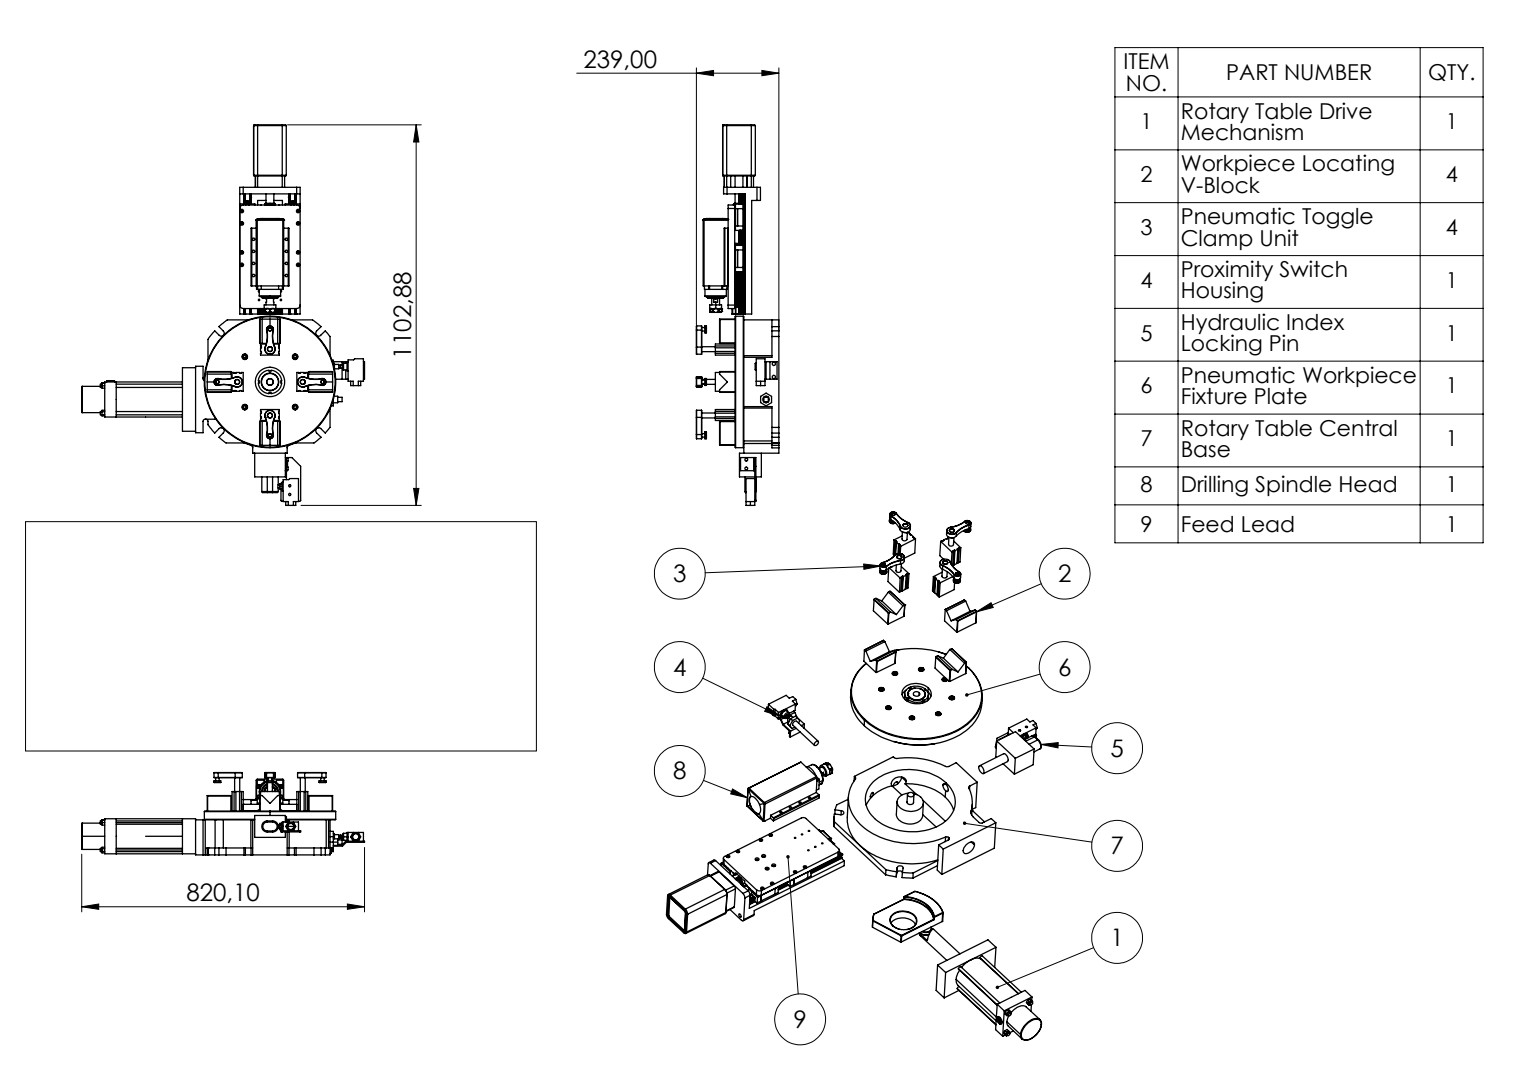
ISO-10303-21;
HEADER;
FILE_DESCRIPTION (('STEP AP214'),
    '1' );
FILE_NAME ('BR-Y-104',
    '2026-10-07T11:37:37',
    ( '' ),
    ( '' ),
    'SwSTEP 2.0',
    'SolidWorks 2020',
    '' );
FILE_SCHEMA (( 'AUTOMOTIVE_DESIGN' ));
ENDSEC;

DATA;
#1 = CARTESIAN_POINT ( 'NONE',  ( 98.82205551832399237, -39.36200594543229414, 279.3785665600675543 ) ) ;
#2 = VECTOR ( 'NONE', #11114, 1000.000000000000000 ) ;
#3 = CARTESIAN_POINT ( 'NONE',  ( -7.205548786489490269E-13, 127.0000000000000000, 111.1250000000000000 ) ) ;
#4 = CARTESIAN_POINT ( 'NONE',  ( 105.4244293397738659, -47.72525222749325735, 147.4584824187689662 ) ) ;
#5 = LINE ( 'NONE', #3140, #30301 ) ;
#6 = CARTESIAN_POINT ( 'NONE',  ( 55.11501535284990183, 101.5999999999999943, 183.9403141659174992 ) ) ;
#7 = DIRECTION ( 'NONE',  ( 0.000000000000000000, 1.000000000000000000, 0.000000000000000000 ) ) ;
#8 = EDGE_CURVE ( 'NONE', #34789, #75812, #45689, .T. ) ;
#9 = CARTESIAN_POINT ( 'NONE',  ( 9.168977498726896158, 73.76155057898466794, 130.2336791939843295 ) ) ;
#10 = CARTESIAN_POINT ( 'NONE',  ( 112.4341072229889136, -46.44469865882210513, 248.9661014663869878 ) ) ;
#11 = CARTESIAN_POINT ( 'NONE',  ( 92.31685958143638970, 83.38015080693119785, -74.38497350661467067 ) ) ;
#12 = AXIS2_PLACEMENT_3D ( 'NONE', #30544, #63723, #30982 ) ;
#13 = ORIENTED_EDGE ( 'NONE', *, *, #80261, .T. ) ;
#14 = CARTESIAN_POINT ( 'NONE',  ( -194.1576000000000022, 0.000000000000000000, -12.69999999999999929 ) ) ;
#15 = EDGE_LOOP ( 'NONE', ( #73624, #35100, #2042, #65680 ) ) ;
#16 = CARTESIAN_POINT ( 'NONE',  ( 97.53157056845665807, -31.04763954905634193, 126.9108633711489915 ) ) ;
#17 = CARTESIAN_POINT ( 'NONE',  ( 83.56670559755357885, -36.73837296219067383, 249.5838068554176630 ) ) ;
#18 = EDGE_CURVE ( 'NONE', #81211, #49424, #24383, .T. ) ;
#19 = VERTEX_POINT ( 'NONE', #31186 ) ;
#20 = ORIENTED_EDGE ( 'NONE', *, *, #86122, .T. ) ;
#21 = ORIENTED_EDGE ( 'NONE', *, *, #73612, .F. ) ;
#22 = DIRECTION ( 'NONE',  ( 0.000000000000000000, 0.000000000000000000, -1.000000000000000000 ) ) ;
#23 = LINE ( 'NONE', #20915, #47197 ) ;
#24 = CARTESIAN_POINT ( 'NONE',  ( 199.3900000000000148, 46.38749999999999574, -50.79999999999999716 ) ) ;
#25 = CARTESIAN_POINT ( 'NONE',  ( 179.7974245136208253, -36.32844715993472562, 237.4678068554150059 ) ) ;
#26 = CARTESIAN_POINT ( 'NONE',  ( 108.8610815749077574, -28.26302276435299987, 182.7404713219719667 ) ) ;
#27 = CARTESIAN_POINT ( 'NONE',  ( 118.1260584382194025, -36.12034675239389259, 269.8822919425776945 ) ) ;
#28 = DIRECTION ( 'NONE',  ( 0.7071067811865491270, -0.7071067811865459074, 7.071067811865492096E-16 ) ) ;
#29 = EDGE_LOOP ( 'NONE', ( #51270, #35552, #65434, #23515 ) ) ;
#30 = CARTESIAN_POINT ( 'NONE',  ( 0.8292115003195463796, 69.84999999999999432, 118.5559999999999832 ) ) ;
#31 = VECTOR ( 'NONE', #9113, 1000.000000000000000 ) ;
#32 = DIRECTION ( 'NONE',  ( 0.2588190451025215166, 0.000000000000000000, -0.9659258262890680902 ) ) ;
#33 = ORIENTED_EDGE ( 'NONE', *, *, #1736, .F. ) ;
#34 = ORIENTED_EDGE ( 'NONE', *, *, #61854, .T. ) ;
#35 = EDGE_CURVE ( 'NONE', #22057, #40854, #8280, .T. ) ;
#36 = DIRECTION ( 'NONE',  ( 0.000000000000000000, 0.000000000000000000, -1.000000000000000000 ) ) ;
#37 = DIRECTION ( 'NONE',  ( 0.000000000000000000, 0.000000000000000000, 1.000000000000000000 ) ) ;
#38 = LINE ( 'NONE', #47715, #64581 ) ;
#39 = CARTESIAN_POINT ( 'NONE',  ( 20.03715912545644073, -24.42818131006202265, 129.9678068554150627 ) ) ;
#40 = CARTESIAN_POINT ( 'NONE',  ( 90.06670390244703128, -104.2784471599414644, 0.2178068554180012661 ) ) ;
#41 = CIRCLE ( 'NONE', #63855, 11.49999999999999645 ) ;
#42 = CARTESIAN_POINT ( 'NONE',  ( 112.8494018163660968, -30.44343212223953543, 198.9067055423629711 ) ) ;
#43 = CARTESIAN_POINT ( 'NONE',  ( 116.1621043582934902, -29.05491297703968101, 74.38419670448293175 ) ) ;
#44 = CARTESIAN_POINT ( 'NONE',  ( 140.9629299006807059, -46.47944715994099596, -5.074374724088994704 ) ) ;
#45 = VERTEX_POINT ( 'NONE', #80264 ) ;
#46 = DIRECTION ( 'NONE',  ( 0.000000000000000000, 0.000000000000000000, -1.000000000000000000 ) ) ;
#47 = ORIENTED_EDGE ( 'NONE', *, *, #89162, .T. ) ;
#48 = LINE ( 'NONE', #40482, #73685 ) ;
#49 = ORIENTED_EDGE ( 'NONE', *, *, #34842, .F. ) ;
#50 = LINE ( 'NONE', #6413, #88589 ) ;
#51 = CARTESIAN_POINT ( 'NONE',  ( 151.0371591254573502, -24.42818131005592974, 249.9678068554149490 ) ) ;
#52 = DIRECTION ( 'NONE',  ( 0.000000000000000000, 0.000000000000000000, -1.000000000000000000 ) ) ;
#53 = AXIS2_PLACEMENT_3D ( 'NONE', #43663, #9164, #36861 ) ;
#54 = CARTESIAN_POINT ( 'NONE',  ( 50.56670390244699576, -22.48495420874030515, 342.9256252759119548 ) ) ;
#55 = ORIENTED_EDGE ( 'NONE', *, *, #81296, .T. ) ;
#56 = CARTESIAN_POINT ( 'NONE',  ( 117.9477513149503523, -41.48675964724572651, 58.49848241876792798 ) ) ;
#58 = DIRECTION ( 'NONE',  ( 0.000000000000000000, -1.000000000000000000, 0.000000000000000000 ) ) ;
#57 = FACE_OUTER_BOUND ( 'NONE', #13007, .T. ) ;
#59 = LINE ( 'NONE', #15039, #77144 ) ;
#60 = CARTESIAN_POINT ( 'NONE',  ( 131.4961476553978912, -17.75123073100106552, 2.855912073278314534 ) ) ;
#61 = EDGE_LOOP ( 'NONE', ( #69387, #53740 ) ) ;
#62 = EDGE_CURVE ( 'NONE', #88900, #78359, #73421, .T. ) ;
#63 = CIRCLE ( 'NONE', #39212, 3.250000000000002665 ) ;
#64 = ADVANCED_FACE ( 'NONE', ( #72976, #57557 ), #58012, .F. ) ;
#65 = DIRECTION ( 'NONE',  ( -0.7071067811865475727, -0.7071067811865475727, 0.000000000000000000 ) ) ;
#66 = ADVANCED_FACE ( 'NONE', ( #65279 ), #44369, .F. ) ;
#67 = DIRECTION ( 'NONE',  ( 0.000000000000000000, -1.000000000000000000, 0.000000000000000000 ) ) ;
#69 = CARTESIAN_POINT ( 'NONE',  ( 163.2449138992999735, -32.11662333284611748, -5.074374724088000832 ) ) ;
#68 = CIRCLE ( 'NONE', #26139, 0.1499999999999965528 ) ;
#70 = VERTEX_POINT ( 'NONE', #52061 ) ;
#71 = CARTESIAN_POINT ( 'NONE',  ( 98.28804800891427362, -28.73186473263583807, 76.73848241876795839 ) ) ;
#72 = ADVANCED_FACE ( 'NONE', ( #9419 ), #85748, .F. ) ;
#74 = CARTESIAN_POINT ( 'NONE',  ( 151.0371591254582881, -46.82818131005593187, 249.9678068554149490 ) ) ;
#73 = FACE_OUTER_BOUND ( 'NONE', #27829, .T. ) ;
#75 = CARTESIAN_POINT ( 'NONE',  ( -9.261585182541612227, 239.0000000000000000, 152.5407914452011369 ) ) ;
#76 = AXIS2_PLACEMENT_3D ( 'NONE', #21854, #16377, #36372 ) ;
#77 = CARTESIAN_POINT ( 'NONE',  ( 128.6924155486683503, -121.3595312563307260, 250.2191008560389776 ) ) ;
#78 = ORIENTED_EDGE ( 'NONE', *, *, #28035, .F. ) ;
#79 = CARTESIAN_POINT ( 'NONE',  ( 116.1942131220465768, -33.21547736372282600, 135.1184824187679396 ) ) ;
#80 = ADVANCED_FACE ( 'NONE', ( #30759 ), #10313, .F. ) ;
#81 = VECTOR ( 'NONE', #81815, 1000.000000000000000 ) ;
#83 = ORIENTED_EDGE ( 'NONE', *, *, #76173, .T. ) ;
#82 = PLANE ( 'NONE',  #68963 ) ;
#84 = CARTESIAN_POINT ( 'NONE',  ( 95.25611604350974915, -37.33230102880721546, 267.3670538473395482 ) ) ;
#85 = DIRECTION ( 'NONE',  ( 0.000000000000000000, 0.000000000000000000, -1.000000000000000000 ) ) ;
#86 = CARTESIAN_POINT ( 'NONE',  ( 143.0667039024470171, -90.27844715994091018, 230.7030882296565721 ) ) ;
#87 = EDGE_CURVE ( 'NONE', #55444, #20525, #67497, .T. ) ;
#88 = CARTESIAN_POINT ( 'NONE',  ( 57.91199999999999903, 20.32000000000000028, 178.6098374884404905 ) ) ;
#89 = CARTESIAN_POINT ( 'NONE',  ( 19.56648329127400032, 0.2215528400590013880, 342.9256252759119548 ) ) ;
#90 = DIRECTION ( 'NONE',  ( 0.000000000000000000, 0.000000000000000000, 1.000000000000000000 ) ) ;
#91 = CARTESIAN_POINT ( 'NONE',  ( -90.24991642302028083, 70.17656663518272353, 94.33976020835999066 ) ) ;
#92 = VECTOR ( 'NONE', #88319, 1000.000000000000000 ) ;
#93 = CARTESIAN_POINT ( 'NONE',  ( 102.2986265273211188, -45.30740241592388884, 187.1727681330549729 ) ) ;
#94 = ORIENTED_EDGE ( 'NONE', *, *, #21602, .F. ) ;
#95 = ORIENTED_EDGE ( 'NONE', *, *, #27973, .F. ) ;
#96 = CARTESIAN_POINT ( 'NONE',  ( 102.7360552222912418, -45.06754756083040547, 163.6149166392309837 ) ) ;
#97 = CARTESIAN_POINT ( 'NONE',  ( 41.56648329127398966, -27.82844715994070484, 78.92562527591199739 ) ) ;
#98 = CARTESIAN_POINT ( 'NONE',  ( 110.5196960824274868, -45.46740155661881033, 19.31967854399191253 ) ) ;
#99 = CARTESIAN_POINT ( 'NONE',  ( 23.49611623194277499, 85.45756874832173366, 299.1102940853953100 ) ) ;
#100 = VECTOR ( 'NONE', #56288, 1000.000000000000000 ) ;
#101 = CARTESIAN_POINT ( 'NONE',  ( 97.80969231062213964, -40.51824920587227297, 266.6357212253427633 ) ) ;
#102 = CARTESIAN_POINT ( 'NONE',  ( 107.3303934170485405, -25.27334761448656764, 321.8751915430112263 ) ) ;
#103 = CIRCLE ( 'NONE', #55178, 11.45913725231036118 ) ;
#104 = CARTESIAN_POINT ( 'NONE',  ( 107.0667039024470313, -104.2784471599420897, -20.48315503890502143 ) ) ;
#105 = CARTESIAN_POINT ( 'NONE',  ( -3.968750000000754508, 127.0000000000000000, 100.8961411191535973 ) ) ;
#106 = CARTESIAN_POINT ( 'NONE',  ( 117.3910620576583312, -35.19077923515891371, 218.9441967044829482 ) ) ;
#107 = CARTESIAN_POINT ( 'NONE',  ( 102.3035641816324102, -89.52844715994213232, -21.78219314458246103 ) ) ;
#108 = ORIENTED_EDGE ( 'NONE', *, *, #23655, .T. ) ;
#109 = ORIENTED_EDGE ( 'NONE', *, *, #12463, .F. ) ;
#110 = CARTESIAN_POINT ( 'NONE',  ( -84.20430400022949868, 76.20343663217360586, -99.77245543246449699 ) ) ;
#111 = CARTESIAN_POINT ( 'NONE',  ( -91.81710919847694186, 87.03046781249439334, -75.00112839233729289 ) ) ;
#112 = CARTESIAN_POINT ( 'NONE',  ( 98.04125204931517601, -41.04130019950920172, 122.6806003489451342 ) ) ;
#113 = DIRECTION ( 'NONE',  ( -1.000000000000000000, 0.000000000000000000, 0.000000000000000000 ) ) ;
#114 = VECTOR ( 'NONE', #52134, 1000.000000000000114 ) ;
#115 = ADVANCED_FACE ( 'NONE', ( #66606 ), #81165, .T. ) ;
#116 = DIRECTION ( 'NONE',  ( 0.000000000000000000, 0.000000000000000000, 1.000000000000000000 ) ) ;
#117 = ORIENTED_EDGE ( 'NONE', *, *, #52215, .T. ) ;
#118 = CARTESIAN_POINT ( 'NONE',  ( 109.6225776363756950, -25.10716277166327615, 25.90419670448196143 ) ) ;
#119 = EDGE_CURVE ( 'NONE', #83222, #86794, #67726, .T. ) ;
#120 = CARTESIAN_POINT ( 'NONE',  ( 116.8850244782298091, -41.80638879970206290, 243.4346728949589647 ) ) ;
#121 = VERTEX_POINT ( 'NONE', #20268 ) ;
#122 = DIRECTION ( 'NONE',  ( 0.000000000000000000, -1.000000000000000000, 0.000000000000000000 ) ) ;
#123 = CARTESIAN_POINT ( 'NONE',  ( 48.16670390244701139, -28.27351298637280408, 342.9256252759109884 ) ) ;
#124 = CARTESIAN_POINT ( 'NONE',  ( 116.9882021585877823, -35.34044312313820058, 168.9370952240663257 ) ) ;
#125 = CARTESIAN_POINT ( 'NONE',  ( 103.0685998583681311, -29.61280089403793525, 58.30237608387695047 ) ) ;
#126 = CARTESIAN_POINT ( 'NONE',  ( 103.0413726597163446, -26.41035368485499646, 166.3603871806729444 ) ) ;
#127 = CIRCLE ( 'NONE', #16099, 7.143750000000004263 ) ;
#128 = DIRECTION ( 'NONE',  ( 1.000000000000000000, 4.163336342344333240E-14, 0.000000000000000000 ) ) ;
#129 = ORIENTED_EDGE ( 'NONE', *, *, #9296, .T. ) ;
#130 = CARTESIAN_POINT ( 'NONE',  ( 27.27158787008327678, 127.0000000000000000, 85.23828826961327820 ) ) ;
#131 = ORIENTED_EDGE ( 'NONE', *, *, #64159, .T. ) ;
#133 = ORIENTED_EDGE ( 'NONE', *, *, #51168, .F. ) ;
#132 = VECTOR ( 'NONE', #74907, 1000.000000000000000 ) ;
#134 = EDGE_CURVE ( 'NONE', #34012, #57634, #4396, .T. ) ;
#135 = DIRECTION ( 'NONE',  ( 0.000000000000000000, -1.000000000000000000, 0.000000000000000000 ) ) ;
#136 = ORIENTED_EDGE ( 'NONE', *, *, #72395, .F. ) ;
#137 = VERTEX_POINT ( 'NONE', #67956 ) ;
#138 = DIRECTION ( 'NONE',  ( 0.000000000000000000, 0.000000000000000000, -1.000000000000000000 ) ) ;
#139 = CARTESIAN_POINT ( 'NONE',  ( 114.8228036748933079, -33.15234975719755539, 103.5924198280769843 ) ) ;
#140 = VECTOR ( 'NONE', #87504, 1000.000000000000000 ) ;
#141 = CARTESIAN_POINT ( 'NONE',  ( 96.49566810458604493, -31.31724962161759507, 245.9499109901969689 ) ) ;
#142 = CARTESIAN_POINT ( 'NONE',  ( 116.8369567342160451, -40.30247308064095790, 218.5470538473399529 ) ) ;
#143 = CARTESIAN_POINT ( 'NONE',  ( 114.8031991714176741, -43.68443766454699073, 34.24419670448197905 ) ) ;
#144 = CARTESIAN_POINT ( 'NONE',  ( 1.925672578516905147E-22, 69.84999999999999432, 130.5560000000000116 ) ) ;
#145 = CARTESIAN_POINT ( 'NONE',  ( 116.7940250750810804, -39.39174829627296504, 94.61447052041835093 ) ) ;
#146 = VECTOR ( 'NONE', #83071, 1000.000000000000000 ) ;
#147 = EDGE_CURVE ( 'NONE', #87632, #64364, #18910, .T. ) ;
#148 = ORIENTED_EDGE ( 'NONE', *, *, #76335, .T. ) ;
#149 = CARTESIAN_POINT ( 'NONE',  ( 70.08426215166053908, -140.6784470016797570, 245.7568090486316805 ) ) ;
#150 = CARTESIAN_POINT ( 'NONE',  ( 98.15811136316399654, -31.42099212808717468, 130.9108633711499863 ) ) ;
#151 = CARTESIAN_POINT ( 'NONE',  ( 106.8402339230401452, -48.62808610490878891, 77.56133956162491927 ) ) ;
#152 = CARTESIAN_POINT ( 'NONE',  ( 104.8318391505165010, -26.46503486849124087, 260.2470538473397710 ) ) ;
#153 = ORIENTED_EDGE ( 'NONE', *, *, #81834, .T. ) ;
#154 = CARTESIAN_POINT ( 'NONE',  ( 115.5175571194294122, -29.60495148624196204, 224.3718157521009573 ) ) ;
#155 = CARTESIAN_POINT ( 'NONE',  ( 47.62500000000000000, 94.53880000000000905, 225.4249999999999829 ) ) ;
#156 = CARTESIAN_POINT ( 'NONE',  ( 107.0664832912739399, -36.72944715994095333, 293.9356252759109793 ) ) ;
#157 = DIRECTION ( 'NONE',  ( 1.000000000000000000, 0.000000000000000000, 0.000000000000000000 ) ) ;
#159 = CARTESIAN_POINT ( 'NONE',  ( 167.2371591254543262, -47.82818131005522844, 249.9678068554149775 ) ) ;
#158 = DIRECTION ( 'NONE',  ( -1.000000000000000078E-15, 0.000000000000000000, 1.000000000000000000 ) ) ;
#160 = CARTESIAN_POINT ( 'NONE',  ( 41.56670390244777735, -36.32844715994104234, 300.4678068554150059 ) ) ;
#161 = CARTESIAN_POINT ( 'NONE',  ( 93.91125933621934507, -111.8737466215629013, -21.78219314458179667 ) ) ;
#162 = DIRECTION ( 'NONE',  ( 3.100000000000000258E-29, -3.100000000000000044E-14, -1.000000000000000000 ) ) ;
#163 = AXIS2_PLACEMENT_3D ( 'NONE', #54109, #40507, #5097 ) ;
#164 = CARTESIAN_POINT ( 'NONE',  ( 88.17226027475679473, -58.72944715994100306, 239.5838068554174924 ) ) ;
#165 = PLANE ( 'NONE',  #8255 ) ;
#166 = ADVANCED_FACE ( 'NONE', ( #82057 ), #80705, .F. ) ;
#167 = CARTESIAN_POINT ( 'NONE',  ( -103.1875000000000000, 127.0000000000000000, -1.080832317973422076E-12 ) ) ;
#169 = ORIENTED_EDGE ( 'NONE', *, *, #32648, .T. ) ;
#168 = DIRECTION ( 'NONE',  ( 0.000000000000000000, 1.000000000000000000, 0.000000000000000000 ) ) ;
#170 = CARTESIAN_POINT ( 'NONE',  ( 147.0667039024470739, -140.6784471599409017, 222.2178068554179902 ) ) ;
#171 = CARTESIAN_POINT ( 'NONE',  ( 96.89273651078235616, -34.20293982824353662, 276.1327681330536734 ) ) ;
#172 = CARTESIAN_POINT ( 'NONE',  ( 117.0331605330187728, -30.31849857022486816, 140.2813395616249750 ) ) ;
#173 = CARTESIAN_POINT ( 'NONE',  ( 106.2234015700748699, -47.79681864418333959, 263.5280062282922131 ) ) ;
#174 = CARTESIAN_POINT ( 'NONE',  ( 51.56670390244799762, -33.35206098992650681, -5.074374724088000832 ) ) ;
#175 = CIRCLE ( 'NONE', #23415, 3.000000000000002665 ) ;
#177 = LINE ( 'NONE', #49653, #51558 ) ;
#176 = DIRECTION ( 'NONE',  ( 1.000000000000000000, 0.000000000000000000, 1.821299053822143307E-16 ) ) ;
#178 = CARTESIAN_POINT ( 'NONE',  ( 164.9212702847350158, -29.73316016639540749, -5.074374724088000832 ) ) ;
#179 = CARTESIAN_POINT ( 'NONE',  ( 84.06648329127399677, -18.82844715994099971, 93.42562527591199739 ) ) ;
#180 = VECTOR ( 'NONE', #42235, 1000.000000000000000 ) ;
#181 = ORIENTED_EDGE ( 'NONE', *, *, #13082, .F. ) ;
#182 = DIRECTION ( 'NONE',  ( 1.000000000000000000, 0.000000000000000000, 0.000000000000000000 ) ) ;
#183 = EDGE_LOOP ( 'NONE', ( #41737, #81659, #77262, #76610 ) ) ;
#184 = CARTESIAN_POINT ( 'NONE',  ( 104.1791519563360993, -28.66003454886012136, 189.7724198280769770 ) ) ;
#185 = EDGE_CURVE ( 'NONE', #48213, #31965, #19881, .T. ) ;
#187 = ORIENTED_EDGE ( 'NONE', *, *, #67758, .F. ) ;
#186 = CARTESIAN_POINT ( 'NONE',  ( 112.0622504009905356, -45.49043716283868832, 187.9900270775093247 ) ) ;
#188 = CARTESIAN_POINT ( 'NONE',  ( -7.661254700127833495, 82.54999999999999716, 275.4630000000000223 ) ) ;
#189 = CARTESIAN_POINT ( 'NONE',  ( 103.8142050530422864, -26.84757730287823563, 161.3299109901969643 ) ) ;
#190 = DIRECTION ( 'NONE',  ( 0.000000000000000000, 1.000000000000000000, 0.000000000000000000 ) ) ;
#191 = EDGE_CURVE ( 'NONE', #23949, #76533, #47936, .T. ) ;
#192 = DIRECTION ( 'NONE',  ( 1.000000000000000000, 0.000000000000000000, 2.283216351027200160E-14 ) ) ;
#193 = DIRECTION ( 'NONE',  ( 0.7071067811865779928, -0.7071067811865171526, 7.071067811865786933E-16 ) ) ;
#194 = AXIS2_PLACEMENT_3D ( 'NONE', #47993, #62984, #27575 ) ;
#195 = LINE ( 'NONE', #54679, #27346 ) ;
#196 = CARTESIAN_POINT ( 'NONE',  ( 31.78666935232898894, -29.62846900982320264, -5.074374724088000832 ) ) ;
#197 = CARTESIAN_POINT ( 'NONE',  ( 97.28369645613162220, -37.51102008256657427, 101.3899109901979472 ) ) ;
#198 = EDGE_LOOP ( 'NONE', ( #58309, #71427, #79095, #45563, #21025 ) ) ;
#199 = ORIENTED_EDGE ( 'NONE', *, *, #77128, .T. ) ;
#201 = ORIENTED_EDGE ( 'NONE', *, *, #40061, .T. ) ;
#200 = VECTOR ( 'NONE', #2081, 1000.000000000000000 ) ;
#202 = CARTESIAN_POINT ( 'NONE',  ( 106.1501016865858844, -27.91533782510476058, 46.59015473446797984 ) ) ;
#203 = DIRECTION ( 'NONE',  ( 5.512527431108029424E-15, -1.000000000000000000, 0.000000000000000000 ) ) ;
#205 = FACE_OUTER_BOUND ( 'NONE', #10836, .T. ) ;
#204 = CARTESIAN_POINT ( 'NONE',  ( 104.6152064257953640, -27.26083179018629465, 196.2784824187679362 ) ) ;
#206 = DIRECTION ( 'NONE',  ( 0.000000000000000000, 0.000000000000000000, -1.000000000000000000 ) ) ;
#207 = DIRECTION ( 'NONE',  ( 1.000000000000000000, 0.000000000000000000, 0.000000000000000000 ) ) ;
#208 = VECTOR ( 'NONE', #84296, 1000.000000000000000 ) ;
#209 = CARTESIAN_POINT ( 'NONE',  ( 37.06648329127298780, 12.92155284005730387, 361.9756252759109998 ) ) ;
#210 = CARTESIAN_POINT ( 'NONE',  ( 41.56670390244777735, -36.32844715994104234, 300.4678068554150059 ) ) ;
#211 = CARTESIAN_POINT ( 'NONE',  ( 67.65599188636636541, -68.44419502099285069, 246.9104243438740696 ) ) ;
#212 = CARTESIAN_POINT ( 'NONE',  ( 107.3333893024683903, -26.32957087652219741, 120.0556252759109555 ) ) ;
#213 = EDGE_LOOP ( 'NONE', ( #60741, #6929, #76892, #6396, #4910, #86505 ) ) ;
#214 = ORIENTED_EDGE ( 'NONE', *, *, #36681, .T. ) ;
#215 = ORIENTED_EDGE ( 'NONE', *, *, #58002, .F. ) ;
#216 = DIRECTION ( 'NONE',  ( -0.000000000000000000, 1.000000000000000000, -0.000000000000000000 ) ) ;
#217 = CARTESIAN_POINT ( 'NONE',  ( 9.720633968232110273E-16, 127.0000000000000000, -111.1250000000000000 ) ) ;
#218 = FACE_OUTER_BOUND ( 'NONE', #6817, .T. ) ;
#219 = CARTESIAN_POINT ( 'NONE',  ( 98.44383420958352815, -35.98725590436672661, 184.0642808457819797 ) ) ;
#220 = CARTESIAN_POINT ( 'NONE',  ( 107.0667039024470313, -104.2784471599414502, 0.2178068554180012661 ) ) ;
#221 = CARTESIAN_POINT ( 'NONE',  ( 104.4907063090252848, -26.97860099647315835, 26.28081536904196014 ) ) ;
#222 = ORIENTED_EDGE ( 'NONE', *, *, #9367, .T. ) ;
#224 = ORIENTED_EDGE ( 'NONE', *, *, #76975, .F. ) ;
#223 = VERTEX_POINT ( 'NONE', #60677 ) ;
#225 = AXIS2_PLACEMENT_3D ( 'NONE', #81195, #12130, #54323 ) ;
#226 = CARTESIAN_POINT ( 'NONE',  ( 136.6090958654750978, -19.77717416134860073, 2.822018739140460308 ) ) ;
#227 = ORIENTED_EDGE ( 'NONE', *, *, #86908, .T. ) ;
#228 = VERTEX_POINT ( 'NONE', #75677 ) ;
#229 = DIRECTION ( 'NONE',  ( 0.7071067811989784069, -0.7071067811741166276, 2.899137802813994686E-29 ) ) ;
#230 = CARTESIAN_POINT ( 'NONE',  ( 115.9278856700424143, -36.79130581669468825, 260.2530118773256049 ) ) ;
#231 = VERTEX_POINT ( 'NONE', #46142 ) ;
#232 = VECTOR ( 'NONE', #61372, 1000.000000000000000 ) ;
#233 = DIRECTION ( 'NONE',  ( 0.000000000000000000, 0.000000000000000000, 1.000000000000000000 ) ) ;
#234 = CARTESIAN_POINT ( 'NONE',  ( -118.6305646578576045, 74.28520294732120988, 54.51736277023807986 ) ) ;
#235 = ORIENTED_EDGE ( 'NONE', *, *, #62757, .T. ) ;
#236 = ORIENTED_EDGE ( 'NONE', *, *, #27432, .F. ) ;
#237 = VECTOR ( 'NONE', #41224, 1000.000000000000114 ) ;
#238 = EDGE_CURVE ( 'NONE', #48773, #70137, #68413, .T. ) ;
#239 = FACE_OUTER_BOUND ( 'NONE', #13018, .T. ) ;
#240 = ORIENTED_EDGE ( 'NONE', *, *, #81916, .T. ) ;
#241 = VERTEX_POINT ( 'NONE', #73874 ) ;
#242 = EDGE_CURVE ( 'NONE', #42621, #19042, #11659, .T. ) ;
#243 = CARTESIAN_POINT ( 'NONE',  ( 102.1978417368446657, -43.31572210571547998, 254.8880903695915947 ) ) ;
#244 = EDGE_CURVE ( 'NONE', #1586, #65784, #48833, .T. ) ;
#245 = CARTESIAN_POINT ( 'NONE',  ( 117.7016330746719035, -39.82606306527180351, 138.5889586092439743 ) ) ;
#246 = CARTESIAN_POINT ( 'NONE',  ( 109.7644292386350457, -47.42453529627131559, 92.78514908543495210 ) ) ;
#247 = SURFACE_STYLE_FILL_AREA ( #77911 ) ;
#248 = DIRECTION ( 'NONE',  ( 0.000000000000000000, 1.000000000000000000, 0.000000000000000000 ) ) ;
#249 = CARTESIAN_POINT ( 'NONE',  ( 118.0406971908402340, -35.41012545131285094, 234.9337205140059552 ) ) ;
#250 = PLANE ( 'NONE',  #16765 ) ;
#251 = CARTESIAN_POINT ( 'NONE',  ( 97.07202379341690346, -35.37891260357572776, 127.2189961379345533 ) ) ;
#252 = ORIENTED_EDGE ( 'NONE', *, *, #45616, .F. ) ;
#253 = CARTESIAN_POINT ( 'NONE',  ( 129.9447564289581010, 80.89704698943971550, 12.61967231918858445 ) ) ;
#255 = EDGE_LOOP ( 'NONE', ( #36658, #16819, #37232, #21617 ) ) ;
#254 = EDGE_CURVE ( 'NONE', #38623, #81994, #26176, .T. ) ;
#256 = VECTOR ( 'NONE', #25789, 1000.000000000000000 ) ;
#257 = EDGE_CURVE ( 'NONE', #42008, #10149, #60224, .T. ) ;
#258 = EDGE_LOOP ( 'NONE', ( #12072, #35059, #37559, #82671 ) ) ;
#259 = CARTESIAN_POINT ( 'NONE',  ( 1.387778780781445676E-14, 224.4999999999999432, 97.27542076772557778 ) ) ;
#260 = EDGE_CURVE ( 'NONE', #76240, #83594, #40692, .T. ) ;
#261 = EDGE_CURVE ( 'NONE', #85910, #25889, #5287, .T. ) ;
#262 = CARTESIAN_POINT ( 'NONE',  ( 50.03799999999999670, 101.5999999999999943, 206.3750000000000000 ) ) ;
#263 = AXIS2_PLACEMENT_3D ( 'NONE', #9661, #10113, #65519 ) ;
#264 = CARTESIAN_POINT ( 'NONE',  ( 113.9865487620526920, -28.11017913222394071, 119.5261014663869474 ) ) ;
#265 = CARTESIAN_POINT ( 'NONE',  ( -6.586072245893089594, 71.69064597417980167, 130.3897833686264676 ) ) ;
#266 = ADVANCED_FACE ( 'NONE', ( #53845 ), #12696, .T. ) ;
#267 = DIRECTION ( 'NONE',  ( 0.000000000000000000, 0.000000000000000000, 1.000000000000000000 ) ) ;
#268 = CYLINDRICAL_SURFACE ( 'NONE', #55688, 7.143750000000004263 ) ;
#271 = CARTESIAN_POINT ( 'NONE',  ( 107.2427983594548948, -47.16656068249876910, 208.5899109901969837 ) ) ;
#270 = CARTESIAN_POINT ( 'NONE',  ( 97.84728005659533778, -40.60342492179871954, 56.64262628539218269 ) ) ;
#269 = LINE ( 'NONE', #28879, #27362 ) ;
#272 = LINE ( 'NONE', #64302, #50971 ) ;
#273 = CARTESIAN_POINT ( 'NONE',  ( 73.06648329127396835, -8.729447159941065237, 14.67562527591093513 ) ) ;
#274 = VERTEX_POINT ( 'NONE', #40238 ) ;
#275 = AXIS2_PLACEMENT_3D ( 'NONE', #19482, #13126, #74898 ) ;
#276 = CARTESIAN_POINT ( 'NONE',  ( 25.56670390244797275, -62.87844715994099687, 262.0928068554150059 ) ) ;
#277 = EDGE_CURVE ( 'NONE', #55396, #20871, #38896, .T. ) ;
#278 = DIRECTION ( 'NONE',  ( 0.000000000000000000, 0.000000000000000000, -1.000000000000000000 ) ) ;
#279 = CARTESIAN_POINT ( 'NONE',  ( 25.56670390244797275, -62.87844715994099687, 173.2178068554149775 ) ) ;
#280 = EDGE_CURVE ( 'NONE', #76657, #85611, #63382, .T. ) ;
#281 = CARTESIAN_POINT ( 'NONE',  ( 147.0268936274260057, -137.6319380618105015, 245.9633055630636704 ) ) ;
#283 = EDGE_LOOP ( 'NONE', ( #66370, #22379, #4924, #25013 ) ) ;
#282 = CARTESIAN_POINT ( 'NONE',  ( 97.18209604296552584, -40.28622700274314639, 266.6013395616253661 ) ) ;
#284 = FACE_OUTER_BOUND ( 'NONE', #2553, .T. ) ;
#285 = CARTESIAN_POINT ( 'NONE',  ( 102.0403423364015509, -46.60028036886249225, 172.2137205140059564 ) ) ;
#286 = CARTESIAN_POINT ( 'NONE',  ( 96.65901483881968659, -33.00673566691533978, 22.06514908543494258 ) ) ;
#287 = CARTESIAN_POINT ( 'NONE',  ( 102.8263616157396854, -46.30098559033366001, 173.2441967044829596 ) ) ;
#288 = DIRECTION ( 'NONE',  ( 0.000000000000000000, 1.000000000000000000, 1.541976423090495239E-15 ) ) ;
#289 = CARTESIAN_POINT ( 'NONE',  ( 194.0667039024482392, -40.32844715993407192, 129.9678068554150343 ) ) ;
#291 = DIRECTION ( 'NONE',  ( -0.9254794337955623007, -0.3787978585227819162, 0.000000000000000000 ) ) ;
#290 = DIRECTION ( 'NONE',  ( 1.000000000000000000, 6.897260540483778545E-11, 0.000000000000000000 ) ) ;
#292 = CARTESIAN_POINT ( 'NONE',  ( 102.0670550211478940, -27.97049802524514561, 190.4897919370553723 ) ) ;
#293 = LINE ( 'NONE', #27992, #72853 ) ;
#294 = ORIENTED_EDGE ( 'NONE', *, *, #45450, .F. ) ;
#295 = DIRECTION ( 'NONE',  ( 0.000000000000000000, -1.000000000000000000, 0.000000000000000000 ) ) ;
#296 = VERTEX_POINT ( 'NONE', #28870 ) ;
#297 = ORIENTED_EDGE ( 'NONE', *, *, #22548, .T. ) ;
#298 = EDGE_CURVE ( 'NONE', #22750, #69972, #67790, .T. ) ;
#299 = ORIENTED_EDGE ( 'NONE', *, *, #29707, .F. ) ;
#300 = CARTESIAN_POINT ( 'NONE',  ( 108.9812119692459049, -46.95502683147942236, 78.72419670448194040 ) ) ;
#301 = DIRECTION ( 'NONE',  ( 1.000000000000000000, 0.000000000000000000, -9.299908063537909262E-17 ) ) ;
#302 = EDGE_CURVE ( 'NONE', #30540, #70341, #82951, .T. ) ;
#303 = EDGE_CURVE ( 'NONE', #54782, #72244, #41574, .T. ) ;
#304 = CARTESIAN_POINT ( 'NONE',  ( 113.7066566934868348, -44.24661119772650864, 118.1542348793510797 ) ) ;
#305 = CARTESIAN_POINT ( 'NONE',  ( 114.3743266858445935, -29.18402207539437399, 170.4641967044829585 ) ) ;
#306 = EDGE_CURVE ( 'NONE', #30320, #66948, #55191, .T. ) ;
#307 = CIRCLE ( 'NONE', #48127, 2.500000000000002220 ) ;
#308 = CARTESIAN_POINT ( 'NONE',  ( 106.3786087989843736, -45.75936958534449417, 266.9505150661723860 ) ) ;
#309 = ORIENTED_EDGE ( 'NONE', *, *, #18028, .F. ) ;
#310 = EDGE_LOOP ( 'NONE', ( #10446, #4525, #31738, #66778 ) ) ;
#311 = VERTEX_POINT ( 'NONE', #89763 ) ;
#312 = CARTESIAN_POINT ( 'NONE',  ( 29.00000000000003553, 172.0000000000000000, 183.8826257785461280 ) ) ;
#313 = CARTESIAN_POINT ( 'NONE',  ( 0.000000000000000000, 184.0000000000000000, 101.0189074266571794 ) ) ;
#314 = DIRECTION ( 'NONE',  ( 1.000000000000000078E-15, -1.000000000000000000, 3.100000000000000044E-14 ) ) ;
#315 = CARTESIAN_POINT ( 'NONE',  ( 105.8005616001767919, -26.72389448867465589, 20.17631252315041124 ) ) ;
#316 = CARTESIAN_POINT ( 'NONE',  ( 89.95943163722039060, 94.84315624882769669, 94.61941200740749025 ) ) ;
#317 = LINE ( 'NONE', #34380, #47959 ) ;
#318 = FACE_OUTER_BOUND ( 'NONE', #73984, .T. ) ;
#319 = DIRECTION ( 'NONE',  ( 0.000000000000000000, 0.000000000000000000, -1.000000000000000000 ) ) ;
#320 = CARTESIAN_POINT ( 'NONE',  ( 116.7068942081672276, -31.36975501082240569, 29.24229194257799236 ) ) ;
#321 = LINE ( 'NONE', #15311, #8132 ) ;
#323 = EDGE_LOOP ( 'NONE', ( #9517, #37915, #44390, #42427, #11200 ) ) ;
#322 = AXIS2_PLACEMENT_3D ( 'NONE', #12515, #67464, #82472 ) ;
#324 = CARTESIAN_POINT ( 'NONE',  ( 199.3900000000000148, 59.08750000000000568, -50.79999999999999716 ) ) ;
#325 = DIRECTION ( 'NONE',  ( 0.000000000000000000, 0.000000000000000000, 1.000000000000000000 ) ) ;
#326 = CARTESIAN_POINT ( 'NONE',  ( 115.3104451506078192, -40.98773602117310588, 91.26523322673496352 ) ) ;
#327 = AXIS2_PLACEMENT_3D ( 'NONE', #13933, #74815, #67998 ) ;
#328 = VECTOR ( 'NONE', #6728, 1000.000000000000114 ) ;
#329 = CARTESIAN_POINT ( 'NONE',  ( 188.5667039024483529, -48.82844715993431350, 293.2178068554150059 ) ) ;
#330 = VECTOR ( 'NONE', #57470, 1000.000000000000000 ) ;
#331 = DIRECTION ( 'NONE',  ( -1.000000000000000000, -4.299999999999999979E-14, -1.000000000000000078E-15 ) ) ;
#332 = ORIENTED_EDGE ( 'NONE', *, *, #80901, .T. ) ;
#333 = ORIENTED_EDGE ( 'NONE', *, *, #85560, .F. ) ;
#334 = DIRECTION ( 'NONE',  ( -1.000000000000000078E-15, 1.000000000000000000, 0.000000000000000000 ) ) ;
#335 = ORIENTED_EDGE ( 'NONE', *, *, #11625, .F. ) ;
#336 = ORIENTED_EDGE ( 'NONE', *, *, #71330, .T. ) ;
#337 = DIRECTION ( 'NONE',  ( 0.000000000000000000, 1.000000000000000000, 0.000000000000000000 ) ) ;
#338 = CARTESIAN_POINT ( 'NONE',  ( 105.5787418010314695, -46.69191849206237066, 143.8901547344689789 ) ) ;
#339 = DIRECTION ( 'NONE',  ( 0.000000000000000000, 0.000000000000000000, -1.000000000000000000 ) ) ;
#340 = CARTESIAN_POINT ( 'NONE',  ( 108.5410322698540853, -26.38715707682645117, 100.9641967044829727 ) ) ;
#341 = CARTESIAN_POINT ( 'NONE',  ( -179.8898777604655095, 101.5999999999999943, 114.2999999999999972 ) ) ;
#342 = ORIENTED_EDGE ( 'NONE', *, *, #66737, .T. ) ;
#343 = CARTESIAN_POINT ( 'NONE',  ( -479.3614999999999782, 100.8062500000000057, 94.61194598552329182 ) ) ;
#344 =( BOUNDED_CURVE ( )  B_SPLINE_CURVE ( 3, ( #44, #89538, #6404, #82288 ),
 .UNSPECIFIED., .F., .F. ) 
 B_SPLINE_CURVE_WITH_KNOTS ( ( 4, 4 ),
 ( 1.570796326796012332, 3.141592653591100071 ),
 .UNSPECIFIED. ) 
 CURVE ( )  GEOMETRIC_REPRESENTATION_ITEM ( )  RATIONAL_B_SPLINE_CURVE ( ( 1.000000000000000000, 0.8047378541243199734, 0.8047378541243199734, 1.000000000000000000 ) ) 
 REPRESENTATION_ITEM ( '' )  );
#345 = ORIENTED_EDGE ( 'NONE', *, *, #9906, .F. ) ;
#347 = EDGE_CURVE ( 'NONE', #71530, #74616, #28405, .T. ) ;
#346 = EDGE_LOOP ( 'NONE', ( #42852, #56752, #84948, #3553, #65109, #46842, #22187 ) ) ;
#348 = EDGE_CURVE ( 'NONE', #63582, #58541, #14803, .T. ) ;
#349 = EDGE_CURVE ( 'NONE', #47011, #27495, #88110, .T. ) ;
#351 = LINE ( 'NONE', #55290, #78955 ) ;
#350 = AXIS2_PLACEMENT_3D ( 'NONE', #71260, #57605, #29916 ) ;
#352 = ORIENTED_EDGE ( 'NONE', *, *, #65760, .T. ) ;
#353 = CARTESIAN_POINT ( 'NONE',  ( 99.85651329992167291, -30.12038005267077878, 275.7356252759109907 ) ) ;
#354 = CARTESIAN_POINT ( 'NONE',  ( 102.3028228262999164, -26.72980997527264790, 136.4422919425779526 ) ) ;
#355 = DIRECTION ( 'NONE',  ( 1.000000000000000078E-15, 1.000000000000000083E-30, -1.000000000000000000 ) ) ;
#356 = DIRECTION ( 'NONE',  ( 0.000000000000000000, 0.000000000000000000, 1.000000000000000000 ) ) ;
#357 = CARTESIAN_POINT ( 'NONE',  ( 103.8413319783160489, -46.68031304110885316, 78.32705384733995402 ) ) ;
#358 = CARTESIAN_POINT ( 'NONE',  ( 113.1782937855189175, -44.75186858143347024, 263.0939586106779871 ) ) ;
#359 = ORIENTED_EDGE ( 'NONE', *, *, #83740, .T. ) ;
#360 = DIRECTION ( 'NONE',  ( 0.000000000000000000, 0.000000000000000000, -1.000000000000000000 ) ) ;
#361 = EDGE_CURVE ( 'NONE', #26848, #11707, #28630, .T. ) ;
#362 = ADVANCED_FACE ( 'NONE', ( #20710 ), #6627, .T. ) ;
#363 = CYLINDRICAL_SURFACE ( 'NONE', #49100, 2.517500000000005844 ) ;
#364 = ORIENTED_EDGE ( 'NONE', *, *, #10443, .F. ) ;
#365 = EDGE_CURVE ( 'NONE', #79893, #74303, #7526, .T. ) ;
#366 = DIRECTION ( 'NONE',  ( 0.000000000000000000, 1.000000000000000000, 0.000000000000000000 ) ) ;
#367 = CARTESIAN_POINT ( 'NONE',  ( 8.616376310055921195, 91.75252788878626120, 118.2428346993085313 ) ) ;
#368 = CARTESIAN_POINT ( 'NONE',  ( 106.5180884070038161, -25.68959433010697779, 45.12800622829193742 ) ) ;
#369 = DIRECTION ( 'NONE',  ( 0.000000000000000000, 0.000000000000000000, 1.000000000000000000 ) ) ;
#370 = ADVANCED_FACE ( 'NONE', ( #49293, #62029 ), #15244, .T. ) ;
#371 = FACE_OUTER_BOUND ( 'NONE', #73680, .T. ) ;
#372 = CARTESIAN_POINT ( 'NONE',  ( 115.7849560329669316, -41.79918665415381440, 93.40735705935379940 ) ) ;
#373 = CARTESIAN_POINT ( 'NONE',  ( 113.6564618781686704, -45.68400828401192371, 33.08133956162595268 ) ) ;
#375 = CARTESIAN_POINT ( 'NONE',  ( 116.9011659702703270, -33.23038410113878882, 110.0984824187679578 ) ) ;
#374 = CARTESIAN_POINT ( 'NONE',  ( 123.6837132603319560, -55.86395651782485317, 239.5838068554170377 ) ) ;
#376 = FACE_BOUND ( 'NONE', #32605, .T. ) ;
#377 = DIRECTION ( 'NONE',  ( -3.100000000000000258E-29, 3.100000000000000044E-14, 1.000000000000000000 ) ) ;
#378 = VERTEX_POINT ( 'NONE', #7971 ) ;
#379 = FACE_OUTER_BOUND ( 'NONE', #43441, .T. ) ;
#380 = LINE ( 'NONE', #54868, #23274 ) ;
#381 = CYLINDRICAL_SURFACE ( 'NONE', #47045, 27.49999999999999645 ) ;
#382 = EDGE_LOOP ( 'NONE', ( #48463, #62234, #46660, #29247, #79434, #62043 ) ) ;
#384 = EDGE_CURVE ( 'NONE', #62636, #60868, #42469, .T. ) ;
#383 = AXIS2_PLACEMENT_3D ( 'NONE', #79227, #30612, #36545 ) ;
#385 = CARTESIAN_POINT ( 'NONE',  ( 97.81305373959743577, -40.51655628150228949, 62.63606721061723448 ) ) ;
#387 = ORIENTED_EDGE ( 'NONE', *, *, #40134, .F. ) ;
#386 = CARTESIAN_POINT ( 'NONE',  ( 113.7136498174399577, -45.61921998050937077, 188.0994347997199725 ) ) ;
#388 = DIRECTION ( 'NONE',  ( 0.000000000000000000, 0.000000000000000000, 1.000000000000000000 ) ) ;
#389 = CARTESIAN_POINT ( 'NONE',  ( 116.3968524479345348, -41.42853965253563331, 199.4556252759109611 ) ) ;
#390 = DIRECTION ( 'NONE',  ( 0.000000000000000000, 0.000000000000000000, -1.000000000000000000 ) ) ;
#391 = CARTESIAN_POINT ( 'NONE',  ( -12.70000000000000107, 82.54999999999999716, 117.8738102209307641 ) ) ;
#392 = ADVANCED_FACE ( 'NONE', ( #48831 ), #55637, .F. ) ;
#393 = CARTESIAN_POINT ( 'NONE',  ( -487.2989999999999782, 14.28749999999982201, 90.48749999999999716 ) ) ;
#394 = VERTEX_POINT ( 'NONE', #62925 ) ;
#395 = CIRCLE ( 'NONE', #51150, 2.029999999999997140 ) ;
#396 = CONTEXT_DEPENDENT_SHAPE_REPRESENTATION ( #72491, #66277 ) ;
#397 = VERTEX_POINT ( 'NONE', #70200 ) ;
#398 = EDGE_LOOP ( 'NONE', ( #88242, #56816, #40923, #15353 ) ) ;
#399 = AXIS2_PLACEMENT_3D ( 'NONE', #39695, #12012, #46047 ) ;
#400 = B_SPLINE_CURVE_WITH_KNOTS ( 'NONE', 3,
 ( #74384, #34379, #5797, #83006, #53452, #62087, #20761, #48432, #41187, #82114, #19868, #6241, #39844, #69366, #89822, #68914, #6681, #20327 ),
 .UNSPECIFIED., .F., .F.,
 ( 4, 2, 2, 2, 2, 2, 2, 2, 4 ),
 ( 0.000000000000000000, 0.06249223058255102409, 0.1249844611651020482, 0.1874766917476530792, 0.2499689223302040963, 0.3124611529127551135, 0.3749533834953061584, 0.4374456140778571478, 0.4999378446604081927 ),
 .UNSPECIFIED. ) ;
#401 = ORIENTED_EDGE ( 'NONE', *, *, #80513, .F. ) ;
#402 = CARTESIAN_POINT ( 'NONE',  ( 0.000000000000000000, 8.255000000000000782, 0.000000000000000000 ) ) ;
#403 = CARTESIAN_POINT ( 'NONE',  ( 100.7501737310821994, -45.80018108968007340, 233.0803871806729717 ) ) ;
#404 = CARTESIAN_POINT ( 'NONE',  ( 107.0664832912739399, -36.72944715994095333, 293.6356252759106837 ) ) ;
#405 = LINE ( 'NONE', #34471, #15075 ) ;
#406 = EDGE_CURVE ( 'NONE', #68641, #20681, #82800, .T. ) ;
#409 = ADVANCED_FACE ( 'NONE', ( #6043 ), #47786, .F. ) ;
#408 = DIRECTION ( 'NONE',  ( 0.000000000000000000, 0.000000000000000000, 1.000000000000000000 ) ) ;
#407 = DIRECTION ( 'NONE',  ( -1.000000000000000078E-15, 1.000000000000000000, 0.000000000000000000 ) ) ;
#410 = LINE ( 'NONE', #49435, #25440 ) ;
#411 = CARTESIAN_POINT ( 'NONE',  ( 96.66715014961923202, -32.91509328854561289, 21.03467289495897319 ) ) ;
#412 = ORIENTED_EDGE ( 'NONE', *, *, #13605, .T. ) ;
#413 = ORIENTED_EDGE ( 'NONE', *, *, #1503, .F. ) ;
#414 = CARTESIAN_POINT ( 'NONE',  ( 89.10937460273881072, -56.62589376934804619, 14.92562527591089072 ) ) ;
#415 = DIRECTION ( 'NONE',  ( 1.000000000000000000, 0.000000000000000000, 0.000000000000000000 ) ) ;
#416 = CARTESIAN_POINT ( 'NONE',  ( 104.3638673426610950, -27.29495504168068365, 221.2984824187679465 ) ) ;
#417 =( REPRESENTATION_RELATIONSHIP ('NONE','NONE', #82876, #19449 ) REPRESENTATION_RELATIONSHIP_WITH_TRANSFORMATION ( #69892 )SHAPE_REPRESENTATION_RELATIONSHIP( ) );
#418 = LINE ( 'NONE', #69017, #71892 ) ;
#419 = VECTOR ( 'NONE', #36946, 1000.000000000000000 ) ;
#420 = CARTESIAN_POINT ( 'NONE',  ( 112.4472966703648780, -46.45872411559670212, 98.97848241876694431 ) ) ;
#421 = CARTESIAN_POINT ( 'NONE',  ( 97.81193015299326987, -40.51731617131004271, 31.63594527021773573 ) ) ;
#422 = CARTESIAN_POINT ( 'NONE',  ( 99.09526974470551863, -30.55101700259475095, 21.80228081981730526 ) ) ;
#423 = ORIENTED_EDGE ( 'NONE', *, *, #49489, .T. ) ;
#424 = EDGE_CURVE ( 'NONE', #58432, #84394, #41641, .T. ) ;
#425 = DIRECTION ( 'NONE',  ( 0.000000000000000000, 0.000000000000000000, -1.000000000000000000 ) ) ;
#426 = ORIENTED_EDGE ( 'NONE', *, *, #55411, .F. ) ;
#427 = EDGE_LOOP ( 'NONE', ( #4062, #28838, #78754, #43787 ) ) ;
#428 = CARTESIAN_POINT ( 'NONE',  ( -92.26493792250037984, 84.21376545118704371, 74.44936585838431142 ) ) ;
#429 = CARTESIAN_POINT ( 'NONE',  ( 114.5810018449060834, -31.08954144758037685, 260.7825356868496556 ) ) ;
#430 = VECTOR ( 'NONE', #89507, 1000.000000000000000 ) ;
#431 = ADVANCED_FACE ( 'NONE', ( #81897 ), #67340, .F. ) ;
#432 = CARTESIAN_POINT ( 'NONE',  ( 164.7830935719630361, -29.99615139349950965, 193.9678068554150059 ) ) ;
#433 = DIRECTION ( 'NONE',  ( 0.000000000000000000, 0.000000000000000000, -1.000000000000000000 ) ) ;
#434 = CARTESIAN_POINT ( 'NONE',  ( 105.8694971003958614, -26.37070548771162493, 321.6188579224977389 ) ) ;
#435 = CARTESIAN_POINT ( 'NONE',  ( 85.00925061400988625, 69.93366089391891194, -82.64146475440696804 ) ) ;
#436 = ORIENTED_EDGE ( 'NONE', *, *, #26526, .T. ) ;
#437 = DIRECTION ( 'NONE',  ( 3.999999999999999995E-14, -1.000000000000000000, 4.100000000000000342E-29 ) ) ;
#438 = CARTESIAN_POINT ( 'NONE',  ( 101.9929361239610586, -45.44564905068737914, 183.1569278323868275 ) ) ;
#439 = ORIENTED_EDGE ( 'NONE', *, *, #54997, .F. ) ;
#440 = CARTESIAN_POINT ( 'NONE',  ( 103.5987056385471448, -46.56110768157568458, 57.30705384733997221 ) ) ;
#441 = ORIENTED_EDGE ( 'NONE', *, *, #18893, .T. ) ;
#442 = CARTESIAN_POINT ( 'NONE',  ( 110.7250417795893611, -29.43255185136001728, 277.5252332267342581 ) ) ;
#443 = DIRECTION ( 'NONE',  ( 0.000000000000000000, 0.000000000000000000, -1.000000000000000000 ) ) ;
#444 = CARTESIAN_POINT ( 'NONE',  ( 113.3375292005774639, -44.23527279707086279, 193.1299109901969757 ) ) ;
#445 = CARTESIAN_POINT ( 'NONE',  ( 23.75871628398702384, 82.54999999999999716, 298.1325000000000500 ) ) ;
#446 = DIRECTION ( 'NONE',  ( 1.000000000000000000, 8.843517682682131024E-16, 1.000000000000000078E-15 ) ) ;
#447 = DIRECTION ( 'NONE',  ( 0.000000000000000000, 1.000000000000000000, 0.000000000000000000 ) ) ;
#448 = CARTESIAN_POINT ( 'NONE',  ( 57.56670390244832447, -48.82844715994039575, 257.2178068554150627 ) ) ;
#449 = EDGE_CURVE ( 'NONE', #89731, #57212, #70727, .T. ) ;
#450 = CARTESIAN_POINT ( 'NONE',  ( 100.8224507837568638, -45.17634439094529597, 253.0699109901969450 ) ) ;
#451 = CARTESIAN_POINT ( 'NONE',  ( 108.4288913835557935, -46.66050271621784873, 117.6868369591917798 ) ) ;
#452 = ORIENTED_EDGE ( 'NONE', *, *, #80459, .T. ) ;
#453 = LINE ( 'NONE', #77219, #11024 ) ;
#454 = ORIENTED_EDGE ( 'NONE', *, *, #16500, .T. ) ;
#455 = CARTESIAN_POINT ( 'NONE',  ( 117.6520138419322734, -33.39117794972031561, 125.0575300378149706 ) ) ;
#456 = CARTESIAN_POINT ( 'NONE',  ( 120.0602177517065314, 48.67389603571125178, -51.28856941560783866 ) ) ;
#457 = AXIS2_PLACEMENT_3D ( 'NONE', #40016, #13662, #12778 ) ;
#458 = ORIENTED_EDGE ( 'NONE', *, *, #7648, .F. ) ;
#460 = EDGE_CURVE ( 'NONE', #23716, #59746, #25705, .T. ) ;
#459 = ORIENTED_EDGE ( 'NONE', *, *, #13256, .F. ) ;
#462 = VERTEX_POINT ( 'NONE', #5128 ) ;
#461 = EDGE_CURVE ( 'NONE', #89089, #79893, #19649, .T. ) ;
#463 = LINE ( 'NONE', #21362, #81231 ) ;
#464 = ADVANCED_FACE ( 'NONE', ( #20109, #60985 ), #12393, .T. ) ;
#465 = DIRECTION ( 'NONE',  ( 1.000000000000000078E-15, -1.000000000000000083E-30, -1.000000000000000000 ) ) ;
#466 = DIRECTION ( 'NONE',  ( 9.351236661543306751E-17, -3.725950533538267725E-29, -1.000000000000000000 ) ) ;
#467 = CARTESIAN_POINT ( 'NONE',  ( 46.03715912545432332, -48.62818131006086020, 249.9678068554150343 ) ) ;
#468 = CARTESIAN_POINT ( 'NONE',  ( 165.2748236753145079, -30.08671355699731720, 313.9678068554149490 ) ) ;
#469 = CARTESIAN_POINT ( 'NONE',  ( 114.5787023362084085, -39.92261033116096058, 166.3252332267339852 ) ) ;
#470 = CARTESIAN_POINT ( 'NONE',  ( 99.31704471179752147, -28.81544643672065220, 266.7051490854347549 ) ) ;
#471 = CARTESIAN_POINT ( 'NONE',  ( 181.9694315774339941, -34.03355364505720360, -5.074374724088000832 ) ) ;
#472 = ORIENTED_EDGE ( 'NONE', *, *, #66905, .F. ) ;
#473 = CARTESIAN_POINT ( 'NONE',  ( 10.08011576702975809, 74.81331742494347736, 118.1269967869636019 ) ) ;
#474 = EDGE_CURVE ( 'NONE', #57694, #54558, #12854, .T. ) ;
#475 = DIRECTION ( 'NONE',  ( 0.000000000000000000, 1.000000000000000000, 0.000000000000000000 ) ) ;
#476 = ORIENTED_EDGE ( 'NONE', *, *, #40956, .T. ) ;
#477 = ORIENTED_EDGE ( 'NONE', *, *, #19060, .T. ) ;
#478 = ADVANCED_FACE ( 'NONE', ( #33732 ), #15616, .T. ) ;
#479 = LINE ( 'NONE', #75450, #54659 ) ;
#480 = VECTOR ( 'NONE', #16393, 1000.000000000000000 ) ;
#481 = LINE ( 'NONE', #28173, #48342 ) ;
#482 = FACE_OUTER_BOUND ( 'NONE', #29717, .T. ) ;
#483 = LINE ( 'NONE', #35438, #14390 ) ;
#484 = CARTESIAN_POINT ( 'NONE',  ( 125.0664851986225159, -56.72944715994101728, 14.67562527591098842 ) ) ;
#485 = EDGE_CURVE ( 'NONE', #9163, #84782, #46440, .T. ) ;
#486 = CARTESIAN_POINT ( 'NONE',  ( 113.4141308401190287, -30.97102092343966007, 208.8352769709339896 ) ) ;
#487 = CARTESIAN_POINT ( 'NONE',  ( 115.7653496281367325, -43.62456195820889349, 48.30514908543492680 ) ) ;
#488 = ORIENTED_EDGE ( 'NONE', *, *, #73147, .F. ) ;
#489 = CARTESIAN_POINT ( 'NONE',  ( 47.62500000000000000, 111.1250000000000000, 257.1750000000000114 ) ) ;
#490 = ORIENTED_EDGE ( 'NONE', *, *, #23966, .T. ) ;
#491 = AXIS2_PLACEMENT_3D ( 'NONE', #81875, #41838, #63202 ) ;
#492 = CARTESIAN_POINT ( 'NONE',  ( -75.10852726169378002, 77.68452076096561143, -91.72954497613109481 ) ) ;
#493 = ORIENTED_EDGE ( 'NONE', *, *, #28288, .T. ) ;
#494 = CARTESIAN_POINT ( 'NONE',  ( 100.9540432847708757, -28.70751825035962668, 261.5939957165031728 ) ) ;
#495 = ORIENTED_EDGE ( 'NONE', *, *, #3649, .T. ) ;
#496 = DIRECTION ( 'NONE',  ( 0.000000000000000000, 1.000000000000000000, 0.000000000000000000 ) ) ;
#497 = DIRECTION ( 'NONE',  ( 0.7071067811864661934, 0.7071067811866289521, 7.071067811864654918E-16 ) ) ;
#498 = CARTESIAN_POINT ( 'NONE',  ( 68.18676274767041434, -81.16192765749869409, 247.4310652601930087 ) ) ;
#499 = AXIS2_PLACEMENT_3D ( 'NONE', #66233, #38984, #31726 ) ;
#500 = DIRECTION ( 'NONE',  ( 0.000000000000000000, 0.000000000000000000, 1.000000000000000000 ) ) ;
#501 = ORIENTED_EDGE ( 'NONE', *, *, #4272, .F. ) ;
#502 = CARTESIAN_POINT ( 'NONE',  ( 117.0750736332619937, -31.98354782443029620, 64.19086337114899266 ) ) ;
#504 = CARTESIAN_POINT ( 'NONE',  ( 85.31568053864954493, 74.16976894168004719, -98.82395782888116287 ) ) ;
#503 = PLANE ( 'NONE',  #15905 ) ;
#505 = CARTESIAN_POINT ( 'NONE',  ( 123.0664832912757021, -36.72944715993921960, 13.92562527591098487 ) ) ;
#506 = CARTESIAN_POINT ( 'NONE',  ( 132.5731111080376081, -16.41810224486803449, 1.981704920701433448 ) ) ;
#507 = ORIENTED_EDGE ( 'NONE', *, *, #40768, .T. ) ;
#508 = DIRECTION ( 'NONE',  ( -1.000000000000000000, -1.734723475976808672E-15, 0.000000000000000000 ) ) ;
#509 = PLANE ( 'NONE',  #44376 ) ;
#510 = DIRECTION ( 'NONE',  ( 1.000000000000000000, 0.000000000000000000, 0.000000000000000000 ) ) ;
#511 = EDGE_LOOP ( 'NONE', ( #26969, #6552, #8684, #42903 ) ) ;
#512 = CARTESIAN_POINT ( 'NONE',  ( 114.0955628336689500, -44.50577255156974843, 129.1613395616249704 ) ) ;
#515 = EDGE_CURVE ( 'NONE', #85162, #7841, #6469, .T. ) ;
#514 = CARTESIAN_POINT ( 'NONE',  ( 0.000000000000000000, 117.4749999999999943, -103.1875000000000000 ) ) ;
#513 = LINE ( 'NONE', #48640, #59500 ) ;
#516 = DIRECTION ( 'NONE',  ( 0.000000000000000000, -1.000000000000000000, 0.000000000000000000 ) ) ;
#517 = VECTOR ( 'NONE', #25289, 1000.000000000000000 ) ;
#518 = CARTESIAN_POINT ( 'NONE',  ( 162.8595971212720031, -23.19206098994050436, -5.074374724088000832 ) ) ;
#519 = CARTESIAN_POINT ( 'NONE',  ( 97.33998274022617636, -37.75834089694784979, 122.4099109901959679 ) ) ;
#521 = ORIENTED_EDGE ( 'NONE', *, *, #75430, .F. ) ;
#520 = FACE_OUTER_BOUND ( 'NONE', #29437, .T. ) ;
#522 = CARTESIAN_POINT ( 'NONE',  ( 115.0380569359701326, -30.04493676975927485, 265.3813395616251682 ) ) ;
#523 = FACE_OUTER_BOUND ( 'NONE', #41384, .T. ) ;
#524 = FACE_OUTER_BOUND ( 'NONE', #14285, .T. ) ;
#525 = CARTESIAN_POINT ( 'NONE',  ( 114.6154092934512647, -77.76606036807542921, 250.2178068554179902 ) ) ;
#526 = LINE ( 'NONE', #77290, #28220 ) ;
#527 = CARTESIAN_POINT ( 'NONE',  ( 48.16670390244701139, -26.71338133339251542, -5.074374724088000832 ) ) ;
#528 = DIRECTION ( 'NONE',  ( 0.000000000000000000, 0.000000000000000000, 1.000000000000000000 ) ) ;
#529 = CARTESIAN_POINT ( 'NONE',  ( 108.1128363339379632, -46.45408497333518483, 202.6613395616259652 ) ) ;
#530 = ORIENTED_EDGE ( 'NONE', *, *, #45775, .T. ) ;
#531 = EDGE_LOOP ( 'NONE', ( #19739, #23308, #31403, #15444, #2300 ) ) ;
#532 = CARTESIAN_POINT ( 'NONE',  ( 113.1755435565086998, -43.14875213554007161, 154.6130118773249649 ) ) ;
#533 = EDGE_CURVE ( 'NONE', #28842, #89511, #38792, .T. ) ;
#534 = AXIS2_PLACEMENT_3D ( 'NONE', #54365, #54819, #13078 ) ;
#535 = CARTESIAN_POINT ( 'NONE',  ( 31.89136050872263439, -31.76306994223845948, 237.4678068554150059 ) ) ;
#536 = CARTESIAN_POINT ( 'NONE',  ( 98.24278011039416469, -41.58876472015902692, 23.15872616303999010 ) ) ;
#537 = AXIS2_PLACEMENT_3D ( 'NONE', #14393, #82553, #62968 ) ;
#538 = CARTESIAN_POINT ( 'NONE',  ( 69.26949937496598864, -71.54137415153812185, 361.9756252759101471 ) ) ;
#539 = DIRECTION ( 'NONE',  ( 1.000000000000000078E-15, 1.000000000000000083E-30, -1.000000000000000000 ) ) ;
#540 = DIRECTION ( 'NONE',  ( -1.000000000000000000, 0.000000000000000000, 0.000000000000000000 ) ) ;
#541 = AXIS2_PLACEMENT_3D ( 'NONE', #19415, #46652, #5344 ) ;
#542 = CARTESIAN_POINT ( 'NONE',  ( 193.0371591254572934, -23.42818131005411786, 237.4678068554150059 ) ) ;
#543 = CYLINDRICAL_SURFACE ( 'NONE', #74912, 9.999999999999998224 ) ;
#544 = CARTESIAN_POINT ( 'NONE',  ( 115.4997179687694882, -29.61999039777954579, 224.3718157521009573 ) ) ;
#545 = CARTESIAN_POINT ( 'NONE',  ( 0.4111459596590908983, 95.14999999999999147, 118.3559999999999945 ) ) ;
#546 = ORIENTED_EDGE ( 'NONE', *, *, #43939, .F. ) ;
#547 = ORIENTED_EDGE ( 'NONE', *, *, #56743, .F. ) ;
#548 = CARTESIAN_POINT ( 'NONE',  ( 98.30753417703368768, -41.72887546760895106, 86.73979194043660357 ) ) ;
#549 = CARTESIAN_POINT ( 'NONE',  ( 82.81647637678409524, -18.77596264856125430, 6.749779334551668342 ) ) ;
#550 = CARTESIAN_POINT ( 'NONE',  ( 113.1793785465512201, -44.75106650107741046, 124.0924085711809965 ) ) ;
#551 = CARTESIAN_POINT ( 'NONE',  ( 25.56670390244797275, -67.87844715994100397, 262.0928068554150059 ) ) ;
#552 = CARTESIAN_POINT ( 'NONE',  ( 11.93654059743609963, 78.49423263675578255, 117.7526061616926398 ) ) ;
#553 = ORIENTED_EDGE ( 'NONE', *, *, #37978, .T. ) ;
#554 = FACE_OUTER_BOUND ( 'NONE', #32275, .T. ) ;
#555 = CARTESIAN_POINT ( 'NONE',  ( 118.1077515449285613, -36.21032982800684152, 268.8518157521015723 ) ) ;
#557 = EDGE_LOOP ( 'NONE', ( #41449, #70059, #56330, #26549 ) ) ;
#556 = EDGE_CURVE ( 'NONE', #40009, #71950, #88711, .T. ) ;
#558 = EDGE_CURVE ( 'NONE', #50481, #68206, #62341, .T. ) ;
#559 = CARTESIAN_POINT ( 'NONE',  ( 107.0664832912739968, -36.72944715994100306, 287.6356252759109680 ) ) ;
#560 = FACE_BOUND ( 'NONE', #57673, .T. ) ;
#561 = ADVANCED_FACE ( 'NONE', ( #55484, #43213 ), #64129, .F. ) ;
#562 = PLANE ( 'NONE',  #46520 ) ;
#563 = CARTESIAN_POINT ( 'NONE',  ( 107.1962421797556289, -28.07588791089852265, 77.89475703625792846 ) ) ;
#564 = CARTESIAN_POINT ( 'NONE',  ( 113.5786777234211939, -44.94349119991360197, 164.1099109901969655 ) ) ;
#565 = LINE ( 'NONE', #61440, #85629 ) ;
#566 = EDGE_LOOP ( 'NONE', ( #67679, #88603, #1718, #53923 ) ) ;
#567 = EDGE_CURVE ( 'NONE', #27001, #32371, #2511, .T. ) ;
#568 = DIRECTION ( 'NONE',  ( 4.237773401492740281E-14, -1.000000000000000000, 0.000000000000000000 ) ) ;
#569 = EDGE_LOOP ( 'NONE', ( #65281, #35010, #45549, #63195, #36234, #78377 ) ) ;
#570 = ORIENTED_EDGE ( 'NONE', *, *, #83826, .F. ) ;
#571 = VECTOR ( 'NONE', #71127, 1000.000000000000000 ) ;
#572 = CARTESIAN_POINT ( 'NONE',  ( -187.8075999999999794, 20.32000000000000028, -12.69999999999999929 ) ) ;
#573 = ORIENTED_EDGE ( 'NONE', *, *, #24287, .F. ) ;
#574 = ORIENTED_EDGE ( 'NONE', *, *, #33050, .F. ) ;
#575 = CARTESIAN_POINT ( 'NONE',  ( -7.941868552260229762E-13, 127.0000000000000000, 107.7702177616926065 ) ) ;
#576 = AXIS2_PLACEMENT_3D ( 'NONE', #61805, #46, #41357 ) ;
#577 = CARTESIAN_POINT ( 'NONE',  ( 106.9471680199217332, -25.26948335760882713, 320.5674069059367639 ) ) ;
#578 = EDGE_CURVE ( 'NONE', #82390, #82238, #27804, .T. ) ;
#579 = CARTESIAN_POINT ( 'NONE',  ( 113.7032067727884197, -42.10625226631949403, 87.70670554236198768 ) ) ;
#580 = CARTESIAN_POINT ( 'NONE',  ( 106.8511556536399780, -47.80415145147887301, 227.5489586092439538 ) ) ;
#581 = CARTESIAN_POINT ( 'NONE',  ( 103.3114313307233658, -27.02747569519249993, 215.3699109901969848 ) ) ;
#582 = CARTESIAN_POINT ( 'NONE',  ( 112.1705331031350283, -27.62378402076942763, 30.66991099019694644 ) ) ;
#583 = CARTESIAN_POINT ( 'NONE',  ( 41.56648329127399677, 0.2215528400590013880, 76.80862527591200717 ) ) ;
#584 = CARTESIAN_POINT ( 'NONE',  ( 60.32499999999999574, 82.54999999999999716, 358.0130000000000337 ) ) ;
#585 = EDGE_LOOP ( 'NONE', ( #73914, #36571, #16667, #18856, #51645, #20721, #25049, #39551, #67761, #8021, #890, #9072, #69488, #83607, #32589, #87543 ) ) ;
#586 = DIRECTION ( 'NONE',  ( -0.8660254037844381525, 0.000000000000000000, -0.5000000000000007772 ) ) ;
#587 = CARTESIAN_POINT ( 'NONE',  ( 96.67439905703392355, -92.77844715994214653, -21.78219314458237932 ) ) ;
#588 = CARTESIAN_POINT ( 'NONE',  ( 70.69106258991376990, -139.4536831229399070, 247.3802696298695594 ) ) ;
#589 = CARTESIAN_POINT ( 'NONE',  ( 96.20363159075253634, -34.36081134307595164, 106.1556252759109640 ) ) ;
#590 = CARTESIAN_POINT ( 'NONE',  ( 101.6881215347969345, -27.70586588967184483, 85.50419670448295051 ) ) ;
#592 = VECTOR ( 'NONE', #33740, 1000.000000000000000 ) ;
#591 = CARTESIAN_POINT ( 'NONE',  ( 106.8354617269136497, -47.19621815579884583, 272.5584824187680510 ) ) ;
#593 = VERTEX_POINT ( 'NONE', #57292 ) ;
#594 = UNCERTAINTY_MEASURE_WITH_UNIT (LENGTH_MEASURE( 1.000000000000000082E-05 ), #15036, 'distance_accuracy_value', 'NONE');
#595 = CARTESIAN_POINT ( 'NONE',  ( 101.6505379212622699, -45.63756515480785225, 247.1413395616249602 ) ) ;
#596 = DIRECTION ( 'NONE',  ( 0.000000000000000000, 0.000000000000000000, 1.000000000000000000 ) ) ;
#597 = VECTOR ( 'NONE', #60325, 1000.000000000000000 ) ;
#599 = CARTESIAN_POINT ( 'NONE',  ( 11.42157353567683842, 76.98139724742750900, 130.0556313956597592 ) ) ;
#598 = VECTOR ( 'NONE', #63493, 1000.000000000000114 ) ;
#600 = CARTESIAN_POINT ( 'NONE',  ( 49.16670390244654243, -28.27351298637376686, 193.9678068554150911 ) ) ;
#602 = CARTESIAN_POINT ( 'NONE',  ( 68.69590989347372556, -139.3001951612658900, 245.8075977448462197 ) ) ;
#601 = DIRECTION ( 'NONE',  ( 0.000000000000000000, 0.000000000000000000, 1.000000000000000000 ) ) ;
#603 = DIRECTION ( 'NONE',  ( 1.000000000000000078E-15, -1.000000000000000083E-30, -1.000000000000000000 ) ) ;
#604 = DIRECTION ( 'NONE',  ( -0.6757246285173468259, -5.929722281754665310E-16, 0.7371541402007408816 ) ) ;
#605 = FACE_OUTER_BOUND ( 'NONE', #87469, .T. ) ;
#606 = VECTOR ( 'NONE', #21628, 1000.000000000000000 ) ;
#607 = CARTESIAN_POINT ( 'NONE',  ( -7.746062721843856025, 92.64813751154241572, 130.3278237768880672 ) ) ;
#608 = LINE ( 'NONE', #29227, #58991 ) ;
#609 = FACE_OUTER_BOUND ( 'NONE', #72490, .T. ) ;
#611 = VERTEX_POINT ( 'NONE', #50480 ) ;
#610 = CARTESIAN_POINT ( 'NONE',  ( 98.34985889676497095, -31.65658483615705521, 260.9064586116816145 ) ) ;
#612 = CARTESIAN_POINT ( 'NONE',  ( 103.2512128930084288, -131.5792096921222480, 250.2178068554180470 ) ) ;
#613 = CARTESIAN_POINT ( 'NONE',  ( 96.99510461011969653, -33.95209312647379818, 251.1127681330538337 ) ) ;
#614 = CARTESIAN_POINT ( 'NONE',  ( 99.10138041440774259, -45.50374834597938900, 152.9899109901969894 ) ) ;
#615 = CARTESIAN_POINT ( 'NONE',  ( 101.3723308891022157, -27.97080072976544685, 21.53562527591096298 ) ) ;
#616 = LINE ( 'NONE', #21531, #83843 ) ;
#619 = EDGE_CURVE ( 'NONE', #6607, #89473, #22352, .T. ) ;
#618 = CARTESIAN_POINT ( 'NONE',  ( 82.31780288914308130, -35.14744377621693161, 7.339349742403836530 ) ) ;
#617 = DIRECTION ( 'NONE',  ( 0.000000000000000000, 0.000000000000000000, -1.000000000000000000 ) ) ;
#620 = CARTESIAN_POINT ( 'NONE',  ( 116.3231543710223121, -32.93883412237410369, 190.1356252759109680 ) ) ;
#621 = CARTESIAN_POINT ( 'NONE',  ( 129.9528072873947053, 84.62817240485476589, 12.53569626682358695 ) ) ;
#622 = EDGE_CURVE ( 'NONE', #11051, #83707, #61099, .T. ) ;
#623 = VERTEX_POINT ( 'NONE', #20999 ) ;
#624 = DIRECTION ( 'NONE',  ( -3.100000000000000258E-29, 3.100000000000000044E-14, 1.000000000000000000 ) ) ;
#625 = EDGE_LOOP ( 'NONE', ( #85460, #52936 ) ) ;
#626 = CARTESIAN_POINT ( 'NONE',  ( 102.7266122873206768, -44.08618886718738139, 161.5752769709339702 ) ) ;
#628 = VERTEX_POINT ( 'NONE', #14642 ) ;
#627 = CARTESIAN_POINT ( 'NONE',  ( 193.5667039024483529, -48.82844715993410034, 300.4678068554149490 ) ) ;
#629 = CARTESIAN_POINT ( 'NONE',  ( -462.0260000000000105, 53.97500000000000142, -3.174999999999999822 ) ) ;
#630 = CARTESIAN_POINT ( 'NONE',  ( 116.9962961068553113, -33.62662860631130712, 170.0670538473399631 ) ) ;
#631 = CARTESIAN_POINT ( 'NONE',  ( 162.7131505118551047, -33.70561438051486647, 313.9678068554149490 ) ) ;
#632 = DIRECTION ( 'NONE',  ( 0.000000000000000000, -1.000000000000000000, 0.000000000000000000 ) ) ;
#633 = CARTESIAN_POINT ( 'NONE',  ( 111.4434818239271436, -27.72135023051140834, 85.71645798515046977 ) ) ;
#634 = CARTESIAN_POINT ( 'NONE',  ( -80.88709205069390862, 70.52090377575432001, 86.67734222162562219 ) ) ;
#635 = DIRECTION ( 'NONE',  ( 1.000000000000000000, 0.000000000000000000, 0.000000000000000000 ) ) ;
#636 = CARTESIAN_POINT ( 'NONE',  ( 112.1775644307544013, -28.39036538331624726, 94.63848241876893042 ) ) ;
#637 = ORIENTED_EDGE ( 'NONE', *, *, #20066, .T. ) ;
#638 = VERTEX_POINT ( 'NONE', #15986 ) ;
#639 = ORIENTED_EDGE ( 'NONE', *, *, #3250, .F. ) ;
#640 = VECTOR ( 'NONE', #25417, 1000.000000000000000 ) ;
#641 = CARTESIAN_POINT ( 'NONE',  ( 115.2933828064165311, -33.43605939358163681, 50.56158330589693861 ) ) ;
#642 = EDGE_CURVE ( 'NONE', #45558, #61357, #53228, .T. ) ;
#643 = CARTESIAN_POINT ( 'NONE',  ( 27.27158787008327678, 184.0000000000000000, 80.02307622376218887 ) ) ;
#645 = FACE_OUTER_BOUND ( 'NONE', #52755, .T. ) ;
#644 = CARTESIAN_POINT ( 'NONE',  ( 107.5349099188610893, -47.08895302312297559, 188.6003871806719587 ) ) ;
#646 = CIRCLE ( 'NONE', #12254, 3.000000000000002665 ) ;
#647 = DIRECTION ( 'NONE',  ( -1.000000000000000000, 0.000000000000000000, 0.000000000000000000 ) ) ;
#648 = DIRECTION ( 'NONE',  ( 3.999999999999999995E-14, -1.000000000000000000, 4.100000000000000342E-29 ) ) ;
#649 = DIRECTION ( 'NONE',  ( -2.900000000000000265E-14, 2.000000000000000155E-15, -1.000000000000000000 ) ) ;
#650 = CARTESIAN_POINT ( 'NONE',  ( 54.06670390244700997, -79.67844715994098692, 222.2178068554179902 ) ) ;
#651 = CARTESIAN_POINT ( 'NONE',  ( 67.18382773639109473, -67.99014260483819783, 246.1660416551738990 ) ) ;
#652 = CARTESIAN_POINT ( 'NONE',  ( 114.0075736764523100, -28.98025818340840942, 114.4956252759109816 ) ) ;
#653 = ORIENTED_EDGE ( 'NONE', *, *, #73659, .T. ) ;
#654 = ORIENTED_EDGE ( 'NONE', *, *, #48753, .F. ) ;
#655 = ORIENTED_EDGE ( 'NONE', *, *, #13603, .F. ) ;
#656 = LINE ( 'NONE', #28362, #8199 ) ;
#657 = CARTESIAN_POINT ( 'NONE',  ( -97.63858630140161665, 92.64237678566784950, -86.67213519546656642 ) ) ;
#658 = CARTESIAN_POINT ( 'NONE',  ( 102.0659489093014685, -27.97114065885338263, 130.4898948659551365 ) ) ;
#659 = DIRECTION ( 'NONE',  ( 1.000000000000000000, 3.930900487435134677E-14, 0.000000000000000000 ) ) ;
#660 = CARTESIAN_POINT ( 'NONE',  ( 112.1932604131138760, -43.70204218538222563, 180.8871379886389832 ) ) ;
#661 = AXIS2_PLACEMENT_3D ( 'NONE', #79117, #10504, #25470 ) ;
#662 = VECTOR ( 'NONE', #54108, 1000.000000000000000 ) ;
#663 = DIRECTION ( 'NONE',  ( -0.8660254037844382635, -0.5000000000000008882, 1.550000000000000022E-14 ) ) ;
#664 = VECTOR ( 'NONE', #62185, 1000.000000000000000 ) ;
#665 = AXIS2_PLACEMENT_3D ( 'NONE', #8895, #11561, #17475 ) ;
#666 = CARTESIAN_POINT ( 'NONE',  ( 83.06670390244796920, -61.87844715994100397, 204.3338068554149913 ) ) ;
#667 = VERTEX_POINT ( 'NONE', #62769 ) ;
#669 = ORIENTED_EDGE ( 'NONE', *, *, #45253, .F. ) ;
#668 = ORIENTED_EDGE ( 'NONE', *, *, #40170, .F. ) ;
#670 = VECTOR ( 'NONE', #88324, 1000.000000000000000 ) ;
#671 = CIRCLE ( 'NONE', #54333, 1.000000000000000888 ) ;
#672 = DIRECTION ( 'NONE',  ( 3.100000000000000258E-29, -3.100000000000000044E-14, -1.000000000000000000 ) ) ;
#673 = ORIENTED_EDGE ( 'NONE', *, *, #65969, .T. ) ;
#674 = EDGE_LOOP ( 'NONE', ( #44663, #41328, #16227, #43214 ) ) ;
#675 = LINE ( 'NONE', #22483, #55023 ) ;
#676 = EDGE_CURVE ( 'NONE', #8470, #22374, #75390, .T. ) ;
#677 = CARTESIAN_POINT ( 'NONE',  ( 104.8088860400571463, -27.60915219823615985, 236.6892023535159808 ) ) ;
#678 = CARTESIAN_POINT ( 'NONE',  ( 72.96458098368650269, 127.0000000000000000, 65.02708098368729850 ) ) ;
#679 = ORIENTED_EDGE ( 'NONE', *, *, #28156, .T. ) ;
#680 = CYLINDRICAL_SURFACE ( 'NONE', #60979, 2.750000000000002665 ) ;
#681 = CARTESIAN_POINT ( 'NONE',  ( -114.0590328520549832, 70.22562679785821160, 63.52550556333007137 ) ) ;
#682 = ORIENTED_EDGE ( 'NONE', *, *, #19511, .F. ) ;
#683 = ORIENTED_EDGE ( 'NONE', *, *, #39535, .T. ) ;
#684 = CARTESIAN_POINT ( 'NONE',  ( -127.5252020268932114, 20.32000000000000028, 177.0380000000000109 ) ) ;
#685 = EDGE_LOOP ( 'NONE', ( #78794, #39701 ) ) ;
#686 = VERTEX_POINT ( 'NONE', #72289 ) ;
#687 = VECTOR ( 'NONE', #72878, 1000.000000000000000 ) ;
#688 = ADVANCED_FACE ( 'NONE', ( #31376, #44999, #10057 ), #30499, .F. ) ;
#689 = CARTESIAN_POINT ( 'NONE',  ( 106.1481202089414637, -44.86820639808929201, 280.3052332267342877 ) ) ;
#690 = CARTESIAN_POINT ( 'NONE',  ( 102.3026241189005532, -26.72939285866361914, 140.4422919425769578 ) ) ;
#691 = CARTESIAN_POINT ( 'NONE',  ( 98.47671751366513604, -30.86049585540210671, 120.8499109901969604 ) ) ;
#692 = CARTESIAN_POINT ( 'NONE',  ( 97.81168895331838087, -40.51742574516882200, 287.6356252759109680 ) ) ;
#693 = ADVANCED_FACE ( 'NONE', ( #58200 ), #71402, .F. ) ;
#694 = DIRECTION ( 'NONE',  ( -0.8660254037844392627, 0.4999999999999990008, -1.549999999999999706E-14 ) ) ;
#695 = CARTESIAN_POINT ( 'NONE',  ( 109.9601702690906677, -48.22123515106449787, 238.7727681330539724 ) ) ;
#696 = FACE_OUTER_BOUND ( 'NONE', #29082, .T. ) ;
#697 = CARTESIAN_POINT ( 'NONE',  ( 142.8698897858160706, -0.9167816978817300289, 542.9756252759101471 ) ) ;
#698 = ORIENTED_EDGE ( 'NONE', *, *, #71843, .F. ) ;
#699 = DIRECTION ( 'NONE',  ( -1.000000000000000000, -4.299999999999999979E-14, -1.000000000000000078E-15 ) ) ;
#700 = ORIENTED_EDGE ( 'NONE', *, *, #62620, .T. ) ;
#701 = VERTEX_POINT ( 'NONE', #9167 ) ;
#702 = DIRECTION ( 'NONE',  ( 0.000000000000000000, -1.000000000000000000, 2.048885995248199879E-16 ) ) ;
#703 = AXIS2_PLACEMENT_3D ( 'NONE', #37504, #57493, #58381 ) ;
#704 = CARTESIAN_POINT ( 'NONE',  ( 115.7771187221315898, -31.78005509801509021, 135.2375939364552266 ) ) ;
#705 = ORIENTED_EDGE ( 'NONE', *, *, #10479, .F. ) ;
#706 = CARTESIAN_POINT ( 'NONE',  ( 98.45613130301506999, -42.66979608177781813, 126.8070538473389490 ) ) ;
#707 = CARTESIAN_POINT ( 'NONE',  ( 120.6562317954107328, -37.89495061977655155, 302.6356252759109680 ) ) ;
#708 = AXIS2_PLACEMENT_3D ( 'NONE', #61591, #89328, #88881 ) ;
#709 = FACE_OUTER_BOUND ( 'NONE', #24326, .T. ) ;
#710 = DIRECTION ( 'NONE',  ( 0.000000000000000000, -1.000000000000000000, 0.000000000000000000 ) ) ;
#713 = CARTESIAN_POINT ( 'NONE',  ( 100.8363305107023820, -45.83159080358277748, 238.1108633711489517 ) ) ;
#712 = CARTESIAN_POINT ( 'NONE',  ( 102.0553424010809351, -45.40300992569917327, 57.15924359062986326 ) ) ;
#711 = CARTESIAN_POINT ( 'NONE',  ( 103.1875000000000000, 127.0000000000000000, -7.937499999999639400 ) ) ;
#714 = PLANE ( 'NONE',  #87235 ) ;
#715 = DIRECTION ( 'NONE',  ( 1.000000000000000078E-15, -1.000000000000000083E-30, -1.000000000000000000 ) ) ;
#716 = ORIENTED_EDGE ( 'NONE', *, *, #77579, .T. ) ;
#717 = CARTESIAN_POINT ( 'NONE',  ( 103.1875000000000000, 117.4749999999999943, 7.937500000000360600 ) ) ;
#718 = FACE_OUTER_BOUND ( 'NONE', #75674, .T. ) ;
#719 = CARTESIAN_POINT ( 'NONE',  ( 107.5667039024470455, -113.7784471599413791, 2.217806855418308132 ) ) ;
#720 = CARTESIAN_POINT ( 'NONE',  ( 146.8610933598213251, -137.5366814833658395, 246.4167843500817412 ) ) ;
#722 = EDGE_LOOP ( 'NONE', ( #23623, #15028, #2356, #87724 ) ) ;
#721 = CARTESIAN_POINT ( 'NONE',  ( 172.5664832912740110, 0.2215528400590013880, 318.9256252759120116 ) ) ;
#723 = CARTESIAN_POINT ( 'NONE',  ( 0.000000000000000000, 101.5999999999999943, 0.000000000000000000 ) ) ;
#724 = CARTESIAN_POINT ( 'NONE',  ( 101.9611696646907433, -46.55956485693801028, 167.1832443235299763 ) ) ;
#725 = CARTESIAN_POINT ( 'NONE',  ( 115.7285985590555129, -43.59543139906921283, 44.30514908543492680 ) ) ;
#726 = CARTESIAN_POINT ( 'NONE',  ( 109.8676264040644526, -26.64249633179236909, 170.8613395616249591 ) ) ;
#727 = CARTESIAN_POINT ( 'NONE',  ( 97.33784125381592389, -34.07106473404611080, 32.11479195932787434 ) ) ;
#728 = DIRECTION ( 'NONE',  ( 1.000000000000000000, 0.000000000000000000, 9.462128050782575008E-16 ) ) ;
#730 = CARTESIAN_POINT ( 'NONE',  ( 0.000000000000000000, 0.000000000000000000, 0.000000000000000000 ) ) ;
#729 = CARTESIAN_POINT ( 'NONE',  ( -13.86911000615384104, 238.5000000000000000, 102.9892450244911828 ) ) ;
#731 = DIRECTION ( 'NONE',  ( -0.000000000000000000, -0.000000000000000000, 1.000000000000000000 ) ) ;
#732 = DIRECTION ( 'NONE',  ( 0.000000000000000000, 0.000000000000000000, 1.000000000000000000 ) ) ;
#733 = VERTEX_POINT ( 'NONE', #85930 ) ;
#734 = CARTESIAN_POINT ( 'NONE',  ( 107.0667039024470313, -104.2784471599418197, -11.78219314458200984 ) ) ;
#735 = CIRCLE ( 'NONE', #25428, 2.117000000000000881 ) ;
#736 = VECTOR ( 'NONE', #34922, 1000.000000000000000 ) ;
#737 = AXIS2_PLACEMENT_3D ( 'NONE', #66551, #4341, #52876 ) ;
#738 = AXIS2_PLACEMENT_3D ( 'NONE', #72305, #37331, #64151 ) ;
#739 = EDGE_CURVE ( 'NONE', #86672, #54266, #21377, .T. ) ;
#740 = ORIENTED_EDGE ( 'NONE', *, *, #36493, .T. ) ;
#741 = ORIENTED_EDGE ( 'NONE', *, *, #80273, .F. ) ;
#742 = VECTOR ( 'NONE', #7772, 1000.000000000000000 ) ;
#743 = CIRCLE ( 'NONE', #67453, 0.5000000000000004441 ) ;
#745 = ORIENTED_EDGE ( 'NONE', *, *, #84172, .F. ) ;
#744 = DIRECTION ( 'NONE',  ( 0.000000000000000000, -1.000000000000000000, 0.000000000000000000 ) ) ;
#746 = CARTESIAN_POINT ( 'NONE',  ( 112.7479404651553949, -27.97242311821442584, 65.61848241876793963 ) ) ;
#747 = DIRECTION ( 'NONE',  ( -0.9068632946707808618, 0.4214249218767877059, 0.000000000000000000 ) ) ;
#748 = CARTESIAN_POINT ( 'NONE',  ( 165.6738106836045006, -28.98061976758433289, 237.4678068554150059 ) ) ;
#749 = CARTESIAN_POINT ( 'NONE',  ( 113.7785824165150643, -44.76317014998476651, 189.1299109901969757 ) ) ;
#751 = CARTESIAN_POINT ( 'NONE',  ( 97.36980136507975203, -37.22440909395530184, 270.7895626852197779 ) ) ;
#750 = AXIS2_PLACEMENT_3D ( 'NONE', #24215, #59157, #1983 ) ;
#752 = VERTEX_POINT ( 'NONE', #65897 ) ;
#753 = VERTEX_POINT ( 'NONE', #23701 ) ;
#754 = ORIENTED_EDGE ( 'NONE', *, *, #13256, .T. ) ;
#755 = ADVANCED_FACE ( 'NONE', ( #10935 ), #56167, .T. ) ;
#756 = ORIENTED_EDGE ( 'NONE', *, *, #83309, .F. ) ;
#757 = DIRECTION ( 'NONE',  ( -2.999999999999999839E-15, 1.000000000000000000, -2.999999999999999900E-30 ) ) ;
#758 = DIRECTION ( 'NONE',  ( -4.237773401492740281E-14, 1.000000000000000000, 0.000000000000000000 ) ) ;
#759 = CARTESIAN_POINT ( 'NONE',  ( 97.31585577103271589, -39.30600539877234922, 162.5314611377484084 ) ) ;
#760 = CARTESIAN_POINT ( 'NONE',  ( 112.1393456390005952, -28.01282277954388888, 74.65645860948981749 ) ) ;
#761 = VECTOR ( 'NONE', #1970, 1000.000000000000000 ) ;
#762 = CARTESIAN_POINT ( 'NONE',  ( 85.30153658290296903, 90.93932679090998761, 98.83759631548571178 ) ) ;
#763 = CYLINDRICAL_SURFACE ( 'NONE', #81462, 13.16666666666669627 ) ;
#764 = EDGE_CURVE ( 'NONE', #26493, #14667, #50932, .T. ) ;
#765 = CYLINDRICAL_SURFACE ( 'NONE', #44229, 34.13125000000000142 ) ;
#766 = CARTESIAN_POINT ( 'NONE',  ( -11.74378193249606106, 87.38464304823123996, 130.0267385514075329 ) ) ;
#767 = CARTESIAN_POINT ( 'NONE',  ( 96.71096103112829212, -32.93116260832594122, 21.03467289495897319 ) ) ;
#768 = CARTESIAN_POINT ( 'NONE',  ( -41.60202597009397607, 76.06518036156089124, 54.55338361873603503 ) ) ;
#769 = EDGE_CURVE ( 'NONE', #62133, #32868, #1079, .T. ) ;
#770 = VERTEX_POINT ( 'NONE', #57750 ) ;
#771 = EDGE_CURVE ( 'NONE', #74494, #28457, #8136, .T. ) ;
#772 = DIRECTION ( 'NONE',  ( 0.000000000000000000, 1.000000000000000000, 0.000000000000000000 ) ) ;
#773 = CARTESIAN_POINT ( 'NONE',  ( 41.56648329127398966, -18.82844715994071194, 258.9256252759120116 ) ) ;
#774 = CARTESIAN_POINT ( 'NONE',  ( 100.6392880577574687, -41.80624237711439406, 89.67666179816296790 ) ) ;
#775 = ADVANCED_FACE ( 'NONE', ( #86365 ), #65018, .T. ) ;
#776 = B_SPLINE_CURVE_WITH_KNOTS ( 'NONE', 3,
 ( #76928, #55545, #48739, #1068, #42379, #61936, #14706, #7433, #21978, #76474, #29230, #13800, #610, #13359, #49645, #42826, #76023, #34679 ),
 .UNSPECIFIED., .F., .F.,
 ( 4, 2, 2, 2, 2, 2, 2, 2, 4 ),
 ( 0.000000000000000000, 0.06250000008602163426, 0.1250000001720432685, 0.1875000002580649028, 0.2500000003440865370, 0.3125000004301081713, 0.3750000005161298056, 0.4375000006021514398, 0.5000000006881730741 ),
 .UNSPECIFIED. ) ;
#777 = AXIS2_PLACEMENT_3D ( 'NONE', #25052, #40017, #47268 ) ;
#778 = VECTOR ( 'NONE', #6983, 1000.000000000000000 ) ;
#779 = EDGE_CURVE ( 'NONE', #44762, #23939, #63516, .T. ) ;
#780 = DIRECTION ( 'NONE',  ( -1.000000000000000000, 0.000000000000000000, 0.000000000000000000 ) ) ;
#781 = CARTESIAN_POINT ( 'NONE',  ( 116.3212776292271258, -32.94146857470711609, 44.13562527591097506 ) ) ;
#782 = ORIENTED_EDGE ( 'NONE', *, *, #58682, .T. ) ;
#783 = VERTEX_POINT ( 'NONE', #55463 ) ;
#784 = DIRECTION ( 'NONE',  ( 1.000000000000000000, -1.000000000000000078E-15, 0.000000000000000000 ) ) ;
#785 = ORIENTED_EDGE ( 'NONE', *, *, #8187, .F. ) ;
#786 = ORIENTED_EDGE ( 'NONE', *, *, #30299, .T. ) ;
#787 = ADVANCED_FACE ( 'NONE', ( #7793 ), #6449, .F. ) ;
#788 = CARTESIAN_POINT ( 'NONE',  ( 104.0080147226004925, -45.04654038386073012, 138.7272975916119435 ) ) ;
#789 = CARTESIAN_POINT ( 'NONE',  ( 1.145694247088684285E-22, 95.25000000000000000, 118.5560000000000116 ) ) ;
#790 = CARTESIAN_POINT ( 'NONE',  ( 117.8979321085648877, -39.04567734339117635, 104.6708633711489824 ) ) ;
#791 = DIRECTION ( 'NONE',  ( -0.7071067811865779928, 0.7071067811865171526, -7.071067811865785947E-16 ) ) ;
#792 = EDGE_LOOP ( 'NONE', ( #87956, #8143, #70608, #66324, #45131 ) ) ;
#793 = AXIS2_PLACEMENT_3D ( 'NONE', #52763, #58282, #86014 ) ;
#794 = VECTOR ( 'NONE', #12046, 1000.000000000000000 ) ;
#795 = TOROIDAL_SURFACE ( 'NONE', #87816, 11.75000000000000000, 2.125000000000000000 ) ;
#796 = ORIENTED_EDGE ( 'NONE', *, *, #68724, .F. ) ;
#797 = ORIENTED_EDGE ( 'NONE', *, *, #47110, .F. ) ;
#798 = CIRCLE ( 'NONE', #70252, 3.000000000000002665 ) ;
#799 = EDGE_CURVE ( 'NONE', #65439, #55059, #50406, .T. ) ;
#800 = FACE_OUTER_BOUND ( 'NONE', #89670, .T. ) ;
#801 = ORIENTED_EDGE ( 'NONE', *, *, #59322, .T. ) ;
#802 = CARTESIAN_POINT ( 'NONE',  ( 97.51798386322114709, -31.03399775848789233, 280.8984824187687082 ) ) ;
#803 = CARTESIAN_POINT ( 'NONE',  ( 106.9748050991984059, -47.17592283179411083, 183.5699109901969734 ) ) ;
#804 = EDGE_CURVE ( 'NONE', #2492, #78417, #79484, .T. ) ;
#805 = FACE_OUTER_BOUND ( 'NONE', #29803, .T. ) ;
#806 = CARTESIAN_POINT ( 'NONE',  ( 101.9928297044944543, -45.44558343088166907, 128.1563855231297850 ) ) ;
#807 = CARTESIAN_POINT ( 'NONE',  ( 113.8434436840914117, -28.76112614263219669, 135.5156252759109634 ) ) ;
#809 = EDGE_CURVE ( 'NONE', #84681, #23299, #69575, .T. ) ;
#808 = CYLINDRICAL_SURFACE ( 'NONE', #21880, 9.999999999999998224 ) ;
#810 = VERTEX_POINT ( 'NONE', #35943 ) ;
#811 = AXIS2_PLACEMENT_3D ( 'NONE', #82943, #28399, #22065 ) ;
#812 = CARTESIAN_POINT ( 'NONE',  ( 144.8664832912740223, -71.52944715994085811, 394.9756252759100903 ) ) ;
#813 = EDGE_CURVE ( 'NONE', #65108, #77202, #82778, .T. ) ;
#814 = DIRECTION ( 'NONE',  ( 0.000000000000000000, 0.000000000000000000, 1.000000000000000000 ) ) ;
#815 = AXIS2_PLACEMENT_3D ( 'NONE', #55356, #35825, #83549 ) ;
#816 = ORIENTED_EDGE ( 'NONE', *, *, #29499, .T. ) ;
#817 = DIRECTION ( 'NONE',  ( -3.100000000000000258E-29, 3.100000000000000044E-14, 1.000000000000000000 ) ) ;
#818 = CARTESIAN_POINT ( 'NONE',  ( 0.8322866307615671699, 95.14999999999997726, 118.5559999999999832 ) ) ;
#819 = CARTESIAN_POINT ( 'NONE',  ( 99.76197604230684135, -44.21744263965017296, 21.96133956162593748 ) ) ;
#820 = CARTESIAN_POINT ( 'NONE',  ( 23.04101804865160119, 56.72370184857491182, 30.34351131950213798 ) ) ;
#821 = CIRCLE ( 'NONE', #18255, 0.4999999999999976685 ) ;
#822 = PLANE ( 'NONE',  #31862 ) ;
#823 = CARTESIAN_POINT ( 'NONE',  ( 105.7154773393596372, -46.72385839336168090, 73.46895860995762462 ) ) ;
#824 = CARTESIAN_POINT ( 'NONE',  ( 104.7983354006062058, -46.84845355260645761, 27.38895860924495196 ) ) ;
#826 = CARTESIAN_POINT ( 'NONE',  ( 117.5859182825551983, -33.41202194707546624, 125.0575300378149706 ) ) ;
#825 = CARTESIAN_POINT ( 'NONE',  ( 97.53201903585136279, -39.74950769135491413, 111.5705769356003287 ) ) ;
#827 = FACE_OUTER_BOUND ( 'NONE', #18181, .T. ) ;
#828 = CARTESIAN_POINT ( 'NONE',  ( 172.5664832912740110, -9.303447159940999356, 201.0426252759120018 ) ) ;
#829 = VERTEX_POINT ( 'NONE', #27783 ) ;
#830 = CYLINDRICAL_SURFACE ( 'NONE', #17828, 3.500000000000003109 ) ;
#831 = FACE_BOUND ( 'NONE', #32263, .T. ) ;
#832 = PLANE ( 'NONE',  #52859 ) ;
#833 = VECTOR ( 'NONE', #85571, 1000.000000000000000 ) ;
#834 = VERTEX_POINT ( 'NONE', #56373 ) ;
#835 = DIRECTION ( 'NONE',  ( -1.000000000000000000, -1.734723475976808672E-15, 0.000000000000000000 ) ) ;
#837 = VERTEX_POINT ( 'NONE', #15063 ) ;
#836 = CARTESIAN_POINT ( 'NONE',  ( 108.3716159000525039, -47.75258262280652843, 162.6822919425769669 ) ) ;
#838 = CARTESIAN_POINT ( 'NONE',  ( 41.56670390244688207, -36.32844715994109208, 193.9678068554150911 ) ) ;
#839 = CARTESIAN_POINT ( 'NONE',  ( 114.6212291911790402, -29.51397259194560263, 230.4327681330539690 ) ) ;
#840 = CARTESIAN_POINT ( 'NONE',  ( 99.26130681012091372, -43.75918647830361863, 52.90991099019698396 ) ) ;
#841 = CARTESIAN_POINT ( 'NONE',  ( 100.8594679592200833, 82.54999999999999716, 82.89895571708400723 ) ) ;
#842 = DIRECTION ( 'NONE',  ( -1.000000000000000000, -4.299999999999999979E-14, 1.230419385187874527E-43 ) ) ;
#843 = VECTOR ( 'NONE', #71770, 1000.000000000000000 ) ;
#844 = FACE_OUTER_BOUND ( 'NONE', #84054, .T. ) ;
#845 = ORIENTED_EDGE ( 'NONE', *, *, #49423, .F. ) ;
#846 = AXIS2_PLACEMENT_3D ( 'NONE', #32859, #19245, #80142 ) ;
#847 = EDGE_LOOP ( 'NONE', ( #47913, #48812, #20485, #2433, #41329, #27512, #86444, #59413, #54279, #89920 ) ) ;
#848 = ORIENTED_EDGE ( 'NONE', *, *, #1891, .F. ) ;
#849 = VERTEX_POINT ( 'NONE', #62748 ) ;
#850 = CARTESIAN_POINT ( 'NONE',  ( 41.56648329127499153, -27.82844715994070484, 83.67562527591201160 ) ) ;
#851 = CARTESIAN_POINT ( 'NONE',  ( 115.7761331719916171, -31.00018137778016936, 250.2899109901966028 ) ) ;
#852 = CARTESIAN_POINT ( 'NONE',  ( 33.91903122894440514, -35.91149509761246605, 193.9678068554150911 ) ) ;
#853 = CARTESIAN_POINT ( 'NONE',  ( 136.1684221027214790, -16.94667169169761678, 2.376609173410517695 ) ) ;
#855 = DIRECTION ( 'NONE',  ( -1.000000000000000000, 0.000000000000000000, 0.000000000000000000 ) ) ;
#854 = CARTESIAN_POINT ( 'NONE',  ( 125.0664851986225159, -56.72944715994101728, 14.92562527591098842 ) ) ;
#856 = DIRECTION ( 'NONE',  ( -7.723290606088049820E-15, 0.000000000000000000, -1.000000000000000000 ) ) ;
#857 = CARTESIAN_POINT ( 'NONE',  ( 109.6484814735558189, -46.85267042889636002, 47.77562527591094721 ) ) ;
#858 = ORIENTED_EDGE ( 'NONE', *, *, #68817, .T. ) ;
#859 = AXIS2_PLACEMENT_3D ( 'NONE', #84695, #41975, #69709 ) ;
#860 = ORIENTED_EDGE ( 'NONE', *, *, #37022, .F. ) ;
#861 = VECTOR ( 'NONE', #43079, 1000.000000000000000 ) ;
#862 = EDGE_CURVE ( 'NONE', #52251, #6347, #68681, .T. ) ;
#863 = DIRECTION ( 'NONE',  ( 1.000000000000000000, 4.237773401492740281E-14, 0.000000000000000000 ) ) ;
#864 = AXIS2_PLACEMENT_3D ( 'NONE', #1232, #17420, #79664 ) ;
#865 = CARTESIAN_POINT ( 'NONE',  ( 97.81483072311490901, -40.51614641965803543, 17.63529977666319937 ) ) ;
#866 = EDGE_CURVE ( 'NONE', #4589, #18695, #41839, .T. ) ;
#867 = CARTESIAN_POINT ( 'NONE',  ( 101.6507727546967743, -27.01955209951630010, 251.4813395616246510 ) ) ;
#868 = CARTESIAN_POINT ( 'NONE',  ( 193.0371591254586860, -47.82818131005411999, 117.4678068554150627 ) ) ;
#869 = ADVANCED_FACE ( 'NONE', ( #70025 ), #14620, .F. ) ;
#870 = CARTESIAN_POINT ( 'NONE',  ( 116.7039036015865037, -32.90075090702275418, 95.13943479971997874 ) ) ;
#871 = DIRECTION ( 'NONE',  ( 0.7071067811865461294, 0.000000000000000000, 0.7071067811865489050 ) ) ;
#872 = CARTESIAN_POINT ( 'NONE',  ( 103.2786946225953244, -27.47457500332495783, 21.38560984476657367 ) ) ;
#873 = EDGE_CURVE ( 'NONE', #43897, #27298, #82327, .T. ) ;
#874 = ORIENTED_EDGE ( 'NONE', *, *, #10631, .F. ) ;
#875 = PLANE ( 'NONE',  #44348 ) ;
#876 = ADVANCED_FACE ( 'NONE', ( #524 ), #35485, .F. ) ;
#877 = VERTEX_POINT ( 'NONE', #75499 ) ;
#878 = ORIENTED_EDGE ( 'NONE', *, *, #89050, .T. ) ;
#879 = VECTOR ( 'NONE', #87402, 1000.000000000000000 ) ;
#881 = B_SPLINE_CURVE_WITH_KNOTS ( 'NONE', 3,
 ( #17422, #9269, #64236, #16531, #16978, #85591, #23803, #2008, #36967, #71065, #72394, #50588, #2459, #10596, #51039, #38300, #44661, #57403, #43321, #8836, #71948, #85144, #37418, #22911, #51470 ),
 .UNSPECIFIED., .F., .F.,
 ( 4, 2, 2, 2, 2, 2, 2, 2, 2, 1, 2, 2, 4 ),
 ( 0.000000000000000000, 0.002464394434560686874, 0.003696591651841050694, 0.004928788869121414513, 0.007393183303682179450, 0.008625380520962545872, 0.009857577738242914028, 0.01232197217280368330, 0.01355416939008405666, 0.01478636660736442829, 0.01601856382464479991, 0.01725076104192517154, 0.01971515547648590785 ),
 .UNSPECIFIED. ) ;
#880 = CARTESIAN_POINT ( 'NONE',  ( -79.76397050720386517, 93.94641470820118911, 87.71185091857950056 ) ) ;
#882 = CARTESIAN_POINT ( 'NONE',  ( 106.2775494337459037, -46.09182447052010190, 258.9292023535161889 ) ) ;
#883 = ADVANCED_FACE ( 'NONE', ( #13270 ), #75941, .F. ) ;
#884 = CARTESIAN_POINT ( 'NONE',  ( 116.7951252649886555, -39.38782981628543922, 193.6147919404536992 ) ) ;
#885 = SHAPE_REPRESENTATION ( 'Workpiece Locating V-Block', ( #50656 ), #34903 ) ;
#886 = CARTESIAN_POINT ( 'NONE',  ( -118.0434137139726118, 88.91291927174616205, 11.02232302911455264 ) ) ;
#887 = EDGE_CURVE ( 'NONE', #701, #2874, #49105, .T. ) ;
#888 = DIRECTION ( 'NONE',  ( 1.000000000000000000, -1.000000000000000078E-15, 0.000000000000000000 ) ) ;
#889 = CARTESIAN_POINT ( 'NONE',  ( 74.70173812346097009, 79.26437155269050550, -92.06079644778149884 ) ) ;
#890 = ORIENTED_EDGE ( 'NONE', *, *, #36462, .T. ) ;
#891 = DIRECTION ( 'NONE',  ( 0.1858654558203195195, -0.9825752044157765042, 0.000000000000000000 ) ) ;
#892 = DIRECTION ( 'NONE',  ( -3.491483361109385222E-15, 0.000000000000000000, 1.000000000000000000 ) ) ;
#893 = VERTEX_POINT ( 'NONE', #76385 ) ;
#894 = CARTESIAN_POINT ( 'NONE',  ( 110.3719962439868425, -47.27708535874812412, 52.80610146638697699 ) ) ;
#895 = ORIENTED_EDGE ( 'NONE', *, *, #68923, .F. ) ;
#896 = CARTESIAN_POINT ( 'NONE',  ( 101.0819131387675611, -42.86434890131523900, 21.38384839950496641 ) ) ;
#897 = ADVANCED_FACE ( 'NONE', ( #76834 ), #14164, .T. ) ;
#898 = CYLINDRICAL_SURFACE ( 'NONE', #14088, 4.749999999999976907 ) ;
#899 = CARTESIAN_POINT ( 'NONE',  ( 116.4500618263486444, -39.48841239489308919, 183.5984824187689526 ) ) ;
#900 = LINE ( 'NONE', #84028, #66537 ) ;
#901 = CARTESIAN_POINT ( 'NONE',  ( -3.968750000000770051, 127.0000000000000000, 105.4788588808462038 ) ) ;
#902 = DIRECTION ( 'NONE',  ( 1.000000000000000000, 4.163336342344333240E-14, 0.000000000000000000 ) ) ;
#903 = LINE ( 'NONE', #51260, #75514 ) ;
#904 = CARTESIAN_POINT ( 'NONE',  ( 109.2209341577003698, -48.43284210327079364, 273.7213395616253706 ) ) ;
#905 = CARTESIAN_POINT ( 'NONE',  ( 76.80574412431069220, 90.93089219781636245, -90.31319802837579402 ) ) ;
#906 = ORIENTED_EDGE ( 'NONE', *, *, #59103, .T. ) ;
#907 = CARTESIAN_POINT ( 'NONE',  ( 48.45959712129000252, -28.98061976758940617, -5.074374724088000832 ) ) ;
#908 = ORIENTED_EDGE ( 'NONE', *, *, #55610, .T. ) ;
#909 = CARTESIAN_POINT ( 'NONE',  ( 117.9015171282527916, -39.13767059441630636, 99.64038718067195077 ) ) ;
#910 = CARTESIAN_POINT ( 'NONE',  ( 121.8078998857219375, 45.20015392834827850, -46.98888152329894297 ) ) ;
#911 = ORIENTED_EDGE ( 'NONE', *, *, #31846, .F. ) ;
#912 = DIRECTION ( 'NONE',  ( 0.000000000000000000, 0.000000000000000000, -1.000000000000000000 ) ) ;
#913 = ORIENTED_EDGE ( 'NONE', *, *, #78891, .T. ) ;
#914 = VERTEX_POINT ( 'NONE', #980 ) ;
#915 = DIRECTION ( 'NONE',  ( -0.7071067811865475727, 0.7071067811865475727, 0.000000000000000000 ) ) ;
#916 = LINE ( 'NONE', #34531, #21635 ) ;
#917 = DIRECTION ( 'NONE',  ( -1.000000000000000000, 3.651563665954184899E-16, 0.000000000000000000 ) ) ;
#918 = CARTESIAN_POINT ( 'NONE',  ( 50.56670390244759972, -18.82844715994099971, -5.074374724088000832 ) ) ;
#919 = FACE_OUTER_BOUND ( 'NONE', #24563, .T. ) ;
#920 = CARTESIAN_POINT ( 'NONE',  ( 100.4792253034169960, -27.85352395805916359, 31.59657765686396758 ) ) ;
#922 = EDGE_CURVE ( 'NONE', #4290, #47689, #37387, .T. ) ;
#921 = FACE_BOUND ( 'NONE', #56521, .T. ) ;
#923 = ORIENTED_EDGE ( 'NONE', *, *, #29698, .F. ) ;
#924 = DIRECTION ( 'NONE',  ( 1.000000000000000000, 0.000000000000000000, -7.340987889507870014E-14 ) ) ;
#925 = EDGE_CURVE ( 'NONE', #41798, #56710, #4893, .T. ) ;
#926 = VECTOR ( 'NONE', #24690, 1000.000000000000000 ) ;
#927 = DIRECTION ( 'NONE',  ( 1.000000000000000000, 4.299999999999999979E-14, 1.000000000000000078E-15 ) ) ;
#928 = ORIENTED_EDGE ( 'NONE', *, *, #2414, .T. ) ;
#929 = EDGE_LOOP ( 'NONE', ( #3602, #48230, #57007, #56048 ) ) ;
#930 = CIRCLE ( 'NONE', #79267, 30.99999999999998579 ) ;
#931 = AXIS2_PLACEMENT_3D ( 'NONE', #34340, #61592, #6645 ) ;
#932 = CARTESIAN_POINT ( 'NONE',  ( 25.56670390244797275, -48.82844715994099971, 293.2178068554150627 ) ) ;
#933 = VECTOR ( 'NONE', #68373, 1000.000000000000000 ) ;
#934 = CARTESIAN_POINT ( 'NONE',  ( 19.56648329127400032, 0.2215528400590083269, 323.8756252759109202 ) ) ;
#935 = CARTESIAN_POINT ( 'NONE',  ( 97.12554568906318764, -37.99677948043573394, 16.42730063705512578 ) ) ;
#936 = VECTOR ( 'NONE', #85029, 1000.000000000000000 ) ;
#937 = DIRECTION ( 'NONE',  ( 0.000000000000000000, 0.000000000000000000, 1.000000000000000000 ) ) ;
#938 = DIRECTION ( 'NONE',  ( 0.000000000000000000, 1.365923996832131856E-16, -1.000000000000000000 ) ) ;
#939 = CARTESIAN_POINT ( 'NONE',  ( 98.04376085404715013, -35.95281974173802553, 185.6686103042669629 ) ) ;
#940 = CARTESIAN_POINT ( 'NONE',  ( 122.6197261538189593, 73.74150706513661646, 44.83011014023653473 ) ) ;
#941 = CARTESIAN_POINT ( 'NONE',  ( 102.5390659930443746, -27.28968240376552501, 95.43276813305395478 ) ) ;
#942 = ORIENTED_EDGE ( 'NONE', *, *, #84667, .T. ) ;
#943 = CARTESIAN_POINT ( 'NONE',  ( 132.1198940698264153, -20.67261125153088841, 7.590611884327144843 ) ) ;
#944 = VERTEX_POINT ( 'NONE', #22782 ) ;
#945 = CARTESIAN_POINT ( 'NONE',  ( -76.79083731950203173, 74.16215221268210200, -90.32738470895317562 ) ) ;
#946 = ORIENTED_EDGE ( 'NONE', *, *, #71953, .T. ) ;
#947 = CARTESIAN_POINT ( 'NONE',  ( 116.3212776292270973, -32.94146857470704504, 49.13562527591097506 ) ) ;
#948 = EDGE_LOOP ( 'NONE', ( #39295, #50309, #44340, #82075, #28155, #33375, #36970, #41977, #80232, #84882, #47381, #79009, #7396, #61225 ) ) ;
#949 = DIRECTION ( 'NONE',  ( 1.000000000000000000, 0.000000000000000000, 0.000000000000000000 ) ) ;
#950 = CARTESIAN_POINT ( 'NONE',  ( 34.92499999999999716, 82.54999999999999716, 290.4490000000000123 ) ) ;
#951 = CARTESIAN_POINT ( 'NONE',  ( 0.000000000000000000, 111.1250000000000000, 0.000000000000000000 ) ) ;
#952 = VECTOR ( 'NONE', #55966, 1000.000000000000000 ) ;
#953 = FACE_BOUND ( 'NONE', #7835, .T. ) ;
#954 = ORIENTED_EDGE ( 'NONE', *, *, #47098, .T. ) ;
#955 = CARTESIAN_POINT ( 'NONE',  ( 110.4638204314202881, -47.27238515144596676, 57.83657765686300678 ) ) ;
#957 = CARTESIAN_POINT ( 'NONE',  ( 87.44698480207823366, 71.76234181793741129, -96.94335780202294472 ) ) ;
#956 = CARTESIAN_POINT ( 'NONE',  ( 116.3201356630459884, -32.94258242523766711, 69.13562527591093954 ) ) ;
#958 = DIRECTION ( 'NONE',  ( -1.000000000000000078E-15, 1.000000000000000000, 0.000000000000000000 ) ) ;
#959 = CARTESIAN_POINT ( 'NONE',  ( 131.8592257737627449, -17.08568546291111190, 2.471387922376312218 ) ) ;
#960 = VERTEX_POINT ( 'NONE', #11251 ) ;
#961 = CARTESIAN_POINT ( 'NONE',  ( 77.31648329127399677, -36.72944715994107412, 14.92562527591094046 ) ) ;
#962 = CARTESIAN_POINT ( 'NONE',  ( 104.4899545134221910, -26.97880756921290413, 155.2814586042531459 ) ) ;
#963 = CARTESIAN_POINT ( 'NONE',  ( 107.0664832912739399, -49.89611382660763184, 308.7195067599733420 ) ) ;
#964 = CARTESIAN_POINT ( 'NONE',  ( 103.1973475860487639, -46.47157139977531415, 113.2756252759109827 ) ) ;
#966 = CARTESIAN_POINT ( 'NONE',  ( 48.86082318535700608, -35.55794170701751256, -5.074374724088000832 ) ) ;
#965 = CARTESIAN_POINT ( 'NONE',  ( 162.9033555647770015, -33.89581943344391135, -5.074374724088000832 ) ) ;
#967 = CARTESIAN_POINT ( 'NONE',  ( 99.06670390244704549, -104.2784471599421323, -21.78219314458201694 ) ) ;
#968 = CIRCLE ( 'NONE', #16988, 7.143750000000004263 ) ;
#969 = EDGE_CURVE ( 'NONE', #72419, #64336, #76549, .T. ) ;
#970 = VERTEX_POINT ( 'NONE', #3995 ) ;
#971 = EDGE_CURVE ( 'NONE', #54474, #73652, #20012, .T. ) ;
#972 = CARTESIAN_POINT ( 'NONE',  ( 97.46300000000010755, 82.54999999999999716, -12.69999999999898144 ) ) ;
#973 = EDGE_CURVE ( 'NONE', #19682, #50715, #60572, .T. ) ;
#974 = CARTESIAN_POINT ( 'NONE',  ( 98.36735121233628831, -42.37464764417345719, 142.7965776568629508 ) ) ;
#976 = VERTEX_POINT ( 'NONE', #80758 ) ;
#975 = CARTESIAN_POINT ( 'NONE',  ( 90.06670420047028358, -137.6784471599409585, 222.2178068554179902 ) ) ;
#977 = EDGE_CURVE ( 'NONE', #57623, #62556, #57271, .T. ) ;
#978 = CARTESIAN_POINT ( 'NONE',  ( 115.6373213143783545, -30.77082676042347487, 275.3099109901965562 ) ) ;
#979 = CARTESIAN_POINT ( 'NONE',  ( 194.0371591254572934, -24.42818131005417825, 300.4678068554149490 ) ) ;
#980 = CARTESIAN_POINT ( 'NONE',  ( 51.03742451361310373, -23.42844715994068849, 193.9678068554150911 ) ) ;
#981 = CARTESIAN_POINT ( 'NONE',  ( 103.2512128930081730, -76.97768462775967180, 250.2178068554180470 ) ) ;
#982 = CARTESIAN_POINT ( 'NONE',  ( 80.06648329127399677, -8.350947159940998787, 293.6356252759119911 ) ) ;
#983 = EDGE_CURVE ( 'NONE', #35866, #2341, #17632, .T. ) ;
#984 = CARTESIAN_POINT ( 'NONE',  ( 68.76253601752615907, -136.8623718444874555, 247.4903208786739981 ) ) ;
#985 = CARTESIAN_POINT ( 'NONE',  ( -93.49502539975199511, 69.93364840292896645, 91.12742965731035838 ) ) ;
#986 = VECTOR ( 'NONE', #84387, 1000.000000000000000 ) ;
#987 = CARTESIAN_POINT ( 'NONE',  ( 116.1939227058878714, -40.33550099034470549, 193.5270538473399426 ) ) ;
#988 = ORIENTED_EDGE ( 'NONE', *, *, #73179, .F. ) ;
#989 = ORIENTED_EDGE ( 'NONE', *, *, #13021, .F. ) ;
#990 = CARTESIAN_POINT ( 'NONE',  ( 107.8658914883948512, -27.90296577952642210, 151.4358690201829631 ) ) ;
#991 = EDGE_CURVE ( 'NONE', #50564, #38934, #59391, .T. ) ;
#992 = VECTOR ( 'NONE', #4749, 1000.000000000000000 ) ;
#993 = CARTESIAN_POINT ( 'NONE',  ( 51.42025729302798709, -31.94127993907680718, -5.074374724088000832 ) ) ;
#994 = AXIS2_PLACEMENT_3D ( 'NONE', #60875, #53588, #6362 ) ;
#995 = CARTESIAN_POINT ( 'NONE',  ( 117.6440909798951253, -33.30491947301820232, 280.0756252759109657 ) ) ;
#996 = CYLINDRICAL_SURFACE ( 'NONE', #75479, 7.143749999999999822 ) ;
#997 = ADVANCED_FACE ( 'NONE', ( #45744 ), #73028, .F. ) ;
#998 = CARTESIAN_POINT ( 'NONE',  ( 158.0667039024469886, -67.87844715994090450, 120.2178068554179902 ) ) ;
#999 = CARTESIAN_POINT ( 'NONE',  ( 107.3241674272228892, -25.27320757387406402, 321.5865679059475610 ) ) ;
#1000 = FACE_OUTER_BOUND ( 'NONE', #74644, .T. ) ;
#1001 = CARTESIAN_POINT ( 'NONE',  ( 131.0667039024480118, -67.87844715994100397, 207.5838068554149913 ) ) ;
#1002 = CARTESIAN_POINT ( 'NONE',  ( 112.4430884738663821, -45.67687932769439385, 238.0070538473389377 ) ) ;
#1003 = DIRECTION ( 'NONE',  ( 1.000000000000000078E-15, -1.000000000000000083E-30, -1.000000000000000000 ) ) ;
#1004 = VERTEX_POINT ( 'NONE', #15963 ) ;
#1005 = ORIENTED_EDGE ( 'NONE', *, *, #10407, .T. ) ;
#1006 = EDGE_CURVE ( 'NONE', #6675, #59868, #43643, .T. ) ;
#1007 = CARTESIAN_POINT ( 'NONE',  ( 99.04406184276894010, -42.84125761936532939, 86.84395860719635607 ) ) ;
#1008 = CARTESIAN_POINT ( 'NONE',  ( 82.81058719979510840, -18.91414947189774409, 6.758631288823465866 ) ) ;
#1009 = DIRECTION ( 'NONE',  ( -0.9254794337955620787, -0.3787978585227822492, 0.000000000000000000 ) ) ;
#1010 = FACE_OUTER_BOUND ( 'NONE', #74696, .T. ) ;
#1011 = VECTOR ( 'NONE', #20035, 1000.000000000000000 ) ;
#1012 = CARTESIAN_POINT ( 'NONE',  ( 114.3402351757609097, -43.26825200597433962, 34.24419670448197905 ) ) ;
#1013 = DIRECTION ( 'NONE',  ( -3.100000000000000258E-29, 3.100000000000000044E-14, 1.000000000000000000 ) ) ;
#1014 = CLOSED_SHELL ( 'NONE', ( #3243, #64982, #6193, #64038, #15469, #48042, #25476 ) ) ;
#1015 = ORIENTED_EDGE ( 'NONE', *, *, #78887, .F. ) ;
#1016 = CARTESIAN_POINT ( 'NONE',  ( 112.1383799374394670, -26.85658479980368440, 15.71086337114896381 ) ) ;
#1017 = DIRECTION ( 'NONE',  ( 0.000000000000000000, 1.000000000000000000, 0.000000000000000000 ) ) ;
#1018 = B_SPLINE_CURVE_WITH_KNOTS ( 'NONE', 3,
 ( #43540, #14059, #62654, #428, #76288, #35382, #57168, #8604, #77636, #56725, #28117, #43086, #41741, #71282, #64450, #70369, #55805, #83560, #36302, #48997, #42634, #21786, #63552, #64010, #70829, #1788, #14519, #22685, #36751, #29485, #35836, #880, #2231, #56264, #29040, #21326, #84471, #50355, #29941, #1338, #42197, #69928, #8145, #84011, #77195, #22234, #69478, #78094, #57625 ),
 .UNSPECIFIED., .F., .F.,
 ( 4, 2, 2, 2, 2, 2, 2, 2, 2, 2, 2, 2, 2, 2, 2, 1, 2, 2, 2, 2, 2, 2, 2, 2, 4 ),
 ( 0.01987186023414422645, 0.02111356671950567407, 0.02235527320486711822, 0.02483868617559002040, 0.02608039266095149578, 0.02732209914631297809, 0.02980551211703592190, 0.03228892508775886572, 0.03353063157312033415, 0.03477233805848178871, 0.03725575102920469783, 0.03849745751456615239, 0.03973916399992760695, 0.04222257697065050913, 0.04346428345601198451, 0.04470598994137346682, 0.04594769642673494914, 0.04718940291209643145, 0.04967281588281940996, 0.05091452236818086452, 0.05215622885354231908, 0.05463964182426526983, 0.05588134830962676602, 0.05712305479498826222, 0.05960646776571128236 ),
 .UNSPECIFIED. ) ;
#1019 = CARTESIAN_POINT ( 'NONE',  ( 112.4118754778678380, -46.40445981238691076, 252.9661014663871583 ) ) ;
#1020 = ORIENTED_EDGE ( 'NONE', *, *, #22420, .F. ) ;
#1021 = B_SPLINE_CURVE_WITH_KNOTS ( 'NONE', 3,
 ( #71671, #64846, #73436, #24410, #51194, #87082, #18468, #18022, #72989, #59353, #45705, #3069, #87525, #9885, #58898, #73886, #65723, #17148 ),
 .UNSPECIFIED., .F., .F.,
 ( 4, 2, 2, 2, 2, 2, 2, 2, 4 ),
 ( 0.000000000000000000, 0.06249843191113654828, 0.1249968638222730966, 0.1874952957334096448, 0.2499937276445461931, 0.3124921595556827691, 0.3749905914668192897, 0.4374890233779558102, 0.4999874552890923862 ),
 .UNSPECIFIED. ) ;
#1022 = CARTESIAN_POINT ( 'NONE',  ( 77.74802179993278628, -38.20859666167125113, 7.273989459505274091 ) ) ;
#1023 = DIRECTION ( 'NONE',  ( 0.000000000000000000, 0.000000000000000000, 1.000000000000000000 ) ) ;
#1024 = DIRECTION ( 'NONE',  ( -4.237773401492740281E-14, 1.000000000000000000, 0.000000000000000000 ) ) ;
#1025 = CARTESIAN_POINT ( 'NONE',  ( 98.46239236780679960, -37.66247686286469332, 79.21856656006798403 ) ) ;
#1026 = CARTESIAN_POINT ( 'NONE',  ( 102.0405519839503086, -46.59986864225058412, 168.2137205140059564 ) ) ;
#1027 = DIRECTION ( 'NONE',  ( 0.000000000000000000, 0.000000000000000000, -1.000000000000000000 ) ) ;
#1028 = ORIENTED_EDGE ( 'NONE', *, *, #76526, .F. ) ;
#1029 = EDGE_CURVE ( 'NONE', #69678, #54710, #73477, .T. ) ;
#1030 = FACE_OUTER_BOUND ( 'NONE', #20809, .T. ) ;
#1031 = ORIENTED_EDGE ( 'NONE', *, *, #56201, .F. ) ;
#1032 = ORIENTED_EDGE ( 'NONE', *, *, #44128, .F. ) ;
#1033 = CARTESIAN_POINT ( 'NONE',  ( 107.0667039024482818, -36.72944715994103149, 249.5838068554170093 ) ) ;
#1034 = ORIENTED_EDGE ( 'NONE', *, *, #40096, .F. ) ;
#1035 = ORIENTED_EDGE ( 'NONE', *, *, #1775, .F. ) ;
#1036 = DIRECTION ( 'NONE',  ( 0.2588190451025180749, 0.000000000000000000, -0.9659258262890690894 ) ) ;
#1037 = CARTESIAN_POINT ( 'NONE',  ( 112.1857315011839802, -29.85591823435125747, 103.9895626852199655 ) ) ;
#1038 = CARTESIAN_POINT ( 'NONE',  ( 118.1310582692406257, -36.20923403681121044, 268.8518157521014587 ) ) ;
#1039 = CARTESIAN_POINT ( 'NONE',  ( 194.5667039024482960, -47.82844715993405771, 300.4678068554149490 ) ) ;
#1040 = DIRECTION ( 'NONE',  ( 0.000000000000000000, 0.000000000000000000, -1.000000000000000000 ) ) ;
#1041 = ADVANCED_FACE ( 'NONE', ( #85016 ), #1147, .F. ) ;
#1042 = VECTOR ( 'NONE', #24862, 1000.000000000000000 ) ;
#1043 = ORIENTED_EDGE ( 'NONE', *, *, #73675, .T. ) ;
#1044 = DIRECTION ( 'NONE',  ( -1.000000000000000000, -2.756263715554006823E-15, 0.000000000000000000 ) ) ;
#1045 = VECTOR ( 'NONE', #50807, 1000.000000000000000 ) ;
#1046 = CYLINDRICAL_SURFACE ( 'NONE', #15910, 2.999999999999999112 ) ;
#1047 = DIRECTION ( 'NONE',  ( 0.000000000000000000, -1.000000000000000000, 0.000000000000000000 ) ) ;
#1048 = CARTESIAN_POINT ( 'NONE',  ( 117.2073019650709256, -38.89799087863980276, 108.6708633711499772 ) ) ;
#1049 = EDGE_CURVE ( 'NONE', #77857, #70798, #9839, .T. ) ;
#1050 = CARTESIAN_POINT ( 'NONE',  ( 98.26918992425659383, -28.71468409831775404, 80.73848241876795839 ) ) ;
#1052 = CARTESIAN_POINT ( 'NONE',  ( 99.30039714715974242, -28.79844535499942637, 270.7051490854347549 ) ) ;
#1051 = CIRCLE ( 'NONE', #41678, 218.1859999999999786 ) ;
#1053 = ORIENTED_EDGE ( 'NONE', *, *, #85400, .T. ) ;
#1054 = AXIS2_PLACEMENT_3D ( 'NONE', #30838, #23597, #85383 ) ;
#1055 = CARTESIAN_POINT ( 'NONE',  ( 98.83914287153486100, -29.34771585412822859, 235.7565776568629872 ) ) ;
#1056 = DIRECTION ( 'NONE',  ( 0.000000000000000000, -1.000000000000000000, 0.000000000000000000 ) ) ;
#1057 = CIRCLE ( 'NONE', #69269, 2.500000000000002220 ) ;
#1058 = PLANE ( 'NONE',  #80794 ) ;
#1060 = CARTESIAN_POINT ( 'NONE',  ( 68.70366513962476063, -139.2930699478345389, 245.9105554508155649 ) ) ;
#1059 = PLANE ( 'NONE',  #8576 ) ;
#1061 = DIRECTION ( 'NONE',  ( 0.000000000000000000, 0.000000000000000000, 1.000000000000000000 ) ) ;
#1062 = DIRECTION ( 'NONE',  ( 0.000000000000000000, 0.000000000000000000, -1.000000000000000000 ) ) ;
#1063 = CARTESIAN_POINT ( 'NONE',  ( 12.53573128184445551, 84.62794568765841063, -117.8914214560859932 ) ) ;
#1064 = CARTESIAN_POINT ( 'NONE',  ( -12.70000000000000107, 82.54999999999999716, 129.9368274816650910 ) ) ;
#1065 = CARTESIAN_POINT ( 'NONE',  ( -3.174999999999644995, 104.3431970271541616, -33.98325472291465132 ) ) ;
#1066 = DIRECTION ( 'NONE',  ( 0.000000000000000000, 0.000000000000000000, 1.000000000000000000 ) ) ;
#1067 = AXIS2_PLACEMENT_3D ( 'NONE', #89420, #55748, #68523 ) ;
#1069 = VERTEX_POINT ( 'NONE', #73932 ) ;
#1068 = CARTESIAN_POINT ( 'NONE',  ( 113.2454986924611831, -28.75867294014850017, 259.5522919431510331 ) ) ;
#1070 = CARTESIAN_POINT ( 'NONE',  ( 116.3212776292296127, -32.94146857471318413, 9.635625275910941312 ) ) ;
#1071 = CARTESIAN_POINT ( 'NONE',  ( 110.9007760261032871, -26.97308707819648887, 269.7784824187680783 ) ) ;
#1072 = CARTESIAN_POINT ( 'NONE',  ( 113.8434436840914117, -28.76112614263219669, 135.5156252759109634 ) ) ;
#1073 = CARTESIAN_POINT ( 'NONE',  ( 97.08395347075709481, -39.80944164022105980, 17.56419670448195092 ) ) ;
#1074 = AXIS2_PLACEMENT_3D ( 'NONE', #83789, #85142, #1565 ) ;
#1075 = DIRECTION ( 'NONE',  ( 0.000000000000000000, 0.000000000000000000, -1.000000000000000000 ) ) ;
#1077 = CARTESIAN_POINT ( 'NONE',  ( 82.81181082189971221, -36.54506369576082392, 6.756870619999560290 ) ) ;
#1076 = DIRECTION ( 'NONE',  ( 0.000000000000000000, 0.000000000000000000, 1.000000000000000000 ) ) ;
#1078 = CARTESIAN_POINT ( 'NONE',  ( 80.06648329127399677, -8.729447159940999512, 308.6356252759119911 ) ) ;
#1079 = CIRCLE ( 'NONE', #5432, 7.143750000000001599 ) ;
#1080 = ORIENTED_EDGE ( 'NONE', *, *, #12504, .T. ) ;
#1081 = EDGE_CURVE ( 'NONE', #311, #15646, #50008, .T. ) ;
#1082 = DIRECTION ( 'NONE',  ( 0.000000000000000000, 1.000000000000000000, 0.000000000000000000 ) ) ;
#1083 = ORIENTED_EDGE ( 'NONE', *, *, #51612, .F. ) ;
#1084 = EDGE_CURVE ( 'NONE', #81584, #10240, #66415, .T. ) ;
#1085 = CARTESIAN_POINT ( 'NONE',  ( 115.8434954054525292, -34.49858887834006538, 168.4590864947439854 ) ) ;
#1087 = ORIENTED_EDGE ( 'NONE', *, *, #37246, .T. ) ;
#1086 = DIRECTION ( 'NONE',  ( -4.299999999999999979E-14, 1.000000000000000000, -4.400000000000000367E-29 ) ) ;
#1088 = CARTESIAN_POINT ( 'NONE',  ( 69.25757238336807120, -1.944390235229864539, 361.9756252759101471 ) ) ;
#1089 = EDGE_CURVE ( 'NONE', #82238, #52360, #8707, .T. ) ;
#1090 = CARTESIAN_POINT ( 'NONE',  ( 107.6517678568360452, -47.10594642807011923, 148.6213395616249784 ) ) ;
#1091 = LINE ( 'NONE', #34257, #64234 ) ;
#1092 = CARTESIAN_POINT ( 'NONE',  ( 100.9550073947607416, -28.70676405461405878, 150.5943758343188676 ) ) ;
#1093 = DIRECTION ( 'NONE',  ( 1.000000000000000000, 1.132880637372608296E-15, 0.000000000000000000 ) ) ;
#1094 = CARTESIAN_POINT ( 'NONE',  ( -85.00925061400930360, 69.93366089391888352, 82.64146475440757911 ) ) ;
#1095 = EDGE_CURVE ( 'NONE', #23005, #54148, #34462, .T. ) ;
#1096 = CARTESIAN_POINT ( 'NONE',  ( -254.0000000000000000, 93.66249999999999432, 15.87500000000039968 ) ) ;
#1097 = CARTESIAN_POINT ( 'NONE',  ( 97.87212830949604836, -31.93334231290197067, 90.93181575210196854 ) ) ;
#1098 = AXIS2_PLACEMENT_3D ( 'NONE', #46225, #82143, #67591 ) ;
#1099 = EDGE_LOOP ( 'NONE', ( #50497, #23649, #64387, #74455 ) ) ;
#1100 = EDGE_LOOP ( 'NONE', ( #17602, #31733, #14707, #68615 ) ) ;
#1102 = EDGE_LOOP ( 'NONE', ( #66047, #88508, #70924, #49259 ) ) ;
#1101 = VECTOR ( 'NONE', #3865, 1000.000000000000000 ) ;
#1103 = CARTESIAN_POINT ( 'NONE',  ( 104.4962338114797262, -45.76661171243296877, 63.79967854399193072 ) ) ;
#1104 = CARTESIAN_POINT ( 'NONE',  ( -76.20505178924449297, 127.0000000000000000, 76.20505178924310030 ) ) ;
#1106 = CARTESIAN_POINT ( 'NONE',  ( 117.0718954832505148, -35.46248234554022360, 38.92729194342982879 ) ) ;
#1105 = CARTESIAN_POINT ( 'NONE',  ( 97.38117110781249153, -35.36630255995241612, 177.2156252759109805 ) ) ;
#1107 = CARTESIAN_POINT ( 'NONE',  ( 98.35008263532775175, -31.65619168214967871, 55.90512834145738452 ) ) ;
#1108 = CARTESIAN_POINT ( 'NONE',  ( 107.0667039024470313, -104.2784471599413934, 2.217806855418003043 ) ) ;
#1109 = ADVANCED_FACE ( 'NONE', ( #1881 ), #58941, .F. ) ;
#1110 = CYLINDRICAL_SURFACE ( 'NONE', #1074, 3.174999999999997158 ) ;
#1111 = DIRECTION ( 'NONE',  ( 0.000000000000000000, 0.000000000000000000, 1.000000000000000000 ) ) ;
#1112 = DIRECTION ( 'NONE',  ( 4.299999999999999979E-14, -1.000000000000000000, 0.000000000000000000 ) ) ;
#1113 = CARTESIAN_POINT ( 'NONE',  ( 96.05093434719793777, -37.29646042206077539, 121.3794347997209684 ) ) ;
#1114 = ORIENTED_EDGE ( 'NONE', *, *, #42132, .T. ) ;
#1115 = EDGE_LOOP ( 'NONE', ( #85274, #9415 ) ) ;
#1116 = ORIENTED_EDGE ( 'NONE', *, *, #64438, .T. ) ;
#1117 = FILL_AREA_STYLE ('',( #49240 ) ) ;
#1118 = CARTESIAN_POINT ( 'NONE',  ( -96.94208673522986430, 93.33885111288434189, -87.44839512528828607 ) ) ;
#1119 = AXIS2_PLACEMENT_3D ( 'NONE', #62798, #47484, #18902 ) ;
#1120 = FACE_OUTER_BOUND ( 'NONE', #51217, .T. ) ;
#1121 = LINE ( 'NONE', #34282, #64196 ) ;
#1122 = CARTESIAN_POINT ( 'NONE',  ( 102.0328030160422230, -28.93470572416599751, 218.3509475124479593 ) ) ;
#1123 = VECTOR ( 'NONE', #70345, 1000.000000000000000 ) ;
#1124 = APPLICATION_CONTEXT ( 'automotive_design' ) ;
#1125 = VECTOR ( 'NONE', #24217, 1000.000000000000000 ) ;
#1126 = CARTESIAN_POINT ( 'NONE',  ( 116.3283240494693160, -32.94276334974209419, 64.13562527591099638 ) ) ;
#1127 = CARTESIAN_POINT ( 'NONE',  ( 128.2586590417343473, -60.54728653293321372, 394.9756252759100903 ) ) ;
#1128 = ORIENTED_EDGE ( 'NONE', *, *, #82632, .T. ) ;
#1130 = ORIENTED_EDGE ( 'NONE', *, *, #23416, .T. ) ;
#1129 = VERTEX_POINT ( 'NONE', #47992 ) ;
#1131 = AXIS2_PLACEMENT_3D ( 'NONE', #86583, #87473, #80666 ) ;
#1132 = CARTESIAN_POINT ( 'NONE',  ( 172.5664832912740110, 0.2215528400590013880, 261.0426252759119734 ) ) ;
#1133 = ORIENTED_EDGE ( 'NONE', *, *, #3086, .T. ) ;
#1134 = VERTEX_POINT ( 'NONE', #61189 ) ;
#1135 = CARTESIAN_POINT ( 'NONE',  ( 80.06648281188262217, -21.47944715903999224, 8.225259175037979986 ) ) ;
#1136 = CARTESIAN_POINT ( 'NONE',  ( 105.1749981762835802, -28.04127050161159218, 256.6787261630399826 ) ) ;
#1137 = CIRCLE ( 'NONE', #51867, 218.1859999999999786 ) ;
#1138 = CARTESIAN_POINT ( 'NONE',  ( 105.7154763623905325, -46.72385826930020158, 272.4689585321721097 ) ) ;
#1139 = ORIENTED_EDGE ( 'NONE', *, *, #52392, .F. ) ;
#1140 = VECTOR ( 'NONE', #9711, 1000.000000000000000 ) ;
#1141 = AXIS2_PLACEMENT_3D ( 'NONE', #65937, #38679, #53176 ) ;
#1142 = EDGE_CURVE ( 'NONE', #55592, #16504, #81665, .T. ) ;
#1143 = FACE_OUTER_BOUND ( 'NONE', #20323, .T. ) ;
#1144 = CARTESIAN_POINT ( 'NONE',  ( -125.2622172144571522, 69.13895712999180887, 36.80031982249843026 ) ) ;
#1145 = VERTEX_POINT ( 'NONE', #33486 ) ;
#1146 = ORIENTED_EDGE ( 'NONE', *, *, #46506, .T. ) ;
#1147 = CONICAL_SURFACE ( 'NONE', #80912, 1.571100913904360796, 1.047197551196591414 ) ;
#1148 = DIRECTION ( 'NONE',  ( 1.000000000000000078E-15, 1.000000000000000083E-30, -1.000000000000000000 ) ) ;
#1149 = EDGE_LOOP ( 'NONE', ( #68518, #70003, #30605, #37059 ) ) ;
#1150 = ORIENTED_EDGE ( 'NONE', *, *, #9525, .F. ) ;
#1151 = EDGE_CURVE ( 'NONE', #29300, #69198, #38864, .T. ) ;
#1152 = CARTESIAN_POINT ( 'NONE',  ( 98.99928044157054785, -35.48447157832033128, 264.0223760838769635 ) ) ;
#1153 = CARTESIAN_POINT ( 'NONE',  ( 101.9737040637596124, -45.89197751792076474, 187.1727681330539781 ) ) ;
#1154 = CARTESIAN_POINT ( 'NONE',  ( 102.3122812202564376, -27.43633205498510108, 120.4527681330539792 ) ) ;
#1155 = LINE ( 'NONE', #58661, #6547 ) ;
#1156 = CARTESIAN_POINT ( 'NONE',  ( 193.0371591254586008, -47.82818131005421236, 193.9678068554150343 ) ) ;
#1157 = CARTESIAN_POINT ( 'NONE',  ( 117.4126858048608000, -35.18755665659306686, 214.9441967044829767 ) ) ;
#1158 = LINE ( 'NONE', #36120, #6583 ) ;
#1159 = PLANE ( 'NONE',  #88725 ) ;
#1160 = ORIENTED_EDGE ( 'NONE', *, *, #77085, .F. ) ;
#1161 = DIRECTION ( 'NONE',  ( 0.000000000000000000, 0.000000000000000000, -1.000000000000000000 ) ) ;
#1162 = VERTEX_POINT ( 'NONE', #12156 ) ;
#1163 = EDGE_LOOP ( 'NONE', ( #74376, #83384, #75990, #89814 ) ) ;
#1164 = CARTESIAN_POINT ( 'NONE',  ( -254.0000000000000000, 3.174999999999999822, -41.27499999999999858 ) ) ;
#1165 = AXIS2_PLACEMENT_3D ( 'NONE', #18310, #30611, #59188 ) ;
#1166 = CIRCLE ( 'NONE', #18523, 2.117000000000000881 ) ;
#1167 = DIRECTION ( 'NONE',  ( 1.000000000000000000, 4.443626637970137948E-14, 0.000000000000000000 ) ) ;
#1168 = EDGE_CURVE ( 'NONE', #65321, #37445, #68012, .T. ) ;
#1169 = ORIENTED_EDGE ( 'NONE', *, *, #25991, .T. ) ;
#1170 = CARTESIAN_POINT ( 'NONE',  ( 117.2382404677042729, -39.01746902538002360, 148.6499109901969859 ) ) ;
#1171 = DIRECTION ( 'NONE',  ( 0.000000000000000000, 0.000000000000000000, -1.000000000000000000 ) ) ;
#1172 = CARTESIAN_POINT ( 'NONE',  ( 107.0667039024470313, -104.2784471599420471, -19.18411693322902423 ) ) ;
#1173 = DIRECTION ( 'NONE',  ( 0.000000000000000000, 0.000000000000000000, -1.000000000000000000 ) ) ;
#1176 = CARTESIAN_POINT ( 'NONE',  ( 115.7579298488886224, -31.01215564512775558, 250.2899109901966028 ) ) ;
#1175 = FACE_OUTER_BOUND ( 'NONE', #74451, .T. ) ;
#1174 = CARTESIAN_POINT ( 'NONE',  ( 142.8824340801165249, -74.11588153691421610, 540.9756252759101471 ) ) ;
#1177 = DIRECTION ( 'NONE',  ( -3.100000000000000258E-29, 3.100000000000000044E-14, 1.000000000000000000 ) ) ;
#1178 = DIRECTION ( 'NONE',  ( -0.000000000000000000, 1.000000000000000000, 0.000000000000000000 ) ) ;
#1179 = CARTESIAN_POINT ( 'NONE',  ( 151.0667039024469886, -79.67844715994088745, 190.2178068554179902 ) ) ;
#1180 = DIRECTION ( 'NONE',  ( 0.000000000000000000, 0.000000000000000000, -1.000000000000000000 ) ) ;
#1181 = DIRECTION ( 'NONE',  ( 0.000000000000000000, -1.000000000000000000, 0.000000000000000000 ) ) ;
#1182 = PRODUCT_DEFINITION ( 'UNKNOWN', '', #76925, #64183 ) ;
#1183 = DIRECTION ( 'NONE',  ( -0.9254794337955620787, -0.3787978585227822492, 0.000000000000000000 ) ) ;
#1185 = ORIENTED_EDGE ( 'NONE', *, *, #8505, .T. ) ;
#1184 = CARTESIAN_POINT ( 'NONE',  ( 110.9088526855213388, -26.95253601363527807, 269.7784824187680783 ) ) ;
#1186 = PLANE ( 'NONE',  #3121 ) ;
#1187 = CARTESIAN_POINT ( 'NONE',  ( 97.65468660891812647, -41.26425114427870255, 171.6841967044819626 ) ) ;
#1188 = CARTESIAN_POINT ( 'NONE',  ( 115.6731346838618464, -43.66482979471727077, 39.27467289495895386 ) ) ;
#1189 = CARTESIAN_POINT ( 'NONE',  ( 112.2265052985635236, -45.83807782717671131, 208.9870538473389558 ) ) ;
#1190 = VECTOR ( 'NONE', #44932, 1000.000000000000000 ) ;
#1191 = CARTESIAN_POINT ( 'NONE',  ( 105.7995183767597211, -26.72403497849174059, 31.17729195139352427 ) ) ;
#1192 = FACE_OUTER_BOUND ( 'NONE', #57543, .T. ) ;
#1194 = CARTESIAN_POINT ( 'NONE',  ( 51.06670390244799762, -33.35206098992630075, -5.074374724088000832 ) ) ;
#1193 = CYLINDRICAL_SURFACE ( 'NONE', #21742, 2.030000000001311644 ) ;
#1195 = DIRECTION ( 'NONE',  ( -3.999999999999999995E-14, 1.000000000000000000, -4.100000000000000342E-29 ) ) ;
#1196 = CARTESIAN_POINT ( 'NONE',  ( 0.000000000000000000, 0.000000000000000000, 0.000000000000000000 ) ) ;
#1197 = VERTEX_POINT ( 'NONE', #55253 ) ;
#1198 = DIRECTION ( 'NONE',  ( 0.000000000000000000, 1.000000000000000000, 0.000000000000000000 ) ) ;
#1199 = AXIS2_PLACEMENT_3D ( 'NONE', #57374, #64210, #15161 ) ;
#1200 = CIRCLE ( 'NONE', #15728, 6.571100913904396990 ) ;
#1201 = EDGE_LOOP ( 'NONE', ( #30232, #45202 ) ) ;
#1202 = VERTEX_POINT ( 'NONE', #26225 ) ;
#1203 = EDGE_CURVE ( 'NONE', #37163, #33963, #54349, .T. ) ;
#1204 = VECTOR ( 'NONE', #3252, 1000.000000000000114 ) ;
#1206 = ORIENTED_EDGE ( 'NONE', *, *, #46372, .T. ) ;
#1205 = CYLINDRICAL_SURFACE ( 'NONE', #12500, 10.00000000000000711 ) ;
#1207 = CARTESIAN_POINT ( 'NONE',  ( 101.0787430638809496, -27.46603582566407908, 66.54514908543495721 ) ) ;
#1208 = CARTESIAN_POINT ( 'NONE',  ( 63.03715912545643363, -24.42818131006017168, 129.9678068554150911 ) ) ;
#1209 = EDGE_CURVE ( 'NONE', #36892, #42299, #54799, .T. ) ;
#1210 = VECTOR ( 'NONE', #71058, 1000.000000000000000 ) ;
#1211 = DIRECTION ( 'NONE',  ( 1.000000000000000000, 0.000000000000000000, 0.000000000000000000 ) ) ;
#1212 = CARTESIAN_POINT ( 'NONE',  ( 117.8238795360118445, -33.99523349031771602, 165.0365776568629315 ) ) ;
#1213 = EDGE_CURVE ( 'NONE', #59215, #59751, #18967, .T. ) ;
#1214 = AXIS2_PLACEMENT_3D ( 'NONE', #4908, #60752, #6253 ) ;
#1215 = VECTOR ( 'NONE', #17266, 1000.000000000000000 ) ;
#1216 = CARTESIAN_POINT ( 'NONE',  ( 116.1088647163993386, -36.23144265813309772, 273.3048007804578674 ) ) ;
#1217 = ORIENTED_EDGE ( 'NONE', *, *, #20900, .F. ) ;
#1218 = ORIENTED_EDGE ( 'NONE', *, *, #74092, .F. ) ;
#1219 = ORIENTED_EDGE ( 'NONE', *, *, #23918, .F. ) ;
#1220 = ORIENTED_EDGE ( 'NONE', *, *, #26232, .F. ) ;
#1221 = CARTESIAN_POINT ( 'NONE',  ( 116.3212776292267989, -32.94146857470629186, 109.1356252759109680 ) ) ;
#1222 = CARTESIAN_POINT ( 'NONE',  ( 0.000000000000000000, 101.5999999999999943, 0.000000000000000000 ) ) ;
#1223 = PLANE ( 'NONE',  #63688 ) ;
#1224 = CARTESIAN_POINT ( 'NONE',  ( 109.7248659172085468, -27.00080517855199602, 74.86479194292134309 ) ) ;
#1225 = CARTESIAN_POINT ( 'NONE',  ( 97.63858630140103401, 92.64237678566784950, 86.67213519546724854 ) ) ;
#1226 = CARTESIAN_POINT ( 'NONE',  ( 74.06670390244701707, -90.27844715994098124, 45.21780685541799727 ) ) ;
#1227 = EDGE_CURVE ( 'NONE', #46193, #83432, #400, .T. ) ;
#1228 = CARTESIAN_POINT ( 'NONE',  ( 51.42025729304100423, -33.70561438051981185, 313.9678068554150059 ) ) ;
#1229 = CARTESIAN_POINT ( 'NONE',  ( 168.0371591254546217, -48.62818131005519007, 129.9678068554150059 ) ) ;
#1230 = EDGE_CURVE ( 'NONE', #47280, #23292, #33932, .T. ) ;
#1231 = CARTESIAN_POINT ( 'NONE',  ( 114.0759046727996093, -46.25395340493279406, 33.08133956162495792 ) ) ;
#1232 = CARTESIAN_POINT ( 'NONE',  ( 41.56648329127499153, -32.07844715994070839, 18.92562527591200094 ) ) ;
#1233 = VERTEX_POINT ( 'NONE', #53904 ) ;
#1234 = CARTESIAN_POINT ( 'NONE',  ( 109.7248663305506824, -27.00080529972676402, 269.8647919088584786 ) ) ;
#1235 = CIRCLE ( 'NONE', #78146, 5.599999999999994316 ) ;
#1236 = CARTESIAN_POINT ( 'NONE',  ( -53.64297985755450782, 53.97500000000000142, 70.79999999999999716 ) ) ;
#1237 = CARTESIAN_POINT ( 'NONE',  ( 99.02147155855831784, -38.11057432192225747, 89.27951894101998676 ) ) ;
#1238 = VECTOR ( 'NONE', #55571, 1000.000000000000000 ) ;
#1239 = DIRECTION ( 'NONE',  ( 0.000000000000000000, 0.000000000000000000, -1.000000000000000000 ) ) ;
#1240 = FACE_OUTER_BOUND ( 'NONE', #74366, .T. ) ;
#1241 = VERTEX_POINT ( 'NONE', #61630 ) ;
#1242 = ORIENTED_EDGE ( 'NONE', *, *, #88066, .T. ) ;
#1243 = CARTESIAN_POINT ( 'NONE',  ( 116.3195061320206207, -32.94150711290046729, 139.1356252759109680 ) ) ;
#1244 = ORIENTED_EDGE ( 'NONE', *, *, #63545, .T. ) ;
#1245 = EDGE_LOOP ( 'NONE', ( #56958, #54258, #46238, #1220 ) ) ;
#1246 = CARTESIAN_POINT ( 'NONE',  ( 113.3535730310440215, -29.74740315656111989, 155.9368214011359726 ) ) ;
#1247 = CIRCLE ( 'NONE', #51976, 6.647542495715439870 ) ;
#1248 = CARTESIAN_POINT ( 'NONE',  ( 0.000000000000000000, 65.60000000000000853, 0.000000000000000000 ) ) ;
#1249 = CARTESIAN_POINT ( 'NONE',  ( 117.6173583669683040, -42.17933576662011319, 89.44705384733997278 ) ) ;
#1250 = LINE ( 'NONE', #55720, #50250 ) ;
#1251 = ORIENTED_EDGE ( 'NONE', *, *, #68598, .T. ) ;
#1252 = VECTOR ( 'NONE', #76868, 1000.000000000000000 ) ;
#1253 = EDGE_LOOP ( 'NONE', ( #76808, #30804, #21641, #56351 ) ) ;
#1254 = ORIENTED_EDGE ( 'NONE', *, *, #34297, .F. ) ;
#1255 = ADVANCED_FACE ( 'NONE', ( #13946 ), #5345, .T. ) ;
#1256 = AXIS2_PLACEMENT_3D ( 'NONE', #56524, #84270, #2479 ) ;
#1257 = CYLINDRICAL_SURFACE ( 'NONE', #57135, 3.968749999999992895 ) ;
#1258 = ORIENTED_EDGE ( 'NONE', *, *, #10802, .T. ) ;
#1259 = CARTESIAN_POINT ( 'NONE',  ( 111.0379167980823496, -47.01981040405703993, 17.85753003781598380 ) ) ;
#1260 = CARTESIAN_POINT ( 'NONE',  ( 109.3632651814324817, -25.89385771158341853, 180.9222919425779708 ) ) ;
#1261 = DIRECTION ( 'NONE',  ( -0.000000000000000000, -0.000000000000000000, -1.000000000000000000 ) ) ;
#1262 = LINE ( 'NONE', #28968, #50442 ) ;
#1263 = CARTESIAN_POINT ( 'NONE',  ( 117.5808906079046352, -33.32045621506634347, 130.0880062282919880 ) ) ;
#1264 = DIRECTION ( 'NONE',  ( -0.04216478779797398074, 0.9991106698809455455, 0.000000000000000000 ) ) ;
#1265 = ORIENTED_EDGE ( 'NONE', *, *, #51238, .T. ) ;
#1266 = CIRCLE ( 'NONE', #37574, 4.762500000000002842 ) ;
#1267 = DIRECTION ( 'NONE',  ( -1.000000000000000078E-15, 1.000000000000000083E-30, 1.000000000000000000 ) ) ;
#1268 = ORIENTED_EDGE ( 'NONE', *, *, #83334, .T. ) ;
#1269 = AXIS2_PLACEMENT_3D ( 'NONE', #52081, #59360, #60251 ) ;
#1270 = CARTESIAN_POINT ( 'NONE',  ( 100.8874142568969887, -44.70019346635132962, 133.0531993215868454 ) ) ;
#1271 = ORIENTED_EDGE ( 'NONE', *, *, #74088, .F. ) ;
#1272 = ORIENTED_EDGE ( 'NONE', *, *, #67656, .T. ) ;
#1273 = FACE_OUTER_BOUND ( 'NONE', #73997, .T. ) ;
#1274 = CARTESIAN_POINT ( 'NONE',  ( 173.9900000000000091, 20.32000000000000028, 71.37400000000000944 ) ) ;
#1275 = CARTESIAN_POINT ( 'NONE',  ( 95.25894796463062164, -35.71821259427313322, 36.25848241876794731 ) ) ;
#1276 = FACE_OUTER_BOUND ( 'NONE', #42259, .T. ) ;
#1277 = CARTESIAN_POINT ( 'NONE',  ( 192.5667039024473013, -23.42844715993434335, 249.9678068554149775 ) ) ;
#1278 = CARTESIAN_POINT ( 'NONE',  ( 109.6430121376341731, -46.48008673325654883, 73.78145860982388626 ) ) ;
#1279 = CARTESIAN_POINT ( 'NONE',  ( 110.1676348244934616, -46.62498374987622896, 52.80610146638697699 ) ) ;
#1281 = CARTESIAN_POINT ( 'NONE',  ( 102.0922439024871551, -27.59239485085799970, 141.4727681330539895 ) ) ;
#1280 = CARTESIAN_POINT ( 'NONE',  ( 37.03715912545347777, -48.62818131006128652, 129.9678068554150911 ) ) ;
#1282 = FACE_OUTER_BOUND ( 'NONE', #76067, .T. ) ;
#1283 = DIRECTION ( 'NONE',  ( -0.08544974978095701279, -0.9963424814100680926, 0.000000000000000000 ) ) ;
#1284 = EDGE_LOOP ( 'NONE', ( #79248, #45274, #6602, #1217 ) ) ;
#1285 = VECTOR ( 'NONE', #59340, 1000.000000000000000 ) ;
#1286 = DIRECTION ( 'NONE',  ( 0.8660254037844345998, 0.5000000000000069944, -1.550000000000018954E-14 ) ) ;
#1287 = PLANE ( 'NONE',  #62261 ) ;
#1288 = LINE ( 'NONE', #22190, #77551 ) ;
#1289 = ORIENTED_EDGE ( 'NONE', *, *, #60837, .T. ) ;
#1290 = ADVANCED_FACE ( 'NONE', ( #75283 ), #32583, .F. ) ;
#1291 = CYLINDRICAL_SURFACE ( 'NONE', #89725, 25.39999999999999858 ) ;
#1293 = ORIENTED_EDGE ( 'NONE', *, *, #65322, .F. ) ;
#1292 = CARTESIAN_POINT ( 'NONE',  ( 101.9629764938643035, -45.91127772325894085, 187.1727681330539781 ) ) ;
#1294 = LINE ( 'NONE', #23102, #82825 ) ;
#1295 = CARTESIAN_POINT ( 'NONE',  ( 96.65238424151439744, -35.53540495314400260, 202.2356252759109623 ) ) ;
#1296 = CARTESIAN_POINT ( 'NONE',  ( 101.7337754387761635, -26.99498644972499051, 96.46324432352997746 ) ) ;
#1297 = CARTESIAN_POINT ( 'NONE',  ( 119.5435152932140284, -31.57448135767196362, 293.6356252759107974 ) ) ;
#1298 = CARTESIAN_POINT ( 'NONE',  ( 107.0664832912739968, -36.72944715994100306, 287.6356252759109680 ) ) ;
#1299 = AXIS2_PLACEMENT_3D ( 'NONE', #44643, #72376, #1552 ) ;
#1300 = CARTESIAN_POINT ( 'NONE',  ( 141.3509999999999991, 0.000000000000000000, -141.3509999999999991 ) ) ;
#1301 = VERTEX_POINT ( 'NONE', #33039 ) ;
#1302 = EDGE_CURVE ( 'NONE', #71592, #61394, #60732, .T. ) ;
#1303 = EDGE_LOOP ( 'NONE', ( #77384, #63806 ) ) ;
#1304 = VERTEX_POINT ( 'NONE', #47095 ) ;
#1305 = VERTEX_POINT ( 'NONE', #40299 ) ;
#1306 = DIRECTION ( 'NONE',  ( 1.907762142705490052E-15, 7.167082501179359715E-16, -1.000000000000000000 ) ) ;
#1307 = CARTESIAN_POINT ( 'NONE',  ( 118.6539291974399219, -39.21253252500506647, 254.6584824187681022 ) ) ;
#1308 = LINE ( 'NONE', #36273, #19986 ) ;
#1309 = DIRECTION ( 'NONE',  ( 0.7759704746411385523, -0.6307692307692301936, 0.000000000000000000 ) ) ;
#1310 = ADVANCED_FACE ( 'NONE', ( #70258 ), #78437, .F. ) ;
#1311 = CIRCLE ( 'NONE', #81076, 3.700000000000001954 ) ;
#1313 = CARTESIAN_POINT ( 'NONE',  ( 86.06670390244796920, -58.35344715994099829, 10.91780685541479734 ) ) ;
#1312 = DIRECTION ( 'NONE',  ( 0.000000000000000000, 0.000000000000000000, -1.000000000000000000 ) ) ;
#1314 = DIRECTION ( 'NONE',  ( 0.000000000000000000, -0.7071067811865474617, -0.7071067811865474617 ) ) ;
#1315 = CARTESIAN_POINT ( 'NONE',  ( 115.9104104090373539, -31.16785412357883800, 34.27276813305396530 ) ) ;
#1316 = ORIENTED_EDGE ( 'NONE', *, *, #15848, .F. ) ;
#1317 = CIRCLE ( 'NONE', #82579, 0.5000000000000004441 ) ;
#1319 = ORIENTED_EDGE ( 'NONE', *, *, #57624, .F. ) ;
#1318 = VECTOR ( 'NONE', #65684, 1000.000000000000000 ) ;
#1320 = CARTESIAN_POINT ( 'NONE',  ( 97.07210785868812764, -35.37808982346257380, 17.22062569094285678 ) ) ;
#1321 = CARTESIAN_POINT ( 'NONE',  ( 104.7413546109693527, -27.22895552020974108, 281.2670538473389570 ) ) ;
#1322 = CARTESIAN_POINT ( 'NONE',  ( 181.5667039024459939, -18.82844715994031048, -5.074374724088000832 ) ) ;
#1323 = EDGE_CURVE ( 'NONE', #68582, #48583, #42528, .T. ) ;
#1324 = CIRCLE ( 'NONE', #86910, 2.999999999999919176 ) ;
#1325 = CARTESIAN_POINT ( 'NONE',  ( 102.6065612795740805, -27.36740250608086100, 136.4422919425769578 ) ) ;
#1327 = EDGE_CURVE ( 'NONE', #9843, #1981, #60064, .T. ) ;
#1326 = DIRECTION ( 'NONE',  ( -0.7071067811865487940, 0.000000000000000000, 0.7071067811865463515 ) ) ;
#1328 = EDGE_CURVE ( 'NONE', #38211, #27387, #71169, .T. ) ;
#1329 = AXIS2_PLACEMENT_3D ( 'NONE', #73383, #39311, #72509 ) ;
#1330 = CARTESIAN_POINT ( 'NONE',  ( 108.5946222506355952, -26.81343367791396659, 20.95493592026397778 ) ) ;
#1331 = ORIENTED_EDGE ( 'NONE', *, *, #52309, .T. ) ;
#1332 = FACE_BOUND ( 'NONE', #25903, .T. ) ;
#1333 = CARTESIAN_POINT ( 'NONE',  ( 134.0664832912740110, -8.729447159940999512, 2.408125275911999097 ) ) ;
#1334 = EDGE_CURVE ( 'NONE', #8126, #49439, #57738, .T. ) ;
#1335 = AXIS2_PLACEMENT_3D ( 'NONE', #83746, #42825, #63746 ) ;
#1336 = ORIENTED_EDGE ( 'NONE', *, *, #44690, .T. ) ;
#1337 = VERTEX_POINT ( 'NONE', #84803 ) ;
#1338 = CARTESIAN_POINT ( 'NONE',  ( -76.20774946062844890, 89.94786999841842601, 90.81826664112044512 ) ) ;
#1339 = CARTESIAN_POINT ( 'NONE',  ( 105.8471956337337190, -45.50678253122700312, 253.8987261630398677 ) ) ;
#1340 = DIRECTION ( 'NONE',  ( 0.000000000000000000, 0.000000000000000000, -1.000000000000000000 ) ) ;
#1341 = CARTESIAN_POINT ( 'NONE',  ( -117.8827734314469069, 84.21498941703525531, 12.61757617297219802 ) ) ;
#1342 = LINE ( 'NONE', #15426, #49019 ) ;
#1343 = CIRCLE ( 'NONE', #68054, 13.44999999999999396 ) ;
#1344 = CARTESIAN_POINT ( 'NONE',  ( 81.46681417397508085, 70.27900073646854651, -86.13269706310863683 ) ) ;
#1345 = VERTEX_POINT ( 'NONE', #4344 ) ;
#1346 = LINE ( 'NONE', #70381, #55192 ) ;
#1347 = FACE_OUTER_BOUND ( 'NONE', #6550, .T. ) ;
#1348 = ORIENTED_EDGE ( 'NONE', *, *, #46560, .F. ) ;
#1349 = CARTESIAN_POINT ( 'NONE',  ( 112.5143773164265184, -27.84083190490108706, 94.63848241876793566 ) ) ;
#1350 = ORIENTED_EDGE ( 'NONE', *, *, #34749, .F. ) ;
#1351 = CARTESIAN_POINT ( 'NONE',  ( 105.0857350373783561, -45.56626257478142605, 26.81146744712498275 ) ) ;
#1352 = CARTESIAN_POINT ( 'NONE',  ( 116.8165727570488741, -34.15080317556459732, 129.0313754411595824 ) ) ;
#1353 = CARTESIAN_POINT ( 'NONE',  ( 116.7860849611261500, -31.33117650353035799, 179.2299109901969700 ) ) ;
#1354 = CARTESIAN_POINT ( 'NONE',  ( 131.3179999999999836, 53.97500000000000142, 50.79999999999999716 ) ) ;
#1355 = CARTESIAN_POINT ( 'NONE',  ( 87.06648329127403940, -46.72944715994105280, -4.824374724089049771 ) ) ;
#1356 = FACE_BOUND ( 'NONE', #25770, .T. ) ;
#1357 = LINE ( 'NONE', #85388, #71182 ) ;
#1358 = VECTOR ( 'NONE', #26134, 1000.000000000000000 ) ;
#1359 = CARTESIAN_POINT ( 'NONE',  ( 116.1774319148507573, -31.53050193741562524, 285.2384824187680579 ) ) ;
#1360 = CARTESIAN_POINT ( 'NONE',  ( 110.4730404891439832, -46.15996163262695973, 117.8541770027330529 ) ) ;
#1361 = ORIENTED_EDGE ( 'NONE', *, *, #7930, .F. ) ;
#1362 = CARTESIAN_POINT ( 'NONE',  ( 136.7660003837311535, -37.25405382162939105, 6.823682607504132136 ) ) ;
#1363 = VERTEX_POINT ( 'NONE', #59288 ) ;
#1364 = CARTESIAN_POINT ( 'NONE',  ( 101.4776230940428832, -27.87746311998561666, 106.5241967044819944 ) ) ;
#1365 = CARTESIAN_POINT ( 'NONE',  ( 122.3663862029045504, 44.85577228901693303, -45.51497792402615516 ) ) ;
#1366 = VERTEX_POINT ( 'NONE', #25221 ) ;
#1367 = EDGE_LOOP ( 'NONE', ( #36346, #35082, #79316, #26677 ) ) ;
#1368 = EDGE_CURVE ( 'NONE', #40826, #8807, #66105, .T. ) ;
#1369 = ORIENTED_EDGE ( 'NONE', *, *, #61406, .F. ) ;
#1370 = CARTESIAN_POINT ( 'NONE',  ( 99.04406175382935373, -42.84125750402932908, 121.8439585956957103 ) ) ;
#1371 = LINE ( 'NONE', #6828, #59327 ) ;
#1372 = CARTESIAN_POINT ( 'NONE',  ( -186.2398777604655038, 20.32000000000000028, -6.349999999999999645 ) ) ;
#1373 = CARTESIAN_POINT ( 'NONE',  ( 179.1667039024476082, -26.71338133338671028, 193.9678068554150059 ) ) ;
#1374 = DIRECTION ( 'NONE',  ( 0.000000000000000000, 1.000000000000000000, 0.000000000000000000 ) ) ;
#1375 = CARTESIAN_POINT ( 'NONE',  ( 116.3364580279229301, -41.54664843801584340, 284.4441967044824082 ) ) ;
#1376 = DIRECTION ( 'NONE',  ( -1.000000000000000000, -2.756263715554006823E-15, 0.000000000000000000 ) ) ;
#1377 = ORIENTED_EDGE ( 'NONE', *, *, #75271, .F. ) ;
#1378 = FACE_OUTER_BOUND ( 'NONE', #72636, .T. ) ;
#1379 = CIRCLE ( 'NONE', #11547, 4.750000000000004441 ) ;
#1380 = DIRECTION ( 'NONE',  ( -0.7071067811865187069, -0.7071067811865764385, -7.071067811865181482E-16 ) ) ;
#1381 = EDGE_LOOP ( 'NONE', ( #14389, #45601, #45690, #35665 ) ) ;
#1382 = VERTEX_POINT ( 'NONE', #52449 ) ;
#1383 = CIRCLE ( 'NONE', #83926, 4.874999999999990230 ) ;
#1384 = VECTOR ( 'NONE', #24697, 1000.000000000000000 ) ;
#1385 = CARTESIAN_POINT ( 'NONE',  ( 161.4809174648183330, -48.32844715993547879, 300.4678068554149490 ) ) ;
#1386 = EDGE_CURVE ( 'NONE', #86177, #20936, #44319, .T. ) ;
#1387 = CARTESIAN_POINT ( 'NONE',  ( 106.5131950068454216, -24.24167068730766417, 320.8164078654934315 ) ) ;
#1388 = ADVANCED_FACE ( 'NONE', ( #30270 ), #32030, .F. ) ;
#1389 = DIRECTION ( 'NONE',  ( -2.170915417798913418E-16, 0.000000000000000000, -1.000000000000000000 ) ) ;
#1390 = DIRECTION ( 'NONE',  ( -0.02150753337723538411, -0.0009076677972193728959, -0.9997682742251812194 ) ) ;
#1391 = CARTESIAN_POINT ( 'NONE',  ( 100.6939357996894557, -31.04202505589751837, 190.1695626852199439 ) ) ;
#1392 = LINE ( 'NONE', #63611, #18562 ) ;
#1393 = CARTESIAN_POINT ( 'NONE',  ( 124.9987061611030299, 69.92834781287285750, 37.68974897191494478 ) ) ;
#1394 = CARTESIAN_POINT ( 'NONE',  ( 114.5992475275822784, -44.05128143045557465, 98.21276813305395592 ) ) ;
#1395 = VERTEX_POINT ( 'NONE', #51577 ) ;
#1396 = CARTESIAN_POINT ( 'NONE',  ( 71.24189083761808661, -0.9290567490904538817, 542.9756252759101471 ) ) ;
#1397 = ORIENTED_EDGE ( 'NONE', *, *, #20074, .T. ) ;
#1399 = EDGE_CURVE ( 'NONE', #84277, #89309, #85337, .T. ) ;
#1398 = AXIS2_PLACEMENT_3D ( 'NONE', #85405, #71315, #36783 ) ;
#1400 = AXIS2_PLACEMENT_3D ( 'NONE', #57244, #72240, #85883 ) ;
#1401 = CARTESIAN_POINT ( 'NONE',  ( 103.2832162603179285, -27.47272535187759956, 276.3852211716737202 ) ) ;
#1402 = ORIENTED_EDGE ( 'NONE', *, *, #53008, .T. ) ;
#1403 = EDGE_CURVE ( 'NONE', #64560, #10945, #72925, .T. ) ;
#1404 = EDGE_CURVE ( 'NONE', #77239, #78071, #17527, .T. ) ;
#1405 = CARTESIAN_POINT ( 'NONE',  ( 152.4532656103850172, -72.54314042502360849, 542.9756252759101471 ) ) ;
#1406 = ORIENTED_EDGE ( 'NONE', *, *, #28026, .F. ) ;
#1407 = CARTESIAN_POINT ( 'NONE',  ( 188.5667039024484950, -48.82844715993430640, 139.7178068554150059 ) ) ;
#1408 = CIRCLE ( 'NONE', #11581, 7.937500000000000000 ) ;
#1409 = CARTESIAN_POINT ( 'NONE',  ( 67.06670390244705970, -127.7048595798752899, 245.5588919304049682 ) ) ;
#1410 = EDGE_CURVE ( 'NONE', #78226, #87811, #22759, .T. ) ;
#1411 = CARTESIAN_POINT ( 'NONE',  ( 172.5664832912740110, -36.32844715994070839, 194.1756252759119832 ) ) ;
#1412 = ORIENTED_EDGE ( 'NONE', *, *, #75155, .T. ) ;
#1413 = CARTESIAN_POINT ( 'NONE',  ( 98.07775226919108036, -31.40506188283435307, 85.90133956162493689 ) ) ;
#1414 = EDGE_CURVE ( 'NONE', #50785, #8401, #18401, .T. ) ;
#1416 = CARTESIAN_POINT ( 'NONE',  ( 93.49502539975264881, 69.93364840292898066, -91.12742965730970468 ) ) ;
#1415 = CARTESIAN_POINT ( 'NONE',  ( 99.09538940105012728, -30.55084863300459475, 165.8023339492073944 ) ) ;
#1417 = CARTESIAN_POINT ( 'NONE',  ( 0.000000000000000000, 61.59999999999999432, 130.5560000000000116 ) ) ;
#1418 = CARTESIAN_POINT ( 'NONE',  ( 107.0664832912730020, -36.72944715994189835, 342.9256252759109884 ) ) ;
#1419 = ORIENTED_EDGE ( 'NONE', *, *, #29735, .F. ) ;
#1420 = ADVANCED_FACE ( 'NONE', ( #38399 ), #3890, .F. ) ;
#1421 = CARTESIAN_POINT ( 'NONE',  ( 131.3164832912739826, -36.72944715994100306, 14.92562527591099553 ) ) ;
#1422 = DIRECTION ( 'NONE',  ( 0.000000000000000000, 1.000000000000000000, 0.000000000000000000 ) ) ;
#1423 = EDGE_CURVE ( 'NONE', #44341, #74855, #9375, .T. ) ;
#1424 = CARTESIAN_POINT ( 'NONE',  ( 144.0667052733537901, -83.77844715994089597, 55.21780685541800437 ) ) ;
#1425 = CARTESIAN_POINT ( 'NONE',  ( 113.0894857754661587, -28.19359922731340262, 125.5870538473399591 ) ) ;
#1427 = CARTESIAN_POINT ( 'NONE',  ( 141.0667039024479834, -50.82844715994100682, 198.9178068554149945 ) ) ;
#1426 = DIRECTION ( 'NONE',  ( 0.000000000000000000, 0.000000000000000000, 1.000000000000000000 ) ) ;
#1428 = LINE ( 'NONE', #77732, #37903 ) ;
#1429 = VECTOR ( 'NONE', #18753, 1000.000000000000000 ) ;
#1430 = VERTEX_POINT ( 'NONE', #64784 ) ;
#1431 = CYLINDRICAL_SURFACE ( 'NONE', #27367, 3.000000000000002665 ) ;
#1432 = CARTESIAN_POINT ( 'NONE',  ( 116.5394839232219510, -34.29517225379352396, 120.0270538473389479 ) ) ;
#1434 = ORIENTED_EDGE ( 'NONE', *, *, #81091, .F. ) ;
#1433 = CARTESIAN_POINT ( 'NONE',  ( 270.8910000000000196, 40.03750000000000142, -2.032000000000000028 ) ) ;
#1435 = VECTOR ( 'NONE', #88705, 1000.000000000000227 ) ;
#1436 = EDGE_CURVE ( 'NONE', #65478, #55247, #52010, .T. ) ;
#1437 = CARTESIAN_POINT ( 'NONE',  ( 117.5198883501232103, -40.51604253736888950, 19.54991099019698453 ) ) ;
#1438 = FACE_OUTER_BOUND ( 'NONE', #32979, .T. ) ;
#1439 = DIRECTION ( 'NONE',  ( 0.000000000000000000, 0.000000000000000000, 1.000000000000000000 ) ) ;
#1441 = EDGE_CURVE ( 'NONE', #36268, #46468, #45639, .T. ) ;
#1440 = CARTESIAN_POINT ( 'NONE',  ( 151.0371591254572934, -24.42818131005592974, 300.4678068554149490 ) ) ;
#1442 = CARTESIAN_POINT ( 'NONE',  ( 151.0371591254575208, -24.42818131005592264, 180.4678068554149775 ) ) ;
#1443 = EDGE_CURVE ( 'NONE', #65895, #81510, #3004, .T. ) ;
#1444 = DIRECTION ( 'NONE',  ( -0.7071067811865634489, 0.7071067811865315855, -7.071067811865641980E-16 ) ) ;
#1445 = CARTESIAN_POINT ( 'NONE',  ( 183.5150000000000148, 36.86249999999999716, -53.61543552338530105 ) ) ;
#1446 = ADVANCED_FACE ( 'NONE', ( #51138, #11142 ), #86131, .T. ) ;
#1447 = CARTESIAN_POINT ( 'NONE',  ( 104.1325824198641499, -27.39908484284267587, 250.3184824187684683 ) ) ;
#1448 = ORIENTED_EDGE ( 'NONE', *, *, #36885, .F. ) ;
#1449 = ORIENTED_EDGE ( 'NONE', *, *, #60949, .F. ) ;
#1450 = CARTESIAN_POINT ( 'NONE',  ( 113.3955173535308063, -30.52198670013464010, 145.8758690201829609 ) ) ;
#1451 = AXIS2_PLACEMENT_3D ( 'NONE', #77132, #55746, #63036 ) ;
#1452 = CARTESIAN_POINT ( 'NONE',  ( 3.175000000000355094, 111.1250000000000000, -33.98325472291460159 ) ) ;
#1453 = CARTESIAN_POINT ( 'NONE',  ( 105.0114852080080254, -45.89751720821543302, 23.82063092494396273 ) ) ;
#1454 = CARTESIAN_POINT ( 'NONE',  ( -446.0240000000000009, 14.28749999999982201, 85.72499999999999432 ) ) ;
#1455 = CARTESIAN_POINT ( 'NONE',  ( 134.0664832912739826, -18.72944715994100306, -5.074374724089001809 ) ) ;
#1456 = VECTOR ( 'NONE', #84613, 1000.000000000000000 ) ;
#1457 = DIRECTION ( 'NONE',  ( 0.000000000000000000, 0.000000000000000000, 1.000000000000000000 ) ) ;
#1458 = DIRECTION ( 'NONE',  ( 1.000000000000000078E-15, 0.000000000000000000, -1.000000000000000000 ) ) ;
#1459 = FACE_OUTER_BOUND ( 'NONE', #4609, .T. ) ;
#1461 = CARTESIAN_POINT ( 'NONE',  ( 116.0363244534468805, -41.99923036749497385, 238.4041967044829562 ) ) ;
#1460 = AXIS2_PLACEMENT_3D ( 'NONE', #71793, #50434, #71357 ) ;
#1462 = CARTESIAN_POINT ( 'NONE',  ( -1.790903581468949841E-22, 95.14999999999999147, 118.3560000000000088 ) ) ;
#1463 = VERTEX_POINT ( 'NONE', #58402 ) ;
#1464 = ORIENTED_EDGE ( 'NONE', *, *, #37003, .T. ) ;
#1465 = DIRECTION ( 'NONE',  ( 0.000000000000000000, 0.000000000000000000, -1.000000000000000000 ) ) ;
#1466 = CARTESIAN_POINT ( 'NONE',  ( -83.54193218351851158, 95.25015226514365452, -84.12159398442685188 ) ) ;
#1467 = VECTOR ( 'NONE', #23210, 1000.000000000000000 ) ;
#1468 = CARTESIAN_POINT ( 'NONE',  ( 97.82696674394188108, -40.55455350847689289, 122.6383624784102722 ) ) ;
#1469 = DIRECTION ( 'NONE',  ( 0.000000000000000000, 0.000000000000000000, 1.000000000000000000 ) ) ;
#1470 = CARTESIAN_POINT ( 'NONE',  ( 106.6352542858682284, -26.36832623700844280, 36.09753003781596448 ) ) ;
#1471 = LINE ( 'NONE', #42765, #9304 ) ;
#1472 = VERTEX_POINT ( 'NONE', #66554 ) ;
#1473 = CARTESIAN_POINT ( 'NONE',  ( 110.2975601020867202, -46.68703778808450267, 8.827053847339950465 ) ) ;
#1474 = CARTESIAN_POINT ( 'NONE',  ( 61.56670390244634916, -23.42844715994023375, 180.4678068554151196 ) ) ;
#1475 = CARTESIAN_POINT ( 'NONE',  ( 97.61519122654028990, -41.12945951998310790, 256.6727681330537507 ) ) ;
#1476 = ORIENTED_EDGE ( 'NONE', *, *, #57990, .F. ) ;
#1477 = VECTOR ( 'NONE', #62930, 1000.000000000000000 ) ;
#1478 = CARTESIAN_POINT ( 'NONE',  ( 77.40528906089568295, -37.42303004212706696, 6.877070700249887203 ) ) ;
#1479 = CARTESIAN_POINT ( 'NONE',  ( 73.06670390244801183, -50.82844715994100682, 10.91780685541510110 ) ) ;
#1480 = FACE_OUTER_BOUND ( 'NONE', #2476, .T. ) ;
#1481 = CARTESIAN_POINT ( 'NONE',  ( 108.0475348069766284, -44.83298120013808585, 115.4909475124489830 ) ) ;
#1482 = CARTESIAN_POINT ( 'NONE',  ( 110.7038792373522824, -48.03394190404919328, 203.8241967044819489 ) ) ;
#1483 = CARTESIAN_POINT ( 'NONE',  ( 31.56670390244800828, -32.29483332968611364, -5.074374724088000832 ) ) ;
#1484 = VERTEX_POINT ( 'NONE', #23906 ) ;
#1485 = CARTESIAN_POINT ( 'NONE',  ( 130.3998166246070127, 12.92155284005802685, 349.2756252759110680 ) ) ;
#1486 = VECTOR ( 'NONE', #6356, 1000.000000000000000 ) ;
#1487 = ORIENTED_EDGE ( 'NONE', *, *, #80879, .F. ) ;
#1488 = ORIENTED_EDGE ( 'NONE', *, *, #52165, .T. ) ;
#1489 = CARTESIAN_POINT ( 'NONE',  ( 141.8664832912729992, -1.929447159941394263, 361.9756252759109998 ) ) ;
#1490 = EDGE_LOOP ( 'NONE', ( #21592, #40625, #23212, #44186 ) ) ;
#1491 = ORIENTED_EDGE ( 'NONE', *, *, #3137, .F. ) ;
#1492 = DIRECTION ( 'NONE',  ( 1.000000000000000000, 6.145690160522439356E-16, 0.000000000000000000 ) ) ;
#1493 = EDGE_CURVE ( 'NONE', #9584, #8177, #75540, .T. ) ;
#1494 = EDGE_CURVE ( 'NONE', #29444, #6827, #10263, .T. ) ;
#1495 = DIRECTION ( 'NONE',  ( -0.000000000000000000, 1.000000000000000000, -0.000000000000000000 ) ) ;
#1496 = CARTESIAN_POINT ( 'NONE',  ( 100.3410792892688761, -42.04179533522079026, 91.28099125664796532 ) ) ;
#1497 = CARTESIAN_POINT ( 'NONE',  ( 108.0161133123553725, -24.89170165127225332, 265.0127681330534415 ) ) ;
#1498 = EDGE_CURVE ( 'NONE', #17889, #3581, #82453, .T. ) ;
#1499 = CARTESIAN_POINT ( 'NONE',  ( -12.70000000000000107, 82.54999999999999716, 129.9368274816650910 ) ) ;
#1500 = CARTESIAN_POINT ( 'NONE',  ( 99.48898161933324502, -91.15344715994181968, -11.78219314458242550 ) ) ;
#1501 = ORIENTED_EDGE ( 'NONE', *, *, #74747, .T. ) ;
#1502 = AXIS2_PLACEMENT_3D ( 'NONE', #54107, #67766, #39599 ) ;
#1503 = EDGE_CURVE ( 'NONE', #25396, #23110, #20428, .T. ) ;
#1504 = ORIENTED_EDGE ( 'NONE', *, *, #70487, .F. ) ;
#1505 = DIRECTION ( 'NONE',  ( 0.000000000000000000, 1.000000000000000000, 0.000000000000000000 ) ) ;
#1506 = DIRECTION ( 'NONE',  ( -3.100000000000000258E-29, 3.100000000000000044E-14, 1.000000000000000000 ) ) ;
#1507 = CARTESIAN_POINT ( 'NONE',  ( 70.74156425739846554, -139.3372952672478675, 247.4251605867160890 ) ) ;
#1508 = VECTOR ( 'NONE', #40924, 1000.000000000000000 ) ;
#1509 = ADVANCED_FACE ( 'NONE', ( #61970, #32925 ), #67902, .T. ) ;
#1510 = CARTESIAN_POINT ( 'NONE',  ( 97.33998274022607688, -37.75834089694785689, 126.4099109901969626 ) ) ;
#1511 = CARTESIAN_POINT ( 'NONE',  ( 102.2821109723304431, -27.37735778705684098, 120.4527681330539792 ) ) ;
#1512 = CARTESIAN_POINT ( 'NONE',  ( 116.3563860081925725, -41.55700552044970664, 288.4441967044822945 ) ) ;
#1513 = ORIENTED_EDGE ( 'NONE', *, *, #16568, .T. ) ;
#1514 = CARTESIAN_POINT ( 'NONE',  ( 113.2201423986613520, -45.14488000985961946, 228.0784824187679760 ) ) ;
#1515 = CARTESIAN_POINT ( 'NONE',  ( 83.06670390244804025, -42.97311385574013798, 207.5838068554169809 ) ) ;
#1516 = DIRECTION ( 'NONE',  ( 0.000000000000000000, 0.000000000000000000, 1.000000000000000000 ) ) ;
#1517 = DIRECTION ( 'NONE',  ( 1.000000000000000078E-15, -1.000000000000000083E-30, -1.000000000000000000 ) ) ;
#1519 = CARTESIAN_POINT ( 'NONE',  ( 69.72411017813010403, 120.6499999999999915, -69.72411017812979139 ) ) ;
#1518 = LINE ( 'NONE', #42816, #49126 ) ;
#1520 = PLANE ( 'NONE',  #1780 ) ;
#1521 = CARTESIAN_POINT ( 'NONE',  ( 141.8545562996768012, -1.932463243632623229, 394.9756252759100903 ) ) ;
#1522 = CARTESIAN_POINT ( 'NONE',  ( 131.3881603334745307, -37.35482103167609580, 6.853567712192067951 ) ) ;
#1523 = CIRCLE ( 'NONE', #72707, 11.45913725231036118 ) ;
#1524 = DIRECTION ( 'NONE',  ( 0.000000000000000000, 0.000000000000000000, -1.000000000000000000 ) ) ;
#1525 = DIRECTION ( 'NONE',  ( -1.047445008332813989E-14, 0.000000000000000000, 1.000000000000000000 ) ) ;
#1526 = CARTESIAN_POINT ( 'NONE',  ( 107.0664832912739968, -36.72944715994100306, 287.6356252759109680 ) ) ;
#1527 = EDGE_CURVE ( 'NONE', #55604, #83594, #25669, .T. ) ;
#1529 = VERTEX_POINT ( 'NONE', #54239 ) ;
#1528 = LINE ( 'NONE', #63747, #61685 ) ;
#1530 = DIRECTION ( 'NONE',  ( -1.000000000000000000, 0.000000000000000000, 2.900000000000000265E-14 ) ) ;
#1531 = CARTESIAN_POINT ( 'NONE',  ( 100.8351866834200337, -45.15911532695984931, 257.0699109901966608 ) ) ;
#1532 = CARTESIAN_POINT ( 'NONE',  ( 102.6835365363430981, -27.27046913952221985, 176.4213395616249898 ) ) ;
#1533 = CARTESIAN_POINT ( 'NONE',  ( 100.4654578171049337, -27.83497312075872188, 31.59657765686396758 ) ) ;
#1534 =( GEOMETRIC_REPRESENTATION_CONTEXT ( 3 ) GLOBAL_UNCERTAINTY_ASSIGNED_CONTEXT ( ( #21509 ) ) GLOBAL_UNIT_ASSIGNED_CONTEXT ( ( #51859, #16479, #85981 ) ) REPRESENTATION_CONTEXT ( 'NONE', 'WORKASPACE' ) );
#1536 = CARTESIAN_POINT ( 'NONE',  ( 81.36335724984412821, -34.30134337669328914, 7.962481652686962619 ) ) ;
#1535 = DIRECTION ( 'NONE',  ( 0.000000000000000000, 1.000000000000000000, 0.000000000000000000 ) ) ;
#1537 = CARTESIAN_POINT ( 'NONE',  ( 97.92333446084529669, -40.78093374296712881, 137.6583996970876456 ) ) ;
#1538 = EDGE_CURVE ( 'NONE', #50564, #46362, #46531, .T. ) ;
#1539 = VERTEX_POINT ( 'NONE', #34271 ) ;
#1540 = FACE_OUTER_BOUND ( 'NONE', #74364, .T. ) ;
#1541 = ORIENTED_EDGE ( 'NONE', *, *, #69904, .T. ) ;
#1542 = VECTOR ( 'NONE', #76999, 1000.000000000000000 ) ;
#1543 = CARTESIAN_POINT ( 'NONE',  ( 115.6043783821399558, -39.74888713174190968, 177.9905150661719802 ) ) ;
#1545 = VERTEX_POINT ( 'NONE', #40641 ) ;
#1544 = CARTESIAN_POINT ( 'NONE',  ( -479.3614999999999782, 97.78694598552380057, 3.968750000000479616 ) ) ;
#1546 = AXIS2_PLACEMENT_3D ( 'NONE', #84659, #29240, #27879 ) ;
#1547 = DIRECTION ( 'NONE',  ( 0.000000000000000000, -1.000000000000000000, 0.000000000000000000 ) ) ;
#1548 = CARTESIAN_POINT ( 'NONE',  ( 102.0615167388205293, -46.55869598106821883, 168.2137205140059564 ) ) ;
#1549 = DIRECTION ( 'NONE',  ( 1.000000000000000078E-15, 0.000000000000000000, 1.000000000000000000 ) ) ;
#1550 = FACE_BOUND ( 'NONE', #55978, .T. ) ;
#1551 = CARTESIAN_POINT ( 'NONE',  ( 110.8974114899633463, -27.49234298998610271, 85.76376216369907013 ) ) ;
#1552 = DIRECTION ( 'NONE',  ( 1.000000000000000000, 0.000000000000000000, 0.000000000000000000 ) ) ;
#1553 = CARTESIAN_POINT ( 'NONE',  ( 97.82527667066705135, -40.55047884729894747, 96.63846944729883148 ) ) ;
#1554 = EDGE_CURVE ( 'NONE', #74158, #31761, #61083, .T. ) ;
#1555 = CARTESIAN_POINT ( 'NONE',  ( 96.76615086495793605, -37.93025403122317130, 86.43086337114897333 ) ) ;
#1556 = ORIENTED_EDGE ( 'NONE', *, *, #26606, .T. ) ;
#1557 = AXIS2_PLACEMENT_3D ( 'NONE', #77427, #56968, #20674 ) ;
#1558 = EDGE_LOOP ( 'NONE', ( #88400, #79193, #56424, #64076 ) ) ;
#1559 = CARTESIAN_POINT ( 'NONE',  ( 97.94737569220006890, -41.00876738043628222, 58.10729759161198160 ) ) ;
#1560 = DIRECTION ( 'NONE',  ( -1.000000000000000078E-15, -1.000000000000000083E-30, 1.000000000000000000 ) ) ;
#1562 = CARTESIAN_POINT ( 'NONE',  ( 100.8874679703711195, -44.70022144079540993, 37.05229195109952656 ) ) ;
#1561 = CARTESIAN_POINT ( 'NONE',  ( 98.96845470676157674, -30.25173782105014197, 191.7775300378149836 ) ) ;
#1563 = LINE ( 'NONE', #29264, #27555 ) ;
#1564 = CARTESIAN_POINT ( 'NONE',  ( 46.32460016641643108, -48.34074026909789268, 129.9678068554150911 ) ) ;
#1565 = DIRECTION ( 'NONE',  ( 0.000000000000000000, 0.000000000000000000, 1.000000000000000000 ) ) ;
#1566 = CARTESIAN_POINT ( 'NONE',  ( -100.8961411191535973, 127.0000000000000000, 3.968749999998880451 ) ) ;
#1567 = CARTESIAN_POINT ( 'NONE',  ( 67.64413875234457407, -68.43291640910719309, 246.8985623378813159 ) ) ;
#1568 = CARTESIAN_POINT ( 'NONE',  ( 108.3168256696638281, -47.05733704442519638, 117.6727681330539639 ) ) ;
#1569 = ORIENTED_EDGE ( 'NONE', *, *, #59201, .F. ) ;
#1570 = ORIENTED_EDGE ( 'NONE', *, *, #83036, .T. ) ;
#1571 = VERTEX_POINT ( 'NONE', #18861 ) ;
#1572 = CIRCLE ( 'NONE', #49391, 13.44999999999999396 ) ;
#1573 = ADVANCED_FACE ( 'NONE', ( #75171, #55136 ), #5237, .T. ) ;
#1574 =( LENGTH_UNIT ( ) NAMED_UNIT ( * ) SI_UNIT ( .MILLI., .METRE. ) );
#1575 = CARTESIAN_POINT ( 'NONE',  ( 51.24204729617298426, -31.76306994223730840, 237.4678068554150059 ) ) ;
#1576 = LINE ( 'NONE', #36087, #46456 ) ;
#1577 = CARTESIAN_POINT ( 'NONE',  ( -473.2019999999999982, 53.97500000000000142, -3.174999999999999822 ) ) ;
#1578 = CARTESIAN_POINT ( 'NONE',  ( 102.6495774910181780, -44.17201850306531696, 204.9804713219729706 ) ) ;
#1579 = VECTOR ( 'NONE', #24525, 1000.000000000000000 ) ;
#1580 = ADVANCED_FACE ( 'NONE', ( #61521 ), #47438, .T. ) ;
#1581 = PLANE ( 'NONE',  #53701 ) ;
#1582 = B_SPLINE_CURVE_WITH_KNOTS ( 'NONE', 3,
 ( #68511, #27613, #81707, #33969, #19908, #40789, #13541, #28053, #41225, #34870, #68955, #6278, #61672, #54394, #20805, #13988, #47590, #34421 ),
 .UNSPECIFIED., .F., .F.,
 ( 4, 2, 2, 2, 2, 2, 2, 2, 4 ),
 ( 0.5000000002310567293, 0.5625000002021746104, 0.6250000001732924915, 0.6875000001444104836, 0.7500000001155283647, 0.8125000000866462457, 0.8750000000577642378, 0.9375000000288821189, 1.000000000000000000 ),
 .UNSPECIFIED. ) ;
#1583 = CARTESIAN_POINT ( 'NONE',  ( 97.74620163809125017, -42.67179083687646823, 141.7661014663869707 ) ) ;
#1584 = CARTESIAN_POINT ( 'NONE',  ( 165.6738106836043585, -28.98061976758451053, 237.4678068554150059 ) ) ;
#1585 = ORIENTED_EDGE ( 'NONE', *, *, #13032, .F. ) ;
#1587 = ORIENTED_EDGE ( 'NONE', *, *, #52130, .F. ) ;
#1586 = VERTEX_POINT ( 'NONE', #81563 ) ;
#1588 = AXIS2_PLACEMENT_3D ( 'NONE', #9865, #37126, #79814 ) ;
#1589 = CARTESIAN_POINT ( 'NONE',  ( 28.57499999999999929, 87.13271776169258942, 310.8325000000000387 ) ) ;
#1590 = ORIENTED_EDGE ( 'NONE', *, *, #84891, .F. ) ;
#1591 = ORIENTED_EDGE ( 'NONE', *, *, #56835, .F. ) ;
#1592 = LINE ( 'NONE', #8403, #57970 ) ;
#1593 = LINE ( 'NONE', #33068, #83246 ) ;
#1594 = CARTESIAN_POINT ( 'NONE',  ( 98.31940232332729579, -40.15947632561638869, 243.0434880678019738 ) ) ;
#1595 = DIRECTION ( 'NONE',  ( -0.000000000000000000, -0.000000000000000000, -1.000000000000000000 ) ) ;
#1596 = ORIENTED_EDGE ( 'NONE', *, *, #78100, .F. ) ;
#1597 = CARTESIAN_POINT ( 'NONE',  ( 100.0187664783711483, -40.62989960760008046, 9.635625275910943088 ) ) ;
#1598 = DIRECTION ( 'NONE',  ( -4.299999999999999979E-14, 1.000000000000000000, -4.400000000000000367E-29 ) ) ;
#1599 = VERTEX_POINT ( 'NONE', #19312 ) ;
#1600 = ORIENTED_EDGE ( 'NONE', *, *, #21100, .T. ) ;
#1601 = DIRECTION ( 'NONE',  ( 1.000000000000000000, 0.000000000000000000, -0.000000000000000000 ) ) ;
#1602 = ORIENTED_EDGE ( 'NONE', *, *, #5397, .T. ) ;
#1603 = EDGE_LOOP ( 'NONE', ( #84238, #42439, #85968, #88448, #51749, #46852, #88301, #60459, #68291, #59099, #73730, #61079, #86150, #31030, #81684, #69215, #63173, #39550, #87001, #53196, #28094, #73403, #88949, #30386 ) ) ;
#1604 = EDGE_CURVE ( 'NONE', #27384, #82662, #81115, .T. ) ;
#1605 = EDGE_CURVE ( 'NONE', #72685, #51113, #82002, .T. ) ;
#1606 = VECTOR ( 'NONE', #41005, 1000.000000000000114 ) ;
#1607 = CARTESIAN_POINT ( 'NONE',  ( 115.7114656938015429, -36.32299383444259888, 266.6699951314962505 ) ) ;
#1608 = CARTESIAN_POINT ( 'NONE',  ( 117.5094658089964241, -40.42262428419060427, 178.5680062282919778 ) ) ;
#1609 = AXIS2_PLACEMENT_3D ( 'NONE', #15949, #58595, #43631 ) ;
#1610 = ADVANCED_FACE ( 'NONE', ( #39738 ), #81397, .T. ) ;
#1611 = CARTESIAN_POINT ( 'NONE',  ( 97.59110611908489830, -31.08311649095515250, 130.9108633711489915 ) ) ;
#1612 =( NAMED_UNIT ( * ) SI_UNIT ( $, .STERADIAN. ) SOLID_ANGLE_UNIT ( ) );
#1613 = CARTESIAN_POINT ( 'NONE',  ( 20.56670390244748603, -48.82844715994200158, 129.9678068554150627 ) ) ;
#1614 = CARTESIAN_POINT ( 'NONE',  ( 115.8552077933167794, -44.67884570232850194, 229.2413395616249545 ) ) ;
#1615 = DIRECTION ( 'NONE',  ( 1.000000000000000000, 4.299999999999999979E-14, 1.000000000000000078E-15 ) ) ;
#1616 = AXIS2_PLACEMENT_3D ( 'NONE', #45612, #38825, #79744 ) ;
#1617 = CARTESIAN_POINT ( 'NONE',  ( 1.224646799147354440E-15, 210.0000000000000000, 144.6557476874258441 ) ) ;
#1618 = VERTEX_POINT ( 'NONE', #88813 ) ;
#1619 = CARTESIAN_POINT ( 'NONE',  ( 164.5667039024479834, -50.82844715994100682, 10.91780685541479734 ) ) ;
#1620 = ORIENTED_EDGE ( 'NONE', *, *, #59322, .F. ) ;
#1621 = EDGE_CURVE ( 'NONE', #77970, #1241, #49387, .T. ) ;
#1622 = ORIENTED_EDGE ( 'NONE', *, *, #61664, .T. ) ;
#1623 = AXIS2_PLACEMENT_3D ( 'NONE', #46896, #47349, #54597 ) ;
#1624 = EDGE_CURVE ( 'NONE', #49936, #14756, #19759, .T. ) ;
#1625 = TOROIDAL_SURFACE ( 'NONE', #36441, 154.1697486074984909, 6.349999999999999645 ) ;
#1626 = CARTESIAN_POINT ( 'NONE',  ( 113.7136498174399577, -45.61921998050937077, 188.0994347997199725 ) ) ;
#1627 = VERTEX_POINT ( 'NONE', #6140 ) ;
#1628 = CARTESIAN_POINT ( 'NONE',  ( 102.3603858057123972, -46.03211757857948783, 127.2041967044829960 ) ) ;
#1629 = CARTESIAN_POINT ( 'NONE',  ( 97.81399847929220925, -40.51646572127298640, 256.6355814287313137 ) ) ;
#1630 = CARTESIAN_POINT ( 'NONE',  ( 135.9194882200285690, -34.69035895458431185, 7.660272404649855815 ) ) ;
#1631 = DIRECTION ( 'NONE',  ( 0.000000000000000000, 0.000000000000000000, -1.000000000000000000 ) ) ;
#1634 = CARTESIAN_POINT ( 'NONE',  ( 113.7851844261089695, -26.99768152489570738, 235.5956252759109759 ) ) ;
#1633 = CARTESIAN_POINT ( 'NONE',  ( -454.6936515812919879, 53.97500000000000142, -3.174999999999999822 ) ) ;
#1632 = CARTESIAN_POINT ( 'NONE',  ( 143.9834832912729894, -71.52944715994142655, 352.4506252759077825 ) ) ;
#1635 = CYLINDRICAL_SURFACE ( 'NONE', #36468, 12.70000000000000107 ) ;
#1637 = EDGE_CURVE ( 'NONE', #12195, #79540, #27020, .T. ) ;
#1636 = DIRECTION ( 'NONE',  ( -4.299999999999999979E-14, 1.000000000000000000, 0.000000000000000000 ) ) ;
#1638 = DIRECTION ( 'NONE',  ( -0.7071067811865475727, 0.7071067811865475727, 0.000000000000000000 ) ) ;
#1639 = CARTESIAN_POINT ( 'NONE',  ( 134.0664832912740110, -8.729447159940999512, 4.925625275911999168 ) ) ;
#1640 = CARTESIAN_POINT ( 'NONE',  ( 117.0608945241952483, -38.08045311458047877, 259.7189586097406391 ) ) ;
#1641 = CARTESIAN_POINT ( 'NONE',  ( 107.0664832912740394, -56.47944715994103149, -4.824374724089029343 ) ) ;
#1642 = AXIS2_PLACEMENT_3D ( 'NONE', #6574, #49231, #61972 ) ;
#1644 = ORIENTED_EDGE ( 'NONE', *, *, #23752, .F. ) ;
#1643 = CARTESIAN_POINT ( 'NONE',  ( 117.5355484441921163, -36.80252840376058288, 263.8213395616250523 ) ) ;
#1645 = PLANE ( 'NONE',  #8923 ) ;
#1646 = CARTESIAN_POINT ( 'NONE',  ( 99.08440026364779385, -45.52245356036965518, 156.9899109901969609 ) ) ;
#1647 = CARTESIAN_POINT ( 'NONE',  ( 97.35162482889903401, -32.85093483786611301, 37.02419670448292521 ) ) ;
#1648 = CARTESIAN_POINT ( 'NONE',  ( 117.3342495501102007, -34.51337161069084658, 179.9956252759109532 ) ) ;
#1649 = LINE ( 'NONE', #29349, #83719 ) ;
#1650 = CARTESIAN_POINT ( 'NONE',  ( 152.0368932755770857, -23.42844715993588522, 249.9678068554149490 ) ) ;
#1652 = DIRECTION ( 'NONE',  ( 0.000000000000000000, 0.000000000000000000, 1.000000000000000000 ) ) ;
#1651 = FACE_OUTER_BOUND ( 'NONE', #25600, .T. ) ;
#1653 = DIRECTION ( 'NONE',  ( 0.000000000000000000, 0.000000000000000000, 1.000000000000000000 ) ) ;
#1654 = LINE ( 'NONE', #56123, #5955 ) ;
#1655 = EDGE_LOOP ( 'NONE', ( #58719, #47475, #58604, #81433 ) ) ;
#1656 = AXIS2_PLACEMENT_3D ( 'NONE', #65732, #23978, #4421 ) ;
#1657 = DIRECTION ( 'NONE',  ( -0.7071067811865510144, 0.000000000000000000, 0.7071067811865441310 ) ) ;
#1658 = EDGE_LOOP ( 'NONE', ( #89720, #70654, #32040, #47006 ) ) ;
#1659 = ORIENTED_EDGE ( 'NONE', *, *, #58078, .F. ) ;
#1660 = CONICAL_SURFACE ( 'NONE', #16179, 9.571100913904340146, 0.7853981633974539411 ) ;
#1662 = ORIENTED_EDGE ( 'NONE', *, *, #34458, .T. ) ;
#1661 = CARTESIAN_POINT ( 'NONE',  ( 41.56648329127499153, -27.82844715994070484, 203.6756252759119832 ) ) ;
#1663 = CARTESIAN_POINT ( 'NONE',  ( 98.60777729073579678, -43.80857954853289016, 67.86895860924497015 ) ) ;
#1664 = DIRECTION ( 'NONE',  ( 0.000000000000000000, -1.000000000000000000, 0.000000000000000000 ) ) ;
#1665 = AXIS2_PLACEMENT_3D ( 'NONE', #30439, #29996, #84972 ) ;
#1666 = CARTESIAN_POINT ( 'NONE',  ( 71.24189083761808661, -0.9290567490904538817, 542.9756252759101471 ) ) ;
#1667 = CARTESIAN_POINT ( 'NONE',  ( 96.00793635059680753, -35.77758691827158799, 182.2461014663869889 ) ) ;
#1668 = EDGE_CURVE ( 'NONE', #27718, #55509, #54582, .T. ) ;
#1669 = CARTESIAN_POINT ( 'NONE',  ( 100.8732324256648951, -44.32512360075851632, 12.03276813305398463 ) ) ;
#1670 = VERTEX_POINT ( 'NONE', #2002 ) ;
#1671 = ORIENTED_EDGE ( 'NONE', *, *, #58217, .F. ) ;
#1672 = VERTEX_POINT ( 'NONE', #14747 ) ;
#1673 = DIRECTION ( 'NONE',  ( -1.000000000000000000, -1.541976423090496028E-15, 0.000000000000000000 ) ) ;
#1674 = FACE_OUTER_BOUND ( 'NONE', #5073, .T. ) ;
#1675 = DIRECTION ( 'NONE',  ( 4.299999999999999979E-14, -1.000000000000000000, 4.400000000000000367E-29 ) ) ;
#1676 = CARTESIAN_POINT ( 'NONE',  ( 98.60478223830740774, 127.0000000000000000, 3.859079674607175002E-13 ) ) ;
#1677 = CARTESIAN_POINT ( 'NONE',  ( 82.89895571708159139, 82.96445444011520465, 100.8594679592221155 ) ) ;
#1678 = DIRECTION ( 'NONE',  ( 0.5000000000000015543, 0.8660254037844377084, -2.688821387764056676E-14 ) ) ;
#1679 = PLANE ( 'NONE',  #16706 ) ;
#1680 = CARTESIAN_POINT ( 'NONE',  ( 130.3998166246059895, 12.92155284005730387, 358.9756252759109998 ) ) ;
#1681 = CARTESIAN_POINT ( 'NONE',  ( 117.4903696573864522, -37.28369426754697002, 18.78419670448294809 ) ) ;
#1682 = ORIENTED_EDGE ( 'NONE', *, *, #11573, .T. ) ;
#1683 = LINE ( 'NONE', #15759, #75101 ) ;
#1684 = VECTOR ( 'NONE', #64083, 1000.000000000000000 ) ;
#1685 = CARTESIAN_POINT ( 'NONE',  ( 76.20505178924339873, 120.6499999999999915, 76.20505178924419454 ) ) ;
#1686 = CARTESIAN_POINT ( 'NONE',  ( 98.42009728606723229, -37.10485906011713553, 114.1671379886389559 ) ) ;
#1687 = CIRCLE ( 'NONE', #19050, 10.04999999999999361 ) ;
#1688 = ADVANCED_FACE ( 'NONE', ( #70144 ), #28818, .F. ) ;
#1689 = CARTESIAN_POINT ( 'NONE',  ( 90.44969454456403923, -17.59493780205715652, 229.5838068554169809 ) ) ;
#1690 = CARTESIAN_POINT ( 'NONE',  ( 118.5256205435843526, -36.72944715994100306, 394.9756252759102040 ) ) ;
#1691 = ORIENTED_EDGE ( 'NONE', *, *, #2750, .F. ) ;
#1692 = ORIENTED_EDGE ( 'NONE', *, *, #42690, .T. ) ;
#1693 = CARTESIAN_POINT ( 'NONE',  ( 99.50491052054114505, -43.30599679329080942, 136.8954324092491959 ) ) ;
#1694 = ORIENTED_EDGE ( 'NONE', *, *, #55189, .F. ) ;
#1695 = ORIENTED_EDGE ( 'NONE', *, *, #73004, .F. ) ;
#1696 = CIRCLE ( 'NONE', #74241, 1.499999999999987788 ) ;
#1697 = CARTESIAN_POINT ( 'NONE',  ( 103.3528332358002331, -45.35993549251112711, 133.6968214011349403 ) ) ;
#1698 = CARTESIAN_POINT ( 'NONE',  ( 107.9678037105606450, -121.2545485715094316, -21.78219314458149114 ) ) ;
#1699 = CARTESIAN_POINT ( 'NONE',  ( 117.3602503114455402, -32.64000144215158628, 95.13943479972097350 ) ) ;
#1700 = AXIS2_PLACEMENT_3D ( 'NONE', #61047, #54207, #6539 ) ;
#1701 = CARTESIAN_POINT ( 'NONE',  ( 112.4304735641928374, -45.18349285385466629, 18.02636112242024424 ) ) ;
#1702 = ORIENTED_EDGE ( 'NONE', *, *, #76963, .T. ) ;
#1703 = ORIENTED_EDGE ( 'NONE', *, *, #9525, .T. ) ;
#1704 = VERTEX_POINT ( 'NONE', #84243 ) ;
#1705 = EDGE_CURVE ( 'NONE', #27930, #72137, #18994, .T. ) ;
#1706 = AXIS2_PLACEMENT_3D ( 'NONE', #3506, #72112, #31203 ) ;
#1707 = CARTESIAN_POINT ( 'NONE',  ( 98.28768183251310120, -28.73153112808589427, 80.73848241876795839 ) ) ;
#1708 = ORIENTED_EDGE ( 'NONE', *, *, #73968, .F. ) ;
#1709 = ADVANCED_FACE ( 'NONE', ( #34722 ), #56947, .F. ) ;
#1710 = CARTESIAN_POINT ( 'NONE',  ( 111.5675350091857325, -45.45035926415926752, 272.9556252759110180 ) ) ;
#1711 = CARTESIAN_POINT ( 'NONE',  ( 107.6557286256638264, -47.79009794008123890, 193.6308633711489620 ) ) ;
#1712 = DIRECTION ( 'NONE',  ( 0.000000000000000000, 0.000000000000000000, -1.000000000000000000 ) ) ;
#1713 = CARTESIAN_POINT ( 'NONE',  ( -37.97768777873315571, 53.97499999999997300, 70.36347694520327423 ) ) ;
#1714 = EDGE_CURVE ( 'NONE', #61133, #37103, #77865, .T. ) ;
#1715 = CARTESIAN_POINT ( 'NONE',  ( 98.20239980326637408, -43.33262854484335946, 107.8480062282919647 ) ) ;
#1716 = AXIS2_PLACEMENT_3D ( 'NONE', #66058, #16155, #51094 ) ;
#1717 = CARTESIAN_POINT ( 'NONE',  ( 107.0664832912739968, -36.72944715994100306, 287.6356252759109680 ) ) ;
#1718 = ORIENTED_EDGE ( 'NONE', *, *, #34498, .F. ) ;
#1719 = DIRECTION ( 'NONE',  ( -0.7071067811865765496, 0.7071067811865185959, -7.071067811865773128E-16 ) ) ;
#1720 = EDGE_CURVE ( 'NONE', #34717, #38575, #50130, .T. ) ;
#1721 = EDGE_LOOP ( 'NONE', ( #9907, #28709, #20435, #18619 ) ) ;
#1722 = CARTESIAN_POINT ( 'NONE',  ( 66.95718368952854860, -124.7784471599409954, 55.21780685541800437 ) ) ;
#1723 = ORIENTED_EDGE ( 'NONE', *, *, #20357, .T. ) ;
#1724 = ORIENTED_EDGE ( 'NONE', *, *, #1621, .T. ) ;
#1725 = DIRECTION ( 'NONE',  ( -3.491483361109380094E-15, 0.000000000000000000, 1.000000000000000000 ) ) ;
#1726 = CARTESIAN_POINT ( 'NONE',  ( 79.06648329127300201, -36.72944715994189835, 361.9756252759109998 ) ) ;
#1727 = CARTESIAN_POINT ( 'NONE',  ( 115.8917813183058740, -31.17956921574393903, 34.27276813305396530 ) ) ;
#1728 = CARTESIAN_POINT ( 'NONE',  ( 5.483693934069210130, 69.93014865207605624, 37.70952975325106848 ) ) ;
#1729 = CARTESIAN_POINT ( 'NONE',  ( -546.0365000000000464, 53.97500000000000142, 14.22400000000000020 ) ) ;
#1730 = DIRECTION ( 'NONE',  ( 0.000000000000000000, -1.000000000000000000, 0.000000000000000000 ) ) ;
#1731 = CARTESIAN_POINT ( 'NONE',  ( 112.3909220325769667, -27.83061929752856400, 54.65943479972096242 ) ) ;
#1733 = CARTESIAN_POINT ( 'NONE',  ( 99.43809884604152671, -27.69271567064635065, 146.6356252759109395 ) ) ;
#1732 = DIRECTION ( 'NONE',  ( -0.000000000000000000, 1.000000000000000000, -0.000000000000000000 ) ) ;
#1734 = FACE_BOUND ( 'NONE', #62684, .T. ) ;
#1736 = EDGE_CURVE ( 'NONE', #19136, #23399, #48323, .T. ) ;
#1735 = DIRECTION ( 'NONE',  ( 0.000000000000000000, 0.000000000000000000, -1.000000000000000000 ) ) ;
#1737 = ORIENTED_EDGE ( 'NONE', *, *, #19258, .F. ) ;
#1738 = DIRECTION ( 'NONE',  ( 1.000000000000000078E-15, -1.000000000000000000, 0.000000000000000000 ) ) ;
#1739 = AXIS2_PLACEMENT_3D ( 'NONE', #45180, #80628, #79299 ) ;
#1740 = DIRECTION ( 'NONE',  ( 0.000000000000000000, 0.000000000000000000, 1.000000000000000000 ) ) ;
#1741 = CARTESIAN_POINT ( 'NONE',  ( 110.0667047667142953, -67.87844715994094713, 115.9678068554179902 ) ) ;
#1742 = VERTEX_POINT ( 'NONE', #13838 ) ;
#1743 = CYLINDRICAL_SURFACE ( 'NONE', #8533, 2.500000000000002220 ) ;
#1745 = VERTEX_POINT ( 'NONE', #41521 ) ;
#1744 = CARTESIAN_POINT ( 'NONE',  ( 113.6419851944692425, -45.67235822675655754, 183.0689586092439640 ) ) ;
#1746 = DIRECTION ( 'NONE',  ( 1.000000000000000000, 0.000000000000000000, 9.462128050782575008E-16 ) ) ;
#1747 = CARTESIAN_POINT ( 'NONE',  ( 116.5464386332369600, -41.20266105201044127, 224.4756252759109714 ) ) ;
#1748 = CARTESIAN_POINT ( 'NONE',  ( 96.04171114508396556, -38.01470880000633201, 82.43086337114895912 ) ) ;
#1749 = CARTESIAN_POINT ( 'NONE',  ( 115.0921083526524313, -30.62179339271783007, 250.3457344079624818 ) ) ;
#1750 = AXIS2_PLACEMENT_3D ( 'NONE', #28533, #56229, #83979 ) ;
#1751 = CARTESIAN_POINT ( 'NONE',  ( -7.205548786489490269E-13, 101.5999999999999943, 103.1875000000000000 ) ) ;
#1752 = FACE_OUTER_BOUND ( 'NONE', #52042, .T. ) ;
#1753 = ORIENTED_EDGE ( 'NONE', *, *, #85215, .T. ) ;
#1754 = AXIS2_PLACEMENT_3D ( 'NONE', #6182, #33870, #20258 ) ;
#1755 = ORIENTED_EDGE ( 'NONE', *, *, #60357, .T. ) ;
#1756 = ORIENTED_EDGE ( 'NONE', *, *, #68896, .F. ) ;
#1757 = VERTEX_POINT ( 'NONE', #62426 ) ;
#1758 = LINE ( 'NONE', #63982, #48154 ) ;
#1759 = CARTESIAN_POINT ( 'NONE',  ( 100.6563598938200812, -44.95093154396422364, 228.0499109901969348 ) ) ;
#1760 = CARTESIAN_POINT ( 'NONE',  ( 142.8821648370248170, -72.54478064608022692, 542.9756252759101471 ) ) ;
#1761 = DIRECTION ( 'NONE',  ( 1.000000000000000000, 0.000000000000000000, 0.000000000000000000 ) ) ;
#1762 = AXIS2_PLACEMENT_3D ( 'NONE', #40307, #88483, #18978 ) ;
#1764 = CARTESIAN_POINT ( 'NONE',  ( 90.65754775987920766, 74.81620433377381119, 76.39898589339244950 ) ) ;
#1763 = CARTESIAN_POINT ( 'NONE',  ( 192.5667039024474434, -23.42844715993433624, 180.4678068554150343 ) ) ;
#1765 = PLANE ( 'NONE',  #84930 ) ;
#1766 = ADVANCED_FACE ( 'NONE', ( #83332 ), #76511, .F. ) ;
#1767 = CARTESIAN_POINT ( 'NONE',  ( 102.7461184130007581, -25.66741906146929253, 20.37276813305294354 ) ) ;
#1768 = VERTEX_POINT ( 'NONE', #64231 ) ;
#1769 = CIRCLE ( 'NONE', #75679, 2.999999999999988898 ) ;
#1770 = VERTEX_POINT ( 'NONE', #49230 ) ;
#1771 = ORIENTED_EDGE ( 'NONE', *, *, #45505, .T. ) ;
#1772 = AXIS2_PLACEMENT_3D ( 'NONE', #8531, #21718, #42565 ) ;
#1773 = DIRECTION ( 'NONE',  ( 1.000000000000000000, 8.673617379883546378E-16, 9.757819552368989676E-16 ) ) ;
#1774 = CARTESIAN_POINT ( 'NONE',  ( 105.7995771162975416, -24.27178701759104840, 322.4846826458744431 ) ) ;
#1775 = EDGE_CURVE ( 'NONE', #14287, #13459, #35615, .T. ) ;
#1776 = CARTESIAN_POINT ( 'NONE',  ( 117.4208826025846690, -36.15918394849474282, 269.8822919425771829 ) ) ;
#1777 = VECTOR ( 'NONE', #19377, 1000.000000000000000 ) ;
#1778 = PLANE ( 'NONE',  #32775 ) ;
#1779 = CARTESIAN_POINT ( 'NONE',  ( 116.9564367646782728, -33.61053620760072391, 125.0575300378159795 ) ) ;
#1780 = AXIS2_PLACEMENT_3D ( 'NONE', #14699, #63285, #70099 ) ;
#1781 = DIRECTION ( 'NONE',  ( -1.000000000000000000, 0.000000000000000000, 0.000000000000000000 ) ) ;
#1782 = ORIENTED_EDGE ( 'NONE', *, *, #57519, .F. ) ;
#1783 = CARTESIAN_POINT ( 'NONE',  ( 74.19170390244700286, -80.65344715994098124, 45.21780685541799727 ) ) ;
#1784 = CARTESIAN_POINT ( 'NONE',  ( 97.60787293175452817, -39.98237518918260491, 57.59005031470000091 ) ) ;
#1786 = ORIENTED_EDGE ( 'NONE', *, *, #238, .F. ) ;
#1785 = B_SPLINE_CURVE_WITH_KNOTS ( 'NONE', 3,
 ( #11511, #25577, #26926, #53253, #18768, #82360, #20122, #74184, #53704, #60994, #81470, #40095, #47796, #26478, #40993, #68714, #87369, #81910, #25130, #62779, #77774, #14654, #7382, #50036, #56406 ),
 .UNSPECIFIED., .F., .F.,
 ( 4, 2, 2, 2, 2, 2, 2, 2, 2, 1, 2, 2, 4 ),
 ( 0.000000000000000000, 0.002464400387950989747, 0.003696600581926483536, 0.004928800775901976891, 0.007393201163853002633, 0.008625401357828533719, 0.009857601551804066539, 0.01232200193975515994, 0.01355420213373072051, 0.01478640232770627762, 0.01601860252168183646, 0.01725080271565739357, 0.01971520310360850431 ),
 .UNSPECIFIED. ) ;
#1787 = ORIENTED_EDGE ( 'NONE', *, *, #17427, .F. ) ;
#1788 = CARTESIAN_POINT ( 'NONE',  ( -83.24211534968669923, 95.24969287062863543, 84.42134122279109931 ) ) ;
#1789 = CARTESIAN_POINT ( 'NONE',  ( 115.9514134386872826, -36.57345012324869060, 285.2730118773255867 ) ) ;
#1790 = ADVANCED_FACE ( 'NONE', ( #15185 ), #15640, .F. ) ;
#1791 = DIRECTION ( 'NONE',  ( 0.000000000000000000, -1.000000000000000000, 0.000000000000000000 ) ) ;
#1792 = DIRECTION ( 'NONE',  ( 1.000000000000000078E-15, 1.000000000000000083E-30, -1.000000000000000000 ) ) ;
#1793 = CARTESIAN_POINT ( 'NONE',  ( 116.3186249068845939, -32.94868901192853627, 254.1356252759109395 ) ) ;
#1794 = VERTEX_POINT ( 'NONE', #76962 ) ;
#1795 = CARTESIAN_POINT ( 'NONE',  ( 29.56648329127400388, 15.62155284005900491, 328.6381252759109088 ) ) ;
#1796 = CARTESIAN_POINT ( 'NONE',  ( 152.0371591254582881, -47.82818131005588214, 300.4678068554149490 ) ) ;
#1797 = CIRCLE ( 'NONE', #52519, 2.517500000000005844 ) ;
#1798 = ORIENTED_EDGE ( 'NONE', *, *, #78237, .T. ) ;
#1799 = CARTESIAN_POINT ( 'NONE',  ( 97.22546204445637841, -31.69621874537715556, 95.96229194257799122 ) ) ;
#1800 = ORIENTED_EDGE ( 'NONE', *, *, #20414, .T. ) ;
#1801 = CARTESIAN_POINT ( 'NONE',  ( 110.6296508234850222, -44.49217663217273611, 27.34099125664796048 ) ) ;
#1802 = EDGE_CURVE ( 'NONE', #74993, #84792, #81200, .T. ) ;
#1803 = CARTESIAN_POINT ( 'NONE',  ( 99.04451456929375297, -42.84186625629031653, 126.8437268382981387 ) ) ;
#1804 = CARTESIAN_POINT ( 'NONE',  ( 97.98063455390165188, -41.72806076336413383, 176.7146728949589658 ) ) ;
#1805 = LINE ( 'NONE', #30840, #53471 ) ;
#1806 = DIRECTION ( 'NONE',  ( 1.000000000000000000, 0.000000000000000000, 0.000000000000000000 ) ) ;
#1807 = CARTESIAN_POINT ( 'NONE',  ( 116.3212776292296127, -32.94146857471318413, 287.6356252759109680 ) ) ;
#1808 = AXIS2_PLACEMENT_3D ( 'NONE', #24429, #39384, #67089 ) ;
#1809 = CARTESIAN_POINT ( 'NONE',  ( 68.91673588226457525, -69.56165432392101877, 247.5002287295815790 ) ) ;
#1810 = CARTESIAN_POINT ( 'NONE',  ( 116.3557873595856336, -41.55669258580370951, 284.4441967044824082 ) ) ;
#1811 = CARTESIAN_POINT ( 'NONE',  ( 106.4460240858017528, -46.73159911271572753, 117.5290179274728075 ) ) ;
#1812 = ORIENTED_EDGE ( 'NONE', *, *, #43102, .T. ) ;
#1813 = CARTESIAN_POINT ( 'NONE',  ( 72.96458098368701428, 101.5999999999999943, -78.00648098368678518 ) ) ;
#1814 = VERTEX_POINT ( 'NONE', #8372 ) ;
#1815 = CARTESIAN_POINT ( 'NONE',  ( 117.7233698349432132, -39.83239211553974712, 134.5889586092439743 ) ) ;
#1816 = PLANE ( 'NONE',  #74416 ) ;
#1817 = ORIENTED_EDGE ( 'NONE', *, *, #32049, .F. ) ;
#1818 = ORIENTED_EDGE ( 'NONE', *, *, #12913, .F. ) ;
#1819 = EDGE_LOOP ( 'NONE', ( #40428, #80947 ) ) ;
#1820 = B_SPLINE_CURVE_WITH_KNOTS ( 'NONE', 3,
 ( #34572, #20518, #75917, #13685, #69105 ),
 .UNSPECIFIED., .F., .F.,
 ( 4, 1, 4 ),
 ( 0.000000000000000000, 0.4316414630428307975, 1.000000000000000000 ),
 .UNSPECIFIED. ) ;
#1821 = CARTESIAN_POINT ( 'NONE',  ( 21.03715912545824551, -47.82818131006186491, 300.4678068554150059 ) ) ;
#1822 = DIRECTION ( 'NONE',  ( -0.000000000000000000, 1.000000000000000000, -0.000000000000000000 ) ) ;
#1823 = CARTESIAN_POINT ( 'NONE',  ( 0.000000000000000000, 223.9999999999999716, 154.6557476874258441 ) ) ;
#1824 = FACE_OUTER_BOUND ( 'NONE', #7569, .T. ) ;
#1825 = DIRECTION ( 'NONE',  ( 0.000000000000000000, 0.000000000000000000, 1.000000000000000000 ) ) ;
#1826 = EDGE_CURVE ( 'NONE', #68103, #39224, #1563, .T. ) ;
#1827 = CARTESIAN_POINT ( 'NONE',  ( 106.6068465219953794, -25.68577410589699994, 36.09753003781596448 ) ) ;
#1828 = AXIS2_PLACEMENT_3D ( 'NONE', #54145, #81016, #19216 ) ;
#1829 = DIRECTION ( 'NONE',  ( 0.000000000000000000, 0.8660254037844383745, -0.5000000000000003331 ) ) ;
#1830 = VERTEX_POINT ( 'NONE', #17415 ) ;
#1831 = CARTESIAN_POINT ( 'NONE',  ( 11.02121562796429899, 76.18511308578193564, 118.0435185069309227 ) ) ;
#1832 = CARTESIAN_POINT ( 'NONE',  ( 32.25690895537100289, -33.54226604285010893, -5.074374724088000832 ) ) ;
#1833 = EDGE_LOOP ( 'NONE', ( #81821, #34815, #69385, #52376 ) ) ;
#1834 = ORIENTED_EDGE ( 'NONE', *, *, #34415, .T. ) ;
#1835 = AXIS2_PLACEMENT_3D ( 'NONE', #87398, #74220, #60113 ) ;
#1836 = CARTESIAN_POINT ( 'NONE',  ( 80.06648329127399677, -21.47944715994105991, 1.625625275910943746 ) ) ;
#1837 = DIRECTION ( 'NONE',  ( -0.7071067811874389708, 0.7071067811856560636, 0.000000000000000000 ) ) ;
#1838 = CARTESIAN_POINT ( 'NONE',  ( 162.5667039024470171, -32.29483332968611364, -5.074374724088000832 ) ) ;
#1839 = DIRECTION ( 'NONE',  ( 0.000000000000000000, 0.000000000000000000, 1.000000000000000000 ) ) ;
#1840 = DIRECTION ( 'NONE',  ( -1.000000000000000000, -2.756263715554006823E-15, 0.000000000000000000 ) ) ;
#1841 = CARTESIAN_POINT ( 'NONE',  ( 103.9834678596679538, -28.76382429851063449, 214.7924198280769872 ) ) ;
#1843 = DIRECTION ( 'NONE',  ( -4.237773401492740281E-14, 1.000000000000000000, 0.000000000000000000 ) ) ;
#1842 = AXIS2_PLACEMENT_3D ( 'NONE', #41040, #67400, #66965 ) ;
#1844 = CARTESIAN_POINT ( 'NONE',  ( 123.4547429832808945, 72.86362559908033631, 42.47335031276299588 ) ) ;
#1845 = CARTESIAN_POINT ( 'NONE',  ( 104.2019728789896078, -25.17854340234507760, 90.26991099019693365 ) ) ;
#1846 = ORIENTED_EDGE ( 'NONE', *, *, #60116, .T. ) ;
#1848 = ADVANCED_FACE ( 'NONE', ( #30598 ), #44655, .F. ) ;
#1847 = CYLINDRICAL_SURFACE ( 'NONE', #68361, 0.4999999999999976685 ) ;
#1849 = EDGE_LOOP ( 'NONE', ( #88194, #34939, #52622, #61995 ) ) ;
#1850 = CARTESIAN_POINT ( 'NONE',  ( 72.96458098368701428, 117.4749999999999943, -65.02708098368670164 ) ) ;
#1851 = EDGE_CURVE ( 'NONE', #85229, #66416, #26062, .T. ) ;
#1852 = LINE ( 'NONE', #29548, #70283 ) ;
#1853 = ORIENTED_EDGE ( 'NONE', *, *, #7488, .F. ) ;
#1854 = DIRECTION ( 'NONE',  ( 0.5477458065102255302, 0.7071067811865671127, 0.4471851198893302959 ) ) ;
#1855 = ORIENTED_EDGE ( 'NONE', *, *, #32760, .T. ) ;
#1856 = CARTESIAN_POINT ( 'NONE',  ( -103.1875000000000000, 127.0000000000000000, -1.080832317973422076E-12 ) ) ;
#1857 = CARTESIAN_POINT ( 'NONE',  ( 67.36714851195648635, -67.87168324244640871, 246.8533852577239998 ) ) ;
#1858 = DIRECTION ( 'NONE',  ( 1.000000000000000078E-15, 0.000000000000000000, -1.000000000000000000 ) ) ;
#1859 = EDGE_LOOP ( 'NONE', ( #80684, #22830, #9417, #17174 ) ) ;
#1860 = CARTESIAN_POINT ( 'NONE',  ( 106.8407094991504209, -48.60307516909384873, 77.56133956162491927 ) ) ;
#1861 = CARTESIAN_POINT ( 'NONE',  ( 97.75839927879950153, -40.38492254185889863, 166.6242597985468308 ) ) ;
#1862 = LINE ( 'NONE', #43169, #22040 ) ;
#1863 = CARTESIAN_POINT ( 'NONE',  ( -11.65426927613973085, 77.70835675146533106, 117.7811321253428787 ) ) ;
#1864 = VERTEX_POINT ( 'NONE', #16088 ) ;
#1865 = AXIS2_PLACEMENT_3D ( 'NONE', #58280, #51884, #79640 ) ;
#1866 = CARTESIAN_POINT ( 'NONE',  ( 172.5664832912740110, -36.32844715994070839, 23.67562527591200094 ) ) ;
#1867 = CARTESIAN_POINT ( 'NONE',  ( -454.6936515812919879, 53.97500000000000142, 3.174999999999999822 ) ) ;
#1868 = CARTESIAN_POINT ( 'NONE',  ( 219.9639999999999986, 40.03750000000000142, -58.73749999999999716 ) ) ;
#1869 = CARTESIAN_POINT ( 'NONE',  ( 106.0743987232105212, -48.56321320874933889, 108.5099109901969712 ) ) ;
#1871 = DIRECTION ( 'NONE',  ( -0.7071067811865192621, -0.7071067811865758834, -7.071067811865186413E-16 ) ) ;
#1870 = DIRECTION ( 'NONE',  ( 1.000000000000000078E-15, -1.000000000000000083E-30, -1.000000000000000000 ) ) ;
#1872 = FACE_BOUND ( 'NONE', #82136, .T. ) ;
#1873 = VECTOR ( 'NONE', #29964, 1000.000000000000000 ) ;
#1874 = ORIENTED_EDGE ( 'NONE', *, *, #12701, .T. ) ;
#1875 = DIRECTION ( 'NONE',  ( 0.000000000000000000, 1.000000000000000000, 0.000000000000000000 ) ) ;
#1876 = CARTESIAN_POINT ( 'NONE',  ( 98.02110346605356028, -41.80092515478911963, 177.7451490854339795 ) ) ;
#1878 = ORIENTED_EDGE ( 'NONE', *, *, #63667, .T. ) ;
#1877 = FACE_OUTER_BOUND ( 'NONE', #3764, .T. ) ;
#1879 = CARTESIAN_POINT ( 'NONE',  ( 110.8002664325828164, -46.40403567634503901, 13.85753003781498016 ) ) ;
#1880 = CARTESIAN_POINT ( 'NONE',  ( 94.06648329127393993, -36.72944715994095333, 294.6356252759106837 ) ) ;
#1881 = FACE_OUTER_BOUND ( 'NONE', #1933, .T. ) ;
#1882 = CARTESIAN_POINT ( 'NONE',  ( 163.5667039024460223, -18.82844715994111340, -5.074374724088000832 ) ) ;
#1883 = LINE ( 'NONE', #28686, #81939 ) ;
#1884 = DIRECTION ( 'NONE',  ( -0.000000000000000000, 1.000000000000000000, 0.000000000000000000 ) ) ;
#1885 = CARTESIAN_POINT ( 'NONE',  ( 118.0655259830059265, -38.35211242607485360, 223.7099109901979546 ) ) ;
#1886 = VERTEX_POINT ( 'NONE', #45098 ) ;
#1887 = ORIENTED_EDGE ( 'NONE', *, *, #8187, .T. ) ;
#1888 = CARTESIAN_POINT ( 'NONE',  ( 115.7036244402283529, -40.42759782077664710, 209.9482499725639855 ) ) ;
#1889 = CONICAL_SURFACE ( 'NONE', #88912, 1.258750000000002922, 1.029744258676650093 ) ;
#1890 = DIRECTION ( 'NONE',  ( -2.108538789381372925E-16, 0.5150380749100580413, 0.8571673007021100021 ) ) ;
#1891 = EDGE_CURVE ( 'NONE', #43116, #66809, #65233, .T. ) ;
#1892 = CARTESIAN_POINT ( 'NONE',  ( 116.2961902049681697, -40.76469377450285947, 54.93015473446794061 ) ) ;
#1893 = CARTESIAN_POINT ( 'NONE',  ( 23.08731596616043191, 87.15077889410697765, 301.6545639882101000 ) ) ;
#1894 = VECTOR ( 'NONE', #46363, 1000.000000000000000 ) ;
#1895 = AXIS2_PLACEMENT_3D ( 'NONE', #16774, #79005, #44455 ) ;
#1896 = CARTESIAN_POINT ( 'NONE',  ( 29.56670390244857316, -48.82844715994099971, 300.4678068554149490 ) ) ;
#1897 = ADVANCED_FACE ( 'NONE', ( #72386, #45530 ), #51033, .F. ) ;
#1898 = CARTESIAN_POINT ( 'NONE',  ( 160.7738106836351051, -48.62134037874900372, 129.9678068554149775 ) ) ;
#1899 = CARTESIAN_POINT ( 'NONE',  ( 194.5667039024479834, -67.87844715994100397, 300.9178068554150514 ) ) ;
#1900 = CARTESIAN_POINT ( 'NONE',  ( 135.2444258376725941, 20.32000000000000028, 147.4575741623265799 ) ) ;
#1901 = CARTESIAN_POINT ( 'NONE',  ( 96.83034234600413015, -40.83861266248845823, 251.6422919425777138 ) ) ;
#1902 = CARTESIAN_POINT ( 'NONE',  ( 11.95695845665503043, 86.60868480869159214, 117.7509010089503363 ) ) ;
#1903 = ORIENTED_EDGE ( 'NONE', *, *, #34266, .T. ) ;
#1904 = PRODUCT ( 'Hydraulic Index Locking Pin', 'Hydraulic Index Locking Pin', '', ( #18150 ) ) ;
#1905 = ORIENTED_EDGE ( 'NONE', *, *, #30326, .F. ) ;
#1906 = EDGE_CURVE ( 'NONE', #78790, #42810, #62296, .T. ) ;
#1907 = EDGE_CURVE ( 'NONE', #41462, #11071, #64672, .T. ) ;
#1908 = CARTESIAN_POINT ( 'NONE',  ( 107.3241674272228892, -25.27320757387406402, 321.5865679059475610 ) ) ;
#1909 = LINE ( 'NONE', #56399, #17152 ) ;
#1910 = CARTESIAN_POINT ( 'NONE',  ( 115.0382812869126923, -42.90717343850143806, 124.3008843337145493 ) ) ;
#1911 = LINE ( 'NONE', #44558, #57846 ) ;
#1912 = EDGE_CURVE ( 'NONE', #54183, #19039, #23242, .T. ) ;
#1913 = CARTESIAN_POINT ( 'NONE',  ( 106.0550521757682816, -27.00111521709629514, 46.15848241876796720 ) ) ;
#1914 = CARTESIAN_POINT ( 'NONE',  ( 11.65927451492354550, 77.72029911766621524, 117.7806352395324723 ) ) ;
#1915 = ORIENTED_EDGE ( 'NONE', *, *, #61465, .T. ) ;
#1916 = CARTESIAN_POINT ( 'NONE',  ( 115.6092852924205943, -42.78035731602705027, 49.33562527591095659 ) ) ;
#1917 = CARTESIAN_POINT ( 'NONE',  ( 27.27158787008327678, 184.0000000000000000, 80.02307622376218887 ) ) ;
#1918 = TOROIDAL_SURFACE ( 'NONE', #52641, 11.75000000000000000, 2.550000000000000266 ) ;
#1919 = EDGE_CURVE ( 'NONE', #28582, #4939, #58727, .T. ) ;
#1920 = CARTESIAN_POINT ( 'NONE',  ( 109.9602307476630330, -48.22147533147688847, 242.7727681330539724 ) ) ;
#1921 = ORIENTED_EDGE ( 'NONE', *, *, #75931, .T. ) ;
#1922 = CIRCLE ( 'NONE', #42546, 4.749999999999976907 ) ;
#1923 = FACE_OUTER_BOUND ( 'NONE', #29612, .T. ) ;
#1924 = CARTESIAN_POINT ( 'NONE',  ( 116.7956705048818833, -39.38589551711255865, 19.61517315323455080 ) ) ;
#1925 = CARTESIAN_POINT ( 'NONE',  ( 50.03799999999999670, 20.32000000000000028, 178.6098374884404905 ) ) ;
#1926 = ADVANCED_FACE ( 'NONE', ( #30152 ), #2454, .F. ) ;
#1927 = CARTESIAN_POINT ( 'NONE',  ( 99.91476266851738330, -32.73750773393640401, 108.7395189410199663 ) ) ;
#1928 = CARTESIAN_POINT ( 'NONE',  ( 113.1681127151884141, -26.54159316308081173, 200.6470538473399756 ) ) ;
#1929 = LINE ( 'NONE', #56417, #15979 ) ;
#1930 = EDGE_LOOP ( 'NONE', ( #65051, #37161, #36735, #53971 ) ) ;
#1931 = CYLINDRICAL_SURFACE ( 'NONE', #10276, 17.33514202138210081 ) ;
#1932 = VERTEX_POINT ( 'NONE', #22906 ) ;
#1933 = EDGE_LOOP ( 'NONE', ( #38657, #38106, #30690, #37524 ) ) ;
#1934 = VECTOR ( 'NONE', #63013, 1000.000000000000000 ) ;
#1935 = CARTESIAN_POINT ( 'NONE',  ( 83.06670390244808289, -58.72944715994108122, 207.5838068554169809 ) ) ;
#1936 = ORIENTED_EDGE ( 'NONE', *, *, #27418, .F. ) ;
#1937 = VERTEX_POINT ( 'NONE', #23798 ) ;
#1938 = DIRECTION ( 'NONE',  ( -6.524622321627019585E-16, -4.013151879589939944E-16, -1.000000000000000000 ) ) ;
#1939 = CARTESIAN_POINT ( 'NONE',  ( 97.12553659991493760, -37.99670770671464481, 42.42725359356597181 ) ) ;
#1940 = CARTESIAN_POINT ( 'NONE',  ( 103.4870123794286059, -45.04810440550495798, 136.6876579233149300 ) ) ;
#1941 = CARTESIAN_POINT ( 'NONE',  ( 105.6290166497307581, -47.07739640705644035, 257.4670538473392298 ) ) ;
#1942 = EDGE_CURVE ( 'NONE', #34565, #32370, #37863, .T. ) ;
#1943 = EDGE_CURVE ( 'NONE', #50013, #35318, #85140, .T. ) ;
#1944 = CARTESIAN_POINT ( 'NONE',  ( 126.8164832912740110, -46.47944715994101017, 14.92562527591099020 ) ) ;
#1945 = ORIENTED_EDGE ( 'NONE', *, *, #81206, .T. ) ;
#1946 = EDGE_CURVE ( 'NONE', #1794, #35668, #24234, .T. ) ;
#1947 = EDGE_LOOP ( 'NONE', ( #11641, #38894 ) ) ;
#1948 = CARTESIAN_POINT ( 'NONE',  ( -487.2989999999999782, 93.66249999999999432, 82.23860802895320887 ) ) ;
#1949 = EDGE_CURVE ( 'NONE', #63134, #36007, #78323, .T. ) ;
#1950 = DIRECTION ( 'NONE',  ( 0.000000000000000000, 0.000000000000000000, -1.000000000000000000 ) ) ;
#1951 = CARTESIAN_POINT ( 'NONE',  ( 70.50919912965197511, -139.8621867207610308, 247.1491889055018305 ) ) ;
#1952 = VECTOR ( 'NONE', #71675, 1000.000000000000000 ) ;
#1953 = CARTESIAN_POINT ( 'NONE',  ( 114.5992475275822784, -44.05128143045557465, 98.21276813305395592 ) ) ;
#1954 = FACE_BOUND ( 'NONE', #72816, .T. ) ;
#1955 = ORIENTED_EDGE ( 'NONE', *, *, #57171, .T. ) ;
#1956 = CARTESIAN_POINT ( 'NONE',  ( 96.53679867426635042, -40.09171982297686299, 281.5603871806728762 ) ) ;
#1957 = CYLINDRICAL_SURFACE ( 'NONE', #84880, 6.349999999999994316 ) ;
#1958 =( NAMED_UNIT ( * ) PLANE_ANGLE_UNIT ( ) SI_UNIT ( $, .RADIAN. ) );
#1959 = AXIS2_PLACEMENT_3D ( 'NONE', #75785, #19470, #26721 ) ;
#1960 = CARTESIAN_POINT ( 'NONE',  ( 11.75171833347117811, 77.73468025497935230, 130.0260221836642813 ) ) ;
#1961 = LINE ( 'NONE', #35113, #15568 ) ;
#1963 = CARTESIAN_POINT ( 'NONE',  ( 167.6524903400755875, -49.32844715993520879, 180.4678068554150059 ) ) ;
#1962 = CARTESIAN_POINT ( 'NONE',  ( 57.56670390244744340, -48.82844715994040286, 170.7178068554150911 ) ) ;
#1964 = CARTESIAN_POINT ( 'NONE',  ( 188.5667039024484097, -48.82844715993431350, 257.2178068554150059 ) ) ;
#1965 = CARTESIAN_POINT ( 'NONE',  ( -462.0260000000000105, 53.97500000000000142, -3.174999999999999822 ) ) ;
#1966 = DIRECTION ( 'NONE',  ( 0.000000000000000000, 0.000000000000000000, 1.000000000000000000 ) ) ;
#1967 = CARTESIAN_POINT ( 'NONE',  ( -10.78734560828563360, 89.26522093196130925, 130.1097824653510315 ) ) ;
#1968 = CARTESIAN_POINT ( 'NONE',  ( 97.81168843500762478, -40.51741166756562507, 12.63579318495451176 ) ) ;
#1969 = CARTESIAN_POINT ( 'NONE',  ( 21.03689327557613709, -23.42844715994197813, 193.9678068554150627 ) ) ;
#1971 = VERTEX_POINT ( 'NONE', #79659 ) ;
#1970 = DIRECTION ( 'NONE',  ( -0.9254794337955621897, -0.3787978585227821382, 0.000000000000000000 ) ) ;
#1972 = CARTESIAN_POINT ( 'NONE',  ( 36.23715912545429063, -47.82818131006125384, 249.9678068554150343 ) ) ;
#1973 = CARTESIAN_POINT ( 'NONE',  ( 116.3368571269942464, -41.54685706111320087, 288.4441967044822945 ) ) ;
#1974 = CARTESIAN_POINT ( 'NONE',  ( 95.91002759172351944, -32.73343517516348555, 172.0527681330539735 ) ) ;
#1975 = CARTESIAN_POINT ( 'NONE',  ( 102.3596500697202174, -47.65578173298946751, 283.2527681330539053 ) ) ;
#1977 = DIRECTION ( 'NONE',  ( 0.000000000000000000, 0.000000000000000000, -1.000000000000000000 ) ) ;
#1976 = DIRECTION ( 'NONE',  ( 1.000000000000000000, 0.000000000000000000, 0.000000000000000000 ) ) ;
#1978 = LINE ( 'NONE', #50556, #23345 ) ;
#1979 = EDGE_LOOP ( 'NONE', ( #57902, #80804, #1590, #27732, #34775 ) ) ;
#1980 = CARTESIAN_POINT ( 'NONE',  ( 71.25614885437424562, -84.12815644128085069, 540.9756252759101471 ) ) ;
#1981 = VERTEX_POINT ( 'NONE', #16527 ) ;
#1982 = CARTESIAN_POINT ( 'NONE',  ( 98.65123886609836745, -31.74476095556103061, 81.90133956162493689 ) ) ;
#1984 = EDGE_LOOP ( 'NONE', ( #10043, #68745, #95, #71951, #82324, #55575 ) ) ;
#1983 = DIRECTION ( 'NONE',  ( 4.299999999999999979E-14, -1.000000000000000000, 4.400000000000000367E-29 ) ) ;
#1985 = AXIS2_PLACEMENT_3D ( 'NONE', #70024, #47761, #75044 ) ;
#1986 = LINE ( 'NONE', #16070, #88215 ) ;
#1987 = CARTESIAN_POINT ( 'NONE',  ( 96.87985868497426623, -34.61725761836213167, 212.1641967044819808 ) ) ;
#1988 = FACE_OUTER_BOUND ( 'NONE', #21891, .T. ) ;
#1989 = CARTESIAN_POINT ( 'NONE',  ( 110.8549113655039378, -45.98405751658768992, 147.8856630510708214 ) ) ;
#1990 = DIRECTION ( 'NONE',  ( -1.000000000000000000, -1.000000000000000078E-15, 5.773159642023980606E-15 ) ) ;
#1991 = FACE_OUTER_BOUND ( 'NONE', #56263, .T. ) ;
#1992 = CARTESIAN_POINT ( 'NONE',  ( 146.5099599153435008, -138.2352025272441836, 245.9283337036430055 ) ) ;
#1993 = CARTESIAN_POINT ( 'NONE',  ( 116.0282290876930773, -41.23944930189807678, 98.45557829630303104 ) ) ;
#1994 = CARTESIAN_POINT ( 'NONE',  ( 118.1720832024965802, -36.20253795304678590, 118.8641967044829784 ) ) ;
#1995 = VERTEX_POINT ( 'NONE', #9708 ) ;
#1996 = ORIENTED_EDGE ( 'NONE', *, *, #71175, .F. ) ;
#1997 = AXIS2_PLACEMENT_3D ( 'NONE', #48456, #76195, #47125 ) ;
#1998 = CARTESIAN_POINT ( 'NONE',  ( 98.44769980935930676, -38.78975051229773641, 52.94444044875496047 ) ) ;
#1999 = CARTESIAN_POINT ( 'NONE',  ( 119.2637946045970097, -42.39761235918182081, 3.024967495036162912 ) ) ;
#2001 = DIRECTION ( 'NONE',  ( -1.000000000000000000, 0.000000000000000000, 0.000000000000000000 ) ) ;
#2000 = CARTESIAN_POINT ( 'NONE',  ( 99.40370404213548738, -29.74227323812501211, 226.7261014663869503 ) ) ;
#2002 = CARTESIAN_POINT ( 'NONE',  ( 4.665904304751420031E-15, 92.07499999999998863, -38.10000000000000142 ) ) ;
#2003 = DIRECTION ( 'NONE',  ( 1.000000000000000078E-15, -1.000000000000000000, 0.000000000000000000 ) ) ;
#2004 = EDGE_CURVE ( 'NONE', #55608, #6226, #43488, .T. ) ;
#2005 = DIRECTION ( 'NONE',  ( 0.000000000000000000, 0.000000000000000000, -1.000000000000000000 ) ) ;
#2006 = ADVANCED_FACE ( 'NONE', ( #31472, #59176 ), #86906, .F. ) ;
#2007 = DIRECTION ( 'NONE',  ( 1.000000000000000000, 0.000000000000000000, 0.000000000000000000 ) ) ;
#2008 = CARTESIAN_POINT ( 'NONE',  ( 11.32175623853374091, 76.95891767344909340, 118.0145928970902816 ) ) ;
#2009 = CARTESIAN_POINT ( 'NONE',  ( 117.0023065291009061, -39.93004192841232936, 158.5784824187679476 ) ) ;
#2010 = ORIENTED_EDGE ( 'NONE', *, *, #76441, .F. ) ;
#2011 = ORIENTED_EDGE ( 'NONE', *, *, #41800, .F. ) ;
#2012 = VERTEX_POINT ( 'NONE', #80102 ) ;
#2013 = EDGE_CURVE ( 'NONE', #61542, #42555, #33274, .T. ) ;
#2014 = EDGE_CURVE ( 'NONE', #42554, #76542, #40577, .T. ) ;
#2015 = CARTESIAN_POINT ( 'NONE',  ( 1.668880554893940493, 69.93234144696143062, 130.5479136978233896 ) ) ;
#2016 = CARTESIAN_POINT ( 'NONE',  ( 145.3595637443018234, -69.45303146431501773, 247.4784022495120155 ) ) ;
#2017 = CARTESIAN_POINT ( 'NONE',  ( 97.70664598133903667, -40.25154286292865891, 131.6128750669620047 ) ) ;
#2018 = CARTESIAN_POINT ( 'NONE',  ( 98.15069168346546746, -41.26105110007194554, 102.7006730368125886 ) ) ;
#2019 = CARTESIAN_POINT ( 'NONE',  ( 115.6671688226974197, -35.76553148137116267, 231.7214237029249659 ) ) ;
#2020 = EDGE_CURVE ( 'NONE', #49604, #54780, #78350, .T. ) ;
#2021 = VECTOR ( 'NONE', #60130, 1000.000000000000000 ) ;
#2022 = CARTESIAN_POINT ( 'NONE',  ( 76.24325998657069192, -5.906223855237660914, -4.824374724089060429 ) ) ;
#2023 = CIRCLE ( 'NONE', #41097, 38.10000000000000142 ) ;
#2024 = EDGE_CURVE ( 'NONE', #71038, #26842, #11493, .T. ) ;
#2025 = CARTESIAN_POINT ( 'NONE',  ( 102.9133425085070712, -27.12904003091135152, 155.4013395616249795 ) ) ;
#2026 = DIRECTION ( 'NONE',  ( 0.000000000000000000, 1.000000000000000000, 0.000000000000000000 ) ) ;
#2027 = EDGE_LOOP ( 'NONE', ( #79805, #9909, #35090, #9036, #6972, #60590 ) ) ;
#2029 = ORIENTED_EDGE ( 'NONE', *, *, #65942, .T. ) ;
#2028 = ORIENTED_EDGE ( 'NONE', *, *, #46820, .T. ) ;
#2030 = DIRECTION ( 'NONE',  ( 1.000000000000000000, 1.000000000000000078E-15, 0.000000000000000000 ) ) ;
#2031 = ORIENTED_EDGE ( 'NONE', *, *, #43091, .T. ) ;
#2032 = ORIENTED_EDGE ( 'NONE', *, *, #52612, .F. ) ;
#2033 = CARTESIAN_POINT ( 'NONE',  ( -103.1875000000000000, 117.4749999999999943, -1.080832317973422076E-12 ) ) ;
#2034 = CARTESIAN_POINT ( 'NONE',  ( 131.5359215223094793, -35.65293368213150416, 7.043713522540487659 ) ) ;
#2035 = EDGE_CURVE ( 'NONE', #3324, #86462, #81453, .T. ) ;
#2036 = CARTESIAN_POINT ( 'NONE',  ( 110.1825742734413609, -44.80353631977761353, 15.67570941721097100 ) ) ;
#2037 = CARTESIAN_POINT ( 'NONE',  ( 88.90000000000000568, 66.67499999999999716, 346.0750000000000455 ) ) ;
#2038 = ORIENTED_EDGE ( 'NONE', *, *, #67864, .T. ) ;
#2039 = CARTESIAN_POINT ( 'NONE',  ( 116.4162535572406227, -39.30367360901732354, 9.635625275910939536 ) ) ;
#2040 = EDGE_CURVE ( 'NONE', #19992, #80451, #49255, .T. ) ;
#2041 = CARTESIAN_POINT ( 'NONE',  ( -126.8825202696031198, 58.88652527941982129, 30.75229511181026609 ) ) ;
#2042 = ORIENTED_EDGE ( 'NONE', *, *, #74462, .F. ) ;
#2043 = EDGE_LOOP ( 'NONE', ( #68408, #37115, #73877, #16147 ) ) ;
#2044 = CIRCLE ( 'NONE', #42603, 2.517500000000005844 ) ;
#2045 = CARTESIAN_POINT ( 'NONE',  ( 109.6431318019857741, -46.48005661577610681, 112.7814924369443048 ) ) ;
#2046 = CIRCLE ( 'NONE', #73144, 0.2999999999999943823 ) ;
#2047 = ORIENTED_EDGE ( 'NONE', *, *, #41980, .T. ) ;
#2048 = ORIENTED_EDGE ( 'NONE', *, *, #59193, .F. ) ;
#2049 = VECTOR ( 'NONE', #49400, 999.9999999999998863 ) ;
#2050 = CARTESIAN_POINT ( 'NONE',  ( 99.35983957736841887, -39.50259174935074213, 264.4195189410201579 ) ) ;
#2052 = CARTESIAN_POINT ( 'NONE',  ( 118.9428397581607442, -36.92852597549882177, 153.8127681330539644 ) ) ;
#2051 = AXIS2_PLACEMENT_3D ( 'NONE', #14860, #42527, #7586 ) ;
#2053 = CARTESIAN_POINT ( 'NONE',  ( 108.2752786314947429, -47.69320359391970499, 157.6518157521019532 ) ) ;
#2054 = LINE ( 'NONE', #1156, #52467 ) ;
#2055 = CARTESIAN_POINT ( 'NONE',  ( 98.03678599612689482, -44.40402742967116723, 222.8870538473399563 ) ) ;
#2056 = CYLINDRICAL_SURFACE ( 'NONE', #89128, 12.69999999999999929 ) ;
#2057 = CARTESIAN_POINT ( 'NONE',  ( 68.09411347895392908, -99.27098689615887395, 247.4783998280180128 ) ) ;
#2058 = ORIENTED_EDGE ( 'NONE', *, *, #78733, .F. ) ;
#2059 = CARTESIAN_POINT ( 'NONE',  ( -130.4793906290846621, 70.66229531820916065, -4.488385961153167791 ) ) ;
#2060 = ORIENTED_EDGE ( 'NONE', *, *, #17855, .F. ) ;
#2061 = EDGE_CURVE ( 'NONE', #51053, #60205, #12385, .T. ) ;
#2062 = VERTEX_POINT ( 'NONE', #26903 ) ;
#2063 = ADVANCED_FACE ( 'NONE', ( #20103 ), #73913, .F. ) ;
#2064 = CARTESIAN_POINT ( 'NONE',  ( 97.01576029581003979, -41.44069443601846814, 211.6632443235299945 ) ) ;
#2065 = ORIENTED_EDGE ( 'NONE', *, *, #74567, .F. ) ;
#2066 = CARTESIAN_POINT ( 'NONE',  ( 97.95630822081318456, -30.46975087157407458, 165.8594347997199634 ) ) ;
#2067 = DIRECTION ( 'NONE',  ( 1.000000000000000000, 0.000000000000000000, 0.000000000000000000 ) ) ;
#2068 = DIRECTION ( 'NONE',  ( 0.000000000000000000, 0.000000000000000000, 1.000000000000000000 ) ) ;
#2069 = FACE_OUTER_BOUND ( 'NONE', #72844, .T. ) ;
#2072 = CARTESIAN_POINT ( 'NONE',  ( 99.55514648348079731, -29.48070623161996551, 246.7156252759109520 ) ) ;
#2071 = CARTESIAN_POINT ( 'NONE',  ( 99.48017111314335637, -43.25549976577509881, 56.89151756084950762 ) ) ;
#2070 = DIRECTION ( 'NONE',  ( -1.000000000000000000, 1.000000000000000078E-15, 0.000000000000000000 ) ) ;
#2073 = DIRECTION ( 'NONE',  ( 0.000000000000000000, 0.000000000000000000, -1.000000000000000000 ) ) ;
#2074 = DIRECTION ( 'NONE',  ( 0.000000000000000000, -1.000000000000000000, 0.000000000000000000 ) ) ;
#2075 = DIRECTION ( 'NONE',  ( 0.000000000000000000, 0.000000000000000000, -1.000000000000000000 ) ) ;
#2076 = DIRECTION ( 'NONE',  ( 1.000000000000000000, 0.000000000000000000, 0.000000000000000000 ) ) ;
#2077 = FACE_OUTER_BOUND ( 'NONE', #12884, .T. ) ;
#2078 = LINE ( 'NONE', #21180, #28830 ) ;
#2080 = ORIENTED_EDGE ( 'NONE', *, *, #9388, .F. ) ;
#2079 = CARTESIAN_POINT ( 'NONE',  ( 102.8854998099173628, -43.62190156306392197, 195.5838068554170945 ) ) ;
#2081 = DIRECTION ( 'NONE',  ( -1.092739197465703932E-16, 1.000000000000000000, 0.000000000000000000 ) ) ;
#2082 = CARTESIAN_POINT ( 'NONE',  ( 98.26213988389305598, -31.03978702703054537, 145.8699109901969848 ) ) ;
#2083 = CARTESIAN_POINT ( 'NONE',  ( 117.9887704088505274, -38.42580343310776669, 64.69181575210097890 ) ) ;
#2084 = CARTESIAN_POINT ( 'NONE',  ( 96.63066398506619237, -35.53291458860860530, 202.2356252759109623 ) ) ;
#2085 = CARTESIAN_POINT ( 'NONE',  ( 33.92127028473601769, -29.73316016639540749, 342.9256252759119548 ) ) ;
#2086 = CARTESIAN_POINT ( 'NONE',  ( 36.65249034007530327, -49.32844715994124130, 300.4678068554150059 ) ) ;
#2088 = CARTESIAN_POINT ( 'NONE',  ( 163.2569089553700223, -33.54226604285010893, -5.074374724088000832 ) ) ;
#2087 = DIRECTION ( 'NONE',  ( 0.000000000000000000, 0.000000000000000000, 1.000000000000000000 ) ) ;
#2089 = CARTESIAN_POINT ( 'NONE',  ( 107.0664832912739399, -36.72944715994096754, 300.2406250056037038 ) ) ;
#2090 = PLANE ( 'NONE',  #6152 ) ;
#2091 = VERTEX_POINT ( 'NONE', #5122 ) ;
#2093 = EDGE_CURVE ( 'NONE', #43862, #24524, #11942, .T. ) ;
#2092 = AXIS2_PLACEMENT_3D ( 'NONE', #19499, #34808, #8462 ) ;
#2094 = DIRECTION ( 'NONE',  ( 0.000000000000000000, 0.000000000000000000, -1.000000000000000000 ) ) ;
#2095 = CIRCLE ( 'NONE', #4929, 4.762500000000000178 ) ;
#2096 = ORIENTED_EDGE ( 'NONE', *, *, #26575, .F. ) ;
#2097 = ORIENTED_EDGE ( 'NONE', *, *, #65777, .F. ) ;
#2099 = VERTEX_POINT ( 'NONE', #68251 ) ;
#2098 = DIRECTION ( 'NONE',  ( 0.000000000000000000, 1.000000000000000000, 0.000000000000000000 ) ) ;
#2100 = CARTESIAN_POINT ( 'NONE',  ( 114.0075736764522389, -28.98025818340847692, 110.4956252759109816 ) ) ;
#2101 = CARTESIAN_POINT ( 'NONE',  ( 36.65249034007526063, -48.32844715994123419, 300.4678068554150059 ) ) ;
#2102 = LINE ( 'NONE', #28917, #67367 ) ;
#2103 = DIRECTION ( 'NONE',  ( -4.237773401492740281E-14, 1.000000000000000000, 0.000000000000000000 ) ) ;
#2104 = CARTESIAN_POINT ( 'NONE',  ( 104.4155842956043614, -46.14412563975625403, 22.35848241876892217 ) ) ;
#2105 = ORIENTED_EDGE ( 'NONE', *, *, #24082, .F. ) ;
#2106 = EDGE_CURVE ( 'NONE', #64360, #47447, #53685, .T. ) ;
#2107 = VERTEX_POINT ( 'NONE', #61415 ) ;
#2108 = ORIENTED_EDGE ( 'NONE', *, *, #25100, .T. ) ;
#2109 = CIRCLE ( 'NONE', #67309, 8.928100000000000591 ) ;
#2110 = AXIS2_PLACEMENT_3D ( 'NONE', #73687, #36936, #64637 ) ;
#2111 = DIRECTION ( 'NONE',  ( -1.000000000000000000, 0.000000000000000000, -2.108231265501709878E-16 ) ) ;
#2112 = AXIS2_PLACEMENT_3D ( 'NONE', #54801, #19863, #47549 ) ;
#2113 = CARTESIAN_POINT ( 'NONE',  ( 33.78129701732233059, -35.65087443489924368, 117.4678068554150485 ) ) ;
#2114 = CARTESIAN_POINT ( 'NONE',  ( 97.07207206033048408, -35.37844118961633910, 117.2189586084917465 ) ) ;
#2115 = AXIS2_PLACEMENT_3D ( 'NONE', #72445, #25624, #25172 ) ;
#2116 = FACE_OUTER_BOUND ( 'NONE', #56016, .T. ) ;
#2117 = CARTESIAN_POINT ( 'NONE',  ( 161.4809174648185603, -49.32844715993547169, 180.4678068554150059 ) ) ;
#2118 = EDGE_CURVE ( 'NONE', #43566, #38211, #79774, .T. ) ;
#2119 = LINE ( 'NONE', #17528, #69835 ) ;
#2120 = ADVANCED_FACE ( 'NONE', ( #74606 ), #13043, .F. ) ;
#2122 = LINE ( 'NONE', #71173, #32626 ) ;
#2121 = AXIS2_PLACEMENT_3D ( 'NONE', #62039, #89773, #41583 ) ;
#2124 = EDGE_CURVE ( 'NONE', #47880, #64107, #46324, .T. ) ;
#2123 = AXIS2_PLACEMENT_3D ( 'NONE', #56026, #28332, #8820 ) ;
#2125 = CARTESIAN_POINT ( 'NONE',  ( 107.0664832912739968, -36.72944715994100306, 277.6356252759110248 ) ) ;
#2126 = CARTESIAN_POINT ( 'NONE',  ( 96.70769389551958284, -42.43415482991314036, 26.72705384733997747 ) ) ;
#2127 = ORIENTED_EDGE ( 'NONE', *, *, #59610, .F. ) ;
#2128 = EDGE_CURVE ( 'NONE', #83421, #73910, #72499, .T. ) ;
#2129 = DIRECTION ( 'NONE',  ( 0.000000000000000000, 0.000000000000000000, 1.000000000000000000 ) ) ;
#2130 = CARTESIAN_POINT ( 'NONE',  ( 0.000000000000000000, 65.60000000000000853, 0.000000000000000000 ) ) ;
#2131 = CARTESIAN_POINT ( 'NONE',  ( 108.5685384152640864, -45.25263643686804471, 120.5214237029249915 ) ) ;
#2132 = EDGE_CURVE ( 'NONE', #7741, #13694, #46432, .T. ) ;
#2133 = CARTESIAN_POINT ( 'NONE',  ( 97.53201689872335578, -39.74949948161557955, 96.57057676354683906 ) ) ;
#2134 = ADVANCED_FACE ( 'NONE', ( #19203 ), #19642, .F. ) ;
#2135 = CARTESIAN_POINT ( 'NONE',  ( 25.56670390244832447, -48.82844715994168183, 257.2178068554150059 ) ) ;
#2136 = ORIENTED_EDGE ( 'NONE', *, *, #46594, .F. ) ;
#2137 = VERTEX_POINT ( 'NONE', #87793 ) ;
#2138 = LINE ( 'NONE', #28949, #75783 ) ;
#2139 = ORIENTED_EDGE ( 'NONE', *, *, #23065, .T. ) ;
#2140 = VERTEX_POINT ( 'NONE', #25558 ) ;
#2141 = EDGE_CURVE ( 'NONE', #16953, #80801, #53232, .T. ) ;
#2142 = CARTESIAN_POINT ( 'NONE',  ( 115.8989637469753831, -39.93316602039875107, 169.9692023535169483 ) ) ;
#2143 = DIRECTION ( 'NONE',  ( 0.000000000000000000, 1.000000000000000000, 0.000000000000000000 ) ) ;
#2144 = CARTESIAN_POINT ( 'NONE',  ( 102.5487710710870033, -27.30991770518087591, 91.43276813305395478 ) ) ;
#2145 = STYLED_ITEM ( 'NONE', ( #66142 ), #80104 ) ;
#2146 = CARTESIAN_POINT ( 'NONE',  ( 111.2589507039926673, -45.80977664277359196, 17.92067989835221553 ) ) ;
#2147 = ORIENTED_EDGE ( 'NONE', *, *, #60736, .T. ) ;
#2148 = VECTOR ( 'NONE', #84868, 1000.000000000000000 ) ;
#2149 = ORIENTED_EDGE ( 'NONE', *, *, #11022, .T. ) ;
#2150 = ORIENTED_EDGE ( 'NONE', *, *, #60777, .T. ) ;
#2151 = CARTESIAN_POINT ( 'NONE',  ( 100.0385306026334717, -40.93546354753772221, 159.5738046553059917 ) ) ;
#2152 = CARTESIAN_POINT ( 'NONE',  ( 117.4695374193713775, -37.69008693337416815, 78.75276813305399060 ) ) ;
#2153 = ORIENTED_EDGE ( 'NONE', *, *, #73110, .T. ) ;
#2154 = CARTESIAN_POINT ( 'NONE',  ( 104.4960957391109417, -46.84663716100912012, 47.37848241876796607 ) ) ;
#2155 = CARTESIAN_POINT ( 'NONE',  ( 102.8351866564443924, -46.28106417705388509, 173.2441967044829596 ) ) ;
#2156 = DIRECTION ( 'NONE',  ( -0.000000000000000000, 1.000000000000000000, 0.000000000000000000 ) ) ;
#2157 = DIRECTION ( 'NONE',  ( -7.136255983449500255E-16, 0.000000000000000000, -1.000000000000000000 ) ) ;
#2158 = CARTESIAN_POINT ( 'NONE',  ( 114.0221110621602492, -28.96402831996850225, 110.4956252759109816 ) ) ;
#2159 = CARTESIAN_POINT ( 'NONE',  ( 48.45959712127231711, -26.00627455219176554, 313.9678068554150059 ) ) ;
#2160 = ORIENTED_EDGE ( 'NONE', *, *, #19869, .F. ) ;
#2161 = FACE_BOUND ( 'NONE', #29161, .T. ) ;
#2162 = VERTEX_POINT ( 'NONE', #60515 ) ;
#2163 = CARTESIAN_POINT ( 'NONE',  ( 107.0664832912739399, -36.72944715994096754, 300.2406250056037038 ) ) ;
#2164 = CARTESIAN_POINT ( 'NONE',  ( 151.0667039024469886, -67.87844715994090450, 190.2178068554179902 ) ) ;
#2165 = EDGE_CURVE ( 'NONE', #24211, #76657, #46873, .T. ) ;
#2166 = ORIENTED_EDGE ( 'NONE', *, *, #69271, .T. ) ;
#2167 = CONICAL_SURFACE ( 'NONE', #38393, 1.258750000000002922, 1.029744258676650093 ) ;
#2168 = LINE ( 'NONE', #56199, #62006 ) ;
#2169 = AXIS2_PLACEMENT_3D ( 'NONE', #19405, #25766, #87556 ) ;
#2170 = VECTOR ( 'NONE', #76166, 1000.000000000000000 ) ;
#2171 = CARTESIAN_POINT ( 'NONE',  ( 123.6837132603320413, -56.64645651782490177, 239.5838068554164693 ) ) ;
#2172 = CARTESIAN_POINT ( 'NONE',  ( 99.06573214631099233, -44.35618096740151373, 36.92038718067297509 ) ) ;
#2173 = CARTESIAN_POINT ( 'NONE',  ( 75.31670390244798341, -50.82844715994100682, 88.43480685541499042 ) ) ;
#2174 = AXIS2_PLACEMENT_3D ( 'NONE', #70061, #41881, #83254 ) ;
#2175 = CYLINDRICAL_SURFACE ( 'NONE', #5758, 0.5000000000000004441 ) ;
#2176 = FACE_OUTER_BOUND ( 'NONE', #18334, .T. ) ;
#2177 = CARTESIAN_POINT ( 'NONE',  ( 101.5079035968563943, -28.64143341885324290, 50.55562527591095545 ) ) ;
#2179 = CARTESIAN_POINT ( 'NONE',  ( 109.1969564574039282, -26.54663071456431211, 135.9127681330539872 ) ) ;
#2178 = CARTESIAN_POINT ( 'NONE',  ( 0.000000000000000000, 2.269999999999994245, 0.000000000000000000 ) ) ;
#2180 = CYLINDRICAL_SURFACE ( 'NONE', #26274, 0.5000000000000104361 ) ;
#2181 = CARTESIAN_POINT ( 'NONE',  ( -446.0240000000000009, 104.7749999999999915, 50.79999999999999716 ) ) ;
#2182 = ORIENTED_EDGE ( 'NONE', *, *, #45449, .F. ) ;
#2183 = LINE ( 'NONE', #38465, #64338 ) ;
#2184 = VECTOR ( 'NONE', #82406, 1000.000000000000114 ) ;
#2185 = CIRCLE ( 'NONE', #13772, 3.999999999999992895 ) ;
#2186 = CARTESIAN_POINT ( 'NONE',  ( 173.9900000000000091, 21.46300000000000097, 41.63456447661474868 ) ) ;
#2187 = EDGE_LOOP ( 'NONE', ( #30572, #48799, #30481, #67896 ) ) ;
#2188 = LINE ( 'NONE', #29442, #60705 ) ;
#2189 = EDGE_CURVE ( 'NONE', #28049, #56291, #13728, .T. ) ;
#2191 = ORIENTED_EDGE ( 'NONE', *, *, #58584, .F. ) ;
#2190 = CARTESIAN_POINT ( 'NONE',  ( 96.69933951777882442, -35.27033920508573317, 181.2156252759109805 ) ) ;
#2192 = LINE ( 'NONE', #83973, #66848 ) ;
#2193 = CARTESIAN_POINT ( 'NONE',  ( 118.6781471654015689, -39.21772221756580734, 254.6584824187681022 ) ) ;
#2194 = CARTESIAN_POINT ( 'NONE',  ( 101.6557087385557736, -27.03816153323032268, 101.4937205140059575 ) ) ;
#2195 = CARTESIAN_POINT ( 'NONE',  ( 102.0693260774676077, -27.96916680133194788, 251.4954626382068170 ) ) ;
#2196 = DIRECTION ( 'NONE',  ( 4.299999999999999979E-14, -1.000000000000000000, 4.400000000000000367E-29 ) ) ;
#2197 = AXIS2_PLACEMENT_3D ( 'NONE', #49101, #70021, #56815 ) ;
#2198 = DIRECTION ( 'NONE',  ( 0.000000000000000000, 0.000000000000000000, 1.000000000000000000 ) ) ;
#2199 = EDGE_LOOP ( 'NONE', ( #46345, #19487, #45707, #60891 ) ) ;
#2200 = EDGE_CURVE ( 'NONE', #24293, #72149, #60865, .T. ) ;
#2201 = CIRCLE ( 'NONE', #32644, 2.029999999999997140 ) ;
#2202 = EDGE_LOOP ( 'NONE', ( #9887, #66284, #10875, #64176 ) ) ;
#2203 = ORIENTED_EDGE ( 'NONE', *, *, #46360, .F. ) ;
#2204 = ORIENTED_EDGE ( 'NONE', *, *, #24360, .F. ) ;
#2205 = LINE ( 'NONE', #8118, #27880 ) ;
#2206 = CARTESIAN_POINT ( 'NONE',  ( 106.5673366543293383, -47.17799660047543853, 243.5384824187679556 ) ) ;
#2207 = FACE_OUTER_BOUND ( 'NONE', #61381, .T. ) ;
#2208 = CARTESIAN_POINT ( 'NONE',  ( 131.5918432679227692, -35.51852171454133611, 2.740177351677670625 ) ) ;
#2210 = DIRECTION ( 'NONE',  ( 0.000000000000000000, 0.000000000000000000, 1.000000000000000000 ) ) ;
#2209 = CARTESIAN_POINT ( 'NONE',  ( 110.2536356736639078, -101.8611209747513868, -19.78219314458209865 ) ) ;
#2211 = DIRECTION ( 'NONE',  ( 0.9834602067019598826, 0.1811243270069988198, 0.000000000000000000 ) ) ;
#2212 = CARTESIAN_POINT ( 'NONE',  ( 99.04884357002234196, -44.37228004027687689, 36.92038718067297509 ) ) ;
#2213 = VERTEX_POINT ( 'NONE', #41413 ) ;
#2214 = VERTEX_POINT ( 'NONE', #82791 ) ;
#2215 = VECTOR ( 'NONE', #80038, 1000.000000000000000 ) ;
#2216 = ORIENTED_EDGE ( 'NONE', *, *, #77802, .T. ) ;
#2217 = CARTESIAN_POINT ( 'NONE',  ( 107.0664832912739968, -36.72944715994100306, 293.2242906452868851 ) ) ;
#2218 = VECTOR ( 'NONE', #39800, 1000.000000000000000 ) ;
#2219 = DIRECTION ( 'NONE',  ( 0.8758084860610321210, 0.03696114963002913867, 0.4812414873652411940 ) ) ;
#2220 = CARTESIAN_POINT ( 'NONE',  ( 113.3415799102510277, -29.55617248177381740, 285.5032443235294863 ) ) ;
#2221 = EDGE_CURVE ( 'NONE', #55274, #46818, #44913, .T. ) ;
#2222 = DIRECTION ( 'NONE',  ( 0.000000000000000000, 0.000000000000000000, 1.000000000000000000 ) ) ;
#2223 = CARTESIAN_POINT ( 'NONE',  ( 103.4152017835536270, -27.65577212482034497, 126.3813395616249835 ) ) ;
#2224 = EDGE_CURVE ( 'NONE', #51923, #24886, #89215, .T. ) ;
#2225 = CARTESIAN_POINT ( 'NONE',  ( 105.7148859710100339, -46.72376874668114510, 27.46891152066978847 ) ) ;
#2226 = ORIENTED_EDGE ( 'NONE', *, *, #83708, .F. ) ;
#2227 = LINE ( 'NONE', #35832, #3709 ) ;
#2228 = EDGE_CURVE ( 'NONE', #8503, #22291, #18794, .T. ) ;
#2229 = CARTESIAN_POINT ( 'NONE',  ( 101.1158614047228070, -28.69863163947533735, 195.5838086201111992 ) ) ;
#2230 = ORIENTED_EDGE ( 'NONE', *, *, #88066, .F. ) ;
#2231 = CARTESIAN_POINT ( 'NONE',  ( -79.21949419058834962, 93.55466788070657458, 88.20392011030202184 ) ) ;
#2232 = CARTESIAN_POINT ( 'NONE',  ( 104.9598549460505126, -28.12176414095025834, 281.6987261630399644 ) ) ;
#2233 = VECTOR ( 'NONE', #17843, 1000.000000000000114 ) ;
#2234 = ADVANCED_FACE ( 'NONE', ( #77753 ), #41852, .T. ) ;
#2235 = AXIS2_PLACEMENT_3D ( 'NONE', #81438, #46860, #26447 ) ;
#2236 = DIRECTION ( 'NONE',  ( 0.000000000000000000, 0.000000000000000000, 1.000000000000000000 ) ) ;
#2237 = AXIS2_PLACEMENT_3D ( 'NONE', #1823, #57207, #23182 ) ;
#2238 = DIRECTION ( 'NONE',  ( 0.000000000000000000, -1.000000000000000000, 0.000000000000000000 ) ) ;
#2239 = EDGE_CURVE ( 'NONE', #23384, #56843, #21449, .T. ) ;
#2240 = CYLINDRICAL_SURFACE ( 'NONE', #2429, 2.517500000000005844 ) ;
#2241 = VECTOR ( 'NONE', #42500, 1000.000000000000000 ) ;
#2242 = EDGE_LOOP ( 'NONE', ( #82053, #59237, #69794, #15889 ) ) ;
#2243 = CARTESIAN_POINT ( 'NONE',  ( 29.77381068363512995, -48.62134037875389936, 180.4678068554150911 ) ) ;
#2244 = DIRECTION ( 'NONE',  ( -1.000000000000000078E-15, -1.000000000000000083E-30, 1.000000000000000000 ) ) ;
#2245 = VERTEX_POINT ( 'NONE', #15076 ) ;
#2246 = CARTESIAN_POINT ( 'NONE',  ( 98.64717563880898865, -43.89145428829765194, 76.89943479971999807 ) ) ;
#2247 = EDGE_LOOP ( 'NONE', ( #64116, #5451, #68628, #29875 ) ) ;
#2248 = CARTESIAN_POINT ( 'NONE',  ( 116.6246688045503248, -35.02307164793359107, 48.38956268521998538 ) ) ;
#2249 = VECTOR ( 'NONE', #61719, 1000.000000000000000 ) ;
#2250 = CARTESIAN_POINT ( 'NONE',  ( 117.1137397764925794, -36.70408575741609525, 89.82803621957074824 ) ) ;
#2251 = CARTESIAN_POINT ( 'NONE',  ( 99.76930146980365066, -30.21680002102808515, 190.7470538473399415 ) ) ;
#2252 = CARTESIAN_POINT ( 'NONE',  ( 83.56670390244801183, -35.47069715994107497, 218.8274735512160589 ) ) ;
#2253 = DIRECTION ( 'NONE',  ( 0.000000000000000000, 0.000000000000000000, 1.000000000000000000 ) ) ;
#2254 = DIRECTION ( 'NONE',  ( -1.000000000000000000, -1.000000000000000078E-15, 0.000000000000000000 ) ) ;
#2255 = VECTOR ( 'NONE', #7789, 1000.000000000000000 ) ;
#2256 = CARTESIAN_POINT ( 'NONE',  ( 116.5760347145385367, -42.45360038892302157, 274.3832443235299365 ) ) ;
#2257 = VERTEX_POINT ( 'NONE', #538 ) ;
#2258 = CYLINDRICAL_SURFACE ( 'NONE', #76327, 0.5000000000000172085 ) ;
#2259 = ORIENTED_EDGE ( 'NONE', *, *, #67555, .F. ) ;
#2260 = CARTESIAN_POINT ( 'NONE',  ( 108.6553284749260229, -25.75107874774626993, 145.9737205140069420 ) ) ;
#2261 = LINE ( 'NONE', #50383, #1873 ) ;
#2262 = ORIENTED_EDGE ( 'NONE', *, *, #58636, .F. ) ;
#2263 = CIRCLE ( 'NONE', #22569, 7.999999999999992895 ) ;
#2264 = ORIENTED_EDGE ( 'NONE', *, *, #48437, .T. ) ;
#2265 = ORIENTED_EDGE ( 'NONE', *, *, #2519, .F. ) ;
#2266 = CARTESIAN_POINT ( 'NONE',  ( 107.0664832912739399, -36.72944715994095333, 302.4856252759109907 ) ) ;
#2267 = DIRECTION ( 'NONE',  ( 3.100000000000000258E-29, -3.100000000000000044E-14, -1.000000000000000000 ) ) ;
#2268 = CARTESIAN_POINT ( 'NONE',  ( 117.2610056464983899, -34.82931580038571440, 203.9851490854349549 ) ) ;
#2269 = CARTESIAN_POINT ( 'NONE',  ( -462.0260000000000105, 53.97500000000000142, -2.412999999999919876 ) ) ;
#2270 = CARTESIAN_POINT ( 'NONE',  ( 143.6785940946288633, -138.5762527540428835, 247.5817532094160072 ) ) ;
#2271 = DIRECTION ( 'NONE',  ( 0.000000000000000000, 1.000000000000000000, 0.000000000000000000 ) ) ;
#2272 = CARTESIAN_POINT ( 'NONE',  ( 117.5122013968931327, -37.28485508719111863, 14.78419670448294454 ) ) ;
#2273 = DIRECTION ( 'NONE',  ( -1.000000000000000078E-15, 1.000000000000000000, 0.000000000000000000 ) ) ;
#2274 = ORIENTED_EDGE ( 'NONE', *, *, #31325, .T. ) ;
#2275 = CARTESIAN_POINT ( 'NONE',  ( 97.39132285814163481, -39.27863230505913350, 172.5314464909690173 ) ) ;
#2276 = CARTESIAN_POINT ( 'NONE',  ( -48.67264380398864176, 64.60000000000000853, 66.68100227564391957 ) ) ;
#2277 = EDGE_CURVE ( 'NONE', #8532, #10148, #83228, .T. ) ;
#2278 = EDGE_LOOP ( 'NONE', ( #26146, #60774, #48811, #5437, #49983, #10714, #79016, #72653, #66355, #63648, #52989, #54495, #41268, #18003 ) ) ;
#2279 = ORIENTED_EDGE ( 'NONE', *, *, #48571, .T. ) ;
#2280 = CIRCLE ( 'NONE', #86442, 2.117000000000007987 ) ;
#2281 = CARTESIAN_POINT ( 'NONE',  ( -12.69999999999999929, 82.54999999999999716, 129.9368274816650057 ) ) ;
#2282 = CARTESIAN_POINT ( 'NONE',  ( 177.1649999999999920, 5.112500000000000711, -58.73749999999999716 ) ) ;
#2284 = CONICAL_SURFACE ( 'NONE', #26902, 13.31607168056649115, 0.1047197551196538678 ) ;
#2283 = CARTESIAN_POINT ( 'NONE',  ( 110.6887065042383256, -47.98678726807249006, 207.8241967044819489 ) ) ;
#2285 = CARTESIAN_POINT ( 'NONE',  ( 47.62500000000000000, 66.67499999999999716, 292.1000000000000227 ) ) ;
#2286 = EDGE_CURVE ( 'NONE', #58230, #18059, #63217, .T. ) ;
#2287 = CYLINDRICAL_SURFACE ( 'NONE', #65139, 2.117000000000000881 ) ;
#2288 = FACE_OUTER_BOUND ( 'NONE', #45660, .T. ) ;
#2289 = CARTESIAN_POINT ( 'NONE',  ( 98.10212974493634874, -35.44374275293071008, 225.6476579233149948 ) ) ;
#2291 = CARTESIAN_POINT ( 'NONE',  ( 118.7081646409640427, -34.65111545711814500, 44.96705384733895272 ) ) ;
#2290 = FACE_OUTER_BOUND ( 'NONE', #53030, .T. ) ;
#2292 = CARTESIAN_POINT ( 'NONE',  ( 126.3208227659863638, 64.39779484612361671, 32.98409395337385064 ) ) ;
#2293 = CARTESIAN_POINT ( 'NONE',  ( 117.4914506980151572, -37.69211045134998272, 78.75276813305399060 ) ) ;
#2294 = ORIENTED_EDGE ( 'NONE', *, *, #64461, .F. ) ;
#2295 = LINE ( 'NONE', #56326, #17593 ) ;
#2296 = VERTEX_POINT ( 'NONE', #76402 ) ;
#2297 = DIRECTION ( 'NONE',  ( 0.000000000000000000, 0.000000000000000000, -1.000000000000000000 ) ) ;
#2298 = B_SPLINE_CURVE_WITH_KNOTS ( 'NONE', 3,
 ( #3064, #28982, #86185, #14912 ),
 .UNSPECIFIED., .F., .F.,
 ( 4, 4 ),
 ( -0.3974825557268150122, -0.3842043193313849914 ),
 .UNSPECIFIED. ) ;
#2299 = CARTESIAN_POINT ( 'NONE',  ( 100.9524021217529111, -28.70875815854373769, 276.5941401920176190 ) ) ;
#2300 = ORIENTED_EDGE ( 'NONE', *, *, #74106, .T. ) ;
#2301 = CARTESIAN_POINT ( 'NONE',  ( 71.06648329127399677, -8.729447159940999512, 323.8756252759120002 ) ) ;
#2302 = ORIENTED_EDGE ( 'NONE', *, *, #57521, .T. ) ;
#2303 = DIRECTION ( 'NONE',  ( -0.4999999999999989453, -0.8660254037844392627, 2.684678751731760294E-14 ) ) ;
#2304 = CARTESIAN_POINT ( 'NONE',  ( 163.1639762274590169, -34.03355364505800651, 193.9678068554150059 ) ) ;
#2306 = VECTOR ( 'NONE', #60851, 1000.000000000000000 ) ;
#2305 = CARTESIAN_POINT ( 'NONE',  ( 0.000000000000000000, 127.0000000000000000, 0.000000000000000000 ) ) ;
#2307 = ORIENTED_EDGE ( 'NONE', *, *, #46424, .T. ) ;
#2308 = EDGE_CURVE ( 'NONE', #9456, #67515, #7262, .T. ) ;
#2309 = CARTESIAN_POINT ( 'NONE',  ( 114.5834136592134200, -44.03589093681723909, 98.21276813305395592 ) ) ;
#2310 = AXIS2_PLACEMENT_3D ( 'NONE', #35040, #41840, #85017 ) ;
#2311 = VECTOR ( 'NONE', #86354, 1000.000000000000000 ) ;
#2312 = DIRECTION ( 'NONE',  ( 0.000000000000000000, 0.000000000000000000, 1.000000000000000000 ) ) ;
#2313 = CIRCLE ( 'NONE', #50193, 8.636000000000004562 ) ;
#2314 = CARTESIAN_POINT ( 'NONE',  ( 134.0664832912740110, -46.72944715994100306, 4.925625275910997303 ) ) ;
#2315 = CARTESIAN_POINT ( 'NONE',  ( 0.000000000000000000, 117.4749999999999943, -98.14560000000000173 ) ) ;
#2316 = CARTESIAN_POINT ( 'NONE',  ( 127.1498166246069985, 12.92155284005802685, 349.2756252759110680 ) ) ;
#2317 = VERTEX_POINT ( 'NONE', #76849 ) ;
#2318 = CARTESIAN_POINT ( 'NONE',  ( 115.9999835663602425, -32.15690669870756579, 120.2027918068147869 ) ) ;
#2319 = DIRECTION ( 'NONE',  ( 0.000000000000000000, -1.000000000000000000, 0.000000000000000000 ) ) ;
#2320 = DIRECTION ( 'NONE',  ( 0.000000000000000000, 1.000000000000000000, 0.000000000000000000 ) ) ;
#2322 = CYLINDRICAL_SURFACE ( 'NONE', #12343, 9.999999999999998224 ) ;
#2321 = DIRECTION ( 'NONE',  ( 0.000000000000000000, 0.000000000000000000, -1.000000000000000000 ) ) ;
#2323 = FACE_OUTER_BOUND ( 'NONE', #74053, .T. ) ;
#2324 = AXIS2_PLACEMENT_3D ( 'NONE', #19974, #41733, #69919 ) ;
#2325 = EDGE_LOOP ( 'NONE', ( #59045, #35444 ) ) ;
#2326 = AXIS2_PLACEMENT_3D ( 'NONE', #9134, #51327, #50895 ) ;
#2327 = CARTESIAN_POINT ( 'NONE',  ( 47.62500000000000000, 69.84999999999999432, 288.9250000000000114 ) ) ;
#2328 = CARTESIAN_POINT ( 'NONE',  ( 112.4269750522866076, -44.91043508143932428, 174.0384824187679556 ) ) ;
#2329 = EDGE_CURVE ( 'NONE', #89894, #9402, #88512, .T. ) ;
#2331 = ORIENTED_EDGE ( 'NONE', *, *, #77422, .F. ) ;
#2330 = LINE ( 'NONE', #23675, #16717 ) ;
#2332 = CARTESIAN_POINT ( 'NONE',  ( 111.1466539572837320, -45.61852150024213870, 23.91848241876692782 ) ) ;
#2333 = LINE ( 'NONE', #57726, #3410 ) ;
#2334 = CARTESIAN_POINT ( 'NONE',  ( 110.8544976311862627, -45.98422686449477936, 52.88562747957674048 ) ) ;
#2335 = ADVANCED_FACE ( 'NONE', ( #70491 ), #27351, .F. ) ;
#2336 = CARTESIAN_POINT ( 'NONE',  ( 168.0371591254543944, -48.62818131005519717, 249.9678068554149775 ) ) ;
#2337 = CARTESIAN_POINT ( 'NONE',  ( 147.0667039024469886, -67.87844715994090450, 222.2178068554179902 ) ) ;
#2338 = ADVANCED_FACE ( 'NONE', ( #56834 ), #996, .T. ) ;
#2339 = CARTESIAN_POINT ( 'NONE',  ( 98.06605190618643064, -40.64173669134676459, 231.6527681330539679 ) ) ;
#2340 = ORIENTED_EDGE ( 'NONE', *, *, #72951, .F. ) ;
#2341 = VERTEX_POINT ( 'NONE', #1454 ) ;
#2342 = CARTESIAN_POINT ( 'NONE',  ( 102.9614994733801439, -44.58294233512814486, 208.6244404487539725 ) ) ;
#2343 = CARTESIAN_POINT ( 'NONE',  ( 117.0713428532484244, -35.45787740602197857, 54.92720707917401768 ) ) ;
#2344 = CARTESIAN_POINT ( 'NONE',  ( 114.4295241859595933, -42.56572631025478870, 44.73682140113599814 ) ) ;
#2345 = CARTESIAN_POINT ( 'NONE',  ( 23.18046939137932583, 86.82760181162625202, 305.0120167406822702 ) ) ;
#2346 = CARTESIAN_POINT ( 'NONE',  ( -473.2019999999999982, 53.97500000000000142, -1.387778780781445991E-14 ) ) ;
#2347 = EDGE_CURVE ( 'NONE', #70579, #56973, #88091, .T. ) ;
#2348 = CARTESIAN_POINT ( 'NONE',  ( 115.0988951105837117, -100.2184096729307328, 2.217806855417864043 ) ) ;
#2349 = ORIENTED_EDGE ( 'NONE', *, *, #6584, .T. ) ;
#2350 = PLANE ( 'NONE',  #26051 ) ;
#2351 = DIRECTION ( 'NONE',  ( 0.000000000000000000, 1.000000000000000000, 0.000000000000000000 ) ) ;
#2352 = EDGE_CURVE ( 'NONE', #18286, #38056, #51216, .T. ) ;
#2353 = CARTESIAN_POINT ( 'NONE',  ( 97.63514171170966449, -41.12017164899860688, 256.6727681330537507 ) ) ;
#2354 = DIRECTION ( 'NONE',  ( 0.000000000000000000, 1.000000000000000000, 0.000000000000000000 ) ) ;
#2355 = ORIENTED_EDGE ( 'NONE', *, *, #75957, .T. ) ;
#2356 = ORIENTED_EDGE ( 'NONE', *, *, #15049, .T. ) ;
#2357 = DIRECTION ( 'NONE',  ( 1.000000000000000000, 3.999999999999999995E-14, 1.000000000000000078E-15 ) ) ;
#2358 = DIRECTION ( 'NONE',  ( 0.9999999853157766072, 0.0001713722456143218888, 0.000000000000000000 ) ) ;
#2359 = DIRECTION ( 'NONE',  ( 1.000000000000000000, 0.000000000000000000, 0.000000000000000000 ) ) ;
#2360 = CARTESIAN_POINT ( 'NONE',  ( 99.99294959284291906, -33.44233276930008714, 9.425625275910963552 ) ) ;
#2361 = VECTOR ( 'NONE', #14084, 1000.000000000000000 ) ;
#2362 = CARTESIAN_POINT ( 'NONE',  ( 103.0217603822331398, -26.37318333953113836, 16.37276813305293999 ) ) ;
#2364 = DIRECTION ( 'NONE',  ( 0.000000000000000000, 1.000000000000000000, 0.000000000000000000 ) ) ;
#2363 = VECTOR ( 'NONE', #69256, 1000.000000000000000 ) ;
#2365 = ORIENTED_EDGE ( 'NONE', *, *, #71733, .T. ) ;
#2366 = CIRCLE ( 'NONE', #31386, 0.5000000000000004441 ) ;
#2367 = CARTESIAN_POINT ( 'NONE',  ( 118.7813114821712901, -34.63805691389952557, 44.96705384733895272 ) ) ;
#2368 = VECTOR ( 'NONE', #76069, 1000.000000000000000 ) ;
#2369 = DIRECTION ( 'NONE',  ( -0.7071067811864676367, -0.7071067811866273978, -7.071067811864669709E-16 ) ) ;
#2370 = AXIS2_PLACEMENT_3D ( 'NONE', #51800, #58622, #16865 ) ;
#2371 = CARTESIAN_POINT ( 'NONE',  ( 105.0216316738932107, -25.86677467614671500, 280.2365776568631759 ) ) ;
#2372 = ORIENTED_EDGE ( 'NONE', *, *, #78459, .F. ) ;
#2373 = CARTESIAN_POINT ( 'NONE',  ( 82.57637212004242144, -17.60518726036903203, 2.783021291305785905 ) ) ;
#2374 = CARTESIAN_POINT ( 'NONE',  ( 97.81863755922226744, -40.53440256270629760, 17.63675073572146346 ) ) ;
#2375 = CARTESIAN_POINT ( 'NONE',  ( 160.7738106836350482, -48.62134037874900372, 180.4678068554150059 ) ) ;
#2376 = CARTESIAN_POINT ( 'NONE',  ( 99.60924227704973077, -33.40991670024246218, 98.81094751244894780 ) ) ;
#2377 = CARTESIAN_POINT ( 'NONE',  ( 99.06932979199925171, -29.95266829982950441, 211.7670538473399517 ) ) ;
#2378 = FACE_OUTER_BOUND ( 'NONE', #26754, .T. ) ;
#2379 = ORIENTED_EDGE ( 'NONE', *, *, #6516, .F. ) ;
#2380 = VECTOR ( 'NONE', #46487, 1000.000000000000000 ) ;
#2381 = DIRECTION ( 'NONE',  ( 0.7071067811861589947, -0.7071067811869361508, 0.000000000000000000 ) ) ;
#2382 = ORIENTED_EDGE ( 'NONE', *, *, #13447, .T. ) ;
#2383 = EDGE_LOOP ( 'NONE', ( #3491, #12437, #2480, #38867, #9258 ) ) ;
#2384 = CARTESIAN_POINT ( 'NONE',  ( 95.60734603896358408, -36.72944715994100306, 300.2406250056037038 ) ) ;
#2385 = VERTEX_POINT ( 'NONE', #5011 ) ;
#2386 = ORIENTED_EDGE ( 'NONE', *, *, #75745, .F. ) ;
#2387 = CARTESIAN_POINT ( 'NONE',  ( 76.20505178924389611, 120.6499999999999915, -76.20505178924359768 ) ) ;
#2388 = AXIS2_PLACEMENT_3D ( 'NONE', #47422, #61503, #12935 ) ;
#2389 = ADVANCED_FACE ( 'NONE', ( #87244 ), #10927, .F. ) ;
#2390 = B_SPLINE_CURVE_WITH_KNOTS ( 'NONE', 3,
 ( #7423, #48730, #29221, #63284, #69654, #35115, #62824, #602, #15597, #21515, #1060, #56908, #49185, #76919, #50085, #77819, #28770, #38692, #65952, #44608, #2409, #23754, #23321, #16931, #36922, #64624, #51861, #72344, #10111, #66397, #17814, #71461, #50987, #43722, #17371, #51422, #9224, #38255, #78728, #16485, #79171, #4187, #37820, #65074, #58684 ),
 .UNSPECIFIED., .F., .F.,
 ( 4, 2, 2, 2, 1, 1, 2, 2, 2, 1, 1, 2, 2, 2, 2, 1, 1, 1, 2, 2, 2, 2, 1, 1, 2, 2, 4 ),
 ( 0.000000000000000000, 0.03125000000003638062, 0.04687500000005471318, 0.06250000000007303880, 0.09375000000011092516, 0.1093750000001298545, 0.1171875000001566386, 0.1250000000001834088, 0.1875000000003400336, 0.2187500000004195255, 0.2343750000004746481, 0.2421875000004988232, 0.2500000000005230261, 0.3750000000008891776, 0.4375000000010721979, 0.4687500000011416423, 0.4843750000011794454, 0.4921875000012016499, 0.4960937500012127521, 0.5000000000012239099, 0.6250000000010771384, 0.6875000000010104140, 0.7187500000009768852, 0.7343750000009601209, 0.7421875000009404699, 0.7500000000009208190, 1.000000000000000000 ),
 .UNSPECIFIED. ) ;
#2391 = CARTESIAN_POINT ( 'NONE',  ( 112.1370707133610551, -28.01151978404558207, 24.65666564914236858 ) ) ;
#2392 = CARTESIAN_POINT ( 'NONE',  ( 100.0120368033278311, -41.59636475471172901, 126.2295626852199746 ) ) ;
#2393 = CARTESIAN_POINT ( 'NONE',  ( 111.7490138926534797, -27.39026733005105640, 279.7070538473396937 ) ) ;
#2394 = DIRECTION ( 'NONE',  ( 0.000000000000000000, 0.000000000000000000, 1.000000000000000000 ) ) ;
#2395 = ORIENTED_EDGE ( 'NONE', *, *, #26112, .F. ) ;
#2396 = VERTEX_POINT ( 'NONE', #53574 ) ;
#2397 = FACE_OUTER_BOUND ( 'NONE', #40658, .T. ) ;
#2398 = DIRECTION ( 'NONE',  ( 0.000000000000000000, 1.000000000000000000, 0.000000000000000000 ) ) ;
#2399 = DIRECTION ( 'NONE',  ( 0.8660254037844382635, 0.5000000000000008882, -1.550000000000000022E-14 ) ) ;
#2400 = AXIS2_PLACEMENT_3D ( 'NONE', #64029, #1806, #29505 ) ;
#2401 = DIRECTION ( 'NONE',  ( 0.000000000000000000, -1.000000000000000000, 0.000000000000000000 ) ) ;
#2402 = ORIENTED_EDGE ( 'NONE', *, *, #19038, .F. ) ;
#2403 = EDGE_CURVE ( 'NONE', #22043, #36708, #81778, .T. ) ;
#2404 = PRODUCT_DEFINITION_CONTEXT ( 'detailed design', #26055, 'design' ) ;
#2405 = CARTESIAN_POINT ( 'NONE',  ( 108.0141129856239957, -24.91663700320364327, 265.0127681330535552 ) ) ;
#2406 = CARTESIAN_POINT ( 'NONE',  ( 96.67145939589113368, -37.96898657530446997, 37.42133956162496844 ) ) ;
#2407 = CARTESIAN_POINT ( 'NONE',  ( 270.8910000000000196, 40.03750000000000142, -67.11950000000000216 ) ) ;
#2409 = CARTESIAN_POINT ( 'NONE',  ( 68.75201276470878042, -139.2464705024164857, 246.2314480513125261 ) ) ;
#2408 = CARTESIAN_POINT ( 'NONE',  ( 123.6837132603318992, -16.81243780205710436, 239.5838068554165545 ) ) ;
#2410 = FACE_OUTER_BOUND ( 'NONE', #58762, .T. ) ;
#2411 = CYLINDRICAL_SURFACE ( 'NONE', #66983, 2.500000000000002220 ) ;
#2412 = CARTESIAN_POINT ( 'NONE',  ( -469.3583484187089994, 53.97500000000000142, -3.174999999999999822 ) ) ;
#2413 = LINE ( 'NONE', #16050, #15526 ) ;
#2414 = EDGE_CURVE ( 'NONE', #34580, #72320, #63, .T. ) ;
#2415 = DIRECTION ( 'NONE',  ( 1.000000000000000000, 0.000000000000000000, 0.000000000000000000 ) ) ;
#2416 = FACE_OUTER_BOUND ( 'NONE', #34062, .T. ) ;
#2417 = ADVANCED_FACE ( 'NONE', ( #39969 ), #32256, .T. ) ;
#2418 = DIRECTION ( 'NONE',  ( 0.7071067811865187069, 0.7071067811865764385, 7.071067811865181482E-16 ) ) ;
#2419 = CARTESIAN_POINT ( 'NONE',  ( 97.19579330311479737, -33.30690068839255957, 286.0613395616251751 ) ) ;
#2420 = CARTESIAN_POINT ( 'NONE',  ( 103.5424053135282634, -26.88047730603072694, 186.3499109901969746 ) ) ;
#2421 = CARTESIAN_POINT ( 'NONE',  ( 104.6438654950096350, -47.53759819287119370, 23.38895860924494841 ) ) ;
#2422 = VECTOR ( 'NONE', #86944, 1000.000000000000000 ) ;
#2424 = CARTESIAN_POINT ( 'NONE',  ( 0.000000000000000000, 127.0000000000000000, 0.000000000000000000 ) ) ;
#2423 = CARTESIAN_POINT ( 'NONE',  ( 61.56670390244634916, -23.42844715994043270, 180.4678068554151196 ) ) ;
#2425 = CARTESIAN_POINT ( 'NONE',  ( 41.56648329127399677, -18.82844715994099971, 16.80862527591200006 ) ) ;
#2426 = CIRCLE ( 'NONE', #50253, 3.299999999999997158 ) ;
#2427 = AXIS2_PLACEMENT_3D ( 'NONE', #81072, #79730, #72455 ) ;
#2428 = AXIS2_PLACEMENT_3D ( 'NONE', #75182, #5245, #32934 ) ;
#2429 = AXIS2_PLACEMENT_3D ( 'NONE', #71288, #17648, #29491 ) ;
#2430 = EDGE_CURVE ( 'NONE', #52659, #76993, #18186, .T. ) ;
#2431 = VERTEX_POINT ( 'NONE', #19529 ) ;
#2432 = LINE ( 'NONE', #50105, #73729 ) ;
#2433 = ORIENTED_EDGE ( 'NONE', *, *, #81943, .F. ) ;
#2434 = CARTESIAN_POINT ( 'NONE',  ( 116.8058161338297509, -37.62879752186919546, 74.75276813305298163 ) ) ;
#2436 = ORIENTED_EDGE ( 'NONE', *, *, #62322, .T. ) ;
#2435 = CARTESIAN_POINT ( 'NONE',  ( 31.90335556477753087, -33.89581943344372661, 117.4678068554150485 ) ) ;
#2437 = FACE_OUTER_BOUND ( 'NONE', #38144, .T. ) ;
#2438 = CARTESIAN_POINT ( 'NONE',  ( 97.42226921825846375, -40.63044708855864684, 202.6327681330539860 ) ) ;
#2439 = DIRECTION ( 'NONE',  ( 1.000000000000000000, 0.000000000000000000, 0.000000000000000000 ) ) ;
#2440 = CARTESIAN_POINT ( 'NONE',  ( 152.0371591254585155, -47.82818131005588214, 193.9678068554149775 ) ) ;
#2441 = DIRECTION ( 'NONE',  ( 1.000000000000000000, 4.299999999999999979E-14, 1.000000000000000078E-15 ) ) ;
#2442 = EDGE_CURVE ( 'NONE', #6249, #50785, #59903, .T. ) ;
#2443 = CARTESIAN_POINT ( 'NONE',  ( 107.0664832912739399, -36.72944715994095333, 302.6356252759109680 ) ) ;
#2444 = CARTESIAN_POINT ( 'NONE',  ( -7.199374239792870816E-13, 101.5999999999999943, 98.14560000000000173 ) ) ;
#2445 = CARTESIAN_POINT ( 'NONE',  ( 101.9926790296990617, -45.44549198893967201, 97.15644839471165994 ) ) ;
#2446 = CARTESIAN_POINT ( 'NONE',  ( 114.2951562036313646, -44.16484043540982185, 118.2022919425779719 ) ) ;
#2447 = ORIENTED_EDGE ( 'NONE', *, *, #64197, .F. ) ;
#2448 = ORIENTED_EDGE ( 'NONE', *, *, #1323, .T. ) ;
#2449 = CARTESIAN_POINT ( 'NONE',  ( 98.70151408295986073, -32.45115127476004346, 92.39396425827794701 ) ) ;
#2450 = CLOSED_SHELL ( 'NONE', ( #67978, #44873, #65919, #73944, #9506, #75828, #29716, #45419, #66834, #4528 ) ) ;
#2451 = DIRECTION ( 'NONE',  ( -1.000000000000000000, -4.299999999999999979E-14, -1.000000000000000078E-15 ) ) ;
#2453 = DIRECTION ( 'NONE',  ( 0.000000000000000000, 1.000000000000000000, 0.000000000000000000 ) ) ;
#2452 = CARTESIAN_POINT ( 'NONE',  ( 104.0204373342842814, -47.42213563049708824, 213.3556252759109668 ) ) ;
#2454 = CYLINDRICAL_SURFACE ( 'NONE', #20307, 2.500000000000002220 ) ;
#2455 = DIRECTION ( 'NONE',  ( 0.000000000000000000, -1.000000000000000000, 0.000000000000000000 ) ) ;
#2456 = CARTESIAN_POINT ( 'NONE',  ( -72.96458098368600531, 127.0000000000000000, -67.92268098368781182 ) ) ;
#2457 = EDGE_CURVE ( 'NONE', #48113, #52443, #27414, .T. ) ;
#2458 = DIRECTION ( 'NONE',  ( 0.000000000000000000, 1.000000000000000000, 0.000000000000000000 ) ) ;
#2459 = CARTESIAN_POINT ( 'NONE',  ( 9.196777273860476498, 73.92746944614621896, 118.1991088758754813 ) ) ;
#2460 = EDGE_CURVE ( 'NONE', #38655, #6628, #78419, .T. ) ;
#2461 = CARTESIAN_POINT ( 'NONE',  ( 97.76587557681018836, -42.65924729906321744, 141.7661014663869707 ) ) ;
#2462 = VERTEX_POINT ( 'NONE', #84014 ) ;
#2463 = ORIENTED_EDGE ( 'NONE', *, *, #46767, .F. ) ;
#2464 = ORIENTED_EDGE ( 'NONE', *, *, #38378, .T. ) ;
#2465 = ADVANCED_FACE ( 'NONE', ( #40860 ), #14970, .F. ) ;
#2466 = CARTESIAN_POINT ( 'NONE',  ( 145.2750608293226833, -69.56425712815943996, 247.5000682988239760 ) ) ;
#2467 = CARTESIAN_POINT ( 'NONE',  ( 146.2016781114348305, -68.71199849507584645, 247.1480963241265272 ) ) ;
#2468 = EDGE_CURVE ( 'NONE', #11178, #18383, #21790, .T. ) ;
#2469 = CARTESIAN_POINT ( 'NONE',  ( 172.5664832912728457, -27.82844715994070484, 141.9256252759119832 ) ) ;
#2470 = CARTESIAN_POINT ( 'NONE',  ( 98.38024141146789248, -41.69495811671281160, 102.7397364358299683 ) ) ;
#2471 = CARTESIAN_POINT ( 'NONE',  ( 115.6591437269271694, -35.69643618062379176, 236.7518998934009460 ) ) ;
#2472 = TOROIDAL_SURFACE ( 'NONE', #43088, 13.50000000000000000, 0.5000000000000000000 ) ;
#2473 = DIRECTION ( 'NONE',  ( -0.000000000000000000, 1.000000000000000000, 0.000000000000000000 ) ) ;
#2474 = CARTESIAN_POINT ( 'NONE',  ( 104.5625478726873894, -48.31265885861421339, 182.4070538473399665 ) ) ;
#2475 = FACE_OUTER_BOUND ( 'NONE', #4820, .T. ) ;
#2476 = EDGE_LOOP ( 'NONE', ( #82219, #32746, #88557, #78259, #36525, #35506, #87850, #66493, #83455, #35952, #23042, #13862, #17754, #32156, #54995, #34490 ) ) ;
#2478 = ORIENTED_EDGE ( 'NONE', *, *, #80459, .F. ) ;
#2477 = EDGE_LOOP ( 'NONE', ( #89283, #43761, #21479, #6064, #55922 ) ) ;
#2479 = DIRECTION ( 'NONE',  ( 0.000000000000000000, 0.000000000000000000, -1.000000000000000000 ) ) ;
#2480 = ORIENTED_EDGE ( 'NONE', *, *, #65974, .F. ) ;
#2481 = ORIENTED_EDGE ( 'NONE', *, *, #35705, .F. ) ;
#2482 = CARTESIAN_POINT ( 'NONE',  ( 204.2160000000000082, 52.73749999999999716, -40.48124999999945572 ) ) ;
#2483 = CARTESIAN_POINT ( 'NONE',  ( 133.6902059199614143, -33.99866847873242648, 8.209451181318698332 ) ) ;
#2484 = CARTESIAN_POINT ( 'NONE',  ( 106.3528233092926740, -46.09786297945525035, 263.9596785439923678 ) ) ;
#2485 = CARTESIAN_POINT ( 'NONE',  ( 116.3114837287122754, -32.94280867712679850, 274.1356252759109680 ) ) ;
#2486 = ORIENTED_EDGE ( 'NONE', *, *, #31297, .F. ) ;
#2487 = AXIS2_PLACEMENT_3D ( 'NONE', #78848, #86101, #15719 ) ;
#2488 = AXIS2_PLACEMENT_3D ( 'NONE', #42561, #63024, #42126 ) ;
#2489 = CARTESIAN_POINT ( 'NONE',  ( 114.0969355440510355, -42.17668752783679054, 9.635625275910941312 ) ) ;
#2490 = FACE_BOUND ( 'NONE', #213, .T. ) ;
#2491 = VERTEX_POINT ( 'NONE', #20881 ) ;
#2492 = VERTEX_POINT ( 'NONE', #35841 ) ;
#2493 = VECTOR ( 'NONE', #56354, 1000.000000000000000 ) ;
#2494 = VECTOR ( 'NONE', #83577, 1000.000000000000000 ) ;
#2495 = DIRECTION ( 'NONE',  ( 0.000000000000000000, 0.000000000000000000, -1.000000000000000000 ) ) ;
#2496 = AXIS2_PLACEMENT_3D ( 'NONE', #9728, #36987, #56519 ) ;
#2497 = ORIENTED_EDGE ( 'NONE', *, *, #86925, .T. ) ;
#2498 = ORIENTED_EDGE ( 'NONE', *, *, #31190, .T. ) ;
#2499 = EDGE_CURVE ( 'NONE', #28622, #16389, #84475, .T. ) ;
#2500 = CARTESIAN_POINT ( 'NONE',  ( 114.7745679063646378, -33.04956858091291139, 18.60384839950496172 ) ) ;
#2501 = CARTESIAN_POINT ( 'NONE',  ( 117.0895389762686136, -39.67643183956238317, 183.5984824187679578 ) ) ;
#2502 = CARTESIAN_POINT ( 'NONE',  ( 97.76587557681018836, -42.65924729906321744, 141.7661014663869707 ) ) ;
#2503 = CARTESIAN_POINT ( 'NONE',  ( 182.5667039024459939, -19.82844715994031759, 342.9256252759109884 ) ) ;
#2504 = CARTESIAN_POINT ( 'NONE',  ( 115.9598434605651107, -30.16574962093465828, 255.3203871806729524 ) ) ;
#2505 = DIRECTION ( 'NONE',  ( 1.000000000000000000, 0.000000000000000000, 0.000000000000000000 ) ) ;
#2506 = CARTESIAN_POINT ( 'NONE',  ( 71.09939861440099662, 20.32000000000000028, 177.8662485265279827 ) ) ;
#2507 = CARTESIAN_POINT ( 'NONE',  ( -130.2871811975775813, 72.98383416765817344, 8.394281761909056172 ) ) ;
#2508 = ORIENTED_EDGE ( 'NONE', *, *, #15756, .F. ) ;
#2509 = VERTEX_POINT ( 'NONE', #14062 ) ;
#2510 = AXIS2_PLACEMENT_3D ( 'NONE', #86283, #13549, #13115 ) ;
#2511 = CIRCLE ( 'NONE', #89528, 0.5000000000000004441 ) ;
#2512 = CARTESIAN_POINT ( 'NONE',  ( 109.4554010020096513, -25.88943074854985227, 179.8918157521019339 ) ) ;
#2513 = ORIENTED_EDGE ( 'NONE', *, *, #76054, .F. ) ;
#2514 = EDGE_CURVE ( 'NONE', #12810, #44525, #54917, .T. ) ;
#2515 = CARTESIAN_POINT ( 'NONE',  ( 111.4173512164996254, -47.75262429423162303, 172.8756252759109771 ) ) ;
#2516 = CARTESIAN_POINT ( 'NONE',  ( -24.79284581386642827, 184.0000000000000000, 0.000000000000000000 ) ) ;
#2517 = CARTESIAN_POINT ( 'NONE',  ( 136.5173892390752712, -35.48112160756611644, 7.135585143040955813 ) ) ;
#2518 = CARTESIAN_POINT ( 'NONE',  ( 51.06648329127330044, -0.7548456658612000547, 331.7756252759120343 ) ) ;
#2519 = EDGE_CURVE ( 'NONE', #38575, #4939, #34813, .T. ) ;
#2522 = CARTESIAN_POINT ( 'NONE',  ( 96.79764630557892247, -40.75620882907055176, 242.6118157521009664 ) ) ;
#2521 = CARTESIAN_POINT ( 'NONE',  ( 90.44969454456413871, -53.34645651782494724, 239.5838068554169809 ) ) ;
#2520 = CARTESIAN_POINT ( 'NONE',  ( 98.00595362218291484, -39.44849273793310829, 277.6356252759110248 ) ) ;
#2523 = LINE ( 'NONE', #57915, #19075 ) ;
#2524 = DIRECTION ( 'NONE',  ( 0.000000000000000000, 0.000000000000000000, 1.000000000000000000 ) ) ;
#2525 = DIRECTION ( 'NONE',  ( 0.000000000000000000, 1.000000000000000000, 0.000000000000000000 ) ) ;
#2526 = EDGE_CURVE ( 'NONE', #8195, #79540, #13099, .T. ) ;
#2527 = CARTESIAN_POINT ( 'NONE',  ( 107.0664832912739399, -36.72944715994096754, 299.5704287327187103 ) ) ;
#2528 = CARTESIAN_POINT ( 'NONE',  ( 176.7738106835694225, -48.62134037881071436, 249.9678068554149775 ) ) ;
#2529 = EDGE_CURVE ( 'NONE', #54739, #53364, #18864, .T. ) ;
#2530 = CARTESIAN_POINT ( 'NONE',  ( 73.06670390244801183, -58.72944715994112386, 198.9178068554149945 ) ) ;
#2532 = ORIENTED_EDGE ( 'NONE', *, *, #31514, .F. ) ;
#2531 = CARTESIAN_POINT ( 'NONE',  ( 114.8835829893441911, -32.52868086562086347, 195.5838068554168103 ) ) ;
#2533 = EDGE_CURVE ( 'NONE', #69150, #57574, #33384, .T. ) ;
#2534 = DIRECTION ( 'NONE',  ( -3.100000000000000258E-29, 3.100000000000000044E-14, 1.000000000000000000 ) ) ;
#2535 = CARTESIAN_POINT ( 'NONE',  ( 107.5668325082694139, -47.79493819276859057, 192.6003871806729535 ) ) ;
#2536 = CARTESIAN_POINT ( 'NONE',  ( 98.64735160015825954, -43.89130460420365409, 72.89943479972099283 ) ) ;
#2537 = CARTESIAN_POINT ( 'NONE',  ( 98.34346157482828232, -29.86603762143552032, 196.8080062282919869 ) ) ;
#2538 = DIRECTION ( 'NONE',  ( 0.000000000000000000, 0.000000000000000000, 1.000000000000000000 ) ) ;
#2539 = PLANE ( 'NONE',  #66307 ) ;
#2541 = LINE ( 'NONE', #8919, #2241 ) ;
#2540 = LINE ( 'NONE', #62954, #23247 ) ;
#2542 = CARTESIAN_POINT ( 'NONE',  ( 115.0889047250496304, -30.61763668164335428, 69.34395860908813347 ) ) ;
#2543 = DIRECTION ( 'NONE',  ( -0.000000000000000000, -0.000000000000000000, 1.000000000000000000 ) ) ;
#2544 = VERTEX_POINT ( 'NONE', #49909 ) ;
#2545 = VECTOR ( 'NONE', #22991, 1000.000000000000000 ) ;
#2546 = ADVANCED_FACE ( 'NONE', ( #57172 ), #77642, .F. ) ;
#2547 = DIRECTION ( 'NONE',  ( 0.000000000000000000, 0.000000000000000000, 1.000000000000000000 ) ) ;
#2548 = EDGE_CURVE ( 'NONE', #85262, #26105, #68216, .T. ) ;
#2549 = VERTEX_POINT ( 'NONE', #51694 ) ;
#2550 = ORIENTED_EDGE ( 'NONE', *, *, #83461, .F. ) ;
#2551 = CARTESIAN_POINT ( 'NONE',  ( 114.8228036748933079, -33.15234975719755539, 103.5924198280769843 ) ) ;
#2553 = EDGE_LOOP ( 'NONE', ( #85925, #24242, #36675, #80564 ) ) ;
#2552 = CARTESIAN_POINT ( 'NONE',  ( -12.70000000000000107, 82.54999999999999716, -129.9368274816650910 ) ) ;
#2554 = CARTESIAN_POINT ( 'NONE',  ( 115.2499566122392736, -44.12502604085369029, 79.25372051400697160 ) ) ;
#2555 = CARTESIAN_POINT ( 'NONE',  ( 123.6837132603319560, -53.34645651782485487, 229.5838068554170093 ) ) ;
#2556 = EDGE_CURVE ( 'NONE', #76619, #84501, #79441, .T. ) ;
#2557 = DIRECTION ( 'NONE',  ( 1.000000000000000000, 3.999999999999999995E-14, 1.000000000000000078E-15 ) ) ;
#2558 = DIRECTION ( 'NONE',  ( 0.000000000000000000, 0.000000000000000000, 1.000000000000000000 ) ) ;
#2559 = VECTOR ( 'NONE', #87502, 1000.000000000000000 ) ;
#2560 = CARTESIAN_POINT ( 'NONE',  ( 106.6352542858682284, -26.36832623700835398, 40.09753003781596448 ) ) ;
#2561 = ORIENTED_EDGE ( 'NONE', *, *, #35543, .T. ) ;
#2562 = ORIENTED_EDGE ( 'NONE', *, *, #7027, .T. ) ;
#2563 = ORIENTED_EDGE ( 'NONE', *, *, #89281, .T. ) ;
#2564 = AXIS2_PLACEMENT_3D ( 'NONE', #83197, #46395, #47297 ) ;
#2565 = AXIS2_PLACEMENT_3D ( 'NONE', #44897, #9954, #78999 ) ;
#2566 = LINE ( 'NONE', #87458, #12345 ) ;
#2567 = CARTESIAN_POINT ( 'NONE',  ( 57.14999999999999858, 60.86974387893089755, 323.0879999999999654 ) ) ;
#2568 = DIRECTION ( 'NONE',  ( 0.000000000000000000, 0.000000000000000000, 1.000000000000000000 ) ) ;
#2569 = DIRECTION ( 'NONE',  ( -1.000000000000000000, 0.000000000000000000, 0.000000000000000000 ) ) ;
#2570 = DIRECTION ( 'NONE',  ( 0.7071067811868672059, 0.7071067811862279395, 6.612322855857878503E-17 ) ) ;
#2571 = CARTESIAN_POINT ( 'NONE',  ( 97.78477890316482046, -40.45109945164446685, 52.62952827575012549 ) ) ;
#2572 = CARTESIAN_POINT ( 'NONE',  ( 67.06681736700808472, -67.87844715931913697, 245.5130139978070076 ) ) ;
#2573 = CARTESIAN_POINT ( 'NONE',  ( -6.676094946653681639, 93.36325093810603448, 130.3857439148796686 ) ) ;
#2574 = CARTESIAN_POINT ( 'NONE',  ( 114.3378803067696765, -44.16957155219879638, 73.19276813305397411 ) ) ;
#2575 = ORIENTED_EDGE ( 'NONE', *, *, #75040, .T. ) ;
#2576 = ADVANCED_FACE ( 'NONE', ( #43542 ), #65345, .F. ) ;
#2577 = VECTOR ( 'NONE', #78490, 1000.000000000000000 ) ;
#2578 = CARTESIAN_POINT ( 'NONE',  ( 102.0670556523651129, -27.97049767320797642, 270.4897918799564422 ) ) ;
#2579 = VECTOR ( 'NONE', #6464, 1000.000000000000000 ) ;
#2580 = EDGE_CURVE ( 'NONE', #65668, #43936, #65776, .T. ) ;
#2581 = VECTOR ( 'NONE', #41232, 1000.000000000000000 ) ;
#2582 = LINE ( 'NONE', #30278, #40896 ) ;
#2583 = CARTESIAN_POINT ( 'NONE',  ( 114.7692409103599687, -39.43078961860824450, 131.3766617981629565 ) ) ;
#2584 = AXIS2_PLACEMENT_3D ( 'NONE', #60286, #27574, #40741 ) ;
#2585 = CARTESIAN_POINT ( 'NONE',  ( 97.80804003460494300, -40.50849928945232392, 96.63485748601286218 ) ) ;
#2586 = DIRECTION ( 'NONE',  ( 0.7071067811739204512, -0.7071067811991745833, 0.000000000000000000 ) ) ;
#2587 = ORIENTED_EDGE ( 'NONE', *, *, #83860, .T. ) ;
#2588 = ORIENTED_EDGE ( 'NONE', *, *, #74749, .T. ) ;
#2589 = CARTESIAN_POINT ( 'NONE',  ( -72.96458098368600531, 117.4749999999999943, -72.96458098368781009 ) ) ;
#2590 = ORIENTED_EDGE ( 'NONE', *, *, #8065, .T. ) ;
#2591 = VERTEX_POINT ( 'NONE', #16310 ) ;
#2592 = CARTESIAN_POINT ( 'NONE',  ( 99.50276801249795255, -32.11225214635365433, 167.3215833058969793 ) ) ;
#2593 = LINE ( 'NONE', #1698, #76570 ) ;
#2594 = CARTESIAN_POINT ( 'NONE',  ( 97.81677459100555438, -31.87350772351088679, 131.9413395616259947 ) ) ;
#2595 = CARTESIAN_POINT ( 'NONE',  ( 97.31584367109211087, -39.30597582529259171, 121.5314585950798403 ) ) ;
#2596 = VECTOR ( 'NONE', #70871, 1000.000000000000114 ) ;
#2597 = CARTESIAN_POINT ( 'NONE',  ( 117.0897445426788295, -37.64026809670689744, 18.75396567128554892 ) ) ;
#2598 = ORIENTED_EDGE ( 'NONE', *, *, #57285, .F. ) ;
#2599 = ORIENTED_EDGE ( 'NONE', *, *, #69975, .F. ) ;
#2600 = EDGE_LOOP ( 'NONE', ( #46917, #45524, #28204, #67495 ) ) ;
#2601 = CARTESIAN_POINT ( 'NONE',  ( 102.5899018517108772, -44.13627803831183627, 199.9499951314959674 ) ) ;
#2602 = CARTESIAN_POINT ( 'NONE',  ( 104.7546666864753320, -46.91776733316893200, 72.39848241876795498 ) ) ;
#2603 = VERTEX_POINT ( 'NONE', #29488 ) ;
#2604 = CARTESIAN_POINT ( 'NONE',  ( 115.5933672690474765, -28.53551910654237389, 39.43562527591099354 ) ) ;
#2605 = CARTESIAN_POINT ( 'NONE',  ( 104.4482647075962518, -26.61598136914473400, 196.2784824187679362 ) ) ;
#2606 = DIRECTION ( 'NONE',  ( 0.000000000000000000, -9.999999999999953445E-16, 1.000000000000000000 ) ) ;
#2607 = CARTESIAN_POINT ( 'NONE',  ( 97.81168569434709070, -40.51740311210409828, 127.6359003399277441 ) ) ;
#2608 = CARTESIAN_POINT ( 'NONE',  ( 108.2766895582742848, -26.33922418024667422, 125.9841967044819597 ) ) ;
#2609 = FACE_BOUND ( 'NONE', #21078, .T. ) ;
#2610 = ORIENTED_EDGE ( 'NONE', *, *, #83767, .T. ) ;
#2611 = DIRECTION ( 'NONE',  ( 1.000000000000000000, 0.000000000000000000, 0.000000000000000000 ) ) ;
#2612 = AXIS2_PLACEMENT_3D ( 'NONE', #50412, #86290, #24070 ) ;
#2613 = ORIENTED_EDGE ( 'NONE', *, *, #68493, .T. ) ;
#2614 = DIRECTION ( 'NONE',  ( 0.000000000000000000, 0.000000000000000000, 1.000000000000000000 ) ) ;
#2615 = CARTESIAN_POINT ( 'NONE',  ( -7.205548786489490269E-13, 127.0000000000000000, 103.1875000000000000 ) ) ;
#2616 = VERTEX_POINT ( 'NONE', #86241 ) ;
#2617 = CIRCLE ( 'NONE', #35929, 25.39999999999999858 ) ;
#2618 = CARTESIAN_POINT ( 'NONE',  ( 116.3259679314843282, -32.93868236591013243, 264.1356252759109680 ) ) ;
#2619 = AXIS2_PLACEMENT_3D ( 'NONE', #65973, #78755, #30135 ) ;
#2620 = CARTESIAN_POINT ( 'NONE',  ( 107.0664832912739968, 19.62155284005901024, 330.1506252759110680 ) ) ;
#2621 = CARTESIAN_POINT ( 'NONE',  ( 96.92686062739846875, -39.15330414739766240, 56.51276813305394597 ) ) ;
#2622 = DIRECTION ( 'NONE',  ( 0.7071067811866516006, -0.7071067811864434338, 0.000000000000000000 ) ) ;
#2623 = ADVANCED_FACE ( 'NONE', ( #24020 ), #36754, .T. ) ;
#2624 = DIRECTION ( 'NONE',  ( -4.237773401492740281E-14, 1.000000000000000000, 0.000000000000000000 ) ) ;
#2625 = FACE_OUTER_BOUND ( 'NONE', #55968, .T. ) ;
#2626 = ADVANCED_FACE ( 'NONE', ( #43089 ), #43987, .F. ) ;
#2627 = CARTESIAN_POINT ( 'NONE',  ( 113.0644005321300511, -46.09090919705352718, 68.02991099019695298 ) ) ;
#2629 = CARTESIAN_POINT ( 'NONE',  ( 98.00553567079155926, -41.84099229931889852, 132.7356252759109623 ) ) ;
#2628 = CARTESIAN_POINT ( 'NONE',  ( 181.8884939055946575, -32.11662333283960180, 237.4678068554150059 ) ) ;
#2630 = LINE ( 'NONE', #24848, #17598 ) ;
#2631 = CARTESIAN_POINT ( 'NONE',  ( 74.15067561874209900, 120.6499999999999915, 68.53801554307469246 ) ) ;
#2632 = ORIENTED_EDGE ( 'NONE', *, *, #298, .T. ) ;
#2633 = DIRECTION ( 'NONE',  ( 0.000000000000000000, 0.000000000000000000, -1.000000000000000000 ) ) ;
#2635 = EDGE_CURVE ( 'NONE', #72873, #48257, #4414, .T. ) ;
#2634 = AXIS2_PLACEMENT_3D ( 'NONE', #66343, #30502, #71407 ) ;
#2636 = DIRECTION ( 'NONE',  ( 0.000000000000000000, 0.000000000000000000, -1.000000000000000000 ) ) ;
#2637 = CARTESIAN_POINT ( 'NONE',  ( 25.56670390244797275, -62.87844715994099687, 137.2178068554150059 ) ) ;
#2638 = VECTOR ( 'NONE', #4954, 1000.000000000000000 ) ;
#2639 = EDGE_CURVE ( 'NONE', #28741, #49561, #9054, .T. ) ;
#2640 = DIRECTION ( 'NONE',  ( -1.000000000000000078E-15, 1.000000000000000083E-30, 1.000000000000000000 ) ) ;
#2642 = ORIENTED_EDGE ( 'NONE', *, *, #1443, .F. ) ;
#2641 = CARTESIAN_POINT ( 'NONE',  ( 99.05215007911658631, -29.93811023049936892, 215.7670538473399517 ) ) ;
#2643 = CARTESIAN_POINT ( 'NONE',  ( 33.78309357196258844, -29.99615139349924675, 342.9256252759109884 ) ) ;
#2644 = CARTESIAN_POINT ( 'NONE',  ( 96.75123844313058896, -34.86533355485506291, 237.1841967044819626 ) ) ;
#2645 = CARTESIAN_POINT ( 'NONE',  ( 96.74875621672018156, -38.50074266403909462, 87.46133956162493917 ) ) ;
#2646 = CIRCLE ( 'NONE', #25835, 4.875000000000017764 ) ;
#2647 = CARTESIAN_POINT ( 'NONE',  ( 194.0667039024479834, -40.32844715993407902, 300.4678068554149490 ) ) ;
#2648 = VECTOR ( 'NONE', #89767, 1000.000000000000000 ) ;
#2649 = CARTESIAN_POINT ( 'NONE',  ( 99.09497285450953541, -30.55141387270104048, 191.8022096076827552 ) ) ;
#2650 = CARTESIAN_POINT ( 'NONE',  ( 115.7831076721481764, -41.80230950652948252, 78.40645860958801450 ) ) ;
#2651 = ORIENTED_EDGE ( 'NONE', *, *, #41288, .F. ) ;
#2652 = EDGE_CURVE ( 'NONE', #77917, #64042, #85371, .T. ) ;
#2653 = ORIENTED_EDGE ( 'NONE', *, *, #88370, .F. ) ;
#2654 = ADVANCED_FACE ( 'NONE', ( #29943 ), #51246, .T. ) ;
#2655 = VERTEX_POINT ( 'NONE', #78554 ) ;
#2656 = AXIS2_PLACEMENT_3D ( 'NONE', #36792, #63601, #44476 ) ;
#2657 = EDGE_LOOP ( 'NONE', ( #68451, #82652, #40751, #53725 ) ) ;
#2658 = CARTESIAN_POINT ( 'NONE',  ( 27.27158787008325902, 184.0000000000000000, -5.920431057502157584E-15 ) ) ;
#2659 = CARTESIAN_POINT ( 'NONE',  ( 105.3240584539683482, -26.47319898023377149, 11.20991099019697046 ) ) ;
#2660 = CARTESIAN_POINT ( 'NONE',  ( 7.661254700127822836, 98.64746158385918307, 275.4630000000000223 ) ) ;
#2661 = CARTESIAN_POINT ( 'NONE',  ( 131.3164832912740110, -36.72944715994100306, 3.101481641215535046 ) ) ;
#2662 = EDGE_CURVE ( 'NONE', #35967, #46977, #71833, .T. ) ;
#2664 = CARTESIAN_POINT ( 'NONE',  ( 75.68572508987453773, 76.20320268897035021, 91.25368348339081592 ) ) ;
#2663 = DIRECTION ( 'NONE',  ( 1.000000000000000000, 4.299999999999999979E-14, 1.000000000000000078E-15 ) ) ;
#2665 = CARTESIAN_POINT ( 'NONE',  ( 179.8585841295800094, -30.08671355700241179, -5.074374724088000832 ) ) ;
#2666 = CARTESIAN_POINT ( 'NONE',  ( 115.0373743241724327, -39.87857374794037923, 192.9495626852199450 ) ) ;
#2667 = ORIENTED_EDGE ( 'NONE', *, *, #22230, .F. ) ;
#2668 = AXIS2_PLACEMENT_3D ( 'NONE', #71158, #37954, #77965 ) ;
#2669 = ORIENTED_EDGE ( 'NONE', *, *, #58690, .F. ) ;
#2670 = VERTEX_POINT ( 'NONE', #86691 ) ;
#2671 = CARTESIAN_POINT ( 'NONE',  ( 110.8549203045407978, -45.98405385848638360, 182.8856638173630529 ) ) ;
#2672 = CARTESIAN_POINT ( 'NONE',  ( 112.1541913332956284, -45.76570811864959154, 253.9965776568629110 ) ) ;
#2673 = CARTESIAN_POINT ( 'NONE',  ( 97.81168895331838087, -40.51742574516882200, 287.6356252759109680 ) ) ;
#2674 = CARTESIAN_POINT ( 'NONE',  ( 0.000000000000000000, 184.0000000000000000, 101.0189074266571794 ) ) ;
#2675 = ORIENTED_EDGE ( 'NONE', *, *, #74928, .F. ) ;
#2676 = AXIS2_PLACEMENT_3D ( 'NONE', #78933, #16698, #44380 ) ;
#2677 = CARTESIAN_POINT ( 'NONE',  ( 107.0667039024470313, -104.2784471599418197, -11.78219314458200984 ) ) ;
#2678 = ORIENTED_EDGE ( 'NONE', *, *, #5270, .T. ) ;
#2679 = ADVANCED_FACE ( 'NONE', ( #53006 ), #52128, .F. ) ;
#2680 = DIRECTION ( 'NONE',  ( 0.000000000000000000, 0.000000000000000000, -1.000000000000000000 ) ) ;
#2681 = CARTESIAN_POINT ( 'NONE',  ( 111.5476492967639359, -29.48535330821865941, 286.0672975916113501 ) ) ;
#2682 = CIRCLE ( 'NONE', #50511, 2.500000000000002220 ) ;
#2683 = AXIS2_PLACEMENT_3D ( 'NONE', #52529, #5317, #32552 ) ;
#2684 = DIRECTION ( 'NONE',  ( 0.000000000000000000, 0.000000000000000000, -1.000000000000000000 ) ) ;
#2685 = CARTESIAN_POINT ( 'NONE',  ( 25.56670390244797275, -58.35344715994099829, 173.2178068554149775 ) ) ;
#2686 = DIRECTION ( 'NONE',  ( 0.000000000000000000, 0.000000000000000000, 1.000000000000000000 ) ) ;
#2687 = ORIENTED_EDGE ( 'NONE', *, *, #76279, .T. ) ;
#2688 = CARTESIAN_POINT ( 'NONE',  ( 0.000000000000000000, 44.45000000000000284, 0.000000000000000000 ) ) ;
#2689 = VECTOR ( 'NONE', #77875, 1000.000000000000000 ) ;
#2690 = FACE_OUTER_BOUND ( 'NONE', #33003, .T. ) ;
#2691 = ORIENTED_EDGE ( 'NONE', *, *, #72281, .T. ) ;
#2692 = CARTESIAN_POINT ( 'NONE',  ( 109.6839073351967642, -47.46854297047285343, 87.75467289495897205 ) ) ;
#2693 = EDGE_LOOP ( 'NONE', ( #48499, #38481 ) ) ;
#2694 = CARTESIAN_POINT ( 'NONE',  ( 114.9815630121539272, -32.32897180620768296, 28.66480078045796631 ) ) ;
#2695 = CIRCLE ( 'NONE', #66468, 2.500000000000002220 ) ;
#2696 = LINE ( 'NONE', #16767, #70704 ) ;
#2697 = CARTESIAN_POINT ( 'NONE',  ( 112.4011824308993397, -28.99526907646757934, 86.03967854399191140 ) ) ;
#2698 = EDGE_CURVE ( 'NONE', #82109, #43994, #17645, .T. ) ;
#2699 = CARTESIAN_POINT ( 'NONE',  ( 116.8176351461798816, -34.15490266430645505, 15.03129702300762638 ) ) ;
#2700 = CARTESIAN_POINT ( 'NONE',  ( 91.27445496092437338, -35.37506862591278889, 302.6356252759109680 ) ) ;
#2701 = CIRCLE ( 'NONE', #7039, 0.5000000000000004441 ) ;
#2702 = CARTESIAN_POINT ( 'NONE',  ( 68.90393785523644965, -69.55022374562288690, 247.4982723397321251 ) ) ;
#2703 = CARTESIAN_POINT ( 'NONE',  ( 117.5626006132557535, -36.54510529939036445, 284.8413395616253752 ) ) ;
#2704 = DIRECTION ( 'NONE',  ( 0.000000000000000000, -0.000000000000000000, 1.000000000000000000 ) ) ;
#2705 = VERTEX_POINT ( 'NONE', #19426 ) ;
#2706 = EDGE_CURVE ( 'NONE', #5970, #80043, #52218, .T. ) ;
#2707 = DIRECTION ( 'NONE',  ( -0.000000000000000000, -0.000000000000000000, -1.000000000000000000 ) ) ;
#2708 = EDGE_LOOP ( 'NONE', ( #58431, #17831, #43894, #14719 ) ) ;
#2709 = CARTESIAN_POINT ( 'NONE',  ( 105.7148016331714757, -24.90641244965552659, 156.1670538473399574 ) ) ;
#2710 = CARTESIAN_POINT ( 'NONE',  ( 79.69020591994394920, -21.46022584114962939, 1.641799370505243827 ) ) ;
#2711 = EDGE_LOOP ( 'NONE', ( #29510, #40676, #50421, #40816 ) ) ;
#2712 = ORIENTED_EDGE ( 'NONE', *, *, #40555, .F. ) ;
#2713 = EDGE_LOOP ( 'NONE', ( #7717, #89123 ) ) ;
#2714 = AXIS2_PLACEMENT_3D ( 'NONE', #31294, #58989, #11763 ) ;
#2715 = DIRECTION ( 'NONE',  ( -0.7071067811865192621, -0.7071067811865758834, -7.071067811865186413E-16 ) ) ;
#2716 = CARTESIAN_POINT ( 'NONE',  ( 89.60916260784479448, 224.4999999999999432, 134.1927865330827103 ) ) ;
#2717 = CARTESIAN_POINT ( 'NONE',  ( 96.12852455334814294, -38.72269610271991525, 201.4699109901969791 ) ) ;
#2718 = CARTESIAN_POINT ( 'NONE',  ( 144.8664832912739939, -71.52944715994085811, 361.9756252759100335 ) ) ;
#2719 = DIRECTION ( 'NONE',  ( 0.000000000000000000, 1.000000000000000000, 0.000000000000000000 ) ) ;
#2720 = DIRECTION ( 'NONE',  ( 1.000000000000000000, 4.299999999999999979E-14, 1.000000000000000078E-15 ) ) ;
#2721 = CARTESIAN_POINT ( 'NONE',  ( 117.5407444095047111, -36.54548251031545192, 284.8413395616252615 ) ) ;
#2722 = DIRECTION ( 'NONE',  ( 1.000000000000000000, 4.163336342344333240E-14, 0.000000000000000000 ) ) ;
#2723 = VERTEX_POINT ( 'NONE', #18524 ) ;
#2724 = CARTESIAN_POINT ( 'NONE',  ( 97.79627733347969354, -40.47956530005762232, 172.6323719911590899 ) ) ;
#2725 = LINE ( 'NONE', #42681, #24433 ) ;
#2727 = VERTEX_POINT ( 'NONE', #73946 ) ;
#2726 = VECTOR ( 'NONE', #73705, 1000.000000000000000 ) ;
#2728 = DIRECTION ( 'NONE',  ( 0.000000000000000000, 0.000000000000000000, 1.000000000000000000 ) ) ;
#2729 = LINE ( 'NONE', #78601, #83208 ) ;
#2730 = CARTESIAN_POINT ( 'NONE',  ( 112.4780167374716058, -46.34085331822173970, 257.9965776568635647 ) ) ;
#2731 = CARTESIAN_POINT ( 'NONE',  ( 1.387778780781445676E-14, 223.9999999999999716, 97.27542076772557778 ) ) ;
#2732 = EDGE_CURVE ( 'NONE', #70235, #30868, #67125, .T. ) ;
#2733 = PLANE ( 'NONE',  #44835 ) ;
#2734 = CARTESIAN_POINT ( 'NONE',  ( 184.5664832912729878, -81.37844715994266664, 361.9756252759109998 ) ) ;
#2735 = ADVANCED_FACE ( 'NONE', ( #88485 ), #26242, .F. ) ;
#2736 = CARTESIAN_POINT ( 'NONE',  ( 98.89771913768545630, -40.63891803577419637, 216.1162293518859485 ) ) ;
#2738 = CARTESIAN_POINT ( 'NONE',  ( 117.4328057974122714, -37.95573561897357706, 49.73276813305393773 ) ) ;
#2737 = CARTESIAN_POINT ( 'NONE',  ( 56.06670390244699576, -67.87844715994098976, 190.2178068554179902 ) ) ;
#2739 = CARTESIAN_POINT ( 'NONE',  ( 126.5345833325615104, 62.85051826981599987, 32.15513509386430258 ) ) ;
#2740 = CARTESIAN_POINT ( 'NONE',  ( 109.0807882705640139, -47.64528240413121551, 127.7337205140059382 ) ) ;
#2741 = ORIENTED_EDGE ( 'NONE', *, *, #83393, .F. ) ;
#2742 = DIRECTION ( 'NONE',  ( 0.000000000000000000, 0.000000000000000000, -1.000000000000000000 ) ) ;
#2743 = ORIENTED_EDGE ( 'NONE', *, *, #61260, .F. ) ;
#2744 = EDGE_CURVE ( 'NONE', #18726, #80899, #47888, .T. ) ;
#2745 = DIRECTION ( 'NONE',  ( 1.000000000000000078E-15, -1.000000000000000000, 0.000000000000000000 ) ) ;
#2746 = CARTESIAN_POINT ( 'NONE',  ( 110.2240687061785707, -27.20640067271266460, 275.8215515107314104 ) ) ;
#2747 = EDGE_LOOP ( 'NONE', ( #68008, #47012, #36592, #22120 ) ) ;
#2748 = VECTOR ( 'NONE', #79612, 1000.000000000000000 ) ;
#2749 = CARTESIAN_POINT ( 'NONE',  ( 107.0667039024469886, -67.87844715994094713, 93.21780685541800437 ) ) ;
#2750 = EDGE_CURVE ( 'NONE', #52484, #27146, #59495, .T. ) ;
#2751 = ORIENTED_EDGE ( 'NONE', *, *, #56201, .T. ) ;
#2752 = PLANE ( 'NONE',  #5918 ) ;
#2753 = DIRECTION ( 'NONE',  ( 4.299999999999999979E-14, -1.000000000000000000, 4.400000000000000367E-29 ) ) ;
#2755 = LINE ( 'NONE', #78623, #59670 ) ;
#2754 = AXIS2_PLACEMENT_3D ( 'NONE', #84563, #50902, #49098 ) ;
#2756 = VERTEX_POINT ( 'NONE', #38518 ) ;
#2757 = AXIS2_PLACEMENT_3D ( 'NONE', #23707, #65023, #56851 ) ;
#2758 = EDGE_CURVE ( 'NONE', #66915, #46344, #79890, .T. ) ;
#2759 = CARTESIAN_POINT ( 'NONE',  ( 95.46334413863738177, -34.19939227723602926, 106.1556252759109640 ) ) ;
#2760 = CARTESIAN_POINT ( 'NONE',  ( 97.80795155074446257, -40.50828509696400914, 166.6348390368860635 ) ) ;
#2761 = CARTESIAN_POINT ( 'NONE',  ( 38.10000000000000142, 95.25000000000000000, 283.4005000000000223 ) ) ;
#2762 = CARTESIAN_POINT ( 'NONE',  ( 104.4081006369549982, -46.45808913368724546, 142.3647919406123208 ) ) ;
#2763 = ORIENTED_EDGE ( 'NONE', *, *, #21714, .T. ) ;
#2764 = EDGE_CURVE ( 'NONE', #51166, #61833, #7332, .T. ) ;
#2765 = AXIS2_PLACEMENT_3D ( 'NONE', #7711, #28138, #27706 ) ;
#2766 = CARTESIAN_POINT ( 'NONE',  ( 99.76704648670056486, 88.91113633199481114, -84.21071524772746386 ) ) ;
#2767 = CARTESIAN_POINT ( 'NONE',  ( 47.62500000000000000, 73.02500000000000568, 219.0749999999999886 ) ) ;
#2768 = VECTOR ( 'NONE', #53000, 1000.000000000000000 ) ;
#2769 = DIRECTION ( 'NONE',  ( -1.000000000000000000, 0.000000000000000000, 0.000000000000000000 ) ) ;
#2770 = CIRCLE ( 'NONE', #60767, 2.517500000000005844 ) ;
#2772 = CARTESIAN_POINT ( 'NONE',  ( 67.06670390244707392, -137.6766936484476958, 245.4930518797220032 ) ) ;
#2771 = DIRECTION ( 'NONE',  ( 1.000000000000000000, 4.163336342344333240E-14, 0.000000000000000000 ) ) ;
#2773 = DIRECTION ( 'NONE',  ( 0.000000000000000000, 0.000000000000000000, 1.000000000000000000 ) ) ;
#2774 = ORIENTED_EDGE ( 'NONE', *, *, #57742, .T. ) ;
#2775 = CARTESIAN_POINT ( 'NONE',  ( 116.3130905035090876, -32.93898513502411163, 35.13562527591096796 ) ) ;
#2776 = CARTESIAN_POINT ( 'NONE',  ( 111.1483613326457629, -47.07112276671751516, 168.8756252759109486 ) ) ;
#2777 = VECTOR ( 'NONE', #34885, 999.9999999999998863 ) ;
#2779 = ORIENTED_EDGE ( 'NONE', *, *, #75020, .T. ) ;
#2778 = FACE_OUTER_BOUND ( 'NONE', #78792, .T. ) ;
#2780 = CARTESIAN_POINT ( 'NONE',  ( 97.33063402535807995, -33.15845140301009053, 17.03467289495797132 ) ) ;
#2781 = DIRECTION ( 'NONE',  ( 0.000000000000000000, 1.000000000000000000, 0.000000000000000000 ) ) ;
#2782 = CARTESIAN_POINT ( 'NONE',  ( 101.9935131536830255, -45.44600547682843938, 52.15652309846547752 ) ) ;
#2783 = PLANE ( 'NONE',  #22479 ) ;
#2784 = EDGE_LOOP ( 'NONE', ( #26357, #21741, #19433, #87508 ) ) ;
#2785 = CARTESIAN_POINT ( 'NONE',  ( 196.2150000000000034, 43.68799999999999528, 44.45000000000000284 ) ) ;
#2786 = CARTESIAN_POINT ( 'NONE',  ( 116.7732407090126827, -35.28285290846962141, 218.9441967044829482 ) ) ;
#2787 = VERTEX_POINT ( 'NONE', #50598 ) ;
#2788 = EDGE_LOOP ( 'NONE', ( #36538, #22888, #1028, #17291 ) ) ;
#2789 = EDGE_CURVE ( 'NONE', #9116, #25721, #63798, .T. ) ;
#2790 = AXIS2_PLACEMENT_3D ( 'NONE', #76630, #62543, #83010 ) ;
#2791 = CARTESIAN_POINT ( 'NONE',  ( 117.1060311394199402, -37.55296641157723769, 185.1930118773259437 ) ) ;
#2792 = DIRECTION ( 'NONE',  ( 1.000000000000000000, 0.000000000000000000, 0.000000000000000000 ) ) ;
#2793 = CARTESIAN_POINT ( 'NONE',  ( 107.5258121372104227, -46.79223613538503912, 39.04444044875393871 ) ) ;
#2794 = CARTESIAN_POINT ( 'NONE',  ( -96.94152442043684914, 93.33921197991993779, 87.44900557253197348 ) ) ;
#2795 = CARTESIAN_POINT ( 'NONE',  ( 31.78666935232998725, -36.02818131005891189, 342.9256252759119548 ) ) ;
#2796 = FACE_OUTER_BOUND ( 'NONE', #75278, .T. ) ;
#2797 = VERTEX_POINT ( 'NONE', #77876 ) ;
#2798 = DIRECTION ( 'NONE',  ( 0.000000000000000000, 1.000000000000000000, 0.000000000000000000 ) ) ;
#2799 = LINE ( 'NONE', #44102, #58933 ) ;
#2800 = CARTESIAN_POINT ( 'NONE',  ( 101.3060704567421197, -26.40153104436172526, 255.4813395616251626 ) ) ;
#2801 = CARTESIAN_POINT ( 'NONE',  ( 12.57992033961893341, 83.37360573934186903, 117.6855557170023019 ) ) ;
#2802 = ORIENTED_EDGE ( 'NONE', *, *, #18081, .T. ) ;
#2803 = AXIS2_PLACEMENT_3D ( 'NONE', #76364, #49979, #28655 ) ;
#2804 = CARTESIAN_POINT ( 'NONE',  ( 33.96670390244744198, -28.27351298637434240, 313.9678068554150059 ) ) ;
#2805 = LINE ( 'NONE', #73162, #20065 ) ;
#2806 = CARTESIAN_POINT ( 'NONE',  ( 188.5667039024483529, -48.82844715993431350, 290.7178068554150059 ) ) ;
#2807 = CARTESIAN_POINT ( 'NONE',  ( 6.938893903907229955E-15, 50.79999999999999716, 216.0269999999999868 ) ) ;
#2808 = CARTESIAN_POINT ( 'NONE',  ( 109.4546162266722575, -25.87086512622489920, 25.90419670448196143 ) ) ;
#2810 = FACE_OUTER_BOUND ( 'NONE', #61011, .T. ) ;
#2809 = AXIS2_PLACEMENT_3D ( 'NONE', #64440, #50346, #78085 ) ;
#2811 = AXIS2_PLACEMENT_3D ( 'NONE', #73164, #46336, #10941 ) ;
#2812 = ORIENTED_EDGE ( 'NONE', *, *, #86456, .T. ) ;
#2813 = EDGE_CURVE ( 'NONE', #19234, #64957, #57658, .T. ) ;
#2814 = CARTESIAN_POINT ( 'NONE',  ( 110.4707641138770668, -47.29393344369797347, 53.83657765686300678 ) ) ;
#2815 = CARTESIAN_POINT ( 'NONE',  ( 118.3411383306134468, -33.07924694129162901, 284.0756252759109657 ) ) ;
#2816 = VERTEX_POINT ( 'NONE', #13071 ) ;
#2817 = VECTOR ( 'NONE', #5606, 1000.000000000000000 ) ;
#2818 = DIRECTION ( 'NONE',  ( -1.000000000000000078E-15, 1.000000000000000083E-30, 1.000000000000000000 ) ) ;
#2819 = CARTESIAN_POINT ( 'NONE',  ( 97.82709414970555883, -40.55490225695719175, 17.63852738896761707 ) ) ;
#2820 = STYLED_ITEM ( 'NONE', ( #7866 ), #65184 ) ;
#2821 = DIRECTION ( 'NONE',  ( 0.000000000000000000, -1.000000000000000000, 0.000000000000000000 ) ) ;
#2822 = CARTESIAN_POINT ( 'NONE',  ( 107.4866789999374390, -28.54983079893278486, 92.85380465530596439 ) ) ;
#2823 = CARTESIAN_POINT ( 'NONE',  ( 108.1840971438632550, -47.11637154254925974, 198.6613395616249989 ) ) ;
#2824 = CARTESIAN_POINT ( 'NONE',  ( 51.06670390244899238, -32.29483332968430886, -5.074374724088000832 ) ) ;
#2825 = DIRECTION ( 'NONE',  ( 0.000000000000000000, 0.000000000000000000, 1.000000000000000000 ) ) ;
#2826 = EDGE_LOOP ( 'NONE', ( #73856, #10535, #25706, #5708 ) ) ;
#2827 = VECTOR ( 'NONE', #16599, 1000.000000000000000 ) ;
#2828 = CYLINDRICAL_SURFACE ( 'NONE', #17543, 2.116999999999993776 ) ;
#2829 = ORIENTED_EDGE ( 'NONE', *, *, #27986, .T. ) ;
#2830 = ORIENTED_EDGE ( 'NONE', *, *, #67015, .T. ) ;
#2831 = LINE ( 'NONE', #35997, #27075 ) ;
#2832 = ORIENTED_EDGE ( 'NONE', *, *, #43523, .T. ) ;
#2833 = VERTEX_POINT ( 'NONE', #28364 ) ;
#2834 = CYLINDRICAL_SURFACE ( 'NONE', #80225, 3.499999999999996003 ) ;
#2835 = CARTESIAN_POINT ( 'NONE',  ( 102.0670447425352165, -27.97050339635270788, 41.48976872766033352 ) ) ;
#2836 = EDGE_CURVE ( 'NONE', #20875, #48555, #1576, .T. ) ;
#2837 = VECTOR ( 'NONE', #22180, 1000.000000000000000 ) ;
#2838 = CARTESIAN_POINT ( 'NONE',  ( 99.43039265704440766, -41.59799905411310306, 141.1886103042669731 ) ) ;
#2839 = CARTESIAN_POINT ( 'NONE',  ( 118.1265197682042327, -36.12032134488166690, 273.8822919425775808 ) ) ;
#2840 = ADVANCED_FACE ( 'NONE', ( #82131 ), #47563, .T. ) ;
#2841 = CARTESIAN_POINT ( 'NONE',  ( -2.883802008152356322, 70.17481864577712258, 130.5247784292598112 ) ) ;
#2842 = ADVANCED_FACE ( 'NONE', ( #63343, #1120 ), #40759, .F. ) ;
#2843 = EDGE_LOOP ( 'NONE', ( #38287, #47019, #30923, #33243 ) ) ;
#2844 = CARTESIAN_POINT ( 'NONE',  ( 104.5600616111754562, -27.04296758930388833, 136.2779522869518303 ) ) ;
#2845 = EDGE_CURVE ( 'NONE', #12768, #20192, #22930, .T. ) ;
#2846 = ORIENTED_EDGE ( 'NONE', *, *, #21323, .F. ) ;
#2847 = DIRECTION ( 'NONE',  ( 1.000000000000000000, 4.510281037539788691E-14, 0.000000000000000000 ) ) ;
#2848 = CARTESIAN_POINT ( 'NONE',  ( 226.4410000000000025, 40.03750000000000142, 10.66800000000000104 ) ) ;
#2849 = DIRECTION ( 'NONE',  ( 0.000000000000000000, 1.000000000000000000, 0.000000000000000000 ) ) ;
#2850 = CARTESIAN_POINT ( 'NONE',  ( -135.2444258376732193, 101.5999999999999943, -147.4575741623275746 ) ) ;
#2851 = VERTEX_POINT ( 'NONE', #52353 ) ;
#2852 = CARTESIAN_POINT ( 'NONE',  ( 96.80868943730629894, -40.84730494075294871, 251.6422919425777138 ) ) ;
#2853 = CARTESIAN_POINT ( 'NONE',  ( 117.5312049024071257, -37.01681686833584450, 39.80419670448193159 ) ) ;
#2854 = CARTESIAN_POINT ( 'NONE',  ( 113.1782937674814491, -44.75186859554625585, 119.0939586088680500 ) ) ;
#2856 = DIRECTION ( 'NONE',  ( 0.7071067811866377228, -0.7071067811864573116, 0.000000000000000000 ) ) ;
#2855 = DIRECTION ( 'NONE',  ( -1.000000000000000078E-15, 0.000000000000000000, 1.000000000000000000 ) ) ;
#2857 = DIRECTION ( 'NONE',  ( 1.000000000000000000, -3.885780586187990841E-13, 0.000000000000000000 ) ) ;
#2858 = CARTESIAN_POINT ( 'NONE',  ( 67.06670390244700286, -67.87844715994098976, 222.2178068554179902 ) ) ;
#2859 = CARTESIAN_POINT ( 'NONE',  ( 131.7480217999342926, -38.20859666167535096, 7.273989459506820410 ) ) ;
#2860 = EDGE_CURVE ( 'NONE', #50592, #42067, #14600, .T. ) ;
#2861 = EDGE_CURVE ( 'NONE', #38542, #32624, #25126, .T. ) ;
#2862 = DIRECTION ( 'NONE',  ( -0.1858654557293184517, 0.9825752044329902901, 0.000000000000000000 ) ) ;
#2863 = CARTESIAN_POINT ( 'NONE',  ( 115.7834167274817503, -41.80178756718994748, 163.4063445344124261 ) ) ;
#2864 = DIRECTION ( 'NONE',  ( 0.000000000000000000, 1.000000000000000000, 0.000000000000000000 ) ) ;
#2865 = AXIS2_PLACEMENT_3D ( 'NONE', #73796, #80184, #86552 ) ;
#2866 = CARTESIAN_POINT ( 'NONE',  ( 49.35031423293201414, -29.99615139349890569, 313.9678068554150059 ) ) ;
#2867 = CARTESIAN_POINT ( 'NONE',  ( 116.5566381636777322, -42.44192488244189576, 278.3832443235297660 ) ) ;
#2868 = CARTESIAN_POINT ( 'NONE',  ( 103.8073934974285066, -26.82688076304711444, 161.3299109901969643 ) ) ;
#2869 = CARTESIAN_POINT ( 'NONE',  ( 96.31605362642591217, -41.77429727756310740, 57.67562527591096710 ) ) ;
#2871 = DIRECTION ( 'NONE',  ( 0.7071067811865758834, -0.7071067811865192621, 7.071067811865766226E-16 ) ) ;
#2870 = PLANE ( 'NONE',  #50830 ) ;
#2872 = CARTESIAN_POINT ( 'NONE',  ( 82.80042800423679239, -36.38432671277497832, 3.076561810303515276 ) ) ;
#2873 = AXIS2_PLACEMENT_3D ( 'NONE', #63355, #56978, #84719 ) ;
#2874 = VERTEX_POINT ( 'NONE', #58738 ) ;
#2875 = CARTESIAN_POINT ( 'NONE',  ( 107.0667039024470313, -104.2784471599420897, -20.48315503890502143 ) ) ;
#2876 = VERTEX_POINT ( 'NONE', #66452 ) ;
#2877 = CARTESIAN_POINT ( 'NONE',  ( 103.6990349130722677, -26.13358598113153164, 51.32133956162493149 ) ) ;
#2878 = AXIS2_PLACEMENT_3D ( 'NONE', #86496, #67361, #11063 ) ;
#2880 = VERTEX_POINT ( 'NONE', #73267 ) ;
#2879 = DIRECTION ( 'NONE',  ( 1.000000000000000078E-15, -1.000000000000000083E-30, -1.000000000000000000 ) ) ;
#2881 = CARTESIAN_POINT ( 'NONE',  ( 99.04401119945882215, -42.84118153451598943, 47.84395147023094097 ) ) ;
#2882 = CARTESIAN_POINT ( 'NONE',  ( 110.4916936757735186, -26.90617889774112825, 205.8099109901969541 ) ) ;
#2883 = CARTESIAN_POINT ( 'NONE',  ( 32.06670390244764945, -33.35206098992742341, 313.9678068554150059 ) ) ;
#2884 = LINE ( 'NONE', #51017, #12434 ) ;
#2885 = CARTESIAN_POINT ( 'NONE',  ( 77.06670390244701707, -90.27844715994098124, 230.7030882296565721 ) ) ;
#2886 = CARTESIAN_POINT ( 'NONE',  ( 97.06107109957150669, -37.99641198294513345, 47.42729194408147464 ) ) ;
#2887 = CARTESIAN_POINT ( 'NONE',  ( 194.5667039024479834, -48.82844715994099971, 310.9178068554150514 ) ) ;
#2888 = CARTESIAN_POINT ( 'NONE',  ( 99.08956738544915765, -42.79550390363951351, 96.84396446119878021 ) ) ;
#2889 = AXIS2_PLACEMENT_3D ( 'NONE', #48360, #76095, #49273 ) ;
#2890 = CARTESIAN_POINT ( 'NONE',  ( 111.8077268321493563, -46.78591733285071541, 137.9270538473399768 ) ) ;
#2891 = EDGE_LOOP ( 'NONE', ( #4565, #87707, #60253, #39963 ) ) ;
#2892 = ORIENTED_EDGE ( 'NONE', *, *, #72960, .T. ) ;
#2893 = ADVANCED_FACE ( 'NONE', ( #24685 ), #11049, .F. ) ;
#2894 = CARTESIAN_POINT ( 'NONE',  ( 115.7982244386701609, -33.26055366603426933, 95.57110711542094350 ) ) ;
#2895 = DIRECTION ( 'NONE',  ( 0.000000000000000000, 1.000000000000000000, 0.000000000000000000 ) ) ;
#2897 = CARTESIAN_POINT ( 'NONE',  ( 52.38749999999999574, 94.53880000000000905, 250.8250000000000171 ) ) ;
#2896 = CARTESIAN_POINT ( 'NONE',  ( 111.8874393434637682, -45.23954810143637673, 208.9870538473389558 ) ) ;
#2898 = DIRECTION ( 'NONE',  ( 9.351236661543306751E-17, -3.725950533538267725E-29, -1.000000000000000000 ) ) ;
#2900 = EDGE_CURVE ( 'NONE', #30367, #30159, #57865, .T. ) ;
#2899 = DIRECTION ( 'NONE',  ( 0.000000000000000000, 1.000000000000000000, 0.000000000000000000 ) ) ;
#2901 = AXIS2_PLACEMENT_3D ( 'NONE', #33441, #54750, #19371 ) ;
#2902 = CARTESIAN_POINT ( 'NONE',  ( 118.1268077877470830, 74.81620433377382540, -10.08232578576091854 ) ) ;
#2903 = CARTESIAN_POINT ( 'NONE',  ( -12.70000000000000107, 82.54999999999999716, 117.8738102209307641 ) ) ;
#2904 = LINE ( 'NONE', #44660, #11603 ) ;
#2905 = DIRECTION ( 'NONE',  ( 0.000000000000000000, -0.7071067811865280328, -0.7071067811865670016 ) ) ;
#2906 = CARTESIAN_POINT ( 'NONE',  ( 116.6407469026009238, -40.79910830432095281, 168.5070538473399608 ) ) ;
#2907 = ORIENTED_EDGE ( 'NONE', *, *, #43181, .F. ) ;
#2908 = VERTEX_POINT ( 'NONE', #31048 ) ;
#2909 = CARTESIAN_POINT ( 'NONE',  ( 90.57859886853759690, -68.78570139166994579, 247.5000682988239760 ) ) ;
#2910 = CARTESIAN_POINT ( 'NONE',  ( 146.9135422721272448, -68.02287184880887594, 246.2552768418564710 ) ) ;
#2911 = DIRECTION ( 'NONE',  ( 0.000000000000000000, 1.000000000000000000, 0.000000000000000000 ) ) ;
#2912 = CARTESIAN_POINT ( 'NONE',  ( 97.81186694083565669, -40.51786060332464956, 102.6356630628624060 ) ) ;
#2913 = CARTESIAN_POINT ( 'NONE',  ( 116.2459175369934172, -38.08366948007849118, 221.5280903695909842 ) ) ;
#2914 = AXIS2_PLACEMENT_3D ( 'NONE', #18645, #74054, #60409 ) ;
#2915 = EDGE_CURVE ( 'NONE', #28761, #77463, #23377, .T. ) ;
#2916 = CARTESIAN_POINT ( 'NONE',  ( 3.174999999999879918, 17.78000000000000114, -33.98325472291465132 ) ) ;
#2917 = CARTESIAN_POINT ( 'NONE',  ( 98.37959078170875671, -29.89446464491232192, 200.8080062282919869 ) ) ;
#2918 = CARTESIAN_POINT ( 'NONE',  ( -30.89999999999999858, 53.97500000000000142, 50.79999999999999716 ) ) ;
#2919 = VERTEX_POINT ( 'NONE', #2469 ) ;
#2921 = ORIENTED_EDGE ( 'NONE', *, *, #10620, .F. ) ;
#2920 = VERTEX_POINT ( 'NONE', #45110 ) ;
#2922 = AXIS2_PLACEMENT_3D ( 'NONE', #15425, #58514, #9487 ) ;
#2923 = CARTESIAN_POINT ( 'NONE',  ( 0.000000000000000000, 67.86880000000000734, 259.9944000000000415 ) ) ;
#2924 = DIRECTION ( 'NONE',  ( -0.9963424814100678706, 0.08544974978095865037, 0.000000000000000000 ) ) ;
#2925 = CARTESIAN_POINT ( 'NONE',  ( 172.5664832912740110, -36.32844715994070839, 18.92562527591200094 ) ) ;
#2926 = CARTESIAN_POINT ( 'NONE',  ( 114.1852310984691883, -41.65497984893937655, 11.17475703625792072 ) ) ;
#2927 = VECTOR ( 'NONE', #1076, 1000.000000000000000 ) ;
#2928 = CARTESIAN_POINT ( 'NONE',  ( 115.7831074623854590, -41.80230988274058035, 273.4064585755251642 ) ) ;
#2929 = ORIENTED_EDGE ( 'NONE', *, *, #70817, .T. ) ;
#2930 = CARTESIAN_POINT ( 'NONE',  ( 116.3422999134539566, -39.38573384602094052, 9.635625275910941312 ) ) ;
#2931 = CYLINDRICAL_SURFACE ( 'NONE', #70630, 2.500000000000002220 ) ;
#2932 = VERTEX_POINT ( 'NONE', #45541 ) ;
#2934 = ORIENTED_EDGE ( 'NONE', *, *, #46666, .F. ) ;
#2933 = CIRCLE ( 'NONE', #73985, 0.5000000000000004441 ) ;
#2935 = CYLINDRICAL_SURFACE ( 'NONE', #19748, 9.999999999999998224 ) ;
#2936 = ORIENTED_EDGE ( 'NONE', *, *, #82900, .T. ) ;
#2937 = ORIENTED_EDGE ( 'NONE', *, *, #22747, .T. ) ;
#2938 = CARTESIAN_POINT ( 'NONE',  ( 110.3949268851355328, -45.15168757608171290, 22.31051506617198754 ) ) ;
#2939 = VECTOR ( 'NONE', #80924, 1000.000000000000000 ) ;
#2940 = CARTESIAN_POINT ( 'NONE',  ( 103.0412047595748959, -26.40992324271003966, 170.3603871806729444 ) ) ;
#2941 = CARTESIAN_POINT ( 'NONE',  ( 103.1828028919049558, -27.07824557232541807, 130.3813395616259925 ) ) ;
#2942 = DIRECTION ( 'NONE',  ( -1.000000000000000078E-15, 1.000000000000000083E-30, 1.000000000000000000 ) ) ;
#2943 = CARTESIAN_POINT ( 'NONE',  ( 99.14341341762981585, -43.50528616620496791, 31.88991099019594699 ) ) ;
#2944 = CARTESIAN_POINT ( 'NONE',  ( 115.3234718241651535, -45.22984455807579707, 264.1899109901965517 ) ) ;
#2945 = DIRECTION ( 'NONE',  ( 0.000000000000000000, -1.000000000000000000, 0.000000000000000000 ) ) ;
#2946 = EDGE_CURVE ( 'NONE', #42715, #65869, #30164, .T. ) ;
#2947 = DIRECTION ( 'NONE',  ( 3.360405532702990443E-14, -1.000000000000000000, 0.000000000000000000 ) ) ;
#2948 = CARTESIAN_POINT ( 'NONE',  ( -130.3273007233323142, 72.45841406287408404, 7.755409066832052112 ) ) ;
#2949 = VERTEX_POINT ( 'NONE', #79226 ) ;
#2950 = VERTEX_POINT ( 'NONE', #78782 ) ;
#2951 = VECTOR ( 'NONE', #72879, 1000.000000000000000 ) ;
#2952 = CARTESIAN_POINT ( 'NONE',  ( 96.69933951777882442, -35.27033920508573317, 181.2156252759109805 ) ) ;
#2953 = VERTEX_POINT ( 'NONE', #86482 ) ;
#2954 = CARTESIAN_POINT ( 'NONE',  ( 98.00691293156391737, -30.39673331971502179, 160.8289586092449497 ) ) ;
#2955 = CARTESIAN_POINT ( 'NONE',  ( 97.80969231062213964, -40.51824920587227297, 266.6357212253427633 ) ) ;
#2956 = CARTESIAN_POINT ( 'NONE',  ( 1.387778780781445676E-14, 239.0000000000000000, 97.27542076772557778 ) ) ;
#2957 = LINE ( 'NONE', #11095, #63039 ) ;
#2960 = CARTESIAN_POINT ( 'NONE',  ( 110.9847977634195928, -46.36662828626490551, 278.8841967044824059 ) ) ;
#2959 = FACE_OUTER_BOUND ( 'NONE', #48584, .T. ) ;
#2958 = CARTESIAN_POINT ( 'NONE',  ( -487.2989999999999782, 21.43125000000035030, 6.988054014476359654 ) ) ;
#2961 = CARTESIAN_POINT ( 'NONE',  ( 33.78309357196401663, -29.99615139349950965, 313.9678068554150059 ) ) ;
#2962 = FACE_OUTER_BOUND ( 'NONE', #41421, .T. ) ;
#2963 = AXIS2_PLACEMENT_3D ( 'NONE', #80579, #60548, #88735 ) ;
#2964 = CARTESIAN_POINT ( 'NONE',  ( 109.7212149768267437, -26.99983785526716318, 270.8646645069375722 ) ) ;
#2965 = ADVANCED_FACE ( 'NONE', ( #4242 ), #69374, .F. ) ;
#2966 = CARTESIAN_POINT ( 'NONE',  ( 32.25690895537100289, -33.54226604285010893, 342.9256252759119548 ) ) ;
#2967 = ADVANCED_FACE ( 'NONE', ( #44669 ), #44213, .F. ) ;
#2968 = CARTESIAN_POINT ( 'NONE',  ( 98.30753420875569759, -41.72887552247058096, 257.7397919454337512 ) ) ;
#2970 = ORIENTED_EDGE ( 'NONE', *, *, #89696, .F. ) ;
#2969 = CARTESIAN_POINT ( 'NONE',  ( 104.1015251979861773, -44.20529628163873781, 195.5838068554170661 ) ) ;
#2971 = CARTESIAN_POINT ( 'NONE',  ( 83.56670559755343675, -40.03837296219064967, 239.5838068554176914 ) ) ;
#2972 = CARTESIAN_POINT ( 'NONE',  ( 117.3133064751534249, -34.51789172102134984, 183.9956252759109532 ) ) ;
#2973 = CARTESIAN_POINT ( 'NONE',  ( 112.7598396812348369, -27.95408244994987967, 65.61848241876793963 ) ) ;
#2974 = CARTESIAN_POINT ( 'NONE',  ( 117.9939971868874125, -34.78344139941312108, 194.9546728949589749 ) ) ;
#2975 = PLANE ( 'NONE',  #30037 ) ;
#2976 = DIRECTION ( 'NONE',  ( 1.000000000000000000, 4.163336342344333240E-14, 0.000000000000000000 ) ) ;
#2977 = CONICAL_SURFACE ( 'NONE', #5894, 1.571100913904333041, 1.047197551196591858 ) ;
#2979 = CARTESIAN_POINT ( 'NONE',  ( 116.9975143198770269, -38.00265672266952066, 39.72466762246843786 ) ) ;
#2978 = CARTESIAN_POINT ( 'NONE',  ( 80.06648329127402519, -46.42944715994105565, 4.925625275910944012 ) ) ;
#2980 = DIRECTION ( 'NONE',  ( 1.000000000000000000, 1.261617073437676668E-15, 9.462128050782575008E-16 ) ) ;
#2981 = FACE_OUTER_BOUND ( 'NONE', #28946, .T. ) ;
#2982 = VERTEX_POINT ( 'NONE', #59630 ) ;
#2983 = CARTESIAN_POINT ( 'NONE',  ( 97.12553845659432739, -37.99676787625246988, 66.42808859729984761 ) ) ;
#2984 = ORIENTED_EDGE ( 'NONE', *, *, #3400, .F. ) ;
#2985 = VERTEX_POINT ( 'NONE', #38308 ) ;
#2986 = CARTESIAN_POINT ( 'NONE',  ( 103.1631342820178929, -29.09950819311272951, 119.8752769709339816 ) ) ;
#2987 = VECTOR ( 'NONE', #10602, 1000.000000000000000 ) ;
#2989 = ORIENTED_EDGE ( 'NONE', *, *, #21081, .F. ) ;
#2988 = CARTESIAN_POINT ( 'NONE',  ( -11.89044713366393680, 87.03112570152840988, -130.0135071244502853 ) ) ;
#2990 = CARTESIAN_POINT ( 'NONE',  ( 96.66103594285313250, -37.56076609107801545, 97.38991099019594344 ) ) ;
#2991 = DIRECTION ( 'NONE',  ( 1.000000000000000078E-15, -1.000000000000000083E-30, -1.000000000000000000 ) ) ;
#2993 = CARTESIAN_POINT ( 'NONE',  ( 77.40046754268362861, -18.03188136815523279, 6.871351212842800926 ) ) ;
#2992 = AXIS2_PLACEMENT_3D ( 'NONE', #72250, #50897, #44516 ) ;
#2994 = DIRECTION ( 'NONE',  ( 1.000000000000000000, 0.000000000000000000, 0.000000000000000000 ) ) ;
#2995 = CARTESIAN_POINT ( 'NONE',  ( 105.4283229756613309, -27.08692670426131954, 15.20991099019697401 ) ) ;
#2996 = ORIENTED_EDGE ( 'NONE', *, *, #11015, .T. ) ;
#2997 = ORIENTED_EDGE ( 'NONE', *, *, #62383, .T. ) ;
#2999 = EDGE_LOOP ( 'NONE', ( #63002, #56856, #5047, #17409, #54291, #77223, #34139, #34652, #30607, #29751, #12971, #71726, #7525, #26455, #29483, #22789 ) ) ;
#2998 = VECTOR ( 'NONE', #39579, 1000.000000000000000 ) ;
#3000 = CARTESIAN_POINT ( 'NONE',  ( 125.0235919798090833, -56.62589376934764118, -5.074374724088935196 ) ) ;
#3001 = DIRECTION ( 'NONE',  ( 1.000000000000000000, 8.673617379883546378E-16, 9.757819552368989676E-16 ) ) ;
#3002 = CARTESIAN_POINT ( 'NONE',  ( 0.000000000000000000, 101.5999999999999943, -103.1875000000000000 ) ) ;
#3003 = CARTESIAN_POINT ( 'NONE',  ( 129.9417039024469886, -68.87844715994091871, 138.7178068554180186 ) ) ;
#3004 = LINE ( 'NONE', #85694, #39287 ) ;
#3006 = EDGE_CURVE ( 'NONE', #2797, #70996, #83842, .T. ) ;
#3005 = CARTESIAN_POINT ( 'NONE',  ( 97.79626992864577062, -40.47954699870867756, 52.63196278063107769 ) ) ;
#3007 = AXIS2_PLACEMENT_3D ( 'NONE', #78593, #71762, #83602 ) ;
#3008 = CARTESIAN_POINT ( 'NONE',  ( 72.06648329127396835, -9.729447159941065237, 14.92562527591093691 ) ) ;
#3009 = CARTESIAN_POINT ( 'NONE',  ( 74.38497350661437224, 83.38015080693121206, 92.31685958143667392 ) ) ;
#3010 = CARTESIAN_POINT ( 'NONE',  ( 99.14404768239418786, -44.40400490628097430, 41.95086337114900488 ) ) ;
#3011 = EDGE_LOOP ( 'NONE', ( #54618, #26924, #77400, #78953 ) ) ;
#3012 = CARTESIAN_POINT ( 'NONE',  ( 7.752238106858494682, 92.64409645872694909, 130.3274943305225122 ) ) ;
#3013 = CARTESIAN_POINT ( 'NONE',  ( 126.6062568295380260, 45.75147977268651545, 31.87055648571903532 ) ) ;
#3014 = DIRECTION ( 'NONE',  ( 0.000000000000000000, 0.000000000000000000, 1.000000000000000000 ) ) ;
#3015 = CARTESIAN_POINT ( 'NONE',  ( 114.5297761857384415, -31.21626383854846765, 107.1509475124489654 ) ) ;
#3016 = ADVANCED_FACE ( 'NONE', ( #3796, #52787 ), #80554, .F. ) ;
#3017 = EDGE_CURVE ( 'NONE', #32697, #73034, #89030, .T. ) ;
#3018 = CARTESIAN_POINT ( 'NONE',  ( 97.78499608817705280, -40.45164102492867642, 96.62997540673826791 ) ) ;
#3019 = VECTOR ( 'NONE', #47360, 1000.000000000000000 ) ;
#3020 = CARTESIAN_POINT ( 'NONE',  ( -446.0240000000000009, 93.66249999999999432, 90.48749999999999716 ) ) ;
#3021 = ORIENTED_EDGE ( 'NONE', *, *, #29193, .T. ) ;
#3022 = ORIENTED_EDGE ( 'NONE', *, *, #18736, .F. ) ;
#3023 = EDGE_CURVE ( 'NONE', #28371, #5243, #34541, .T. ) ;
#3024 = DIRECTION ( 'NONE',  ( -2.170915417798913418E-16, 0.000000000000000000, -1.000000000000000000 ) ) ;
#3025 = VECTOR ( 'NONE', #19725, 1000.000000000000000 ) ;
#3026 = ORIENTED_EDGE ( 'NONE', *, *, #12789, .T. ) ;
#3027 = EDGE_LOOP ( 'NONE', ( #48707, #4492, #67828, #78131, #34277, #73610 ) ) ;
#3028 = EDGE_CURVE ( 'NONE', #64725, #32634, #70806, .T. ) ;
#3029 = CARTESIAN_POINT ( 'NONE',  ( 99.82831888057269509, -43.73513634207608902, 188.3701547344689686 ) ) ;
#3030 = EDGE_CURVE ( 'NONE', #45213, #82293, #20566, .T. ) ;
#3031 = CARTESIAN_POINT ( 'NONE',  ( -487.2989999999999782, 22.53639197104660141, 90.48749999999999716 ) ) ;
#3032 = AXIS2_PLACEMENT_3D ( 'NONE', #32379, #68272, #87814 ) ;
#3033 = CARTESIAN_POINT ( 'NONE',  ( 96.00479252368074867, -37.29883552165912874, 117.3794347997199594 ) ) ;
#3034 = LINE ( 'NONE', #23930, #39994 ) ;
#3035 = EDGE_CURVE ( 'NONE', #54987, #56697, #11507, .T. ) ;
#3036 = CARTESIAN_POINT ( 'NONE',  ( 104.4076680213851489, -46.45796240592144244, 17.36483092543189244 ) ) ;
#3037 = ORIENTED_EDGE ( 'NONE', *, *, #67402, .T. ) ;
#3038 = EDGE_CURVE ( 'NONE', #23716, #49134, #19215, .T. ) ;
#3039 = AXIS2_PLACEMENT_3D ( 'NONE', #66814, #19562, #39106 ) ;
#3040 = ORIENTED_EDGE ( 'NONE', *, *, #50901, .T. ) ;
#3041 = ORIENTED_EDGE ( 'NONE', *, *, #54810, .F. ) ;
#3042 = EDGE_CURVE ( 'NONE', #1363, #27566, #46445, .T. ) ;
#3043 = CARTESIAN_POINT ( 'NONE',  ( 109.9085748933103162, -45.56225229135190347, 205.6423760838769681 ) ) ;
#3044 = CARTESIAN_POINT ( 'NONE',  ( 100.9280588457464489, -46.89575235069233372, 52.14419670448194921 ) ) ;
#3045 = ORIENTED_EDGE ( 'NONE', *, *, #2639, .T. ) ;
#3046 = CARTESIAN_POINT ( 'NONE',  ( 97.79189512308828114, -32.01662636557816199, 50.95276813305294183 ) ) ;
#3047 = CARTESIAN_POINT ( 'NONE',  ( 98.30744901804703773, -41.72866419761319179, 251.7400428627262272 ) ) ;
#3048 = CARTESIAN_POINT ( 'NONE',  ( 107.0664832912739968, 19.62155284005901024, 333.4006252759110112 ) ) ;
#3049 = DIRECTION ( 'NONE',  ( 1.000000000000000000, 4.012088370409549976E-14, 0.000000000000000000 ) ) ;
#3050 = CARTESIAN_POINT ( 'NONE',  ( 116.8065287754011337, -43.47971597432173496, 159.3441967044829539 ) ) ;
#3051 = EDGE_CURVE ( 'NONE', #58818, #51146, #39200, .T. ) ;
#3052 = PLANE ( 'NONE',  #49461 ) ;
#3053 = VERTEX_POINT ( 'NONE', #87807 ) ;
#3054 = CARTESIAN_POINT ( 'NONE',  ( 184.3595971212631071, -48.62134037874749026, 129.9678068554150059 ) ) ;
#3055 = CIRCLE ( 'NONE', #46533, 5.599999999999994316 ) ;
#3056 = VERTEX_POINT ( 'NONE', #66910 ) ;
#3057 = DIRECTION ( 'NONE',  ( 4.299999999999999979E-14, -1.000000000000000000, 4.400000000000000367E-29 ) ) ;
#3058 = DIRECTION ( 'NONE',  ( 0.000000000000000000, -0.000000000000000000, 1.000000000000000000 ) ) ;
#3059 = ORIENTED_EDGE ( 'NONE', *, *, #48221, .T. ) ;
#3060 = VECTOR ( 'NONE', #65842, 999.9999999999998863 ) ;
#3061 = DIRECTION ( 'NONE',  ( 0.3182345505295408605, 0.3182345505294081889, -0.8930025429407280058 ) ) ;
#3062 = CARTESIAN_POINT ( 'NONE',  ( 98.72235591169328472, -42.97945265871884857, 66.83848241876793850 ) ) ;
#3063 = CARTESIAN_POINT ( 'NONE',  ( -479.3614999999999782, 53.97500000000000142, 50.79999999999999716 ) ) ;
#3064 = CARTESIAN_POINT ( 'NONE',  ( 107.9678037105606023, -87.30234574837474781, -19.18411693322955003 ) ) ;
#3065 = DIRECTION ( 'NONE',  ( 0.000000000000000000, 0.000000000000000000, -1.000000000000000000 ) ) ;
#3066 = CARTESIAN_POINT ( 'NONE',  ( 98.34688518126456813, -32.29864090244028318, 50.95276813305393659 ) ) ;
#3068 = CARTESIAN_POINT ( 'NONE',  ( 114.1099639442525699, -29.07320488188167218, 195.4841967044819739 ) ) ;
#3067 = DIRECTION ( 'NONE',  ( -1.000000000000000000, 0.000000000000000000, -2.108231265501709878E-16 ) ) ;
#3069 = CARTESIAN_POINT ( 'NONE',  ( 99.09461421399829817, -30.55189217855991757, 60.80243564339674833 ) ) ;
#3070 = LINE ( 'NONE', #30333, #46669 ) ;
#3071 = ORIENTED_EDGE ( 'NONE', *, *, #17294, .F. ) ;
#3072 = CIRCLE ( 'NONE', #33470, 42.54500000000000171 ) ;
#3073 = CARTESIAN_POINT ( 'NONE',  ( 134.0664832912739826, -36.72944715994100306, 14.92562527591099908 ) ) ;
#3074 = EDGE_CURVE ( 'NONE', #25046, #85174, #31586, .T. ) ;
#3075 = CARTESIAN_POINT ( 'NONE',  ( 143.0667039024470171, -118.2784471599408960, 230.7030882296565721 ) ) ;
#3076 = EDGE_CURVE ( 'NONE', #39961, #13820, #74179, .T. ) ;
#3077 = CARTESIAN_POINT ( 'NONE',  ( 82.96822048844396136, -129.2743616038035555, 249.3173333679100097 ) ) ;
#3078 = VECTOR ( 'NONE', #53283, 1000.000000000000000 ) ;
#3079 = ADVANCED_FACE ( 'NONE', ( #55042, #19655 ), #26033, .F. ) ;
#3080 = DIRECTION ( 'NONE',  ( 0.000000000000000000, 1.000000000000000000, 0.000000000000000000 ) ) ;
#3082 = ORIENTED_EDGE ( 'NONE', *, *, #36963, .F. ) ;
#3081 = CARTESIAN_POINT ( 'NONE',  ( 117.9786848761844453, -34.69554937534774552, 203.9851490854349549 ) ) ;
#3083 = CARTESIAN_POINT ( 'NONE',  ( 105.7993243576699740, -26.72405701148164425, 145.1773073154230929 ) ) ;
#3084 = CARTESIAN_POINT ( 'NONE',  ( 118.1046235831494755, -32.34975429571041161, 245.1270538473389706 ) ) ;
#3085 = CARTESIAN_POINT ( 'NONE',  ( 108.0381942455320967, -25.67262681319542494, 105.9946728949589811 ) ) ;
#3086 = EDGE_CURVE ( 'NONE', #59810, #59306, #11959, .T. ) ;
#3087 = CARTESIAN_POINT ( 'NONE',  ( 97.33812840985710579, -34.06989766951477350, 252.1185538372223789 ) ) ;
#3088 = FACE_OUTER_BOUND ( 'NONE', #30243, .T. ) ;
#3089 = FACE_OUTER_BOUND ( 'NONE', #23564, .T. ) ;
#3090 = CARTESIAN_POINT ( 'NONE',  ( 113.1776118851075523, -44.75237816312386485, 264.0940798895346688 ) ) ;
#3091 = VERTEX_POINT ( 'NONE', #53698 ) ;
#3092 = ORIENTED_EDGE ( 'NONE', *, *, #87930, .T. ) ;
#3093 = VERTEX_POINT ( 'NONE', #81465 ) ;
#3094 = CIRCLE ( 'NONE', #14702, 2.117000000000000881 ) ;
#3095 = ORIENTED_EDGE ( 'NONE', *, *, #80064, .T. ) ;
#3096 = CARTESIAN_POINT ( 'NONE',  ( 116.3212776292269837, -32.94146857470673240, 74.13562527591093954 ) ) ;
#3097 = CARTESIAN_POINT ( 'NONE',  ( 106.2269110120561635, -47.75074920971118075, 263.5280062282920994 ) ) ;
#3098 = CARTESIAN_POINT ( 'NONE',  ( -69.72411017813060141, 120.6499999999999915, 69.72411017812929401 ) ) ;
#3099 = CARTESIAN_POINT ( 'NONE',  ( 47.62500000000000000, 69.84999999999999432, 292.1000000000000227 ) ) ;
#3101 = CARTESIAN_POINT ( 'NONE',  ( 89.13771950014249512, 72.45860812971086773, 78.16952835488777396 ) ) ;
#3100 = CARTESIAN_POINT ( 'NONE',  ( -492.0614999999999668, 14.28750000000026077, 15.87499999999969802 ) ) ;
#3102 = CARTESIAN_POINT ( 'NONE',  ( 173.9900000000000091, 20.32000000000000028, 71.37400000000000944 ) ) ;
#3103 = AXIS2_PLACEMENT_3D ( 'NONE', #79956, #38152, #4076 ) ;
#3104 = CARTESIAN_POINT ( 'NONE',  ( 115.3915529780678781, -40.29397869100746021, 212.9390864947429804 ) ) ;
#3105 = ORIENTED_EDGE ( 'NONE', *, *, #42203, .F. ) ;
#3106 = ORIENTED_EDGE ( 'NONE', *, *, #1441, .F. ) ;
#3107 = VERTEX_POINT ( 'NONE', #74619 ) ;
#3108 = AXIS2_PLACEMENT_3D ( 'NONE', #72090, #44361, #64381 ) ;
#3109 = FACE_BOUND ( 'NONE', #78919, .T. ) ;
#3110 = CARTESIAN_POINT ( 'NONE',  ( 98.38056673804321406, -41.69552625526764444, 181.7398107738224553 ) ) ;
#3111 = CARTESIAN_POINT ( 'NONE',  ( 105.2300248619054344, -26.52326248388681051, 271.2061014663865990 ) ) ;
#3112 = DIRECTION ( 'NONE',  ( 1.000000000000000078E-15, -1.000000000000000083E-30, -1.000000000000000000 ) ) ;
#3113 = DIRECTION ( 'NONE',  ( -1.000000000000000078E-15, 1.000000000000000000, 0.000000000000000000 ) ) ;
#3114 = CARTESIAN_POINT ( 'NONE',  ( 141.0667039024479834, -50.82844715994100682, 310.9178068554150514 ) ) ;
#3116 = ORIENTED_EDGE ( 'NONE', *, *, #65169, .T. ) ;
#3115 = VECTOR ( 'NONE', #25222, 1000.000000000000000 ) ;
#3117 = CARTESIAN_POINT ( 'NONE',  ( 97.33759702722761631, -34.07205617727079527, 57.11479585955967764 ) ) ;
#3118 = ORIENTED_EDGE ( 'NONE', *, *, #26315, .F. ) ;
#3119 = LINE ( 'NONE', #37644, #65548 ) ;
#3120 = CARTESIAN_POINT ( 'NONE',  ( 110.1825742734413609, -44.80353631977761353, 15.67570941721097100 ) ) ;
#3121 = AXIS2_PLACEMENT_3D ( 'NONE', #15266, #48855, #55656 ) ;
#3122 = DIRECTION ( 'NONE',  ( 1.000000000000000078E-15, 0.000000000000000000, -1.000000000000000000 ) ) ;
#3123 = EDGE_CURVE ( 'NONE', #59883, #27284, #6049, .T. ) ;
#3124 = EDGE_CURVE ( 'NONE', #26617, #74993, #5594, .T. ) ;
#3125 = DIRECTION ( 'NONE',  ( 4.299999999999999979E-14, -1.000000000000000000, 4.400000000000000367E-29 ) ) ;
#3126 = CIRCLE ( 'NONE', #14750, 1.500000000000001332 ) ;
#3127 = CARTESIAN_POINT ( 'NONE',  ( 31.90335556477812773, -33.89581943344378345, 342.9256252759109884 ) ) ;
#3128 = ORIENTED_EDGE ( 'NONE', *, *, #41850, .T. ) ;
#3129 = FACE_OUTER_BOUND ( 'NONE', #76203, .T. ) ;
#3130 = EDGE_CURVE ( 'NONE', #73516, #22726, #80355, .T. ) ;
#3131 = CARTESIAN_POINT ( 'NONE',  ( 107.0664832912750057, -36.72944715993903486, 3.024967495036150922 ) ) ;
#3132 = ORIENTED_EDGE ( 'NONE', *, *, #63384, .F. ) ;
#3133 = CARTESIAN_POINT ( 'NONE',  ( 97.28826076399516865, -33.11373220042904109, 66.04419670448297097 ) ) ;
#3134 = ORIENTED_EDGE ( 'NONE', *, *, #36753, .F. ) ;
#3136 = CIRCLE ( 'NONE', #7483, 4.500000000000003553 ) ;
#3135 = CARTESIAN_POINT ( 'NONE',  ( 112.8214380862813755, -44.54936551000075440, 32.50384839950498872 ) ) ;
#3137 = EDGE_CURVE ( 'NONE', #87926, #55506, #28713, .T. ) ;
#3138 = PLANE ( 'NONE',  #51795 ) ;
#3139 = CARTESIAN_POINT ( 'NONE',  ( 97.72568451978753501, -37.74236564027221874, 77.83205949637394383 ) ) ;
#3140 = CARTESIAN_POINT ( 'NONE',  ( 67.06670390244707392, -137.6784471599409869, 228.4678068554179902 ) ) ;
#3141 = ADVANCED_FACE ( 'NONE', ( #63232 ), #49129, .F. ) ;
#3142 = CARTESIAN_POINT ( 'NONE',  ( 92.91125933621934507, -113.6057974291316981, -19.26696060647573105 ) ) ;
#3143 = CYLINDRICAL_SURFACE ( 'NONE', #12103, 24.50000000000000711 ) ;
#3144 = CARTESIAN_POINT ( 'NONE',  ( 116.4070807376042609, -31.97209126034463011, 40.20133956162496958 ) ) ;
#3146 = EDGE_CURVE ( 'NONE', #19524, #58138, #56850, .T. ) ;
#3145 = DIRECTION ( 'NONE',  ( 0.000000000000000000, -0.8660254037844383745, -0.5000000000000003331 ) ) ;
#3147 = ORIENTED_EDGE ( 'NONE', *, *, #23047, .F. ) ;
#3148 = DIRECTION ( 'NONE',  ( 0.000000000000000000, 0.000000000000000000, 1.000000000000000000 ) ) ;
#3149 = ORIENTED_EDGE ( 'NONE', *, *, #11965, .F. ) ;
#3150 = CARTESIAN_POINT ( 'NONE',  ( 111.8139374584311554, -25.81739915606283375, 130.7499109901969518 ) ) ;
#3151 = CARTESIAN_POINT ( 'NONE',  ( 79.00802158143517318, -21.26771232012923463, 1.799893082726899740 ) ) ;
#3152 = ORIENTED_EDGE ( 'NONE', *, *, #799, .T. ) ;
#3153 = ORIENTED_EDGE ( 'NONE', *, *, #55507, .T. ) ;
#3154 = ADVANCED_FACE ( 'NONE', ( #14648 ), #84594, .T. ) ;
#3155 = AXIS2_PLACEMENT_3D ( 'NONE', #31336, #37271, #57706 ) ;
#3156 = DIRECTION ( 'NONE',  ( 0.000000000000000000, -1.000000000000000000, 0.000000000000000000 ) ) ;
#3157 = DIRECTION ( 'NONE',  ( 0.000000000000000000, 0.4999999999999995004, 0.8660254037844390407 ) ) ;
#3158 = CARTESIAN_POINT ( 'NONE',  ( 109.1965444620390571, -27.18343884754219886, 224.9013395616259459 ) ) ;
#3159 = CARTESIAN_POINT ( 'NONE',  ( 172.5664832912740110, -9.303447159940999356, 138.9256252759119832 ) ) ;
#3160 = CARTESIAN_POINT ( 'NONE',  ( 130.3998166246070127, 12.92155284005802685, 349.2756252759110680 ) ) ;
#3161 = CARTESIAN_POINT ( 'NONE',  ( 97.81170999498195329, -40.51745678363457159, 187.6351607544849287 ) ) ;
#3162 = CARTESIAN_POINT ( 'NONE',  ( 97.28846512631339749, -33.11380776793520653, 62.04419670448196911 ) ) ;
#3163 = EDGE_CURVE ( 'NONE', #17742, #41217, #13740, .T. ) ;
#3164 = CARTESIAN_POINT ( 'NONE',  ( 98.04129921502178036, -41.04139788470866534, 42.68115173508382298 ) ) ;
#3165 = ORIENTED_EDGE ( 'NONE', *, *, #82118, .T. ) ;
#3166 = CARTESIAN_POINT ( 'NONE',  ( 105.0192423035563678, -26.92869720746245576, 171.2403743890392320 ) ) ;
#3167 = DIRECTION ( 'NONE',  ( -0.9770521142508956647, -0.000000000000000000, 0.2130003897598659046 ) ) ;
#3168 = CIRCLE ( 'NONE', #78661, 12.69999999999999929 ) ;
#3170 = ORIENTED_EDGE ( 'NONE', *, *, #16091, .F. ) ;
#3169 = EDGE_CURVE ( 'NONE', #75163, #32749, #49582, .T. ) ;
#3171 = AXIS2_PLACEMENT_3D ( 'NONE', #33661, #51948, #31080 ) ;
#3172 = DIRECTION ( 'NONE',  ( 0.7071067811865784369, -0.7071067811865165975, 7.071067811865791864E-16 ) ) ;
#3173 = DIRECTION ( 'NONE',  ( 0.000000000000000000, 0.000000000000000000, 1.000000000000000000 ) ) ;
#3174 = CARTESIAN_POINT ( 'NONE',  ( 104.3301552612371381, -26.04411461992200927, 245.2880062282919482 ) ) ;
#3175 = FACE_OUTER_BOUND ( 'NONE', #62080, .T. ) ;
#3176 = LINE ( 'NONE', #30874, #50678 ) ;
#3177 = DIRECTION ( 'NONE',  ( -0.04216478779797398074, 0.9991106698809455455, 0.000000000000000000 ) ) ;
#3178 = CARTESIAN_POINT ( 'NONE',  ( 100.3258375188005402, -30.68160747159130963, 235.1790864947439559 ) ) ;
#3180 = CARTESIAN_POINT ( 'NONE',  ( 103.9639062230919251, -47.31423993612432355, 58.33753003781600199 ) ) ;
#3179 = DIRECTION ( 'NONE',  ( -1.000000000000000000, -4.299999999999999979E-14, -1.000000000000000078E-15 ) ) ;
#3181 = CARTESIAN_POINT ( 'NONE',  ( 111.1294417335836044, 64.57244353077730636, 68.52200795564769464 ) ) ;
#3182 = CARTESIAN_POINT ( 'NONE',  ( 102.6790914627476070, -46.92570513279398625, 137.2651490854349561 ) ) ;
#3183 = ORIENTED_EDGE ( 'NONE', *, *, #68690, .F. ) ;
#3184 = CARTESIAN_POINT ( 'NONE',  ( 179.7974245136200011, -36.32844715994040996, 342.9256252759119548 ) ) ;
#3185 = ORIENTED_EDGE ( 'NONE', *, *, #57679, .F. ) ;
#3186 = CARTESIAN_POINT ( 'NONE',  ( 82.54999999999999716, 95.25000000000000000, 280.2255000000000109 ) ) ;
#3187 = FACE_OUTER_BOUND ( 'NONE', #7952, .T. ) ;
#3188 = CARTESIAN_POINT ( 'NONE',  ( 115.8332703014196312, -31.75044964869108810, 275.2380515835822052 ) ) ;
#3189 = EDGE_LOOP ( 'NONE', ( #71067, #73722, #49504, #27268 ) ) ;
#3190 = AXIS2_PLACEMENT_3D ( 'NONE', #44429, #24903, #23581 ) ;
#3191 = EDGE_CURVE ( 'NONE', #23399, #67629, #41787, .T. ) ;
#3192 = DIRECTION ( 'NONE',  ( 0.000000000000000000, 1.000000000000000000, 0.000000000000000000 ) ) ;
#3193 = ORIENTED_EDGE ( 'NONE', *, *, #4873, .T. ) ;
#3194 = CARTESIAN_POINT ( 'NONE',  ( 110.2536356736639220, -106.6957733451320394, 2.217806855418086087 ) ) ;
#3195 = EDGE_CURVE ( 'NONE', #66655, #15446, #15088, .T. ) ;
#3196 = DIRECTION ( 'NONE',  ( 0.000000000000000000, 0.000000000000000000, 1.000000000000000000 ) ) ;
#3197 = CIRCLE ( 'NONE', #10449, 3.500000000000003109 ) ;
#3198 = CARTESIAN_POINT ( 'NONE',  ( 141.0667039024479834, -48.82844715994099971, 250.9178068554160461 ) ) ;
#3199 = ORIENTED_EDGE ( 'NONE', *, *, #89002, .T. ) ;
#3200 = VECTOR ( 'NONE', #39348, 1000.000000000000114 ) ;
#3201 = CARTESIAN_POINT ( 'NONE',  ( 101.6994268497411724, -27.72483345503921370, 85.50419670448295051 ) ) ;
#3202 = DIRECTION ( 'NONE',  ( 0.000000000000000000, 0.000000000000000000, 1.000000000000000000 ) ) ;
#3203 = CARTESIAN_POINT ( 'NONE',  ( 97.78490694950903617, -40.45141876997547570, 166.6299563115132116 ) ) ;
#3204 = CARTESIAN_POINT ( 'NONE',  ( -55.48342271751670296, 20.32000000000000028, 171.1197181046785261 ) ) ;
#3205 = CARTESIAN_POINT ( 'NONE',  ( 105.7154773070653704, -46.72385838926080481, 142.4689586073946543 ) ) ;
#3206 = ORIENTED_EDGE ( 'NONE', *, *, #39653, .T. ) ;
#3207 = VECTOR ( 'NONE', #82179, 1000.000000000000000 ) ;
#3208 = CARTESIAN_POINT ( 'NONE',  ( 100.8465607796070742, 83.38002811471481834, -82.91466710319141953 ) ) ;
#3209 = LINE ( 'NONE', #30019, #61414 ) ;
#3210 = VECTOR ( 'NONE', #26083, 1000.000000000000000 ) ;
#3211 = CARTESIAN_POINT ( 'NONE',  ( 71.06648329127399677, -8.729447159940999512, -5.074374724088000832 ) ) ;
#3212 = VECTOR ( 'NONE', #50264, 1000.000000000000000 ) ;
#3214 = PLANE ( 'NONE',  #31191 ) ;
#3213 = CARTESIAN_POINT ( 'NONE',  ( 117.1057691840046147, -37.46862480412959684, 249.7680016665607354 ) ) ;
#3215 = DIRECTION ( 'NONE',  ( 0.000000000000000000, 1.000000000000000000, 0.000000000000000000 ) ) ;
#3216 = EDGE_CURVE ( 'NONE', #74303, #21031, #48681, .T. ) ;
#3217 = EDGE_LOOP ( 'NONE', ( #66937, #30175 ) ) ;
#3218 = LINE ( 'NONE', #45850, #54897 ) ;
#3219 = CARTESIAN_POINT ( 'NONE',  ( 112.1511370651176662, -26.84216853020821958, 165.6984824187679521 ) ) ;
#3221 = EDGE_LOOP ( 'NONE', ( #56278, #7392, #79586 ) ) ;
#3220 = CARTESIAN_POINT ( 'NONE',  ( 144.4409906766500455, -0.9165124547899898833, 540.9756252759101471 ) ) ;
#3222 = CARTESIAN_POINT ( 'NONE',  ( 116.2977993645975232, -41.52656014244012539, 284.4441967044824082 ) ) ;
#3223 = CARTESIAN_POINT ( 'NONE',  ( 79.56670390244796920, -50.82844715994100682, 104.9178068554150087 ) ) ;
#3224 = CARTESIAN_POINT ( 'NONE',  ( 98.54782847511336286, -41.97726656945443580, 51.76585797866146521 ) ) ;
#3225 = FACE_BOUND ( 'NONE', #50152, .T. ) ;
#3226 = ORIENTED_EDGE ( 'NONE', *, *, #41674, .F. ) ;
#3227 = CARTESIAN_POINT ( 'NONE',  ( 102.0677619940791914, -27.97008352907843687, 30.48995469929853286 ) ) ;
#3228 = ORIENTED_EDGE ( 'NONE', *, *, #59103, .F. ) ;
#3229 = VECTOR ( 'NONE', #9904, 1000.000000000000000 ) ;
#3230 = ORIENTED_EDGE ( 'NONE', *, *, #31735, .F. ) ;
#3231 = EDGE_CURVE ( 'NONE', #61365, #36567, #8275, .T. ) ;
#3232 = CARTESIAN_POINT ( 'NONE',  ( 109.9841060568515729, -28.36190534590500434, 206.2415833058969667 ) ) ;
#3233 = VECTOR ( 'NONE', #6596, 1000.000000000000000 ) ;
#3234 = DIRECTION ( 'NONE',  ( -1.000000000000000000, 1.011922027653136551E-15, 0.000000000000000000 ) ) ;
#3235 = CARTESIAN_POINT ( 'NONE',  ( 99.19755098026091389, -30.44051964901187191, 42.22158330589692810 ) ) ;
#3236 = CARTESIAN_POINT ( 'NONE',  ( -95.16331303980125256, 94.60320878023493663, 89.38347482486680917 ) ) ;
#3237 = EDGE_CURVE ( 'NONE', #33634, #13721, #35974, .T. ) ;
#3238 = ADVANCED_FACE ( 'NONE', ( #41867 ), #15543, .F. ) ;
#3239 = CARTESIAN_POINT ( 'NONE',  ( 108.4174892568073005, -26.73503592836434706, 79.96895860887276797 ) ) ;
#3240 = CYLINDRICAL_SURFACE ( 'NONE', #58938, 9.999999999999998224 ) ;
#3241 = ORIENTED_EDGE ( 'NONE', *, *, #60322, .F. ) ;
#3242 = LINE ( 'NONE', #37310, #40634 ) ;
#3243 = ADVANCED_FACE ( 'NONE', ( #79113 ), #10501, .F. ) ;
#3244 = CARTESIAN_POINT ( 'NONE',  ( -31.27367473141074683, 148.4450814996825443, 74.45358409497265484 ) ) ;
#3245 = VERTEX_POINT ( 'NONE', #2806 ) ;
#3246 = CARTESIAN_POINT ( 'NONE',  ( 117.4695305279094981, -36.80206755349689729, 263.8213395616251660 ) ) ;
#3247 = CARTESIAN_POINT ( 'NONE',  ( 10.08805235722132565, 90.30997682696688855, 118.1269383658995338 ) ) ;
#3248 = VERTEX_POINT ( 'NONE', #3687 ) ;
#3249 = VECTOR ( 'NONE', #48898, 1000.000000000000000 ) ;
#3250 = EDGE_CURVE ( 'NONE', #25538, #23113, #65902, .T. ) ;
#3251 = CARTESIAN_POINT ( 'NONE',  ( 116.8171228667533796, -34.15291832118845150, 84.03145860919784127 ) ) ;
#3252 = DIRECTION ( 'NONE',  ( 0.9130365726098600421, 0.000000000000000000, 0.4078776986755215939 ) ) ;
#3253 = CARTESIAN_POINT ( 'NONE',  ( -465.6921742093550165, 47.62500000000000000, 3.174999999999999822 ) ) ;
#3254 = CARTESIAN_POINT ( 'NONE',  ( 0.000000000000000000, 124.5870000000000033, 0.000000000000000000 ) ) ;
#3255 = CARTESIAN_POINT ( 'NONE',  ( 96.60079736239889314, -36.47965167166085365, 192.3070538473399438 ) ) ;
#3256 = DIRECTION ( 'NONE',  ( 0.000000000000000000, 1.000000000000000000, 0.000000000000000000 ) ) ;
#3257 = EDGE_CURVE ( 'NONE', #21223, #28033, #72293, .T. ) ;
#3258 = EDGE_LOOP ( 'NONE', ( #10676, #48610 ) ) ;
#3259 = CIRCLE ( 'NONE', #74314, 3.000000000000002665 ) ;
#3260 = CARTESIAN_POINT ( 'NONE',  ( 112.9878179797879909, -28.09632633057573159, 40.59848241876795782 ) ) ;
#3261 = DIRECTION ( 'NONE',  ( 2.900000000000000265E-14, -2.000000000000000155E-15, 1.000000000000000000 ) ) ;
#3262 = CARTESIAN_POINT ( 'NONE',  ( 111.7391504816189212, -27.40993963462091543, 279.7070538473396937 ) ) ;
#3263 = ORIENTED_EDGE ( 'NONE', *, *, #64249, .T. ) ;
#3264 = ADVANCED_FACE ( 'NONE', ( #51813 ), #9609, .T. ) ;
#3265 = CIRCLE ( 'NONE', #72887, 9.425000000000000711 ) ;
#3266 = DIRECTION ( 'NONE',  ( 1.000000000000000078E-15, -1.000000000000000000, 3.100000000000000044E-14 ) ) ;
#3267 = CARTESIAN_POINT ( 'NONE',  ( 105.7160904893042783, -46.72395770272043336, 18.46948113466270769 ) ) ;
#3268 = DIRECTION ( 'NONE',  ( 0.000000000000000000, 0.000000000000000000, 1.000000000000000000 ) ) ;
#3269 = CARTESIAN_POINT ( 'NONE',  ( 114.8246268090051245, -34.19154740317726038, 86.89666179816296676 ) ) ;
#3270 = CARTESIAN_POINT ( 'NONE',  ( 98.24294948823698803, -42.32252413779357170, 182.7756252759109543 ) ) ;
#3271 = LINE ( 'NONE', #67262, #65315 ) ;
#3272 = ORIENTED_EDGE ( 'NONE', *, *, #5036, .F. ) ;
#3273 = PLANE ( 'NONE',  #49425 ) ;
#3274 = EDGE_LOOP ( 'NONE', ( #29356, #25141, #17679, #23241 ) ) ;
#3275 = ORIENTED_EDGE ( 'NONE', *, *, #16027, .F. ) ;
#3276 = CARTESIAN_POINT ( 'NONE',  ( 0.000000000000000000, 114.2999999999999972, 0.000000000000000000 ) ) ;
#3277 =( BOUNDED_CURVE ( )  B_SPLINE_CURVE ( 3, ( #1908, #7374, #21913, #28711 ),
 .UNSPECIFIED., .F., .T. ) 
 B_SPLINE_CURVE_WITH_KNOTS ( ( 4, 4 ),
 ( 1.506129919829842123, 1.572423208257343274 ),
 .UNSPECIFIED. ) 
 CURVE ( )  GEOMETRIC_REPRESENTATION_ITEM ( )  RATIONAL_B_SPLINE_CURVE ( ( 1.000000000000000000, 0.9996338001896092340, 0.9996338001896092340, 1.000000000000000000 ) ) 
 REPRESENTATION_ITEM ( '' )  );
#3278 = ORIENTED_EDGE ( 'NONE', *, *, #8194, .F. ) ;
#3279 = ORIENTED_EDGE ( 'NONE', *, *, #89079, .T. ) ;
#3280 = CARTESIAN_POINT ( 'NONE',  ( 112.0675020739599006, -45.48750542127923779, 168.9906668250784776 ) ) ;
#3281 = CARTESIAN_POINT ( 'NONE',  ( 99.09569553996823288, -30.55044851293582653, 41.80222573704838851 ) ) ;
#3282 = CARTESIAN_POINT ( 'NONE',  ( 98.01892258562502036, -37.12227740767932715, 115.7714674471239675 ) ) ;
#3283 = B_SPLINE_CURVE_WITH_KNOTS ( 'NONE', 3,
 ( #20790, #13973, #42112, #69838, #69391 ),
 .UNSPECIFIED., .F., .F.,
 ( 4, 1, 4 ),
 ( 0.000000000000000000, 0.5713596581863561452, 1.000000000000000000 ),
 .UNSPECIFIED. ) ;
#3284 = CARTESIAN_POINT ( 'NONE',  ( 105.4140021367065003, -47.06753073853725056, 37.44991099019695469 ) ) ;
#3285 = VECTOR ( 'NONE', #50335, 1000.000000000000000 ) ;
#3286 = CARTESIAN_POINT ( 'NONE',  ( -11.39831192919941927, 76.93384533283848725, 130.0576265831481635 ) ) ;
#3287 = ORIENTED_EDGE ( 'NONE', *, *, #64697, .T. ) ;
#3288 = CARTESIAN_POINT ( 'NONE',  ( 103.2790154487345688, -27.47444377515469682, 136.3855822504286266 ) ) ;
#3289 = ORIENTED_EDGE ( 'NONE', *, *, #36504, .T. ) ;
#3290 = CARTESIAN_POINT ( 'NONE',  ( 80.06648329127401098, -41.22944715994105280, 4.925625275910944012 ) ) ;
#3291 = CARTESIAN_POINT ( 'NONE',  ( 117.0605793477646444, -38.08267519577708526, 33.71899569443299782 ) ) ;
#3292 = ADVANCED_FACE ( 'NONE', ( #87259 ), #30504, .F. ) ;
#3293 = DIRECTION ( 'NONE',  ( -1.000000000000000000, -3.999999999999999995E-14, -1.000000000000000078E-15 ) ) ;
#3294 = VECTOR ( 'NONE', #20015, 1000.000000000000000 ) ;
#3295 = DIRECTION ( 'NONE',  ( -0.000000000000000000, 1.000000000000000000, -0.000000000000000000 ) ) ;
#3296 = ORIENTED_EDGE ( 'NONE', *, *, #51682, .F. ) ;
#3297 = CARTESIAN_POINT ( 'NONE',  ( 115.6554515427140473, -30.75822225795367970, 279.3099109901966131 ) ) ;
#3298 = CARTESIAN_POINT ( 'NONE',  ( 104.2291421067619694, -46.80627582718438617, 18.35848241876792031 ) ) ;
#3299 = SURFACE_STYLE_USAGE ( .BOTH. , #17812 ) ;
#3300 = CARTESIAN_POINT ( 'NONE',  ( 90.44969454456415292, -53.34645651782494724, 229.5838068554169809 ) ) ;
#3302 = DIRECTION ( 'NONE',  ( 0.000000000000000000, 0.000000000000000000, -1.000000000000000000 ) ) ;
#3301 = CARTESIAN_POINT ( 'NONE',  ( 76.24325998657069192, -5.906223855237660914, -5.074374724089060429 ) ) ;
#3303 = FACE_OUTER_BOUND ( 'NONE', #82744, .T. ) ;
#3304 = CARTESIAN_POINT ( 'NONE',  ( 83.06670390244796920, -67.87844715994100397, 201.9838068554149970 ) ) ;
#3305 = CARTESIAN_POINT ( 'NONE',  ( 51.06670390244799762, -33.35206098992630075, 342.9256252759119548 ) ) ;
#3306 = FACE_OUTER_BOUND ( 'NONE', #82321, .T. ) ;
#3307 = CARTESIAN_POINT ( 'NONE',  ( 99.04410099017079006, -42.84131659189329611, 161.8437698291777735 ) ) ;
#3308 = AXIS2_PLACEMENT_3D ( 'NONE', #22031, #8389, #659 ) ;
#3309 = DIRECTION ( 'NONE',  ( 1.000000000000000078E-15, -1.000000000000000083E-30, -1.000000000000000000 ) ) ;
#3310 = CARTESIAN_POINT ( 'NONE',  ( 111.7836659179374408, -46.75466717335095268, 287.9146728949587555 ) ) ;
#3311 = CARTESIAN_POINT ( 'NONE',  ( 109.3584748782654401, -25.91645705315499981, 180.9222919425779708 ) ) ;
#3312 = CARTESIAN_POINT ( 'NONE',  ( 106.6058858729755201, -25.66269263286424263, 36.09753003781596448 ) ) ;
#3314 = PLANE ( 'NONE',  #39955 ) ;
#3313 = FACE_OUTER_BOUND ( 'NONE', #54090, .T. ) ;
#3315 = CARTESIAN_POINT ( 'NONE',  ( 81.97596355239819843, -34.74831825238398864, 2.232988539021949492 ) ) ;
#3317 = EDGE_CURVE ( 'NONE', #45463, #28588, #11335, .T. ) ;
#3316 = AXIS2_PLACEMENT_3D ( 'NONE', #89644, #6080, #54627 ) ;
#3318 = ORIENTED_EDGE ( 'NONE', *, *, #88036, .T. ) ;
#3319 = FACE_OUTER_BOUND ( 'NONE', #48560, .T. ) ;
#3320 = ORIENTED_EDGE ( 'NONE', *, *, #23264, .T. ) ;
#3321 = AXIS2_PLACEMENT_3D ( 'NONE', #11100, #2524, #79282 ) ;
#3322 = CARTESIAN_POINT ( 'NONE',  ( 114.7602587138392209, -43.68247563549507362, 79.25372051400597684 ) ) ;
#3324 = VERTEX_POINT ( 'NONE', #9172 ) ;
#3323 = CARTESIAN_POINT ( 'NONE',  ( 6.966821914208871647, 93.16860575031896019, 130.3699860581843382 ) ) ;
#3325 = CARTESIAN_POINT ( 'NONE',  ( 1.598849875094818280E-14, 101.5999999999999943, -130.5560000000000116 ) ) ;
#3326 = CARTESIAN_POINT ( 'NONE',  ( 101.4371718687638406, -46.21494532752021200, 203.1622919425779514 ) ) ;
#3327 = CARTESIAN_POINT ( 'NONE',  ( 107.7702177616926065, 120.6499999999999915, 4.179089330879380409E-13 ) ) ;
#3328 = CARTESIAN_POINT ( 'NONE',  ( 105.7153080974451882, -46.72383283222870887, 147.4690131811856872 ) ) ;
#3329 = DIRECTION ( 'NONE',  ( 0.000000000000000000, -1.000000000000000000, 0.000000000000000000 ) ) ;
#3330 = DIRECTION ( 'NONE',  ( -6.831565154159360295E-14, 1.000000000000000000, 0.000000000000000000 ) ) ;
#3331 = PRODUCT_DEFINITION ( 'UNKNOWN', '', #4369, #22642 ) ;
#3332 = FACE_OUTER_BOUND ( 'NONE', #52166, .T. ) ;
#3333 = CARTESIAN_POINT ( 'NONE',  ( 111.3489484856832235, -45.76813167571804541, 97.92856849314694045 ) ) ;
#3334 = CARTESIAN_POINT ( 'NONE',  ( 108.9483104351207317, -46.92736419409159510, 127.7337205140069472 ) ) ;
#3335 = ORIENTED_EDGE ( 'NONE', *, *, #973, .T. ) ;
#3336 = VERTEX_POINT ( 'NONE', #37770 ) ;
#3337 = CARTESIAN_POINT ( 'NONE',  ( 107.2073525216087120, -27.33494443775582639, 76.50824997256394511 ) ) ;
#3338 = CARTESIAN_POINT ( 'NONE',  ( 31.56670390244800828, -32.29483332968611364, -5.074374724088000832 ) ) ;
#3340 = DIRECTION ( 'NONE',  ( 0.000000000000000000, 0.000000000000000000, -1.000000000000000000 ) ) ;
#3339 = CARTESIAN_POINT ( 'NONE',  ( 101.2091419812965256, -45.28691980162477648, 238.1108633711489517 ) ) ;
#3341 = CARTESIAN_POINT ( 'NONE',  ( 25.56670390244797275, -62.87844715994099687, 293.2178068554150627 ) ) ;
#3342 = CARTESIAN_POINT ( 'NONE',  ( 179.4595971212889935, -28.98061976758940617, -5.074374724088000832 ) ) ;
#3343 = B_SPLINE_CURVE_WITH_KNOTS ( 'NONE', 3,
 ( #16058, #84658, #1077, #27878, #76937, #8804, #50100, #15158, #35131, #56469, #71476, #50554, #64206, #14266, #84217, #55553, #42834, #28789, #618, #21987, #9238, #49203, #21073, #43286, #70571, #7443, #41939, #14715, #48749, #57368, #63300, #8345, #1536, #62842, #28315, #77836, #85109 ),
 .UNSPECIFIED., .F., .F.,
 ( 4, 2, 2, 1, 2, 2, 2, 1, 1, 2, 2, 2, 2, 1, 2, 2, 2, 1, 1, 1, 2, 4 ),
 ( 0.6666501603264138875, 0.6874845253060100081, 0.6926931165509091493, 0.6979017077958082904, 0.7083188902856059066, 0.7499876202447992579, 0.7525919158672497167, 0.7551962114897000644, 0.7604048027346009819, 0.7708219852244027059, 0.7916563502040085964, 0.8124907151836144870, 0.8176993064285161816, 0.8229078976734178763, 0.8333250801632203775, 0.8749938101224256082, 0.8775981057448752898, 0.8802024013673249714, 0.8854109926122243346, 0.8958281751020222838, 0.9166625400816181823, 1.000000000000000000 ),
 .UNSPECIFIED. ) ;
#3344 = ADVANCED_FACE ( 'NONE', ( #86813 ), #10940, .F. ) ;
#3345 = CARTESIAN_POINT ( 'NONE',  ( 117.8738102209308920, 82.54999999999999716, -12.69999999999876827 ) ) ;
#3346 = DIRECTION ( 'NONE',  ( -1.387778780781444413E-14, -1.000000000000000000, 0.000000000000000000 ) ) ;
#3347 = AXIS2_PLACEMENT_3D ( 'NONE', #55568, #56024, #63315 ) ;
#3348 = FACE_OUTER_BOUND ( 'NONE', #21113, .T. ) ;
#3349 = ADVANCED_FACE ( 'NONE', ( #72732, #43672 ), #85936, .F. ) ;
#3350 = DIRECTION ( 'NONE',  ( -0.000000000000000000, 1.000000000000000000, 0.000000000000000000 ) ) ;
#3351 = CARTESIAN_POINT ( 'NONE',  ( 102.0922439024870982, -27.59239485085791088, 145.4727681330539610 ) ) ;
#3352 = EDGE_CURVE ( 'NONE', #66793, #76220, #23706, .T. ) ;
#3353 = VERTEX_POINT ( 'NONE', #3253 ) ;
#3354 = ORIENTED_EDGE ( 'NONE', *, *, #70618, .F. ) ;
#3355 = ADVANCED_FACE ( 'NONE', ( #71408 ), #38206, .T. ) ;
#3356 = CARTESIAN_POINT ( 'NONE',  ( 86.71899144006731319, -85.80981821983746727, 250.2201230397200220 ) ) ;
#3357 = CARTESIAN_POINT ( 'NONE',  ( 97.33784134183721903, -34.07106442030320892, 152.1147919335942333 ) ) ;
#3358 = DIRECTION ( 'NONE',  ( -1.000000000000000000, 0.000000000000000000, 0.000000000000000000 ) ) ;
#3359 = CARTESIAN_POINT ( 'NONE',  ( 97.86644802266228282, -40.64892155565895848, 102.6469608634411372 ) ) ;
#3360 = VECTOR ( 'NONE', #83469, 1000.000000000000000 ) ;
#3361 = CARTESIAN_POINT ( 'NONE',  ( 108.3334346252740517, -46.73486118540429857, 268.6772908713167567 ) ) ;
#3362 = CARTESIAN_POINT ( 'NONE',  ( 102.9670468844020235, -26.46427747797763175, 175.3908633711489813 ) ) ;
#3363 = CYLINDRICAL_SURFACE ( 'NONE', #34239, 9.999999999999998224 ) ;
#3364 = ORIENTED_EDGE ( 'NONE', *, *, #17294, .T. ) ;
#3366 = VERTEX_POINT ( 'NONE', #59074 ) ;
#3365 = ORIENTED_EDGE ( 'NONE', *, *, #29121, .T. ) ;
#3367 = ADVANCED_FACE ( 'NONE', ( #24580 ), #52247, .F. ) ;
#3368 = CARTESIAN_POINT ( 'NONE',  ( 97.90457037977253663, -40.73788048421130981, 62.65513217813478519 ) ) ;
#3369 = DIRECTION ( 'NONE',  ( 0.000000000000000000, 1.000000000000000000, 0.000000000000000000 ) ) ;
#3370 = DIRECTION ( 'NONE',  ( 3.100000000000000258E-29, -3.100000000000000044E-14, -1.000000000000000000 ) ) ;
#3371 = CARTESIAN_POINT ( 'NONE',  ( 114.0851551000824600, -43.95502333027237540, 264.6215833058971043 ) ) ;
#3372 = LINE ( 'NONE', #66469, #46346 ) ;
#3373 = ORIENTED_EDGE ( 'NONE', *, *, #13817, .T. ) ;
#3374 = CARTESIAN_POINT ( 'NONE',  ( 110.3061846121042464, -44.54875278746831668, 9.635625275910943088 ) ) ;
#3375 = CARTESIAN_POINT ( 'NONE',  ( 163.0664832912739826, -0.7548456658610993575, 333.4006252759120343 ) ) ;
#3376 = ORIENTED_EDGE ( 'NONE', *, *, #64892, .F. ) ;
#3377 = VERTEX_POINT ( 'NONE', #50938 ) ;
#3378 = VECTOR ( 'NONE', #53973, 1000.000000000000000 ) ;
#3379 = CARTESIAN_POINT ( 'NONE',  ( 116.5693234920293406, -33.54757666135687089, 114.0835099680320468 ) ) ;
#3380 = ORIENTED_EDGE ( 'NONE', *, *, #47014, .T. ) ;
#3381 = VERTEX_POINT ( 'NONE', #80009 ) ;
#3382 = FACE_OUTER_BOUND ( 'NONE', #82012, .T. ) ;
#3383 = VECTOR ( 'NONE', #82830, 1000.000000000000000 ) ;
#3384 = CARTESIAN_POINT ( 'NONE',  ( 105.7183000297088284, -45.16381338481517815, 36.87241982807598362 ) ) ;
#3385 = CARTESIAN_POINT ( 'NONE',  ( 96.16820482414080118, -32.01123326506838396, 211.0013395616249738 ) ) ;
#3386 = CARTESIAN_POINT ( 'NONE',  ( 95.33621695423326514, -38.27597901479985865, 151.4299109901969871 ) ) ;
#3387 = DIRECTION ( 'NONE',  ( 0.000000000000000000, 1.000000000000000000, 0.000000000000000000 ) ) ;
#3388 = CARTESIAN_POINT ( 'NONE',  ( 105.1090458072749527, -25.85091697680629608, 271.2061014663872243 ) ) ;
#3389 = CARTESIAN_POINT ( 'NONE',  ( 141.8664832912729992, -71.52944715994142655, 352.4506252759077825 ) ) ;
#3390 = CARTESIAN_POINT ( 'NONE',  ( -129.9778716492873230, 79.25971567868511158, -12.27341459163442039 ) ) ;
#3391 = ORIENTED_EDGE ( 'NONE', *, *, #2013, .T. ) ;
#3392 = VERTEX_POINT ( 'NONE', #17764 ) ;
#3393 = EDGE_CURVE ( 'NONE', #60724, #64884, #18658, .T. ) ;
#3394 = CARTESIAN_POINT ( 'NONE',  ( 115.0114139542580318, -28.97761122332106964, 194.4537205140059370 ) ) ;
#3395 = VERTEX_POINT ( 'NONE', #59523 ) ;
#3396 = CARTESIAN_POINT ( 'NONE',  ( 95.90979441981569664, -32.73335165780250122, 176.0527681330539735 ) ) ;
#3397 = CARTESIAN_POINT ( 'NONE',  ( 116.3259679314843282, -32.93868236591013243, 264.1356252759109680 ) ) ;
#3398 = AXIS2_PLACEMENT_3D ( 'NONE', #24982, #52649, #18157 ) ;
#3399 = CARTESIAN_POINT ( 'NONE',  ( 123.1292039024470029, -68.87844715994093292, 222.2178068554179902 ) ) ;
#3400 = EDGE_CURVE ( 'NONE', #19567, #38055, #1235, .T. ) ;
#3401 = LINE ( 'NONE', #46493, #50803 ) ;
#3402 = CARTESIAN_POINT ( 'NONE',  ( 32.09598329127712901, -23.42844715994121785, 237.4678068554150059 ) ) ;
#3405 = CARTESIAN_POINT ( 'NONE',  ( 100.1919508713739759, -45.35525880799009713, 268.0289586092443415 ) ) ;
#3404 = CARTESIAN_POINT ( 'NONE',  ( 70.63919639214310564, 65.60000000000000853, 95.21359708083839735 ) ) ;
#3403 = LINE ( 'NONE', #58358, #84123 ) ;
#3406 = CARTESIAN_POINT ( 'NONE',  ( 71.25529199314600248, -79.12815651470191369, 394.9756252759101471 ) ) ;
#3407 = DIRECTION ( 'NONE',  ( 0.000000000000000000, 0.000000000000000000, -1.000000000000000000 ) ) ;
#3408 = ADVANCED_BREP_SHAPE_REPRESENTATION ( '', ( #20639, #50656 ), #4304 ) ;
#3409 = CARTESIAN_POINT ( 'NONE',  ( 97.07198150990221563, -35.37932431885204210, 272.2185945074161282 ) ) ;
#3410 = VECTOR ( 'NONE', #78654, 1000.000000000000000 ) ;
#3411 = CARTESIAN_POINT ( 'NONE',  ( 67.49635100332064042, -137.4243301806155841, 246.7471779864713994 ) ) ;
#3412 = DIRECTION ( 'NONE',  ( -3.100000000000000258E-29, 3.100000000000000044E-14, 1.000000000000000000 ) ) ;
#3413 = CARTESIAN_POINT ( 'NONE',  ( 97.81169182074827972, -40.51741433969252881, 77.63574375254798099 ) ) ;
#3415 = ORIENTED_EDGE ( 'NONE', *, *, #59729, .T. ) ;
#3414 = CARTESIAN_POINT ( 'NONE',  ( 114.5003034259403876, -40.32092683139836709, 195.5838068554168103 ) ) ;
#3416 = CARTESIAN_POINT ( 'NONE',  ( 136.4532669483820086, -20.09809895853697626, 7.205238605735853952 ) ) ;
#3417 = CARTESIAN_POINT ( 'NONE',  ( 113.1683672335202431, -26.54116819535108363, 204.6470538473399756 ) ) ;
#3418 = CARTESIAN_POINT ( 'NONE',  ( 110.4565933333529699, -47.24995733706104062, 53.83657765686300678 ) ) ;
#3419 = CARTESIAN_POINT ( 'NONE',  ( 110.2692182064865420, -26.72542277727598403, 230.8299109901969643 ) ) ;
#3420 = CARTESIAN_POINT ( 'NONE',  ( 71.06648329127399677, -18.82844715994099971, -5.074374724088000832 ) ) ;
#3421 = FACE_OUTER_BOUND ( 'NONE', #44834, .T. ) ;
#3423 = CARTESIAN_POINT ( 'NONE',  ( 99.03269296098446262, -42.71672268585848542, 37.83590083622135580 ) ) ;
#3422 = CARTESIAN_POINT ( 'NONE',  ( 37.06648329127400388, 12.92155284005802685, 335.5992267699910485 ) ) ;
#3424 = DIRECTION ( 'NONE',  ( 0.000000000000000000, -1.000000000000000000, 0.000000000000000000 ) ) ;
#3425 = DIRECTION ( 'NONE',  ( 1.000000000000000000, 0.000000000000000000, 0.000000000000000000 ) ) ;
#3426 = VECTOR ( 'NONE', #74195, 1000.000000000000000 ) ;
#3427 = CARTESIAN_POINT ( 'NONE',  ( 97.53191058446375905, -39.74916629817411717, 66.57112017202103971 ) ) ;
#3428 = EDGE_CURVE ( 'NONE', #10086, #80351, #7057, .T. ) ;
#3429 = ORIENTED_EDGE ( 'NONE', *, *, #25778, .T. ) ;
#3430 = ORIENTED_EDGE ( 'NONE', *, *, #49161, .F. ) ;
#3431 = CARTESIAN_POINT ( 'NONE',  ( 115.5032561769494066, -38.06248691838574416, 113.1238483995059596 ) ) ;
#3433 = ORIENTED_EDGE ( 'NONE', *, *, #35404, .F. ) ;
#3432 = FACE_OUTER_BOUND ( 'NONE', #89510, .T. ) ;
#3434 = CARTESIAN_POINT ( 'NONE',  ( 103.3702027031294648, -47.12181610991854086, 98.31657765686297523 ) ) ;
#3435 = DIRECTION ( 'NONE',  ( 0.000000000000000000, 0.000000000000000000, 1.000000000000000000 ) ) ;
#3436 = CARTESIAN_POINT ( 'NONE',  ( 78.64593636902102958, -16.36767598605628393, 7.908804215164068729 ) ) ;
#3437 = CARTESIAN_POINT ( 'NONE',  ( -44.45000000000000284, 50.79999999999999716, 206.3750000000000000 ) ) ;
#3438 = CARTESIAN_POINT ( 'NONE',  ( 105.5226833586260682, -46.38761039419750176, 37.44991099019695469 ) ) ;
#3439 = ORIENTED_EDGE ( 'NONE', *, *, #23571, .T. ) ;
#3440 = ORIENTED_EDGE ( 'NONE', *, *, #73892, .F. ) ;
#3441 = VERTEX_POINT ( 'NONE', #73616 ) ;
#3442 = AXIS2_PLACEMENT_3D ( 'NONE', #11677, #66625, #40255 ) ;
#3443 = CARTESIAN_POINT ( 'NONE',  ( 147.0667039024470739, -137.6784471599409017, 228.4678068554179902 ) ) ;
#3444 = DIRECTION ( 'NONE',  ( 1.000000000000000078E-15, 1.000000000000000083E-30, -1.000000000000000000 ) ) ;
#3446 = AXIS2_PLACEMENT_3D ( 'NONE', #51287, #18570, #3173 ) ;
#3445 = CARTESIAN_POINT ( 'NONE',  ( 196.2150000000000034, 37.33800000000000097, 50.79999999999999716 ) ) ;
#3447 = CARTESIAN_POINT ( 'NONE',  ( -446.0240000000000009, 53.97500000000000142, -1.387778780781445991E-14 ) ) ;
#3448 = CARTESIAN_POINT ( 'NONE',  ( 130.5667039024479834, -36.72944715994100306, 239.5838068554162987 ) ) ;
#3449 = CARTESIAN_POINT ( 'NONE',  ( 109.7256116747375785, -27.00100285621926233, 50.86608334895753813 ) ) ;
#3450 = EDGE_CURVE ( 'NONE', #51171, #80177, #61760, .T. ) ;
#3451 = CARTESIAN_POINT ( 'NONE',  ( 223.2659999999999911, 52.73749999999999716, -32.00399999999999778 ) ) ;
#3452 = CARTESIAN_POINT ( 'NONE',  ( -7.303152832728717847, 92.94038696238578723, 130.3515497892399821 ) ) ;
#3453 = CARTESIAN_POINT ( 'NONE',  ( 112.7298150101557894, -27.26422151970076158, 54.65943479971996055 ) ) ;
#3454 = ORIENTED_EDGE ( 'NONE', *, *, #53244, .F. ) ;
#3455 = EDGE_CURVE ( 'NONE', #79347, #59817, #19546, .T. ) ;
#3456 = ORIENTED_EDGE ( 'NONE', *, *, #348, .T. ) ;
#3457 = CARTESIAN_POINT ( 'NONE',  ( 1.653891986036727157, 95.16955141394545592, 130.5480982590283929 ) ) ;
#3458 = CARTESIAN_POINT ( 'NONE',  ( -158.9822249764580135, 20.32000000000000028, 107.9500000000000028 ) ) ;
#3459 = FACE_BOUND ( 'NONE', #49722, .T. ) ;
#3460 = CARTESIAN_POINT ( 'NONE',  ( 98.14730025337767927, -34.17130281729839680, 138.9223760838769692 ) ) ;
#3461 = VECTOR ( 'NONE', #53125, 1000.000000000000000 ) ;
#3462 = AXIS2_PLACEMENT_3D ( 'NONE', #13486, #56133, #747 ) ;
#3463 = CARTESIAN_POINT ( 'NONE',  ( 34.27258461953899626, -35.55794170701810941, -5.074374724088000832 ) ) ;
#3464 = EDGE_LOOP ( 'NONE', ( #42569, #33408, #27715, #60217, #68798, #53637, #1185, #81075, #30294, #70743, #67951, #15665, #4398, #59481, #21360, #55428, #73289, #84793, #23699, #19501, #86373, #70073 ) ) ;
#3465 = EDGE_LOOP ( 'NONE', ( #22122, #15213, #52644, #21783 ) ) ;
#3466 = EDGE_CURVE ( 'NONE', #51387, #71603, #40435, .T. ) ;
#3467 = CARTESIAN_POINT ( 'NONE',  ( 151.0371591254575776, -24.42818131005592974, 117.4678068554150485 ) ) ;
#3468 = CIRCLE ( 'NONE', #15079, 16.00000000000000000 ) ;
#3469 = ORIENTED_EDGE ( 'NONE', *, *, #88264, .F. ) ;
#3470 = ORIENTED_EDGE ( 'NONE', *, *, #14907, .F. ) ;
#3471 = EDGE_CURVE ( 'NONE', #54390, #10350, #12838, .T. ) ;
#3472 = CARTESIAN_POINT ( 'NONE',  ( 57.14999999999999858, 69.84999999999999432, 323.0879999999999654 ) ) ;
#3473 = CARTESIAN_POINT ( 'NONE',  ( 102.8032110495234264, -45.10208326393837552, 168.6453928297069353 ) ) ;
#3474 = FACE_OUTER_BOUND ( 'NONE', #11009, .T. ) ;
#3475 = CARTESIAN_POINT ( 'NONE',  ( 68.53801554307449351, 120.6499999999999915, -74.15067561874229796 ) ) ;
#3476 = DIRECTION ( 'NONE',  ( -1.000000000000000078E-15, 1.000000000000000000, 0.000000000000000000 ) ) ;
#3477 = VERTEX_POINT ( 'NONE', #5028 ) ;
#3478 = ORIENTED_EDGE ( 'NONE', *, *, #38035, .F. ) ;
#3479 = ORIENTED_EDGE ( 'NONE', *, *, #7458, .T. ) ;
#3480 = CARTESIAN_POINT ( 'NONE',  ( 104.4487311862825578, -28.48030787377049577, 203.1271379886389639 ) ) ;
#3481 = CARTESIAN_POINT ( 'NONE',  ( 98.62940354253828446, -43.90657238178356181, 76.89943479971999807 ) ) ;
#3482 = CARTESIAN_POINT ( 'NONE',  ( 96.70769389551958284, -42.43415482991314036, 26.72705384733997747 ) ) ;
#3483 = CARTESIAN_POINT ( 'NONE',  ( 64.68306507141296890, -72.55818180160879649, 361.9756252759101471 ) ) ;
#3484 = CARTESIAN_POINT ( 'NONE',  ( 182.5667039024478413, -32.29483332967956244, 193.9678068554150059 ) ) ;
#3485 = CARTESIAN_POINT ( 'NONE',  ( 98.16828830165673025, -31.29763223543249850, 166.8899109901969950 ) ) ;
#3486 = LINE ( 'NONE', #30751, #59578 ) ;
#3487 = EDGE_LOOP ( 'NONE', ( #22652, #78379, #77739, #75778 ) ) ;
#3488 = CARTESIAN_POINT ( 'NONE',  ( 116.3212776292270973, -32.94146857470704504, 49.13562527591097506 ) ) ;
#3489 = ORIENTED_EDGE ( 'NONE', *, *, #1775, .T. ) ;
#3490 = FACE_OUTER_BOUND ( 'NONE', #41059, .T. ) ;
#3491 = ORIENTED_EDGE ( 'NONE', *, *, #4004, .F. ) ;
#3492 = ORIENTED_EDGE ( 'NONE', *, *, #83767, .F. ) ;
#3493 = AXIS2_PLACEMENT_3D ( 'NONE', #36604, #29780, #57471 ) ;
#3494 = DIRECTION ( 'NONE',  ( -0.000000000000000000, 0.000000000000000000, -1.000000000000000000 ) ) ;
#3495 = CARTESIAN_POINT ( 'NONE',  ( 70.63919639214310564, 100.5999999999999659, 56.85413200336923012 ) ) ;
#3496 = CARTESIAN_POINT ( 'NONE',  ( 101.1408812403245747, -27.39851324166288649, 65.51467289495799662 ) ) ;
#3497 = CARTESIAN_POINT ( 'NONE',  ( 86.06670390244796920, -48.82844715994099971, 310.9178068554150514 ) ) ;
#3498 = VECTOR ( 'NONE', #48714, 1000.000000000000114 ) ;
#3499 = EDGE_CURVE ( 'NONE', #67881, #66948, #40876, .T. ) ;
#3500 = DIRECTION ( 'NONE',  ( 4.299999999999999979E-14, -1.000000000000000000, 4.400000000000000367E-29 ) ) ;
#3501 = CARTESIAN_POINT ( 'NONE',  ( 24.79284581386629327, 127.0000000000000000, -3.384395586952189366E-14 ) ) ;
#3502 = CARTESIAN_POINT ( 'NONE',  ( 107.8187922529720026, -26.97765417004747945, 70.01562527591099183 ) ) ;
#3504 = CARTESIAN_POINT ( 'NONE',  ( 116.7748712849171255, -40.56502120445009751, 189.5270538473389479 ) ) ;
#3503 = FACE_OUTER_BOUND ( 'NONE', #64211, .T. ) ;
#3505 = DIRECTION ( 'NONE',  ( 0.000000000000000000, -1.000000000000000000, 0.000000000000000000 ) ) ;
#3506 = CARTESIAN_POINT ( 'NONE',  ( 27.27158787008325902, 184.0000000000000000, -5.920431057502157584E-15 ) ) ;
#3507 = ORIENTED_EDGE ( 'NONE', *, *, #4307, .T. ) ;
#3508 = FACE_OUTER_BOUND ( 'NONE', #6204, .T. ) ;
#3509 = DIRECTION ( 'NONE',  ( 0.000000000000000000, 0.000000000000000000, -1.000000000000000000 ) ) ;
#3510 = CARTESIAN_POINT ( 'NONE',  ( 97.60821144546386563, -39.98336359112931859, 136.5904942992093538 ) ) ;
#3511 = CARTESIAN_POINT ( 'NONE',  ( 177.0371591254545365, -48.62818131005479927, 193.9678068554150059 ) ) ;
#3513 = ORIENTED_EDGE ( 'NONE', *, *, #36390, .F. ) ;
#3512 = CARTESIAN_POINT ( 'NONE',  ( 116.8989603263487567, -40.32514756444775372, 218.5470538473399529 ) ) ;
#3514 = CARTESIAN_POINT ( 'NONE',  ( 97.80413494325495094, -40.49892049533512051, 146.6340343114085840 ) ) ;
#3515 = CARTESIAN_POINT ( 'NONE',  ( 111.6179861195847849, -46.13269558042843244, 243.9356252759109509 ) ) ;
#3516 = CARTESIAN_POINT ( 'NONE',  ( 104.9540660161283370, -25.01839229886434524, 121.2184824187679766 ) ) ;
#3517 = LINE ( 'NONE', #31217, #34566 ) ;
#3518 = CARTESIAN_POINT ( 'NONE',  ( 82.49755700851245876, -38.01506174167302987, 7.157201688890673985 ) ) ;
#3519 = CARTESIAN_POINT ( 'NONE',  ( 128.5492039024480277, -51.22944715994093912, 231.5838068554170093 ) ) ;
#3520 = DIRECTION ( 'NONE',  ( 1.000000000000000078E-15, -1.000000000000000083E-30, -1.000000000000000000 ) ) ;
#3521 = EDGE_LOOP ( 'NONE', ( #36204, #39976, #27229, #43307, #43469 ) ) ;
#3522 = VECTOR ( 'NONE', #75529, 999.9999999999998863 ) ;
#3523 = EDGE_CURVE ( 'NONE', #55364, #65449, #59232, .T. ) ;
#3524 = VECTOR ( 'NONE', #83759, 1000.000000000000000 ) ;
#3525 = AXIS2_PLACEMENT_3D ( 'NONE', #13100, #56185, #40783 ) ;
#3526 = AXIS2_PLACEMENT_3D ( 'NONE', #32532, #10753, #86632 ) ;
#3527 = VERTEX_POINT ( 'NONE', #39985 ) ;
#3528 = ORIENTED_EDGE ( 'NONE', *, *, #29932, .T. ) ;
#3529 = VECTOR ( 'NONE', #59244, 1000.000000000000114 ) ;
#3530 = CIRCLE ( 'NONE', #26738, 2.117000000000007987 ) ;
#3531 = ORIENTED_EDGE ( 'NONE', *, *, #47110, .T. ) ;
#3532 = DIRECTION ( 'NONE',  ( 0.000000000000000000, 1.000000000000000000, 0.000000000000000000 ) ) ;
#3533 = CARTESIAN_POINT ( 'NONE',  ( 97.21679027376985971, -33.31418093018012172, 282.0613395616252888 ) ) ;
#3534 = DIRECTION ( 'NONE',  ( 0.000000000000000000, 1.000000000000000000, 0.000000000000000000 ) ) ;
#3535 = CARTESIAN_POINT ( 'NONE',  ( 131.9692527705847169, -34.94806367531011659, 2.376725340804888731 ) ) ;
#3536 = ADVANCED_FACE ( 'NONE', ( #68604 ), #67700, .T. ) ;
#3537 = ADVANCED_FACE ( 'NONE', ( #26804 ), #33627, .T. ) ;
#3539 = DIRECTION ( 'NONE',  ( -1.000000000000000000, -1.541976423090496028E-15, 0.000000000000000000 ) ) ;
#3538 = DIRECTION ( 'NONE',  ( 1.000000000000000000, 4.163336342344333240E-14, 0.000000000000000000 ) ) ;
#3540 = CARTESIAN_POINT ( 'NONE',  ( 115.9692459539148643, -35.07008363779494431, 203.4076579233149573 ) ) ;
#3541 = ORIENTED_EDGE ( 'NONE', *, *, #83553, .T. ) ;
#3542 = ORIENTED_EDGE ( 'NONE', *, *, #71061, .T. ) ;
#3543 = ORIENTED_EDGE ( 'NONE', *, *, #20270, .F. ) ;
#3544 = LINE ( 'NONE', #10796, #16633 ) ;
#3546 = ADVANCED_FACE ( 'NONE', ( #87699 ), #13193, .T. ) ;
#3545 = CARTESIAN_POINT ( 'NONE',  ( 105.7152538737207834, -46.72382489312290943, 182.4690088981411407 ) ) ;
#3547 = DIRECTION ( 'NONE',  ( 1.000000000000000000, 0.000000000000000000, 0.000000000000000000 ) ) ;
#3548 = CARTESIAN_POINT ( 'NONE',  ( 116.4309197881342612, -37.49355097060504249, 35.20539282970796791 ) ) ;
#3549 = CARTESIAN_POINT ( 'NONE',  ( 118.2605848834651425, 92.12496802699139664, 8.385272115322319308 ) ) ;
#3550 = CARTESIAN_POINT ( 'NONE',  ( 193.0371591254585155, -47.82818131005411999, 180.4678068554150343 ) ) ;
#3551 = EDGE_CURVE ( 'NONE', #88193, #23818, #74962, .T. ) ;
#3552 = DIRECTION ( 'NONE',  ( 0.000000000000000000, 0.000000000000000000, -1.000000000000000000 ) ) ;
#3553 = ORIENTED_EDGE ( 'NONE', *, *, #14732, .F. ) ;
#3554 = CARTESIAN_POINT ( 'NONE',  ( 173.9900000000000091, 37.33800000000000097, 32.46912895322940074 ) ) ;
#3555 = ORIENTED_EDGE ( 'NONE', *, *, #9128, .T. ) ;
#3556 = CARTESIAN_POINT ( 'NONE',  ( 172.5667039024480687, -36.32844715993499563, 129.9678068554150059 ) ) ;
#3557 = CARTESIAN_POINT ( 'NONE',  ( 105.2414988608755522, -45.18937368885499950, 30.23761417911497063 ) ) ;
#3558 = CIRCLE ( 'NONE', #22446, 4.762500000000000178 ) ;
#3559 = CARTESIAN_POINT ( 'NONE',  ( 89.06648138392553449, -56.72944715994104570, -5.074374724089047106 ) ) ;
#3560 = AXIS2_PLACEMENT_3D ( 'NONE', #18472, #58464, #67077 ) ;
#3561 = CARTESIAN_POINT ( 'NONE',  ( 172.5664832912740110, -32.07844715994070839, 194.1756252759119832 ) ) ;
#3562 = FACE_OUTER_BOUND ( 'NONE', #19344, .T. ) ;
#3563 = ORIENTED_EDGE ( 'NONE', *, *, #4315, .F. ) ;
#3564 = CARTESIAN_POINT ( 'NONE',  ( 71.24189083761808661, -0.9290567490904538817, 540.9756252759101471 ) ) ;
#3565 = EDGE_CURVE ( 'NONE', #43245, #5020, #52687, .T. ) ;
#3566 = DIRECTION ( 'NONE',  ( 1.000000000000000000, 0.000000000000000000, 0.000000000000000000 ) ) ;
#3567 = ORIENTED_EDGE ( 'NONE', *, *, #18617, .T. ) ;
#3568 = CARTESIAN_POINT ( 'NONE',  ( 117.3389957193927131, -32.64844533837379004, 99.13943479972098771 ) ) ;
#3569 = ORIENTED_EDGE ( 'NONE', *, *, #67007, .T. ) ;
#3570 = EDGE_CURVE ( 'NONE', #32266, #69245, #75200, .T. ) ;
#3571 = CARTESIAN_POINT ( 'NONE',  ( 114.7034172354883168, -32.83980166744527196, 43.62384839950495063 ) ) ;
#3572 = EDGE_CURVE ( 'NONE', #54506, #83131, #72295, .T. ) ;
#3573 = CARTESIAN_POINT ( 'NONE',  ( 102.0492436467375654, -45.42708556363530192, 88.15966356583727759 ) ) ;
#3574 = CARTESIAN_POINT ( 'NONE',  ( 105.1055546886446308, -45.37138199117224957, 68.83015473446796761 ) ) ;
#3575 = LINE ( 'NONE', #17660, #7097 ) ;
#3576 = DIRECTION ( 'NONE',  ( 0.000000000000000000, -1.000000000000000000, 0.000000000000000000 ) ) ;
#3577 = EDGE_CURVE ( 'NONE', #66754, #16125, #18204, .T. ) ;
#3578 = CARTESIAN_POINT ( 'NONE',  ( 112.7812478461076040, -67.87844715994094713, 245.8358747327640117 ) ) ;
#3579 = CARTESIAN_POINT ( 'NONE',  ( 109.6483737747080198, -46.85224817473300618, 43.77562527591094721 ) ) ;
#3580 = CARTESIAN_POINT ( 'NONE',  ( 22.49541547940750164, -78.44951497180814215, 342.9256252759109884 ) ) ;
#3581 = VERTEX_POINT ( 'NONE', #53591 ) ;
#3582 = CARTESIAN_POINT ( 'NONE',  ( -3.174999999999644995, 124.5870000000000033, -33.98325472291465132 ) ) ;
#3583 = AXIS2_PLACEMENT_3D ( 'NONE', #26369, #33633, #89501 ) ;
#3584 = ORIENTED_EDGE ( 'NONE', *, *, #49359, .F. ) ;
#3585 = CARTESIAN_POINT ( 'NONE',  ( 48.79742451362098166, -36.32844715994040996, -5.074374724088000832 ) ) ;
#3586 = VECTOR ( 'NONE', #16838, 1000.000000000000000 ) ;
#3587 = AXIS2_PLACEMENT_3D ( 'NONE', #87118, #79875, #44874 ) ;
#3588 = AXIS2_PLACEMENT_3D ( 'NONE', #82069, #47499, #84753 ) ;
#3589 = EDGE_LOOP ( 'NONE', ( #36625, #20781, #42240, #17760 ) ) ;
#3590 = VERTEX_POINT ( 'NONE', #46335 ) ;
#3591 = CIRCLE ( 'NONE', #55758, 1.000000000000000888 ) ;
#3592 = DIRECTION ( 'NONE',  ( 0.000000000000000000, -1.000000000000000000, 0.000000000000000000 ) ) ;
#3593 = AXIS2_PLACEMENT_3D ( 'NONE', #24118, #38620, #37292 ) ;
#3594 = CARTESIAN_POINT ( 'NONE',  ( 115.3120223323506792, -44.18753462406608179, 233.2413395616259493 ) ) ;
#3595 = CARTESIAN_POINT ( 'NONE',  ( 101.0140741488528846, -28.73402828939939369, 125.5909382567238453 ) ) ;
#3596 = LINE ( 'NONE', #65219, #86816 ) ;
#3597 = CARTESIAN_POINT ( 'NONE',  ( 100.9432064590905469, -28.29215089373294489, 71.57562527591099411 ) ) ;
#3598 = CARTESIAN_POINT ( 'NONE',  ( 98.15075042664197724, -41.26116664859105043, 42.70068335180353358 ) ) ;
#3599 = ORIENTED_EDGE ( 'NONE', *, *, #13625, .F. ) ;
#3600 = CARTESIAN_POINT ( 'NONE',  ( 97.78478760265450376, -40.45112112471975507, 172.6299302010647239 ) ) ;
#3601 = CARTESIAN_POINT ( 'NONE',  ( 63.56670390244745050, -47.82844715994014706, 129.9678068554150911 ) ) ;
#3602 = ORIENTED_EDGE ( 'NONE', *, *, #89579, .F. ) ;
#3603 = FACE_OUTER_BOUND ( 'NONE', #9763, .T. ) ;
#3604 = LINE ( 'NONE', #11766, #22319 ) ;
#3605 = CARTESIAN_POINT ( 'NONE',  ( 107.5091008941355994, -47.12332782054438951, 237.6099109901969655 ) ) ;
#3606 = CARTESIAN_POINT ( 'NONE',  ( 164.9212702847350158, -29.73316016639540749, -5.074374724088000832 ) ) ;
#3607 = AXIS2_PLACEMENT_3D ( 'NONE', #78386, #70661, #1171 ) ;
#3608 = LINE ( 'NONE', #58999, #12955 ) ;
#3609 = CARTESIAN_POINT ( 'NONE',  ( 97.81413906161476746, -40.51632882248723888, 267.6361360915977343 ) ) ;
#3610 = CARTESIAN_POINT ( 'NONE',  ( 114.8173571680961231, -40.38677627709480333, 227.8981341137909453 ) ) ;
#3612 = CARTESIAN_POINT ( 'NONE',  ( 104.0490797691970073, -47.33883444496879633, 63.36800622829197494 ) ) ;
#3611 = DIRECTION ( 'NONE',  ( 0.7071067811866377228, -0.7071067811864573116, 0.000000000000000000 ) ) ;
#3613 = CARTESIAN_POINT ( 'NONE',  ( 117.1417030460440003, 73.45442465866868531, 57.64679522113551968 ) ) ;
#3614 = CARTESIAN_POINT ( 'NONE',  ( 114.0157635323931515, -28.07379075743241259, 119.5261014663869474 ) ) ;
#3615 = ORIENTED_EDGE ( 'NONE', *, *, #62505, .F. ) ;
#3616 = CARTESIAN_POINT ( 'NONE',  ( 133.3151861768397168, -21.40257939794838293, 8.160477455083581688 ) ) ;
#3617 = ORIENTED_EDGE ( 'NONE', *, *, #17476, .F. ) ;
#3618 = DIRECTION ( 'NONE',  ( -6.524622321627019585E-16, -3.741823817616790462E-31, -1.000000000000000000 ) ) ;
#3619 = DIRECTION ( 'NONE',  ( -0.9254794337955623007, -0.3787978585227819162, 0.000000000000000000 ) ) ;
#3620 = DIRECTION ( 'NONE',  ( 0.000000000000000000, 0.000000000000000000, -1.000000000000000000 ) ) ;
#3621 = ORIENTED_EDGE ( 'NONE', *, *, #78173, .F. ) ;
#3622 = CARTESIAN_POINT ( 'NONE',  ( 97.79834681188958712, -40.48468739506365210, 51.63281160315436580 ) ) ;
#3624 = ORIENTED_EDGE ( 'NONE', *, *, #67742, .T. ) ;
#3623 = CARTESIAN_POINT ( 'NONE',  ( 104.0952645214482430, -46.76829794407347407, 107.3470538473389411 ) ) ;
#3625 = LINE ( 'NONE', #25407, #53791 ) ;
#3626 = LINE ( 'NONE', #36818, #72255 ) ;
#3627 = AXIS2_PLACEMENT_3D ( 'NONE', #24939, #15904, #71322 ) ;
#3628 = DIRECTION ( 'NONE',  ( 1.000000000000000078E-15, -1.000000000000000000, 0.000000000000000000 ) ) ;
#3629 = VERTEX_POINT ( 'NONE', #81360 ) ;
#3630 = CARTESIAN_POINT ( 'NONE',  ( 116.9427733469681385, -33.21558069166144378, 114.0984824187679720 ) ) ;
#3631 = EDGE_CURVE ( 'NONE', #50606, #71390, #83912, .T. ) ;
#3632 = CIRCLE ( 'NONE', #54360, 2.517500000000000071 ) ;
#3633 = DIRECTION ( 'NONE',  ( 1.000000000000000000, 0.000000000000000000, 0.000000000000000000 ) ) ;
#3634 = FACE_BOUND ( 'NONE', #68129, .T. ) ;
#3635 = CARTESIAN_POINT ( 'NONE',  ( 32.09598329127609873, -23.42844715994129956, 193.9678068554150911 ) ) ;
#3636 = EDGE_CURVE ( 'NONE', #45956, #11616, #5573, .T. ) ;
#3637 = CARTESIAN_POINT ( 'NONE',  ( 116.3212776292272537, -32.94146857470742162, 144.1356252759109680 ) ) ;
#3638 = ORIENTED_EDGE ( 'NONE', *, *, #88566, .F. ) ;
#3639 = EDGE_CURVE ( 'NONE', #77842, #64816, #77212, .T. ) ;
#3640 = EDGE_LOOP ( 'NONE', ( #24121, #11356, #56768, #63460 ) ) ;
#3641 = DIRECTION ( 'NONE',  ( -1.000000000000000078E-15, 1.000000000000000000, 0.000000000000000000 ) ) ;
#3642 = DIRECTION ( 'NONE',  ( 1.000000000000000078E-15, 1.000000000000000083E-30, -1.000000000000000000 ) ) ;
#3643 = CARTESIAN_POINT ( 'NONE',  ( 177.1649999999999920, 5.112500000000000711, -7.937500000000000000 ) ) ;
#3644 = EDGE_CURVE ( 'NONE', #41573, #70760, #28139, .T. ) ;
#3645 = ADVANCED_FACE ( 'NONE', ( #55830 ), #67932, .T. ) ;
#3647 = CARTESIAN_POINT ( 'NONE',  ( 93.79772160076439036, -35.59147263058779487, 299.5704287327187103 ) ) ;
#3646 = FACE_OUTER_BOUND ( 'NONE', #46762, .T. ) ;
#3648 = DIRECTION ( 'NONE',  ( 9.912705577010326536E-16, 1.000000000000000000, 0.000000000000000000 ) ) ;
#3649 = EDGE_CURVE ( 'NONE', #24119, #5757, #31685, .T. ) ;
#3650 = EDGE_CURVE ( 'NONE', #623, #79790, #41762, .T. ) ;
#3651 = CIRCLE ( 'NONE', #41367, 10.26166025953212468 ) ;
#3652 = EDGE_LOOP ( 'NONE', ( #65461, #50322, #39157, #72622 ) ) ;
#3653 = AXIS2_PLACEMENT_3D ( 'NONE', #38063, #36731, #64432 ) ;
#3654 = VECTOR ( 'NONE', #59725, 1000.000000000000000 ) ;
#3655 = AXIS2_PLACEMENT_3D ( 'NONE', #13751, #6936, #28260 ) ;
#3657 = EDGE_CURVE ( 'NONE', #35758, #26375, #76305, .T. ) ;
#3656 = FACE_OUTER_BOUND ( 'NONE', #37612, .T. ) ;
#3658 = CARTESIAN_POINT ( 'NONE',  ( 99.36405074150921735, -30.70139697576588134, 151.7984824187679465 ) ) ;
#3660 = ORIENTED_EDGE ( 'NONE', *, *, #21086, .F. ) ;
#3659 = DIRECTION ( 'NONE',  ( 0.9999999853157766072, 0.0001713722456134502174, 0.000000000000000000 ) ) ;
#3661 = CARTESIAN_POINT ( 'NONE',  ( 98.38136461969652657, -29.78821554292439444, 41.78991099019696520 ) ) ;
#3662 = DIRECTION ( 'NONE',  ( 1.000000000000000078E-15, -1.000000000000000083E-30, -1.000000000000000000 ) ) ;
#3663 = CARTESIAN_POINT ( 'NONE',  ( 172.5664832912729878, -27.82844715994070484, 318.9256252759120116 ) ) ;
#3664 = EDGE_CURVE ( 'NONE', #76633, #10599, #23030, .T. ) ;
#3665 = VECTOR ( 'NONE', #23121, 1000.000000000000000 ) ;
#3666 = VERTEX_POINT ( 'NONE', #43106 ) ;
#3667 = CARTESIAN_POINT ( 'NONE',  ( 223.2659999999999911, 52.73749999999999716, -44.45000000000000284 ) ) ;
#3668 = ORIENTED_EDGE ( 'NONE', *, *, #67409, .F. ) ;
#3669 = ORIENTED_EDGE ( 'NONE', *, *, #1328, .T. ) ;
#3670 = VECTOR ( 'NONE', #89572, 1000.000000000000000 ) ;
#3671 = CARTESIAN_POINT ( 'NONE',  ( 112.1289716242999361, -44.03925847519028025, 199.4901547344690016 ) ) ;
#3672 = CYLINDRICAL_SURFACE ( 'NONE', #73405, 2.030000000001869864 ) ;
#3673 = CARTESIAN_POINT ( 'NONE',  ( -100.0213216842699779, 88.17609398443094904, 83.90854149456468747 ) ) ;
#3674 = AXIS2_PLACEMENT_3D ( 'NONE', #56916, #83748, #70562 ) ;
#3675 = CARTESIAN_POINT ( 'NONE',  ( 183.5150000000000148, 21.46300000000000097, 59.96543552338529537 ) ) ;
#3676 = CARTESIAN_POINT ( 'NONE',  ( 0.000000000000000000, 8.255000000000000782, 0.000000000000000000 ) ) ;
#3677 = EDGE_LOOP ( 'NONE', ( #25344, #41434 ) ) ;
#3678 = CARTESIAN_POINT ( 'NONE',  ( -74.15067561874160162, 120.6499999999999915, -68.53801554307528932 ) ) ;
#3679 = CARTESIAN_POINT ( 'NONE',  ( 116.3130905035090876, -32.93898513502411163, 35.13562527591096796 ) ) ;
#3680 = EDGE_LOOP ( 'NONE', ( #75447, #6355, #76872, #82445 ) ) ;
#3681 = CARTESIAN_POINT ( 'NONE',  ( 106.2286657330468103, -47.72771449247521502, 267.5280062282920994 ) ) ;
#3682 = CARTESIAN_POINT ( 'NONE',  ( 11.39249797916225759, 88.17791239546554038, 118.0075204203976114 ) ) ;
#3683 = EDGE_LOOP ( 'NONE', ( #37779, #86747, #48970, #84441 ) ) ;
#3684 = EDGE_CURVE ( 'NONE', #59373, #41311, #73765, .T. ) ;
#3685 = FILL_AREA_STYLE ('',( #37767 ) ) ;
#3686 = DIRECTION ( 'NONE',  ( -1.000000000000000000, 0.000000000000000000, 0.000000000000000000 ) ) ;
#3687 = CARTESIAN_POINT ( 'NONE',  ( 182.4202572930269923, -31.94127993907680718, -5.074374724088000832 ) ) ;
#3689 = EDGE_CURVE ( 'NONE', #31817, #11027, #21806, .T. ) ;
#3688 = CARTESIAN_POINT ( 'NONE',  ( 77.39114642429960611, 127.0000000000000000, -71.77848634863110533 ) ) ;
#3691 = CARTESIAN_POINT ( 'NONE',  ( 102.2170635254687454, -46.00716819922848799, 208.1927681330539599 ) ) ;
#3690 = STYLED_ITEM ( 'NONE', ( #30873 ), #80543 ) ;
#3692 = LINE ( 'NONE', #31384, #19527 ) ;
#3693 = ORIENTED_EDGE ( 'NONE', *, *, #61802, .F. ) ;
#3694 = CARTESIAN_POINT ( 'NONE',  ( 97.03360904796217312, -33.74039811955494628, 27.09562527591097236 ) ) ;
#3695 = CARTESIAN_POINT ( 'NONE',  ( 72.06648329127399677, -9.729447159941065237, -4.824374724089063982 ) ) ;
#3696 = VECTOR ( 'NONE', #13797, 1000.000000000000000 ) ;
#3697 = CARTESIAN_POINT ( 'NONE',  ( 116.5821416419259435, -42.35362450032752690, 283.4137205140060587 ) ) ;
#3698 = ORIENTED_EDGE ( 'NONE', *, *, #86343, .T. ) ;
#3699 = CARTESIAN_POINT ( 'NONE',  ( 81.12494507884962047, -16.19118199975293848, 1.799893109327372009 ) ) ;
#3700 = CARTESIAN_POINT ( 'NONE',  ( 98.04140782067196369, -41.04162603110138718, 17.68090933045322899 ) ) ;
#3701 = LINE ( 'NONE', #74532, #55266 ) ;
#3702 = CARTESIAN_POINT ( 'NONE',  ( 114.7692409103599687, -39.43078961860824450, 131.3766617981629565 ) ) ;
#3703 = CARTESIAN_POINT ( 'NONE',  ( 116.6256809191353909, -40.94358996305180654, 249.4956252759109532 ) ) ;
#3704 = DIRECTION ( 'NONE',  ( -0.000000000000000000, 1.000000000000000000, -0.000000000000000000 ) ) ;
#3705 = ORIENTED_EDGE ( 'NONE', *, *, #4708, .F. ) ;
#3706 = CARTESIAN_POINT ( 'NONE',  ( 135.5598545223519693, -39.04079274305309610, 1.981704437697082488 ) ) ;
#3707 = EDGE_LOOP ( 'NONE', ( #12509, #31854, #37787, #38344 ) ) ;
#3708 = EDGE_LOOP ( 'NONE', ( #86674, #58448, #5739, #63634 ) ) ;
#3709 = VECTOR ( 'NONE', #70823, 1000.000000000000114 ) ;
#3710 = VECTOR ( 'NONE', #80088, 1000.000000000000000 ) ;
#3711 = DIRECTION ( 'NONE',  ( 1.000000000000000000, 0.000000000000000000, 0.000000000000000000 ) ) ;
#3712 = AXIS2_PLACEMENT_3D ( 'NONE', #39625, #80999, #88702 ) ;
#3713 = ORIENTED_EDGE ( 'NONE', *, *, #21319, .F. ) ;
#3714 = ORIENTED_EDGE ( 'NONE', *, *, #48510, .F. ) ;
#3715 = DIRECTION ( 'NONE',  ( 0.000000000000000000, 1.000000000000000000, 0.000000000000000000 ) ) ;
#3716 = VECTOR ( 'NONE', #8640, 1000.000000000000000 ) ;
#3717 = CARTESIAN_POINT ( 'NONE',  ( 100.9535868929799989, -28.70787548350885388, 25.59406758372123392 ) ) ;
#3718 = CARTESIAN_POINT ( 'NONE',  ( 99.50386058399449496, -32.75919911893461034, 135.3638483995049739 ) ) ;
#3720 = CARTESIAN_POINT ( 'NONE',  ( 99.10996421577944204, -43.53389204880360097, 31.88991099019594699 ) ) ;
#3719 = VECTOR ( 'NONE', #61055, 1000.000000000000000 ) ;
#3721 = VERTEX_POINT ( 'NONE', #69497 ) ;
#3722 = DIRECTION ( 'NONE',  ( 0.000000000000000000, 0.000000000000000000, -1.000000000000000000 ) ) ;
#3723 = ORIENTED_EDGE ( 'NONE', *, *, #17531, .F. ) ;
#3724 = AXIS2_PLACEMENT_3D ( 'NONE', #82886, #32914, #40629 ) ;
#3725 = FACE_OUTER_BOUND ( 'NONE', #16206, .T. ) ;
#3726 = ORIENTED_EDGE ( 'NONE', *, *, #57993, .F. ) ;
#3727 = DIRECTION ( 'NONE',  ( 0.000000000000000000, 0.000000000000000000, 1.000000000000000000 ) ) ;
#3728 = DIRECTION ( 'NONE',  ( -0.04216478779797398074, 0.9991106698809455455, 0.000000000000000000 ) ) ;
#3729 = DIRECTION ( 'NONE',  ( 1.000000000000000078E-15, -1.000000000000000083E-30, -1.000000000000000000 ) ) ;
#3730 = AXIS2_PLACEMENT_3D ( 'NONE', #30373, #9044, #2222 ) ;
#3731 = EDGE_CURVE ( 'NONE', #26105, #85262, #8497, .T. ) ;
#3732 = DIRECTION ( 'NONE',  ( 0.000000000000000000, 0.000000000000000000, -1.000000000000000000 ) ) ;
#3733 = VERTEX_POINT ( 'NONE', #69944 ) ;
#3734 = CARTESIAN_POINT ( 'NONE',  ( 100.1774089044720881, -45.37350532423673144, 272.0289586092443415 ) ) ;
#3735 = CARTESIAN_POINT ( 'NONE',  ( 111.1459338097010914, -47.05202348217205355, 18.88800622829195319 ) ) ;
#3736 =( LENGTH_UNIT ( ) NAMED_UNIT ( * ) SI_UNIT ( .MILLI., .METRE. ) );
#3737 = VECTOR ( 'NONE', #84099, 1000.000000000000000 ) ;
#3738 = EDGE_CURVE ( 'NONE', #68582, #12535, #85414, .T. ) ;
#3740 = DIRECTION ( 'NONE',  ( 2.900000000000000265E-14, -2.000000000000000155E-15, 1.000000000000000000 ) ) ;
#3739 = CARTESIAN_POINT ( 'NONE',  ( 47.62500000000000000, 111.1250000000000000, 257.1750000000000114 ) ) ;
#3741 = CARTESIAN_POINT ( 'NONE',  ( 107.0664832912730020, -36.72944715994189835, 361.9756252759109998 ) ) ;
#3742 = EDGE_CURVE ( 'NONE', #75550, #1586, #63574, .T. ) ;
#3743 = CARTESIAN_POINT ( 'NONE',  ( -50.03799999999999670, 101.5999999999999943, 206.3750000000000000 ) ) ;
#3744 = CARTESIAN_POINT ( 'NONE',  ( 83.06670390244796920, -64.87844715994098976, 231.5838068554150198 ) ) ;
#3745 = EDGE_CURVE ( 'NONE', #37737, #2431, #35401, .T. ) ;
#3746 = PLANE ( 'NONE',  #6882 ) ;
#3747 = PLANE ( 'NONE',  #31791 ) ;
#3748 = DIRECTION ( 'NONE',  ( 0.000000000000000000, 0.000000000000000000, -1.000000000000000000 ) ) ;
#3749 = EDGE_CURVE ( 'NONE', #86967, #73636, #69045, .T. ) ;
#3750 = CARTESIAN_POINT ( 'NONE',  ( 111.1461885285858671, -47.05266801877174032, 22.88800622829195675 ) ) ;
#3751 = CARTESIAN_POINT ( 'NONE',  ( 110.1374552785425323, -26.11139123911904036, 210.8403871806729626 ) ) ;
#3752 = CARTESIAN_POINT ( 'NONE',  ( 96.89995799317335923, -32.33320227283598314, 57.01372051400599616 ) ) ;
#3754 = FACE_OUTER_BOUND ( 'NONE', #40941, .T. ) ;
#3753 = CARTESIAN_POINT ( 'NONE',  ( 137.0667039024479834, -50.82844715994100682, 10.91780685541479734 ) ) ;
#3755 = DIRECTION ( 'NONE',  ( 1.000000000000000078E-15, -1.000000000000000083E-30, -1.000000000000000000 ) ) ;
#3756 = EDGE_CURVE ( 'NONE', #84589, #44354, #49476, .T. ) ;
#3757 = VECTOR ( 'NONE', #82035, 1000.000000000000000 ) ;
#3758 = ORIENTED_EDGE ( 'NONE', *, *, #77992, .T. ) ;
#3759 = CARTESIAN_POINT ( 'NONE',  ( 97.06107108242123616, -37.99641184083684919, 187.4272919328122953 ) ) ;
#3760 = ORIENTED_EDGE ( 'NONE', *, *, #23279, .T. ) ;
#3761 = ADVANCED_FACE ( 'NONE', ( #54931 ), #8166, .T. ) ;
#3762 = CARTESIAN_POINT ( 'NONE',  ( 97.55373691267115532, -39.00345059616618215, 52.51276813305294411 ) ) ;
#3764 = EDGE_LOOP ( 'NONE', ( #73099, #42268, #13323, #10176 ) ) ;
#3763 = CARTESIAN_POINT ( 'NONE',  ( 4.048368076483533251, 94.58941606601858609, 130.4932642680670654 ) ) ;
#3765 = DIRECTION ( 'NONE',  ( -1.000000000000000000, 0.000000000000000000, 0.000000000000000000 ) ) ;
#3766 = CARTESIAN_POINT ( 'NONE',  ( 103.8265608274144398, -48.10271009292816302, 213.3556252759109668 ) ) ;
#3767 = CARTESIAN_POINT ( 'NONE',  ( 163.0667039024478697, -33.35206098992140511, 193.9678068554149775 ) ) ;
#3768 = LINE ( 'NONE', #2440, #5172 ) ;
#3769 = DIRECTION ( 'NONE',  ( 1.000000000000000000, 4.163336342344333240E-14, 0.000000000000000000 ) ) ;
#3770 = CARTESIAN_POINT ( 'NONE',  ( 95.60734603896362671, -36.72944715994100306, 312.6356252759112522 ) ) ;
#3771 = ADVANCED_FACE ( 'NONE', ( #84492 ), #77658, .T. ) ;
#3772 = CARTESIAN_POINT ( 'NONE',  ( 131.6146038194004007, -37.97617057399416751, 2.716753174567031692 ) ) ;
#3773 = DIRECTION ( 'NONE',  ( 0.000000000000000000, -0.5000000000000007772, 0.8660254037844381525 ) ) ;
#3774 = CARTESIAN_POINT ( 'NONE',  ( 96.37928053093608582, -33.66421044892479131, 141.1041967044829732 ) ) ;
#3775 = ORIENTED_EDGE ( 'NONE', *, *, #28084, .F. ) ;
#3776 = ORIENTED_EDGE ( 'NONE', *, *, #52717, .T. ) ;
#3777 = VECTOR ( 'NONE', #65567, 1000.000000000000000 ) ;
#3778 = CARTESIAN_POINT ( 'NONE',  ( 102.5524010923236915, -28.48932656383806972, 96.89491663923000431 ) ) ;
#3779 = AXIS2_PLACEMENT_3D ( 'NONE', #86414, #78718, #10103 ) ;
#3780 = LINE ( 'NONE', #66438, #13834 ) ;
#3781 = AXIS2_PLACEMENT_3D ( 'NONE', #47669, #88590, #75403 ) ;
#3783 = CARTESIAN_POINT ( 'NONE',  ( 41.56648329127399677, -9.303447159940999356, 78.92562527591199739 ) ) ;
#3782 = CARTESIAN_POINT ( 'NONE',  ( 116.5994914424365021, -40.81117973626238893, 209.5165776568629497 ) ) ;
#3784 = VECTOR ( 'NONE', #77088, 1000.000000000000000 ) ;
#3785 = DIRECTION ( 'NONE',  ( 0.000000000000000000, 1.000000000000000000, 0.000000000000000000 ) ) ;
#3786 = CARTESIAN_POINT ( 'NONE',  ( 98.58946256649487339, -99.96145986183429955, -19.78219314458215550 ) ) ;
#3787 = CARTESIAN_POINT ( 'NONE',  ( 117.9189190431816172, 79.26437155269050550, -12.27470785613960835 ) ) ;
#3788 = CARTESIAN_POINT ( 'NONE',  ( -12.29201543513789652, 79.25066774386124280, 117.9171666014395043 ) ) ;
#3789 = CARTESIAN_POINT ( 'NONE',  ( 1.387778780781445676E-14, 239.0000000000000000, 90.27542076772557778 ) ) ;
#3790 = DIRECTION ( 'NONE',  ( 0.000000000000000000, 1.000000000000000000, 0.000000000000000000 ) ) ;
#3791 = CARTESIAN_POINT ( 'NONE',  ( 103.4759237351580623, -46.49349013887667326, 142.2956252759109645 ) ) ;
#3792 = ORIENTED_EDGE ( 'NONE', *, *, #60951, .F. ) ;
#3793 = ORIENTED_EDGE ( 'NONE', *, *, #73379, .T. ) ;
#3794 = CARTESIAN_POINT ( 'NONE',  ( 130.8259623650636172, -69.00418878328892447, 247.5000682988239760 ) ) ;
#3795 = DIRECTION ( 'NONE',  ( 0.000000000000000000, 0.000000000000000000, 1.000000000000000000 ) ) ;
#3796 = FACE_BOUND ( 'NONE', #78200, .T. ) ;
#3798 = EDGE_CURVE ( 'NONE', #74769, #67371, #6811, .T. ) ;
#3797 = LINE ( 'NONE', #31484, #16345 ) ;
#3799 = CIRCLE ( 'NONE', #87897, 5.000000000000004441 ) ;
#3800 = DIRECTION ( 'NONE',  ( 3.100000000000000258E-29, -3.100000000000000044E-14, -1.000000000000000000 ) ) ;
#3801 =( BOUNDED_CURVE ( )  B_SPLINE_CURVE ( 3, ( #64744, #24307, #51973, #79731 ),
 .UNSPECIFIED., .F., .T. ) 
 B_SPLINE_CURVE_WITH_KNOTS ( ( 4, 4 ),
 ( 1.570796326793645337, 3.141592653589136308 ),
 .UNSPECIFIED. ) 
 CURVE ( )  GEOMETRIC_REPRESENTATION_ITEM ( )  RATIONAL_B_SPLINE_CURVE ( ( 1.000000000000000000, 0.8047378541242249383, 0.8047378541242249383, 1.000000000000000000 ) ) 
 REPRESENTATION_ITEM ( '' )  );
#3802 = CIRCLE ( 'NONE', #21247, 1.000000000000000888 ) ;
#3803 = CARTESIAN_POINT ( 'NONE',  ( 102.6834449319766378, -27.27027144519976787, 180.4213395616249898 ) ) ;
#3804 = FACE_OUTER_BOUND ( 'NONE', #54938, .T. ) ;
#3805 = ORIENTED_EDGE ( 'NONE', *, *, #17430, .T. ) ;
#3807 = ORIENTED_EDGE ( 'NONE', *, *, #50702, .T. ) ;
#3806 = ORIENTED_EDGE ( 'NONE', *, *, #71834, .F. ) ;
#3808 = CARTESIAN_POINT ( 'NONE',  ( 111.1351804138767108, -45.89630524753858509, 63.90945011243512397 ) ) ;
#3809 = DIRECTION ( 'NONE',  ( 0.000000000000000000, 0.000000000000000000, -1.000000000000000000 ) ) ;
#3810 = CARTESIAN_POINT ( 'NONE',  ( 131.3165190107491185, -36.55810522840583587, 6.749822759741316069 ) ) ;
#3811 = CARTESIAN_POINT ( 'NONE',  ( 105.3283384058428851, -27.49606390364131414, 276.6682499725636717 ) ) ;
#3812 = CARTESIAN_POINT ( 'NONE',  ( -446.0240000000000009, 53.97500000000000142, 101.5999999999999943 ) ) ;
#3813 = EDGE_LOOP ( 'NONE', ( #88115, #39666, #14670, #13222 ) ) ;
#3814 = EDGE_CURVE ( 'NONE', #87871, #80786, #55383, .T. ) ;
#3815 = CARTESIAN_POINT ( 'NONE',  ( -74.15067561874160162, 120.6499999999999915, -68.53801554307528932 ) ) ;
#3816 = DIRECTION ( 'NONE',  ( -0.02150753337723812844, -0.0009076677972192511400, -0.9997682742251809973 ) ) ;
#3817 = ORIENTED_EDGE ( 'NONE', *, *, #71946, .T. ) ;
#3818 = ORIENTED_EDGE ( 'NONE', *, *, #35470, .T. ) ;
#3819 = ADVANCED_FACE ( 'NONE', ( #17221, #78119 ), #17661, .F. ) ;
#3820 = DIRECTION ( 'NONE',  ( 0.000000000000000000, -1.000000000000000000, 0.000000000000000000 ) ) ;
#3821 = ORIENTED_EDGE ( 'NONE', *, *, #37455, .T. ) ;
#3822 = ORIENTED_EDGE ( 'NONE', *, *, #13507, .F. ) ;
#3823 = CARTESIAN_POINT ( 'NONE',  ( 104.4882991616644290, -26.97926274729164575, 156.2813675130791751 ) ) ;
#3824 = CARTESIAN_POINT ( 'NONE',  ( 114.2970346969270565, -32.18244176163005221, 33.69527697093299423 ) ) ;
#3825 = CARTESIAN_POINT ( 'NONE',  ( 98.36125384756333290, -29.88003685912757490, 200.8080062282919869 ) ) ;
#3826 = CARTESIAN_POINT ( 'NONE',  ( 115.0229693000241156, -29.09019634776596419, 189.4232443235299570 ) ) ;
#3827 = CARTESIAN_POINT ( 'NONE',  ( 63.06670390244707392, -40.32844715994016838, 180.4678068554151196 ) ) ;
#3828 = CARTESIAN_POINT ( 'NONE',  ( 96.77613930368880801, -40.76464245898888095, 242.6118157521009664 ) ) ;
#3829 = CARTESIAN_POINT ( 'NONE',  ( 107.0667039024470313, -104.2784471599408676, 19.21780685541799016 ) ) ;
#3830 = DIRECTION ( 'NONE',  ( 0.000000000000000000, 1.000000000000000000, 0.000000000000000000 ) ) ;
#3831 = VERTEX_POINT ( 'NONE', #85830 ) ;
#3832 = ORIENTED_EDGE ( 'NONE', *, *, #72216, .F. ) ;
#3833 = VECTOR ( 'NONE', #60083, 1000.000000000000000 ) ;
#3834 = AXIS2_PLACEMENT_3D ( 'NONE', #63675, #55033, #13732 ) ;
#3835 = CARTESIAN_POINT ( 'NONE',  ( 107.0664832912739399, -36.72944715994096754, 296.0306255462182321 ) ) ;
#3836 = CARTESIAN_POINT ( 'NONE',  ( 99.72210660708088881, -29.26842865273154004, 225.6956252759109702 ) ) ;
#3837 = VERTEX_POINT ( 'NONE', #24482 ) ;
#3838 = VECTOR ( 'NONE', #48336, 1000.000000000000000 ) ;
#3839 = CARTESIAN_POINT ( 'NONE',  ( 117.7793243111075157, -34.00655811778471360, 169.0365776568629599 ) ) ;
#3840 = PLANE ( 'NONE',  #10867 ) ;
#3841 = CARTESIAN_POINT ( 'NONE',  ( -8.813809904571851206, 69.38616896394334788, 37.07268381226281662 ) ) ;
#3842 = AXIS2_PLACEMENT_3D ( 'NONE', #36859, #57745, #72282 ) ;
#3843 = CARTESIAN_POINT ( 'NONE',  ( 107.0667039024470313, -104.2784471599414502, 0.2178068554180012661 ) ) ;
#3844 = CARTESIAN_POINT ( 'NONE',  ( 143.2522959336310748, -139.0102598546870922, 247.5112310255240118 ) ) ;
#3845 = EDGE_CURVE ( 'NONE', #87253, #75711, #50372, .T. ) ;
#3848 = CARTESIAN_POINT ( 'NONE',  ( 95.25611604350974915, -37.33230102880721546, 267.3670538473395482 ) ) ;
#3847 = DIRECTION ( 'NONE',  ( -0.000000000000000000, -0.000000000000000000, 1.000000000000000000 ) ) ;
#3846 = DIRECTION ( 'NONE',  ( 0.000000000000000000, 0.000000000000000000, -1.000000000000000000 ) ) ;
#3849 = LINE ( 'NONE', #9776, #78567 ) ;
#3850 = EDGE_CURVE ( 'NONE', #44698, #89450, #63272, .T. ) ;
#3851 = CARTESIAN_POINT ( 'NONE',  ( 0.000000000000000000, 17.78000000000000114, 0.000000000000000000 ) ) ;
#3852 = CARTESIAN_POINT ( 'NONE',  ( 99.09464024186620179, -30.55185734355772098, 271.8020006611150734 ) ) ;
#3853 = ADVANCED_FACE ( 'NONE', ( #45336 ), #44451, .T. ) ;
#3854 = CARTESIAN_POINT ( 'NONE',  ( 67.10629922391730418, -137.6313948336576232, 245.9678581484365907 ) ) ;
#3855 = DIRECTION ( 'NONE',  ( 1.000000000000000000, 4.510281037539819615E-14, 0.000000000000000000 ) ) ;
#3856 = CARTESIAN_POINT ( 'NONE',  ( 97.07207206141239908, -35.37844118198271559, 77.21895860788390564 ) ) ;
#3858 = ORIENTED_EDGE ( 'NONE', *, *, #2106, .T. ) ;
#3857 = CARTESIAN_POINT ( 'NONE',  ( 98.71706140474314850, -34.42688893107280990, 195.5838068554172366 ) ) ;
#3859 = EDGE_CURVE ( 'NONE', #24397, #60648, #74883, .T. ) ;
#3860 = CYLINDRICAL_SURFACE ( 'NONE', #81467, 3.300000000000000711 ) ;
#3861 = CARTESIAN_POINT ( 'NONE',  ( 95.88624405714097065, -32.72491640434669335, 176.0527681330539735 ) ) ;
#3862 = CARTESIAN_POINT ( 'NONE',  ( 107.9456208643995012, -25.71123053419755422, 111.0251490854349754 ) ) ;
#3863 = CARTESIAN_POINT ( 'NONE',  ( 98.80492496406409941, -29.31701487593723598, 231.7565776568629587 ) ) ;
#3864 = CARTESIAN_POINT ( 'NONE',  ( 163.2449138993005988, -32.11662333284040471, 313.9678068554149490 ) ) ;
#3865 = DIRECTION ( 'NONE',  ( 1.907762142705490052E-15, 7.167082501179359715E-16, -1.000000000000000000 ) ) ;
#3866 = CIRCLE ( 'NONE', #73486, 2.116999999999993776 ) ;
#3868 = CARTESIAN_POINT ( 'NONE',  ( 116.9761379366299536, -35.34627962053155414, 39.93653275092082566 ) ) ;
#3867 = CARTESIAN_POINT ( 'NONE',  ( 173.9899999999999807, 52.73749999999999716, -52.28750000000000142 ) ) ;
#3869 = DIRECTION ( 'NONE',  ( 0.000000000000000000, 0.000000000000000000, 1.000000000000000000 ) ) ;
#3870 = DIRECTION ( 'NONE',  ( 1.000000000000000078E-15, -1.000000000000000083E-30, -1.000000000000000000 ) ) ;
#3871 = CARTESIAN_POINT ( 'NONE',  ( 107.0664832912739968, -36.72944715994100306, 287.6356252759109680 ) ) ;
#3872 = VERTEX_POINT ( 'NONE', #85386 ) ;
#3873 = EDGE_LOOP ( 'NONE', ( #7907, #32328, #73171, #70582 ) ) ;
#3874 = EDGE_CURVE ( 'NONE', #75709, #88176, #47359, .T. ) ;
#3875 = CARTESIAN_POINT ( 'NONE',  ( 99.91372553312717741, -41.39787175238471661, 101.2095626852199644 ) ) ;
#3877 = ORIENTED_EDGE ( 'NONE', *, *, #33688, .F. ) ;
#3876 = CARTESIAN_POINT ( 'NONE',  ( -3.174999999999664979, 111.1250000000000000, -31.75000000000000000 ) ) ;
#3878 = CARTESIAN_POINT ( 'NONE',  ( 117.0854383170105564, -39.53109055650221393, 94.60991099019693706 ) ) ;
#3879 = DIRECTION ( 'NONE',  ( 3.100000000000000258E-29, -3.100000000000000044E-14, -1.000000000000000000 ) ) ;
#3880 = CARTESIAN_POINT ( 'NONE',  ( 78.15700282949597977, -16.74831852143626776, 7.618261863063606754 ) ) ;
#3881 = DIRECTION ( 'NONE',  ( 1.639958061481212836E-42, -4.100000000000000342E-29, -1.000000000000000000 ) ) ;
#3882 = CARTESIAN_POINT ( 'NONE',  ( 97.35451824726682446, -37.88753622196094994, 41.42133956162496844 ) ) ;
#3883 = ORIENTED_EDGE ( 'NONE', *, *, #74025, .T. ) ;
#3884 = EDGE_LOOP ( 'NONE', ( #55485, #43005, #50208, #1541 ) ) ;
#3885 = ORIENTED_EDGE ( 'NONE', *, *, #60743, .T. ) ;
#3886 = DIRECTION ( 'NONE',  ( 0.000000000000000000, -1.000000000000000000, 0.000000000000000000 ) ) ;
#3888 = CARTESIAN_POINT ( 'NONE',  ( 73.06648329127402519, -46.72944715994106701, -4.824374724089063982 ) ) ;
#3887 = CARTESIAN_POINT ( 'NONE',  ( 96.70615320395842218, -37.17927570127480408, 112.3489586092439652 ) ) ;
#3889 = CARTESIAN_POINT ( 'NONE',  ( 97.33784131355466229, -34.07106452111344908, 117.1147919418627197 ) ) ;
#3890 = CYLINDRICAL_SURFACE ( 'NONE', #71207, 3.299999999999997158 ) ;
#3891 = CARTESIAN_POINT ( 'NONE',  ( 97.81452210549078075, -40.51628237377364883, 52.63520911028864901 ) ) ;
#3892 = FACE_OUTER_BOUND ( 'NONE', #68733, .T. ) ;
#3893 = CARTESIAN_POINT ( 'NONE',  ( -10.40475206047886836, 89.83749360592842947, 130.1408237963791805 ) ) ;
#3894 = CARTESIAN_POINT ( 'NONE',  ( 0.000000000000000000, 117.4749999999999943, -110.3312500000000114 ) ) ;
#3895 = CARTESIAN_POINT ( 'NONE',  ( 97.30890135812528285, -33.12136451854834007, 66.04419670448297097 ) ) ;
#3896 = VERTEX_POINT ( 'NONE', #30396 ) ;
#3897 = VERTEX_POINT ( 'NONE', #78572 ) ;
#3898 = CARTESIAN_POINT ( 'NONE',  ( 3.291704278000434414, 94.82304653311919651, 130.5151038487541939 ) ) ;
#3899 = DIRECTION ( 'NONE',  ( 1.639958061481212836E-42, -4.100000000000000342E-29, -1.000000000000000000 ) ) ;
#3900 = CONICAL_SURFACE ( 'NONE', #54630, 1.624999999999987566, 1.029744258676650093 ) ;
#3902 = EDGE_CURVE ( 'NONE', #43122, #1162, #15882, .T. ) ;
#3901 = CARTESIAN_POINT ( 'NONE',  ( 82.02983075842482208, -92.77767617834393832, 250.2178068554179902 ) ) ;
#3903 = CARTESIAN_POINT ( 'NONE',  ( 101.0810522191901981, -29.63898995574150419, 148.4538046553059587 ) ) ;
#3904 = VECTOR ( 'NONE', #25181, 1000.000000000000000 ) ;
#3905 = CIRCLE ( 'NONE', #50324, 173.3227045127110273 ) ;
#3906 = AXIS2_PLACEMENT_3D ( 'NONE', #3463, #72069, #79341 ) ;
#3907 = EDGE_CURVE ( 'NONE', #66196, #3366, #89475, .T. ) ;
#3908 = CARTESIAN_POINT ( 'NONE',  ( 33.96670390244699433, -28.27351298637401200, -5.074374724088000832 ) ) ;
#3909 = ORIENTED_EDGE ( 'NONE', *, *, #10072, .T. ) ;
#3910 = ORIENTED_EDGE ( 'NONE', *, *, #54882, .T. ) ;
#3911 = DIRECTION ( 'NONE',  ( 0.000000000000000000, 0.000000000000000000, 1.000000000000000000 ) ) ;
#3912 = ORIENTED_EDGE ( 'NONE', *, *, #71345, .F. ) ;
#3913 = EDGE_LOOP ( 'NONE', ( #31915, #88377, #7942 ) ) ;
#3914 = CARTESIAN_POINT ( 'NONE',  ( 141.0667039024479834, -58.72944715994110254, 250.9178068554160461 ) ) ;
#3915 = CARTESIAN_POINT ( 'NONE',  ( 112.6322303140947838, -44.29905650357037672, 179.5006309249449430 ) ) ;
#3916 = FACE_BOUND ( 'NONE', #1115, .T. ) ;
#3917 = AXIS2_PLACEMENT_3D ( 'NONE', #27024, #56950, #14751 ) ;
#3918 = AXIS2_PLACEMENT_3D ( 'NONE', #54513, #5968, #40012 ) ;
#3919 = FACE_BOUND ( 'NONE', #68705, .T. ) ;
#3920 = PLANE ( 'NONE',  #88005 ) ;
#3921 = VERTEX_POINT ( 'NONE', #72181 ) ;
#3922 = AXIS2_PLACEMENT_3D ( 'NONE', #47491, #67058, #74771 ) ;
#3923 = ADVANCED_FACE ( 'NONE', ( #86704 ), #10832, .F. ) ;
#3924 = ORIENTED_EDGE ( 'NONE', *, *, #7846, .T. ) ;
#3925 = ORIENTED_EDGE ( 'NONE', *, *, #49577, .T. ) ;
#3926 = CARTESIAN_POINT ( 'NONE',  ( 98.43814749271325582, -36.05658283995993685, 189.0947570362579597 ) ) ;
#3927 = CARTESIAN_POINT ( 'NONE',  ( 101.4890226443523744, -27.89551843606815495, 110.5241967044819944 ) ) ;
#3928 = CARTESIAN_POINT ( 'NONE',  ( 114.8031991714177451, -43.68443766454706889, 38.24419670448192221 ) ) ;
#3929 = CARTESIAN_POINT ( 'NONE',  ( 117.0602230546818703, -38.08518235923209971, 253.7190022475310229 ) ) ;
#3930 = CARTESIAN_POINT ( 'NONE',  ( 110.2536356736639078, -101.8611209747513868, -19.78219314458209865 ) ) ;
#3931 = CARTESIAN_POINT ( 'NONE',  ( 163.0664832912739826, 19.62155284005901024, 327.8006252759110453 ) ) ;
#3932 = CARTESIAN_POINT ( 'NONE',  ( 102.9671325615611437, -26.46449201736525225, 171.3908633711489813 ) ) ;
#3933 = CARTESIAN_POINT ( 'NONE',  ( 107.0664832912739968, -36.72944715994100306, 287.6356252759109680 ) ) ;
#3934 = ORIENTED_EDGE ( 'NONE', *, *, #14312, .F. ) ;
#3935 = CARTESIAN_POINT ( 'NONE',  ( 1.796236281188243881E-22, 69.84999999999999432, 118.5560000000000116 ) ) ;
#3936 = VERTEX_POINT ( 'NONE', #2700 ) ;
#3937 = ORIENTED_EDGE ( 'NONE', *, *, #41802, .T. ) ;
#3938 = CARTESIAN_POINT ( 'NONE',  ( 97.81461822720238786, -40.51595288653417981, 132.6359866545674890 ) ) ;
#3939 = ORIENTED_EDGE ( 'NONE', *, *, #36113, .T. ) ;
#3940 = ORIENTED_EDGE ( 'NONE', *, *, #6641, .T. ) ;
#3941 = AXIS2_PLACEMENT_3D ( 'NONE', #44606, #87647, #23751 ) ;
#3942 = CARTESIAN_POINT ( 'NONE',  ( -446.0240000000000009, 3.174999999999999822, -1.387778780781445991E-14 ) ) ;
#3943 = ORIENTED_EDGE ( 'NONE', *, *, #75724, .F. ) ;
#3944 = CARTESIAN_POINT ( 'NONE',  ( 116.3212776292296127, -32.94146857471318413, 287.6356252759109680 ) ) ;
#3945 = CARTESIAN_POINT ( 'NONE',  ( 113.4596546395850680, -46.70781606211470205, 68.02991099019695298 ) ) ;
#3946 = CARTESIAN_POINT ( 'NONE',  ( 51.23005224011622261, -33.89581943344351345, 193.9678068554150911 ) ) ;
#3947 = CARTESIAN_POINT ( 'NONE',  ( 46.83715912545429916, -47.82818131006083462, 237.4678068554150059 ) ) ;
#3948 = LINE ( 'NONE', #31649, #78956 ) ;
#3949 = CARTESIAN_POINT ( 'NONE',  ( 109.9668656698224822, -46.07028316908886723, 97.81562527591097478 ) ) ;
#3951 = CARTESIAN_POINT ( 'NONE',  ( 117.4355769707882473, -40.49052663852277334, 169.5375300378159693 ) ) ;
#3950 = CARTESIAN_POINT ( 'NONE',  ( 72.17003668186727339, -45.68655394112764156, 14.92562527591097776 ) ) ;
#3952 = CARTESIAN_POINT ( 'NONE',  ( 97.06670390244703128, -109.9573555057411340, 17.71780685541815714 ) ) ;
#3953 = EDGE_CURVE ( 'NONE', #84928, #42564, #84934, .T. ) ;
#3954 = LINE ( 'NONE', #37593, #32226 ) ;
#3955 = ORIENTED_EDGE ( 'NONE', *, *, #34121, .F. ) ;
#3956 = FACE_OUTER_BOUND ( 'NONE', #75464, .T. ) ;
#3957 = EDGE_CURVE ( 'NONE', #17048, #13307, #32851, .T. ) ;
#3958 = CARTESIAN_POINT ( 'NONE',  ( 31.71315051185421297, -33.70561438052095582, 193.9678068554150911 ) ) ;
#3959 = EDGE_CURVE ( 'NONE', #53860, #137, #64472, .T. ) ;
#3960 = CARTESIAN_POINT ( 'NONE',  ( 103.8797721312301547, -106.6957733451327215, -19.78219314458193168 ) ) ;
#3961 = FACE_OUTER_BOUND ( 'NONE', #27959, .T. ) ;
#3963 = ORIENTED_EDGE ( 'NONE', *, *, #73004, .T. ) ;
#3962 = CARTESIAN_POINT ( 'NONE',  ( 96.14524839136181811, -32.00129468986670389, 211.0013395616249738 ) ) ;
#3964 = EDGE_CURVE ( 'NONE', #57201, #18286, #79002, .T. ) ;
#3965 = CARTESIAN_POINT ( 'NONE',  ( 107.0667039024470313, -104.2784471599413934, 2.217806855418003043 ) ) ;
#3966 = CARTESIAN_POINT ( 'NONE',  ( 116.2377588530493995, -41.80555791324388082, 259.4241967044827106 ) ) ;
#3967 = CARTESIAN_POINT ( 'NONE',  ( 117.2518684062627727, -39.29770432102194633, 119.6299109901969615 ) ) ;
#3968 = VECTOR ( 'NONE', #26272, 1000.000000000000000 ) ;
#3969 = CARTESIAN_POINT ( 'NONE',  ( 193.0371591254572365, -23.42818131005412496, 300.4678068554149490 ) ) ;
#3970 = CARTESIAN_POINT ( 'NONE',  ( 82.10313645209993183, -38.57950990140825098, 7.523361336351456430 ) ) ;
#3971 = CARTESIAN_POINT ( 'NONE',  ( 172.5664832912740110, -9.303447159940999356, 18.92562527591200094 ) ) ;
#3972 = CARTESIAN_POINT ( 'NONE',  ( 164.7812970173289955, -35.65087443492610930, 193.9678068554150059 ) ) ;
#3973 = VERTEX_POINT ( 'NONE', #44001 ) ;
#3974 = CIRCLE ( 'NONE', #15588, 7.199999999999998401 ) ;
#3975 = VECTOR ( 'NONE', #27151, 1000.000000000000000 ) ;
#3976 = VECTOR ( 'NONE', #24362, 1000.000000000000000 ) ;
#3977 = EDGE_LOOP ( 'NONE', ( #36622, #51457, #49224, #77566 ) ) ;
#3978 = ORIENTED_EDGE ( 'NONE', *, *, #866, .F. ) ;
#3979 = EDGE_CURVE ( 'NONE', #70069, #39961, #44453, .T. ) ;
#3980 = ORIENTED_EDGE ( 'NONE', *, *, #65488, .F. ) ;
#3981 = DIRECTION ( 'NONE',  ( 0.000000000000000000, 0.000000000000000000, -1.000000000000000000 ) ) ;
#3982 = CARTESIAN_POINT ( 'NONE',  ( 104.5881800117806932, -26.60309611811081254, 281.2670538473395823 ) ) ;
#3983 = FACE_OUTER_BOUND ( 'NONE', #80737, .T. ) ;
#3984 = EDGE_CURVE ( 'NONE', #79449, #88193, #70403, .T. ) ;
#3985 = LINE ( 'NONE', #85345, #68695 ) ;
#3987 = DIRECTION ( 'NONE',  ( 0.000000000000000000, 0.000000000000000000, -1.000000000000000000 ) ) ;
#3986 = CARTESIAN_POINT ( 'NONE',  ( 122.2189888861420286, -111.9861225405540353, -19.18411693322877198 ) ) ;
#3988 = CARTESIAN_POINT ( 'NONE',  ( 104.9258105463076873, -28.46061097091046577, 199.7009912566479386 ) ) ;
#3989 = EDGE_LOOP ( 'NONE', ( #47707, #62457 ) ) ;
#3990 = VERTEX_POINT ( 'NONE', #30841 ) ;
#3991 = ORIENTED_EDGE ( 'NONE', *, *, #40474, .F. ) ;
#3992 = VECTOR ( 'NONE', #27514, 1000.000000000000000 ) ;
#3993 = DIRECTION ( 'NONE',  ( 1.000000000000000000, 0.000000000000000000, 0.000000000000000000 ) ) ;
#3994 = CARTESIAN_POINT ( 'NONE',  ( 104.4079088469246130, -46.45803334375896299, 182.3648505240071245 ) ) ;
#3995 = CARTESIAN_POINT ( 'NONE',  ( -487.2989999999999782, 18.41194598552324990, 83.34375000000000000 ) ) ;
#3996 = CARTESIAN_POINT ( 'NONE',  ( 113.0371668699568204, -44.84250099658410704, 29.51301187732496700 ) ) ;
#3997 = CARTESIAN_POINT ( 'NONE',  ( 118.5451175586561874, 95.14807216649714405, 1.659552426424649729 ) ) ;
#3998 = CYLINDRICAL_SURFACE ( 'NONE', #11467, 0.9999999999991942001 ) ;
#3999 = DIRECTION ( 'NONE',  ( 0.000000000000000000, 0.000000000000000000, -1.000000000000000000 ) ) ;
#4000 = VERTEX_POINT ( 'NONE', #58530 ) ;
#4001 = DIRECTION ( 'NONE',  ( 0.000000000000000000, 0.000000000000000000, 1.000000000000000000 ) ) ;
#4002 = ORIENTED_EDGE ( 'NONE', *, *, #27222, .T. ) ;
#4004 = EDGE_CURVE ( 'NONE', #21043, #43807, #26692, .T. ) ;
#4003 = CARTESIAN_POINT ( 'NONE',  ( 83.56670559755343675, -40.03837296219067099, 249.5838068554176630 ) ) ;
#4005 = CARTESIAN_POINT ( 'NONE',  ( 99.12746238500623974, -38.62725459667914407, 54.33094751244893672 ) ) ;
#4006 = AXIS2_PLACEMENT_3D ( 'NONE', #62057, #27544, #85664 ) ;
#4007 = CARTESIAN_POINT ( 'NONE',  ( 135.5068622967207830, -16.38644903112292894, 7.895285856717910278 ) ) ;
#4008 = ADVANCED_FACE ( 'NONE', ( #24920 ), #47573, .T. ) ;
#4009 = CYLINDRICAL_SURFACE ( 'NONE', #78061, 2.750000000000002665 ) ;
#4010 = CARTESIAN_POINT ( 'NONE',  ( -8.690350657389011246, 91.82034414994009808, 118.2374269007433440 ) ) ;
#4011 = ORIENTED_EDGE ( 'NONE', *, *, #16740, .F. ) ;
#4012 = LINE ( 'NONE', #59851, #114 ) ;
#4013 = CARTESIAN_POINT ( 'NONE',  ( 119.5843592605237120, 53.27973259447988141, -52.38750000000000995 ) ) ;
#4014 = VERTEX_POINT ( 'NONE', #38537 ) ;
#4015 = CARTESIAN_POINT ( 'NONE',  ( 97.54218415029114908, -32.48978251111615378, 100.9927681330539713 ) ) ;
#4016 = ORIENTED_EDGE ( 'NONE', *, *, #35881, .T. ) ;
#4017 = CARTESIAN_POINT ( 'NONE',  ( 100.6982016950751699, -42.46504578929962292, 56.33241982807696502 ) ) ;
#4018 = CARTESIAN_POINT ( 'NONE',  ( 142.8687636814962616, 5.654319119531167281, 361.9756252759100335 ) ) ;
#4019 = CARTESIAN_POINT ( 'NONE',  ( 99.62013013265574557, -29.94545647671011679, 77.17015473446797102 ) ) ;
#4020 = CARTESIAN_POINT ( 'NONE',  ( 123.6837132603319418, -53.34645651782485487, 239.5838068554170377 ) ) ;
#4021 = DIRECTION ( 'NONE',  ( 0.9130365726098600421, -0.000000000000000000, 0.4078776986755216494 ) ) ;
#4022 = VECTOR ( 'NONE', #18685, 1000.000000000000000 ) ;
#4023 = FACE_OUTER_BOUND ( 'NONE', #50223, .T. ) ;
#4024 = CARTESIAN_POINT ( 'NONE',  ( 110.5624684038761814, -46.61161715960605534, 33.84705384733993583 ) ) ;
#4025 = CYLINDRICAL_SURFACE ( 'NONE', #58292, 0.4999999999999933387 ) ;
#4026 = ORIENTED_EDGE ( 'NONE', *, *, #41664, .F. ) ;
#4027 = CARTESIAN_POINT ( 'NONE',  ( -48.67264380398864176, 54.97499999999996589, 66.68100227564391957 ) ) ;
#4028 = CIRCLE ( 'NONE', #56198, 2.117000000000007987 ) ;
#4029 = ORIENTED_EDGE ( 'NONE', *, *, #80806, .F. ) ;
#4031 = EDGE_CURVE ( 'NONE', #78275, #57034, #51709, .T. ) ;
#4030 = AXIS2_PLACEMENT_3D ( 'NONE', #44635, #64216, #64650 ) ;
#4032 = CARTESIAN_POINT ( 'NONE',  ( -118.1268077877469977, 74.81620433377381119, 10.08232578576174099 ) ) ;
#4033 = ORIENTED_EDGE ( 'NONE', *, *, #33159, .T. ) ;
#4034 = ORIENTED_EDGE ( 'NONE', *, *, #12569, .F. ) ;
#4035 = CARTESIAN_POINT ( 'NONE',  ( -3.175000000000120171, 17.78000000000000114, -33.98325472291465132 ) ) ;
#4036 = AXIS2_PLACEMENT_3D ( 'NONE', #47451, #20670, #82910 ) ;
#4037 = ORIENTED_EDGE ( 'NONE', *, *, #51338, .F. ) ;
#4038 = CARTESIAN_POINT ( 'NONE',  ( 116.5994914424366016, -40.81117973626242446, 213.5165776568640013 ) ) ;
#4039 = CARTESIAN_POINT ( 'NONE',  ( 98.47266077831692144, -31.55723625645210362, 125.8945218809075470 ) ) ;
#4040 = FACE_OUTER_BOUND ( 'NONE', #569, .T. ) ;
#4041 = CARTESIAN_POINT ( 'NONE',  ( 112.8177273059790764, -27.29031728650405597, 45.62895860924398761 ) ) ;
#4042 = CARTESIAN_POINT ( 'NONE',  ( 143.0664832912740110, -8.729447159940999512, -5.074374724088000832 ) ) ;
#4043 = ORIENTED_EDGE ( 'NONE', *, *, #87102, .T. ) ;
#4044 = FACE_OUTER_BOUND ( 'NONE', #20744, .T. ) ;
#4045 = EDGE_CURVE ( 'NONE', #78144, #37970, #73960, .T. ) ;
#4046 = VECTOR ( 'NONE', #67580, 1000.000000000000000 ) ;
#4047 = AXIS2_PLACEMENT_3D ( 'NONE', #28872, #44145, #71886 ) ;
#4048 = CYLINDRICAL_SURFACE ( 'NONE', #52014, 31.75000000000000000 ) ;
#4049 = ORIENTED_EDGE ( 'NONE', *, *, #30302, .T. ) ;
#4050 = LINE ( 'NONE', #10863, #30063 ) ;
#4051 = CARTESIAN_POINT ( 'NONE',  ( 125.5177273812784762, -131.0330679306342461, 55.21780685541800437 ) ) ;
#4052 = CARTESIAN_POINT ( 'NONE',  ( 98.91597900623158068, -29.29754952351876796, 230.7261014663869503 ) ) ;
#4053 = LINE ( 'NONE', #12215, #21138 ) ;
#4054 = EDGE_CURVE ( 'NONE', #8960, #63665, #52584, .T. ) ;
#4055 = DIRECTION ( 'NONE',  ( 9.351236661543306751E-17, -3.725950533538267725E-29, -1.000000000000000000 ) ) ;
#4056 = CARTESIAN_POINT ( 'NONE',  ( 77.85525873416882803, -38.37463194330737082, 2.472581811079971104 ) ) ;
#4057 = CARTESIAN_POINT ( 'NONE',  ( 114.2024335102360908, -32.03537151136463734, 253.7124198280768042 ) ) ;
#4059 = CARTESIAN_POINT ( 'NONE',  ( 104.7644060343265551, -46.87484541886965417, 68.39848241876794077 ) ) ;
#4058 = DIRECTION ( 'NONE',  ( 1.000000000000000078E-15, -1.000000000000000083E-30, -1.000000000000000000 ) ) ;
#4060 = CARTESIAN_POINT ( 'NONE',  ( 112.1769819967410768, 67.02335788169725106, 66.79262069672253688 ) ) ;
#4061 = CARTESIAN_POINT ( 'NONE',  ( 97.89382931228060158, -31.60946541130721954, 110.9213395616259703 ) ) ;
#4062 = ORIENTED_EDGE ( 'NONE', *, *, #65190, .F. ) ;
#4063 = FACE_OUTER_BOUND ( 'NONE', #32493, .T. ) ;
#4064 = ORIENTED_EDGE ( 'NONE', *, *, #48198, .F. ) ;
#4065 = DIRECTION ( 'NONE',  ( 1.000000000000000000, -0.000000000000000000, 2.108231265501709878E-16 ) ) ;
#4066 = DIRECTION ( 'NONE',  ( 0.8660254037844379305, 0.000000000000000000, -0.5000000000000011102 ) ) ;
#4067 = CARTESIAN_POINT ( 'NONE',  ( 19.56648329127303043, -18.82844715994100326, 342.9256252759109884 ) ) ;
#4069 = ORIENTED_EDGE ( 'NONE', *, *, #17170, .T. ) ;
#4068 = EDGE_CURVE ( 'NONE', #54103, #41996, #66232, .T. ) ;
#4070 = CARTESIAN_POINT ( 'NONE',  ( 97.12558208529860337, -37.99706834861481042, 51.42732375708717996 ) ) ;
#4072 = EDGE_LOOP ( 'NONE', ( #12695, #78909 ) ) ;
#4071 = CARTESIAN_POINT ( 'NONE',  ( 97.50197496249766971, -32.47188371672483242, 100.9927681330539713 ) ) ;
#4073 = DIRECTION ( 'NONE',  ( 1.000000000000000078E-15, -1.000000000000000083E-30, -1.000000000000000000 ) ) ;
#4074 = CARTESIAN_POINT ( 'NONE',  ( 147.9050922409201121, -0.9159188039171800577, 542.9756252759101471 ) ) ;
#4075 = VECTOR ( 'NONE', #69517, 1000.000000000000114 ) ;
#4076 = DIRECTION ( 'NONE',  ( -1.000000000000000000, -2.756263715554006823E-15, 0.000000000000000000 ) ) ;
#4077 = ORIENTED_EDGE ( 'NONE', *, *, #86797, .F. ) ;
#4078 = CARTESIAN_POINT ( 'NONE',  ( 108.2792694979413568, -26.31707411447196421, 129.9841967044819739 ) ) ;
#4079 = APPLICATION_PROTOCOL_DEFINITION ( 'draft international standard', 'automotive_design', 1998, #86420 ) ;
#4080 = CARTESIAN_POINT ( 'NONE',  ( 168.5667039024480687, -48.82844715993517326, 300.4678068554149490 ) ) ;
#4081 = CARTESIAN_POINT ( 'NONE',  ( 91.91229715706504066, -111.9484203394872850, -19.21044887263775891 ) ) ;
#4082 = ORIENTED_EDGE ( 'NONE', *, *, #12572, .F. ) ;
#4083 = EDGE_CURVE ( 'NONE', #64107, #47880, #968, .T. ) ;
#4084 = ORIENTED_EDGE ( 'NONE', *, *, #37132, .F. ) ;
#4085 = DIRECTION ( 'NONE',  ( 0.000000000000000000, 0.000000000000000000, 1.000000000000000000 ) ) ;
#4086 = EDGE_CURVE ( 'NONE', #81729, #45431, #45779, .T. ) ;
#4087 = LINE ( 'NONE', #31788, #80241 ) ;
#4088 = EDGE_CURVE ( 'NONE', #60868, #9815, #53023, .T. ) ;
#4089 = PLANE ( 'NONE',  #64691 ) ;
#4090 = EDGE_CURVE ( 'NONE', #62556, #26370, #60766, .T. ) ;
#4092 = CARTESIAN_POINT ( 'NONE',  ( 67.06673837846007302, -137.6758525980020806, 245.5072637273240161 ) ) ;
#4091 = CARTESIAN_POINT ( 'NONE',  ( 0.000000000000000000, 127.0000000000000000, 42.54500000000000171 ) ) ;
#4093 = CARTESIAN_POINT ( 'NONE',  ( 41.56648329127399677, -18.82844715994099971, 256.8086252759120498 ) ) ;
#4094 = CIRCLE ( 'NONE', #86776, 7.999999999999992895 ) ;
#4095 = ORIENTED_EDGE ( 'NONE', *, *, #9873, .F. ) ;
#4096 = VECTOR ( 'NONE', #56793, 1000.000000000000000 ) ;
#4097 = DIRECTION ( 'NONE',  ( 0.9130365726098600421, 0.000000000000000000, 0.4078776986755215939 ) ) ;
#4098 = CARTESIAN_POINT ( 'NONE',  ( 97.71246005893831921, -41.20616857227587815, 212.6937205140059461 ) ) ;
#4100 = VERTEX_POINT ( 'NONE', #67139 ) ;
#4099 = CARTESIAN_POINT ( 'NONE',  ( 105.8259002483207922, -25.33766151058717142, 321.6188579224977389 ) ) ;
#4101 = VECTOR ( 'NONE', #45439, 1000.000000000000000 ) ;
#4102 = CARTESIAN_POINT ( 'NONE',  ( 97.89279369561094768, -33.33727167892453735, 62.04419670448196911 ) ) ;
#4103 = CARTESIAN_POINT ( 'NONE',  ( 108.3332121129147225, -46.73488633077575827, 52.67731614845624932 ) ) ;
#4104 = CARTESIAN_POINT ( 'NONE',  ( 97.81168895331838087, -40.51742574516882200, 11.63562527591094309 ) ) ;
#4105 = VECTOR ( 'NONE', #79320, 1000.000000000000000 ) ;
#4106 = CARTESIAN_POINT ( 'NONE',  ( 173.8164832912740110, 12.92155284005802685, 349.2756252759111248 ) ) ;
#4107 = ORIENTED_EDGE ( 'NONE', *, *, #65605, .T. ) ;
#4108 = DIRECTION ( 'NONE',  ( 1.000000000000000000, 1.000000000000013883E-15, 4.440892098500630106E-16 ) ) ;
#4109 = VECTOR ( 'NONE', #17206, 1000.000000000000000 ) ;
#4110 = AXIS2_PLACEMENT_3D ( 'NONE', #71347, #36370, #58144 ) ;
#4111 = VERTEX_POINT ( 'NONE', #81691 ) ;
#4112 = EDGE_LOOP ( 'NONE', ( #48740, #73787, #79436, #49787 ) ) ;
#4113 = CARTESIAN_POINT ( 'NONE',  ( 100.2828564484647274, -30.98100942051235052, 212.1987261630399360 ) ) ;
#4114 = CARTESIAN_POINT ( 'NONE',  ( 105.7167024970128608, -46.72405552150465269, 53.46869760484980816 ) ) ;
#4115 = CARTESIAN_POINT ( 'NONE',  ( -85.52787878288653189, 91.23859726994542996, 98.64044413063014360 ) ) ;
#4116 = ADVANCED_FACE ( 'NONE', ( #87154 ), #18998, .F. ) ;
#4117 = CARTESIAN_POINT ( 'NONE',  ( 173.9900000000000091, 52.73749999999999716, -62.78087104677060637 ) ) ;
#4118 = AXIS2_PLACEMENT_3D ( 'NONE', #12771, #68181, #83166 ) ;
#4119 = DIRECTION ( 'NONE',  ( 0.000000000000000000, 0.000000000000000000, -1.000000000000000000 ) ) ;
#4120 = ORIENTED_EDGE ( 'NONE', *, *, #22845, .F. ) ;
#4121 = DIRECTION ( 'NONE',  ( 1.000000000000000000, 2.999999999999999839E-15, 1.000000000000000078E-15 ) ) ;
#4122 = DIRECTION ( 'NONE',  ( 0.4999999999999994449, 0.8660254037844390407, -2.684678751731759347E-14 ) ) ;
#4123 = ORIENTED_EDGE ( 'NONE', *, *, #34464, .T. ) ;
#4124 = CARTESIAN_POINT ( 'NONE',  ( 96.68905559037375497, -32.92312794843576995, 21.03467289495897319 ) ) ;
#4125 = DIRECTION ( 'NONE',  ( -0.7071067811865495711, 0.000000000000000000, 0.7071067811865455743 ) ) ;
#4126 = EDGE_LOOP ( 'NONE', ( #54924, #32505 ) ) ;
#4127 = CARTESIAN_POINT ( 'NONE',  ( 99.04406185070456559, -42.84125762965616957, 81.84395860822249347 ) ) ;
#4128 = DIRECTION ( 'NONE',  ( 0.7071067811865758834, -0.7071067811865192621, 7.071067811865765240E-16 ) ) ;
#4129 = CARTESIAN_POINT ( 'NONE',  ( 83.73314995793998605, 12.92155284005730387, 355.9756252759109998 ) ) ;
#4130 = CARTESIAN_POINT ( 'NONE',  ( 122.2221484686745185, -96.57698625956679450, -11.78219314458225853 ) ) ;
#4131 = VECTOR ( 'NONE', #28596, 1000.000000000000114 ) ;
#4132 = VECTOR ( 'NONE', #47429, 1000.000000000000000 ) ;
#4133 = CARTESIAN_POINT ( 'NONE',  ( 98.50201126197670476, -30.70924794336980668, 201.8384824187679385 ) ) ;
#4134 = CARTESIAN_POINT ( 'NONE',  ( 4.052643387441906775, 70.61235367433147303, 118.2872599129365057 ) ) ;
#4135 = VERTEX_POINT ( 'NONE', #88501 ) ;
#4136 = CARTESIAN_POINT ( 'NONE',  ( 115.2006710226633004, -43.31943727361606733, 84.28419670448195689 ) ) ;
#4137 = ADVANCED_FACE ( 'NONE', ( #38983 ), #88939, .F. ) ;
#4138 = DIRECTION ( 'NONE',  ( 1.000000000000000078E-15, -1.000000000000000083E-30, -1.000000000000000000 ) ) ;
#4139 = ORIENTED_EDGE ( 'NONE', *, *, #52958, .T. ) ;
#4141 = EDGE_CURVE ( 'NONE', #52360, #19111, #12186, .T. ) ;
#4140 = ORIENTED_EDGE ( 'NONE', *, *, #28041, .T. ) ;
#4142 = VERTEX_POINT ( 'NONE', #53933 ) ;
#4143 = ADVANCED_FACE ( 'NONE', ( #5369 ), #33516, .F. ) ;
#4144 = CARTESIAN_POINT ( 'NONE',  ( 78.49243656059439900, -38.98954602991467056, 7.829737348688145637 ) ) ;
#4145 = CARTESIAN_POINT ( 'NONE',  ( 141.0664832912740110, -8.729447159940995959, -4.824374724088991151 ) ) ;
#4146 = CARTESIAN_POINT ( 'NONE',  ( 112.0636451658066193, -45.48965997882522316, 152.9902778487048636 ) ) ;
#4147 = CARTESIAN_POINT ( 'NONE',  ( 110.7682021097048306, -28.22102727396991284, 132.5680903695919710 ) ) ;
#4148 = CARTESIAN_POINT ( 'NONE',  ( 110.2625522973084600, -26.74624433126517076, 230.8299109901969643 ) ) ;
#4149 = EDGE_CURVE ( 'NONE', #45090, #23101, #11262, .T. ) ;
#4150 = DIRECTION ( 'NONE',  ( 0.000000000000000000, 0.000000000000000000, 1.000000000000000000 ) ) ;
#4151 = EDGE_LOOP ( 'NONE', ( #9354, #88619 ) ) ;
#4152 = VECTOR ( 'NONE', #34784, 1000.000000000000000 ) ;
#4153 = EDGE_CURVE ( 'NONE', #35419, #51043, #47124, .T. ) ;
#4154 = CARTESIAN_POINT ( 'NONE',  ( 135.2499137886250935, -39.21189172703900994, 1.845048092479758095 ) ) ;
#4155 = ORIENTED_EDGE ( 'NONE', *, *, #70123, .T. ) ;
#4156 = VERTEX_POINT ( 'NONE', #40321 ) ;
#4157 = ADVANCED_FACE ( 'NONE', ( #68042, #19892 ), #42550, .T. ) ;
#4158 = AXIS2_PLACEMENT_3D ( 'NONE', #33701, #54554, #69120 ) ;
#4159 = ADVANCED_FACE ( 'NONE', ( #70277 ), #56177, .F. ) ;
#4160 = CARTESIAN_POINT ( 'NONE',  ( 223.2659999999999911, 52.73749999999999716, -32.00399999999999778 ) ) ;
#4161 = EDGE_LOOP ( 'NONE', ( #16368, #78238, #47634, #25917 ) ) ;
#4162 = ORIENTED_EDGE ( 'NONE', *, *, #87447, .F. ) ;
#4163 = DIRECTION ( 'NONE',  ( 0.7071067811865784369, -0.7071067811865165975, 7.071067811865480264E-16 ) ) ;
#4164 = DIRECTION ( 'NONE',  ( 0.7071067811865431318, -0.7071067811865517916, 7.071067811865425043E-16 ) ) ;
#4165 = EDGE_CURVE ( 'NONE', #1484, #54987, #83927, .T. ) ;
#4166 = LINE ( 'NONE', #59110, #4022 ) ;
#4167 = CARTESIAN_POINT ( 'NONE',  ( 105.6324958909751075, -46.33196107771311745, 146.8809912566479738 ) ) ;
#4168 = CARTESIAN_POINT ( 'NONE',  ( 97.06250871634010480, -39.81605817309107920, 21.56419670448195092 ) ) ;
#4169 = ORIENTED_EDGE ( 'NONE', *, *, #2189, .T. ) ;
#4170 = AXIS2_PLACEMENT_3D ( 'NONE', #13419, #41103, #42887 ) ;
#4171 = EDGE_CURVE ( 'NONE', #43699, #82504, #79437, .T. ) ;
#4172 = CARTESIAN_POINT ( 'NONE',  ( -88.20503424218274802, 71.54629894495528220, -79.21825297796436871 ) ) ;
#4174 = ORIENTED_EDGE ( 'NONE', *, *, #74964, .F. ) ;
#4173 = EDGE_CURVE ( 'NONE', #40480, #68811, #82455, .T. ) ;
#4175 = VECTOR ( 'NONE', #18293, 1000.000000000000000 ) ;
#4176 = LINE ( 'NONE', #52725, #54794 ) ;
#4177 = VERTEX_POINT ( 'NONE', #89392 ) ;
#4178 = CARTESIAN_POINT ( 'NONE',  ( 97.74156636318205926, -40.34206866484610288, 167.6208556024714653 ) ) ;
#4179 = CIRCLE ( 'NONE', #31725, 3.499999999999996003 ) ;
#4180 = FACE_OUTER_BOUND ( 'NONE', #6599, .T. ) ;
#4181 = CARTESIAN_POINT ( 'NONE',  ( 97.81556180715350024, -40.52687500387260400, 131.6364377373729440 ) ) ;
#4182 = LINE ( 'NONE', #45048, #56706 ) ;
#4183 = ORIENTED_EDGE ( 'NONE', *, *, #13488, .T. ) ;
#4184 = CARTESIAN_POINT ( 'NONE',  ( 101.5973605122076862, -47.27098594307553725, 17.19562527591095247 ) ) ;
#4185 = CARTESIAN_POINT ( 'NONE',  ( 115.9822161205003397, -42.21601869724081268, 14.38705384733995984 ) ) ;
#4187 = CARTESIAN_POINT ( 'NONE',  ( 69.39098523492604897, -138.6132424365590623, 247.3878207843068537 ) ) ;
#4186 = FACE_OUTER_BOUND ( 'NONE', #25960, .T. ) ;
#4188 = CARTESIAN_POINT ( 'NONE',  ( 112.1393585966182656, -28.01283025110964786, 145.6568144398399340 ) ) ;
#4189 = DIRECTION ( 'NONE',  ( -1.000000000000000000, -4.299999999999999979E-14, -1.000000000000000078E-15 ) ) ;
#4190 = LINE ( 'NONE', #60937, #70232 ) ;
#4191 = VECTOR ( 'NONE', #3167, 1000.000000000000114 ) ;
#4192 = EDGE_CURVE ( 'NONE', #61394, #71543, #77107, .T. ) ;
#4193 = CARTESIAN_POINT ( 'NONE',  ( 113.2454986892643802, -28.75867293750068043, 10.55229194345644039 ) ) ;
#4194 = EDGE_CURVE ( 'NONE', #8698, #37391, #44436, .T. ) ;
#4195 = EDGE_CURVE ( 'NONE', #27163, #62031, #66364, .T. ) ;
#4196 = DIRECTION ( 'NONE',  ( -1.000000000000000000, 0.000000000000000000, -1.840813417405305102E-14 ) ) ;
#4197 = CARTESIAN_POINT ( 'NONE',  ( 96.88405369895032493, -39.16353706000892032, 56.51276813305394597 ) ) ;
#4198 = CARTESIAN_POINT ( 'NONE',  ( 101.2007021600770855, -45.34774740814643934, 193.1013395616249682 ) ) ;
#4199 = CARTESIAN_POINT ( 'NONE',  ( 99.96594057013267332, -44.39231554709003547, 42.98133956162492098 ) ) ;
#4200 = ADVANCED_FACE ( 'NONE', ( #89847 ), #13527, .T. ) ;
#4202 = CARTESIAN_POINT ( 'NONE',  ( 151.0371591254573787, -24.95799193692592866, 249.9678068554149490 ) ) ;
#4201 = CARTESIAN_POINT ( 'NONE',  ( 177.1649999999999920, 14.63749999999999929, -52.38749999999999574 ) ) ;
#4203 = DIRECTION ( 'NONE',  ( 0.000000000000000000, 1.000000000000000000, 0.000000000000000000 ) ) ;
#4204 = AXIS2_PLACEMENT_3D ( 'NONE', #83664, #90, #27340 ) ;
#4205 = ORIENTED_EDGE ( 'NONE', *, *, #88673, .F. ) ;
#4206 = CARTESIAN_POINT ( 'NONE',  ( 172.5664832912740110, -32.07844715994070839, 258.9256252759120116 ) ) ;
#4207 = ORIENTED_EDGE ( 'NONE', *, *, #20358, .F. ) ;
#4208 = CARTESIAN_POINT ( 'NONE',  ( 107.8912859324307192, -26.39220933555703752, 111.0251490854339806 ) ) ;
#4210 = VERTEX_POINT ( 'NONE', #34406 ) ;
#4209 = CARTESIAN_POINT ( 'NONE',  ( 7.283224538747764321, 92.95786475339244248, 130.3529002834609969 ) ) ;
#4211 = CARTESIAN_POINT ( 'NONE',  ( 52.06670390244699576, -68.87844715994100397, 180.4678068554179902 ) ) ;
#4212 = CARTESIAN_POINT ( 'NONE',  ( 110.8089421659425540, -26.35361831834165969, 245.7889586092439629 ) ) ;
#4213 = CARTESIAN_POINT ( 'NONE',  ( 163.0664832912739826, 12.92155284005902516, 336.6506252759110112 ) ) ;
#4214 = PLANE ( 'NONE',  #89922 ) ;
#4215 = DIRECTION ( 'NONE',  ( 1.000000000000000078E-15, 0.000000000000000000, 1.000000000000000000 ) ) ;
#4216 = CARTESIAN_POINT ( 'NONE',  ( 116.1804594027163517, -40.96476762480074996, 9.425625275910979539 ) ) ;
#4217 = VECTOR ( 'NONE', #69205, 1000.000000000000000 ) ;
#4218 = DIRECTION ( 'NONE',  ( -1.000000000000000000, -8.163404592832032979E-16, 0.000000000000000000 ) ) ;
#4219 = CARTESIAN_POINT ( 'NONE',  ( -84.91200770515607132, 74.81660785136577374, 99.17101862044627580 ) ) ;
#4220 = CARTESIAN_POINT ( 'NONE',  ( 103.2204921605863888, -27.09891563476508836, 175.3908633711489813 ) ) ;
#4221 = ORIENTED_EDGE ( 'NONE', *, *, #34620, .F. ) ;
#4222 = ORIENTED_EDGE ( 'NONE', *, *, #83968, .T. ) ;
#4223 = AXIS2_PLACEMENT_3D ( 'NONE', #40840, #62186, #20423 ) ;
#4224 = CARTESIAN_POINT ( 'NONE',  ( 103.2343105203340201, -28.73928255177903068, 91.86444044875396742 ) ) ;
#4225 = DIRECTION ( 'NONE',  ( -0.7071067811865784369, 0.7071067811865165975, -7.071067811865480264E-16 ) ) ;
#4227 = CARTESIAN_POINT ( 'NONE',  ( 107.5667039024470455, -113.7784471599420613, -19.78219314458171141 ) ) ;
#4226 = CARTESIAN_POINT ( 'NONE',  ( 110.8764511561472119, -27.72125199330416478, 240.7584824187679544 ) ) ;
#4228 = DIRECTION ( 'NONE',  ( 1.000000000000000078E-15, 0.000000000000000000, -1.000000000000000000 ) ) ;
#4229 = LINE ( 'NONE', #83118, #49579 ) ;
#4230 = CARTESIAN_POINT ( 'NONE',  ( 118.1704280561596931, 74.16215221268205937, 9.571784452934572585 ) ) ;
#4231 = AXIS2_PLACEMENT_3D ( 'NONE', #29075, #15456, #57206 ) ;
#4232 = CARTESIAN_POINT ( 'NONE',  ( -4.091298994373309128, 70.49827730944788584, 118.4878841633551474 ) ) ;
#4233 = DIRECTION ( 'NONE',  ( 1.639958061481212836E-42, -4.100000000000000342E-29, -1.000000000000000000 ) ) ;
#4234 = CARTESIAN_POINT ( 'NONE',  ( 31.56670390244800828, -33.35206098992711077, 237.4678068554150059 ) ) ;
#4236 = CARTESIAN_POINT ( 'NONE',  ( 110.6887065042383256, -47.98678726807249006, 207.8241967044819489 ) ) ;
#4235 = AXIS2_PLACEMENT_3D ( 'NONE', #11559, #63500, #66051 ) ;
#4237 = EDGE_LOOP ( 'NONE', ( #60350, #14798 ) ) ;
#4238 = ORIENTED_EDGE ( 'NONE', *, *, #48664, .F. ) ;
#4239 = DIRECTION ( 'NONE',  ( 0.7071067811865604513, 0.000000000000000000, -0.7071067811865344721 ) ) ;
#4240 = CARTESIAN_POINT ( 'NONE',  ( 108.4174892996514075, -26.73503593485758145, 150.9689586054618360 ) ) ;
#4241 = VECTOR ( 'NONE', #29666, 1000.000000000000000 ) ;
#4242 = FACE_OUTER_BOUND ( 'NONE', #42519, .T. ) ;
#4243 = DIRECTION ( 'NONE',  ( 1.000000000000000000, -0.000000000000000000, 2.108231265501710124E-16 ) ) ;
#4244 = ORIENTED_EDGE ( 'NONE', *, *, #4944, .F. ) ;
#4245 = CARTESIAN_POINT ( 'NONE',  ( 99.04404884010753563, -42.84124075760115602, 267.8439569258346751 ) ) ;
#4246 = EDGE_CURVE ( 'NONE', #43807, #18476, #3283, .T. ) ;
#4247 = CARTESIAN_POINT ( 'NONE',  ( 109.3585227812971539, -25.91623105973918939, 184.9222919425779708 ) ) ;
#4248 = EDGE_CURVE ( 'NONE', #29169, #86897, #7611, .T. ) ;
#4249 = LINE ( 'NONE', #18318, #38584 ) ;
#4250 = ORIENTED_EDGE ( 'NONE', *, *, #78426, .T. ) ;
#4252 = ORIENTED_EDGE ( 'NONE', *, *, #64976, .T. ) ;
#4251 = ORIENTED_EDGE ( 'NONE', *, *, #30489, .F. ) ;
#4253 = AXIS2_PLACEMENT_3D ( 'NONE', #41794, #20931, #49057 ) ;
#4254 = EDGE_CURVE ( 'NONE', #84281, #82155, #2593, .T. ) ;
#4255 = CARTESIAN_POINT ( 'NONE',  ( -11.00664350276215941, 76.20047485311516766, 118.0441341279204721 ) ) ;
#4256 = CARTESIAN_POINT ( 'NONE',  ( 188.5667039024479834, -67.87844715994100397, 173.2178068554149775 ) ) ;
#4257 = CARTESIAN_POINT ( 'NONE',  ( 97.81555538561684671, -40.52686194202485837, 166.6364365798628171 ) ) ;
#4258 = CARTESIAN_POINT ( 'NONE',  ( 115.2261106523039444, -36.95351711827176899, 41.62237608387797394 ) ) ;
#4259 = EDGE_CURVE ( 'NONE', #83807, #51539, #49605, .T. ) ;
#4260 = DIRECTION ( 'NONE',  ( 0.7071067811571474238, 0.7071067812159476107, 0.000000000000000000 ) ) ;
#4261 = EDGE_LOOP ( 'NONE', ( #57389, #30712 ) ) ;
#4262 = LINE ( 'NONE', #61007, #47994 ) ;
#4263 = CIRCLE ( 'NONE', #15885, 2.500000000000002220 ) ;
#4264 = DIRECTION ( 'NONE',  ( -0.04216478779797398074, 0.9991106698809455455, 1.084202172485504434E-19 ) ) ;
#4265 = EDGE_LOOP ( 'NONE', ( #76368, #16996, #77568, #21622 ) ) ;
#4266 = EDGE_LOOP ( 'NONE', ( #24443, #28092, #88300, #78688 ) ) ;
#4267 = ADVANCED_FACE ( 'NONE', ( #64810 ), #23048, .F. ) ;
#4268 = LINE ( 'NONE', #59656, #67666 ) ;
#4269 = EDGE_LOOP ( 'NONE', ( #55960, #32869, #57323, #66768 ) ) ;
#4270 = EDGE_LOOP ( 'NONE', ( #6902, #9144, #40909, #60507, #65679 ) ) ;
#4271 = DIRECTION ( 'NONE',  ( -1.000000000000000078E-15, 1.000000000000000000, 0.000000000000000000 ) ) ;
#4272 = EDGE_CURVE ( 'NONE', #60191, #24962, #85893, .T. ) ;
#4273 = CARTESIAN_POINT ( 'NONE',  ( 102.0495883242188171, -29.81664044981240025, 74.99813411379096806 ) ) ;
#4274 = CARTESIAN_POINT ( 'NONE',  ( 108.1841437630847338, -47.11680481413669952, 202.6613395616249704 ) ) ;
#4275 = AXIS2_PLACEMENT_3D ( 'NONE', #27906, #57398, #8832 ) ;
#4276 = CARTESIAN_POINT ( 'NONE',  ( 113.6717327907684165, -45.56316108038149082, 188.0994347997199725 ) ) ;
#4278 = CARTESIAN_POINT ( 'NONE',  ( 118.1029919389229406, -36.12161712796727642, 269.8822919425776945 ) ) ;
#4277 = LINE ( 'NONE', #33320, #46100 ) ;
#4279 = CARTESIAN_POINT ( 'NONE',  ( -3.968750000000770051, 120.6499999999999915, 105.4788588808462038 ) ) ;
#4280 = DIRECTION ( 'NONE',  ( 0.000000000000000000, 0.000000000000000000, 1.000000000000000000 ) ) ;
#4281 = EDGE_LOOP ( 'NONE', ( #13317, #49329 ) ) ;
#4282 = EDGE_CURVE ( 'NONE', #36892, #34120, #15326, .T. ) ;
#4283 = VECTOR ( 'NONE', #60707, 999.9999999999998863 ) ;
#4284 = VERTEX_POINT ( 'NONE', #78901 ) ;
#4285 = ADVANCED_FACE ( 'NONE', ( #3474 ), #15774, .T. ) ;
#4286 = AXIS2_PLACEMENT_3D ( 'NONE', #3445, #51574, #78876 ) ;
#4287 = AXIS2_PLACEMENT_3D ( 'NONE', #39761, #68388, #20237 ) ;
#4288 = CARTESIAN_POINT ( 'NONE',  ( 183.5150000000000148, 52.73749999999999716, -26.11912895322935313 ) ) ;
#4289 = CARTESIAN_POINT ( 'NONE',  ( 99.05215007911658631, -29.93811023049936892, 215.7670538473399517 ) ) ;
#4290 = VERTEX_POINT ( 'NONE', #85277 ) ;
#4291 = CARTESIAN_POINT ( 'NONE',  ( 103.6385507868184277, -26.22095696399066966, 210.3394347997209763 ) ) ;
#4292 = DIRECTION ( 'NONE',  ( 1.000000000000000078E-15, 0.000000000000000000, -1.000000000000000000 ) ) ;
#4293 = CARTESIAN_POINT ( 'NONE',  ( -6.832456821293724225, 69.76561602091111070, 37.50674678103825244 ) ) ;
#4294 = DIRECTION ( 'NONE',  ( 0.000000000000000000, 0.000000000000000000, 1.000000000000000000 ) ) ;
#4295 = CARTESIAN_POINT ( 'NONE',  ( 143.3672529448882642, -139.2813379893231343, 247.4476445910851510 ) ) ;
#4298 = CARTESIAN_POINT ( 'NONE',  ( 96.58568816239609589, -40.17018292043292860, 282.5908633711490552 ) ) ;
#4297 = LINE ( 'NONE', #24735, #58623 ) ;
#4296 = CARTESIAN_POINT ( 'NONE',  ( 97.86360378202594745, -40.49644234972143408, 277.6356252759112522 ) ) ;
#4299 = DIRECTION ( 'NONE',  ( 0.000000000000000000, 1.000000000000000000, 0.000000000000000000 ) ) ;
#4300 = LINE ( 'NONE', #30664, #24978 ) ;
#4301 = FACE_OUTER_BOUND ( 'NONE', #13829, .T. ) ;
#4302 = VECTOR ( 'NONE', #21212, 1000.000000000000000 ) ;
#4303 = LINE ( 'NONE', #38361, #41347 ) ;
#4304 =( GEOMETRIC_REPRESENTATION_CONTEXT ( 3 ) GLOBAL_UNCERTAINTY_ASSIGNED_CONTEXT ( ( #33563 ) ) GLOBAL_UNIT_ASSIGNED_CONTEXT ( ( #70451, #75914, #70908 ) ) REPRESENTATION_CONTEXT ( 'NONE', 'WORKASPACE' ) );
#4305 = CARTESIAN_POINT ( 'NONE',  ( -72.96458098368751166, 127.0000000000000000, 65.82083098368619289 ) ) ;
#4306 = CARTESIAN_POINT ( 'NONE',  ( 97.81168883536605563, -40.51740680051663190, 96.63562987897269352 ) ) ;
#4307 = EDGE_CURVE ( 'NONE', #70385, #9455, #35083, .T. ) ;
#4309 = VERTEX_POINT ( 'NONE', #31165 ) ;
#4308 = DIRECTION ( 'NONE',  ( 1.000000000000000078E-15, 0.000000000000000000, -1.000000000000000000 ) ) ;
#4310 = CARTESIAN_POINT ( 'NONE',  ( 194.5667039024479834, -67.87844715994100397, 20.91780685541479912 ) ) ;
#4311 = CARTESIAN_POINT ( 'NONE',  ( 106.9748012750099946, -47.17635858745483546, 187.5699109901969734 ) ) ;
#4312 = CARTESIAN_POINT ( 'NONE',  ( 113.9169062821921727, -28.05502007051373070, 120.5565776568639507 ) ) ;
#4313 = CARTESIAN_POINT ( 'NONE',  ( 104.1737878132142043, -26.63141132829087354, 221.2984824187679465 ) ) ;
#4314 = CARTESIAN_POINT ( 'NONE',  ( 27.27158787008328389, 184.0000000000000000, 106.1020876358972629 ) ) ;
#4315 = EDGE_CURVE ( 'NONE', #32905, #16980, #30289, .T. ) ;
#4316 = CARTESIAN_POINT ( 'NONE',  ( 37.06648329127298780, 12.92155284005730387, 355.9756252759109998 ) ) ;
#4318 = DIRECTION ( 'NONE',  ( -1.514143847546114723E-15, -0.8660254037844387076, 0.4999999999999998890 ) ) ;
#4317 = DIRECTION ( 'NONE',  ( -1.000000000000000000, -1.000000000000000078E-15, 0.000000000000000000 ) ) ;
#4319 = CARTESIAN_POINT ( 'NONE',  ( 107.0664832912739968, -36.72944715994100306, 287.6356252759109680 ) ) ;
#4320 = CARTESIAN_POINT ( 'NONE',  ( 150.5667039024473297, -25.42844715993594562, 300.4678068554149490 ) ) ;
#4321 = CARTESIAN_POINT ( 'NONE',  ( 131.4004675426834865, -19.42701295172721387, 2.979899338979302037 ) ) ;
#4322 = AXIS2_PLACEMENT_3D ( 'NONE', #59666, #74660, #20151 ) ;
#4323 = ORIENTED_EDGE ( 'NONE', *, *, #74462, .T. ) ;
#4324 = ORIENTED_EDGE ( 'NONE', *, *, #66591, .T. ) ;
#4325 = AXIS2_PLACEMENT_3D ( 'NONE', #31197, #60237, #38904 ) ;
#4326 = CARTESIAN_POINT ( 'NONE',  ( 97.58007606596183336, -34.66094392094686327, 105.5781341137909664 ) ) ;
#4328 = ORIENTED_EDGE ( 'NONE', *, *, #59587, .F. ) ;
#4327 = CARTESIAN_POINT ( 'NONE',  ( 107.5667039024470455, -113.7784471599413791, 2.217806855418308132 ) ) ;
#4329 = CARTESIAN_POINT ( 'NONE',  ( 105.3199149336540046, -48.42511963160323774, 143.4584824187689662 ) ) ;
#4330 = DIRECTION ( 'NONE',  ( -2.108231265501709878E-16, 0.000000000000000000, 1.000000000000000000 ) ) ;
#4331 = DIRECTION ( 'NONE',  ( 9.351236661543306751E-17, -3.725950533538267725E-29, -1.000000000000000000 ) ) ;
#4332 = EDGE_CURVE ( 'NONE', #26394, #5757, #44344, .T. ) ;
#4333 = CARTESIAN_POINT ( 'NONE',  ( 104.0667030381801936, -67.87844715994094713, 173.2178086137559774 ) ) ;
#4334 = CARTESIAN_POINT ( 'NONE',  ( 116.3212776292293569, -32.94146857471253753, 110.1356252759109822 ) ) ;
#4335 = CARTESIAN_POINT ( 'NONE',  ( 112.4622727538958884, -27.87370092883236694, 49.62895860924398761 ) ) ;
#4336 = ORIENTED_EDGE ( 'NONE', *, *, #74635, .T. ) ;
#4337 = VECTOR ( 'NONE', #55934, 1000.000000000000000 ) ;
#4338 = ORIENTED_EDGE ( 'NONE', *, *, #33616, .F. ) ;
#4339 = EDGE_LOOP ( 'NONE', ( #37405, #61513 ) ) ;
#4340 = ADVANCED_FACE ( 'NONE', ( #64368 ), #37554, .F. ) ;
#4341 = DIRECTION ( 'NONE',  ( -1.000000000000000000, 0.000000000000000000, 0.000000000000000000 ) ) ;
#4343 = DIRECTION ( 'NONE',  ( 0.000000000000000000, 1.000000000000000000, 0.000000000000000000 ) ) ;
#4342 = CARTESIAN_POINT ( 'NONE',  ( 98.40655050692429029, -32.18313002855528993, 131.9413395616250000 ) ) ;
#4344 = CARTESIAN_POINT ( 'NONE',  ( 182.4202572930400095, -33.70561438051981185, -5.074374724088000832 ) ) ;
#4345 = CARTESIAN_POINT ( 'NONE',  ( 33.78309357195740859, -29.99615139352333060, 193.9678068554150911 ) ) ;
#4346 = DIRECTION ( 'NONE',  ( 2.900000000000000265E-14, -2.000000000000000155E-15, 1.000000000000000000 ) ) ;
#4347 = AXIS2_PLACEMENT_3D ( 'NONE', #81002, #52775, #26462 ) ;
#4348 = CARTESIAN_POINT ( 'NONE',  ( 173.9900000000000091, 0.000000000000000000, -131.6533725204182019 ) ) ;
#4349 = DIRECTION ( 'NONE',  ( -1.000000000000000000, -1.000000000000000078E-15, -1.000000000000000078E-15 ) ) ;
#4350 = CARTESIAN_POINT ( 'NONE',  ( 96.73636544059188225, -37.96124694896867169, 41.42133956162496844 ) ) ;
#4351 = VERTEX_POINT ( 'NONE', #78005 ) ;
#4352 = ORIENTED_EDGE ( 'NONE', *, *, #69221, .T. ) ;
#4353 = CIRCLE ( 'NONE', #30423, 4.750000000000004441 ) ;
#4354 = CARTESIAN_POINT ( 'NONE',  ( 139.9417039024470171, -80.65344715994091018, 45.21780685541799727 ) ) ;
#4355 = CARTESIAN_POINT ( 'NONE',  ( -7.661254700127829942, 66.45253841614081125, 275.4630000000000223 ) ) ;
#4356 = PLANE ( 'NONE',  #322 ) ;
#4357 = CARTESIAN_POINT ( 'NONE',  ( 115.0306645585770298, -38.52089976383655312, 146.4680903695919767 ) ) ;
#4358 = VECTOR ( 'NONE', #85533, 1000.000000000000000 ) ;
#4359 = ADVANCED_FACE ( 'NONE', ( #23495 ), #57986, .F. ) ;
#4360 = ADVANCED_FACE ( 'NONE', ( #16659 ), #51160, .F. ) ;
#4361 = CARTESIAN_POINT ( 'NONE',  ( 87.17003668186721654, -54.68655584847608964, -5.074374724089126154 ) ) ;
#4362 = ORIENTED_EDGE ( 'NONE', *, *, #88052, .F. ) ;
#4363 = ORIENTED_EDGE ( 'NONE', *, *, #78833, .F. ) ;
#4364 = CIRCLE ( 'NONE', #88475, 0.3000000000000062617 ) ;
#4365 = CARTESIAN_POINT ( 'NONE',  ( 107.0667039024470313, -104.2784471599409528, 222.2178068554179902 ) ) ;
#4366 = ADVANCED_FACE ( 'NONE', ( #65254 ), #23928, .F. ) ;
#4367 = ORIENTED_EDGE ( 'NONE', *, *, #33334, .F. ) ;
#4368 = ORIENTED_EDGE ( 'NONE', *, *, #69515, .F. ) ;
#4369 = PRODUCT_DEFINITION_FORMATION_WITH_SPECIFIED_SOURCE ( 'ANY', '', #38722, .NOT_KNOWN. ) ;
#4370 = DIRECTION ( 'NONE',  ( -0.000000000000000000, 1.000000000000000000, -0.000000000000000000 ) ) ;
#4371 = CARTESIAN_POINT ( 'NONE',  ( 104.2245914675057321, -27.77399204033938318, 201.7406309249449521 ) ) ;
#4372 = EDGE_CURVE ( 'NONE', #14487, #29010, #58426, .T. ) ;
#4373 = CARTESIAN_POINT ( 'NONE',  ( 122.2221484686747317, -101.0284471599423171, -21.78219314458213063 ) ) ;
#4374 = AXIS2_PLACEMENT_3D ( 'NONE', #33557, #87196, #52627 ) ;
#4375 = LINE ( 'NONE', #19787, #8114 ) ;
#4376 = CARTESIAN_POINT ( 'NONE',  ( -109.3711719371063822, 56.43282072966933072, 71.29388279269264217 ) ) ;
#4377 = ORIENTED_EDGE ( 'NONE', *, *, #50333, .T. ) ;
#4378 = ORIENTED_EDGE ( 'NONE', *, *, #71601, .T. ) ;
#4379 = EDGE_CURVE ( 'NONE', #13459, #54369, #44796, .T. ) ;
#4380 = VERTEX_POINT ( 'NONE', #86599 ) ;
#4381 = VERTEX_POINT ( 'NONE', #8512 ) ;
#4382 = EDGE_CURVE ( 'NONE', #77354, #40177, #81552, .T. ) ;
#4383 = CARTESIAN_POINT ( 'NONE',  ( 104.3071780974205183, -29.01783752938878180, 188.1680903695909706 ) ) ;
#4384 = CARTESIAN_POINT ( 'NONE',  ( 110.1645224859485808, -46.70684747839494833, 97.81562527591097478 ) ) ;
#4385 = CARTESIAN_POINT ( 'NONE',  ( 108.9812119692459049, -46.95502683147942236, 82.72419670448194040 ) ) ;
#4386 = CARTESIAN_POINT ( 'NONE',  ( 104.4065072340926577, -46.45762169397040964, 252.3649774052962300 ) ) ;
#4387 = DIRECTION ( 'NONE',  ( 0.000000000000000000, 1.000000000000000000, 0.000000000000000000 ) ) ;
#4388 = LINE ( 'NONE', #3484, #79459 ) ;
#4389 = CARTESIAN_POINT ( 'NONE',  ( 117.8006386470660658, -34.09280371250640940, 160.0061014663869798 ) ) ;
#4390 = DIRECTION ( 'NONE',  ( 0.000000000000000000, 0.000000000000000000, 1.000000000000000000 ) ) ;
#4391 = VERTEX_POINT ( 'NONE', #67035 ) ;
#4392 = DIRECTION ( 'NONE',  ( 0.000000000000000000, 1.000000000000000000, 0.000000000000000000 ) ) ;
#4393 = VERTEX_POINT ( 'NONE', #80679 ) ;
#4394 = EDGE_LOOP ( 'NONE', ( #9420, #41528, #9038, #63812, #54045 ) ) ;
#4395 = DIRECTION ( 'NONE',  ( 1.000000000000000078E-15, 0.000000000000000000, -1.000000000000000000 ) ) ;
#4396 = LINE ( 'NONE', #89310, #30010 ) ;
#4398 = ORIENTED_EDGE ( 'NONE', *, *, #64525, .T. ) ;
#4397 = AXIS2_PLACEMENT_3D ( 'NONE', #18884, #77203, #891 ) ;
#4399 = DIRECTION ( 'NONE',  ( 0.000000000000000000, 1.000000000000000000, 0.000000000000000000 ) ) ;
#4400 = ORIENTED_EDGE ( 'NONE', *, *, #36676, .F. ) ;
#4401 = CARTESIAN_POINT ( 'NONE',  ( 111.8884855208196569, -27.93222315804501932, 130.6774218487876453 ) ) ;
#4402 = CARTESIAN_POINT ( 'NONE',  ( 107.6031522308233974, -26.28253885536559764, 95.03562527591097364 ) ) ;
#4403 = CARTESIAN_POINT ( 'NONE',  ( 103.7793689006360580, -43.80298085837112154, 0.4256252759109674932 ) ) ;
#4404 = B_SPLINE_CURVE_WITH_KNOTS ( 'NONE', 3,
 ( #4877, #17175, #31227, #44858, #38057, #32568, #59818, #58922, #45295, #25759, #73015, #73457, #10784, #59375, #38487, #66187, #52541, #3096 ),
 .UNSPECIFIED., .F., .F.,
 ( 4, 2, 2, 2, 2, 2, 2, 2, 4 ),
 ( 0.4999999996252184609, 0.5624999996720660977, 0.6249999997189138456, 0.6874999997657615936, 0.7499999998126092304, 0.8124999998594568673, 0.8749999999063046152, 0.9374999999531523631, 1.000000000000000000 ),
 .UNSPECIFIED. ) ;
#4405 = CARTESIAN_POINT ( 'NONE',  ( 132.3254539024480323, -42.97311385573998876, 207.5838068554170377 ) ) ;
#4406 = CYLINDRICAL_SURFACE ( 'NONE', #68755, 7.199999999999998401 ) ;
#4407 = CARTESIAN_POINT ( 'NONE',  ( 97.87212830949604836, -31.93334231290197067, 90.93181575210196854 ) ) ;
#4409 = CARTESIAN_POINT ( 'NONE',  ( 113.6005200848514107, -45.61596423689125146, 179.0689586092439640 ) ) ;
#4408 = CARTESIAN_POINT ( 'NONE',  ( 89.06648138392553449, -56.72944715994104570, -4.824374724089047106 ) ) ;
#4410 = LINE ( 'NONE', #86190, #87171 ) ;
#4411 = CARTESIAN_POINT ( 'NONE',  ( 51.27381068362094396, -23.19206098993945275, 342.9256252759109884 ) ) ;
#4412 = ORIENTED_EDGE ( 'NONE', *, *, #30964, .F. ) ;
#4413 = CARTESIAN_POINT ( 'NONE',  ( 51.06670390244799762, -33.35206098992630075, -5.074374724088000832 ) ) ;
#4414 = CIRCLE ( 'NONE', #65297, 29.00000000000000000 ) ;
#4415 = B_SPLINE_CURVE_WITH_KNOTS ( 'NONE', 3,
 ( #19740, #33815, #75610, #73809, #88798, #52865, #47424, #61065, #4772, #18847, #46968, #75151, #54673, #25203, #53781, #74263, #39284, #32456 ),
 .UNSPECIFIED., .F., .F.,
 ( 4, 2, 2, 2, 2, 2, 2, 2, 4 ),
 ( 0.000000000000000000, 0.06249238482208734763, 0.1249847696441746953, 0.1874771544662620359, 0.2499695392883493905, 0.3124619241104367173, 0.3749543089325240719, 0.4374466937546114265, 0.4999390785766987810 ),
 .UNSPECIFIED. ) ;
#4416 = DIRECTION ( 'NONE',  ( -1.000000000000000000, 6.036837696399408848E-13, 0.000000000000000000 ) ) ;
#4417 = AXIS2_PLACEMENT_3D ( 'NONE', #29238, #57367, #1976 ) ;
#4418 = CARTESIAN_POINT ( 'NONE',  ( -74.15067561874160162, 127.0000000000000000, -68.53801554307528932 ) ) ;
#4420 = EDGE_LOOP ( 'NONE', ( #18490, #13736, #2274, #22151 ) ) ;
#4419 = CARTESIAN_POINT ( 'NONE',  ( 103.2876017065440664, -26.96590681778891252, 215.3699109901969848 ) ) ;
#4421 = DIRECTION ( 'NONE',  ( 9.912705577010326536E-16, 1.000000000000000000, 0.000000000000000000 ) ) ;
#4422 = CARTESIAN_POINT ( 'NONE',  ( 96.54178838847580835, -40.18459672615917100, 282.5908633711491120 ) ) ;
#4423 = CARTESIAN_POINT ( 'NONE',  ( 114.8035609388329021, -44.68778416175712920, 114.2022919425779719 ) ) ;
#4424 = CARTESIAN_POINT ( 'NONE',  ( 172.5667039024480687, -42.82844715993500273, 300.4678068554149490 ) ) ;
#4425 = EDGE_CURVE ( 'NONE', #29546, #38331, #73848, .T. ) ;
#4426 = CARTESIAN_POINT ( 'NONE',  ( 11.00078833628932173, 88.90974477516434149, -130.0918550420129236 ) ) ;
#4427 = FACE_OUTER_BOUND ( 'NONE', #35154, .T. ) ;
#4428 = CARTESIAN_POINT ( 'NONE',  ( 57.14999999999999858, 95.25000000000000000, 304.0379999999999541 ) ) ;
#4429 = ORIENTED_EDGE ( 'NONE', *, *, #69265, .T. ) ;
#4430 = AXIS2_PLACEMENT_3D ( 'NONE', #64080, #9119, #949 ) ;
#4431 = ORIENTED_EDGE ( 'NONE', *, *, #31694, .F. ) ;
#4432 = ORIENTED_EDGE ( 'NONE', *, *, #58954, .T. ) ;
#4433 = ORIENTED_EDGE ( 'NONE', *, *, #63334, .F. ) ;
#4434 = LINE ( 'NONE', #80740, #50896 ) ;
#4435 = CARTESIAN_POINT ( 'NONE',  ( 105.0216744116726630, -25.86700170375123520, 276.2365776568634033 ) ) ;
#4436 = LINE ( 'NONE', #76035, #20054 ) ;
#4437 = CARTESIAN_POINT ( 'NONE',  ( 144.0769060499356726, -139.5326789363695070, 247.4193337233699879 ) ) ;
#4439 = CARTESIAN_POINT ( 'NONE',  ( 70.06670390834486284, -140.6784471658387758, 245.4415720115519832 ) ) ;
#4438 = DIRECTION ( 'NONE',  ( -4.299999999999999979E-14, 1.000000000000000000, -4.400000000000000367E-29 ) ) ;
#4440 = CARTESIAN_POINT ( 'NONE',  ( 104.2579841207466984, -28.11985932224000351, 209.7619436376009787 ) ) ;
#4441 = ORIENTED_EDGE ( 'NONE', *, *, #23065, .F. ) ;
#4442 = ORIENTED_EDGE ( 'NONE', *, *, #82573, .T. ) ;
#4443 = ORIENTED_EDGE ( 'NONE', *, *, #9309, .T. ) ;
#4444 = EDGE_CURVE ( 'NONE', #2908, #18234, #5259, .T. ) ;
#4445 = DIRECTION ( 'NONE',  ( 0.000000000000000000, 0.000000000000000000, -1.000000000000000000 ) ) ;
#4446 = B_SPLINE_CURVE_WITH_KNOTS ( 'NONE', 3,
 ( #23982, #71246, #85775, #29902, #29450, #51656, #2649, #58473, #64416, #23107, #36717, #57130, #42599, #8562, #30347, #15383, #70335, #71685 ),
 .UNSPECIFIED., .F., .F.,
 ( 4, 2, 2, 2, 2, 2, 2, 2, 4 ),
 ( 0.5000275190869877262, 0.5625240792011142466, 0.6250206393152407669, 0.6875171994293673983, 0.7500137595434939186, 0.8125103196576204390, 0.8750068797717469593, 0.9375034398858734797, 1.000000000000000000 ),
 .UNSPECIFIED. ) ;
#4447 = DIRECTION ( 'NONE',  ( -0.000000000000000000, -0.000000000000000000, -1.000000000000000000 ) ) ;
#4448 = DIRECTION ( 'NONE',  ( 0.000000000000000000, 0.000000000000000000, 1.000000000000000000 ) ) ;
#4449 = CARTESIAN_POINT ( 'NONE',  ( 114.6135591410776016, -41.37377328621888495, 14.81872616303997425 ) ) ;
#4450 = VECTOR ( 'NONE', #68836, 1000.000000000000000 ) ;
#4451 = CARTESIAN_POINT ( 'NONE',  ( 118.0074504647926688, 88.17653575778740560, 11.39323553397083444 ) ) ;
#4452 = CIRCLE ( 'NONE', #18971, 2.750000000000002665 ) ;
#4453 = DIRECTION ( 'NONE',  ( 0.000000000000000000, 0.000000000000000000, 1.000000000000000000 ) ) ;
#4454 = CARTESIAN_POINT ( 'NONE',  ( 109.7813264909552515, -47.51098736074730766, 242.7727681330539724 ) ) ;
#4455 = CARTESIAN_POINT ( 'NONE',  ( 107.0667039024470313, -104.2784471599408676, 19.21780685541799016 ) ) ;
#4456 = VERTEX_POINT ( 'NONE', #74308 ) ;
#4457 = DIRECTION ( 'NONE',  ( -0.7071067811865692221, -0.7071067811865259234, -7.071067811865685367E-16 ) ) ;
#4458 = AXIS2_PLACEMENT_3D ( 'NONE', #38524, #25342, #5361 ) ;
#4459 = PLANE ( 'NONE',  #6046 ) ;
#4460 = CARTESIAN_POINT ( 'NONE',  ( 100.9805754248354788, -42.21072563198327998, 54.72809036959092310 ) ) ;
#4461 = CARTESIAN_POINT ( 'NONE',  ( 136.5173892390865831, -17.48112160758304867, 7.135585143028393418 ) ) ;
#4462 = CARTESIAN_POINT ( 'NONE',  ( 182.2420472961719895, -31.76306994223730840, -5.074374724088000832 ) ) ;
#4463 = EDGE_CURVE ( 'NONE', #1539, #26346, #26878, .T. ) ;
#4464 = CARTESIAN_POINT ( 'NONE',  ( -5.634993000313458289, 93.96183429002098819, 118.4245090560989837 ) ) ;
#4465 = ORIENTED_EDGE ( 'NONE', *, *, #80244, .T. ) ;
#4466 = DIRECTION ( 'NONE',  ( -0.000000000000000000, -1.000000000000000000, 0.000000000000000000 ) ) ;
#4467 = DIRECTION ( 'NONE',  ( -1.000000000000000000, -4.299999999999999979E-14, -1.000000000000000078E-15 ) ) ;
#4468 = EDGE_CURVE ( 'NONE', #87925, #48525, #81139, .T. ) ;
#4469 = ORIENTED_EDGE ( 'NONE', *, *, #25900, .F. ) ;
#4470 = CARTESIAN_POINT ( 'NONE',  ( 101.7558625676976618, -27.03530485730228250, 100.4632443235299633 ) ) ;
#4471 = ORIENTED_EDGE ( 'NONE', *, *, #81841, .T. ) ;
#4472 = ADVANCED_FACE ( 'NONE', ( #18432 ), #25697, .T. ) ;
#4473 = CARTESIAN_POINT ( 'NONE',  ( 115.2492312947614437, -32.84933048162275071, 63.61337220902895950 ) ) ;
#4474 = VECTOR ( 'NONE', #75714, 1000.000000000000000 ) ;
#4475 = CARTESIAN_POINT ( 'NONE',  ( 116.8171228655006075, -34.15291831812996293, 70.03145860946138157 ) ) ;
#4476 = CARTESIAN_POINT ( 'NONE',  ( 116.3507336416864746, -38.17139756410392692, 65.12348806780198629 ) ) ;
#4477 = EDGE_CURVE ( 'NONE', #29470, #28274, #76239, .T. ) ;
#4478 = DIRECTION ( 'NONE',  ( 1.000000000000000000, 1.000000000000000078E-15, 0.000000000000000000 ) ) ;
#4479 = CARTESIAN_POINT ( 'NONE',  ( 125.5177273812784762, -137.6784471599409301, 222.2178068554179902 ) ) ;
#4480 = CARTESIAN_POINT ( 'NONE',  ( 118.0985323217624057, -37.71894194680212564, 29.74324432352998215 ) ) ;
#4481 = VECTOR ( 'NONE', #89437, 1000.000000000000000 ) ;
#4482 = CARTESIAN_POINT ( 'NONE',  ( 130.5667039024481255, -40.02944715994100022, 239.5838068554162987 ) ) ;
#4483 = ORIENTED_EDGE ( 'NONE', *, *, #77723, .F. ) ;
#4484 = DIRECTION ( 'NONE',  ( -4.093947403305260305E-16, 1.000000000000000000, -6.162975822039159109E-32 ) ) ;
#4485 = ORIENTED_EDGE ( 'NONE', *, *, #24366, .F. ) ;
#4486 = CARTESIAN_POINT ( 'NONE',  ( 77.71552635665730691, -20.16021090639628710, 2.608895778936489940 ) ) ;
#4487 = ORIENTED_EDGE ( 'NONE', *, *, #59743, .F. ) ;
#4488 = ORIENTED_EDGE ( 'NONE', *, *, #36368, .F. ) ;
#4489 = EDGE_CURVE ( 'NONE', #56634, #71751, #79798, .T. ) ;
#4490 = VECTOR ( 'NONE', #50742, 1000.000000000000000 ) ;
#4491 = CARTESIAN_POINT ( 'NONE',  ( 173.9900000000000091, 101.5999999999999943, 71.37400000000000944 ) ) ;
#4492 = ORIENTED_EDGE ( 'NONE', *, *, #62549, .T. ) ;
#4493 = CARTESIAN_POINT ( 'NONE',  ( 110.0587659310071729, -27.38278898179161658, 234.8299109901969643 ) ) ;
#4494 = CARTESIAN_POINT ( 'NONE',  ( 97.80136889829883273, -40.49211973435467371, 126.6329963442747442 ) ) ;
#4495 = CARTESIAN_POINT ( 'NONE',  ( 98.30753412580686756, -41.72887537901419108, 187.7397919323684334 ) ) ;
#4496 = CARTESIAN_POINT ( 'NONE',  ( 116.2315886754559386, -31.76121500512346074, 65.22133956162595325 ) ) ;
#4497 = AXIS2_PLACEMENT_3D ( 'NONE', #52951, #65293, #23965 ) ;
#4498 = DIRECTION ( 'NONE',  ( -3.100000000000000258E-29, 3.100000000000000044E-14, 1.000000000000000000 ) ) ;
#4499 = VERTEX_POINT ( 'NONE', #17553 ) ;
#4500 = CARTESIAN_POINT ( 'NONE',  ( 109.7248998095299868, -27.00080582534542017, 114.8665783998315533 ) ) ;
#4501 = DIRECTION ( 'NONE',  ( 0.000000000000000000, -1.000000000000000000, 0.000000000000000000 ) ) ;
#4502 = EDGE_LOOP ( 'NONE', ( #18058, #89019, #52076, #26220 ) ) ;
#4503 = DIRECTION ( 'NONE',  ( -2.900000000000000265E-14, 2.000000000000000155E-15, -1.000000000000000000 ) ) ;
#4504 = CARTESIAN_POINT ( 'NONE',  ( 98.30746919718092158, -41.72870820425139726, 112.7403801342047416 ) ) ;
#4505 = CARTESIAN_POINT ( 'NONE',  ( 118.0279888096068390, -35.50094427011355691, 233.9032443235299752 ) ) ;
#4506 = DIRECTION ( 'NONE',  ( 0.000000000000000000, -1.000000000000000000, 0.000000000000000000 ) ) ;
#4507 = LINE ( 'NONE', #32196, #82601 ) ;
#4508 = CARTESIAN_POINT ( 'NONE',  ( 79.11888855178027313, -39.31186128672827351, 1.764000668897422130 ) ) ;
#4509 = AXIS2_PLACEMENT_3D ( 'NONE', #33754, #28266, #13318 ) ;
#4510 = CARTESIAN_POINT ( 'NONE',  ( 111.5095219758393483, -44.62071306430618023, 257.4190864947434534 ) ) ;
#4512 = CARTESIAN_POINT ( 'NONE',  ( 99.51750086509218818, -43.88776608678588786, 77.92991099019597812 ) ) ;
#4511 = CARTESIAN_POINT ( 'NONE',  ( 182.3467384525657167, -29.62846900981657683, 193.9678068554150059 ) ) ;
#4513 = CARTESIAN_POINT ( 'NONE',  ( 122.0810025972884034, 74.11507855671040090, 46.27428068823228813 ) ) ;
#4514 = CARTESIAN_POINT ( 'NONE',  ( 117.7240352459720043, -39.83258586197658246, 138.5889586092439743 ) ) ;
#4515 = ORIENTED_EDGE ( 'NONE', *, *, #27620, .F. ) ;
#4516 = CARTESIAN_POINT ( 'NONE',  ( 132.3477924061144222, -20.87777042261643601, 7.743969477060447026 ) ) ;
#4517 = VERTEX_POINT ( 'NONE', #32501 ) ;
#4518 = DIRECTION ( 'NONE',  ( -0.000000000000000000, -1.000000000000000000, -0.000000000000000000 ) ) ;
#4519 = CIRCLE ( 'NONE', #53815, 4.750000000000004441 ) ;
#4520 = CARTESIAN_POINT ( 'NONE',  ( 122.2189888861420286, -111.9861225405540353, -19.18411693322877198 ) ) ;
#4521 = DIRECTION ( 'NONE',  ( 0.000000000000000000, 0.000000000000000000, -1.000000000000000000 ) ) ;
#4522 = ORIENTED_EDGE ( 'NONE', *, *, #26681, .T. ) ;
#4523 = LINE ( 'NONE', #45386, #1215 ) ;
#4525 = ORIENTED_EDGE ( 'NONE', *, *, #43523, .F. ) ;
#4524 = CARTESIAN_POINT ( 'NONE',  ( 108.9929891821633134, -47.66111943275755181, 122.7032443235299723 ) ) ;
#4526 = DIRECTION ( 'NONE',  ( 0.000000000000000000, 1.000000000000000000, 0.000000000000000000 ) ) ;
#4527 = CARTESIAN_POINT ( 'NONE',  ( -129.9368274816650626, 82.96445444011519044, -12.70000000000045404 ) ) ;
#4528 = ADVANCED_FACE ( 'NONE', ( #3916, #60197 ), #73397, .T. ) ;
#4529 = DIRECTION ( 'NONE',  ( 0.000000000000000000, 0.000000000000000000, -1.000000000000000000 ) ) ;
#4530 = VERTEX_POINT ( 'NONE', #72952 ) ;
#4531 = AXIS2_PLACEMENT_3D ( 'NONE', #49039, #35424, #76772 ) ;
#4532 = CARTESIAN_POINT ( 'NONE',  ( 109.0765542020472907, -47.62233732142709641, 127.7337205140059382 ) ) ;
#4533 = SHAPE_DEFINITION_REPRESENTATION ( #67029, #19449 ) ;
#4534 = EDGE_CURVE ( 'NONE', #66251, #28958, #10722, .T. ) ;
#4535 = CARTESIAN_POINT ( 'NONE',  ( 31.89136050872173911, -31.76306994223854119, 117.4678068554150485 ) ) ;
#4536 = DIRECTION ( 'NONE',  ( 0.000000000000000000, 0.000000000000000000, 1.000000000000000000 ) ) ;
#4537 = ORIENTED_EDGE ( 'NONE', *, *, #34187, .F. ) ;
#4538 = ORIENTED_EDGE ( 'NONE', *, *, #17583, .T. ) ;
#4539 = CARTESIAN_POINT ( 'NONE',  ( 41.56648329127399677, 0.2215528400590013880, 21.04262527591200183 ) ) ;
#4540 = B_SPLINE_SURFACE_WITH_KNOTS ( 'NONE', 3, 3, ( 
 ( #64494, #2270, #29525, #9526 ),
 ( #84952, #37228, #16342, #70415 ),
 ( #57208, #9975, #77229, #16787 ),
 ( #37680, #64933, #43578, #29972 ),
 ( #42675, #58546, #30858, #58114 ) ),
 .UNSPECIFIED., .F., .F., .F.,
 ( 4, 1, 4 ),
 ( 4, 4 ),
 ( 0.000000000000000000, 0.5714285714285709528, 1.000000000000000000 ),
 ( 4.195560071017320097E-05, 0.2154603786882610117 ),
 .UNSPECIFIED. ) ;
#4541 = CARTESIAN_POINT ( 'NONE',  ( 63.03715912545825262, -46.82818131006018092, 249.9678068554150343 ) ) ;
#4542 = CARTESIAN_POINT ( 'NONE',  ( 112.0659115677942310, -45.48839629263709128, 157.9897919375864603 ) ) ;
#4543 = CARTESIAN_POINT ( 'NONE',  ( -7.205548786489490269E-13, 117.4749999999999943, 103.1875000000000000 ) ) ;
#4544 = AXIS2_PLACEMENT_3D ( 'NONE', #29708, #2003, #57399 ) ;
#4546 = CARTESIAN_POINT ( 'NONE',  ( -9.275582543403935176, 73.86526018886296185, -118.1929554227103267 ) ) ;
#4545 = CARTESIAN_POINT ( 'NONE',  ( 104.4897549782674417, -26.97886241702974885, 105.2814749527903615 ) ) ;
#4547 = FACE_OUTER_BOUND ( 'NONE', #43550, .T. ) ;
#4548 = AXIS2_PLACEMENT_3D ( 'NONE', #56114, #28896, #21642 ) ;
#4549 = ORIENTED_EDGE ( 'NONE', *, *, #3250, .T. ) ;
#4550 = EDGE_CURVE ( 'NONE', #79544, #60263, #66127, .T. ) ;
#4551 = DIRECTION ( 'NONE',  ( -1.000000000000000000, 9.376883653928684652E-16, 1.500301384628589584E-15 ) ) ;
#4552 = CARTESIAN_POINT ( 'NONE',  ( 111.8874393434637682, -45.23954810143637673, 208.9870538473389558 ) ) ;
#4553 = VECTOR ( 'NONE', #7313, 1000.000000000000000 ) ;
#4555 = ORIENTED_EDGE ( 'NONE', *, *, #88789, .F. ) ;
#4554 = DIRECTION ( 'NONE',  ( -1.000000000000000000, 0.000000000000000000, 0.000000000000000000 ) ) ;
#4556 = CARTESIAN_POINT ( 'NONE',  ( 115.6651410650258214, -32.06827565682262815, 65.22133956162495849 ) ) ;
#4557 = CARTESIAN_POINT ( 'NONE',  ( 117.0519585894030001, -35.94438672013124858, 53.88895366790352881 ) ) ;
#4558 = DIRECTION ( 'NONE',  ( -3.100000000000000258E-29, 3.100000000000000044E-14, 1.000000000000000000 ) ) ;
#4559 = AXIS2_PLACEMENT_3D ( 'NONE', #7540, #41585, #77475 ) ;
#4560 = DIRECTION ( 'NONE',  ( 1.000000000000000000, -1.709087168450053042E-15, 0.000000000000000000 ) ) ;
#4561 = ADVANCED_FACE ( 'NONE', ( #31612 ), #52477, .T. ) ;
#4562 = ORIENTED_EDGE ( 'NONE', *, *, #34291, .F. ) ;
#4563 = PLANE ( 'NONE',  #15329 ) ;
#4564 = ORIENTED_EDGE ( 'NONE', *, *, #88178, .F. ) ;
#4565 = ORIENTED_EDGE ( 'NONE', *, *, #73775, .F. ) ;
#4566 = CARTESIAN_POINT ( 'NONE',  ( 98.23953817868523686, -35.94630056370082372, 227.6872975916109567 ) ) ;
#4567 =( REPRESENTATION_RELATIONSHIP ('NONE','NONE', #82876, #885 ) REPRESENTATION_RELATIONSHIP_WITH_TRANSFORMATION ( #28089 )SHAPE_REPRESENTATION_RELATIONSHIP( ) );
#4568 = DIRECTION ( 'NONE',  ( 0.000000000000000000, 0.000000000000000000, 1.000000000000000000 ) ) ;
#4569 = CARTESIAN_POINT ( 'NONE',  ( -82.89895571708294142, 83.38918798244689867, 100.8594679592209502 ) ) ;
#4570 = CARTESIAN_POINT ( 'NONE',  ( 115.7831076496464249, -41.80230954688622091, 154.4064586059346595 ) ) ;
#4571 = DIRECTION ( 'NONE',  ( 0.000000000000000000, 0.000000000000000000, -1.000000000000000000 ) ) ;
#4573 = VERTEX_POINT ( 'NONE', #38874 ) ;
#4572 = VECTOR ( 'NONE', #22994, 1000.000000000000000 ) ;
#4574 = FACE_OUTER_BOUND ( 'NONE', #30067, .T. ) ;
#4575 = FACE_OUTER_BOUND ( 'NONE', #80124, .T. ) ;
#4576 = ORIENTED_EDGE ( 'NONE', *, *, #69295, .F. ) ;
#4577 = CARTESIAN_POINT ( 'NONE',  ( 96.34404753607181249, -39.41381804822120216, 16.53372051400597798 ) ) ;
#4578 = ORIENTED_EDGE ( 'NONE', *, *, #49606, .F. ) ;
#4580 = EDGE_LOOP ( 'NONE', ( #33206, #53501, #39020, #4323, #51486, #11776 ) ) ;
#4579 = EDGE_CURVE ( 'NONE', #82504, #43699, #67548, .T. ) ;
#4581 = CARTESIAN_POINT ( 'NONE',  ( 106.8863607564096725, -44.89016293055450291, 270.3766617981627860 ) ) ;
#4582 = CARTESIAN_POINT ( 'NONE',  ( 31.56670390244800828, -33.35206098992711077, 342.9256252759119548 ) ) ;
#4583 = CARTESIAN_POINT ( 'NONE',  ( 23.22033092422023159, 78.41772510193747792, 300.5067426286719297 ) ) ;
#4584 = CARTESIAN_POINT ( 'NONE',  ( 20.03715912545739997, -46.82818131006202123, 129.9678068554150627 ) ) ;
#4585 = DIRECTION ( 'NONE',  ( -0.7071067811578587436, 0.7071067812152364018, 0.000000000000000000 ) ) ;
#4586 = CONICAL_SURFACE ( 'NONE', #43737, 188.9759999999999991, 0.7853981633974758125 ) ;
#4587 = CARTESIAN_POINT ( 'NONE',  ( 117.2394727393827765, -34.25896837304814113, 205.0156252759109634 ) ) ;
#4588 = CARTESIAN_POINT ( 'NONE',  ( 24.79284581386643893, 184.0000000000000000, 106.1020876358972629 ) ) ;
#4589 = VERTEX_POINT ( 'NONE', #36947 ) ;
#4590 = VECTOR ( 'NONE', #84397, 1000.000000000000000 ) ;
#4591 = CARTESIAN_POINT ( 'NONE',  ( 106.8402480490632342, -48.62734320582506342, 73.56133956162497611 ) ) ;
#4592 = CARTESIAN_POINT ( 'NONE',  ( 32.25690895537100289, -33.54226604285010893, -5.074374724088000832 ) ) ;
#4593 = ORIENTED_EDGE ( 'NONE', *, *, #1423, .F. ) ;
#4594 = ORIENTED_EDGE ( 'NONE', *, *, #37798, .F. ) ;
#4595 = EDGE_LOOP ( 'NONE', ( #78765, #27282, #59296, #21833 ) ) ;
#4596 = ADVANCED_FACE ( 'NONE', ( #31457 ), #57834, .T. ) ;
#4597 = CARTESIAN_POINT ( 'NONE',  ( -68.53801554307339927, 120.6499999999999915, -74.15067561874339219 ) ) ;
#4599 = EDGE_CURVE ( 'NONE', #70197, #22586, #3768, .T. ) ;
#4598 = DIRECTION ( 'NONE',  ( 0.000000000000000000, 1.000000000000000000, 0.000000000000000000 ) ) ;
#4600 = CYLINDRICAL_SURFACE ( 'NONE', #42180, 2.116999999999980009 ) ;
#4601 = CARTESIAN_POINT ( 'NONE',  ( 103.3362113047044772, -29.43782462767379116, 118.2709475124489842 ) ) ;
#4602 = CARTESIAN_POINT ( 'NONE',  ( 97.14909927861904748, -40.01315743934404878, 237.5813395616249579 ) ) ;
#4603 = VECTOR ( 'NONE', #73253, 1000.000000000000000 ) ;
#4604 = CARTESIAN_POINT ( 'NONE',  ( -487.2989999999999782, 100.8062500000000057, 86.36305401447658880 ) ) ;
#4605 = ORIENTED_EDGE ( 'NONE', *, *, #46308, .F. ) ;
#4606 = FACE_OUTER_BOUND ( 'NONE', #12495, .T. ) ;
#4607 = ORIENTED_EDGE ( 'NONE', *, *, #23186, .F. ) ;
#4609 = EDGE_LOOP ( 'NONE', ( #82337, #46693, #74543, #83845 ) ) ;
#4608 = AXIS2_PLACEMENT_3D ( 'NONE', #71908, #72353, #9666 ) ;
#4610 = CARTESIAN_POINT ( 'NONE',  ( 107.0664832912739541, -36.72944715994095333, 305.7008218191032256 ) ) ;
#4611 = VERTEX_POINT ( 'NONE', #71043 ) ;
#4612 = VERTEX_POINT ( 'NONE', #86890 ) ;
#4613 = CARTESIAN_POINT ( 'NONE',  ( 20.03715912545733602, -46.82818131006202123, 193.9678068554150627 ) ) ;
#4614 = DIRECTION ( 'NONE',  ( 0.7071067811865473507, 0.000000000000000000, -0.7071067811865476838 ) ) ;
#4615 = CARTESIAN_POINT ( 'NONE',  ( 97.06112373929039450, -37.99668619498721256, 26.42731374779140197 ) ) ;
#4616 = CARTESIAN_POINT ( 'NONE',  ( 99.64399296875224366, -31.54106566633107533, 160.2514674471249521 ) ) ;
#4617 = AXIS2_PLACEMENT_3D ( 'NONE', #51747, #55317, #83073 ) ;
#4618 = CARTESIAN_POINT ( 'NONE',  ( 105.1555015486555078, -47.05240725173535310, 12.42991099019596923 ) ) ;
#4619 = DIRECTION ( 'NONE',  ( 0.000000000000000000, 0.000000000000000000, -1.000000000000000000 ) ) ;
#4620 = ORIENTED_EDGE ( 'NONE', *, *, #46310, .T. ) ;
#4621 = CARTESIAN_POINT ( 'NONE',  ( -92.32962665258507684, 82.54999999999999716, -74.36911441044765070 ) ) ;
#4622 = AXIS2_PLACEMENT_3D ( 'NONE', #87415, #16593, #72009 ) ;
#4623 = EDGE_LOOP ( 'NONE', ( #58418, #31773 ) ) ;
#4624 = CARTESIAN_POINT ( 'NONE',  ( 131.0667039024480118, -58.35344715994099829, 231.5838068554150198 ) ) ;
#4625 = ORIENTED_EDGE ( 'NONE', *, *, #59195, .F. ) ;
#4626 = CARTESIAN_POINT ( 'NONE',  ( 99.16350003447738004, -30.55523068857526070, 166.7982118921487142 ) ) ;
#4627 = CARTESIAN_POINT ( 'NONE',  ( 83.34564128298197261, -139.5081389887196792, 247.5112265945679724 ) ) ;
#4628 = CARTESIAN_POINT ( 'NONE',  ( 99.08970013401406618, -42.79568349143557526, 131.8439815248826221 ) ) ;
#4629 = DIRECTION ( 'NONE',  ( -0.000000000000000000, -0.000000000000000000, -1.000000000000000000 ) ) ;
#4630 = ORIENTED_EDGE ( 'NONE', *, *, #42086, .T. ) ;
#4631 = CARTESIAN_POINT ( 'NONE',  ( 96.66715014961923202, -32.91509328854561289, 21.03467289495897319 ) ) ;
#4632 = CARTESIAN_POINT ( 'NONE',  ( 109.6537587170975030, -46.87336088289573865, 43.77562527591094721 ) ) ;
#4635 = EDGE_CURVE ( 'NONE', #11339, #44492, #58712, .T. ) ;
#4634 = FACE_OUTER_BOUND ( 'NONE', #56633, .T. ) ;
#4633 = CARTESIAN_POINT ( 'NONE',  ( -487.2989999999999782, 97.78694598552370110, 18.25625000000050235 ) ) ;
#4636 = CARTESIAN_POINT ( 'NONE',  ( 104.4899661847896368, -26.97880442220879260, 146.2818772940478596 ) ) ;
#4637 = CARTESIAN_POINT ( 'NONE',  ( 106.6019379103756535, -25.27972995136449441, 322.9014499992877631 ) ) ;
#4638 = CARTESIAN_POINT ( 'NONE',  ( -3.968750000000754508, 120.6499999999999915, 100.8961411191535973 ) ) ;
#4639 = CARTESIAN_POINT ( 'NONE',  ( 85.24325998657072034, -58.55267046464445002, 14.67562527591094756 ) ) ;
#4640 = CARTESIAN_POINT ( 'NONE',  ( 72.96458098368701428, 117.4749999999999943, -72.96458098368670164 ) ) ;
#4641 = ORIENTED_EDGE ( 'NONE', *, *, #33159, .F. ) ;
#4642 = CARTESIAN_POINT ( 'NONE',  ( 99.95068698205643898, -44.40877713917536340, 46.98133956162592284 ) ) ;
#4643 = CARTESIAN_POINT ( 'NONE',  ( 103.7231914492017637, -26.19396519929847145, 201.3089586092439731 ) ) ;
#4644 = CARTESIAN_POINT ( 'NONE',  ( 112.7717388973142647, -27.93574178168534061, 65.61848241876793963 ) ) ;
#4645 = CIRCLE ( 'NONE', #55385, 4.762500000000000178 ) ;
#4647 = CARTESIAN_POINT ( 'NONE',  ( 149.4409906032288973, -0.9156555935619370423, 394.9756252759100903 ) ) ;
#4646 = FACE_OUTER_BOUND ( 'NONE', #63564, .T. ) ;
#4648 = FACE_OUTER_BOUND ( 'NONE', #61663, .T. ) ;
#4649 = VECTOR ( 'NONE', #45141, 1000.000000000000000 ) ;
#4650 = EDGE_CURVE ( 'NONE', #68005, #70474, #37848, .T. ) ;
#4651 = ORIENTED_EDGE ( 'NONE', *, *, #30926, .F. ) ;
#4652 = DIRECTION ( 'NONE',  ( 0.000000000000000000, 0.000000000000000000, -1.000000000000000000 ) ) ;
#4653 = ORIENTED_EDGE ( 'NONE', *, *, #60973, .F. ) ;
#4654 = CARTESIAN_POINT ( 'NONE',  ( 97.42673588038243793, -38.38435052442952866, 87.46133956162493917 ) ) ;
#4655 = EDGE_CURVE ( 'NONE', #9197, #63483, #24655, .T. ) ;
#4657 = EDGE_LOOP ( 'NONE', ( #47184, #42725, #74552, #10877 ) ) ;
#4656 = CARTESIAN_POINT ( 'NONE',  ( 7.043515244065597258, 93.11782407023925145, 130.3658622353028136 ) ) ;
#4658 = CARTESIAN_POINT ( 'NONE',  ( 107.5091008941355994, -47.12332782054429714, 233.6099109901969655 ) ) ;
#4659 = DIRECTION ( 'NONE',  ( -4.237773401492740281E-14, 1.000000000000000000, 0.000000000000000000 ) ) ;
#4660 = CARTESIAN_POINT ( 'NONE',  ( 80.06648329127399677, -8.729447159940999512, 4.925625275911999168 ) ) ;
#4661 = DIRECTION ( 'NONE',  ( -1.000000000000000078E-15, 1.000000000000000000, 0.000000000000000000 ) ) ;
#4662 = CARTESIAN_POINT ( 'NONE',  ( 115.0889047255370770, -30.61763668237492908, 80.34395860901999242 ) ) ;
#4663 = EDGE_CURVE ( 'NONE', #18701, #8408, #30583, .T. ) ;
#4664 = AXIS2_PLACEMENT_3D ( 'NONE', #75186, #6153, #39312 ) ;
#4665 = EDGE_CURVE ( 'NONE', #20875, #15623, #55915, .T. ) ;
#4666 = DIRECTION ( 'NONE',  ( 0.000000000000000000, -1.000000000000000000, 0.000000000000000000 ) ) ;
#4667 = CARTESIAN_POINT ( 'NONE',  ( 37.56670390244833158, -48.82844715994119866, 249.9678068554150343 ) ) ;
#4668 = CARTESIAN_POINT ( 'NONE',  ( 116.7860849611261500, -31.33117650353035799, 179.2299109901969700 ) ) ;
#4669 = EDGE_LOOP ( 'NONE', ( #51025, #88414, #58517, #70659 ) ) ;
#4670 = ORIENTED_EDGE ( 'NONE', *, *, #13499, .F. ) ;
#4671 = VECTOR ( 'NONE', #61175, 1000.000000000000000 ) ;
#4672 = EDGE_CURVE ( 'NONE', #85158, #68630, #2884, .T. ) ;
#4673 = CARTESIAN_POINT ( 'NONE',  ( 116.0040243724562146, -33.83170925634997417, 130.5196785439929670 ) ) ;
#4674 = VECTOR ( 'NONE', #66600, 1000.000000000000000 ) ;
#4675 = DIRECTION ( 'NONE',  ( -0.8660254037844382635, -0.5000000000000008882, 1.550000000000000022E-14 ) ) ;
#4677 = DIRECTION ( 'NONE',  ( -5.551115123125777653E-14, -1.000000000000000000, 0.000000000000000000 ) ) ;
#4676 = CARTESIAN_POINT ( 'NONE',  ( 115.3604274781776411, -30.50455558986046256, 260.3508633711485345 ) ) ;
#4678 = CARTESIAN_POINT ( 'NONE',  ( 179.4595971212889935, -28.98061976758940617, -5.074374724088000832 ) ) ;
#4679 = ADVANCED_FACE ( 'NONE', ( #51885 ), #37398, .T. ) ;
#4680 = CARTESIAN_POINT ( 'NONE',  ( 51.06648329127400388, -18.82844715994099971, 333.4006252759120343 ) ) ;
#4681 = VECTOR ( 'NONE', #26631, 1000.000000000000000 ) ;
#4682 = CARTESIAN_POINT ( 'NONE',  ( 118.2371168503541838, 73.28361289573329884, 8.694557611693589649 ) ) ;
#4683 = DIRECTION ( 'NONE',  ( -0.9254794337955620787, -0.3787978585227822492, 0.000000000000000000 ) ) ;
#4684 = DIRECTION ( 'NONE',  ( 0.000000000000000000, 0.000000000000000000, -1.000000000000000000 ) ) ;
#4685 = DIRECTION ( 'NONE',  ( 0.000000000000000000, 0.000000000000000000, 1.000000000000000000 ) ) ;
#4686 = CARTESIAN_POINT ( 'NONE',  ( 117.1710321396411416, -41.15233254730030410, 208.4861014663869696 ) ) ;
#4687 = ORIENTED_EDGE ( 'NONE', *, *, #4920, .F. ) ;
#4688 = VECTOR ( 'NONE', #77267, 1000.000000000000000 ) ;
#4690 = ORIENTED_EDGE ( 'NONE', *, *, #46902, .T. ) ;
#4689 = EDGE_CURVE ( 'NONE', #65816, #49816, #85505, .T. ) ;
#4691 = CARTESIAN_POINT ( 'NONE',  ( -97.63922045723913357, 72.45841406287408404, -86.67141577317428869 ) ) ;
#4692 = LINE ( 'NONE', #60525, #5547 ) ;
#4693 = CARTESIAN_POINT ( 'NONE',  ( 108.4182250531618763, -26.73512938305734110, 184.9693472879707201 ) ) ;
#4694 = DIRECTION ( 'NONE',  ( 0.000000000000000000, 1.000000000000000000, 0.000000000000000000 ) ) ;
#4695 = CARTESIAN_POINT ( 'NONE',  ( 115.8229818292872295, -31.72577650744706901, 94.24017908913180008 ) ) ;
#4696 = ORIENTED_EDGE ( 'NONE', *, *, #70237, .F. ) ;
#4697 = PLANE ( 'NONE',  #3032 ) ;
#4698 = CARTESIAN_POINT ( 'NONE',  ( 97.05801352979682406, -41.42088835504144839, 211.6632443235299945 ) ) ;
#4699 = LINE ( 'NONE', #80121, #3833 ) ;
#4700 = ORIENTED_EDGE ( 'NONE', *, *, #62567, .T. ) ;
#4701 = VERTEX_POINT ( 'NONE', #59600 ) ;
#4702 = ADVANCED_FACE ( 'NONE', ( #39613 ), #33259, .F. ) ;
#4703 = VECTOR ( 'NONE', #56703, 1000.000000000000000 ) ;
#4704 = CARTESIAN_POINT ( 'NONE',  ( 108.8069666745183639, -46.61095096727596143, 63.71573676758425364 ) ) ;
#4706 = ADVANCED_FACE ( 'NONE', ( #33709 ), #32345, .T. ) ;
#4705 = CARTESIAN_POINT ( 'NONE',  ( -15.88716625750469902, 91.07499999999996021, -53.54073290201169044 ) ) ;
#4707 = CARTESIAN_POINT ( 'NONE',  ( 98.04152846853264691, -41.04187693203201093, 166.6812038652217041 ) ) ;
#4708 = EDGE_CURVE ( 'NONE', #70, #58818, #82663, .T. ) ;
#4709 = CARTESIAN_POINT ( 'NONE',  ( 105.7780793485435851, -44.78982812472496988, 35.26809036959094357 ) ) ;
#4710 = CARTESIAN_POINT ( 'NONE',  ( 117.2433672581536968, -42.84935593481555571, 124.3956252759109731 ) ) ;
#4711 = CARTESIAN_POINT ( 'NONE',  ( 147.4575741623270062, 101.5999999999999943, -135.2444258376734183 ) ) ;
#4712 = ORIENTED_EDGE ( 'NONE', *, *, #13239, .F. ) ;
#4713 = EDGE_CURVE ( 'NONE', #40161, #80487, #36214, .T. ) ;
#4714 = CARTESIAN_POINT ( 'NONE',  ( 49.21213752016101495, -29.73316016639650172, 313.9678068554150059 ) ) ;
#4715 = CARTESIAN_POINT ( 'NONE',  ( 97.95250717983365973, -32.49412669507731266, 25.56312527591095929 ) ) ;
#4716 = ORIENTED_EDGE ( 'NONE', *, *, #41987, .F. ) ;
#4717 = ORIENTED_EDGE ( 'NONE', *, *, #71378, .T. ) ;
#4718 = VECTOR ( 'NONE', #60646, 1000.000000000000000 ) ;
#4719 = CARTESIAN_POINT ( 'NONE',  ( -57.91199999999999903, 20.32000000000000028, 178.6098374884404905 ) ) ;
#4720 = EDGE_LOOP ( 'NONE', ( #2642, #2588, #42246, #5622 ) ) ;
#4721 = ORIENTED_EDGE ( 'NONE', *, *, #7417, .T. ) ;
#4722 = CYLINDRICAL_SURFACE ( 'NONE', #51592, 7.937500000000000000 ) ;
#4723 = CARTESIAN_POINT ( 'NONE',  ( 104.1257281832662613, -27.47619977921510781, 54.74384839950496939 ) ) ;
#4724 = CARTESIAN_POINT ( 'NONE',  ( 110.1440020323170330, -26.08875547494869451, 214.8403871806729342 ) ) ;
#4725 = CARTESIAN_POINT ( 'NONE',  ( 112.7681627534586681, -45.43114336468926950, 178.0384824187679556 ) ) ;
#4727 = CARTESIAN_POINT ( 'NONE',  ( 100.5643946202652756, -27.81952766013699119, 26.56610146638793779 ) ) ;
#4726 = CARTESIAN_POINT ( 'NONE',  ( 97.81938603920509934, -40.53623202280513738, 21.63691838182942107 ) ) ;
#4728 = DIRECTION ( 'NONE',  ( 0.000000000000000000, -1.000000000000000000, 0.000000000000000000 ) ) ;
#4729 = PLANE ( 'NONE',  #67107 ) ;
#4730 = VERTEX_POINT ( 'NONE', #60499 ) ;
#4731 = VECTOR ( 'NONE', #76980, 1000.000000000000000 ) ;
#4732 = ORIENTED_EDGE ( 'NONE', *, *, #77938, .T. ) ;
#4733 = AXIS2_PLACEMENT_3D ( 'NONE', #50180, #43366, #16579 ) ;
#4734 = DIRECTION ( 'NONE',  ( -0.000000000000000000, -0.000000000000000000, -1.000000000000000000 ) ) ;
#4735 = CARTESIAN_POINT ( 'NONE',  ( 110.1504846022309607, -26.06634163003500859, 214.8403871806729342 ) ) ;
#4736 = ORIENTED_EDGE ( 'NONE', *, *, #73574, .F. ) ;
#4737 = CARTESIAN_POINT ( 'NONE',  ( 113.7507820938996872, -44.72989589602062210, 193.1299109901969757 ) ) ;
#4738 = DIRECTION ( 'NONE',  ( 0.000000000000000000, 0.000000000000000000, -1.000000000000000000 ) ) ;
#4739 = DIRECTION ( 'NONE',  ( 1.000000000000000078E-15, 1.000000000000000083E-30, -1.000000000000000000 ) ) ;
#4740 = CARTESIAN_POINT ( 'NONE',  ( 181.8764988495240118, -33.54226604284930602, -5.074374724088000832 ) ) ;
#4741 = CARTESIAN_POINT ( 'NONE',  ( 70.06202783732101125, -36.73691869758536654, 361.9756252759101471 ) ) ;
#4743 = DIRECTION ( 'NONE',  ( 0.000000000000000000, 0.000000000000000000, 1.000000000000000000 ) ) ;
#4742 = CARTESIAN_POINT ( 'NONE',  ( 113.7157087630704240, -42.06174584507512293, 277.6356252759110816 ) ) ;
#4744 = CARTESIAN_POINT ( 'NONE',  ( 29.56648329127298069, 25.62155284005700295, 361.9756252759109998 ) ) ;
#4745 = CARTESIAN_POINT ( 'NONE',  ( 149.4532656544376721, -72.54365454176046057, 361.9756252759100335 ) ) ;
#4746 = VECTOR ( 'NONE', #74236, 1000.000000000000000 ) ;
#4747 = CARTESIAN_POINT ( 'NONE',  ( 0.000000000000000000, 223.9999999999999716, 164.1557476874258441 ) ) ;
#4748 = CARTESIAN_POINT ( 'NONE',  ( 3.968750000000050182, 127.0000000000000000, -100.8961411191535973 ) ) ;
#4749 = DIRECTION ( 'NONE',  ( -2.981567257902526681E-15, 0.8571673007021100021, 0.5150380749100580413 ) ) ;
#4750 = CARTESIAN_POINT ( 'NONE',  ( 105.7995184961486217, -26.72403496493496888, 76.17729194189745101 ) ) ;
#4752 = VERTEX_POINT ( 'NONE', #53670 ) ;
#4751 = CARTESIAN_POINT ( 'NONE',  ( -12.27452259663393264, 85.83635631587365822, -117.9189384461415813 ) ) ;
#4753 = CARTESIAN_POINT ( 'NONE',  ( 41.56670390244689628, -36.32844715994109208, 180.4678068554150911 ) ) ;
#4754 = CARTESIAN_POINT ( 'NONE',  ( 101.3926005705062749, -45.54394758209068073, 222.1213395616249784 ) ) ;
#4755 = CARTESIAN_POINT ( 'NONE',  ( 96.03574380810476896, -41.06042880536169548, 92.62419670448296927 ) ) ;
#4756 = CARTESIAN_POINT ( 'NONE',  ( 116.9258602667948566, -41.82750404599077854, 239.4346728949589647 ) ) ;
#4757 = CARTESIAN_POINT ( 'NONE',  ( 107.0664832912750057, -36.72944715993903486, 4.925625275910970657 ) ) ;
#4758 = CARTESIAN_POINT ( 'NONE',  ( 116.3212776292296127, -32.94146857471318413, 287.6356252759109680 ) ) ;
#4760 = CARTESIAN_POINT ( 'NONE',  ( 103.6593828106357904, -46.19869665420930005, 38.30169458292214557 ) ) ;
#4759 = DIRECTION ( 'NONE',  ( 0.000000000000000000, 0.000000000000000000, -1.000000000000000000 ) ) ;
#4761 = CARTESIAN_POINT ( 'NONE',  ( 179.7974245136200011, -36.32844715994040996, 193.9678068554150059 ) ) ;
#4762 = CARTESIAN_POINT ( 'NONE',  ( 69.63919639214307722, 92.07499999999998863, 53.63573739454427880 ) ) ;
#4763 = ADVANCED_FACE ( 'NONE', ( #12370, #81437 ), #4214, .F. ) ;
#4764 = ORIENTED_EDGE ( 'NONE', *, *, #39152, .T. ) ;
#4765 = EDGE_CURVE ( 'NONE', #7062, #74740, #81876, .T. ) ;
#4766 = ORIENTED_EDGE ( 'NONE', *, *, #28796, .T. ) ;
#4767 = CARTESIAN_POINT ( 'NONE',  ( 115.6810990589499397, -33.93640840262257541, 133.5105150661719620 ) ) ;
#4768 = ADVANCED_FACE ( 'NONE', ( #45517 ), #25099, .T. ) ;
#4770 = ORIENTED_EDGE ( 'NONE', *, *, #12341, .F. ) ;
#4769 = CARTESIAN_POINT ( 'NONE',  ( 21.73093249848547259, 47.21781368078172392, 31.29576654108570111 ) ) ;
#4771 = VECTOR ( 'NONE', #45623, 1000.000000000000000 ) ;
#4772 = CARTESIAN_POINT ( 'NONE',  ( 104.4898545173444973, -26.97883498049986883, 90.27984912381337779 ) ) ;
#4773 = CARTESIAN_POINT ( 'NONE',  ( 98.00553567079155926, -41.84099229931889852, 132.7356252759109623 ) ) ;
#4774 = DIRECTION ( 'NONE',  ( 1.000000000000000078E-15, 0.000000000000000000, 1.000000000000000000 ) ) ;
#4775 = CARTESIAN_POINT ( 'NONE',  ( 77.96454488115479364, -16.94667115355656151, 7.474641677899402481 ) ) ;
#4776 = EDGE_CURVE ( 'NONE', #88384, #78380, #88690, .T. ) ;
#4777 = EDGE_CURVE ( 'NONE', #3721, #89894, #60048, .T. ) ;
#4778 = CYLINDRICAL_SURFACE ( 'NONE', #24444, 9.524999999999998579 ) ;
#4779 = DIRECTION ( 'NONE',  ( 1.000000000000000078E-15, 1.000000000000000083E-30, -1.000000000000000000 ) ) ;
#4780 = CARTESIAN_POINT ( 'NONE',  ( 116.8058161338298504, -37.62879752186918836, 78.75276813305399060 ) ) ;
#4781 = VERTEX_POINT ( 'NONE', #26446 ) ;
#4782 = ORIENTED_EDGE ( 'NONE', *, *, #27446, .T. ) ;
#4783 = VERTEX_POINT ( 'NONE', #80526 ) ;
#4784 = EDGE_CURVE ( 'NONE', #86805, #69972, #74151, .T. ) ;
#4785 = VECTOR ( 'NONE', #4138, 1000.000000000000000 ) ;
#4786 = PLANE ( 'NONE',  #18166 ) ;
#4788 = LINE ( 'NONE', #5235, #17155 ) ;
#4787 = CARTESIAN_POINT ( 'NONE',  ( 102.3610132369663432, -45.97051510703448685, 168.2137205140059564 ) ) ;
#4789 = DIRECTION ( 'NONE',  ( -1.000000000000000000, -1.734723475976808672E-15, 0.000000000000000000 ) ) ;
#4790 = EDGE_CURVE ( 'NONE', #2982, #52784, #78320, .T. ) ;
#4791 = DIRECTION ( 'NONE',  ( 0.000000000000000000, 0.000000000000000000, 1.000000000000000000 ) ) ;
#4792 = CARTESIAN_POINT ( 'NONE',  ( -68.53801554307499089, 120.6499999999999915, 74.15067561874188584 ) ) ;
#4793 = CARTESIAN_POINT ( 'NONE',  ( 41.56648329127499153, -36.32844715994070839, 83.67562527591201160 ) ) ;
#4794 = DIRECTION ( 'NONE',  ( -1.000000000000000078E-15, 0.000000000000000000, 1.000000000000000000 ) ) ;
#4795 = CARTESIAN_POINT ( 'NONE',  ( 116.1047473792920357, -29.10330858331343151, 74.38419670448293175 ) ) ;
#4796 = ORIENTED_EDGE ( 'NONE', *, *, #22027, .T. ) ;
#4798 = EDGE_LOOP ( 'NONE', ( #83931, #169 ) ) ;
#4797 = EDGE_CURVE ( 'NONE', #54712, #28958, #8678, .T. ) ;
#4799 = CARTESIAN_POINT ( 'NONE',  ( 162.7866693523299944, -36.02818131005322044, 193.9678068554149775 ) ) ;
#4800 = CARTESIAN_POINT ( 'NONE',  ( 126.6659102797931808, 46.32248961978775981, 31.63262298343003920 ) ) ;
#4801 = LINE ( 'NONE', #19772, #49644 ) ;
#4802 = CARTESIAN_POINT ( 'NONE',  ( 98.92690986002996567, -36.11615286530263091, 144.0852332267349709 ) ) ;
#4803 = EDGE_CURVE ( 'NONE', #31453, #63618, #67841, .T. ) ;
#4804 = CIRCLE ( 'NONE', #70087, 5.599999999999994316 ) ;
#4805 = AXIS2_PLACEMENT_3D ( 'NONE', #33070, #54377, #19444 ) ;
#4806 = CARTESIAN_POINT ( 'NONE',  ( 136.8164806451551669, -18.72944715939129523, 6.749772901088581634 ) ) ;
#4807 = VERTEX_POINT ( 'NONE', #11544 ) ;
#4808 = ORIENTED_EDGE ( 'NONE', *, *, #31445, .F. ) ;
#4809 = FACE_OUTER_BOUND ( 'NONE', #78924, .T. ) ;
#4810 = ORIENTED_EDGE ( 'NONE', *, *, #76659, .T. ) ;
#4811 = ORIENTED_EDGE ( 'NONE', *, *, #56951, .T. ) ;
#4812 = LINE ( 'NONE', #75198, #66583 ) ;
#4813 = EDGE_CURVE ( 'NONE', #4000, #21358, #40122, .T. ) ;
#4814 = CARTESIAN_POINT ( 'NONE',  ( 98.38943151359886485, -34.93026649658274607, 212.5958690201829597 ) ) ;
#4815 = DIRECTION ( 'NONE',  ( -1.000000000000000000, 0.000000000000000000, 0.000000000000000000 ) ) ;
#4816 = ADVANCED_FACE ( 'NONE', ( #18798 ), #87397, .T. ) ;
#4817 = PLANE ( 'NONE',  #38563 ) ;
#4818 = CARTESIAN_POINT ( 'NONE',  ( -109.4150722537221867, 56.95621006804009312, 71.22652974919590463 ) ) ;
#4819 = ORIENTED_EDGE ( 'NONE', *, *, #87208, .F. ) ;
#4820 = EDGE_LOOP ( 'NONE', ( #70863, #83092, #88200, #13402 ) ) ;
#4821 = CIRCLE ( 'NONE', #38214, 4.762500000000002842 ) ;
#4822 = ORIENTED_EDGE ( 'NONE', *, *, #21901, .F. ) ;
#4823 = EDGE_LOOP ( 'NONE', ( #86998, #19685, #65029, #53257 ) ) ;
#4824 = CARTESIAN_POINT ( 'NONE',  ( 115.6671688226974197, -35.76553148137116267, 231.7214237029249659 ) ) ;
#4826 = CARTESIAN_POINT ( 'NONE',  ( 114.5834136592134200, -44.03589093681723909, 98.21276813305395592 ) ) ;
#4825 = VECTOR ( 'NONE', #4659, 1000.000000000000000 ) ;
#4827 = CARTESIAN_POINT ( 'NONE',  ( 98.60777729073571152, -43.80857954853296121, 71.86895860924397539 ) ) ;
#4828 = CARTESIAN_POINT ( 'NONE',  ( 109.6404665629360267, -46.48072720445416195, 252.7816004336761466 ) ) ;
#4829 = CARTESIAN_POINT ( 'NONE',  ( 77.11675609725448055, -140.6784471599409869, 245.5822774315739991 ) ) ;
#4830 = DIRECTION ( 'NONE',  ( 1.000000000000000078E-15, -1.000000000000000083E-30, -1.000000000000000000 ) ) ;
#4831 = CARTESIAN_POINT ( 'NONE',  ( 103.0497676667862947, -26.43187579209836002, 166.3603871806729444 ) ) ;
#4832 = DIRECTION ( 'NONE',  ( 0.000000000000000000, 1.000000000000000000, 0.000000000000000000 ) ) ;
#4833 = ORIENTED_EDGE ( 'NONE', *, *, #81603, .T. ) ;
#4834 = FACE_OUTER_BOUND ( 'NONE', #32177, .T. ) ;
#4835 = ORIENTED_EDGE ( 'NONE', *, *, #9659, .F. ) ;
#4836 = ORIENTED_EDGE ( 'NONE', *, *, #10479, .T. ) ;
#4837 = CYLINDRICAL_SURFACE ( 'NONE', #41834, 2.517500000000005844 ) ;
#4838 = DIRECTION ( 'NONE',  ( 1.000000000000000000, 0.000000000000000000, 0.000000000000000000 ) ) ;
#4839 = ORIENTED_EDGE ( 'NONE', *, *, #54784, .T. ) ;
#4840 = VECTOR ( 'NONE', #4779, 1000.000000000000000 ) ;
#4841 = ADVANCED_FACE ( 'NONE', ( #33322 ), #74219, .T. ) ;
#4842 = CARTESIAN_POINT ( 'NONE',  ( 107.0664832912739968, -8.979447159941031487, -5.074374724089029343 ) ) ;
#4843 = VERTEX_POINT ( 'NONE', #68299 ) ;
#4844 = CARTESIAN_POINT ( 'NONE',  ( 115.7831076647344588, -41.80230951982593979, 178.4064586084813016 ) ) ;
#4845 = CARTESIAN_POINT ( 'NONE',  ( 96.07744114619573850, -37.92110155076959899, 81.40038718067299328 ) ) ;
#4846 = PLANE ( 'NONE',  #69282 ) ;
#4847 = DIRECTION ( 'NONE',  ( 0.000000000000000000, 0.000000000000000000, 1.000000000000000000 ) ) ;
#4848 = CARTESIAN_POINT ( 'NONE',  ( 123.5667039024469886, -71.37844715994093292, 222.2178068554179902 ) ) ;
#4850 = CARTESIAN_POINT ( 'NONE',  ( 97.40233316251689644, -42.04621543282986096, 172.7146728949589942 ) ) ;
#4849 = FACE_OUTER_BOUND ( 'NONE', #37716, .T. ) ;
#4851 = FACE_OUTER_BOUND ( 'NONE', #27361, .T. ) ;
#4852 = LINE ( 'NONE', #68427, #33726 ) ;
#4853 = EDGE_LOOP ( 'NONE', ( #37804, #41543, #10759, #75209 ) ) ;
#4854 = CARTESIAN_POINT ( 'NONE',  ( 107.0664832912739541, -36.72944715994095333, 307.1356252759109680 ) ) ;
#4855 = CARTESIAN_POINT ( 'NONE',  ( 92.91125933621934507, -113.6057974291314565, -11.78219314458173272 ) ) ;
#4856 = DIRECTION ( 'NONE',  ( 0.9834602067019604377, 0.1811243270069963496, 0.000000000000000000 ) ) ;
#4857 = CARTESIAN_POINT ( 'NONE',  ( 32.56670390244712365, -18.82844715994099616, -5.074374724088000832 ) ) ;
#4859 = ORIENTED_EDGE ( 'NONE', *, *, #12120, .T. ) ;
#4858 = CARTESIAN_POINT ( 'NONE',  ( 118.1283360304583994, -32.34034571477864262, 249.1270538473389706 ) ) ;
#4860 = CARTESIAN_POINT ( 'NONE',  ( 24.79284581386643893, 184.0000000000000000, 106.1020876358972629 ) ) ;
#4861 = CARTESIAN_POINT ( 'NONE',  ( 97.48672026426986292, -32.61689163886055809, 12.00419670448293985 ) ) ;
#4862 = CARTESIAN_POINT ( 'NONE',  ( 116.9629591039797845, -33.20839883953882321, 110.0984824187679578 ) ) ;
#4863 = CARTESIAN_POINT ( 'NONE',  ( 70.63919639214310564, 91.07499999999996021, 53.63573739454427880 ) ) ;
#4864 = CARTESIAN_POINT ( 'NONE',  ( 12.67977336836082891, 83.37982733273462088, -129.9388093972407603 ) ) ;
#4865 = EDGE_CURVE ( 'NONE', #76536, #26931, #52822, .T. ) ;
#4866 = FACE_OUTER_BOUND ( 'NONE', #12549, .T. ) ;
#4867 = DIRECTION ( 'NONE',  ( -2.981567257902526681E-15, 0.8571673007021100021, 0.5150380749100580413 ) ) ;
#4868 = ORIENTED_EDGE ( 'NONE', *, *, #862, .F. ) ;
#4869 = VECTOR ( 'NONE', #26634, 1000.000000000000000 ) ;
#4870 = AXIS2_PLACEMENT_3D ( 'NONE', #47714, #75453, #20492 ) ;
#4871 = ADVANCED_FACE ( 'NONE', ( #61022 ), #88750, .T. ) ;
#4872 = ORIENTED_EDGE ( 'NONE', *, *, #37268, .T. ) ;
#4873 = EDGE_CURVE ( 'NONE', #80721, #83896, #54180, .T. ) ;
#4874 = ORIENTED_EDGE ( 'NONE', *, *, #88312, .T. ) ;
#4875 = ADVANCED_FACE ( 'NONE', ( #88308 ), #54626, .F. ) ;
#4876 = VERTEX_POINT ( 'NONE', #60112 ) ;
#4877 = CARTESIAN_POINT ( 'NONE',  ( 97.81169150544869240, -40.51741169384158781, 71.63577594787710723 ) ) ;
#4878 = CARTESIAN_POINT ( 'NONE',  ( 104.4960957391109559, -46.84663716100901354, 43.37848241876896083 ) ) ;
#4879 = CARTESIAN_POINT ( 'NONE',  ( 72.26648329127297643, -1.929447159941394263, 342.9256252759109884 ) ) ;
#4880 = CARTESIAN_POINT ( 'NONE',  ( 87.66583711884676688, -139.6647249350598656, 247.4938686140749837 ) ) ;
#4882 = CARTESIAN_POINT ( 'NONE',  ( 69.59601834107196794, -140.2077779303689908, 245.9389812651000113 ) ) ;
#4881 = DIRECTION ( 'NONE',  ( 0.000000000000000000, 0.000000000000000000, 1.000000000000000000 ) ) ;
#4883 = CARTESIAN_POINT ( 'NONE',  ( 101.8145705177301892, -43.46543587290290134, 231.4724198280769940 ) ) ;
#4884 = ORIENTED_EDGE ( 'NONE', *, *, #77980, .T. ) ;
#4885 = ORIENTED_EDGE ( 'NONE', *, *, #8686, .F. ) ;
#4886 = ORIENTED_EDGE ( 'NONE', *, *, #76905, .T. ) ;
#4887 = EDGE_CURVE ( 'NONE', #61102, #77844, #81944, .T. ) ;
#4888 = CIRCLE ( 'NONE', #534, 24.63800000000000168 ) ;
#4889 = DIRECTION ( 'NONE',  ( 0.0001211784769810529054, -0.7071067708032295895, 0.7071067811865515695 ) ) ;
#4890 = CIRCLE ( 'NONE', #6317, 1.000000000000000888 ) ;
#4891 = CARTESIAN_POINT ( 'NONE',  ( 116.8170317996813736, -34.15256532312115212, 104.0313894407264996 ) ) ;
#4892 = CARTESIAN_POINT ( 'NONE',  ( 1.387778780781445676E-14, 239.0000000000000000, 97.27542076772557778 ) ) ;
#4893 = LINE ( 'NONE', #79877, #11248 ) ;
#4894 = CARTESIAN_POINT ( 'NONE',  ( 98.24278011039416469, -41.58876472015902692, 23.15872616303999010 ) ) ;
#4895 = EDGE_CURVE ( 'NONE', #87481, #34970, #11079, .T. ) ;
#4896 = DIRECTION ( 'NONE',  ( -7.980413499659419871E-32, 1.000000000000000000, 3.785359618865284342E-16 ) ) ;
#4897 = VECTOR ( 'NONE', #26224, 1000.000000000000114 ) ;
#4898 = PLANE ( 'NONE',  #8627 ) ;
#4899 = CARTESIAN_POINT ( 'NONE',  ( 100.6696166679599003, -29.33055989933767904, 260.6441967044828516 ) ) ;
#4900 = PLANE ( 'NONE',  #42862 ) ;
#4902 = ORIENTED_EDGE ( 'NONE', *, *, #60403, .F. ) ;
#4901 = EDGE_CURVE ( 'NONE', #82261, #75851, #23145, .T. ) ;
#4903 = PLANE ( 'NONE',  #5472 ) ;
#4904 = CARTESIAN_POINT ( 'NONE',  ( 80.06648329127399677, -8.350947159940998787, 308.6356252759119911 ) ) ;
#4905 = CARTESIAN_POINT ( 'NONE',  ( 114.3647906391003630, -33.01227106732497418, 42.01951894101996032 ) ) ;
#4906 = VECTOR ( 'NONE', #50613, 1000.000000000000114 ) ;
#4907 = DIRECTION ( 'NONE',  ( -0.000000000000000000, 1.000000000000000000, 0.000000000000000000 ) ) ;
#4908 = CARTESIAN_POINT ( 'NONE',  ( 0.000000000000000000, 44.45000000000000284, 0.000000000000000000 ) ) ;
#4909 = DIRECTION ( 'NONE',  ( -0.8571673007021084478, -0.5150380749100604838, -8.571673007021083688E-16 ) ) ;
#4910 = ORIENTED_EDGE ( 'NONE', *, *, #61291, .T. ) ;
#4911 = DIRECTION ( 'NONE',  ( 1.000000000000000078E-15, 0.000000000000000000, 1.000000000000000000 ) ) ;
#4912 = CARTESIAN_POINT ( 'NONE',  ( 125.2832873508473455, 54.59514987206014069, -36.72832927292047600 ) ) ;
#4913 = EDGE_LOOP ( 'NONE', ( #17845, #82775, #14973, #80685 ) ) ;
#4914 = CARTESIAN_POINT ( 'NONE',  ( 98.45854724665603896, -30.84808103350501085, 120.8499109901969604 ) ) ;
#4915 = ORIENTED_EDGE ( 'NONE', *, *, #50358, .T. ) ;
#4916 = CARTESIAN_POINT ( 'NONE',  ( 100.8685319560204050, -42.60665150962044123, 81.35241982807694683 ) ) ;
#4917 = DIRECTION ( 'NONE',  ( 0.000000000000000000, 0.000000000000000000, -1.000000000000000000 ) ) ;
#4918 = CARTESIAN_POINT ( 'NONE',  ( 112.8895349442155265, -29.35594087158844445, 120.9882499725639633 ) ) ;
#4919 = CARTESIAN_POINT ( 'NONE',  ( 131.0667039024480118, -67.87844715994100397, 231.5838068554150198 ) ) ;
#4920 = EDGE_CURVE ( 'NONE', #40277, #9193, #18341, .T. ) ;
#4921 = FACE_OUTER_BOUND ( 'NONE', #41166, .T. ) ;
#4922 = CARTESIAN_POINT ( 'NONE',  ( 99.74686247383996829, -44.23293585951837059, 17.96133956162493206 ) ) ;
#4923 = CARTESIAN_POINT ( 'NONE',  ( 97.07208394142573127, -35.37832485732319299, 182.2194452067948873 ) ) ;
#4924 = ORIENTED_EDGE ( 'NONE', *, *, #30752, .F. ) ;
#4925 = VECTOR ( 'NONE', #31546, 999.9999999999998863 ) ;
#4926 = DIRECTION ( 'NONE',  ( 0.000000000000000000, 1.000000000000000000, 0.000000000000000000 ) ) ;
#4927 = ORIENTED_EDGE ( 'NONE', *, *, #39896, .T. ) ;
#4928 = CARTESIAN_POINT ( 'NONE',  ( -117.9189190431815462, 79.26437155269051971, 12.27470785614043436 ) ) ;
#4929 = AXIS2_PLACEMENT_3D ( 'NONE', #46373, #67741, #39575 ) ;
#4930 = ORIENTED_EDGE ( 'NONE', *, *, #6167, .T. ) ;
#4931 = VERTEX_POINT ( 'NONE', #73761 ) ;
#4932 = CARTESIAN_POINT ( 'NONE',  ( -492.0614999999999668, 14.28749999999982201, 90.48749999999999716 ) ) ;
#4933 = ORIENTED_EDGE ( 'NONE', *, *, #78641, .T. ) ;
#4934 = CARTESIAN_POINT ( 'NONE',  ( 101.2091419812964830, -45.28691980162484754, 242.1108633711499465 ) ) ;
#4935 = CARTESIAN_POINT ( 'NONE',  ( 97.61330010463601070, -39.99285327795418254, 126.5905029351318802 ) ) ;
#4936 = FACE_OUTER_BOUND ( 'NONE', #10175, .T. ) ;
#4937 = CARTESIAN_POINT ( 'NONE',  ( 110.3719271596222882, -47.27686491584164941, 48.80610146638797175 ) ) ;
#4938 = DIRECTION ( 'NONE',  ( -1.000000000000000000, 0.000000000000000000, 3.491483361109380094E-15 ) ) ;
#4939 = VERTEX_POINT ( 'NONE', #39239 ) ;
#4940 = CARTESIAN_POINT ( 'NONE',  ( 182.2300522401169758, -33.89581943343728199, 313.9678068554149490 ) ) ;
#4941 = EDGE_CURVE ( 'NONE', #64462, #86177, #25609, .T. ) ;
#4942 = LINE ( 'NONE', #88072, #23024 ) ;
#4943 = VERTEX_POINT ( 'NONE', #5171 ) ;
#4944 = EDGE_CURVE ( 'NONE', #1484, #88413, #60565, .T. ) ;
#4945 = VECTOR ( 'NONE', #85269, 1000.000000000000000 ) ;
#4946 = CARTESIAN_POINT ( 'NONE',  ( 193.0374249753377001, -23.42844715993431848, 129.9678068554150343 ) ) ;
#4947 = CARTESIAN_POINT ( 'NONE',  ( 34.67381068362062280, -26.00627455219358453, 342.9256252759109884 ) ) ;
#4948 = CARTESIAN_POINT ( 'NONE',  ( 117.4695305279094981, -36.80206755349689729, 263.8213395616251660 ) ) ;
#4949 = DIRECTION ( 'NONE',  ( -0.8660254037844390407, 0.000000000000000000, -0.4999999999999995004 ) ) ;
#4950 = VECTOR ( 'NONE', #1730, 1000.000000000000000 ) ;
#4951 = CARTESIAN_POINT ( 'NONE',  ( 85.31670390244703128, -104.2784471599409670, 19.21780685541800437 ) ) ;
#4952 = LINE ( 'NONE', #32647, #1190 ) ;
#4953 = CARTESIAN_POINT ( 'NONE',  ( 113.0872481101271205, -29.11229423309321618, 273.9667055423626039 ) ) ;
#4955 = CARTESIAN_POINT ( 'NONE',  ( 113.4926247784320452, -28.54816540729044405, 75.54705384733995288 ) ) ;
#4954 = DIRECTION ( 'NONE',  ( 0.000000000000000000, 0.000000000000000000, 1.000000000000000000 ) ) ;
#4956 = CARTESIAN_POINT ( 'NONE',  ( 120.5244058523157662, 74.60816462893807000, 50.18922276370457780 ) ) ;
#4957 = CARTESIAN_POINT ( 'NONE',  ( 95.96722792477895325, -36.58315769931292749, 156.3280062282919687 ) ) ;
#4958 = ORIENTED_EDGE ( 'NONE', *, *, #85234, .F. ) ;
#4959 = CARTESIAN_POINT ( 'NONE',  ( 57.14999999999999858, 60.86974387893089755, 326.2630000000000337 ) ) ;
#4960 = VERTEX_POINT ( 'NONE', #81500 ) ;
#4961 = DIRECTION ( 'NONE',  ( 0.000000000000000000, 0.000000000000000000, -1.000000000000000000 ) ) ;
#4962 = AXIS2_PLACEMENT_3D ( 'NONE', #65180, #44719, #65621 ) ;
#4963 = DIRECTION ( 'NONE',  ( 1.000000000000000078E-15, 1.000000000000000083E-30, -1.000000000000000000 ) ) ;
#4964 = DIRECTION ( 'NONE',  ( 0.000000000000000000, 1.000000000000000000, 0.000000000000000000 ) ) ;
#4965 = EDGE_LOOP ( 'NONE', ( #19056, #80784, #40633, #54726, #43123 ) ) ;
#4966 = DIRECTION ( 'NONE',  ( 1.000000000000000000, 0.000000000000000000, 9.351236661543306751E-17 ) ) ;
#4968 = ORIENTED_EDGE ( 'NONE', *, *, #80762, .F. ) ;
#4967 = CARTESIAN_POINT ( 'NONE',  ( 114.2838679902333610, -44.31336211532283897, 158.1813395616249807 ) ) ;
#4969 = CARTESIAN_POINT ( 'NONE',  ( 19.56670390244643443, -25.42844715994203852, 180.4678068554150911 ) ) ;
#4970 = CARTESIAN_POINT ( 'NONE',  ( -130.4924867222203773, 94.58014758961631685, 4.091264198876692681 ) ) ;
#4971 = CARTESIAN_POINT ( 'NONE',  ( 108.5351697880554696, -105.7036166034834963, -19.78219314458196010 ) ) ;
#4972 = LINE ( 'NONE', #60365, #32186 ) ;
#4973 = VERTEX_POINT ( 'NONE', #22287 ) ;
#4974 = CARTESIAN_POINT ( 'NONE',  ( 97.96720171806632038, -41.86261760143219846, 136.7356252759109623 ) ) ;
#4975 = APPLICATION_PROTOCOL_DEFINITION ( 'draft international standard', 'automotive_design', 1998, #12135 ) ;
#4976 = CARTESIAN_POINT ( 'NONE',  ( 106.5667039024470313, -99.52844715994206126, -19.78219314458215550 ) ) ;
#4977 = DIRECTION ( 'NONE',  ( 0.000000000000000000, -1.000000000000000000, 0.000000000000000000 ) ) ;
#4978 = ORIENTED_EDGE ( 'NONE', *, *, #38037, .F. ) ;
#4979 = EDGE_CURVE ( 'NONE', #61259, #7662, #85767, .T. ) ;
#4980 = EDGE_CURVE ( 'NONE', #64268, #63182, #88670, .T. ) ;
#4981 = ORIENTED_EDGE ( 'NONE', *, *, #19440, .T. ) ;
#4982 = LINE ( 'NONE', #30118, #27812 ) ;
#4983 = CARTESIAN_POINT ( 'NONE',  ( 94.61941200740719182, 94.84315624882772511, -89.95943163722073166 ) ) ;
#4984 = PLANE ( 'NONE',  #41057 ) ;
#4985 = CARTESIAN_POINT ( 'NONE',  ( 3.174999999999889688, 124.5870000000000033, 31.75000000000000000 ) ) ;
#4986 = EDGE_CURVE ( 'NONE', #68369, #33468, #71336, .T. ) ;
#4988 = DIRECTION ( 'NONE',  ( 0.000000000000000000, 0.000000000000000000, -1.000000000000000000 ) ) ;
#4987 = LINE ( 'NONE', #47189, #82819 ) ;
#4989 = CARTESIAN_POINT ( 'NONE',  ( 113.2454463666727946, -28.75862960087268405, 179.5522973137137228 ) ) ;
#4990 = VECTOR ( 'NONE', #29562, 1000.000000000000114 ) ;
#4991 = VERTEX_POINT ( 'NONE', #23204 ) ;
#4992 = EDGE_CURVE ( 'NONE', #36895, #11918, #7408, .T. ) ;
#4993 = AXIS2_PLACEMENT_3D ( 'NONE', #26299, #53975, #21740 ) ;
#4994 = LINE ( 'NONE', #61727, #28812 ) ;
#4995 = CARTESIAN_POINT ( 'NONE',  ( 103.8504807240353500, -26.87063827031099450, 206.3394347997199816 ) ) ;
#4996 = EDGE_CURVE ( 'NONE', #49134, #63259, #6000, .T. ) ;
#4998 = ORIENTED_EDGE ( 'NONE', *, *, #79153, .T. ) ;
#4997 = CARTESIAN_POINT ( 'NONE',  ( -71.09939861440099662, 101.5999999999999943, 177.8662485265279827 ) ) ;
#4999 = CARTESIAN_POINT ( 'NONE',  ( 97.00151786184787284, -41.45262973156711439, 57.67562527591096710 ) ) ;
#5000 = CYLINDRICAL_SURFACE ( 'NONE', #35672, 9.999999999999998224 ) ;
#5001 = LINE ( 'NONE', #12264, #5018 ) ;
#5002 = CARTESIAN_POINT ( 'NONE',  ( 97.75828313668286285, -40.38462675027328430, 22.62423254407919160 ) ) ;
#5003 = ORIENTED_EDGE ( 'NONE', *, *, #65300, .T. ) ;
#5004 = DIRECTION ( 'NONE',  ( 0.8660254037844387076, -0.4999999999999998335, 1.550000000000002231E-14 ) ) ;
#5005 = ORIENTED_EDGE ( 'NONE', *, *, #88470, .T. ) ;
#5006 = VERTEX_POINT ( 'NONE', #35900 ) ;
#5007 = CARTESIAN_POINT ( 'NONE',  ( 106.9593448401346620, -46.12439510495315886, 229.0111071154209696 ) ) ;
#5008 = VECTOR ( 'NONE', #32730, 1000.000000000000114 ) ;
#5009 = CARTESIAN_POINT ( 'NONE',  ( 173.9900000000000091, 20.32000000000000028, 71.37400000000000944 ) ) ;
#5010 = AXIS2_PLACEMENT_3D ( 'NONE', #56810, #14607, #41387 ) ;
#5011 = CARTESIAN_POINT ( 'NONE',  ( 184.5664832912729878, 25.62155284005700295, 361.9756252759109998 ) ) ;
#5012 = CIRCLE ( 'NONE', #16636, 4.874999999999990230 ) ;
#5013 = CARTESIAN_POINT ( 'NONE',  ( 116.7951252642580329, -39.38782981925626103, 154.6147919402135642 ) ) ;
#5014 = CARTESIAN_POINT ( 'NONE',  ( 82.81648329127399677, -36.72944715994106701, 3.101481641215461327 ) ) ;
#5015 = AXIS2_PLACEMENT_3D ( 'NONE', #1963, #35567, #83738 ) ;
#5016 = ORIENTED_EDGE ( 'NONE', *, *, #50973, .T. ) ;
#5017 = FACE_OUTER_BOUND ( 'NONE', #21001, .T. ) ;
#5018 = VECTOR ( 'NONE', #39958, 1000.000000000000000 ) ;
#5019 = CARTESIAN_POINT ( 'NONE',  ( 116.3212776292269268, -32.94146857470660450, 84.13562527591095375 ) ) ;
#5020 = VERTEX_POINT ( 'NONE', #64068 ) ;
#5021 = CARTESIAN_POINT ( 'NONE',  ( 99.76197604230684135, -44.21744263965017296, 21.96133956162593748 ) ) ;
#5022 = ORIENTED_EDGE ( 'NONE', *, *, #6422, .F. ) ;
#5023 = VERTEX_POINT ( 'NONE', #49513 ) ;
#5024 = CARTESIAN_POINT ( 'NONE',  ( 114.7541070161690158, -40.70454043057743121, 241.2528522743529606 ) ) ;
#5025 = PLANE ( 'NONE',  #6821 ) ;
#5026 = CARTESIAN_POINT ( 'NONE',  ( 113.8091913586854531, -43.81457933525494042, 158.1813395616259754 ) ) ;
#5027 = DIRECTION ( 'NONE',  ( 0.000000000000000000, 0.000000000000000000, 1.000000000000000000 ) ) ;
#5028 = CARTESIAN_POINT ( 'NONE',  ( 177.8371591254545194, -47.82818131005477369, 180.4678068554150343 ) ) ;
#5029 = CARTESIAN_POINT ( 'NONE',  ( -492.0614999999999668, 93.66249999999999432, 90.48749999999999716 ) ) ;
#5030 = EDGE_CURVE ( 'NONE', #48763, #65538, #23636, .T. ) ;
#5031 = CARTESIAN_POINT ( 'NONE',  ( 110.0644950372451945, -26.04256623378434554, 215.8708633711489711 ) ) ;
#5032 = LINE ( 'NONE', #11851, #84848 ) ;
#5033 = ORIENTED_EDGE ( 'NONE', *, *, #23143, .T. ) ;
#5034 = CARTESIAN_POINT ( 'NONE',  ( 118.0477628396966310, -38.34468641101997122, 69.72229194257801055 ) ) ;
#5035 = CARTESIAN_POINT ( 'NONE',  ( 116.3183303039212291, -32.94226276200836878, 104.1356252759109680 ) ) ;
#5036 = EDGE_CURVE ( 'NONE', #85840, #76619, #8207, .T. ) ;
#5037 = ORIENTED_EDGE ( 'NONE', *, *, #82023, .F. ) ;
#5038 = CIRCLE ( 'NONE', #54348, 24.50000000000000711 ) ;
#5039 = ORIENTED_EDGE ( 'NONE', *, *, #17313, .F. ) ;
#5040 = ORIENTED_EDGE ( 'NONE', *, *, #14758, .T. ) ;
#5041 = CARTESIAN_POINT ( 'NONE',  ( 105.7976818973178581, -26.72428486692769312, 160.1772091339258282 ) ) ;
#5042 = CARTESIAN_POINT ( 'NONE',  ( -123.4696824136392053, 20.32000000000000028, -179.8898777604655095 ) ) ;
#5043 = CARTESIAN_POINT ( 'NONE',  ( 117.0667039024470313, -104.2784471599412086, 7.717806855417980394 ) ) ;
#5044 = CARTESIAN_POINT ( 'NONE',  ( 99.63185314732805864, -32.29918761127225224, 128.7290427505439823 ) ) ;
#5045 = CARTESIAN_POINT ( 'NONE',  ( 96.75123844313058896, -34.86533355485506291, 237.1841967044819626 ) ) ;
#5046 = CARTESIAN_POINT ( 'NONE',  ( 103.1875000000000000, 117.4749999999999943, 3.602774393244745134E-13 ) ) ;
#5047 = ORIENTED_EDGE ( 'NONE', *, *, #43636, .F. ) ;
#5048 = CARTESIAN_POINT ( 'NONE',  ( 129.9368274816652331, 83.38918798244689867, -12.69999999999863505 ) ) ;
#5049 = LINE ( 'NONE', #45024, #11322 ) ;
#5050 = VERTEX_POINT ( 'NONE', #22742 ) ;
#5051 = ORIENTED_EDGE ( 'NONE', *, *, #38184, .T. ) ;
#5052 = AXIS2_PLACEMENT_3D ( 'NONE', #3871, #64324, #86109 ) ;
#5053 = EDGE_CURVE ( 'NONE', #31466, #21936, #69233, .T. ) ;
#5054 = LINE ( 'NONE', #60449, #40154 ) ;
#5055 = ORIENTED_EDGE ( 'NONE', *, *, #764, .T. ) ;
#5056 = ORIENTED_EDGE ( 'NONE', *, *, #20635, .T. ) ;
#5057 = CARTESIAN_POINT ( 'NONE',  ( 152.5667039024472160, -23.42844715993585325, 129.9678068554149775 ) ) ;
#5058 = VECTOR ( 'NONE', #74347, 1000.000000000000000 ) ;
#5059 = CARTESIAN_POINT ( 'NONE',  ( 107.0667039024470313, -104.2784471599418197, -11.78219314458200984 ) ) ;
#5060 = DIRECTION ( 'NONE',  ( 0.1811243268507098381, -0.9834602067307437467, 0.000000000000000000 ) ) ;
#5061 = CARTESIAN_POINT ( 'NONE',  ( 99.60253261678104764, -31.60088882024776780, 165.2819436375999658 ) ) ;
#5062 = CARTESIAN_POINT ( 'NONE',  ( 101.3600985487617692, -27.95198515609010315, 25.53562527591096654 ) ) ;
#5063 = CARTESIAN_POINT ( 'NONE',  ( 109.7229095233572878, -27.00028666605756555, 125.8649514782447199 ) ) ;
#5064 = VERTEX_POINT ( 'NONE', #5411 ) ;
#5065 = DIRECTION ( 'NONE',  ( -1.000000000000000000, 9.376883653928684652E-16, 1.500301384628589584E-15 ) ) ;
#5066 = ORIENTED_EDGE ( 'NONE', *, *, #16121, .T. ) ;
#5067 = CARTESIAN_POINT ( 'NONE',  ( 162.0667039024469886, -68.87844715994089029, 55.21780685541800437 ) ) ;
#5068 = ORIENTED_EDGE ( 'NONE', *, *, #67811, .F. ) ;
#5069 = CARTESIAN_POINT ( 'NONE',  ( 31.89136050872121331, -31.76306994223872238, 193.9678068554150911 ) ) ;
#5070 = CARTESIAN_POINT ( 'NONE',  ( 108.8673596973266058, 37.33800000000000097, 58.73749999999999716 ) ) ;
#5071 = CARTESIAN_POINT ( 'NONE',  ( 117.0922404263411778, -37.60051096986498465, 133.7571228985926552 ) ) ;
#5072 = FACE_OUTER_BOUND ( 'NONE', #24791, .T. ) ;
#5073 = EDGE_LOOP ( 'NONE', ( #25165, #17668, #3430, #31072 ) ) ;
#5074 = CARTESIAN_POINT ( 'NONE',  ( 107.1956731390977779, -26.28293224109629733, 35.06705384733893283 ) ) ;
#5075 = AXIS2_PLACEMENT_3D ( 'NONE', #89456, #62633, #408 ) ;
#5076 = CARTESIAN_POINT ( 'NONE',  ( 111.9491823805485922, -27.46919719833538309, 55.68991099019693536 ) ) ;
#5077 = AXIS2_PLACEMENT_3D ( 'NONE', #83899, #21670, #28458 ) ;
#5078 =( LENGTH_UNIT ( ) NAMED_UNIT ( * ) SI_UNIT ( .MILLI., .METRE. ) );
#5079 = VECTOR ( 'NONE', #48586, 1000.000000000000000 ) ;
#5081 = DIRECTION ( 'NONE',  ( -1.000000000000000000, 0.000000000000000000, 0.000000000000000000 ) ) ;
#5080 = LINE ( 'NONE', #12348, #15836 ) ;
#5082 = LINE ( 'NONE', #26426, #8983 ) ;
#5083 = DIRECTION ( 'NONE',  ( 0.000000000000000000, 0.000000000000000000, -1.000000000000000000 ) ) ;
#5084 = PLANE ( 'NONE',  #36834 ) ;
#5085 = ADVANCED_FACE ( 'NONE', ( #82176 ), #7200, .F. ) ;
#5086 = AXIS2_PLACEMENT_3D ( 'NONE', #62727, #62275, #55888 ) ;
#5087 = CARTESIAN_POINT ( 'NONE',  ( 51.23005224011598102, -33.89581943344511217, 342.9256252759109884 ) ) ;
#5088 = EDGE_CURVE ( 'NONE', #4730, #54028, #14006, .T. ) ;
#5089 = FACE_OUTER_BOUND ( 'NONE', #13996, .T. ) ;
#5090 = ORIENTED_EDGE ( 'NONE', *, *, #17976, .F. ) ;
#5091 = CARTESIAN_POINT ( 'NONE',  ( 97.31040724827032307, -32.83447933365327742, 41.02419670448193045 ) ) ;
#5092 = CARTESIAN_POINT ( 'NONE',  ( 117.9325828832643026, -34.70414220975756336, 199.9851490854349549 ) ) ;
#5093 = CARTESIAN_POINT ( 'NONE',  ( 114.5831001172654595, -44.03558617456690172, 94.21276813305395592 ) ) ;
#5094 = EDGE_CURVE ( 'NONE', #74091, #88572, #10334, .T. ) ;
#5096 = CARTESIAN_POINT ( 'NONE',  ( 25.56670390244745050, -48.82844715994178841, 170.7178068554150627 ) ) ;
#5095 = CARTESIAN_POINT ( 'NONE',  ( 194.0371591254572934, -24.89890238294407965, 300.4678068554149490 ) ) ;
#5097 = DIRECTION ( 'NONE',  ( 0.000000000000000000, 0.000000000000000000, -1.000000000000000000 ) ) ;
#5098 = AXIS2_PLACEMENT_3D ( 'NONE', #70473, #83656, #35937 ) ;
#5099 = AXIS2_PLACEMENT_3D ( 'NONE', #721, #20727, #22528 ) ;
#5100 = CARTESIAN_POINT ( 'NONE',  ( 72.96458098368701428, 127.0000000000000000, -72.96458098368670164 ) ) ;
#5101 = ORIENTED_EDGE ( 'NONE', *, *, #61889, .F. ) ;
#5102 = CARTESIAN_POINT ( 'NONE',  ( 117.1895451461016648, -38.97942580829903392, 99.64038718067195077 ) ) ;
#5103 = EDGE_CURVE ( 'NONE', #58908, #41468, #74447, .T. ) ;
#5105 = ORIENTED_EDGE ( 'NONE', *, *, #8074, .T. ) ;
#5104 = CARTESIAN_POINT ( 'NONE',  ( 11.71028986373773861, 87.46520591134841993, 130.0297596498208463 ) ) ;
#5106 = CARTESIAN_POINT ( 'NONE',  ( 118.0177608886752836, -35.41288285714062312, 234.9337205140059552 ) ) ;
#5107 = DIRECTION ( 'NONE',  ( 0.000000000000000000, -1.000000000000000000, 0.000000000000000000 ) ) ;
#5108 = DIRECTION ( 'NONE',  ( 0.000000000000000000, 0.000000000000000000, -1.000000000000000000 ) ) ;
#5109 = ADVANCED_FACE ( 'NONE', ( #89426 ), #33550, .F. ) ;
#5110 = DIRECTION ( 'NONE',  ( 1.000000000000000000, 0.000000000000000000, 0.000000000000000000 ) ) ;
#5111 = CARTESIAN_POINT ( 'NONE',  ( 105.7995185016981026, -26.72403496430482406, 81.17729194145603344 ) ) ;
#5112 = CARTESIAN_POINT ( 'NONE',  ( 131.8552587341645221, -38.37463194330769767, 2.472581811083949255 ) ) ;
#5113 = DIRECTION ( 'NONE',  ( 0.000000000000000000, -1.000000000000000000, 0.000000000000000000 ) ) ;
#5114 = CARTESIAN_POINT ( 'NONE',  ( 98.25516505653058630, -40.97492784622586015, 171.6841967044829573 ) ) ;
#5115 = ORIENTED_EDGE ( 'NONE', *, *, #87035, .T. ) ;
#5116 = ORIENTED_EDGE ( 'NONE', *, *, #14443, .T. ) ;
#5117 = CARTESIAN_POINT ( 'NONE',  ( 115.5384384484689804, -31.27996107247446744, 140.7130118773259539 ) ) ;
#5118 = LINE ( 'NONE', #5579, #18233 ) ;
#5120 = CARTESIAN_POINT ( 'NONE',  ( 106.1586424053106299, -121.2541776101292186, -11.78219314458148226 ) ) ;
#5119 = CARTESIAN_POINT ( 'NONE',  ( 97.63766479707265944, -34.12929003103651127, 247.1127681330529811 ) ) ;
#5121 = AXIS2_PLACEMENT_3D ( 'NONE', #8792, #57356, #48736 ) ;
#5122 = CARTESIAN_POINT ( 'NONE',  ( 149.4512091874902922, -60.54365471797113685, 361.9756252759100335 ) ) ;
#5123 = CARTESIAN_POINT ( 'NONE',  ( 3.968749999999229949, 120.6499999999999915, 100.8961411191535973 ) ) ;
#5124 = PLANE ( 'NONE',  #24094 ) ;
#5125 = CARTESIAN_POINT ( 'NONE',  ( 168.0371591254546217, -48.62818131005518296, 117.4678068554150485 ) ) ;
#5126 = CYLINDRICAL_SURFACE ( 'NONE', #69075, 9.425000000000000711 ) ;
#5127 = CARTESIAN_POINT ( 'NONE',  ( 107.5647246096319236, -47.74832088493825211, 192.6003871806729535 ) ) ;
#5128 = CARTESIAN_POINT ( 'NONE',  ( 49.21213752016101495, -29.73316016639650172, 237.4678068554150059 ) ) ;
#5129 = ORIENTED_EDGE ( 'NONE', *, *, #57413, .F. ) ;
#5130 = VERTEX_POINT ( 'NONE', #27187 ) ;
#5131 = CARTESIAN_POINT ( 'NONE',  ( -88.24354053934787601, 71.14122173980733521, -96.22129751242513862 ) ) ;
#5132 = CARTESIAN_POINT ( 'NONE',  ( 53.56670390244828184, -48.82844715994055917, 300.4678068554150059 ) ) ;
#5133 = CARTESIAN_POINT ( 'NONE',  ( -27.27158787008326968, 184.0000000000000000, 85.23828826961327820 ) ) ;
#5134 = CARTESIAN_POINT ( 'NONE',  ( 31.56670390244800828, -33.35206098992711077, -5.074374724088000832 ) ) ;
#5136 = FACE_OUTER_BOUND ( 'NONE', #78983, .T. ) ;
#5135 = VECTOR ( 'NONE', #38406, 1000.000000000000000 ) ;
#5137 = VERTEX_POINT ( 'NONE', #54862 ) ;
#5138 = CIRCLE ( 'NONE', #42858, 13.00000000000000355 ) ;
#5139 = CARTESIAN_POINT ( 'NONE',  ( 99.04388118832164878, -42.84098620836660132, 61.84393314859575241 ) ) ;
#5140 = CIRCLE ( 'NONE', #5211, 2.999999999999933387 ) ;
#5141 = VECTOR ( 'NONE', #32143, 1000.000000000000000 ) ;
#5142 = EDGE_CURVE ( 'NONE', #28975, #81967, #53804, .T. ) ;
#5143 = CARTESIAN_POINT ( 'NONE',  ( 96.85831052012196096, -34.61278962133658155, 216.1641967044819808 ) ) ;
#5144 = DIRECTION ( 'NONE',  ( 0.000000000000000000, 0.000000000000000000, -1.000000000000000000 ) ) ;
#5145 = ORIENTED_EDGE ( 'NONE', *, *, #29847, .T. ) ;
#5146 = CIRCLE ( 'NONE', #74789, 4.749999999999976907 ) ;
#5147 = CARTESIAN_POINT ( 'NONE',  ( 50.79999999999999716, 69.84999999999999432, 257.1750000000000114 ) ) ;
#5148 = CARTESIAN_POINT ( 'NONE',  ( -254.0000000000000000, 93.66249999999999432, 95.25000000000000000 ) ) ;
#5149 = CARTESIAN_POINT ( 'NONE',  ( 72.17003668186724497, -9.772340378754513779, 14.92562527591103461 ) ) ;
#5150 = CARTESIAN_POINT ( 'NONE',  ( 105.1735626975883662, -45.17443245699572429, 25.20713798863899413 ) ) ;
#5152 = AXIS2_PLACEMENT_3D ( 'NONE', #84294, #43363, #15236 ) ;
#5151 = CARTESIAN_POINT ( 'NONE',  ( 102.3506485400807975, -46.05136549539959390, 123.2041967044829818 ) ) ;
#5153 = DIRECTION ( 'NONE',  ( 0.7071067811864661934, 0.7071067811866289521, 7.071067811864654918E-16 ) ) ;
#5154 = EDGE_LOOP ( 'NONE', ( #63827, #17226, #55272, #36192 ) ) ;
#5155 = CIRCLE ( 'NONE', #815, 3.299999999999999822 ) ;
#5156 = DIRECTION ( 'NONE',  ( 0.9068632946707807507, -0.4214249218767880945, 9.080193194566099635E-16 ) ) ;
#5157 = CARTESIAN_POINT ( 'NONE',  ( 82.81648124396200217, -18.63640413217068925, 6.749771997051031036 ) ) ;
#5158 = ORIENTED_EDGE ( 'NONE', *, *, #87521, .T. ) ;
#5159 = ORIENTED_EDGE ( 'NONE', *, *, #12701, .F. ) ;
#5160 = ADVANCED_FACE ( 'NONE', ( #81283 ), #26290, .F. ) ;
#5161 = CARTESIAN_POINT ( 'NONE',  ( 56.06670390244700997, -79.67844715994098692, 85.21780685541799016 ) ) ;
#5162 = ORIENTED_EDGE ( 'NONE', *, *, #61363, .T. ) ;
#5163 = ORIENTED_EDGE ( 'NONE', *, *, #6131, .T. ) ;
#5164 = DIRECTION ( 'NONE',  ( 0.000000000000000000, 1.000000000000000000, 0.000000000000000000 ) ) ;
#5165 = AXIS2_PLACEMENT_3D ( 'NONE', #51868, #50994, #16492 ) ;
#5166 = CARTESIAN_POINT ( 'NONE',  ( 102.0478764085966361, -45.04113848309104640, 51.56670554236298187 ) ) ;
#5167 = CARTESIAN_POINT ( 'NONE',  ( 114.1397626436471171, -29.04081378529519597, 199.4841967044819739 ) ) ;
#5168 = CARTESIAN_POINT ( 'NONE',  ( 98.10941331148539746, -42.08998169807674117, 161.7556252759109725 ) ) ;
#5170 = CARTESIAN_POINT ( 'NONE',  ( 115.9265467165007379, -42.18176083994490000, 14.38705384733995984 ) ) ;
#5169 = CARTESIAN_POINT ( 'NONE',  ( 97.87036982965192067, -40.65816500629669150, 21.64744875867875251 ) ) ;
#5171 = CARTESIAN_POINT ( 'NONE',  ( -127.0239848601435995, 53.97500000000000142, 30.16249999999999787 ) ) ;
#5172 = VECTOR ( 'NONE', #43299, 1000.000000000000000 ) ;
#5173 = CARTESIAN_POINT ( 'NONE',  ( 188.5667039024479834, -62.87844715994099687, 137.2178068554150059 ) ) ;
#5175 = ORIENTED_EDGE ( 'NONE', *, *, #61362, .T. ) ;
#5174 = EDGE_CURVE ( 'NONE', #45687, #15550, #19931, .T. ) ;
#5176 = ADVANCED_FACE ( 'NONE', ( #41690 ), #53967, .F. ) ;
#5177 = ORIENTED_EDGE ( 'NONE', *, *, #32590, .T. ) ;
#5178 = CIRCLE ( 'NONE', #55924, 1.000000000000000888 ) ;
#5179 = CYLINDRICAL_SURFACE ( 'NONE', #41512, 13.00000000000000355 ) ;
#5180 = CARTESIAN_POINT ( 'NONE',  ( 113.1256532486054880, -46.02994946121840769, 223.0480062282919675 ) ) ;
#5181 = ORIENTED_EDGE ( 'NONE', *, *, #52435, .F. ) ;
#5182 = CARTESIAN_POINT ( 'NONE',  ( 117.1973380236488111, -34.26920065746595867, 209.0156252759109634 ) ) ;
#5183 = CARTESIAN_POINT ( 'NONE',  ( 100.9546727506802455, -28.70702577259136135, 35.59395861520961546 ) ) ;
#5184 = AXIS2_PLACEMENT_3D ( 'NONE', #72080, #69958, #78903 ) ;
#5185 = CARTESIAN_POINT ( 'NONE',  ( -21.51128027773100015, 61.17290208904554305, 31.44902489669063073 ) ) ;
#5186 = EDGE_CURVE ( 'NONE', #48446, #25704, #67627, .T. ) ;
#5187 = LINE ( 'NONE', #41035, #37729 ) ;
#5188 = CARTESIAN_POINT ( 'NONE',  ( 140.0667039024470171, -90.27844715994091018, 51.21780685541800437 ) ) ;
#5190 = CARTESIAN_POINT ( 'NONE',  ( 188.5667039024479834, -62.87844715994099687, 257.2178068554150059 ) ) ;
#5189 = CARTESIAN_POINT ( 'NONE',  ( 115.1018088917358426, -38.78897616956993488, 277.6356252759109680 ) ) ;
#5191 = CARTESIAN_POINT ( 'NONE',  ( 101.9933622192556015, -45.44592330270667446, 173.1564353148846465 ) ) ;
#5192 = DIRECTION ( 'NONE',  ( 0.7071067811989762975, -0.7071067811741188480, 2.899137802814003655E-29 ) ) ;
#5193 = CARTESIAN_POINT ( 'NONE',  ( 19.56670390244643443, -25.42844715994203852, 180.4678068554150911 ) ) ;
#5194 = LINE ( 'NONE', #27416, #34155 ) ;
#5195 = DIRECTION ( 'NONE',  ( 1.000000000000000000, 4.163336342344333240E-14, 0.000000000000000000 ) ) ;
#5196 = EDGE_CURVE ( 'NONE', #72082, #39122, #33106, .T. ) ;
#5197 = DIRECTION ( 'NONE',  ( -1.000000000000000000, 0.000000000000000000, 1.094868876412250136E-15 ) ) ;
#5199 = ORIENTED_EDGE ( 'NONE', *, *, #31953, .T. ) ;
#5198 = DIRECTION ( 'NONE',  ( -0.000000000000000000, -0.000000000000000000, -1.000000000000000000 ) ) ;
#5200 = PLANE ( 'NONE',  #7466 ) ;
#5201 = CARTESIAN_POINT ( 'NONE',  ( 118.8150946519381250, -38.46269469016341702, 223.7099109901969598 ) ) ;
#5202 = CARTESIAN_POINT ( 'NONE',  ( 114.7260775003150712, -43.80144150384058577, 119.2327681330539804 ) ) ;
#5203 = CARTESIAN_POINT ( 'NONE',  ( 118.1491249375158645, -36.11907637682050165, 269.8822919425776945 ) ) ;
#5204 = DIRECTION ( 'NONE',  ( 1.000000000000000000, 4.163336342344333240E-14, 0.000000000000000000 ) ) ;
#5205 = DIRECTION ( 'NONE',  ( 0.000000000000000000, 0.000000000000000000, -1.000000000000000000 ) ) ;
#5206 = FACE_OUTER_BOUND ( 'NONE', #62465, .T. ) ;
#5207 = DIRECTION ( 'NONE',  ( 0.000000000000000000, 0.000000000000000000, -1.000000000000000000 ) ) ;
#5208 = PLANE ( 'NONE',  #34085 ) ;
#5209 = CIRCLE ( 'NONE', #44293, 9.425000000000000711 ) ;
#5210 = AXIS2_PLACEMENT_3D ( 'NONE', #35376, #34934, #21779 ) ;
#5211 = AXIS2_PLACEMENT_3D ( 'NONE', #74162, #11938, #49566 ) ;
#5212 = CIRCLE ( 'NONE', #19732, 0.5000000000000004441 ) ;
#5213 = ORIENTED_EDGE ( 'NONE', *, *, #41344, .F. ) ;
#5214 = VERTEX_POINT ( 'NONE', #19029 ) ;
#5215 = CARTESIAN_POINT ( 'NONE',  ( 104.1185212827848545, -44.74603268130591971, 141.7181341137909669 ) ) ;
#5216 = EDGE_CURVE ( 'NONE', #38814, #71713, #42213, .T. ) ;
#5218 = ORIENTED_EDGE ( 'NONE', *, *, #19222, .T. ) ;
#5217 = PLANE ( 'NONE',  #2388 ) ;
#5219 = DIRECTION ( 'NONE',  ( 0.000000000000000000, 1.000000000000000000, 0.000000000000000000 ) ) ;
#5220 = CARTESIAN_POINT ( 'NONE',  ( 113.0643619202157453, -28.22920495858477352, 125.5870538473399591 ) ) ;
#5221 = DIRECTION ( 'NONE',  ( 0.000000000000000000, 0.000000000000000000, 1.000000000000000000 ) ) ;
#5222 = EDGE_CURVE ( 'NONE', #10055, #87762, #62150, .T. ) ;
#5223 = EDGE_CURVE ( 'NONE', #89871, #64817, #41244, .T. ) ;
#5224 = CARTESIAN_POINT ( 'NONE',  ( 92.81551872686563343, -113.5468731908973723, -19.18411693322874356 ) ) ;
#5225 = CARTESIAN_POINT ( 'NONE',  ( -75.67519899969657615, 76.18740257834568297, 91.26337341211453236 ) ) ;
#5226 = CARTESIAN_POINT ( 'NONE',  ( 97.81169789812091153, -40.51742632959496859, 107.6355761348045519 ) ) ;
#5227 = EDGE_CURVE ( 'NONE', #72723, #16229, #68530, .T. ) ;
#5229 = CARTESIAN_POINT ( 'NONE',  ( 116.4719273984281784, -32.36179259691358823, 59.16038718067295576 ) ) ;
#5228 = VECTOR ( 'NONE', #47995, 1000.000000000000114 ) ;
#5230 = VERTEX_POINT ( 'NONE', #13559 ) ;
#5231 = ORIENTED_EDGE ( 'NONE', *, *, #85702, .F. ) ;
#5232 = VERTEX_POINT ( 'NONE', #48058 ) ;
#5233 = LINE ( 'NONE', #32922, #8062 ) ;
#5235 = CARTESIAN_POINT ( 'NONE',  ( -28.99999999999997513, 172.0000000000000000, 183.8826257785461280 ) ) ;
#5234 = CARTESIAN_POINT ( 'NONE',  ( 113.2097911582632292, -29.11871762112829032, 160.5356252759109736 ) ) ;
#5236 = VECTOR ( 'NONE', #48189, 1000.000000000000000 ) ;
#5237 = PLANE ( 'NONE',  #87148 ) ;
#5238 = DIRECTION ( 'NONE',  ( 0.7118375500324360949, -0.7021341844428906631, 0.01717234406061140736 ) ) ;
#5239 = DIRECTION ( 'NONE',  ( 0.000000000000000000, -1.000000000000000000, 0.000000000000000000 ) ) ;
#5240 = DIRECTION ( 'NONE',  ( 0.0001484127182026448726, -0.8660253910675250744, -0.5000000000000052180 ) ) ;
#5241 = DIRECTION ( 'NONE',  ( -4.237773401492740281E-14, 1.000000000000000000, 0.000000000000000000 ) ) ;
#5242 = CARTESIAN_POINT ( 'NONE',  ( 97.64212626138829876, -32.24102647341085515, 75.97276813305397525 ) ) ;
#5243 = VERTEX_POINT ( 'NONE', #75793 ) ;
#5244 = ORIENTED_EDGE ( 'NONE', *, *, #6536, .F. ) ;
#5245 = DIRECTION ( 'NONE',  ( 0.000000000000000000, -1.000000000000000000, 0.000000000000000000 ) ) ;
#5246 = DIRECTION ( 'NONE',  ( 1.000000000000000000, 0.000000000000000000, 0.000000000000000000 ) ) ;
#5247 = CARTESIAN_POINT ( 'NONE',  ( 107.0664832912739257, -50.22944715994095333, 312.1356252759112522 ) ) ;
#5248 = CARTESIAN_POINT ( 'NONE',  ( 102.2276451341571999, -43.90295244235954897, 149.9099951314959753 ) ) ;
#5249 = B_SPLINE_CURVE_WITH_KNOTS ( 'NONE', 3,
 ( #421, #69921, #7686, #31875, #66846, #30098, #30983, #23310, #25064, #85973, #57797, #80050, #11442, #79605, #3291, #58670, #17805, #51408 ),
 .UNSPECIFIED., .F., .F.,
 ( 4, 2, 2, 2, 2, 2, 2, 2, 4 ),
 ( 0.5000352890896443414, 0.5625308779534388126, 0.6250264668172332838, 0.6875220556810277550, 0.7500176445448221152, 0.8125132334086166974, 0.8750088222724110576, 0.9375044111362055288, 1.000000000000000000 ),
 .UNSPECIFIED. ) ;
#5250 = EDGE_CURVE ( 'NONE', #52977, #6408, #68975, .T. ) ;
#5251 = DIRECTION ( 'NONE',  ( 0.000000000000000000, 0.000000000000000000, -1.000000000000000000 ) ) ;
#5252 = ORIENTED_EDGE ( 'NONE', *, *, #17423, .T. ) ;
#5253 = ORIENTED_EDGE ( 'NONE', *, *, #11813, .T. ) ;
#5254 = CARTESIAN_POINT ( 'NONE',  ( 107.0664832912739399, -36.72944715994095333, 311.6356252759109680 ) ) ;
#5255 = ORIENTED_EDGE ( 'NONE', *, *, #11778, .F. ) ;
#5256 = ORIENTED_EDGE ( 'NONE', *, *, #32648, .F. ) ;
#5257 = CARTESIAN_POINT ( 'NONE',  ( 77.42411991178802566, -19.49143581486272225, 6.902478035881912000 ) ) ;
#5258 = CARTESIAN_POINT ( 'NONE',  ( 111.4343887032284783, -44.43980907907789657, 209.4187261630399632 ) ) ;
#5259 = LINE ( 'NONE', #59315, #77191 ) ;
#5260 = LINE ( 'NONE', #5719, #32735 ) ;
#5261 = DIRECTION ( 'NONE',  ( -0.000000000000000000, -1.000000000000000000, -0.000000000000000000 ) ) ;
#5262 = AXIS2_PLACEMENT_3D ( 'NONE', #49235, #6578, #70148 ) ;
#5263 = EDGE_LOOP ( 'NONE', ( #87268, #44025, #39183, #38550 ) ) ;
#5264 = ORIENTED_EDGE ( 'NONE', *, *, #25267, .F. ) ;
#5266 = ADVANCED_FACE ( 'NONE', ( #1282 ), #77583, .F. ) ;
#5265 = AXIS2_PLACEMENT_3D ( 'NONE', #68587, #61743, #89479 ) ;
#5267 = AXIS2_PLACEMENT_3D ( 'NONE', #84018, #63105, #69933 ) ;
#5268 = ORIENTED_EDGE ( 'NONE', *, *, #31343, .F. ) ;
#5269 = ORIENTED_EDGE ( 'NONE', *, *, #50579, .F. ) ;
#5270 = EDGE_CURVE ( 'NONE', #88352, #83829, #83961, .T. ) ;
#5271 = CARTESIAN_POINT ( 'NONE',  ( 99.55502339443899018, -39.99451353983162960, 229.4709475124479638 ) ) ;
#5272 = EDGE_CURVE ( 'NONE', #87926, #37760, #43933, .T. ) ;
#5273 = CARTESIAN_POINT ( 'NONE',  ( 115.1840797895677611, -43.30599572718466561, 88.28419670448195689 ) ) ;
#5274 = CARTESIAN_POINT ( 'NONE',  ( 109.6783822832554449, -47.44587409406599932, 87.75467289495897205 ) ) ;
#5275 = CARTESIAN_POINT ( 'NONE',  ( 111.1802904571995896, -44.25639671664211505, 249.5838068554169524 ) ) ;
#5276 = B_SPLINE_SURFACE_WITH_KNOTS ( 'NONE', 3, 3, ( 
 ( #34173, #27817, #21466, #63692, #1473, #69611, #62335, #56858, #55493, #49135, #82810, #35515, #70056, #21923, #42325, #89613, #76419, #1016, #20571, #41874, #28721, #6930, #83249, #48687, #84148, #27370, #49589, #15094, #8283, #48240, #84599, #35979, #22362, #41430, #69159, #34631, #118, #80017, #3694, #9616, #51374, #37776, #43680, #71415, #30951, #10507, #31387, #17332, #23712, #9177, #44564, #79119, #10070, #15998, #16885, #72740, #59082, #72300, #78690, #65473, #86820, #58213, #44113, #65030, #3260, #58640, #17771, #78239, #57763, #64585, #85500, #36877, #2367, #38212, #16437, #86374, #65908, #24587, #22818, #24147, #1916, #51819, #79570, #30068, #23281, #85942, #45010, #52252, #64142, #2814, #50945, #71853, #37326, #29613, #30509, #45445, #85048, #8741, #36442, #57302, #50492, #74970, #18662, #10946, #59972, #38651, #45892, #74521, #61326, #66352, #68162, #39095, #73169, #66804, #53599, #33636, #89049, #54041, #46341, #5034, #39992, #32733, #60425, #26810, #5944, #59528, #4591, #31836, #5492, #11854, #87266, #26372, #32276, #54491, #82255, #20014, #39547, #88173, #25930, #87705, #74069, #25472, #53142, #19108, #25030, #81365, #4136, #60887, #11401, #67250, #80914, #46790, #81800, #88616, #52693, #12300, #19552, #67708, #33188, #80452, #47242, #18211, #12756, #40442, #73625, #83149, #76313, #28607, #69955, #82705, #49484, #21354, #7722, #6373, #68612, #909, #54939, #40885, #77221, #70401, #13640, #89505, #49027, #27716, #27265, #42663, #7282, #63129, #1364, #84502, #20463, #55393, #35411, #21815, #63585, #76763, #34523, #34063, #62682, #48579, #61767, #56294, #48135, #75869, #41324, #42225, #84038, #14087, #69052, #20906, #14993, #8175, #55839, #35867, #29067, #75426, #56755, #41771, #14548, #47691, #34968, #6820, #62230, #455, #28149, #69506, #13200, #16, #83589, #49932, #43569, #16778, #58104, #30405, #3150, #85837, #22710, #15447, #65368, #58538, #23171, #1815, #29514, #23609, #84944, #85395, #8633, #36328, #64037, #57196, #77667, #71307, #9076, #70861, #50381, #78129, #51715, #51267, #44459, #36776, #43117, #15890, #64478, #2260, #37219, #30849, #29963, #37671, #57651, #22261, #79010, #50842, #78580, #16332, #44009, #86263, #71745, #72190, #9515, #9966, #64923, #2709, #24045, #69803, #49783, #22559, #7126, #7575, #42962, #70696, #48875, #41615, #8476, #34821, #76615, #62075, #77068, #49335, #1212, #42072, #57045, #55677, #14396, #89811, #83429, #21204, #76158, #62530, #305, #28002, #13489, #28452, #63425, #77511, #41174, #63889, #28918, #83891, #15293, #34365, #14848, #35261, #84790, #36173, #62970, #56136, #42516, #48421, #13937, #35713, #1667, #29368, #22114, #21663, #69353, #70245, #8019, #56603, #20749, #84348, #50233, #68904, #6670, #749, #27563, #55243, #82995, #39090, #66801, #3255, #25026, #60421, #59968, #10503, #45442, #31383, #38208, #53136, #87701, #25927, #73165, #25469, #31831, #59078, #53594, #32273, #67246, #4133, #52689, #10943, #17766, #38646, #80910, #4587, #17327, #24582, #52249, #45007, #86817, #3691, #80013, #72297, #87262, #18659, #46337, #10065, #32729, #74066, #80449, #11850, #30948, #73621, #66348, #81362, #5031, #59525, #18207, #11398, #72735, #65905, #39543, #88168, #19103, #37772, #45887, #65469, #58637, #86371, #24142, #79567, #51816, #20901, #7276, #61763, #26807, #20459, #34963, #41766, #54935, #13196, #12751, #13635, #55834, #26368, #5941, #40439, #33632, #74966, #68156, #76308, #54488, #6815, #48574, #62675, #60882, #75863, #39989, #34518, #48129, #81796, #61323, #34059, #62225, #69501, #12297, #40881, #89045, #54037, #19549, #67703, #82251, #20010, #33184, #47687, #47239, #83584, #10, #14081, #75422, #74517, #68608, #5488, #6368, #41320, #450, #88613, #28142, #89500, #46786, #27261, #82699, #69048, #27710, #55387, #83142, #43110, #7715, #22705, #69949, #36771, #29508, #64474, #77661, #57645, #30400, #14987, #15442, #50836, #78575, #56750, #49479, #16326, #42656, #84496, #35405, #84939, #57190, #9071, #49926, #64918, #63580, #22255, #63123, #904, #2256, #50377, #29959, #70856, #85390, #58097, #70396, #8628, #44003, #71739, #36322, #77216, #9510, #8169, #64032, #28601, #78124, #15886, #23165, #1810, #2703, #1359, #43564, #56289 ),
 ( #84033, #21809, #37214, #35861, #71303, #29061, #21348, #49022, #76758, #14542, #42220, #18543, #72184, #51710, #44454, #18093, #24484, #9961, #38985, #79461, #80793, #4922, #46228, #52146, #45339, #73059, #10398, #58970, #72633, #52586, #80344, #16773, #38540, #73963, #73509, #24040, #86707, #44904, #17224, #66694, #11280, #39439, #79908, #4480, #10834, #38103, #67141, #45782, #11740, #17663, #66234, #4024, #31276, #31727, #32168, #59863, #30843, #87595, #59425, #25353, #37665, #65362, #53025, #3144, #79004, #32612, #85832, #65793, #58532, #87156, #3579, #86257, #23603, #24923, #51261, #13975, #7170, #5371, #68045, #20351, #34408, #76196, #89395, #47126, #81250, #75310, #61220, #53485, #41211, #33519, #74863, #27155, #54828, #19000, #13089, #48457, #48024, #88505, #88941, #19443, #26257, #68938, #75760, #41654, #26694, #13529, #19895, #12637, #69392, #6708, #55280, #82146, #40774, #54376, #5831, #47576, #62116, #82594, #33069, #89850, #33955, #27600, #46684, #74414, #83039, #67594, #12188, #20792, #60313, #53935, #39873, #61654, #40324, #60769, #88049, #68499, #25812, #81693, #6265, #69840, #42551, #84825, #8967, #50725, #63923, #21700, #55718, #49821, #35751, #28040, #15775, #14437, #21242, #83465, #29404, #43452, #1249, #35295, #70279, #36665, #2144, #43000, #64369, #78006, #62565, #71192, #28956, #1699, #8513, #84385, #48912, #49374, #22154, #15327, #8056, #78463, #57083, #63464, #340, #77108, #29851, #22592, #50266, #85278, #57539, #790, #76651, #23049, #16222, #77546, #42114, #7612, #43900, #63008, #56638, #28489, #56178, #71634, #70739, #36210, #34860, #83928, #14886, #65255, #57988, #32848, #37992, #23496, #53713, #3033, #5612, #19674, #33304, #65688, #60090, #87826, #23929, #78902, #85721, #30290, #5151, #19231, #4710, #9851, #44798, #74637, #67820, #18778, #40104, #81480, #37108, #46907, #32388, #39660, #74198, #25590, #2594, #51602, #53263, #81033, #72526, #26486, #60543, #46461, #64813, #79352, #12414, #88291, #26046, #61002, #88731, #30732, #51161, #54159, #81921, #11976, #16660, #72079, #47356, #37555, #67360, #44345, #58427, #9399, #86154, #17113, #10287, #7832, #61439, #41001, #33750, #7389, #13754, #89169, #28263, #68721, #70064, #84159, #35527, #41439, #34642, #62346, #89623, #48249, #61891, #41885, #69621, #6062, #27826, #63251, #62787, #13315, #75981, #34185, #6487, #55958, #564, #28729, #69169, #83702, #126, #27379, #56416, #35080, #1026, #6940, #55504, #83257, #20582, #21018, #21473, #49147, #20132, #76883, #48696, #14664, #26939, #54607, #42334, #82367, #68281, #21933, #75085, #55057, #47805, #76426, #82818, #75542, #12876, #14205, #40561, #3270, #86383, #84612, #57312, #9628, #23722, #65484, #78698, #36450, #70521, #64596, #50504, #42778, #30520, #64155, #77784, #15562, #79131, #85059, #37334, #51382, #30961, #63702, #16447, #8292, #65039, #23290, #22370, #8750, #36887, #2823, #44576, #15103, #43688, #1928, #29182, #50047, #35988, #29624, #22826, #1482, #43235, #56870, #49602, #58222, #16897, #78250, #77328, #16007, #70977, #71425, #50953, #37785, #9190, #72308, #2377, #30077, #57771, #85512, #10081, #58648, #85951, #44124, #71863, #10518, #25483, #72749, #39558, #32286, #67261, #80464, #60439, #33198, #17780, #18223, #53609, #81375, #59541, #52261, #19120, #45458, #87275, #38223, #87714, #59984, #11866, #52704, #67718, #66361, #25041, #65916, #4148, #31848, #86829, #73178, #10956, #38661, #24159, #39108, #74083, #88183, #51829, #74534, #5045, #4602, #25939, #45021, #53154, #45903, #5504, #46801, #73634, #66817, #80923, #59093, #24598, #46352, #12310, #40003, #32743, #18671, #80026, #60899, #79580, #17341, #31396, #3703, #11410, #49042, #13653, #68622, #62240, #76776, #83601, #6834, #54950, #54504, #55406, #7735, #68175, #47701, #82267, #75441, #75881, #76323, #21368, #54055, #82717, #13212, #5957, #33646, #81814, #6386, #34075, #74982, #20025, #61337, #35426, #14102, #470, #61780, #26382, #40895, #19565, #89064, #27, #14564, #47253, #42238, #89519, #88628, #27275, #69064, #69966, #12766, #69519, #20478, #48146, #40455, #27727, #26823, #41783, #34537, #7295, #41335, #34980, #83161, #20919, #48590, #28164, #55851, #62693, #1375, #2721, #56766, #36340, #21827 ),
 ( #78141, #23185, #37230, #63142, #23620, #78592, #43580, #9529, #84051, #64496, #29527, #44471, #58116, #64049, #15900, #2272, #8186, #35879, #85410, #64935, #85848, #71761, #71319, #63596, #9087, #36788, #29974, #70417, #57665, #30419, #51278, #50853, #43129, #16344, #79025, #16791, #44022, #57210, #29079, #72202, #9977, #42677, #22271, #84514, #49946, #77678, #15460, #920, #70872, #28620, #56306, #49497, #77231, #15003, #8643, #1827, #84954, #22720, #50396, #37682, #31290, #18112, #88065, #53499, #18559, #73076, #59439, #24056, #39000, #86277, #53042, #45797, #80809, #4041, #73977, #46698, #58983, #31743, #67155, #4937, #10855, #65809, #32632, #86724, #38554, #51725, #11297, #73523, #25374, #66249, #81265, #79923, #87170, #79478, #17677, #45356, #10414, #24497, #52159, #24936, #65382, #52600, #87610, #11757, #3162, #25830, #46242, #66710, #39454, #58548, #4496, #80361, #19013, #60330, #32181, #59877, #74429, #72648, #38117, #30860, #17238, #44917, #3597, #27168, #74877, #48040, #82608, #13542, #19460, #20367, #76213, #62581, #54843, #82160, #75775, #357, #7183, #41226, #68512, #68061, #68956, #21256, #81709, #61234, #5846, #88956, #40343, #33534, #41670, #19909, #62131, #13989, #28054, #26273, #6725, #5388, #89864, #34422, #47144, #26710, #89410, #27614, #34871, #67609, #6280, #54395, #12652, #47591, #33087, #75326, #13106, #88519, #40790, #33970, #48926, #55296, #69408, #61674, #39892, #83054, #60785, #20806, #48470, #55734, #53949, #83482, #12203, #35764, #8073, #63476, #76669, #1715, #36682, #50741, #14451, #37125, #2158, #57095, #23069, #7625, #78022, #43015, #58005, #71651, #77560, #29417, #15790, #21715, #49386, #8982, #78476, #9413, #85293, #84838, #77121, #22608, #50280, #43465, #83944, #71206, #16239, #64826, #64383, #56652, #29867, #2608, #30309, #57551, #70753, #42562, #43915, #85738, #56191, #1263, #70295, #28969, #14898, #84399, #23512, #22166, #42127, #69854, #35311, #807, #63025, #28500, #49833, #15345, #8527, #36225, #63935, #38889, #46135, #16678, #45248, #10304, #30749, #86170, #44363, #31180, #58879, #37571, #44812, #58441, #87951, #66597, #52927, #86616, #78917, #38010, #72092, #23944, #52492, #39345, #9864, #73866, #17127, #51176, #72540, #31630, #11651, #67051, #32076, #24389, #72968, #65271, #80255, #3050, #4389, #59333, #59772, #17567, #87503, #60215, #65704, #10735, #80698, #18447, #52052, #79368, #4831, #3485, #79813, #51622, #24827, #87061, #25261, #38439, #32514, #66145, #3932, #18000, #45681, #73414, #11186, #34316, #82051, #26170, #61129, #89755, #82942, #33872, #55182, #68849, #53389, #62021, #19805, #54737, #89303, #75218, #18903, #40230, #12999, #6184, #88857, #41566, #47929, #54287, #81157, #67948, #27506, #13439, #75670, #76104, #41125, #81608, #46588, #48370, #69301, #40686, #32974, #88409, #6620, #53838, #47485, #67491, #5279, #82500, #68406, #61567, #7072, #13883, #12094, #19358, #74325, #20703, #27067, #39778, #34770, #47030, #62473, #25716, #60670, #20260, #74765, #12544, #5737, #26611, #33427, #56998, #84741, #21152, #42910, #78374, #77913, #28398, #63375, #49284, #56086, #71106, #15690, #43812, #1157, #43362, #49734, #77014, #71552, #50176, #85187, #22064, #70649, #28862, #35662, #56551, #8881, #22500, #35207, #2055, #63835, #36580, #48824, #76561, #64283, #7518, #83378, #29760, #22958, #83834, #42021, #1614, #70191, #69749, #50632, #77457, #57445, #9314, #37015, #62917, #7963, #16136, #249, #27952, #29315, #14795, #14342, #15235, #84293, #695, #55630, #21609, #42462, #8423, #36119, #78816, #3828, #57897, #24720, #38341, #9758, #23844, #51949, #52384, #59665, #30203, #58774, #51512, #44254, #37461, #85634, #44704, #72432, #51076, #58342, #71988, #11543, #80147, #66490, #10200, #2504, #79259, #23409, #65160, #66039, #52821, #16576, #87396, #30646, #64720, #86071, #45142, #25156, #80594, #45578, #37906, #86514, #2944, #31521, #17021, #17897, #72867, #73304, #31081, #11078, #73760, #65607, #24283, #4278, #31971, #3388, #79707, #18340, #17462, #10637, #59226, #86955, #38784, #46026, #67840, #82836, #81499, #40121, #87845, #19251, #46924, #11992, #88307, #60564, #26065, #39238, #54179, #89194, #13331, #66945, #89642, #54625, #19693, #75563, #60111 ),
 ( #75104, #47373, #40580, #46481, #12892, #41018, #27395, #81942, #74659, #68298, #55074, #34207, #6078, #5631, #5170, #33767, #48263, #18797, #53733, #32864, #12432, #67381, #33321, #68740, #61021, #26958, #6510, #61909, #20597, #88749, #81051, #61460, #26507, #74218, #75997, #82386, #20150, #4727, #32406, #39678, #47823, #25608, #53282, #30879, #44040, #582, #34658, #29995, #15919, #6958, #85865, #83272, #143, #62361, #9546, #23635, #71335, #14226, #50416, #79042, #72221, #23203, #44489, #58133, #41458, #51295, #9107, #71775, #78608, #64511, #27841, #29541, #2291, #85428, #78159, #58563, #37251, #43596, #69186, #57226, #16807, #2738, #64954, #65400, #30438, #69636, #55520, #37701, #86293, #57685, #21039, #76443, #9992, #41902, #36803, #48713, #7405, #3180, #50870, #16363, #24073, #51743, #35096, #62803, #84971, #13774, #22741, #3612, #32651, #73094, #74446, #88535, #12221, #18129, #39017, #66727, #4059, #52619, #66268, #46258, #73994, #10432, #32200, #67626, #67173, #17695, #80380, #38570, #45375, #60347, #4955, #33105, #45813, #88085, #4512, #31758, #60802, #39470, #39909, #11316, #59897, #73542, #24952, #87629, #25848, #11773, #24512, #81282, #53059, #53514, #38135, #65827, #19028, #86741, #72665, #80829, #31307, #46715, #25393, #5410, #18578, #26289, #79493, #10872, #17255, #44935, #59003, #52176, #59454, #79939, #87188, #27186, #12672, #27633, #89882, #41689, #82626, #7643, #6297, #54861, #40363, #33988, #61690, #26729, #13123, #75344, #40807, #53966, #68974, #14005, #28070, #81726, #14466, #69424, #34440, #375, #74894, #55314, #20387, #35332, #48944, #48057, #6741, #83070, #88973, #54412, #76231, #55753, #76686, #62599, #62149, #82175, #20824, #48489, #7199, #61251, #34889, #83500, #42143, #21271, #89425, #69871, #63044, #826, #19478, #75792, #19930, #47161, #68077, #33549, #68529, #47611, #13558, #41243, #5864, #58023, #36244, #78497, #2629, #44381, #42582, #57571, #21731, #16257, #2179, #63496, #77582, #15810, #43932, #23531, #83960, #22629, #15367, #8092, #1281, #49403, #8546, #63954, #14916, #22184, #35782, #65292, #71670, #30331, #1733, #56209, #43032, #77139, #28986, #29888, #16699, #70317, #51193, #84416, #28516, #49853, #8999, #78934, #72110, #9433, #29434, #50302, #56672, #70774, #85315, #23088, #57114, #71227, #9884, #37144, #84860, #78042, #43483, #36700, #64845, #85759, #37591, #64401, #50762, #52513, #79833, #74341, #52950, #87972, #24847, #45704, #3951, #38461, #31652, #73885, #25285, #38030, #4850, #66618, #80718, #51641, #23964, #46156, #10326, #86189, #32536, #25734, #58897, #44831, #4409, #72988, #72559, #53409, #80278, #18467, #46608, #39795, #65722, #10756, #11672, #67071, #18922, #32095, #17589, #79385, #18021, #59352, #17147, #39365, #3504, #31201, #86635, #87524, #60241, #87081, #24409, #66165, #81176, #12112, #11208, #3068, #30769, #58459, #52073, #73435, #59792, #45271, #38908, #60689, #82072, #54754, #47946, #40702, #83397, #89774, #6201, #32991, #19822, #13902, #55204, #27525, #27968, #82961, #33445, #88427, #271, #21172, #27085, #74784, #40251, #20718, #5754, #89322, #19375, #47050, #34334, #82519, #20281, #48841, #55646, #53856, #61148, #26188, #48388, #33888, #81625, #76122, #88873, #62492, #76581, #14362, #61585, #75687, #13456, #47503, #68425, #75240, #41584, #69318, #7092, #67512, #34786, #26629, #12564, #5302, #67968, #41142, #54305, #13015, #68866, #6638, #62040, #83852, #21629, #8898, #63851, #1634, #85649, #64738, #28420, #7982, #713, #64301, #70666, #56104, #85209, #35682, #37032, #51093, #2522, #8441, #29334, #57014, #56570, #15256, #28881, #36599, #2072, #62934, #84756, #30223, #29777, #70212, #42929, #1176, #63395, #22975, #57468, #23427, #36138, #50650, #22519, #84313, #78831, #78392, #57914, #50199, #77932, #15706, #77474, #43381, #16154, #43829, #77035, #71568, #71123, #9329, #49302, #14813, #42040, #42480, #35228, #69767, #7539, #22084, #49749, #3848, #3405, #30662, #31988, #17479, #80167, #80611, #46045, #86087, #31096, #52401, #38804, #25175, #31542, #10217, #9775, #72884, #86535, #37479, #73325, #58360, #65181, #2960, #86975, #11098, #51967, #51530, #58790, #66509, #4298, #38357, #59682, #17914, #44271, #87414, #79723, #59245 ),
 ( #23858, #79280, #17040, #24736, #24301, #44720, #45593, #72449, #52837, #18360, #16592, #45161, #10651, #66057, #72008, #37922, #65622, #64582, #2362, #28718, #50489, #85938, #85495, #35976, #70964, #56854, #63687, #78686, #23277, #51371, #8738, #50941, #57299, #84596, #79116, #57759, #2808, #29610, #78233, #36438, #43222, #64138, #16434, #30065, #42764, #9611, #71411, #44110, #56402, #84145, #71850, #15091, #1012, #37322, #30506, #1470, #49585, #9174, #77768, #77316, #58208, #85043, #65027, #16880, #44560, #70504, #15547, #23709, #7821, #35512, #36874, #22359, #21919, #22814, #1913, #8278, #63234, #29167, #50033, #15995, #43676, #51443, #71919, #30131, #2877, #65970, #3762, #9683, #64646, #31451, #57828, #37392, #85118, #10132, #72365, #24214, #65094, #80078, #78752, #30576, #22886, #16505, #44184, #9245, #85564, #23342, #51009, #36509, #79194, #86447, #10570, #64213, #86884, #51880, #16951, #72803, #57376, #37841, #58275, #17833, #59156, #86006, #44631, #38274, #79634, #58706, #24647, #17393, #2434, #50562, #52314, #45510, #23778, #43747, #36941, #45075, #65539, #3322, #78303, #16066, #31014, #73232, #1982, #29681, #71484, #87330, #66872, #59592, #33254, #39607, #25092, #54114, #4654, #6013, #20082, #33704, #67313, #60493, #88239, #25536, #74145, #87774, #67773, #5562, #31901, #53664, #89124, #88684, #39169, #11920, #60041, #32340, #81870, #26441, #54556, #5102, #19621, #25995, #53211, #82322, #60955, #61395, #32798, #81431, #19183, #46410, #46854, #47308, #75039, #45958, #12826, #74585, #40511, #52756, #80520, #68231, #18274, #4208, #26883, #47757, #80980, #73695, #12365, #18728, #11472, #11011, #40054, #38716, #66419, #22321, #20533, #83211, #35478, #49548, #1432, #14614, #62293, #6443, #519, #76380, #68676, #56366, #55004, #61835, #34137, #69569, #62743, #7343, #35936, #20972, #77281, #42730, #83655, #15057, #28678, #13264, #84108, #35032, #42286, #49099, #28216, #89571, #79, #55907, #21426, #48649, #29134, #7788, #14159, #40953, #27777, #41833, #21879, #63198, #48201, #70472, #76828, #974, #27330, #82772, #8241, #75935, #13707, #63651, #56814, #41393, #69122, #70019, #55458, #6887, #84564, #75493, #34589, #3658, #86781, #85010, #57721, #10032, #24112, #65867, #79082, #36839, #70928, #64991, #50904, #43185, #30912, #29574, #36401, #8701, #44079, #37284, #71812, #10472, #85462, #51779, #17293, #58171, #79531, #3219, #77737, #58602, #9582, #16845, #23674, #2776, #64105, #64549, #30472, #85901, #23239, #31352, #72258, #78650, #15511, #2328, #86334, #37739, #65437, #38174, #44973, #15956, #1876, #72706, #59043, #51335, #57263, #22777, #50000, #78197, #44523, #50451, #43637, #71375, #9142, #30028, #16401, #47199, #10909, #80415, #73130, #46753, #53102, #38615, #67670, #18169, #19515, #33593, #74935, #80868, #74034, #11814, #39059, #87668, #11358, #81325, #19068, #45411, #67210, #12714, #12256, #52657, #25433, #73584, #45852, #5449, #39951, #68118, #18623, #33145, #39511, #66766, #5899, #74485, #40405, #46301, #4995, #32695, #59936, #88128, #59492, #4552, #60390, #60840, #61288, #79980, #25887, #32238, #4098, #87225, #17734, #53558, #88575, #66310, #26331, #31798, #24551, #54004, #81763, #52214, #24994, #75826, #26770, #61729, #416, #77179, #82216, #84001, #54902, #89012, #82666, #69466, #49444, #14956, #69916, #34481, #20864, #75386, #28108, #47653, #14508, #7240, #35824, #42182, #14050, #62187, #20424, #55355, #28564, #56250, #89925, #27221, #21775, #48094, #27676, #13160, #62642, #34930, #76726, #83107, #42624, #41283, #48533, #40842, #69016, #6782, #89465, #13600, #76274, #41732, #54453, #55793, #48987, #63085, #19972, #70360, #7682, #83548, #35373, #68572, #21313, #867, #8134, #6335, #34026, #16296, #2672, #8591, #36287, #85799, #65333, #86229, #72154, #78541, #63999, #9475, #43975, #64891, #70815, #71709, #37635, #24008, #37184, #43529, #30372, #51683, #58503, #58066, #29931, #29475, #23572, #72604, #43076, #22674, #57155, #50347, #1776, #84904, #3111, #71271, #51233, #30810, #79430, #77625, #78977, #56714, #16741, #44420, #17190, #44876, #9930, #9042, #85358, #49894, #10369, #22219, #63541, #1321, #29028, #84458, #15410, #36742, #78086, #57616, #15849, #64442, #2220, #23129 ),
 ( #50802, #59392, #87122, #38072, #52994, #88017, #12158, #65761, #88473, #53453, #18512, #74385, #58942, #39407, #4449, #19417, #33040, #38954, #80760, #67113, #73029, #10800, #60287, #39845, #60734, #46654, #46197, #38505, #73933, #11713, #4894, #45312, #32584, #67564, #26226, #25779, #18064, #81221, #53905, #81666, #18968, #32137, #3996, #5346, #47097, #17633, #24892, #31696, #52558, #66206, #80318, #74833, #45746, #3548, #31243, #86680, #52114, #24451, #79878, #73478, #11252, #66663, #59835, #25327, #87567, #8828, #68013, #7910, #62866, #83327, #48776, #5799, #83783, #21555, #202, #7468, #21099, #50578, #29260, #15635, #49226, #40300, #641, #33487, #76507, #15180, #1998, #61190, #36527, #69699, #12611, #35155, #76958, #27902, #77404, #49680, #1559, #42412, #57392, #56035, #14743, #55579, #70140, #35608, #14290, #28340, #63325, #1103, #41963, #28813, #63782, #77860, #56496, #64227, #56943, #84239, #50123, #22009, #42857, #70595, #85135, #29700, #8368, #36067, #84685, #22447, #43309, #71054, #22902, #11029, #86900, #3337, #51028, #24229, #58722, #79654, #85581, #86464, #52332, #38733, #31031, #58291, #51895, #66437, #73248, #17411, #44650, #44198, #45093, #87347, #57845, #37407, #71934, #65110, #16523, #9702, #17848, #86022, #38289, #80097, #4224, #2449, #72818, #71500, #65987, #10584, #23357, #2894, #65555, #3778, #31916, #43764, #72382, #30592, #78767, #23794, #9261, #51460, #79208, #64664, #16966, #10150, #25108, #31467, #45525, #37858, #16084, #59172, #36955, #24667, #59611, #78318, #30148, #47773, #18743, #52771, #46428, #33269, #13279, #68691, #33720, #88255, #74602, #39184, #54127, #11488, #68247, #60972, #89589, #6029, #67789, #26012, #74160, #19198, #82338, #20099, #53681, #80997, #75508, #11936, #75056, #87788, #54571, #26457, #12843, #66887, #73711, #61410, #60057, #45976, #40969, #6459, #39624, #4673, #81884, #32813, #32354, #34151, #12380, #89139, #61850, #80535, #25551, #60509, #40526, #26897, #18288, #19637, #67328, #53227, #5577, #81448, #5117, #46867, #40071, #88700, #47324, #21445, #14629, #49114, #77750, #62758, #1450, #84577, #35493, #56829, #70486, #55022, #35954, #76844, #56385, #990, #42302, #20548, #41848, #70035, #7802, #532, #43200, #49564, #55925, #82787, #69587, #63668, #15071, #77296, #15524, #42746, #83223, #48215, #50015, #70944, #63213, #34607, #96, #8254, #55472, #28697, #69137, #6903, #84124, #21893, #29148, #8717, #36419, #13724, #20988, #75950, #22335, #83671, #41409, #64119, #48666, #27347, #62310, #27793, #76396, #14175, #7358, #35048, #28231, #78664, #58614, #86353, #22791, #44538, #79994, #79546, #30042, #65007, #50919, #57737, #72718, #17309, #45423, #2791, #44987, #51351, #16415, #73142, #51792, #86795, #23687, #72276, #30487, #37300, #58186, #10484, #71391, #44090, #85476, #71826, #23252, #9594, #31366, #85916, #38185, #65879, #17748, #15971, #30925, #85023, #3671, #65450, #36850, #79097, #16858, #59055, #24564, #57280, #10046, #37752, #9153, #64563, #50467, #3232, #24123, #78211, #52230, #2342, #38627, #10924, #1888, #29587, #43653, #53115, #4113, #39072, #67683, #54467, #59506, #61304, #32253, #66326, #59948, #46764, #26781, #82232, #47218, #11827, #88141, #52669, #5462, #25007, #81774, #74496, #13172, #19526, #81342, #39523, #87679, #32708, #5917, #33608, #67225, #4566, #89023, #25448, #5007, #80427, #39966, #12271, #54016, #60402, #19985, #18638, #25904, #18184, #46318, #74046, #66779, #80883, #53572, #19081, #31811, #33160, #26348, #40418, #87242, #47668, #74947, #60856, #12727, #45865, #88588, #68132, #75401, #73597, #11378, #83561, #69929, #75840, #13612, #63095, #42635, #63553, #49455, #55806, #41297, #76738, #21327, #42198, #48106, #48998, #14968, #1339, #14520, #20877, #7695, #29041, #35837, #35383, #7255, #6792, #882, #49906, #41742, #84012, #429, #27689, #22235, #28576, #56726, #62655, #56265, #69479, #76289, #34942, #21787, #77196, #69028, #70370, #8146, #84472, #89477, #61742, #77637, #34492, #34036, #40857, #68585, #62204, #82678, #6349, #48545, #20437, #27236, #28118, #54915, #55098, #55367, #83119, #14060, #65343, #79439, #31253, #44430, #2232, #36303, #30380, #16309, #8605, #86239, #84915, #1789, #64011, #9483, #2681 ),
 ( #43985, #58951, #57626, #71718, #29486, #85367, #23141, #78095, #64451, #36752, #29942, #15422, #58075, #3120, #17202, #43087, #65773, #30822, #85811, #51692, #57169, #16749, #37196, #86688, #10378, #64899, #23582, #72165, #50356, #15863, #37645, #44885, #38081, #24016, #51244, #43541, #78985, #9940, #58513, #22686, #72615, #3557, #24460, #52127, #50816, #70830, #71283, #9053, #78552, #46208, #45757, #46663, #88926, #59402, #38965, #73488, #66674, #18072, #11264, #19425, #87578, #39855, #10811, #4905, #80772, #73038, #60746, #87136, #66217, #38514, #73945, #67124, #11723, #40308, #25335, #53915, #47108, #88026, #74843, #33048, #17643, #88484, #39417, #18980, #53462, #32594, #4005, #4460, #60295, #25790, #53002, #5813, #12171, #18522, #45321, #32149, #26240, #67574, #5355, #68022, #81675, #59846, #31705, #12622, #33500, #81233, #24904, #52569, #61201, #74394, #26680, #80327, #79889, #21227, #76181, #13957, #8039, #77094, #40756, #20338, #13069, #76637, #83017, #68478, #7599, #48004, #49358, #63451, #14873, #20774, #41640, #69376, #68924, #27587, #41199, #48900, #14418, #75293, #7151, #42539, #42099, #82578, #55265, #13513, #75741, #35283, #69826, #35735, #48442, #62993, #34846, #6690, #1237, #774, #70268, #62552, #326, #28023, #89834, #55703, #28473, #56166, #89375, #83915, #83450, #21684, #6252, #33942, #54357, #61638, #47562, #82126, #19880, #34391, #27140, #54814, #62101, #8499, #23917, #78448, #44329, #72512, #65674, #63911, #36652, #78888, #3015, #44783, #57968, #15762, #22580, #36196, #28940, #72062, #30718, #64353, #56625, #43434, #84369, #1686, #30279, #17099, #22141, #51589, #84813, #49807, #50252, #9385, #79334, #10274, #9837, #2131, #50708, #15315, #85706, #77536, #37543, #37094, #42981, #65241, #43887, #29836, #77990, #85267, #58413, #86141, #57524, #57069, #37976, #71180, #23032, #70726, #2583, #64795, #16648, #16210, #29388, #8954, #71620, #23481, #51149, #73385, #66117, #52466, #24797, #80223, #3460, #18417, #53362, #67466, #31155, #53810, #18875, #73836, #39751, #24358, #4802, #59742, #74737, #88382, #4357, #46106, #32487, #38414, #3903, #25683, #5248, #26143, #12064, #11623, #31600, #39313, #67020, #60186, #10707, #87918, #32938, #81576, #81128, #11155, #46559, #19323, #46999, #74292, #87476, #59300, #60641, #12516, #72935, #17969, #87032, #45653, #38863, #66567, #40196, #32047, #58851, #86586, #52025, #17542, #79784, #45219, #25232, #52895, #80668, #27036, #55150, #55597, #62884, #33397, #61987, #54705, #47455, #12966, #61098, #47897, #75641, #54251, #48339, #14309, #88827, #69264, #34283, #49244, #660, #68818, #20672, #7041, #40655, #68376, #219, #69719, #28367, #76525, #82912, #6154, #13853, #76072, #34737, #75187, #41534, #41985, #56055, #62444, #13411, #27920, #83802, #21577, #83348, #89727, #33843, #21121, #76981, #61534, #82473, #89271, #20227, #41095, #6589, #7491, #27476, #48794, #35173, #14764, #82020, #67918, #26579, #5705, #19773, #77425, #1578, #29722, #30166, #37429, #7929, #36546, #29280, #22032, #15198, #35631, #22469, #50145, #28834, #36089, #49702, #80444, #57867, #44215, #77878, #70157, #56965, #63345, #42880, #43783, #30613, #1122, #65131, #8390, #42434, #63801, #22920, #2913, #58315, #23379, #15653, #64245, #56515, #71519, #84258, #85600, #50600, #70613, #51048, #57417, #43333, #84706, #8848, #71959, #9724, #71074, #2019, #86042, #85152, #78341, #16104, #9278, #36978, #78785, #64689, #25020, #2471, #16540, #52684, #60415, #88159, #80900, #67241, #39537, #5024, #18200, #33176, #68147, #82244, #45879, #68599, #33622, #39085, #19542, #74511, #89491, #13188, #19095, #60872, #47231, #53130, #18651, #40431, #19999, #40871, #26799, #88604, #46331, #54029, #26361, #74958, #25463, #81788, #47680, #6361, #12741, #25919, #5932, #34052, #61755, #61316, #12291, #74060, #89038, #27251, #87696, #32722, #11841, #53585, #81356, #46778, #75414, #39981, #54481, #54927, #73611, #32267, #11391, #66794, #4581, #59962, #67696, #5478, #69940, #70386, #77653, #48120, #76750, #41756, #62217, #27701, #75854, #62666, #442, #69041, #76301, #1, #29500, #8161, #84487, #28134, #20450, #69492, #13626, #55379, #84025, #70845, #41312, #15434, #48564, #82690, #14072, #63114, #43101 ),
 ( #22248, #49918, #55825, #20892, #8618, #7268, #83575, #6805, #56279, #28590, #35851, #21340, #36314, #34954, #49013, #34508, #14534, #42212, #83134, #7707, #35397, #896, #21800, #49470, #42648, #56741, #77208, #64024, #63568, #14979, #29054, #1351, #1801, #86700, #24476, #2694, #85381, #52139, #50828, #30392, #15877, #30836, #3135, #44896, #85825, #10827, #9501, #58089, #43554, #37209, #64910, #29953, #16320, #78566, #43997, #57183, #72177, #17216, #31268, #84929, #17655, #72625, #37657, #3571, #78113, #58525, #23595, #38531, #79899, #51255, #9952, #86251, #2248, #57637, #79453, #58963, #45332, #65787, #65354, #23156, #24032, #51703, #10390, #64466, #38095, #73051, #66228, #4017, #78998, #22697, #50368, #71295, #9064, #16764, #71732, #36763, #44446, #45774, #87589, #32162, #25347, #4473, #59857, #19437, #18535, #67588, #53929, #68036, #80338, #74408, #24916, #5366, #18993, #11275, #53018, #60307, #33061, #47121, #87147, #67136, #80787, #73502, #38979, #59417, #46221, #73957, #18086, #11734, #66687, #61213, #60761, #81687, #39432, #52580, #4916, #32606, #88042, #46677, #40318, #25805, #74856, #53477, #31719, #12631, #81244, #12183, #39867, #88497, #26251, #5824, #33512, #24324, #71594, #38382, #31122, #59707, #66084, #37947, #58385, #37511, #59270, #10677, #45187, #73353, #72909, #78861, #43860, #45619, #66536, #72477, #30249, #85675, #3875, #51118, #44748, #64765, #2551, #79750, #10242, #65646, #4326, #11123, #9355, #16618, #37062, #31566, #51559, #57942, #86999, #44299, #17940, #32012, #38831, #79306, #3431, #58822, #65210, #86113, #9801, #17507, #24761, #23453, #86559, #23002, #52431, #72032, #23887, #2986, #30688, #80191, #50679, #78418, #17064, #16180, #51991, #74260, #68786, #47421, #82434, #19293, #40162, #88349, #32908, #26108, #68339, #19736, #32453, #89237, #61062, #75147, #46068, #18384, #40623, #4767, #80636, #27002, #20193, #53325, #39281, #88795, #67426, #66986, #47868, #46965, #12933, #41061, #34252, #60150, #5215, #6120, #61502, #13376, #26547, #12032, #73805, #12482, #53778, #11591, #33811, #87888, #25651, #81093, #81543, #74699, #67883, #75607, #60607, #54669, #6553, #5672, #87442, #25199, #52862, #18844, #33363, #54220, #81982, #46525, #39716, #76491, #49210, #42397, #35139, #77845, #84223, #626, #27439, #41502, #56930, #21539, #77387, #15621, #8812, #7002, #69680, #21993, #36049, #43293, #1085, #48761, #82880, #76943, #62849, #55117, #42841, #69234, #48305, #20641, #56018, #14723, #83768, #22432, #7451, #63765, #29245, #70122, #1543, #15163, #89687, #70580, #7894, #28797, #35593, #63310, #76038, #14273, #56478, #49662, #28325, #71035, #8353, #84666, #13818, #41947, #50107, #61953, #34698, #62406, #184, #27887, #55562, #83313, #21082, #44867, #2666, #64883, #72148, #66653, #80310, #86223, #38064, #24442, #30365, #58060, #17624, #87114, #18057, #3988, #10361, #85790, #31234, #65752, #86671, #23563, #3540, #59382, #45735, #58930, #65327, #52104, #73466, #11244, #79870, #51673, #51226, #45304, #4440, #78971, #44410, #16732, #9922, #37627, #3104, #24883, #30801, #73021, #52549, #38946, #9465, #10791, #78532, #38495, #66195, #58494, #24000, #72596, #31687, #32128, #50794, #79422, #17182, #85352, #23122, #16288, #43968, #71703, #37174, #53443, #67103, #6673, #75276, #61621, #5336, #87557, #88462, #40733, #82106, #4883, #89356, #33478, #19856, #18504, #80747, #13051, #32575, #52985, #27118, #82557, #25768, #11704, #61181, #39835, #39397, #54795, #19406, #68459, #13491, #59826, #60277, #67553, #47544, #33923, #75720, #88908, #46644, #46189, #74822, #60723, #73923, #6233, #88006, #81210, #18960, #53896, #47087, #81657, #20319, #33031, #47985, #41177, #68004, #68906, #25320, #74375, #12147, #12600, #26661, #54340, #40292, #26218, #5787, #21664, #14850, #7577, #50235, #56605, #62971, #89813, #48877, #70699, #22116, #84349, #84791, #49784, #308, #55246, #57046, #77967, #83894, #62079, #42517, #751, #62531, #56140, #76162, #13939, #1216, #49337, #77069, #15742, #22561, #20751, #28003, #82998, #77512, #28453, #48423, #15296, #55678, #29370, #43415, #71160, #70247, #8020, #35714, #76618, #35263, #21206, #28919, #42963, #41620, #63428, #34369, #8479, #83431, #36175, #14397, #42073 ),
 ( #63890, #27565, #1669, #69357, #7128, #34823, #69804, #86123, #2995, #59280, #44309, #72916, #66096, #17072, #38389, #52001, #36634, #17518, #30696, #37955, #72486, #58393, #2104, #23461, #23894, #79314, #72039, #24774, #31132, #37522, #64334, #51129, #45199, #86567, #58831, #87006, #24333, #64775, #29816, #31575, #52442, #51568, #57505, #44761, #65221, #37071, #10254, #50686, #78428, #65654, #3438, #79760, #80204, #17948, #85245, #2560, #23013, #10684, #3882, #16191, #45627, #30262, #8936, #43868, #71602, #9363, #57949, #85684, #78869, #9812, #16626, #40175, #67893, #4335, #26120, #61512, #61075, #11601, #46537, #32464, #39293, #54229, #88806, #27012, #74272, #26558, #32917, #60163, #54681, #33372, #68350, #5229, #53788, #12041, #18853, #39728, #81991, #5684, #18393, #75161, #46974, #19749, #32022, #59720, #47431, #80647, #66547, #12945, #6133, #66996, #25212, #74711, #53336, #52871, #33822, #60617, #40632, #82444, #20207, #46081, #81108, #89246, #73363, #11134, #12493, #87898, #87453, #38839, #4780, #73816, #25660, #67437, #88361, #81555, #19303, #76502, #76049, #69693, #89699, #27451, #14737, #7463, #35151, #1555, #70591, #34262, #13827, #6563, #70135, #14284, #61962, #1097, #41513, #42851, #56940, #8363, #41959, #62861, #636, #62417, #21094, #34714, #42408, #7905, #68795, #28335, #36062, #35603, #69243, #48772, #7012, #197, #28808, #63321, #29256, #56031, #56492, #83778, #27898, #84680, #84234, #63778, #21551, #49222, #76953, #83323, #22004, #49675, #77399, #82890, #15175, #47877, #75617, #55128, #20651, #13386, #48315, #41074, #55573, #45089, #78315, #64224, #86019, #2446, #1994, #17408, #71930, #37854, #65983, #59167, #57388, #30144, #72378, #86460, #38286, #51456, #9257, #43305, #37404, #23354, #15631, #3334, #29695, #8824, #71051, #16519, #9698, #44195, #72814, #57840, #24226, #79649, #30588, #51890, #65551, #50119, #31028, #65107, #79205, #23791, #2890, #36523, #36952, #58287, #16963, #85578, #3774, #44645, #51024, #77856, #64660, #58718, #10147, #10581, #31464, #22443, #85132, #22897, #50574, #16080, #78764, #43760, #71497, #60054, #12837, #19195, #25547, #52328, #11485, #33265, #74598, #46864, #47320, #12376, #52767, #17844, #19633, #40522, #46425, #24663, #67325, #53224, #25105, #18739, #38730, #66432, #53678, #74157, #11932, #68244, #75053, #73244, #80531, #45522, #40067, #80993, #11025, #67785, #18285, #81881, #6026, #33716, #39620, #5114, #32808, #39181, #87784, #73707, #81444, #5572, #4220, #60506, #86896, #60969, #45973, #88250, #66883, #4668, #88696, #26454, #80093, #26008, #54124, #31913, #32351, #59607, #87344, #56381, #83220, #14172, #62306, #6900, #93, #42298, #83667, #6456, #63209, #35044, #21442, #20095, #82335, #14626, #68687, #54568, #987, #84120, #27342, #13275, #62754, #41405, #40966, #21890, #20985, #76840, #15068, #8251, #34147, #69133, #49110, #35490, #77293, #529, #48212, #47768, #76393, #27788, #75505, #70032, #61846, #89586, #55018, #55469, #48661, #41844, #49560, #34603, #28693, #42742, #69583, #70482, #7798, #89136, #61407, #26893, #82783, #20544, #7355, #28228, #55921, #75947, #13720, #22787, #2786, #30484, #56825, #78659, #25330, #23684, #64115, #9150, #85020, #1885, #16855, #51348, #80764, #36847, #79093, #85472, #50464, #18516, #85912, #32142, #57733, #16412, #64559, #71387, #2339, #44535, #58182, #70940, #38957, #9591, #72273, #84574, #22332, #11257, #43197, #29145, #66668, #59840, #29584, #77746, #37297, #15968, #15521, #87571, #23249, #4454, #46202, #73938, #8713, #43649, #52997, #35951, #63663, #65004, #78207, #50012, #50916, #30039, #36416, #1447, #57277, #44087, #71822, #5805, #88920, #33492, #62094, #47102, #75733, #68918, #19872, #41194, #54808, #39410, #20332, #61195, #40747, #75286, #26675, #4899, #26233, #54352, #82120, #74837, #27579, #33936, #40303, #67118, #53908, #47998, #89368, #61633, #89827, #27132, #67567, #32587, #34383, #55259, #47555, #60290, #13063, #68016, #39849, #68471, #53456, #81227, #6247, #82570, #13506, #83011, #20767, #88020, #5349, #25782, #6685, #48436, #18973, #11717, #33043, #46657, #74389, #12164, #60738, #88477, #81670, #19420, #12614, #71176, #84363, #42532, #42092, #42976, #85261, #55696, #35278, #69820 ),
 ( #63443, #63905, #8948, #41634, #70263, #62988, #83444, #21221, #69370, #56158, #83908, #62544, #7591, #48892, #23027, #1681, #77983, #21678, #13950, #767, #7144, #76631, #77529, #64349, #34840, #36647, #28466, #76176, #49352, #56619, #2126, #29831, #57064, #77087, #8034, #320, #15310, #28018, #29384, #22134, #14413, #84808, #1231, #14866, #35728, #28933, #15755, #43428, #49801, #70716, #57517, #8493, #36191, #22574, #50247, #86579, #38407, #79327, #4350, #3010, #51581, #9381, #30711, #58406, #23474, #9829, #72055, #37536, #50701, #65667, #10700, #24790, #78442, #11148, #66111, #31149, #10268, #57963, #30275, #65235, #32039, #45646, #17089, #3453, #79776, #85699, #51144, #72929, #52458, #73377, #59294, #58844, #78883, #24349, #52018, #17534, #16644, #86136, #44323, #23912, #44776, #72503, #80217, #37969, #3895, #17963, #66560, #64789, #45212, #43881, #31591, #87024, #38853, #59734, #87468, #16205, #71616, #37089, #2574, #74285, #4795, #60180, #80661, #5242, #32931, #11615, #18867, #32479, #61978, #40646, #27028, #60633, #52888, #12057, #18407, #87912, #26571, #13401, #46097, #20220, #81122, #25226, #46551, #5697, #75632, #41088, #6146, #88374, #46991, #39307, #54244, #73829, #68366, #33387, #67012, #33835, #40188, #26136, #39744, #81568, #54696, #82462, #53802, #53352, #47891, #67457, #19317, #25674, #88818, #61090, #12959, #74729, #68810, #12508, #67909, #82010, #19765, #47444, #75177, #61526, #89262, #6579, #34276, #14755, #49693, #63792, #89716, #50135, #15190, #70149, #49236, #7030, #69257, #76516, #71066, #84697, #652, #42424, #28824, #34729, #62434, #22022, #1568, #22459, #8379, #7921, #212, #35621, #63336, #1113, #27913, #56506, #29270, #77871, #84248, #69710, #77415, #15645, #43322, #42870, #56047, #55589, #70605, #8837, #83339, #36079, #56955, #36537, #21112, #27467, #55142, #82904, #20664, #7480, #48330, #76065, #13844, #41526, #83792, #48786, #14301, #41976, #35165, #62876, #28355, #21566, #76970, #2461, #3791, #71949, #24240, #38301, #80110, #78331, #3351, #57405, #51908, #37870, #9270, #23369, #51471, #79667, #59182, #29713, #58305, #51040, #43775, #36968, #85145, #44208, #9716, #50589, #57857, #71510, #11044, #17424, #65999, #37419, #2009, #78777, #22912, #64679, #65568, #52345, #16095, #86915, #30157, #64237, #85592, #44662, #24679, #17861, #45104, #65122, #86035, #16532, #31043, #2906, #72830, #72396, #30604, #10597, #79221, #23804, #16979, #10161, #31478, #45536, #58733, #86477, #73260, #32368, #11951, #87361, #12392, #74612, #26468, #67339, #82349, #81009, #39636, #25121, #18755, #46439, #11501, #87800, #60068, #25566, #38745, #53691, #88710, #12853, #66447, #89148, #54138, #19209, #88266, #45989, #18303, #53240, #20108, #33731, #5127, #81458, #67800, #73721, #39195, #60984, #40539, #61421, #47338, #46881, #81896, #26026, #74172, #47785, #19648, #26910, #60520, #40084, #32827, #5587, #33282, #75066, #68261, #66902, #6042, #54586, #75520, #52782, #59623, #4236, #4686, #31930, #80548, #35965, #69148, #55035, #76858, #83237, #82799, #8268, #62768, #28706, #56841, #50023, #48228, #20998, #63225, #77308, #29157, #42313, #106, #34161, #28243, #14185, #6468, #84136, #20559, #89600, #61865, #7370, #544, #35057, #63676, #48674, #15082, #70496, #21454, #42756, #56393, #40982, #21906, #55936, #70045, #14641, #83681, #27358, #27803, #49122, #7813, #76407, #84587, #35503, #41859, #68702, #55483, #49574, #1002, #1461, #22351, #13292, #6915, #75963, #13733, #41418, #34617, #62324, #69599, #16427, #15985, #9603, #29601, #57291, #44549, #37313, #65017, #31375, #10495, #64128, #43665, #36429, #10056, #44103, #1901, #30940, #71401, #72727, #86806, #38200, #71839, #2800, #30498, #2353, #50931, #64572, #72288, #37764, #8727, #58199, #65896, #65462, #9166, #78675, #36863, #30054, #58628, #3246, #59068, #85929, #22804, #50479, #86364, #79557, #3681, #24134, #23700, #78223, #51364, #79109, #16870, #85033, #51805, #17320, #24573, #44998, #57749, #77759, #15537, #43212, #70954, #85486, #23267, #19092, #61314, #31821, #11388, #18197, #39082, #80441, #45876, #81786, #59959, #12288, #26358, #68145, #66338, #81353, #45435, #39977, #25916, #87254, #66791, #39533, #67693, #47229, #17758, #46328 ),
 ( #74956, #11838, #5475, #5930, #89036, #25017, #87693, #33173, #54027, #33619, #46775, #4577, #73158, #67238, #53127, #10934, #60869, #59517, #38636, #4124, #74057, #5021, #32718, #12739, #25459, #19539, #40429, #60412, #52242, #88600, #80004, #52681, #88156, #74507, #53582, #73608, #32264, #80897, #18648, #7266, #2943, #42646, #49011, #55377, #82242, #41310, #63112, #14530, #76748, #77206, #42210, #82688, #47678, #49467, #70384, #76299, #54478, #34952, #83132, #54925, #48561, #68596, #6359, #83572, #14070, #69039, #27699, #13623, #21338, #69938, #75412, #69489, #14977, #7705, #20448, #20890, #75852, #48118, #35395, #894, #8159, #41754, #28587, #62664, #6803, #35849, #56277, #21798, #440, #28132, #55823, #62215, #84023, #63565, #26797, #61753, #19997, #13186, #40869, #34050, #89488, #27249, #34505, #84484, #3133, #24030, #57181, #71730, #78563, #57635, #85379, #86249, #50826, #16762, #44894, #38093, #36312, #9062, #51253, #65352, #17214, #30390, #78110, #22246, #16318, #2246, #49916, #72175, #70843, #77651, #15432, #23154, #43995, #9498, #51701, #36761, #30834, #58522, #37207, #79450, #44443, #29052, #9950, #64908, #58087, #2692, #85823, #43099, #15875, #23592, #78996, #64463, #72623, #37654, #29951, #56739, #43551, #10388, #1349, #8615, #64022, #1799, #84927, #29497, #22695, #50366, #71293, #3568, #46219, #4470, #4015, #87587, #17653, #45330, #32604, #25345, #53016, #19434, #88494, #52137, #31717, #24473, #88039, #32160, #79897, #18991, #59414, #60759, #74854, #26249, #59855, #80785, #18532, #53927, #25803, #87145, #86698, #81685, #47119, #73955, #31266, #11732, #39429, #24914, #67134, #73049, #10825, #60305, #4914, #53474, #12629, #65785, #38528, #52578, #66226, #81242, #46675, #80336, #74405, #18084, #58961, #45772, #73499, #12181, #39865, #67586, #11273, #38977, #66685, #5364, #33059, #61211, #83030, #29729, #29284, #68489, #13522, #89386, #6259, #22473, #56970, #85156, #41205, #84709, #89843, #27149, #22925, #1583, #36549, #62110, #20785, #68932, #75752, #6701, #50149, #63804, #75303, #43335, #13969, #77882, #88935, #26688, #15657, #47569, #33509, #71077, #64250, #33949, #48450, #27594, #34400, #55273, #2025, #76190, #8851, #50602, #78344, #13080, #48014, #57420, #40316, #68034, #69386, #54821, #54368, #41649, #7163, #82139, #5822, #19888, #40766, #61647, #34854, #82587, #20345, #66458, #51484, #80120, #73276, #24250, #45545, #59194, #43785, #24689, #10172, #45115, #79678, #65579, #9283, #30616, #3362, #86487, #79232, #31944, #38313, #44674, #71523, #58317, #52357, #3803, #66011, #86929, #85602, #2474, #36986, #37880, #31052, #58745, #4247, #16993, #17871, #11054, #51921, #38756, #59635, #64692, #87371, #17434, #72841, #10605, #31489, #30171, #86045, #25132, #52792, #72408, #16106, #57870, #23382, #51050, #23815, #78788, #16545, #44222, #71964, #9727, #37433, #65134, #2917, #34176, #40097, #18317, #60995, #19221, #18769, #12406, #32380, #60082, #47350, #67813, #5600, #61883, #13306, #66918, #46452, #39207, #12868, #46898, #4698, #33743, #74186, #75532, #89614, #40994, #74627, #33295, #88723, #5143, #53705, #67352, #75079, #40551, #11512, #26479, #68715, #68274, #11966, #81471, #39649, #32841, #61433, #6055, #27371, #54151, #89161, #81913, #60533, #80562, #26930, #6481, #19664, #54598, #82361, #26038, #20124, #47798, #45999, #25579, #73733, #87817, #53254, #81023, #88281, #8285, #62338, #48241, #56861, #77778, #21012, #35518, #42326, #21467, #49137, #50040, #14655, #70512, #8743, #1920, #120, #62780, #15097, #29174, #70971, #84151, #41876, #75975, #70058, #55951, #13748, #76875, #21926, #28723, #7826, #41433, #69612, #63244, #1019, #28256, #36444, #77321, #83696, #20572, #7383, #1475, #42772, #35982, #15553, #63694, #48690, #69161, #43228, #64145, #56408, #82811, #49591, #84602, #83250, #22364, #6932, #34632, #55050, #27818, #55494, #76420, #14197, #35072, #555, #50494, #37778, #37328, #16000, #58642, #30071, #72742, #31390, #10509, #65033, #30511, #58215, #50947, #71856, #23283, #10073, #72302, #22820, #85944, #38215, #3262, #2371, #9620, #85502, #57765, #86377, #30954, #3697, #2815, #24151, #23715, #78692, #59085, #65475, #45013, #51376, #79123, #16890, #44116, #44566, #51822 ),
 ( #79572, #17334, #65910, #29615, #57306, #85053, #78241, #16440, #43682, #71417, #9181, #36880, #64588, #7677, #41725, #35817, #21769, #14044, #1767, #411, #7235, #69458, #14950, #8125, #42619, #71264, #56244, #84895, #78079, #29023, #50340, #63992, #48524, #29467, #69908, #42177, #35368, #20856, #63533, #70807, #22665, #76265, #9035, #36281, #1315, #70352, #28102, #55785, #63078, #2212, #15840, #49437, #56708, #49889, #83537, #21307, #43069, #43521, #36734, #57149, #84450, #48981, #22214, #77618, #15401, #76719, #8581, #64434, #29920, #57609, #857, #34925, #62635, #14502, #28555, #77173, #83995, #15339, #3044, #29861, #77554, #50734, #36674, #43459, #58435, #65265, #31175, #78470, #30742, #37119, #64377, #58874, #37565, #72534, #9407, #30303, #16233, #23061, #43909, #86164, #9859, #22602, #79363, #51170, #23938, #36219, #8521, #51614, #84832, #70746, #17121, #10298, #71200, #57998, #64820, #71643, #2602, #38004, #85731, #44807, #86609, #24384, #50274, #85287, #65697, #3481, #43008, #16670, #2152, #63929, #23506, #78911, #1707, #29411, #57089, #78015, #15783, #44357, #72086, #8976, #57545, #87498, #26165, #19353, #60210, #81602, #5273, #79808, #60664, #46130, #81152, #25710, #11645, #45243, #66590, #39339, #32509, #25256, #67943, #74320, #80693, #53384, #67046, #72963, #4384, #4826, #87945, #52922, #5731, #12089, #18443, #17562, #32071, #88403, #39773, #67486, #12538, #32969, #17995, #10730, #74760, #33422, #18898, #38434, #46581, #73860, #80250, #53833, #3927, #31623, #47025, #40225, #61123, #88852, #52047, #66140, #45676, #59328, #87056, #24822, #52487, #73409, #11181, #38885, #59767, #49279, #55177, #76100, #13879, #41121, #89751, #13435, #83375, #21148, #47480, #54282, #42017, #68845, #26605, #27501, #75665, #82496, #7514, #14338, #70187, #82938, #69745, #41561, #6615, #7959, #76556, #21604, #48366, #69297, #20698, #62017, #7068, #35203, #48820, #61562, #28394, #245, #62913, #75213, #12994, #690, #33867, #19799, #56082, #77009, #20255, #34765, #62468, #27948, #55625, #14791, #83831, #42458, #35657, #63371, #89299, #34312, #82046, #40679, #68400, #6179, #27063, #54733, #47924, #2052, #84288, #71985, #70644, #77453, #22060, #85184, #78370, #22955, #51508, #36575, #65157, #58339, #9312, #30641, #44251, #28858, #9755, #50628, #30200, #16132, #8420, #29757, #77909, #56995, #15686, #29312, #84738, #86068, #8877, #51073, #2940, #17018, #15231, #57894, #49730, #78813, #64717, #36115, #50172, #43810, #16572, #23840, #56545, #71549, #43358, #63830, #1608, #42907, #71104, #64279, #22497, #57442, #37012, #37902, #37458, #2501, #85630, #23405, #79256, #44701, #72429, #10197, #1153, #58771, #60559, #31517, #65603, #59223, #46023, #26061, #81494, #46477, #11075, #87393, #51946, #66941, #24280, #81048, #73757, #12429, #18793, #80590, #38780, #86952, #31968, #5167, #32861, #66486, #3825, #88304, #24717, #4274, #79704, #39235, #11538, #53279, #59661, #19248, #17894, #25153, #17459, #45574, #73301, #38337, #52380, #80144, #52817, #3385, #18337, #25604, #39675, #31078, #53730, #74214, #4724, #32403, #72864, #45138, #60107, #46921, #74655, #87842, #11989, #67377, #10633, #66036, #86510, #41899, #62801, #48711, #55070, #12889, #75995, #20595, #41455, #47370, #48261, #14223, #580, #82834, #20147, #13771, #28280, #35094, #69184, #6506, #6075, #49165, #55973, #68737, #89638, #27392, #54622, #13327, #26954, #6954, #34656, #61018, #67836, #55518, #82382, #40118, #41015, #89190, #33764, #21036, #27839, #83715, #34204, #83270, #62358, #47819, #21490, #141, #76896, #61905, #76440, #69633, #75560, #7403, #5628, #33317, #75100, #88745, #26503, #54176, #81937, #19690, #40576, #68295, #61456, #16462, #37350, #70537, #85074, #1941, #70992, #8764, #9643, #64171, #30091, #58238, #51399, #49616, #22386, #64609, #78711, #30537, #43704, #1497, #35546, #29638, #15578, #7848, #85529, #84175, #1038, #63264, #36465, #57330, #22840, #65056, #50065, #44141, #71879, #50521, #2839, #57786, #42348, #23303, #78264, #71440, #16022, #9207, #28746, #29202, #36900, #2393, #77799, #85965, #50969, #43249, #70078, #56882, #23736, #14680, #56432, #21947, #77342, #8306, #15119, #42796, #36003, #63717, #84626, #59555, #17794, #17356 ),
 ( #72765, #74103, #39571, #4618, #87292, #38675, #86403, #58664, #65932, #60457, #11883, #80042, #31864, #18240, #24176, #51842, #11428, #80940, #67278, #87731, #4168, #79596, #25055, #52719, #80482, #45036, #45918, #53171, #5062, #73648, #59112, #39130, #32762, #88199, #66832, #45474, #10534, #10973, #38237, #73194, #3720, #31410, #86845, #24613, #52277, #18687, #66377, #32302, #46369, #25958, #3284, #60000, #72325, #25503, #79152, #16912, #44589, #10096, #37800, #65501, #30976, #47720, #12784, #33217, #88645, #19143, #33665, #61354, #40021, #47274, #60918, #487, #69087, #89083, #54968, #26840, #89537, #81392, #26403, #82735, #41797, #46815, #48606, #19582, #53625, #75000, #34096, #14121, #69534, #34552, #54523, #75460, #67736, #20499, #12328, #6851, #61800, #74548, #62257, #68638, #82287, #40476, #20043, #83176, #20934, #13229, #81829, #76343, #68193, #40916, #5524, #27294, #48166, #41353, #6403, #7311, #5975, #75899, #54075, #13667, #43, #27742, #55426, #34996, #62709, #28178, #43150, #78161, #2293, #55868, #36359, #84531, #84072, #49963, #7752, #29098, #15020, #21844, #42694, #56324, #49514, #57687, #35901, #15921, #29997, #44042, #42254, #57228, #21386, #43598, #1845, #63159, #77250, #15481, #71337, #23205, #83619, #22288, #70435, #35443, #941, #49060, #8208, #63613, #14579, #1394, #28638, #64956, #9109, #56782, #29543, #77697, #64069, #76792, #70891, #84973, #16365, #69983, #50872, #8661, #22743, #50418, #36805, #78610, #71777, #64513, #85430, #9548, #37253, #4061, #51297, #18131, #10874, #39472, #45815, #17697, #38137, #86295, #59005, #32202, #59899, #65830, #30881, #87631, #24075, #3614, #79044, #66270, #38572, #80382, #31309, #46260, #44937, #86743, #16809, #72667, #10434, #65402, #51745, #79495, #17257, #2740, #45377, #52621, #66729, #30440, #53061, #73544, #73096, #52178, #9994, #72223, #24514, #73996, #25395, #79941, #31760, #59456, #37703, #3182, #24954, #4514, #80831, #11318, #87190, #58565, #39019, #18580, #11775, #58135, #85867, #23637, #44491, #82177, #47163, #40809, #55316, #62151, #40365, #83072, #89427, #5866, #32653, #81728, #13560, #54863, #27188, #27635, #82628, #33107, #88087, #89884, #20826, #26731, #4957, #47613, #33551, #5412, #88975, #19030, #46717, #33990, #54414, #19932, #48491, #76233, #53516, #60804, #25850, #20389, #61253, #81284, #48059, #88537, #14007, #67175, #60349, #75346, #13125, #68531, #19480, #68079, #53968, #61692, #75794, #74448, #12223, #41245, #74896, #39911, #6299, #26291, #12674, #68976, #6743, #67628, #34442, #86078, #2512, #29768, #24292, #2952, #37914, #64729, #85641, #43821, #78383, #71560, #23850, #65172, #77924, #44712, #16584, #30654, #1626, #63843, #51521, #50188, #36130, #72439, #65613, #8890, #23418, #30214, #9321, #37023, #3394, #57906, #58351, #86524, #79714, #15698, #50642, #79269, #17032, #58780, #71998, #57456, #29326, #51085, #78822, #57006, #10208, #22508, #84748, #43372, #44262, #9767, #37469, #31087, #16146, #51958, #41691, #69426, #7201, #71115, #36591, #64291, #2064, #85200, #22967, #66955, #10642, #31979, #4735, #87853, #4289, #88756, #67387, #12441, #39247, #60119, #18349, #52828, #46036, #88315, #39684, #52390, #19261, #81059, #5180, #66046, #38347, #60574, #24727, #3836, #46933, #40129, #73314, #25617, #32412, #73768, #11555, #67851, #53293, #32873, #61027, #54186, #80157, #25164, #26074, #81509, #33330, #46488, #59673, #31533, #18806, #74227, #59236, #53739, #86966, #17904, #45584, #12002, #74665, #5638, #26515, #80601, #17468, #45151, #72875, #11088, #38794, #66500, #87403, #76005, #21050, #55529, #41467, #75114, #6519, #69197, #62370, #55082, #7859, #14239, #20605, #47380, #34215, #28293, #69647, #41915, #42360, #7415, #47834, #12899, #14690, #35559, #6971, #19698, #152, #48271, #20159, #13781, #33774, #61468, #48722, #34665, #27852, #63275, #70089, #68303, #75572, #40588, #35107, #83280, #6087, #62815, #13342, #76911, #1052, #28760, #76456, #591, #55985, #61919, #82845, #68748, #83729, #21507, #89202, #26968, #49177, #89652, #81950, #54634, #41029, #27402, #82397, #44150, #10106, #57341, #9652, #16035, #43714, #63730, #36018, #43262, #37813, #51411, #85083, #9216, #85536, #1512, #29214, #78721, #58248, #79164 ) ),
 .UNSPECIFIED., .F., .F., .F.,
 ( 4, 3, 1, 1, 1, 3, 4 ),
 ( 4, 1, 1, 1, 1, 1, 1, 1, 1, 1, 1, 1, 1, 1, 1, 1, 1, 1, 1, 1, 1, 1, 1, 1, 1, 1, 1, 1, 1, 1, 1, 1, 1, 1, 1, 1, 1, 1, 1, 1, 1, 1, 1, 1, 1, 1, 1, 1, 1, 1, 1, 1, 1, 1, 1, 1, 1, 1, 1, 1, 1, 1, 1, 1, 1, 1, 1, 1, 1, 1, 1, 1, 1, 1, 1, 1, 1, 1, 1, 1, 1, 1, 1, 1, 1, 1, 1, 1, 1, 1, 1, 1, 1, 1, 1, 1, 1, 1, 1, 1, 1, 1, 1, 1, 1, 1, 1, 1, 1, 1, 1, 1, 1, 1, 1, 1, 1, 1, 1, 1, 1, 1, 1, 1, 1, 1, 1, 1, 1, 1, 1, 1, 1, 1, 1, 1, 1, 1, 1, 1, 1, 1, 1, 1, 1, 1, 1, 1, 1, 1, 1, 1, 1, 1, 1, 1, 1, 1, 1, 1, 1, 1, 1, 1, 1, 1, 1, 1, 1, 1, 1, 1, 1, 1, 1, 1, 1, 1, 1, 1, 1, 1, 1, 1, 1, 1, 1, 1, 1, 1, 1, 1, 1, 1, 1, 1, 1, 1, 1, 1, 1, 1, 1, 1, 1, 1, 1, 1, 1, 1, 1, 1, 1, 1, 1, 1, 1, 1, 1, 1, 1, 1, 1, 1, 1, 1, 1, 1, 1, 1, 1, 1, 1, 1, 1, 1, 1, 1, 1, 1, 1, 1, 1, 1, 1, 1, 1, 1, 1, 1, 1, 1, 1, 1, 1, 1, 1, 1, 1, 1, 1, 1, 1, 1, 1, 1, 1, 1, 1, 1, 1, 1, 1, 1, 1, 1, 1, 1, 1, 1, 1, 1, 1, 1, 1, 1, 1, 1, 1, 1, 1, 1, 1, 1, 1, 1, 1, 1, 1, 1, 1, 1, 1, 1, 1, 1, 1, 1, 1, 1, 1, 1, 1, 1, 1, 1, 1, 1, 1, 1, 1, 1, 1, 1, 1, 1, 1, 1, 1, 1, 1, 1, 1, 1, 1, 1, 1, 1, 1, 1, 1, 1, 1, 1, 1, 1, 1, 1, 1, 1, 1, 1, 1, 1, 1, 1, 1, 1, 1, 1, 1, 1, 1, 1, 1, 1, 1, 1, 1, 1, 1, 1, 1, 1, 1, 1, 1, 1, 1, 1, 1, 1, 1, 1, 1, 1, 1, 1, 1, 1, 1, 1, 1, 1, 1, 1, 1, 1, 1, 1, 1, 1, 1, 1, 1, 1, 1, 1, 1, 1, 1, 1, 1, 1, 1, 1, 1, 1, 1, 1, 1, 1, 1, 1, 1, 1, 1, 1, 1, 1, 1, 1, 1, 1, 1, 1, 1, 1, 1, 1, 1, 1, 1, 1, 1, 1, 1, 1, 1, 1, 1, 1, 1, 1, 1, 1, 1, 1, 1, 1, 1, 1, 1, 1, 1, 1, 1, 1, 1, 1, 1, 1, 1, 1, 1, 1, 1, 1, 1, 1, 1, 1, 1, 1, 1, 1, 1, 1, 1, 1, 1, 1, 1, 1, 1, 1, 1, 1, 1, 1, 1, 1, 1, 1, 1, 1, 1, 1, 1, 1, 1, 1, 1, 1, 1, 1, 1, 1, 1, 1, 1, 1, 1, 1, 1, 4 ),
 ( -1.602212253331664948, -1.570796326795749875, -0.6731984257695950991, -0.2243994752565149908, 0.6731984257696440599, 1.570796326795800057, 1.602526412597075067 ),
 ( 0.000000000000000000, 0.4990644329702639825, 0.9981288659405289643, 1.497193298910790116, 1.996257731881059927, 2.994386597821590001, 3.992515463762110084, 4.491579896732379673, 4.990644329702639936, 5.489708762672909970, 5.988773195643170233, 6.986902061583700529, 7.985030927524229938, 8.484095360494489313, 8.983159793464759346, 9.482224226435020498, 9.981288659405290531, 10.97941752534580040, 11.97754639128630139, 12.47661082425659984, 12.97567525722690007, 13.47473969019709905, 13.97380412316740106, 14.97193298910790027, 15.97006185504850073, 16.46912628801869971, 16.96819072098899994, 17.46725515395930017, 17.96631958692950093, 18.96444845286999836, 19.96257731881059883, 20.46164175178079958, 20.96070618475109981, 21.45977061772140004, 21.95883505069160080, 22.95696391663220126, 23.95509278257270225, 24.45415721554289945, 24.95322164851319968, 25.45228608148349991, 25.95135051445370067, 26.94947938039430113, 27.94760824633480212, 28.44667267930509880, 28.94573711227529955, 29.44480154524559978, 29.94386597821590001, 30.94199484415640100, 31.94012371009690199, 32.43918814306720577, 32.93825257603739942, 33.43731700900769965, 33.93638144197799988, 34.93451030791850087, 35.93263917385900186, 36.43170360682930209, 36.93076803979960232, 37.42983247276980308, 37.92889690574009620, 38.92702577168060429, 39.92515463762109817, 40.42421907059139841, 40.92328350356169864, 41.42234793653189939, 41.92141236950219962, 42.91954123544270061, 43.91767010138330107, 44.41673453435349472, 44.91579896732380206, 45.41486340029400282, 45.91392783326430305, 46.91205669920479693, 47.91018556514539739, 48.40924999811559815, 48.90831443108589838, 49.40737886405619861, 49.90644329702639936, 50.90457216296699983, 51.90270102890750081, 52.40176546187770157, 52.90082989484799469, 53.39989432781830203, 53.89895876078850279, 54.89708762672909614, 55.89521649266960424, 56.39428092563989736, 56.89334535861009812, 57.39240979158039835, 57.89147422455069858, 58.88960309049119957, 59.88773195643170055, 60.38679638940200078, 60.88586082237220154, 61.38492525534249467, 61.88398968831280200, 62.88211855425329588, 63.88024742019380398, 64.37931185316409710, 64.87837628613441154, 65.37744071910459809, 65.87650515207489832, 66.87463401801539931, 67.87276288395590029, 68.37182731692620052, 68.87089174989650076, 69.36995618286670151, 69.86902061583700174, 70.86714948177750273, 71.86527834771810319, 72.36434278068828974, 72.86340721365860418, 73.36247164662880493, 73.86153607959910516, 74.85966494553959194, 75.85779381148019240, 76.35685824445040737, 76.85592267742069339, 77.35498711039100783, 77.85405154336119438, 78.85218040930179484, 79.85030927524229583, 80.34937370821249658, 80.84843814118279681, 81.34750257415311125, 81.84656700712329780, 82.84469587306389826, 83.84282473900439925, 84.34188917197469948, 84.84095360494490023, 85.34001803791520047, 85.83908247088550070, 86.83721133682600168, 87.83534020276650267, 88.33440463573680290, 88.83346906870698945, 89.33253350167728968, 89.83159793464760412, 90.82972680058810511, 91.82785566652860609, 92.32692009949890632, 92.82598453246910708, 93.32504896543939310, 93.82411339840969333, 94.82224226435020853, 95.82037113029070952, 96.31943556326099554, 96.81849999623130998, 97.31756442920149652, 97.81662886217179675, 98.81475772811229774, 99.81288659405289820, 100.3119510270229995, 100.8110154599930013, 101.3100798929639978, 101.8091443259339997, 102.8072731918740033, 103.8054020578150016, 104.3044664907849892, 104.8035309237550052, 105.3025953567259876, 105.8016597896960036, 106.7997886556370020, 107.7979175215769914, 108.2969819545470074, 108.7960463875180039, 109.2951108204880057, 109.7941752534579933, 110.7923041193989917, 111.7904329853389953, 112.2894974183089971, 112.7885618512799937, 113.2876262842500097, 113.7866907172199973, 114.7848195831609956, 115.7829484491009993, 116.2820128820720100, 116.7810773150420118, 117.2801417480119994, 117.7792061809820012, 118.7773350469229996, 119.7754639128630032, 120.2745283458339998, 120.7735927788040016, 121.2726572117740034, 121.7717216447440052, 122.7698505106850035, 123.7679793766259877, 124.2670438095959895, 124.7661082425660055, 125.2651726755359931, 125.7642371085070039, 126.7623659744470075, 127.7604948403880059, 128.2595592733580077, 128.7586237063279953, 129.2576881392979828, 129.7567525722689936, 130.7548814382089972, 131.7530103041499956, 132.2520747371200116, 132.7511391700899992, 133.2502036030609815, 133.7492680360309976, 134.7473969019710012, 135.7455257679119995, 136.2445902008820156, 136.7436546338520031, 137.2427190668229855, 137.7417834997930015, 138.7399123657329767, 139.7380412316740035, 140.2371056646440195, 140.7361700976149734, 141.2352345305849894, 141.7342989635550055, 142.7324278294960038, 143.7305566954360074, 144.2296211284059950, 144.7286855613770058, 145.2277499943469934, 145.7268144273169810, 146.7249432932580078, 147.7230721591979830, 148.2221365921679990, 148.7212010251390097, 149.2202654581089973, 149.7193298910789849, 150.7174587570200117, 151.7155876229599869, 152.2146520559309977, 152.7137164889010137, 153.2127809218710013, 153.7118453548409889, 154.7099742207820157, 155.7081030867219908, 156.2071675196930016, 156.7062319526630176, 157.2052963856329768, 157.7043608186039876, 158.7024896845440196, 159.7006185504849896, 160.1996829834550056, 160.6987474164249932, 161.1978118493950092, 161.6968762823659915, 162.6950051483059951, 163.6931340142469935, 164.1921984472169811, 164.6912628801869971, 165.1903273131570131, 165.6893917461279955, 166.6875206120679991, 167.6856494780089974, 168.1847139109789850, 168.6837783439490011, 169.1828427769200118, 169.6819072098899994, 170.6800360758300030, 171.6781649417710014, 172.1772293747409890, 172.6762938077110050, 173.1753582406820158, 173.6744226736520034, 174.6725515395920070, 175.6706804055330053, 176.6688092714740037, 177.1678737044439913, 177.6669381374140073, 178.6650670033550057, 179.6631958692950093, 180.1622603022650253, 180.6613247352360077, 181.1603891682059952, 181.6594536011760113, 182.6575824671170096, 183.6557113330570132, 184.1547757660279956, 184.6538401989979832, 185.1529046319679992, 185.6519690649380152, 186.6500979308789852, 187.6482267968190172, 188.1472912297899995, 188.6463556627599871, 189.1454200957300031, 189.6444845286999907, 190.6426133946409891, 191.6407422605809927, 192.1398066935519751, 192.6388711265219911, 193.1379355594920071, 193.6369999924630179, 194.6351288584029930, 195.6332577243439914, 196.1323221573140074, 196.6313865902839950, 197.1304510232539826, 197.6295154562249934, 198.6276443221649970, 199.6257731881059954, 200.1248376210760114, 200.6239020540459990, 201.1229664870159866, 201.6220309199869973, 202.6201597859270009, 203.6182886518679993, 204.1173530848380153, 204.6164175178080029, 205.1154819507789853, 205.6145463837490013, 206.6126752496890049, 207.6108041156300033, 208.1098685485999908, 208.6089329815700069, 209.1079974145409892, 209.6070618475110052, 210.6051907134520036, 211.6033195793920072, 212.1023840123619948, 212.6014484453330056, 213.1005128783029932, 213.5995773112729808, 214.5977061772140075, 215.5958350431539827, 216.0948994761239987, 216.5939639090950095, 217.0930283420649971, 217.5920927750350131, 218.5902216409760115, 219.5883505069159867, 220.0874149398869974, 220.5864793728569850, 221.0855438058270011, 221.5846082387970171, 222.5827371047380154, 223.5808659706779906, 224.0799304036490014, 224.5789948366189890, 225.0780592695890050, 225.5771237025589926, 226.5752525685000194, 227.5733814344410177, 228.0724458674109769, 228.5715103003809929, 229.0705747333509805, 229.5696391663219913, 230.5677680322619949, 231.5658968982030217, 232.0649613311730093, 232.5640257641429969, 233.0630901971129845, 233.5621546300839952, 234.5602834960239989, 235.5584123619649972, 236.0574767949350132, 236.5565412279050008, 237.0556056608760116, 237.5546700938459992, 238.5527989597860028, 239.5509278257270012, 240.0499922586970172, 240.5490566916670048, 241.0481211246380155, 241.5471855576080031, 242.5453144235479783, 243.5434432894890051, 244.0425077224589927, 244.5415721554290087, 245.0406365884000195, 245.5397010213700071, 246.5378298873109770, 247.5359587532509806, 248.0350231862209966, 248.5340876191920074, 249.0331520521619950, 249.5322164851320110, 250.5303453510730094, 251.5284742170129846, 252.0275386499830006, 252.5266030829539829, 253.0256675159239990, 253.5247319488940150, 254.5228608148350133, 255.5209896807749885, 256.0200541137460277, 256.5191185467160153, 257.0181829796860029, 257.5172474126559905, 258.5153762785969889, 259.5135051445370209, 260.0125695775079748, 260.5116340104780193, 261.0106984434480069, 261.5097628764180513, 262.5078917423589928, 263.5060206082999912, 264.0050850412700356, 264.5041494742399664, 265.0032139072100108, 265.5022783401809647, 266.5004072061209968, 267.4985360720619951, 267.9976005050319827, 268.4966649380020272, 268.9957293709719579, 269.4947938039430255, 270.4929226698830007, 271.4910515358239991, 271.9901159687939867, 272.4891804017639743, 272.9882448347349850, 273.4873092677049726, 274.4854381336450047, 275.4835669995860030, 275.9826314325560475, 276.4816958655259782, 276.9807602984969890, 277.4798247314670334, 278.4779535974070086, 279.4760824633480070, 279.9751468963179946, 280.4742113292880390, 280.9732757622589929, 281.4723401952289805, 282.4704690611699789, 283.4685979271100109, 283.9676623600799985, 284.4667267930510093, 284.9657912260209969, 285.4648556589909845, 286.4629845249319828, 287.4611133908720149, 287.9601778238429688, 288.4592422568130132, 288.9583066897830008, 289.4573711227530453, 290.4554999886939868, 291.4536288546339620, 291.9526932876050296, 292.4517577205749603, 292.9508221535450048, 293.4498865865149924, 294.4480154524559907, 295.4461443183960228, 295.9452087513669767, 296.4442731843370211, 296.9433376173070087, 297.4424020502780195, 298.4405309162180515, 299.4386597821589930, 299.9377242151289806, 300.4367886480989682, 300.9358530810690127, 301.4349175140399666, 302.4330463799799986, 303.4311752459209970, 303.9302396788909846, 304.4293041118610290, 304.9283685448309598, 305.4274329778020274, 306.4255618437420026, 307.4236907096830009, 307.9227551426529885, 308.4218195756230330, 308.9208840085939869, 309.4199484415639745, 310.4180773075040065, 311.4162061734450049, 311.9152706064150493, 312.4143350393849801, 312.9133994723560477, 313.4124639053259784, 314.4105927712660105, 315.4087216372070088, 315.9077860701769964, 316.4068505031480072, 316.9059149361179948, 317.4049793690880392, 318.4031082350289807, 319.4012371009689559, 319.9003015339390004, 320.3993659669100111, 320.8984303998799987, 321.3974948328499863, 322.3956236987909847, 323.3937525647310167, 323.8928169977019706, 324.3918814306720151, 324.8909458636420027, 325.3900102966119903, 326.3881391625530455, 327.3862680284929638, 327.8853324614640314, 328.3843968944339622, 328.8834613274040066, 329.3825257603739942, 330.3806546263149926, 331.3787834922550246, 331.8778479252259785, 332.3769123581960230, 332.8759767911659537, 333.3750412241370213, 334.3731700900769965, 335.3712989560180517, 335.8703633889879825, 336.3694278219579701, 336.8684922549280145, 337.3675566878989684, 338.3656855538390005, 339.3638144197799988, 339.8628788527500433, 340.3619432857199740, 340.8610077186899616, 341.3600721516610292, 342.3582010176010044, 343.3563298835420028, 343.8553943165119904, 344.3544587494820348, 344.8535231824529887, 345.3525876154230332, 346.3507164813629515, 347.3488453473040067, 347.8479097802739943, 348.3469742132439819, 348.8460386462150495, 349.3451030791849803 ),
 .UNSPECIFIED. ) ;
#5277 = FACE_OUTER_BOUND ( 'NONE', #63993, .T. ) ;
#5278 = CARTESIAN_POINT ( 'NONE',  ( 108.0837332833436903, -25.31555065790283976, 321.9052427074753382 ) ) ;
#5279 = CARTESIAN_POINT ( 'NONE',  ( 109.6058369744873886, -26.58188510553521056, 195.8813395616249977 ) ) ;
#5280 = LINE ( 'NONE', #25262, #55233 ) ;
#5281 = EDGE_LOOP ( 'NONE', ( #69172, #68289, #3335, #46454, #66843 ) ) ;
#5282 = CARTESIAN_POINT ( 'NONE',  ( 130.0566129357926570, 76.91670260214422683, -11.41267162807792168 ) ) ;
#5284 = ORIENTED_EDGE ( 'NONE', *, *, #3572, .F. ) ;
#5283 = ADVANCED_FACE ( 'NONE', ( #1734, #21732, #77140, #376, #85316, #23089, #14917, #49854, #28517, #827 ), #14467, .F. ) ;
#5285 = EDGE_CURVE ( 'NONE', #87042, #9292, #46553, .T. ) ;
#5286 = ORIENTED_EDGE ( 'NONE', *, *, #48110, .T. ) ;
#5287 = LINE ( 'NONE', #32981, #77861 ) ;
#5288 = AXIS2_PLACEMENT_3D ( 'NONE', #1935, #65050, #8299 ) ;
#5289 = ORIENTED_EDGE ( 'NONE', *, *, #45576, .T. ) ;
#5290 = ADVANCED_FACE ( 'NONE', ( #70318 ), #2180, .T. ) ;
#5291 = B_SPLINE_CURVE_WITH_KNOTS ( 'NONE', 3,
 ( #34983, #70420, #13656, #35884 ),
 .UNSPECIFIED., .F., .F.,
 ( 4, 4 ),
 ( -0.3974825557268110154, -0.3842043193313819938 ),
 .UNSPECIFIED. ) ;
#5292 = DIRECTION ( 'NONE',  ( 0.000000000000000000, -0.8660254037844432595, 0.4999999999999921174 ) ) ;
#5293 = CARTESIAN_POINT ( 'NONE',  ( 109.7217209985873723, -26.99997186863735621, 90.86504839370768138 ) ) ;
#5294 = CARTESIAN_POINT ( 'NONE',  ( 104.1077555235347631, -46.72609462085661391, 107.3470538473389411 ) ) ;
#5295 = CARTESIAN_POINT ( 'NONE',  ( -10.54933103719152143, 75.47881567405516989, 130.1290928247797751 ) ) ;
#5296 = AXIS2_PLACEMENT_3D ( 'NONE', #5890, #744, #63420 ) ;
#5297 = EDGE_CURVE ( 'NONE', #11982, #19831, #35333, .T. ) ;
#5298 = CARTESIAN_POINT ( 'NONE',  ( 107.0664832912730020, -36.72944715994189835, 342.9256252759109884 ) ) ;
#5299 = CARTESIAN_POINT ( 'NONE',  ( 51.24204729617298426, -31.76306994223730840, -5.074374724088000832 ) ) ;
#5302 = CARTESIAN_POINT ( 'NONE',  ( 115.8368392028493190, -44.66223131803943858, 229.2413395616249545 ) ) ;
#5301 = CARTESIAN_POINT ( 'NONE',  ( -492.0614999999999668, 14.28749999999982201, 90.48749999999999716 ) ) ;
#5300 = DIRECTION ( 'NONE',  ( 0.000000000000000000, -1.000000000000000000, 0.000000000000000000 ) ) ;
#5303 = CARTESIAN_POINT ( 'NONE',  ( -160.2664750769294812, 101.5999999999999943, -148.0533267522755807 ) ) ;
#5304 = CYLINDRICAL_SURFACE ( 'NONE', #27886, 4.500000000000003553 ) ;
#5305 = ORIENTED_EDGE ( 'NONE', *, *, #67681, .F. ) ;
#5306 = FACE_OUTER_BOUND ( 'NONE', #17306, .T. ) ;
#5307 = EDGE_CURVE ( 'NONE', #37024, #29858, #42184, .T. ) ;
#5308 = CARTESIAN_POINT ( 'NONE',  ( 128.5492039024480562, -43.72944715994093912, 207.5838068554170377 ) ) ;
#5309 = CARTESIAN_POINT ( 'NONE',  ( 97.31323396095949363, -38.96131870160394328, 136.5057903769251482 ) ) ;
#5310 = EDGE_CURVE ( 'NONE', #27284, #47135, #33535, .T. ) ;
#5311 = DIRECTION ( 'NONE',  ( 0.000000000000000000, 0.000000000000000000, 1.000000000000000000 ) ) ;
#5313 = ORIENTED_EDGE ( 'NONE', *, *, #53539, .F. ) ;
#5312 = CARTESIAN_POINT ( 'NONE',  ( 103.0736367338192139, -47.94042275923426644, 252.3041967044822798 ) ) ;
#5314 = LINE ( 'NONE', #75699, #87222 ) ;
#5315 = CARTESIAN_POINT ( 'NONE',  ( 113.7700232194324883, -29.06831460768450626, 285.5032443235299979 ) ) ;
#5316 = CARTESIAN_POINT ( 'NONE',  ( 95.97749374758174667, -37.21091289986100037, 112.3489586092449599 ) ) ;
#5317 = DIRECTION ( 'NONE',  ( 0.7071067811865969777, -0.7071067811864980568, 0.000000000000000000 ) ) ;
#5318 = DIRECTION ( 'NONE',  ( 0.000000000000000000, 1.000000000000000000, 0.000000000000000000 ) ) ;
#5319 = AXIS2_PLACEMENT_3D ( 'NONE', #71737, #9507, #9957 ) ;
#5321 = CARTESIAN_POINT ( 'NONE',  ( 3.968749999999215294, 120.6499999999999915, 105.4788588808464027 ) ) ;
#5320 = CARTESIAN_POINT ( 'NONE',  ( 177.0371591254543944, -48.62818131005480637, 237.4678068554150059 ) ) ;
#5322 = CARTESIAN_POINT ( 'NONE',  ( -50.35902679310718355, 148.4450814996825443, 27.95514712793348977 ) ) ;
#5323 = CARTESIAN_POINT ( 'NONE',  ( 73.17003668186727339, -8.979447159941065237, 14.92562527591093691 ) ) ;
#5324 = EDGE_LOOP ( 'NONE', ( #52472, #14426 ) ) ;
#5325 = EDGE_LOOP ( 'NONE', ( #77996, #11515, #17710, #80426, #77333 ) ) ;
#5326 = ORIENTED_EDGE ( 'NONE', *, *, #15556, .F. ) ;
#5327 = VERTEX_POINT ( 'NONE', #64402 ) ;
#5328 = DIRECTION ( 'NONE',  ( 0.000000000000000000, 1.000000000000000000, 0.000000000000000000 ) ) ;
#5329 = CARTESIAN_POINT ( 'NONE',  ( 100.6111884388667335, -28.52632756463412633, 11.60705384733995515 ) ) ;
#5330 = CARTESIAN_POINT ( 'NONE',  ( 134.0664832912740110, 0.2215528400590013880, 293.6356252759119911 ) ) ;
#5331 = ADVANCED_FACE ( 'NONE', ( #9000 ), #15811, .F. ) ;
#5332 = DIRECTION ( 'NONE',  ( -1.000000000000000000, 0.000000000000000000, 0.000000000000000000 ) ) ;
#5335 = EDGE_CURVE ( 'NONE', #4752, #31084, #1021, .T. ) ;
#5334 = CARTESIAN_POINT ( 'NONE',  ( 41.56648329127398966, -27.57844715994070484, 261.9256252759120116 ) ) ;
#5333 = LINE ( 'NONE', #80744, #20661 ) ;
#5336 = CARTESIAN_POINT ( 'NONE',  ( 113.9432952986174854, -30.83689873488770061, 228.8248007804579629 ) ) ;
#5337 = ORIENTED_EDGE ( 'NONE', *, *, #39900, .F. ) ;
#5338 = ORIENTED_EDGE ( 'NONE', *, *, #9361, .T. ) ;
#5339 = ORIENTED_EDGE ( 'NONE', *, *, #25665, .F. ) ;
#5340 = AXIS2_PLACEMENT_3D ( 'NONE', #51972, #10657, #87868 ) ;
#5341 = CARTESIAN_POINT ( 'NONE',  ( 74.15067561874269586, 120.6499999999999915, -68.53801554307419508 ) ) ;
#5342 = VECTOR ( 'NONE', #33504, 1000.000000000000114 ) ;
#5343 = LINE ( 'NONE', #47550, #70965 ) ;
#5344 = DIRECTION ( 'NONE',  ( -0.7071067811865475727, 0.000000000000000000, -0.7071067811865475727 ) ) ;
#5345 = PLANE ( 'NONE',  #15680 ) ;
#5346 = CARTESIAN_POINT ( 'NONE',  ( 116.4244759746951985, -37.56879123375174601, 30.17491663923099665 ) ) ;
#5347 = CARTESIAN_POINT ( 'NONE',  ( 118.5559670995753407, 95.24969287062864964, -0.8338386114217244405 ) ) ;
#5348 = CARTESIAN_POINT ( 'NONE',  ( 107.0667039024467186, -36.72944715994091069, 195.5838068554169809 ) ) ;
#5349 = CARTESIAN_POINT ( 'NONE',  ( 115.9511604156667772, -42.07746527209881293, 278.3832443235305618 ) ) ;
#5350 = DIRECTION ( 'NONE',  ( 0.000000000000000000, 1.000000000000000000, 0.000000000000000000 ) ) ;
#5351 = EDGE_LOOP ( 'NONE', ( #75429, #65487 ) ) ;
#5352 = LINE ( 'NONE', #62548, #62068 ) ;
#5353 = AXIS2_PLACEMENT_3D ( 'NONE', #20928, #55418, #33209 ) ;
#5354 = DIRECTION ( 'NONE',  ( -0.000000000000000000, 1.000000000000000000, -0.000000000000000000 ) ) ;
#5355 = CARTESIAN_POINT ( 'NONE',  ( 109.9854453146643039, -44.35239847312019634, 60.68523322673397047 ) ) ;
#5356 = VECTOR ( 'NONE', #78484, 1000.000000000000000 ) ;
#5357 = DIRECTION ( 'NONE',  ( -0.7071067811865512365, 0.000000000000000000, 0.7071067811865436870 ) ) ;
#5358 = CARTESIAN_POINT ( 'NONE',  ( 107.0664832912739399, -36.72944715994095333, 311.6343304127839815 ) ) ;
#5359 = CARTESIAN_POINT ( 'NONE',  ( -10.09401914261505517, 90.30230937457700691, 118.1264283250772564 ) ) ;
#5360 = EDGE_LOOP ( 'NONE', ( #8884, #6285 ) ) ;
#5361 = DIRECTION ( 'NONE',  ( -1.000000000000000000, 0.000000000000000000, 0.000000000000000000 ) ) ;
#5362 = CARTESIAN_POINT ( 'NONE',  ( -47.02966122971771767, 65.60000000000000853, -44.00307561052233751 ) ) ;
#5363 = VERTEX_POINT ( 'NONE', #11673 ) ;
#5364 = CARTESIAN_POINT ( 'NONE',  ( 102.6160711382646156, -46.84739750188308705, 132.2346728949579528 ) ) ;
#5365 = ORIENTED_EDGE ( 'NONE', *, *, #34693, .F. ) ;
#5366 = CARTESIAN_POINT ( 'NONE',  ( 111.7311378220509255, -29.53965576977622831, 69.04099125664797043 ) ) ;
#5367 = FACE_OUTER_BOUND ( 'NONE', #29897, .T. ) ;
#5368 = CARTESIAN_POINT ( 'NONE',  ( 102.4863184357179051, -28.52587382674474981, 101.9253928297069791 ) ) ;
#5369 = FACE_OUTER_BOUND ( 'NONE', #18449, .T. ) ;
#5370 = CARTESIAN_POINT ( 'NONE',  ( 177.8371591254545478, -47.82818131005477369, 117.4678068554150485 ) ) ;
#5371 = CARTESIAN_POINT ( 'NONE',  ( 96.17045672112728028, -38.71987694442820782, 47.48229194257797303 ) ) ;
#5372 = AXIS2_PLACEMENT_3D ( 'NONE', #9450, #16273, #43500 ) ;
#5373 = LINE ( 'NONE', #19001, #23693 ) ;
#5374 = CARTESIAN_POINT ( 'NONE',  ( 163.0664832912739826, -0.7548456658610993575, 333.4006252759120343 ) ) ;
#5375 = VERTEX_POINT ( 'NONE', #86636 ) ;
#5376 = CARTESIAN_POINT ( 'NONE',  ( -118.1931971052175783, 73.86197090048098346, 9.272510012971169502 ) ) ;
#5377 = ORIENTED_EDGE ( 'NONE', *, *, #9296, .F. ) ;
#5379 = EDGE_CURVE ( 'NONE', #12604, #2603, #52514, .T. ) ;
#5378 = EDGE_LOOP ( 'NONE', ( #88618, #74920, #19766, #63380, #521, #25496 ) ) ;
#5380 = ADVANCED_FACE ( 'NONE', ( #11209 ), #38031, .F. ) ;
#5381 = EDGE_CURVE ( 'NONE', #67371, #54555, #46157, .T. ) ;
#5382 = DIRECTION ( 'NONE',  ( 1.000000000000000078E-15, -1.000000000000000000, 0.000000000000000000 ) ) ;
#5383 = ORIENTED_EDGE ( 'NONE', *, *, #7749, .T. ) ;
#5384 = CARTESIAN_POINT ( 'NONE',  ( 116.8464009251322153, -35.91275531464980020, 253.8927681330545454 ) ) ;
#5385 = CARTESIAN_POINT ( 'NONE',  ( 117.6028659061361736, -33.31333136338176359, 130.0880062282919880 ) ) ;
#5386 = CARTESIAN_POINT ( 'NONE',  ( 102.8734617018388633, -27.62276334107901121, 125.4186639751545869 ) ) ;
#5387 = CARTESIAN_POINT ( 'NONE',  ( 116.8181881254705274, -34.15704652260703966, 130.0311224560221035 ) ) ;
#5388 = CARTESIAN_POINT ( 'NONE',  ( 109.7700798034136511, -47.44693503648352362, 88.78514908543493789 ) ) ;
#5389 = CARTESIAN_POINT ( 'NONE',  ( 107.0664832912750057, -36.72944715993903486, 4.925625275910970657 ) ) ;
#5390 = EDGE_LOOP ( 'NONE', ( #42426, #41819, #67161, #56127 ) ) ;
#5391 = DIRECTION ( 'NONE',  ( -1.000000000000000000, 0.000000000000000000, 0.000000000000000000 ) ) ;
#5392 = EDGE_CURVE ( 'NONE', #68630, #79853, #74132, .T. ) ;
#5393 = VECTOR ( 'NONE', #68884, 1000.000000000000000 ) ;
#5394 = VECTOR ( 'NONE', #75774, 999.9999999999998863 ) ;
#5395 = DIRECTION ( 'NONE',  ( 0.000000000000000000, 1.000000000000000000, 0.000000000000000000 ) ) ;
#5396 = EDGE_LOOP ( 'NONE', ( #15482, #17028, #56494, #54162 ) ) ;
#5397 = EDGE_CURVE ( 'NONE', #52525, #17066, #2630, .T. ) ;
#5398 = CIRCLE ( 'NONE', #59056, 3.500000000000003109 ) ;
#5399 = CYLINDRICAL_SURFACE ( 'NONE', #47471, 2.517499999999998739 ) ;
#5400 = VECTOR ( 'NONE', #8620, 1000.000000000000000 ) ;
#5401 = PLANE ( 'NONE',  #1959 ) ;
#5402 = CARTESIAN_POINT ( 'NONE',  ( 97.57986484199619781, -43.79006170206860560, 261.8356252759109566 ) ) ;
#5403 = CARTESIAN_POINT ( 'NONE',  ( 90.06670420047028358, -131.9777253117771636, 222.2178068554179902 ) ) ;
#5404 = VECTOR ( 'NONE', #79234, 1000.000000000000000 ) ;
#5405 = DIRECTION ( 'NONE',  ( -0.000000000000000000, -0.000000000000000000, 1.000000000000000000 ) ) ;
#5406 = LINE ( 'NONE', #32197, #63549 ) ;
#5407 = ADVANCED_FACE ( 'NONE', ( #30332 ), #17590, .F. ) ;
#5408 = CARTESIAN_POINT ( 'NONE',  ( 98.80150335516665905, -38.88496061976939444, 275.9524198280767564 ) ) ;
#5410 = CARTESIAN_POINT ( 'NONE',  ( 107.6020193903983966, -26.30459096080998904, 91.03562527591097364 ) ) ;
#5409 = CARTESIAN_POINT ( 'NONE',  ( 116.3121618740066623, -32.93870344941997530, 39.13562527591096796 ) ) ;
#5411 = CARTESIAN_POINT ( 'NONE',  ( 20.56670390244748603, -48.82844715994200158, 129.9678068554150627 ) ) ;
#5412 = CARTESIAN_POINT ( 'NONE',  ( 114.2838679902333610, -44.31336211532283897, 158.1813395616249807 ) ) ;
#5413 = ORIENTED_EDGE ( 'NONE', *, *, #57133, .T. ) ;
#5414 = LINE ( 'NONE', #89428, #45186 ) ;
#5415 = VERTEX_POINT ( 'NONE', #85760 ) ;
#5416 = CARTESIAN_POINT ( 'NONE',  ( 107.0667039024470313, -104.2784471599409102, 17.71780685541799016 ) ) ;
#5417 = DIRECTION ( 'NONE',  ( 0.000000000000000000, 0.000000000000000000, -1.000000000000000000 ) ) ;
#5418 = CARTESIAN_POINT ( 'NONE',  ( 135.1249450788490378, -34.19118199975285677, 1.799893109327216578 ) ) ;
#5419 = ORIENTED_EDGE ( 'NONE', *, *, #61560, .T. ) ;
#5420 = EDGE_CURVE ( 'NONE', #8128, #25485, #13252, .T. ) ;
#5421 = AXIS2_PLACEMENT_3D ( 'NONE', #13118, #37584, #16252 ) ;
#5422 = CARTESIAN_POINT ( 'NONE',  ( 97.06098165937136457, -37.99585007323931762, 62.42765791910697715 ) ) ;
#5424 = ORIENTED_EDGE ( 'NONE', *, *, #4996, .T. ) ;
#5423 = CARTESIAN_POINT ( 'NONE',  ( 102.6790914627476070, -46.92570513279398625, 137.2651490854349561 ) ) ;
#5425 = CARTESIAN_POINT ( 'NONE',  ( 144.1872411114284773, -138.0587426716868151, 247.6570821702239869 ) ) ;
#5426 = AXIS2_PLACEMENT_3D ( 'NONE', #64233, #7475, #43317 ) ;
#5427 = CARTESIAN_POINT ( 'NONE',  ( -130.2872239869710143, 92.11674985319542941, 8.393624206580916791 ) ) ;
#5428 = AXIS2_PLACEMENT_3D ( 'NONE', #54403, #53957, #68965 ) ;
#5429 = CARTESIAN_POINT ( 'NONE',  ( 108.3334480883274722, -46.73485935487656917, 118.6772919420508430 ) ) ;
#5430 = CARTESIAN_POINT ( 'NONE',  ( 99.04406186696009229, -42.84125765073620329, 76.84395861032450625 ) ) ;
#5431 = ORIENTED_EDGE ( 'NONE', *, *, #86780, .F. ) ;
#5432 = AXIS2_PLACEMENT_3D ( 'NONE', #64573, #2354, #4125 ) ;
#5433 = SHAPE_DEFINITION_REPRESENTATION ( #46585, #64293 ) ;
#5434 = DIRECTION ( 'NONE',  ( 0.000000000000000000, 0.000000000000000000, -1.000000000000000000 ) ) ;
#5435 = PLANE ( 'NONE',  #64452 ) ;
#5436 = ORIENTED_EDGE ( 'NONE', *, *, #4444, .T. ) ;
#5437 = ORIENTED_EDGE ( 'NONE', *, *, #25200, .T. ) ;
#5438 = CARTESIAN_POINT ( 'NONE',  ( 172.5664832912729878, -27.82844715994070484, 18.92562527591200094 ) ) ;
#5439 = CARTESIAN_POINT ( 'NONE',  ( 84.19383299529407338, 88.91243380484084469, -99.78216974382846161 ) ) ;
#5440 = DIRECTION ( 'NONE',  ( 0.000000000000000000, 1.000000000000000000, 0.000000000000000000 ) ) ;
#5441 = CARTESIAN_POINT ( 'NONE',  ( 172.5664832912729878, -27.82844715994070484, 258.9256252759120116 ) ) ;
#5444 = EDGE_CURVE ( 'NONE', #38655, #86561, #29205, .T. ) ;
#5443 = CARTESIAN_POINT ( 'NONE',  ( -11.02404012120765842, 76.19011824550719325, -118.0432514857309911 ) ) ;
#5442 = DIRECTION ( 'NONE',  ( 3.999999999999999995E-14, -1.000000000000000000, 4.100000000000000342E-29 ) ) ;
#5445 = LINE ( 'NONE', #68114, #10349 ) ;
#5446 = AXIS2_PLACEMENT_3D ( 'NONE', #1248, #35749, #56176 ) ;
#5447 = VERTEX_POINT ( 'NONE', #66619 ) ;
#5448 = LINE ( 'NONE', #12255, #10007 ) ;
#5449 = CARTESIAN_POINT ( 'NONE',  ( 112.7790632652331482, -27.19118669266625687, 200.6470538473389809 ) ) ;
#5451 = ORIENTED_EDGE ( 'NONE', *, *, #41175, .T. ) ;
#5450 = LINE ( 'NONE', #4997, #48643 ) ;
#5452 = CARTESIAN_POINT ( 'NONE',  ( 106.0550521757682816, -27.00111521709629514, 46.15848241876796720 ) ) ;
#5453 = LINE ( 'NONE', #87671, #40011 ) ;
#5454 = FACE_OUTER_BOUND ( 'NONE', #53926, .T. ) ;
#5455 = DIRECTION ( 'NONE',  ( 0.000000000000000000, 0.000000000000000000, 1.000000000000000000 ) ) ;
#5456 = VERTEX_POINT ( 'NONE', #58460 ) ;
#5457 = EDGE_CURVE ( 'NONE', #5214, #37298, #4410, .T. ) ;
#5458 = DIRECTION ( 'NONE',  ( -1.175184669632759901E-16, 1.000000000000000000, 2.000000000000003705E-15 ) ) ;
#5459 = VECTOR ( 'NONE', #11881, 1000.000000000000000 ) ;
#5460 = ORIENTED_EDGE ( 'NONE', *, *, #62886, .F. ) ;
#5461 = VERTEX_POINT ( 'NONE', #3952 ) ;
#5462 = CARTESIAN_POINT ( 'NONE',  ( 114.2499829074921820, -30.67355260991839216, 220.8034880678019647 ) ) ;
#5463 = EDGE_CURVE ( 'NONE', #5997, #54334, #32096, .T. ) ;
#5464 = VECTOR ( 'NONE', #21761, 1000.000000000000000 ) ;
#5465 = CARTESIAN_POINT ( 'NONE',  ( 98.54763758010979302, -41.97696078833845235, 52.76539822096258803 ) ) ;
#5466 = VECTOR ( 'NONE', #63769, 1000.000000000000000 ) ;
#5467 = CARTESIAN_POINT ( 'NONE',  ( -118.3860192952351014, 93.55239623846829033, -6.356965277239823742 ) ) ;
#5468 = CYLINDRICAL_SURFACE ( 'NONE', #34455, 1.999999999999995781 ) ;
#5469 = DIRECTION ( 'NONE',  ( 0.000000000000000000, 0.000000000000000000, -1.000000000000000000 ) ) ;
#5470 = ORIENTED_EDGE ( 'NONE', *, *, #67338, .T. ) ;
#5471 = CARTESIAN_POINT ( 'NONE',  ( -41.60202597009397607, 65.59999999999998010, 50.85338361873603219 ) ) ;
#5472 = AXIS2_PLACEMENT_3D ( 'NONE', #33497, #40305, #55262 ) ;
#5473 = CYLINDRICAL_SURFACE ( 'NONE', #89048, 34.13125000000000142 ) ;
#5474 = VERTEX_POINT ( 'NONE', #59793 ) ;
#5475 = CARTESIAN_POINT ( 'NONE',  ( 100.4652087429556815, -44.82591848225601439, 12.03276813305398463 ) ) ;
#5476 = EDGE_LOOP ( 'NONE', ( #76093, #83527 ) ) ;
#5477 = ORIENTED_EDGE ( 'NONE', *, *, #60787, .T. ) ;
#5478 = CARTESIAN_POINT ( 'NONE',  ( 115.7079196686036653, -36.25352450022288764, 271.7004713219723726 ) ) ;
#5479 = AXIS2_PLACEMENT_3D ( 'NONE', #36802, #16362, #57225 ) ;
#5480 = FACE_BOUND ( 'NONE', #70811, .T. ) ;
#5481 = CARTESIAN_POINT ( 'NONE',  ( 104.0088209277215583, -27.43890701233894092, 165.3299109901969643 ) ) ;
#5482 = DIRECTION ( 'NONE',  ( 0.7071067811865344721, 0.000000000000000000, 0.7071067811865604513 ) ) ;
#5483 = DIRECTION ( 'NONE',  ( 1.000000000000000000, 4.163336342344333240E-14, 0.000000000000000000 ) ) ;
#5484 = VECTOR ( 'NONE', #51037, 1000.000000000000000 ) ;
#5485 = CYLINDRICAL_SURFACE ( 'NONE', #37631, 0.5000000000000104361 ) ;
#5486 = AXIS2_PLACEMENT_3D ( 'NONE', #42470, #70203, #30980 ) ;
#5487 = CARTESIAN_POINT ( 'NONE',  ( 10.40652293068787237, 75.26502159733162500, 130.1406823708988156 ) ) ;
#5488 = CARTESIAN_POINT ( 'NONE',  ( 101.2698767154569168, -26.33663883357058921, 251.4813395616249920 ) ) ;
#5489 = CARTESIAN_POINT ( 'NONE',  ( 51.06648329127400388, 25.62155284005901379, 339.0006252759110339 ) ) ;
#5490 = VECTOR ( 'NONE', #88016, 1000.000000000000000 ) ;
#5491 = EDGE_LOOP ( 'NONE', ( #48251, #44791, #53737, #18869 ) ) ;
#5492 = CARTESIAN_POINT ( 'NONE',  ( 117.4907998085504062, -37.69205034685562339, 74.75276813305397638 ) ) ;
#5493 = DIRECTION ( 'NONE',  ( 0.000000000000000000, 0.000000000000000000, 1.000000000000000000 ) ) ;
#5494 = ORIENTED_EDGE ( 'NONE', *, *, #78133, .T. ) ;
#5496 = ADVANCED_FACE ( 'NONE', ( #72111 ), #37592, .T. ) ;
#5495 = ORIENTED_EDGE ( 'NONE', *, *, #33810, .T. ) ;
#5498 = ORIENTED_EDGE ( 'NONE', *, *, #89800, .T. ) ;
#5497 = EDGE_CURVE ( 'NONE', #28392, #34697, #51642, .T. ) ;
#5499 = EDGE_CURVE ( 'NONE', #33876, #11706, #66860, .T. ) ;
#5500 = LINE ( 'NONE', #53605, #14427 ) ;
#5501 = CYLINDRICAL_SURFACE ( 'NONE', #79080, 4.750000000000004441 ) ;
#5502 = CARTESIAN_POINT ( 'NONE',  ( 25.56670390244808289, -42.82844715994167473, 257.2178068554150059 ) ) ;
#5503 = CARTESIAN_POINT ( 'NONE',  ( 99.80647774793122551, -41.44074323372286273, 144.6147570362579415 ) ) ;
#5504 = CARTESIAN_POINT ( 'NONE',  ( 115.2688234373398046, -30.20251741173218818, 240.3613395616249875 ) ) ;
#5505 = LINE ( 'NONE', #54057, #81 ) ;
#5506 = ORIENTED_EDGE ( 'NONE', *, *, #84263, .F. ) ;
#5507 = CARTESIAN_POINT ( 'NONE',  ( 130.2064250969986006, 90.93081950567962224, -9.551273559373818500 ) ) ;
#5508 = EDGE_CURVE ( 'NONE', #783, #78421, #13313, .T. ) ;
#5509 = VECTOR ( 'NONE', #48236, 1000.000000000000000 ) ;
#5510 = CARTESIAN_POINT ( 'NONE',  ( 136.6493805748345665, -37.67376371870763307, 2.871651383882680708 ) ) ;
#5511 = VERTEX_POINT ( 'NONE', #67072 ) ;
#5513 = ORIENTED_EDGE ( 'NONE', *, *, #88264, .T. ) ;
#5512 = VECTOR ( 'NONE', #27725, 1000.000000000000000 ) ;
#5514 = ADVANCED_FACE ( 'NONE', ( #53410 ), #18923, .F. ) ;
#5515 = FACE_OUTER_BOUND ( 'NONE', #85195, .T. ) ;
#5516 = EDGE_LOOP ( 'NONE', ( #41606, #76428, #2590 ) ) ;
#5517 = ORIENTED_EDGE ( 'NONE', *, *, #7445, .T. ) ;
#5518 = CARTESIAN_POINT ( 'NONE',  ( 107.0664832912739541, -36.72944715994095333, 307.1356252759109680 ) ) ;
#5519 = CARTESIAN_POINT ( 'NONE',  ( -12.61757850223405519, 80.88535426119446470, -129.9449579601741505 ) ) ;
#5520 = LINE ( 'NONE', #78815, #30719 ) ;
#5521 = DIRECTION ( 'NONE',  ( 0.000000000000000000, 0.000000000000000000, -1.000000000000000000 ) ) ;
#5522 = EDGE_CURVE ( 'NONE', #59384, #8859, #64095, .T. ) ;
#5523 = CARTESIAN_POINT ( 'NONE',  ( 109.0154912191213583, -27.88557705556195998, 179.3143245899819647 ) ) ;
#5524 = CARTESIAN_POINT ( 'NONE',  ( 116.2704737988580206, -31.74013610724590961, 69.22133956162495849 ) ) ;
#5525 = ORIENTED_EDGE ( 'NONE', *, *, #2836, .F. ) ;
#5526 = CARTESIAN_POINT ( 'NONE',  ( 164.9190312289439930, -35.91149509761220315, -5.074374724088000832 ) ) ;
#5527 = EDGE_LOOP ( 'NONE', ( #19094, #2058, #66080, #20754 ) ) ;
#5528 = CARTESIAN_POINT ( 'NONE',  ( -92.27764637677461224, 80.88465057165898031, -74.43377912862176515 ) ) ;
#5529 = VERTEX_POINT ( 'NONE', #68867 ) ;
#5530 = LINE ( 'NONE', #80047, #43196 ) ;
#5531 = ORIENTED_EDGE ( 'NONE', *, *, #51235, .F. ) ;
#5532 = CARTESIAN_POINT ( 'NONE',  ( 99.64972233663489476, -29.98183745677715351, 166.7387298538411073 ) ) ;
#5533 = AXIS2_PLACEMENT_3D ( 'NONE', #85862, #29992, #8204 ) ;
#5534 = DIRECTION ( 'NONE',  ( 1.000000000000000000, 0.000000000000000000, 2.108231265501709878E-16 ) ) ;
#5535 = CARTESIAN_POINT ( 'NONE',  ( 116.7444820060442083, -34.14078160163364828, 134.0345115328372856 ) ) ;
#5537 = FACE_OUTER_BOUND ( 'NONE', #47265, .T. ) ;
#5536 = CIRCLE ( 'NONE', #37430, 4.875000000000017764 ) ;
#5538 = VERTEX_POINT ( 'NONE', #55205 ) ;
#5539 = AXIS2_PLACEMENT_3D ( 'NONE', #16821, #3196, #79506 ) ;
#5540 = CARTESIAN_POINT ( 'NONE',  ( 100.5368863760760973, -27.78183265877541430, 30.56610146638794134 ) ) ;
#5541 = CARTESIAN_POINT ( 'NONE',  ( 104.7499416563296961, -46.93859083614567140, 68.39848241876794077 ) ) ;
#5542 = SURFACE_SIDE_STYLE ('',( #82302 ) ) ;
#5544 = DIRECTION ( 'NONE',  ( 0.7071067811865473507, 0.7071067811865476838, 0.000000000000000000 ) ) ;
#5543 = LINE ( 'NONE', #54539, #85490 ) ;
#5545 = CARTESIAN_POINT ( 'NONE',  ( 116.3212776292293569, -32.94146857471253753, 110.1356252759109822 ) ) ;
#5546 = FACE_BOUND ( 'NONE', #55591, .T. ) ;
#5547 = VECTOR ( 'NONE', #47790, 1000.000000000000000 ) ;
#5548 = CARTESIAN_POINT ( 'NONE',  ( 70.56670390244700286, -68.87844715994098976, 222.2178068554179902 ) ) ;
#5549 = CIRCLE ( 'NONE', #37518, 10.00000000000000711 ) ;
#5550 = CARTESIAN_POINT ( 'NONE',  ( 95.35945913470564506, -35.72541260001472097, 298.1356252759109680 ) ) ;
#5551 = ORIENTED_EDGE ( 'NONE', *, *, #29206, .T. ) ;
#5552 = CARTESIAN_POINT ( 'NONE',  ( 114.1203865811702087, -46.31439608500644312, 33.08133956162495792 ) ) ;
#5553 = CARTESIAN_POINT ( 'NONE',  ( 118.0249073071387471, -38.34132458482030614, 69.72229194257801055 ) ) ;
#5554 = VECTOR ( 'NONE', #88031, 1000.000000000000000 ) ;
#5555 = AXIS2_PLACEMENT_3D ( 'NONE', #2749, #43157, #77256 ) ;
#5558 = EDGE_CURVE ( 'NONE', #41931, #57180, #39366, .T. ) ;
#5557 = CARTESIAN_POINT ( 'NONE',  ( 141.0664832912740110, -8.729447159940995959, -4.824374724088991151 ) ) ;
#5556 = CARTESIAN_POINT ( 'NONE',  ( 99.50511838765265793, -43.30624115933716922, 171.8947509423747135 ) ) ;
#5559 = CARTESIAN_POINT ( 'NONE',  ( 144.9829487194917590, -139.7622023428961029, 245.5930228935639832 ) ) ;
#5560 = CARTESIAN_POINT ( 'NONE',  ( 127.3855720247629222, -85.76459861161312404, 250.2191008560389776 ) ) ;
#5561 = ORIENTED_EDGE ( 'NONE', *, *, #72944, .T. ) ;
#5562 = CARTESIAN_POINT ( 'NONE',  ( 103.5129713284350146, -46.47169217660395191, 93.28610146638693834 ) ) ;
#5564 = ORIENTED_EDGE ( 'NONE', *, *, #80802, .F. ) ;
#5563 = DIRECTION ( 'NONE',  ( -0.9130365726098601531, 0.000000000000000000, -0.4078776986755215384 ) ) ;
#5565 = CARTESIAN_POINT ( 'NONE',  ( 96.70388795518327640, -35.81005419191409089, 227.2556252759109725 ) ) ;
#5566 = CARTESIAN_POINT ( 'NONE',  ( 105.7144241109852345, -46.72372135719457020, 253.4708212861533241 ) ) ;
#5567 = CARTESIAN_POINT ( 'NONE',  ( 115.0663604721750488, -42.78498363884347810, 148.3107124467303777 ) ) ;
#5568 = CARTESIAN_POINT ( 'NONE',  ( -28.99999999999997513, 172.0000000000000000, 183.8826257785461280 ) ) ;
#5569 = CARTESIAN_POINT ( 'NONE',  ( 97.81169817874256012, -40.51742791483425776, 82.63555527327814332 ) ) ;
#5570 = LINE ( 'NONE', #33263, #12897 ) ;
#5571 = DIRECTION ( 'NONE',  ( -2.973811673103097665E-16, 0.000000000000000000, -1.000000000000000000 ) ) ;
#5572 = CARTESIAN_POINT ( 'NONE',  ( 109.6835627966675162, -27.30531164764922991, 174.8613395616259822 ) ) ;
#5573 = CIRCLE ( 'NONE', #27343, 20.63750000000000284 ) ;
#5574 = ORIENTED_EDGE ( 'NONE', *, *, #86507, .F. ) ;
#5575 = VERTEX_POINT ( 'NONE', #32992 ) ;
#5576 = VECTOR ( 'NONE', #2103, 1000.000000000000000 ) ;
#5577 = CARTESIAN_POINT ( 'NONE',  ( 112.3917779585437131, -43.81249117439911345, 139.5215833058969679 ) ) ;
#5578 = ADVANCED_FACE ( 'NONE', ( #4851 ), #48389, .F. ) ;
#5579 = CARTESIAN_POINT ( 'NONE',  ( 188.5667039024479834, -58.35344715994099829, 259.9678068554150059 ) ) ;
#5581 = CARTESIAN_POINT ( 'NONE',  ( 71.24076473329807868, 5.642044068322332961, 361.9756252759101471 ) ) ;
#5580 = CARTESIAN_POINT ( 'NONE',  ( 106.8506556707825013, -46.50783423188139665, 268.5584824187674258 ) ) ;
#5582 = CARTESIAN_POINT ( 'NONE',  ( 41.56648329127398966, -27.57844715994070484, 201.9256252759119832 ) ) ;
#5583 = DIRECTION ( 'NONE',  ( -0.4999999999999990563, 0.000000000000000000, -0.8660254037844392627 ) ) ;
#5584 = LINE ( 'NONE', #61862, #61796 ) ;
#5585 = LINE ( 'NONE', #17859, #13035 ) ;
#5586 = CARTESIAN_POINT ( 'NONE',  ( 106.1656040943334460, -121.2545485715091047, -11.78219314458148226 ) ) ;
#5587 = CARTESIAN_POINT ( 'NONE',  ( 108.1794352217186344, -47.07304438381573419, 202.6613395616249704 ) ) ;
#5588 = DIRECTION ( 'NONE',  ( 0.7071067811874244269, -0.7071067811856707186, 7.071067811874251411E-16 ) ) ;
#5589 = ORIENTED_EDGE ( 'NONE', *, *, #22322, .T. ) ;
#5590 = ORIENTED_EDGE ( 'NONE', *, *, #16353, .T. ) ;
#5591 = AXIS2_PLACEMENT_3D ( 'NONE', #65291, #17146, #23963 ) ;
#5592 = LINE ( 'NONE', #12858, #82256 ) ;
#5593 = DIRECTION ( 'NONE',  ( 0.000000000000000000, 1.000000000000000000, 0.000000000000000000 ) ) ;
#5594 = LINE ( 'NONE', #40546, #75139 ) ;
#5595 = DIRECTION ( 'NONE',  ( 0.000000000000000000, 0.000000000000000000, -1.000000000000000000 ) ) ;
#5597 = CARTESIAN_POINT ( 'NONE',  ( 34.96670390244699433, -26.71338133339301635, -5.074374724088000832 ) ) ;
#5596 = VECTOR ( 'NONE', #39950, 1000.000000000000000 ) ;
#5598 = ORIENTED_EDGE ( 'NONE', *, *, #3017, .T. ) ;
#5599 = CARTESIAN_POINT ( 'NONE',  ( 107.0664832912739968, -36.72944715994100306, 287.6356252759109680 ) ) ;
#5600 = CARTESIAN_POINT ( 'NONE',  ( 101.4252639664679094, -46.23501037223531540, 207.1622919425779514 ) ) ;
#5601 = DIRECTION ( 'NONE',  ( 9.351236661543306751E-17, -3.725950533538267725E-29, -1.000000000000000000 ) ) ;
#5603 = VERTEX_POINT ( 'NONE', #60690 ) ;
#5602 = ADVANCED_FACE ( 'NONE', ( #13016 ), #74342, .T. ) ;
#5604 = CIRCLE ( 'NONE', #2765, 31.75000000000000000 ) ;
#5605 = EDGE_CURVE ( 'NONE', #75812, #26236, #75241, .T. ) ;
#5606 = DIRECTION ( 'NONE',  ( -1.000000000000000000, -4.299999999999999979E-14, -1.000000000000000078E-15 ) ) ;
#5607 = LINE ( 'NONE', #47353, #10128 ) ;
#5608 = EDGE_CURVE ( 'NONE', #36627, #83684, #62582, .T. ) ;
#5609 = CARTESIAN_POINT ( 'NONE',  ( 100.8872380539724247, -44.70003101589365713, 163.0522683080627075 ) ) ;
#5610 = CARTESIAN_POINT ( 'NONE',  ( 111.0712550167563677, -29.58490437025668740, 32.48809036959193719 ) ) ;
#5612 = CARTESIAN_POINT ( 'NONE',  ( 99.66919142226757344, -46.01935155626545537, 118.0413395616259606 ) ) ;
#5611 = AXIS2_PLACEMENT_3D ( 'NONE', #4511, #32199, #59896 ) ;
#5613 = FACE_OUTER_BOUND ( 'NONE', #66534, .T. ) ;
#5614 = ORIENTED_EDGE ( 'NONE', *, *, #64657, .F. ) ;
#5615 = EDGE_CURVE ( 'NONE', #23299, #61548, #26189, .T. ) ;
#5616 = AXIS2_PLACEMENT_3D ( 'NONE', #25293, #52962, #18474 ) ;
#5617 = PLANE ( 'NONE',  #42165 ) ;
#5618 = CARTESIAN_POINT ( 'NONE',  ( 82.31780288913714116, -17.14744377620639781, 7.339349742409305044 ) ) ;
#5619 = ORIENTED_EDGE ( 'NONE', *, *, #51143, .F. ) ;
#5620 = ORIENTED_EDGE ( 'NONE', *, *, #89388, .T. ) ;
#5621 = DIRECTION ( 'NONE',  ( -0.7071067811865274777, 0.7071067811865675568, -7.071067811864971448E-16 ) ) ;
#5622 = ORIENTED_EDGE ( 'NONE', *, *, #18355, .F. ) ;
#5623 = ORIENTED_EDGE ( 'NONE', *, *, #79508, .F. ) ;
#5624 = DIRECTION ( 'NONE',  ( -4.237773401492740281E-14, 1.000000000000000000, 0.000000000000000000 ) ) ;
#5625 = EDGE_CURVE ( 'NONE', #59703, #76619, #81626, .T. ) ;
#5626 = CIRCLE ( 'NONE', #73755, 16.00000000000000000 ) ;
#5627 = CARTESIAN_POINT ( 'NONE',  ( 109.3970511370136904, -44.97690468586920787, 72.21813411379096692 ) ) ;
#5628 = CARTESIAN_POINT ( 'NONE',  ( 110.8247753047693749, -26.30972152642112150, 249.7889586092445882 ) ) ;
#5629 = CARTESIAN_POINT ( 'NONE',  ( 96.76471471792625323, -35.27954033865438532, 181.2156252759109805 ) ) ;
#5631 = CARTESIAN_POINT ( 'NONE',  ( 111.0379167980822928, -47.01981040405694756, 13.85753003781498016 ) ) ;
#5630 = PLANE ( 'NONE',  #78054 ) ;
#5632 = CARTESIAN_POINT ( 'NONE',  ( 106.0039306387646860, -11.55185827894094786, 322.0356252759110021 ) ) ;
#5633 = FACE_OUTER_BOUND ( 'NONE', #85283, .T. ) ;
#5634 = ORIENTED_EDGE ( 'NONE', *, *, #80248, .T. ) ;
#5635 = B_SPLINE_CURVE_WITH_KNOTS ( 'NONE', 3,
 ( #56799, #54983, #35915, #82753, #20516, #15037, #15496, #70453, #8225, #69103, #63629, #1415, #68655, #84546, #44060, #85884, #72241, #78181, #15939, #65421, #44955, #9124, #1861, #3203, #72690, #8680, #2760, #64531, #36824 ),
 .UNSPECIFIED., .F., .F.,
 ( 4, 2, 2, 2, 2, 2, 2, 2, 2, 2, 1, 1, 1, 1, 1, 2, 4 ),
 ( 0.000000000000000000, 0.06250185081845154034, 0.1250037016369030807, 0.1875055524553546071, 0.2500074032738061613, 0.3125092540922577156, 0.3750111049107092143, 0.4375129557291607685, 0.4687638811383865733, 0.4843893438429994203, 0.4922020751953060658, 0.4961084408714594440, 0.4980616237095359944, 0.4990382151285742696, 0.4995265108380935182, 0.4997706586928529204, 0.5000148065476123227 ),
 .UNSPECIFIED. ) ;
#5636 = AXIS2_PLACEMENT_3D ( 'NONE', #37638, #3113, #10803 ) ;
#5637 = LINE ( 'NONE', #31978, #54533 ) ;
#5638 = CARTESIAN_POINT ( 'NONE',  ( 97.12779447186500192, -40.02021159927672755, 241.5813395616249863 ) ) ;
#5639 = ORIENTED_EDGE ( 'NONE', *, *, #63169, .F. ) ;
#5640 = CARTESIAN_POINT ( 'NONE',  ( 98.43480628652092435, -29.82486610537253569, 195.7775300378159784 ) ) ;
#5641 = PLANE ( 'NONE',  #28235 ) ;
#5642 = DIRECTION ( 'NONE',  ( 1.000000000000000000, 0.000000000000000000, 0.000000000000000000 ) ) ;
#5643 = CARTESIAN_POINT ( 'NONE',  ( 180.3521107875639871, -35.65087443492551245, -5.074374724088000832 ) ) ;
#5644 = PLANE ( 'NONE',  #39818 ) ;
#5646 = CARTESIAN_POINT ( 'NONE',  ( 25.56670390244797275, -67.87844715994100397, 293.2178068554150627 ) ) ;
#5645 = CARTESIAN_POINT ( 'NONE',  ( 114.2883772398465538, -33.13574786571706454, 277.6356252759109680 ) ) ;
#5647 = CARTESIAN_POINT ( 'NONE',  ( 107.0667039024470313, -104.2784471599409528, 45.21780685541799727 ) ) ;
#5648 = DIRECTION ( 'NONE',  ( -1.000000000000000000, 0.000000000000000000, 4.277118011829300531E-15 ) ) ;
#5649 = CARTESIAN_POINT ( 'NONE',  ( 92.91125933621934507, -113.6057974291316981, -19.26696060647573105 ) ) ;
#5650 = CARTESIAN_POINT ( 'NONE',  ( -12.59999999999999964, 82.54999999999999716, -190.5010000000000048 ) ) ;
#5651 = DIRECTION ( 'NONE',  ( 0.000000000000000000, -1.000000000000000000, 0.000000000000000000 ) ) ;
#5652 = DIRECTION ( 'NONE',  ( 1.000000000000000000, 0.000000000000000000, 0.000000000000000000 ) ) ;
#5654 = ORIENTED_EDGE ( 'NONE', *, *, #24887, .F. ) ;
#5653 = CARTESIAN_POINT ( 'NONE',  ( -1.654053778667912145, 95.16954379564980115, -118.5472977239360830 ) ) ;
#5655 = VECTOR ( 'NONE', #66396, 1000.000000000000000 ) ;
#5656 = CYLINDRICAL_SURFACE ( 'NONE', #56794, 6.571100913904396990 ) ;
#5657 = CARTESIAN_POINT ( 'NONE',  ( 97.03688691280343903, -41.43079139552996537, 211.6632443235299945 ) ) ;
#5658 = CARTESIAN_POINT ( 'NONE',  ( 114.5674230198705317, -44.02034806205370643, 94.21276813305395592 ) ) ;
#5659 = CARTESIAN_POINT ( 'NONE',  ( 111.0094172226674374, -46.42718045843506047, 278.8841967044824059 ) ) ;
#5660 = DIRECTION ( 'NONE',  ( 0.000000000000000000, 0.000000000000000000, -1.000000000000000000 ) ) ;
#5661 = CARTESIAN_POINT ( 'NONE',  ( 68.53801554307449351, 120.6499999999999915, -74.15067561874229796 ) ) ;
#5664 = EDGE_CURVE ( 'NONE', #22107, #30158, #47504, .T. ) ;
#5663 = CARTESIAN_POINT ( 'NONE',  ( 50.96943157743499597, -34.03355364505720360, -5.074374724088000832 ) ) ;
#5662 = LINE ( 'NONE', #74689, #18801 ) ;
#5665 = CARTESIAN_POINT ( 'NONE',  ( 31.89136050872298966, -31.76306994223740432, -5.074374724088000832 ) ) ;
#5666 = CARTESIAN_POINT ( 'NONE',  ( 132.6459363690182158, -21.09121833381622935, 1.942446336659213513 ) ) ;
#5667 = AXIS2_PLACEMENT_3D ( 'NONE', #7135, #22567, #50241 ) ;
#5668 = AXIS2_PLACEMENT_3D ( 'NONE', #25024, #11395, #24581 ) ;
#5669 = EDGE_CURVE ( 'NONE', #78421, #12031, #11821, .T. ) ;
#5670 = ORIENTED_EDGE ( 'NONE', *, *, #9489, .F. ) ;
#5671 = ORIENTED_EDGE ( 'NONE', *, *, #63009, .T. ) ;
#5672 = CARTESIAN_POINT ( 'NONE',  ( 116.7762654731291860, -36.89220852042034693, 153.2352769709339668 ) ) ;
#5673 = AXIS2_PLACEMENT_3D ( 'NONE', #27722, #7289, #22 ) ;
#5675 = ORIENTED_EDGE ( 'NONE', *, *, #4665, .F. ) ;
#5674 = LINE ( 'NONE', #88796, #89401 ) ;
#5676 = CARTESIAN_POINT ( 'NONE',  ( -254.0000000000000000, 14.28750000000026077, 6.349999999999710099 ) ) ;
#5677 = CARTESIAN_POINT ( 'NONE',  ( 113.8292797163801851, -28.77778007523028947, 135.5156252759109634 ) ) ;
#5678 = DIRECTION ( 'NONE',  ( 1.000000000000000000, 1.000000000000000078E-15, 0.000000000000000000 ) ) ;
#5679 = VECTOR ( 'NONE', #66892, 1000.000000000000000 ) ;
#5680 = DIRECTION ( 'NONE',  ( -6.524622321627019585E-16, -4.013151879589939944E-16, -1.000000000000000000 ) ) ;
#5681 = LINE ( 'NONE', #66543, #62102 ) ;
#5682 = DIRECTION ( 'NONE',  ( 0.000000000000000000, 0.000000000000000000, 1.000000000000000000 ) ) ;
#5683 = VECTOR ( 'NONE', #87533, 1000.000000000000114 ) ;
#5684 = CARTESIAN_POINT ( 'NONE',  ( 104.1495640007033217, -46.68084741754461220, 62.33753003781600199 ) ) ;
#5685 = EDGE_LOOP ( 'NONE', ( #59721, #87560, #42855, #18953 ) ) ;
#5686 = ORIENTED_EDGE ( 'NONE', *, *, #55498, .F. ) ;
#5687 = ORIENTED_EDGE ( 'NONE', *, *, #20576, .T. ) ;
#5688 = ADVANCED_FACE ( 'NONE', ( #82520 ), #60242, .T. ) ;
#5689 = DIRECTION ( 'NONE',  ( -1.000000000000000000, -3.999999999999999995E-14, -1.000000000000000078E-15 ) ) ;
#5691 = LINE ( 'NONE', #75170, #23008 ) ;
#5690 = CARTESIAN_POINT ( 'NONE',  ( 96.69720940280909360, -36.59277893904148726, 152.3280062282909739 ) ) ;
#5692 = DIRECTION ( 'NONE',  ( -3.100000000000000258E-29, 3.100000000000000044E-14, 1.000000000000000000 ) ) ;
#5693 = DIRECTION ( 'NONE',  ( -0.09234423430305457869, -0.06932666101729537123, 0.9933108055705301975 ) ) ;
#5694 = DIRECTION ( 'NONE',  ( 0.000000000000000000, 0.000000000000000000, -1.000000000000000000 ) ) ;
#5695 = CARTESIAN_POINT ( 'NONE',  ( 88.20392011030118340, 93.55466788070657458, 79.21949419058924491 ) ) ;
#5696 = CARTESIAN_POINT ( 'NONE',  ( 101.9935007850360620, -45.44599742214800386, 178.1564475108619945 ) ) ;
#5697 = CARTESIAN_POINT ( 'NONE',  ( 96.11054930851071276, -38.00668368623060189, 86.43086337114897333 ) ) ;
#5698 = ORIENTED_EDGE ( 'NONE', *, *, #39851, .T. ) ;
#5699 = ORIENTED_EDGE ( 'NONE', *, *, #26616, .T. ) ;
#5700 = ORIENTED_EDGE ( 'NONE', *, *, #78720, .T. ) ;
#5701 = EDGE_CURVE ( 'NONE', #44803, #41711, #82073, .T. ) ;
#5702 = DIRECTION ( 'NONE',  ( 0.000000000000000000, 0.000000000000000000, 1.000000000000000000 ) ) ;
#5703 = CARTESIAN_POINT ( 'NONE',  ( -89.38347482486648232, 94.60320878023493663, -95.16331303980157941 ) ) ;
#5704 = CARTESIAN_POINT ( 'NONE',  ( 122.2221484686747459, -107.5284471599419192, -21.78219314458190681 ) ) ;
#5705 = CARTESIAN_POINT ( 'NONE',  ( 100.3885320853208896, -32.03533449533603772, 203.6566617981629577 ) ) ;
#5706 = CIRCLE ( 'NONE', #78272, 36.57600000000000051 ) ;
#5707 = DIRECTION ( 'NONE',  ( -3.100000000000000258E-29, 3.100000000000000044E-14, 1.000000000000000000 ) ) ;
#5708 = ORIENTED_EDGE ( 'NONE', *, *, #64246, .F. ) ;
#5710 = EDGE_LOOP ( 'NONE', ( #59053, #79670, #15981, #57002, #87201, #51776 ) ) ;
#5709 = ORIENTED_EDGE ( 'NONE', *, *, #23596, .F. ) ;
#5711 = CARTESIAN_POINT ( 'NONE',  ( 70.14948329127297200, -71.52944715994141234, 342.9256252759110453 ) ) ;
#5712 = CARTESIAN_POINT ( 'NONE',  ( 135.1908702341724506, -21.23918067504807894, 1.822998012174642968 ) ) ;
#5713 = ORIENTED_EDGE ( 'NONE', *, *, #8156, .F. ) ;
#5714 = VERTEX_POINT ( 'NONE', #27526 ) ;
#5715 = CARTESIAN_POINT ( 'NONE',  ( 141.3509999999999991, 0.000000000000000000, 141.3509999999999991 ) ) ;
#5716 = EDGE_CURVE ( 'NONE', #19751, #49481, #75635, .T. ) ;
#5717 = CARTESIAN_POINT ( 'NONE',  ( 116.3029726692365813, -35.00788115540211010, 200.4168214011349676 ) ) ;
#5718 = AXIS2_PLACEMENT_3D ( 'NONE', #62512, #13036, #27546 ) ;
#5719 = CARTESIAN_POINT ( 'NONE',  ( 69.63919639214310564, 101.5999999999999943, 0.000000000000000000 ) ) ;
#5720 = CARTESIAN_POINT ( 'NONE',  ( -109.4815320936060061, 57.56471201436704632, 71.12429803595952649 ) ) ;
#5721 = AXIS2_PLACEMENT_3D ( 'NONE', #64400, #57570, #63953 ) ;
#5722 = ORIENTED_EDGE ( 'NONE', *, *, #71101, .F. ) ;
#5724 = ORIENTED_EDGE ( 'NONE', *, *, #558, .F. ) ;
#5723 = AXIS2_PLACEMENT_3D ( 'NONE', #20898, #38872, #77213 ) ;
#5725 = DIRECTION ( 'NONE',  ( -0.9963424814100680926, 0.08544974978095698503, 0.000000000000000000 ) ) ;
#5726 = ORIENTED_EDGE ( 'NONE', *, *, #88491, .F. ) ;
#5727 = EDGE_LOOP ( 'NONE', ( #35153, #3045, #53805 ) ) ;
#5728 = ADVANCED_FACE ( 'NONE', ( #63396 ), #83398, .T. ) ;
#5729 = CARTESIAN_POINT ( 'NONE',  ( 113.4754094548699186, -31.62960856676687982, 242.1795189410199782 ) ) ;
#5730 = VECTOR ( 'NONE', #10618, 1000.000000000000000 ) ;
#5731 = CARTESIAN_POINT ( 'NONE',  ( 111.0910783018720025, -25.55641485417826431, 99.80133956162498521 ) ) ;
#5732 = CARTESIAN_POINT ( 'NONE',  ( 98.66494773507966443, -43.87633619481174918, 76.89943479971999807 ) ) ;
#5733 = CARTESIAN_POINT ( 'NONE',  ( 115.7727261665505836, -40.42085123866506535, 249.5838068554168103 ) ) ;
#5734 = EDGE_CURVE ( 'NONE', #89264, #76080, #272, .T. ) ;
#5735 = CARTESIAN_POINT ( 'NONE',  ( 133.1862368104802670, -16.12360705087672130, 8.106403045237987826 ) ) ;
#5736 = CARTESIAN_POINT ( 'NONE',  ( 105.8320912101120399, -25.33698730529098953, 321.9074507037550461 ) ) ;
#5737 = CARTESIAN_POINT ( 'NONE',  ( 103.6386224297199163, -26.22117658871400181, 206.3394347997209763 ) ) ;
#5738 = DIRECTION ( 'NONE',  ( 0.000000000000000000, 0.8660254037844387076, 0.4999999999999998890 ) ) ;
#5739 = ORIENTED_EDGE ( 'NONE', *, *, #86797, .T. ) ;
#5740 = CARTESIAN_POINT ( 'NONE',  ( -27.27158787008326968, 184.0000000000000000, 101.0189074266571794 ) ) ;
#5741 = ORIENTED_EDGE ( 'NONE', *, *, #46269, .F. ) ;
#5742 = VERTEX_POINT ( 'NONE', #36600 ) ;
#5743 = AXIS2_PLACEMENT_3D ( 'NONE', #21977, #36492, #62833 ) ;
#5744 = CARTESIAN_POINT ( 'NONE',  ( 45.76696975232771081, -48.62818131006091704, 180.4678068554150911 ) ) ;
#5745 = ORIENTED_EDGE ( 'NONE', *, *, #42698, .F. ) ;
#5746 = CARTESIAN_POINT ( 'NONE',  ( 97.75827573275111604, -40.38460791318124166, 137.6242309511203246 ) ) ;
#5747 = CARTESIAN_POINT ( 'NONE',  ( 98.34920873643025629, -31.65775108644640312, 91.90656420394297754 ) ) ;
#5748 = CARTESIAN_POINT ( 'NONE',  ( 111.0826007845189736, -25.57995003598136208, 99.80133956162498521 ) ) ;
#5749 = CARTESIAN_POINT ( 'NONE',  ( -10.52353995119061381, 75.44045292000316749, 130.1311838323437371 ) ) ;
#5750 = DIRECTION ( 'NONE',  ( 0.000000000000000000, -1.000000000000000000, 0.000000000000000000 ) ) ;
#5751 = CARTESIAN_POINT ( 'NONE',  ( 149.4409906032288973, -0.9156555935619370423, 394.9756252759100903 ) ) ;
#5754 = CARTESIAN_POINT ( 'NONE',  ( 99.10268845779070546, -29.98093639561600909, 211.7670538473399517 ) ) ;
#5753 = DIRECTION ( 'NONE',  ( 1.000000000000000000, 0.000000000000000000, 0.000000000000000000 ) ) ;
#5752 = CARTESIAN_POINT ( 'NONE',  ( 19.56670390244734747, -25.42844715994192129, 300.4678068554150059 ) ) ;
#5755 = DIRECTION ( 'NONE',  ( 0.000000000000000000, 0.000000000000000000, 1.000000000000000000 ) ) ;
#5756 = DIRECTION ( 'NONE',  ( 1.000000000000000000, 0.000000000000000000, 0.000000000000000000 ) ) ;
#5757 = VERTEX_POINT ( 'NONE', #49303 ) ;
#5758 = AXIS2_PLACEMENT_3D ( 'NONE', #71666, #49849, #36240 ) ;
#5759 = DIRECTION ( 'NONE',  ( 1.000000000000000000, 4.163336342344333240E-14, 0.000000000000000000 ) ) ;
#5760 = CARTESIAN_POINT ( 'NONE',  ( 0.000000000000000000, 50.79999999999999716, 265.5569999999999595 ) ) ;
#5761 = CARTESIAN_POINT ( 'NONE',  ( 131.0667039024480118, -64.87844715994098976, 207.5838068554149913 ) ) ;
#5762 = DIRECTION ( 'NONE',  ( -0.7071067811865506814, 0.7071067811865443531, -7.071067811865500971E-16 ) ) ;
#5764 = VERTEX_POINT ( 'NONE', #13903 ) ;
#5763 = CARTESIAN_POINT ( 'NONE',  ( 116.9671346634708442, -41.74840980516093936, 248.4651490854349731 ) ) ;
#5765 = CARTESIAN_POINT ( 'NONE',  ( 111.1917831817336975, -27.58851263026131306, 194.7389780491331521 ) ) ;
#5766 = CARTESIAN_POINT ( 'NONE',  ( 96.89316087236547048, -34.20304521249558150, 272.1327681330539576 ) ) ;
#5767 = CARTESIAN_POINT ( 'NONE',  ( 95.96792091384095613, -36.58316683298836125, 152.3280062282919971 ) ) ;
#5768 = CARTESIAN_POINT ( 'NONE',  ( 97.81169952324414396, -40.51743120087827776, 141.6355106266202313 ) ) ;
#5769 = CARTESIAN_POINT ( 'NONE',  ( 97.39129596614627360, -39.27853438940273634, 102.5314386769556876 ) ) ;
#5770 = VECTOR ( 'NONE', #32365, 1000.000000000000000 ) ;
#5772 = DIRECTION ( 'NONE',  ( 1.000000000000000000, 0.000000000000000000, 0.000000000000000000 ) ) ;
#5771 = LINE ( 'NONE', #33011, #4283 ) ;
#5773 = DIRECTION ( 'NONE',  ( -0.4078776986755215384, 0.000000000000000000, 0.9130365726098602641 ) ) ;
#5774 = CARTESIAN_POINT ( 'NONE',  ( 71.06648329127399677, -8.729447159940999512, 342.9256252759119548 ) ) ;
#5775 = ORIENTED_EDGE ( 'NONE', *, *, #46372, .F. ) ;
#5776 = ADVANCED_FACE ( 'NONE', ( #77036 ), #76582, .F. ) ;
#5777 = ORIENTED_EDGE ( 'NONE', *, *, #45261, .T. ) ;
#5778 = ORIENTED_EDGE ( 'NONE', *, *, #35823, .F. ) ;
#5779 = AXIS2_PLACEMENT_3D ( 'NONE', #31921, #16971, #10590 ) ;
#5780 = ORIENTED_EDGE ( 'NONE', *, *, #24270, .T. ) ;
#5781 = FACE_OUTER_BOUND ( 'NONE', #14219, .T. ) ;
#5782 = CARTESIAN_POINT ( 'NONE',  ( 104.2468583329775811, -46.74335657891433726, 18.35848241876792031 ) ) ;
#5783 = CARTESIAN_POINT ( 'NONE',  ( 113.5015236877822389, -120.9585416479406348, -9.274842254010115639 ) ) ;
#5785 = CARTESIAN_POINT ( 'NONE',  ( 145.4449125191942187, -139.3071378063975203, 245.7427791856104875 ) ) ;
#5784 = AXIS2_PLACEMENT_3D ( 'NONE', #2978, #23876, #44736 ) ;
#5786 = CARTESIAN_POINT ( 'NONE',  ( 36.65249034007450746, -49.32844715994130524, 129.9678068554150911 ) ) ;
#5787 = CARTESIAN_POINT ( 'NONE',  ( 105.2433400634091925, -28.35518594498741507, 259.6695626852197734 ) ) ;
#5788 = ORIENTED_EDGE ( 'NONE', *, *, #15223, .T. ) ;
#5789 = ORIENTED_EDGE ( 'NONE', *, *, #65411, .T. ) ;
#5790 = CIRCLE ( 'NONE', #75224, 2.029999999999997140 ) ;
#5792 = ORIENTED_EDGE ( 'NONE', *, *, #53890, .F. ) ;
#5791 = CIRCLE ( 'NONE', #85559, 2.124999999999994227 ) ;
#5793 = EDGE_CURVE ( 'NONE', #16304, #57152, #43382, .T. ) ;
#5794 = DIRECTION ( 'NONE',  ( -1.000000000000000000, -1.000000000000000078E-15, 0.000000000000000000 ) ) ;
#5795 = CARTESIAN_POINT ( 'NONE',  ( 98.15101130392974937, -41.26167982539337942, 101.7011238567067011 ) ) ;
#5796 = DIRECTION ( 'NONE',  ( -1.000000000000000078E-15, 0.000000000000000000, 1.000000000000000000 ) ) ;
#5797 = CARTESIAN_POINT ( 'NONE',  ( 115.0859250807818910, -30.61377459442804039, 274.3439221958257690 ) ) ;
#5798 = EDGE_CURVE ( 'NONE', #960, #25814, #3136, .T. ) ;
#5799 = CARTESIAN_POINT ( 'NONE',  ( 114.4295241859595933, -42.56572631025478870, 44.73682140113599814 ) ) ;
#5800 = DIRECTION ( 'NONE',  ( 0.000000000000000000, -1.000000000000000000, 0.000000000000000000 ) ) ;
#5802 = EDGE_CURVE ( 'NONE', #75262, #34651, #57469, .T. ) ;
#5801 = AXIS2_PLACEMENT_3D ( 'NONE', #51830, #31849, #23724 ) ;
#5803 = CARTESIAN_POINT ( 'NONE',  ( 83.56670390244799762, -36.72944715994108122, 229.5838068554169524 ) ) ;
#5804 = PRODUCT_DEFINITION_FORMATION_WITH_SPECIFIED_SOURCE ( 'ANY', '', #11164, .NOT_KNOWN. ) ;
#5805 = CARTESIAN_POINT ( 'NONE',  ( 103.3362402991319442, -47.20309360805218546, 252.3041967044827913 ) ) ;
#5806 = LINE ( 'NONE', #27580, #71941 ) ;
#5807 = EDGE_CURVE ( 'NONE', #83951, #5456, #42041, .T. ) ;
#5808 = ORIENTED_EDGE ( 'NONE', *, *, #45188, .F. ) ;
#5809 = EDGE_CURVE ( 'NONE', #33347, #54218, #77122, .T. ) ;
#5810 = DIRECTION ( 'NONE',  ( 0.000000000000000000, -1.000000000000000000, 0.000000000000000000 ) ) ;
#5811 = CIRCLE ( 'NONE', #76866, 5.599999999999994316 ) ;
#5812 = CARTESIAN_POINT ( 'NONE',  ( 25.56670390244797275, -62.87844715994099687, 142.0928068554150059 ) ) ;
#5813 = CARTESIAN_POINT ( 'NONE',  ( 114.9159532999967723, -33.08434830970520579, 56.97856656006794651 ) ) ;
#5814 = ADVANCED_FACE ( 'NONE', ( #14814 ), #1635, .F. ) ;
#5815 = DIRECTION ( 'NONE',  ( 0.000000000000000000, 1.000000000000000000, 0.000000000000000000 ) ) ;
#5816 = EDGE_CURVE ( 'NONE', #33347, #61554, #35229, .T. ) ;
#5817 = CARTESIAN_POINT ( 'NONE',  ( 57.56670390244718760, -42.82844715994040996, 170.7178068554150911 ) ) ;
#5818 = LINE ( 'NONE', #39860, #5342 ) ;
#5819 = EDGE_LOOP ( 'NONE', ( #59355, #48354 ) ) ;
#5820 = CARTESIAN_POINT ( 'NONE',  ( 57.14999999999999858, 69.84999999999999432, 280.2255000000000109 ) ) ;
#5821 = ORIENTED_EDGE ( 'NONE', *, *, #41372, .T. ) ;
#5822 = CARTESIAN_POINT ( 'NONE',  ( 117.8008629928215782, -34.09274860618955216, 164.0061014663869798 ) ) ;
#5823 = ORIENTED_EDGE ( 'NONE', *, *, #87919, .T. ) ;
#5824 = CARTESIAN_POINT ( 'NONE',  ( 112.2084326156563066, -29.27471527533065299, 89.03051506617198640 ) ) ;
#5825 = ADVANCED_FACE ( 'NONE', ( #83853, #63852 ), #714, .T. ) ;
#5826 = LINE ( 'NONE', #4018, #46016 ) ;
#5827 = CARTESIAN_POINT ( 'NONE',  ( 117.1284314671335665, -36.25205438732766083, 115.2958690201829626 ) ) ;
#5828 = DIRECTION ( 'NONE',  ( 0.7071067811985215501, -0.7071067811745735954, 0.000000000000000000 ) ) ;
#5829 = DIRECTION ( 'NONE',  ( 1.000000000000000078E-15, -1.000000000000000083E-30, -1.000000000000000000 ) ) ;
#5830 = AXIS2_PLACEMENT_3D ( 'NONE', #67234, #32715, #52678 ) ;
#5831 = CARTESIAN_POINT ( 'NONE',  ( 95.32466046839788021, -34.95410283156319053, 67.20705384733894050 ) ) ;
#5832 = DIRECTION ( 'NONE',  ( 0.7071067708032310328, 0.0001211784769794162209, 0.7071067811865502373 ) ) ;
#5833 = DIRECTION ( 'NONE',  ( -0.9999999853157766072, -0.0001713722456120069274, 0.000000000000000000 ) ) ;
#5834 = VERTEX_POINT ( 'NONE', #50200 ) ;
#5835 = CARTESIAN_POINT ( 'NONE',  ( 77.55659459556798652, -19.85370728022772013, 2.783021134847694089 ) ) ;
#5836 = ORIENTED_EDGE ( 'NONE', *, *, #31797, .T. ) ;
#5837 = ORIENTED_EDGE ( 'NONE', *, *, #86155, .T. ) ;
#5838 = EDGE_CURVE ( 'NONE', #52709, #40784, #55647, .T. ) ;
#5839 = LINE ( 'NONE', #88950, #86209 ) ;
#5840 = ORIENTED_EDGE ( 'NONE', *, *, #23811, .T. ) ;
#5841 = CARTESIAN_POINT ( 'NONE',  ( 97.44287158780957725, -40.59272077381807975, 251.6422919425783675 ) ) ;
#5842 = CARTESIAN_POINT ( 'NONE',  ( 117.3314307007336481, -34.78826007317788083, 154.9756252759109714 ) ) ;
#5843 = ADVANCED_FACE ( 'NONE', ( #70213 ), #69768, .T. ) ;
#5844 = CARTESIAN_POINT ( 'NONE',  ( 0.8399620612054651270, 69.85000000000003695, -118.5560000000000400 ) ) ;
#5845 = DIRECTION ( 'NONE',  ( 0.000000000000000000, -1.000000000000000000, 0.000000000000000000 ) ) ;
#5846 = CARTESIAN_POINT ( 'NONE',  ( 100.2987399830848432, -46.45735886148204941, 83.09276813305294240 ) ) ;
#5848 = ADVANCED_FACE ( 'NONE', ( #7093 ), #15257, .T. ) ;
#5847 = FACE_OUTER_BOUND ( 'NONE', #7286, .T. ) ;
#5849 = ORIENTED_EDGE ( 'NONE', *, *, #60743, .F. ) ;
#5850 = DIRECTION ( 'NONE',  ( 4.299999999999999979E-14, -1.000000000000000000, 0.000000000000000000 ) ) ;
#5851 = VECTOR ( 'NONE', #66411, 1000.000000000000000 ) ;
#5852 = EDGE_CURVE ( 'NONE', #43862, #27454, #10391, .T. ) ;
#5853 = CARTESIAN_POINT ( 'NONE',  ( 80.48314995793998605, 12.92155284005802862, 355.9756252759109998 ) ) ;
#5854 = ORIENTED_EDGE ( 'NONE', *, *, #63910, .T. ) ;
#5855 = CIRCLE ( 'NONE', #29008, 38.10000000000000142 ) ;
#5856 = FACE_OUTER_BOUND ( 'NONE', #52161, .T. ) ;
#5857 = CARTESIAN_POINT ( 'NONE',  ( 149.4409906032289257, -0.9156555935619231645, 543.8623766218582887 ) ) ;
#5858 = CARTESIAN_POINT ( 'NONE',  ( 116.5166575185069462, -42.41785904284980546, 278.3832443235298797 ) ) ;
#5859 = LINE ( 'NONE', #61246, #43133 ) ;
#5860 = CARTESIAN_POINT ( 'NONE',  ( 25.56670390244748248, -48.82844715994178841, 137.2178068554150627 ) ) ;
#5861 = DIRECTION ( 'NONE',  ( 0.000000000000000000, 0.000000000000000000, -1.000000000000000000 ) ) ;
#5862 = CARTESIAN_POINT ( 'NONE',  ( 101.7353989658528661, -28.52926574610319932, 25.53562527591096654 ) ) ;
#5864 = CARTESIAN_POINT ( 'NONE',  ( 111.7842945758856246, -25.88553347519915349, 130.7499109901969518 ) ) ;
#5863 = CARTESIAN_POINT ( 'NONE',  ( 107.0667039024470313, -104.2784471599418197, -11.78219314458200984 ) ) ;
#5865 = CARTESIAN_POINT ( 'NONE',  ( 138.0667039024479550, -14.72944715994091069, 199.5838068554170093 ) ) ;
#5866 = CARTESIAN_POINT ( 'NONE',  ( 117.1686558484209826, -33.85615284218268073, 149.0470538473389581 ) ) ;
#5867 = EDGE_LOOP ( 'NONE', ( #37005, #35358 ) ) ;
#5868 = DIRECTION ( 'NONE',  ( 0.08219486863338737459, 0.05370816768103092026, 0.9951680442491540601 ) ) ;
#5869 = ORIENTED_EDGE ( 'NONE', *, *, #17666, .T. ) ;
#5870 = CIRCLE ( 'NONE', #29073, 50.79999999999999716 ) ;
#5871 = DIRECTION ( 'NONE',  ( -1.000000000000000000, 0.000000000000000000, -9.713237310806269221E-16 ) ) ;
#5872 = DIRECTION ( 'NONE',  ( 3.999999999999999995E-14, -1.000000000000000000, 4.100000000000000342E-29 ) ) ;
#5873 = CARTESIAN_POINT ( 'NONE',  ( 177.4809174648215730, -48.32844715993478246, 129.9678068554150059 ) ) ;
#5874 = ORIENTED_EDGE ( 'NONE', *, *, #70925, .T. ) ;
#5875 = CARTESIAN_POINT ( 'NONE',  ( 109.7274606350641903, -27.00149574038083955, 60.86486693327666586 ) ) ;
#5877 = ORIENTED_EDGE ( 'NONE', *, *, #45802, .T. ) ;
#5876 = CARTESIAN_POINT ( 'NONE',  ( 103.4531379826000261, -46.55545292317445671, 142.2956252759109645 ) ) ;
#5878 = CARTESIAN_POINT ( 'NONE',  ( 63.06670390244700997, -79.67844715994098692, 120.2178068554179902 ) ) ;
#5879 = CARTESIAN_POINT ( 'NONE',  ( -130.0566101429361368, 88.18319050751495070, 11.41270026320447428 ) ) ;
#5880 = DIRECTION ( 'NONE',  ( -0.7071067812123270624, -0.7071067811607679721, 0.000000000000000000 ) ) ;
#5881 = CARTESIAN_POINT ( 'NONE',  ( 173.9900000000000091, 5.112500000000000711, -7.937500000000000000 ) ) ;
#5882 = ORIENTED_EDGE ( 'NONE', *, *, #80979, .T. ) ;
#5883 = EDGE_LOOP ( 'NONE', ( #43237, #15243 ) ) ;
#5885 = VERTEX_POINT ( 'NONE', #15707 ) ;
#5884 = AXIS2_PLACEMENT_3D ( 'NONE', #62901, #41110, #42896 ) ;
#5886 = CIRCLE ( 'NONE', #77010, 7.499999999999996447 ) ;
#5887 = EDGE_LOOP ( 'NONE', ( #80313, #60469, #21818, #23580 ) ) ;
#5888 = DIRECTION ( 'NONE',  ( 0.000000000000000000, 0.000000000000000000, -1.000000000000000000 ) ) ;
#5889 = CARTESIAN_POINT ( 'NONE',  ( 107.8867142951287974, -26.70539886071778923, 250.0113088905621623 ) ) ;
#5890 = CARTESIAN_POINT ( 'NONE',  ( 41.56648329127399677, 0.2215528400590013880, 258.9256252759120116 ) ) ;
#5892 = LINE ( 'NONE', #45844, #22545 ) ;
#5891 = CARTESIAN_POINT ( 'NONE',  ( 115.8252488141339427, -31.72970135207203057, 104.2398208576954630 ) ) ;
#5893 = CARTESIAN_POINT ( 'NONE',  ( 52.06670390244700286, -77.67844715994100113, 180.4678068554179902 ) ) ;
#5894 = AXIS2_PLACEMENT_3D ( 'NONE', #3564, #31263, #10821 ) ;
#5895 = ORIENTED_EDGE ( 'NONE', *, *, #65706, .T. ) ;
#5896 = FACE_OUTER_BOUND ( 'NONE', #83381, .T. ) ;
#5897 = LINE ( 'NONE', #88573, #28871 ) ;
#5898 = EDGE_CURVE ( 'NONE', #2880, #34477, #35022, .T. ) ;
#5899 = CARTESIAN_POINT ( 'NONE',  ( 116.5663773505004315, -40.88766770462209621, 204.4861014663869696 ) ) ;
#5901 = ORIENTED_EDGE ( 'NONE', *, *, #50920, .F. ) ;
#5900 = DIRECTION ( 'NONE',  ( 1.000000000000000078E-15, 1.000000000000000083E-30, -1.000000000000000000 ) ) ;
#5902 = ADVANCED_FACE ( 'NONE', ( #85650 ), #23428, .T. ) ;
#5903 = CARTESIAN_POINT ( 'NONE',  ( 108.4470127171751983, -27.04659769318761775, 100.9641967044819779 ) ) ;
#5904 = CARTESIAN_POINT ( 'NONE',  ( 151.0371591254572934, -24.42818131005592974, 313.9678068554149490 ) ) ;
#5905 = DIRECTION ( 'NONE',  ( 0.000000000000000000, 0.000000000000000000, 1.000000000000000000 ) ) ;
#5906 = AXIS2_PLACEMENT_3D ( 'NONE', #42863, #7472, #206 ) ;
#5907 = CARTESIAN_POINT ( 'NONE',  ( 162.7866693523298522, -36.02818131005322755, 237.4678068554150059 ) ) ;
#5908 = VECTOR ( 'NONE', #36831, 1000.000000000000000 ) ;
#5909 = EDGE_CURVE ( 'NONE', #2603, #55318, #48041, .T. ) ;
#5910 = ORIENTED_EDGE ( 'NONE', *, *, #85334, .T. ) ;
#5911 = CARTESIAN_POINT ( 'NONE',  ( -487.2989999999999782, 21.43125000000029701, 15.23694598552314972 ) ) ;
#5912 = ADVANCED_FACE ( 'NONE', ( #25176 ), #23859, .T. ) ;
#5913 = B_SPLINE_CURVE_WITH_KNOTS ( 'NONE', 3,
 ( #36275, #69485, #54920, #7700, #889, #77201, #34947, #77645, #48553, #62659, #69034, #55816, #89483, #34499, #83126, #20885, #76294, #14065, #14972, #63559, #1344, #41749, #83566, #76743, #29046, #435, #56734, #84478, #27243, #21333, #22241, #15427, #43093, #6354, #82682, #48112, #75847, #41303, #49005, #14525, #78103, #72170, #37202, #52132, #65779, #71725, #23585, #9944 ),
 .UNSPECIFIED., .F., .F.,
 ( 4, 2, 2, 2, 2, 2, 2, 2, 2, 1, 2, 2, 2, 2, 2, 2, 2, 2, 2, 2, 2, 1, 2, 2, 4 ),
 ( 0.05960646776571126848, 0.06208927922045071740, 0.06333068494782044533, 0.06457209067519016632, 0.06705490212992966381, 0.06829630785729939868, 0.06953771358466911967, 0.07202052503940853390, 0.07326193076677825489, 0.07450333649414797588, 0.07574474222151769687, 0.07698614794888740398, 0.07946895940362684596, 0.08195177085836627406, 0.08319317658573600893, 0.08443458231310574380, 0.08691739376784522741, 0.08815879949521496228, 0.08940020522258468327, 0.09188301667732418077, 0.09312442240469391563, 0.09436582813206365050, 0.09560723385943339925, 0.09684863958680312024, 0.09933145104154256222 ),
 .UNSPECIFIED. ) ;
#5914 = ORIENTED_EDGE ( 'NONE', *, *, #62547, .F. ) ;
#5915 = ORIENTED_EDGE ( 'NONE', *, *, #38752, .T. ) ;
#5916 = B_SPLINE_CURVE_WITH_KNOTS ( 'NONE', 3,
 ( #41503, #7003, #29246, #14274, #84224, #34701, #62407, #84668, #21994, #186, #55563, #83314, #22433, #41949, #50109, #77846, #16952, #37393 ),
 .UNSPECIFIED., .F., .F.,
 ( 4, 2, 2, 2, 2, 2, 2, 2, 4 ),
 ( 0.5000699581767007462, 0.5625612134046131807, 0.6250524686325256152, 0.6875437238604379386, 0.7500349790883503731, 0.8125262343162628076, 0.8750174895441751310, 0.9375087447720875655, 1.000000000000000000 ),
 .UNSPECIFIED. ) ;
#5917 = CARTESIAN_POINT ( 'NONE',  ( 114.2010777387499587, -30.61601215110631458, 225.8339642582779447 ) ) ;
#5918 = AXIS2_PLACEMENT_3D ( 'NONE', #23646, #43608, #8217 ) ;
#5919 = EDGE_CURVE ( 'NONE', #1069, #69462, #2523, .T. ) ;
#5920 = DIRECTION ( 'NONE',  ( 0.000000000000000000, 1.000000000000000000, 0.000000000000000000 ) ) ;
#5921 = DIRECTION ( 'NONE',  ( 0.000000000000000000, -1.000000000000000000, 0.000000000000000000 ) ) ;
#5922 = EDGE_CURVE ( 'NONE', #14739, #67885, #32103, .T. ) ;
#5923 = CARTESIAN_POINT ( 'NONE',  ( 109.6430120555397707, -46.48008675582220661, 153.7814586030977466 ) ) ;
#5924 = CIRCLE ( 'NONE', #47977, 15.69999999999999574 ) ;
#5925 = CARTESIAN_POINT ( 'NONE',  ( 83.73314995794051185, 12.92155284005802685, 335.5992267699911054 ) ) ;
#5926 = VERTEX_POINT ( 'NONE', #3406 ) ;
#5927 = CARTESIAN_POINT ( 'NONE',  ( 179.4595971212723100, -26.00627455218570461, 313.9678068554149490 ) ) ;
#5928 = CARTESIAN_POINT ( 'NONE',  ( 172.5664832912740110, 0.2215528400590013880, 318.9256252759120116 ) ) ;
#5929 = ORIENTED_EDGE ( 'NONE', *, *, #30363, .T. ) ;
#5930 = CARTESIAN_POINT ( 'NONE',  ( 105.1635383257858507, -47.00901688944614421, 12.42991099019596923 ) ) ;
#5931 = VERTEX_POINT ( 'NONE', #65623 ) ;
#5932 = CARTESIAN_POINT ( 'NONE',  ( 101.7278717236064836, -30.55458258274888905, 258.4623760838770750 ) ) ;
#5933 = ADVANCED_FACE ( 'NONE', ( #31543 ), #33601, .F. ) ;
#5934 = CARTESIAN_POINT ( 'NONE',  ( 47.62500000000000000, 111.1250000000000000, 257.1750000000000114 ) ) ;
#5935 = CARTESIAN_POINT ( 'NONE',  ( 97.29384000864233428, -37.12803473146956890, 161.3584824187679487 ) ) ;
#5936 = LINE ( 'NONE', #80446, #21491 ) ;
#5937 = CARTESIAN_POINT ( 'NONE',  ( 107.0664832912739968, -36.72944715994100306, 287.6356252759109680 ) ) ;
#5938 = CARTESIAN_POINT ( 'NONE',  ( 165.2748236753140247, -30.08671355700301575, -5.074374724088000832 ) ) ;
#5939 = CARTESIAN_POINT ( 'NONE',  ( 25.56670390244797275, -48.82844715994099971, 293.2178068554150627 ) ) ;
#5940 = EDGE_CURVE ( 'NONE', #11071, #61542, #58361, .T. ) ;
#5941 = CARTESIAN_POINT ( 'NONE',  ( 98.80492496406409941, -29.31701487593723598, 231.7565776568629587 ) ) ;
#5942 = CARTESIAN_POINT ( 'NONE',  ( 223.2659999999999911, 36.86249999999999716, -2.032000000000000028 ) ) ;
#5943 = ORIENTED_EDGE ( 'NONE', *, *, #9393, .T. ) ;
#5944 = CARTESIAN_POINT ( 'NONE',  ( 96.61310803562074057, -37.29506674262550803, 72.36991099019596163 ) ) ;
#5945 = CARTESIAN_POINT ( 'NONE',  ( 87.06648329127401098, -46.72944715994105280, 14.67562527591094934 ) ) ;
#5946 = ORIENTED_EDGE ( 'NONE', *, *, #11065, .F. ) ;
#5947 = VERTEX_POINT ( 'NONE', #65182 ) ;
#5948 = ORIENTED_EDGE ( 'NONE', *, *, #50388, .T. ) ;
#5949 = CIRCLE ( 'NONE', #33488, 13.00000000000000355 ) ;
#5950 = CIRCLE ( 'NONE', #8878, 4.762500000000000178 ) ;
#5951 = CARTESIAN_POINT ( 'NONE',  ( 98.34940958104101583, -31.65739082969338369, 160.9063178345361962 ) ) ;
#5952 = DIRECTION ( 'NONE',  ( -1.000000000000000000, 0.000000000000000000, 1.071939472051879986E-15 ) ) ;
#5953 = PLANE ( 'NONE',  #79958 ) ;
#5954 = FACE_BOUND ( 'NONE', #68854, .T. ) ;
#5955 = VECTOR ( 'NONE', #8460, 1000.000000000000000 ) ;
#5956 = CARTESIAN_POINT ( 'NONE',  ( 114.6928066196564515, -42.01481596195104373, 161.1623760838769783 ) ) ;
#5957 = CARTESIAN_POINT ( 'NONE',  ( 99.38090234834324121, -28.75341736348360655, 261.6746728949589169 ) ) ;
#5959 = EDGE_CURVE ( 'NONE', #84182, #45804, #3849, .T. ) ;
#5958 = CARTESIAN_POINT ( 'NONE',  ( 112.0640897386794563, -45.48941479919412245, 58.98962357542096413 ) ) ;
#5960 = VERTEX_POINT ( 'NONE', #45594 ) ;
#5961 = CARTESIAN_POINT ( 'NONE',  ( 130.0566101429361936, 88.18319050751496491, -11.41270026320357189 ) ) ;
#5962 = ADVANCED_FACE ( 'NONE', ( #72450 ), #59246, .F. ) ;
#5963 = CARTESIAN_POINT ( 'NONE',  ( 41.56648329127398966, -27.82844715994070484, 18.92562527591200094 ) ) ;
#5964 = CIRCLE ( 'NONE', #17554, 2.500000000000002220 ) ;
#5965 = VERTEX_POINT ( 'NONE', #64739 ) ;
#5966 = ORIENTED_EDGE ( 'NONE', *, *, #15096, .F. ) ;
#5967 = AXIS2_PLACEMENT_3D ( 'NONE', #54604, #28727, #82365 ) ;
#5968 = DIRECTION ( 'NONE',  ( 0.000000000000000000, 0.000000000000000000, 1.000000000000000000 ) ) ;
#5969 = VERTEX_POINT ( 'NONE', #2961 ) ;
#5970 = VERTEX_POINT ( 'NONE', #30663 ) ;
#5971 = DIRECTION ( 'NONE',  ( -1.000000000000000000, 0.000000000000000000, 0.000000000000000000 ) ) ;
#5972 = CARTESIAN_POINT ( 'NONE',  ( 128.5492039024480846, -58.72944715994093201, 207.5838068554170377 ) ) ;
#5973 = DIRECTION ( 'NONE',  ( -1.000000000000000000, 1.011922027653136551E-15, 0.000000000000000000 ) ) ;
#5974 = CARTESIAN_POINT ( 'NONE',  ( 112.9548150380649503, -42.91681406074877003, 157.6038483995049830 ) ) ;
#5975 = CARTESIAN_POINT ( 'NONE',  ( 104.7497970125497204, -46.93922829031851762, 72.39848241876795498 ) ) ;
#5976 = CARTESIAN_POINT ( 'NONE',  ( 25.56670390244828539, -48.82844715994168183, 295.7178068554150059 ) ) ;
#5977 = EDGE_LOOP ( 'NONE', ( #88634, #62408 ) ) ;
#5978 = CARTESIAN_POINT ( 'NONE',  ( -77.69145367648802392, 73.00424585431358082, -89.55259891852590215 ) ) ;
#5979 = ORIENTED_EDGE ( 'NONE', *, *, #87623, .T. ) ;
#5980 = AXIS2_PLACEMENT_3D ( 'NONE', #38848, #5238, #5693 ) ;
#5981 = CARTESIAN_POINT ( 'NONE',  ( -34.93928583487483763, 65.60000000000000853, 35.93880153443800651 ) ) ;
#5982 = ORIENTED_EDGE ( 'NONE', *, *, #85735, .T. ) ;
#5983 = DIRECTION ( 'NONE',  ( 1.000000000000000000, 8.673617379883546378E-16, 9.757819552368989676E-16 ) ) ;
#5984 = DIRECTION ( 'NONE',  ( -0.7071067811865345831, 0.000000000000000000, -0.7071067811865604513 ) ) ;
#5985 = FACE_OUTER_BOUND ( 'NONE', #54548, .T. ) ;
#5986 = AXIS2_PLACEMENT_3D ( 'NONE', #7656, #14927, #35344 ) ;
#5987 = ADVANCED_FACE ( 'NONE', ( #44721 ), #10218, .T. ) ;
#5988 = CYLINDRICAL_SURFACE ( 'NONE', #36500, 0.9999999999999731326 ) ;
#5989 = ORIENTED_EDGE ( 'NONE', *, *, #47000, .T. ) ;
#5990 = CARTESIAN_POINT ( 'NONE',  ( 99.27722696178533113, -43.74484797918319856, 56.90991099019593236 ) ) ;
#5991 = CARTESIAN_POINT ( 'NONE',  ( 106.8402480490632342, -48.62734320582506342, 73.56133956162497611 ) ) ;
#5992 = PRESENTATION_STYLE_ASSIGNMENT (( #68209 ) ) ;
#5994 = FACE_OUTER_BOUND ( 'NONE', #22245, .T. ) ;
#5993 = DIRECTION ( 'NONE',  ( 0.000000000000000000, 1.000000000000000000, 0.000000000000000000 ) ) ;
#5995 = CARTESIAN_POINT ( 'NONE',  ( 107.0664832912739399, -36.72944715994096754, 296.5517437918485939 ) ) ;
#5996 = CARTESIAN_POINT ( 'NONE',  ( -0.8322931907936803597, 69.95000000000001705, 118.3559999999999519 ) ) ;
#5997 = VERTEX_POINT ( 'NONE', #73326 ) ;
#5998 = CIRCLE ( 'NONE', #22017, 4.875000000000017764 ) ;
#5999 = DIRECTION ( 'NONE',  ( 9.351236661543306751E-17, -3.725950533538267725E-29, -1.000000000000000000 ) ) ;
#6000 = CIRCLE ( 'NONE', #69800, 7.499999999999996447 ) ;
#6001 = CARTESIAN_POINT ( 'NONE',  ( 107.0664832912750057, -36.72944715993903486, 9.125625275910969947 ) ) ;
#6002 = DIRECTION ( 'NONE',  ( 0.000000000000000000, 1.000000000000000000, 0.000000000000000000 ) ) ;
#6003 = VERTEX_POINT ( 'NONE', #79724 ) ;
#6004 = CARTESIAN_POINT ( 'NONE',  ( 97.20510023974232183, -31.68580462152881339, 91.96229194257693962 ) ) ;
#6006 = CARTESIAN_POINT ( 'NONE',  ( 0.000000000000000000, 92.07499999999998863, 39.10000000000005116 ) ) ;
#6005 = DIRECTION ( 'NONE',  ( 0.000000000000000000, 0.000000000000000000, 1.000000000000000000 ) ) ;
#6007 = CYLINDRICAL_SURFACE ( 'NONE', #84289, 2.749999999999974687 ) ;
#6008 = EDGE_CURVE ( 'NONE', #86967, #60336, #52402, .T. ) ;
#6009 = EDGE_CURVE ( 'NONE', #78871, #26653, #17480, .T. ) ;
#6010 = DIRECTION ( 'NONE',  ( 0.000000000000000000, 1.000000000000000000, 0.000000000000000000 ) ) ;
#6011 = ORIENTED_EDGE ( 'NONE', *, *, #6855, .T. ) ;
#6012 = EDGE_CURVE ( 'NONE', #17169, #71916, #56867, .T. ) ;
#6013 = CARTESIAN_POINT ( 'NONE',  ( 99.36524671511907059, -42.81259845621065807, 87.85848241876792031 ) ) ;
#6015 = EDGE_LOOP ( 'NONE', ( #61285, #39036, #56974, #71418 ) ) ;
#6014 = CARTESIAN_POINT ( 'NONE',  ( 12.06576689403630454, 86.60966479152391173, 129.9976963971240025 ) ) ;
#6016 = VECTOR ( 'NONE', #12823, 1000.000000000000000 ) ;
#6017 = EDGE_CURVE ( 'NONE', #11918, #36895, #80112, .T. ) ;
#6018 = CARTESIAN_POINT ( 'NONE',  ( 117.4525030917817645, -36.13006561810995976, 224.8727681330539667 ) ) ;
#6019 = DIRECTION ( 'NONE',  ( 0.000000000000000000, 0.000000000000000000, 1.000000000000000000 ) ) ;
#6020 = CARTESIAN_POINT ( 'NONE',  ( 116.5687119429383642, -33.54617018878323620, 149.0836319459096728 ) ) ;
#6021 = FACE_OUTER_BOUND ( 'NONE', #49369, .T. ) ;
#6022 = CARTESIAN_POINT ( 'NONE',  ( 109.7248659309123013, -27.00080518256924478, 80.86479194179250385 ) ) ;
#6023 = CARTESIAN_POINT ( 'NONE',  ( 144.0667052733537901, -83.77844715994089597, 55.21780685541800437 ) ) ;
#6024 = ADVANCED_FACE ( 'NONE', ( #10652 ), #38358, .F. ) ;
#6025 = CARTESIAN_POINT ( 'NONE',  ( -98.26026929335812099, 73.28356282573676594, 85.96437953530717380 ) ) ;
#6026 = CARTESIAN_POINT ( 'NONE',  ( 103.2980200187117390, -27.06831524915186904, 170.3603871806729444 ) ) ;
#6027 = ORIENTED_EDGE ( 'NONE', *, *, #49419, .T. ) ;
#6028 = ORIENTED_EDGE ( 'NONE', *, *, #41359, .T. ) ;
#6029 = CARTESIAN_POINT ( 'NONE',  ( 97.68334685095105385, -37.21243378447991290, 117.8111071154209526 ) ) ;
#6030 = EDGE_CURVE ( 'NONE', #26732, #33670, #35078, .T. ) ;
#6031 = CIRCLE ( 'NONE', #58270, 5.599999999999994316 ) ;
#6032 = DIRECTION ( 'NONE',  ( 1.000000000000000000, 0.000000000000000000, 0.000000000000000000 ) ) ;
#6034 = DIRECTION ( 'NONE',  ( 4.299999999999999979E-14, -1.000000000000000000, 4.400000000000000367E-29 ) ) ;
#6033 = CARTESIAN_POINT ( 'NONE',  ( 100.0046238269857639, -29.91446987444276928, 246.7156252759109520 ) ) ;
#6035 = DIRECTION ( 'NONE',  ( -1.000000000000000078E-15, 0.000000000000000000, 1.000000000000000000 ) ) ;
#6036 = EDGE_CURVE ( 'NONE', #57999, #76564, #46678, .T. ) ;
#6037 = DIRECTION ( 'NONE',  ( 0.000000000000000000, 1.000000000000000000, 0.000000000000000000 ) ) ;
#6038 = FACE_OUTER_BOUND ( 'NONE', #60661, .T. ) ;
#6039 = DIRECTION ( 'NONE',  ( 0.000000000000000000, -1.000000000000000000, 0.000000000000000000 ) ) ;
#6040 = DIRECTION ( 'NONE',  ( 0.7071067811865446862, -0.7071067811865504593, 0.000000000000000000 ) ) ;
#6041 = B_SPLINE_SURFACE_WITH_KNOTS ( 'NONE', 3, 3, ( 
 ( #46816, #74104, #23846, #64722 ),
 ( #25959, #79261, #74549, #65162 ),
 ( #17023, #44706, #64285, #11429 ),
 ( #2057, #39131, #32303, #87732 ),
 ( #25504, #46370, #57447, #85189 ),
 ( #22961, #78376, #51078, #16138 ),
 ( #71554, #37017, #61356, #67738 ) ),
 .UNSPECIFIED., .F., .F., .F.,
 ( 4, 1, 1, 1, 4 ),
 ( 4, 4 ),
 ( -0.0004298309602272039798, 0.2857142857142860315, 0.5714285714285709528, 0.8571428571428569843, 1.000429830960229971 ),
 ( 0.08686432420013849576, 1.000429830960229971 ),
 .UNSPECIFIED. ) ;
#6042 = CARTESIAN_POINT ( 'NONE',  ( 103.7301789885933658, -26.21598454391059363, 205.3089586092439731 ) ) ;
#6043 = FACE_OUTER_BOUND ( 'NONE', #3274, .T. ) ;
#6044 = EDGE_LOOP ( 'NONE', ( #76094, #26745 ) ) ;
#6045 = ORIENTED_EDGE ( 'NONE', *, *, #75444, .T. ) ;
#6046 = AXIS2_PLACEMENT_3D ( 'NONE', #3556, #53001, #61637 ) ;
#6047 = DIRECTION ( 'NONE',  ( 0.000000000000000000, 0.000000000000000000, -1.000000000000000000 ) ) ;
#6048 = CARTESIAN_POINT ( 'NONE',  ( 79.31510987520707090, -16.05633243510678554, 1.690787911858472770 ) ) ;
#6049 = LINE ( 'NONE', #12398, #89676 ) ;
#6050 = CARTESIAN_POINT ( 'NONE',  ( 36.65249034007535300, -49.32844715994124130, 249.9678068554150343 ) ) ;
#6051 = AXIS2_PLACEMENT_3D ( 'NONE', #88438, #81637, #18938 ) ;
#6052 = CARTESIAN_POINT ( 'NONE',  ( 25.56670390244797275, -58.35344715994099829, 134.4678068554150059 ) ) ;
#6053 = ORIENTED_EDGE ( 'NONE', *, *, #84154, .F. ) ;
#6054 = CARTESIAN_POINT ( 'NONE',  ( 100.8869726253045513, -44.69981113982900922, 62.05224101154388450 ) ) ;
#6055 = CARTESIAN_POINT ( 'NONE',  ( 118.7903470546216482, -38.45904373001069843, 223.7099109901969598 ) ) ;
#6056 = VERTEX_POINT ( 'NONE', #4744 ) ;
#6057 = CIRCLE ( 'NONE', #51036, 175.7032523792620111 ) ;
#6058 = CARTESIAN_POINT ( 'NONE',  ( -7.674860457568732031, 92.55144245102577827, 118.3077557055132161 ) ) ;
#6059 = LINE ( 'NONE', #33747, #39093 ) ;
#6060 = DIRECTION ( 'NONE',  ( -4.237773401492740281E-14, 1.000000000000000000, 0.000000000000000000 ) ) ;
#6061 = CARTESIAN_POINT ( 'NONE',  ( 109.0595394021483742, -27.66723669546327358, 27.72237608387795404 ) ) ;
#6062 = CARTESIAN_POINT ( 'NONE',  ( 116.8268856436350518, -43.49382415615948361, 159.3441967044829539 ) ) ;
#6063 = DIRECTION ( 'NONE',  ( 1.000000000000000000, 0.000000000000000000, 0.000000000000000000 ) ) ;
#6064 = ORIENTED_EDGE ( 'NONE', *, *, #6716, .T. ) ;
#6065 = EDGE_CURVE ( 'NONE', #73752, #73831, #6095, .T. ) ;
#6066 = DIRECTION ( 'NONE',  ( -2.108538789381372925E-16, 0.5150380749100580413, 0.8571673007021100021 ) ) ;
#6067 = CARTESIAN_POINT ( 'NONE',  ( 115.6377686515996999, -42.05128457402461351, 68.38507870720354731 ) ) ;
#6068 = ORIENTED_EDGE ( 'NONE', *, *, #82003, .F. ) ;
#6069 = EDGE_LOOP ( 'NONE', ( #19306, #40053, #46832, #51115 ) ) ;
#6070 = CARTESIAN_POINT ( 'NONE',  ( 3.292096649336123892, 94.82294024675948663, 118.5109520256350208 ) ) ;
#6071 = ORIENTED_EDGE ( 'NONE', *, *, #10614, .T. ) ;
#6072 = ORIENTED_EDGE ( 'NONE', *, *, #38605, .T. ) ;
#6073 = DIRECTION ( 'NONE',  ( 0.8660254037844390407, 0.000000000000000000, -0.4999999999999995004 ) ) ;
#6074 = CARTESIAN_POINT ( 'NONE',  ( 109.1774539423994952, -45.00591588954721800, 47.19813411379097801 ) ) ;
#6075 = CARTESIAN_POINT ( 'NONE',  ( 97.45268567403179816, -40.90835349962023315, 231.6527681330539679 ) ) ;
#6076 = CARTESIAN_POINT ( 'NONE',  ( 97.93839266929572318, -41.72010113774609152, 221.7241967044819546 ) ) ;
#6078 = CARTESIAN_POINT ( 'NONE',  ( 101.6204011159890541, -47.22657592904984369, 13.19562527591094891 ) ) ;
#6077 = LINE ( 'NONE', #33766, #20000 ) ;
#6079 = DIRECTION ( 'NONE',  ( 0.000000000000000000, 1.000000000000000000, 0.000000000000000000 ) ) ;
#6080 = DIRECTION ( 'NONE',  ( 0.000000000000000000, 1.000000000000000000, 0.000000000000000000 ) ) ;
#6081 = ORIENTED_EDGE ( 'NONE', *, *, #80766, .T. ) ;
#6082 = VECTOR ( 'NONE', #11793, 1000.000000000000000 ) ;
#6083 = AXIS2_PLACEMENT_3D ( 'NONE', #79258, #54520, #62255 ) ;
#6084 = CARTESIAN_POINT ( 'NONE',  ( 97.28369645613162220, -37.51102008256657427, 101.3899109901979472 ) ) ;
#6085 = EDGE_CURVE ( 'NONE', #30833, #66460, #68313, .T. ) ;
#6086 = CARTESIAN_POINT ( 'NONE',  ( 113.3690198962888758, -27.59211078819982887, 89.60800622829195561 ) ) ;
#6087 = CARTESIAN_POINT ( 'NONE',  ( 118.1543649935527185, -36.20813824561556515, 268.8518157521014587 ) ) ;
#6088 = ORIENTED_EDGE ( 'NONE', *, *, #85066, .T. ) ;
#6089 = CARTESIAN_POINT ( 'NONE',  ( 96.85831052012196096, -34.61278962133658155, 216.1641967044819808 ) ) ;
#6090 = CARTESIAN_POINT ( 'NONE',  ( 107.0664832912739968, -36.72944715994100306, 287.6356252759109680 ) ) ;
#6091 = CARTESIAN_POINT ( 'NONE',  ( 99.50458969558927436, -43.30562421865187872, 22.89600243872639140 ) ) ;
#6092 = LINE ( 'NONE', #12449, #22404 ) ;
#6094 = DIRECTION ( 'NONE',  ( -0.000000000000000000, 1.000000000000000000, 0.000000000000000000 ) ) ;
#6093 = CARTESIAN_POINT ( 'NONE',  ( 114.7357040289479642, -40.07855725538382075, 277.6356252759111953 ) ) ;
#6095 = LINE ( 'NONE', #18361, #87295 ) ;
#6096 = DIRECTION ( 'NONE',  ( 1.000000000000000078E-15, -1.000000000000000083E-30, -1.000000000000000000 ) ) ;
#6097 = CARTESIAN_POINT ( 'NONE',  ( 106.5667039024470313, -108.2470741265389620, -19.78219314458190681 ) ) ;
#6098 = DIRECTION ( 'NONE',  ( 0.000000000000000000, 1.000000000000000000, 0.000000000000000000 ) ) ;
#6099 = FACE_OUTER_BOUND ( 'NONE', #72737, .T. ) ;
#6100 = CARTESIAN_POINT ( 'NONE',  ( -27.27158787008326968, 184.0000000000000000, 90.32146847885337593 ) ) ;
#6101 = VECTOR ( 'NONE', #34390, 1000.000000000000000 ) ;
#6103 = ORIENTED_EDGE ( 'NONE', *, *, #36413, .F. ) ;
#6102 = CARTESIAN_POINT ( 'NONE',  ( 101.1435383712028511, -28.73162758398862238, 195.5838068554171514 ) ) ;
#6104 = CYLINDRICAL_SURFACE ( 'NONE', #64082, 0.4999999999999982236 ) ;
#6105 = CARTESIAN_POINT ( 'NONE',  ( 100.7367085078155640, -45.81951824476916357, 237.0803871806729717 ) ) ;
#6106 = CARTESIAN_POINT ( 'NONE',  ( 103.1746689306972939, -27.05803214298817849, 126.3813395616259783 ) ) ;
#6107 = CARTESIAN_POINT ( 'NONE',  ( 101.2698767154569168, -26.33663883357058921, 251.4813395616249920 ) ) ;
#6108 = CARTESIAN_POINT ( 'NONE',  ( 88.90000000000000568, 66.67499999999999716, 244.4749999999999943 ) ) ;
#6109 = FACE_OUTER_BOUND ( 'NONE', #40985, .T. ) ;
#6111 = DIRECTION ( 'NONE',  ( 1.000000000000000000, -5.337610695313248426E-16, 0.000000000000000000 ) ) ;
#6110 = DIRECTION ( 'NONE',  ( -1.000000000000000000, 0.000000000000000000, 0.000000000000000000 ) ) ;
#6112 = DIRECTION ( 'NONE',  ( -1.000000000000000000, 0.000000000000000000, 0.000000000000000000 ) ) ;
#6113 = AXIS2_PLACEMENT_3D ( 'NONE', #34013, #61714, #14494 ) ;
#6114 = CARTESIAN_POINT ( 'NONE',  ( -465.6921742093539933, 60.32499999999999574, -3.174999999999999822 ) ) ;
#6115 = VECTOR ( 'NONE', #1267, 1000.000000000000000 ) ;
#6116 = ORIENTED_EDGE ( 'NONE', *, *, #76740, .T. ) ;
#6117 = ORIENTED_EDGE ( 'NONE', *, *, #29807, .T. ) ;
#6118 = EDGE_CURVE ( 'NONE', #686, #19911, #65828, .T. ) ;
#6119 = CIRCLE ( 'NONE', #26402, 25.39999999999999858 ) ;
#6120 = CARTESIAN_POINT ( 'NONE',  ( 108.3145574644059224, -45.20850512633867169, 142.1152769709339907 ) ) ;
#6122 = ORIENTED_EDGE ( 'NONE', *, *, #8150, .T. ) ;
#6121 = LINE ( 'NONE', #73807, #22688 ) ;
#6123 = LINE ( 'NONE', #53328, #25685 ) ;
#6124 = EDGE_CURVE ( 'NONE', #1539, #13040, #66964, .T. ) ;
#6125 = CARTESIAN_POINT ( 'NONE',  ( 96.72090476913471946, -37.82382852467499390, 122.4099109901969626 ) ) ;
#6126 = CARTESIAN_POINT ( 'NONE',  ( 105.7137884042412139, -46.72360237654041271, 148.4694629689294061 ) ) ;
#6127 = ADVANCED_FACE ( 'NONE', ( #34225 ), #74235, .T. ) ;
#6128 = AXIS2_PLACEMENT_3D ( 'NONE', #20061, #25977, #47294 ) ;
#6129 = DIRECTION ( 'NONE',  ( -0.000000000000000000, 1.000000000000000000, 0.000000000000000000 ) ) ;
#6130 = LINE ( 'NONE', #74709, #43288 ) ;
#6131 = EDGE_CURVE ( 'NONE', #43708, #22746, #39694, .T. ) ;
#6132 = DIRECTION ( 'NONE',  ( 1.000000000000000078E-15, -1.000000000000000000, 0.000000000000000000 ) ) ;
#6133 = CARTESIAN_POINT ( 'NONE',  ( 113.0644005321300511, -46.09090919705352718, 68.02991099019695298 ) ) ;
#6134 = ORIENTED_EDGE ( 'NONE', *, *, #75777, .T. ) ;
#6135 = VERTEX_POINT ( 'NONE', #80612 ) ;
#6136 = ORIENTED_EDGE ( 'NONE', *, *, #29617, .T. ) ;
#6137 = CARTESIAN_POINT ( 'NONE',  ( 107.5667039024470313, -100.3098201933451605, -19.78219314458212708 ) ) ;
#6139 = DIRECTION ( 'NONE',  ( 0.000000000000000000, 1.000000000000000000, 0.000000000000000000 ) ) ;
#6138 = CARTESIAN_POINT ( 'NONE',  ( 114.0663967180212950, -29.08153105160607410, 150.4746728949579619 ) ) ;
#6140 = CARTESIAN_POINT ( 'NONE',  ( 144.1741131095133994, -138.0461895383712942, 247.6591799766680140 ) ) ;
#6141 = CARTESIAN_POINT ( 'NONE',  ( 182.4202572930258839, -31.94127993907126140, 237.4678068554150059 ) ) ;
#6142 = ADVANCED_FACE ( 'NONE', ( #60128 ), #60583, .T. ) ;
#6143 = CARTESIAN_POINT ( 'NONE',  ( 86.06670390244796920, -50.82844715994100682, 250.9178068554150514 ) ) ;
#6144 = CARTESIAN_POINT ( 'NONE',  ( 92.32962665258456525, 82.54999999999999716, 74.36911441044829019 ) ) ;
#6145 = CYLINDRICAL_SURFACE ( 'NONE', #12475, 2.517499999999998739 ) ;
#6146 = CARTESIAN_POINT ( 'NONE',  ( 115.1498815335951491, -43.27828968249936992, 88.28419670448195689 ) ) ;
#6147 = VERTEX_POINT ( 'NONE', #67399 ) ;
#6148 = VERTEX_POINT ( 'NONE', #81517 ) ;
#6149 = ORIENTED_EDGE ( 'NONE', *, *, #14150, .T. ) ;
#6150 = CARTESIAN_POINT ( 'NONE',  ( 51.06648329127400388, 19.62155284005901024, 333.4006252759110112 ) ) ;
#6151 = CARTESIAN_POINT ( 'NONE',  ( -92.02731164704657374, 95.25015599858943460, -92.60677566276801542 ) ) ;
#6152 = AXIS2_PLACEMENT_3D ( 'NONE', #57490, #49768, #42502 ) ;
#6153 = DIRECTION ( 'NONE',  ( 0.000000000000000000, -1.000000000000000000, 0.000000000000000000 ) ) ;
#6154 = CARTESIAN_POINT ( 'NONE',  ( 116.3142130228717264, -37.48801553205211690, 186.5795189410199555 ) ) ;
#6155 = CIRCLE ( 'NONE', #56895, 2.517500000000005844 ) ;
#6156 = CARTESIAN_POINT ( 'NONE',  ( 97.07209691576048272, -35.37819998029382162, 27.21882120925108239 ) ) ;
#6157 = EDGE_LOOP ( 'NONE', ( #84451, #51196, #64072, #13535 ) ) ;
#6159 = VERTEX_POINT ( 'NONE', #19270 ) ;
#6158 = ORIENTED_EDGE ( 'NONE', *, *, #70057, .F. ) ;
#6160 = DIRECTION ( 'NONE',  ( -1.000000000000000078E-15, 1.000000000000000083E-30, 1.000000000000000000 ) ) ;
#6161 = CARTESIAN_POINT ( 'NONE',  ( 134.0664832912739826, -21.47944715994100306, 1.625625275910997480 ) ) ;
#6162 = VERTEX_POINT ( 'NONE', #21059 ) ;
#6163 = ORIENTED_EDGE ( 'NONE', *, *, #33409, .T. ) ;
#6164 = CARTESIAN_POINT ( 'NONE',  ( 77.43469508765193154, -19.52719034724596270, 6.916533740477924574 ) ) ;
#6165 = AXIS2_PLACEMENT_3D ( 'NONE', #29279, #27475, #76071 ) ;
#6166 = CARTESIAN_POINT ( 'NONE',  ( 106.8838381269920745, -46.12323054477403161, 223.9806309249449612 ) ) ;
#6167 = EDGE_CURVE ( 'NONE', #20535, #26172, #16240, .T. ) ;
#6168 = CARTESIAN_POINT ( 'NONE',  ( 158.0667039024469886, -67.87844715994090450, 85.21780685541799016 ) ) ;
#6169 = CARTESIAN_POINT ( 'NONE',  ( -112.4269219824620478, 67.52370228190351042, 66.37105824381433195 ) ) ;
#6170 = ORIENTED_EDGE ( 'NONE', *, *, #39839, .T. ) ;
#6171 = VERTEX_POINT ( 'NONE', #34673 ) ;
#6172 = AXIS2_PLACEMENT_3D ( 'NONE', #87194, #24958, #10438 ) ;
#6173 = CARTESIAN_POINT ( 'NONE',  ( 107.0667039024479834, -36.72944715994100306, 239.5838068554170093 ) ) ;
#6174 = ORIENTED_EDGE ( 'NONE', *, *, #42937, .F. ) ;
#6175 = ORIENTED_EDGE ( 'NONE', *, *, #43855, .F. ) ;
#6176 = EDGE_CURVE ( 'NONE', #1337, #53380, #82971, .T. ) ;
#6177 = AXIS2_PLACEMENT_3D ( 'NONE', #63854, #43383, #64303 ) ;
#6178 = CARTESIAN_POINT ( 'NONE',  ( 102.8259602516037177, -43.70423678882019658, 244.9595189410199794 ) ) ;
#6179 = CARTESIAN_POINT ( 'NONE',  ( 95.28658997325378266, -38.28252189325972665, 151.4299109901969871 ) ) ;
#6180 = CARTESIAN_POINT ( 'NONE',  ( 110.4495079430909641, -47.22796928374267367, 57.83657765686300678 ) ) ;
#6181 = CARTESIAN_POINT ( 'NONE',  ( 112.3819288266831933, -43.64340785303151904, 249.5838068554168956 ) ) ;
#6182 = CARTESIAN_POINT ( 'NONE',  ( 188.5667039024479834, -65.37844715994100397, 173.2178068554149775 ) ) ;
#6183 = CARTESIAN_POINT ( 'NONE',  ( 108.0878824955162969, -25.31592121169968479, 322.1035414506763459 ) ) ;
#6184 = CARTESIAN_POINT ( 'NONE',  ( 106.9749963086187279, -47.15413504876184447, 183.5699109901969734 ) ) ;
#6185 = DIRECTION ( 'NONE',  ( -1.000000000000000078E-15, 1.000000000000000083E-30, 1.000000000000000000 ) ) ;
#6186 = ORIENTED_EDGE ( 'NONE', *, *, #1081, .F. ) ;
#6187 = CARTESIAN_POINT ( 'NONE',  ( -129.9368274816651194, 81.71102547120852932, 12.69999999999954809 ) ) ;
#6188 = ORIENTED_EDGE ( 'NONE', *, *, #16385, .F. ) ;
#6189 = ORIENTED_EDGE ( 'NONE', *, *, #87977, .F. ) ;
#6190 = DIRECTION ( 'NONE',  ( 0.000000000000000000, 0.000000000000000000, 1.000000000000000000 ) ) ;
#6191 = ORIENTED_EDGE ( 'NONE', *, *, #64163, .T. ) ;
#6192 = DIRECTION ( 'NONE',  ( -3.100000000000000258E-29, 3.100000000000000044E-14, 1.000000000000000000 ) ) ;
#6193 = ADVANCED_FACE ( 'NONE', ( #82854 ), #14248, .T. ) ;
#6194 =( BOUNDED_CURVE ( )  B_SPLINE_CURVE ( 3, ( #77075, #51572, #3000, #72921 ),
 .UNSPECIFIED., .F., .F. ) 
 B_SPLINE_CURVE_WITH_KNOTS ( ( 4, 4 ),
 ( 3.141592653593537232, 4.712388980388810822 ),
 .UNSPECIFIED. ) 
 CURVE ( )  GEOMETRIC_REPRESENTATION_ITEM ( )  RATIONAL_B_SPLINE_CURVE ( ( 1.000000000000000000, 0.8047378541242761196, 0.8047378541242761196, 1.000000000000000000 ) ) 
 REPRESENTATION_ITEM ( '' )  );
#6195 = CARTESIAN_POINT ( 'NONE',  ( 102.5580992528948912, -27.32936716964785262, 95.43276813305395478 ) ) ;
#6196 = CARTESIAN_POINT ( 'NONE',  ( -7.057195792612153795, 71.99130726259811297, 130.3651223555374941 ) ) ;
#6197 = CARTESIAN_POINT ( 'NONE',  ( -50.03799999999999670, 0.000000000000000000, 206.3750000000000000 ) ) ;
#6198 = PLANE ( 'NONE',  #52814 ) ;
#6201 = CARTESIAN_POINT ( 'NONE',  ( 101.4371718687638406, -46.21494532752021200, 203.1622919425779514 ) ) ;
#6200 = LINE ( 'NONE', #12563, #31077 ) ;
#6199 = DIRECTION ( 'NONE',  ( 0.000000000000000000, 0.000000000000000000, -1.000000000000000000 ) ) ;
#6202 = DIRECTION ( 'NONE',  ( 1.000000000000000078E-15, -1.000000000000000083E-30, -1.000000000000000000 ) ) ;
#6203 = FACE_OUTER_BOUND ( 'NONE', #78703, .T. ) ;
#6204 = EDGE_LOOP ( 'NONE', ( #70066, #3026, #55067, #82122 ) ) ;
#6205 = FACE_OUTER_BOUND ( 'NONE', #16900, .T. ) ;
#6206 = VECTOR ( 'NONE', #17621, 1000.000000000000000 ) ;
#6207 = CARTESIAN_POINT ( 'NONE',  ( -3.968750000000770051, 120.6499999999999915, 105.4788588808462038 ) ) ;
#6208 = DIRECTION ( 'NONE',  ( 1.000000000000000078E-15, -1.000000000000000083E-30, -1.000000000000000000 ) ) ;
#6209 = CARTESIAN_POINT ( 'NONE',  ( -89.60916260784479448, 238.5000000000000000, 134.1927865330827103 ) ) ;
#6211 = ORIENTED_EDGE ( 'NONE', *, *, #47633, .F. ) ;
#6210 = CARTESIAN_POINT ( 'NONE',  ( 100.2192867603235840, -28.80968922735345927, 260.6441967044821695 ) ) ;
#6212 = CARTESIAN_POINT ( 'NONE',  ( -3.174999999999664979, 111.1250000000000000, -31.75000000000000000 ) ) ;
#6213 = CARTESIAN_POINT ( 'NONE',  ( 117.4513846513745960, -35.59318846168486772, 274.9127681330539872 ) ) ;
#6214 = CARTESIAN_POINT ( 'NONE',  ( 114.5432832596865325, -29.39626808186021378, 145.4441967044819819 ) ) ;
#6215 = DIRECTION ( 'NONE',  ( -1.000000000000000000, 0.000000000000000000, 0.000000000000000000 ) ) ;
#6216 = CARTESIAN_POINT ( 'NONE',  ( 97.80494262393504812, -40.50090711907665764, 102.6342054156130246 ) ) ;
#6218 = PLANE ( 'NONE',  #57329 ) ;
#6217 = DIRECTION ( 'NONE',  ( 0.000000000000000000, 0.000000000000000000, 1.000000000000000000 ) ) ;
#6219 = CARTESIAN_POINT ( 'NONE',  ( 134.0664832912740110, -46.72944715994100306, 4.925625275910997303 ) ) ;
#6220 = CARTESIAN_POINT ( 'NONE',  ( -487.2989999999999782, 86.51875000000001137, 94.61194598552339130 ) ) ;
#6221 = ORIENTED_EDGE ( 'NONE', *, *, #60158, .T. ) ;
#6222 = CIRCLE ( 'NONE', #81646, 2.500000000000002220 ) ;
#6223 = ORIENTED_EDGE ( 'NONE', *, *, #82792, .T. ) ;
#6224 = ORIENTED_EDGE ( 'NONE', *, *, #69511, .T. ) ;
#6225 = EDGE_CURVE ( 'NONE', #59810, #42074, #66992, .T. ) ;
#6226 = VERTEX_POINT ( 'NONE', #42370 ) ;
#6227 = CARTESIAN_POINT ( 'NONE',  ( 107.5667039024470455, -113.7784471599420613, -19.78219314458171141 ) ) ;
#6228 = CARTESIAN_POINT ( 'NONE',  ( 116.4547782460826255, -32.24742764444982157, 15.18133956162492915 ) ) ;
#6229 = CARTESIAN_POINT ( 'NONE',  ( 164.9667039024475059, -28.27351298636832766, 237.4678068554150059 ) ) ;
#6230 = ADVANCED_FACE ( 'NONE', ( #55093 ), #76016, .T. ) ;
#6231 = DIRECTION ( 'NONE',  ( -0.000000000000000000, -0.000000000000000000, -1.000000000000000000 ) ) ;
#6232 = CARTESIAN_POINT ( 'NONE',  ( 182.4202572930400095, -33.70561438051981185, -5.074374724088000832 ) ) ;
#6233 = CARTESIAN_POINT ( 'NONE',  ( 116.0913394378304702, -33.14858145062638073, 248.5495626852199678 ) ) ;
#6234 = ORIENTED_EDGE ( 'NONE', *, *, #59230, .T. ) ;
#6235 = ORIENTED_EDGE ( 'NONE', *, *, #28451, .T. ) ;
#6236 = EDGE_LOOP ( 'NONE', ( #15494, #3095, #25016, #35416 ) ) ;
#6237 = VECTOR ( 'NONE', #52625, 999.9999999999998863 ) ;
#6238 = CARTESIAN_POINT ( 'NONE',  ( 34.67381068360400320, -28.98061976758901892, -5.074374724088000832 ) ) ;
#6239 = CARTESIAN_POINT ( 'NONE',  ( 105.7155907543573790, -46.72387588654685686, 102.4688864389793110 ) ) ;
#6240 = DIRECTION ( 'NONE',  ( 6.524622321627019585E-16, 3.741823817616790462E-31, 1.000000000000000000 ) ) ;
#6241 = CARTESIAN_POINT ( 'NONE',  ( 99.09464024186353015, -30.55185734356122396, 275.8020006352290352 ) ) ;
#6242 = AXIS2_PLACEMENT_3D ( 'NONE', #76921, #14249, #8788 ) ;
#6243 = DIRECTION ( 'NONE',  ( 0.000000000000000000, 1.000000000000000000, 0.000000000000000000 ) ) ;
#6244 = EDGE_CURVE ( 'NONE', #81257, #74753, #51042, .T. ) ;
#6245 = DIRECTION ( 'NONE',  ( 0.000000000000000000, 1.000000000000000000, 0.000000000000000000 ) ) ;
#6246 = ADVANCED_FACE ( 'NONE', ( #69655 ), #43271, .F. ) ;
#6247 = CARTESIAN_POINT ( 'NONE',  ( 105.2300248619626757, -26.52326248392216357, 275.2061014663877927 ) ) ;
#6248 = DIRECTION ( 'NONE',  ( 4.299999999999999979E-14, -1.000000000000000000, 4.400000000000000367E-29 ) ) ;
#6249 = VERTEX_POINT ( 'NONE', #8328 ) ;
#6250 = LINE ( 'NONE', #68921, #12940 ) ;
#6251 = DIRECTION ( 'NONE',  ( 1.000000000000000078E-15, 1.000000000000000083E-30, -1.000000000000000000 ) ) ;
#6252 = CARTESIAN_POINT ( 'NONE',  ( 114.9276189159122907, -38.92769025571944042, 96.42809036959192781 ) ) ;
#6253 = DIRECTION ( 'NONE',  ( 0.000000000000000000, 0.000000000000000000, 1.000000000000000000 ) ) ;
#6254 = CARTESIAN_POINT ( 'NONE',  ( 97.81169160209351787, -40.51741184665055329, 67.63577596198375375 ) ) ;
#6255 = ORIENTED_EDGE ( 'NONE', *, *, #19055, .F. ) ;
#6256 = CARTESIAN_POINT ( 'NONE',  ( 78.35735255115685050, -34.57277629267482411, 7.749696248610925764 ) ) ;
#6257 = VECTOR ( 'NONE', #72913, 1000.000000000000000 ) ;
#6258 = ORIENTED_EDGE ( 'NONE', *, *, #53593, .T. ) ;
#6259 = CARTESIAN_POINT ( 'NONE',  ( 97.98636869442889008, -41.85180495037556625, 136.7356252759109623 ) ) ;
#6260 = EDGE_LOOP ( 'NONE', ( #79761, #49258, #35291, #60478 ) ) ;
#6261 = CARTESIAN_POINT ( 'NONE',  ( 41.56648329127499153, -32.07844715994070839, 263.6756252759120116 ) ) ;
#6262 = CARTESIAN_POINT ( 'NONE',  ( 98.20536012454746810, -36.63577306554869750, 107.7501547344689783 ) ) ;
#6263 = CARTESIAN_POINT ( 'NONE',  ( 63.03715912545826683, -46.82818131006018092, 236.4678068554150343 ) ) ;
#6264 = CARTESIAN_POINT ( 'NONE',  ( 74.67063729340679856, -69.52133568612056536, 247.5307829608580050 ) ) ;
#6265 = CARTESIAN_POINT ( 'NONE',  ( 118.8673094125028200, -35.40175986820349152, 79.91562527591095488 ) ) ;
#6266 = AXIS2_PLACEMENT_3D ( 'NONE', #40173, #80645, #5682 ) ;
#6267 = CARTESIAN_POINT ( 'NONE',  ( 172.5667039024480687, -36.32844715993499563, 129.9678068554150059 ) ) ;
#6268 = ORIENTED_EDGE ( 'NONE', *, *, #25378, .T. ) ;
#6269 = LINE ( 'NONE', #343, #54088 ) ;
#6270 = ORIENTED_EDGE ( 'NONE', *, *, #26131, .F. ) ;
#6271 = ORIENTED_EDGE ( 'NONE', *, *, #25926, .T. ) ;
#6272 = ADVANCED_FACE ( 'NONE', ( #62379, #41476 ), #1520, .T. ) ;
#6273 = DIRECTION ( 'NONE',  ( 0.000000000000000000, 0.000000000000000000, 1.000000000000000000 ) ) ;
#6274 = ORIENTED_EDGE ( 'NONE', *, *, #68447, .F. ) ;
#6275 = CARTESIAN_POINT ( 'NONE',  ( 97.83217745605946902, -40.05230289513916375, 266.6013395616258776 ) ) ;
#6276 = CARTESIAN_POINT ( 'NONE',  ( 95.28708132950120557, -38.28245711228485959, 147.4299109901969871 ) ) ;
#6277 = CARTESIAN_POINT ( 'NONE',  ( -123.4696824136392053, 20.32000000000000028, -179.8898777604655095 ) ) ;
#6278 = CARTESIAN_POINT ( 'NONE',  ( 108.4174892569846946, -26.73503592839110610, 140.9689586088591966 ) ) ;
#6279 = B_SPLINE_CURVE_WITH_KNOTS ( 'NONE', 3,
 ( #22716, #36336, #35422, #84047, #70413, #14097, #41777, #63592, #43125, #64045, #49942, #56302, #69513, #34975, #14999, #41330, #42673, #84950 ),
 .UNSPECIFIED., .F., .F.,
 ( 4, 2, 2, 2, 2, 2, 2, 2, 4 ),
 ( 0.5000003672892693318, 0.5625003213781106792, 0.6250002754669520266, 0.6875002295557932630, 0.7500001836446346104, 0.8125001377334759578, 0.8750000918223173052, 0.9375000459111586526, 1.000000000000000000 ),
 .UNSPECIFIED. ) ;
#6280 = CARTESIAN_POINT ( 'NONE',  ( 110.1579320793587442, -46.68562272277494429, 93.81562527591097478 ) ) ;
#6281 = CARTESIAN_POINT ( 'NONE',  ( 108.4209149160002710, -26.73547159001482498, 95.96804306659618078 ) ) ;
#6282 = ORIENTED_EDGE ( 'NONE', *, *, #88739, .F. ) ;
#6283 = DIRECTION ( 'NONE',  ( 0.000000000000000000, 0.000000000000000000, 1.000000000000000000 ) ) ;
#6284 = CARTESIAN_POINT ( 'NONE',  ( 112.0662701423777463, -45.48819631686011888, 158.9896538191669606 ) ) ;
#6285 = ORIENTED_EDGE ( 'NONE', *, *, #3191, .F. ) ;
#6286 = CIRCLE ( 'NONE', #41096, 7.143749999999999822 ) ;
#6287 = DIRECTION ( 'NONE',  ( 0.000000000000000000, -1.000000000000000000, 0.000000000000000000 ) ) ;
#6288 = EDGE_CURVE ( 'NONE', #72100, #74329, #50086, .T. ) ;
#6289 = CYLINDRICAL_SURFACE ( 'NONE', #80350, 4.749999999999976907 ) ;
#6290 = CARTESIAN_POINT ( 'NONE',  ( 100.2615012876617726, -45.41023301258256595, 277.0594347997204636 ) ) ;
#6291 = DIRECTION ( 'NONE',  ( -0.7071067811864634178, 0.7071067811866316166, -7.071067811864330499E-16 ) ) ;
#6292 = AXIS2_PLACEMENT_3D ( 'NONE', #14676, #55969, #6952 ) ;
#6293 = CARTESIAN_POINT ( 'NONE',  ( 107.5667039024470313, -100.3098201933444926, 2.217806855417892020 ) ) ;
#6294 = CARTESIAN_POINT ( 'NONE',  ( 56.06670390244700997, -79.67844715994098692, 120.2178068554179902 ) ) ;
#6295 = CARTESIAN_POINT ( 'NONE',  ( 103.0217603569634690, -26.37318327779222216, 20.37276813305394185 ) ) ;
#6297 = CARTESIAN_POINT ( 'NONE',  ( 108.5348814579965904, -26.43029805172858460, 100.9641967044829727 ) ) ;
#6296 = CARTESIAN_POINT ( 'NONE',  ( 97.79849751320908524, -40.48507364506422590, 101.6332966594512754 ) ) ;
#6298 = CARTESIAN_POINT ( 'NONE',  ( 48.79742451362098166, -36.32844715994040996, -5.074374724088000832 ) ) ;
#6299 = CARTESIAN_POINT ( 'NONE',  ( 102.9497400982657069, -26.42094052169726837, 175.3908633711489813 ) ) ;
#6300 = DIRECTION ( 'NONE',  ( 0.7017307308178937220, -0.7121747104280534701, -0.01952340268762070216 ) ) ;
#6301 = VERTEX_POINT ( 'NONE', #8786 ) ;
#6302 = LINE ( 'NONE', #80835, #13495 ) ;
#6303 = CARTESIAN_POINT ( 'NONE',  ( 83.06670390244796920, -67.87844715994100397, 231.5838068554150198 ) ) ;
#6304 = DIRECTION ( 'NONE',  ( 1.000000000000000078E-15, -1.000000000000000000, 0.000000000000000000 ) ) ;
#6305 = ORIENTED_EDGE ( 'NONE', *, *, #50819, .T. ) ;
#6306 = ADVANCED_FACE ( 'NONE', ( #35116 ), #69207, .T. ) ;
#6307 = EDGE_CURVE ( 'NONE', #63968, #39230, #35592, .T. ) ;
#6308 = CARTESIAN_POINT ( 'NONE',  ( 98.35048176673211628, -31.65547862740807616, 61.90667382029496935 ) ) ;
#6310 = ORIENTED_EDGE ( 'NONE', *, *, #55368, .T. ) ;
#6309 = CARTESIAN_POINT ( 'NONE',  ( 109.5188487141873850, -46.90749067903785630, 132.7641967044819751 ) ) ;
#6311 = CYLINDRICAL_SURFACE ( 'NONE', #45112, 4.750000000000004441 ) ;
#6312 = CARTESIAN_POINT ( 'NONE',  ( -130.1664033068596495, 90.28418055714726620, 10.08203418473845936 ) ) ;
#6313 = CARTESIAN_POINT ( 'NONE',  ( 90.44969454456405344, -20.11243780205715481, 229.5838068554169809 ) ) ;
#6314 = CARTESIAN_POINT ( 'NONE',  ( -458.3598257906459708, 47.62500000000000000, -3.174999999999999822 ) ) ;
#6315 = ORIENTED_EDGE ( 'NONE', *, *, #17305, .T. ) ;
#6316 = ITEM_DEFINED_TRANSFORMATION ( 'NONE', 'NONE', #46349,  #50656 ) ;
#6317 = AXIS2_PLACEMENT_3D ( 'NONE', #6229, #12594, #18957 ) ;
#6318 = EDGE_CURVE ( 'NONE', #86212, #51499, #17372, .T. ) ;
#6319 = ORIENTED_EDGE ( 'NONE', *, *, #2845, .F. ) ;
#6320 = ORIENTED_EDGE ( 'NONE', *, *, #66389, .F. ) ;
#6321 = EDGE_LOOP ( 'NONE', ( #5256, #65707, #58201, #18689 ) ) ;
#6322 = FACE_OUTER_BOUND ( 'NONE', #62638, .T. ) ;
#6323 = DIRECTION ( 'NONE',  ( 0.000000000000000000, 0.000000000000000000, -1.000000000000000000 ) ) ;
#6324 = FACE_OUTER_BOUND ( 'NONE', #47432, .T. ) ;
#6325 = ADVANCED_FACE ( 'NONE', ( #2410 ), #72785, .F. ) ;
#6326 = DIRECTION ( 'NONE',  ( -0.000000000000000000, 1.000000000000000000, -0.000000000000000000 ) ) ;
#6328 = CARTESIAN_POINT ( 'NONE',  ( 116.3212776292296127, -32.94146857471318413, 287.6356252759109680 ) ) ;
#6327 = CARTESIAN_POINT ( 'NONE',  ( 102.0669035284297479, -27.97058685607146700, 105.4898057718093156 ) ) ;
#6329 = DIRECTION ( 'NONE',  ( 1.000000000000000000, 1.000000000000000078E-15, 0.000000000000000000 ) ) ;
#6330 = ORIENTED_EDGE ( 'NONE', *, *, #3953, .T. ) ;
#6331 = CIRCLE ( 'NONE', #59991, 4.762500000000001066 ) ;
#6332 = ORIENTED_EDGE ( 'NONE', *, *, #9029, .T. ) ;
#6333 = DIRECTION ( 'NONE',  ( 0.000000000000000000, 0.000000000000000000, 1.000000000000000000 ) ) ;
#6334 = LINE ( 'NONE', #83106, #44742 ) ;
#6335 = CARTESIAN_POINT ( 'NONE',  ( 98.19951187208815213, -40.85743130997446571, 252.6727681330533812 ) ) ;
#6336 = DIRECTION ( 'NONE',  ( 0.5000000000000003331, 0.000000000000000000, 0.8660254037844383745 ) ) ;
#6337 = EDGE_CURVE ( 'NONE', #70385, #70167, #10112, .T. ) ;
#6338 = CARTESIAN_POINT ( 'NONE',  ( 118.1148702536303290, -35.48641528967803538, 79.91562527591095488 ) ) ;
#6340 = EDGE_CURVE ( 'NONE', #88945, #59559, #10994, .T. ) ;
#6339 = CYLINDRICAL_SURFACE ( 'NONE', #73404, 12.69999999999999929 ) ;
#6341 = ADVANCED_FACE ( 'NONE', ( #3303 ), #45491, .T. ) ;
#6342 = CARTESIAN_POINT ( 'NONE',  ( 111.0271110396046765, -27.49575338583956352, 20.75426942819767362 ) ) ;
#6343 = VERTEX_POINT ( 'NONE', #86428 ) ;
#6344 = LINE ( 'NONE', #34032, #80630 ) ;
#6345 = EDGE_CURVE ( 'NONE', #38746, #26493, #23513, .T. ) ;
#6346 = ORIENTED_EDGE ( 'NONE', *, *, #29504, .T. ) ;
#6347 = VERTEX_POINT ( 'NONE', #73214 ) ;
#6348 = CARTESIAN_POINT ( 'NONE',  ( 34.27482367531500529, -30.08671355700301575, -5.074374724088000832 ) ) ;
#6349 = CARTESIAN_POINT ( 'NONE',  ( 108.8902037297786762, -46.63625027785658972, 274.1530118773256390 ) ) ;
#6350 = AXIS2_PLACEMENT_3D ( 'NONE', #37482, #65185, #65626 ) ;
#6351 = DIRECTION ( 'NONE',  ( -0.9254794337955623007, -0.3787978585227819162, 0.000000000000000000 ) ) ;
#6352 = CARTESIAN_POINT ( 'NONE',  ( 100.9544641706648065, -28.70718897609401665, 140.5939795459164543 ) ) ;
#6353 = CARTESIAN_POINT ( 'NONE',  ( 97.07207206064353500, -35.37844118740781596, 81.21895860831540404 ) ) ;
#6354 = CARTESIAN_POINT ( 'NONE',  ( 89.12695577293594340, 72.47328848629024378, -78.17938156622481927 ) ) ;
#6355 = ORIENTED_EDGE ( 'NONE', *, *, #42854, .F. ) ;
#6356 = DIRECTION ( 'NONE',  ( -0.9999999853157766072, -0.0001713722456143214551, 0.000000000000000000 ) ) ;
#6357 = DIRECTION ( 'NONE',  ( 0.000000000000000000, -1.000000000000000000, 0.000000000000000000 ) ) ;
#6358 = ORIENTED_EDGE ( 'NONE', *, *, #42537, .F. ) ;
#6359 = CARTESIAN_POINT ( 'NONE',  ( 117.4878618838608872, -37.01562663403593234, 43.80419670448293346 ) ) ;
#6360 = VERTEX_POINT ( 'NONE', #29660 ) ;
#6361 = CARTESIAN_POINT ( 'NONE',  ( 114.0298635175061008, -31.59016113260716097, 257.1385665600676589 ) ) ;
#6362 = DIRECTION ( 'NONE',  ( 1.000000000000000000, 0.000000000000000000, 0.000000000000000000 ) ) ;
#6363 = CARTESIAN_POINT ( 'NONE',  ( 98.64540312569886282, -41.76920806142285159, 161.7556252759109725 ) ) ;
#6364 = CARTESIAN_POINT ( 'NONE',  ( 23.11218988842089672, 78.03196636687118826, 304.4337129636800796 ) ) ;
#6365 = CARTESIAN_POINT ( 'NONE',  ( 131.0667039024480118, -61.87844715994100397, 207.5838068554149913 ) ) ;
#6366 = DIRECTION ( 'NONE',  ( -0.7071067811571960515, 0.7071067812158990940, 0.000000000000000000 ) ) ;
#6367 = FACE_OUTER_BOUND ( 'NONE', #77444, .T. ) ;
#6368 = CARTESIAN_POINT ( 'NONE',  ( 96.22287284433019749, -34.36014117848482385, 252.1432443235303538 ) ) ;
#6369 = CARTESIAN_POINT ( 'NONE',  ( 92.26493792250094828, 84.21376545118702950, -74.44936585838367193 ) ) ;
#6370 = VERTEX_POINT ( 'NONE', #71462 ) ;
#6371 = VECTOR ( 'NONE', #84925, 1000.000000000000000 ) ;
#6372 = EDGE_LOOP ( 'NONE', ( #67957, #41774, #73157, #58921, #62892 ) ) ;
#6373 = CARTESIAN_POINT ( 'NONE',  ( 103.3469782872468130, -47.18711328981185460, 98.31657765686297523 ) ) ;
#6374 = CARTESIAN_POINT ( 'NONE',  ( 122.5505378705195909, 44.80423684447521993, -45.01691195935249112 ) ) ;
#6375 = VECTOR ( 'NONE', #19609, 1000.000000000000000 ) ;
#6376 = AXIS2_PLACEMENT_3D ( 'NONE', #40699, #82958, #27082 ) ;
#6377 = ORIENTED_EDGE ( 'NONE', *, *, #69578, .F. ) ;
#6378 = ORIENTED_EDGE ( 'NONE', *, *, #85745, .F. ) ;
#6379 = EDGE_LOOP ( 'NONE', ( #29242, #79517, #85233, #49817, #49646, #1703 ) ) ;
#6380 = CIRCLE ( 'NONE', #2051, 4.874999999999990230 ) ;
#6381 = CARTESIAN_POINT ( 'NONE',  ( 116.3214453605167478, -32.94026287388232532, 159.1356252759109680 ) ) ;
#6382 = DIRECTION ( 'NONE',  ( -1.000000000000000000, 0.000000000000000000, 0.000000000000000000 ) ) ;
#6383 = DIRECTION ( 'NONE',  ( 1.000000000000000078E-15, -1.000000000000000083E-30, -1.000000000000000000 ) ) ;
#6384 = DIRECTION ( 'NONE',  ( -4.237773401492740281E-14, 1.000000000000000000, 0.000000000000000000 ) ) ;
#6385 = CARTESIAN_POINT ( 'NONE',  ( 102.9190449779222405, -43.75998617602524376, 159.9709475124489586 ) ) ;
#6386 = CARTESIAN_POINT ( 'NONE',  ( 100.1243021666677606, -44.53607127582347402, 262.9984824187678782 ) ) ;
#6387 = CARTESIAN_POINT ( 'NONE',  ( 104.4069165777156059, -46.45774650464046829, 58.36469172372787284 ) ) ;
#6388 = ORIENTED_EDGE ( 'NONE', *, *, #79508, .T. ) ;
#6389 = CARTESIAN_POINT ( 'NONE',  ( 129.9761744276714523, 85.85000629251470627, 12.29186252049211880 ) ) ;
#6390 = CARTESIAN_POINT ( 'NONE',  ( 138.8167039024479834, -67.87844715994100397, 60.91780685541480267 ) ) ;
#6391 = ORIENTED_EDGE ( 'NONE', *, *, #54427, .F. ) ;
#6392 = ORIENTED_EDGE ( 'NONE', *, *, #65080, .F. ) ;
#6393 = LINE ( 'NONE', #81820, #60443 ) ;
#6394 = EDGE_CURVE ( 'NONE', #32539, #79573, #52493, .T. ) ;
#6395 = ORIENTED_EDGE ( 'NONE', *, *, #72472, .F. ) ;
#6396 = ORIENTED_EDGE ( 'NONE', *, *, #81332, .T. ) ;
#6397 = LINE ( 'NONE', #48160, #38253 ) ;
#6398 = CARTESIAN_POINT ( 'NONE',  ( 182.0667039024476139, -32.29483332967959086, 313.9678068554149490 ) ) ;
#6399 = EDGE_CURVE ( 'NONE', #20410, #16018, #14820, .T. ) ;
#6400 = LINE ( 'NONE', #34093, #11517 ) ;
#6401 = LINE ( 'NONE', #42252, #8454 ) ;
#6402 = CARTESIAN_POINT ( 'NONE',  ( 115.3626348109362425, -40.36077478062563983, 207.9086103042679667 ) ) ;
#6403 = CARTESIAN_POINT ( 'NONE',  ( 95.29943635023701631, -34.95028898632038050, 71.20705384733993526 ) ) ;
#6404 = CARTESIAN_POINT ( 'NONE',  ( 141.0664832912740394, -46.72944715994108122, -4.970821333495771377 ) ) ;
#6405 = ORIENTED_EDGE ( 'NONE', *, *, #13290, .T. ) ;
#6406 = ADVANCED_FACE ( 'NONE', ( #57353, #85094 ), #22863, .T. ) ;
#6407 = CARTESIAN_POINT ( 'NONE',  ( -72.96458098368600531, 117.4749999999999943, -72.96458098368781009 ) ) ;
#6408 = VERTEX_POINT ( 'NONE', #36923 ) ;
#6409 = ADVANCED_FACE ( 'NONE', ( #64626 ), #57807, .F. ) ;
#6410 = EDGE_CURVE ( 'NONE', #78558, #73485, #7548, .T. ) ;
#6411 = FACE_OUTER_BOUND ( 'NONE', #27480, .T. ) ;
#6412 = VERTEX_POINT ( 'NONE', #44163 ) ;
#6413 = CARTESIAN_POINT ( 'NONE',  ( 143.9834832912729894, -1.929447159941392931, 352.4506252759079530 ) ) ;
#6414 = CARTESIAN_POINT ( 'NONE',  ( 117.0467990990870675, -131.0263588434231110, 250.2203867545810283 ) ) ;
#6415 = CARTESIAN_POINT ( 'NONE',  ( 112.4849986523878442, -45.14882631497925303, 133.0314946533368925 ) ) ;
#6416 = ADVANCED_FACE ( 'NONE', ( #71902 ), #9660, .T. ) ;
#6417 = AXIS2_PLACEMENT_3D ( 'NONE', #81310, #67196, #73567 ) ;
#6418 = FACE_BOUND ( 'NONE', #41890, .T. ) ;
#6419 = ORIENTED_EDGE ( 'NONE', *, *, #7776, .F. ) ;
#6420 = CARTESIAN_POINT ( 'NONE',  ( 115.6914824993820901, -43.67961476919119690, 43.27467289495795200 ) ) ;
#6421 = VECTOR ( 'NONE', #10000, 1000.000000000000000 ) ;
#6422 = EDGE_CURVE ( 'NONE', #25932, #4530, #65075, .T. ) ;
#6424 = PLANE ( 'NONE',  #52955 ) ;
#6423 = CARTESIAN_POINT ( 'NONE',  ( 1.166476076187854022E-15, 114.2999999999999972, 9.525000000000000355 ) ) ;
#6425 = CARTESIAN_POINT ( 'NONE',  ( 158.0667039024469886, -67.87844715994090450, 120.2178068554179902 ) ) ;
#6426 = CARTESIAN_POINT ( 'NONE',  ( 131.6688901780889296, -17.37024878623243751, 2.654395752964755051 ) ) ;
#6427 = ORIENTED_EDGE ( 'NONE', *, *, #18510, .F. ) ;
#6428 = CARTESIAN_POINT ( 'NONE',  ( 0.000000000000000000, 20.32000000000000028, 0.000000000000000000 ) ) ;
#6429 = EDGE_CURVE ( 'NONE', #58142, #24085, #13382, .T. ) ;
#6430 = PLANE ( 'NONE',  #48709 ) ;
#6431 = CARTESIAN_POINT ( 'NONE',  ( 6.802569982901797644E-16, 69.84999999999999432, 118.5560000000000116 ) ) ;
#6432 = ORIENTED_EDGE ( 'NONE', *, *, #60162, .F. ) ;
#6433 = CARTESIAN_POINT ( 'NONE',  ( 108.9892323659770170, -46.99785963944585632, 78.72419670448194040 ) ) ;
#6435 = DIRECTION ( 'NONE',  ( 1.000000000000000000, 0.000000000000000000, 3.491483361109385222E-15 ) ) ;
#6434 = LINE ( 'NONE', #47751, #46462 ) ;
#6436 = CARTESIAN_POINT ( 'NONE',  ( 193.0371591254583734, -47.82818131005411999, 313.9678068554149490 ) ) ;
#6437 = VECTOR ( 'NONE', #780, 1000.000000000000000 ) ;
#6438 = VECTOR ( 'NONE', #47304, 1000.000000000000000 ) ;
#6439 = PRESENTATION_LAYER_ASSIGNMENT (  '', '', ( #23901 ) ) ;
#6440 = AXIS2_PLACEMENT_3D ( 'NONE', #77470, #710, #7979 ) ;
#6441 = CARTESIAN_POINT ( 'NONE',  ( 135.1911801492854011, -84.41530667025313051, 249.3055338466990065 ) ) ;
#6442 = EDGE_LOOP ( 'NONE', ( #81703, #80864, #13278, #43018, #80926, #20940 ) ) ;
#6443 = CARTESIAN_POINT ( 'NONE',  ( 98.20106483660288177, -31.34956418181673854, 121.8803871806729546 ) ) ;
#6445 = ORIENTED_EDGE ( 'NONE', *, *, #85042, .F. ) ;
#6444 = CARTESIAN_POINT ( 'NONE',  ( 97.80792351950141494, -40.51905676813210988, 116.6359120812046939 ) ) ;
#6446 = AXIS2_PLACEMENT_3D ( 'NONE', #51966, #17478, #52400 ) ;
#6447 = CARTESIAN_POINT ( 'NONE',  ( 116.1995025514323316, -41.78438384397597360, 259.4241967044825969 ) ) ;
#6448 = CARTESIAN_POINT ( 'NONE',  ( 97.86619352455458909, -40.64832413407319933, 252.6469055415188620 ) ) ;
#6449 = CYLINDRICAL_SURFACE ( 'NONE', #33035, 38.10000000000000142 ) ;
#6450 = FACE_BOUND ( 'NONE', #21334, .T. ) ;
#6451 = CARTESIAN_POINT ( 'NONE',  ( 87.31648329127401098, -46.47944715994105280, 14.92562527591095112 ) ) ;
#6452 = ADVANCED_FACE ( 'NONE', ( #26864 ), #18258, .F. ) ;
#6453 = LINE ( 'NONE', #61843, #54934 ) ;
#6454 = CARTESIAN_POINT ( 'NONE',  ( -99.63271100832207594, 75.84295037288958952, 84.36969927706194028 ) ) ;
#6455 = EDGE_CURVE ( 'NONE', #3936, #783, #48170, .T. ) ;
#6456 = CARTESIAN_POINT ( 'NONE',  ( 118.1473594538626486, -37.63838399483783093, 188.7613395616259595 ) ) ;
#6457 = EDGE_LOOP ( 'NONE', ( #63258, #10362, #21308, #58387, #67657, #6886 ) ) ;
#6458 = ORIENTED_EDGE ( 'NONE', *, *, #37422, .F. ) ;
#6459 = CARTESIAN_POINT ( 'NONE',  ( 113.0289363901617889, -43.32575541760495241, 129.5930118773259778 ) ) ;
#6460 = LINE ( 'NONE', #46868, #60231 ) ;
#6462 = LINE ( 'NONE', #13283, #5679 ) ;
#6461 = CARTESIAN_POINT ( 'NONE',  ( 115.3146942856800337, -32.23016485065021897, 20.64348806780197521 ) ) ;
#6463 = DIRECTION ( 'NONE',  ( 0.000000000000000000, 0.000000000000000000, -1.000000000000000000 ) ) ;
#6464 = DIRECTION ( 'NONE',  ( -0.000000000000000000, -0.000000000000000000, 1.000000000000000000 ) ) ;
#6465 = CARTESIAN_POINT ( 'NONE',  ( 135.2444258376730204, 0.000000000000000000, -147.4575741623271767 ) ) ;
#6466 = DIRECTION ( 'NONE',  ( -3.100000000000000258E-29, 3.100000000000000044E-14, 1.000000000000000000 ) ) ;
#6467 = DIRECTION ( 'NONE',  ( 0.000000000000000000, 0.000000000000000000, -1.000000000000000000 ) ) ;
#6468 = CARTESIAN_POINT ( 'NONE',  ( 96.16101635903902434, -35.07578045570937775, 221.1946728949589840 ) ) ;
#6469 = LINE ( 'NONE', #61422, #27205 ) ;
#6470 = ORIENTED_EDGE ( 'NONE', *, *, #70535, .T. ) ;
#6471 = ORIENTED_EDGE ( 'NONE', *, *, #60434, .F. ) ;
#6472 = CARTESIAN_POINT ( 'NONE',  ( -86.93292302958607820, 72.22361908171431821, -97.40459591070893453 ) ) ;
#6473 = CARTESIAN_POINT ( 'NONE',  ( 82.31791107858144585, -20.31136518418547965, 7.339178645752261865 ) ) ;
#6474 = CARTESIAN_POINT ( 'NONE',  ( 116.3216177720312317, -32.94249360885015676, 184.1356252759109680 ) ) ;
#6475 = CARTESIAN_POINT ( 'NONE',  ( 172.5664832912740110, -18.82844715994099971, 81.04262527591200183 ) ) ;
#6476 = AXIS2_PLACEMENT_3D ( 'NONE', #8190, #42680, #69522 ) ;
#6477 = CARTESIAN_POINT ( 'NONE',  ( 194.5667039024480403, -40.82844715993405771, 249.9678068554149775 ) ) ;
#6478 = ORIENTED_EDGE ( 'NONE', *, *, #12450, .T. ) ;
#6479 = DIRECTION ( 'NONE',  ( 0.000000000000000000, 1.000000000000000000, 0.000000000000000000 ) ) ;
#6480 = CIRCLE ( 'NONE', #74626, 12.44599999999999795 ) ;
#6481 = CARTESIAN_POINT ( 'NONE',  ( 113.2201423986613520, -45.14488000985961946, 228.0784824187679760 ) ) ;
#6482 = VERTEX_POINT ( 'NONE', #5545 ) ;
#6483 = CARTESIAN_POINT ( 'NONE',  ( -1.652225533659690049, 95.06819236710590815, 118.5472263177064889 ) ) ;
#6484 = DIRECTION ( 'NONE',  ( 1.000000000000000000, 3.999999999999999995E-14, 1.000000000000000078E-15 ) ) ;
#6485 = CARTESIAN_POINT ( 'NONE',  ( -105.4788588808464027, 120.6499999999999915, 3.968749999998844924 ) ) ;
#6486 = CARTESIAN_POINT ( 'NONE',  ( 112.1086029179114547, -30.31019831854434443, 77.36523322673394887 ) ) ;
#6487 = CARTESIAN_POINT ( 'NONE',  ( 101.9613826146451885, -46.55915482862852173, 163.1832443235299763 ) ) ;
#6488 = CARTESIAN_POINT ( 'NONE',  ( 105.8444747722200674, -25.33565403619829226, 322.4846826458744431 ) ) ;
#6489 = ORIENTED_EDGE ( 'NONE', *, *, #13107, .F. ) ;
#6490 = DIRECTION ( 'NONE',  ( -0.8660254037844387076, 0.4999999999999998890, 0.000000000000000000 ) ) ;
#6491 = EDGE_CURVE ( 'NONE', #47477, #14995, #80961, .T. ) ;
#6492 = CARTESIAN_POINT ( 'NONE',  ( 99.42197401388541778, -43.20727476509772202, 66.88677594099895884 ) ) ;
#6493 = VERTEX_POINT ( 'NONE', #45937 ) ;
#6494 = ORIENTED_EDGE ( 'NONE', *, *, #9824, .T. ) ;
#6495 = AXIS2_PLACEMENT_3D ( 'NONE', #68455, #47983, #67550 ) ;
#6496 = CIRCLE ( 'NONE', #2169, 13.49999999999999822 ) ;
#6497 = CARTESIAN_POINT ( 'NONE',  ( 11.02155491792549924, 88.91427639974089914, 118.0434862571550099 ) ) ;
#6498 = AXIS2_PLACEMENT_3D ( 'NONE', #7238, #40403, #54900 ) ;
#6499 = ORIENTED_EDGE ( 'NONE', *, *, #69170, .F. ) ;
#6500 = EDGE_LOOP ( 'NONE', ( #74205, #67199, #86606, #69951, #18273, #76747 ) ) ;
#6501 = LINE ( 'NONE', #34200, #17892 ) ;
#6502 = CIRCLE ( 'NONE', #10905, 4.749999999999976907 ) ;
#6503 = EDGE_CURVE ( 'NONE', #23851, #2670, #11453, .T. ) ;
#6504 = EDGE_CURVE ( 'NONE', #40777, #74550, #22090, .T. ) ;
#6505 = CARTESIAN_POINT ( 'NONE',  ( 102.6785256587874926, -29.36752282311925200, 84.92670554236298130 ) ) ;
#6506 = CARTESIAN_POINT ( 'NONE',  ( 96.66004714996478242, -35.80616453621266970, 231.2556252759109725 ) ) ;
#6507 = ADVANCED_FACE ( 'NONE', ( #75476 ), #88220, .T. ) ;
#6508 = CARTESIAN_POINT ( 'NONE',  ( 113.7366723824214887, -44.71300795807898965, 193.1299109901969757 ) ) ;
#6510 = CARTESIAN_POINT ( 'NONE',  ( 111.3142535964730371, -27.23286288913599051, 20.74133956162494030 ) ) ;
#6509 = DIRECTION ( 'NONE',  ( -1.000000000000000000, 0.000000000000000000, 0.000000000000000000 ) ) ;
#6511 = CARTESIAN_POINT ( 'NONE',  ( -458.3598257906459708, 47.62500000000000000, 3.174999999999999822 ) ) ;
#6512 = DIRECTION ( 'NONE',  ( 0.000000000000000000, 0.000000000000000000, -1.000000000000000000 ) ) ;
#6513 = EDGE_CURVE ( 'NONE', #89449, #64543, #37532, .T. ) ;
#6514 = EDGE_LOOP ( 'NONE', ( #45341, #3807, #52181, #75038 ) ) ;
#6515 = ORIENTED_EDGE ( 'NONE', *, *, #54234, .T. ) ;
#6516 = EDGE_CURVE ( 'NONE', #55655, #87716, #5082, .T. ) ;
#6517 = CARTESIAN_POINT ( 'NONE',  ( 118.1148702536304427, -35.48641528967804248, 83.91562527591095488 ) ) ;
#6518 = CARTESIAN_POINT ( 'NONE',  ( 102.9537058647788967, -46.35710148923402585, 92.25562527591097250 ) ) ;
#6519 = CARTESIAN_POINT ( 'NONE',  ( 110.8326918741827711, -26.28777313046090569, 249.7889586092445882 ) ) ;
#6520 = ORIENTED_EDGE ( 'NONE', *, *, #66494, .F. ) ;
#6521 = CARTESIAN_POINT ( 'NONE',  ( 107.5100371804366688, -47.14531440222233272, 237.6099109901969655 ) ) ;
#6522 = CARTESIAN_POINT ( 'NONE',  ( 99.09570902266669634, -30.55043182097106680, 35.80229194939514059 ) ) ;
#6523 =( NAMED_UNIT ( * ) PLANE_ANGLE_UNIT ( ) SI_UNIT ( $, .RADIAN. ) );
#6524 = DIRECTION ( 'NONE',  ( 1.000000000000000078E-15, -1.000000000000000083E-30, -1.000000000000000000 ) ) ;
#6525 = CARTESIAN_POINT ( 'NONE',  ( 117.0407245441959816, -35.29532848343978202, 29.94117331857431807 ) ) ;
#6526 = CIRCLE ( 'NONE', #45655, 3.174999999999997158 ) ;
#6528 = DIRECTION ( 'NONE',  ( 0.000000000000000000, 0.000000000000000000, 1.000000000000000000 ) ) ;
#6527 = CARTESIAN_POINT ( 'NONE',  ( 112.6803783697433516, -30.99839248778516776, 277.6356252759110248 ) ) ;
#6529 = CARTESIAN_POINT ( 'NONE',  ( 117.0719014705369716, -35.46251353140062434, 174.9272894658773509 ) ) ;
#6531 = EDGE_CURVE ( 'NONE', #26221, #51337, #54095, .T. ) ;
#6530 = LINE ( 'NONE', #61036, #10569 ) ;
#6532 = CARTESIAN_POINT ( 'NONE',  ( 8.387180980836969724, 92.12328101316224149, -118.2604483546762282 ) ) ;
#6533 = CARTESIAN_POINT ( 'NONE',  ( 151.5667039024483245, -48.82844715993591223, 300.4678068554149490 ) ) ;
#6534 = CARTESIAN_POINT ( 'NONE',  ( 116.3121618740066623, -32.93870344941997530, 39.13562527591096796 ) ) ;
#6535 = CARTESIAN_POINT ( 'NONE',  ( 51.03742451361635091, -23.42844715994068849, 117.4678068554150485 ) ) ;
#6536 = EDGE_CURVE ( 'NONE', #3590, #7607, #59773, .T. ) ;
#6538 = ORIENTED_EDGE ( 'NONE', *, *, #28055, .F. ) ;
#6537 = CARTESIAN_POINT ( 'NONE',  ( -72.96458098368751166, 127.0000000000000000, 72.96458098368620426 ) ) ;
#6539 = DIRECTION ( 'NONE',  ( 1.000000000000000000, -4.163336342344333240E-14, 0.000000000000000000 ) ) ;
#6540 = CARTESIAN_POINT ( 'NONE',  ( 117.2187229798756363, -34.26400738748503727, 209.0156252759109634 ) ) ;
#6541 = CARTESIAN_POINT ( 'NONE',  ( 95.77906782739819391, -40.33899944578667629, 127.5727681330539554 ) ) ;
#6542 = CARTESIAN_POINT ( 'NONE',  ( 105.0131270392176646, -25.82159629633810738, 276.2365776568634033 ) ) ;
#6543 = CARTESIAN_POINT ( 'NONE',  ( 97.81171236172070849, -40.51746256574213589, 261.6350867226296941 ) ) ;
#6545 = CARTESIAN_POINT ( 'NONE',  ( 83.06670390244796920, -58.72944715994093912, 207.5838068554149913 ) ) ;
#6544 = CARTESIAN_POINT ( 'NONE',  ( 116.3212776292296127, -32.94146857471318413, 287.6356252759109680 ) ) ;
#6546 = LINE ( 'NONE', #81085, #16069 ) ;
#6547 = VECTOR ( 'NONE', #22499, 1000.000000000000000 ) ;
#6548 = CARTESIAN_POINT ( 'NONE',  ( 72.25757238336808541, -1.944390235229867425, 361.9756252759101471 ) ) ;
#6549 = AXIS2_PLACEMENT_3D ( 'NONE', #16158, #31547, #65187 ) ;
#6550 = EDGE_LOOP ( 'NONE', ( #12801, #8970, #77761, #49075 ) ) ;
#6551 = DIRECTION ( 'NONE',  ( 1.000000000000000000, 0.000000000000000000, 0.000000000000000000 ) ) ;
#6552 = ORIENTED_EDGE ( 'NONE', *, *, #75938, .F. ) ;
#6553 = CARTESIAN_POINT ( 'NONE',  ( 112.9437820074331569, -43.62348782359368471, 152.5733722090289746 ) ) ;
#6555 = VERTEX_POINT ( 'NONE', #61379 ) ;
#6554 = CARTESIAN_POINT ( 'NONE',  ( 22.25283182517284075, 48.39572325881615456, 30.92657878646921432 ) ) ;
#6556 = DIRECTION ( 'NONE',  ( -0.7071067811865495711, 0.000000000000000000, 0.7071067811865455743 ) ) ;
#6557 = CARTESIAN_POINT ( 'NONE',  ( 99.11802762103509679, -45.48540990049882282, 152.9899109901969894 ) ) ;
#6558 = CARTESIAN_POINT ( 'NONE',  ( 104.4066719782816790, -46.45767031374273870, 148.3653026159171588 ) ) ;
#6559 = CARTESIAN_POINT ( 'NONE',  ( -47.05489187827554076, 92.24160055789619150, 74.44168661866966374 ) ) ;
#6560 = CARTESIAN_POINT ( 'NONE',  ( -91.50401754987770175, 76.93600387762164416, 75.38287938185037262 ) ) ;
#6561 = LINE ( 'NONE', #76048, #86108 ) ;
#6562 = EDGE_CURVE ( 'NONE', #27190, #49111, #31884, .T. ) ;
#6563 = CARTESIAN_POINT ( 'NONE',  ( 116.7176835877704946, -38.50936494796418685, 88.68133956162593279 ) ) ;
#6564 = VERTEX_POINT ( 'NONE', #39590 ) ;
#6565 = ORIENTED_EDGE ( 'NONE', *, *, #41456, .F. ) ;
#6566 = VERTEX_POINT ( 'NONE', #25521 ) ;
#6567 = CIRCLE ( 'NONE', #76198, 2.517499999999998739 ) ;
#6568 = AXIS2_PLACEMENT_3D ( 'NONE', #5568, #33260, #74592 ) ;
#6569 = CARTESIAN_POINT ( 'NONE',  ( 31.75000000000000000, 24.56180297284579694, -3.174999999999999822 ) ) ;
#6571 = CARTESIAN_POINT ( 'NONE',  ( 28.57499999999999929, 77.96728223830730542, 294.9574999999999818 ) ) ;
#6570 = CARTESIAN_POINT ( 'NONE',  ( 97.31342953368671544, -35.99458159538090030, 142.2670538473389570 ) ) ;
#6572 = VECTOR ( 'NONE', #68618, 1000.000000000000000 ) ;
#6573 = DIRECTION ( 'NONE',  ( 0.000000000000000000, 1.000000000000000000, 0.000000000000000000 ) ) ;
#6574 = CARTESIAN_POINT ( 'NONE',  ( 183.5150000000000148, 14.63749999999999929, -14.28749999999999964 ) ) ;
#6576 = FACE_OUTER_BOUND ( 'NONE', #74868, .T. ) ;
#6575 = AXIS2_PLACEMENT_3D ( 'NONE', #39383, #17608, #59808 ) ;
#6577 = CARTESIAN_POINT ( 'NONE',  ( 194.5664832912739826, 0.2215528400590013880, -5.074374724088000832 ) ) ;
#6578 = DIRECTION ( 'NONE',  ( -4.237773401492740281E-14, 1.000000000000000000, 0.000000000000000000 ) ) ;
#6579 = CARTESIAN_POINT ( 'NONE',  ( 98.16825066461156268, -43.24752039522714142, 106.8175300378159704 ) ) ;
#6580 = ORIENTED_EDGE ( 'NONE', *, *, #1414, .T. ) ;
#6581 = EDGE_LOOP ( 'NONE', ( #41739, #16307, #89460, #44337 ) ) ;
#6582 = ORIENTED_EDGE ( 'NONE', *, *, #67116, .F. ) ;
#6583 = VECTOR ( 'NONE', #50177, 1000.000000000000114 ) ;
#6584 = EDGE_CURVE ( 'NONE', #7678, #6003, #53191, .T. ) ;
#6585 = FACE_OUTER_BOUND ( 'NONE', #46124, .T. ) ;
#6586 = DIRECTION ( 'NONE',  ( 0.000000000000000000, 0.000000000000000000, 1.000000000000000000 ) ) ;
#6587 = DIRECTION ( 'NONE',  ( 4.299999999999999979E-14, -1.000000000000000000, 4.400000000000000367E-29 ) ) ;
#6589 = CARTESIAN_POINT ( 'NONE',  ( 100.2649065926023297, -31.37786052998579223, 198.6261856076869776 ) ) ;
#6588 = CIRCLE ( 'NONE', #58759, 3.499999999999996003 ) ;
#6590 = EDGE_CURVE ( 'NONE', #87925, #55605, #83194, .T. ) ;
#6591 = CIRCLE ( 'NONE', #5099, 2.116999999999980009 ) ;
#6592 = CARTESIAN_POINT ( 'NONE',  ( 104.0667030381801936, -70.87844715994094713, 173.2178086137559774 ) ) ;
#6593 = EDGE_LOOP ( 'NONE', ( #52539, #85685, #2712 ) ) ;
#6595 = ORIENTED_EDGE ( 'NONE', *, *, #78349, .F. ) ;
#6594 = EDGE_LOOP ( 'NONE', ( #20081, #79463, #81931, #87329, #17183 ) ) ;
#6596 = DIRECTION ( 'NONE',  ( 1.000000000000000078E-15, -1.000000000000000083E-30, -1.000000000000000000 ) ) ;
#6597 = DIRECTION ( 'NONE',  ( 0.000000000000000000, 1.000000000000000000, 0.000000000000000000 ) ) ;
#6598 = ORIENTED_EDGE ( 'NONE', *, *, #1368, .T. ) ;
#6599 = EDGE_LOOP ( 'NONE', ( #29196, #73199 ) ) ;
#6600 = CARTESIAN_POINT ( 'NONE',  ( -48.02966122971776741, 91.07499999999996021, 74.26049396966043048 ) ) ;
#6601 = CARTESIAN_POINT ( 'NONE',  ( 115.4123442176498173, -41.04489973583525142, 239.8663452106589773 ) ) ;
#6602 = ORIENTED_EDGE ( 'NONE', *, *, #38525, .F. ) ;
#6603 = PLANE ( 'NONE',  #69679 ) ;
#6604 = VECTOR ( 'NONE', #10866, 1000.000000000000000 ) ;
#6605 = CARTESIAN_POINT ( 'NONE',  ( -121.9014056762777329, 74.22174993621874250, 46.74836492626587159 ) ) ;
#6606 = ORIENTED_EDGE ( 'NONE', *, *, #42189, .F. ) ;
#6607 = VERTEX_POINT ( 'NONE', #505 ) ;
#6608 = PLANE ( 'NONE',  #72525 ) ;
#6609 = AXIS2_PLACEMENT_3D ( 'NONE', #50543, #35571, #56456 ) ;
#6610 = ORIENTED_EDGE ( 'NONE', *, *, #82344, .T. ) ;
#6611 = ORIENTED_EDGE ( 'NONE', *, *, #47315, .T. ) ;
#6612 = ADVANCED_FACE ( 'NONE', ( #41375 ), #71423, .F. ) ;
#6613 = EDGE_CURVE ( 'NONE', #83706, #79712, #41817, .T. ) ;
#6614 = CARTESIAN_POINT ( 'NONE',  ( 109.5637425988213636, -28.92903792723274847, 232.6480903695909603 ) ) ;
#6615 = CARTESIAN_POINT ( 'NONE',  ( 95.75500511041516916, -40.34669435480882527, 131.5727681330539554 ) ) ;
#6616 = EDGE_CURVE ( 'NONE', #54796, #20434, #35014, .T. ) ;
#6617 = CARTESIAN_POINT ( 'NONE',  ( 116.5135284680788175, -32.37261310794432490, 104.1699109901969535 ) ) ;
#6618 = CARTESIAN_POINT ( 'NONE',  ( 101.9411125306454124, -42.93772781322726217, 249.5838068554172366 ) ) ;
#6619 = CARTESIAN_POINT ( 'NONE',  ( 133.3217830637516101, -16.08035908359601152, 8.141856907853265213 ) ) ;
#6620 = CARTESIAN_POINT ( 'NONE',  ( 107.6544996609965352, -47.76702919738148267, 193.6308633711489620 ) ) ;
#6621 = CARTESIAN_POINT ( 'NONE',  ( 46.48091746482130304, -49.32844715994084339, 300.4678068554150059 ) ) ;
#6622 = ORIENTED_EDGE ( 'NONE', *, *, #13910, .T. ) ;
#6623 = CARTESIAN_POINT ( 'NONE',  ( 130.3463096697861943, 72.22361908171431821, 7.404590904609912982 ) ) ;
#6624 = ORIENTED_EDGE ( 'NONE', *, *, #76370, .F. ) ;
#6625 = EDGE_CURVE ( 'NONE', #3921, #12790, #63631, .T. ) ;
#6626 = ORIENTED_EDGE ( 'NONE', *, *, #45969, .T. ) ;
#6627 = CYLINDRICAL_SURFACE ( 'NONE', #11176, 9.999999999999998224 ) ;
#6628 = VERTEX_POINT ( 'NONE', #20952 ) ;
#6629 = CARTESIAN_POINT ( 'NONE',  ( 69.56670390244704549, -118.2784471599409812, 45.21780685541799727 ) ) ;
#6630 = AXIS2_PLACEMENT_3D ( 'NONE', #82779, #20540, #67779 ) ;
#6631 = CARTESIAN_POINT ( 'NONE',  ( 95.67500926166044906, -33.46221576448694890, 141.1041967044829732 ) ) ;
#6632 = CARTESIAN_POINT ( 'NONE',  ( -12.69999999999999751, 81.76470274209911793, 129.9368274816649773 ) ) ;
#6633 = VECTOR ( 'NONE', #15534, 1000.000000000000000 ) ;
#6634 = DIRECTION ( 'NONE',  ( 0.4999999999999998890, 0.000000000000000000, -0.8660254037844387076 ) ) ;
#6635 = LINE ( 'NONE', #61582, #51356 ) ;
#6638 = CARTESIAN_POINT ( 'NONE',  ( 95.31970492887387536, -38.09378048407035777, 232.4184824187679794 ) ) ;
#6637 = DIRECTION ( 'NONE',  ( 8.659560562355552854E-17, -0.7071067811864968355, 0.7071067811865981989 ) ) ;
#6636 = CARTESIAN_POINT ( 'NONE',  ( 51.24204729617191845, -31.76306994223763880, 193.9678068554150911 ) ) ;
#6639 = CARTESIAN_POINT ( 'NONE',  ( 107.0664832912739541, -20.87944715994095546, 302.7856252759109452 ) ) ;
#6641 = EDGE_CURVE ( 'NONE', #88962, #75252, #59, .T. ) ;
#6640 = CARTESIAN_POINT ( 'NONE',  ( 107.0664832912739399, -36.72944715994096754, 296.0306255462182321 ) ) ;
#6642 = ORIENTED_EDGE ( 'NONE', *, *, #79967, .T. ) ;
#6643 = DIRECTION ( 'NONE',  ( 1.000000000000000000, 0.000000000000000000, 0.000000000000000000 ) ) ;
#6644 = CARTESIAN_POINT ( 'NONE',  ( 13.86911000615387302, 238.5000000000000000, 102.9892450244911686 ) ) ;
#6645 = DIRECTION ( 'NONE',  ( 0.000000000000000000, 0.000000000000000000, 1.000000000000000000 ) ) ;
#6646 = VECTOR ( 'NONE', #89694, 1000.000000000000000 ) ;
#6647 = CARTESIAN_POINT ( 'NONE',  ( 194.0371591254582881, -46.82818131005407736, 237.4678068554150059 ) ) ;
#6649 = ORIENTED_EDGE ( 'NONE', *, *, #66403, .T. ) ;
#6648 = CARTESIAN_POINT ( 'NONE',  ( 112.6874404347162084, -45.56185944854193792, 263.0270538473394026 ) ) ;
#6650 = CARTESIAN_POINT ( 'NONE',  ( 105.9948944823395891, -26.75816435948428307, 195.1613249903887493 ) ) ;
#6651 = CARTESIAN_POINT ( 'NONE',  ( 96.58491273044850800, -36.88769195468244533, 136.3384824187679385 ) ) ;
#6652 = CARTESIAN_POINT ( 'NONE',  ( 115.4446095375818970, -42.99269977972175383, 24.31562527591096767 ) ) ;
#6653 = CARTESIAN_POINT ( 'NONE',  ( 113.5922599384962552, -44.96062289245586641, 164.1099109901969655 ) ) ;
#6654 = DIRECTION ( 'NONE',  ( 0.7071067811865504593, 0.000000000000000000, 0.7071067811865445751 ) ) ;
#6655 = CARTESIAN_POINT ( 'NONE',  ( 36.65249034007446483, -48.32844715994130524, 129.9678068554150911 ) ) ;
#6656 = AXIS2_PLACEMENT_3D ( 'NONE', #73585, #5900, #45412 ) ;
#6658 = CARTESIAN_POINT ( 'NONE',  ( 25.56670390244797275, -62.87844715994099687, 252.3428068554150059 ) ) ;
#6657 = DIRECTION ( 'NONE',  ( 3.491483361109380094E-15, 0.000000000000000000, 1.000000000000000000 ) ) ;
#6659 = DIRECTION ( 'NONE',  ( 0.7071067811866279529, -0.7071067811864671926, 7.071067811866286874E-16 ) ) ;
#6660 = CARTESIAN_POINT ( 'NONE',  ( 107.0667039024469886, -70.87844715994094713, 93.21780685541800437 ) ) ;
#6661 = EDGE_LOOP ( 'NONE', ( #50660, #37749, #10474, #55160 ) ) ;
#6662 = VECTOR ( 'NONE', #57712, 1000.000000000000000 ) ;
#6663 = EDGE_LOOP ( 'NONE', ( #44477, #73581 ) ) ;
#6664 = ORIENTED_EDGE ( 'NONE', *, *, #58592, .F. ) ;
#6665 = ORIENTED_EDGE ( 'NONE', *, *, #9732, .F. ) ;
#6666 = CARTESIAN_POINT ( 'NONE',  ( 49.35031423293201414, -29.99615139349890569, -5.074374724088000832 ) ) ;
#6667 = CARTESIAN_POINT ( 'NONE',  ( 106.8416606513710008, -48.55305329746386178, 73.56133956162497611 ) ) ;
#6668 = CARTESIAN_POINT ( 'NONE',  ( 156.5667039024480971, -42.82844715993568485, 293.2178068554149490 ) ) ;
#6669 = DIRECTION ( 'NONE',  ( 0.000000000000000000, -1.000000000000000000, 0.000000000000000000 ) ) ;
#6670 = CARTESIAN_POINT ( 'NONE',  ( 107.5678551521628492, -47.81755451042874228, 188.6003871806729535 ) ) ;
#6671 = DIRECTION ( 'NONE',  ( 0.000000000000000000, 0.000000000000000000, -1.000000000000000000 ) ) ;
#6672 = EDGE_CURVE ( 'NONE', #70541, #52915, #56349, .T. ) ;
#6673 = CARTESIAN_POINT ( 'NONE',  ( 112.1081655520365388, -43.62419673505787898, 227.5009912566479784 ) ) ;
#6674 = EDGE_LOOP ( 'NONE', ( #84794, #57553, #83720, #34810 ) ) ;
#6675 = VERTEX_POINT ( 'NONE', #55889 ) ;
#6676 = VERTEX_POINT ( 'NONE', #6425 ) ;
#6677 = CARTESIAN_POINT ( 'NONE',  ( 24.79284581386643183, 127.0000000000000000, 101.0189074266571794 ) ) ;
#6678 = CARTESIAN_POINT ( 'NONE',  ( 116.3435622888236196, -40.58882322890893590, 183.5124998200998334 ) ) ;
#6679 = EDGE_CURVE ( 'NONE', #53803, #54103, #34118, .T. ) ;
#6680 = CARTESIAN_POINT ( 'NONE',  ( 98.34985890712087553, -31.65658481866827501, 75.90645861007901374 ) ) ;
#6681 = CARTESIAN_POINT ( 'NONE',  ( 97.31592806723180900, -39.30618353892431571, 276.5310398549307251 ) ) ;
#6682 = CARTESIAN_POINT ( 'NONE',  ( 177.8371591254545478, -47.82818131005477369, 129.9678068554150059 ) ) ;
#6683 = LINE ( 'NONE', #89825, #34261 ) ;
#6684 = CARTESIAN_POINT ( 'NONE',  ( 97.07201651732883363, -35.37898364459096001, 176.2190017941805422 ) ) ;
#6685 = CARTESIAN_POINT ( 'NONE',  ( 115.1244435679684699, -31.12738977229718884, 279.3099109901971815 ) ) ;
#6686 = CARTESIAN_POINT ( 'NONE',  ( -68.53801554307339927, 120.6499999999999915, -74.15067561874339219 ) ) ;
#6687 = ORIENTED_EDGE ( 'NONE', *, *, #41444, .F. ) ;
#6688 = LINE ( 'NONE', #62098, #79473 ) ;
#6689 = CYLINDRICAL_SURFACE ( 'NONE', #20563, 3.174999999999983391 ) ;
#6690 = CARTESIAN_POINT ( 'NONE',  ( 99.39318122740648676, -32.72677799018995870, 88.74999513149600716 ) ) ;
#6691 = AXIS2_PLACEMENT_3D ( 'NONE', #23368, #3350, #52343 ) ;
#6692 = EDGE_CURVE ( 'NONE', #86269, #87632, #55442, .T. ) ;
#6693 = VECTOR ( 'NONE', #23245, 1000.000000000000000 ) ;
#6694 = AXIS2_PLACEMENT_3D ( 'NONE', #30490, #23689, #51353 ) ;
#6695 = AXIS2_PLACEMENT_3D ( 'NONE', #26465, #54583, #39192 ) ;
#6696 = DIRECTION ( 'NONE',  ( -0.9254794337955620787, -0.3787978585227822492, 0.000000000000000000 ) ) ;
#6697 = DIRECTION ( 'NONE',  ( -1.000000000000000078E-15, 1.000000000000000000, 0.000000000000000000 ) ) ;
#6698 = EDGE_LOOP ( 'NONE', ( #20480, #67587, #30407, #21376, #27468 ) ) ;
#6699 = DIRECTION ( 'NONE',  ( 0.000000000000000000, 0.000000000000000000, -1.000000000000000000 ) ) ;
#6700 = ORIENTED_EDGE ( 'NONE', *, *, #46702, .T. ) ;
#6701 = CARTESIAN_POINT ( 'NONE',  ( 108.7432494476977922, -25.80391683235395917, 144.9432443235299672 ) ) ;
#6702 = ORIENTED_EDGE ( 'NONE', *, *, #27816, .T. ) ;
#6703 = CARTESIAN_POINT ( 'NONE',  ( 5.041900000000000048, 117.4749999999999943, -103.1875000000000000 ) ) ;
#6704 = CARTESIAN_POINT ( 'NONE',  ( 99.03419491772403660, -31.85514013008181777, 122.3120594963729673 ) ) ;
#6705 = CARTESIAN_POINT ( 'NONE',  ( -47.08814856060967458, 100.9334351204065001, 108.4402773162242823 ) ) ;
#6706 = CARTESIAN_POINT ( 'NONE',  ( 67.05444493988859733, -69.17499946017586865, 247.4285673639549827 ) ) ;
#6707 = AXIS2_PLACEMENT_3D ( 'NONE', #88018, #40743, #48434 ) ;
#6708 = CARTESIAN_POINT ( 'NONE',  ( 118.0115981831179113, -38.42934884787886318, 64.69181575210097890 ) ) ;
#6709 = CARTESIAN_POINT ( 'NONE',  ( 116.3212776292296127, -32.94146857471318413, 287.6356252759109680 ) ) ;
#6710 = ORIENTED_EDGE ( 'NONE', *, *, #81812, .F. ) ;
#6711 = CARTESIAN_POINT ( 'NONE',  ( -117.9083433361413285, 79.66725693986899159, -12.37555662352200336 ) ) ;
#6712 =( BOUNDED_CURVE ( )  B_SPLINE_CURVE ( 3, ( #29501, #58964, #85827, #57184 ),
 .UNSPECIFIED., .F., .T. ) 
 B_SPLINE_CURVE_WITH_KNOTS ( ( 4, 4 ),
 ( 5.813027347256379151, 6.753343267102791536 ),
 .UNSPECIFIED. ) 
 CURVE ( )  GEOMETRIC_REPRESENTATION_ITEM ( )  RATIONAL_B_SPLINE_CURVE ( ( 1.000000000000000000, 0.9276644927932374829, 0.9276644927932374829, 1.000000000000000000 ) ) 
 REPRESENTATION_ITEM ( '' )  );
#6713 = VERTEX_POINT ( 'NONE', #84091 ) ;
#6714 = AXIS2_PLACEMENT_3D ( 'NONE', #45189, #10678, #34253 ) ;
#6715 = ORIENTED_EDGE ( 'NONE', *, *, #74936, .F. ) ;
#6716 = EDGE_CURVE ( 'NONE', #50271, #41960, #65521, .T. ) ;
#6717 = LINE ( 'NONE', #20361, #64420 ) ;
#6718 = VERTEX_POINT ( 'NONE', #14597 ) ;
#6719 = EDGE_CURVE ( 'NONE', #88931, #55655, #49080, .T. ) ;
#6720 = CARTESIAN_POINT ( 'NONE',  ( 115.1619974903381518, -42.21817061296157192, 273.3527681330542691 ) ) ;
#6721 = CARTESIAN_POINT ( 'NONE',  ( 103.4608836344597194, -46.53438966646587005, 138.2956252759109645 ) ) ;
#6722 = CARTESIAN_POINT ( 'NONE',  ( 107.0664832912739541, -23.22944715994095333, 311.6356252759109680 ) ) ;
#6723 = CARTESIAN_POINT ( 'NONE',  ( 112.0638110394401679, -45.48956745532829871, 128.9896019377486027 ) ) ;
#6724 = ADVANCED_FACE ( 'NONE', ( #7773 ), #54985, .F. ) ;
#6725 = CARTESIAN_POINT ( 'NONE',  ( 102.9710815734590454, -46.31642646611675218, 88.25562527591095829 ) ) ;
#6726 = CYLINDRICAL_SURFACE ( 'NONE', #60956, 218.1859999999999786 ) ;
#6727 = ORIENTED_EDGE ( 'NONE', *, *, #19121, .T. ) ;
#6728 = DIRECTION ( 'NONE',  ( 0.000000000000000000, -0.7071067811865315855, -0.7071067811865634489 ) ) ;
#6729 = ADVANCED_FACE ( 'NONE', ( #21409 ), #89554, .T. ) ;
#6730 = DIRECTION ( 'NONE',  ( 0.000000000000000000, 0.000000000000000000, 1.000000000000000000 ) ) ;
#6731 = AXIS2_PLACEMENT_3D ( 'NONE', #56747, #49922, #41316 ) ;
#6732 = EDGE_LOOP ( 'NONE', ( #4607, #6799, #66363, #66183 ) ) ;
#6733 = DIRECTION ( 'NONE',  ( -1.000000000000000078E-15, 0.000000000000000000, 1.000000000000000000 ) ) ;
#6734 = CARTESIAN_POINT ( 'NONE',  ( 133.5842039024481096, -58.72944715994091780, 207.5838068554170377 ) ) ;
#6735 = CARTESIAN_POINT ( 'NONE',  ( 108.0121126588926046, -24.94157235513505100, 265.0127681330535552 ) ) ;
#6736 = LINE ( 'NONE', #81720, #17027 ) ;
#6737 = DIRECTION ( 'NONE',  ( 2.505701470911820065E-15, 0.000000000000000000, 1.000000000000000000 ) ) ;
#6738 = DIRECTION ( 'NONE',  ( 0.000000000000000000, 1.000000000000000000, 0.000000000000000000 ) ) ;
#6739 = CARTESIAN_POINT ( 'NONE',  ( 109.4546162266718454, -25.87086512622375878, 29.90419670448296685 ) ) ;
#6741 = CARTESIAN_POINT ( 'NONE',  ( 108.3168256696638281, -47.05733704442508980, 113.6727681330539639 ) ) ;
#6740 = CARTESIAN_POINT ( 'NONE',  ( 97.19020072829189871, -38.39417980001610431, 101.4598920277657186 ) ) ;
#6742 = CARTESIAN_POINT ( 'NONE',  ( -44.45000000000000284, 114.2999999999999972, 275.4630000000000223 ) ) ;
#6743 = CARTESIAN_POINT ( 'NONE',  ( 107.9218747862861250, -47.19940893231376577, 177.6413395616249886 ) ) ;
#6745 = EDGE_CURVE ( 'NONE', #48789, #57151, #42713, .T. ) ;
#6744 = CARTESIAN_POINT ( 'NONE',  ( 183.5150000000000148, 68.61249999999999716, -35.28456447661459805 ) ) ;
#6746 = ORIENTED_EDGE ( 'NONE', *, *, #89384, .T. ) ;
#6747 = LINE ( 'NONE', #34894, #46849 ) ;
#6748 = FACE_BOUND ( 'NONE', #68398, .T. ) ;
#6749 = EDGE_CURVE ( 'NONE', #12034, #72171, #35917, .T. ) ;
#6750 = CARTESIAN_POINT ( 'NONE',  ( 107.0667039024470313, -104.2784471599420755, -19.78219314458201694 ) ) ;
#6751 = ORIENTED_EDGE ( 'NONE', *, *, #40651, .T. ) ;
#6752 = CYLINDRICAL_SURFACE ( 'NONE', #25901, 5.041900000000000048 ) ;
#6754 = ORIENTED_EDGE ( 'NONE', *, *, #15746, .F. ) ;
#6753 = CARTESIAN_POINT ( 'NONE',  ( 117.2811830599562057, -39.02712847638015603, 148.6499109901969859 ) ) ;
#6755 = CARTESIAN_POINT ( 'NONE',  ( 72.96458098368701428, 117.4749999999999943, -72.96458098368670164 ) ) ;
#6756 = CARTESIAN_POINT ( 'NONE',  ( 97.03730526165486481, -41.43059529571826261, 207.6632443235299661 ) ) ;
#6757 = VECTOR ( 'NONE', #78361, 1000.000000000000000 ) ;
#6758 = CARTESIAN_POINT ( 'NONE',  ( 85.96437953530612219, 73.28356282573676594, 98.26026929335903048 ) ) ;
#6759 = CARTESIAN_POINT ( 'NONE',  ( -105.4788588808464027, 127.0000000000000000, 3.968749999998844924 ) ) ;
#6760 = CARTESIAN_POINT ( 'NONE',  ( 116.3114837287122754, -32.94280867712679850, 274.1356252759109680 ) ) ;
#6761 = ORIENTED_EDGE ( 'NONE', *, *, #44679, .T. ) ;
#6762 = AXIS2_PLACEMENT_3D ( 'NONE', #75247, #82970, #40708 ) ;
#6763 = VECTOR ( 'NONE', #27033, 1000.000000000000000 ) ;
#6764 = CONTEXT_DEPENDENT_SHAPE_REPRESENTATION ( #417, #59750 ) ;
#6765 = VERTEX_POINT ( 'NONE', #22307 ) ;
#6766 = ORIENTED_EDGE ( 'NONE', *, *, #54500, .T. ) ;
#6767 = VERTEX_POINT ( 'NONE', #49981 ) ;
#6768 = DIRECTION ( 'NONE',  ( 1.000000000000000078E-15, -1.000000000000000000, 0.000000000000000000 ) ) ;
#6769 = CARTESIAN_POINT ( 'NONE',  ( 97.91927484100293100, -41.73055353899491138, 217.7241967044829494 ) ) ;
#6770 = CARTESIAN_POINT ( 'NONE',  ( 29.77381068363482441, -48.62134037875501491, 249.9678068554150059 ) ) ;
#6771 = CARTESIAN_POINT ( 'NONE',  ( 136.5970450997423313, -17.65293374834612194, 2.807537076566525513 ) ) ;
#6773 = CARTESIAN_POINT ( 'NONE',  ( 0.000000000000000000, 127.0000000000000000, -103.1875000000000000 ) ) ;
#6772 = LINE ( 'NONE', #55346, #59560 ) ;
#6774 = DIRECTION ( 'NONE',  ( -8.673617379884035472E-16, -1.000000000000000000, 0.000000000000000000 ) ) ;
#6775 = AXIS2_PLACEMENT_3D ( 'NONE', #50056, #56423, #43697 ) ;
#6776 = EDGE_CURVE ( 'NONE', #38828, #71132, #1820, .T. ) ;
#6777 = EDGE_LOOP ( 'NONE', ( #35142, #56537, #570, #38893 ) ) ;
#6778 = EDGE_LOOP ( 'NONE', ( #30179, #38020, #19796, #18154 ) ) ;
#6779 = CARTESIAN_POINT ( 'NONE',  ( 194.0371591254584587, -46.82818131005407736, 180.4678068554150343 ) ) ;
#6780 = CARTESIAN_POINT ( 'NONE',  ( 177.4809174648213741, -48.32844715993478957, 249.9678068554149775 ) ) ;
#6781 = EDGE_CURVE ( 'NONE', #69697, #57874, #27780, .T. ) ;
#6782 = CARTESIAN_POINT ( 'NONE',  ( 101.9853755998761500, -45.08682593082387058, 243.1413395616249886 ) ) ;
#6783 = CARTESIAN_POINT ( 'NONE',  ( 172.5664832912729878, -27.57844715994070484, 78.92562527591199739 ) ) ;
#6784 = CARTESIAN_POINT ( 'NONE',  ( 116.9446180447426826, -41.83184233209001235, 89.44705384733897802 ) ) ;
#6785 = DIRECTION ( 'NONE',  ( 0.000000000000000000, 1.000000000000000000, 0.000000000000000000 ) ) ;
#6786 = CARTESIAN_POINT ( 'NONE',  ( 102.0661958919803425, -27.97100149082080378, 21.48984596613240683 ) ) ;
#6787 = ORIENTED_EDGE ( 'NONE', *, *, #71437, .T. ) ;
#6788 = DIRECTION ( 'NONE',  ( 0.000000000000000000, 1.000000000000000000, 0.000000000000000000 ) ) ;
#6789 = EDGE_LOOP ( 'NONE', ( #2741, #76107 ) ) ;
#6790 = ORIENTED_EDGE ( 'NONE', *, *, #14089, .F. ) ;
#6791 = CARTESIAN_POINT ( 'NONE',  ( 48.16670390244701139, -28.27351298637280408, -5.074374724088000832 ) ) ;
#6792 = CARTESIAN_POINT ( 'NONE',  ( 98.98570259493575918, -42.74373749968300729, 258.2672975916112819 ) ) ;
#6793 = VECTOR ( 'NONE', #21750, 1000.000000000000000 ) ;
#6794 = DIRECTION ( 'NONE',  ( -0.000000000000000000, -0.000000000000000000, -1.000000000000000000 ) ) ;
#6795 = EDGE_CURVE ( 'NONE', #65795, #61431, #32119, .T. ) ;
#6796 = CARTESIAN_POINT ( 'NONE',  ( 108.4170684944699019, -26.73498250654907693, 139.9689921095843772 ) ) ;
#6797 = DIRECTION ( 'NONE',  ( 0.000000000000000000, 0.000000000000000000, -1.000000000000000000 ) ) ;
#6798 = DIRECTION ( 'NONE',  ( -0.7071067811865784369, 0.7071067811865165975, -7.071067811865791864E-16 ) ) ;
#6799 = ORIENTED_EDGE ( 'NONE', *, *, #35830, .F. ) ;
#6800 = DIRECTION ( 'NONE',  ( 0.000000000000000000, 0.000000000000000000, -1.000000000000000000 ) ) ;
#6801 = CARTESIAN_POINT ( 'NONE',  ( 98.30747440715256857, -41.72872907108401108, 182.7402955621933813 ) ) ;
#6802 = ORIENTED_EDGE ( 'NONE', *, *, #6613, .T. ) ;
#6803 = CARTESIAN_POINT ( 'NONE',  ( 103.4771249150381749, -25.43533399052049049, 55.32133956162594046 ) ) ;
#6804 = ORIENTED_EDGE ( 'NONE', *, *, #34638, .T. ) ;
#6805 = CARTESIAN_POINT ( 'NONE',  ( 111.2703484347609333, -28.70728902343469002, 14.10289601855296837 ) ) ;
#6806 = EDGE_CURVE ( 'NONE', #59337, #59214, #36383, .T. ) ;
#6807 = CARTESIAN_POINT ( 'NONE',  ( 112.0672218174811974, -45.48765836883565328, 127.9900062656194564 ) ) ;
#6808 = CARTESIAN_POINT ( 'NONE',  ( 98.40655050692420502, -32.18313002855524729, 135.9413395616259947 ) ) ;
#6809 = CARTESIAN_POINT ( 'NONE',  ( 107.0667039024470313, -104.2784471599421323, -21.78219314458201694 ) ) ;
#6810 = AXIS2_PLACEMENT_3D ( 'NONE', #48859, #14378, #28434 ) ;
#6811 = LINE ( 'NONE', #6, #53048 ) ;
#6812 = FACE_OUTER_BOUND ( 'NONE', #46378, .T. ) ;
#6813 = VECTOR ( 'NONE', #58508, 1000.000000000000000 ) ;
#6814 = CARTESIAN_POINT ( 'NONE',  ( 1.594823438788931513, 69.92315182778645521, 130.5484606227018958 ) ) ;
#6815 = CARTESIAN_POINT ( 'NONE',  ( 113.8273992703627044, -26.93653503804465288, 235.5956252759109759 ) ) ;
#6816 = CARTESIAN_POINT ( 'NONE',  ( 91.11128979799246963, 89.26692529358288652, -75.85717701425140547 ) ) ;
#6817 = EDGE_LOOP ( 'NONE', ( #76793, #58348, #12878, #82892 ) ) ;
#6818 = CIRCLE ( 'NONE', #18418, 2.030000000001872529 ) ;
#6819 = VERTEX_POINT ( 'NONE', #38157 ) ;
#6820 = CARTESIAN_POINT ( 'NONE',  ( 109.0806625061526205, -47.64460086702110431, 123.7337205140059666 ) ) ;
#6821 = AXIS2_PLACEMENT_3D ( 'NONE', #87697, #18653, #45881 ) ;
#6822 = LINE ( 'NONE', #61768, #430 ) ;
#6823 = AXIS2_PLACEMENT_3D ( 'NONE', #77995, #8502, #58417 ) ;
#6824 = EDGE_CURVE ( 'NONE', #83969, #22713, #52381, .T. ) ;
#6825 = ORIENTED_EDGE ( 'NONE', *, *, #20550, .F. ) ;
#6826 = VERTEX_POINT ( 'NONE', #64973 ) ;
#6827 = VERTEX_POINT ( 'NONE', #2315 ) ;
#6828 = CARTESIAN_POINT ( 'NONE',  ( 32.09598329127609873, -23.42844715994129956, 193.9678068554150911 ) ) ;
#6829 = CARTESIAN_POINT ( 'NONE',  ( 25.56670390244722313, -42.82844715994178131, 137.2178068554150627 ) ) ;
#6830 = FACE_OUTER_BOUND ( 'NONE', #78515, .T. ) ;
#6831 = CARTESIAN_POINT ( 'NONE',  ( 3.968750000000000000, 120.6499999999999915, -105.4788588808464027 ) ) ;
#6832 = ADVANCED_FACE ( 'NONE', ( #50436 ), #37725, .T. ) ;
#6833 = CARTESIAN_POINT ( 'NONE',  ( 100.4889591185686015, -31.84898980388015843, 178.6366617981629474 ) ) ;
#6834 = CARTESIAN_POINT ( 'NONE',  ( 105.6290766085263044, -47.07696477925017575, 253.4670538473393719 ) ) ;
#6835 = CARTESIAN_POINT ( 'NONE',  ( 97.81170508561586985, -40.51744524251693491, 57.63550115181184452 ) ) ;
#6836 = ORIENTED_EDGE ( 'NONE', *, *, #53919, .F. ) ;
#6837 = CARTESIAN_POINT ( 'NONE',  ( 6.349546116388139261, 71.54336850463093356, 118.3864143103247812 ) ) ;
#6838 = VECTOR ( 'NONE', #82006, 1000.000000000000000 ) ;
#6839 = VECTOR ( 'NONE', #25383, 1000.000000000000000 ) ;
#6840 = CARTESIAN_POINT ( 'NONE',  ( 7.661254700127833495, 82.54999999999999716, 317.6630000000000109 ) ) ;
#6841 = ORIENTED_EDGE ( 'NONE', *, *, #55333, .F. ) ;
#6842 = ORIENTED_EDGE ( 'NONE', *, *, #73835, .F. ) ;
#6843 = AXIS2_PLACEMENT_3D ( 'NONE', #81615, #19364, #12550 ) ;
#6844 = CARTESIAN_POINT ( 'NONE',  ( 46.48091746482045750, -49.32844715994088602, 180.4678068554150911 ) ) ;
#6845 = VERTEX_POINT ( 'NONE', #3204 ) ;
#6846 = CARTESIAN_POINT ( 'NONE',  ( 78.56670390244701707, -90.27844715994098124, 51.21780685541800437 ) ) ;
#6847 = CARTESIAN_POINT ( 'NONE',  ( 97.53184222742581255, -39.74894927286113955, 16.57053032456689934 ) ) ;
#6848 = CARTESIAN_POINT ( 'NONE',  ( 33.91903122894598965, -35.91149509761181235, -5.074374724088000832 ) ) ;
#6849 = CARTESIAN_POINT ( 'NONE',  ( 62.56670390244828184, -48.82844715994019680, 300.4678068554150627 ) ) ;
#6850 = CARTESIAN_POINT ( 'NONE',  ( 98.03781028509631312, -36.02536330594374192, 190.6990864947429998 ) ) ;
#6851 = CARTESIAN_POINT ( 'NONE',  ( 96.87811797401508329, -32.32375813437732859, 61.01372051400599616 ) ) ;
#6853 = ADVANCED_FACE ( 'NONE', ( #65849 ), #58583, .F. ) ;
#6852 = CARTESIAN_POINT ( 'NONE',  ( 50.56670390244699576, -18.82844715994031048, -5.074374724088000832 ) ) ;
#6854 = VERTEX_POINT ( 'NONE', #64533 ) ;
#6855 = EDGE_CURVE ( 'NONE', #14017, #70942, #24872, .T. ) ;
#6856 = DIRECTION ( 'NONE',  ( 0.7071067811873696929, 0.7071067811857253416, 7.071067811873690333E-16 ) ) ;
#6857 = ORIENTED_EDGE ( 'NONE', *, *, #28591, .T. ) ;
#6858 = LINE ( 'NONE', #62264, #22943 ) ;
#6859 = ORIENTED_EDGE ( 'NONE', *, *, #84996, .F. ) ;
#6860 = B_SPLINE_CURVE_WITH_KNOTS ( 'NONE', 3,
 ( #5014, #26790, #32713, #74502, #60407, #46770, #12280, #66786, #32259, #87247, #39972, #54022, #59954, #25454, #87687, #31816, #47224, #54473, #74951, #59512, #82237, #19991, #75406, #13180, #40863, #25012, #52676, #80435, #61748, #70378 ),
 .UNSPECIFIED., .F., .F.,
 ( 4, 2, 2, 2, 1, 2, 2, 2, 2, 2, 2, 2, 1, 2, 2, 4 ),
 ( 0.5000000000000000000, 0.5625000000000165423, 0.5937500000000232037, 0.6093750000000266454, 0.6171875000000283107, 0.6210937500000291989, 0.6250000000000299760, 0.6875000000000308642, 0.7187500000000315303, 0.7500000000000321965, 0.8125000000000320854, 0.8437500000000304201, 0.8593750000000295319, 0.8671875000000290878, 0.8750000000000286438, 1.000000000000000000 ),
 .UNSPECIFIED. ) ;
#6861 = DIRECTION ( 'NONE',  ( 0.000000000000000000, 0.000000000000000000, 1.000000000000000000 ) ) ;
#6862 = CARTESIAN_POINT ( 'NONE',  ( 168.0371591254543944, -48.62818131005519717, 249.9678068554149775 ) ) ;
#6863 = CARTESIAN_POINT ( 'NONE',  ( 68.78290018810869810, -67.86861087870656206, 247.4717563792629846 ) ) ;
#6864 = VECTOR ( 'NONE', #86102, 1000.000000000000000 ) ;
#6865 = DIRECTION ( 'NONE',  ( -0.2588190451025206285, 0.000000000000000000, 0.9659258262890683122 ) ) ;
#6866 = ORIENTED_EDGE ( 'NONE', *, *, #29322, .F. ) ;
#6867 = CARTESIAN_POINT ( 'NONE',  ( 103.9507802182147600, -47.35902078718802954, 62.33753003781600199 ) ) ;
#6869 = CARTESIAN_POINT ( 'NONE',  ( 82.89895571708365196, 82.54999999999999716, -100.8594679592203818 ) ) ;
#6868 = CARTESIAN_POINT ( 'NONE',  ( 0.000000000000000000, 353.0471713899363522, 0.000000000000000000 ) ) ;
#6870 = CARTESIAN_POINT ( 'NONE',  ( 107.0664832912739399, -36.72944715994096754, 296.0306255462182321 ) ) ;
#6871 = LINE ( 'NONE', #76814, #22376 ) ;
#6872 = ORIENTED_EDGE ( 'NONE', *, *, #15858, .T. ) ;
#6873 = CARTESIAN_POINT ( 'NONE',  ( 100.2031981095150854, -29.33968530819532461, 121.6706578896535405 ) ) ;
#6874 = DIRECTION ( 'NONE',  ( 0.000000000000000000, 0.000000000000000000, 1.000000000000000000 ) ) ;
#6875 = CARTESIAN_POINT ( 'NONE',  ( 52.65249034007751305, -49.32844715994061602, 129.9678068554150911 ) ) ;
#6876 = ORIENTED_EDGE ( 'NONE', *, *, #56333, .T. ) ;
#6877 = CARTESIAN_POINT ( 'NONE',  ( 98.57234554589554421, -43.83823254894062416, 67.86895860924497015 ) ) ;
#6878 = AXIS2_PLACEMENT_3D ( 'NONE', #9641, #71438, #63714 ) ;
#6880 = DIRECTION ( 'NONE',  ( 1.000000000000000000, 8.843517682682131024E-16, 1.000000000000000078E-15 ) ) ;
#6879 = LINE ( 'NONE', #20527, #43625 ) ;
#6881 = DIRECTION ( 'NONE',  ( 1.000000000000000000, 0.000000000000000000, 0.000000000000000000 ) ) ;
#6882 = AXIS2_PLACEMENT_3D ( 'NONE', #23760, #51428, #38698 ) ;
#6883 = CIRCLE ( 'NONE', #80887, 4.500000000000003553 ) ;
#6884 = VECTOR ( 'NONE', #81579, 1000.000000000000000 ) ;
#6885 = CARTESIAN_POINT ( 'NONE',  ( 132.1532570847676595, -116.6569832596315166, 250.2191008560389776 ) ) ;
#6886 = ORIENTED_EDGE ( 'NONE', *, *, #62105, .F. ) ;
#6887 = CARTESIAN_POINT ( 'NONE',  ( 118.1851208724671238, -36.91582462397654751, 149.8127681330539644 ) ) ;
#6889 = ORIENTED_EDGE ( 'NONE', *, *, #17770, .F. ) ;
#6888 = DIRECTION ( 'NONE',  ( -0.4999999999999990008, 0.000000000000000000, 0.8660254037844392627 ) ) ;
#6890 = CARTESIAN_POINT ( 'NONE',  ( 97.24442698086048154, -40.26379795196656630, 262.6013395616254797 ) ) ;
#6891 = CARTESIAN_POINT ( 'NONE',  ( 98.04096435976430257, -41.04069707603596129, 252.6812049413570946 ) ) ;
#6892 = CARTESIAN_POINT ( 'NONE',  ( 0.000000000000000000, 65.60000000000000853, 0.000000000000000000 ) ) ;
#6893 = FACE_OUTER_BOUND ( 'NONE', #5867, .T. ) ;
#6894 = LINE ( 'NONE', #22330, #26794 ) ;
#6895 = AXIS2_PLACEMENT_3D ( 'NONE', #44826, #66613, #12107 ) ;
#6896 = CARTESIAN_POINT ( 'NONE',  ( 67.78013389119247734, -136.6656689513177696, 247.3338295459389826 ) ) ;
#6897 = DIRECTION ( 'NONE',  ( 0.000000000000000000, 0.000000000000000000, -1.000000000000000000 ) ) ;
#6898 = VECTOR ( 'NONE', #7808, 1000.000000000000000 ) ;
#6900 = CARTESIAN_POINT ( 'NONE',  ( 98.80555182512723889, -41.96590078842033478, 186.7756252759109543 ) ) ;
#6899 = AXIS2_PLACEMENT_3D ( 'NONE', #17138, #45262, #25273 ) ;
#6901 = VERTEX_POINT ( 'NONE', #78182 ) ;
#6902 = ORIENTED_EDGE ( 'NONE', *, *, #6590, .T. ) ;
#6903 = CARTESIAN_POINT ( 'NONE',  ( 111.6733053606431412, -27.77132819582071122, 166.1301547344679932 ) ) ;
#6904 = LINE ( 'NONE', #29149, #19730 ) ;
#6905 = ADVANCED_FACE ( 'NONE', ( #44061 ), #23654, .T. ) ;
#6907 = CARTESIAN_POINT ( 'NONE',  ( 79.68958420874191972, -33.97944715994105991, 1.625625275910942635 ) ) ;
#6906 = CARTESIAN_POINT ( 'NONE',  ( 98.92341559625380398, -33.23365848574461268, 12.43586902018295426 ) ) ;
#6908 = CARTESIAN_POINT ( 'NONE',  ( -103.1875000000000000, 127.0000000000000000, -1.080832317973422076E-12 ) ) ;
#6909 = EDGE_CURVE ( 'NONE', #14493, #24486, #1862, .T. ) ;
#6910 = LINE ( 'NONE', #33727, #2579 ) ;
#6911 = ADVANCED_FACE ( 'NONE', ( #30458 ), #58156, .T. ) ;
#6912 = CARTESIAN_POINT ( 'NONE',  ( 60.32499999999999574, 82.54999999999999716, 335.3740053999999304 ) ) ;
#6913 = CARTESIAN_POINT ( 'NONE',  ( 107.0667039024479834, -36.72944715994100306, 239.5838068554170093 ) ) ;
#6914 = CARTESIAN_POINT ( 'NONE',  ( 88.06670390244796920, -14.72944715994105991, 199.5838068554169809 ) ) ;
#6915 = CARTESIAN_POINT ( 'NONE',  ( 104.4161250475293343, -26.02246701806295448, 240.2575300378159682 ) ) ;
#6916 = CARTESIAN_POINT ( 'NONE',  ( 97.78518716477550754, -40.45211749721122629, 171.6302806827789311 ) ) ;
#6917 = ORIENTED_EDGE ( 'NONE', *, *, #58349, .T. ) ;
#6918 = ORIENTED_EDGE ( 'NONE', *, *, #65156, .T. ) ;
#6919 = EDGE_CURVE ( 'NONE', #47694, #68380, #71313, .T. ) ;
#6920 = EDGE_CURVE ( 'NONE', #77431, #38484, #16830, .T. ) ;
#6921 = CARTESIAN_POINT ( 'NONE',  ( -83.41622542100893156, 78.46444036551650925, -100.4321520267697707 ) ) ;
#6922 = CARTESIAN_POINT ( 'NONE',  ( -84.42134122279082931, 95.24969287062862122, -83.24211534968698345 ) ) ;
#6923 = CARTESIAN_POINT ( 'NONE',  ( 109.6438830164042031, -46.47987668453704657, 123.7798306129299846 ) ) ;
#6924 = CARTESIAN_POINT ( 'NONE',  ( 0.000000000000000000, 238.7999999999999829, 154.6557476874258441 ) ) ;
#6925 = CIRCLE ( 'NONE', #38826, 4.749999999999976907 ) ;
#6926 = EDGE_CURVE ( 'NONE', #17700, #2162, #72691, .T. ) ;
#6927 = FACE_OUTER_BOUND ( 'NONE', #37041, .T. ) ;
#6928 = ADVANCED_FACE ( 'NONE', ( #3634, #60261 ), #87993, .T. ) ;
#6929 = ORIENTED_EDGE ( 'NONE', *, *, #44609, .T. ) ;
#6930 = CARTESIAN_POINT ( 'NONE',  ( 99.73159624296292236, -44.24858557630691536, 17.96133956162493206 ) ) ;
#6931 = EDGE_CURVE ( 'NONE', #65097, #79518, #43615, .T. ) ;
#6932 = CARTESIAN_POINT ( 'NONE',  ( 115.9069864544413662, -30.09434420101750973, 264.3508633711492735 ) ) ;
#6933 = ORIENTED_EDGE ( 'NONE', *, *, #83123, .T. ) ;
#6934 = CARTESIAN_POINT ( 'NONE',  ( -11.93654268304338650, 86.60576128432494158, 117.9536290563174674 ) ) ;
#6935 = ADVANCED_FACE ( 'NONE', ( #50890 ), #78630, .F. ) ;
#6936 = DIRECTION ( 'NONE',  ( 0.000000000000000000, 0.000000000000000000, -1.000000000000000000 ) ) ;
#6937 = CARTESIAN_POINT ( 'NONE',  ( 116.9214244060436840, -38.68692813258547147, 168.6706793604847974 ) ) ;
#6938 = ADVANCED_FACE ( 'NONE', ( #18945 ), #67991, .F. ) ;
#6939 = CARTESIAN_POINT ( 'NONE',  ( 114.1581430127411352, -30.74577825543392606, 72.20237608387697037 ) ) ;
#6940 = CARTESIAN_POINT ( 'NONE',  ( 111.4263534857568771, -47.77543206737910708, 168.8756252759109486 ) ) ;
#6941 = CYLINDRICAL_SURFACE ( 'NONE', #84131, 4.762500000000002842 ) ;
#6942 = ORIENTED_EDGE ( 'NONE', *, *, #70237, .T. ) ;
#6943 = VECTOR ( 'NONE', #50867, 1000.000000000000000 ) ;
#6944 = CARTESIAN_POINT ( 'NONE',  ( 107.0667039024470313, -104.2784471599409528, 222.2178068554179902 ) ) ;
#6945 = VERTEX_POINT ( 'NONE', #26647 ) ;
#6946 = ORIENTED_EDGE ( 'NONE', *, *, #32941, .T. ) ;
#6947 = VECTOR ( 'NONE', #16726, 1000.000000000000000 ) ;
#6948 = CIRCLE ( 'NONE', #48936, 3.299999999999999822 ) ;
#6949 = CARTESIAN_POINT ( 'NONE',  ( 4.868064396069526900, 94.30179516618007085, 118.4578665249601102 ) ) ;
#6950 = EDGE_LOOP ( 'NONE', ( #51440, #38418, #68909, #17358 ) ) ;
#6951 = ORIENTED_EDGE ( 'NONE', *, *, #37541, .F. ) ;
#6952 = DIRECTION ( 'NONE',  ( 1.000000000000000000, 0.000000000000000000, 0.000000000000000000 ) ) ;
#6953 = CARTESIAN_POINT ( 'NONE',  ( 106.7337219657603100, -28.19449539544314476, 84.52956268522000016 ) ) ;
#6954 = CARTESIAN_POINT ( 'NONE',  ( 95.27000809083011745, -38.09955253919518015, 236.4184824187679510 ) ) ;
#6955 = ADVANCED_FACE ( 'NONE', ( #75260, #89344 ), #88895, .F. ) ;
#6956 = AXIS2_PLACEMENT_3D ( 'NONE', #76634, #2129, #42979 ) ;
#6957 = CARTESIAN_POINT ( 'NONE',  ( 113.1426608820138426, -26.58408993604425419, 204.6470538473399756 ) ) ;
#6959 = ADVANCED_FACE ( 'NONE', ( #41604 ), #17614, .F. ) ;
#6958 = CARTESIAN_POINT ( 'NONE',  ( 99.08262072259969955, -44.34008189452608661, 32.92038718067297509 ) ) ;
#6960 = DIRECTION ( 'NONE',  ( 1.000000000000000000, 0.000000000000000000, 0.000000000000000000 ) ) ;
#6961 = CARTESIAN_POINT ( 'NONE',  ( 108.3313211724201182, -46.73510064337951064, 93.67712277074488725 ) ) ;
#6962 = EDGE_CURVE ( 'NONE', #24929, #20886, #89795, .T. ) ;
#6963 = VECTOR ( 'NONE', #89812, 999.9999999999998863 ) ;
#6964 = ORIENTED_EDGE ( 'NONE', *, *, #67334, .T. ) ;
#6965 = AXIS2_PLACEMENT_3D ( 'NONE', #25339, #11726, #73948 ) ;
#6966 = ADVANCED_FACE ( 'NONE', ( #54774 ), #34805, .F. ) ;
#6967 = CIRCLE ( 'NONE', #17097, 1.000000000000000888 ) ;
#6968 = VECTOR ( 'NONE', #15751, 1000.000000000000000 ) ;
#6969 = CARTESIAN_POINT ( 'NONE',  ( 96.71010325458811963, -37.26253042779857338, 121.3794347997209684 ) ) ;
#6970 = CARTESIAN_POINT ( 'NONE',  ( 117.4914506980151572, -37.69211045134998272, 78.75276813305399060 ) ) ;
#6971 = CARTESIAN_POINT ( 'NONE',  ( 115.9975756407361018, -30.13790158448777845, 259.3203871806730945 ) ) ;
#6972 = ORIENTED_EDGE ( 'NONE', *, *, #47399, .F. ) ;
#6973 = CARTESIAN_POINT ( 'NONE',  ( 115.4600223225059494, -29.53725764737424342, 229.4022919425779605 ) ) ;
#6974 = CARTESIAN_POINT ( 'NONE',  ( 25.56670390244744340, -48.82844715994178841, 175.7178068554150627 ) ) ;
#6975 = DIRECTION ( 'NONE',  ( 1.000000000000000000, 3.999999999999999995E-14, 1.000000000000000078E-15 ) ) ;
#6976 = CARTESIAN_POINT ( 'NONE',  ( 72.96458098368650269, 127.0000000000000000, 67.92268098368730023 ) ) ;
#6978 = LINE ( 'NONE', #43270, #45641 ) ;
#6977 = FACE_OUTER_BOUND ( 'NONE', #33388, .T. ) ;
#6979 = DIRECTION ( 'NONE',  ( -1.000000000000000000, 1.816601132648505598E-15, 0.000000000000000000 ) ) ;
#6980 = DIRECTION ( 'NONE',  ( 0.000000000000000000, -1.000000000000000000, 0.000000000000000000 ) ) ;
#6981 = CARTESIAN_POINT ( 'NONE',  ( 0.8301440424157503495, 95.22976080284070122, -118.5538265829301565 ) ) ;
#6982 = AXIS2_PLACEMENT_3D ( 'NONE', #74538, #19127, #39561 ) ;
#6983 = DIRECTION ( 'NONE',  ( -1.000000000000000000, -4.299999999999999979E-14, -1.000000000000000078E-15 ) ) ;
#6984 = DIRECTION ( 'NONE',  ( 1.000000000000000000, 0.000000000000000000, 0.000000000000000000 ) ) ;
#6985 = LINE ( 'NONE', #28306, #18761 ) ;
#6987 = ORIENTED_EDGE ( 'NONE', *, *, #54071, .T. ) ;
#6986 = CARTESIAN_POINT ( 'NONE',  ( 107.0667039024470313, -104.2784471599420755, -19.78219314458201694 ) ) ;
#6988 = CARTESIAN_POINT ( 'NONE',  ( 107.0667039024467186, -36.72944715994091069, 195.5838068554169809 ) ) ;
#6989 = CARTESIAN_POINT ( 'NONE',  ( 99.36516439250377175, -29.66998179773359823, 275.7356252759109907 ) ) ;
#6990 = CARTESIAN_POINT ( 'NONE',  ( 108.0069324954157537, -26.34569400419502827, 151.0041967044829505 ) ) ;
#6991 = CARTESIAN_POINT ( 'NONE',  ( 100.8224507837568638, -45.17634439094529597, 253.0699109901969450 ) ) ;
#6992 = CARTESIAN_POINT ( 'NONE',  ( -45.51636842011945561, 65.60000000000000853, -45.51636842012056405 ) ) ;
#6993 = VECTOR ( 'NONE', #76413, 1000.000000000000000 ) ;
#6995 = CARTESIAN_POINT ( 'NONE',  ( 0.000000000000000000, 117.4749999999999943, -103.1875000000000000 ) ) ;
#6994 = DIRECTION ( 'NONE',  ( -1.000000000000000000, -0.000000000000000000, -0.000000000000000000 ) ) ;
#6996 = CARTESIAN_POINT ( 'NONE',  ( 108.3333560997344733, -46.73487186194755338, 138.6772847610721726 ) ) ;
#6997 = VECTOR ( 'NONE', #73521, 1000.000000000000000 ) ;
#6998 = PLANE ( 'NONE',  #73185 ) ;
#6999 = ORIENTED_EDGE ( 'NONE', *, *, #78443, .T. ) ;
#7000 = DIRECTION ( 'NONE',  ( -1.000000000000000000, -1.734723475976808672E-15, 0.000000000000000000 ) ) ;
#7001 = VERTEX_POINT ( 'NONE', #19840 ) ;
#7002 = CARTESIAN_POINT ( 'NONE',  ( 97.64684354035226477, -39.08338314719364348, 165.9438483995059528 ) ) ;
#7004 = ORIENTED_EDGE ( 'NONE', *, *, #65276, .T. ) ;
#7003 = CARTESIAN_POINT ( 'NONE',  ( 98.30741342104360569, -41.72858007013866910, 186.7402835883439138 ) ) ;
#7005 = FACE_OUTER_BOUND ( 'NONE', #28073, .T. ) ;
#7006 = CARTESIAN_POINT ( 'NONE',  ( 113.5515132932710713, -44.90922781482908732, 164.1099109901969655 ) ) ;
#7007 = FACE_OUTER_BOUND ( 'NONE', #63430, .T. ) ;
#7008 = LINE ( 'NONE', #33029, #79141 ) ;
#7009 = LINE ( 'NONE', #12941, #6646 ) ;
#7010 = CARTESIAN_POINT ( 'NONE',  ( 148.0533267522749838, 20.32000000000000028, -160.2664750769289697 ) ) ;
#7011 = DIRECTION ( 'NONE',  ( 0.000000000000000000, 0.000000000000000000, -1.000000000000000000 ) ) ;
#7012 = CARTESIAN_POINT ( 'NONE',  ( 98.13101841594837538, -32.75189731695855500, 100.9927681330539713 ) ) ;
#7013 = ORIENTED_EDGE ( 'NONE', *, *, #30020, .F. ) ;
#7014 = EDGE_LOOP ( 'NONE', ( #70795, #75809 ) ) ;
#7015 = EDGE_LOOP ( 'NONE', ( #31162, #32205 ) ) ;
#7016 = AXIS2_PLACEMENT_3D ( 'NONE', #14271, #41945, #88001 ) ;
#7017 = AXIS2_PLACEMENT_3D ( 'NONE', #2647, #44845, #16715 ) ;
#7018 = CARTESIAN_POINT ( 'NONE',  ( 41.56648329127499153, -36.32844715994070839, 254.1756252759120400 ) ) ;
#7020 = CARTESIAN_POINT ( 'NONE',  ( 101.9936210298387635, -45.44607158966083205, 37.15645861734014233 ) ) ;
#7019 = CARTESIAN_POINT ( 'NONE',  ( 102.9544237342424395, -27.85507949283302764, 176.4213395616249898 ) ) ;
#7021 = DIRECTION ( 'NONE',  ( 1.000000000000000078E-15, -1.000000000000000083E-30, -1.000000000000000000 ) ) ;
#7022 = EDGE_CURVE ( 'NONE', #64215, #2723, #84200, .T. ) ;
#7023 = CARTESIAN_POINT ( 'NONE',  ( 90.69304023831777783, -109.5826158781451340, -10.56397404668060780 ) ) ;
#7024 = EDGE_CURVE ( 'NONE', #75662, #21236, #20302, .T. ) ;
#7025 = DIRECTION ( 'NONE',  ( -1.000000000000000078E-15, 0.000000000000000000, 1.000000000000000000 ) ) ;
#7027 = EDGE_CURVE ( 'NONE', #10583, #42662, #50991, .T. ) ;
#7026 = AXIS2_PLACEMENT_3D ( 'NONE', #40544, #5593, #33288 ) ;
#7028 = DIRECTION ( 'NONE',  ( 0.000000000000000000, 0.000000000000000000, -1.000000000000000000 ) ) ;
#7029 = DIRECTION ( 'NONE',  ( 0.7071067811865434649, 0.7071067811865516806, 7.071067811865440820E-16 ) ) ;
#7030 = CARTESIAN_POINT ( 'NONE',  ( 98.22092589535427010, -43.31882777834842813, 111.8480062282919647 ) ) ;
#7031 = ORIENTED_EDGE ( 'NONE', *, *, #39109, .T. ) ;
#7032 = ORIENTED_EDGE ( 'NONE', *, *, #15977, .F. ) ;
#7033 = ORIENTED_EDGE ( 'NONE', *, *, #68027, .T. ) ;
#7034 = AXIS2_PLACEMENT_3D ( 'NONE', #26127, #53795, #67003 ) ;
#7035 = EDGE_CURVE ( 'NONE', #67326, #24182, #79999, .T. ) ;
#7036 = ADVANCED_FACE ( 'NONE', ( #19393 ), #13475, .T. ) ;
#7037 = CARTESIAN_POINT ( 'NONE',  ( 0.000000000000000000, 210.0000000000000000, 154.6557476874258441 ) ) ;
#7038 = CARTESIAN_POINT ( 'NONE',  ( 41.56648329127398966, -27.82844715994070484, 135.9256252759119832 ) ) ;
#7039 = AXIS2_PLACEMENT_3D ( 'NONE', #89892, #40817, #28079 ) ;
#7040 = LINE ( 'NONE', #48792, #36648 ) ;
#7041 = CARTESIAN_POINT ( 'NONE',  ( 113.2509217664418202, -31.40192927973085801, 182.2109475124489677 ) ) ;
#7042 = EDGE_CURVE ( 'NONE', #60711, #79108, #87248, .T. ) ;
#7043 = CARTESIAN_POINT ( 'NONE',  ( 167.2371591254542693, -47.82818131005522844, 313.9678068554149490 ) ) ;
#7044 = EDGE_CURVE ( 'NONE', #67515, #86125, #11833, .T. ) ;
#7045 = CARTESIAN_POINT ( 'NONE',  ( 134.0664832912739826, -9.029447159941003775, 8.225625275910998013 ) ) ;
#7046 = ORIENTED_EDGE ( 'NONE', *, *, #55799, .T. ) ;
#7048 = ORIENTED_EDGE ( 'NONE', *, *, #86607, .F. ) ;
#7047 = ORIENTED_EDGE ( 'NONE', *, *, #70922, .F. ) ;
#7049 = VECTOR ( 'NONE', #29422, 1000.000000000000000 ) ;
#7050 = LINE ( 'NONE', #68830, #34635 ) ;
#7051 = ORIENTED_EDGE ( 'NONE', *, *, #33199, .F. ) ;
#7052 = ORIENTED_EDGE ( 'NONE', *, *, #50031, .T. ) ;
#7053 = CARTESIAN_POINT ( 'NONE',  ( 78.26014418490247238, -20.80290789369970739, 7.687431601936206782 ) ) ;
#7054 = EDGE_CURVE ( 'NONE', #65246, #67223, #27862, .T. ) ;
#7055 = CARTESIAN_POINT ( 'NONE',  ( 101.7595872045747285, -44.48272901101389465, 238.5425356868499591 ) ) ;
#7056 = ORIENTED_EDGE ( 'NONE', *, *, #27552, .T. ) ;
#7057 = CIRCLE ( 'NONE', #57820, 1.000000000000000888 ) ;
#7058 = DIRECTION ( 'NONE',  ( 0.000000000000000000, 0.000000000000000000, 1.000000000000000000 ) ) ;
#7060 = EDGE_CURVE ( 'NONE', #82586, #50189, #36158, .T. ) ;
#7059 = AXIS2_PLACEMENT_3D ( 'NONE', #19419, #34382, #33042 ) ;
#7061 = CARTESIAN_POINT ( 'NONE',  ( -114.5280640324896808, 70.85472008698103252, 62.67561285116475744 ) ) ;
#7062 = VERTEX_POINT ( 'NONE', #28905 ) ;
#7063 = ORIENTED_EDGE ( 'NONE', *, *, #81554, .T. ) ;
#7064 = DIRECTION ( 'NONE',  ( -0.08544974978095701279, -0.9963424814100680926, -0.000000000000000000 ) ) ;
#7065 = ORIENTED_EDGE ( 'NONE', *, *, #72271, .F. ) ;
#7066 = VERTEX_POINT ( 'NONE', #70683 ) ;
#7067 = CARTESIAN_POINT ( 'NONE',  ( 114.3096959184101280, -40.49343719410034481, 286.2623760838771432 ) ) ;
#7068 = CARTESIAN_POINT ( 'NONE',  ( 97.81638875629413121, -31.87330516686267501, 135.9413395616259947 ) ) ;
#7069 = CARTESIAN_POINT ( 'NONE',  ( 103.2134869792595708, -46.43093390711695889, 117.2756252759109543 ) ) ;
#7070 = CARTESIAN_POINT ( 'NONE',  ( 99.34172024792457023, -34.41985901539234760, 249.5838068554171798 ) ) ;
#7071 = DIRECTION ( 'NONE',  ( 0.7071067811874389708, -0.7071067811856560636, 0.000000000000000000 ) ) ;
#7072 = CARTESIAN_POINT ( 'NONE',  ( 101.3491664457538945, -46.18916536780651683, 198.1318157521009482 ) ) ;
#7073 = CARTESIAN_POINT ( 'NONE',  ( 163.0667039024470171, -32.29483332968611364, -5.074374724088000832 ) ) ;
#7074 = CARTESIAN_POINT ( 'NONE',  ( 194.0371591254585155, -46.82818131005408446, 117.4678068554150627 ) ) ;
#7075 = ORIENTED_EDGE ( 'NONE', *, *, #76850, .F. ) ;
#7076 = CARTESIAN_POINT ( 'NONE',  ( 130.4023353925299489, 71.53177522571071734, 6.370020420676822503 ) ) ;
#7077 = ORIENTED_EDGE ( 'NONE', *, *, #61560, .F. ) ;
#7078 = EDGE_CURVE ( 'NONE', #59914, #49287, #8459, .T. ) ;
#7079 = VECTOR ( 'NONE', #84196, 1000.000000000000000 ) ;
#7080 = VERTEX_POINT ( 'NONE', #35700 ) ;
#7081 = DIRECTION ( 'NONE',  ( 4.299999999999999979E-14, -1.000000000000000000, 4.400000000000000367E-29 ) ) ;
#7082 = EDGE_CURVE ( 'NONE', #69308, #85489, #23472, .T. ) ;
#7083 = AXIS2_PLACEMENT_3D ( 'NONE', #59042, #64990, #45410 ) ;
#7084 = DIRECTION ( 'NONE',  ( 1.000000000000000000, 0.000000000000000000, 0.000000000000000000 ) ) ;
#7085 = VECTOR ( 'NONE', #22358, 1000.000000000000000 ) ;
#7086 = CARTESIAN_POINT ( 'NONE',  ( 107.9456392385311005, -25.71100025151098478, 115.0251490854349612 ) ) ;
#7087 = CARTESIAN_POINT ( 'NONE',  ( -9.371942588247355488, 73.96144982415154345, 130.2197749970455050 ) ) ;
#7088 = CARTESIAN_POINT ( 'NONE',  ( 3.968749999999229949, 120.6499999999999915, 100.8961411191535973 ) ) ;
#7089 = FACE_OUTER_BOUND ( 'NONE', #25418, .T. ) ;
#7092 = CARTESIAN_POINT ( 'NONE',  ( 98.91597900623165174, -29.29754952351882480, 226.7261014663869503 ) ) ;
#7091 = CARTESIAN_POINT ( 'NONE',  ( 103.1008684890620799, -45.92814942240114107, 57.25235007397393616 ) ) ;
#7090 = PLANE ( 'NONE',  #72513 ) ;
#7093 = FACE_OUTER_BOUND ( 'NONE', #29007, .T. ) ;
#7094 = CARTESIAN_POINT ( 'NONE',  ( 0.000000000000000000, 12.27000000000000313, 0.000000000000000000 ) ) ;
#7095 = VERTEX_POINT ( 'NONE', #14384 ) ;
#7096 = DIRECTION ( 'NONE',  ( 0.000000000000000000, 0.000000000000000000, -1.000000000000000000 ) ) ;
#7097 = VECTOR ( 'NONE', #45335, 1000.000000000000000 ) ;
#7098 = DIRECTION ( 'NONE',  ( 0.000000000000000000, -1.000000000000000000, 0.000000000000000000 ) ) ;
#7099 = FACE_BOUND ( 'NONE', #7499, .T. ) ;
#7100 = AXIS2_PLACEMENT_3D ( 'NONE', #16306, #22231, #27350 ) ;
#7101 = CARTESIAN_POINT ( 'NONE',  ( -48.02966122971777452, 66.60000000000003695, 108.3913132043271617 ) ) ;
#7102 = EDGE_CURVE ( 'NONE', #76987, #81147, #71142, .T. ) ;
#7104 = VERTEX_POINT ( 'NONE', #56122 ) ;
#7103 = CARTESIAN_POINT ( 'NONE',  ( 105.8886092880350560, -47.16805723083484736, 282.4870538473393253 ) ) ;
#7105 = CYLINDRICAL_SURFACE ( 'NONE', #65491, 5.041900000000001825 ) ;
#7106 = CARTESIAN_POINT ( 'NONE',  ( 96.59657429157336139, -36.21044007025302136, 171.2870538473399620 ) ) ;
#7107 = CARTESIAN_POINT ( 'NONE',  ( 95.25919473906076007, -35.71823372881362957, 32.25848241876794020 ) ) ;
#7108 = CARTESIAN_POINT ( 'NONE',  ( 96.60651355459405920, -37.15606806638657389, 157.3584824187679487 ) ) ;
#7109 = CARTESIAN_POINT ( 'NONE',  ( 34.67381068362099228, -26.00627455219321860, -5.074374724088000832 ) ) ;
#7110 = VECTOR ( 'NONE', #49412, 1000.000000000000000 ) ;
#7111 = CARTESIAN_POINT ( 'NONE',  ( 97.78479533213763375, -40.45114042110355967, 102.6299318713464714 ) ) ;
#7113 = DIRECTION ( 'NONE',  ( 0.000000000000000000, 0.000000000000000000, 1.000000000000000000 ) ) ;
#7112 = DIRECTION ( 'NONE',  ( 0.000000000000000000, 0.000000000000000000, 1.000000000000000000 ) ) ;
#7114 = DIRECTION ( 'NONE',  ( -0.000000000000000000, 1.000000000000000000, 0.000000000000000000 ) ) ;
#7115 = CARTESIAN_POINT ( 'NONE',  ( 63.56670390244739366, -47.82844715994014706, 180.4678068554151196 ) ) ;
#7116 = EDGE_LOOP ( 'NONE', ( #68504, #70383 ) ) ;
#7117 = EDGE_CURVE ( 'NONE', #43071, #5926, #74215, .T. ) ;
#7118 = LINE ( 'NONE', #35703, #73125 ) ;
#7119 = VERTEX_POINT ( 'NONE', #57489 ) ;
#7120 = ORIENTED_EDGE ( 'NONE', *, *, #49047, .F. ) ;
#7121 = VECTOR ( 'NONE', #81722, 1000.000000000000000 ) ;
#7122 = ORIENTED_EDGE ( 'NONE', *, *, #85011, .T. ) ;
#7123 = CARTESIAN_POINT ( 'NONE',  ( 107.3204973292724134, -25.70223992296343241, 71.04610146638795243 ) ) ;
#7124 = CARTESIAN_POINT ( 'NONE',  ( 50.87649884952499946, -33.54226604284930602, 342.9256252759119548 ) ) ;
#7125 = CYLINDRICAL_SURFACE ( 'NONE', #13762, 11.57110091390450179 ) ;
#7126 = CARTESIAN_POINT ( 'NONE',  ( 108.3715344132687051, -47.75189438633907457, 158.6822919425779617 ) ) ;
#7127 = DIRECTION ( 'NONE',  ( 0.000000000000000000, -1.000000000000000000, 0.000000000000000000 ) ) ;
#7128 = CARTESIAN_POINT ( 'NONE',  ( 110.0852322082900372, -46.03269033891531592, 12.82705384733995402 ) ) ;
#7129 = ORIENTED_EDGE ( 'NONE', *, *, #9959, .F. ) ;
#7131 = EDGE_CURVE ( 'NONE', #15176, #54672, #85227, .T. ) ;
#7130 = AXIS2_PLACEMENT_3D ( 'NONE', #2125, #319, #62987 ) ;
#7132 = VERTEX_POINT ( 'NONE', #50670 ) ;
#7133 = EDGE_LOOP ( 'NONE', ( #59269, #52202, #83808, #54745 ) ) ;
#7134 = LINE ( 'NONE', #49792, #75369 ) ;
#7135 = CARTESIAN_POINT ( 'NONE',  ( 25.56670390244744695, -48.82844715994178841, 173.2178068554150627 ) ) ;
#7136 = DIRECTION ( 'NONE',  ( 0.9242245927363033076, 0.3818493186865918876, 0.000000000000000000 ) ) ;
#7137 = CARTESIAN_POINT ( 'NONE',  ( 94.33669211993637305, 94.92443974548203300, 90.25311968877711877 ) ) ;
#7138 = ADVANCED_FACE ( 'NONE', ( #42060 ), #78411, .T. ) ;
#7139 = DIRECTION ( 'NONE',  ( -2.999999999999999839E-15, 1.000000000000000000, -2.999999999999999900E-30 ) ) ;
#7140 = EDGE_CURVE ( 'NONE', #68199, #3973, #46633, .T. ) ;
#7141 = DIRECTION ( 'NONE',  ( 0.000000000000000000, 1.000000000000000000, 0.000000000000000000 ) ) ;
#7142 = EDGE_CURVE ( 'NONE', #29714, #47593, #30709, .T. ) ;
#7143 = CARTESIAN_POINT ( 'NONE',  ( -12.04016146640379148, 86.59615096602188089, 129.9997639365609245 ) ) ;
#7144 = CARTESIAN_POINT ( 'NONE',  ( 97.12559377168363994, -39.79659400623925336, 21.56419670448195092 ) ) ;
#7145 = DIRECTION ( 'NONE',  ( 1.000000000000000000, 2.999999999999999839E-15, 1.000000000000000078E-15 ) ) ;
#7146 = ORIENTED_EDGE ( 'NONE', *, *, #86511, .T. ) ;
#7147 = CIRCLE ( 'NONE', #57903, 0.5000000000000079936 ) ;
#7148 = ADVANCED_FACE ( 'NONE', ( #49322 ), #69786, .T. ) ;
#7149 = DIRECTION ( 'NONE',  ( 1.000000000000000078E-15, -1.000000000000000083E-30, -1.000000000000000000 ) ) ;
#7150 = DIRECTION ( 'NONE',  ( 0.000000000000000000, 0.000000000000000000, -1.000000000000000000 ) ) ;
#7151 = CARTESIAN_POINT ( 'NONE',  ( 116.2870986197744969, -35.69205421237206366, 81.73380465530594563 ) ) ;
#7152 = CIRCLE ( 'NONE', #76784, 7.143750000000001599 ) ;
#7153 = AXIS2_PLACEMENT_3D ( 'NONE', #80907, #18656, #17765 ) ;
#7154 = EDGE_CURVE ( 'NONE', #38840, #14111, #13328, .T. ) ;
#7155 = CARTESIAN_POINT ( 'NONE',  ( -22.62762465138237644, 172.0000000000000000, 183.8826257785461280 ) ) ;
#7156 = EDGE_CURVE ( 'NONE', #38464, #33505, #29290, .T. ) ;
#7157 = CARTESIAN_POINT ( 'NONE',  ( 90.44969454456439450, -20.11243780205712639, 249.5838068554174924 ) ) ;
#7158 = VERTEX_POINT ( 'NONE', #24754 ) ;
#7159 = EDGE_LOOP ( 'NONE', ( #22491, #36896 ) ) ;
#7160 = VECTOR ( 'NONE', #57308, 999.9999999999998863 ) ;
#7161 = CARTESIAN_POINT ( 'NONE',  ( 79.32178306377458910, -34.08035908359609323, 8.141856907858651127 ) ) ;
#7162 = VERTEX_POINT ( 'NONE', #17500 ) ;
#7163 = CARTESIAN_POINT ( 'NONE',  ( 108.3661291232776023, -47.70624136733754028, 162.6822919425769669 ) ) ;
#7164 = ORIENTED_EDGE ( 'NONE', *, *, #70515, .T. ) ;
#7165 =( GEOMETRIC_REPRESENTATION_CONTEXT ( 3 ) GLOBAL_UNCERTAINTY_ASSIGNED_CONTEXT ( ( #28762 ) ) GLOBAL_UNIT_ASSIGNED_CONTEXT ( ( #3736, #71897, #44158 ) ) REPRESENTATION_CONTEXT ( 'NONE', 'WORKASPACE' ) );
#7166 = DIRECTION ( 'NONE',  ( 0.000000000000000000, -1.000000000000000000, 0.000000000000000000 ) ) ;
#7167 = CARTESIAN_POINT ( 'NONE',  ( 113.1640969444738971, -43.88191609279036243, 149.5825356868499512 ) ) ;
#7168 = DIRECTION ( 'NONE',  ( -1.054009200593500181E-15, -1.000000000000000000, 0.000000000000000000 ) ) ;
#7169 = AXIS2_PLACEMENT_3D ( 'NONE', #46950, #81965, #75588 ) ;
#7170 = CARTESIAN_POINT ( 'NONE',  ( 97.75304581901603740, -31.99688534799786765, 46.95276813305393659 ) ) ;
#7171 = LINE ( 'NONE', #63466, #86584 ) ;
#7172 = VERTEX_POINT ( 'NONE', #59700 ) ;
#7173 = CARTESIAN_POINT ( 'NONE',  ( -118.3034456680046702, 72.47328848629024378, -7.741103959107750399 ) ) ;
#7174 = VERTEX_POINT ( 'NONE', #18378 ) ;
#7175 = ORIENTED_EDGE ( 'NONE', *, *, #42821, .T. ) ;
#7176 = VECTOR ( 'NONE', #78493, 1000.000000000000000 ) ;
#7177 = DIRECTION ( 'NONE',  ( -1.000000000000000000, 0.000000000000000000, 0.000000000000000000 ) ) ;
#7178 = ORIENTED_EDGE ( 'NONE', *, *, #49138, .T. ) ;
#7179 = CARTESIAN_POINT ( 'NONE',  ( 98.44183741489689510, -42.05700530801252768, 11.76800622829193799 ) ) ;
#7180 = CARTESIAN_POINT ( 'NONE',  ( 114.5277216628477248, -29.41153075798395733, 145.4441967044819819 ) ) ;
#7181 = CARTESIAN_POINT ( 'NONE',  ( 97.81670390244700286, -67.87844715994096134, 222.2178068554179902 ) ) ;
#7182 = CARTESIAN_POINT ( 'NONE',  ( 116.7941748454729378, -39.39121522621098137, 129.6145142487127373 ) ) ;
#7183 = CARTESIAN_POINT ( 'NONE',  ( 108.9852221676114539, -46.97644323546262513, 78.72419670448194040 ) ) ;
#7184 = CARTESIAN_POINT ( 'NONE',  ( 109.6430121533087174, -46.48008672894804505, 262.7814586111080644 ) ) ;
#7185 = ORIENTED_EDGE ( 'NONE', *, *, #8377, .T. ) ;
#7186 = DIRECTION ( 'NONE',  ( 0.000000000000000000, 1.000000000000000000, 0.000000000000000000 ) ) ;
#7187 = DIRECTION ( 'NONE',  ( 0.000000000000000000, 0.000000000000000000, 1.000000000000000000 ) ) ;
#7188 = EDGE_CURVE ( 'NONE', #85115, #59657, #80062, .T. ) ;
#7190 = ORIENTED_EDGE ( 'NONE', *, *, #23703, .F. ) ;
#7189 = AXIS2_PLACEMENT_3D ( 'NONE', #25118, #11042, #19646 ) ;
#7191 = CARTESIAN_POINT ( 'NONE',  ( 0.000000000000000000, 50.79999999999999716, 265.5569999999999595 ) ) ;
#7192 = PLANE ( 'NONE',  #14544 ) ;
#7193 = CARTESIAN_POINT ( 'NONE',  ( 116.7701435943788653, -31.43623786049258584, 24.21181575210196257 ) ) ;
#7194 = CARTESIAN_POINT ( 'NONE',  ( 72.96458098368650269, 127.0000000000000000, 72.96458098368729850 ) ) ;
#7195 = CARTESIAN_POINT ( 'NONE',  ( 69.47395303589517823, 92.29081221604221241, 54.20185447853388894 ) ) ;
#7196 = CARTESIAN_POINT ( 'NONE',  ( 194.0667039024482108, -40.32844715993407192, 180.4678068554150343 ) ) ;
#7197 = CARTESIAN_POINT ( 'NONE',  ( 104.4155842956043614, -46.14412563975625403, 22.35848241876892217 ) ) ;
#7199 = CARTESIAN_POINT ( 'NONE',  ( 117.1424269838422987, -34.14023410701943817, 120.0270538473389479 ) ) ;
#7198 = CARTESIAN_POINT ( 'NONE',  ( 97.01979814536845481, -36.11691246787002285, 101.2783118708028098 ) ) ;
#7200 = CYLINDRICAL_SURFACE ( 'NONE', #47982, 2.500000000000002220 ) ;
#7201 = CARTESIAN_POINT ( 'NONE',  ( 114.8468557742592822, -29.67128889090990640, 209.4127681330539872 ) ) ;
#7202 = CARTESIAN_POINT ( 'NONE',  ( 129.7322073617410751, -147.4828892792592399, 72.80491793818269741 ) ) ;
#7203 = ORIENTED_EDGE ( 'NONE', *, *, #5664, .F. ) ;
#7204 = CARTESIAN_POINT ( 'NONE',  ( 172.5664832912740110, 0.2215528400590013880, 256.8086252759120498 ) ) ;
#7205 = AXIS2_PLACEMENT_3D ( 'NONE', #34611, #55477, #20554 ) ;
#7206 = LINE ( 'NONE', #76237, #21831 ) ;
#7207 = CARTESIAN_POINT ( 'NONE',  ( 162.8913605087219878, -31.76306994223740432, -5.074374724088000832 ) ) ;
#7208 = ORIENTED_EDGE ( 'NONE', *, *, #50630, .T. ) ;
#7209 = CIRCLE ( 'NONE', #49195, 0.5000000000000004441 ) ;
#7210 = DIRECTION ( 'NONE',  ( -1.000000000000000000, 0.000000000000000000, 0.000000000000000000 ) ) ;
#7212 = EDGE_LOOP ( 'NONE', ( #25505, #37112, #454, #32977 ) ) ;
#7211 = CARTESIAN_POINT ( 'NONE',  ( 106.9746081534954669, -47.19836424831742505, 187.5699109901969734 ) ) ;
#7213 = LINE ( 'NONE', #75358, #49456 ) ;
#7214 = CARTESIAN_POINT ( 'NONE',  ( 106.8511646352646380, -47.80368950967726249, 223.5489586092439538 ) ) ;
#7215 = CARTESIAN_POINT ( 'NONE',  ( 98.06260288352331145, 72.98383416765820186, 86.19129576945198323 ) ) ;
#7216 = LINE ( 'NONE', #34905, #72101 ) ;
#7218 = DIRECTION ( 'NONE',  ( 1.000000000000000000, 0.000000000000000000, 0.000000000000000000 ) ) ;
#7217 = CIRCLE ( 'NONE', #37689, 2.517500000000005844 ) ;
#7219 = ORIENTED_EDGE ( 'NONE', *, *, #66210, .T. ) ;
#7220 = AXIS2_PLACEMENT_3D ( 'NONE', #69280, #36558, #77890 ) ;
#7221 = EDGE_CURVE ( 'NONE', #43788, #6945, #30241, .T. ) ;
#7222 = ORIENTED_EDGE ( 'NONE', *, *, #56888, .T. ) ;
#7223 = ORIENTED_EDGE ( 'NONE', *, *, #30920, .T. ) ;
#7224 = VECTOR ( 'NONE', #79020, 1000.000000000000000 ) ;
#7225 = EDGE_LOOP ( 'NONE', ( #4998, #65786, #65384, #60754 ) ) ;
#7226 = DIRECTION ( 'NONE',  ( 0.000000000000000000, 1.000000000000000000, 0.000000000000000000 ) ) ;
#7227 = CARTESIAN_POINT ( 'NONE',  ( 118.0509465330791983, -35.49837129967784222, 229.9032443235299468 ) ) ;
#7228 = CARTESIAN_POINT ( 'NONE',  ( 72.96458098368650269, 117.4749999999999943, 72.96458098368729850 ) ) ;
#7229 = CARTESIAN_POINT ( 'NONE',  ( 107.0667039024470597, -133.7784471599409528, 25.71780685541800437 ) ) ;
#7230 = MECHANICAL_DESIGN_GEOMETRIC_PRESENTATION_REPRESENTATION (  '', ( #50720 ), #63772 ) ;
#7231 = CIRCLE ( 'NONE', #36209, 3.000000000000002665 ) ;
#7233 = DIRECTION ( 'NONE',  ( -0.7071067811865453523, -0.7071067811865496822, 0.000000000000000000 ) ) ;
#7232 = CARTESIAN_POINT ( 'NONE',  ( 162.0667039024469886, -68.87844715994089029, 222.2178068554179902 ) ) ;
#7234 = FACE_OUTER_BOUND ( 'NONE', #183, .T. ) ;
#7235 = CARTESIAN_POINT ( 'NONE',  ( 97.08353706812128792, -39.80957011747380392, 21.56419670448195092 ) ) ;
#7236 = ORIENTED_EDGE ( 'NONE', *, *, #33494, .T. ) ;
#7237 = ORIENTED_EDGE ( 'NONE', *, *, #47452, .T. ) ;
#7238 = CARTESIAN_POINT ( 'NONE',  ( 25.56670390244722313, -42.82844715994178131, 137.2178068554150627 ) ) ;
#7239 = CARTESIAN_POINT ( 'NONE',  ( 104.4910769649052895, -26.97849904278172417, 16.28477933405083178 ) ) ;
#7240 = CARTESIAN_POINT ( 'NONE',  ( 114.1395267584829014, -29.97404255306821241, 230.4327681330529742 ) ) ;
#7241 = EDGE_CURVE ( 'NONE', #65898, #53353, #87435, .T. ) ;
#7242 = AXIS2_PLACEMENT_3D ( 'NONE', #69203, #47839, #68756 ) ;
#7243 = DIRECTION ( 'NONE',  ( 0.000000000000000000, 0.000000000000000000, 1.000000000000000000 ) ) ;
#7244 = CARTESIAN_POINT ( 'NONE',  ( 97.28369645613172167, -37.51102008256656717, 97.38991099019594344 ) ) ;
#7245 = ADVANCED_FACE ( 'NONE', ( #79743, #72904 ), #52857, .F. ) ;
#7246 = CARTESIAN_POINT ( 'NONE',  ( -254.0000000000000000, 104.7749999999999915, 142.8750000000000000 ) ) ;
#7247 = EDGE_CURVE ( 'NONE', #28751, #45771, #17057, .T. ) ;
#7248 = CARTESIAN_POINT ( 'NONE',  ( -76.76533072354217779, 55.69843073979289727, 30.87393032424260753 ) ) ;
#7249 = ORIENTED_EDGE ( 'NONE', *, *, #89219, .F. ) ;
#7250 = DIRECTION ( 'NONE',  ( 1.000000000000000000, 0.000000000000000000, 0.000000000000000000 ) ) ;
#7251 = EDGE_CURVE ( 'NONE', #79223, #55335, #11116, .T. ) ;
#7252 = ORIENTED_EDGE ( 'NONE', *, *, #22626, .T. ) ;
#7253 = VERTEX_POINT ( 'NONE', #17934 ) ;
#7254 = LINE ( 'NONE', #76737, #64077 ) ;
#7255 = CARTESIAN_POINT ( 'NONE',  ( 97.87165577458247867, -34.79769342939158605, 257.6053928297065454 ) ) ;
#7256 = FACE_OUTER_BOUND ( 'NONE', #74119, .T. ) ;
#7257 = CARTESIAN_POINT ( 'NONE',  ( -117.9438598201574990, 86.63388195152280957, 12.03269986015488868 ) ) ;
#7258 = DIRECTION ( 'NONE',  ( -3.100000000000000258E-29, 3.100000000000000044E-14, 1.000000000000000000 ) ) ;
#7259 = ADVANCED_FACE ( 'NONE', ( #59264 ), #58811, .T. ) ;
#7260 = DIRECTION ( 'NONE',  ( -0.7071067811865462405, 0.000000000000000000, 0.7071067811865486830 ) ) ;
#7261 = EDGE_LOOP ( 'NONE', ( #38067, #49841, #8229, #77872 ) ) ;
#7262 = CIRCLE ( 'NONE', #29048, 11.57110091390434192 ) ;
#7263 = CARTESIAN_POINT ( 'NONE',  ( -123.4696824136392053, 101.5999999999999943, -179.8898777604655095 ) ) ;
#7264 = DIRECTION ( 'NONE',  ( 0.000000000000000000, 0.000000000000000000, -1.000000000000000000 ) ) ;
#7265 = EDGE_LOOP ( 'NONE', ( #54230, #18485, #1020 ) ) ;
#7266 = CARTESIAN_POINT ( 'NONE',  ( 96.83338659586634378, -38.89961736000394410, 31.49276813305495892 ) ) ;
#7267 = ORIENTED_EDGE ( 'NONE', *, *, #75622, .T. ) ;
#7268 = CARTESIAN_POINT ( 'NONE',  ( 114.5155466417691912, -41.88356374938643256, 12.77908649474396263 ) ) ;
#7269 = AXIS2_PLACEMENT_3D ( 'NONE', #35245, #42949, #69784 ) ;
#7270 = CARTESIAN_POINT ( 'NONE',  ( 168.5667039024482960, -48.82844715993516616, 180.4678068554150059 ) ) ;
#7271 = CARTESIAN_POINT ( 'NONE',  ( 98.33750497493203113, -41.21483588869663350, 196.7041967044829676 ) ) ;
#7272 = DIRECTION ( 'NONE',  ( -0.9999999999998281375, 0.000000000000000000, 5.861124988064729938E-07 ) ) ;
#7273 = DIRECTION ( 'NONE',  ( 0.000000000000000000, 0.000000000000000000, -1.000000000000000000 ) ) ;
#7274 = CARTESIAN_POINT ( 'NONE',  ( 41.56648329127398966, -27.82844715994070484, 78.92562527591199739 ) ) ;
#7275 = CARTESIAN_POINT ( 'NONE',  ( 172.5664832912729878, -27.82844715994070484, 15.92562527591200094 ) ) ;
#7276 = CARTESIAN_POINT ( 'NONE',  ( 115.4949314580552624, -29.50734498268579387, 225.4022919425769658 ) ) ;
#7277 = CARTESIAN_POINT ( 'NONE',  ( 77.01901799881285626, 91.23868085022587593, -90.13147184857885463 ) ) ;
#7278 = VECTOR ( 'NONE', #36907, 1000.000000000000000 ) ;
#7279 = ORIENTED_EDGE ( 'NONE', *, *, #556, .F. ) ;
#7280 = CARTESIAN_POINT ( 'NONE',  ( 136.5939002653012437, -37.81452881270037381, 7.047625865518532429 ) ) ;
#7281 = ORIENTED_EDGE ( 'NONE', *, *, #49359, .T. ) ;
#7282 = CARTESIAN_POINT ( 'NONE',  ( 116.6381559899473217, -29.65878987416117241, 105.3327681330539463 ) ) ;
#7283 = CARTESIAN_POINT ( 'NONE',  ( 119.5843592605237262, 52.19558960403061576, -52.38750000000002416 ) ) ;
#7284 = ORIENTED_EDGE ( 'NONE', *, *, #58792, .T. ) ;
#7285 = ORIENTED_EDGE ( 'NONE', *, *, #44170, .T. ) ;
#7286 = EDGE_LOOP ( 'NONE', ( #82988, #76591, #25242, #57925 ) ) ;
#7287 = AXIS2_PLACEMENT_3D ( 'NONE', #50048, #64597, #36451 ) ;
#7288 = CARTESIAN_POINT ( 'NONE',  ( 179.1667039024475230, -28.27351298636771659, 237.4678068554150059 ) ) ;
#7289 = DIRECTION ( 'NONE',  ( -4.237773401492740281E-14, 1.000000000000000000, 0.000000000000000000 ) ) ;
#7290 = FACE_OUTER_BOUND ( 'NONE', #87103, .T. ) ;
#7291 = AXIS2_PLACEMENT_3D ( 'NONE', #19497, #19051, #68101 ) ;
#7292 = DIRECTION ( 'NONE',  ( 0.000000000000000000, 1.000000000000000000, 0.000000000000000000 ) ) ;
#7293 = CARTESIAN_POINT ( 'NONE',  ( 3.174999999999879918, 124.5870000000000033, 33.98325472291465132 ) ) ;
#7294 = CARTESIAN_POINT ( 'NONE',  ( 113.2509217664418202, -31.40192927973085801, 182.2109475124489677 ) ) ;
#7295 = CARTESIAN_POINT ( 'NONE',  ( 116.6018303087422225, -42.36526137987677743, 279.4137205140061724 ) ) ;
#7296 = CARTESIAN_POINT ( 'NONE',  ( 97.86663541234594277, -40.64936128125661696, 57.64699884062476798 ) ) ;
#7297 = ORIENTED_EDGE ( 'NONE', *, *, #46817, .F. ) ;
#7298 = FACE_OUTER_BOUND ( 'NONE', #46385, .T. ) ;
#7299 = AXIS2_PLACEMENT_3D ( 'NONE', #68980, #21738, #13564 ) ;
#7300 = FACE_OUTER_BOUND ( 'NONE', #45974, .T. ) ;
#7301 = EDGE_CURVE ( 'NONE', #6408, #46574, #73798, .T. ) ;
#7302 = ORIENTED_EDGE ( 'NONE', *, *, #12341, .T. ) ;
#7303 = ORIENTED_EDGE ( 'NONE', *, *, #48623, .T. ) ;
#7304 = CARTESIAN_POINT ( 'NONE',  ( 172.5664832912728457, -18.82844715994071194, 21.92562527591192989 ) ) ;
#7305 = CYLINDRICAL_SURFACE ( 'NONE', #25410, 3.000000000000002665 ) ;
#7306 = ADVANCED_FACE ( 'NONE', ( #66074 ), #51548, .F. ) ;
#7307 = DIRECTION ( 'NONE',  ( 0.000000000000000000, 1.000000000000000000, 0.000000000000000000 ) ) ;
#7308 = DIRECTION ( 'NONE',  ( 0.000000000000000000, -1.000000000000000000, 0.000000000000000000 ) ) ;
#7309 = CIRCLE ( 'NONE', #36288, 2.030000000002079918 ) ;
#7310 = CARTESIAN_POINT ( 'NONE',  ( 99.85230398470191915, -41.30238370604462261, 186.1981341137909567 ) ) ;
#7311 = CARTESIAN_POINT ( 'NONE',  ( 98.55409819730274990, -43.85350384415066571, 71.86895860924397539 ) ) ;
#7312 = ORIENTED_EDGE ( 'NONE', *, *, #10778, .T. ) ;
#7313 = DIRECTION ( 'NONE',  ( -1.087812297297669405E-15, 1.000000000000000000, -3.100000000000000044E-14 ) ) ;
#7314 = ORIENTED_EDGE ( 'NONE', *, *, #77485, .F. ) ;
#7315 = CARTESIAN_POINT ( 'NONE',  ( -74.36911441044667015, 81.72118090664557144, -92.32962665258587265 ) ) ;
#7316 = ORIENTED_EDGE ( 'NONE', *, *, #84660, .F. ) ;
#7317 = DIRECTION ( 'NONE',  ( 1.821299053822143307E-16, 0.000000000000000000, -1.000000000000000000 ) ) ;
#7318 = ORIENTED_EDGE ( 'NONE', *, *, #75547, .T. ) ;
#7319 = LINE ( 'NONE', #69992, #34879 ) ;
#7320 = DIRECTION ( 'NONE',  ( -1.046082768126375896E-16, 0.000000000000000000, -1.000000000000000000 ) ) ;
#7321 = CARTESIAN_POINT ( 'NONE',  ( 113.1800950244601296, -44.75052191892536513, 274.0936886138787258 ) ) ;
#7322 = CIRCLE ( 'NONE', #50814, 15.69999999999999041 ) ;
#7323 = DIRECTION ( 'NONE',  ( -1.000000000000000000, 1.011922027653136551E-15, 0.000000000000000000 ) ) ;
#7324 = ORIENTED_EDGE ( 'NONE', *, *, #52668, .F. ) ;
#7325 = EDGE_CURVE ( 'NONE', #79308, #13477, #52422, .T. ) ;
#7326 = CARTESIAN_POINT ( 'NONE',  ( 96.31560519187928548, -41.77450771427546528, 61.67562527591097421 ) ) ;
#7328 = CARTESIAN_POINT ( 'NONE',  ( 118.5667039024470313, -104.2784471599411376, 17.71780685541799016 ) ) ;
#7327 = LINE ( 'NONE', #83192, #12981 ) ;
#7329 = DIRECTION ( 'NONE',  ( 2.900000000000000265E-14, -2.000000000000000155E-15, 1.000000000000000000 ) ) ;
#7330 = CARTESIAN_POINT ( 'NONE',  ( 134.0664832912739826, -15.97944715994100306, 1.625625275910997480 ) ) ;
#7331 = ORIENTED_EDGE ( 'NONE', *, *, #72210, .F. ) ;
#7332 = CIRCLE ( 'NONE', #85676, 2.749999999999974687 ) ;
#7333 = DIRECTION ( 'NONE',  ( -0.8543009526837940237, -0.03605348183280988883, 0.5185267868599396923 ) ) ;
#7334 = LINE ( 'NONE', #69112, #28369 ) ;
#7336 = DIRECTION ( 'NONE',  ( 1.000000000000000000, 4.163336342344333240E-14, 0.000000000000000000 ) ) ;
#7335 = VECTOR ( 'NONE', #54998, 1000.000000000000000 ) ;
#7337 = EDGE_LOOP ( 'NONE', ( #10568, #6933 ) ) ;
#7338 = CARTESIAN_POINT ( 'NONE',  ( 117.2433672581536968, -42.84935593481555571, 124.3956252759109731 ) ) ;
#7340 = CARTESIAN_POINT ( 'NONE',  ( 127.0664832912738262, -46.72944715994102438, 14.82207188531765318 ) ) ;
#7339 = CARTESIAN_POINT ( 'NONE',  ( 91.12500358871285755, -35.36225116344564157, 247.7440089327910755 ) ) ;
#7341 = DIRECTION ( 'NONE',  ( -1.000000000000000000, 8.775353200852647323E-16, 0.000000000000000000 ) ) ;
#7342 = CARTESIAN_POINT ( 'NONE',  ( 51.56670390244799762, -33.35206098992650681, -5.074374724088000832 ) ) ;
#7343 = CARTESIAN_POINT ( 'NONE',  ( 98.15811136316406760, -31.42099212808723863, 126.9108633711489915 ) ) ;
#7344 = AXIS2_PLACEMENT_3D ( 'NONE', #26384, #47254, #33200 ) ;
#7346 = ORIENTED_EDGE ( 'NONE', *, *, #52721, .T. ) ;
#7345 = CARTESIAN_POINT ( 'NONE',  ( 31.56670390244671509, -32.29483332968584364, 193.9678068554150911 ) ) ;
#7347 = CARTESIAN_POINT ( 'NONE',  ( 108.0121126588926046, -24.94157235513516468, 261.0127681330534415 ) ) ;
#7348 = FACE_OUTER_BOUND ( 'NONE', #61786, .T. ) ;
#7349 = DIRECTION ( 'NONE',  ( -0.7071067811866279529, 0.7071067811864671926, -7.071067811866286874E-16 ) ) ;
#7350 = CARTESIAN_POINT ( 'NONE',  ( 107.0664832912750057, -36.72944715993903486, 9.425625275910970657 ) ) ;
#7351 = EDGE_CURVE ( 'NONE', #36821, #75352, #80186, .T. ) ;
#7352 = LINE ( 'NONE', #62302, #21037 ) ;
#7353 = CARTESIAN_POINT ( 'NONE',  ( 67.17963690485876782, -137.3494469986182764, 246.8019061136969867 ) ) ;
#7354 = CARTESIAN_POINT ( 'NONE',  ( -88.25674559704555122, 71.15434825076368952, 96.20681132576139305 ) ) ;
#7355 = CARTESIAN_POINT ( 'NONE',  ( 99.57924082623969753, -30.38476633542323313, 215.7670538473399517 ) ) ;
#7356 = EDGE_LOOP ( 'NONE', ( #11026, #89700, #66603, #77445, #33510, #74262 ) ) ;
#7357 = ORIENTED_EDGE ( 'NONE', *, *, #76967, .F. ) ;
#7358 = CARTESIAN_POINT ( 'NONE',  ( 109.0885512386393259, -27.55405797182273631, 176.3234880678019465 ) ) ;
#7359 = CARTESIAN_POINT ( 'NONE',  ( -446.0240000000000009, 3.174999999999999822, -1.387778780781445991E-14 ) ) ;
#7360 = CARTESIAN_POINT ( 'NONE',  ( 113.3415799102510277, -29.55617248177381740, 285.5032443235294863 ) ) ;
#7361 = CARTESIAN_POINT ( 'NONE',  ( 63.06670390244799052, -40.32844715994017548, 249.9678068554150343 ) ) ;
#7362 = AXIS2_PLACEMENT_3D ( 'NONE', #20241, #35647, #69286 ) ;
#7363 = CARTESIAN_POINT ( 'NONE',  ( 109.6423509097492683, -46.48025314540840469, 267.7815664546420180 ) ) ;
#7364 = EDGE_CURVE ( 'NONE', #40724, #8960, #59535, .T. ) ;
#7365 = CARTESIAN_POINT ( 'NONE',  ( 68.53801554307449351, 127.0000000000000000, -74.15067561874229796 ) ) ;
#7366 = CIRCLE ( 'NONE', #68257, 11.45913725231036118 ) ;
#7367 = CARTESIAN_POINT ( 'NONE',  ( 1.166476076187854022E-15, 95.25000000000000000, -9.525000000000000355 ) ) ;
#7368 = DIRECTION ( 'NONE',  ( 0.000000000000000000, 0.000000000000000000, -1.000000000000000000 ) ) ;
#7369 = EDGE_CURVE ( 'NONE', #52825, #27442, #31113, .T. ) ;
#7370 = CARTESIAN_POINT ( 'NONE',  ( 118.7655994573051714, -38.45539276985795851, 223.7099109901969598 ) ) ;
#7371 = DIRECTION ( 'NONE',  ( 0.000000000000000000, 1.000000000000000000, 0.000000000000000000 ) ) ;
#7372 = ORIENTED_EDGE ( 'NONE', *, *, #4672, .F. ) ;
#7373 = ORIENTED_EDGE ( 'NONE', *, *, #87930, .F. ) ;
#7374 = CARTESIAN_POINT ( 'NONE',  ( 107.0709637938113445, -25.26751228799909299, 321.4478161181093583 ) ) ;
#7375 = CARTESIAN_POINT ( 'NONE',  ( 82.76600038373111090, -19.25405382162969303, 6.823682607504162334 ) ) ;
#7376 = DIRECTION ( 'NONE',  ( 1.000000000000000000, 4.510281037539788691E-14, 0.000000000000000000 ) ) ;
#7377 = CYLINDRICAL_SURFACE ( 'NONE', #36068, 2.749999999999974687 ) ;
#7378 = CIRCLE ( 'NONE', #56637, 4.762500000000002842 ) ;
#7379 = B_SPLINE_CURVE_WITH_KNOTS ( 'NONE', 3,
 ( #52273, #67731, #5519, #60913, #88641, #26397, #54070, #19578, #48602, #34091, #69081, #40471, #89078, #40911, #28174, #68188, #56318, #49508, #20039, #28633, #48161, #61795, #26836, #14116, #84065 ),
 .UNSPECIFIED., .F., .F.,
 ( 4, 2, 2, 2, 2, 2, 2, 2, 2, 1, 2, 2, 4 ),
 ( 0.05959919981814688211, 0.06208050401323544909, 0.06332115611077974993, 0.06456180820832406464, 0.06704311240341262468, 0.06828376450095689776, 0.06952441659850118472, 0.07200572079358977251, 0.07324637289113407335, 0.07448702498867838806, 0.07572767708622268890, 0.07696832918376700361, 0.07944963337885561916 ),
 .UNSPECIFIED. ) ;
#7380 = CARTESIAN_POINT ( 'NONE',  ( 97.81168895331838087, -40.51742574516882200, 287.6356252759109680 ) ) ;
#7381 = ORIENTED_EDGE ( 'NONE', *, *, #9709, .T. ) ;
#7382 = CARTESIAN_POINT ( 'NONE',  ( -1.640892575522350905, 95.07020838220610415, 118.3474229726581939 ) ) ;
#7383 = CARTESIAN_POINT ( 'NONE',  ( 96.26778515314977369, -34.36995442310919202, 256.1432443235300980 ) ) ;
#7384 = ORIENTED_EDGE ( 'NONE', *, *, #59975, .F. ) ;
#7385 = CARTESIAN_POINT ( 'NONE',  ( 77.72936414032395191, -38.17925173417307150, 7.255518600572461452 ) ) ;
#7386 = FACE_BOUND ( 'NONE', #7494, .T. ) ;
#7387 = LINE ( 'NONE', #27376, #23358 ) ;
#7388 = CARTESIAN_POINT ( 'NONE',  ( 107.2657893863845260, -28.07721033202879113, 72.86428084578200526 ) ) ;
#7389 = CARTESIAN_POINT ( 'NONE',  ( 108.0088980509730305, -26.32399177548269620, 151.0041967044829505 ) ) ;
#7390 = AXIS2_PLACEMENT_3D ( 'NONE', #33918, #70259, #36186 ) ;
#7391 = DIRECTION ( 'NONE',  ( 1.000000000000000078E-15, -1.000000000000000000, 0.000000000000000000 ) ) ;
#7392 = ORIENTED_EDGE ( 'NONE', *, *, #82329, .F. ) ;
#7393 = CARTESIAN_POINT ( 'NONE',  ( 142.8841478025725849, -84.11588139007200482, 542.9756252759101471 ) ) ;
#7394 = ORIENTED_EDGE ( 'NONE', *, *, #21957, .T. ) ;
#7396 = ORIENTED_EDGE ( 'NONE', *, *, #48538, .T. ) ;
#7395 = AXIS2_PLACEMENT_3D ( 'NONE', #64411, #42155, #77151 ) ;
#7397 = LINE ( 'NONE', #41447, #47346 ) ;
#7398 = ORIENTED_EDGE ( 'NONE', *, *, #74567, .T. ) ;
#7399 = ORIENTED_EDGE ( 'NONE', *, *, #80773, .T. ) ;
#7400 = DIRECTION ( 'NONE',  ( -0.000000000000000000, -0.000000000000000000, 1.000000000000000000 ) ) ;
#7401 = ADVANCED_FACE ( 'NONE', ( #45611 ), #66529, .T. ) ;
#7402 = CARTESIAN_POINT ( 'NONE',  ( 109.2109342822782168, -45.52796977871753370, 87.17718173283900285 ) ) ;
#7403 = CARTESIAN_POINT ( 'NONE',  ( 118.1050840190196567, -32.34957160481850025, 249.1270538473389706 ) ) ;
#7404 = CARTESIAN_POINT ( 'NONE',  ( 109.6005296801413351, -26.60309369064632534, 199.8813395616249977 ) ) ;
#7405 = CARTESIAN_POINT ( 'NONE',  ( 96.36089708107968477, -41.75325360632972149, 57.67562527591096710 ) ) ;
#7406 = CARTESIAN_POINT ( 'NONE',  ( 95.60734603896359829, -36.72944715994100306, 305.0306255462182321 ) ) ;
#7407 = CARTESIAN_POINT ( 'NONE',  ( -148.0533267522752112, 101.5999999999999943, 160.2664750769289697 ) ) ;
#7408 = CIRCLE ( 'NONE', #21952, 2.517500000000005844 ) ;
#7409 = ORIENTED_EDGE ( 'NONE', *, *, #86155, .F. ) ;
#7410 = CARTESIAN_POINT ( 'NONE',  ( 116.3212776292278363, -32.94146857470881429, 179.1356252759109395 ) ) ;
#7411 = DIRECTION ( 'NONE',  ( 0.000000000000000000, 1.000000000000000000, 0.000000000000000000 ) ) ;
#7412 = DIRECTION ( 'NONE',  ( -0.1811243269278930978, 0.9834602067165288952, 0.000000000000000000 ) ) ;
#7413 = CARTESIAN_POINT ( 'NONE',  ( 107.8912859324307334, -26.39220933555693094, 115.0251490854349612 ) ) ;
#7414 = CARTESIAN_POINT ( 'NONE',  ( 98.68712911129445331, -43.00583860492766064, 66.83848241876793850 ) ) ;
#7415 = CARTESIAN_POINT ( 'NONE',  ( 97.57529025620152652, -41.14803526195210992, 256.6727681330537507 ) ) ;
#7416 = ORIENTED_EDGE ( 'NONE', *, *, #44096, .F. ) ;
#7417 = EDGE_CURVE ( 'NONE', #29419, #49604, #85668, .T. ) ;
#7418 = CARTESIAN_POINT ( 'NONE',  ( 104.3243669996922307, -26.02151151870134171, 245.2880062282919482 ) ) ;
#7419 = CARTESIAN_POINT ( 'NONE',  ( -72.96458098368600531, 127.0000000000000000, -65.82083098368781293 ) ) ;
#7420 = CARTESIAN_POINT ( 'NONE',  ( 10.58784659601187350, 75.53659449424580430, 130.1259651751956312 ) ) ;
#7421 = DIRECTION ( 'NONE',  ( -1.000000000000000078E-15, 1.000000000000000000, -3.100000000000000044E-14 ) ) ;
#7423 = CARTESIAN_POINT ( 'NONE',  ( 68.69171528984767860, -139.3034585473416769, 245.6607614303540004 ) ) ;
#7422 = LINE ( 'NONE', #14697, #10002 ) ;
#7424 = CARTESIAN_POINT ( 'NONE',  ( 170.2205283966864897, 20.32000000000000028, 79.24800000000000466 ) ) ;
#7425 = CARTESIAN_POINT ( 'NONE',  ( 20.75871628398702384, 82.54999999999999716, 320.6630000000000109 ) ) ;
#7426 = CARTESIAN_POINT ( 'NONE',  ( 6.715083999775234069, 93.33742752469728998, -118.3661748111209420 ) ) ;
#7427 = EDGE_CURVE ( 'NONE', #75208, #22872, #16610, .T. ) ;
#7428 = AXIS2_PLACEMENT_3D ( 'NONE', #14154, #7341, #516 ) ;
#7429 = CARTESIAN_POINT ( 'NONE',  ( -10.09777173618929602, 90.29655250510948861, 130.1657284840295006 ) ) ;
#7430 = LINE ( 'NONE', #15602, #66256 ) ;
#7431 = EDGE_CURVE ( 'NONE', #3837, #27267, #34243, .T. ) ;
#7432 = LINE ( 'NONE', #22870, #17287 ) ;
#7434 = ORIENTED_EDGE ( 'NONE', *, *, #61383, .T. ) ;
#7433 = CARTESIAN_POINT ( 'NONE',  ( 105.7995184695716802, -26.72403496795282152, 260.1772919440113583 ) ) ;
#7435 = ADVANCED_FACE ( 'NONE', ( #48298 ), #41055, .T. ) ;
#7436 = FACE_OUTER_BOUND ( 'NONE', #36178, .T. ) ;
#7437 = CARTESIAN_POINT ( 'NONE',  ( 111.1360948925329808, -27.10735667079447353, 244.7584824187679544 ) ) ;
#7438 = CARTESIAN_POINT ( 'NONE',  ( 109.0722782120600840, -47.59916505968618594, 123.7337205140059666 ) ) ;
#7439 = CARTESIAN_POINT ( 'NONE',  ( 105.1596118751612323, -47.03031267540156080, 8.429910990196965770 ) ) ;
#7440 = DIRECTION ( 'NONE',  ( 0.7071067811865503483, 0.7071067811865445751, 0.000000000000000000 ) ) ;
#7441 = AXIS2_PLACEMENT_3D ( 'NONE', #48341, #13855, #10169 ) ;
#7443 = CARTESIAN_POINT ( 'NONE',  ( 81.91948822001464237, -34.69035895457181340, 7.660272404659449919 ) ) ;
#7442 = DIRECTION ( 'NONE',  ( -0.4999999999999998890, 0.000000000000000000, 0.8660254037844387076 ) ) ;
#7444 = CARTESIAN_POINT ( 'NONE',  ( 116.7951173353165188, -39.38786206668564915, 139.6147893462380409 ) ) ;
#7445 = EDGE_CURVE ( 'NONE', #32962, #84043, #7366, .T. ) ;
#7446 = CARTESIAN_POINT ( 'NONE',  ( -3.175000000000109956, 17.78000000000000114, -31.75000000000000000 ) ) ;
#7447 = ADVANCED_FACE ( 'NONE', ( #81536, #61947 ), #76032, .T. ) ;
#7448 = VERTEX_POINT ( 'NONE', #41494 ) ;
#7449 = DIRECTION ( 'NONE',  ( -3.100000000000000258E-29, 3.100000000000000044E-14, 1.000000000000000000 ) ) ;
#7450 = EDGE_LOOP ( 'NONE', ( #3584, #60194, #67290, #34318, #22309, #33034 ) ) ;
#7451 = CARTESIAN_POINT ( 'NONE',  ( 99.13191293290623207, -41.09468066504173578, 176.1371817328389966 ) ) ;
#7453 = ORIENTED_EDGE ( 'NONE', *, *, #30720, .T. ) ;
#7452 = FACE_OUTER_BOUND ( 'NONE', #33256, .T. ) ;
#7454 = CARTESIAN_POINT ( 'NONE',  ( 51.24204729617298426, -31.76306994223730840, 342.9256252759119548 ) ) ;
#7455 = CARTESIAN_POINT ( 'NONE',  ( 118.8928063919343145, -36.92768728534039013, 149.8127681330539644 ) ) ;
#7456 = DIRECTION ( 'NONE',  ( 0.7071067811566161820, 0.7071067812164789634, 0.000000000000000000 ) ) ;
#7457 = CARTESIAN_POINT ( 'NONE',  ( 172.5664832912740110, 0.2215528400590013880, 76.80862527591200717 ) ) ;
#7458 = EDGE_CURVE ( 'NONE', #37406, #65511, #13810, .T. ) ;
#7459 = CARTESIAN_POINT ( 'NONE',  ( 112.9729688188983658, -28.63767724599300735, 85.57429560595268470 ) ) ;
#7460 = AXIS2_PLACEMENT_3D ( 'NONE', #80213, #88814, #19761 ) ;
#7461 = CARTESIAN_POINT ( 'NONE',  ( 196.2150000000000034, 43.68799999999999528, 57.14999999999999858 ) ) ;
#7462 = FACE_OUTER_BOUND ( 'NONE', #34948, .T. ) ;
#7463 = CARTESIAN_POINT ( 'NONE',  ( 102.0418483691416469, -28.29933337693050532, 85.50419670448295051 ) ) ;
#7464 = VERTEX_POINT ( 'NONE', #54216 ) ;
#7465 = ORIENTED_EDGE ( 'NONE', *, *, #78125, .F. ) ;
#7467 = ORIENTED_EDGE ( 'NONE', *, *, #48631, .T. ) ;
#7466 = AXIS2_PLACEMENT_3D ( 'NONE', #4753, #60137, #67410 ) ;
#7468 = CARTESIAN_POINT ( 'NONE',  ( 102.0302726170450711, -29.40150668315268234, 46.98729759161196284 ) ) ;
#7469 = CARTESIAN_POINT ( 'NONE',  ( 134.5667039024471023, -105.9704134719595601, 250.2178068554179902 ) ) ;
#7471 = PLANE ( 'NONE',  #9953 ) ;
#7470 = CARTESIAN_POINT ( 'NONE',  ( 96.72778144249465981, -35.92320320382071230, 187.2765776568629406 ) ) ;
#7472 = DIRECTION ( 'NONE',  ( 0.000000000000000000, 1.000000000000000000, 0.000000000000000000 ) ) ;
#7473 = CARTESIAN_POINT ( 'NONE',  ( 131.0667039024480118, -61.87844715994100397, 225.9838068554150254 ) ) ;
#7474 = AXIS2_PLACEMENT_3D ( 'NONE', #77017, #14797, #62475 ) ;
#7475 = DIRECTION ( 'NONE',  ( 5.440892098500631367E-15, -1.000000000000000000, 3.100000000000000044E-14 ) ) ;
#7476 = EDGE_CURVE ( 'NONE', #74301, #28950, #103, .T. ) ;
#7477 = FACE_OUTER_BOUND ( 'NONE', #14553, .T. ) ;
#7478 = DIRECTION ( 'NONE',  ( 0.000000000000000000, 0.000000000000000000, -1.000000000000000000 ) ) ;
#7479 = EDGE_CURVE ( 'NONE', #75690, #32614, #68333, .T. ) ;
#7480 = CARTESIAN_POINT ( 'NONE',  ( 117.5589153096732105, -33.32758106675089493, 134.0880062282919880 ) ) ;
#7481 = ORIENTED_EDGE ( 'NONE', *, *, #39232, .F. ) ;
#7482 = ORIENTED_EDGE ( 'NONE', *, *, #50855, .F. ) ;
#7483 = AXIS2_PLACEMENT_3D ( 'NONE', #8442, #14363, #62935 ) ;
#7484 = ORIENTED_EDGE ( 'NONE', *, *, #10397, .T. ) ;
#7485 = EDGE_CURVE ( 'NONE', #81994, #84665, #6546, .T. ) ;
#7486 = DIRECTION ( 'NONE',  ( 0.000000000000000000, 0.000000000000000000, 1.000000000000000000 ) ) ;
#7487 = CARTESIAN_POINT ( 'NONE',  ( -100.8961411191535973, 120.6499999999999915, 3.968749999998880451 ) ) ;
#7488 = EDGE_CURVE ( 'NONE', #58627, #69807, #33804, .T. ) ;
#7489 = CARTESIAN_POINT ( 'NONE',  ( 152.0368932755773130, -23.42844715993587812, 129.9678068554149775 ) ) ;
#7490 = DIRECTION ( 'NONE',  ( 0.000000000000000000, -1.000000000000000000, 0.000000000000000000 ) ) ;
#7491 = CARTESIAN_POINT ( 'NONE',  ( 97.93802767643609286, -38.39294625876189571, 199.2880903695909751 ) ) ;
#7492 = LINE ( 'NONE', #27923, #62481 ) ;
#7493 = LINE ( 'NONE', #35178, #50384 ) ;
#7494 = EDGE_LOOP ( 'NONE', ( #6606, #75462 ) ) ;
#7496 = ORIENTED_EDGE ( 'NONE', *, *, #29183, .T. ) ;
#7495 = EDGE_LOOP ( 'NONE', ( #4885, #24710 ) ) ;
#7497 = AXIS2_PLACEMENT_3D ( 'NONE', #39813, #67535, #20737 ) ;
#7498 = CARTESIAN_POINT ( 'NONE',  ( 20.56670390244833158, -48.82844715994187368, 249.9678068554150059 ) ) ;
#7499 = EDGE_LOOP ( 'NONE', ( #88999, #5162 ) ) ;
#7500 = ORIENTED_EDGE ( 'NONE', *, *, #38690, .T. ) ;
#7501 = DIRECTION ( 'NONE',  ( 0.000000000000000000, 1.000000000000000000, 0.000000000000000000 ) ) ;
#7502 = CARTESIAN_POINT ( 'NONE',  ( 110.9273191204289191, -44.70580129652318391, 244.3672975916109635 ) ) ;
#7503 = CARTESIAN_POINT ( 'NONE',  ( 118.5256205435843526, -36.72944715994100306, 293.2242906452868851 ) ) ;
#7504 = ORIENTED_EDGE ( 'NONE', *, *, #24315, .T. ) ;
#7505 = VECTOR ( 'NONE', #9121, 1000.000000000000000 ) ;
#7506 = DIRECTION ( 'NONE',  ( -1.000000000000000078E-15, 1.000000000000000083E-30, 1.000000000000000000 ) ) ;
#7507 = CARTESIAN_POINT ( 'NONE',  ( -115.9581729443846143, 72.46394936478256454, 59.99146676500703990 ) ) ;
#7508 = ORIENTED_EDGE ( 'NONE', *, *, #20968, .T. ) ;
#7509 = VERTEX_POINT ( 'NONE', #4761 ) ;
#7510 = DIRECTION ( 'NONE',  ( 0.9963424814100663163, -0.08544974978097671925, 0.000000000000000000 ) ) ;
#7511 = ORIENTED_EDGE ( 'NONE', *, *, #32436, .F. ) ;
#7512 = ORIENTED_EDGE ( 'NONE', *, *, #19440, .F. ) ;
#7513 = CARTESIAN_POINT ( 'NONE',  ( 99.62303294566419254, -42.26939103296757594, 259.6538046553056915 ) ) ;
#7514 = CARTESIAN_POINT ( 'NONE',  ( 117.2437917682886592, -42.84961121563711828, 128.3956252759109873 ) ) ;
#7515 = CARTESIAN_POINT ( 'NONE',  ( 113.9719413768824694, -28.12837331961970122, 119.5261014663869474 ) ) ;
#7516 = CARTESIAN_POINT ( 'NONE',  ( 8.748570571408901218E-16, 117.4749999999999943, -96.04375000000000284 ) ) ;
#7517 = SURFACE_STYLE_FILL_AREA ( #21608 ) ;
#7518 = CARTESIAN_POINT ( 'NONE',  ( 107.2492351517315683, -24.88034519751278850, 226.0641967044829812 ) ) ;
#7519 = FACE_OUTER_BOUND ( 'NONE', #57138, .T. ) ;
#7520 = CARTESIAN_POINT ( 'NONE',  ( -98.60478223830740774, 127.0000000000000000, -1.074461880482445986E-12 ) ) ;
#7521 = ORIENTED_EDGE ( 'NONE', *, *, #25382, .F. ) ;
#7522 = CARTESIAN_POINT ( 'NONE',  ( 41.56648329127398966, -27.57844715994070484, 18.92562527591200094 ) ) ;
#7523 = ORIENTED_EDGE ( 'NONE', *, *, #85177, .F. ) ;
#7524 = VECTOR ( 'NONE', #52776, 1000.000000000000000 ) ;
#7525 = ORIENTED_EDGE ( 'NONE', *, *, #77993, .F. ) ;
#7526 = LINE ( 'NONE', #34778, #3992 ) ;
#7527 = CIRCLE ( 'NONE', #58290, 0.5000000000000004441 ) ;
#7528 = CARTESIAN_POINT ( 'NONE',  ( 103.2855693325404047, -27.47176340111613513, 136.3850188330253275 ) ) ;
#7529 = AXIS2_PLACEMENT_3D ( 'NONE', #73060, #10835, #87158 ) ;
#7530 = ORIENTED_EDGE ( 'NONE', *, *, #64647, .T. ) ;
#7531 = ADVANCED_FACE ( 'NONE', ( #54662 ), #75142, .T. ) ;
#7532 = CARTESIAN_POINT ( 'NONE',  ( 114.0810491752689160, -44.48971597834975000, 133.1613395616249989 ) ) ;
#7533 = DIRECTION ( 'NONE',  ( 0.000000000000000000, 0.000000000000000000, 1.000000000000000000 ) ) ;
#7534 = CARTESIAN_POINT ( 'NONE',  ( 68.86456684384336313, 353.0471713899363522, 56.22171674193015178 ) ) ;
#7535 = DIRECTION ( 'NONE',  ( 1.000000000000000000, 4.163336342344333240E-14, 0.000000000000000000 ) ) ;
#7536 = EDGE_CURVE ( 'NONE', #58062, #14741, #61498, .T. ) ;
#7539 = CARTESIAN_POINT ( 'NONE',  ( 110.8846227072671979, -27.01418920731900641, 265.7784824187680783 ) ) ;
#7538 = CARTESIAN_POINT ( 'NONE',  ( 114.7059021729713919, -43.25973416145915706, 58.26301525237845169 ) ) ;
#7537 = DIRECTION ( 'NONE',  ( 0.000000000000000000, 0.000000000000000000, -1.000000000000000000 ) ) ;
#7540 = CARTESIAN_POINT ( 'NONE',  ( 0.000000000000000000, 92.07499999999998863, 0.000000000000000000 ) ) ;
#7541 = CARTESIAN_POINT ( 'NONE',  ( -77.39114642430010349, 120.6499999999999915, 71.77848634863050847 ) ) ;
#7542 = ORIENTED_EDGE ( 'NONE', *, *, #47527, .T. ) ;
#7543 = CIRCLE ( 'NONE', #68429, 7.937500000000000000 ) ;
#7544 = DIRECTION ( 'NONE',  ( -1.000000000000000000, 0.000000000000000000, 2.820351377559424413E-14 ) ) ;
#7545 = ADVANCED_FACE ( 'NONE', ( #26102 ), #61056, .T. ) ;
#7546 = DIRECTION ( 'NONE',  ( 0.000000000000000000, 0.000000000000000000, -1.000000000000000000 ) ) ;
#7547 = CARTESIAN_POINT ( 'NONE',  ( -7.199374239792870816E-13, 117.4749999999999943, 98.14560000000000173 ) ) ;
#7548 = CIRCLE ( 'NONE', #19148, 9.810460662156732070 ) ;
#7549 = EDGE_CURVE ( 'NONE', #89358, #54421, #88786, .T. ) ;
#7550 = CARTESIAN_POINT ( 'NONE',  ( 146.5536166493005226, -137.3844657570545564, 246.8455049394716809 ) ) ;
#7552 = VERTEX_POINT ( 'NONE', #55111 ) ;
#7551 = CARTESIAN_POINT ( 'NONE',  ( 96.87130625142565066, -34.19761792387945576, 276.1327681330536734 ) ) ;
#7553 = ADVANCED_FACE ( 'NONE', ( #88342 ), #75601, .T. ) ;
#7554 = LINE ( 'NONE', #83866, #58229 ) ;
#7555 = CARTESIAN_POINT ( 'NONE',  ( 102.3026241189005532, -26.72939285866361914, 140.4422919425769578 ) ) ;
#7556 = CARTESIAN_POINT ( 'NONE',  ( 109.6429888323185224, -46.83113546657025950, 43.77562527591094721 ) ) ;
#7557 = CARTESIAN_POINT ( 'NONE',  ( 108.2828737166157964, -47.76209090725709672, 153.6518157521009584 ) ) ;
#7558 = PLANE ( 'NONE',  #9741 ) ;
#7559 = CARTESIAN_POINT ( 'NONE',  ( 97.81169951533574647, -40.51743117454552134, 102.6356342116286413 ) ) ;
#7561 = DIRECTION ( 'NONE',  ( 0.7071067811861589947, -0.7071067811869361508, 0.000000000000000000 ) ) ;
#7560 = DIRECTION ( 'NONE',  ( 0.000000000000000000, 1.000000000000000000, 0.000000000000000000 ) ) ;
#7562 = DIRECTION ( 'NONE',  ( 0.000000000000000000, 1.000000000000000000, 0.000000000000000000 ) ) ;
#7563 = DIRECTION ( 'NONE',  ( 0.000000000000000000, 1.000000000000000000, 0.000000000000000000 ) ) ;
#7564 = ORIENTED_EDGE ( 'NONE', *, *, #39208, .F. ) ;
#7565 = ADVANCED_FACE ( 'NONE', ( #26543 ), #46502, .F. ) ;
#7566 = CARTESIAN_POINT ( 'NONE',  ( 72.06648329127401098, -45.72944715994106701, 14.67562527591093513 ) ) ;
#7567 = ADVANCED_FACE ( 'NONE', ( #60145 ), #87880, .F. ) ;
#7568 = ORIENTED_EDGE ( 'NONE', *, *, #59083, .F. ) ;
#7569 = EDGE_LOOP ( 'NONE', ( #81110, #73297 ) ) ;
#7570 = ORIENTED_EDGE ( 'NONE', *, *, #13107, .T. ) ;
#7571 = CARTESIAN_POINT ( 'NONE',  ( 110.3472192523918238, -25.36789009815987228, 60.85276813305395649 ) ) ;
#7572 = LINE ( 'NONE', #83888, #41115 ) ;
#7573 = EDGE_CURVE ( 'NONE', #12738, #4589, #76938, .T. ) ;
#7574 = LINE ( 'NONE', #70695, #67441 ) ;
#7575 = CARTESIAN_POINT ( 'NONE',  ( 116.8472425118689841, -43.50793233799721094, 159.3441967044829539 ) ) ;
#7576 = AXIS2_PLACEMENT_3D ( 'NONE', #86311, #24088, #66746 ) ;
#7577 = CARTESIAN_POINT ( 'NONE',  ( 99.27767200979357654, -42.52643314540505060, 261.2581341137909590 ) ) ;
#7578 = ORIENTED_EDGE ( 'NONE', *, *, #75886, .F. ) ;
#7579 = VERTEX_POINT ( 'NONE', #178 ) ;
#7580 = ORIENTED_EDGE ( 'NONE', *, *, #8070, .T. ) ;
#7581 = AXIS2_PLACEMENT_3D ( 'NONE', #23924, #52902, #52032 ) ;
#7582 = ORIENTED_EDGE ( 'NONE', *, *, #69182, .T. ) ;
#7583 = CARTESIAN_POINT ( 'NONE',  ( 204.2160000000000082, 52.73749999999999716, -40.48124999999945572 ) ) ;
#7584 = CARTESIAN_POINT ( 'NONE',  ( 162.5667039024476139, -32.29483332967974718, 313.9678068554149490 ) ) ;
#7585 = CARTESIAN_POINT ( 'NONE',  ( 116.3183303039212291, -32.94226276200836878, 104.1356252759109680 ) ) ;
#7586 = DIRECTION ( 'NONE',  ( 0.000000000000000000, 0.000000000000000000, -1.000000000000000000 ) ) ;
#7587 = CARTESIAN_POINT ( 'NONE',  ( 100.8594679592200691, 83.38918798244691288, 82.89895571708403565 ) ) ;
#7588 = DIRECTION ( 'NONE',  ( 0.000000000000000000, 0.000000000000000000, -1.000000000000000000 ) ) ;
#7589 = CARTESIAN_POINT ( 'NONE',  ( 156.5667039024483529, -42.82844715993568485, 134.7178068554149775 ) ) ;
#7590 = CARTESIAN_POINT ( 'NONE',  ( 50.56670390244699576, -18.82844715994031048, -5.074374724088000832 ) ) ;
#7591 = CARTESIAN_POINT ( 'NONE',  ( 101.6204011159889831, -47.22657592904994317, 17.19562527591095247 ) ) ;
#7592 = CARTESIAN_POINT ( 'NONE',  ( 34.67381068360400320, -28.98061976758901892, -5.074374724088000832 ) ) ;
#7594 = ORIENTED_EDGE ( 'NONE', *, *, #51478, .T. ) ;
#7593 = CIRCLE ( 'NONE', #62694, 17.00000000000000000 ) ;
#7595 = ADVANCED_FACE ( 'NONE', ( #63301 ), #16059, .F. ) ;
#7596 = DIRECTION ( 'NONE',  ( 0.000000000000000000, -1.000000000000000000, 0.000000000000000000 ) ) ;
#7597 = EDGE_CURVE ( 'NONE', #35491, #78335, #53754, .T. ) ;
#7598 = DIRECTION ( 'NONE',  ( 0.000000000000000000, -1.000000000000000000, 0.000000000000000000 ) ) ;
#7599 = CARTESIAN_POINT ( 'NONE',  ( 98.91570299145236334, -37.17047609451836365, 74.18809036959095238 ) ) ;
#7600 = CIRCLE ( 'NONE', #68480, 50.79999999999999716 ) ;
#7601 = DIRECTION ( 'NONE',  ( 0.000000000000000000, 1.000000000000000000, 0.000000000000000000 ) ) ;
#7602 = VECTOR ( 'NONE', #28422, 1000.000000000000000 ) ;
#7603 = PLANE ( 'NONE',  #16947 ) ;
#7604 = EDGE_LOOP ( 'NONE', ( #54535, #24412, #47241, #75658 ) ) ;
#7605 = ORIENTED_EDGE ( 'NONE', *, *, #59367, .F. ) ;
#7606 = CARTESIAN_POINT ( 'NONE',  ( 77.71552635664649245, -35.29868341350233862, 7.242354772874388225 ) ) ;
#7607 = VERTEX_POINT ( 'NONE', #21988 ) ;
#7608 = ORIENTED_EDGE ( 'NONE', *, *, #45954, .F. ) ;
#7609 = LINE ( 'NONE', #6261, #43118 ) ;
#7610 = CARTESIAN_POINT ( 'NONE',  ( 97.38361328163530573, -33.95226689236985607, 137.5358690201829575 ) ) ;
#7611 = LINE ( 'NONE', #28039, #60528 ) ;
#7612 = CARTESIAN_POINT ( 'NONE',  ( 98.18387371117843543, -43.34642931133835475, 107.8480062282919647 ) ) ;
#7613 = CARTESIAN_POINT ( 'NONE',  ( 142.8841478025725849, -84.11588139007200482, 540.9756252759101471 ) ) ;
#7614 = ORIENTED_EDGE ( 'NONE', *, *, #58904, .T. ) ;
#7615 = CARTESIAN_POINT ( 'NONE',  ( 92.55667057654251551, -29.98664840991042269, 9.125625275910955736 ) ) ;
#7616 = VERTEX_POINT ( 'NONE', #15615 ) ;
#7617 = ORIENTED_EDGE ( 'NONE', *, *, #1493, .F. ) ;
#7619 = FACE_BOUND ( 'NONE', #67240, .T. ) ;
#7618 = VECTOR ( 'NONE', #29464, 1000.000000000000000 ) ;
#7620 = VERTEX_POINT ( 'NONE', #62843 ) ;
#7621 = CARTESIAN_POINT ( 'NONE',  ( 100.6111884388666766, -28.52632756463403751, 15.60705384733995871 ) ) ;
#7622 = CARTESIAN_POINT ( 'NONE',  ( 107.5668116379858787, -47.79447663526521239, 188.6003871806729535 ) ) ;
#7623 = CARTESIAN_POINT ( 'NONE',  ( 11.00664350276215941, 76.20047485311516766, -118.0441341279204721 ) ) ;
#7624 = DIRECTION ( 'NONE',  ( 0.7071067811865460184, 0.000000000000000000, -0.7071067811865489050 ) ) ;
#7625 = CARTESIAN_POINT ( 'NONE',  ( 96.02365317015762969, -37.20890873343472549, 112.3489586092449599 ) ) ;
#7626 = DIRECTION ( 'NONE',  ( 0.000000000000000000, 0.000000000000000000, 1.000000000000000000 ) ) ;
#7627 = EDGE_LOOP ( 'NONE', ( #78906, #19146, #10783, #85873 ) ) ;
#7628 = LINE ( 'NONE', #36228, #6115 ) ;
#7629 = LINE ( 'NONE', #57556, #37533 ) ;
#7631 = ORIENTED_EDGE ( 'NONE', *, *, #40285, .T. ) ;
#7630 = EDGE_CURVE ( 'NONE', #10930, #17773, #11553, .T. ) ;
#7632 = AXIS2_PLACEMENT_3D ( 'NONE', #19110, #14090, #7723 ) ;
#7633 = PLANE ( 'NONE',  #56164 ) ;
#7634 = CARTESIAN_POINT ( 'NONE',  ( 4.049525628232704122, 94.48868704156625142, 118.4874810299777437 ) ) ;
#7635 = CARTESIAN_POINT ( 'NONE',  ( 99.14341341762981585, -43.50528616620496791, 31.88991099019594699 ) ) ;
#7636 = CYLINDRICAL_SURFACE ( 'NONE', #44553, 3.500000000000003109 ) ;
#7637 = ADVANCED_FACE ( 'NONE', ( #22881 ), #42389, .F. ) ;
#7638 = DIRECTION ( 'NONE',  ( 0.000000000000000000, 0.000000000000000000, -1.000000000000000000 ) ) ;
#7639 = CARTESIAN_POINT ( 'NONE',  ( 156.5667039024483245, -42.82844715993568485, 173.2178068554149775 ) ) ;
#7640 = ADVANCED_FACE ( 'NONE', ( #57369 ), #49204, .F. ) ;
#7641 = CARTESIAN_POINT ( 'NONE',  ( 98.46141696562543189, -39.55439615822902510, 286.0133722090292849 ) ) ;
#7643 = CARTESIAN_POINT ( 'NONE',  ( 113.3016265961369697, -28.35762455946455773, 100.5670538473389684 ) ) ;
#7642 = CARTESIAN_POINT ( 'NONE',  ( 99.09540760583590213, -30.55081426086826113, 110.8023302363145461 ) ) ;
#7644 = DIRECTION ( 'NONE',  ( 0.000000000000000000, 0.000000000000000000, 1.000000000000000000 ) ) ;
#7645 = CARTESIAN_POINT ( 'NONE',  ( 108.4336792877692517, -20.78796745737986740, 293.6356252759109680 ) ) ;
#7646 = VERTEX_POINT ( 'NONE', #64207 ) ;
#7647 = CARTESIAN_POINT ( 'NONE',  ( -41.60202597009397607, 54.97499999999995879, 33.51824159735392783 ) ) ;
#7648 = EDGE_CURVE ( 'NONE', #83946, #1545, #1978, .T. ) ;
#7649 = FACE_BOUND ( 'NONE', #22946, .T. ) ;
#7650 = DIRECTION ( 'NONE',  ( -3.100000000000000258E-29, 3.100000000000000044E-14, 1.000000000000000000 ) ) ;
#7651 = EDGE_LOOP ( 'NONE', ( #4839, #67483, #36780, #19790 ) ) ;
#7652 = EDGE_CURVE ( 'NONE', #22487, #20369, #62399, .T. ) ;
#7653 = CARTESIAN_POINT ( 'NONE',  ( 270.8910000000000196, 65.43750000000000000, -2.032000000000000028 ) ) ;
#7655 = VERTEX_POINT ( 'NONE', #620 ) ;
#7654 = CARTESIAN_POINT ( 'NONE',  ( 117.8245512228195224, -33.99506276729055543, 169.0365776568629599 ) ) ;
#7656 = CARTESIAN_POINT ( 'NONE',  ( 162.7866693523289996, -36.02818131005891189, -5.074374724088000832 ) ) ;
#7657 = CARTESIAN_POINT ( 'NONE',  ( 117.2182995153958132, -34.26411022451439692, 205.0156252759109634 ) ) ;
#7658 = CARTESIAN_POINT ( 'NONE',  ( 96.14773132834588409, -38.72402830165600562, 47.48229194257797303 ) ) ;
#7659 = DIRECTION ( 'NONE',  ( 4.012088370409549976E-14, -1.000000000000000000, 0.000000000000000000 ) ) ;
#7660 = DIRECTION ( 'NONE',  ( 1.000000000000000078E-15, 0.000000000000000000, -1.000000000000000000 ) ) ;
#7661 = CARTESIAN_POINT ( 'NONE',  ( 109.6430121383572072, -46.48008673305788108, 77.78145860988261973 ) ) ;
#7662 = VERTEX_POINT ( 'NONE', #79187 ) ;
#7663 = EDGE_CURVE ( 'NONE', #48540, #38670, #5886, .T. ) ;
#7664 = ITEM_DEFINED_TRANSFORMATION ( 'NONE', 'NONE', #74002,  #50656 ) ;
#7665 = ORIENTED_EDGE ( 'NONE', *, *, #37483, .T. ) ;
#7666 = ADVANCED_FACE ( 'NONE', ( #37386 ), #79627, .F. ) ;
#7667 = ORIENTED_EDGE ( 'NONE', *, *, #29206, .F. ) ;
#7668 = VERTEX_POINT ( 'NONE', #59586 ) ;
#7669 = FACE_OUTER_BOUND ( 'NONE', #27591, .T. ) ;
#7670 = CARTESIAN_POINT ( 'NONE',  ( 99.53941477645811631, -29.46552450412116997, 246.7156252759109520 ) ) ;
#7671 = CARTESIAN_POINT ( 'NONE',  ( 143.0667039024470171, -83.77844715994091018, 55.21780685541800437 ) ) ;
#7672 = CARTESIAN_POINT ( 'NONE',  ( 50.88849390559378350, -32.11662333284569115, 117.4678068554150485 ) ) ;
#7673 = EDGE_CURVE ( 'NONE', #37315, #18895, #19107, .T. ) ;
#7675 = CARTESIAN_POINT ( 'NONE',  ( -12.70000000000000107, 82.54999999999999716, 129.9368274816650910 ) ) ;
#7674 = DIRECTION ( 'NONE',  ( -0.7071067811567173234, 0.7071067812163779331, 0.000000000000000000 ) ) ;
#7676 = CARTESIAN_POINT ( 'NONE',  ( 31.46648329127298993, 12.92155284005730387, 361.9756252759109998 ) ) ;
#7677 = CARTESIAN_POINT ( 'NONE',  ( 111.0547186471684995, -47.06334559972322751, 17.85753003781598380 ) ) ;
#7678 = VERTEX_POINT ( 'NONE', #2425 ) ;
#7679 = ORIENTED_EDGE ( 'NONE', *, *, #25926, .F. ) ;
#7680 = LINE ( 'NONE', #8588, #52810 ) ;
#7681 = PLANE ( 'NONE',  #27434 ) ;
#7682 = CARTESIAN_POINT ( 'NONE',  ( 112.0813997088635432, -45.80630777137064058, 248.9661014663869878 ) ) ;
#7683 = DIRECTION ( 'NONE',  ( 1.000000000000000078E-15, -1.000000000000000083E-30, -1.000000000000000000 ) ) ;
#7684 = VECTOR ( 'NONE', #4774, 1000.000000000000000 ) ;
#7685 = CARTESIAN_POINT ( 'NONE',  ( 104.3903674582245742, -25.93822912171390982, 86.26991099019598153 ) ) ;
#7686 = CARTESIAN_POINT ( 'NONE',  ( 99.04393567086002292, -42.84106820361873247, 31.84416257778224946 ) ) ;
#7687 = CARTESIAN_POINT ( 'NONE',  ( 103.2776430504499388, -27.47500554358347813, 21.38570024634822886 ) ) ;
#7688 = VERTEX_POINT ( 'NONE', #45070 ) ;
#7689 = DIRECTION ( 'NONE',  ( 0.000000000000000000, 0.6088800793514597132, 0.7932622825831063818 ) ) ;
#7690 = B_SPLINE_CURVE_WITH_KNOTS ( 'NONE', 3,
 ( #45426, #15974, #2343, #73143, #10926, #43654, #19082, #11828, #54468, #60858, #67227, #4114, #53116, #74948, #26349, #33609, #61306, #5465, #89025, #59508, #26783, #46766, #88143, #45867, #18185, #25450, #19987 ),
 .UNSPECIFIED., .F., .F.,
 ( 4, 2, 2, 2, 2, 2, 2, 2, 2, 2, 1, 1, 1, 2, 4 ),
 ( 0.000000000000000000, 0.06251142263352413297, 0.1250228452670482659, 0.1875342679005723989, 0.2500456905340965319, 0.3125571131676206371, 0.3750685358011447978, 0.4375799584346689031, 0.4688356697514310945, 0.4844635254098123567, 0.4922774532390031266, 0.4961844171535987891, 0.4981378991108966203, 0.4991146400895454804, 0.5000913810681943961 ),
 .UNSPECIFIED. ) ;
#7691 = ORIENTED_EDGE ( 'NONE', *, *, #66765, .F. ) ;
#7692 = ORIENTED_EDGE ( 'NONE', *, *, #7597, .F. ) ;
#7693 = EDGE_CURVE ( 'NONE', #67525, #4530, #4452, .T. ) ;
#7694 = PLANE ( 'NONE',  #29253 ) ;
#7695 = CARTESIAN_POINT ( 'NONE',  ( 114.6260888371869555, -31.15012018194425281, 255.7520594963732492 ) ) ;
#7696 = VECTOR ( 'NONE', #31389, 1000.000000000000000 ) ;
#7697 = CARTESIAN_POINT ( 'NONE',  ( 115.0372574805542740, -42.90846260123733913, 193.3022919391792698 ) ) ;
#7698 = CARTESIAN_POINT ( 'NONE',  ( 25.56670390244797275, -65.37844715994100397, 173.2178068554149775 ) ) ;
#7699 = CARTESIAN_POINT ( 'NONE',  ( 107.0667039024470313, -104.2784471599418197, -11.78219314458200984 ) ) ;
#7700 = CARTESIAN_POINT ( 'NONE',  ( 74.62312585591649849, 79.66685870724424490, -92.12448541806578817 ) ) ;
#7701 = ORIENTED_EDGE ( 'NONE', *, *, #61457, .F. ) ;
#7702 = DIRECTION ( 'NONE',  ( 0.000000000000000000, 0.000000000000000000, -1.000000000000000000 ) ) ;
#7703 = CARTESIAN_POINT ( 'NONE',  ( 109.6412978090997967, -46.48051820152372215, 183.7818762376771247 ) ) ;
#7704 = ORIENTED_EDGE ( 'NONE', *, *, #53723, .T. ) ;
#7705 = CARTESIAN_POINT ( 'NONE',  ( 112.8178475080015772, -27.29012000701139939, 49.62895860924498947 ) ) ;
#7706 = ORIENTED_EDGE ( 'NONE', *, *, #13742, .T. ) ;
#7707 = CARTESIAN_POINT ( 'NONE',  ( 98.56427472769081533, -33.61093641167653345, 20.45718173283900398 ) ) ;
#7708 = CARTESIAN_POINT ( 'NONE',  ( 172.5664832912729878, -27.82844715994070484, 198.9256252759119832 ) ) ;
#7709 = CARTESIAN_POINT ( 'NONE',  ( 108.5755967597531821, -27.06580334247533770, 189.9527681330539792 ) ) ;
#7710 = ADVANCED_FACE ( 'NONE', ( #44179 ), #9674, .F. ) ;
#7711 = CARTESIAN_POINT ( 'NONE',  ( -158.9822249764575020, 101.5999999999999943, 139.6999999999999886 ) ) ;
#7712 = DIRECTION ( 'NONE',  ( 1.000000000000000000, 4.163336342344333240E-14, 0.000000000000000000 ) ) ;
#7713 = CARTESIAN_POINT ( 'NONE',  ( 142.8679068202682458, 10.65431904611001634, 396.9756252759102040 ) ) ;
#7714 = LINE ( 'NONE', #30397, #14577 ) ;
#7715 = CARTESIAN_POINT ( 'NONE',  ( 116.2568870038579547, -41.81614494787783798, 259.4241967044827106 ) ) ;
#7716 = CARTESIAN_POINT ( 'NONE',  ( 99.36242816078741669, -43.15851294862928711, 116.8811511109068562 ) ) ;
#7717 = ORIENTED_EDGE ( 'NONE', *, *, #78008, .F. ) ;
#7719 = ADVANCED_FACE ( 'NONE', ( #52308 ), #16945, .T. ) ;
#7718 = AXIS2_PLACEMENT_3D ( 'NONE', #40812, #47167, #20393 ) ;
#7720 = CARTESIAN_POINT ( 'NONE',  ( 154.4532655810166091, -72.54279768053238797, 396.9756252759102040 ) ) ;
#7721 = VERTEX_POINT ( 'NONE', #72359 ) ;
#7722 = CARTESIAN_POINT ( 'NONE',  ( 98.29982688861167617, -42.45122269429050021, 97.78705384733993355 ) ) ;
#7723 = DIRECTION ( 'NONE',  ( 0.000000000000000000, 0.000000000000000000, -1.000000000000000000 ) ) ;
#7724 = CIRCLE ( 'NONE', #26582, 2.030000000001311644 ) ;
#7725 = ORIENTED_EDGE ( 'NONE', *, *, #42991, .F. ) ;
#7726 = LINE ( 'NONE', #79353, #73386 ) ;
#7727 = ORIENTED_EDGE ( 'NONE', *, *, #64673, .T. ) ;
#7728 = EDGE_LOOP ( 'NONE', ( #45921, #35994 ) ) ;
#7729 = AXIS2_PLACEMENT_3D ( 'NONE', #59864, #53026, #67142 ) ;
#7730 = CARTESIAN_POINT ( 'NONE',  ( -31.75000000000000000, 111.1250000000000000, 3.174999999999779998 ) ) ;
#7731 = LINE ( 'NONE', #8182, #68030 ) ;
#7732 = CARTESIAN_POINT ( 'NONE',  ( -41.60202597009397607, 54.97499999999995879, 50.85338361873603219 ) ) ;
#7733 = CARTESIAN_POINT ( 'NONE',  ( 33.98325472291465132, 24.56180297284579694, -3.174999999999999822 ) ) ;
#7734 = DIRECTION ( 'NONE',  ( 0.000000000000000000, 0.000000000000000000, 1.000000000000000000 ) ) ;
#7735 = CARTESIAN_POINT ( 'NONE',  ( 109.9953477121747767, -26.70153551007575388, 255.8499109901966051 ) ) ;
#7736 = CARTESIAN_POINT ( 'NONE',  ( 121.2862988949694483, -113.5675617909524817, -19.21044887263773049 ) ) ;
#7737 = ORIENTED_EDGE ( 'NONE', *, *, #34405, .F. ) ;
#7738 = CARTESIAN_POINT ( 'NONE',  ( 11.89015833661310850, 78.06809816022375514, 117.9583611672943277 ) ) ;
#7739 = DIRECTION ( 'NONE',  ( 1.000000000000000000, 0.000000000000000000, 0.000000000000000000 ) ) ;
#7740 = ORIENTED_EDGE ( 'NONE', *, *, #23144, .T. ) ;
#7741 = VERTEX_POINT ( 'NONE', #10126 ) ;
#7742 = CARTESIAN_POINT ( 'NONE',  ( 82.61444500289061921, -19.76411817600001442, 2.828498113172249528 ) ) ;
#7743 = AXIS2_PLACEMENT_3D ( 'NONE', #40152, #45176, #46957 ) ;
#7744 = FACE_OUTER_BOUND ( 'NONE', #86214, .T. ) ;
#7745 = CARTESIAN_POINT ( 'NONE',  ( 97.80400251452438454, -40.49860548021092654, 16.63400711711531699 ) ) ;
#7746 = ADVANCED_FACE ( 'NONE', ( #31444 ), #45502, .T. ) ;
#7747 = DIRECTION ( 'NONE',  ( 0.000000000000000000, 0.000000000000000000, 1.000000000000000000 ) ) ;
#7748 = CARTESIAN_POINT ( 'NONE',  ( 34.67381068360400320, -28.98061976758901892, -5.074374724088000832 ) ) ;
#7749 = EDGE_CURVE ( 'NONE', #44764, #75304, #38707, .T. ) ;
#7750 = CARTESIAN_POINT ( 'NONE',  ( 102.3821975904229333, -44.47993990548584975, 201.5543245899819738 ) ) ;
#7751 = CARTESIAN_POINT ( 'NONE',  ( 126.0950369046984747, 65.73012104574902992, 33.83669062937374861 ) ) ;
#7752 = CARTESIAN_POINT ( 'NONE',  ( 99.46959489307312197, -43.93319290153426238, 81.92991099019597812 ) ) ;
#7753 = ORIENTED_EDGE ( 'NONE', *, *, #14720, .T. ) ;
#7754 = CARTESIAN_POINT ( 'NONE',  ( 37.56670390244722313, -48.82844715994106366, 180.4678068554150911 ) ) ;
#7755 = VERTEX_POINT ( 'NONE', #12360 ) ;
#7756 = AXIS2_PLACEMENT_3D ( 'NONE', #36514, #22891, #50567 ) ;
#7757 = ADVANCED_FACE ( 'NONE', ( #60487 ), #6007, .F. ) ;
#7758 = CARTESIAN_POINT ( 'NONE',  ( 34.27482367531500529, -30.08671355700301575, -5.074374724088000832 ) ) ;
#7759 = ORIENTED_EDGE ( 'NONE', *, *, #54168, .F. ) ;
#7760 = CYLINDRICAL_SURFACE ( 'NONE', #66410, 34.13125000000000142 ) ;
#7761 = EDGE_CURVE ( 'NONE', #1197, #4589, #89117, .T. ) ;
#7762 = ORIENTED_EDGE ( 'NONE', *, *, #58424, .F. ) ;
#7763 = CARTESIAN_POINT ( 'NONE',  ( 107.0667039024470313, -104.2784471599421323, -21.78219314458201694 ) ) ;
#7764 = DIRECTION ( 'NONE',  ( 1.000000000000000078E-15, -1.000000000000000000, 0.000000000000000000 ) ) ;
#7765 = DIRECTION ( 'NONE',  ( 0.000000000000000000, 0.000000000000000000, 1.000000000000000000 ) ) ;
#7766 = AXIS2_PLACEMENT_3D ( 'NONE', #81248, #18092, #80792 ) ;
#7767 = LINE ( 'NONE', #63624, #1684 ) ;
#7768 = ORIENTED_EDGE ( 'NONE', *, *, #73671, .T. ) ;
#7769 = CARTESIAN_POINT ( 'NONE',  ( 103.5913855974186362, -46.58186107657011377, 57.30705384733997221 ) ) ;
#7770 = FILL_AREA_STYLE ('',( #49530 ) ) ;
#7772 = DIRECTION ( 'NONE',  ( 1.986798540846734824E-16, 0.000000000000000000, -1.000000000000000000 ) ) ;
#7771 = CARTESIAN_POINT ( 'NONE',  ( 107.0667039024479834, -48.82844715994099971, 160.9178068554150229 ) ) ;
#7773 = FACE_OUTER_BOUND ( 'NONE', #68488, .T. ) ;
#7774 = CARTESIAN_POINT ( 'NONE',  ( 133.3151098752327925, -16.05633243510672159, 1.690787911849395364 ) ) ;
#7775 = EDGE_LOOP ( 'NONE', ( #22072, #31962, #50120, #49364 ) ) ;
#7776 = EDGE_CURVE ( 'NONE', #47465, #51228, #45057, .T. ) ;
#7777 = DIRECTION ( 'NONE',  ( 1.000000000000000078E-15, -1.000000000000000083E-30, -1.000000000000000000 ) ) ;
#7778 = CARTESIAN_POINT ( 'NONE',  ( 116.3162492855249894, -32.94856389518969308, 154.1356252759109680 ) ) ;
#7779 = CARTESIAN_POINT ( 'NONE',  ( -127.5252020268932114, 101.5999999999999943, 177.0380000000000109 ) ) ;
#7780 = CARTESIAN_POINT ( 'NONE',  ( 96.00057345886969529, -37.20991081664785582, 112.3489586092449599 ) ) ;
#7782 = CARTESIAN_POINT ( 'NONE',  ( 172.5664832912729878, -18.82844715994071194, 138.9256252759119832 ) ) ;
#7781 = DIRECTION ( 'NONE',  ( -0.7071067811865462405, 0.000000000000000000, 0.7071067811865486830 ) ) ;
#7783 = LINE ( 'NONE', #35471, #74148 ) ;
#7784 = VECTOR ( 'NONE', #72011, 1000.000000000000000 ) ;
#7785 = EDGE_LOOP ( 'NONE', ( #7679, #59910, #42118, #48186 ) ) ;
#7786 = TOROIDAL_SURFACE ( 'NONE', #13553, 11.75000000000000000, 2.125000000000000000 ) ;
#7787 = CARTESIAN_POINT ( 'NONE',  ( 0.000000000000000000, 211.0000000000000000, 154.6557476874258441 ) ) ;
#7788 = CARTESIAN_POINT ( 'NONE',  ( 98.32242264099485851, -42.30440888850449710, 137.7661014663869992 ) ) ;
#7790 = ORIENTED_EDGE ( 'NONE', *, *, #88880, .F. ) ;
#7789 = DIRECTION ( 'NONE',  ( 0.000000000000000000, 0.000000000000000000, -1.000000000000000000 ) ) ;
#7791 = CARTESIAN_POINT ( 'NONE',  ( 96.55902551080276908, -40.08462249002850086, 277.5603871806729899 ) ) ;
#7792 = FACE_OUTER_BOUND ( 'NONE', #47351, .T. ) ;
#7793 = FACE_OUTER_BOUND ( 'NONE', #57939, .T. ) ;
#7794 = CARTESIAN_POINT ( 'NONE',  ( 89.44289600121240369, -83.08196156581377068, 250.2178068554179902 ) ) ;
#7795 = CARTESIAN_POINT ( 'NONE',  ( 180.1667039024476082, -26.71338133338667120, 193.9678068554150059 ) ) ;
#7796 = CARTESIAN_POINT ( 'NONE',  ( 31.78666935232975987, -36.02818131005922453, 313.9678068554150059 ) ) ;
#7797 = CYLINDRICAL_SURFACE ( 'NONE', #61656, 9.999999999999998224 ) ;
#7798 = CARTESIAN_POINT ( 'NONE',  ( 107.2322476904469966, -46.54200526979099095, 212.5899109901969837 ) ) ;
#7799 = ORIENTED_EDGE ( 'NONE', *, *, #61457, .T. ) ;
#7800 = VERTEX_POINT ( 'NONE', #67768 ) ;
#7801 = ADVANCED_FACE ( 'NONE', ( #4648 ), #33249, .T. ) ;
#7802 = CARTESIAN_POINT ( 'NONE',  ( 108.0961452412413166, -46.06846630830715128, 154.0834880678019374 ) ) ;
#7803 = CARTESIAN_POINT ( 'NONE',  ( -479.3614999999999782, 14.28750000000023945, 19.36139197104649767 ) ) ;
#7804 = CARTESIAN_POINT ( 'NONE',  ( 115.0635112019030686, -32.91162553226137533, 15.61301187732594364 ) ) ;
#7805 = AXIS2_PLACEMENT_3D ( 'NONE', #55343, #29018, #76713 ) ;
#7806 = CARTESIAN_POINT ( 'NONE',  ( 59.67079009362632291, -0.9310397146383332379, 542.9756252759101471 ) ) ;
#7807 = ADVANCED_FACE ( 'NONE', ( #20079 ), #47753, .F. ) ;
#7808 = DIRECTION ( 'NONE',  ( 0.000000000000000000, -1.000000000000000000, 0.000000000000000000 ) ) ;
#7809 = FACE_OUTER_BOUND ( 'NONE', #85300, .T. ) ;
#7810 = CIRCLE ( 'NONE', #541, 10.00000000000000888 ) ;
#7811 = CARTESIAN_POINT ( 'NONE',  ( 0.000000000000000000, 2.269999999999994245, -9.425000000000000711 ) ) ;
#7812 = CARTESIAN_POINT ( 'NONE',  ( 31.56670390244700641, -19.82844715994111340, 342.9256252759119548 ) ) ;
#7813 = CARTESIAN_POINT ( 'NONE',  ( 118.0279888096068390, -35.50094427011355691, 233.9032443235299752 ) ) ;
#7814 = CARTESIAN_POINT ( 'NONE',  ( 123.0664832912757163, -36.72944715993921960, -5.074374724089014244 ) ) ;
#7815 = ORIENTED_EDGE ( 'NONE', *, *, #81938, .T. ) ;
#7816 = ORIENTED_EDGE ( 'NONE', *, *, #69676, .T. ) ;
#7817 = LINE ( 'NONE', #14646, #41625 ) ;
#7818 = CARTESIAN_POINT ( 'NONE',  ( -75.69222284415457125, 88.91144712388911842, -91.24829632406229507 ) ) ;
#7819 = CARTESIAN_POINT ( 'NONE',  ( 97.83871787020589750, -40.58289724771079676, 122.6407992083991587 ) ) ;
#7820 = CARTESIAN_POINT ( 'NONE',  ( 151.0371591254575208, -24.42818131005592264, 193.9678068554149775 ) ) ;
#7821 = CARTESIAN_POINT ( 'NONE',  ( 100.4186822966650539, -43.90371905523895890, 42.98133956162492098 ) ) ;
#7822 = FACE_OUTER_BOUND ( 'NONE', #3521, .T. ) ;
#7823 = VERTEX_POINT ( 'NONE', #46848 ) ;
#7824 = EDGE_CURVE ( 'NONE', #56124, #22947, #87768, .T. ) ;
#7825 = CARTESIAN_POINT ( 'NONE',  ( 72.96458098368701428, 127.0000000000000000, -72.96458098368670164 ) ) ;
#7826 = CARTESIAN_POINT ( 'NONE',  ( 99.53925745938779812, -29.46537268684611632, 250.7156252759109520 ) ) ;
#7827 = ORIENTED_EDGE ( 'NONE', *, *, #14724, .F. ) ;
#7828 = CARTESIAN_POINT ( 'NONE',  ( 77.37801896924342770, -37.30949827216422676, 6.839365140900691031 ) ) ;
#7829 = DIRECTION ( 'NONE',  ( -0.04216478779797398074, 0.9991106698809455455, 0.000000000000000000 ) ) ;
#7830 = FACE_OUTER_BOUND ( 'NONE', #40384, .T. ) ;
#7831 = CARTESIAN_POINT ( 'NONE',  ( 104.6321197217979488, -45.03455396584281800, 60.15570941721099274 ) ) ;
#7832 = CARTESIAN_POINT ( 'NONE',  ( 107.6542194910912684, -47.14941140656445384, 148.6213395616249784 ) ) ;
#7833 = ORIENTED_CLOSED_SHELL ( 'NONE', *, #2450, .F. );
#7834 = CARTESIAN_POINT ( 'NONE',  ( 107.0667039024470313, -104.2784471599409528, 23.21780685541800082 ) ) ;
#7835 = EDGE_LOOP ( 'NONE', ( #49339, #29904 ) ) ;
#7836 = DIRECTION ( 'NONE',  ( -2.973811673103097665E-16, -0.000000000000000000, -1.000000000000000000 ) ) ;
#7837 = ORIENTED_EDGE ( 'NONE', *, *, #15525, .T. ) ;
#7838 = ORIENTED_EDGE ( 'NONE', *, *, #34373, .F. ) ;
#7839 = AXIS2_PLACEMENT_3D ( 'NONE', #67861, #26528, #35570 ) ;
#7840 = DIRECTION ( 'NONE',  ( 0.000000000000000000, 0.000000000000000000, -1.000000000000000000 ) ) ;
#7841 = VERTEX_POINT ( 'NONE', #80974 ) ;
#7842 = ORIENTED_EDGE ( 'NONE', *, *, #59061, .F. ) ;
#7843 = DIRECTION ( 'NONE',  ( 0.000000000000000000, 0.000000000000000000, 1.000000000000000000 ) ) ;
#7844 = AXIS2_PLACEMENT_3D ( 'NONE', #81164, #41904, #28748 ) ;
#7845 = LINE ( 'NONE', #53388, #88137 ) ;
#7846 = EDGE_CURVE ( 'NONE', #20236, #60890, #4519, .T. ) ;
#7847 = CARTESIAN_POINT ( 'NONE',  ( 99.00375160886646597, -32.60573182744733600, 95.38480078045697041 ) ) ;
#7848 = CARTESIAN_POINT ( 'NONE',  ( 100.1240125862563275, -44.53639691489608765, 266.9984824187678782 ) ) ;
#7849 = CARTESIAN_POINT ( 'NONE',  ( 117.9098725419245000, -34.70837513311212064, 203.9851490854349549 ) ) ;
#7850 = FACE_OUTER_BOUND ( 'NONE', #83657, .T. ) ;
#7851 = CARTESIAN_POINT ( 'NONE',  ( 113.1758862902701850, -44.75366746424991504, 94.09372177059972842 ) ) ;
#7852 = EDGE_CURVE ( 'NONE', #2949, #67327, #5950, .T. ) ;
#7853 = ORIENTED_EDGE ( 'NONE', *, *, #40241, .T. ) ;
#7854 = DIRECTION ( 'NONE',  ( 0.000000000000000000, 0.000000000000000000, -1.000000000000000000 ) ) ;
#7855 = CARTESIAN_POINT ( 'NONE',  ( 61.06670403655746782, -83.77844715994098124, 55.21780685541800437 ) ) ;
#7856 = CARTESIAN_POINT ( 'NONE',  ( 70.35947989645553946, -140.1803810602137617, 246.8545327174207387 ) ) ;
#7857 = CARTESIAN_POINT ( 'NONE',  ( 98.20106483660278229, -31.34956418181668880, 125.8803871806729546 ) ) ;
#7858 = CARTESIAN_POINT ( 'NONE',  ( 110.8102856614596021, -46.50649220725635757, 62.86705384733992474 ) ) ;
#7860 = AXIS2_PLACEMENT_3D ( 'NONE', #83022, #42987, #83453 ) ;
#7859 = CARTESIAN_POINT ( 'NONE',  ( 96.76538361991065074, -40.86468949728195099, 251.6422919425776001 ) ) ;
#7861 = VERTEX_POINT ( 'NONE', #26438 ) ;
#7862 = CARTESIAN_POINT ( 'NONE',  ( 116.0552987087602048, -42.01037774571695849, 238.4041967044829562 ) ) ;
#7863 = AXIS2_PLACEMENT_3D ( 'NONE', #22880, #56008, #35582 ) ;
#7864 = LINE ( 'NONE', #78277, #34134 ) ;
#7865 = AXIS2_PLACEMENT_3D ( 'NONE', #14892, #89858, #33964 ) ;
#7866 = PRESENTATION_STYLE_ASSIGNMENT (( #76915 ) ) ;
#7868 = DIRECTION ( 'NONE',  ( 0.000000000000000000, 0.000000000000000000, -1.000000000000000000 ) ) ;
#7867 = VECTOR ( 'NONE', #23528, 1000.000000000000000 ) ;
#7869 = LINE ( 'NONE', #69652, #12638 ) ;
#7871 = DIRECTION ( 'NONE',  ( 1.000000000000000000, 0.000000000000000000, 0.000000000000000000 ) ) ;
#7870 = DIRECTION ( 'NONE',  ( 0.000000000000000000, 0.000000000000000000, 1.000000000000000000 ) ) ;
#7872 = DIRECTION ( 'NONE',  ( 0.000000000000000000, 0.000000000000000000, -1.000000000000000000 ) ) ;
#7873 = CARTESIAN_POINT ( 'NONE',  ( 0.000000000000000000, 0.000000000000000000, 0.000000000000000000 ) ) ;
#7874 = CARTESIAN_POINT ( 'NONE',  ( 51.03742451361310373, -23.42844715994068849, 193.9678068554150911 ) ) ;
#7875 = ADVANCED_FACE ( 'NONE', ( #67308 ), #18269, .F. ) ;
#7876 = VECTOR ( 'NONE', #21171, 1000.000000000000000 ) ;
#7877 = DIRECTION ( 'NONE',  ( -1.000000000000000000, 0.000000000000000000, 0.000000000000000000 ) ) ;
#7878 = EDGE_CURVE ( 'NONE', #47474, #22206, #68226, .T. ) ;
#7879 = CARTESIAN_POINT ( 'NONE',  ( 109.7248659022256732, -27.00080517415949188, 10.86479194411551852 ) ) ;
#7880 = CARTESIAN_POINT ( 'NONE',  ( 92.91125933621933086, -94.95109689075242443, -19.26696060647628528 ) ) ;
#7882 = ORIENTED_EDGE ( 'NONE', *, *, #78459, .T. ) ;
#7881 = CARTESIAN_POINT ( 'NONE',  ( -3.968749999999935163, 120.6499999999999915, -100.8961411191535973 ) ) ;
#7883 = DIRECTION ( 'NONE',  ( 1.000000000000000000, 3.999999999999999995E-14, 1.000000000000000078E-15 ) ) ;
#7884 = CARTESIAN_POINT ( 'NONE',  ( 110.8247753047693749, -26.30972152642112150, 249.7889586092445882 ) ) ;
#7885 = CARTESIAN_POINT ( 'NONE',  ( 98.45631125714150755, -42.66967193002393088, 122.8070538473389490 ) ) ;
#7886 = CARTESIAN_POINT ( 'NONE',  ( 96.32186211137589282, -39.41937243639647903, 12.53372051400597442 ) ) ;
#7887 = DIRECTION ( 'NONE',  ( 1.327617956749546798E-15, -0.7071067811865555663, -0.7071067811865394681 ) ) ;
#7889 = CARTESIAN_POINT ( 'NONE',  ( 107.5667039024470313, -108.2470741265389620, -19.78219314458190681 ) ) ;
#7888 = DIRECTION ( 'NONE',  ( 1.000000000000000000, 4.299999999999999979E-14, 1.000000000000000078E-15 ) ) ;
#7890 = DIRECTION ( 'NONE',  ( 0.000000000000000000, 0.4999999999999995004, -0.8660254037844390407 ) ) ;
#7891 = EDGE_LOOP ( 'NONE', ( #32107, #84662, #32304, #2160 ) ) ;
#7892 = CARTESIAN_POINT ( 'NONE',  ( -3.968750000000770051, 120.6499999999999915, 105.4788588808462038 ) ) ;
#7893 = ORIENTED_EDGE ( 'NONE', *, *, #57603, .F. ) ;
#7894 = CARTESIAN_POINT ( 'NONE',  ( 100.1837753934783990, -31.62254652264567767, 180.2409912566479591 ) ) ;
#7896 = ORIENTED_EDGE ( 'NONE', *, *, #89251, .F. ) ;
#7895 = CARTESIAN_POINT ( 'NONE',  ( 91.91125933621933086, -101.0284471599423739, -21.78219314458213063 ) ) ;
#7897 = LINE ( 'NONE', #35596, #31580 ) ;
#7898 = CARTESIAN_POINT ( 'NONE',  ( 102.9221092647374149, -27.14930527916913050, 151.4013395616249511 ) ) ;
#7899 = CARTESIAN_POINT ( 'NONE',  ( 116.3159136950847170, -32.94903743517052419, 150.1356252759109680 ) ) ;
#7900 = CARTESIAN_POINT ( 'NONE',  ( 41.56670390244718050, -42.82844715994109208, 180.4678068554150911 ) ) ;
#7901 = CARTESIAN_POINT ( 'NONE',  ( 105.4788588808464027, 120.6499999999999915, 3.968750000000405009 ) ) ;
#7902 = CARTESIAN_POINT ( 'NONE',  ( -92.12462914090755817, 79.66725693986894896, 74.62294912200682973 ) ) ;
#7903 = CARTESIAN_POINT ( 'NONE',  ( 107.0667039024479834, -36.72944715994100306, 239.5838068554170093 ) ) ;
#7904 = AXIS2_PLACEMENT_3D ( 'NONE', #83592, #10723, #65256 ) ;
#7905 = CARTESIAN_POINT ( 'NONE',  ( 103.5129713284349720, -46.47169217660404428, 97.28610146638794731 ) ) ;
#7906 = ORIENTED_EDGE ( 'NONE', *, *, #78989, .F. ) ;
#7907 = ORIENTED_EDGE ( 'NONE', *, *, #35199, .F. ) ;
#7908 = VERTEX_POINT ( 'NONE', #11466 ) ;
#7909 = CIRCLE ( 'NONE', #81907, 3.500000000000003109 ) ;
#7910 = CARTESIAN_POINT ( 'NONE',  ( 97.81060075337646254, -38.34349919808700236, 42.88348806780201272 ) ) ;
#7911 = FACE_OUTER_BOUND ( 'NONE', #33733, .T. ) ;
#7913 = CARTESIAN_POINT ( 'NONE',  ( -44.45000000000000284, 50.79999999999999716, 206.3750000000000000 ) ) ;
#7912 = CARTESIAN_POINT ( 'NONE',  ( 98.02110346605356028, -41.80092515478911963, 177.7451490854339795 ) ) ;
#7914 = CIRCLE ( 'NONE', #42710, 4.000000000000002665 ) ;
#7915 = CARTESIAN_POINT ( 'NONE',  ( 163.0667039024468465, -32.29483332967940612, 193.9678068554149775 ) ) ;
#7917 = EDGE_CURVE ( 'NONE', #3897, #50079, #75033, .T. ) ;
#7916 = CYLINDRICAL_SURFACE ( 'NONE', #48017, 2.500000000000002220 ) ;
#7918 = DIRECTION ( 'NONE',  ( -1.000000000000000000, -1.541976423090496028E-15, 0.000000000000000000 ) ) ;
#7919 = CARTESIAN_POINT ( 'NONE',  ( 107.0664832912739541, -23.72944715994095688, 311.6343304127839815 ) ) ;
#7920 = CARTESIAN_POINT ( 'NONE',  ( 67.58630777427835312, -68.37784050924791757, 246.8383462433463933 ) ) ;
#7921 = CARTESIAN_POINT ( 'NONE',  ( 113.9719413768824694, -28.12837331961970122, 119.5261014663869474 ) ) ;
#7922 = ORIENTED_EDGE ( 'NONE', *, *, #1403, .F. ) ;
#7923 = VERTEX_POINT ( 'NONE', #6436 ) ;
#7924 = ORIENTED_EDGE ( 'NONE', *, *, #29692, .T. ) ;
#7925 = PRESENTATION_STYLE_ASSIGNMENT (( #70153 ) ) ;
#7926 = DIRECTION ( 'NONE',  ( 0.000000000000000000, 0.000000000000000000, -1.000000000000000000 ) ) ;
#7927 = CARTESIAN_POINT ( 'NONE',  ( 97.75843501427306137, -40.38501350233762821, 131.6242676007061903 ) ) ;
#7928 = CARTESIAN_POINT ( 'NONE',  ( 62.03742497533751532, -23.42844715994041849, 249.9678068554150343 ) ) ;
#7929 = CARTESIAN_POINT ( 'NONE',  ( 113.1326720373799617, -31.22635327163875374, 207.2309475124489495 ) ) ;
#7930 = EDGE_CURVE ( 'NONE', #67598, #66630, #40745, .T. ) ;
#7931 = AXIS2_PLACEMENT_3D ( 'NONE', #12359, #54551, #60947 ) ;
#7932 = DIRECTION ( 'NONE',  ( 0.7071067811865466846, -0.7071067811865483499, 7.071067811865460542E-16 ) ) ;
#7933 = VECTOR ( 'NONE', #18061, 1000.000000000000000 ) ;
#7934 = CIRCLE ( 'NONE', #58680, 4.500000000000003553 ) ;
#7935 = LINE ( 'NONE', #71078, #28610 ) ;
#7936 = EDGE_LOOP ( 'NONE', ( #35636, #71289 ) ) ;
#7938 = ORIENTED_EDGE ( 'NONE', *, *, #69390, .T. ) ;
#7937 = VERTEX_POINT ( 'NONE', #25533 ) ;
#7939 = CIRCLE ( 'NONE', #80504, 13.99999999999999822 ) ;
#7940 = CIRCLE ( 'NONE', #61613, 5.562600000000000655 ) ;
#7941 = DIRECTION ( 'NONE',  ( 0.2588190451025189631, 0.000000000000000000, 0.9659258262890688673 ) ) ;
#7942 = ORIENTED_EDGE ( 'NONE', *, *, #45195, .F. ) ;
#7943 = EDGE_LOOP ( 'NONE', ( #54308, #70249, #16013, #33847 ) ) ;
#7944 = CARTESIAN_POINT ( 'NONE',  ( 78.24498361945106240, -20.78962918510159952, 7.677444906559778737 ) ) ;
#7945 = CARTESIAN_POINT ( 'NONE',  ( 112.7895289397446561, -28.43984804668171051, 236.0272975916119549 ) ) ;
#7946 = EDGE_CURVE ( 'NONE', #88413, #88172, #88235, .T. ) ;
#7947 = CARTESIAN_POINT ( 'NONE',  ( 100.8874669139039355, -44.70022063263273537, 272.0522918462373241 ) ) ;
#7948 = ORIENTED_EDGE ( 'NONE', *, *, #75934, .T. ) ;
#7949 = CARTESIAN_POINT ( 'NONE',  ( 134.0664832912740110, -36.72944715994100306, -5.074374724089001809 ) ) ;
#7950 = CARTESIAN_POINT ( 'NONE',  ( -112.9545031557597099, 68.49197848692702451, 65.46872494430569134 ) ) ;
#7951 = ORIENTED_EDGE ( 'NONE', *, *, #3074, .T. ) ;
#7952 = EDGE_LOOP ( 'NONE', ( #65165, #34982, #21396 ) ) ;
#7953 = CARTESIAN_POINT ( 'NONE',  ( 45.66030316258350297, 82.54999999999999716, 346.9005000000000223 ) ) ;
#7954 = ORIENTED_EDGE ( 'NONE', *, *, #72453, .T. ) ;
#7955 = ORIENTED_EDGE ( 'NONE', *, *, #36671, .F. ) ;
#7956 = EDGE_CURVE ( 'NONE', #38989, #12332, #74142, .T. ) ;
#7957 = AXIS2_PLACEMENT_3D ( 'NONE', #75575, #53742, #61030 ) ;
#7958 = CARTESIAN_POINT ( 'NONE',  ( 113.8227294809096435, -41.31015272151215356, 271.1709475124484925 ) ) ;
#7959 = CARTESIAN_POINT ( 'NONE',  ( 102.6066768796756037, -46.86875521856975269, 132.2346728949579528 ) ) ;
#7960 = CARTESIAN_POINT ( 'NONE',  ( 117.3497117099304745, -32.73958051198272301, 94.10895860924395606 ) ) ;
#7961 = DIRECTION ( 'NONE',  ( -1.000000000000000000, -3.999999999999999995E-14, -1.000000000000000078E-15 ) ) ;
#7962 = SURFACE_SIDE_STYLE ('',( #7517 ) ) ;
#7963 = CARTESIAN_POINT ( 'NONE',  ( 112.4543492094282726, -45.69561878580546477, 234.0070538473389377 ) ) ;
#7964 = PLANE ( 'NONE',  #39959 ) ;
#7965 = EDGE_CURVE ( 'NONE', #80800, #50606, #32794, .T. ) ;
#7966 = PLANE ( 'NONE',  #65500 ) ;
#7967 = ORIENTED_EDGE ( 'NONE', *, *, #71001, .T. ) ;
#7968 = CARTESIAN_POINT ( 'NONE',  ( 46.48091746482041486, -48.32844715994088602, 180.4678068554150911 ) ) ;
#7969 = ORIENTED_EDGE ( 'NONE', *, *, #74224, .T. ) ;
#7970 = ORIENTED_EDGE ( 'NONE', *, *, #78837, .T. ) ;
#7971 = CARTESIAN_POINT ( 'NONE',  ( 19.89663890320305839, 44.45000000000000284, 32.49205688096009936 ) ) ;
#7972 = CIRCLE ( 'NONE', #84826, 3.000000000000002665 ) ;
#7973 = CARTESIAN_POINT ( 'NONE',  ( 50.56670390244699576, -18.82844715994031048, 342.9256252759119548 ) ) ;
#7974 = ORIENTED_EDGE ( 'NONE', *, *, #45300, .F. ) ;
#7975 = CARTESIAN_POINT ( 'NONE',  ( 109.0723201335305816, -47.59939223872296310, 127.7337205140059382 ) ) ;
#7976 = LINE ( 'NONE', #50645, #86287 ) ;
#7977 = VECTOR ( 'NONE', #8445, 1000.000000000000000 ) ;
#7978 = FACE_OUTER_BOUND ( 'NONE', #85148, .T. ) ;
#7979 = DIRECTION ( 'NONE',  ( 0.000000000000000000, 0.000000000000000000, 1.000000000000000000 ) ) ;
#7982 = CARTESIAN_POINT ( 'NONE',  ( 97.19046783542286505, -39.99946004141659017, 237.5813395616249579 ) ) ;
#7981 = CARTESIAN_POINT ( 'NONE',  ( 107.8260946937819398, -46.73210543769128833, 57.63636942760201265 ) ) ;
#7980 = CYLINDRICAL_SURFACE ( 'NONE', #47642, 3.000000000000002665 ) ;
#7983 = CARTESIAN_POINT ( 'NONE',  ( 106.6093434278972865, -26.33948225654953035, 321.1698005525342978 ) ) ;
#7984 = DIRECTION ( 'NONE',  ( 0.7071067811578790607, 0.7071067812152160847, 0.000000000000000000 ) ) ;
#7985 = CARTESIAN_POINT ( 'NONE',  ( 107.0664832912739541, -20.72944715994095333, 302.7856252759109452 ) ) ;
#7986 = EDGE_CURVE ( 'NONE', #82149, #45331, #69119, .T. ) ;
#7987 = FACE_OUTER_BOUND ( 'NONE', #48562, .T. ) ;
#7988 = EDGE_CURVE ( 'NONE', #30366, #80402, #56811, .T. ) ;
#7989 = DIRECTION ( 'NONE',  ( 0.000000000000000000, -1.000000000000000000, 0.000000000000000000 ) ) ;
#7990 = ADVANCED_FACE ( 'NONE', ( #14608 ), #56696, .F. ) ;
#7991 = DIRECTION ( 'NONE',  ( -0.7071067811865453523, -0.7071067811865496822, -7.071067811865460542E-16 ) ) ;
#7993 = ORIENTED_EDGE ( 'NONE', *, *, #82925, .F. ) ;
#7992 = CARTESIAN_POINT ( 'NONE',  ( 97.17500156396280886, -33.29969143728342829, 286.0613395616251751 ) ) ;
#7994 = PLANE ( 'NONE',  #50960 ) ;
#7995 = CARTESIAN_POINT ( 'NONE',  ( 117.2597117638302393, -39.02229875088008981, 148.6499109901969859 ) ) ;
#7996 = CARTESIAN_POINT ( 'NONE',  ( 112.7416762643710229, -27.24439759747685486, 50.65943479972101215 ) ) ;
#7997 = CARTESIAN_POINT ( 'NONE',  ( 96.00793635059680753, -35.77758691827158799, 182.2461014663869889 ) ) ;
#7998 = EDGE_CURVE ( 'NONE', #1864, #11319, #83651, .T. ) ;
#7999 = CARTESIAN_POINT ( 'NONE',  ( 98.34985881564388421, -31.65658497315240183, 31.90645862423135881 ) ) ;
#8000 = DIRECTION ( 'NONE',  ( 1.000000000000000000, 4.163336342344333240E-14, 0.000000000000000000 ) ) ;
#8002 = DIRECTION ( 'NONE',  ( 1.387778780781444492E-15, 0.000000000000000000, -1.000000000000000000 ) ) ;
#8001 = DIRECTION ( 'NONE',  ( -1.000000000000000000, 0.000000000000000000, 0.000000000000000000 ) ) ;
#8003 = DIRECTION ( 'NONE',  ( -0.9999999853157766072, -0.0001713722456150811827, 0.000000000000000000 ) ) ;
#8004 = LINE ( 'NONE', #22995, #29369 ) ;
#8005 = ORIENTED_EDGE ( 'NONE', *, *, #2744, .T. ) ;
#8006 = CARTESIAN_POINT ( 'NONE',  ( 128.0667039024480118, -58.72944715994110254, 10.91780685541499807 ) ) ;
#8007 = AXIS2_PLACEMENT_3D ( 'NONE', #52766, #74597, #81442 ) ;
#8008 = VECTOR ( 'NONE', #50898, 1000.000000000000000 ) ;
#8009 = AXIS2_PLACEMENT_3D ( 'NONE', #64340, #2111, #29821 ) ;
#8010 = CONICAL_SURFACE ( 'NONE', #28276, 24.50000000000000711, 0.7419472680059182590 ) ;
#8011 = VERTEX_POINT ( 'NONE', #64102 ) ;
#8012 = ORIENTED_EDGE ( 'NONE', *, *, #6719, .T. ) ;
#8014 = ORIENTED_EDGE ( 'NONE', *, *, #64355, .T. ) ;
#8013 = DIRECTION ( 'NONE',  ( -1.000000000000000000, 1.011922027653136551E-15, 0.000000000000000000 ) ) ;
#8015 = CARTESIAN_POINT ( 'NONE',  ( 117.0705705820183482, -32.08379757587637471, 55.16038718067301261 ) ) ;
#8016 = CARTESIAN_POINT ( 'NONE',  ( 70.06964507117767482, -140.6784471599286519, 245.5331643397809671 ) ) ;
#8017 = VECTOR ( 'NONE', #84742, 1000.000000000000000 ) ;
#8018 = DIRECTION ( 'NONE',  ( 1.000000000000000000, 0.000000000000000000, -1.821231995776179916E-16 ) ) ;
#8019 = CARTESIAN_POINT ( 'NONE',  ( 115.0729613760110084, -29.04219751930509119, 185.4232443235299570 ) ) ;
#8020 = CARTESIAN_POINT ( 'NONE',  ( 110.2835424219824034, -44.64187515646635518, 282.3067055423625789 ) ) ;
#8021 = ORIENTED_EDGE ( 'NONE', *, *, #81289, .F. ) ;
#8022 = EDGE_LOOP ( 'NONE', ( #54716, #83488, #2307, #18096 ) ) ;
#8023 = ORIENTED_EDGE ( 'NONE', *, *, #39509, .F. ) ;
#8024 = ORIENTED_EDGE ( 'NONE', *, *, #43855, .T. ) ;
#8025 = CARTESIAN_POINT ( 'NONE',  ( 101.9936209452192344, -45.44607154117929326, 107.1564586096423000 ) ) ;
#8026 = DIRECTION ( 'NONE',  ( 1.000000000000000000, 4.299999999999999979E-14, 1.000000000000000078E-15 ) ) ;
#8027 = LINE ( 'NONE', #76624, #17270 ) ;
#8028 = CARTESIAN_POINT ( 'NONE',  ( 107.0664832912739399, -36.72944715994095333, 290.1356252759106837 ) ) ;
#8029 = VECTOR ( 'NONE', #67867, 1000.000000000000000 ) ;
#8030 = CARTESIAN_POINT ( 'NONE',  ( 88.53717826876548713, 94.12569442554141119, 95.94886839522675359 ) ) ;
#8031 = DIRECTION ( 'NONE',  ( 0.000000000000000000, -1.000000000000000000, 0.000000000000000000 ) ) ;
#8032 = FACE_OUTER_BOUND ( 'NONE', #67940, .T. ) ;
#8033 = CARTESIAN_POINT ( 'NONE',  ( -11.02761275263880592, 88.85312730307458651, 130.0895250074965475 ) ) ;
#8034 = CARTESIAN_POINT ( 'NONE',  ( 117.3629797429381654, -38.21633193987523214, 28.71276813305395592 ) ) ;
#8035 = CARTESIAN_POINT ( 'NONE',  ( 97.81252181392954981, -40.51708140501057187, 272.6353344860016819 ) ) ;
#8036 = VERTEX_POINT ( 'NONE', #69565 ) ;
#8037 = CARTESIAN_POINT ( 'NONE',  ( 103.1875000000000000, 127.0000000000000000, 7.937500000000360600 ) ) ;
#8038 = CARTESIAN_POINT ( 'NONE',  ( 29.00000000000001421, 127.0000000000000000, 113.8826257785461280 ) ) ;
#8039 = CARTESIAN_POINT ( 'NONE',  ( 105.2602129278706400, -44.68979347096200883, 70.21666179816293152 ) ) ;
#8040 = CIRCLE ( 'NONE', #47177, 13.63963572536219715 ) ;
#8041 = EDGE_CURVE ( 'NONE', #82100, #70996, #35030, .T. ) ;
#8042 = VECTOR ( 'NONE', #10892, 1000.000000000000114 ) ;
#8043 = ADVANCED_FACE ( 'NONE', ( #27774 ), #43180, .F. ) ;
#8044 = CARTESIAN_POINT ( 'NONE',  ( 107.0667039024470313, -119.4690460831836276, -21.78219314458154798 ) ) ;
#8045 = DIRECTION ( 'NONE',  ( 0.000000000000000000, -1.000000000000000000, 0.000000000000000000 ) ) ;
#8046 = ORIENTED_EDGE ( 'NONE', *, *, #70831, .T. ) ;
#8047 = VERTEX_POINT ( 'NONE', #34585 ) ;
#8048 = ADVANCED_FACE ( 'NONE', ( #42283 ), #84559, .T. ) ;
#8049 = CARTESIAN_POINT ( 'NONE',  ( 115.0439452383992318, -109.4614598618342853, -19.78219314458184996 ) ) ;
#8050 = ORIENTED_EDGE ( 'NONE', *, *, #47623, .T. ) ;
#8051 = ORIENTED_EDGE ( 'NONE', *, *, #88668, .T. ) ;
#8052 = ADVANCED_FACE ( 'NONE', ( #1872, #55900 ), #48642, .T. ) ;
#8053 = CARTESIAN_POINT ( 'NONE',  ( 109.1422557193553047, -45.34451810791325954, 129.1958690201829825 ) ) ;
#8054 = EDGE_CURVE ( 'NONE', #69100, #19524, #62740, .T. ) ;
#8055 = CARTESIAN_POINT ( 'NONE',  ( -12.70000000000000462, 82.96441223327236969, 117.8738102209307641 ) ) ;
#8056 = CARTESIAN_POINT ( 'NONE',  ( 112.8137514937528891, -47.12132662887700008, 98.97848241876793907 ) ) ;
#8057 = EDGE_CURVE ( 'NONE', #66754, #75737, #56363, .T. ) ;
#8058 = DIRECTION ( 'NONE',  ( 0.000000000000000000, 0.000000000000000000, 1.000000000000000000 ) ) ;
#8059 = VECTOR ( 'NONE', #55363, 1000.000000000000000 ) ;
#8060 = ORIENTED_EDGE ( 'NONE', *, *, #4332, .F. ) ;
#8061 = VECTOR ( 'NONE', #37399, 1000.000000000000000 ) ;
#8062 = VECTOR ( 'NONE', #60624, 999.9999999999998863 ) ;
#8063 = EDGE_LOOP ( 'NONE', ( #15193, #69490, #36757, #22324 ) ) ;
#8064 = EDGE_LOOP ( 'NONE', ( #83886, #3320, #1150, #32681, #73638, #52637, #41775, #28996 ) ) ;
#8065 = EDGE_CURVE ( 'NONE', #24929, #40317, #75584, .T. ) ;
#8066 = CYLINDRICAL_SURFACE ( 'NONE', #84733, 2.116999999999993776 ) ;
#8067 = ORIENTED_EDGE ( 'NONE', *, *, #57062, .T. ) ;
#8068 = CARTESIAN_POINT ( 'NONE',  ( 111.2075918398242038, -27.22220237496667394, 284.7375300378162706 ) ) ;
#8069 = CARTESIAN_POINT ( 'NONE',  ( 97.40507707138063154, -42.14631300639911160, 177.7451490854349743 ) ) ;
#8070 = EDGE_CURVE ( 'NONE', #17172, #39484, #42723, .T. ) ;
#8071 = CARTESIAN_POINT ( 'NONE',  ( 12.70000000000000284, 81.72078997525719046, -117.8738102209307641 ) ) ;
#8072 = DIRECTION ( 'NONE',  ( -4.237773401492740281E-14, 1.000000000000000000, 0.000000000000000000 ) ) ;
#8073 = CARTESIAN_POINT ( 'NONE',  ( 101.5008874824296896, -27.91431070382771651, 106.5241967044819944 ) ) ;
#8074 = EDGE_CURVE ( 'NONE', #77506, #66460, #1428, .T. ) ;
#8075 = DIRECTION ( 'NONE',  ( -1.000000000000000000, 0.000000000000000000, -2.108231265501709878E-16 ) ) ;
#8076 = VERTEX_POINT ( 'NONE', #20530 ) ;
#8077 = AXIS2_PLACEMENT_3D ( 'NONE', #86892, #38283, #51019 ) ;
#8078 = LINE ( 'NONE', #27617, #67041 ) ;
#8079 = ORIENTED_EDGE ( 'NONE', *, *, #32049, .T. ) ;
#8080 = CARTESIAN_POINT ( 'NONE',  ( 194.5664832912739826, -18.82844715994099971, -5.074374724088000832 ) ) ;
#8081 = VECTOR ( 'NONE', #29575, 1000.000000000000000 ) ;
#8082 = EDGE_LOOP ( 'NONE', ( #47579, #58887, #32435, #23390 ) ) ;
#8083 = CARTESIAN_POINT ( 'NONE',  ( 107.0667039024470313, -104.2784471599420755, -19.78219314458201694 ) ) ;
#8084 = DIRECTION ( 'NONE',  ( -0.7071067811875165754, -0.7071067811855784591, -7.071067811875158601E-16 ) ) ;
#8085 = CARTESIAN_POINT ( 'NONE',  ( 111.0463177226254174, -47.04157800189014438, 17.85753003781598380 ) ) ;
#8086 = DIRECTION ( 'NONE',  ( 0.000000000000000000, 0.000000000000000000, -1.000000000000000000 ) ) ;
#8087 = AXIS2_PLACEMENT_3D ( 'NONE', #88225, #12353, #40044 ) ;
#8088 = DIRECTION ( 'NONE',  ( 0.000000000000000000, 0.000000000000000000, 1.000000000000000000 ) ) ;
#8089 = DIRECTION ( 'NONE',  ( 0.000000000000000000, 0.000000000000000000, -1.000000000000000000 ) ) ;
#8090 = CARTESIAN_POINT ( 'NONE',  ( 116.4719273984281784, -32.36179259691358823, 59.16038718067295576 ) ) ;
#8092 = CARTESIAN_POINT ( 'NONE',  ( 108.7397100058831256, -25.82697924850577920, 140.9432443235299672 ) ) ;
#8091 = FACE_OUTER_BOUND ( 'NONE', #31997, .T. ) ;
#8093 = CARTESIAN_POINT ( 'NONE',  ( -72.96458098368751166, 127.0000000000000000, 80.90208098368620426 ) ) ;
#8094 = DIRECTION ( 'NONE',  ( 0.000000000000000000, 1.000000000000000000, 0.000000000000000000 ) ) ;
#8095 = ORIENTED_EDGE ( 'NONE', *, *, #63519, .T. ) ;
#8096 = DIRECTION ( 'NONE',  ( 1.000000000000000000, 1.000000000000000078E-15, 0.000000000000000000 ) ) ;
#8097 = EDGE_CURVE ( 'NONE', #78413, #69399, #75927, .T. ) ;
#8098 = FACE_OUTER_BOUND ( 'NONE', #53166, .T. ) ;
#8099 = CARTESIAN_POINT ( 'NONE',  ( 0.000000000000000000, 82.54999999999999716, 206.3750000000000000 ) ) ;
#8100 = EDGE_CURVE ( 'NONE', #67885, #54402, #7783, .T. ) ;
#8101 = ORIENTED_EDGE ( 'NONE', *, *, #74307, .F. ) ;
#8102 = EDGE_CURVE ( 'NONE', #34909, #55155, #68317, .T. ) ;
#8103 = DIRECTION ( 'NONE',  ( 0.7071067811865525687, -0.7071067811865425767, 7.071067811865221912E-16 ) ) ;
#8105 = VERTEX_POINT ( 'NONE', #21421 ) ;
#8104 = CARTESIAN_POINT ( 'NONE',  ( 103.5274535807004384, -26.83869072616077744, 190.3499109901969746 ) ) ;
#8106 = PLANE ( 'NONE',  #27690 ) ;
#8107 = CARTESIAN_POINT ( 'NONE',  ( 97.38187162881654046, -40.64678755884852279, 202.6327681330539860 ) ) ;
#8108 = CARTESIAN_POINT ( 'NONE',  ( 113.5330014162060195, -28.49676089798827405, 75.54705384733995288 ) ) ;
#8109 = EDGE_CURVE ( 'NONE', #88572, #54506, #28209, .T. ) ;
#8110 = CARTESIAN_POINT ( 'NONE',  ( 94.33976020835903853, 70.17656663518266669, 90.24991642302124717 ) ) ;
#8111 = CARTESIAN_POINT ( 'NONE',  ( 196.2150000000000034, 37.33800000000000097, 50.79999999999999716 ) ) ;
#8112 = CARTESIAN_POINT ( 'NONE',  ( 46.48091746482126041, -48.32844715994084339, 300.4678068554150059 ) ) ;
#8113 = ORIENTED_EDGE ( 'NONE', *, *, #80354, .F. ) ;
#8114 = VECTOR ( 'NONE', #47016, 1000.000000000000000 ) ;
#8115 = ORIENTED_EDGE ( 'NONE', *, *, #6394, .T. ) ;
#8116 = ORIENTED_EDGE ( 'NONE', *, *, #43016, .F. ) ;
#8117 = ORIENTED_EDGE ( 'NONE', *, *, #62939, .T. ) ;
#8118 = CARTESIAN_POINT ( 'NONE',  ( 106.5667039024470313, -108.2470741265382799, 2.217806855418114065 ) ) ;
#8119 = CARTESIAN_POINT ( 'NONE',  ( 116.6057436952887372, -40.93480069938575383, 249.4956252759109532 ) ) ;
#8120 = CARTESIAN_POINT ( 'NONE',  ( 114.6444261855607891, -91.15344715994180547, -11.78219314458242550 ) ) ;
#8121 = FACE_OUTER_BOUND ( 'NONE', #86008, .T. ) ;
#8123 = DIRECTION ( 'NONE',  ( -0.9834602067153815907, -0.1811243269341220596, 0.000000000000000000 ) ) ;
#8122 = PLANE ( 'NONE',  #78712 ) ;
#8124 = PLANE ( 'NONE',  #73287 ) ;
#8125 = CARTESIAN_POINT ( 'NONE',  ( 111.1376129892989013, -47.03096861136451423, 22.88800622829195675 ) ) ;
#8126 = VERTEX_POINT ( 'NONE', #10469 ) ;
#8127 = VECTOR ( 'NONE', #52781, 1000.000000000000000 ) ;
#8128 = VERTEX_POINT ( 'NONE', #30468 ) ;
#8129 = AXIS2_PLACEMENT_3D ( 'NONE', #24557, #79537, #58177 ) ;
#8130 = AXIS2_PLACEMENT_3D ( 'NONE', #84126, #21447, #42304 ) ;
#8131 =( LENGTH_UNIT ( ) NAMED_UNIT ( * ) SI_UNIT ( .MILLI., .METRE. ) );
#8132 = VECTOR ( 'NONE', #24237, 1000.000000000000000 ) ;
#8133 = CARTESIAN_POINT ( 'NONE',  ( 109.7263425203086484, -27.00119676199070895, 15.86761370455112896 ) ) ;
#8134 = CARTESIAN_POINT ( 'NONE',  ( 96.93540839703301515, -34.51582869190843894, 252.1432443235293590 ) ) ;
#8135 = DIRECTION ( 'NONE',  ( -0.9825752044165969590, -0.1858654558159821002, 0.000000000000000000 ) ) ;
#8136 = B_SPLINE_CURVE_WITH_KNOTS ( 'NONE', 3,
 ( #79110, #17759, #52243, #37765, #16871, #16428, #72728, #44550, #44104, #38637, #51806, #9604, #10496, #52682, #3247, #80005, #71840, #3682, #37314, #58629, #45436, #80442, #73159, #31822, #18198 ),
 .UNSPECIFIED., .F., .F.,
 ( 4, 2, 2, 2, 2, 2, 2, 2, 2, 1, 2, 2, 4 ),
 ( 0.05960644416065473405, 0.06208808443815339029, 0.06332890457690272534, 0.06456972471565204652, 0.06705136499315070275, 0.06829218513190002393, 0.06953300527064934511, 0.07201464554814800134, 0.07325546568689735027, 0.07449628582564669921, 0.07573710596439604814, 0.07697792610314539707, 0.07945956638064405331 ),
 .UNSPECIFIED. ) ;
#8137 = CARTESIAN_POINT ( 'NONE',  ( 102.5967720069230893, -27.99243076246528261, 116.4527681330529703 ) ) ;
#8138 = DIRECTION ( 'NONE',  ( -1.000000000000000000, 0.000000000000000000, 9.299908063537909262E-17 ) ) ;
#8139 = CARTESIAN_POINT ( 'NONE',  ( -75.89055769641095139, 54.33720168335926815, 30.80247753283806844 ) ) ;
#8140 = ORIENTED_EDGE ( 'NONE', *, *, #47737, .F. ) ;
#8141 = CARTESIAN_POINT ( 'NONE',  ( 116.3214902495786873, -32.94210931476069248, 180.1356252759109680 ) ) ;
#8142 = VERTEX_POINT ( 'NONE', #31347 ) ;
#8143 = ORIENTED_EDGE ( 'NONE', *, *, #13308, .T. ) ;
#8144 = AXIS2_PLACEMENT_3D ( 'NONE', #28016, #40301, #33489 ) ;
#8145 = CARTESIAN_POINT ( 'NONE',  ( -75.00112839233693762, 87.03046781249436492, 91.81710919847719765 ) ) ;
#8146 = CARTESIAN_POINT ( 'NONE',  ( 101.2106992548341822, -44.07698544542078167, 268.4606309249448941 ) ) ;
#8147 = DIRECTION ( 'NONE',  ( -1.000000000000000000, 0.000000000000000000, 0.000000000000000000 ) ) ;
#8148 = CARTESIAN_POINT ( 'NONE',  ( 97.07206128885297858, -35.37854637286780957, 141.2189669822484461 ) ) ;
#8149 = CIRCLE ( 'NONE', #85071, 9.500000000000008882 ) ;
#8150 = EDGE_CURVE ( 'NONE', #86064, #29444, #34973, .T. ) ;
#8151 = EDGE_CURVE ( 'NONE', #46099, #2137, #71805, .T. ) ;
#8152 = CARTESIAN_POINT ( 'NONE',  ( 150.5667039024475571, -25.42844715993593852, 180.4678068554149775 ) ) ;
#8153 = CARTESIAN_POINT ( 'NONE',  ( 61.56670390244639890, -23.42844715994043270, 129.9678068554150911 ) ) ;
#8154 = ORIENTED_EDGE ( 'NONE', *, *, #53746, .T. ) ;
#8155 = DIRECTION ( 'NONE',  ( 0.000000000000000000, -0.5150380749100549327, -0.8571673007021118895 ) ) ;
#8156 = EDGE_CURVE ( 'NONE', #85809, #32010, #72702, .T. ) ;
#8157 = CARTESIAN_POINT ( 'NONE',  ( 83.06670390244801183, -42.21678055153920184, 231.5838068554169524 ) ) ;
#8158 = EDGE_LOOP ( 'NONE', ( #20110, #78432, #2029, #49660 ) ) ;
#8159 = CARTESIAN_POINT ( 'NONE',  ( 115.5739025235967716, -42.75529552070533867, 53.33562527591095659 ) ) ;
#8160 = ORIENTED_EDGE ( 'NONE', *, *, #46691, .F. ) ;
#8161 = CARTESIAN_POINT ( 'NONE',  ( 106.1481202089414637, -44.86820639808929201, 280.3052332267342877 ) ) ;
#8162 = EDGE_CURVE ( 'NONE', #61548, #88283, #17290, .T. ) ;
#8163 = CARTESIAN_POINT ( 'NONE',  ( 115.0383104642609311, -42.90711831593061731, 128.3024873213930448 ) ) ;
#8164 = CARTESIAN_POINT ( 'NONE',  ( 116.4020974974656042, -33.81230083437810663, 174.0670538473399347 ) ) ;
#8165 = DIRECTION ( 'NONE',  ( -0.7071067811869841124, 0.7071067811861110330, 0.000000000000000000 ) ) ;
#8166 = CYLINDRICAL_SURFACE ( 'NONE', #6731, 11.45913725231036118 ) ;
#8167 = CARTESIAN_POINT ( 'NONE',  ( -7.205548786489490269E-13, 127.0000000000000000, 103.1875000000000000 ) ) ;
#8168 = CARTESIAN_POINT ( 'NONE',  ( 68.91169813362903085, -69.55710376154327435, 247.4994584470433381 ) ) ;
#8169 = CARTESIAN_POINT ( 'NONE',  ( 104.5778203770529586, -26.56076746289640411, 281.2670538473396959 ) ) ;
#8170 = CARTESIAN_POINT ( 'NONE',  ( 79.21949419058893227, 93.55466788070661721, -88.20392011030149604 ) ) ;
#8171 = ADVANCED_FACE ( 'NONE', ( #2323 ), #38169, .F. ) ;
#8172 = ORIENTED_EDGE ( 'NONE', *, *, #31445, .T. ) ;
#8173 = CARTESIAN_POINT ( 'NONE',  ( 136.5307003794576133, -37.95069274174123564, 7.120636252910355957 ) ) ;
#8174 = ORIENTED_EDGE ( 'NONE', *, *, #74635, .F. ) ;
#8175 = CARTESIAN_POINT ( 'NONE',  ( 108.9928688995437653, -47.66043690685247469, 118.7032443235299723 ) ) ;
#8176 = CARTESIAN_POINT ( 'NONE',  ( 119.9517054789250210, 49.13249813668914356, -51.54132924209260835 ) ) ;
#8177 = VERTEX_POINT ( 'NONE', #79977 ) ;
#8178 = ORIENTED_EDGE ( 'NONE', *, *, #58478, .T. ) ;
#8179 = ORIENTED_EDGE ( 'NONE', *, *, #72960, .F. ) ;
#8180 = ADVANCED_FACE ( 'NONE', ( #66306 ), #37735, .F. ) ;
#8181 = DIRECTION ( 'NONE',  ( -0.9254794337955620787, -0.3787978585227822492, 0.000000000000000000 ) ) ;
#8182 = CARTESIAN_POINT ( 'NONE',  ( 52.06670390244699576, -67.87844715994100397, 55.21780685541800437 ) ) ;
#8183 = DIRECTION ( 'NONE',  ( 1.000000000000000000, 5.440892098500631367E-15, -1.376676550535195643E-28 ) ) ;
#8184 = FACE_OUTER_BOUND ( 'NONE', #30031, .T. ) ;
#8185 = CARTESIAN_POINT ( 'NONE',  ( 80.06648329127399677, -18.72944715994105991, -5.074374724089057764 ) ) ;
#8186 = CARTESIAN_POINT ( 'NONE',  ( 116.4744410436840383, -32.23804052137624865, 15.18133956162492915 ) ) ;
#8187 = EDGE_CURVE ( 'NONE', #53265, #24560, #86328, .T. ) ;
#8188 = CARTESIAN_POINT ( 'NONE',  ( 51.56670390244899238, -32.29483332968450782, -5.074374724088000832 ) ) ;
#8189 = ORIENTED_EDGE ( 'NONE', *, *, #75557, .F. ) ;
#8190 = CARTESIAN_POINT ( 'NONE',  ( 183.5150000000000148, 14.63749999999999929, -52.38749999999999574 ) ) ;
#8191 = VECTOR ( 'NONE', #30847, 1000.000000000000000 ) ;
#8192 = PLANE ( 'NONE',  #14251 ) ;
#8193 = VERTEX_POINT ( 'NONE', #24107 ) ;
#8195 = VERTEX_POINT ( 'NONE', #85896 ) ;
#8194 = EDGE_CURVE ( 'NONE', #77917, #85594, #65859, .T. ) ;
#8196 = VECTOR ( 'NONE', #66336, 1000.000000000000114 ) ;
#8197 = AXIS2_PLACEMENT_3D ( 'NONE', #83628, #62720, #15030 ) ;
#8198 = CARTESIAN_POINT ( 'NONE',  ( 82.60909586547545302, -19.77717416134804651, 2.822018739140870203 ) ) ;
#8199 = VECTOR ( 'NONE', #4239, 1000.000000000000114 ) ;
#8200 = LINE ( 'NONE', #84964, #9221 ) ;
#8201 = CARTESIAN_POINT ( 'NONE',  ( 188.5667039024479834, -62.87844715994099687, 173.2178068554149775 ) ) ;
#8202 = CIRCLE ( 'NONE', #24150, 13.16666666666669627 ) ;
#8203 = LINE ( 'NONE', #76340, #18711 ) ;
#8204 = DIRECTION ( 'NONE',  ( 0.000000000000000000, 0.000000000000000000, -1.000000000000000000 ) ) ;
#8205 = CARTESIAN_POINT ( 'NONE',  ( 111.2765704384832759, -44.16122339008717290, 212.4095626852199530 ) ) ;
#8206 = DIRECTION ( 'NONE',  ( -4.237773401492740281E-14, 1.000000000000000000, 0.000000000000000000 ) ) ;
#8207 = LINE ( 'NONE', #56781, #27702 ) ;
#8208 = CARTESIAN_POINT ( 'NONE',  ( 95.98894329157613470, -41.07880401750329469, 96.62419670448197451 ) ) ;
#8209 = ORIENTED_EDGE ( 'NONE', *, *, #23422, .T. ) ;
#8210 = LINE ( 'NONE', #64071, #11815 ) ;
#8211 = ORIENTED_EDGE ( 'NONE', *, *, #72869, .F. ) ;
#8212 = DIRECTION ( 'NONE',  ( 0.000000000000000000, -1.000000000000000000, 0.000000000000000000 ) ) ;
#8213 = VERTEX_POINT ( 'NONE', #23668 ) ;
#8214 = B_SPLINE_CURVE_WITH_KNOTS ( 'NONE', 3,
 ( #4334, #19302, #12040, #46973, #25659, #81106, #17947, #18852, #19747, #47430, #74710, #61510, #59719, #46535, #74271, #52441, #39727, #5226 ),
 .UNSPECIFIED., .F., .F.,
 ( 4, 2, 2, 2, 2, 2, 2, 2, 4 ),
 ( 0.000000000000000000, 0.06249999998159491699, 0.1249999999631898340, 0.1874999999447847510, 0.2499999999263796679, 0.3124999999079746127, 0.3749999998895695019, 0.4374999998711643912, 0.4999999998527593359 ),
 .UNSPECIFIED. ) ;
#8215 = CARTESIAN_POINT ( 'NONE',  ( 19.56670390244796920, -48.82844715994099971, 10.91780685541479734 ) ) ;
#8216 = ORIENTED_EDGE ( 'NONE', *, *, #16078, .T. ) ;
#8217 = DIRECTION ( 'NONE',  ( 1.000000000000000000, 0.000000000000000000, 9.351236661543306751E-17 ) ) ;
#8218 = EDGE_CURVE ( 'NONE', #6713, #29287, #3094, .T. ) ;
#8219 = CARTESIAN_POINT ( 'NONE',  ( 67.06670390244707392, -137.6779871412748832, 245.9128651760420041 ) ) ;
#8220 = AXIS2_PLACEMENT_3D ( 'NONE', #28271, #88740, #14673 ) ;
#8221 = CARTESIAN_POINT ( 'NONE',  ( 131.0667039024480118, -58.72944715994097464, 228.3338068554150198 ) ) ;
#8222 = ORIENTED_EDGE ( 'NONE', *, *, #27745, .F. ) ;
#8223 = CARTESIAN_POINT ( 'NONE',  ( 115.1840797895677611, -43.30599572718466561, 88.28419670448195689 ) ) ;
#8224 = PRESENTATION_STYLE_ASSIGNMENT (( #77716 ) ) ;
#8226 = LINE ( 'NONE', #15038, #42795 ) ;
#8225 = CARTESIAN_POINT ( 'NONE',  ( 104.4893447449655923, -26.97897155733640417, 165.2815092204904772 ) ) ;
#8227 = CARTESIAN_POINT ( 'NONE',  ( 191.6375511031394865, 22.69262065192448574, 328.6381252759109088 ) ) ;
#8228 = CARTESIAN_POINT ( 'NONE',  ( 115.0372574993704404, -42.90846257614333581, 143.3022919416527827 ) ) ;
#8229 = ORIENTED_EDGE ( 'NONE', *, *, #9209, .T. ) ;
#8230 = CARTESIAN_POINT ( 'NONE',  ( -47.82553099389205187, 100.8041302358256814, 75.75399279458846991 ) ) ;
#8231 = DIRECTION ( 'NONE',  ( 0.000000000000000000, 0.000000000000000000, -1.000000000000000000 ) ) ;
#8232 = DIRECTION ( 'NONE',  ( 1.000000000000000000, 0.000000000000000000, 0.000000000000000000 ) ) ;
#8233 = EDGE_CURVE ( 'NONE', #1069, #34489, #65457, .T. ) ;
#8234 = CARTESIAN_POINT ( 'NONE',  ( 95.46382812221506242, -34.19949780945433560, 102.1556252759109640 ) ) ;
#8236 = CARTESIAN_POINT ( 'NONE',  ( 127.0664832912740110, -46.72944715994101017, 14.67562527591099197 ) ) ;
#8235 = FACE_OUTER_BOUND ( 'NONE', #52359, .T. ) ;
#8237 = CARTESIAN_POINT ( 'NONE',  ( 72.96458098368650269, 127.0000000000000000, 72.96458098368729850 ) ) ;
#8238 = ADVANCED_FACE ( 'NONE', ( #59039 ), #85459, .F. ) ;
#8239 = EDGE_LOOP ( 'NONE', ( #55078, #23976, #21834, #58747 ) ) ;
#8240 = DIRECTION ( 'NONE',  ( 0.000000000000000000, 0.000000000000000000, 1.000000000000000000 ) ) ;
#8241 = CARTESIAN_POINT ( 'NONE',  ( 116.6093774848465472, -38.87601340171671893, 144.6499109901959628 ) ) ;
#8243 = ORIENTED_EDGE ( 'NONE', *, *, #53674, .F. ) ;
#8242 = DIRECTION ( 'NONE',  ( 9.030537910253610117E-13, -1.000000000000000000, 9.040537910253610592E-28 ) ) ;
#8244 = CARTESIAN_POINT ( 'NONE',  ( 109.4546162266722575, -25.87086512622489920, 25.90419670448196143 ) ) ;
#8245 = CARTESIAN_POINT ( 'NONE',  ( 194.0667039024473581, -24.92844715993408045, 249.9678068554149775 ) ) ;
#8246 = DIRECTION ( 'NONE',  ( -0.000000000000000000, 1.000000000000000000, -0.000000000000000000 ) ) ;
#8247 = CARTESIAN_POINT ( 'NONE',  ( 177.8371591254543205, -47.82818131005477369, 300.4678068554149490 ) ) ;
#8248 = FACE_OUTER_BOUND ( 'NONE', #41714, .T. ) ;
#8249 = CARTESIAN_POINT ( 'NONE',  ( 165.3359832912740046, -36.32844715994100682, -5.074374724088000832 ) ) ;
#8250 = DIRECTION ( 'NONE',  ( 0.000000000000000000, 0.000000000000000000, -1.000000000000000000 ) ) ;
#8251 = CARTESIAN_POINT ( 'NONE',  ( 113.6884830475839152, -29.53135334845044468, 199.4841967044829687 ) ) ;
#8252 = ORIENTED_EDGE ( 'NONE', *, *, #36016, .T. ) ;
#8253 = VERTEX_POINT ( 'NONE', #4093 ) ;
#8254 = CARTESIAN_POINT ( 'NONE',  ( 108.5815432132388878, -45.46059095889125246, 164.1444404487539828 ) ) ;
#8255 = AXIS2_PLACEMENT_3D ( 'NONE', #1065, #70560, #1525 ) ;
#8256 = PLANE ( 'NONE',  #64668 ) ;
#8257 = CIRCLE ( 'NONE', #19862, 1.000000000000000888 ) ;
#8258 = CARTESIAN_POINT ( 'NONE',  ( 112.0124476237220676, -28.73397683645143275, 285.6356252759109680 ) ) ;
#8259 = AXIS2_PLACEMENT_3D ( 'NONE', #22584, #44335, #29394 ) ;
#8260 = CARTESIAN_POINT ( 'NONE',  ( 72.25757238336811383, -1.944390235229867425, 394.9756252759101471 ) ) ;
#8261 = EDGE_CURVE ( 'NONE', #31858, #78258, #52210, .T. ) ;
#8262 = EDGE_CURVE ( 'NONE', #73152, #70182, #26297, .T. ) ;
#8263 = DIRECTION ( 'NONE',  ( 0.000000000000000000, 1.000000000000000000, 0.000000000000000000 ) ) ;
#8264 = DIRECTION ( 'NONE',  ( 1.000000000000000000, 4.299999999999999979E-14, 1.000000000000000078E-15 ) ) ;
#8265 = CARTESIAN_POINT ( 'NONE',  ( 113.2454986968446207, -28.75867294377915684, 105.5522919427003359 ) ) ;
#8266 = EDGE_CURVE ( 'NONE', #52316, #46913, #38608, .T. ) ;
#8267 = FACE_OUTER_BOUND ( 'NONE', #9614, .T. ) ;
#8268 = CARTESIAN_POINT ( 'NONE',  ( 112.1942863616536386, -45.78120396183496155, 212.9870538473389558 ) ) ;
#8269 = CARTESIAN_POINT ( 'NONE',  ( 97.53211619416173050, -39.74981511173461257, 171.5707515385688566 ) ) ;
#8270 = ORIENTED_EDGE ( 'NONE', *, *, #31933, .F. ) ;
#8271 = ORIENTED_EDGE ( 'NONE', *, *, #37995, .T. ) ;
#8272 = EDGE_CURVE ( 'NONE', #36906, #67921, #9138, .T. ) ;
#8273 = CARTESIAN_POINT ( 'NONE',  ( 117.0718954857576932, -35.46248235859899722, 88.92729194239142032 ) ) ;
#8274 = CARTESIAN_POINT ( 'NONE',  ( -80.89343850130802593, 94.60304557064716846, -86.67392531623340801 ) ) ;
#8275 = LINE ( 'NONE', #43219, #12770 ) ;
#8276 = CARTESIAN_POINT ( 'NONE',  ( 172.5664832912740110, -36.32844715994070839, 318.9256252759120116 ) ) ;
#8277 = AXIS2_PLACEMENT_3D ( 'NONE', #9537, #35892, #76786 ) ;
#8278 = CARTESIAN_POINT ( 'NONE',  ( 101.5079035968564654, -28.64143341885332816, 46.55562527591094835 ) ) ;
#8279 = CARTESIAN_POINT ( 'NONE',  ( 120.2221484686747317, -96.68314769832136335, -21.78219314458224076 ) ) ;
#8281 = EDGE_CURVE ( 'NONE', #12059, #34909, #88687, .T. ) ;
#8280 = CIRCLE ( 'NONE', #50269, 2.117000000000000881 ) ;
#8282 = ORIENTED_EDGE ( 'NONE', *, *, #18037, .T. ) ;
#8283 = CARTESIAN_POINT ( 'NONE',  ( 101.3604548305157920, -27.95253318249931596, 21.53562527591096298 ) ) ;
#8284 = CARTESIAN_POINT ( 'NONE',  ( 82.54999999999999716, 95.25000000000000000, 280.2255000000000109 ) ) ;
#8285 = CARTESIAN_POINT ( 'NONE',  ( 105.1109252617814604, -26.48919212138316581, 235.2270538473399313 ) ) ;
#8286 = EDGE_LOOP ( 'NONE', ( #52225, #51606 ) ) ;
#8287 = EDGE_CURVE ( 'NONE', #85160, #11890, #35352, .T. ) ;
#8288 = LINE ( 'NONE', #76878, #33220 ) ;
#8289 = LINE ( 'NONE', #22367, #55813 ) ;
#8290 = CARTESIAN_POINT ( 'NONE',  ( 80.06648329127402519, -46.72944715994105991, 4.925625275910944012 ) ) ;
#8291 = CARTESIAN_POINT ( 'NONE',  ( 115.1946057043837328, -37.48001498139237953, 76.57094751244896713 ) ) ;
#8292 = CARTESIAN_POINT ( 'NONE',  ( 114.1394676070193839, -29.04113448922185370, 195.4841967044819739 ) ) ;
#8293 = DIRECTION ( 'NONE',  ( 4.299999999999999979E-14, -1.000000000000000000, 4.400000000000000367E-29 ) ) ;
#8294 = VERTEX_POINT ( 'NONE', #73578 ) ;
#8295 = DIRECTION ( 'NONE',  ( 0.000000000000000000, 0.000000000000000000, -1.000000000000000000 ) ) ;
#8296 = ORIENTED_EDGE ( 'NONE', *, *, #24380, .F. ) ;
#8298 = EDGE_LOOP ( 'NONE', ( #11752, #11986, #4469, #54961 ) ) ;
#8297 = AXIS2_PLACEMENT_3D ( 'NONE', #6313, #7660, #61268 ) ;
#8299 = DIRECTION ( 'NONE',  ( -1.000000000000000000, -2.756263715554006823E-15, 0.000000000000000000 ) ) ;
#8300 = ORIENTED_EDGE ( 'NONE', *, *, #41642, .F. ) ;
#8301 = EDGE_LOOP ( 'NONE', ( #33096, #28179 ) ) ;
#8302 = FACE_BOUND ( 'NONE', #23000, .T. ) ;
#8303 = FACE_OUTER_BOUND ( 'NONE', #76421, .T. ) ;
#8305 = B_SPLINE_CURVE_WITH_KNOTS ( 'NONE', 3,
 ( #73524, #79479, #66711, #24937, #52601, #11298, #38119, #59878, #65810, #45798, #86278, #59440, #18560, #25375, #17239, #24057, #46243, #39001, #24498, #3598, #3164, #53044, #80810, #17678, #45357, #31291, #31744, #86725, #79924, #9530 ),
 .UNSPECIFIED., .F., .F.,
 ( 4, 2, 2, 2, 2, 2, 2, 2, 2, 2, 1, 1, 1, 1, 1, 1, 2, 4 ),
 ( 0.000000000000000000, 0.06250181204942577284, 0.1250036240988515457, 0.1875054361482773324, 0.2500072481977030914, 0.3125090602471288226, 0.3750108722965546648, 0.4375126843459803960, 0.4687635903706935392, 0.4843890433830502218, 0.4922017698892287019, 0.4961081331423181084, 0.4980613147688628395, 0.4990379055821350662, 0.4995262009887708743, 0.4997703486920889726, 0.4998924225437479940, 0.5000144963954069599 ),
 .UNSPECIFIED. ) ;
#8304 = CARTESIAN_POINT ( 'NONE',  ( 101.5215670198552544, -44.69967496328137457, 86.51527697093396796 ) ) ;
#8306 = CARTESIAN_POINT ( 'NONE',  ( 97.19579330311479737, -33.30690068839255957, 286.0613395616251751 ) ) ;
#8307 = CARTESIAN_POINT ( 'NONE',  ( 107.5667039024470455, -113.7784471599420613, -19.78219314458171141 ) ) ;
#8308 = LINE ( 'NONE', #1500, #29453 ) ;
#8309 = VERTEX_POINT ( 'NONE', #32688 ) ;
#8310 = ORIENTED_EDGE ( 'NONE', *, *, #33389, .F. ) ;
#8311 = DIRECTION ( 'NONE',  ( 0.000000000000000000, 0.000000000000000000, 1.000000000000000000 ) ) ;
#8312 = AXIS2_PLACEMENT_3D ( 'NONE', #79989, #17741, #5455 ) ;
#8313 = DIRECTION ( 'NONE',  ( 0.000000000000000000, 0.000000000000000000, -1.000000000000000000 ) ) ;
#8314 = ADVANCED_FACE ( 'NONE', ( #88122 ), #87664, .T. ) ;
#8315 = CARTESIAN_POINT ( 'NONE',  ( 70.55471543514235577, -139.7618167078771023, 247.2193956393660983 ) ) ;
#8316 = CARTESIAN_POINT ( 'NONE',  ( 118.1720832024965802, -36.20253795304678590, 118.8641967044829784 ) ) ;
#8317 = CARTESIAN_POINT ( 'NONE',  ( 102.5390659930443746, -27.28968240376552501, 95.43276813305395478 ) ) ;
#8319 = CYLINDRICAL_SURFACE ( 'NONE', #87204, 3.499999999999996003 ) ;
#8318 = CIRCLE ( 'NONE', #79406, 11.45913725231036118 ) ;
#8320 = ORIENTED_EDGE ( 'NONE', *, *, #1802, .F. ) ;
#8321 = VECTOR ( 'NONE', #21803, 1000.000000000000000 ) ;
#8322 = CARTESIAN_POINT ( 'NONE',  ( 116.5268644012694637, -41.19342475044518181, 228.4756252759109714 ) ) ;
#8323 = CARTESIAN_POINT ( 'NONE',  ( -22.62762465138237644, 172.0000000000000000, 183.8826257785461280 ) ) ;
#8324 = AXIS2_PLACEMENT_3D ( 'NONE', #43786, #85603, #63805 ) ;
#8325 = FACE_OUTER_BOUND ( 'NONE', #20911, .T. ) ;
#8327 = LINE ( 'NONE', #55537, #13770 ) ;
#8326 = CARTESIAN_POINT ( 'NONE',  ( 168.3595971214444376, -48.62134037892997895, 129.9678068554150059 ) ) ;
#8328 = CARTESIAN_POINT ( 'NONE',  ( -117.8738102209307215, 82.54999999999999716, -12.70000000000041318 ) ) ;
#8329 = DIRECTION ( 'NONE',  ( -0.000000000000000000, -1.000000000000000000, -0.000000000000000000 ) ) ;
#8330 = CARTESIAN_POINT ( 'NONE',  ( 132.2129280580803652, -38.76093376058476991, 7.655955902698878823 ) ) ;
#8331 = CARTESIAN_POINT ( 'NONE',  ( -11.39408073823492806, 88.17482193101731980, 130.0579986637597187 ) ) ;
#8332 = DIRECTION ( 'NONE',  ( 1.000000000000000000, 4.237773401492740281E-14, 0.000000000000000000 ) ) ;
#8333 = CYLINDRICAL_SURFACE ( 'NONE', #40485, 9.999999999999998224 ) ;
#8334 = CONICAL_SURFACE ( 'NONE', #6895, 11.57110091390449469, 0.7853981633974471688 ) ;
#8336 = ORIENTED_EDGE ( 'NONE', *, *, #10117, .F. ) ;
#8335 = DIRECTION ( 'NONE',  ( -4.237773401492740281E-14, 1.000000000000000000, 0.000000000000000000 ) ) ;
#8337 = CARTESIAN_POINT ( 'NONE',  ( 57.91199999999999903, 0.000000000000000000, 191.3008000794699797 ) ) ;
#8338 = CARTESIAN_POINT ( 'NONE',  ( 96.75420216176078725, -40.77324476150559462, 246.6118157521009664 ) ) ;
#8339 = CARTESIAN_POINT ( 'NONE',  ( 98.00710227423795118, -30.39686567179408172, 156.8289586092439549 ) ) ;
#8340 = CARTESIAN_POINT ( 'NONE',  ( 97.05449064767977063, -33.74661928051879300, 27.09562527591097236 ) ) ;
#8341 = VECTOR ( 'NONE', #82456, 1000.000000000000000 ) ;
#8342 = FACE_OUTER_BOUND ( 'NONE', #54952, .T. ) ;
#8343 = CIRCLE ( 'NONE', #89585, 2.116999999999980009 ) ;
#8345 = CARTESIAN_POINT ( 'NONE',  ( 81.50686229670706950, -34.38644903112238893, 7.895285856724627571 ) ) ;
#8344 = CARTESIAN_POINT ( 'NONE',  ( 100.8961411191535973, 120.6499999999999915, -3.968749999999580336 ) ) ;
#8346 = CARTESIAN_POINT ( 'NONE',  ( 109.6429292107771687, -46.48010952738405166, 138.7814519316777648 ) ) ;
#8347 = B_SPLINE_CURVE_WITH_KNOTS ( 'NONE', 3,
 ( #80272, #18015, #80712, #45698, #18461, #73880, #32528, #60234, #81620, #88868, #13010, #41137, #20713, #61579, #62486, #55198, #13896, #40697, #265, #68419, #27519, #67963, #67504, #76116, #89316, #41579, #6196, #27080, #82513, #54749, #21166, #75234, #69313, #7087, #47941, #75682, #33883, #62035, #20275, #13450, #48382, #5749, #82956, #5295, #83390, #76576, #47044, #55641, #68860, #88421, #89769, #12557, #47497, #19817, #27963, #32986, #34781, #60684, #26183, #26624, #48836, #6632, #53851 ),
 .UNSPECIFIED., .F., .F.,
 ( 4, 2, 2, 2, 1, 1, 1, 2, 2, 2, 2, 1, 1, 1, 1, 1, 2, 2, 2, 2, 2, 2, 2, 2, 1, 1, 1, 1, 2, 2, 2, 2, 1, 1, 1, 2, 2, 2, 4 ),
 ( 0.000000000000000000, 0.1249999999995831390, 0.1874999999993746669, 0.2187499999992704169, 0.2343749999992183475, 0.2421874999991923960, 0.2460937499991793231, 0.2480468749991724398, 0.2499999999991655286, 0.3124999999989367949, 0.3437499999988225530, 0.3593749999987653765, 0.3671874999987362886, 0.3710937499987211896, 0.3730468749987142507, 0.3740234374987106980, 0.3745117187487095323, 0.3749999999987083665, 0.4374999999987584376, 0.4687499999987840282, 0.4999999999988096189, 0.5624999999988609112, 0.5937499999988865573, 0.6093749999988995469, 0.6171874999989048760, 0.6210937499989086508, 0.6230468749989095389, 0.6240234374989099830, 0.6245117187489113153, 0.6249999999989126476, 0.6874999999990776267, 0.7187499999991611155, 0.7343749999992028599, 0.7421874999992246202, 0.7460937499992355004, 0.7480468749992409405, 0.7499999999992463806, 0.8749999999996231903, 1.000000000000000000 ),
 .UNSPECIFIED. ) ;
#8348 = AXIS2_PLACEMENT_3D ( 'NONE', #21159, #22073, #56093 ) ;
#8349 = EDGE_CURVE ( 'NONE', #47225, #2985, #5445, .T. ) ;
#8350 = ORIENTED_EDGE ( 'NONE', *, *, #49991, .T. ) ;
#8351 = DIRECTION ( 'NONE',  ( -4.237773401492740281E-14, 1.000000000000000000, 0.000000000000000000 ) ) ;
#8352 = ORIENTED_EDGE ( 'NONE', *, *, #44355, .F. ) ;
#8353 = CARTESIAN_POINT ( 'NONE',  ( 98.04376085404715013, -35.95281974173802553, 185.6686103042669629 ) ) ;
#8355 = EDGE_LOOP ( 'NONE', ( #12936, #72521, #82908, #33431 ) ) ;
#8354 = LINE ( 'NONE', #42398, #13778 ) ;
#8356 = CARTESIAN_POINT ( 'NONE',  ( 123.4696824136382105, 101.5999999999999943, -179.8898777604649979 ) ) ;
#8357 = CARTESIAN_POINT ( 'NONE',  ( 96.76471471792635271, -35.27954033865441374, 177.2156252759109805 ) ) ;
#8358 = CARTESIAN_POINT ( 'NONE',  ( 80.06648329127402519, -41.22944715994105280, -0.5743747240890559880 ) ) ;
#8359 = DIRECTION ( 'NONE',  ( -1.000000000000000000, 0.000000000000000000, -0.000000000000000000 ) ) ;
#8360 = CARTESIAN_POINT ( 'NONE',  ( 98.35372588324824505, -31.64965747931991302, 86.90591219145825619 ) ) ;
#8361 = DIRECTION ( 'NONE',  ( 1.000000000000000078E-15, -1.000000000000000083E-30, -1.000000000000000000 ) ) ;
#8362 = CYLINDRICAL_SURFACE ( 'NONE', #9199, 2.030000000001310312 ) ;
#8363 = CARTESIAN_POINT ( 'NONE',  ( 109.6029845306728419, -46.78454271877410520, 92.78514908543594686 ) ) ;
#8364 = ORIENTED_EDGE ( 'NONE', *, *, #80879, .T. ) ;
#8365 = ORIENTED_EDGE ( 'NONE', *, *, #83144, .T. ) ;
#8367 = ORIENTED_EDGE ( 'NONE', *, *, #34749, .T. ) ;
#8366 = VECTOR ( 'NONE', #75704, 1000.000000000000000 ) ;
#8368 = CARTESIAN_POINT ( 'NONE',  ( 101.8615262650677522, -29.55750872133152640, 72.00729759161094989 ) ) ;
#8369 = CARTESIAN_POINT ( 'NONE',  ( 107.0667039024470313, -104.2784471599408676, 19.21780685541799016 ) ) ;
#8371 = CARTESIAN_POINT ( 'NONE',  ( 70.06871658682176474, -140.6784471599409869, 245.5179332689559999 ) ) ;
#8370 = CARTESIAN_POINT ( 'NONE',  ( 103.1049807579881588, -45.67203811392940338, 173.2441967044819648 ) ) ;
#8372 = CARTESIAN_POINT ( 'NONE',  ( 60.32499999999999574, 82.54999999999999716, 330.0094617072599590 ) ) ;
#8373 = DIRECTION ( 'NONE',  ( 0.000000000000000000, -1.000000000000000000, 0.000000000000000000 ) ) ;
#8374 = ADVANCED_FACE ( 'NONE', ( #46298, #31794, #12251 ), #39944, .F. ) ;
#8375 = CARTESIAN_POINT ( 'NONE',  ( 61.00843881761244347, 65.60000000000000853, -33.74458626278666884 ) ) ;
#8376 = CARTESIAN_POINT ( 'NONE',  ( 165.3359832912740046, -36.32844715994100682, -5.074374724088000832 ) ) ;
#8377 = EDGE_CURVE ( 'NONE', #79697, #6854, #40398, .T. ) ;
#8378 = CARTESIAN_POINT ( 'NONE',  ( 67.45090841991523689, -68.24843840015816454, 246.6732856276495909 ) ) ;
#8379 = CARTESIAN_POINT ( 'NONE',  ( 118.8789388927533111, -36.16900092901214947, 118.8641967044819836 ) ) ;
#8380 = ORIENTED_EDGE ( 'NONE', *, *, #25773, .F. ) ;
#8381 = ADVANCED_FACE ( 'NONE', ( #39055, #59487 ), #66761, .T. ) ;
#8382 = ORIENTED_EDGE ( 'NONE', *, *, #8566, .T. ) ;
#8383 = ORIENTED_EDGE ( 'NONE', *, *, #4307, .F. ) ;
#8384 = EDGE_CURVE ( 'NONE', #54125, #74866, #74480, .T. ) ;
#8385 = CARTESIAN_POINT ( 'NONE',  ( 12.61757850223405519, 80.88535426119446470, 129.9449579601741505 ) ) ;
#8386 = CARTESIAN_POINT ( 'NONE',  ( -100.8594679592206802, 82.54999999999999716, -82.89895571708333932 ) ) ;
#8387 = VECTOR ( 'NONE', #78916, 1000.000000000000000 ) ;
#8388 = CARTESIAN_POINT ( 'NONE',  ( 97.07198155714206678, -35.37918349729778100, 131.2190186775771679 ) ) ;
#8389 = DIRECTION ( 'NONE',  ( 1.000000000000000078E-15, -1.000000000000000083E-30, -1.000000000000000000 ) ) ;
#8390 = CARTESIAN_POINT ( 'NONE',  ( 99.90434330870786539, -40.64524553156628173, 219.5423760838769738 ) ) ;
#8391 = AXIS2_PLACEMENT_3D ( 'NONE', #72589, #17177, #10353 ) ;
#8392 = VECTOR ( 'NONE', #46829, 1000.000000000000000 ) ;
#8393 = LINE ( 'NONE', #62887, #46515 ) ;
#8394 = DIRECTION ( 'NONE',  ( 1.000000000000000000, 0.000000000000000000, 0.000000000000000000 ) ) ;
#8395 = VERTEX_POINT ( 'NONE', #81758 ) ;
#8397 = ORIENTED_EDGE ( 'NONE', *, *, #32033, .T. ) ;
#8396 = ORIENTED_EDGE ( 'NONE', *, *, #38268, .F. ) ;
#8398 = ADVANCED_FACE ( 'NONE', ( #4547 ), #32235, .F. ) ;
#8399 = CIRCLE ( 'NONE', #59135, 21.75000000000000711 ) ;
#8400 = CARTESIAN_POINT ( 'NONE',  ( 135.5667039024470171, -90.27844715994091018, 51.21780685541800437 ) ) ;
#8401 = VERTEX_POINT ( 'NONE', #11810 ) ;
#8402 = ORIENTED_EDGE ( 'NONE', *, *, #63979, .F. ) ;
#8403 = CARTESIAN_POINT ( 'NONE',  ( 4.163101094985349692E-14, 120.6499999999999915, -98.60478223830740774 ) ) ;
#8404 = CARTESIAN_POINT ( 'NONE',  ( 143.2710647978358054, -69.54852422598250428, 247.5103554657479776 ) ) ;
#8405 = CARTESIAN_POINT ( 'NONE',  ( 115.7948931938460362, -35.19871557519451954, 240.3958690201829427 ) ) ;
#8406 = VECTOR ( 'NONE', #26506, 1000.000000000000000 ) ;
#8407 = FACE_OUTER_BOUND ( 'NONE', #12138, .T. ) ;
#8408 = VERTEX_POINT ( 'NONE', #39507 ) ;
#8409 = VECTOR ( 'NONE', #72721, 1000.000000000000114 ) ;
#8410 = AXIS2_PLACEMENT_3D ( 'NONE', #59783, #31189, #85751 ) ;
#8411 = CARTESIAN_POINT ( 'NONE',  ( 104.1241784947088149, -44.29815144288988193, 9.635625275910944865 ) ) ;
#8412 = CARTESIAN_POINT ( 'NONE',  ( 162.8913605087219878, -31.76306994223740432, -5.074374724088000832 ) ) ;
#8413 = VERTEX_POINT ( 'NONE', #55784 ) ;
#8414 = ORIENTED_EDGE ( 'NONE', *, *, #29367, .T. ) ;
#8415 = AXIS2_PLACEMENT_3D ( 'NONE', #78203, #15516, #39406 ) ;
#8416 = DIRECTION ( 'NONE',  ( 8.503806984168930281E-16, 0.000000000000000000, -1.000000000000000000 ) ) ;
#8417 = ORIENTED_EDGE ( 'NONE', *, *, #68253, .T. ) ;
#8418 = VERTEX_POINT ( 'NONE', #7676 ) ;
#8419 = CARTESIAN_POINT ( 'NONE',  ( 102.3843679657495329, -43.41581164733459985, 279.9080903695913776 ) ) ;
#8420 = CARTESIAN_POINT ( 'NONE',  ( 108.9491902927665734, -26.41713524962505133, 164.9327681330529742 ) ) ;
#8421 = CARTESIAN_POINT ( 'NONE',  ( 114.6914383512288254, -44.69963429152232237, 113.1718157521009687 ) ) ;
#8422 = SURFACE_STYLE_USAGE ( .BOTH. , #49732 ) ;
#8423 = CARTESIAN_POINT ( 'NONE',  ( 111.1274376763295635, -27.12782558180003889, 240.7584824187679544 ) ) ;
#8424 = DIRECTION ( 'NONE',  ( 4.299999999999999979E-14, -1.000000000000000000, 0.000000000000000000 ) ) ;
#8425 = LINE ( 'NONE', #50178, #34946 ) ;
#8426 = EDGE_LOOP ( 'NONE', ( #76762, #16841, #34066, #28559 ) ) ;
#8427 = CARTESIAN_POINT ( 'NONE',  ( -130.5477899301573927, 69.93364840292896645, -1.674143004589110140 ) ) ;
#8428 = VERTEX_POINT ( 'NONE', #21767 ) ;
#8429 = ORIENTED_EDGE ( 'NONE', *, *, #4489, .F. ) ;
#8430 = VECTOR ( 'NONE', #24139, 1000.000000000000000 ) ;
#8431 = ADVANCED_FACE ( 'NONE', ( #83994 ), #48523, .T. ) ;
#8432 = VECTOR ( 'NONE', #26540, 1000.000000000000000 ) ;
#8433 = ORIENTED_EDGE ( 'NONE', *, *, #991, .F. ) ;
#8434 = CARTESIAN_POINT ( 'NONE',  ( 96.02342237304465300, -37.20891875426686823, 116.3489586092439652 ) ) ;
#8435 = CARTESIAN_POINT ( 'NONE',  ( 107.0664832912739968, 19.62155284005901024, 336.6506252759110112 ) ) ;
#8436 = EDGE_CURVE ( 'NONE', #57610, #43708, #410, .T. ) ;
#8437 = DIRECTION ( 'NONE',  ( 0.000000000000000000, -1.000000000000000000, 0.000000000000000000 ) ) ;
#8438 = DIRECTION ( 'NONE',  ( -1.000000000000000000, -8.540177112501204385E-16, 0.000000000000000000 ) ) ;
#8441 = CARTESIAN_POINT ( 'NONE',  ( 101.6619702986603073, -45.61876124157276280, 243.1413395616249886 ) ) ;
#8440 = CARTESIAN_POINT ( 'NONE',  ( 112.5709320333848069, -45.13014110428505177, 58.03751997880807068 ) ) ;
#8439 = DIRECTION ( 'NONE',  ( -1.000000000000000000, -1.206764157201257538E-15, 0.000000000000000000 ) ) ;
#8442 = CARTESIAN_POINT ( 'NONE',  ( 74.06670390244701707, -90.27844715994098124, 51.21780685541800437 ) ) ;
#8443 = DIRECTION ( 'NONE',  ( 0.7071067811865483499, 0.7071067811865466846, 7.071067811865491110E-16 ) ) ;
#8444 = CARTESIAN_POINT ( 'NONE',  ( 134.0664832912739826, -9.029447159941003775, 4.925625275910997303 ) ) ;
#8445 = DIRECTION ( 'NONE',  ( 0.000000000000000000, -1.000000000000000000, 0.000000000000000000 ) ) ;
#8446 = CARTESIAN_POINT ( 'NONE',  ( 97.06107110138425753, -37.99641199796607793, 257.4272919453096051 ) ) ;
#8447 = CARTESIAN_POINT ( 'NONE',  ( 146.5179483142460128, -137.3672551618605269, 246.8848049447683763 ) ) ;
#8449 = VERTEX_POINT ( 'NONE', #77172 ) ;
#8448 = CARTESIAN_POINT ( 'NONE',  ( 96.51917584821923413, -40.19201726479878545, 286.5908633711491120 ) ) ;
#8450 = CARTESIAN_POINT ( 'NONE',  ( -3.175000000000109956, 24.56180297284579694, -31.75000000000000000 ) ) ;
#8451 = CARTESIAN_POINT ( 'NONE',  ( 105.3125257651413307, -48.47460025707392361, 147.4584824187679715 ) ) ;
#8452 = CARTESIAN_POINT ( 'NONE',  ( 106.5180998683148488, -25.68982506017174927, 41.12800622829193742 ) ) ;
#8453 = CARTESIAN_POINT ( 'NONE',  ( 117.4569897637122011, -35.45259360763351708, 189.9241967044829664 ) ) ;
#8454 = VECTOR ( 'NONE', #938, 1000.000000000000000 ) ;
#8455 = CARTESIAN_POINT ( 'NONE',  ( 248.6659999999999968, 52.73749999999999716, 10.66800000000000104 ) ) ;
#8456 = CARTESIAN_POINT ( 'NONE',  ( 51.34673845256583036, -36.02818131005845004, 237.4678068554150059 ) ) ;
#8458 = LINE ( 'NONE', #22993, #74725 ) ;
#8457 = CYLINDRICAL_SURFACE ( 'NONE', #37623, 4.875000000000017764 ) ;
#8459 = LINE ( 'NONE', #21191, #35036 ) ;
#8460 = DIRECTION ( 'NONE',  ( -1.000000000000000078E-15, 1.000000000000000083E-30, 1.000000000000000000 ) ) ;
#8461 = ORIENTED_EDGE ( 'NONE', *, *, #57159, .T. ) ;
#8462 = DIRECTION ( 'NONE',  ( -1.000000000000000000, 3.651563665954189830E-16, 0.000000000000000000 ) ) ;
#8463 = CIRCLE ( 'NONE', #7016, 3.299999999999997158 ) ;
#8465 = EDGE_CURVE ( 'NONE', #8076, #83603, #69457, .T. ) ;
#8464 = AXIS2_PLACEMENT_3D ( 'NONE', #28531, #82642, #49418 ) ;
#8466 = ORIENTED_EDGE ( 'NONE', *, *, #72556, .T. ) ;
#8467 = ORIENTED_EDGE ( 'NONE', *, *, #38910, .F. ) ;
#8468 = AXIS2_PLACEMENT_3D ( 'NONE', #19654, #12859, #81464 ) ;
#8470 = VERTEX_POINT ( 'NONE', #21305 ) ;
#8469 = FACE_OUTER_BOUND ( 'NONE', #4265, .T. ) ;
#8471 = CARTESIAN_POINT ( 'NONE',  ( 115.5559444348970857, -42.74257571503945741, 49.33562527591095659 ) ) ;
#8472 = CYLINDRICAL_SURFACE ( 'NONE', #537, 38.10000000000000142 ) ;
#8473 = CIRCLE ( 'NONE', #28750, 82.41591158490091118 ) ;
#8474 = DIRECTION ( 'NONE',  ( -1.000000000000000000, 0.000000000000000000, 5.463695987328529395E-16 ) ) ;
#8475 = EDGE_CURVE ( 'NONE', #36180, #15997, #60250, .T. ) ;
#8476 = CARTESIAN_POINT ( 'NONE',  ( 97.91841856125127208, -30.44371649139010927, 161.8594347997199918 ) ) ;
#8477 = CIRCLE ( 'NONE', #38859, 190.5000000000000000 ) ;
#8478 = VECTOR ( 'NONE', #73106, 1000.000000000000000 ) ;
#8479 = CARTESIAN_POINT ( 'NONE',  ( 114.6457050300329996, -40.66804080626008044, 287.8667055423626380 ) ) ;
#8480 = EDGE_LOOP ( 'NONE', ( #48865, #25062, #72959, #34194 ) ) ;
#8481 = ORIENTED_EDGE ( 'NONE', *, *, #73481, .F. ) ;
#8482 = ORIENTED_EDGE ( 'NONE', *, *, #35140, .T. ) ;
#8483 = ORIENTED_EDGE ( 'NONE', *, *, #71364, .F. ) ;
#8484 = DIRECTION ( 'NONE',  ( 1.000000000000000078E-15, -1.000000000000000000, 0.000000000000000000 ) ) ;
#8485 = CARTESIAN_POINT ( 'NONE',  ( 138.8167039024479834, -67.87844715994100397, 37.63480685541480852 ) ) ;
#8486 = LINE ( 'NONE', #35270, #33207 ) ;
#8487 = CARTESIAN_POINT ( 'NONE',  ( 80.06648329127402519, -46.72944715994105991, 8.225625275910942946 ) ) ;
#8488 = CARTESIAN_POINT ( 'NONE',  ( 87.44900557253099294, 93.33921197991990937, 96.94152442043777285 ) ) ;
#8489 = CARTESIAN_POINT ( 'NONE',  ( 34.92499999999999716, 82.54999999999999716, 302.8950000000000387 ) ) ;
#8490 = VECTOR ( 'NONE', #28169, 1000.000000000000000 ) ;
#8491 = DIRECTION ( 'NONE',  ( 0.000000000000000000, -1.000000000000000000, 0.000000000000000000 ) ) ;
#8492 = CARTESIAN_POINT ( 'NONE',  ( -546.0365000000000464, 53.97500000000000142, 50.79999999999999716 ) ) ;
#8493 = CARTESIAN_POINT ( 'NONE',  ( 110.5478855402368197, -46.57039549162855963, 37.84705384733994293 ) ) ;
#8494 = ADVANCED_FACE ( 'NONE', ( #7234 ), #28101, .T. ) ;
#8495 = ORIENTED_EDGE ( 'NONE', *, *, #2004, .F. ) ;
#8496 = CARTESIAN_POINT ( 'NONE',  ( 142.8821648370248170, -72.54478064608022692, 542.9756252759101471 ) ) ;
#8497 = CIRCLE ( 'NONE', #20096, 2.999999999999933387 ) ;
#8498 = CARTESIAN_POINT ( 'NONE',  ( -15.60269531711297830, 92.07499999999998863, -52.58204823848948450 ) ) ;
#8499 = CARTESIAN_POINT ( 'NONE',  ( 111.9587407205840890, -30.16069495786998544, 102.3852332267339591 ) ) ;
#8500 = CIRCLE ( 'NONE', #2668, 3.500000000000003109 ) ;
#8501 = FACE_OUTER_BOUND ( 'NONE', #63614, .T. ) ;
#8502 = DIRECTION ( 'NONE',  ( -1.000000000000000000, 0.000000000000000000, 0.000000000000000000 ) ) ;
#8503 = VERTEX_POINT ( 'NONE', #70351 ) ;
#8504 = EDGE_LOOP ( 'NONE', ( #15770, #26334, #71639, #3615 ) ) ;
#8505 = EDGE_CURVE ( 'NONE', #3053, #49629, #34019, .T. ) ;
#8506 = DIRECTION ( 'NONE',  ( 1.000000000000000000, 8.953411488912556626E-16, 0.000000000000000000 ) ) ;
#8507 = ORIENTED_EDGE ( 'NONE', *, *, #32673, .F. ) ;
#8508 = VERTEX_POINT ( 'NONE', #34474 ) ;
#8509 = EDGE_CURVE ( 'NONE', #593, #42450, #35367, .T. ) ;
#8510 = CARTESIAN_POINT ( 'NONE',  ( 113.1089835609813719, -43.92423027677314451, 144.5520594963729764 ) ) ;
#8511 = VECTOR ( 'NONE', #47048, 1000.000000000000000 ) ;
#8512 = CARTESIAN_POINT ( 'NONE',  ( 76.06670390244703128, -104.2784471599409812, 25.71780685541800437 ) ) ;
#8513 = CARTESIAN_POINT ( 'NONE',  ( 111.0909104302412373, -25.55688089738240976, 95.80133956162495679 ) ) ;
#8514 = CARTESIAN_POINT ( 'NONE',  ( 37.35959712133814747, -48.62134037883198090, 180.4678068554150911 ) ) ;
#8515 = VECTOR ( 'NONE', #15056, 999.9999999999998863 ) ;
#8516 = ORIENTED_EDGE ( 'NONE', *, *, #26265, .T. ) ;
#8517 = AXIS2_PLACEMENT_3D ( 'NONE', #30505, #24140, #1469 ) ;
#8518 = ORIENTED_EDGE ( 'NONE', *, *, #89490, .F. ) ;
#8519 = VERTEX_POINT ( 'NONE', #75820 ) ;
#8520 = CIRCLE ( 'NONE', #65057, 15.50000000000000000 ) ;
#8521 = CARTESIAN_POINT ( 'NONE',  ( 98.70474251149389033, -42.99264563182325816, 66.83848241876793850 ) ) ;
#8522 = VERTEX_POINT ( 'NONE', #63077 ) ;
#8523 = CARTESIAN_POINT ( 'NONE',  ( 99.81116105471912192, -29.32005551970541291, 270.7051490854354938 ) ) ;
#8524 = CARTESIAN_POINT ( 'NONE',  ( 97.74302678327005367, -41.52030872683848628, 192.7041967044819728 ) ) ;
#8525 = LINE ( 'NONE', #77119, #69827 ) ;
#8526 = CARTESIAN_POINT ( 'NONE',  ( 98.30746454995575334, -41.72870539506785548, 127.7397773158203620 ) ) ;
#8527 = CARTESIAN_POINT ( 'NONE',  ( 103.4684036848089050, -46.51393990267121836, 138.2956252759109645 ) ) ;
#8528 = CARTESIAN_POINT ( 'NONE',  ( 149.4409906032288973, -0.9156555935619370423, 394.9756252759100903 ) ) ;
#8529 = ORIENTED_EDGE ( 'NONE', *, *, #31487, .T. ) ;
#8530 = VECTOR ( 'NONE', #84911, 1000.000000000000000 ) ;
#8531 = CARTESIAN_POINT ( 'NONE',  ( -75.61066417432020614, 101.5999999999999943, 177.0380000000000109 ) ) ;
#8532 = VERTEX_POINT ( 'NONE', #89457 ) ;
#8533 = AXIS2_PLACEMENT_3D ( 'NONE', #28997, #15376, #56682 ) ;
#8534 = CARTESIAN_POINT ( 'NONE',  ( 98.04140018452436323, -41.04160969738705944, 132.6816209718298012 ) ) ;
#8535 = ORIENTED_EDGE ( 'NONE', *, *, #14089, .T. ) ;
#8536 = ORIENTED_EDGE ( 'NONE', *, *, #7142, .T. ) ;
#8537 = CARTESIAN_POINT ( 'NONE',  ( -487.2989999999999782, 6.038608028953049711, 90.48749999999999716 ) ) ;
#8538 = CARTESIAN_POINT ( 'NONE',  ( 51.42025729303981052, -33.70561438052008896, 193.9678068554150911 ) ) ;
#8539 = CARTESIAN_POINT ( 'NONE',  ( 101.6088808140983417, -47.24878093606274376, 17.19562527591095247 ) ) ;
#8540 = DIRECTION ( 'NONE',  ( 0.000000000000000000, 0.000000000000000000, 1.000000000000000000 ) ) ;
#8541 = ADVANCED_FACE ( 'NONE', ( #48980 ), #8124, .F. ) ;
#8542 = DIRECTION ( 'NONE',  ( 1.000000000000000000, 4.163336342344333240E-14, 0.000000000000000000 ) ) ;
#8543 = CARTESIAN_POINT ( 'NONE',  ( 117.0608945237863736, -38.08045311857467397, 74.71895860942261436 ) ) ;
#8544 = CARTESIAN_POINT ( 'NONE',  ( 114.5308976578478735, -43.10096916487051288, 63.26419670448296984 ) ) ;
#8546 = CARTESIAN_POINT ( 'NONE',  ( 96.69266148864274157, -35.94780844399463149, 142.2670538473399517 ) ) ;
#8545 = LINE ( 'NONE', #84859, #23194 ) ;
#8547 = CARTESIAN_POINT ( 'NONE',  ( 116.3212776292294421, -32.94146857471278622, 70.13562527591093954 ) ) ;
#8548 = CYLINDRICAL_SURFACE ( 'NONE', #58299, 2.116999999999980009 ) ;
#8549 = EDGE_LOOP ( 'NONE', ( #2632, #34325 ) ) ;
#8550 = VECTOR ( 'NONE', #6730, 1000.000000000000000 ) ;
#8551 = CARTESIAN_POINT ( 'NONE',  ( 20.03715912545739997, -46.82818131006202123, 129.9678068554150627 ) ) ;
#8552 = DIRECTION ( 'NONE',  ( -4.299999999999999979E-14, 1.000000000000000000, 0.000000000000000000 ) ) ;
#8553 = DIRECTION ( 'NONE',  ( 0.000000000000000000, 0.000000000000000000, -1.000000000000000000 ) ) ;
#8554 = ORIENTED_EDGE ( 'NONE', *, *, #43746, .F. ) ;
#8555 = CARTESIAN_POINT ( 'NONE',  ( 36.23715912545339535, -47.82818131006131779, 180.4678068554150911 ) ) ;
#8557 = ORIENTED_EDGE ( 'NONE', *, *, #33517, .T. ) ;
#8556 = CARTESIAN_POINT ( 'NONE',  ( 109.4554010020096513, -25.88943074854985227, 179.8918157521019339 ) ) ;
#8558 = CARTESIAN_POINT ( 'NONE',  ( 75.26949937496601706, -71.54137415153812185, 394.9756252759101471 ) ) ;
#8559 = CARTESIAN_POINT ( 'NONE',  ( 116.8778831976698882, -40.31743973661899361, 214.5470538473389581 ) ) ;
#8560 = CARTESIAN_POINT ( 'NONE',  ( 115.3013748915712711, -44.17149383341634206, 79.25372051400697160 ) ) ;
#8561 = CARTESIAN_POINT ( 'NONE',  ( 97.63922045723853671, 72.45841406287408404, 86.67141577317495660 ) ) ;
#8562 = CARTESIAN_POINT ( 'NONE',  ( 112.1368176753006338, -28.01137494322663102, 190.6564328795896586 ) ) ;
#8563 = AXIS2_PLACEMENT_3D ( 'NONE', #60502, #74596, #32349 ) ;
#8564 = CARTESIAN_POINT ( 'NONE',  ( 179.7974245136200011, -36.32844715994040996, -5.074374724088000832 ) ) ;
#8565 = VERTEX_POINT ( 'NONE', #56243 ) ;
#8566 = EDGE_CURVE ( 'NONE', #16628, #88630, #35815, .T. ) ;
#8567 = ORIENTED_EDGE ( 'NONE', *, *, #86852, .F. ) ;
#8568 = ORIENTED_EDGE ( 'NONE', *, *, #45907, .F. ) ;
#8569 = EDGE_CURVE ( 'NONE', #74616, #52978, #27215, .T. ) ;
#8570 = ORIENTED_EDGE ( 'NONE', *, *, #77192, .F. ) ;
#8571 = CARTESIAN_POINT ( 'NONE',  ( 172.5667039024478129, -36.32844715993500273, 300.4678068554149490 ) ) ;
#8572 = CARTESIAN_POINT ( 'NONE',  ( 110.2558863881303779, -26.76706588525435748, 230.8299109901969643 ) ) ;
#8573 = DIRECTION ( 'NONE',  ( 0.000000000000000000, 1.000000000000000000, 0.000000000000000000 ) ) ;
#8574 = CARTESIAN_POINT ( 'NONE',  ( 136.8164832912739826, -18.72944715994099951, 3.101481641215532825 ) ) ;
#8575 = EDGE_CURVE ( 'NONE', #42339, #84277, #84449, .T. ) ;
#8576 = AXIS2_PLACEMENT_3D ( 'NONE', #76918, #14246, #158 ) ;
#8577 = ADVANCED_FACE ( 'NONE', ( #22213 ), #49888, .T. ) ;
#8579 = CARTESIAN_POINT ( 'NONE',  ( 165.9667039024459996, -28.27351298637401200, -5.074374724088000832 ) ) ;
#8578 = LINE ( 'NONE', #1763, #7618 ) ;
#8580 = CARTESIAN_POINT ( 'NONE',  ( 107.0664832912739968, -8.350947159940998787, 333.4006252759120343 ) ) ;
#8581 = CARTESIAN_POINT ( 'NONE',  ( 97.78948648769619467, -29.31518076255846239, 45.78991099019697231 ) ) ;
#8582 = VERTEX_POINT ( 'NONE', #54895 ) ;
#8583 = ADVANCED_FACE ( 'NONE', ( #82660 ), #86408, .T. ) ;
#8584 = ORIENTED_EDGE ( 'NONE', *, *, #84149, .F. ) ;
#8585 = CIRCLE ( 'NONE', #82644, 5.041900000000001825 ) ;
#8587 = ORIENTED_EDGE ( 'NONE', *, *, #9605, .T. ) ;
#8586 = AXIS2_PLACEMENT_3D ( 'NONE', #45884, #66800, #11848 ) ;
#8588 = CARTESIAN_POINT ( 'NONE',  ( 194.0667039024482108, -40.32844715993407192, 180.4678068554150343 ) ) ;
#8590 = EDGE_CURVE ( 'NONE', #16335, #48763, #48088, .T. ) ;
#8589 = CARTESIAN_POINT ( 'NONE',  ( 97.79625303259112457, -40.47954707014128672, 17.63206288286017553 ) ) ;
#8591 = CARTESIAN_POINT ( 'NONE',  ( 117.9377692877171313, -39.05906590213764673, 254.6584824187675338 ) ) ;
#8592 = DIRECTION ( 'NONE',  ( 0.000000000000000000, 0.000000000000000000, -1.000000000000000000 ) ) ;
#8593 = VECTOR ( 'NONE', #32739, 1000.000000000000000 ) ;
#8594 = CARTESIAN_POINT ( 'NONE',  ( 97.33998274022617636, -37.75834089694784979, 122.4099109901959679 ) ) ;
#8595 = COLOUR_RGB ( '', 0.31764706, 0.68627451, 0.89019608) ;
#8596 = EDGE_CURVE ( 'NONE', #9390, #47902, #36732, .T. ) ;
#8597 = LINE ( 'NONE', #2674, #24265 ) ;
#8598 = ORIENTED_EDGE ( 'NONE', *, *, #30832, .F. ) ;
#8599 = DIRECTION ( 'NONE',  ( 0.000000000000000000, 1.000000000000000000, 0.000000000000000000 ) ) ;
#8600 = CARTESIAN_POINT ( 'NONE',  ( 78.94209639488894936, -34.21971364483395206, 1.822997995688476314 ) ) ;
#8601 = AXIS2_PLACEMENT_3D ( 'NONE', #60134, #48288, #61044 ) ;
#8602 = ORIENTED_EDGE ( 'NONE', *, *, #69802, .F. ) ;
#8603 = ORIENTED_EDGE ( 'NONE', *, *, #40169, .F. ) ;
#8604 = CARTESIAN_POINT ( 'NONE',  ( -91.61507027739536113, 87.79588542099537563, 75.24778849303649508 ) ) ;
#8605 = CARTESIAN_POINT ( 'NONE',  ( 103.0821812797523194, -45.97846664716049503, 283.6844404487542874 ) ) ;
#8606 = CARTESIAN_POINT ( 'NONE',  ( 196.2150000000000034, 37.33800000000000097, 50.79999999999999716 ) ) ;
#8607 = CARTESIAN_POINT ( 'NONE',  ( 97.33784131715731291, -34.07106450827230049, 86.11479194080892796 ) ) ;
#8608 = CIRCLE ( 'NONE', #57875, 7.937500000000000000 ) ;
#8609 = CARTESIAN_POINT ( 'NONE',  ( 107.0664832912739968, -36.72944715994100306, 287.6356252759109680 ) ) ;
#8610 = ORIENTED_EDGE ( 'NONE', *, *, #3051, .T. ) ;
#8611 = DIRECTION ( 'NONE',  ( -1.000000000000000078E-15, 1.000000000000000000, 0.000000000000000000 ) ) ;
#8612 = ADVANCED_FACE ( 'NONE', ( #23999 ), #51225, .T. ) ;
#8613 = CARTESIAN_POINT ( 'NONE',  ( -487.2989999999999782, 100.8062500000000057, 94.61194598552329182 ) ) ;
#8614 = ORIENTED_EDGE ( 'NONE', *, *, #49441, .T. ) ;
#8615 = CARTESIAN_POINT ( 'NONE',  ( 107.6031522308233974, -26.28253885536559764, 95.03562527591097364 ) ) ;
#8616 = EDGE_LOOP ( 'NONE', ( #54076, #71189, #24363, #22148 ) ) ;
#8617 = ADVANCED_FACE ( 'NONE', ( #64433 ), #10359, .T. ) ;
#8618 = CARTESIAN_POINT ( 'NONE',  ( 109.7027494226597071, -44.85393009491053817, 12.24956268521998304 ) ) ;
#8619 = ADVANCED_FACE ( 'NONE', ( #57148 ), #9464, .F. ) ;
#8620 = DIRECTION ( 'NONE',  ( 0.000000000000000000, 1.000000000000000000, 0.000000000000000000 ) ) ;
#8621 = CARTESIAN_POINT ( 'NONE',  ( 103.7602102885707183, -27.48919103108766748, 190.3499109901969746 ) ) ;
#8622 = CARTESIAN_POINT ( 'NONE',  ( 49.16670390244654953, -26.71338133339277121, 117.4678068554150485 ) ) ;
#8623 = DIRECTION ( 'NONE',  ( 1.000000000000000000, 4.299999999999999979E-14, 1.000000000000000078E-15 ) ) ;
#8625 = EDGE_CURVE ( 'NONE', #26264, #21297, #85350, .T. ) ;
#8624 = DIRECTION ( 'NONE',  ( -1.000000000000000000, 0.000000000000000000, 0.000000000000000000 ) ) ;
#8626 = CARTESIAN_POINT ( 'NONE',  ( 154.4532655810166091, -72.54279768053238797, 396.9756252759102040 ) ) ;
#8627 = AXIS2_PLACEMENT_3D ( 'NONE', #47101, #32586, #26674 ) ;
#8628 = CARTESIAN_POINT ( 'NONE',  ( 101.0616705854173460, -45.30470917520826646, 278.0899109901965858 ) ) ;
#8629 = CARTESIAN_POINT ( 'NONE',  ( 85.28591416242399248, 95.08639429146514033, -82.35292268805471849 ) ) ;
#8630 = ORIENTED_EDGE ( 'NONE', *, *, #36475, .F. ) ;
#8631 = CARTESIAN_POINT ( 'NONE',  ( 136.8037680012515409, -37.00431460297851061, 6.768845952122538812 ) ) ;
#8632 = ORIENTED_EDGE ( 'NONE', *, *, #25255, .T. ) ;
#8633 = CARTESIAN_POINT ( 'NONE',  ( 95.62763156918455820, -33.44862719079586810, 137.1041967044819501 ) ) ;
#8634 = FACE_OUTER_BOUND ( 'NONE', #89382, .T. ) ;
#8635 = ORIENTED_EDGE ( 'NONE', *, *, #50292, .F. ) ;
#8636 = ORIENTED_EDGE ( 'NONE', *, *, #61694, .T. ) ;
#8637 = ORIENTED_EDGE ( 'NONE', *, *, #37486, .F. ) ;
#8638 = DIRECTION ( 'NONE',  ( 0.000000000000000000, 0.000000000000000000, -1.000000000000000000 ) ) ;
#8639 = CARTESIAN_POINT ( 'NONE',  ( 116.3153332067577850, -32.94059133099460723, 170.1356252759109680 ) ) ;
#8640 = DIRECTION ( 'NONE',  ( 1.000000000000000078E-15, 0.000000000000000000, 1.000000000000000000 ) ) ;
#8641 = PLANE ( 'NONE',  #77096 ) ;
#8642 = CARTESIAN_POINT ( 'NONE',  ( 41.56670390244695312, -36.32844715994109208, 129.9678068554150911 ) ) ;
#8643 = CARTESIAN_POINT ( 'NONE',  ( 115.6112259330891305, -28.51835778375803798, 35.43562527591098643 ) ) ;
#8644 = CARTESIAN_POINT ( 'NONE',  ( 25.56670390244797275, -67.87844715994100397, 178.0928068554149775 ) ) ;
#8645 = VERTEX_POINT ( 'NONE', #57607 ) ;
#8646 = CARTESIAN_POINT ( 'NONE',  ( 127.0664832912740394, -54.72944906728950798, -4.824374724089008915 ) ) ;
#8647 = VECTOR ( 'NONE', #20300, 1000.000000000000000 ) ;
#8648 = LINE ( 'NONE', #49501, #50474 ) ;
#8649 = ORIENTED_EDGE ( 'NONE', *, *, #29402, .F. ) ;
#8650 = ORIENTED_EDGE ( 'NONE', *, *, #22790, .T. ) ;
#8651 = VECTOR ( 'NONE', #58400, 1000.000000000000000 ) ;
#8652 = AXIS2_PLACEMENT_3D ( 'NONE', #25137, #32385, #39655 ) ;
#8653 = CARTESIAN_POINT ( 'NONE',  ( 81.19087023417348803, -21.23918067504819263, 1.822998012174939397 ) ) ;
#8654 = DIRECTION ( 'NONE',  ( -1.000000000000000000, -6.493183223601999383E-14, -1.000000000000000078E-15 ) ) ;
#8655 = DIRECTION ( 'NONE',  ( 0.000000000000000000, 0.000000000000000000, -1.000000000000000000 ) ) ;
#8656 = FACE_BOUND ( 'NONE', #65713, .T. ) ;
#8657 = PLANE ( 'NONE',  #76596 ) ;
#8658 = CARTESIAN_POINT ( 'NONE',  ( 104.4064053327731472, -46.06725273453308489, 216.7781341137909692 ) ) ;
#8659 = CARTESIAN_POINT ( 'NONE',  ( 172.5664832912729878, -27.82844715994070484, 18.92562527591200094 ) ) ;
#8660 = CARTESIAN_POINT ( 'NONE',  ( 124.1141232347067529, 71.87613260885804323, 40.50830340569535792 ) ) ;
#8661 = CARTESIAN_POINT ( 'NONE',  ( 101.6553708923145649, -27.03755641387271069, 105.4937205140069665 ) ) ;
#8662 = ORIENTED_EDGE ( 'NONE', *, *, #2286, .T. ) ;
#8663 = DIRECTION ( 'NONE',  ( -0.7071067811892205457, 0.7071067811838745998, -7.071067811892213774E-16 ) ) ;
#8664 = ORIENTED_EDGE ( 'NONE', *, *, #38112, .F. ) ;
#8665 = AXIS2_PLACEMENT_3D ( 'NONE', #71975, #85616, #85167 ) ;
#8666 = DIRECTION ( 'NONE',  ( 0.000000000000000000, 0.000000000000000000, -1.000000000000000000 ) ) ;
#8667 = COLOUR_RGB ( '', 0.66274510, 0.83137255, 0.94901961) ;
#8668 = CARTESIAN_POINT ( 'NONE',  ( 41.56648329127398966, -27.82844715994070484, 138.9256252759119832 ) ) ;
#8669 = ORIENTED_EDGE ( 'NONE', *, *, #42492, .F. ) ;
#8670 = CARTESIAN_POINT ( 'NONE',  ( -2.852988951225258196E-12, 11.69999999999217977, 8.005813272589510943E-12 ) ) ;
#8671 = ORIENTED_EDGE ( 'NONE', *, *, #59216, .T. ) ;
#8672 = DIRECTION ( 'NONE',  ( -1.000000000000000000, 0.000000000000000000, -1.000000000000000078E-15 ) ) ;
#8673 = VECTOR ( 'NONE', #62687, 1000.000000000000000 ) ;
#8674 = CARTESIAN_POINT ( 'NONE',  ( 115.0388443161213416, -42.90644873051409292, 274.3020457939018115 ) ) ;
#8675 = DIRECTION ( 'NONE',  ( 0.000000000000000000, 1.000000000000000000, 0.000000000000000000 ) ) ;
#8676 = ORIENTED_EDGE ( 'NONE', *, *, #55628, .T. ) ;
#8677 = CARTESIAN_POINT ( 'NONE',  ( 109.9170780819575839, -46.81718586395340509, 72.79562527591099297 ) ) ;
#8678 = CIRCLE ( 'NONE', #4322, 5.041900000000000048 ) ;
#8679 = SURFACE_SIDE_STYLE ('',( #22304 ) ) ;
#8680 = CARTESIAN_POINT ( 'NONE',  ( 97.80409201228124516, -40.49881500342829810, 166.6340252493254752 ) ) ;
#8681 = CARTESIAN_POINT ( 'NONE',  ( 150.8167039024480118, -58.72944715994110254, 10.91780685541479734 ) ) ;
#8682 = ADVANCED_FACE ( 'NONE', ( #30364 ), #44409, .F. ) ;
#8683 = CARTESIAN_POINT ( 'NONE',  ( -12.51828503297007167, 80.89413879163728893, 117.6922344853366127 ) ) ;
#8684 = ORIENTED_EDGE ( 'NONE', *, *, #280, .F. ) ;
#8685 = AXIS2_PLACEMENT_3D ( 'NONE', #9429, #37140, #8088 ) ;
#8686 = EDGE_CURVE ( 'NONE', #9382, #30460, #47147, .T. ) ;
#8687 = DIRECTION ( 'NONE',  ( 0.000000000000000000, 1.000000000000000000, 0.000000000000000000 ) ) ;
#8688 = DIRECTION ( 'NONE',  ( 0.000000000000000000, 0.000000000000000000, -1.000000000000000000 ) ) ;
#8689 = CARTESIAN_POINT ( 'NONE',  ( 162.5667039024471308, -32.29483332967974718, 313.9678068554149490 ) ) ;
#8690 = EDGE_CURVE ( 'NONE', #71713, #16666, #65326, .T. ) ;
#8692 = EDGE_CURVE ( 'NONE', #23885, #31453, #63990, .T. ) ;
#8691 = CARTESIAN_POINT ( 'NONE',  ( 98.44073678691454177, -30.83591204966533894, 116.8499109901969604 ) ) ;
#8693 = B_SPLINE_CURVE_WITH_KNOTS ( 'NONE', 3,
 ( #67204, #5891, #88120, #66759, #25878, #53093, #33584, #18614, #4545, #6327, #74929, #53551, #46296, #53998, #32686, #47643, #81319, #60833 ),
 .UNSPECIFIED., .F., .F.,
 ( 4, 2, 2, 2, 2, 2, 2, 2, 4 ),
 ( 0.000000000000000000, 0.06249962285685504298, 0.1249992457137100860, 0.1874988685705651359, 0.2499984914274201719, 0.3124981142842752080, 0.3749977371411302718, 0.4374973599979852801, 0.4999969828548403439 ),
 .UNSPECIFIED. ) ;
#8695 = DIRECTION ( 'NONE',  ( 1.000000000000000078E-15, -1.000000000000000000, 0.000000000000000000 ) ) ;
#8694 = CYLINDRICAL_SURFACE ( 'NONE', #8768, 10.00000000000000711 ) ;
#8696 = CARTESIAN_POINT ( 'NONE',  ( -487.2989999999999782, 22.53639197104660141, 90.48749999999999716 ) ) ;
#8697 = EDGE_CURVE ( 'NONE', #59609, #24211, #79420, .T. ) ;
#8698 = VERTEX_POINT ( 'NONE', #84894 ) ;
#8700 = ADVANCED_FACE ( 'NONE', ( #85788 ), #43967, .F. ) ;
#8699 = DIRECTION ( 'NONE',  ( -4.299999999999999979E-14, 1.000000000000000000, -4.400000000000000367E-29 ) ) ;
#8701 = CARTESIAN_POINT ( 'NONE',  ( 113.2097911582632292, -29.11871762112829032, 160.5356252759109736 ) ) ;
#8703 = ORIENTED_EDGE ( 'NONE', *, *, #57058, .F. ) ;
#8702 = FACE_OUTER_BOUND ( 'NONE', #44461, .T. ) ;
#8704 = AXIS2_PLACEMENT_3D ( 'NONE', #17853, #43769, #31036 ) ;
#8705 = CARTESIAN_POINT ( 'NONE',  ( 115.3461623907573710, -31.52268719801068642, 30.27276813305296344 ) ) ;
#8706 = LINE ( 'NONE', #10038, #19352 ) ;
#8707 = LINE ( 'NONE', #52993, #51876 ) ;
#8708 = CARTESIAN_POINT ( 'NONE',  ( 97.69261636184602082, -78.35517403977323170, 250.2178068554180470 ) ) ;
#8709 = CARTESIAN_POINT ( 'NONE',  ( 1.598849875094819542E-14, 44.45000000000000284, -130.5560000000000116 ) ) ;
#8710 = EDGE_CURVE ( 'NONE', #13820, #24965, #17181, .T. ) ;
#8711 = TOROIDAL_SURFACE ( 'NONE', #31890, 11.75000000000000000, 2.125000000000000000 ) ;
#8712 = FACE_OUTER_BOUND ( 'NONE', #60714, .T. ) ;
#8713 = CARTESIAN_POINT ( 'NONE',  ( 114.7458293810857128, -30.61868467657531312, 244.3613395616259822 ) ) ;
#8714 = ORIENTED_EDGE ( 'NONE', *, *, #72286, .F. ) ;
#8715 = ORIENTED_EDGE ( 'NONE', *, *, #48760, .T. ) ;
#8716 = ADVANCED_FACE ( 'NONE', ( #36280 ), #1765, .F. ) ;
#8717 = CARTESIAN_POINT ( 'NONE',  ( 99.08321105494920289, -40.57595765811257138, 168.1158690201829700 ) ) ;
#8718 = VECTOR ( 'NONE', #36237, 1000.000000000000000 ) ;
#8719 = DIRECTION ( 'NONE',  ( 1.000000000000000000, 0.000000000000000000, 0.000000000000000000 ) ) ;
#8720 = CARTESIAN_POINT ( 'NONE',  ( 98.47292639957201743, -32.93111785796080682, 52.41491663922997901 ) ) ;
#8721 = CARTESIAN_POINT ( 'NONE',  ( 23.22106422052441133, 86.67941937331816860, 305.2876845235662699 ) ) ;
#8722 = CARTESIAN_POINT ( 'NONE',  ( -458.3598257906459708, 47.62500000000000000, 3.174999999999999822 ) ) ;
#8723 = CIRCLE ( 'NONE', #59460, 13.63963572536219715 ) ;
#8724 = DIRECTION ( 'NONE',  ( 1.067522139062650671E-15, 1.000000000000000000, 0.000000000000000000 ) ) ;
#8725 = FACE_OUTER_BOUND ( 'NONE', #39998, .T. ) ;
#8726 = CARTESIAN_POINT ( 'NONE',  ( 270.8910000000000196, 40.03750000000000142, -7.937500000000000000 ) ) ;
#8727 = CARTESIAN_POINT ( 'NONE',  ( 115.9412561796928429, -30.17946786548967353, 259.3203871806730945 ) ) ;
#8728 = CARTESIAN_POINT ( 'NONE',  ( 11.48301363694224442, 87.75296475977089017, 117.7977433391754118 ) ) ;
#8729 = ORIENTED_EDGE ( 'NONE', *, *, #77481, .F. ) ;
#8730 = ORIENTED_EDGE ( 'NONE', *, *, #38917, .T. ) ;
#8731 = EDGE_CURVE ( 'NONE', #11327, #70447, #71262, .T. ) ;
#8732 = DIRECTION ( 'NONE',  ( -2.900000000000000265E-14, 2.000000000000000155E-15, -1.000000000000000000 ) ) ;
#8733 = CARTESIAN_POINT ( 'NONE',  ( -88.44471653959766400, 93.33860577356858812, -78.95047879920376488 ) ) ;
#8734 = CIRCLE ( 'NONE', #50790, 4.750000000000004441 ) ;
#8735 = DIRECTION ( 'NONE',  ( 0.000000000000000000, -1.000000000000000000, 0.000000000000000000 ) ) ;
#8737 = ADVANCED_FACE ( 'NONE', ( #70192 ), #7964, .F. ) ;
#8736 = CARTESIAN_POINT ( 'NONE',  ( 103.1875000000000000, 117.4749999999999943, 3.602774393244745134E-13 ) ) ;
#8738 = CARTESIAN_POINT ( 'NONE',  ( 97.32756240345236165, -42.09278592124177010, 22.72705384733897205 ) ) ;
#8739 = DIRECTION ( 'NONE',  ( 0.000000000000000000, 0.000000000000000000, 1.000000000000000000 ) ) ;
#8740 = VERTEX_POINT ( 'NONE', #48371 ) ;
#8741 = CARTESIAN_POINT ( 'NONE',  ( 103.9444121564427235, -47.38074615057520589, 58.33753003781600199 ) ) ;
#8742 = FACE_OUTER_BOUND ( 'NONE', #64337, .T. ) ;
#8743 = CARTESIAN_POINT ( 'NONE',  ( 100.8231516252168234, -45.85084492350206631, 242.1108633711489517 ) ) ;
#8744 = VERTEX_POINT ( 'NONE', #62022 ) ;
#8745 = VECTOR ( 'NONE', #82403, 1000.000000000000000 ) ;
#8746 = DIRECTION ( 'NONE',  ( -7.559289460184342508E-16, 0.7559289460184340781, -0.6546536707080007345 ) ) ;
#8747 = CARTESIAN_POINT ( 'NONE',  ( 115.0382687573691527, -42.90718446363899830, 19.30286595434970209 ) ) ;
#8748 = DIRECTION ( 'NONE',  ( 0.000000000000000000, 0.000000000000000000, -1.000000000000000000 ) ) ;
#8749 = CARTESIAN_POINT ( 'NONE',  ( 112.4846873277006267, -29.98081840548436006, 117.3442808457819666 ) ) ;
#8750 = CARTESIAN_POINT ( 'NONE',  ( 95.38360599640527937, -38.85844429501600672, 197.4699109901969791 ) ) ;
#8751 = DIRECTION ( 'NONE',  ( 0.000000000000000000, 0.000000000000000000, -1.000000000000000000 ) ) ;
#8752 = VERTEX_POINT ( 'NONE', #27953 ) ;
#8753 = CYLINDRICAL_SURFACE ( 'NONE', #52313, 3.250000000000002665 ) ;
#8754 = VECTOR ( 'NONE', #25014, 1000.000000000000000 ) ;
#8755 = ORIENTED_EDGE ( 'NONE', *, *, #71273, .T. ) ;
#8756 = ORIENTED_EDGE ( 'NONE', *, *, #62994, .F. ) ;
#8757 = EDGE_CURVE ( 'NONE', #36458, #75252, #56552, .T. ) ;
#8758 = FACE_BOUND ( 'NONE', #60618, .T. ) ;
#8759 = EDGE_LOOP ( 'NONE', ( #15462, #58081, #53631, #61782 ) ) ;
#8760 = ORIENTED_EDGE ( 'NONE', *, *, #24177, .F. ) ;
#8761 = PLANE ( 'NONE',  #54111 ) ;
#8762 = CARTESIAN_POINT ( 'NONE',  ( 109.7225942113134067, -27.00020313397157423, 24.86497719015990882 ) ) ;
#8763 = CARTESIAN_POINT ( 'NONE',  ( 112.7360809596688966, -29.66769577629168353, 118.9486103042669782 ) ) ;
#8764 = CARTESIAN_POINT ( 'NONE',  ( 118.6786315247609167, -39.21782601141705271, 258.6584824187679033 ) ) ;
#8765 = AXIS2_PLACEMENT_3D ( 'NONE', #53918, #5815, #11725 ) ;
#8766 = CARTESIAN_POINT ( 'NONE',  ( -7.399926448127667200, 72.22026871922481916, 130.3465752436562468 ) ) ;
#8767 = VERTEX_POINT ( 'NONE', #28863 ) ;
#8768 = AXIS2_PLACEMENT_3D ( 'NONE', #22314, #62287, #42281 ) ;
#8769 = ORIENTED_EDGE ( 'NONE', *, *, #39109, .F. ) ;
#8770 = CARTESIAN_POINT ( 'NONE',  ( 150.5667039024483529, -47.82844715993594775, 249.9678068554149490 ) ) ;
#8771 = DIRECTION ( 'NONE',  ( -0.7071067812152160847, 0.7071067811578790607, 0.000000000000000000 ) ) ;
#8772 = CARTESIAN_POINT ( 'NONE',  ( 70.65700412096775551, -139.5313073890320368, 247.3443455604209760 ) ) ;
#8773 = EDGE_CURVE ( 'NONE', #4701, #24255, #13884, .T. ) ;
#8774 = AXIS2_PLACEMENT_3D ( 'NONE', #17804, #38243, #3727 ) ;
#8775 = CARTESIAN_POINT ( 'NONE',  ( 109.7815504499144339, -47.49240650911489325, 92.78514908543495210 ) ) ;
#8776 = CARTESIAN_POINT ( 'NONE',  ( -103.1875000000000000, 127.0000000000000000, -1.080832317973422076E-12 ) ) ;
#8777 = EDGE_LOOP ( 'NONE', ( #27747, #33110, #33191, #81616 ) ) ;
#8778 = UNCERTAINTY_MEASURE_WITH_UNIT (LENGTH_MEASURE( 1.000000000000000082E-05 ), #5078, 'distance_accuracy_value', 'NONE');
#8779 = CARTESIAN_POINT ( 'NONE',  ( 96.88875151864165503, -30.65867585538550344, 280.8984824187682534 ) ) ;
#8780 = LINE ( 'NONE', #8323, #31223 ) ;
#8781 = CARTESIAN_POINT ( 'NONE',  ( -487.2989999999999782, 101.9113919710471947, 11.11250000000054072 ) ) ;
#8782 = CARTESIAN_POINT ( 'NONE',  ( 172.5667039024478129, -36.32844715993500273, 300.4678068554149490 ) ) ;
#8783 = ADVANCED_FACE ( 'NONE', ( #7519 ), #48825, .T. ) ;
#8785 = FACE_OUTER_BOUND ( 'NONE', #9630, .T. ) ;
#8784 = LINE ( 'NONE', #70554, #17265 ) ;
#8786 = CARTESIAN_POINT ( 'NONE',  ( 97.81170242524891023, -40.51743837274789684, 121.6354095930283137 ) ) ;
#8787 = EDGE_CURVE ( 'NONE', #64021, #49178, #15291, .T. ) ;
#8788 = DIRECTION ( 'NONE',  ( 0.7759704746411385523, -0.6307692307692301936, 0.000000000000000000 ) ) ;
#8789 = CARTESIAN_POINT ( 'NONE',  ( 131.9720459102087489, -38.52018918697933714, 7.480061334670521589 ) ) ;
#8790 = AXIS2_PLACEMENT_3D ( 'NONE', #41784, #89066, #13654 ) ;
#8791 = EDGE_CURVE ( 'NONE', #49629, #51345, #55894, .T. ) ;
#8792 = CARTESIAN_POINT ( 'NONE',  ( 0.000000000000000000, 20.32000000000000028, 0.000000000000000000 ) ) ;
#8793 = CARTESIAN_POINT ( 'NONE',  ( 46.48091746482047171, -48.32844715994088602, 129.9678068554150911 ) ) ;
#8794 = DIRECTION ( 'NONE',  ( -1.000000000000000000, 1.122464679914735423E-15, 0.000000000000000000 ) ) ;
#8796 = EDGE_LOOP ( 'NONE', ( #37537, #4238 ) ) ;
#8795 = FACE_OUTER_BOUND ( 'NONE', #50182, .T. ) ;
#8797 = ADVANCED_FACE ( 'NONE', ( #70650 ), #83379, .F. ) ;
#8798 = CARTESIAN_POINT ( 'NONE',  ( 97.69261636184624820, -130.2017202801087876, 250.2178068554180470 ) ) ;
#8799 = CARTESIAN_POINT ( 'NONE',  ( 96.64195684025510502, -42.47035700268206426, 26.72705384733997747 ) ) ;
#8800 = CARTESIAN_POINT ( 'NONE',  ( 101.7695353289030322, -45.70857994070590991, 158.1527681330539963 ) ) ;
#8801 = CARTESIAN_POINT ( 'NONE',  ( 111.4245298313290107, -46.22390286880558818, 23.91848241876792969 ) ) ;
#8802 = STYLED_ITEM ( 'NONE', ( #50984 ), #28324 ) ;
#8804 = CARTESIAN_POINT ( 'NONE',  ( 82.79255470691698804, -36.36732994130517227, 6.785344856283535897 ) ) ;
#8803 = CYLINDRICAL_SURFACE ( 'NONE', #21801, 7.199999999999998401 ) ;
#8805 = CARTESIAN_POINT ( 'NONE',  ( 116.3212776292297406, -32.94146857471347545, 140.1356252759109680 ) ) ;
#8806 = ADVANCED_FACE ( 'NONE', ( #62918 ), #250, .F. ) ;
#8807 = VERTEX_POINT ( 'NONE', #29316 ) ;
#8808 = DIRECTION ( 'NONE',  ( -1.000000000000000000, -8.540177112501204385E-16, 0.000000000000000000 ) ) ;
#8809 = VERTEX_POINT ( 'NONE', #42022 ) ;
#8810 = EDGE_CURVE ( 'NONE', #32576, #20813, #1158, .T. ) ;
#8811 = AXIS2_PLACEMENT_3D ( 'NONE', #84031, #9508, #85831 ) ;
#8812 = CARTESIAN_POINT ( 'NONE',  ( 99.60253261678104764, -31.60088882024776780, 165.2819436375999658 ) ) ;
#8813 = ORIENTED_EDGE ( 'NONE', *, *, #25368, .T. ) ;
#8814 = VECTOR ( 'NONE', #9792, 1000.000000000000000 ) ;
#8815 = CARTESIAN_POINT ( 'NONE',  ( 72.96458098368701428, 127.0000000000000000, -72.96458098368670164 ) ) ;
#8816 = CARTESIAN_POINT ( 'NONE',  ( 98.27975524859429868, -42.29919363830185119, 182.7756252759109543 ) ) ;
#8817 = DIRECTION ( 'NONE',  ( 0.000000000000000000, -1.000000000000000000, 0.000000000000000000 ) ) ;
#8818 = DIRECTION ( 'NONE',  ( 1.000000000000000078E-15, 1.000000000000000083E-30, -1.000000000000000000 ) ) ;
#8819 = CARTESIAN_POINT ( 'NONE',  ( 0.000000000000000000, 101.5999999999999943, 0.000000000000000000 ) ) ;
#8820 = DIRECTION ( 'NONE',  ( 0.000000000000000000, 0.000000000000000000, -1.000000000000000000 ) ) ;
#8821 = ADVANCED_FACE ( 'NONE', ( #696 ), #28360, .T. ) ;
#8822 = CARTESIAN_POINT ( 'NONE',  ( 147.0667039036620451, -137.6784471587259020, 245.4218662566639750 ) ) ;
#8823 = CARTESIAN_POINT ( 'NONE',  ( 110.8996159922621842, -45.96566293992800922, 97.88950923702800822 ) ) ;
#8824 = CARTESIAN_POINT ( 'NONE',  ( 116.9564367646783722, -33.61053620760070260, 129.0575300378169743 ) ) ;
#8825 = VERTEX_POINT ( 'NONE', #22501 ) ;
#8826 = AXIS2_PLACEMENT_3D ( 'NONE', #80781, #60302, #11270 ) ;
#8827 = VERTEX_POINT ( 'NONE', #27507 ) ;
#8828 = CARTESIAN_POINT ( 'NONE',  ( 106.6003420031022415, -27.34545878416701115, 41.55967854399195005 ) ) ;
#8829 = DIRECTION ( 'NONE',  ( 1.000000000000000078E-15, 0.000000000000000000, -1.000000000000000000 ) ) ;
#8831 = LINE ( 'NONE', #22450, #63570 ) ;
#8830 = CARTESIAN_POINT ( 'NONE',  ( 116.8431970675091662, -40.18699730018602168, 174.5680062282909546 ) ) ;
#8832 = DIRECTION ( 'NONE',  ( 0.000000000000000000, 0.000000000000000000, 1.000000000000000000 ) ) ;
#8833 = CARTESIAN_POINT ( 'NONE',  ( 115.0889048001385646, -30.61763654108453281, 110.3441337246927674 ) ) ;
#8834 = DIRECTION ( 'NONE',  ( 0.000000000000000000, 0.000000000000000000, -1.000000000000000000 ) ) ;
#8835 = LINE ( 'NONE', #51038, #44903 ) ;
#8836 = CARTESIAN_POINT ( 'NONE',  ( 4.055565339044333584, 70.61339494146574225, 118.4872713058879441 ) ) ;
#8837 = CARTESIAN_POINT ( 'NONE',  ( 117.5859182825552978, -33.41202194707543782, 129.0575300378159795 ) ) ;
#8838 = ORIENTED_EDGE ( 'NONE', *, *, #15556, .T. ) ;
#8839 = ORIENTED_EDGE ( 'NONE', *, *, #79967, .F. ) ;
#8840 = EDGE_LOOP ( 'NONE', ( #73351, #26546, #41726, #34278, #45152, #42465 ) ) ;
#8841 = AXIS2_PLACEMENT_3D ( 'NONE', #68562, #18159, #45843 ) ;
#8842 = VECTOR ( 'NONE', #62070, 1000.000000000000000 ) ;
#8843 = DIRECTION ( 'NONE',  ( 0.000000000000000000, 1.000000000000000000, 0.000000000000000000 ) ) ;
#8844 = CARTESIAN_POINT ( 'NONE',  ( 145.4407362117956097, -69.39660493469676794, 247.4650063441803809 ) ) ;
#8845 = CARTESIAN_POINT ( 'NONE',  ( 97.81168839172025287, -40.51739946886939947, 131.6358419732753475 ) ) ;
#8847 = ADVANCED_FACE ( 'NONE', ( #77015 ), #77914, .T. ) ;
#8846 = LINE ( 'NONE', #37428, #84515 ) ;
#8848 = CARTESIAN_POINT ( 'NONE',  ( 99.55502339443899018, -39.99451353983162960, 229.4709475124479638 ) ) ;
#8849 = AXIS2_PLACEMENT_3D ( 'NONE', #6755, #48503, #55328 ) ;
#8850 = DIRECTION ( 'NONE',  ( 0.000000000000000000, 0.000000000000000000, 1.000000000000000000 ) ) ;
#8851 = CARTESIAN_POINT ( 'NONE',  ( 96.01388918828124019, -36.58377270012555726, 156.3280062282919687 ) ) ;
#8852 = DIRECTION ( 'NONE',  ( 1.000000000000000000, 6.493183223601999383E-14, 9.351236661543306751E-17 ) ) ;
#8853 = ORIENTED_EDGE ( 'NONE', *, *, #79635, .F. ) ;
#8855 = ORIENTED_EDGE ( 'NONE', *, *, #24492, .F. ) ;
#8854 = ORIENTED_EDGE ( 'NONE', *, *, #78387, .F. ) ;
#8856 = AXIS2_PLACEMENT_3D ( 'NONE', #58442, #24828, #80256 ) ;
#8857 = PLANE ( 'NONE',  #25890 ) ;
#8858 = ORIENTED_EDGE ( 'NONE', *, *, #75266, .F. ) ;
#8859 = VERTEX_POINT ( 'NONE', #49735 ) ;
#8860 = CARTESIAN_POINT ( 'NONE',  ( 162.9033555647771436, -33.89581943344378345, 342.9256252759109884 ) ) ;
#8861 = CARTESIAN_POINT ( 'NONE',  ( 131.6146038193916468, -35.48272374590327871, 7.134497377245147653 ) ) ;
#8862 = VECTOR ( 'NONE', #20825, 1000.000000000000000 ) ;
#8863 = CARTESIAN_POINT ( 'NONE',  ( 101.8980524138101345, -43.06915566006364315, 9.850947512448971821 ) ) ;
#8864 = CARTESIAN_POINT ( 'NONE',  ( 205.0097499999990305, 52.73749999999999716, -49.21249999999999858 ) ) ;
#8865 = ORIENTED_EDGE ( 'NONE', *, *, #87411, .T. ) ;
#8866 = EDGE_CURVE ( 'NONE', #18132, #14582, #70387, .T. ) ;
#8867 = CARTESIAN_POINT ( 'NONE',  ( 115.8629299651497035, -40.02386399094653058, 9.635625275910941312 ) ) ;
#8868 = CARTESIAN_POINT ( 'NONE',  ( 172.5667039024480118, -36.32844715993499563, 180.4678068554150059 ) ) ;
#8869 = EDGE_LOOP ( 'NONE', ( #26561, #21478, #18962, #3621 ) ) ;
#8870 = ORIENTED_EDGE ( 'NONE', *, *, #6399, .F. ) ;
#8871 = EDGE_CURVE ( 'NONE', #12810, #31262, #83835, .T. ) ;
#8872 = CARTESIAN_POINT ( 'NONE',  ( 99.08985776380760058, -42.79589758595945170, 111.8440019053259391 ) ) ;
#8873 = EDGE_LOOP ( 'NONE', ( #44938, #65304 ) ) ;
#8874 = VERTEX_POINT ( 'NONE', #14796 ) ;
#8875 = CIRCLE ( 'NONE', #53752, 175.7032523735949781 ) ;
#8876 = CARTESIAN_POINT ( 'NONE',  ( 99.16797791762762415, -38.78938375721887155, 274.3480903695913184 ) ) ;
#8877 = CARTESIAN_POINT ( 'NONE',  ( 117.8019377669635190, -34.00081044253764162, 169.0365776568629599 ) ) ;
#8878 = AXIS2_PLACEMENT_3D ( 'NONE', #39164, #40051, #19615 ) ;
#8879 = CARTESIAN_POINT ( 'NONE',  ( 99.11802762103501152, -45.48540990049890809, 156.9899109901969609 ) ) ;
#8880 = DIRECTION ( 'NONE',  ( 0.000000000000000000, 1.000000000000000000, 0.000000000000000000 ) ) ;
#8881 = CARTESIAN_POINT ( 'NONE',  ( 104.1858290503737408, -26.67344577167302688, 221.2984824187679465 ) ) ;
#8882 = CARTESIAN_POINT ( 'NONE',  ( 151.0371591254584871, -46.82818131005592477, 180.4678068554149775 ) ) ;
#8883 = DIRECTION ( 'NONE',  ( 1.000000000000000000, 1.000000000000000078E-15, -0.000000000000000000 ) ) ;
#8884 = ORIENTED_EDGE ( 'NONE', *, *, #74509, .F. ) ;
#8885 = CARTESIAN_POINT ( 'NONE',  ( -130.5560612649026666, 69.84937019662270075, 0.8297548318613829910 ) ) ;
#8886 = EDGE_LOOP ( 'NONE', ( #17390, #83813, #44144, #69741 ) ) ;
#8887 = ORIENTED_EDGE ( 'NONE', *, *, #38171, .T. ) ;
#8888 = CIRCLE ( 'NONE', #14650, 0.5000000000000004441 ) ;
#8889 = VECTOR ( 'NONE', #48143, 1000.000000000000000 ) ;
#8890 = CARTESIAN_POINT ( 'NONE',  ( 98.51514891278741004, -45.00612994150532842, 191.9384824187679612 ) ) ;
#8891 = ORIENTED_EDGE ( 'NONE', *, *, #42690, .F. ) ;
#8892 = CARTESIAN_POINT ( 'NONE',  ( 103.8073253818723316, -26.82667379764869153, 165.3299109901969643 ) ) ;
#8893 = DIRECTION ( 'NONE',  ( 4.299999999999999979E-14, -1.000000000000000000, 4.400000000000000367E-29 ) ) ;
#8894 = CARTESIAN_POINT ( 'NONE',  ( 91.91125933621934507, -107.5284471599419049, -21.78219314458190681 ) ) ;
#8895 = CARTESIAN_POINT ( 'NONE',  ( 0.000000000000000000, 100.5999999999999659, 0.000000000000000000 ) ) ;
#8898 = CARTESIAN_POINT ( 'NONE',  ( 116.0363244534468237, -41.99923036749492411, 234.4041967044819899 ) ) ;
#8897 = CARTESIAN_POINT ( 'NONE',  ( 97.86538016267786588, -40.64618032142375625, 56.64632583547473388 ) ) ;
#8896 = DIRECTION ( 'NONE',  ( 0.000000000000000000, 0.000000000000000000, 1.000000000000000000 ) ) ;
#8899 = CARTESIAN_POINT ( 'NONE',  ( 51.06648329127400388, 19.62155284005901024, 333.4006252759110112 ) ) ;
#8900 = EDGE_CURVE ( 'NONE', #462, #7080, #13848, .T. ) ;
#8901 = PLANE ( 'NONE',  #67044 ) ;
#8902 = CARTESIAN_POINT ( 'NONE',  ( 112.1356898331065537, -28.01072921633739554, 270.6563675837870164 ) ) ;
#8903 = EDGE_CURVE ( 'NONE', #48200, #21095, #17022, .T. ) ;
#8904 = CARTESIAN_POINT ( 'NONE',  ( 3.175000000000334666, 111.1250000000000000, -31.75000000000000000 ) ) ;
#8905 = ADVANCED_FACE ( 'NONE', ( #17463 ), #2056, .F. ) ;
#8906 = CARTESIAN_POINT ( 'NONE',  ( 0.000000000000000000, 2.269999999999994245, -9.525000000000000355 ) ) ;
#8907 = CYLINDRICAL_SURFACE ( 'NONE', #78190, 2.030000000001807248 ) ;
#8908 = AXIS2_PLACEMENT_3D ( 'NONE', #35616, #70145, #89258 ) ;
#8910 = VERTEX_POINT ( 'NONE', #85635 ) ;
#8909 = CARTESIAN_POINT ( 'NONE',  ( 115.4825246836782640, -36.90214395232434441, 195.5838068554167535 ) ) ;
#8911 = ADVANCED_FACE ( 'NONE', ( #78375 ), #10638, .T. ) ;
#8912 = CARTESIAN_POINT ( 'NONE',  ( -103.1875000000000000, 127.0000000000000000, -7.143750000001079847 ) ) ;
#8913 = CARTESIAN_POINT ( 'NONE',  ( 103.8004457107024194, -26.80577029241926112, 165.3299109901969643 ) ) ;
#8914 = CARTESIAN_POINT ( 'NONE',  ( 97.26643838138058129, -31.61739275409173544, 86.93181575210095957 ) ) ;
#8915 = CARTESIAN_POINT ( 'NONE',  ( 98.50201126197670476, -30.70924794336980668, 201.8384824187679385 ) ) ;
#8916 = CARTESIAN_POINT ( 'NONE',  ( 134.0664832912740110, -46.72944715994100306, -0.8743747240890020755 ) ) ;
#8917 = CARTESIAN_POINT ( 'NONE',  ( 138.8167039024479834, -50.82844715994100682, 33.40080685541480676 ) ) ;
#8919 = CARTESIAN_POINT ( 'NONE',  ( 31.75000000000000000, 17.78000000000000114, 3.174999999999999822 ) ) ;
#8918 = DIRECTION ( 'NONE',  ( 0.6537961156249325612, 0.7071067811865220376, -0.2693522585644785305 ) ) ;
#8920 = CARTESIAN_POINT ( 'NONE',  ( 97.31584371032013792, -39.30597597718078617, 71.53145860744848505 ) ) ;
#8921 = LINE ( 'NONE', #83416, #33493 ) ;
#8922 = ORIENTED_EDGE ( 'NONE', *, *, #49156, .T. ) ;
#8923 = AXIS2_PLACEMENT_3D ( 'NONE', #50209, #28430, #36611 ) ;
#8924 = CARTESIAN_POINT ( 'NONE',  ( 97.81315821180474757, -40.51681016098617505, 66.63608906629065132 ) ) ;
#8925 = ADVANCED_FACE ( 'NONE', ( #16137 ), #30204, .T. ) ;
#8926 = VERTEX_POINT ( 'NONE', #57898 ) ;
#8927 = ORIENTED_EDGE ( 'NONE', *, *, #21621, .T. ) ;
#8928 = ADVANCED_FACE ( 'NONE', ( #10201 ), #51950, .F. ) ;
#8930 = ORIENTED_EDGE ( 'NONE', *, *, #36053, .T. ) ;
#8929 = DIRECTION ( 'NONE',  ( 0.000000000000000000, 0.000000000000000000, -1.000000000000000000 ) ) ;
#8931 = CARTESIAN_POINT ( 'NONE',  ( 106.0785370228625055, -48.51385081415330092, 108.5099109901969712 ) ) ;
#8932 = DIRECTION ( 'NONE',  ( 0.000000000000000000, 0.000000000000000000, -1.000000000000000000 ) ) ;
#8933 = AXIS2_PLACEMENT_3D ( 'NONE', #78393, #86976, #37923 ) ;
#8934 = CARTESIAN_POINT ( 'NONE',  ( 52.38749999999999574, 94.53880000000000905, 225.4249999999999829 ) ) ;
#8935 = FACE_OUTER_BOUND ( 'NONE', #49948, .T. ) ;
#8936 = CARTESIAN_POINT ( 'NONE',  ( 116.8435662018514307, -36.99793375417353758, 43.80419670448193159 ) ) ;
#8937 = ORIENTED_EDGE ( 'NONE', *, *, #49035, .F. ) ;
#8938 = ORIENTED_EDGE ( 'NONE', *, *, #10937, .F. ) ;
#8939 = ORIENTED_EDGE ( 'NONE', *, *, #89621, .F. ) ;
#8940 = FACE_OUTER_BOUND ( 'NONE', #79633, .T. ) ;
#8941 = DIRECTION ( 'NONE',  ( 0.7071067811571405404, 0.7071067812159546051, 0.000000000000000000 ) ) ;
#8942 = CARTESIAN_POINT ( 'NONE',  ( 142.8696205427243626, 0.6543191929522288453, 540.9756252759101471 ) ) ;
#8943 = FACE_OUTER_BOUND ( 'NONE', #20353, .T. ) ;
#8944 = DIRECTION ( 'NONE',  ( 0.000000000000000000, 0.000000000000000000, -1.000000000000000000 ) ) ;
#8945 = CARTESIAN_POINT ( 'NONE',  ( 99.09592356364612442, -30.55014542244788700, 51.80351315582143457 ) ) ;
#8946 = VECTOR ( 'NONE', #1653, 1000.000000000000000 ) ;
#8947 = CARTESIAN_POINT ( 'NONE',  ( -11.93153746469517884, 86.90202483595902549, 130.0097012715444862 ) ) ;
#8948 = CARTESIAN_POINT ( 'NONE',  ( 100.4791399132688809, -44.80881982087489490, 12.03276813305398463 ) ) ;
#8949 = EDGE_LOOP ( 'NONE', ( #85518, #2182, #67689, #32378, #40237 ) ) ;
#8950 = DIRECTION ( 'NONE',  ( 1.000000000000000000, 1.000000000000000078E-15, -0.000000000000000000 ) ) ;
#8951 = CIRCLE ( 'NONE', #16208, 2.030000000000003801 ) ;
#8953 = EDGE_CURVE ( 'NONE', #26697, #53561, #31522, .T. ) ;
#8952 = CYLINDRICAL_SURFACE ( 'NONE', #13358, 11.57110091390434903 ) ;
#8954 = CARTESIAN_POINT ( 'NONE',  ( 98.87701435734486211, -36.85308710711977653, 134.1566617981629577 ) ) ;
#8955 = AXIS2_PLACEMENT_3D ( 'NONE', #65380, #36785, #29077 ) ;
#8956 = EDGE_CURVE ( 'NONE', #64680, #13607, #78666, .T. ) ;
#8957 = DIRECTION ( 'NONE',  ( 0.000000000000000000, 1.000000000000000000, 0.000000000000000000 ) ) ;
#8958 = DIRECTION ( 'NONE',  ( -0.000000000000000000, 1.000000000000000000, -0.000000000000000000 ) ) ;
#8959 = ORIENTED_EDGE ( 'NONE', *, *, #7652, .T. ) ;
#8960 = VERTEX_POINT ( 'NONE', #64721 ) ;
#8961 = CARTESIAN_POINT ( 'NONE',  ( 164.9667039024459996, -28.27351298637401200, -5.074374724088000832 ) ) ;
#8962 = EDGE_LOOP ( 'NONE', ( #82259, #47216, #39376, #70405 ) ) ;
#8963 = VERTEX_POINT ( 'NONE', #85188 ) ;
#8964 = VECTOR ( 'NONE', #60745, 1000.000000000000000 ) ;
#8965 = CARTESIAN_POINT ( 'NONE',  ( 108.8812380984771835, -28.05563920549329993, 136.3444404487549662 ) ) ;
#8966 = DIRECTION ( 'NONE',  ( 0.000000000000000000, 0.000000000000000000, 1.000000000000000000 ) ) ;
#8967 = CARTESIAN_POINT ( 'NONE',  ( 98.07812720205548374, -31.40528397058157850, 81.90133956162493689 ) ) ;
#8968 = VECTOR ( 'NONE', #63293, 1000.000000000000000 ) ;
#8969 = CARTESIAN_POINT ( 'NONE',  ( 101.9936209174699258, -45.44607152528067928, 83.15645860711320836 ) ) ;
#8970 = ORIENTED_EDGE ( 'NONE', *, *, #39952, .F. ) ;
#8971 = ADVANCED_FACE ( 'NONE', ( #71989 ), #52385, .F. ) ;
#8972 = ORIENTED_EDGE ( 'NONE', *, *, #28236, .T. ) ;
#8973 = VERTEX_POINT ( 'NONE', #51077 ) ;
#8974 = TOROIDAL_SURFACE ( 'NONE', #87291, 36.57600000000000051, 1.524000000000000021 ) ;
#8975 = CARTESIAN_POINT ( 'NONE',  ( 100.1721853667017825, -41.09961673838238028, 184.5938046553059735 ) ) ;
#8976 = CARTESIAN_POINT ( 'NONE',  ( 113.4288541212755348, -27.66216098611360152, 84.57753003781698453 ) ) ;
#8977 = ORIENTED_EDGE ( 'NONE', *, *, #88960, .F. ) ;
#8978 = CARTESIAN_POINT ( 'NONE',  ( 118.7081646409642133, -34.65111545711807395, 48.96705384733895983 ) ) ;
#8979 = CARTESIAN_POINT ( 'NONE',  ( 96.59701100649584760, -36.21046171878319342, 167.2870538473399620 ) ) ;
#8980 = CARTESIAN_POINT ( 'NONE',  ( 173.9900000000000091, 37.33800000000000097, 69.13087104677069306 ) ) ;
#8981 = DIRECTION ( 'NONE',  ( 0.000000000000000000, 0.000000000000000000, -1.000000000000000000 ) ) ;
#8982 = CARTESIAN_POINT ( 'NONE',  ( 96.02786343543940006, -37.29764797185995207, 117.3794347997199594 ) ) ;
#8983 = VECTOR ( 'NONE', #32322, 1000.000000000000000 ) ;
#8984 = FACE_OUTER_BOUND ( 'NONE', #929, .T. ) ;
#8985 = ORIENTED_EDGE ( 'NONE', *, *, #84507, .F. ) ;
#8986 = FACE_BOUND ( 'NONE', #61, .T. ) ;
#8987 = ORIENTED_CLOSED_SHELL ( 'NONE', *, #31468, .F. );
#8988 = EDGE_LOOP ( 'NONE', ( #78923, #43522, #2486, #39731 ) ) ;
#8989 = PLANE ( 'NONE',  #69429 ) ;
#8990 = ORIENTED_EDGE ( 'NONE', *, *, #60455, .F. ) ;
#8991 = ORIENTED_EDGE ( 'NONE', *, *, #40768, .F. ) ;
#8992 = PLANE ( 'NONE',  #76544 ) ;
#8993 = DIRECTION ( 'NONE',  ( 0.000000000000000000, 1.000000000000000000, 0.000000000000000000 ) ) ;
#8994 = CARTESIAN_POINT ( 'NONE',  ( 97.48652011608379553, -32.61680585812226241, 16.00419670448194154 ) ) ;
#8995 = CARTESIAN_POINT ( 'NONE',  ( 116.3212776292267989, -32.94146857470629186, 109.1356252759109680 ) ) ;
#8996 = DIRECTION ( 'NONE',  ( 0.000000000000000000, -1.000000000000000000, 0.000000000000000000 ) ) ;
#8997 = CARTESIAN_POINT ( 'NONE',  ( 97.35451824726682446, -37.88753622196094994, 41.42133956162496844 ) ) ;
#8999 = CARTESIAN_POINT ( 'NONE',  ( 108.2752786314947286, -47.69320359391959840, 153.6518157521009584 ) ) ;
#8998 = CARTESIAN_POINT ( 'NONE',  ( 104.4896289049376605, -26.97888955764241814, 110.2814849738620069 ) ) ;
#9000 = FACE_OUTER_BOUND ( 'NONE', #48637, .T. ) ;
#9001 = EDGE_CURVE ( 'NONE', #30523, #73517, #78817, .T. ) ;
#9002 = FACE_OUTER_BOUND ( 'NONE', #71931, .T. ) ;
#9003 = ORIENTED_EDGE ( 'NONE', *, *, #13599, .F. ) ;
#9004 = LINE ( 'NONE', #30773, #56989 ) ;
#9005 = CARTESIAN_POINT ( 'NONE',  ( 8.748570571408911079E-16, 127.0000000000000000, -96.04375000000000284 ) ) ;
#9006 = LINE ( 'NONE', #36251, #13747 ) ;
#9008 = ORIENTED_EDGE ( 'NONE', *, *, #77478, .T. ) ;
#9007 = EDGE_CURVE ( 'NONE', #29697, #34694, #9759, .T. ) ;
#9009 = DIRECTION ( 'NONE',  ( 0.000000000000000000, 1.000000000000000000, 0.000000000000000000 ) ) ;
#9011 = ORIENTED_EDGE ( 'NONE', *, *, #6692, .T. ) ;
#9010 = CARTESIAN_POINT ( 'NONE',  ( 115.0114139542580318, -28.97761122332106964, 194.4537205140059370 ) ) ;
#9012 = EDGE_CURVE ( 'NONE', #27479, #49045, #30647, .T. ) ;
#9013 = FACE_OUTER_BOUND ( 'NONE', #79748, .T. ) ;
#9014 = CARTESIAN_POINT ( 'NONE',  ( 101.6393319275751992, -45.65599671332518028, 243.1413395616249886 ) ) ;
#9015 = CARTESIAN_POINT ( 'NONE',  ( 117.3817195963474518, -32.63147225404833307, 95.13943479972097350 ) ) ;
#9016 = LINE ( 'NONE', #29901, #60622 ) ;
#9017 = AXIS2_PLACEMENT_3D ( 'NONE', #26749, #89901, #55334 ) ;
#9018 = DIRECTION ( 'NONE',  ( 0.9586846635221889512, 0.000000000000000000, -0.2844709403917162205 ) ) ;
#9019 = CARTESIAN_POINT ( 'NONE',  ( 70.56670390244700286, -67.87844715994098976, 55.21780685541800437 ) ) ;
#9020 = VERTEX_POINT ( 'NONE', #27008 ) ;
#9021 = AXIS2_PLACEMENT_3D ( 'NONE', #24719, #65606, #12780 ) ;
#9022 = VERTEX_POINT ( 'NONE', #33819 ) ;
#9023 = ORIENTED_EDGE ( 'NONE', *, *, #46375, .T. ) ;
#9024 = ADVANCED_FACE ( 'NONE', ( #20648 ), #40171, .T. ) ;
#9025 = ORIENTED_EDGE ( 'NONE', *, *, #59757, .F. ) ;
#9026 = CARTESIAN_POINT ( 'NONE',  ( 168.3595971214449207, -48.62134037892947447, 129.9678068554150059 ) ) ;
#9027 = CARTESIAN_POINT ( 'NONE',  ( 107.5100279102752552, -47.14509671329473406, 233.6099109901969655 ) ) ;
#9028 = DIRECTION ( 'NONE',  ( 0.000000000000000000, 0.000000000000000000, 1.000000000000000000 ) ) ;
#9029 = EDGE_CURVE ( 'NONE', #74702, #47878, #46532, .T. ) ;
#9030 = CARTESIAN_POINT ( 'NONE',  ( 194.0371591254585155, -46.82818131005407736, 129.9678068554150343 ) ) ;
#9031 = CIRCLE ( 'NONE', #46727, 190.5000000000000000 ) ;
#9033 = CARTESIAN_POINT ( 'NONE',  ( 86.13269706310835261, 70.27900073646853230, 81.46681417397539349 ) ) ;
#9032 = CARTESIAN_POINT ( 'NONE',  ( 188.5667039024482960, -42.82844715993431350, 259.7178068554150059 ) ) ;
#9034 = DIRECTION ( 'NONE',  ( 0.000000000000000000, -1.000000000000000000, 0.000000000000000000 ) ) ;
#9035 = CARTESIAN_POINT ( 'NONE',  ( 114.1055592783800137, -46.29424852498188869, 33.08133956162495792 ) ) ;
#9036 = ORIENTED_EDGE ( 'NONE', *, *, #30296, .F. ) ;
#9037 = VERTEX_POINT ( 'NONE', #60159 ) ;
#9038 = ORIENTED_EDGE ( 'NONE', *, *, #6562, .F. ) ;
#9039 = AXIS2_PLACEMENT_3D ( 'NONE', #9867, #72095, #31183 ) ;
#9040 = CARTESIAN_POINT ( 'NONE',  ( 100.5881272547050429, -39.38103216960048059, -2.364374724089013391 ) ) ;
#9041 = LINE ( 'NONE', #48986, #46279 ) ;
#9042 = CARTESIAN_POINT ( 'NONE',  ( 101.4562479827646371, -44.74122725731964323, 278.0899109901961879 ) ) ;
#9043 = AXIS2_PLACEMENT_3D ( 'NONE', #44383, #9886, #24849 ) ;
#9044 = DIRECTION ( 'NONE',  ( 1.000000000000000000, 1.000000000000000078E-15, -0.000000000000000000 ) ) ;
#9045 = CARTESIAN_POINT ( 'NONE',  ( 103.4440497394146092, -45.85039829771042719, 113.2756252759109827 ) ) ;
#9046 = VECTOR ( 'NONE', #27312, 1000.000000000000114 ) ;
#9047 = CARTESIAN_POINT ( 'NONE',  ( 116.7947425855253130, -39.38919346347031336, 28.61468008947841568 ) ) ;
#9048 = ORIENTED_EDGE ( 'NONE', *, *, #61121, .T. ) ;
#9049 = CARTESIAN_POINT ( 'NONE',  ( 0.000000000000000000, 12.27000000000000313, 0.000000000000000000 ) ) ;
#9050 = CARTESIAN_POINT ( 'NONE',  ( 77.59184326792608033, -35.51852171453446516, 2.740177351673668937 ) ) ;
#9051 = ORIENTED_EDGE ( 'NONE', *, *, #24870, .T. ) ;
#9052 = FACE_OUTER_BOUND ( 'NONE', #86603, .T. ) ;
#9053 = CARTESIAN_POINT ( 'NONE',  ( 101.9087497524793804, -29.77971984236790703, 33.41475703625796001 ) ) ;
#9054 = LINE ( 'NONE', #16754, #40643 ) ;
#9055 = EDGE_CURVE ( 'NONE', #65784, #88397, #42900, .T. ) ;
#9056 = DIRECTION ( 'NONE',  ( 0.000000000000000000, 0.000000000000000000, -1.000000000000000000 ) ) ;
#9057 = DIRECTION ( 'NONE',  ( 1.000000000000000000, 0.000000000000000000, 0.000000000000000000 ) ) ;
#9058 = ORIENTED_EDGE ( 'NONE', *, *, #7035, .F. ) ;
#9059 = DIRECTION ( 'NONE',  ( 1.000000000000000078E-15, 0.000000000000000000, -1.000000000000000000 ) ) ;
#9060 = CARTESIAN_POINT ( 'NONE',  ( 164.9667039024459996, -26.71338133339301635, 342.9256252759119548 ) ) ;
#9061 = ORIENTED_EDGE ( 'NONE', *, *, #13025, .T. ) ;
#9062 = CARTESIAN_POINT ( 'NONE',  ( 109.9110735108787793, -46.79593677437021881, 72.79562527591099297 ) ) ;
#9063 = ORIENTED_EDGE ( 'NONE', *, *, #61454, .T. ) ;
#9064 = CARTESIAN_POINT ( 'NONE',  ( 111.0503013157718044, -29.17396400730615369, 59.11241982807696616 ) ) ;
#9065 = DIRECTION ( 'NONE',  ( -3.491483361109380094E-15, 0.000000000000000000, -1.000000000000000000 ) ) ;
#9066 = CARTESIAN_POINT ( 'NONE',  ( 98.96845470676149148, -30.25173782105007803, 195.7775300378159784 ) ) ;
#9067 = CARTESIAN_POINT ( 'NONE',  ( -20.41604128349800007, 45.08960384674290367, 32.16949814425970544 ) ) ;
#9068 = CARTESIAN_POINT ( 'NONE',  ( 107.0664832912748068, -36.72944715993923381, 14.92562527591097066 ) ) ;
#9069 = DIRECTION ( 'NONE',  ( 0.000000000000000000, 0.000000000000000000, 1.000000000000000000 ) ) ;
#9070 = DIRECTION ( 'NONE',  ( 1.000000000000000078E-15, -1.000000000000000083E-30, -1.000000000000000000 ) ) ;
#9071 = CARTESIAN_POINT ( 'NONE',  ( 114.4457317200277089, -27.39361268404408634, 270.5441967044823741 ) ) ;
#9072 = ORIENTED_EDGE ( 'NONE', *, *, #20266, .T. ) ;
#9073 = CIRCLE ( 'NONE', #53956, 0.9999999999991942001 ) ;
#9074 = DIRECTION ( 'NONE',  ( 0.000000000000000000, 1.000000000000000000, 0.000000000000000000 ) ) ;
#9075 = EDGE_LOOP ( 'NONE', ( #73691, #80111, #44227, #16782, #27296 ) ) ;
#9076 = CARTESIAN_POINT ( 'NONE',  ( 117.0748215982922176, -30.29170057715430531, 140.2813395616249750 ) ) ;
#9077 = ADVANCED_FACE ( 'NONE', ( #48312, #19743 ), #41070, .F. ) ;
#9078 = CARTESIAN_POINT ( 'NONE',  ( 142.8832909413445122, -79.11588146349311046, 394.9756252759100903 ) ) ;
#9079 = ORIENTED_EDGE ( 'NONE', *, *, #38806, .F. ) ;
#9080 = ORIENTED_EDGE ( 'NONE', *, *, #79136, .T. ) ;
#9081 = VERTEX_POINT ( 'NONE', #53784 ) ;
#9082 = CARTESIAN_POINT ( 'NONE',  ( -55.48342271751670296, 101.5999999999999943, 171.1197181046785261 ) ) ;
#9083 = DIRECTION ( 'NONE',  ( 0.9999999853157766072, 0.0001713722456143218888, -0.000000000000000000 ) ) ;
#9084 = DIRECTION ( 'NONE',  ( 0.000000000000000000, 0.000000000000000000, -1.000000000000000000 ) ) ;
#9085 = DIRECTION ( 'NONE',  ( 1.000000000000000000, -5.337610695313248426E-16, 0.000000000000000000 ) ) ;
#9086 = DIRECTION ( 'NONE',  ( 0.000000000000000000, 0.000000000000000000, -1.000000000000000000 ) ) ;
#9087 = CARTESIAN_POINT ( 'NONE',  ( 118.2085198165198676, -40.76548936363617059, 19.54991099019698453 ) ) ;
#9088 = EDGE_CURVE ( 'NONE', #23895, #63431, #34258, .T. ) ;
#9089 = VECTOR ( 'NONE', #89726, 1000.000000000000000 ) ;
#9090 = CARTESIAN_POINT ( 'NONE',  ( 83.73314995794051185, 12.92155284005802685, 336.5756252759109657 ) ) ;
#9091 = EDGE_LOOP ( 'NONE', ( #36094, #41540 ) ) ;
#9092 = CARTESIAN_POINT ( 'NONE',  ( 101.3372171518963398, -46.20893634704900421, 198.1318157521009482 ) ) ;
#9093 = ADVANCED_FACE ( 'NONE', ( #75156 ), #38338, .T. ) ;
#9094 = CARTESIAN_POINT ( 'NONE',  ( 115.0372571628051048, -42.90846324673419332, 43.30193824323413310 ) ) ;
#9095 = ORIENTED_EDGE ( 'NONE', *, *, #23860, .T. ) ;
#9096 = VERTEX_POINT ( 'NONE', #5224 ) ;
#9097 = AXIS2_PLACEMENT_3D ( 'NONE', #41460, #14683, #70081 ) ;
#9098 = DIRECTION ( 'NONE',  ( 0.000000000000000000, 1.000000000000000000, 0.000000000000000000 ) ) ;
#9099 = DIRECTION ( 'NONE',  ( -6.493183223601999383E-14, 1.000000000000000000, -2.193183223602000424E-29 ) ) ;
#9100 = DIRECTION ( 'NONE',  ( -3.491483361109380094E-15, 0.000000000000000000, -1.000000000000000000 ) ) ;
#9101 = EDGE_CURVE ( 'NONE', #28081, #17066, #88357, .T. ) ;
#9102 = CARTESIAN_POINT ( 'NONE',  ( -103.1875000000000000, 101.5999999999999943, 5.041899999998910253 ) ) ;
#9103 = FACE_OUTER_BOUND ( 'NONE', #16025, .T. ) ;
#9104 = CARTESIAN_POINT ( 'NONE',  ( 98.55846751192062527, -35.97459669770627499, 230.6781341137909465 ) ) ;
#9107 = CARTESIAN_POINT ( 'NONE',  ( 97.82856912889593559, -29.34641599088761765, 41.78991099019596334 ) ) ;
#9106 = DIRECTION ( 'NONE',  ( 0.000000000000000000, 1.000000000000000000, 0.000000000000000000 ) ) ;
#9105 = VECTOR ( 'NONE', #58256, 1000.000000000000000 ) ;
#9108 = CARTESIAN_POINT ( 'NONE',  ( 68.06670390244705970, -121.7784471599409954, 55.21780685541800437 ) ) ;
#9109 = CARTESIAN_POINT ( 'NONE',  ( 111.0995558192250456, -25.53287967237518430, 99.80133956162498521 ) ) ;
#9110 = VERTEX_POINT ( 'NONE', #12038 ) ;
#9111 = CARTESIAN_POINT ( 'NONE',  ( 131.5555141844761522, -19.85480617632529743, 7.067502061084848464 ) ) ;
#9112 = VERTEX_POINT ( 'NONE', #54226 ) ;
#9113 = DIRECTION ( 'NONE',  ( 1.000000000000000000, 0.000000000000000000, 0.000000000000000000 ) ) ;
#9114 = CARTESIAN_POINT ( 'NONE',  ( 103.9854521423141875, -27.20984610156289207, 276.3255691088649542 ) ) ;
#9116 = VERTEX_POINT ( 'NONE', #87894 ) ;
#9115 = EDGE_CURVE ( 'NONE', #16229, #54739, #7009, .T. ) ;
#9117 = CARTESIAN_POINT ( 'NONE',  ( 41.56670390244689628, -36.32844715994109208, 180.4678068554150911 ) ) ;
#9118 = EDGE_LOOP ( 'NONE', ( #16068, #24050, #85374, #45043 ) ) ;
#9119 = DIRECTION ( 'NONE',  ( 0.000000000000000000, 0.000000000000000000, 1.000000000000000000 ) ) ;
#9120 = DIRECTION ( 'NONE',  ( 0.000000000000000000, 0.000000000000000000, 1.000000000000000000 ) ) ;
#9121 = DIRECTION ( 'NONE',  ( 0.9999999853157766072, 0.0001713722456133601202, -9.999999853157765648E-16 ) ) ;
#9122 = ORIENTED_EDGE ( 'NONE', *, *, #84900, .T. ) ;
#9123 = CARTESIAN_POINT ( 'NONE',  ( 116.9960073371140652, -33.48122977351050622, 89.07848241876791917 ) ) ;
#9124 = CARTESIAN_POINT ( 'NONE',  ( 97.70660944625170430, -40.25144590732936933, 166.6128667725130299 ) ) ;
#9125 = CARTESIAN_POINT ( 'NONE',  ( 70.63919639214310564, 65.60000000000000853, -53.97512327982435210 ) ) ;
#9126 = FACE_OUTER_BOUND ( 'NONE', #79650, .T. ) ;
#9127 = VERTEX_POINT ( 'NONE', #81988 ) ;
#9128 = EDGE_CURVE ( 'NONE', #7579, #9112, #70461, .T. ) ;
#9129 = CIRCLE ( 'NONE', #16390, 0.5000000000000004441 ) ;
#9130 = CARTESIAN_POINT ( 'NONE',  ( 46.03715912545348488, -48.62818131006090283, 117.4678068554150485 ) ) ;
#9131 = ADVANCED_FACE ( 'NONE', ( #13824 ), #12489, .T. ) ;
#9132 = CARTESIAN_POINT ( 'NONE',  ( 184.5664832912729878, -71.37844715994266664, 361.9756252759109998 ) ) ;
#9133 = EDGE_CURVE ( 'NONE', #87762, #45263, #82080, .T. ) ;
#9134 = CARTESIAN_POINT ( 'NONE',  ( 131.0667039024480118, -61.87844715994100397, 207.5838068554149913 ) ) ;
#9135 = EDGE_CURVE ( 'NONE', #47300, #27344, #25310, .T. ) ;
#9137 = CARTESIAN_POINT ( 'NONE',  ( 107.0667039024470313, -104.2784471599421323, -21.78219314458201694 ) ) ;
#9136 = DIRECTION ( 'NONE',  ( 0.1858654558203329255, -0.9825752044157738396, 0.000000000000000000 ) ) ;
#9138 = LINE ( 'NONE', #57256, #77084 ) ;
#9139 = B_SPLINE_CURVE_WITH_KNOTS ( 'NONE', 3,
 ( #78753, #16506, #44185, #65971, #86007, #86448, #3763, #51881, #58707, #79195, #36510, #29683, #9246, #79636, #10134, #44633, #72804, #85120, #50563, #78305, #37842, #3323, #16067, #43748, #20085, #4656, #81432, #4209, #12828, #33705, #66873, #25537, #74146, #40512, #53212, #25094, #11921, #26884, #81871, #73697, #39609, #19622, #47758, #11012, #74587, #61396, #47309, #67314, #39171, #38717, #75041, #60494, #68233, #5104, #32799, #32341, #6014, #60043, #89125, #26442, #66420 ),
 .UNSPECIFIED., .F., .F.,
 ( 4, 2, 2, 2, 1, 1, 1, 2, 2, 2, 2, 1, 1, 1, 1, 1, 2, 2, 2, 2, 2, 2, 2, 1, 1, 1, 1, 2, 2, 2, 2, 1, 1, 1, 2, 2, 2, 4 ),
 ( 0.000000000000000000, 0.1249999999998101241, 0.1874999999997149780, 0.2187499999996670441, 0.2343749999996433686, 0.2421874999996319611, 0.2460937499996265487, 0.2480468749996235234, 0.2499999999996205258, 0.3124999999995198285, 0.3437499999994693689, 0.3593749999994442779, 0.3671874999994313438, 0.3710937499994253486, 0.3730468749994229061, 0.3740234374994215738, 0.3745117187494213518, 0.3749999999994211297, 0.4374999999993766098, 0.4999999999993320898, 0.5624999999992875699, 0.5937499999992651434, 0.6093749999992530419, 0.6171874999992470467, 0.6210937499992429389, 0.6230468749992407185, 0.6240234374992398303, 0.6245117187492407185, 0.6249999999992417177, 0.6874999999993813837, 0.7187499999994504396, 0.7343749999994850786, 0.7421874999995022870, 0.7460937499995110578, 0.7480468749995142774, 0.7499999999995174971, 0.8749999999997587485, 1.000000000000000000 ),
 .UNSPECIFIED. ) ;
#9140 = VERTEX_POINT ( 'NONE', #81103 ) ;
#9141 = CARTESIAN_POINT ( 'NONE',  ( -446.0240000000000009, 93.66249999999999432, 90.48749999999999716 ) ) ;
#9142 = CARTESIAN_POINT ( 'NONE',  ( 113.2764755850017480, -45.03455287549797248, 184.0994347997199725 ) ) ;
#9144 = ORIENTED_EDGE ( 'NONE', *, *, #74811, .F. ) ;
#9143 = CARTESIAN_POINT ( 'NONE',  ( 67.06670390244700286, -67.87844716047356997, 245.4920193514540188 ) ) ;
#9145 = CARTESIAN_POINT ( 'NONE',  ( 111.8051046833288353, -27.50533224649500497, 15.71086337114796549 ) ) ;
#9146 = DIRECTION ( 'NONE',  ( 0.000000000000000000, 0.000000000000000000, -1.000000000000000000 ) ) ;
#9147 = DIRECTION ( 'NONE',  ( 0.000000000000000000, -1.000000000000000000, 0.000000000000000000 ) ) ;
#9148 = CARTESIAN_POINT ( 'NONE',  ( 109.6408691443087804, -46.48062605549592519, 12.78166324958517919 ) ) ;
#9149 = CARTESIAN_POINT ( 'NONE',  ( -446.0240000000000009, 3.174999999999999822, 50.79999999999999716 ) ) ;
#9150 = CARTESIAN_POINT ( 'NONE',  ( 106.3491918589965763, -46.48387837312656501, 222.5184824187689401 ) ) ;
#9151 = ORIENTED_EDGE ( 'NONE', *, *, #22173, .T. ) ;
#9152 = ORIENTED_EDGE ( 'NONE', *, *, #21504, .F. ) ;
#9153 = CARTESIAN_POINT ( 'NONE',  ( 115.6736222539786638, -40.49689781175994341, 204.9177737820879486 ) ) ;
#9154 = VECTOR ( 'NONE', #28074, 1000.000000000000000 ) ;
#9155 = CARTESIAN_POINT ( 'NONE',  ( 134.0664832912740110, 0.2215528400590013880, 2.408125275911999097 ) ) ;
#9156 = CARTESIAN_POINT ( 'NONE',  ( 111.8905564713631549, -28.66688903671830246, 51.09110711541997318 ) ) ;
#9157 = CARTESIAN_POINT ( 'NONE',  ( -94.61941200740652391, 94.84315624882771090, 89.95943163722139957 ) ) ;
#9158 = AXIS2_PLACEMENT_3D ( 'NONE', #2387, #1036, #63260 ) ;
#9159 = ADVANCED_FACE ( 'NONE', ( #18850 ), #60613, .F. ) ;
#9160 = AXIS2_PLACEMENT_3D ( 'NONE', #16933, #38695, #24629 ) ;
#9161 = CARTESIAN_POINT ( 'NONE',  ( 102.3035641816324102, -89.52844715994213232, -21.78219314458246103 ) ) ;
#9162 = FACE_OUTER_BOUND ( 'NONE', #49253, .T. ) ;
#9163 = VERTEX_POINT ( 'NONE', #35148 ) ;
#9164 = DIRECTION ( 'NONE',  ( -0.7071067811865171526, -0.7071067811865779928, -7.071067811865164719E-16 ) ) ;
#9165 = CARTESIAN_POINT ( 'NONE',  ( 97.70656171685999425, -40.25131786594292294, 37.61256612285666989 ) ) ;
#9166 = CARTESIAN_POINT ( 'NONE',  ( 96.27200394136420414, -34.46162041542910970, 261.1737205140064475 ) ) ;
#9167 = CARTESIAN_POINT ( 'NONE',  ( 143.0667039024470171, -90.27844715994091018, 222.2178068554179902 ) ) ;
#9168 = ORIENTED_EDGE ( 'NONE', *, *, #31013, .F. ) ;
#9169 = EDGE_LOOP ( 'NONE', ( #51584, #84923, #18907, #86107 ) ) ;
#9170 = CARTESIAN_POINT ( 'NONE',  ( 100.8874678751566165, -44.70022136795945755, 82.05229194164871842 ) ) ;
#9171 = CARTESIAN_POINT ( 'NONE',  ( 177.4809174648214309, -49.32844715993478957, 249.9678068554149775 ) ) ;
#9172 = CARTESIAN_POINT ( 'NONE',  ( 41.56648329127381203, -27.82844715994070484, 201.9256252759119832 ) ) ;
#9173 = DIRECTION ( 'NONE',  ( 0.000000000000000000, 1.000000000000000000, 0.000000000000000000 ) ) ;
#9174 = CARTESIAN_POINT ( 'NONE',  ( 97.95204982468537480, -33.09064556074058316, 37.02419670448192335 ) ) ;
#9175 = CARTESIAN_POINT ( 'NONE',  ( 10.01454489833087003, 74.85873851776135268, 117.9324610216481517 ) ) ;
#9176 = ORIENTED_EDGE ( 'NONE', *, *, #36504, .F. ) ;
#9177 = CARTESIAN_POINT ( 'NONE',  ( 99.03245663461365211, -44.38790092286875932, 32.92038718067297509 ) ) ;
#9178 = EDGE_CURVE ( 'NONE', #21130, #70069, #22894, .T. ) ;
#9179 = DIRECTION ( 'NONE',  ( -4.299999999999999979E-14, 1.000000000000000000, -4.400000000000000367E-29 ) ) ;
#9180 = AXIS2_PLACEMENT_3D ( 'NONE', #75373, #18610, #46292 ) ;
#9181 = CARTESIAN_POINT ( 'NONE',  ( 97.46629803964546568, -32.60812463323921406, 16.00419670448194154 ) ) ;
#9182 = EDGE_CURVE ( 'NONE', #13694, #21258, #48768, .T. ) ;
#9183 = EDGE_LOOP ( 'NONE', ( #68958, #35707, #79608, #71525 ) ) ;
#9184 = EDGE_CURVE ( 'NONE', #78468, #61208, #22336, .T. ) ;
#9185 = VECTOR ( 'NONE', #18966, 1000.000000000000000 ) ;
#9186 = DIRECTION ( 'NONE',  ( 0.3535533905932722321, 0.6123724356958172299, 0.7071067811865286989 ) ) ;
#9187 = CARTESIAN_POINT ( 'NONE',  ( 183.5150000000000148, 14.63749999999999929, -9.525000000000000355 ) ) ;
#9188 = FACE_OUTER_BOUND ( 'NONE', #53338, .T. ) ;
#9189 = CARTESIAN_POINT ( 'NONE',  ( 98.90423600646026614, -36.64316113183544843, 109.1366617981629474 ) ) ;
#9190 = CARTESIAN_POINT ( 'NONE',  ( 110.1438736645959580, -26.08919931346192911, 210.8403871806729626 ) ) ;
#9191 = EDGE_CURVE ( 'NONE', #81699, #76096, #56487, .T. ) ;
#9192 = LINE ( 'NONE', #76884, #76923 ) ;
#9193 = VERTEX_POINT ( 'NONE', #41955 ) ;
#9194 = EDGE_CURVE ( 'NONE', #71111, #35866, #73358, .T. ) ;
#9195 = DIRECTION ( 'NONE',  ( 0.000000000000000000, 1.047445008332813989E-14, -1.000000000000000000 ) ) ;
#9196 = VERTEX_POINT ( 'NONE', #34708 ) ;
#9197 = VERTEX_POINT ( 'NONE', #7901 ) ;
#9198 = ADVANCED_FACE ( 'NONE', ( #84231 ), #21090, .T. ) ;
#9199 = AXIS2_PLACEMENT_3D ( 'NONE', #196, #41510, #82443 ) ;
#9200 = CARTESIAN_POINT ( 'NONE',  ( 107.0664832912739968, -8.350947159940998787, 333.4006252759120343 ) ) ;
#9201 = ORIENTED_EDGE ( 'NONE', *, *, #34828, .T. ) ;
#9202 = EDGE_LOOP ( 'NONE', ( #48581, #80882, #34303, #83240 ) ) ;
#9203 = DIRECTION ( 'NONE',  ( -0.9825752044165969590, -0.1858654558159821002, 0.000000000000000000 ) ) ;
#9204 = ADVANCED_FACE ( 'NONE', ( #1991 ), #52818, .T. ) ;
#9205 = CARTESIAN_POINT ( 'NONE',  ( 104.9213734224019987, -26.94988814155465207, 41.24833046483934851 ) ) ;
#9206 = CARTESIAN_POINT ( 'NONE',  ( 113.3268105416314171, -43.27322076882862945, 112.5943245899819516 ) ) ;
#9207 = CARTESIAN_POINT ( 'NONE',  ( 109.2165397428488376, -48.40897078886088423, 277.7213395616254843 ) ) ;
#9208 = DIRECTION ( 'NONE',  ( 1.000000000000000000, 4.299999999999999979E-14, 1.000000000000000078E-15 ) ) ;
#9210 = ORIENTED_EDGE ( 'NONE', *, *, #24168, .T. ) ;
#9209 = EDGE_CURVE ( 'NONE', #54183, #78471, #29690, .T. ) ;
#9211 = VERTEX_POINT ( 'NONE', #3770 ) ;
#9212 = CARTESIAN_POINT ( 'NONE',  ( 33.96670390244699433, -26.71338133339301635, -5.074374724088000832 ) ) ;
#9213 = CARTESIAN_POINT ( 'NONE',  ( 97.81281252356875200, -40.52015776331121089, 277.6356251289804504 ) ) ;
#9214 = CARTESIAN_POINT ( 'NONE',  ( 70.21108942365968630, -140.4774569966043885, 246.4394912367985739 ) ) ;
#9215 = CIRCLE ( 'NONE', #71606, 10.00000000000000888 ) ;
#9216 = CARTESIAN_POINT ( 'NONE',  ( 102.3593652026347343, -47.65646955129418672, 287.2527681330535643 ) ) ;
#9217 = ORIENTED_EDGE ( 'NONE', *, *, #61350, .T. ) ;
#9218 = APPLICATION_CONTEXT ( 'automotive_design' ) ;
#9219 = CARTESIAN_POINT ( 'NONE',  ( 105.7763445623522500, -26.38427570067176831, 270.1756252759109884 ) ) ;
#9220 = CARTESIAN_POINT ( 'NONE',  ( 107.0664832912739399, -36.72944715994095333, 302.7856252759109452 ) ) ;
#9221 = VECTOR ( 'NONE', #43143, 1000.000000000000000 ) ;
#9222 = CARTESIAN_POINT ( 'NONE',  ( 21.03715912545829880, -47.82818131006185780, 237.4678068554150059 ) ) ;
#9224 = CARTESIAN_POINT ( 'NONE',  ( 69.30126767323736203, -138.7022917610363777, 247.3064795105084102 ) ) ;
#9223 = LINE ( 'NONE', #72343, #47705 ) ;
#9225 = DIRECTION ( 'NONE',  ( 2.900000000000000265E-14, -2.000000000000000155E-15, 1.000000000000000000 ) ) ;
#9226 = CARTESIAN_POINT ( 'NONE',  ( 135.5667039024470455, -118.2784471599408960, 51.21780685541800437 ) ) ;
#9227 = CARTESIAN_POINT ( 'NONE',  ( 131.4346950876521589, -37.52719034724653113, 6.916533740478220338 ) ) ;
#9228 = CARTESIAN_POINT ( 'NONE',  ( 97.06107110476884259, -37.99641202601070233, 12.42729194741101750 ) ) ;
#9229 = FACE_BOUND ( 'NONE', #1303, .T. ) ;
#9230 = EDGE_CURVE ( 'NONE', #60102, #37281, #77727, .T. ) ;
#9231 = CYLINDRICAL_SURFACE ( 'NONE', #73299, 9.999999999999998224 ) ;
#9232 = CARTESIAN_POINT ( 'NONE',  ( -179.8898777604649979, 0.000000000000000000, 122.9960808104842016 ) ) ;
#9233 = CARTESIAN_POINT ( 'NONE',  ( 113.7702145813751571, -29.06794043779556347, 289.5032443235301116 ) ) ;
#9234 = CARTESIAN_POINT ( 'NONE',  ( 106.9749963086187279, -47.15413504876184447, 183.5699109901969734 ) ) ;
#9235 = CARTESIAN_POINT ( 'NONE',  ( 99.74686247383996829, -44.23293585951837059, 17.96133956162493206 ) ) ;
#9236 = EDGE_CURVE ( 'NONE', #32634, #45956, #85000, .T. ) ;
#9238 = CARTESIAN_POINT ( 'NONE',  ( 82.19340217262779902, -34.98608769071991276, 7.448832051635564611 ) ) ;
#9237 = CARTESIAN_POINT ( 'NONE',  ( 263.3306968374159851, 52.73749999999999716, -2.032000000000000028 ) ) ;
#9239 = CARTESIAN_POINT ( 'NONE',  ( 81.33214528239159335, -34.28157797492866621, 1.873071231920440560 ) ) ;
#9240 = VECTOR ( 'NONE', #71291, 1000.000000000000000 ) ;
#9241 = AXIS2_PLACEMENT_3D ( 'NONE', #70346, #57144, #83531 ) ;
#9242 = ORIENTED_EDGE ( 'NONE', *, *, #76000, .T. ) ;
#9243 = DIRECTION ( 'NONE',  ( 4.012088370409549976E-14, -1.000000000000000000, 0.000000000000000000 ) ) ;
#9244 = ORIENTED_EDGE ( 'NONE', *, *, #38935, .F. ) ;
#9245 = CARTESIAN_POINT ( 'NONE',  ( 101.5072281473882612, -27.97539281467255279, 61.51467289495899138 ) ) ;
#9247 = ORIENTED_EDGE ( 'NONE', *, *, #60667, .F. ) ;
#9246 = CARTESIAN_POINT ( 'NONE',  ( 4.836742537503020856, 94.29291739919693782, 130.4663756832428305 ) ) ;
#9248 = VECTOR ( 'NONE', #82071, 1000.000000000000000 ) ;
#9249 = CARTESIAN_POINT ( 'NONE',  ( 104.4077974134580415, -46.45800023490631503, 48.36476695192959596 ) ) ;
#9250 = CARTESIAN_POINT ( 'NONE',  ( 96.69582475441080760, -35.54038568221479011, 202.2356252759109623 ) ) ;
#9251 = DIRECTION ( 'NONE',  ( 0.7071067811865434649, 0.7071067811865516806, 7.071067811865440820E-16 ) ) ;
#9252 = CARTESIAN_POINT ( 'NONE',  ( 100.8874001080617830, -44.70016547043675814, 147.0523531915934541 ) ) ;
#9253 = CARTESIAN_POINT ( 'NONE',  ( 97.07208990303480789, -35.37826891733848811, 151.2194583338160783 ) ) ;
#9254 = DIRECTION ( 'NONE',  ( 0.000000000000000000, 0.000000000000000000, 1.000000000000000000 ) ) ;
#9255 = CARTESIAN_POINT ( 'NONE',  ( 112.0305244341996342, -48.74436686551289455, 289.6356252759107406 ) ) ;
#9256 = CARTESIAN_POINT ( 'NONE',  ( 98.54768855250307524, -41.97703652509544980, 96.76583743525021930 ) ) ;
#9257 = CARTESIAN_POINT ( 'NONE',  ( 105.0928733274061670, -25.78792777683064585, 125.2184824187689856 ) ) ;
#9258 = ORIENTED_EDGE ( 'NONE', *, *, #69074, .T. ) ;
#9259 = ORIENTED_EDGE ( 'NONE', *, *, #65988, .F. ) ;
#9260 = AXIS2_PLACEMENT_3D ( 'NONE', #51058, #78355, #84721 ) ;
#9261 = CARTESIAN_POINT ( 'NONE',  ( 115.1135551441502258, -33.01825958633261848, 100.6015833058969378 ) ) ;
#9262 = DIRECTION ( 'NONE',  ( 0.7071067810573865575, 0.7071067813157084769, 7.071067810573858582E-16 ) ) ;
#9264 = CARTESIAN_POINT ( 'NONE',  ( 205.0097499999990305, 52.73749999999999716, -44.45000000000000284 ) ) ;
#9263 = CARTESIAN_POINT ( 'NONE',  ( 109.8674951572811267, -26.74480306206640989, 215.8708633711489711 ) ) ;
#9265 = CARTESIAN_POINT ( 'NONE',  ( 132.2857443282839824, -83.77844715994092439, 45.21780685541799727 ) ) ;
#9266 = CARTESIAN_POINT ( 'NONE',  ( 109.7248605079479518, -27.00080355044804037, 110.8650604066596941 ) ) ;
#9267 = DIRECTION ( 'NONE',  ( 1.000000000000000000, 0.000000000000000000, 0.000000000000000000 ) ) ;
#9268 = CARTESIAN_POINT ( 'NONE',  ( 31.56670390244760327, -32.29483332968575837, 313.9678068554150059 ) ) ;
#9269 = CARTESIAN_POINT ( 'NONE',  ( 12.60000000000000497, 81.71666160541465729, 117.8845415480757879 ) ) ;
#9270 = CARTESIAN_POINT ( 'NONE',  ( 105.3199149336540046, -48.42511963160334432, 147.4584824187679715 ) ) ;
#9271 = VERTEX_POINT ( 'NONE', #78760 ) ;
#9272 = ORIENTED_EDGE ( 'NONE', *, *, #78745, .F. ) ;
#9273 = ORIENTED_EDGE ( 'NONE', *, *, #40956, .F. ) ;
#9274 = PLANE ( 'NONE',  #48755 ) ;
#9275 = DIRECTION ( 'NONE',  ( 0.5000000000000061062, 0.000000000000000000, -0.8660254037844351549 ) ) ;
#9276 = CARTESIAN_POINT ( 'NONE',  ( 97.80412695053506411, -40.49890085506758908, 131.6340326293677663 ) ) ;
#9277 = DIRECTION ( 'NONE',  ( 1.000000000000000000, -1.387778780781444413E-13, 0.000000000000000000 ) ) ;
#9278 = CARTESIAN_POINT ( 'NONE',  ( 97.84965203270614609, -37.79993896977983070, 234.2366617981629702 ) ) ;
#9279 = EDGE_CURVE ( 'NONE', #89264, #2491, #10578, .T. ) ;
#9280 = VECTOR ( 'NONE', #18363, 1000.000000000000000 ) ;
#9281 = CARTESIAN_POINT ( 'NONE',  ( 115.7831043715999613, -41.80231542608780870, 269.4064580736135781 ) ) ;
#9282 = EDGE_CURVE ( 'NONE', #611, #50783, #45776, .T. ) ;
#9283 = CARTESIAN_POINT ( 'NONE',  ( 114.3440588962603215, -29.21527388614784115, 174.4641967044819637 ) ) ;
#9284 = EDGE_CURVE ( 'NONE', #5969, #27916, #52325, .T. ) ;
#9285 = CARTESIAN_POINT ( 'NONE',  ( 69.63919639214310564, 101.5999999999999943, 56.85413200336908801 ) ) ;
#9286 = ORIENTED_EDGE ( 'NONE', *, *, #44441, .F. ) ;
#9288 = VERTEX_POINT ( 'NONE', #66427 ) ;
#9287 = ORIENTED_EDGE ( 'NONE', *, *, #4054, .T. ) ;
#9289 = EDGE_CURVE ( 'NONE', #66368, #28588, #45086, .T. ) ;
#9290 = LINE ( 'NONE', #28375, #11431 ) ;
#9291 = ORIENTED_EDGE ( 'NONE', *, *, #74697, .T. ) ;
#9292 = VERTEX_POINT ( 'NONE', #31024 ) ;
#9293 = CARTESIAN_POINT ( 'NONE',  ( -487.2989999999999782, 6.038608028953049711, 90.48749999999999716 ) ) ;
#9294 = CARTESIAN_POINT ( 'NONE',  ( 83.96770390244803650, -18.82844715994099971, 199.5838068554169524 ) ) ;
#9295 = CARTESIAN_POINT ( 'NONE',  ( 116.4478251454372923, -36.21277458701120366, 270.3139642582781335 ) ) ;
#9296 = EDGE_CURVE ( 'NONE', #57531, #81381, #37507, .T. ) ;
#9297 = CARTESIAN_POINT ( 'NONE',  ( 101.9936199353088995, -45.44607096256550705, 272.1564585177210915 ) ) ;
#9298 = ORIENTED_EDGE ( 'NONE', *, *, #89274, .T. ) ;
#9299 = CARTESIAN_POINT ( 'NONE',  ( 106.8296037779400081, -44.95279291948936873, 9.635625275910939536 ) ) ;
#9300 = DIRECTION ( 'NONE',  ( -4.093947403305260305E-16, 1.000000000000000000, -6.162975822039159109E-32 ) ) ;
#9301 = EDGE_LOOP ( 'NONE', ( #39882, #88682, #62816, #26599, #52697 ) ) ;
#9302 = ORIENTED_EDGE ( 'NONE', *, *, #66389, .T. ) ;
#9303 = EDGE_CURVE ( 'NONE', #46763, #44762, #71927, .T. ) ;
#9304 = VECTOR ( 'NONE', #2364, 1000.000000000000000 ) ;
#9305 = CARTESIAN_POINT ( 'NONE',  ( 116.3225472244029817, -32.94146556017791738, 114.1356252759109822 ) ) ;
#9306 = VERTEX_POINT ( 'NONE', #59164 ) ;
#9307 = ORIENTED_EDGE ( 'NONE', *, *, #60712, .T. ) ;
#9308 = CONICAL_SURFACE ( 'NONE', #16567, 8.928100000000000591, 1.029744258676653645 ) ;
#9309 = EDGE_CURVE ( 'NONE', #25396, #42066, #79202, .T. ) ;
#9310 = CARTESIAN_POINT ( 'NONE',  ( 114.0673224709094598, -30.00197523691782209, 38.85813411379096749 ) ) ;
#9312 = CARTESIAN_POINT ( 'NONE',  ( 97.98778932149404852, -30.38336575973633913, 160.8289586092449497 ) ) ;
#9311 = CIRCLE ( 'NONE', #25309, 0.5000000000000197620 ) ;
#9313 = CARTESIAN_POINT ( 'NONE',  ( 102.3703197837810279, -46.01248081495484854, 127.2041967044829960 ) ) ;
#9314 = CARTESIAN_POINT ( 'NONE',  ( 95.29510253380274776, -38.09663793710245017, 232.4184824187679794 ) ) ;
#9315 = CARTESIAN_POINT ( 'NONE',  ( 105.7155902736374600, -46.72387562369726766, 98.47046800182013726 ) ) ;
#9316 = CARTESIAN_POINT ( 'NONE',  ( 97.33769884349207757, -34.07164404254515944, 127.1148388564199934 ) ) ;
#9317 = CARTESIAN_POINT ( 'NONE',  ( -130.0004344034682617, 78.46444036551649504, -12.03207709110584211 ) ) ;
#9318 = VERTEX_POINT ( 'NONE', #17841 ) ;
#9319 = EDGE_CURVE ( 'NONE', #11706, #33876, #76083, .T. ) ;
#9320 = VERTEX_POINT ( 'NONE', #44192 ) ;
#9321 = CARTESIAN_POINT ( 'NONE',  ( 116.8364808817232756, -40.58936182315601116, 193.5270538473389479 ) ) ;
#9322 = EDGE_LOOP ( 'NONE', ( #33471, #65911, #68678, #88721 ) ) ;
#9323 = CARTESIAN_POINT ( 'NONE',  ( 114.4629700169191580, -28.51537706926042404, 159.5051490854349652 ) ) ;
#9324 = CARTESIAN_POINT ( 'NONE',  ( 97.81168895331838087, -40.51742574516882200, 287.6356252759109680 ) ) ;
#9325 = CARTESIAN_POINT ( 'NONE',  ( 136.4140944162674032, -35.29397280665119752, 7.245803660799283286 ) ) ;
#9326 = DIRECTION ( 'NONE',  ( 0.000000000000000000, 0.000000000000000000, -1.000000000000000000 ) ) ;
#9329 = CARTESIAN_POINT ( 'NONE',  ( 96.78489722101822679, -35.14273565208915073, 262.2041967044821149 ) ) ;
#9328 = CARTESIAN_POINT ( 'NONE',  ( 107.0664832912748068, -36.72944715993923381, -4.074374724089028454 ) ) ;
#9327 = CARTESIAN_POINT ( 'NONE',  ( 97.98476046313764698, -40.12019249911318752, 277.6356252759110248 ) ) ;
#9330 = DIRECTION ( 'NONE',  ( -1.000000000000000078E-15, 1.000000000000000000, 0.000000000000000000 ) ) ;
#9331 = DIRECTION ( 'NONE',  ( 0.0001713722456129695634, -0.9999999853157764962, 0.000000000000000000 ) ) ;
#9332 = CARTESIAN_POINT ( 'NONE',  ( 52.99265158129170317, 95.25000000000000000, 346.9005000000000223 ) ) ;
#9333 = DIRECTION ( 'NONE',  ( 0.000000000000000000, -1.000000000000000000, 0.000000000000000000 ) ) ;
#9334 = PLANE ( 'NONE',  #53141 ) ;
#9335 = FACE_OUTER_BOUND ( 'NONE', #41361, .T. ) ;
#9337 = VERTEX_POINT ( 'NONE', #11020 ) ;
#9336 = CARTESIAN_POINT ( 'NONE',  ( 115.2812845904211798, -33.79598010883771053, 195.5838068554166966 ) ) ;
#9338 = CARTESIAN_POINT ( 'NONE',  ( 127.0664832912739257, -54.72944906728947245, 14.82207188531768871 ) ) ;
#9339 = CARTESIAN_POINT ( 'NONE',  ( 114.9947137121727820, -28.99390558034420451, 194.4537205140059370 ) ) ;
#9340 = CARTESIAN_POINT ( 'NONE',  ( 110.7944688027788658, -46.46518603654068613, 58.86705384733998159 ) ) ;
#9341 = CARTESIAN_POINT ( 'NONE',  ( 96.14593026560288536, -32.00158989507077223, 207.0013395616249738 ) ) ;
#9342 = LINE ( 'NONE', #50213, #28595 ) ;
#9343 = ADVANCED_FACE ( 'NONE', ( #25102 ), #37401, .T. ) ;
#9344 = DIRECTION ( 'NONE',  ( -1.000000000000000000, 0.000000000000000000, 0.000000000000000000 ) ) ;
#9346 = CYLINDRICAL_SURFACE ( 'NONE', #54456, 1.523999999999053889 ) ;
#9345 = CARTESIAN_POINT ( 'NONE',  ( 165.6738106836199904, -26.00627455219321860, -5.074374724088000832 ) ) ;
#9347 = DIRECTION ( 'NONE',  ( 1.000000000000000000, 0.000000000000000000, 0.000000000000000000 ) ) ;
#9348 = CARTESIAN_POINT ( 'NONE',  ( 134.0664832912739826, -15.97944715994100306, 8.225625275910998013 ) ) ;
#9349 = ORIENTED_EDGE ( 'NONE', *, *, #38715, .T. ) ;
#9350 = VECTOR ( 'NONE', #62960, 1000.000000000000000 ) ;
#9351 = CARTESIAN_POINT ( 'NONE',  ( 108.4199059663018829, -26.73533934207818774, 64.97014767438379579 ) ) ;
#9352 = AXIS2_PLACEMENT_3D ( 'NONE', #32660, #10880, #11326 ) ;
#9353 = ORIENTED_EDGE ( 'NONE', *, *, #60434, .T. ) ;
#9354 = ORIENTED_EDGE ( 'NONE', *, *, #3393, .F. ) ;
#9355 = CARTESIAN_POINT ( 'NONE',  ( 104.6424027498074025, -44.91968313032340632, 106.7695626852199808 ) ) ;
#9357 = ORIENTED_EDGE ( 'NONE', *, *, #84275, .F. ) ;
#9356 = CARTESIAN_POINT ( 'NONE',  ( -7.752238106858478695, 92.64409645872694909, -130.3274943305225406 ) ) ;
#9358 = CARTESIAN_POINT ( 'NONE',  ( 99.07096106853141748, -43.38529345585680375, 112.8784824187679732 ) ) ;
#9359 = FACE_OUTER_BOUND ( 'NONE', #17449, .T. ) ;
#9360 = DIRECTION ( 'NONE',  ( -1.821231995776179916E-16, 0.000000000000000000, -1.000000000000000000 ) ) ;
#9361 = EDGE_CURVE ( 'NONE', #81364, #3107, #18244, .T. ) ;
#9362 = CARTESIAN_POINT ( 'NONE',  ( 116.3212776292303090, -32.94146857471486811, 175.1356252759109680 ) ) ;
#9363 = CARTESIAN_POINT ( 'NONE',  ( 106.5519926023875712, -26.37212682281782250, 45.12800622829394115 ) ) ;
#9364 = ORIENTED_EDGE ( 'NONE', *, *, #15451, .T. ) ;
#9365 = ORIENTED_EDGE ( 'NONE', *, *, #68567, .F. ) ;
#9366 = ORIENTED_EDGE ( 'NONE', *, *, #9824, .F. ) ;
#9367 = EDGE_CURVE ( 'NONE', #61103, #84281, #56897, .T. ) ;
#9368 = VECTOR ( 'NONE', #55946, 1000.000000000000000 ) ;
#9369 = CONICAL_SURFACE ( 'NONE', #74646, 7.249999999999998224, 0.7853981633974772558 ) ;
#9370 = CARTESIAN_POINT ( 'NONE',  ( 117.0608945236646861, -38.08045311976564307, 108.7189586093281264 ) ) ;
#9371 = AXIS2_PLACEMENT_3D ( 'NONE', #31239, #73473, #30807 ) ;
#9372 = LINE ( 'NONE', #73369, #4105 ) ;
#9373 = CARTESIAN_POINT ( 'NONE',  ( 37.06648329127400388, 12.92155284005802685, 336.5756252759108520 ) ) ;
#9374 = CIRCLE ( 'NONE', #6440, 6.349999999999994316 ) ;
#9375 = LINE ( 'NONE', #87015, #84251 ) ;
#9376 = CARTESIAN_POINT ( 'NONE',  ( 98.35000982325539098, -31.65631374779490059, 51.90755703618102501 ) ) ;
#9378 = CARTESIAN_POINT ( 'NONE',  ( 77.39114642429899504, 120.6499999999999915, 71.77848634863160271 ) ) ;
#9377 = VECTOR ( 'NONE', #39588, 1000.000000000000000 ) ;
#9379 = VECTOR ( 'NONE', #33369, 1000.000000000000000 ) ;
#9380 = CARTESIAN_POINT ( 'NONE',  ( 76.38857008572915674, 90.29828471680515634, 90.66710916952514765 ) ) ;
#9381 = CARTESIAN_POINT ( 'NONE',  ( 115.6551466294303623, -43.65033472170377138, 43.27467289495795200 ) ) ;
#9382 = VERTEX_POINT ( 'NONE', #4216 ) ;
#9383 = CARTESIAN_POINT ( 'NONE',  ( 104.4899551042411190, -26.97880742045457936, 270.2814585562571779 ) ) ;
#9384 = CARTESIAN_POINT ( 'NONE',  ( 82.78637150392549415, -117.3006669637344714, 250.2178068554180470 ) ) ;
#9385 = CARTESIAN_POINT ( 'NONE',  ( 103.3362113047044772, -29.43782462767379116, 118.2709475124489842 ) ) ;
#9386 = EDGE_CURVE ( 'NONE', #48508, #62608, #16959, .T. ) ;
#9387 = CARTESIAN_POINT ( 'NONE',  ( -72.96458098368751166, 117.4749999999999943, 72.96458098368620426 ) ) ;
#9388 = EDGE_CURVE ( 'NONE', #57294, #52002, #52537, .T. ) ;
#9389 = LINE ( 'NONE', #37099, #83734 ) ;
#9390 = VERTEX_POINT ( 'NONE', #6451 ) ;
#9391 = ORIENTED_EDGE ( 'NONE', *, *, #81886, .F. ) ;
#9392 = DIRECTION ( 'NONE',  ( -1.000000000000000000, -3.999999999999999995E-14, -1.000000000000000078E-15 ) ) ;
#9393 = EDGE_CURVE ( 'NONE', #86161, #37287, #73703, .T. ) ;
#9394 = EDGE_LOOP ( 'NONE', ( #14304, #65698 ) ) ;
#9395 = ORIENTED_EDGE ( 'NONE', *, *, #84590, .F. ) ;
#9396 = CARTESIAN_POINT ( 'NONE',  ( 109.4376220470258119, -28.19094731436911871, 171.2930118773249717 ) ) ;
#9397 = EDGE_CURVE ( 'NONE', #29192, #19551, #80642, .T. ) ;
#9398 = CARTESIAN_POINT ( 'NONE',  ( -41.60202597009397607, 76.06518036156089124, 47.15338361873602935 ) ) ;
#9399 = CARTESIAN_POINT ( 'NONE',  ( 108.6520215831686329, -25.77392822130451577, 145.9737205140069420 ) ) ;
#9400 = CARTESIAN_POINT ( 'NONE',  ( 97.06107107668189826, -37.99641179327961993, 121.4272919290289963 ) ) ;
#9401 = PLANE ( 'NONE',  #48807 ) ;
#9402 = VERTEX_POINT ( 'NONE', #47316 ) ;
#9403 = ORIENTED_EDGE ( 'NONE', *, *, #86345, .F. ) ;
#9404 = ORIENTED_EDGE ( 'NONE', *, *, #3631, .T. ) ;
#9405 = EDGE_CURVE ( 'NONE', #68551, #42008, #3530, .T. ) ;
#9406 = CARTESIAN_POINT ( 'NONE',  ( 111.8340120402796032, -28.76913304608537914, 202.4652332267339716 ) ) ;
#9407 = CARTESIAN_POINT ( 'NONE',  ( 101.9496561033292039, -27.62096520655628851, 60.48419670448296159 ) ) ;
#9408 = ORIENTED_EDGE ( 'NONE', *, *, #13796, .F. ) ;
#9409 = CARTESIAN_POINT ( 'NONE',  ( 99.08262072259961428, -44.34008189452615056, 36.92038718067297509 ) ) ;
#9410 = CARTESIAN_POINT ( 'NONE',  ( 109.6111442688334563, -26.56067652042401406, 195.8813395616249977 ) ) ;
#9411 = CARTESIAN_POINT ( 'NONE',  ( 57.56670390244816815, -48.82844715994039575, 295.7178068554150627 ) ) ;
#9412 = CARTESIAN_POINT ( 'NONE',  ( 107.0667039024470313, -104.2784471599409528, 23.21780685541800082 ) ) ;
#9413 = CARTESIAN_POINT ( 'NONE',  ( 108.9848500582430404, -47.61493517985451973, 118.7032443235299723 ) ) ;
#9414 = CARTESIAN_POINT ( 'NONE',  ( -546.0365000000000464, 53.97500000000000142, 50.79999999999999716 ) ) ;
#9415 = ORIENTED_EDGE ( 'NONE', *, *, #18030, .F. ) ;
#9416 = LINE ( 'NONE', #16681, #52483 ) ;
#9417 = ORIENTED_EDGE ( 'NONE', *, *, #83533, .T. ) ;
#9418 = CARTESIAN_POINT ( 'NONE',  ( 164.7812970173289955, -35.65087443492610930, 117.4678068554150485 ) ) ;
#9419 = FACE_OUTER_BOUND ( 'NONE', #77322, .T. ) ;
#9420 = ORIENTED_EDGE ( 'NONE', *, *, #53914, .T. ) ;
#9421 = AXIS2_PLACEMENT_3D ( 'NONE', #82252, #47240, #74967 ) ;
#9422 = CARTESIAN_POINT ( 'NONE',  ( 107.0667039024467329, -36.72944715994091780, 196.2188068554169718 ) ) ;
#9423 = CIRCLE ( 'NONE', #63098, 5.041900000000000048 ) ;
#9424 = AXIS2_PLACEMENT_3D ( 'NONE', #65659, #59285, #52006 ) ;
#9425 = CARTESIAN_POINT ( 'NONE',  ( 109.6678112925185076, -27.04287877648044613, 130.8675598213152966 ) ) ;
#9426 = CARTESIAN_POINT ( 'NONE',  ( 115.2074362016368099, -44.20634311780637660, 78.22324432352995416 ) ) ;
#9427 = DIRECTION ( 'NONE',  ( 2.973811673103097665E-16, 0.000000000000000000, 1.000000000000000000 ) ) ;
#9428 = AXIS2_PLACEMENT_3D ( 'NONE', #73175, #31844, #32283 ) ;
#9429 = CARTESIAN_POINT ( 'NONE',  ( 0.000000000000000000, 92.07499999999998863, 0.000000000000000000 ) ) ;
#9430 = CARTESIAN_POINT ( 'NONE',  ( 113.1782937756739642, -44.75186858913631482, 74.09395860969014791 ) ) ;
#9431 = CARTESIAN_POINT ( 'NONE',  ( 100.4186822966649828, -43.90371905523902996, 46.98133956162492098 ) ) ;
#9433 = CARTESIAN_POINT ( 'NONE',  ( 117.2886123466743129, -34.79635738071010564, 154.9756252759109714 ) ) ;
#9432 = CARTESIAN_POINT ( 'NONE',  ( 107.0664832912739968, -36.72944715994100306, 287.6356252759109680 ) ) ;
#9434 = DIRECTION ( 'NONE',  ( -0.000000000000000000, 1.000000000000000000, 0.000000000000000000 ) ) ;
#9435 = DIRECTION ( 'NONE',  ( -1.000000000000000000, 0.000000000000000000, 0.000000000000000000 ) ) ;
#9436 = VERTEX_POINT ( 'NONE', #40063 ) ;
#9437 = CARTESIAN_POINT ( 'NONE',  ( 120.0056275895821898, -31.38355669832866468, 293.1356252759106837 ) ) ;
#9438 = CIRCLE ( 'NONE', #22551, 7.499999999999996447 ) ;
#9439 = AXIS2_PLACEMENT_3D ( 'NONE', #1442, #14166, #70937 ) ;
#9440 = DIRECTION ( 'NONE',  ( 0.000000000000000000, -1.000000000000000000, 0.000000000000000000 ) ) ;
#9441 = FACE_OUTER_BOUND ( 'NONE', #38855, .T. ) ;
#9442 = FACE_OUTER_BOUND ( 'NONE', #83982, .T. ) ;
#9444 = EDGE_LOOP ( 'NONE', ( #4222, #7504, #36954, #60326, #3909 ) ) ;
#9443 = CARTESIAN_POINT ( 'NONE',  ( 106.4811411369643679, -24.84306116243460139, 195.1156252759109861 ) ) ;
#9445 = CARTESIAN_POINT ( 'NONE',  ( -469.3583484187089994, 53.97500000000000142, -3.174999999999999822 ) ) ;
#9446 = CARTESIAN_POINT ( 'NONE',  ( 97.14909927861904748, -40.01315743934404878, 237.5813395616249579 ) ) ;
#9447 = CARTESIAN_POINT ( 'NONE',  ( 116.6381559899473217, -29.65878987416117241, 105.3327681330539463 ) ) ;
#9448 = CARTESIAN_POINT ( 'NONE',  ( 97.31575293894259460, -39.30575261481694582, 252.5323662874646118 ) ) ;
#9449 = ADVANCED_FACE ( 'NONE', ( #40518 ), #27339, .T. ) ;
#9450 = CARTESIAN_POINT ( 'NONE',  ( 90.44969454456405344, -20.11243780205715481, 219.5838068554169809 ) ) ;
#9451 = CIRCLE ( 'NONE', #15295, 5.599999999999994316 ) ;
#9452 = DIRECTION ( 'NONE',  ( 0.000000000000000000, 0.000000000000000000, -1.000000000000000000 ) ) ;
#9453 = ORIENTED_EDGE ( 'NONE', *, *, #7476, .F. ) ;
#9454 = AXIS2_PLACEMENT_3D ( 'NONE', #76914, #14693, #84193 ) ;
#9455 = VERTEX_POINT ( 'NONE', #80989 ) ;
#9456 = VERTEX_POINT ( 'NONE', #19191 ) ;
#9457 = ORIENTED_EDGE ( 'NONE', *, *, #30218, .T. ) ;
#9458 = LINE ( 'NONE', #84442, #67037 ) ;
#9459 = CARTESIAN_POINT ( 'NONE',  ( 96.76336351750784104, -35.13941245127819002, 262.2041967044821149 ) ) ;
#9460 = CARTESIAN_POINT ( 'NONE',  ( 84.32545390244801808, -42.97311385574013087, 231.5838068554169524 ) ) ;
#9461 = PLANE ( 'NONE',  #83227 ) ;
#9463 = LINE ( 'NONE', #43518, #54382 ) ;
#9462 = FACE_OUTER_BOUND ( 'NONE', #33858, .T. ) ;
#9464 = PLANE ( 'NONE',  #57333 ) ;
#9465 = CARTESIAN_POINT ( 'NONE',  ( 98.89771913768545630, -40.63891803577419637, 216.1162293518859485 ) ) ;
#9466 = ORIENTED_EDGE ( 'NONE', *, *, #1436, .F. ) ;
#9467 = ORIENTED_EDGE ( 'NONE', *, *, #2845, .T. ) ;
#9468 = B_SPLINE_CURVE_WITH_KNOTS ( 'NONE', 3,
 ( #50207, #49310, #77043, #28893, #24744, #58368, #51101, #17047, #57924, #37040, #78841, #30670, #65630, #2531, #43840, #9336, #44727, #71131, #72458, #52411, #8909, #64745, #72015, #17924, #3414, #64309, #23435, #71577, #30231, #16600, #31103, #85657, #17489, #86983, #44278, #9782, #37488, #51974, #58799, #80176, #65192, #86543, #24308, #2969, #36609, #2079, #86095, #79732, #10226, #23867, #45170, #66064, #29784, #57477, #51538, #79287, #85217, #78400, #37931, #72894, #10659, #22984, #38364, #3857, #31550, #59252, #50659, #16162, #87870, #59690, #18824, #61488, #26533, #19714, #40605, #25633, #53759, #82415, #45600, #19278, #6102, #33346 ),
 .UNSPECIFIED., .F., .F.,
 ( 4, 2, 2, 2, 2, 2, 2, 2, 2, 2, 2, 2, 2, 2, 2, 2, 2, 2, 2, 2, 2, 2, 2, 2, 2, 2, 2, 2, 2, 2, 2, 2, 2, 2, 2, 2, 2, 2, 2, 2, 4 ),
 ( 6.061704139448921493E-05, 0.0002290496303638520949, 0.0003974822193332150019, 0.0007343473972719562117, 0.001408077753149438848, 0.002755538464904434912, 0.004102999176659431410, 0.005450459888414427474, 0.006797920600169424406, 0.008145381311924420470, 0.009492842023679417401, 0.01084030273543441433, 0.01353522415894439952, 0.01623014558245438818, 0.01690387593833189359, 0.01757760629420940246, 0.01892506700596442368, 0.01959879736184192908, 0.02027252771771943796, 0.02161998842947449387, 0.02296744914122954978, 0.02431490985298460222, 0.02566237056473966507, 0.02700983127649471752, 0.02835729198824977343, 0.02970475270000482934, 0.03037848305588235903, 0.03105221341175988872, 0.03239967412351493076, 0.03374713483526996238, 0.03509459554702500095, 0.03644205625878003951, 0.03778951697053507808, 0.03913697768229010970, 0.04048443839404514827, 0.04183189910580018683, 0.04250562946167770612, 0.04284249463961645188, 0.04301092722858581435, 0.04309514352307049906, 0.04317935981755517683 ),
 .UNSPECIFIED. ) ;
#9469 = AXIS2_PLACEMENT_3D ( 'NONE', #28860, #84291, #15233 ) ;
#9470 = ORIENTED_EDGE ( 'NONE', *, *, #86312, .F. ) ;
#9471 = ADVANCED_FACE ( 'NONE', ( #11479 ), #60501, .F. ) ;
#9472 = CARTESIAN_POINT ( 'NONE',  ( 20.56670390244743984, -48.82844715994200158, 180.4678068554150911 ) ) ;
#9473 = CIRCLE ( 'NONE', #89294, 2.750000000000002665 ) ;
#9474 = CARTESIAN_POINT ( 'NONE',  ( 97.82528911858155141, -40.55050895928604149, 181.6384720198973071 ) ) ;
#9475 = CARTESIAN_POINT ( 'NONE',  ( 112.3177584634462534, -44.98096486020153151, 259.0270538473389479 ) ) ;
#9476 = CARTESIAN_POINT ( 'NONE',  ( 141.0664832912740394, -46.72944715994099596, -4.824374724088994704 ) ) ;
#9477 = CARTESIAN_POINT ( 'NONE',  ( 118.1720832024964807, -36.20253795304678590, 114.8641967044819694 ) ) ;
#9478 = DIRECTION ( 'NONE',  ( -1.000000000000000078E-15, 1.000000000000000083E-30, 1.000000000000000000 ) ) ;
#9479 = ORIENTED_EDGE ( 'NONE', *, *, #13090, .F. ) ;
#9480 = CARTESIAN_POINT ( 'NONE',  ( 77.31651910784952975, -36.55813574389581078, 3.101427645696278379 ) ) ;
#9481 = VERTEX_POINT ( 'NONE', #67780 ) ;
#9482 = DIRECTION ( 'NONE',  ( 0.000000000000000000, -1.000000000000000000, 0.000000000000000000 ) ) ;
#9483 = CARTESIAN_POINT ( 'NONE',  ( 112.7530619618799932, -30.23101651580132199, 285.9349166392303800 ) ) ;
#9484 = AXIS2_PLACEMENT_3D ( 'NONE', #21438, #34602, #48660 ) ;
#9485 = AXIS2_PLACEMENT_3D ( 'NONE', #31684, #59381, #25318 ) ;
#9486 = VECTOR ( 'NONE', #87349, 1000.000000000000000 ) ;
#9487 = DIRECTION ( 'NONE',  ( 1.000000000000000000, 0.000000000000000000, 0.000000000000000000 ) ) ;
#9488 = DIRECTION ( 'NONE',  ( 0.000000000000000000, 0.000000000000000000, -1.000000000000000000 ) ) ;
#9489 = EDGE_CURVE ( 'NONE', #59170, #12768, #70923, .T. ) ;
#9490 = DIRECTION ( 'NONE',  ( 1.000000000000000078E-15, -1.000000000000000083E-30, -1.000000000000000000 ) ) ;
#9491 = AXIS2_PLACEMENT_3D ( 'NONE', #52307, #80072, #17826 ) ;
#9492 = ORIENTED_EDGE ( 'NONE', *, *, #66796, .T. ) ;
#9493 = CARTESIAN_POINT ( 'NONE',  ( 34.96670390244699433, -26.71338133339301635, 342.9256252759109884 ) ) ;
#9494 = DIRECTION ( 'NONE',  ( 0.000000000000000000, 0.000000000000000000, -1.000000000000000000 ) ) ;
#9495 = EDGE_CURVE ( 'NONE', #58352, #7509, #54563, .T. ) ;
#9496 = B_SPLINE_CURVE_WITH_KNOTS ( 'NONE', 3,
 ( #4621, #67281, #5528, #33221, #60460, #54080, #19585, #47277, #11433, #75003, #65934, #59115, #10975, #38677, #31868, #32306, #4172, #34555, #62714, #76347, #47726, #13671, #62262, #20046, #48609, #41803, #69539, #89087, #35447, #56329, #63163, #75463, #54972, #82739, #5978, #14583, #945, #68643, #54526, #14125, #20503, #492, #42258, #21391, #83623, #13232, #7315, #28182 ),
 .UNSPECIFIED., .F., .F.,
 ( 4, 2, 2, 2, 2, 2, 2, 2, 2, 1, 2, 2, 2, 2, 2, 2, 2, 2, 2, 2, 2, 1, 2, 2, 4 ),
 ( 0.05960646776571127542, 0.06208927922045080761, 0.06333068494782057023, 0.06457209067519034673, 0.06705490212992989973, 0.06829630785729966236, 0.06953771358466942498, 0.07202052503940886696, 0.07326193076677858795, 0.07450333649414830894, 0.07574474222151801606, 0.07698614794888773705, 0.07946895940362716515, 0.08195177085836659325, 0.08319317658573632812, 0.08443458231310606299, 0.08691739376784554660, 0.08815879949521529535, 0.08940020522258504410, 0.09188301667732448608, 0.09312442240469417931, 0.09436582813206385867, 0.09560723385943355190, 0.09684863958680324514, 0.09933145104154257610 ),
 .UNSPECIFIED. ) ;
#9497 = ORIENTED_EDGE ( 'NONE', *, *, #34286, .F. ) ;
#9498 = CARTESIAN_POINT ( 'NONE',  ( 96.07744114619573850, -37.92110155076959899, 81.40038718067299328 ) ) ;
#9499 = ORIENTED_EDGE ( 'NONE', *, *, #86846, .T. ) ;
#9500 = EDGE_CURVE ( 'NONE', #65538, #9127, #82330, .T. ) ;
#9501 = CARTESIAN_POINT ( 'NONE',  ( 107.1721053552439713, -28.18866407513752392, 34.48956268521896362 ) ) ;
#9502 = AXIS2_PLACEMENT_3D ( 'NONE', #80863, #18616, #74030 ) ;
#9503 = CARTESIAN_POINT ( 'NONE',  ( 110.0265056719061363, -46.30983220778679055, 88.81405189569714764 ) ) ;
#9504 = CARTESIAN_POINT ( 'NONE',  ( 109.3646161452266767, -45.83961241216247373, 89.21682140113502157 ) ) ;
#9505 = CARTESIAN_POINT ( 'NONE',  ( 115.0363764831674303, -42.90958019793037437, 14.30217953636555706 ) ) ;
#9506 = ADVANCED_FACE ( 'NONE', ( #75501 ), #53673, .T. ) ;
#9507 = DIRECTION ( 'NONE',  ( 1.000000000000000078E-15, -1.000000000000000083E-30, -1.000000000000000000 ) ) ;
#9508 = DIRECTION ( 'NONE',  ( -1.000000000000000078E-15, 1.000000000000000083E-30, 1.000000000000000000 ) ) ;
#9509 = VECTOR ( 'NONE', #19516, 1000.000000000000000 ) ;
#9510 = CARTESIAN_POINT ( 'NONE',  ( 111.4988423704183020, -26.55354146975621177, 280.7375300378156453 ) ) ;
#9511 = CARTESIAN_POINT ( 'NONE',  ( 127.0664832912740394, -46.72944715994101017, -4.824374724089008915 ) ) ;
#9512 = ORIENTED_EDGE ( 'NONE', *, *, #5608, .F. ) ;
#9513 = CARTESIAN_POINT ( 'NONE',  ( 68.56670390244707392, -139.1784471599409869, 228.4678068554179902 ) ) ;
#9514 = ORIENTED_EDGE ( 'NONE', *, *, #10852, .F. ) ;
#9515 = CARTESIAN_POINT ( 'NONE',  ( 117.0647351476834643, -39.95015185843580952, 154.5784824187679476 ) ) ;
#9516 = CARTESIAN_POINT ( 'NONE',  ( 80.06648329127399677, -21.47944715994105991, 1.625625275910943746 ) ) ;
#9517 = ORIENTED_EDGE ( 'NONE', *, *, #61403, .T. ) ;
#9518 = ORIENTED_EDGE ( 'NONE', *, *, #59603, .T. ) ;
#9519 = ORIENTED_EDGE ( 'NONE', *, *, #88579, .F. ) ;
#9520 = EDGE_CURVE ( 'NONE', #7908, #81729, #1883, .T. ) ;
#9521 = DIRECTION ( 'NONE',  ( 1.067350013832299363E-17, -0.9961946980917455452, 0.08715574274765836016 ) ) ;
#9522 = CARTESIAN_POINT ( 'NONE',  ( 61.67079006425787924, -0.9306969701460061639, 394.9756252759102040 ) ) ;
#9523 = CARTESIAN_POINT ( 'NONE',  ( 99.06478422775786896, -31.10483629442210329, 205.8384824187689617 ) ) ;
#9525 = EDGE_CURVE ( 'NONE', #62756, #15555, #526, .T. ) ;
#9524 = DIRECTION ( 'NONE',  ( 0.000000000000000000, -1.000000000000000000, 0.000000000000000000 ) ) ;
#9526 = CARTESIAN_POINT ( 'NONE',  ( 142.6617037637538772, -139.6113389983086108, 247.4111996305669834 ) ) ;
#9527 = DIRECTION ( 'NONE',  ( 1.000000000000000078E-15, -1.000000000000000083E-30, -1.000000000000000000 ) ) ;
#9528 = AXIS2_PLACEMENT_3D ( 'NONE', #39764, #67476, #59756 ) ;
#9529 = CARTESIAN_POINT ( 'NONE',  ( 112.1974349349366804, -26.93816038506360755, 10.68038718067299087 ) ) ;
#9530 = CARTESIAN_POINT ( 'NONE',  ( 97.81170003938157720, -40.51743348276853851, 42.63567940883270069 ) ) ;
#9531 = ORIENTED_EDGE ( 'NONE', *, *, #48509, .F. ) ;
#9532 = CARTESIAN_POINT ( 'NONE',  ( 98.34947374717273760, -31.65727468815311596, 171.9064461681665534 ) ) ;
#9533 = CARTESIAN_POINT ( 'NONE',  ( 108.3334406624257298, -46.73486044134102713, 42.67684850810000086 ) ) ;
#9534 = VECTOR ( 'NONE', #89496, 1000.000000000000000 ) ;
#9535 = EDGE_LOOP ( 'NONE', ( #63387, #29373 ) ) ;
#9536 = VECTOR ( 'NONE', #67619, 1000.000000000000114 ) ;
#9537 = CARTESIAN_POINT ( 'NONE',  ( 7.661254700127822836, 95.64746158385918307, 317.6630000000000109 ) ) ;
#9538 = CARTESIAN_POINT ( 'NONE',  ( 88.90000000000000568, 69.84999999999999432, 346.0750000000000455 ) ) ;
#9540 = VECTOR ( 'NONE', #35415, 1000.000000000000000 ) ;
#9539 = CARTESIAN_POINT ( 'NONE',  ( 104.4161250475293343, -26.02246701806295448, 240.2575300378159682 ) ) ;
#9541 = DIRECTION ( 'NONE',  ( 0.000000000000000000, 0.000000000000000000, 1.000000000000000000 ) ) ;
#9542 = CARTESIAN_POINT ( 'NONE',  ( 131.3179999999999836, 53.97500000000000142, 50.79999999999999716 ) ) ;
#9543 = DIRECTION ( 'NONE',  ( 1.075267683398002218E-15, -1.000000000000000000, 3.100000000000000044E-14 ) ) ;
#9544 = CARTESIAN_POINT ( 'NONE',  ( 115.5937312905896022, -36.23733611532740184, 228.2952769709339691 ) ) ;
#9546 = CARTESIAN_POINT ( 'NONE',  ( 115.5933672690473912, -28.53551910654245205, 35.43562527591098643 ) ) ;
#9545 = PLANE ( 'NONE',  #75107 ) ;
#9547 = CARTESIAN_POINT ( 'NONE',  ( 122.8489780378840948, 73.53925275838706455, 44.19769267541737179 ) ) ;
#9548 = CARTESIAN_POINT ( 'NONE',  ( 108.0382549187111607, -25.67193643048636886, 109.9946728949589811 ) ) ;
#9549 = ORIENTED_EDGE ( 'NONE', *, *, #33571, .F. ) ;
#9550 = CARTESIAN_POINT ( 'NONE',  ( 131.3165200636276211, -18.90534128959012961, 6.749824347015441539 ) ) ;
#9551 = ORIENTED_EDGE ( 'NONE', *, *, #58496, .T. ) ;
#9552 = CARTESIAN_POINT ( 'NONE',  ( -141.3509999999999991, 101.5999999999999943, 132.7150000000000034 ) ) ;
#9553 = DIRECTION ( 'NONE',  ( 0.000000000000000000, 1.000000000000000000, 0.000000000000000000 ) ) ;
#9554 = EDGE_LOOP ( 'NONE', ( #88538, #53393, #38933, #6918 ) ) ;
#9555 = LINE ( 'NONE', #29550, #81036 ) ;
#9556 = EDGE_LOOP ( 'NONE', ( #48445, #70706, #84538, #29947 ) ) ;
#9557 = CARTESIAN_POINT ( 'NONE',  ( 71.25416588882602298, -72.55705569728901594, 394.9756252759102040 ) ) ;
#9558 = DIRECTION ( 'NONE',  ( 0.000000000000000000, 0.000000000000000000, 1.000000000000000000 ) ) ;
#9559 = EDGE_CURVE ( 'NONE', #28103, #62184, #7352, .T. ) ;
#9561 = AXIS2_PLACEMENT_3D ( 'NONE', #41738, #6788, #28114 ) ;
#9560 = DIRECTION ( 'NONE',  ( 0.000000000000000000, 0.000000000000000000, -1.000000000000000000 ) ) ;
#9562 = ORIENTED_EDGE ( 'NONE', *, *, #33286, .T. ) ;
#9563 = CARTESIAN_POINT ( 'NONE',  ( 112.5258771334048475, -27.82206915948941273, 94.63848241876793566 ) ) ;
#9564 = VECTOR ( 'NONE', #48655, 1000.000000000000000 ) ;
#9565 = VECTOR ( 'NONE', #4568, 1000.000000000000000 ) ;
#9566 = CARTESIAN_POINT ( 'NONE',  ( 0.000000000000000000, 0.000000000000000000, 0.000000000000000000 ) ) ;
#9567 = AXIS2_PLACEMENT_3D ( 'NONE', #59620, #52779, #3346 ) ;
#9569 = ADVANCED_FACE ( 'NONE', ( #76387 ), #42739, .F. ) ;
#9568 = CARTESIAN_POINT ( 'NONE',  ( 28.57499999999999929, 82.54999999999999716, 307.6574999999999704 ) ) ;
#9570 = DIRECTION ( 'NONE',  ( -1.000000000000000000, 0.000000000000000000, -2.108231265501709878E-16 ) ) ;
#9571 = CARTESIAN_POINT ( 'NONE',  ( 100.8961411191535973, 127.0000000000000000, -3.968749999999580336 ) ) ;
#9572 = ORIENTED_EDGE ( 'NONE', *, *, #56651, .F. ) ;
#9573 = CYLINDRICAL_SURFACE ( 'NONE', #18486, 3.000000000000002665 ) ;
#9574 = DIRECTION ( 'NONE',  ( 0.000000000000000000, 0.000000000000000000, 1.000000000000000000 ) ) ;
#9575 = CARTESIAN_POINT ( 'NONE',  ( 142.0664832912740678, -45.72944715994100306, 14.82207188531769049 ) ) ;
#9577 = LINE ( 'NONE', #87220, #70374 ) ;
#9576 = CYLINDRICAL_SURFACE ( 'NONE', #56657, 2.999999999999999112 ) ;
#9578 = CARTESIAN_POINT ( 'NONE',  ( 84.06648329127399677, -14.47844715994100007, 284.9256252759119548 ) ) ;
#9579 = ORIENTED_EDGE ( 'NONE', *, *, #52583, .F. ) ;
#9580 = VECTOR ( 'NONE', #76819, 1000.000000000000000 ) ;
#9581 = DIRECTION ( 'NONE',  ( 0.000000000000000000, 0.000000000000000000, 1.000000000000000000 ) ) ;
#9582 = CARTESIAN_POINT ( 'NONE',  ( 97.26456095925938428, -36.24355304347524509, 167.2870538473389672 ) ) ;
#9584 = VERTEX_POINT ( 'NONE', #55916 ) ;
#9583 = DIRECTION ( 'NONE',  ( 0.000000000000000000, 0.000000000000000000, -1.000000000000000000 ) ) ;
#9585 = CARTESIAN_POINT ( 'NONE',  ( 104.4155842969358332, -46.14412564300911157, 18.35848241876792031 ) ) ;
#9586 = DIRECTION ( 'NONE',  ( 0.000000000000000000, -1.000000000000000000, 0.000000000000000000 ) ) ;
#9587 = CARTESIAN_POINT ( 'NONE',  ( 97.81219525132515002, -40.51866273574350430, 51.63573126026001603 ) ) ;
#9588 = CARTESIAN_POINT ( 'NONE',  ( 116.7940960725532733, -39.39149561008477463, 13.61514541225734298 ) ) ;
#9589 = EDGE_CURVE ( 'NONE', #84035, #35999, #6894, .T. ) ;
#9590 = CARTESIAN_POINT ( 'NONE',  ( 98.35011216517960975, -31.65613066903540229, 30.90664309484206385 ) ) ;
#9591 = CARTESIAN_POINT ( 'NONE',  ( 114.1395267584829867, -29.97404255306813781, 234.4327681330549638 ) ) ;
#9592 = VERTEX_POINT ( 'NONE', #35945 ) ;
#9593 = ORIENTED_EDGE ( 'NONE', *, *, #36997, .F. ) ;
#9594 = CARTESIAN_POINT ( 'NONE',  ( 114.9579445475069264, -42.99008164810605592, 194.7244404487539668 ) ) ;
#9595 = CARTESIAN_POINT ( 'NONE',  ( 31.56670390244800828, -32.29483332968611364, -5.074374724088000832 ) ) ;
#9596 = CARTESIAN_POINT ( 'NONE',  ( 99.16631175631914630, -32.71502711089942039, 47.38444044875394923 ) ) ;
#9597 = CARTESIAN_POINT ( 'NONE',  ( -89.37916159652597514, 94.58014758961630264, 95.16508291382922380 ) ) ;
#9598 = CARTESIAN_POINT ( 'NONE',  ( 105.7995184934298152, -26.72403496524378141, 80.17729194211321442 ) ) ;
#9599 = DIRECTION ( 'NONE',  ( -0.9254794337955620787, -0.3787978585227822492, 0.000000000000000000 ) ) ;
#9600 = ORIENTED_EDGE ( 'NONE', *, *, #44551, .F. ) ;
#9601 = DIRECTION ( 'NONE',  ( 0.000000000000000000, 1.000000000000000000, 0.000000000000000000 ) ) ;
#9602 = CARTESIAN_POINT ( 'NONE',  ( 34.67381068362099228, -26.00627455219321860, 237.4678068554150059 ) ) ;
#9603 = CARTESIAN_POINT ( 'NONE',  ( 111.1189502094635202, -27.14789314160929479, 244.7584824187679544 ) ) ;
#9604 = CARTESIAN_POINT ( 'NONE',  ( 8.377092249087933595, 92.10453133679206417, 118.2601133684811856 ) ) ;
#9606 = ORIENTED_EDGE ( 'NONE', *, *, #45425, .T. ) ;
#9605 = EDGE_CURVE ( 'NONE', #14493, #20049, #84866, .T. ) ;
#9607 = CARTESIAN_POINT ( 'NONE',  ( 109.6430121231974653, -46.48008673722491579, 82.78145860864054839 ) ) ;
#9608 = FACE_OUTER_BOUND ( 'NONE', #50137, .T. ) ;
#9609 = CYLINDRICAL_SURFACE ( 'NONE', #37467, 9.999999999999998224 ) ;
#9610 = FACE_BOUND ( 'NONE', #21066, .T. ) ;
#9611 = CARTESIAN_POINT ( 'NONE',  ( 111.8651074766111293, -28.16866562884743885, 30.66991099019594813 ) ) ;
#9613 = DIRECTION ( 'NONE',  ( 0.000000000000000000, -1.000000000000000000, 0.000000000000000000 ) ) ;
#9612 = VECTOR ( 'NONE', #76064, 1000.000000000000000 ) ;
#9614 = EDGE_LOOP ( 'NONE', ( #23057, #72319, #10441, #33365 ) ) ;
#9615 = AXIS2_PLACEMENT_3D ( 'NONE', #41148, #62942, #42047 ) ;
#9616 = CARTESIAN_POINT ( 'NONE',  ( 96.79082665085387305, -38.90864320302405588, 27.49276813305395706 ) ) ;
#9617 = VECTOR ( 'NONE', #21788, 999.9999999999998863 ) ;
#9618 = DIRECTION ( 'NONE',  ( 1.000000000000000000, 1.000000000000000078E-15, 0.000000000000000000 ) ) ;
#9619 = VECTOR ( 'NONE', #53121, 1000.000000000000114 ) ;
#9620 = CARTESIAN_POINT ( 'NONE',  ( 96.88875151864165503, -30.65867585538550344, 280.8984824187682534 ) ) ;
#9621 = ORIENTED_EDGE ( 'NONE', *, *, #3984, .F. ) ;
#9622 = EDGE_CURVE ( 'NONE', #84402, #10839, #85018, .T. ) ;
#9623 = CARTESIAN_POINT ( 'NONE',  ( 82.58883806303657593, -17.63381004753172121, 2.797770231024844456 ) ) ;
#9625 = EDGE_CURVE ( 'NONE', #30248, #45134, #32566, .T. ) ;
#9624 = CARTESIAN_POINT ( 'NONE',  ( 99.08975689199405679, -42.79577111913272347, 17.84389778671033966 ) ) ;
#9626 = DIRECTION ( 'NONE',  ( 0.000000000000000000, 0.000000000000000000, -1.000000000000000000 ) ) ;
#9627 = CARTESIAN_POINT ( 'NONE',  ( 111.9587407205840890, -30.16069495786998544, 102.3852332267339591 ) ) ;
#9628 = CARTESIAN_POINT ( 'NONE',  ( 118.9020112566783354, -37.70028621367283961, 184.7613395616249647 ) ) ;
#9629 = LINE ( 'NONE', #70978, #43507 ) ;
#9630 = EDGE_LOOP ( 'NONE', ( #64937, #654, #60672, #82707 ) ) ;
#9631 = VECTOR ( 'NONE', #18232, 1000.000000000000000 ) ;
#9632 = FACE_OUTER_BOUND ( 'NONE', #22649, .T. ) ;
#9633 = VERTEX_POINT ( 'NONE', #21434 ) ;
#9634 = ORIENTED_EDGE ( 'NONE', *, *, #89028, .T. ) ;
#9635 = FACE_BOUND ( 'NONE', #1819, .T. ) ;
#9636 =( BOUNDED_CURVE ( )  B_SPLINE_CURVE ( 3, ( #80555, #18311, #40091, #17867 ),
 .UNSPECIFIED., .F., .T. ) 
 B_SPLINE_CURVE_WITH_KNOTS ( ( 4, 4 ),
 ( 5.813027347256380040, 6.753343267102792424 ),
 .UNSPECIFIED. ) 
 CURVE ( )  GEOMETRIC_REPRESENTATION_ITEM ( )  RATIONAL_B_SPLINE_CURVE ( ( 1.000000000000000000, 0.9276644927932374829, 0.9276644927932374829, 1.000000000000000000 ) ) 
 REPRESENTATION_ITEM ( '' )  );
#9637 = ORIENTED_EDGE ( 'NONE', *, *, #10817, .T. ) ;
#9638 = ORIENTED_EDGE ( 'NONE', *, *, #60540, .T. ) ;
#9639 = DIRECTION ( 'NONE',  ( 0.000000000000000000, -1.000000000000000000, 0.000000000000000000 ) ) ;
#9640 = AXIS2_PLACEMENT_3D ( 'NONE', #29360, #70238, #8929 ) ;
#9641 = CARTESIAN_POINT ( 'NONE',  ( 34.27482367531452212, -30.08671355700332839, 313.9678068554150059 ) ) ;
#9642 = CARTESIAN_POINT ( 'NONE',  ( 115.7614890496577402, -39.26115509793221747, 138.0114674471239766 ) ) ;
#9643 = CARTESIAN_POINT ( 'NONE',  ( 115.9788024870550061, -30.15175701148841725, 259.3203871806730945 ) ) ;
#9644 = CARTESIAN_POINT ( 'NONE',  ( 49.21213752016100784, -29.73316016639650883, 342.9256252759109884 ) ) ;
#9645 = ORIENTED_EDGE ( 'NONE', *, *, #44960, .T. ) ;
#9646 = CARTESIAN_POINT ( 'NONE',  ( 103.2780950051364925, -27.47482052217685222, 136.3856613811564671 ) ) ;
#9647 = ORIENTED_EDGE ( 'NONE', *, *, #8475, .T. ) ;
#9648 = LINE ( 'NONE', #42803, #62367 ) ;
#9649 = LINE ( 'NONE', #2848, #27057 ) ;
#9650 = DIRECTION ( 'NONE',  ( 0.000000000000000000, 1.000000000000000000, 0.000000000000000000 ) ) ;
#9651 = AXIS2_PLACEMENT_3D ( 'NONE', #10395, #72631, #51707 ) ;
#9652 = CARTESIAN_POINT ( 'NONE',  ( 105.8886092880350560, -47.16805723083484736, 282.4870538473393253 ) ) ;
#9653 = VERTEX_POINT ( 'NONE', #49556 ) ;
#9654 = CARTESIAN_POINT ( 'NONE',  ( 95.23113311243525914, -37.33357626913954164, 271.3670538473393776 ) ) ;
#9655 = CARTESIAN_POINT ( 'NONE',  ( 100.3832715781272356, -28.67167693828054453, 36.62705384733894221 ) ) ;
#9656 = DIRECTION ( 'NONE',  ( 5.512527431108029424E-15, -1.000000000000000000, 0.000000000000000000 ) ) ;
#9659 = EDGE_CURVE ( 'NONE', #29066, #2140, #84115, .T. ) ;
#9658 = FACE_OUTER_BOUND ( 'NONE', #36723, .T. ) ;
#9657 = LINE ( 'NONE', #58683, #2748 ) ;
#9660 = CYLINDRICAL_SURFACE ( 'NONE', #42332, 0.5000000000000073275 ) ;
#9661 = CARTESIAN_POINT ( 'NONE',  ( 83.56670559755329464, -36.73837296219065252, 239.5838068554176914 ) ) ;
#9662 = CARTESIAN_POINT ( 'NONE',  ( 131.6875538713384799, -38.11069332324941428, 7.213126773498808930 ) ) ;
#9663 = CARTESIAN_POINT ( 'NONE',  ( 162.8595971212720031, -23.19206098994089160, 342.9256252759109884 ) ) ;
#9664 = CYLINDRICAL_SURFACE ( 'NONE', #86922, 179.8898777604655095 ) ;
#9665 = DIRECTION ( 'NONE',  ( 0.000000000000000000, 1.000000000000000000, 0.000000000000000000 ) ) ;
#9666 = DIRECTION ( 'NONE',  ( 1.000000000000000000, 4.510281037539788691E-14, 0.000000000000000000 ) ) ;
#9667 = CARTESIAN_POINT ( 'NONE',  ( 96.54134661961150243, -40.18473915001016650, 286.5908633711491120 ) ) ;
#9668 = CARTESIAN_POINT ( 'NONE',  ( 100.0081584303796944, -27.21027357624165788, 181.5841967044829630 ) ) ;
#9669 = CARTESIAN_POINT ( 'NONE',  ( 116.4070807376042609, -31.97209126034463011, 40.20133956162496958 ) ) ;
#9670 = AXIS2_PLACEMENT_3D ( 'NONE', #79696, #24707, #73292 ) ;
#9671 = B_SPLINE_CURVE_WITH_KNOTS ( 'NONE', 3,
 ( #55481, #20106, #69146, #47783, #55032, #83679, #70494, #75518, #77305, #48225, #82346, #13731, #62766, #42754, #8265, #63222, #83234, #14182 ),
 .UNSPECIFIED., .F., .F.,
 ( 4, 2, 2, 2, 2, 2, 2, 2, 4 ),
 ( 0.4999999998527593359, 0.5624999998711643912, 0.6249999998895694464, 0.6874999999079746127, 0.7499999999263796679, 0.8124999999447847232, 0.8749999999631898895, 0.9374999999815949447, 1.000000000000000000 ),
 .UNSPECIFIED. ) ;
#9673 = DIRECTION ( 'NONE',  ( 3.999999999999999995E-14, -1.000000000000000000, 4.100000000000000342E-29 ) ) ;
#9672 = DIRECTION ( 'NONE',  ( 0.000000000000000000, 0.000000000000000000, -1.000000000000000000 ) ) ;
#9674 = CYLINDRICAL_SURFACE ( 'NONE', #13147, 2.030000000002079918 ) ;
#9675 = VECTOR ( 'NONE', #22869, 1000.000000000000000 ) ;
#9677 = EDGE_CURVE ( 'NONE', #15221, #62972, #21887, .T. ) ;
#9676 = AXIS2_PLACEMENT_3D ( 'NONE', #28248, #22808, #1465 ) ;
#9678 = VECTOR ( 'NONE', #2686, 1000.000000000000000 ) ;
#9679 = ORIENTED_EDGE ( 'NONE', *, *, #64054, .F. ) ;
#9680 = EDGE_CURVE ( 'NONE', #37237, #3921, #64113, .T. ) ;
#9681 = CYLINDRICAL_SURFACE ( 'NONE', #1199, 118.5560000000000116 ) ;
#9682 = ORIENTED_EDGE ( 'NONE', *, *, #33810, .F. ) ;
#9683 = CARTESIAN_POINT ( 'NONE',  ( 99.77418633167441442, -43.29726106931974527, 52.90991099019598209 ) ) ;
#9684 = EDGE_CURVE ( 'NONE', #6056, #89556, #14622, .T. ) ;
#9686 = ORIENTED_EDGE ( 'NONE', *, *, #64270, .T. ) ;
#9685 = CARTESIAN_POINT ( 'NONE',  ( 161.0667039024469886, -67.87844715994089029, 96.96780685541800437 ) ) ;
#9687 = CARTESIAN_POINT ( 'NONE',  ( 109.6425287038660343, -46.48020844107070815, 48.78141933728851853 ) ) ;
#9688 = CARTESIAN_POINT ( 'NONE',  ( 116.3308458273175603, -44.07926308385594183, 194.2927681330539542 ) ) ;
#9689 = DIRECTION ( 'NONE',  ( 4.299999999999999979E-14, -1.000000000000000000, 0.000000000000000000 ) ) ;
#9690 = CARTESIAN_POINT ( 'NONE',  ( 97.92339371807813109, -40.78106740870623526, 146.6584159238782661 ) ) ;
#9691 = CARTESIAN_POINT ( 'NONE',  ( 106.5667039024470455, -113.2645475377471058, 2.217806855418280598 ) ) ;
#9692 = DIRECTION ( 'NONE',  ( 1.000000000000000000, 6.831565154159360295E-14, 0.000000000000000000 ) ) ;
#9693 = ADVANCED_FACE ( 'NONE', ( #69577 ), #15065, .T. ) ;
#9694 = EDGE_CURVE ( 'NONE', #19831, #72752, #38404, .T. ) ;
#9695 = CARTESIAN_POINT ( 'NONE',  ( 50.56670390244699576, -22.48495420874030515, -5.074374724088000832 ) ) ;
#9696 = CARTESIAN_POINT ( 'NONE',  ( 110.9332348646555175, -45.95165287104040885, 97.89240726581952856 ) ) ;
#9698 = CARTESIAN_POINT ( 'NONE',  ( 103.4152017835535844, -27.65577212482025971, 130.3813395616259925 ) ) ;
#9697 = VECTOR ( 'NONE', #73084, 1000.000000000000000 ) ;
#9699 = EDGE_LOOP ( 'NONE', ( #9466, #4221, #32353, #21465 ) ) ;
#9700 = ORIENTED_EDGE ( 'NONE', *, *, #72938, .T. ) ;
#9701 = ADVANCED_FACE ( 'NONE', ( #8248 ), #35487, .T. ) ;
#9702 = CARTESIAN_POINT ( 'NONE',  ( 109.3646161452266767, -45.83961241216247373, 89.21682140113502157 ) ) ;
#9703 = EDGE_CURVE ( 'NONE', #67094, #28641, #42295, .T. ) ;
#9704 = AXIS2_PLACEMENT_3D ( 'NONE', #23520, #17134, #3058 ) ;
#9705 = PLANE ( 'NONE',  #89314 ) ;
#9707 = DIRECTION ( 'NONE',  ( 1.000000000000000000, 0.000000000000000000, 0.000000000000000000 ) ) ;
#9706 = CARTESIAN_POINT ( 'NONE',  ( 104.3638673426610950, -27.29495504168068365, 221.2984824187679465 ) ) ;
#9708 = CARTESIAN_POINT ( 'NONE',  ( 116.3135889066590636, -32.94480564983713577, 259.1356252759109680 ) ) ;
#9709 = EDGE_CURVE ( 'NONE', #36458, #49665, #671, .T. ) ;
#9710 = DIRECTION ( 'NONE',  ( 0.000000000000000000, 0.000000000000000000, 1.000000000000000000 ) ) ;
#9711 = DIRECTION ( 'NONE',  ( 1.000000000000000078E-15, -1.000000000000000083E-30, -1.000000000000000000 ) ) ;
#9712 = CARTESIAN_POINT ( 'NONE',  ( -12.05184559704344593, 78.45907740360294724, 117.9422764726210602 ) ) ;
#9713 = LINE ( 'NONE', #71508, #28976 ) ;
#9714 = DIRECTION ( 'NONE',  ( 0.000000000000000000, -1.000000000000000000, 0.000000000000000000 ) ) ;
#9715 = ADVANCED_FACE ( 'NONE', ( #63206 ), #36411, .F. ) ;
#9716 = CARTESIAN_POINT ( 'NONE',  ( 114.5119312840560184, -28.59475203354325501, 154.4746728949589851 ) ) ;
#9717 = ORIENTED_EDGE ( 'NONE', *, *, #30070, .T. ) ;
#9719 = VERTEX_POINT ( 'NONE', #73135 ) ;
#9718 = EDGE_CURVE ( 'NONE', #20143, #71729, #50005, .T. ) ;
#9720 = CARTESIAN_POINT ( 'NONE',  ( 111.8591559558596060, -71.06560796536048485, 248.4067532124560103 ) ) ;
#9721 = CARTESIAN_POINT ( 'NONE',  ( 146.9828512772299121, -67.95600236836138208, 246.0626215148325286 ) ) ;
#9722 = CARTESIAN_POINT ( 'NONE',  ( 100.8874678708047412, -44.70022136463035167, 78.05229194121726266 ) ) ;
#9723 = CARTESIAN_POINT ( 'NONE',  ( 25.56670390244797275, -65.37844715994100397, 178.0928068554149775 ) ) ;
#9724 = CARTESIAN_POINT ( 'NONE',  ( 106.9677948388671069, -45.38341651713141545, 230.3976141791149814 ) ) ;
#9725 = AXIS2_PLACEMENT_3D ( 'NONE', #76917, #42367, #63735 ) ;
#9726 = CARTESIAN_POINT ( 'NONE',  ( 131.0667039024480118, -67.87844715994100397, 237.1838068554150141 ) ) ;
#9727 = CARTESIAN_POINT ( 'NONE',  ( 114.1248632939498719, -29.05700933358840032, 199.4841967044819739 ) ) ;
#9728 = CARTESIAN_POINT ( 'NONE',  ( 134.0664832912740110, -46.72944715994100306, 4.925625275910997303 ) ) ;
#9729 = ORIENTED_EDGE ( 'NONE', *, *, #68600, .T. ) ;
#9731 = ORIENTED_EDGE ( 'NONE', *, *, #37455, .F. ) ;
#9730 = ORIENTED_EDGE ( 'NONE', *, *, #1049, .T. ) ;
#9732 = EDGE_CURVE ( 'NONE', #43936, #37298, #51427, .T. ) ;
#9733 = CARTESIAN_POINT ( 'NONE',  ( 113.0895751218732244, -44.74357622511442401, 64.08993167605405006 ) ) ;
#9735 = ADVANCED_FACE ( 'NONE', ( #16851 ), #71820, .T. ) ;
#9734 = DIRECTION ( 'NONE',  ( 0.000000000000000000, 1.000000000000000000, -0.000000000000000000 ) ) ;
#9736 = CARTESIAN_POINT ( 'NONE',  ( 133.8780722764369386, -33.97944715994099596, 8.225625275910998013 ) ) ;
#9737 = EDGE_CURVE ( 'NONE', #79573, #32539, #63050, .T. ) ;
#9738 = CARTESIAN_POINT ( 'NONE',  ( 99.80492824067951574, -39.70159478663597241, 9.453804655305930282 ) ) ;
#9739 = FACE_OUTER_BOUND ( 'NONE', #2713, .T. ) ;
#9740 = ORIENTED_EDGE ( 'NONE', *, *, #39321, .T. ) ;
#9741 = AXIS2_PLACEMENT_3D ( 'NONE', #35243, #61599, #6215 ) ;
#9742 = EDGE_CURVE ( 'NONE', #52329, #85158, #7940, .T. ) ;
#9743 = AXIS2_PLACEMENT_3D ( 'NONE', #36746, #65337, #38076 ) ;
#9744 = CARTESIAN_POINT ( 'NONE',  ( 109.6203647746237948, -44.72533910755026909, 9.635625275910941312 ) ) ;
#9745 = DIRECTION ( 'NONE',  ( 1.000000000000000000, -5.337610695313248426E-16, 0.000000000000000000 ) ) ;
#9746 = ORIENTED_EDGE ( 'NONE', *, *, #45076, .F. ) ;
#9747 = VERTEX_POINT ( 'NONE', #65873 ) ;
#9748 = AXIS2_PLACEMENT_3D ( 'NONE', #85452, #38601, #10461 ) ;
#9749 = CIRCLE ( 'NONE', #21355, 7.143750000000001599 ) ;
#9750 = CARTESIAN_POINT ( 'NONE',  ( 111.4545423736837648, -45.72122411965542454, 112.9377471918615328 ) ) ;
#9751 = VECTOR ( 'NONE', #35635, 1000.000000000000000 ) ;
#9752 = ORIENTED_EDGE ( 'NONE', *, *, #38767, .T. ) ;
#9753 = EDGE_LOOP ( 'NONE', ( #85688, #83935 ) ) ;
#9754 = CARTESIAN_POINT ( 'NONE',  ( 115.0166753900997065, -32.39272993814809354, 23.63432458998199337 ) ) ;
#9755 = CARTESIAN_POINT ( 'NONE',  ( 108.3688725116650602, -47.72941199507204146, 162.6822919425769669 ) ) ;
#9756 = CARTESIAN_POINT ( 'NONE',  ( 96.69266148864264210, -35.94780844399461017, 146.2670538473399517 ) ) ;
#9757 = DIRECTION ( 'NONE',  ( -0.7071067811864666375, -0.7071067811866283970, -7.071067811864971448E-16 ) ) ;
#9758 = CARTESIAN_POINT ( 'NONE',  ( 116.9253062793529665, -41.72720563489927770, 244.4651490854349731 ) ) ;
#9759 = LINE ( 'NONE', #65161, #80438 ) ;
#9760 = CARTESIAN_POINT ( 'NONE',  ( 104.4884655257109642, -26.97921697585386980, 126.2815806043031444 ) ) ;
#9761 = LINE ( 'NONE', #19253, #19259 ) ;
#9762 = ORIENTED_EDGE ( 'NONE', *, *, #2556, .T. ) ;
#9763 = EDGE_LOOP ( 'NONE', ( #22885, #39877, #51909, #10660, #56595, #72729, #25972, #86063, #29563, #24401, #13494, #38447, #82801, #4822, #72600, #86296 ) ) ;
#9764 = CIRCLE ( 'NONE', #44557, 42.54500000000000171 ) ;
#9765 = AXIS2_PLACEMENT_3D ( 'NONE', #65283, #10317, #46145 ) ;
#9766 = AXIS2_PLACEMENT_3D ( 'NONE', #67801, #75067, #40983 ) ;
#9767 = CARTESIAN_POINT ( 'NONE',  ( 98.50147650033493107, -30.70887204493662281, 205.8384824187679669 ) ) ;
#9768 = ORIENTED_EDGE ( 'NONE', *, *, #63647, .T. ) ;
#9769 = CARTESIAN_POINT ( 'NONE',  ( 102.9133425085070712, -27.12904003091135152, 155.4013395616249795 ) ) ;
#9770 = CARTESIAN_POINT ( 'NONE',  ( 107.0667039024470313, -104.2784471599409528, 23.21780685541800082 ) ) ;
#9771 = CARTESIAN_POINT ( 'NONE',  ( 136.1113402350696049, -34.88977106732826172, 7.516154048594613890 ) ) ;
#9772 = CARTESIAN_POINT ( 'NONE',  ( 143.5715564487395852, -139.7453820604759187, 247.2256998566546713 ) ) ;
#9775 = CARTESIAN_POINT ( 'NONE',  ( 115.6373213143783545, -30.77082676042347487, 275.3099109901965562 ) ) ;
#9774 = LINE ( 'NONE', #80610, #29663 ) ;
#9773 = DIRECTION ( 'NONE',  ( 0.000000000000000000, -0.5000000000000061062, 0.8660254037844351549 ) ) ;
#9776 = CARTESIAN_POINT ( 'NONE',  ( -29.99999999999998224, 127.0000000000000000, 114.8826257785461280 ) ) ;
#9777 = DIRECTION ( 'NONE',  ( 0.000000000000000000, -0.000000000000000000, -1.000000000000000000 ) ) ;
#9778 = DIRECTION ( 'NONE',  ( 0.000000000000000000, 0.000000000000000000, 1.000000000000000000 ) ) ;
#9779 = DIRECTION ( 'NONE',  ( -1.000000000000000000, 0.000000000000000000, 4.496403249731880833E-15 ) ) ;
#9780 = CARTESIAN_POINT ( 'NONE',  ( 100.8874679095308409, -44.70022139425450547, 258.0522919450611994 ) ) ;
#9781 = CARTESIAN_POINT ( 'NONE',  ( 70.06670390441306040, -140.6784471619069734, 245.4415720117440003 ) ) ;
#9783 = ORIENTED_EDGE ( 'NONE', *, *, #51517, .F. ) ;
#9782 = CARTESIAN_POINT ( 'NONE',  ( 108.9306573623864267, -44.50959214567147626, 195.5838068554169240 ) ) ;
#9784 = CARTESIAN_POINT ( 'NONE',  ( 134.4432975232482761, -21.47944369576867985, 8.225625303283965906 ) ) ;
#9785 = CARTESIAN_POINT ( 'NONE',  ( 115.0566306311886819, -29.05787713660226856, 189.4232443235299570 ) ) ;
#9786 = CARTESIAN_POINT ( 'NONE',  ( 96.33847535375279847, -41.76377544194641445, 57.67562527591096710 ) ) ;
#9787 = CARTESIAN_POINT ( 'NONE',  ( 113.0470503471827044, -45.36488765107162635, 199.0584824187679374 ) ) ;
#9788 = CARTESIAN_POINT ( 'NONE',  ( 141.8164832912740110, -45.62589376934770513, 14.92562527591100618 ) ) ;
#9789 = FACE_OUTER_BOUND ( 'NONE', #38510, .T. ) ;
#9791 = CARTESIAN_POINT ( 'NONE',  ( 114.1825262577302027, -43.80211088142657161, 39.20373200096445032 ) ) ;
#9790 = DIRECTION ( 'NONE',  ( -3.360405532702990443E-14, 1.000000000000000000, 0.000000000000000000 ) ) ;
#9792 = DIRECTION ( 'NONE',  ( -0.4999999999999998890, 0.000000000000000000, 0.8660254037844387076 ) ) ;
#9793 = DIRECTION ( 'NONE',  ( -0.9254794337955620787, -0.3787978585227822492, 0.000000000000000000 ) ) ;
#9794 = ORIENTED_EDGE ( 'NONE', *, *, #39227, .F. ) ;
#9795 = CIRCLE ( 'NONE', #75074, 12.44599999999999795 ) ;
#9796 = DIRECTION ( 'NONE',  ( 0.000000000000000000, 0.000000000000000000, 1.000000000000000000 ) ) ;
#9797 = EDGE_CURVE ( 'NONE', #44789, #53353, #72267, .T. ) ;
#9798 = VERTEX_POINT ( 'NONE', #44981 ) ;
#9799 = ADVANCED_FACE ( 'NONE', ( #78205 ), #2783, .T. ) ;
#9800 = ORIENTED_EDGE ( 'NONE', *, *, #1826, .T. ) ;
#9801 = CARTESIAN_POINT ( 'NONE',  ( 100.3264543382982907, -29.74069638407027938, 115.1095626852199558 ) ) ;
#9802 = EDGE_CURVE ( 'NONE', #52977, #50184, #65443, .T. ) ;
#9804 = EDGE_LOOP ( 'NONE', ( #68646, #37684, #458, #48010 ) ) ;
#9803 = CARTESIAN_POINT ( 'NONE',  ( -6.710386649963790084, 93.34051461951032991, -130.3838978039176482 ) ) ;
#9805 = CARTESIAN_POINT ( 'NONE',  ( 113.4020503763144063, -27.70036014686462522, 80.57753003781597556 ) ) ;
#9806 = DIRECTION ( 'NONE',  ( 1.000000000000000078E-15, -1.000000000000000083E-30, -1.000000000000000000 ) ) ;
#9807 = DIRECTION ( 'NONE',  ( 0.000000000000000000, 0.000000000000000000, 1.000000000000000000 ) ) ;
#9808 = EDGE_CURVE ( 'NONE', #69984, #86558, #30919, .T. ) ;
#9809 = ADVANCED_FACE ( 'NONE', ( #3225, #86344 ), #51785, .F. ) ;
#9810 = CARTESIAN_POINT ( 'NONE',  ( 97.81169128372820865, -40.51741339292117772, 177.6357569005977268 ) ) ;
#9811 = AXIS2_PLACEMENT_3D ( 'NONE', #49510, #34094, #27292 ) ;
#9812 = CARTESIAN_POINT ( 'NONE',  ( 104.6499073705539331, -46.24122592705978718, 47.37848241876896083 ) ) ;
#9813 = ORIENTED_EDGE ( 'NONE', *, *, #36190, .T. ) ;
#9814 = ORIENTED_EDGE ( 'NONE', *, *, #89251, .T. ) ;
#9815 = VERTEX_POINT ( 'NONE', #24558 ) ;
#9816 = EDGE_CURVE ( 'NONE', #58010, #15778, #29736, .T. ) ;
#9817 = AXIS2_PLACEMENT_3D ( 'NONE', #42171, #43512, #77612 ) ;
#9818 = VECTOR ( 'NONE', #47734, 1000.000000000000000 ) ;
#9819 = DIRECTION ( 'NONE',  ( 4.299999999999999979E-14, -1.000000000000000000, 4.400000000000000367E-29 ) ) ;
#9820 = LINE ( 'NONE', #52448, #56357 ) ;
#9821 = DIRECTION ( 'NONE',  ( 0.000000000000000000, 1.000000000000000000, 0.000000000000000000 ) ) ;
#9822 = CARTESIAN_POINT ( 'NONE',  ( 151.0371591254573502, -24.42818131005592974, 249.9678068554149490 ) ) ;
#9823 = DIRECTION ( 'NONE',  ( 1.000000000000000000, 0.000000000000000000, -0.000000000000000000 ) ) ;
#9824 = EDGE_CURVE ( 'NONE', #20049, #35637, #17740, .T. ) ;
#9825 = CARTESIAN_POINT ( 'NONE',  ( 97.81193178031652735, -40.51732023384165160, 27.63604381180012837 ) ) ;
#9826 = DIRECTION ( 'NONE',  ( 0.7071067811865561215, 1.189321603860061305E-16, -0.7071067811865389130 ) ) ;
#9827 = AXIS2_PLACEMENT_3D ( 'NONE', #10808, #4001, #87575 ) ;
#9828 = CARTESIAN_POINT ( 'NONE',  ( -7.057053722110693705, 93.10878806376580030, 130.3651300669557997 ) ) ;
#9829 = CARTESIAN_POINT ( 'NONE',  ( 106.5192459994187715, -25.71289806663794408, 45.12800622829193742 ) ) ;
#9831 = ORIENTED_EDGE ( 'NONE', *, *, #36375, .F. ) ;
#9830 = EDGE_CURVE ( 'NONE', #43807, #65403, #26495, .T. ) ;
#9832 = CIRCLE ( 'NONE', #89580, 0.5000000000000104361 ) ;
#9833 = CARTESIAN_POINT ( 'NONE',  ( 2.883471595053340053, 94.92538689125287021, 130.5247975405367811 ) ) ;
#9834 = DIRECTION ( 'NONE',  ( 0.000000000000000000, 0.000000000000000000, -1.000000000000000000 ) ) ;
#9835 = CIRCLE ( 'NONE', #86728, 4.875000000000017764 ) ;
#9836 = LINE ( 'NONE', #72934, #56846 ) ;
#9837 = CARTESIAN_POINT ( 'NONE',  ( 101.2865843167392654, -43.98814532200950822, 119.8595189410199566 ) ) ;
#9838 = ADVANCED_FACE ( 'NONE', ( #88581 ), #33151, .T. ) ;
#9839 = CIRCLE ( 'NONE', #73623, 2.116999999999980009 ) ;
#9840 = CARTESIAN_POINT ( 'NONE',  ( 41.56648329127399677, -9.303447159940999356, 318.9256252759120116 ) ) ;
#9841 = DIRECTION ( 'NONE',  ( 0.7071067811868035902, 0.7071067811862914443, 7.071067811868340870E-16 ) ) ;
#9842 = EDGE_LOOP ( 'NONE', ( #26792, #47677, #68908, #15386, #47022, #11163 ) ) ;
#9843 = VERTEX_POINT ( 'NONE', #67675 ) ;
#9844 = CARTESIAN_POINT ( 'NONE',  ( 97.82526847378206014, -40.55045903170837818, 136.6388370546689259 ) ) ;
#9845 = ORIENTED_EDGE ( 'NONE', *, *, #78062, .T. ) ;
#9846 = ORIENTED_EDGE ( 'NONE', *, *, #29676, .T. ) ;
#9847 = EDGE_CURVE ( 'NONE', #42012, #48511, #74941, .T. ) ;
#9848 = CARTESIAN_POINT ( 'NONE',  ( 98.83447963006204873, -41.25831470702095061, 173.1463452106589784 ) ) ;
#9849 = DIRECTION ( 'NONE',  ( -0.000000000000000000, -1.000000000000000000, -0.000000000000000000 ) ) ;
#9850 = EDGE_CURVE ( 'NONE', #17117, #5375, #19074, .T. ) ;
#9851 = CARTESIAN_POINT ( 'NONE',  ( 117.6299819888065912, -33.39812594883869679, 125.0575300378149706 ) ) ;
#9852 = DIRECTION ( 'NONE',  ( -1.000000000000000000, 0.000000000000000000, 4.496403249731880833E-15 ) ) ;
#9853 = VECTOR ( 'NONE', #36339, 1000.000000000000000 ) ;
#9854 = CARTESIAN_POINT ( 'NONE',  ( 77.31648329127401098, -36.72944715994107412, 6.749768910606400496 ) ) ;
#9855 = ORIENTED_EDGE ( 'NONE', *, *, #47390, .F. ) ;
#9856 = ORIENTED_EDGE ( 'NONE', *, *, #30132, .T. ) ;
#9857 = ORIENTED_EDGE ( 'NONE', *, *, #64872, .T. ) ;
#9858 = CARTESIAN_POINT ( 'NONE',  ( 98.92939184154955967, -35.79647825066581390, 204.0538046553059814 ) ) ;
#9859 = CARTESIAN_POINT ( 'NONE',  ( 117.2885226371813872, -38.88728764921428649, 63.66133956162494911 ) ) ;
#9860 = ORIENTED_EDGE ( 'NONE', *, *, #46396, .T. ) ;
#9861 = CARTESIAN_POINT ( 'NONE',  ( 104.7405551043178491, -47.51155644559854352, 32.41943479972098174 ) ) ;
#9862 = LINE ( 'NONE', #25714, #21989 ) ;
#9863 = CARTESIAN_POINT ( 'NONE',  ( 52.06670390244700997, -79.67844715994100113, 55.21780685541800437 ) ) ;
#9864 = CARTESIAN_POINT ( 'NONE',  ( 96.01412018463531695, -36.58377574468403282, 152.3280062282919971 ) ) ;
#9865 = CARTESIAN_POINT ( 'NONE',  ( 19.56670390244740076, -47.82844715994204421, 180.4678068554150911 ) ) ;
#9866 = ORIENTED_EDGE ( 'NONE', *, *, #41587, .F. ) ;
#9867 = CARTESIAN_POINT ( 'NONE',  ( -544.5124999999999318, 53.97500000000000142, 14.22400000000000020 ) ) ;
#9868 = VECTOR ( 'NONE', #24949, 1000.000000000000000 ) ;
#9869 = ORIENTED_EDGE ( 'NONE', *, *, #8233, .T. ) ;
#9870 = FACE_OUTER_BOUND ( 'NONE', #6661, .T. ) ;
#9871 = EDGE_LOOP ( 'NONE', ( #69340, #89239, #33946, #88363 ) ) ;
#9872 = EDGE_LOOP ( 'NONE', ( #22194, #88936 ) ) ;
#9873 = EDGE_CURVE ( 'NONE', #12790, #87834, #54010, .T. ) ;
#9874 = AXIS2_PLACEMENT_3D ( 'NONE', #65092, #71481, #77843 ) ;
#9875 = PLANE ( 'NONE',  #11303 ) ;
#9876 = CIRCLE ( 'NONE', #53400, 1.000000000000000888 ) ;
#9877 = FACE_OUTER_BOUND ( 'NONE', #57266, .T. ) ;
#9878 = CARTESIAN_POINT ( 'NONE',  ( 101.1416012009399026, -28.10844496237015733, 50.55562527591095545 ) ) ;
#9879 = CARTESIAN_POINT ( 'NONE',  ( 6.836113969089879561, 69.74575608423708672, 37.48795912257015317 ) ) ;
#9880 = CARTESIAN_POINT ( 'NONE',  ( 107.0664832912739968, 12.92155284005902516, 333.4006252759110112 ) ) ;
#9881 = CARTESIAN_POINT ( 'NONE',  ( 108.3334481027989540, -46.73485935290891291, 73.67729194320179431 ) ) ;
#9882 = CARTESIAN_POINT ( 'NONE',  ( 97.35459460924916186, -38.14118110200430323, 66.44133956162595211 ) ) ;
#9884 = CARTESIAN_POINT ( 'NONE',  ( 117.7782040715256926, -34.09831434418946827, 160.0061014663869798 ) ) ;
#9883 = DIRECTION ( 'NONE',  ( -1.000000000000000000, -1.206764157201257538E-15, 0.000000000000000000 ) ) ;
#9885 = CARTESIAN_POINT ( 'NONE',  ( 97.33756857962994502, -34.07217399619458575, 61.11488175924079513 ) ) ;
#9886 = DIRECTION ( 'NONE',  ( 4.194175870806139918E-14, -1.000000000000000000, 0.000000000000000000 ) ) ;
#9887 = ORIENTED_EDGE ( 'NONE', *, *, #68087, .F. ) ;
#9888 = CARTESIAN_POINT ( 'NONE',  ( 173.9900000000000091, 20.32000000000000028, -71.37400000000000944 ) ) ;
#9889 = VECTOR ( 'NONE', #5482, 1000.000000000000114 ) ;
#9890 = CARTESIAN_POINT ( 'NONE',  ( 257.5940999999999690, 52.73749999999999716, 10.66800000000000104 ) ) ;
#9891 = PLANE ( 'NONE',  #79268 ) ;
#9892 = CONICAL_SURFACE ( 'NONE', #62073, 7.000000000000006217, 0.7853981633974699283 ) ;
#9893 = PLANE ( 'NONE',  #66545 ) ;
#9895 = ORIENTED_EDGE ( 'NONE', *, *, #22033, .F. ) ;
#9894 = CARTESIAN_POINT ( 'NONE',  ( 97.88046564956832185, -41.75177191353013484, 221.7241967044819546 ) ) ;
#9896 = CARTESIAN_POINT ( 'NONE',  ( 113.2454386374689221, -28.75862319911502851, 144.5522981085485412 ) ) ;
#9897 = CARTESIAN_POINT ( 'NONE',  ( 115.9252781128442535, -30.08061567962537453, 260.3508633711493871 ) ) ;
#9898 = CARTESIAN_POINT ( 'NONE',  ( 113.3408031569382644, -28.30502284670691182, 100.5670538473389684 ) ) ;
#9899 = CARTESIAN_POINT ( 'NONE',  ( 0.000000000000000000, 61.59999999999999432, 130.5560000000000116 ) ) ;
#9900 = VECTOR ( 'NONE', #33881, 1000.000000000000000 ) ;
#9901 = FACE_BOUND ( 'NONE', #72544, .T. ) ;
#9902 = ADVANCED_FACE ( 'NONE', ( #75393 ), #47209, .T. ) ;
#9903 = CARTESIAN_POINT ( 'NONE',  ( 107.0667039024470313, -104.2784471599413791, 2.217806855418003043 ) ) ;
#9904 = DIRECTION ( 'NONE',  ( -0.7071067811865175967, -0.7071067811865774377, -7.071067811865480264E-16 ) ) ;
#9905 = ORIENTED_EDGE ( 'NONE', *, *, #5669, .F. ) ;
#9906 = EDGE_CURVE ( 'NONE', #34082, #88226, #40411, .T. ) ;
#9907 = ORIENTED_EDGE ( 'NONE', *, *, #11122, .T. ) ;
#9908 = ADVANCED_FACE ( 'NONE', ( #74039 ), #46758, .F. ) ;
#9909 = ORIENTED_EDGE ( 'NONE', *, *, #75396, .F. ) ;
#9910 = CIRCLE ( 'NONE', #21520, 2.029999999999997140 ) ;
#9911 = EDGE_CURVE ( 'NONE', #71729, #20143, #19536, .T. ) ;
#9912 = ORIENTED_EDGE ( 'NONE', *, *, #29499, .F. ) ;
#9913 = DIRECTION ( 'NONE',  ( 0.000000000000000000, 0.000000000000000000, 1.000000000000000000 ) ) ;
#9914 = CARTESIAN_POINT ( 'NONE',  ( 106.8364377494367403, -47.15199802307920152, 268.5584824187679374 ) ) ;
#9915 = DIRECTION ( 'NONE',  ( -1.000000000000000000, 0.000000000000000000, 0.000000000000000000 ) ) ;
#9916 = DIRECTION ( 'NONE',  ( 0.000000000000000000, 0.000000000000000000, 1.000000000000000000 ) ) ;
#9917 = ADVANCED_FACE ( 'NONE', ( #5454 ), #14411, .F. ) ;
#9919 = CARTESIAN_POINT ( 'NONE',  ( 91.90737012895596081, 78.46643079253878739, 74.89042153202969132 ) ) ;
#9918 = LINE ( 'NONE', #24439, #6206 ) ;
#9920 = CARTESIAN_POINT ( 'NONE',  ( 156.5667039024483813, -48.82844715993569196, 257.2178068554149490 ) ) ;
#9921 = AXIS2_PLACEMENT_3D ( 'NONE', #60878, #88164, #12746 ) ;
#9922 = CARTESIAN_POINT ( 'NONE',  ( 107.2112434921279629, -45.29864470754334604, 212.0124198280769861 ) ) ;
#9923 = ORIENTED_EDGE ( 'NONE', *, *, #82809, .T. ) ;
#9924 = VECTOR ( 'NONE', #27448, 1000.000000000000000 ) ;
#9925 = ORIENTED_EDGE ( 'NONE', *, *, #46820, .F. ) ;
#9926 = ORIENTED_EDGE ( 'NONE', *, *, #48509, .T. ) ;
#9927 = EDGE_CURVE ( 'NONE', #9271, #35871, #2185, .T. ) ;
#9928 = FACE_OUTER_BOUND ( 'NONE', #51130, .T. ) ;
#9929 = DIRECTION ( 'NONE',  ( 0.7071067811865398012, 0.000000000000000000, 0.7071067811865552333 ) ) ;
#9930 = CARTESIAN_POINT ( 'NONE',  ( 97.18779024860596394, -39.88384922728100435, 277.5603871806723646 ) ) ;
#9931 = ADVANCED_FACE ( 'NONE', ( #18629 ), #26775, .F. ) ;
#9932 = CARTESIAN_POINT ( 'NONE',  ( 107.0664832912750057, -36.72944715993903486, 3.024967495036150922 ) ) ;
#9933 = CARTESIAN_POINT ( 'NONE',  ( 3.175000000000334666, 17.78000000000000114, 31.75000000000000000 ) ) ;
#9934 = CARTESIAN_POINT ( 'NONE',  ( -492.0614999999999668, 14.28750000000026077, 11.11249999999970051 ) ) ;
#9935 = ORIENTED_EDGE ( 'NONE', *, *, #460, .T. ) ;
#9936 = AXIS2_PLACEMENT_3D ( 'NONE', #40700, #74339, #6199 ) ;
#9937 = FACE_OUTER_BOUND ( 'NONE', #49697, .T. ) ;
#9938 = VERTEX_POINT ( 'NONE', #7589 ) ;
#9939 = DIRECTION ( 'NONE',  ( 1.000000000000000000, 1.709087168450053081E-14, 0.000000000000000000 ) ) ;
#9940 = CARTESIAN_POINT ( 'NONE',  ( 101.9647735066782843, -29.73848997801458083, 28.38428084578198352 ) ) ;
#9941 = CIRCLE ( 'NONE', #43242, 2.999999999999975131 ) ;
#9942 = DIRECTION ( 'NONE',  ( 0.8571673007021091140, -8.250245410175212261E-16, 0.5150380749100597066 ) ) ;
#9943 = CYLINDRICAL_SURFACE ( 'NONE', #33093, 9.525000000000000355 ) ;
#9944 = CARTESIAN_POINT ( 'NONE',  ( 92.32962665258612844, 82.54999999999999716, -74.36911441044637172 ) ) ;
#9945 = ORIENTED_EDGE ( 'NONE', *, *, #73982, .F. ) ;
#9946 = LINE ( 'NONE', #36309, #81322 ) ;
#9947 = VECTOR ( 'NONE', #15211, 1000.000000000000000 ) ;
#9948 = FACE_OUTER_BOUND ( 'NONE', #11664, .T. ) ;
#9949 = VERTEX_POINT ( 'NONE', #35276 ) ;
#9950 = CARTESIAN_POINT ( 'NONE',  ( 98.09668637883959263, -31.41627731406707724, 85.90133956162493689 ) ) ;
#9951 = ORIENTED_EDGE ( 'NONE', *, *, #21931, .F. ) ;
#9952 = CARTESIAN_POINT ( 'NONE',  ( 109.1774539423994952, -45.00591588954721800, 47.19813411379097801 ) ) ;
#9953 = AXIS2_PLACEMENT_3D ( 'NONE', #48779, #14294, #50128 ) ;
#9954 = DIRECTION ( 'NONE',  ( 0.000000000000000000, 0.000000000000000000, 1.000000000000000000 ) ) ;
#9955 = CARTESIAN_POINT ( 'NONE',  ( 106.8749774919903359, -46.80089345537784595, 73.99301187732598351 ) ) ;
#9956 = CARTESIAN_POINT ( 'NONE',  ( 108.3325648527817719, -46.73495960743948530, 13.67722169067239157 ) ) ;
#9957 = DIRECTION ( 'NONE',  ( 1.000000000000000000, 4.163336342344333240E-14, 0.000000000000000000 ) ) ;
#9958 = AXIS2_PLACEMENT_3D ( 'NONE', #22751, #57235, #22295 ) ;
#9959 = EDGE_CURVE ( 'NONE', #74494, #10702, #5001, .T. ) ;
#9960 = CARTESIAN_POINT ( 'NONE',  ( 112.7920658800750005, -68.84166263841879640, 247.5834178368470191 ) ) ;
#9961 = CARTESIAN_POINT ( 'NONE',  ( 112.1278237076712543, -26.87713336146359211, 15.71086337114896381 ) ) ;
#9962 = LINE ( 'NONE', #58099, #30736 ) ;
#9963 = ORIENTED_EDGE ( 'NONE', *, *, #20468, .F. ) ;
#9964 = CARTESIAN_POINT ( 'NONE',  ( -31.75000000000000000, 111.1250000000000000, 3.174999999999779998 ) ) ;
#9965 = VERTEX_POINT ( 'NONE', #32246 ) ;
#9966 = CARTESIAN_POINT ( 'NONE',  ( 117.3528398777633299, -34.78421141941176842, 154.9756252759109714 ) ) ;
#9967 = DIRECTION ( 'NONE',  ( 0.7071067811865460184, 0.000000000000000000, -0.7071067811865489050 ) ) ;
#9968 = ORIENTED_EDGE ( 'NONE', *, *, #52726, .T. ) ;
#9969 = ORIENTED_EDGE ( 'NONE', *, *, #48563, .T. ) ;
#9970 = VECTOR ( 'NONE', #77127, 1000.000000000000000 ) ;
#9971 = CARTESIAN_POINT ( 'NONE',  ( 83.56670559755329464, -36.73837296219065252, 239.5838068554176914 ) ) ;
#9972 = DIRECTION ( 'NONE',  ( 0.000000000000000000, 1.000000000000000000, 0.000000000000000000 ) ) ;
#9973 = CARTESIAN_POINT ( 'NONE',  ( 101.7740290765682403, -45.64733444449330335, 207.1622919425779514 ) ) ;
#9974 = DIRECTION ( 'NONE',  ( 0.000000000000000000, 1.000000000000000000, 0.000000000000000000 ) ) ;
#9975 = CARTESIAN_POINT ( 'NONE',  ( 144.7505022533608496, -139.5561530133492170, 246.9828090814930022 ) ) ;
#9976 = CARTESIAN_POINT ( 'NONE',  ( 123.4403675665762989, -109.5826158781450914, -10.56397404668061135 ) ) ;
#9977 = CARTESIAN_POINT ( 'NONE',  ( 99.14357900773808296, -43.50514455292471894, 27.88991099019694175 ) ) ;
#9978 = DIRECTION ( 'NONE',  ( 0.000000000000000000, 0.000000000000000000, 1.000000000000000000 ) ) ;
#9979 = ORIENTED_EDGE ( 'NONE', *, *, #65322, .T. ) ;
#9980 = CARTESIAN_POINT ( 'NONE',  ( 103.2773610487370632, -27.47512100226090581, 171.3857244979931522 ) ) ;
#9981 = FACE_OUTER_BOUND ( 'NONE', #16758, .T. ) ;
#9982 = ORIENTED_EDGE ( 'NONE', *, *, #32866, .T. ) ;
#9983 = EDGE_CURVE ( 'NONE', #84959, #7062, #13479, .T. ) ;
#9984 = CARTESIAN_POINT ( 'NONE',  ( 183.5150000000000148, 68.61249999999999716, -53.61543552338530105 ) ) ;
#9985 = CARTESIAN_POINT ( 'NONE',  ( 107.0664832912739968, 25.62155284005901379, 327.8006252759110453 ) ) ;
#9986 = CARTESIAN_POINT ( 'NONE',  ( 112.4430884738663821, -45.67687932769439385, 238.0070538473389377 ) ) ;
#9987 = DIRECTION ( 'NONE',  ( 0.000000000000000000, 1.000000000000000000, 0.000000000000000000 ) ) ;
#9988 = CARTESIAN_POINT ( 'NONE',  ( 107.0664832912750057, -36.72944715993903486, 9.425625275910970657 ) ) ;
#9989 = FACE_OUTER_BOUND ( 'NONE', #58277, .T. ) ;
#9990 = CARTESIAN_POINT ( 'NONE',  ( 100.3746636439974935, -30.62762610928201568, 230.1486103042669811 ) ) ;
#9992 = CARTESIAN_POINT ( 'NONE',  ( 111.9186950350129877, -27.52701776748444473, 55.68991099019693536 ) ) ;
#9991 = FACE_OUTER_BOUND ( 'NONE', #10922, .T. ) ;
#9993 = CARTESIAN_POINT ( 'NONE',  ( 114.4819906290133247, 70.80449033172386919, 62.76244765184264907 ) ) ;
#9994 = CARTESIAN_POINT ( 'NONE',  ( 109.5188487141873850, -46.90749067903785630, 132.7641967044819751 ) ) ;
#9995 = EDGE_LOOP ( 'NONE', ( #17315, #57981, #23039, #45726 ) ) ;
#9996 = LINE ( 'NONE', #3184, #32154 ) ;
#9997 = ORIENTED_EDGE ( 'NONE', *, *, #87623, .F. ) ;
#9998 = CARTESIAN_POINT ( 'NONE',  ( 51.23005224011598102, -33.89581943344511217, -5.074374724088000832 ) ) ;
#9999 = CARTESIAN_POINT ( 'NONE',  ( 97.07207205126279348, -35.37844125359542602, 67.21895861358602531 ) ) ;
#10000 = DIRECTION ( 'NONE',  ( -0.7071067811865483499, -7.937023868100978726E-16, -0.7071067811865466846 ) ) ;
#10001 = EDGE_LOOP ( 'NONE', ( #13076, #16866, #26174, #40502 ) ) ;
#10002 = VECTOR ( 'NONE', #27858, 1000.000000000000000 ) ;
#10003 = CARTESIAN_POINT ( 'NONE',  ( 152.0371591254585724, -47.82818131005587503, 117.4678068554150485 ) ) ;
#10004 = ORIENTED_EDGE ( 'NONE', *, *, #84548, .T. ) ;
#10005 = DIRECTION ( 'NONE',  ( 0.000000000000000000, 0.000000000000000000, -1.000000000000000000 ) ) ;
#10006 = LINE ( 'NONE', #24526, #24400 ) ;
#10008 = CARTESIAN_POINT ( 'NONE',  ( 50.97905606903270836, -31.62489322948282222, 117.4678068554150485 ) ) ;
#10007 = VECTOR ( 'NONE', #74934, 1000.000000000000000 ) ;
#10009 = VERTEX_POINT ( 'NONE', #87672 ) ;
#10010 = AXIS2_PLACEMENT_3D ( 'NONE', #8276, #56401, #27811 ) ;
#10011 = CARTESIAN_POINT ( 'NONE',  ( 115.2246207261642894, -44.22212590188486558, 78.22324432352995416 ) ) ;
#10012 = FILL_AREA_STYLE_COLOUR ( '', #21696 ) ;
#10013 = DIRECTION ( 'NONE',  ( 0.000000000000000000, 0.000000000000000000, -1.000000000000000000 ) ) ;
#10014 = DIRECTION ( 'NONE',  ( -4.237773401492740281E-14, 1.000000000000000000, 0.000000000000000000 ) ) ;
#10015 = CARTESIAN_POINT ( 'NONE',  ( 137.0667039024470171, -90.27844715994091018, 51.21780685541800437 ) ) ;
#10016 = ORIENTED_EDGE ( 'NONE', *, *, #13908, .F. ) ;
#10017 = EDGE_CURVE ( 'NONE', #5965, #20346, #28194, .T. ) ;
#10018 = AXIS2_PLACEMENT_3D ( 'NONE', #19116, #88179, #46796 ) ;
#10019 = EDGE_CURVE ( 'NONE', #47532, #43122, #25894, .T. ) ;
#10020 = CYLINDRICAL_SURFACE ( 'NONE', #50447, 1.000000000000000888 ) ;
#10021 = LINE ( 'NONE', #23229, #70117 ) ;
#10022 = ADVANCED_FACE ( 'NONE', ( #84360 ), #77083, .T. ) ;
#10023 = AXIS2_PLACEMENT_3D ( 'NONE', #3783, #65560, #3340 ) ;
#10024 = LINE ( 'NONE', #43624, #79169 ) ;
#10025 = ADVANCED_FACE ( 'NONE', ( #8032 ), #22572, .T. ) ;
#10026 = CIRCLE ( 'NONE', #20135, 1.000000000002049694 ) ;
#10028 = DIRECTION ( 'NONE',  ( 3.100000000000000258E-29, -3.100000000000000044E-14, -1.000000000000000000 ) ) ;
#10027 = DIRECTION ( 'NONE',  ( 1.000000000000000078E-15, -1.000000000000000083E-30, -1.000000000000000000 ) ) ;
#10029 = DIRECTION ( 'NONE',  ( -0.000000000000000000, 1.000000000000000000, -0.000000000000000000 ) ) ;
#10030 = ORIENTED_EDGE ( 'NONE', *, *, #36905, .T. ) ;
#10031 = CARTESIAN_POINT ( 'NONE',  ( 134.0664832912740110, -46.72944715994100306, 4.925625275910997303 ) ) ;
#10032 = CARTESIAN_POINT ( 'NONE',  ( 113.8091913586853821, -43.81457933525486936, 154.1813395616249807 ) ) ;
#10033 = ADVANCED_FACE ( 'NONE', ( #35726 ), #28281, .F. ) ;
#10034 = VECTOR ( 'NONE', #6737, 1000.000000000000000 ) ;
#10036 = ORIENTED_EDGE ( 'NONE', *, *, #24204, .T. ) ;
#10035 = CARTESIAN_POINT ( 'NONE',  ( 67.06673837846007302, -137.6758525980020806, 245.5072637273240161 ) ) ;
#10037 = CARTESIAN_POINT ( 'NONE',  ( 100.9974690995740190, -29.01719307973645812, 11.60705384733895507 ) ) ;
#10038 = CARTESIAN_POINT ( 'NONE',  ( 141.8164832912740394, -36.72944715994099596, -5.074374724088994704 ) ) ;
#10039 = DIRECTION ( 'NONE',  ( 0.000000000000000000, 1.000000000000000000, 0.000000000000000000 ) ) ;
#10040 = DIRECTION ( 'NONE',  ( 0.000000000000000000, -1.000000000000000000, 0.000000000000000000 ) ) ;
#10041 = ORIENTED_EDGE ( 'NONE', *, *, #31933, .T. ) ;
#10042 = DIRECTION ( 'NONE',  ( -0.9254794337955620787, -0.3787978585227822492, 0.000000000000000000 ) ) ;
#10043 = ORIENTED_EDGE ( 'NONE', *, *, #13403, .F. ) ;
#10044 = ORIENTED_EDGE ( 'NONE', *, *, #81496, .F. ) ;
#10045 = VECTOR ( 'NONE', #49690, 1000.000000000000000 ) ;
#10046 = CARTESIAN_POINT ( 'NONE',  ( 102.2713888833019240, -44.80927359098731699, 203.5939642582779641 ) ) ;
#10047 = CARTESIAN_POINT ( 'NONE',  ( 4.163101094985349692E-14, 120.6499999999999915, -98.60478223830740774 ) ) ;
#10048 = CARTESIAN_POINT ( 'NONE',  ( 100.2657625843003899, -43.21224928579215430, 33.35205949637398959 ) ) ;
#10049 = CARTESIAN_POINT ( 'NONE',  ( 23.71360729876448303, 83.79303145207032344, 307.5031054200276799 ) ) ;
#10050 = CARTESIAN_POINT ( 'NONE',  ( 115.0889047246006669, -30.61763668096888580, 79.34395860915145704 ) ) ;
#10051 = CARTESIAN_POINT ( 'NONE',  ( -254.0000000000000000, 93.66249999999999432, 90.48749999999999716 ) ) ;
#10052 = ORIENTED_EDGE ( 'NONE', *, *, #47098, .F. ) ;
#10053 = FACE_OUTER_BOUND ( 'NONE', #17360, .T. ) ;
#10054 = LINE ( 'NONE', #10493, #35736 ) ;
#10055 = VERTEX_POINT ( 'NONE', #64787 ) ;
#10056 = CARTESIAN_POINT ( 'NONE',  ( 99.55514648348071205, -29.48070623161989801, 250.7156252759109520 ) ) ;
#10057 = FACE_BOUND ( 'NONE', #73819, .T. ) ;
#10058 = EDGE_LOOP ( 'NONE', ( #1921, #38732, #57507, #10281 ) ) ;
#10059 = AXIS2_PLACEMENT_3D ( 'NONE', #2314, #24095, #30897 ) ;
#10060 = CARTESIAN_POINT ( 'NONE',  ( 165.3359832912747436, -36.32844715993532958, 313.9678068554149490 ) ) ;
#10061 = CARTESIAN_POINT ( 'NONE',  ( 164.9667039024474491, -28.27351298636832766, 313.9678068554149490 ) ) ;
#10062 = CARTESIAN_POINT ( 'NONE',  ( 107.0664832912739968, -36.72944715994100306, 287.6356252759109680 ) ) ;
#10063 = CARTESIAN_POINT ( 'NONE',  ( 131.2274048610838406, -69.45962296279897430, 247.5830566269779922 ) ) ;
#10064 = ADVANCED_FACE ( 'NONE', ( #43879 ), #1679, .T. ) ;
#10065 = CARTESIAN_POINT ( 'NONE',  ( 103.2878376434171628, -26.96651641063459337, 211.3699109901969848 ) ) ;
#10067 = CARTESIAN_POINT ( 'NONE',  ( 103.1875000000000000, 127.0000000000000000, 7.143750000000359535 ) ) ;
#10066 = VECTOR ( 'NONE', #82564, 1000.000000000000000 ) ;
#10068 = AXIS2_PLACEMENT_3D ( 'NONE', #58861, #24807, #66576 ) ;
#10069 = ORIENTED_EDGE ( 'NONE', *, *, #11842, .F. ) ;
#10070 = CARTESIAN_POINT ( 'NONE',  ( 114.8518103909616315, -43.72813715869710904, 34.24419670448197905 ) ) ;
#10071 = CARTESIAN_POINT ( 'NONE',  ( 59.56670390244699576, -67.87844715994098976, 85.21780685541799016 ) ) ;
#10072 = EDGE_CURVE ( 'NONE', #12139, #34789, #46750, .T. ) ;
#10073 = CARTESIAN_POINT ( 'NONE',  ( 100.2471064434660093, -45.42859581790747825, 277.0594347997204636 ) ) ;
#10074 = EDGE_LOOP ( 'NONE', ( #48070, #72758, #3943, #72224 ) ) ;
#10075 = CIRCLE ( 'NONE', #11568, 1.000000000000000888 ) ;
#10076 = FACE_OUTER_BOUND ( 'NONE', #82013, .T. ) ;
#10077 = CARTESIAN_POINT ( 'NONE',  ( 117.0716111955790808, -35.46010980090269982, 19.92736465657518963 ) ) ;
#10078 =( GEOMETRIC_REPRESENTATION_CONTEXT ( 3 ) GLOBAL_UNCERTAINTY_ASSIGNED_CONTEXT ( ( #71455 ) ) GLOBAL_UNIT_ASSIGNED_CONTEXT ( ( #87751, #12805, #53188 ) ) REPRESENTATION_CONTEXT ( 'NONE', 'WORKASPACE' ) );
#10079 = DIRECTION ( 'NONE',  ( -0.9254794337955620787, -0.3787978585227822492, 0.000000000000000000 ) ) ;
#10080 = CARTESIAN_POINT ( 'NONE',  ( 104.1008407059626251, -44.85999997644839254, 95.10428084578198593 ) ) ;
#10081 = CARTESIAN_POINT ( 'NONE',  ( 113.0378785334839193, -46.05830800173890793, 214.0175300378159591 ) ) ;
#10082 = DIRECTION ( 'NONE',  ( 0.000000000000000000, 0.000000000000000000, 1.000000000000000000 ) ) ;
#10083 = ORIENTED_EDGE ( 'NONE', *, *, #27713, .T. ) ;
#10084 = CIRCLE ( 'NONE', #1335, 38.10000000000000142 ) ;
#10085 = PLANE ( 'NONE',  #37456 ) ;
#10086 = VERTEX_POINT ( 'NONE', #56155 ) ;
#10087 = ORIENTED_EDGE ( 'NONE', *, *, #81401, .T. ) ;
#10088 = EDGE_CURVE ( 'NONE', #52469, #64816, #83906, .T. ) ;
#10089 = DIRECTION ( 'NONE',  ( -4.237773401492740281E-14, 1.000000000000000000, 0.000000000000000000 ) ) ;
#10090 = VERTEX_POINT ( 'NONE', #50245 ) ;
#10091 = ORIENTED_EDGE ( 'NONE', *, *, #8218, .T. ) ;
#10092 = CARTESIAN_POINT ( 'NONE',  ( 107.0664832912739399, -36.72944715994095333, 312.1356252759112522 ) ) ;
#10093 = FACE_OUTER_BOUND ( 'NONE', #9804, .T. ) ;
#10094 = CIRCLE ( 'NONE', #4325, 2.750000000000002665 ) ;
#10095 = CARTESIAN_POINT ( 'NONE',  ( 98.49703967840136443, -36.85882374884989332, 135.7609912566479409 ) ) ;
#10096 = CARTESIAN_POINT ( 'NONE',  ( 97.31040724827032307, -32.83447933365327742, 41.02419670448193045 ) ) ;
#10097 = CARTESIAN_POINT ( 'NONE',  ( -4.084841600441663445, 70.51762400537137410, 130.4926920574403937 ) ) ;
#10098 = EDGE_LOOP ( 'NONE', ( #34355, #17990 ) ) ;
#10099 = ORIENTED_CLOSED_SHELL ( 'NONE', *, #85136, .F. );
#10100 = CARTESIAN_POINT ( 'NONE',  ( 103.2778847236115780, -27.47490660443877886, 136.3856794586381511 ) ) ;
#10101 = VERTEX_POINT ( 'NONE', #21676 ) ;
#10102 = DIRECTION ( 'NONE',  ( -0.7071067811875186848, -0.7071067811855763496, -7.071067811875180294E-16 ) ) ;
#10103 = DIRECTION ( 'NONE',  ( 1.000000000000000000, 0.000000000000000000, 0.000000000000000000 ) ) ;
#10104 = DIRECTION ( 'NONE',  ( 0.000000000000000000, 0.000000000000000000, -1.000000000000000000 ) ) ;
#10105 = AXIS2_PLACEMENT_3D ( 'NONE', #87358, #12851, #67336 ) ;
#10106 = CARTESIAN_POINT ( 'NONE',  ( 96.49234500119369784, -40.10591448887350197, 281.5603871806727625 ) ) ;
#10107 = ORIENTED_EDGE ( 'NONE', *, *, #37291, .T. ) ;
#10108 = CARTESIAN_POINT ( 'NONE',  ( 118.1032226039154267, -36.12160442421116358, 273.8822919425776945 ) ) ;
#10109 = CARTESIAN_POINT ( 'NONE',  ( 101.3604548305157920, -27.95253318249931596, 21.53562527591096298 ) ) ;
#10110 = CARTESIAN_POINT ( 'NONE',  ( 116.7951252708672456, -39.38782979237640802, 119.6147919423895019 ) ) ;
#10111 = CARTESIAN_POINT ( 'NONE',  ( 68.95691901195219486, -139.0437307363913817, 246.8274569434534840 ) ) ;
#10112 = LINE ( 'NONE', #59131, #62647 ) ;
#10113 = DIRECTION ( 'NONE',  ( 2.900000000000000265E-14, -2.000000000000000155E-15, 1.000000000000000000 ) ) ;
#10114 = DIRECTION ( 'NONE',  ( 0.000000000000000000, 1.000000000000000000, 0.000000000000000000 ) ) ;
#10115 = VECTOR ( 'NONE', #55027, 1000.000000000000000 ) ;
#10116 = DIRECTION ( 'NONE',  ( 2.900000000000000265E-14, -2.000000000000000155E-15, 1.000000000000000000 ) ) ;
#10117 = EDGE_CURVE ( 'NONE', #74315, #83594, #743, .T. ) ;
#10118 = CARTESIAN_POINT ( 'NONE',  ( 117.0718015256225328, -35.46170398102030674, 163.9272027694907194 ) ) ;
#10119 = FACE_OUTER_BOUND ( 'NONE', #66222, .T. ) ;
#10120 = AXIS2_PLACEMENT_3D ( 'NONE', #44287, #17498, #17055 ) ;
#10121 = CARTESIAN_POINT ( 'NONE',  ( 99.73113825573250324, -44.24905506706784308, 21.96133956162593748 ) ) ;
#10122 = CARTESIAN_POINT ( 'NONE',  ( 113.6855667929701923, -45.58166236755234024, 184.0994347997199725 ) ) ;
#10123 = CARTESIAN_POINT ( 'NONE',  ( 116.7650972879214919, -32.84690348374694224, 50.12991099019698282 ) ) ;
#10125 = CARTESIAN_POINT ( 'NONE',  ( 117.0718954852358706, -35.46248235588101494, 48.92729194260762426 ) ) ;
#10124 = LINE ( 'NONE', #44177, #44982 ) ;
#10126 = CARTESIAN_POINT ( 'NONE',  ( 179.4595971212889935, -28.98061976758940617, -5.074374724088000832 ) ) ;
#10127 = CIRCLE ( 'NONE', #31832, 5.041900000000001825 ) ;
#10128 = VECTOR ( 'NONE', #26483, 1000.000000000000000 ) ;
#10129 = VERTEX_POINT ( 'NONE', #63903 ) ;
#10130 = CARTESIAN_POINT ( 'NONE',  ( 97.33784133995732191, -34.07106442700378324, 187.1147919341439660 ) ) ;
#10131 = ORIENTED_EDGE ( 'NONE', *, *, #87867, .T. ) ;
#10132 = CARTESIAN_POINT ( 'NONE',  ( 106.9359508110862578, -26.91635713860572920, 56.08705384733897148 ) ) ;
#10133 = ADVANCED_FACE ( 'NONE', ( #42530 ), #765, .T. ) ;
#10135 = ORIENTED_EDGE ( 'NONE', *, *, #83445, .F. ) ;
#10134 = CARTESIAN_POINT ( 'NONE',  ( 5.207367076801767247, 94.13935037115494708, 130.4525656815699790 ) ) ;
#10136 = CARTESIAN_POINT ( 'NONE',  ( 144.0667052733537901, -75.82844715994092155, 55.21780685541800437 ) ) ;
#10137 = CARTESIAN_POINT ( 'NONE',  ( 110.6887065042382545, -47.98678726807230532, 203.8241967044819489 ) ) ;
#10138 = CARTESIAN_POINT ( 'NONE',  ( 57.56670390244732260, -48.82844715994040286, 175.7178068554150911 ) ) ;
#10139 = CARTESIAN_POINT ( 'NONE',  ( 101.9935279254791993, -45.44601432983314737, 147.1565244394456897 ) ) ;
#10140 = EDGE_CURVE ( 'NONE', #30286, #53126, #2122, .T. ) ;
#10141 = ORIENTED_EDGE ( 'NONE', *, *, #25552, .F. ) ;
#10142 = CARTESIAN_POINT ( 'NONE',  ( 34.67381068362099228, -26.00627455219321860, 342.9256252759119548 ) ) ;
#10143 = CARTESIAN_POINT ( 'NONE',  ( 99.09570906733897289, -30.55043176429327545, 46.80229194367134227 ) ) ;
#10144 = LINE ( 'NONE', #2887, #50488 ) ;
#10145 = CARTESIAN_POINT ( 'NONE',  ( 98.15093366565197641, -41.26152608243540243, 96.70072996894096207 ) ) ;
#10146 = VECTOR ( 'NONE', #86718, 1000.000000000000000 ) ;
#10147 = CARTESIAN_POINT ( 'NONE',  ( 116.4171719250473984, -30.71472603919669098, 144.2813395616259697 ) ) ;
#10148 = VERTEX_POINT ( 'NONE', #57515 ) ;
#10149 = VERTEX_POINT ( 'NONE', #43426 ) ;
#10150 = CARTESIAN_POINT ( 'NONE',  ( 99.48689454471329441, -42.28159629070200509, 103.2492023535159831 ) ) ;
#10151 = CARTESIAN_POINT ( 'NONE',  ( 25.56670390244797275, -58.35344715994099829, 293.2178068554150627 ) ) ;
#10153 = CYLINDRICAL_SURFACE ( 'NONE', #12875, 3.968750000000020872 ) ;
#10152 = CARTESIAN_POINT ( 'NONE',  ( 96.81359797424460112, -35.17473563989039320, 217.1946728949579608 ) ) ;
#10154 = CARTESIAN_POINT ( 'NONE',  ( 138.8167039024479834, -57.40094715994099772, 88.43480685541499042 ) ) ;
#10155 = FACE_OUTER_BOUND ( 'NONE', #73262, .T. ) ;
#10156 = CIRCLE ( 'NONE', #82733, 17.00000000000000000 ) ;
#10157 = CARTESIAN_POINT ( 'NONE',  ( 118.1931971052176777, 73.86197090048099767, -9.272510012970347049 ) ) ;
#10158 = CARTESIAN_POINT ( 'NONE',  ( -8.388013673212871169, 72.97744838846872995, 118.2603890449115340 ) ) ;
#10159 = CARTESIAN_POINT ( 'NONE',  ( -254.0000000000000000, 3.174999999999999822, 50.79999999999999716 ) ) ;
#10160 = DIRECTION ( 'NONE',  ( 2.108231265501709878E-16, 0.000000000000000000, -1.000000000000000000 ) ) ;
#10161 = CARTESIAN_POINT ( 'NONE',  ( 111.4081670832169237, -47.72935575799012753, 172.8756252759109771 ) ) ;
#10162 = VERTEX_POINT ( 'NONE', #1228 ) ;
#10163 = ORIENTED_EDGE ( 'NONE', *, *, #48411, .F. ) ;
#10164 = FACE_OUTER_BOUND ( 'NONE', #78384, .T. ) ;
#10165 = CARTESIAN_POINT ( 'NONE',  ( 146.3552114757505080, -68.56422815332481946, 247.0266215615655767 ) ) ;
#10166 = DIRECTION ( 'NONE',  ( 0.000000000000000000, -1.000000000000000000, 0.000000000000000000 ) ) ;
#10167 = CARTESIAN_POINT ( 'NONE',  ( 113.1780517095743477, -44.75205797978776445, 104.0939343869516449 ) ) ;
#10168 = VECTOR ( 'NONE', #2798, 1000.000000000000000 ) ;
#10169 = DIRECTION ( 'NONE',  ( -0.9068632946707808618, 0.4214249218767877059, 0.000000000000000000 ) ) ;
#10170 =( BOUNDED_CURVE ( )  B_SPLINE_CURVE ( 3, ( #82205, #88563, #13586, #19061 ),
 .UNSPECIFIED., .F., .T. ) 
 B_SPLINE_CURVE_WITH_KNOTS ( ( 4, 4 ),
 ( 1.719776299252462559, 1.732437064411955996 ),
 .UNSPECIFIED. ) 
 CURVE ( )  GEOMETRIC_REPRESENTATION_ITEM ( )  RATIONAL_B_SPLINE_CURVE ( ( 1.000000000000000000, 0.9999866421300730446, 0.9999866421300730446, 1.000000000000000000 ) ) 
 REPRESENTATION_ITEM ( '' )  );
#10171 = EDGE_CURVE ( 'NONE', #78871, #2616, #23025, .T. ) ;
#10172 = CARTESIAN_POINT ( 'NONE',  ( 102.0509295376110117, -46.57948817496540528, 172.2137205140059564 ) ) ;
#10173 = DIRECTION ( 'NONE',  ( -0.7071067811865360264, 0.000000000000000000, 0.7071067811865588970 ) ) ;
#10174 = ORIENTED_EDGE ( 'NONE', *, *, #51929, .F. ) ;
#10176 = ORIENTED_EDGE ( 'NONE', *, *, #57413, .T. ) ;
#10175 = EDGE_LOOP ( 'NONE', ( #8529, #47975, #81461, #54697 ) ) ;
#10177 = AXIS2_PLACEMENT_3D ( 'NONE', #7806, #63671, #49568 ) ;
#10178 = CARTESIAN_POINT ( 'NONE',  ( 110.3946058071659024, -46.19501636738639405, 63.84634919539954012 ) ) ;
#10179 = CARTESIAN_POINT ( 'NONE',  ( 72.26949937496598864, -71.54137415153812185, 361.9756252759101471 ) ) ;
#10180 = CARTESIAN_POINT ( 'NONE',  ( 133.1188885517861991, -34.14703303315379657, 8.087249882926339950 ) ) ;
#10181 = CARTESIAN_POINT ( 'NONE',  ( 115.8755296135227724, -35.76560983836216678, 275.3444404487542556 ) ) ;
#10182 = VECTOR ( 'NONE', #42721, 1000.000000000000000 ) ;
#10183 = DIRECTION ( 'NONE',  ( 1.514143847546114723E-15, -0.8660254037844387076, -0.4999999999999998890 ) ) ;
#10184 = EDGE_LOOP ( 'NONE', ( #70204, #48138, #57097, #54140 ) ) ;
#10185 = CARTESIAN_POINT ( 'NONE',  ( 115.0891813775823920, -41.06744293826255188, 9.635625275910941312 ) ) ;
#10186 = CARTESIAN_POINT ( 'NONE',  ( -127.0239848601435995, 53.97500000000000142, 30.16249999999999787 ) ) ;
#10187 = ORIENTED_EDGE ( 'NONE', *, *, #83020, .T. ) ;
#10189 = EDGE_LOOP ( 'NONE', ( #46755, #38718, #10091, #69521 ) ) ;
#10188 = VECTOR ( 'NONE', #47495, 999.9999999999998863 ) ;
#10190 = ADVANCED_FACE ( 'NONE', ( #57960 ), #15308, .T. ) ;
#10191 = CARTESIAN_POINT ( 'NONE',  ( 116.3347860427986120, -40.61045514847694449, 113.5106497359954290 ) ) ;
#10192 = ORIENTED_EDGE ( 'NONE', *, *, #9589, .F. ) ;
#10193 = ORIENTED_EDGE ( 'NONE', *, *, #71546, .F. ) ;
#10194 = CARTESIAN_POINT ( 'NONE',  ( 101.6694414210978294, -29.45726664942652917, 35.01908649474394508 ) ) ;
#10196 = EDGE_CURVE ( 'NONE', #61676, #81923, #62136, .T. ) ;
#10195 = TOROIDAL_SURFACE ( 'NONE', #44992, 11.75000000000000000, 2.550000000000000266 ) ;
#10197 = CARTESIAN_POINT ( 'NONE',  ( 98.24258143063333648, -42.32275744278853580, 186.7756252759109543 ) ) ;
#10198 = CARTESIAN_POINT ( 'NONE',  ( 117.0123300003821640, -30.33189756676010163, 144.2813395616249750 ) ) ;
#10199 = DIRECTION ( 'NONE',  ( 0.000000000000000000, 1.000000000000000000, 0.000000000000000000 ) ) ;
#10200 = CARTESIAN_POINT ( 'NONE',  ( 118.6539291974399219, -39.21253252500506647, 254.6584824187681022 ) ) ;
#10201 = FACE_OUTER_BOUND ( 'NONE', #35231, .T. ) ;
#10202 = CARTESIAN_POINT ( 'NONE',  ( -130.3836616406706526, 71.76234181793739708, 6.714949744938381038 ) ) ;
#10204 = ORIENTED_EDGE ( 'NONE', *, *, #72427, .T. ) ;
#10203 = EDGE_CURVE ( 'NONE', #27885, #59978, #27323, .T. ) ;
#10205 = ADVANCED_FACE ( 'NONE', ( #81119 ), #87019, .T. ) ;
#10206 = ORIENTED_EDGE ( 'NONE', *, *, #63390, .F. ) ;
#10207 = VECTOR ( 'NONE', #12229, 1000.000000000000000 ) ;
#10208 = CARTESIAN_POINT ( 'NONE',  ( 113.0474237710022578, -45.36542684395109148, 203.0584824187679374 ) ) ;
#10209 = ORIENTED_EDGE ( 'NONE', *, *, #58077, .T. ) ;
#10210 = CARTESIAN_POINT ( 'NONE',  ( 98.66574799139598895, -30.49618532553466110, 180.8184824187679567 ) ) ;
#10211 = DIRECTION ( 'NONE',  ( 1.000000000000000078E-15, 1.000000000000000083E-30, -1.000000000000000000 ) ) ;
#10212 = EDGE_CURVE ( 'NONE', #26208, #6412, #32035, .T. ) ;
#10213 = DIRECTION ( 'NONE',  ( -1.000000000000000000, -1.206764157201257538E-15, 0.000000000000000000 ) ) ;
#10214 = CARTESIAN_POINT ( 'NONE',  ( 143.7067540604739690, -140.0404100990022584, 247.0021857859347847 ) ) ;
#10217 = CARTESIAN_POINT ( 'NONE',  ( 117.4080659314678314, -35.59792815749688089, 274.9127681330538735 ) ) ;
#10216 = DIRECTION ( 'NONE',  ( -1.000000000000000000, 9.251858538542979716E-16, 0.000000000000000000 ) ) ;
#10215 = CYLINDRICAL_SURFACE ( 'NONE', #46205, 0.4999999999999994449 ) ;
#10218 = CYLINDRICAL_SURFACE ( 'NONE', #1716, 11.45913725231036118 ) ;
#10219 = DIRECTION ( 'NONE',  ( 0.000000000000000000, 0.000000000000000000, -1.000000000000000000 ) ) ;
#10220 = AXIS2_PLACEMENT_3D ( 'NONE', #5939, #20009, #26806 ) ;
#10221 = CARTESIAN_POINT ( 'NONE',  ( 149.4532656544376721, -72.54365454176046057, 361.9756252759100335 ) ) ;
#10222 = DIRECTION ( 'NONE',  ( 0.000000000000000000, 0.000000000000000000, -1.000000000000000000 ) ) ;
#10223 = LINE ( 'NONE', #39262, #35801 ) ;
#10224 = EDGE_CURVE ( 'NONE', #19595, #26178, #10266, .T. ) ;
#10225 = CARTESIAN_POINT ( 'NONE',  ( 72.96458098368701428, 101.5999999999999943, -72.96458098368670164 ) ) ;
#10227 = EDGE_LOOP ( 'NONE', ( #53256, #34294 ) ) ;
#10226 = CARTESIAN_POINT ( 'NONE',  ( 101.4389981506307237, -42.56717821295191584, 195.5838068554170377 ) ) ;
#10228 = CARTESIAN_POINT ( 'NONE',  ( 90.44969454456408187, -20.11243780205710507, 239.5838068554175209 ) ) ;
#10229 = CARTESIAN_POINT ( 'NONE',  ( 108.1841437630847338, -47.11680481413669952, 202.6613395616249704 ) ) ;
#10230 = CARTESIAN_POINT ( 'NONE',  ( 96.65662162753720565, -37.29271227441797265, 72.36991099019596163 ) ) ;
#10231 = CARTESIAN_POINT ( 'NONE',  ( 100.6295653500825154, -44.98529764103543727, 228.0499109901969348 ) ) ;
#10232 = CARTESIAN_POINT ( 'NONE',  ( -492.0614999999999668, 93.66249999999999432, 11.11250000000040217 ) ) ;
#10233 = LINE ( 'NONE', #37938, #1101 ) ;
#10234 = AXIS2_PLACEMENT_3D ( 'NONE', #52574, #4911, #18988 ) ;
#10236 = PLANE ( 'NONE',  #42665 ) ;
#10235 = PLANE ( 'NONE',  #18870 ) ;
#10237 = DIRECTION ( 'NONE',  ( 4.299999999999999979E-14, -1.000000000000000000, 0.000000000000000000 ) ) ;
#10238 = CARTESIAN_POINT ( 'NONE',  ( 107.0667039024479834, -48.82844715994099971, 160.9178068554150229 ) ) ;
#10239 = LINE ( 'NONE', #72906, #77620 ) ;
#10240 = VERTEX_POINT ( 'NONE', #31146 ) ;
#10241 = EDGE_LOOP ( 'NONE', ( #29274, #17213, #47247, #38005 ) ) ;
#10242 = CARTESIAN_POINT ( 'NONE',  ( 108.2720842404240926, -28.27352272357859420, 104.3867055423629608 ) ) ;
#10243 = EDGE_CURVE ( 'NONE', #2816, #67094, #73826, .T. ) ;
#10245 = ORIENTED_EDGE ( 'NONE', *, *, #6455, .T. ) ;
#10244 = LINE ( 'NONE', #4327, #77795 ) ;
#10246 = CARTESIAN_POINT ( 'NONE',  ( 116.9011659702703270, -33.23038410113878882, 110.0984824187679578 ) ) ;
#10247 = FACE_OUTER_BOUND ( 'NONE', #22024, .T. ) ;
#10248 = EDGE_CURVE ( 'NONE', #43365, #83807, #31587, .T. ) ;
#10249 = EDGE_CURVE ( 'NONE', #59883, #72947, #19877, .T. ) ;
#10251 = CARTESIAN_POINT ( 'NONE',  ( 77.71552635664387765, -17.29868341350664451, 7.242354772871751223 ) ) ;
#10250 = AXIS2_PLACEMENT_3D ( 'NONE', #58593, #2321, #37277 ) ;
#10252 = CARTESIAN_POINT ( 'NONE',  ( 99.09570909151958062, -30.55043173361417175, 176.8022919406010374 ) ) ;
#10253 = EDGE_CURVE ( 'NONE', #64446, #83766, #52015, .T. ) ;
#10254 = CARTESIAN_POINT ( 'NONE',  ( 107.1874307469290386, -26.94942635195914349, 35.06705384733993469 ) ) ;
#10255 = VERTEX_POINT ( 'NONE', #59731 ) ;
#10256 = ORIENTED_EDGE ( 'NONE', *, *, #69689, .F. ) ;
#10258 = ORIENTED_EDGE ( 'NONE', *, *, #55698, .T. ) ;
#10257 = AXIS2_PLACEMENT_3D ( 'NONE', #35005, #496, #89544 ) ;
#10259 = LINE ( 'NONE', #32027, #31192 ) ;
#10260 = LINE ( 'NONE', #23466, #18631 ) ;
#10261 = CARTESIAN_POINT ( 'NONE',  ( 116.3167039024470029, -68.87844715994093292, 55.21780685541800437 ) ) ;
#10262 = FACE_OUTER_BOUND ( 'NONE', #35085, .T. ) ;
#10263 = LINE ( 'NONE', #37963, #52280 ) ;
#10264 = CARTESIAN_POINT ( 'NONE',  ( 112.1400935167290100, -28.01325122303620319, 50.65751264254551955 ) ) ;
#10265 = CIRCLE ( 'NONE', #43574, 4.762499999999999289 ) ;
#10266 = LINE ( 'NONE', #3008, #23011 ) ;
#10267 = CARTESIAN_POINT ( 'NONE',  ( -4.054936310288488777, 94.61721499974834160, 130.4955353351740257 ) ) ;
#10268 = CARTESIAN_POINT ( 'NONE',  ( 97.79189512308828114, -32.01662636557816199, 50.95276813305294183 ) ) ;
#10269 = ORIENTED_EDGE ( 'NONE', *, *, #47623, .F. ) ;
#10270 = VERTEX_POINT ( 'NONE', #46093 ) ;
#10271 = DIRECTION ( 'NONE',  ( 1.000000000000000078E-15, -1.000000000000000083E-30, -1.000000000000000000 ) ) ;
#10272 = CARTESIAN_POINT ( 'NONE',  ( 126.6266614082200732, 45.94094662677520802, 31.78937376590539898 ) ) ;
#10273 = DIRECTION ( 'NONE',  ( -0.04216478779797398074, 0.9991106698809455455, 0.000000000000000000 ) ) ;
#10274 = CARTESIAN_POINT ( 'NONE',  ( 98.42339386660059120, -37.17434067858062008, 119.1976141791149786 ) ) ;
#10275 = CARTESIAN_POINT ( 'NONE',  ( 104.4870417173576556, -26.97960265801549795, 95.28170196733614716 ) ) ;
#10276 = AXIS2_PLACEMENT_3D ( 'NONE', #30965, #64160, #30080 ) ;
#10277 = CARTESIAN_POINT ( 'NONE',  ( 121.2221484686747459, -113.6057974291316839, -19.26696060647573105 ) ) ;
#10278 = VERTEX_POINT ( 'NONE', #17960 ) ;
#10279 = ORIENTED_EDGE ( 'NONE', *, *, #62430, .T. ) ;
#10280 = CARTESIAN_POINT ( 'NONE',  ( -75.61066417432020614, 0.000000000000000000, 189.7379999999999995 ) ) ;
#10281 = ORIENTED_EDGE ( 'NONE', *, *, #15477, .F. ) ;
#10282 = ORIENTED_EDGE ( 'NONE', *, *, #76853, .T. ) ;
#10283 = CIRCLE ( 'NONE', #61042, 161.5439999999999827 ) ;
#10284 = CARTESIAN_POINT ( 'NONE',  ( 112.6324721509601545, -29.83393797428842831, 160.9672975916109579 ) ) ;
#10285 = CARTESIAN_POINT ( 'NONE',  ( 172.5667039024478413, -36.32844715993500273, 249.9678068554149775 ) ) ;
#10286 = CIRCLE ( 'NONE', #78531, 7.143750000000004263 ) ;
#10287 = CARTESIAN_POINT ( 'NONE',  ( 100.8735899011331014, -45.91031909761725416, 148.0918157521009562 ) ) ;
#10288 = CARTESIAN_POINT ( 'NONE',  ( 113.2454987219876728, -28.75867296460453559, 119.5522919401142445 ) ) ;
#10289 = CARTESIAN_POINT ( 'NONE',  ( 85.06670390244700286, -71.37844715994096134, 55.21780685541800437 ) ) ;
#10290 = ORIENTED_EDGE ( 'NONE', *, *, #57784, .T. ) ;
#10291 = VECTOR ( 'NONE', #47250, 1000.000000000000000 ) ;
#10292 = EDGE_CURVE ( 'NONE', #64140, #37193, #87463, .T. ) ;
#10293 = EDGE_LOOP ( 'NONE', ( #78266, #51391, #72287, #47534 ) ) ;
#10294 = ORIENTED_EDGE ( 'NONE', *, *, #67526, .T. ) ;
#10295 = ADVANCED_FACE ( 'NONE', ( #37966 ), #46548, .T. ) ;
#10296 = CARTESIAN_POINT ( 'NONE',  ( 100.3991921706488171, -43.18259834960616672, 189.7566617981629804 ) ) ;
#10297 = EDGE_CURVE ( 'NONE', #26172, #43699, #31462, .T. ) ;
#10298 = CARTESIAN_POINT ( 'NONE',  ( 112.7719768816358936, -27.93537496831996592, 69.61848241876793963 ) ) ;
#10299 = EDGE_LOOP ( 'NONE', ( #70905, #1160, #4174, #80190 ) ) ;
#10300 = CARTESIAN_POINT ( 'NONE',  ( 115.5559444348971851, -42.74257571503951425, 53.33562527591095659 ) ) ;
#10301 = CARTESIAN_POINT ( 'NONE',  ( 97.81085527707094229, -40.51777768585955641, 251.6359959587111064 ) ) ;
#10302 = CARTESIAN_POINT ( 'NONE',  ( 144.0637245237351749, -140.6784087391956746, 245.5331728883010101 ) ) ;
#10303 = LINE ( 'NONE', #24388, #14151 ) ;
#10304 = CARTESIAN_POINT ( 'NONE',  ( 98.28086921530724851, -31.05189054518432101, 141.8699109901969564 ) ) ;
#10305 = LINE ( 'NONE', #66598, #78501 ) ;
#10306 = ORIENTED_EDGE ( 'NONE', *, *, #15906, .T. ) ;
#10307 = DIRECTION ( 'NONE',  ( 1.000000000000000078E-15, -1.000000000000000083E-30, -1.000000000000000000 ) ) ;
#10308 = EDGE_CURVE ( 'NONE', #56609, #53213, #65232, .T. ) ;
#10309 = CIRCLE ( 'NONE', #52349, 4.500000000000003553 ) ;
#10310 = ADVANCED_FACE ( 'NONE', ( #66557 ), #87909, .F. ) ;
#10311 = ORIENTED_EDGE ( 'NONE', *, *, #9236, .F. ) ;
#10312 = DIRECTION ( 'NONE',  ( -1.000000000000000078E-15, 1.000000000000000083E-30, 1.000000000000000000 ) ) ;
#10313 = CYLINDRICAL_SURFACE ( 'NONE', #14047, 3.174999999999983391 ) ;
#10314 = ORIENTED_EDGE ( 'NONE', *, *, #6781, .F. ) ;
#10315 = AXIS2_PLACEMENT_3D ( 'NONE', #85327, #15379, #1746 ) ;
#10316 = EDGE_CURVE ( 'NONE', #74086, #65069, #17086, .T. ) ;
#10317 = DIRECTION ( 'NONE',  ( -4.237773401492740281E-14, 1.000000000000000000, 0.000000000000000000 ) ) ;
#10318 = CARTESIAN_POINT ( 'NONE',  ( 97.81170212845945855, -40.51743756719207568, 176.6354241348688277 ) ) ;
#10319 = CARTESIAN_POINT ( 'NONE',  ( 112.8178475080015772, -27.29012000701139939, 49.62895860924498947 ) ) ;
#10320 = PLANE ( 'NONE',  #59071 ) ;
#10321 = ADVANCED_FACE ( 'NONE', ( #25223 ), #58404, .F. ) ;
#10322 = DIRECTION ( 'NONE',  ( 0.000000000000000000, -1.000000000000000000, 0.000000000000000000 ) ) ;
#10323 = DIRECTION ( 'NONE',  ( -0.9254794337955620787, -0.3787978585227822492, 0.000000000000000000 ) ) ;
#10324 = CARTESIAN_POINT ( 'NONE',  ( 116.7176835877704946, -38.50936494796418685, 88.68133956162593279 ) ) ;
#10326 = CARTESIAN_POINT ( 'NONE',  ( 109.4403364888816981, -25.95778788316477304, 175.8918157521009391 ) ) ;
#10325 = DIRECTION ( 'NONE',  ( -1.000000000000000000, 0.000000000000000000, 0.000000000000000000 ) ) ;
#10327 = DIRECTION ( 'NONE',  ( 0.000000000000000000, 0.000000000000000000, 1.000000000000000000 ) ) ;
#10328 = CARTESIAN_POINT ( 'NONE',  ( 55.11501535284990183, 20.32000000000000028, 183.9403141659174992 ) ) ;
#10329 = ORIENTED_EDGE ( 'NONE', *, *, #51143, .T. ) ;
#10330 = AXIS2_PLACEMENT_3D ( 'NONE', #33971, #4938, #25831 ) ;
#10331 = LINE ( 'NONE', #9888, #65740 ) ;
#10332 = DIRECTION ( 'NONE',  ( -0.000000000000000000, -0.000000000000000000, -1.000000000000000000 ) ) ;
#10333 = CARTESIAN_POINT ( 'NONE',  ( 108.4192877796676555, -26.73525438302016966, 134.9688338521367257 ) ) ;
#10334 = CIRCLE ( 'NONE', #63965, 4.750000000000004441 ) ;
#10335 = ADVANCED_FACE ( 'NONE', ( #86134 ), #23909, .F. ) ;
#10336 = CARTESIAN_POINT ( 'NONE',  ( 162.7131505118679797, -31.94127993907790852, -5.074374724088000832 ) ) ;
#10338 = ORIENTED_EDGE ( 'NONE', *, *, #15746, .T. ) ;
#10337 = CARTESIAN_POINT ( 'NONE',  ( 115.5532354207493171, -29.57487366316678745, 224.3718157521009573 ) ) ;
#10339 = FACE_OUTER_BOUND ( 'NONE', #88951, .T. ) ;
#10340 = CARTESIAN_POINT ( 'NONE',  ( 104.3186933571878399, -25.99935600364358024, 241.2880062282919482 ) ) ;
#10341 = CARTESIAN_POINT ( 'NONE',  ( 114.1102230946791707, -44.52199131239810015, 129.1613395616249704 ) ) ;
#10342 = DIRECTION ( 'NONE',  ( -0.8660254037844382635, -0.5000000000000008882, 1.550000000000000022E-14 ) ) ;
#10343 = CARTESIAN_POINT ( 'NONE',  ( 80.44329752325863581, -39.47944369577015067, 8.225625303283912615 ) ) ;
#10344 = DIRECTION ( 'NONE',  ( 0.000000000000000000, 0.000000000000000000, -1.000000000000000000 ) ) ;
#10345 = FACE_OUTER_BOUND ( 'NONE', #86076, .T. ) ;
#10346 = ORIENTED_EDGE ( 'NONE', *, *, #15764, .F. ) ;
#10347 = ORIENTED_EDGE ( 'NONE', *, *, #80633, .T. ) ;
#10348 = EDGE_LOOP ( 'NONE', ( #5840, #60301, #8959, #32910, #3193 ) ) ;
#10349 = VECTOR ( 'NONE', #13155, 1000.000000000000000 ) ;
#10350 = VERTEX_POINT ( 'NONE', #3451 ) ;
#10351 = CARTESIAN_POINT ( 'NONE',  ( 47.62500000000000000, 94.53880000000000905, 250.8250000000000171 ) ) ;
#10352 = CARTESIAN_POINT ( 'NONE',  ( 117.4297252914212066, -35.59555830959087075, 274.9127681330538735 ) ) ;
#10353 = DIRECTION ( 'NONE',  ( 1.000000000000000000, 1.000000000000000078E-15, 0.000000000000000000 ) ) ;
#10354 = LINE ( 'NONE', #65320, #77448 ) ;
#10355 = EDGE_CURVE ( 'NONE', #82750, #78071, #72927, .T. ) ;
#10358 = ADVANCED_FACE ( 'NONE', ( #3892 ), #68807, .T. ) ;
#10357 = CARTESIAN_POINT ( 'NONE',  ( 74.43211355457049194, 80.89685143461890959, 92.27899210470947367 ) ) ;
#10356 = DIRECTION ( 'NONE',  ( 2.108231265501709878E-16, 0.000000000000000000, -1.000000000000000000 ) ) ;
#10359 = CYLINDRICAL_SURFACE ( 'NONE', #80574, 0.5000000000000104361 ) ;
#10360 = VECTOR ( 'NONE', #31878, 1000.000000000000000 ) ;
#10361 = CARTESIAN_POINT ( 'NONE',  ( 99.94932728663779642, -31.12955780999732980, 200.2305150661719892 ) ) ;
#10362 = ORIENTED_EDGE ( 'NONE', *, *, #51847, .F. ) ;
#10363 = EDGE_LOOP ( 'NONE', ( #46261, #11269 ) ) ;
#10364 = ORIENTED_EDGE ( 'NONE', *, *, #27657, .T. ) ;
#10365 = AXIS2_PLACEMENT_3D ( 'NONE', #79811, #59330, #58439 ) ;
#10366 = PLANE ( 'NONE',  #67370 ) ;
#10367 = CARTESIAN_POINT ( 'NONE',  ( -72.96458098368600531, 127.0000000000000000, -72.96458098368781009 ) ) ;
#10368 = DIRECTION ( 'NONE',  ( 0.000000000000000000, 0.000000000000000000, 1.000000000000000000 ) ) ;
#10369 = CARTESIAN_POINT ( 'NONE',  ( 115.9938408324894539, -42.00591253359444011, 279.4137205140056608 ) ) ;
#10370 = CARTESIAN_POINT ( 'NONE',  ( 99.08946256649485917, -109.4614598618336174, 2.217806855418169576 ) ) ;
#10371 = CARTESIAN_POINT ( 'NONE',  ( -27.27158787008326968, 127.0000000000000000, 101.0189074266571794 ) ) ;
#10372 = CARTESIAN_POINT ( 'NONE',  ( 115.7824607000603123, -41.80340193948442362, 28.40635853151320589 ) ) ;
#10374 = ORIENTED_EDGE ( 'NONE', *, *, #33623, .F. ) ;
#10373 = AXIS2_PLACEMENT_3D ( 'NONE', #76964, #41969, #35160 ) ;
#10375 = CARTESIAN_POINT ( 'NONE',  ( 37.56670390244828184, -48.82844715994119866, 300.4678068554150059 ) ) ;
#10376 = ORIENTED_EDGE ( 'NONE', *, *, #3237, .T. ) ;
#10377 = CARTESIAN_POINT ( 'NONE',  ( 36.23715912545344509, -47.82818131006131779, 117.4678068554150485 ) ) ;
#10378 = CARTESIAN_POINT ( 'NONE',  ( 115.7905465638341553, -39.88961339014866070, 21.36809036959191843 ) ) ;
#10379 = VECTOR ( 'NONE', #76132, 1000.000000000000000 ) ;
#10380 = CARTESIAN_POINT ( 'NONE',  ( 90.44969454456415292, -53.34645651782494724, 229.5838068554169809 ) ) ;
#10381 = CARTESIAN_POINT ( 'NONE',  ( 97.95250717983367394, -32.49412669507730556, 0.4256252759109618311 ) ) ;
#10382 = VECTOR ( 'NONE', #30205, 1000.000000000000114 ) ;
#10383 = DIRECTION ( 'NONE',  ( 4.299999999999999979E-14, -1.000000000000000000, 4.400000000000000367E-29 ) ) ;
#10384 = EDGE_LOOP ( 'NONE', ( #66042, #43587, #23502, #24758 ) ) ;
#10385 = DIRECTION ( 'NONE',  ( 0.000000000000000000, 1.000000000000000000, 0.000000000000000000 ) ) ;
#10386 = CARTESIAN_POINT ( 'NONE',  ( 168.0371591254545365, -48.62818131005519007, 193.9678068554149775 ) ) ;
#10387 = VERTEX_POINT ( 'NONE', #6143 ) ;
#10388 = CARTESIAN_POINT ( 'NONE',  ( 117.3714642245996629, -32.73114059124436892, 94.10895860924395606 ) ) ;
#10389 = VERTEX_POINT ( 'NONE', #12956 ) ;
#10391 = CIRCLE ( 'NONE', #88729, 1.000000000000000888 ) ;
#10390 = CARTESIAN_POINT ( 'NONE',  ( 114.9961339231967798, -33.55505389859023069, 53.55241982807695678 ) ) ;
#10392 = CARTESIAN_POINT ( 'NONE',  ( 116.0020177893944435, -41.25514887265125452, 89.45255704496776161 ) ) ;
#10393 = CARTESIAN_POINT ( 'NONE',  ( 97.73412737207827661, -37.81740788287748956, 82.86253568684892912 ) ) ;
#10394 = CYLINDRICAL_SURFACE ( 'NONE', #37512, 7.143750000000004263 ) ;
#10395 = CARTESIAN_POINT ( 'NONE',  ( 183.5150000000000148, 37.33800000000000097, 50.79999999999999716 ) ) ;
#10396 = DIRECTION ( 'NONE',  ( 0.000000000000000000, 0.000000000000000000, -1.000000000000000000 ) ) ;
#10397 = EDGE_CURVE ( 'NONE', #66460, #80913, #70723, .T. ) ;
#10398 = CARTESIAN_POINT ( 'NONE',  ( 111.3320466151124322, -27.19308368994588676, 20.74133956162494030 ) ) ;
#10399 = LINE ( 'NONE', #37666, #46665 ) ;
#10400 = ORIENTED_EDGE ( 'NONE', *, *, #67614, .F. ) ;
#10401 = CARTESIAN_POINT ( 'NONE',  ( 194.0371591254582881, -46.82818131005408446, 237.4678068554150059 ) ) ;
#10402 = EDGE_LOOP ( 'NONE', ( #42548, #72070 ) ) ;
#10403 = CARTESIAN_POINT ( 'NONE',  ( 78.42773927738237205, -20.94013506381011425, 2.060080721656760705 ) ) ;
#10404 = ORIENTED_EDGE ( 'NONE', *, *, #12172, .T. ) ;
#10406 = EDGE_CURVE ( 'NONE', #82390, #19111, #26568, .T. ) ;
#10405 = ORIENTED_EDGE ( 'NONE', *, *, #57344, .T. ) ;
#10407 = EDGE_CURVE ( 'NONE', #15778, #58010, #70657, .T. ) ;
#10408 = AXIS2_PLACEMENT_3D ( 'NONE', #36825, #70910, #72242 ) ;
#10409 = FACE_OUTER_BOUND ( 'NONE', #86279, .T. ) ;
#10410 = ADVANCED_FACE ( 'NONE', ( #6576 ), #88815, .T. ) ;
#10411 = CARTESIAN_POINT ( 'NONE',  ( 101.7025241355416796, -45.60450926735023813, 202.1318157521019430 ) ) ;
#10412 = CARTESIAN_POINT ( 'NONE',  ( 104.8368789347731536, -26.95710669931445125, 125.2537966132911436 ) ) ;
#10413 = CARTESIAN_POINT ( 'NONE',  ( 131.8286686973700910, -67.87844715994091871, 245.6137563491429887 ) ) ;
#10414 = CARTESIAN_POINT ( 'NONE',  ( 96.33847535375279847, -41.76377544194641445, 57.67562527591096710 ) ) ;
#10415 = LINE ( 'NONE', #51726, #33404 ) ;
#10416 = ORIENTED_EDGE ( 'NONE', *, *, #81289, .T. ) ;
#10417 = CARTESIAN_POINT ( 'NONE',  ( 103.3097373732736912, -27.46191326970934909, 171.3829422610906761 ) ) ;
#10418 = ADVANCED_FACE ( 'NONE', ( #34726 ), #41085, .T. ) ;
#10419 = LINE ( 'NONE', #3601, #62209 ) ;
#10420 = ORIENTED_EDGE ( 'NONE', *, *, #63881, .T. ) ;
#10421 = EDGE_CURVE ( 'NONE', #19365, #53353, #13396, .T. ) ;
#10422 = AXIS2_PLACEMENT_3D ( 'NONE', #76560, #50175, #64719 ) ;
#10423 = LINE ( 'NONE', #4946, #18434 ) ;
#10424 = CARTESIAN_POINT ( 'NONE',  ( 188.5667039024479834, -67.87844715994100397, 257.2178068554150059 ) ) ;
#10425 = CARTESIAN_POINT ( 'NONE',  ( 107.2488531970940073, -24.90511003128400347, 230.0641967044819580 ) ) ;
#10426 = DIRECTION ( 'NONE',  ( 0.7071067811868693154, 0.7071067811862258301, -2.899137802863410076E-29 ) ) ;
#10427 = FACE_BOUND ( 'NONE', #14936, .T. ) ;
#10428 = CARTESIAN_POINT ( 'NONE',  ( 77.31648329127401098, -36.72944715994107412, 3.101481641215480867 ) ) ;
#10429 = EDGE_CURVE ( 'NONE', #43983, #18666, #20660, .T. ) ;
#10430 = CARTESIAN_POINT ( 'NONE',  ( 101.8914336387190502, -44.16123909860101548, 236.5028960185529456 ) ) ;
#10432 = CARTESIAN_POINT ( 'NONE',  ( 107.3204973292724134, -25.70223992296343241, 71.04610146638795243 ) ) ;
#10431 = CARTESIAN_POINT ( 'NONE',  ( 151.0371591254585155, -46.82818131005592477, 129.9678068554149775 ) ) ;
#10433 = CARTESIAN_POINT ( 'NONE',  ( 109.6451729131657657, 58.77969955619902720, 70.87177885828612034 ) ) ;
#10434 = CARTESIAN_POINT ( 'NONE',  ( 104.9539341177782177, -25.01766106605714768, 125.2184824187689856 ) ) ;
#10435 = ORIENTED_EDGE ( 'NONE', *, *, #61910, .F. ) ;
#10436 = CARTESIAN_POINT ( 'NONE',  ( 132.9232751754135222, -21.23064218986711893, 8.021355262920867091 ) ) ;
#10437 = VERTEX_POINT ( 'NONE', #83335 ) ;
#10438 = DIRECTION ( 'NONE',  ( 1.000000000000000000, 4.299999999999999979E-14, 1.000000000000000078E-15 ) ) ;
#10439 = CARTESIAN_POINT ( 'NONE',  ( 172.5664832912740110, 0.2215528400590013880, 196.8086252759119645 ) ) ;
#10440 = DIRECTION ( 'NONE',  ( 0.000000000000000000, 0.000000000000000000, 1.000000000000000000 ) ) ;
#10441 = ORIENTED_EDGE ( 'NONE', *, *, #73968, .T. ) ;
#10443 = EDGE_CURVE ( 'NONE', #62569, #85065, #88103, .T. ) ;
#10442 = CIRCLE ( 'NONE', #61197, 2.030000000000003801 ) ;
#10444 = CARTESIAN_POINT ( 'NONE',  ( 1.475953350320055108E-14, 223.9999999999999716, 90.07542076772557493 ) ) ;
#10446 = ORIENTED_EDGE ( 'NONE', *, *, #22282, .F. ) ;
#10445 = CARTESIAN_POINT ( 'NONE',  ( 114.0516219551475245, -28.93108169718528444, 114.4956252759109816 ) ) ;
#10447 = CARTESIAN_POINT ( 'NONE',  ( 168.0371591254543091, -48.62818131005519717, 313.9678068554149490 ) ) ;
#10448 = LINE ( 'NONE', #15934, #86778 ) ;
#10449 = AXIS2_PLACEMENT_3D ( 'NONE', #34682, #41486, #29669 ) ;
#10450 = CARTESIAN_POINT ( 'NONE',  ( 131.3179999999999836, 34.75001145038169881, 58.30374716505330213 ) ) ;
#10451 = ORIENTED_EDGE ( 'NONE', *, *, #48121, .T. ) ;
#10452 = VECTOR ( 'NONE', #26713, 1000.000000000000000 ) ;
#10453 = CARTESIAN_POINT ( 'NONE',  ( 97.91311022844104173, -31.62022761154550210, 110.9213395616259703 ) ) ;
#10454 = CARTESIAN_POINT ( 'NONE',  ( 170.2205283966864897, 20.32000000000000028, 71.37400000000000944 ) ) ;
#10455 = DIRECTION ( 'NONE',  ( -0.000000000000000000, 1.000000000000000000, -0.000000000000000000 ) ) ;
#10456 = CARTESIAN_POINT ( 'NONE',  ( -2.077912807000512618, 95.08573034283286063, 130.5400978111108259 ) ) ;
#10457 = DIRECTION ( 'NONE',  ( 0.000000000000000000, -1.000000000000000000, 0.000000000000000000 ) ) ;
#10458 = VERTEX_POINT ( 'NONE', #67905 ) ;
#10459 = AXIS2_PLACEMENT_3D ( 'NONE', #24077, #88089, #51299 ) ;
#10460 = EDGE_LOOP ( 'NONE', ( #15861, #83793, #36202, #61115 ) ) ;
#10461 = DIRECTION ( 'NONE',  ( 0.000000000000000000, 0.000000000000000000, -1.000000000000000000 ) ) ;
#10462 = CARTESIAN_POINT ( 'NONE',  ( 115.0439452383991892, -99.09543445804915507, 2.217806855417836509 ) ) ;
#10463 = AXIS2_PLACEMENT_3D ( 'NONE', #54197, #40597, #32884 ) ;
#10464 = DIRECTION ( 'NONE',  ( 0.000000000000000000, 1.000000000000000000, 0.000000000000000000 ) ) ;
#10465 = VECTOR ( 'NONE', #79350, 1000.000000000000000 ) ;
#10468 = EDGE_CURVE ( 'NONE', #29480, #89346, #9764, .T. ) ;
#10467 = DIRECTION ( 'NONE',  ( 0.000000000000000000, -1.000000000000000000, 0.000000000000000000 ) ) ;
#10466 = CARTESIAN_POINT ( 'NONE',  ( 116.9517947088517218, -38.63056867187965793, 249.6760957642232484 ) ) ;
#10469 = CARTESIAN_POINT ( 'NONE',  ( 134.0664832912740110, 0.2215528400590013880, 7.443125275912000127 ) ) ;
#10470 = ORIENTED_EDGE ( 'NONE', *, *, #36676, .T. ) ;
#10471 = CARTESIAN_POINT ( 'NONE',  ( 116.7951252848263692, -39.38782973560361000, 34.61479194698554096 ) ) ;
#10472 = CARTESIAN_POINT ( 'NONE',  ( 96.28008679191522390, -39.42493101749851547, 162.5213395616249841 ) ) ;
#10474 = ORIENTED_EDGE ( 'NONE', *, *, #62910, .T. ) ;
#10473 = DIRECTION ( 'NONE',  ( 0.7071067811987160612, 0.7071067811743789733, 0.000000000000000000 ) ) ;
#10475 = CARTESIAN_POINT ( 'NONE',  ( 106.5519926023875712, -26.37212682281792198, 41.12800622829093555 ) ) ;
#10476 = CARTESIAN_POINT ( 'NONE',  ( 97.92339011489026745, -40.78105927379723283, 51.65841521686554927 ) ) ;
#10477 = DIRECTION ( 'NONE',  ( 1.000000000000000078E-15, -1.000000000000000083E-30, -1.000000000000000000 ) ) ;
#10478 = EDGE_LOOP ( 'NONE', ( #9551, #35108, #63456, #33435 ) ) ;
#10479 = EDGE_CURVE ( 'NONE', #8418, #87481, #12689, .T. ) ;
#10480 = CARTESIAN_POINT ( 'NONE',  ( 83.06670390244796920, -67.87844715994100397, 237.1838068554150141 ) ) ;
#10481 = VERTEX_POINT ( 'NONE', #19314 ) ;
#10482 = AXIS2_PLACEMENT_3D ( 'NONE', #20738, #41161, #13039 ) ;
#10483 = ORIENTED_EDGE ( 'NONE', *, *, #38941, .F. ) ;
#10484 = CARTESIAN_POINT ( 'NONE',  ( 106.5710281304903901, -26.66837221057895846, 191.5472975916109704 ) ) ;
#10485 = CIRCLE ( 'NONE', #38053, 13.49999999999999822 ) ;
#10486 = EDGE_CURVE ( 'NONE', #68920, #69055, #40211, .T. ) ;
#10487 = LINE ( 'NONE', #38187, #86467 ) ;
#10488 = CARTESIAN_POINT ( 'NONE',  ( -100.8594679592212344, 82.54999999999999716, 82.89895571708261457 ) ) ;
#10489 = CARTESIAN_POINT ( 'NONE',  ( 72.96458098368701428, 127.0000000000000000, -72.96458098368670164 ) ) ;
#10490 = CARTESIAN_POINT ( 'NONE',  ( 107.0664832912739399, -36.72944715994096754, 296.5517437918485939 ) ) ;
#10491 = ORIENTED_EDGE ( 'NONE', *, *, #61889, .T. ) ;
#10492 = DIRECTION ( 'NONE',  ( -0.4999999999999985567, -0.8660254037844395958, 2.602085213965200860E-14 ) ) ;
#10493 = CARTESIAN_POINT ( 'NONE',  ( 184.3595971212623112, -48.62134037874549364, 300.4678068554149490 ) ) ;
#10494 = EDGE_LOOP ( 'NONE', ( #50510, #34195, #31839, #72704, #2096 ) ) ;
#10495 = CARTESIAN_POINT ( 'NONE',  ( 116.9047011640240754, -41.71676023082953577, 248.4651490854349731 ) ) ;
#10496 = CARTESIAN_POINT ( 'NONE',  ( 8.684762001849648527, 91.82556179790852013, 118.2378372707471641 ) ) ;
#10497 = ORIENTED_EDGE ( 'NONE', *, *, #85801, .F. ) ;
#10498 = AXIS2_PLACEMENT_3D ( 'NONE', #13512, #41198, #68922 ) ;
#10499 = DIRECTION ( 'NONE',  ( 1.000000000000000000, 4.163336342344333240E-14, 0.000000000000000000 ) ) ;
#10500 = CARTESIAN_POINT ( 'NONE',  ( 63.03715912545732181, -24.89890238295017966, 300.4678068554150627 ) ) ;
#10501 = CYLINDRICAL_SURFACE ( 'NONE', #65024, 2.117000000000007987 ) ;
#10502 = DIRECTION ( 'NONE',  ( 1.000000000000000000, 0.000000000000000000, 0.000000000000000000 ) ) ;
#10503 = CARTESIAN_POINT ( 'NONE',  ( 116.3890555338844450, -44.12544333927958462, 194.2927681330539542 ) ) ;
#10504 = DIRECTION ( 'NONE',  ( 0.000000000000000000, 0.000000000000000000, -1.000000000000000000 ) ) ;
#10505 = EDGE_LOOP ( 'NONE', ( #77700, #79668, #86686, #34967 ) ) ;
#10506 = VECTOR ( 'NONE', #81501, 1000.000000000000000 ) ;
#10507 = CARTESIAN_POINT ( 'NONE',  ( 112.2026027939200361, -27.56657145192123082, 30.66991099019694644 ) ) ;
#10508 = CARTESIAN_POINT ( 'NONE',  ( 52.38749999999999574, 94.53880000000000905, 221.4562499999999829 ) ) ;
#10509 = CARTESIAN_POINT ( 'NONE',  ( 115.6954802162012044, -42.57986958318428350, 273.3527681330537575 ) ) ;
#10510 = EDGE_CURVE ( 'NONE', #67090, #35473, #12053, .T. ) ;
#10512 = ORIENTED_EDGE ( 'NONE', *, *, #14902, .T. ) ;
#10511 = EDGE_CURVE ( 'NONE', #20321, #73048, #39741, .T. ) ;
#10513 = EDGE_CURVE ( 'NONE', #54496, #72895, #57604, .T. ) ;
#10514 = CARTESIAN_POINT ( 'NONE',  ( 80.81118397279384169, -16.08035908359608612, 1.709393751552206631 ) ) ;
#10515 = CARTESIAN_POINT ( 'NONE',  ( 113.1794018818664398, -44.75104475741103016, 19.09459687979077458 ) ) ;
#10516 = DIRECTION ( 'NONE',  ( 1.387778780781444492E-15, 0.000000000000000000, -1.000000000000000000 ) ) ;
#10517 = CARTESIAN_POINT ( 'NONE',  ( 112.5126453671185942, -30.64922967528412556, 112.3138046553059723 ) ) ;
#10518 = CARTESIAN_POINT ( 'NONE',  ( 100.6242249862060731, -26.75349815150567778, 216.5327681330539633 ) ) ;
#10519 = CARTESIAN_POINT ( 'NONE',  ( -254.0000000000000000, 14.28749999999982201, 90.48749999999999716 ) ) ;
#10520 = ORIENTED_EDGE ( 'NONE', *, *, #31918, .F. ) ;
#10521 = EDGE_CURVE ( 'NONE', #31120, #29962, #19762, .T. ) ;
#10522 = CARTESIAN_POINT ( 'NONE',  ( 136.6090958654756662, -37.77717416134755268, 2.822018739141234800 ) ) ;
#10523 = B_SPLINE_CURVE_WITH_KNOTS ( 'NONE', 3,
 ( #22587, #49814, #56172, #37102, #9844, #64805, #30284, #57979, #22149, #36203, #57533, #23489, #63917, #1693, #37549, #84819, #64361, #71186, #14880, #77999, #51156, #42992, #70733, #56631, #77541, #42545, #15768, #78896, #1243 ),
 .UNSPECIFIED., .F., .F.,
 ( 4, 2, 1, 1, 1, 1, 1, 2, 2, 2, 2, 2, 2, 2, 2, 2, 4 ),
 ( 0.5000903094201638588, 0.5003344059487672135, 0.5005785024773704572, 0.5010666955345773887, 0.5020430816489914738, 0.5039958538778193109, 0.5079013983354746520, 0.5157124872507848901, 0.5313346650814048111, 0.5625790207426447642, 0.6250677320651241153, 0.6875564433876033554, 0.7500451547100827066, 0.8125338660325620577, 0.8750225773550412978, 0.9375112886775206489, 1.000000000000000000 ),
 .UNSPECIFIED. ) ;
#10524 = ORIENTED_EDGE ( 'NONE', *, *, #68571, .T. ) ;
#10525 = ORIENTED_EDGE ( 'NONE', *, *, #76339, .F. ) ;
#10526 = CARTESIAN_POINT ( 'NONE',  ( 172.5664832912740110, 0.2215528400590013880, 78.92562527591199739 ) ) ;
#10527 = ORIENTED_EDGE ( 'NONE', *, *, #4425, .F. ) ;
#10528 = ORIENTED_EDGE ( 'NONE', *, *, #37995, .F. ) ;
#10529 = CARTESIAN_POINT ( 'NONE',  ( 152.0371591254585724, -47.82818131005588214, 129.9678068554149775 ) ) ;
#10530 = LINE ( 'NONE', #14340, #29767 ) ;
#10531 = CARTESIAN_POINT ( 'NONE',  ( 106.4620492377333392, -26.72629803759836520, 41.12456998439165545 ) ) ;
#10532 = EDGE_CURVE ( 'NONE', #45, #17090, #75173, .T. ) ;
#10533 = CARTESIAN_POINT ( 'NONE',  ( 115.0376279413645761, -33.66073653188622927, 138.5409912566489652 ) ) ;
#10534 = CARTESIAN_POINT ( 'NONE',  ( 109.6227372377152847, -25.10643708164309018, 29.90419670448196854 ) ) ;
#10535 = ORIENTED_EDGE ( 'NONE', *, *, #5420, .F. ) ;
#10536 = CIRCLE ( 'NONE', #22159, 4.762500000000002842 ) ;
#10537 = CARTESIAN_POINT ( 'NONE',  ( -12.70000000000000462, 81.72090770373000623, 129.9368274816651194 ) ) ;
#10538 = ORIENTED_EDGE ( 'NONE', *, *, #6118, .F. ) ;
#10539 = DIRECTION ( 'NONE',  ( 0.000000000000000000, 0.000000000000000000, 1.000000000000000000 ) ) ;
#10540 = ORIENTED_EDGE ( 'NONE', *, *, #84842, .F. ) ;
#10541 = CARTESIAN_POINT ( 'NONE',  ( 179.4595971212735890, -26.00627455218472406, 117.4678068554150627 ) ) ;
#10542 = CARTESIAN_POINT ( 'NONE',  ( 71.24189083761808661, -0.9290567490904538817, 540.9756252759101471 ) ) ;
#10543 = DIRECTION ( 'NONE',  ( -1.000000000000000000, -1.000000000000000078E-15, -1.000000000000000078E-15 ) ) ;
#10544 = VECTOR ( 'NONE', #41772, 1000.000000000000000 ) ;
#10545 = DIRECTION ( 'NONE',  ( 1.387778780781444492E-15, 0.000000000000000000, -1.000000000000000000 ) ) ;
#10546 = ORIENTED_EDGE ( 'NONE', *, *, #10689, .T. ) ;
#10547 = CARTESIAN_POINT ( 'NONE',  ( 103.0904226585672916, -47.89329182393425555, 252.3041967044823366 ) ) ;
#10548 = CARTESIAN_POINT ( 'NONE',  ( 110.5697598356958764, -46.63222799359486714, 33.84705384733993583 ) ) ;
#10550 = CARTESIAN_POINT ( 'NONE',  ( 107.0667039024479834, -36.72944715994100306, 239.5838068554170093 ) ) ;
#10549 = DIRECTION ( 'NONE',  ( -0.7071067812162665778, -0.7071067811568285677, -7.071067812162659944E-16 ) ) ;
#10551 = DIRECTION ( 'NONE',  ( -0.7071067811865462405, -0.7071067811865489050, 0.000000000000000000 ) ) ;
#10552 = FACE_OUTER_BOUND ( 'NONE', #61752, .T. ) ;
#10553 = CARTESIAN_POINT ( 'NONE',  ( 48.85858412957961860, -30.08671355700278127, 193.9678068554150911 ) ) ;
#10554 = CARTESIAN_POINT ( 'NONE',  ( 115.0889047207443525, -30.61763667517494980, 10.34395860968370862 ) ) ;
#10555 = LINE ( 'NONE', #65956, #36154 ) ;
#10556 = FACE_OUTER_BOUND ( 'NONE', #80709, .T. ) ;
#10557 = CARTESIAN_POINT ( 'NONE',  ( 105.8910851810002356, -47.14611527663348056, 282.4870538473393253 ) ) ;
#10558 = CARTESIAN_POINT ( 'NONE',  ( 113.0221554258835823, -45.32894145911351558, 199.0584824187679374 ) ) ;
#10559 = CARTESIAN_POINT ( 'NONE',  ( 100.9283148882350787, -46.89532829952024429, 48.14419670448194211 ) ) ;
#10562 = ADVANCED_FACE ( 'NONE', ( #68362 ), #89259, .T. ) ;
#10561 = CARTESIAN_POINT ( 'NONE',  ( 112.0659116242543263, -45.48839625953056043, 47.98979194274246396 ) ) ;
#10560 = CARTESIAN_POINT ( 'NONE',  ( 186.6899999999999977, 59.08750000000000568, -50.79999999999999716 ) ) ;
#10563 = CARTESIAN_POINT ( 'NONE',  ( 151.0371591254582881, -46.82818131005593187, 249.9678068554149490 ) ) ;
#10564 = VECTOR ( 'NONE', #39476, 1000.000000000000000 ) ;
#10565 = EDGE_CURVE ( 'NONE', #64058, #22586, #70602, .T. ) ;
#10566 = ORIENTED_EDGE ( 'NONE', *, *, #15989, .T. ) ;
#10567 = CYLINDRICAL_SURFACE ( 'NONE', #14289, 7.937500000000000000 ) ;
#10568 = ORIENTED_EDGE ( 'NONE', *, *, #78704, .T. ) ;
#10569 = VECTOR ( 'NONE', #5192, 999.9999999999998863 ) ;
#10570 = CARTESIAN_POINT ( 'NONE',  ( 115.6651410650258214, -32.06827565682262815, 65.22133956162495849 ) ) ;
#10572 = VERTEX_POINT ( 'NONE', #49688 ) ;
#10571 = DIRECTION ( 'NONE',  ( -0.7071067811607679721, 0.7071067812123270624, 0.000000000000000000 ) ) ;
#10573 = FACE_OUTER_BOUND ( 'NONE', #30474, .T. ) ;
#10574 = CARTESIAN_POINT ( 'NONE',  ( 106.9751875180390641, -47.13234726572959232, 183.5699109901969734 ) ) ;
#10575 = DIRECTION ( 'NONE',  ( 0.8660254037844384856, 0.000000000000000000, -0.5000000000000003331 ) ) ;
#10576 = DIRECTION ( 'NONE',  ( -2.900000000000000265E-14, 2.000000000000000155E-15, -1.000000000000000000 ) ) ;
#10577 = DIRECTION ( 'NONE',  ( 1.000000000000000078E-15, -1.000000000000000083E-30, -1.000000000000000000 ) ) ;
#10578 = LINE ( 'NONE', #24657, #18049 ) ;
#10579 = DIRECTION ( 'NONE',  ( 1.000000000000000000, 4.237773401492740281E-14, 0.000000000000000000 ) ) ;
#10580 = CARTESIAN_POINT ( 'NONE',  ( 112.2009934676607656, -45.31764602677214526, 98.00527226877483145 ) ) ;
#10581 = CARTESIAN_POINT ( 'NONE',  ( 108.6395843534182291, -26.47938140272615470, 144.9432443235309904 ) ) ;
#10582 = ORIENTED_EDGE ( 'NONE', *, *, #63743, .F. ) ;
#10583 = VERTEX_POINT ( 'NONE', #50585 ) ;
#10584 = CARTESIAN_POINT ( 'NONE',  ( 113.4424924140864590, -42.92691738999312889, 94.64444044875396855 ) ) ;
#10585 = ADVANCED_FACE ( 'NONE', ( #63789 ), #22909, .F. ) ;
#10586 = CARTESIAN_POINT ( 'NONE',  ( 32.15435173583699680, -31.62489322948790971, -5.074374724088000832 ) ) ;
#10588 = DIRECTION ( 'NONE',  ( 0.000000000000000000, 0.000000000000000000, -1.000000000000000000 ) ) ;
#10587 = CARTESIAN_POINT ( 'NONE',  ( 116.2779988688839552, -41.49250982992358416, 239.4346728949579699 ) ) ;
#10589 = VECTOR ( 'NONE', #12468, 1000.000000000000000 ) ;
#10590 = DIRECTION ( 'NONE',  ( -0.9068632946707805287, 0.4214249218767882610, -9.061988307341536250E-16 ) ) ;
#10591 = LINE ( 'NONE', #3786, #17637 ) ;
#10592 = CARTESIAN_POINT ( 'NONE',  ( 118.0058494126929816, 76.91656954603718077, -11.41259371393238098 ) ) ;
#10593 = CARTESIAN_POINT ( 'NONE',  ( -2.077948353448777485, 70.01426914847409932, 118.5384880737505995 ) ) ;
#10594 = AXIS2_PLACEMENT_3D ( 'NONE', #30255, #85680, #65651 ) ;
#10595 = CARTESIAN_POINT ( 'NONE',  ( 162.7131505118539962, -33.70561438052111214, -5.074374724088000832 ) ) ;
#10596 = CARTESIAN_POINT ( 'NONE',  ( 8.325040720630020985, 73.05638748903209034, 118.2647812922514987 ) ) ;
#10597 = CARTESIAN_POINT ( 'NONE',  ( 98.18688568738947708, -31.30898482519904036, 170.8899109901960003 ) ) ;
#10598 = ORIENTED_EDGE ( 'NONE', *, *, #6745, .F. ) ;
#10599 = VERTEX_POINT ( 'NONE', #77410 ) ;
#10600 = DIRECTION ( 'NONE',  ( 0.000000000000000000, 0.000000000000000000, -1.000000000000000000 ) ) ;
#10601 = CARTESIAN_POINT ( 'NONE',  ( 112.1393456672597466, -28.01282279697495525, 150.6564586068802498 ) ) ;
#10602 = DIRECTION ( 'NONE',  ( 0.000000000000000000, 0.000000000000000000, 1.000000000000000000 ) ) ;
#10603 = DIRECTION ( 'NONE',  ( -1.000000000000000000, -1.734723475976808672E-15, 0.000000000000000000 ) ) ;
#10604 = CARTESIAN_POINT ( 'NONE',  ( 0.000000000000000000, 101.5999999999999943, 0.000000000000000000 ) ) ;
#10605 = CARTESIAN_POINT ( 'NONE',  ( 99.28842769779902255, -29.78762595464951346, 190.7470538473399415 ) ) ;
#10606 = CARTESIAN_POINT ( 'NONE',  ( 179.1667039024460166, -26.71338133339251542, 193.9678068554150059 ) ) ;
#10607 = ORIENTED_EDGE ( 'NONE', *, *, #13627, .F. ) ;
#10610 = ORIENTED_EDGE ( 'NONE', *, *, #27093, .T. ) ;
#10609 = ORIENTED_EDGE ( 'NONE', *, *, #66890, .T. ) ;
#10608 = EDGE_CURVE ( 'NONE', #87053, #12518, #59075, .T. ) ;
#10611 = CARTESIAN_POINT ( 'NONE',  ( -4.481911866145203760, 70.65984535152513502, 118.4718773200152384 ) ) ;
#10612 = B_SPLINE_CURVE_WITH_KNOTS ( 'NONE', 3,
 ( #44819, #23950, #52499, #86175, #80263 ),
 .UNSPECIFIED., .F., .F.,
 ( 4, 1, 4 ),
 ( 0.1438945294004070063, 4.132355267033809731, 7.123703416098150498 ),
 .UNSPECIFIED. ) ;
#10613 = DIRECTION ( 'NONE',  ( 0.000000000000000000, 0.000000000000000000, 1.000000000000000000 ) ) ;
#10614 = EDGE_CURVE ( 'NONE', #72800, #40087, #16092, .T. ) ;
#10615 = B_SPLINE_CURVE_WITH_KNOTS ( 'NONE', 3,
 ( #83811, #42440, #87822, #72414, #59202, #71969, #80569, #11519, #44681, #65585, #51489, #60086, #31057, #9733, #86050, #3808, #10178, #4704, #18322, #17876, #87377, #25585, #38319, #51926, #79685, #66464, #37886, #38761, #78793, #66923, #86492, #3368, #16550, #31950, #31494, #24257, #58751, #45121, #46003 ),
 .UNSPECIFIED., .F., .F.,
 ( 4, 2, 2, 2, 2, 2, 2, 2, 2, 2, 2, 2, 2, 2, 2, 1, 1, 1, 1, 1, 2, 4 ),
 ( 0.000000000000000000, 0.06249293107409987363, 0.1249858621481997473, 0.1874787932222996278, 0.2187252587593494224, 0.2499717242963992725, 0.2812181898334490948, 0.3124646553704988894, 0.3437111209075487395, 0.3749575864445985895, 0.4062040519816483841, 0.4374505175186981787, 0.4686969830557480843, 0.4843202158242727595, 0.4921318322085349584, 0.4960376404006660578, 0.4979905444967314687, 0.4989669965447642852, 0.4994552225687807767, 0.4996993355807888837, 0.4998213920867929372, 0.4999434485927969907 ),
 .UNSPECIFIED. ) ;
#10616 = CARTESIAN_POINT ( 'NONE',  ( 133.3217830637655936, -34.08035908359602217, 8.141856907856576342 ) ) ;
#10617 = CARTESIAN_POINT ( 'NONE',  ( 105.5764564592757466, -44.77785207962899250, 10.24809036959195652 ) ) ;
#10618 = DIRECTION ( 'NONE',  ( 0.000000000000000000, 0.000000000000000000, 1.000000000000000000 ) ) ;
#10619 = ORIENTED_EDGE ( 'NONE', *, *, #88693, .F. ) ;
#10620 = EDGE_CURVE ( 'NONE', #61315, #86385, #56163, .T. ) ;
#10621 = FACE_OUTER_BOUND ( 'NONE', #75644, .T. ) ;
#10622 = CARTESIAN_POINT ( 'NONE',  ( 81.57739926165950806, -16.43204134599606903, 7.859568798195391004 ) ) ;
#10623 = ORIENTED_EDGE ( 'NONE', *, *, #79318, .F. ) ;
#10624 = ORIENTED_EDGE ( 'NONE', *, *, #30029, .F. ) ;
#10625 = AXIS2_PLACEMENT_3D ( 'NONE', #69771, #76126, #42045 ) ;
#10626 = DIRECTION ( 'NONE',  ( 0.000000000000000000, 1.000000000000000000, 0.000000000000000000 ) ) ;
#10627 = EDGE_LOOP ( 'NONE', ( #85791, #64927, #18024, #74144 ) ) ;
#10628 = ORIENTED_EDGE ( 'NONE', *, *, #87102, .F. ) ;
#10629 = CARTESIAN_POINT ( 'NONE',  ( 97.07201853420036741, -35.37896439201897891, 157.2187929798531627 ) ) ;
#10630 = CIRCLE ( 'NONE', #80298, 5.041900000000001825 ) ;
#10631 = EDGE_CURVE ( 'NONE', #17742, #10129, #17029, .T. ) ;
#10632 = CARTESIAN_POINT ( 'NONE',  ( 110.5540359372802328, -28.93245362646326768, 24.16384839950497110 ) ) ;
#10633 = CARTESIAN_POINT ( 'NONE',  ( 110.0583800183467957, -26.06436417334086642, 219.8708633711489711 ) ) ;
#10634 = CARTESIAN_POINT ( 'NONE',  ( 114.0662423116486082, -44.47333502991310183, 133.1613395616249989 ) ) ;
#10635 = ADVANCED_FACE ( 'NONE', ( #78327 ), #1110, .T. ) ;
#10636 = CARTESIAN_POINT ( 'NONE',  ( 80.06648329127399677, -8.350947159940998787, 308.6356252759119911 ) ) ;
#10637 = CARTESIAN_POINT ( 'NONE',  ( 100.2472489666992743, -45.42841400796814355, 273.0594347997205773 ) ) ;
#10638 = PLANE ( 'NONE',  #36927 ) ;
#10639 = CARTESIAN_POINT ( 'NONE',  ( 41.56648329127398966, -18.82844715994071194, 75.92562527591206845 ) ) ;
#10640 = ORIENTED_EDGE ( 'NONE', *, *, #24101, .F. ) ;
#10641 = ORIENTED_EDGE ( 'NONE', *, *, #51621, .F. ) ;
#10642 = CARTESIAN_POINT ( 'NONE',  ( 117.2706010548463667, -41.09852764615815346, 213.5165776568629781 ) ) ;
#10643 = ORIENTED_EDGE ( 'NONE', *, *, #68710, .T. ) ;
#10644 = CARTESIAN_POINT ( 'NONE',  ( 108.6487477603288170, -25.79654920012707109, 149.9737205140059473 ) ) ;
#10645 = CARTESIAN_POINT ( 'NONE',  ( 204.2160000000000082, 52.73749999999999716, -44.45000000000000284 ) ) ;
#10646 = VECTOR ( 'NONE', #59927, 1000.000000000000000 ) ;
#10647 = FACE_OUTER_BOUND ( 'NONE', #70912, .T. ) ;
#10648 = CARTESIAN_POINT ( 'NONE',  ( 143.6231792275268617, -139.8594620027156736, 247.1482994587078394 ) ) ;
#10651 = CARTESIAN_POINT ( 'NONE',  ( 101.9462946551393543, -46.59843102978671681, 13.19562527591094891 ) ) ;
#10650 = DIRECTION ( 'NONE',  ( 0.000000000000000000, -1.000000000000000000, 0.000000000000000000 ) ) ;
#10649 = DIRECTION ( 'NONE',  ( 0.1858654558203195195, -0.9825752044157765042, 0.000000000000000000 ) ) ;
#10652 = FACE_OUTER_BOUND ( 'NONE', #84153, .T. ) ;
#10653 = LINE ( 'NONE', #51532, #64148 ) ;
#10654 = CARTESIAN_POINT ( 'NONE',  ( -97.46299999999992281, 82.54999999999999716, -12.70000000000034035 ) ) ;
#10655 = CIRCLE ( 'NONE', #36744, 4.874999999999990230 ) ;
#10656 = CARTESIAN_POINT ( 'NONE',  ( 75.31670390244798341, -67.87844715994100397, 37.63480685541480852 ) ) ;
#10657 = DIRECTION ( 'NONE',  ( -0.7071067811745735954, -0.7071067811985214391, 0.000000000000000000 ) ) ;
#10658 = DIRECTION ( 'NONE',  ( 0.000000000000000000, -1.000000000000000000, 0.000000000000000000 ) ) ;
#10660 = ORIENTED_EDGE ( 'NONE', *, *, #35021, .T. ) ;
#10659 = CARTESIAN_POINT ( 'NONE',  ( 98.61155387813832363, -36.65781496683363372, 195.5838068554172082 ) ) ;
#10661 = CARTESIAN_POINT ( 'NONE',  ( 107.0667039024470313, -104.2784471599421323, -21.78219314458201694 ) ) ;
#10662 = CARTESIAN_POINT ( 'NONE',  ( 116.3700403630726612, -44.11035778917459993, 198.2927681330539542 ) ) ;
#10663 = CARTESIAN_POINT ( 'NONE',  ( 100.2987399830848432, -46.45735886148204941, 83.09276813305294240 ) ) ;
#10664 = CARTESIAN_POINT ( 'NONE',  ( 96.07947519314286922, -35.15364532898842498, 222.2251490854349640 ) ) ;
#10665 = DIRECTION ( 'NONE',  ( -0.7071067811862239427, -0.7071067811868709807, 0.000000000000000000 ) ) ;
#10666 = DIRECTION ( 'NONE',  ( 0.000000000000000000, 1.000000000000000000, 5.463695987328529395E-16 ) ) ;
#10669 = EDGE_CURVE ( 'NONE', #16246, #61667, #35161, .T. ) ;
#10668 = CARTESIAN_POINT ( 'NONE',  ( 116.4530457758195752, -40.23956994039711077, 39.54146743497934580 ) ) ;
#10667 = CARTESIAN_POINT ( 'NONE',  ( 103.8797721312301405, -101.8611209747514010, -19.78219314458209865 ) ) ;
#10670 = DIRECTION ( 'NONE',  ( 1.000000000000000000, 0.000000000000000000, 0.000000000000000000 ) ) ;
#10671 = DIRECTION ( 'NONE',  ( 0.7071067811865459074, 0.7071067811865491270, 7.071067811865459556E-16 ) ) ;
#10672 = VECTOR ( 'NONE', #17000, 1000.000000000000000 ) ;
#10673 = CARTESIAN_POINT ( 'NONE',  ( 115.8272920594983049, -31.73323121823576898, 64.24007680160269729 ) ) ;
#10674 = EDGE_CURVE ( 'NONE', #5130, #16097, #69220, .T. ) ;
#10675 = ORIENTED_EDGE ( 'NONE', *, *, #32577, .F. ) ;
#10676 = ORIENTED_EDGE ( 'NONE', *, *, #50721, .F. ) ;
#10677 = CARTESIAN_POINT ( 'NONE',  ( 99.00375160886646597, -32.60573182744733600, 95.38480078045697041 ) ) ;
#10679 = EDGE_LOOP ( 'NONE', ( #43599, #72030, #76312, #61680 ) ) ;
#10678 = DIRECTION ( 'NONE',  ( -0.000000000000000000, -0.000000000000000000, 1.000000000000000000 ) ) ;
#10680 = CARTESIAN_POINT ( 'NONE',  ( 110.1514708964275684, -46.66481413883387575, 93.81562527591097478 ) ) ;
#10681 = DIRECTION ( 'NONE',  ( 0.000000000000000000, 0.000000000000000000, -1.000000000000000000 ) ) ;
#10682 = CARTESIAN_POINT ( 'NONE',  ( 160.7738106836348209, -48.62134037874901082, 300.4678068554149490 ) ) ;
#10683 = CARTESIAN_POINT ( 'NONE',  ( 51.27381068362099370, -23.19206098993950604, -5.074374724088000832 ) ) ;
#10684 = CARTESIAN_POINT ( 'NONE',  ( 97.95204982468527533, -33.09064556074055474, 41.02419670448293232 ) ) ;
#10685 = EDGE_LOOP ( 'NONE', ( #12209, #62229, #80700, #16228 ) ) ;
#10686 = ORIENTED_EDGE ( 'NONE', *, *, #66208, .F. ) ;
#10687 = VERTEX_POINT ( 'NONE', #8375 ) ;
#10688 = VECTOR ( 'NONE', #11101, 1000.000000000000000 ) ;
#10689 = EDGE_CURVE ( 'NONE', #28034, #25618, #28820, .T. ) ;
#10690 = DIRECTION ( 'NONE',  ( 1.000000000000000078E-15, -1.000000000000000083E-30, -1.000000000000000000 ) ) ;
#10691 = DIRECTION ( 'NONE',  ( 0.7071067811864676367, 0.7071067811866273978, 7.071067811864669709E-16 ) ) ;
#10693 = VECTOR ( 'NONE', #82168, 1000.000000000000000 ) ;
#10692 = CARTESIAN_POINT ( 'NONE',  ( 108.4174892559276913, -26.73503592823092845, 115.9689586089433391 ) ) ;
#10694 = FACE_OUTER_BOUND ( 'NONE', #3683, .T. ) ;
#10695 = CARTESIAN_POINT ( 'NONE',  ( 32.56670390244700997, -22.48495420874110806, 342.9256252759119548 ) ) ;
#10696 = CARTESIAN_POINT ( 'NONE',  ( 97.33789353722791304, -34.07085096390528633, 52.11557580465839123 ) ) ;
#10697 = CARTESIAN_POINT ( 'NONE',  ( 107.0664832912739683, -24.97944715994095333, 307.1356252759109680 ) ) ;
#10698 = CARTESIAN_POINT ( 'NONE',  ( -4.878244184937265970, 94.27573757619954620, 130.4648306225670353 ) ) ;
#10699 = LINE ( 'NONE', #1783, #48684 ) ;
#10700 = CARTESIAN_POINT ( 'NONE',  ( 109.6376038899290677, -46.81002275840761939, 47.77562527591094721 ) ) ;
#10701 = ORIENTED_EDGE ( 'NONE', *, *, #2789, .F. ) ;
#10702 = VERTEX_POINT ( 'NONE', #14297 ) ;
#10703 = ADVANCED_FACE ( 'NONE', ( #71506 ), #69706, .T. ) ;
#10704 = CARTESIAN_POINT ( 'NONE',  ( 9.549815870737170087, 90.93248498521381862, 130.2065322450557119 ) ) ;
#10705 = CYLINDRICAL_SURFACE ( 'NONE', #86719, 5.500000000000000888 ) ;
#10706 = DIRECTION ( 'NONE',  ( 0.000000000000000000, -1.000000000000000000, 0.000000000000000000 ) ) ;
#10707 = CARTESIAN_POINT ( 'NONE',  ( 98.41263308787671349, -36.61538842024999241, 154.1461856076869594 ) ) ;
#10708 = VECTOR ( 'NONE', #21796, 1000.000000000000000 ) ;
#10709 = AXIS2_PLACEMENT_3D ( 'NONE', #6668, #34362, #89808 ) ;
#10710 = EDGE_CURVE ( 'NONE', #64009, #56554, #36964, .T. ) ;
#10711 = AXIS2_PLACEMENT_3D ( 'NONE', #17144, #38458, #32093 ) ;
#10712 = DIRECTION ( 'NONE',  ( -0.2884130866282269556, 0.7071067811865447972, 0.6456143519637576045 ) ) ;
#10713 = ORIENTED_EDGE ( 'NONE', *, *, #42100, .F. ) ;
#10714 = ORIENTED_EDGE ( 'NONE', *, *, #48793, .F. ) ;
#10715 = FACE_OUTER_BOUND ( 'NONE', #84284, .T. ) ;
#10716 = CIRCLE ( 'NONE', #25179, 0.4999999999999976685 ) ;
#10717 = ORIENTED_EDGE ( 'NONE', *, *, #67518, .T. ) ;
#10718 = ORIENTED_EDGE ( 'NONE', *, *, #75928, .F. ) ;
#10719 = DIRECTION ( 'NONE',  ( -0.9254794337955620787, -0.3787978585227822492, 0.000000000000000000 ) ) ;
#10720 = EDGE_CURVE ( 'NONE', #66156, #87997, #42418, .T. ) ;
#10721 = CARTESIAN_POINT ( 'NONE',  ( 108.4337774161041921, -27.97394686652187090, 186.3844404487539634 ) ) ;
#10722 = LINE ( 'NONE', #12079, #60272 ) ;
#10723 = DIRECTION ( 'NONE',  ( 0.000000000000000000, -1.000000000000000000, 0.000000000000000000 ) ) ;
#10724 = CARTESIAN_POINT ( 'NONE',  ( -110.3511101689945093, 62.10781539098685045, 69.76748536262132916 ) ) ;
#10725 = ORIENTED_EDGE ( 'NONE', *, *, #26800, .F. ) ;
#10726 = ORIENTED_EDGE ( 'NONE', *, *, #67301, .F. ) ;
#10727 = ORIENTED_EDGE ( 'NONE', *, *, #56375, .T. ) ;
#10728 = ADVANCED_FACE ( 'NONE', ( #70146 ), #84245, .T. ) ;
#10729 = CARTESIAN_POINT ( 'NONE',  ( 113.1326720373799617, -31.22635327163875374, 207.2309475124489495 ) ) ;
#10730 = CARTESIAN_POINT ( 'NONE',  ( 101.6667450491003706, -27.05792876557581650, 105.4937205140069665 ) ) ;
#10731 = CARTESIAN_POINT ( 'NONE',  ( 114.0759046727996093, -46.25395340493279406, 33.08133956162495792 ) ) ;
#10732 =( NAMED_UNIT ( * ) PLANE_ANGLE_UNIT ( ) SI_UNIT ( $, .RADIAN. ) );
#10733 = ADVANCED_FACE ( 'NONE', ( #42867 ), #77868, .F. ) ;
#10734 = CARTESIAN_POINT ( 'NONE',  ( 73.06670390244801183, -50.82844715994100682, 310.9178068554150514 ) ) ;
#10735 = CARTESIAN_POINT ( 'NONE',  ( 108.8488479242245290, -47.00104215551821341, 163.7127681330539701 ) ) ;
#10737 = EDGE_CURVE ( 'NONE', #34489, #60854, #36534, .T. ) ;
#10736 = CYLINDRICAL_SURFACE ( 'NONE', #84268, 9.999999999999998224 ) ;
#10738 = EDGE_LOOP ( 'NONE', ( #44986, #19954, #54006, #64514 ) ) ;
#10739 = LINE ( 'NONE', #23516, #49588 ) ;
#10740 = ORIENTED_EDGE ( 'NONE', *, *, #67463, .T. ) ;
#10741 = EDGE_CURVE ( 'NONE', #30195, #49111, #16529, .T. ) ;
#10742 = ORIENTED_EDGE ( 'NONE', *, *, #36602, .F. ) ;
#10743 = DIRECTION ( 'NONE',  ( 1.000000000000000000, 4.299999999999999979E-14, 1.000000000000000078E-15 ) ) ;
#10744 = ORIENTED_EDGE ( 'NONE', *, *, #52344, .F. ) ;
#10745 = ORIENTED_EDGE ( 'NONE', *, *, #16731, .F. ) ;
#10746 = AXIS2_PLACEMENT_3D ( 'NONE', #25629, #18818, #53305 ) ;
#10747 = ORIENTED_EDGE ( 'NONE', *, *, #2946, .T. ) ;
#10748 = CARTESIAN_POINT ( 'NONE',  ( 115.5446080981639057, -31.35709777695358369, 130.2761217128978899 ) ) ;
#10749 = CARTESIAN_POINT ( 'NONE',  ( 110.7945467183388502, -46.46538951521414873, 62.86705384733992474 ) ) ;
#10750 = FACE_OUTER_BOUND ( 'NONE', #72031, .T. ) ;
#10751 = AXIS2_PLACEMENT_3D ( 'NONE', #6511, #41459, #69187 ) ;
#10752 = DIRECTION ( 'NONE',  ( -0.08544974978095701279, -0.9963424814100680926, 0.000000000000000000 ) ) ;
#10753 = DIRECTION ( 'NONE',  ( 1.000000000000000078E-15, -1.000000000000000083E-30, -1.000000000000000000 ) ) ;
#10754 = CARTESIAN_POINT ( 'NONE',  ( 108.8666348730871221, -46.34312957481634498, 82.72419670448294937 ) ) ;
#10756 = CARTESIAN_POINT ( 'NONE',  ( 106.9751875180390641, -47.13234726572959232, 183.5699109901969734 ) ) ;
#10755 = CARTESIAN_POINT ( 'NONE',  ( 33.98325472291465132, 111.1250000000000000, -3.174999999999999822 ) ) ;
#10757 = DIRECTION ( 'NONE',  ( 0.000000000000000000, 1.000000000000000000, 0.000000000000000000 ) ) ;
#10758 = DIRECTION ( 'NONE',  ( 1.042073847087816516E-15, 1.000000000000000000, 0.000000000000000000 ) ) ;
#10759 = ORIENTED_EDGE ( 'NONE', *, *, #75212, .T. ) ;
#10760 = CARTESIAN_POINT ( 'NONE',  ( -465.6921742093550165, 47.62500000000000000, 3.174999999999999822 ) ) ;
#10761 = DIRECTION ( 'NONE',  ( 0.000000000000000000, 2.135044278125299371E-15, -1.000000000000000000 ) ) ;
#10762 = CARTESIAN_POINT ( 'NONE',  ( 70.63919639214310564, 49.07499999999999574, -53.97512327982435210 ) ) ;
#10763 = FACE_OUTER_BOUND ( 'NONE', #52290, .T. ) ;
#10765 = EDGE_LOOP ( 'NONE', ( #51611, #37216, #50236, #79252 ) ) ;
#10764 = CARTESIAN_POINT ( 'NONE',  ( 117.2351557800294870, -41.18040025386632408, 208.4861014663869696 ) ) ;
#10766 = CARTESIAN_POINT ( 'NONE',  ( 115.0888828095797010, -30.61760375934272105, 144.3439616953089342 ) ) ;
#10767 = CARTESIAN_POINT ( 'NONE',  ( 113.8133276556114595, -26.95691720032833416, 235.5956252759109759 ) ) ;
#10768 = CARTESIAN_POINT ( 'NONE',  ( 107.3350663223963153, -26.26422652666180468, 116.0556252759109555 ) ) ;
#10769 = CARTESIAN_POINT ( 'NONE',  ( 84.20430400022883077, 76.20343663217362007, 99.77245543246509385 ) ) ;
#10770 = CARTESIAN_POINT ( 'NONE',  ( 82.50377070433003723, -38.00325133681918288, 7.150416387932702733 ) ) ;
#10771 = CARTESIAN_POINT ( 'NONE',  ( 44.45000000000000284, 50.79999999999999716, 206.3750000000000000 ) ) ;
#10772 = PLANE ( 'NONE',  #79949 ) ;
#10773 = ORIENTED_EDGE ( 'NONE', *, *, #39623, .F. ) ;
#10774 = VECTOR ( 'NONE', #27813, 1000.000000000000000 ) ;
#10775 = CONICAL_SURFACE ( 'NONE', #77518, 24.63800000000000168, 0.7853981633974710386 ) ;
#10776 = AXIS2_PLACEMENT_3D ( 'NONE', #69, #27769, #83645 ) ;
#10777 = CONICAL_SURFACE ( 'NONE', #86210, 6.858000000000003205, 0.02993239667170383839 ) ;
#10778 = EDGE_CURVE ( 'NONE', #52534, #17788, #87796, .T. ) ;
#10779 = ORIENTED_EDGE ( 'NONE', *, *, #42102, .T. ) ;
#10780 = ORIENTED_EDGE ( 'NONE', *, *, #27281, .F. ) ;
#10781 = AXIS2_PLACEMENT_3D ( 'NONE', #85648, #66056, #17039 ) ;
#10782 = VECTOR ( 'NONE', #51887, 1000.000000000000000 ) ;
#10783 = ORIENTED_EDGE ( 'NONE', *, *, #41535, .F. ) ;
#10784 = CARTESIAN_POINT ( 'NONE',  ( 115.7831076666659413, -41.80230951636190895, 73.40645860869774708 ) ) ;
#10785 = CARTESIAN_POINT ( 'NONE',  ( 113.7560087186648730, -29.08427257552855494, 285.5032443235299979 ) ) ;
#10786 = B_SPLINE_CURVE_WITH_KNOTS ( 'NONE', 3,
 ( #53614, #52264, #81379, #40007, #67723, #32290, #66365, #5510, #38665, #33204, #73637, #10522, #18227, #51832, #79584, #38226, #59098, #80030, #73182, #65920, #3706, #31399, #24602, #10960, #4154, #31852, #25044, #45908, #49048, #61341 ),
 .UNSPECIFIED., .F., .F.,
 ( 4, 2, 2, 2, 1, 2, 2, 2, 2, 2, 2, 2, 1, 2, 2, 4 ),
 ( 0.5000000000000000000, 0.5625000000000072164, 0.5937500000000088818, 0.6093750000000097700, 0.6171875000000102141, 0.6210937500000091038, 0.6250000000000078826, 0.6875000000000095479, 0.7187500000000133227, 0.7500000000000170974, 0.8125000000000208722, 0.8437500000000262013, 0.8593750000000288658, 0.8671875000000301981, 0.8750000000000315303, 1.000000000000000000 ),
 .UNSPECIFIED. ) ;
#10787 = CARTESIAN_POINT ( 'NONE',  ( -492.0614999999999668, 14.28749999999982201, 85.72499999999999432 ) ) ;
#10788 = CARTESIAN_POINT ( 'NONE',  ( -40.89999999999999858, 53.97500000000000142, 30.79999999999999361 ) ) ;
#10790 = CARTESIAN_POINT ( 'NONE',  ( 77.69145367648738443, 73.00424585431355240, 89.55259891852641374 ) ) ;
#10789 = DIRECTION ( 'NONE',  ( 0.000000000000000000, 0.000000000000000000, -1.000000000000000000 ) ) ;
#10791 = CARTESIAN_POINT ( 'NONE',  ( 104.4064053327731472, -46.06725273453308489, 216.7781341137909692 ) ) ;
#10792 = ORIENTED_EDGE ( 'NONE', *, *, #33079, .T. ) ;
#10793 = ORIENTED_EDGE ( 'NONE', *, *, #3455, .F. ) ;
#10794 = EDGE_LOOP ( 'NONE', ( #43035, #72771, #64959, #11516 ) ) ;
#10795 = EDGE_CURVE ( 'NONE', #44803, #20780, #71945, .T. ) ;
#10796 = CARTESIAN_POINT ( 'NONE',  ( 20.03715912545736089, -24.42818131006190541, 237.4678068554150059 ) ) ;
#10797 = FACE_BOUND ( 'NONE', #84551, .T. ) ;
#10798 = DIRECTION ( 'NONE',  ( 0.000000000000000000, -1.000000000000000000, 0.000000000000000000 ) ) ;
#10799 = EDGE_CURVE ( 'NONE', #81090, #79139, #89250, .T. ) ;
#10800 = CARTESIAN_POINT ( 'NONE',  ( 100.8575770528253628, -43.09432028306430595, 18.39301187732595011 ) ) ;
#10801 = CARTESIAN_POINT ( 'NONE',  ( 117.8827734314469637, 84.21498941703524110, -12.61757617297137024 ) ) ;
#10802 = EDGE_CURVE ( 'NONE', #67480, #12481, #45985, .T. ) ;
#10803 = DIRECTION ( 'NONE',  ( 1.000000000000000078E-15, 1.000000000000000083E-30, -1.000000000000000000 ) ) ;
#10804 = DIRECTION ( 'NONE',  ( 4.299999999999999979E-14, -1.000000000000000000, 4.400000000000000367E-29 ) ) ;
#10805 = ADVANCED_FACE ( 'NONE', ( #11495 ), #39191, .F. ) ;
#10806 = ORIENTED_EDGE ( 'NONE', *, *, #9802, .T. ) ;
#10807 = EDGE_CURVE ( 'NONE', #75812, #80812, #81454, .T. ) ;
#10808 = CARTESIAN_POINT ( 'NONE',  ( 179.8608231853560255, -35.55794170701751256, -5.074374724088000832 ) ) ;
#10809 = ORIENTED_EDGE ( 'NONE', *, *, #43096, .F. ) ;
#10810 = CARTESIAN_POINT ( 'NONE',  ( 30.00000000000003553, 172.0000000000000000, 182.8826257785461280 ) ) ;
#10811 = CARTESIAN_POINT ( 'NONE',  ( 115.2261106523039444, -36.95351711827176899, 41.62237608387797394 ) ) ;
#10812 = ADVANCED_FACE ( 'NONE', ( #26020 ), #39631, .T. ) ;
#10813 = VECTOR ( 'NONE', #83878, 1000.000000000000000 ) ;
#10814 = ADVANCED_FACE ( 'NONE', ( #12386 ), #20104, .T. ) ;
#10815 = DIRECTION ( 'NONE',  ( 0.000000000000000000, -1.000000000000000000, 0.000000000000000000 ) ) ;
#10816 = CIRCLE ( 'NONE', #67422, 2.117000000000000881 ) ;
#10817 = EDGE_CURVE ( 'NONE', #2727, #42703, #82392, .T. ) ;
#10818 = FACE_OUTER_BOUND ( 'NONE', #85392, .T. ) ;
#10819 = CARTESIAN_POINT ( 'NONE',  ( -462.0260000000000105, 53.97500000000000142, -1.387778780781445991E-14 ) ) ;
#10820 = VERTEX_POINT ( 'NONE', #47780 ) ;
#10821 = DIRECTION ( 'NONE',  ( 1.000000000000000000, 0.000000000000000000, 0.000000000000000000 ) ) ;
#10822 = CARTESIAN_POINT ( 'NONE',  ( 19.56670390244643443, -25.42844715994203852, 180.4678068554150911 ) ) ;
#10823 = EDGE_CURVE ( 'NONE', #73627, #67094, #54581, .T. ) ;
#10824 = ORIENTED_EDGE ( 'NONE', *, *, #40474, .T. ) ;
#10825 = CARTESIAN_POINT ( 'NONE',  ( 107.3339538991774447, -26.30757161206916095, 120.0556252759109555 ) ) ;
#10826 = ORIENTED_EDGE ( 'NONE', *, *, #2277, .F. ) ;
#10827 = CARTESIAN_POINT ( 'NONE',  ( 111.2570682682515439, -29.25341213619239156, 34.09241982807698434 ) ) ;
#10828 = ADVANCED_FACE ( 'NONE', ( #26464 ), #40079, .F. ) ;
#10829 = LINE ( 'NONE', #22698, #73600 ) ;
#10830 = CARTESIAN_POINT ( 'NONE',  ( 112.5403241924349942, -29.76056314593741803, 75.97872616303996551 ) ) ;
#10831 = DIRECTION ( 'NONE',  ( 2.973811673103097665E-16, -0.000000000000000000, 1.000000000000000000 ) ) ;
#10832 = CYLINDRICAL_SURFACE ( 'NONE', #2400, 7.937500000000000000 ) ;
#10833 = CARTESIAN_POINT ( 'NONE',  ( 147.0761462423337775, -68.28389950123539620, 246.9923701901030029 ) ) ;
#10834 = CARTESIAN_POINT ( 'NONE',  ( 115.9100415161514945, -31.16808610560197224, 30.27276813305396175 ) ) ;
#10835 = DIRECTION ( 'NONE',  ( 1.000000000000000000, 0.000000000000000000, -3.406823656978775284E-15 ) ) ;
#10836 = EDGE_LOOP ( 'NONE', ( #78401, #77253, #65207, #69259, #65581, #48476, #23835, #25122, #31605, #28971, #23926, #82289, #62450, #36495, #14722, #29877, #4368, #34971 ) ) ;
#10837 = CARTESIAN_POINT ( 'NONE',  ( 194.0667039024482108, -40.32844715993407192, 180.4678068554150343 ) ) ;
#10838 = AXIS2_PLACEMENT_3D ( 'NONE', #82700, #54489, #67247 ) ;
#10839 = VERTEX_POINT ( 'NONE', #25560 ) ;
#10840 = CARTESIAN_POINT ( 'NONE',  ( 77.31648329127399677, -18.72944715994106346, 3.101481641215480867 ) ) ;
#10841 = AXIS2_PLACEMENT_3D ( 'NONE', #48641, #42722, #6880 ) ;
#10842 = VECTOR ( 'NONE', #59597, 1000.000000000000000 ) ;
#10843 = AXIS2_PLACEMENT_3D ( 'NONE', #66961, #30659, #59242 ) ;
#10844 = ORIENTED_EDGE ( 'NONE', *, *, #85425, .F. ) ;
#10845 = VERTEX_POINT ( 'NONE', #82343 ) ;
#10846 = VECTOR ( 'NONE', #84197, 1000.000000000000000 ) ;
#10847 = DIRECTION ( 'NONE',  ( -1.000000000000000000, 0.000000000000000000, 0.000000000000000000 ) ) ;
#10848 = EDGE_CURVE ( 'NONE', #34776, #76744, #60980, .T. ) ;
#10849 = VECTOR ( 'NONE', #56822, 1000.000000000000000 ) ;
#10850 = ORIENTED_EDGE ( 'NONE', *, *, #51520, .T. ) ;
#10851 = CARTESIAN_POINT ( 'NONE',  ( 100.2051353121704835, -29.75912871662441361, 225.6956252759109702 ) ) ;
#10852 = EDGE_CURVE ( 'NONE', #27163, #4309, #40533, .T. ) ;
#10853 = CARTESIAN_POINT ( 'NONE',  ( 116.0120085738102631, -32.18627031846445874, 124.2002723411735872 ) ) ;
#10854 = CYLINDRICAL_SURFACE ( 'NONE', #70881, 4.762500000000002842 ) ;
#10855 = CARTESIAN_POINT ( 'NONE',  ( 115.5737247207382552, -42.75516958203532880, 49.33562527591095659 ) ) ;
#10857 = ADVANCED_FACE ( 'NONE', ( #47332 ), #75515, .F. ) ;
#10856 = DIRECTION ( 'NONE',  ( 0.000000000000000000, 0.000000000000000000, 1.000000000000000000 ) ) ;
#10858 = ORIENTED_EDGE ( 'NONE', *, *, #59471, .T. ) ;
#10859 = CARTESIAN_POINT ( 'NONE',  ( 103.7225970069647474, -27.30339880462703661, 171.3477492379661555 ) ) ;
#10860 = EDGE_CURVE ( 'NONE', #52412, #74795, #6910, .T. ) ;
#10861 = CARTESIAN_POINT ( 'NONE',  ( 90.06670390244703128, -104.2784471599417770, -9.937637710810031777 ) ) ;
#10862 = EDGE_LOOP ( 'NONE', ( #89859, #72958 ) ) ;
#10863 = CARTESIAN_POINT ( 'NONE',  ( 61.56670390244634916, -23.42844715994043270, 180.4678068554151196 ) ) ;
#10864 = DIRECTION ( 'NONE',  ( 0.000000000000000000, 0.000000000000000000, 1.000000000000000000 ) ) ;
#10865 = CARTESIAN_POINT ( 'NONE',  ( 113.7851844261090264, -26.99768152489561501, 239.5956252759109759 ) ) ;
#10866 = DIRECTION ( 'NONE',  ( 1.000000000000000078E-15, 1.000000000000000083E-30, -1.000000000000000000 ) ) ;
#10867 = AXIS2_PLACEMENT_3D ( 'NONE', #78825, #31536, #37917 ) ;
#10868 = DIRECTION ( 'NONE',  ( -1.000000000000000000, 0.000000000000000000, -1.840813417405305102E-14 ) ) ;
#10869 = CARTESIAN_POINT ( 'NONE',  ( 77.54412859703529648, -37.82508440162273189, 2.797770139040228976 ) ) ;
#10870 = CARTESIAN_POINT ( 'NONE',  ( 101.4793796374089965, -43.85664460571122447, 276.4819436376007502 ) ) ;
#10872 = CARTESIAN_POINT ( 'NONE',  ( 103.2867953297129873, -47.09177226061134292, 93.28610146638693834 ) ) ;
#10871 = LINE ( 'NONE', #73993, #34509 ) ;
#10873 = CARTESIAN_POINT ( 'NONE',  ( 121.7044748306527424, 74.30620332398891037, 47.25378613605970202 ) ) ;
#10874 = CARTESIAN_POINT ( 'NONE',  ( 106.0722674988897296, -48.58863484196640314, 112.5099109901969712 ) ) ;
#10875 = ORIENTED_EDGE ( 'NONE', *, *, #26341, .T. ) ;
#10876 = LINE ( 'NONE', #72225, #71287 ) ;
#10877 = ORIENTED_EDGE ( 'NONE', *, *, #33199, .T. ) ;
#10878 = CARTESIAN_POINT ( 'NONE',  ( 4.163101094985349692E-14, 120.6499999999999915, -107.7702177616926065 ) ) ;
#10879 = LINE ( 'NONE', #66276, #24662 ) ;
#10880 = DIRECTION ( 'NONE',  ( 1.000000000000000078E-15, 1.000000000000000083E-30, -1.000000000000000000 ) ) ;
#10881 = VERTEX_POINT ( 'NONE', #19205 ) ;
#10882 = DIRECTION ( 'NONE',  ( 0.000000000000000000, 0.000000000000000000, -1.000000000000000000 ) ) ;
#10884 = ORIENTED_EDGE ( 'NONE', *, *, #42633, .F. ) ;
#10883 = CARTESIAN_POINT ( 'NONE',  ( 117.9212005353621322, -39.05065313503074975, 108.6708633711489824 ) ) ;
#10885 = CARTESIAN_POINT ( 'NONE',  ( 183.6524903400785433, -48.32844715993451956, 180.4678068554150343 ) ) ;
#10886 = FACE_OUTER_BOUND ( 'NONE', #4161, .T. ) ;
#10887 = AXIS2_PLACEMENT_3D ( 'NONE', #63416, #1198, #28908 ) ;
#10888 = DIRECTION ( 'NONE',  ( 1.000000000000000078E-15, -1.000000000000000083E-30, -1.000000000000000000 ) ) ;
#10889 = ORIENTED_EDGE ( 'NONE', *, *, #32592, .T. ) ;
#10890 = CARTESIAN_POINT ( 'NONE',  ( 96.00011186464382718, -37.20993085831212710, 116.3489586092439652 ) ) ;
#10891 = SURFACE_STYLE_FILL_AREA ( #79060 ) ;
#10892 = DIRECTION ( 'NONE',  ( -0.8660253910675250744, -0.0001484127182050486030, -0.5000000000000052180 ) ) ;
#10893 = CARTESIAN_POINT ( 'NONE',  ( 177.8371591254543489, -47.82818131005477369, 249.9678068554149775 ) ) ;
#10894 = ORIENTED_EDGE ( 'NONE', *, *, #29850, .F. ) ;
#10895 = ORIENTED_EDGE ( 'NONE', *, *, #60157, .T. ) ;
#10896 = CARTESIAN_POINT ( 'NONE',  ( 140.0667039024470171, -90.27844715994091018, 45.21780685541799727 ) ) ;
#10897 = CARTESIAN_POINT ( 'NONE',  ( -479.3614999999999782, 3.174999999999999822, -1.387778780781445991E-14 ) ) ;
#10898 = LINE ( 'NONE', #38603, #74808 ) ;
#10900 = CARTESIAN_POINT ( 'NONE',  ( 120.2221484686747317, -96.68314769832106492, -11.78219314458223188 ) ) ;
#10899 = CYLINDRICAL_SURFACE ( 'NONE', #10250, 12.99999999999999822 ) ;
#10901 = DIRECTION ( 'NONE',  ( 0.000000000000000000, 0.000000000000000000, -1.000000000000000000 ) ) ;
#10902 = ORIENTED_EDGE ( 'NONE', *, *, #64830, .T. ) ;
#10903 = AXIS2_PLACEMENT_3D ( 'NONE', #22212, #49887, #8123 ) ;
#10904 = CIRCLE ( 'NONE', #57260, 7.799999999999994493 ) ;
#10905 = AXIS2_PLACEMENT_3D ( 'NONE', #63698, #84607, #21470 ) ;
#10906 = EDGE_CURVE ( 'NONE', #82312, #51989, #61860, .T. ) ;
#10907 = CARTESIAN_POINT ( 'NONE',  ( 41.56670390244777735, -36.32844715994104234, 300.4678068554150059 ) ) ;
#10908 = ADVANCED_FACE ( 'NONE', ( #27352 ), #32822, .F. ) ;
#10909 = CARTESIAN_POINT ( 'NONE',  ( 103.7602102885707467, -27.48919103108776341, 186.3499109901959798 ) ) ;
#10911 = ORIENTED_EDGE ( 'NONE', *, *, #51400, .T. ) ;
#10910 = FACE_BOUND ( 'NONE', #89150, .T. ) ;
#10912 = AXIS2_PLACEMENT_3D ( 'NONE', #3971, #79851, #10344 ) ;
#10913 = EDGE_CURVE ( 'NONE', #57450, #52412, #13729, .T. ) ;
#10914 = CARTESIAN_POINT ( 'NONE',  ( 99.77418633167441442, -43.29726106931974527, 52.90991099019598209 ) ) ;
#10915 = CARTESIAN_POINT ( 'NONE',  ( 100.8873880383125936, -44.70015583377661983, 52.05235198494534643 ) ) ;
#10916 = DIRECTION ( 'NONE',  ( 0.000000000000000000, 0.000000000000000000, -1.000000000000000000 ) ) ;
#10917 = VECTOR ( 'NONE', #20418, 1000.000000000000000 ) ;
#10918 = DIRECTION ( 'NONE',  ( 1.907762142705490052E-15, 7.167082501179359715E-16, -1.000000000000000000 ) ) ;
#10919 = EDGE_CURVE ( 'NONE', #32855, #84272, #82794, .T. ) ;
#10920 = EDGE_LOOP ( 'NONE', ( #86351, #45913 ) ) ;
#10921 = FACE_OUTER_BOUND ( 'NONE', #82280, .T. ) ;
#10922 = EDGE_LOOP ( 'NONE', ( #27485, #15450 ) ) ;
#10923 = ORIENTED_EDGE ( 'NONE', *, *, #58584, .T. ) ;
#10924 = CARTESIAN_POINT ( 'NONE',  ( 111.4343887032284783, -44.43980907907789657, 209.4187261630399632 ) ) ;
#10925 = ADVANCED_FACE ( 'NONE', ( #20555 ), #75958, .F. ) ;
#10926 = CARTESIAN_POINT ( 'NONE',  ( 116.7961848845175865, -39.38406792386692246, 54.61469027183413516 ) ) ;
#10927 = PLANE ( 'NONE',  #66769 ) ;
#10928 = CARTESIAN_POINT ( 'NONE',  ( 31.71315051185471390, -33.70561438052040160, 237.4678068554150059 ) ) ;
#10929 = DIRECTION ( 'NONE',  ( 0.9963424814100679816, -0.08544974978095716545, 0.000000000000000000 ) ) ;
#10930 = VERTEX_POINT ( 'NONE', #74167 ) ;
#10931 = CARTESIAN_POINT ( 'NONE',  ( 114.0075790447422577, -33.88846322101949227, 9.125625275910969947 ) ) ;
#10932 = CARTESIAN_POINT ( 'NONE',  ( 105.7925177523798368, -26.72498828120203740, 36.17735711206680094 ) ) ;
#10933 = ORIENTED_EDGE ( 'NONE', *, *, #69248, .T. ) ;
#10934 = CARTESIAN_POINT ( 'NONE',  ( 117.5124197103495050, -37.28486668576427121, 18.78419670448294809 ) ) ;
#10935 = FACE_OUTER_BOUND ( 'NONE', #80727, .T. ) ;
#10936 = EDGE_LOOP ( 'NONE', ( #6174, #2108, #10609, #33361 ) ) ;
#10937 = EDGE_CURVE ( 'NONE', #25134, #76956, #36857, .T. ) ;
#10938 = CARTESIAN_POINT ( 'NONE',  ( 101.9936209311938740, -45.44607153314367309, 82.15645860836184511 ) ) ;
#10939 = DIRECTION ( 'NONE',  ( -4.237773401492740281E-14, 1.000000000000000000, 0.000000000000000000 ) ) ;
#10940 = PLANE ( 'NONE',  #59168 ) ;
#10941 = DIRECTION ( 'NONE',  ( 1.000000000000000000, 4.163336342344333240E-14, 0.000000000000000000 ) ) ;
#10942 = EDGE_CURVE ( 'NONE', #28049, #52806, #35961, .T. ) ;
#10943 = CARTESIAN_POINT ( 'NONE',  ( 97.36167283409557172, -40.65495779399346077, 202.6327681330539860 ) ) ;
#10944 = DIRECTION ( 'NONE',  ( 1.000000000000000000, 0.000000000000000000, -5.463695987328529395E-16 ) ) ;
#10945 = VERTEX_POINT ( 'NONE', #48670 ) ;
#10946 = CARTESIAN_POINT ( 'NONE',  ( 101.1162363742629253, -27.35970543535582422, 61.51467289495899138 ) ) ;
#10947 = CARTESIAN_POINT ( 'NONE',  ( 75.26949937496598864, -71.54137415153812185, 361.9756252759101471 ) ) ;
#10948 = VECTOR ( 'NONE', #26981, 1000.000000000000000 ) ;
#10949 = ORIENTED_EDGE ( 'NONE', *, *, #37347, .T. ) ;
#10950 = ORIENTED_EDGE ( 'NONE', *, *, #36413, .T. ) ;
#10951 = VERTEX_POINT ( 'NONE', #15533 ) ;
#10952 = CARTESIAN_POINT ( 'NONE',  ( 82.27770840671846031, -17.08426318373788177, 2.472582314378777291 ) ) ;
#10953 = DIRECTION ( 'NONE',  ( -0.7071067811865171526, -0.7071067811865779928, -7.071067811865164719E-16 ) ) ;
#10954 = LINE ( 'NONE', #88624, #53774 ) ;
#10955 = CARTESIAN_POINT ( 'NONE',  ( 103.6457284375485131, -44.67924975648479347, 135.0833284648299752 ) ) ;
#10956 = CARTESIAN_POINT ( 'NONE',  ( 100.7369725318012570, -45.81913908486538389, 233.0803871806729717 ) ) ;
#10957 = CARTESIAN_POINT ( 'NONE',  ( 134.0664832912739826, -15.97944715994100306, 1.625625275910997480 ) ) ;
#10958 = ORIENTED_EDGE ( 'NONE', *, *, #84275, .T. ) ;
#10959 = ADVANCED_FACE ( 'NONE', ( #70041 ), #42307, .F. ) ;
#10960 = CARTESIAN_POINT ( 'NONE',  ( 135.3099588812963816, -39.18301917769485954, 1.868341932363548619 ) ) ;
#10961 = ORIENTED_EDGE ( 'NONE', *, *, #79037, .F. ) ;
#10962 = VERTEX_POINT ( 'NONE', #28702 ) ;
#10963 = AXIS2_PLACEMENT_3D ( 'NONE', #7900, #15627, #2441 ) ;
#10964 = PLANE ( 'NONE',  #48771 ) ;
#10965 = VECTOR ( 'NONE', #17412, 1000.000000000000000 ) ;
#10966 = VERTEX_POINT ( 'NONE', #8722 ) ;
#10967 = EDGE_LOOP ( 'NONE', ( #87494, #40712, #87038, #72397 ) ) ;
#10968 = DIRECTION ( 'NONE',  ( 0.0001713722455994998422, -0.9999999853157766072, 0.000000000000000000 ) ) ;
#10969 = CARTESIAN_POINT ( 'NONE',  ( 80.06648329127402519, -46.72944715994105991, 8.225625275910942946 ) ) ;
#10970 = AXIS2_PLACEMENT_3D ( 'NONE', #54499, #21823, #41331 ) ;
#10971 = CARTESIAN_POINT ( 'NONE',  ( 104.4882254922823819, -26.97928299422803278, 25.28160027219495021 ) ) ;
#10972 = CARTESIAN_POINT ( 'NONE',  ( 115.2241057928380599, -39.35723584706951783, 158.0009912566479500 ) ) ;
#10973 = CARTESIAN_POINT ( 'NONE',  ( 100.5231322539815153, -27.76298515809465073, 30.56610146638794134 ) ) ;
#10974 = VERTEX_POINT ( 'NONE', #42752 ) ;
#10975 = CARTESIAN_POINT ( 'NONE',  ( -90.13186587200952715, 73.86197090048101188, -77.01855645442566356 ) ) ;
#10976 = VERTEX_POINT ( 'NONE', #35053 ) ;
#10977 = AXIS2_PLACEMENT_3D ( 'NONE', #69240, #67434, #53331 ) ;
#10978 = EDGE_CURVE ( 'NONE', #6676, #53380, #28238, .T. ) ;
#10979 = DIRECTION ( 'NONE',  ( 0.000000000000000000, 0.000000000000000000, -1.000000000000000000 ) ) ;
#10980 = ORIENTED_EDGE ( 'NONE', *, *, #73804, .T. ) ;
#10981 = CARTESIAN_POINT ( 'NONE',  ( 97.29212427557061460, -38.88438501596571939, 167.4992703951793089 ) ) ;
#10982 = CARTESIAN_POINT ( 'NONE',  ( 188.5667039024479834, -67.87844715994100397, 132.3428068554150343 ) ) ;
#10983 = CARTESIAN_POINT ( 'NONE',  ( 97.81362146037459127, -40.52214467932135022, 131.6360307733190211 ) ) ;
#10984 = CIRCLE ( 'NONE', #21120, 9.524999999999998579 ) ;
#10985 = EDGE_CURVE ( 'NONE', #24816, #41305, #63510, .T. ) ;
#10986 = FACE_BOUND ( 'NONE', #27944, .T. ) ;
#10987 = ORIENTED_EDGE ( 'NONE', *, *, #22142, .T. ) ;
#10988 = CARTESIAN_POINT ( 'NONE',  ( 95.23402374720009789, -35.71607800568281021, 36.25848241876794731 ) ) ;
#10989 = CARTESIAN_POINT ( 'NONE',  ( 118.2550939253582811, -40.78236016348033388, 19.54991099019698453 ) ) ;
#10990 =( NAMED_UNIT ( * ) PLANE_ANGLE_UNIT ( ) SI_UNIT ( $, .RADIAN. ) );
#10991 = AXIS2_PLACEMENT_3D ( 'NONE', #57252, #15946, #78639 ) ;
#10993 = DIRECTION ( 'NONE',  ( 1.000000000000000078E-15, 1.000000000000000083E-30, -1.000000000000000000 ) ) ;
#10992 = CARTESIAN_POINT ( 'NONE',  ( -479.3614999999999782, 21.43125000000029701, 15.23694598552314972 ) ) ;
#10994 = LINE ( 'NONE', #30557, #45249 ) ;
#10995 = DIRECTION ( 'NONE',  ( 0.7071067811566161820, 0.7071067812164789634, 0.000000000000000000 ) ) ;
#10996 = CARTESIAN_POINT ( 'NONE',  ( 132.9421938897440896, -39.23922437001930774, 8.028287874532662016 ) ) ;
#10997 = CARTESIAN_POINT ( 'NONE',  ( 25.56670390244797275, -58.35344715994099829, 259.9678068554150059 ) ) ;
#10998 = CARTESIAN_POINT ( 'NONE',  ( 145.4469796106781416, -124.3929973698032114, 247.5412109164290086 ) ) ;
#10999 = CARTESIAN_POINT ( 'NONE',  ( 100.4512773062034370, -27.81586575833916442, 35.59657765686397113 ) ) ;
#11000 = CARTESIAN_POINT ( 'NONE',  ( 116.3502490628398647, -44.09465650233049416, 194.2927681330539542 ) ) ;
#11001 = CARTESIAN_POINT ( 'NONE',  ( 115.6911227382933873, -43.67932486773085543, 39.27467289495895386 ) ) ;
#11003 = CARTESIAN_POINT ( 'NONE',  ( 196.2150000000000034, 37.33800000000000097, 41.27499999999999858 ) ) ;
#11002 = DIRECTION ( 'NONE',  ( 0.000000000000000000, 0.000000000000000000, 1.000000000000000000 ) ) ;
#11004 = CARTESIAN_POINT ( 'NONE',  ( 81.70522810117023482, -34.51875982968658718, 2.060081176875012243 ) ) ;
#11005 = AXIS2_PLACEMENT_3D ( 'NONE', #33413, #73849, #11636 ) ;
#11006 = EDGE_LOOP ( 'NONE', ( #34465, #44985 ) ) ;
#11007 = EDGE_CURVE ( 'NONE', #22788, #75220, #48961, .T. ) ;
#11008 = CARTESIAN_POINT ( 'NONE',  ( 138.0667039024480403, -58.72944715994091069, 239.5838068554170377 ) ) ;
#11009 = EDGE_LOOP ( 'NONE', ( #52588, #8554, #45030, #4244, #36247, #45912, #83324, #73113, #13509, #5033, #77672, #72489, #16612, #35301 ) ) ;
#11010 = EDGE_CURVE ( 'NONE', #80032, #68275, #22344, .T. ) ;
#11011 = CARTESIAN_POINT ( 'NONE',  ( 113.5587197313313936, -28.64306037466259625, 115.5261014663869474 ) ) ;
#11013 = VERTEX_POINT ( 'NONE', #77302 ) ;
#11012 = CARTESIAN_POINT ( 'NONE',  ( 10.54993534173505054, 89.62028068362222655, 130.1290436628989653 ) ) ;
#11014 = FACE_BOUND ( 'NONE', #2325, .T. ) ;
#11015 = EDGE_CURVE ( 'NONE', #50715, #19682, #62005, .T. ) ;
#11016 = CARTESIAN_POINT ( 'NONE',  ( 115.2346088729119629, -30.22974330756305505, 240.3613395616249875 ) ) ;
#11017 = DIRECTION ( 'NONE',  ( 1.000000000000000078E-15, -1.000000000000000083E-30, -1.000000000000000000 ) ) ;
#11018 = DIRECTION ( 'NONE',  ( 1.000000000000000000, 0.000000000000000000, 0.000000000000000000 ) ) ;
#11019 = DIRECTION ( 'NONE',  ( 1.000000000000000078E-15, 1.000000000000000083E-30, -1.000000000000000000 ) ) ;
#11020 = CARTESIAN_POINT ( 'NONE',  ( 51.06648329127400388, -18.82844715994099971, 330.8831252759119934 ) ) ;
#11021 = DIRECTION ( 'NONE',  ( 0.000000000000000000, 0.000000000000000000, -1.000000000000000000 ) ) ;
#11022 = EDGE_CURVE ( 'NONE', #52329, #79853, #56836, .T. ) ;
#11023 = CARTESIAN_POINT ( 'NONE',  ( -83.15068351451286333, 79.66695435136418268, 100.6520717229721527 ) ) ;
#11024 = VECTOR ( 'NONE', #55391, 1000.000000000000000 ) ;
#11025 = CARTESIAN_POINT ( 'NONE',  ( 113.1634500054122583, -44.41975088505045477, 168.1099109901969939 ) ) ;
#11026 = ORIENTED_EDGE ( 'NONE', *, *, #63567, .F. ) ;
#11027 = VERTEX_POINT ( 'NONE', #50019 ) ;
#11028 = AXIS2_PLACEMENT_3D ( 'NONE', #26135, #4349, #25225 ) ;
#11029 = CARTESIAN_POINT ( 'NONE',  ( 115.2337707449818680, -33.21411712777100433, 75.58158330589692753 ) ) ;
#11030 = EDGE_CURVE ( 'NONE', #79712, #48254, #64124, .T. ) ;
#11031 = VECTOR ( 'NONE', #51852, 1000.000000000000000 ) ;
#11032 = LINE ( 'NONE', #52334, #45761 ) ;
#11033 = AXIS2_PLACEMENT_3D ( 'NONE', #48667, #83225, #89591 ) ;
#11035 = DIRECTION ( 'NONE',  ( -4.237773401492740281E-14, 1.000000000000000000, 0.000000000000000000 ) ) ;
#11034 = CARTESIAN_POINT ( 'NONE',  ( 117.9377692877171313, -39.05906590213764673, 254.6584824187675338 ) ) ;
#11036 = VECTOR ( 'NONE', #81006, 1000.000000000000000 ) ;
#11037 = DIRECTION ( 'NONE',  ( 0.7071067811865573427, -0.7071067811865376918, 1.287852911526298168E-16 ) ) ;
#11038 = FACE_OUTER_BOUND ( 'NONE', #57099, .T. ) ;
#11039 = ADVANCED_FACE ( 'NONE', ( #43207 ), #63220, .F. ) ;
#11040 = CARTESIAN_POINT ( 'NONE',  ( 118.5214188546241161, 70.17671898886891313, 2.891923471344727492 ) ) ;
#11041 = CARTESIAN_POINT ( 'NONE',  ( 1.387778780781445676E-14, 239.0000000000000000, 90.07542076772557493 ) ) ;
#11042 = DIRECTION ( 'NONE',  ( -1.000000000000000000, 0.000000000000000000, 0.000000000000000000 ) ) ;
#11043 = DIRECTION ( 'NONE',  ( 0.000000000000000000, 0.000000000000000000, -1.000000000000000000 ) ) ;
#11044 = CARTESIAN_POINT ( 'NONE',  ( 96.03721982003239077, -36.58408020053186505, 156.3280062282919687 ) ) ;
#11045 = ORIENTED_EDGE ( 'NONE', *, *, #87356, .F. ) ;
#11046 = ORIENTED_EDGE ( 'NONE', *, *, #42431, .T. ) ;
#11047 = LINE ( 'NONE', #31935, #54636 ) ;
#11048 = CARTESIAN_POINT ( 'NONE',  ( 105.7995185470425952, -26.72403495915586547, 151.1772919378495317 ) ) ;
#11049 = PLANE ( 'NONE',  #42120 ) ;
#11050 = CARTESIAN_POINT ( 'NONE',  ( 117.9332873271178102, -93.05227202534730679, -21.78219314458237932 ) ) ;
#11051 = VERTEX_POINT ( 'NONE', #9161 ) ;
#11052 = CARTESIAN_POINT ( 'NONE',  ( 160.7738106836383167, -48.62134037874550785, 300.4678068554149490 ) ) ;
#11053 = CIRCLE ( 'NONE', #38612, 3.299999999999997158 ) ;
#11054 = CARTESIAN_POINT ( 'NONE',  ( 98.26116833961376074, -42.31097554054522902, 186.7756252759109543 ) ) ;
#11055 = CARTESIAN_POINT ( 'NONE',  ( 135.5597725514587069, -39.04085022828070350, 7.869587501215970171 ) ) ;
#11056 = ORIENTED_EDGE ( 'NONE', *, *, #9284, .T. ) ;
#11058 = ORIENTED_EDGE ( 'NONE', *, *, #12443, .F. ) ;
#11057 = EDGE_LOOP ( 'NONE', ( #61723, #24419, #34680, #36827 ) ) ;
#11059 = CARTESIAN_POINT ( 'NONE',  ( -10.79070278320184073, 75.83992121942911524, 118.0641357957730264 ) ) ;
#11060 = FACE_OUTER_BOUND ( 'NONE', #54415, .T. ) ;
#11061 = CARTESIAN_POINT ( 'NONE',  ( 97.81285236004582373, -40.52026819599429786, 166.6358693223811542 ) ) ;
#11062 = CARTESIAN_POINT ( 'NONE',  ( 111.5696292435227122, -29.33873666780462486, 47.44713798863897836 ) ) ;
#11063 = DIRECTION ( 'NONE',  ( 0.000000000000000000, 0.000000000000000000, -1.000000000000000000 ) ) ;
#11064 = VERTEX_POINT ( 'NONE', #1896 ) ;
#11065 = EDGE_CURVE ( 'NONE', #5327, #1305, #55578, .T. ) ;
#11066 = DIRECTION ( 'NONE',  ( -0.08901729878539284269, 0.06045726171402947963, 0.9941935626541712478 ) ) ;
#11067 = CARTESIAN_POINT ( 'NONE',  ( -47.02966122971777452, 101.5999999999999943, 107.7386843274874053 ) ) ;
#11068 = ORIENTED_EDGE ( 'NONE', *, *, #5716, .T. ) ;
#11069 = ORIENTED_EDGE ( 'NONE', *, *, #1302, .T. ) ;
#11070 = CARTESIAN_POINT ( 'NONE',  ( -0.8023776826656670025, 65.59999999999998010, -4.197052493943455254 ) ) ;
#11071 = VERTEX_POINT ( 'NONE', #24128 ) ;
#11072 = ORIENTED_EDGE ( 'NONE', *, *, #31459, .T. ) ;
#11073 = FACE_OUTER_BOUND ( 'NONE', #82463, .T. ) ;
#11074 = CARTESIAN_POINT ( 'NONE',  ( 116.0925701722734686, -37.46594287791281630, 38.19622935188693447 ) ) ;
#11075 = CARTESIAN_POINT ( 'NONE',  ( 107.5668325082694139, -47.79493819276859057, 192.6003871806729535 ) ) ;
#11076 = CARTESIAN_POINT ( 'NONE',  ( 95.59354794629800267, -39.59649474372138656, 166.5213395616259788 ) ) ;
#11077 = DIRECTION ( 'NONE',  ( 0.7071067811866279529, -0.7071067811864671926, 7.071067811866286874E-16 ) ) ;
#11078 = CARTESIAN_POINT ( 'NONE',  ( 100.1775528843425178, -45.37332466565996469, 268.0289586092443415 ) ) ;
#11079 = LINE ( 'NONE', #38785, #66620 ) ;
#11080 = DIRECTION ( 'NONE',  ( 0.9961946980917455452, 0.000000000000000000, 0.08715574274765836016 ) ) ;
#11081 = ORIENTED_EDGE ( 'NONE', *, *, #20034, .F. ) ;
#11082 = ORIENTED_EDGE ( 'NONE', *, *, #71720, .F. ) ;
#11083 = AXIS2_PLACEMENT_3D ( 'NONE', #39442, #80347, #54378 ) ;
#11084 = AXIS2_PLACEMENT_3D ( 'NONE', #17317, #77758, #37762 ) ;
#11085 = ADVANCED_FACE ( 'NONE', ( #64567 ), #79997, .T. ) ;
#11086 = CARTESIAN_POINT ( 'NONE',  ( -479.3614999999999782, 93.66249999999999432, 82.23860802895320887 ) ) ;
#11088 = CARTESIAN_POINT ( 'NONE',  ( 111.1446672340677111, -27.08708843538706645, 244.7584824187679544 ) ) ;
#11087 = CIRCLE ( 'NONE', #18348, 17.00000000000000000 ) ;
#11089 = ORIENTED_EDGE ( 'NONE', *, *, #15170, .F. ) ;
#11090 = PRESENTATION_LAYER_ASSIGNMENT (  '', '', ( #83612 ) ) ;
#11091 = CARTESIAN_POINT ( 'NONE',  ( 99.28842769779902255, -29.78762595464951346, 190.7470538473399415 ) ) ;
#11092 = DIRECTION ( 'NONE',  ( 0.000000000000000000, -1.000000000000000000, 0.000000000000000000 ) ) ;
#11093 = FACE_BOUND ( 'NONE', #47070, .T. ) ;
#11094 = DIRECTION ( 'NONE',  ( 0.000000000000000000, 0.000000000000000000, 1.000000000000000000 ) ) ;
#11095 = CARTESIAN_POINT ( 'NONE',  ( 183.5150000000000148, 21.46300000000000097, 41.63456447661474868 ) ) ;
#11098 = CARTESIAN_POINT ( 'NONE',  ( 118.3173389373706925, -33.08695204176930105, 280.0756252759109657 ) ) ;
#11097 = CARTESIAN_POINT ( 'NONE',  ( 51.06648329127330044, -0.7548456658612000547, 333.4006252759120343 ) ) ;
#11096 = CARTESIAN_POINT ( 'NONE',  ( 106.1656040943334318, -87.30234574837481887, -21.78219314458254630 ) ) ;
#11099 = CARTESIAN_POINT ( 'NONE',  ( 77.39114642429899504, 120.6499999999999915, 71.77848634863160271 ) ) ;
#11100 = CARTESIAN_POINT ( 'NONE',  ( 107.0664832912739399, -36.72944715994095333, 299.5571190294419921 ) ) ;
#11101 = DIRECTION ( 'NONE',  ( 1.000000000000000078E-15, -1.000000000000000083E-30, -1.000000000000000000 ) ) ;
#11102 = CARTESIAN_POINT ( 'NONE',  ( 67.63716323619298976, -137.3564796873130263, 246.9094381074559408 ) ) ;
#11103 = LINE ( 'NONE', #4305, #16946 ) ;
#11104 = CARTESIAN_POINT ( 'NONE',  ( 152.0371591254583450, -47.82818131005588214, 249.9678068554149490 ) ) ;
#11106 = ORIENTED_EDGE ( 'NONE', *, *, #83522, .F. ) ;
#11105 = CARTESIAN_POINT ( 'NONE',  ( 1.451892247740217613E-14, 95.25000000000000000, -118.5560000000000116 ) ) ;
#11107 = CARTESIAN_POINT ( 'NONE',  ( 182.4202572930266228, -31.94127993907054730, 237.4678068554150059 ) ) ;
#11108 = CARTESIAN_POINT ( 'NONE',  ( 113.6996774752161201, -45.60053368046675359, 188.0994347997199725 ) ) ;
#11109 = CARTESIAN_POINT ( 'NONE',  ( 98.45872715028987443, -30.84820395253375125, 116.8499109901969604 ) ) ;
#11110 = CARTESIAN_POINT ( 'NONE',  ( 116.0926836276447460, -42.03234139191665975, 234.4041967044819899 ) ) ;
#11111 = DIRECTION ( 'NONE',  ( 1.000000000000000078E-15, -1.000000000000000083E-30, -1.000000000000000000 ) ) ;
#11112 = CARTESIAN_POINT ( 'NONE',  ( 188.5667039024485518, -48.82844715993430640, 175.7178068554150343 ) ) ;
#11113 = VECTOR ( 'NONE', #47364, 1000.000000000000114 ) ;
#11115 = CARTESIAN_POINT ( 'NONE',  ( 97.81748826816456699, -40.53157710480042653, 37.63655137377492110 ) ) ;
#11114 = DIRECTION ( 'NONE',  ( 4.299999999999999979E-14, -1.000000000000000000, 0.000000000000000000 ) ) ;
#11116 = LINE ( 'NONE', #65640, #8814 ) ;
#11117 = DIRECTION ( 'NONE',  ( 1.000000000000000000, 0.000000000000000000, 0.000000000000000000 ) ) ;
#11118 = CARTESIAN_POINT ( 'NONE',  ( 76.20505178924389611, 127.0000000000000000, -76.20505178924359768 ) ) ;
#11119 = CLOSED_SHELL ( 'NONE', ( #60929, #9449, #21616, #44974 ) ) ;
#11120 = VERTEX_POINT ( 'NONE', #30049 ) ;
#11121 = ORIENTED_EDGE ( 'NONE', *, *, #64702, .T. ) ;
#11122 = EDGE_CURVE ( 'NONE', #48508, #49976, #57743, .T. ) ;
#11123 = CARTESIAN_POINT ( 'NONE',  ( 99.76075522406560481, -42.08098971643298825, 106.2400388756959728 ) ) ;
#11125 = ORIENTED_EDGE ( 'NONE', *, *, #73258, .F. ) ;
#11124 = LINE ( 'NONE', #58823, #86486 ) ;
#11126 = ADVANCED_FACE ( 'NONE', ( #38193 ), #45429, .F. ) ;
#11127 = CARTESIAN_POINT ( 'NONE',  ( 108.7397100058831256, -25.82697924850577920, 140.9432443235299672 ) ) ;
#11128 = CARTESIAN_POINT ( 'NONE',  ( -215.9000000000000057, 101.5999999999999943, 146.9389999999999930 ) ) ;
#11129 = EDGE_CURVE ( 'NONE', #1886, #21233, #9835, .T. ) ;
#11130 = CARTESIAN_POINT ( 'NONE',  ( 79.69020591995840164, -15.99866847873249931, 8.209451181318300428 ) ) ;
#11131 = CARTESIAN_POINT ( 'NONE',  ( -487.2989999999999782, 97.78694598552380057, 3.968750000000479616 ) ) ;
#11132 = EDGE_CURVE ( 'NONE', #81323, #86805, #47541, .T. ) ;
#11133 = CARTESIAN_POINT ( 'NONE',  ( 44.45000000000000284, 69.84999999999999432, 219.0749999999999886 ) ) ;
#11134 = CARTESIAN_POINT ( 'NONE',  ( 98.20607846729126322, -32.50961293922092210, 75.97276813305397525 ) ) ;
#11135 = ORIENTED_EDGE ( 'NONE', *, *, #64461, .T. ) ;
#11136 = ORIENTED_EDGE ( 'NONE', *, *, #13699, .T. ) ;
#11138 = ORIENTED_EDGE ( 'NONE', *, *, #185, .T. ) ;
#11137 = VECTOR ( 'NONE', #46277, 1000.000000000000114 ) ;
#11139 = FACE_OUTER_BOUND ( 'NONE', #63943, .T. ) ;
#11141 = DIRECTION ( 'NONE',  ( -3.100000000000000258E-29, 3.100000000000000044E-14, 1.000000000000000000 ) ) ;
#11140 = CARTESIAN_POINT ( 'NONE',  ( 98.75024281215311817, -42.92452016420547523, 107.8480062282919647 ) ) ;
#11142 = FACE_OUTER_BOUND ( 'NONE', #31045, .T. ) ;
#11143 = CARTESIAN_POINT ( 'NONE',  ( 116.3212776292294421, -32.94146857471278622, 70.13562527591093954 ) ) ;
#11144 = EDGE_CURVE ( 'NONE', #1770, #41877, #44991, .T. ) ;
#11145 = DIRECTION ( 'NONE',  ( 1.000000000000000078E-15, -1.000000000000000083E-30, -1.000000000000000000 ) ) ;
#11146 = CARTESIAN_POINT ( 'NONE',  ( 79.76258624986769519, 93.94553785444269067, 87.71311422381614875 ) ) ;
#11147 = CARTESIAN_POINT ( 'NONE',  ( 7.760385678595139561E-15, 60.82030000000000314, 222.5849787991094786 ) ) ;
#11148 = CARTESIAN_POINT ( 'NONE',  ( 112.8057071037347754, -27.31004523576145360, 49.62895860924498947 ) ) ;
#11149 = EDGE_LOOP ( 'NONE', ( #60096, #84479 ) ) ;
#11150 = ORIENTED_EDGE ( 'NONE', *, *, #54100, .T. ) ;
#11151 = CYLINDRICAL_SURFACE ( 'NONE', #18351, 24.50000000000000711 ) ;
#11152 = LINE ( 'NONE', #52023, #89639 ) ;
#11153 = VECTOR ( 'NONE', #16238, 1000.000000000000000 ) ;
#11154 = CARTESIAN_POINT ( 'NONE',  ( 241.3336515812914911, 65.43750000000000000, -2.032000000000000028 ) ) ;
#11155 = CARTESIAN_POINT ( 'NONE',  ( 115.0870346033256055, -35.21269407640084381, 156.7938046553059905 ) ) ;
#11156 = AXIS2_PLACEMENT_3D ( 'NONE', #54648, #60587, #13356 ) ;
#11157 = AXIS2_PLACEMENT_3D ( 'NONE', #75968, #60072, #27363 ) ;
#11158 = VECTOR ( 'NONE', #9841, 1000.000000000000000 ) ;
#11159 = CARTESIAN_POINT ( 'NONE',  ( 99.03451269431033666, -100.2184096729307470, 2.217806855417864043 ) ) ;
#11160 = ORIENTED_EDGE ( 'NONE', *, *, #24837, .F. ) ;
#11161 = ORIENTED_EDGE ( 'NONE', *, *, #81296, .F. ) ;
#11162 = CARTESIAN_POINT ( 'NONE',  ( -487.2989999999999782, 89.53805401447691281, 18.25625000000039933 ) ) ;
#11163 = ORIENTED_EDGE ( 'NONE', *, *, #925, .F. ) ;
#11164 = PRODUCT ( 'Rotary Table Drive Mechanism', 'Rotary Table Drive Mechanism', '', ( #74016 ) ) ;
#11165 = EDGE_LOOP ( 'NONE', ( #43808, #49860, #50879, #56493, #74952, #52267, #43683, #43081, #52460, #67556, #60658, #86519, #81909 ) ) ;
#11166 = DIRECTION ( 'NONE',  ( 0.000000000000000000, 0.000000000000000000, -1.000000000000000000 ) ) ;
#11167 = CARTESIAN_POINT ( 'NONE',  ( 111.9232213988593827, -44.14162454355680865, 174.4701547344689629 ) ) ;
#11168 = DIRECTION ( 'NONE',  ( -0.7071067811855830110, -0.7071067811875120235, 0.000000000000000000 ) ) ;
#11169 = AXIS2_PLACEMENT_3D ( 'NONE', #51579, #65665, #45209 ) ;
#11170 = CIRCLE ( 'NONE', #76482, 1.000000000000000888 ) ;
#11171 = EDGE_CURVE ( 'NONE', #78707, #44910, #80434, .T. ) ;
#11172 = CARTESIAN_POINT ( 'NONE',  ( 95.60734603896362671, -36.72944715994100306, 311.6356252759112522 ) ) ;
#11173 = CARTESIAN_POINT ( 'NONE',  ( -111.0232030825078624, 64.26406744673955984, 68.69319255069000008 ) ) ;
#11174 = ORIENTED_EDGE ( 'NONE', *, *, #9495, .F. ) ;
#11175 = ORIENTED_EDGE ( 'NONE', *, *, #50407, .F. ) ;
#11176 = AXIS2_PLACEMENT_3D ( 'NONE', #41131, #56560, #69756 ) ;
#11177 = EDGE_LOOP ( 'NONE', ( #41145, #78809, #77255, #62677 ) ) ;
#11178 = VERTEX_POINT ( 'NONE', #3675 ) ;
#11179 = EDGE_CURVE ( 'NONE', #18758, #15646, #57670, .T. ) ;
#11180 = CARTESIAN_POINT ( 'NONE',  ( 113.5820732635001491, -31.81245485458596889, 217.1595189410199396 ) ) ;
#11181 = CARTESIAN_POINT ( 'NONE',  ( 108.3221154657901337, -47.10103102204929826, 117.6727681330539639 ) ) ;
#11182 = CARTESIAN_POINT ( 'NONE',  ( 115.1902516771093445, -44.19056033372790893, 78.22324432352995416 ) ) ;
#11183 = CARTESIAN_POINT ( 'NONE',  ( 34.33598329127499227, -36.32844715994100682, 342.9256252759119548 ) ) ;
#11184 = PLANE ( 'NONE',  #10365 ) ;
#11185 = LINE ( 'NONE', #17566, #47519 ) ;
#11186 = CARTESIAN_POINT ( 'NONE',  ( 107.9182609186041333, -47.15517531916538019, 173.6413395616249886 ) ) ;
#11187 = CARTESIAN_POINT ( 'NONE',  ( -72.96458098368751166, 127.0000000000000000, 72.96458098368620426 ) ) ;
#11188 = ORIENTED_EDGE ( 'NONE', *, *, #25908, .T. ) ;
#11189 = CARTESIAN_POINT ( 'NONE',  ( 173.8164832912729878, 12.92155284005802862, 355.9756252759109998 ) ) ;
#11190 = VERTEX_POINT ( 'NONE', #18190 ) ;
#11191 = ORIENTED_EDGE ( 'NONE', *, *, #59367, .T. ) ;
#11192 = CARTESIAN_POINT ( 'NONE',  ( 147.0667039024469886, -67.87844715994090450, 222.2178068554179902 ) ) ;
#11193 = VERTEX_POINT ( 'NONE', #85923 ) ;
#11194 = AXIS2_PLACEMENT_3D ( 'NONE', #75307, #59860, #61218 ) ;
#11195 = VERTEX_POINT ( 'NONE', #4117 ) ;
#11196 = B_SPLINE_CURVE_WITH_KNOTS ( 'NONE', 3,
 ( #58504, #45314, #81222, #52560, #67115, #24452, #38506, #74387, #4451, #65762, #52116, #66207, #53454, #3549, #81668, #74835, #46198, #38955, #60735, #60288, #45747, #26228, #3997, #53906, #31244, #5347, #58943, #86681, #24894, #19418, #18970, #59393, #47099, #12160, #79881, #59838, #73934, #38074, #25328, #18065, #11715, #80319, #17634, #73030, #87568, #39408, #10801, #39847, #31697 ),
 .UNSPECIFIED., .F., .F.,
 ( 4, 2, 2, 2, 2, 2, 2, 2, 2, 2, 2, 2, 2, 2, 2, 1, 2, 2, 2, 2, 2, 2, 2, 2, 4 ),
 ( 0.01987186023414422298, 0.02111356671950568101, 0.02235527320486713557, 0.02483868617559004816, 0.02608039266095152353, 0.02732209914631299891, 0.02980551211703595313, 0.03228892508775890735, 0.03353063157312036885, 0.03477233805848183035, 0.03725575102920476722, 0.03849745751456623566, 0.03973916399992770410, 0.04222257697065064097, 0.04346428345601210247, 0.04470598994137356397, 0.04594769642673503240, 0.04718940291209650084, 0.04967281588281945159, 0.05091452236818090615, 0.05215622885354237459, 0.05463964182426532534, 0.05588134830962680072, 0.05712305479498827609, 0.05960646776571126848 ),
 .UNSPECIFIED. ) ;
#11197 = AXIS2_PLACEMENT_3D ( 'NONE', #8456, #29351, #50667 ) ;
#11198 = CARTESIAN_POINT ( 'NONE',  ( 107.0664832912750057, -36.72944715993903486, 0.7256252759109708128 ) ) ;
#11199 = ADVANCED_FACE ( 'NONE', ( #31815, #59510 ), #87245, .T. ) ;
#11200 = ORIENTED_EDGE ( 'NONE', *, *, #1942, .F. ) ;
#11201 = DIRECTION ( 'NONE',  ( 1.000000000000000078E-15, -1.000000000000000000, 0.000000000000000000 ) ) ;
#11202 = CARTESIAN_POINT ( 'NONE',  ( 117.9248307134361937, -41.47673871369620002, 58.49848241876792798 ) ) ;
#11203 = DIRECTION ( 'NONE',  ( -1.000000000000000000, 0.000000000000000000, -1.424786214935630051E-15 ) ) ;
#11204 = DIRECTION ( 'NONE',  ( 0.9963424814100678706, -0.08544974978095865037, 0.000000000000000000 ) ) ;
#11205 = DIRECTION ( 'NONE',  ( 0.000000000000000000, -1.000000000000000000, 0.000000000000000000 ) ) ;
#11206 = CARTESIAN_POINT ( 'NONE',  ( 116.8058161338298504, -37.62879752186918836, 78.75276813305399060 ) ) ;
#11208 = CARTESIAN_POINT ( 'NONE',  ( 117.9257662994439499, -34.79559216868042171, 194.9546728949589749 ) ) ;
#11207 = CARTESIAN_POINT ( 'NONE',  ( -3.968749999999935163, 127.0000000000000000, -100.8961411191535973 ) ) ;
#11209 = FACE_OUTER_BOUND ( 'NONE', #35306, .T. ) ;
#11210 = FACE_OUTER_BOUND ( 'NONE', #27148, .T. ) ;
#11211 = VERTEX_POINT ( 'NONE', #23694 ) ;
#11212 = CARTESIAN_POINT ( 'NONE',  ( 184.3595971212630502, -48.62134037874749026, 180.4678068554150343 ) ) ;
#11213 = LINE ( 'NONE', #52079, #61641 ) ;
#11214 = CARTESIAN_POINT ( 'NONE',  ( 143.0667039024470455, -124.7784471599409102, 55.21780685541800437 ) ) ;
#11215 = EDGE_CURVE ( 'NONE', #76329, #50184, #45870, .T. ) ;
#11216 = CARTESIAN_POINT ( 'NONE',  ( 142.8682495647594521, 8.654319075478468903, 394.9756252759102040 ) ) ;
#11218 = ORIENTED_EDGE ( 'NONE', *, *, #66795, .F. ) ;
#11217 = CARTESIAN_POINT ( 'NONE',  ( 110.1504846022309607, -26.06634163003500859, 214.8403871806729342 ) ) ;
#11219 = DIRECTION ( 'NONE',  ( -3.100000000000000258E-29, 3.100000000000000044E-14, 1.000000000000000000 ) ) ;
#11220 = CARTESIAN_POINT ( 'NONE',  ( 110.2841144599940577, -46.64559811412390644, 8.827053847339950465 ) ) ;
#11221 = CARTESIAN_POINT ( 'NONE',  ( 117.2057360052074415, -34.12396560160815540, 120.0270538473389479 ) ) ;
#11222 = AXIS2_PLACEMENT_3D ( 'NONE', #59771, #3049, #60214 ) ;
#11223 = CARTESIAN_POINT ( 'NONE',  ( 182.5667039024476139, -32.29483332967956954, 313.9678068554149490 ) ) ;
#11224 = CARTESIAN_POINT ( 'NONE',  ( 81.91398979882924891, -38.77444411305296512, 7.664507283848216446 ) ) ;
#11225 = DIRECTION ( 'NONE',  ( 0.8861241255175467124, 0.000000000000000000, -0.4634479843259253218 ) ) ;
#11226 = LINE ( 'NONE', #46175, #40878 ) ;
#11227 = ORIENTED_EDGE ( 'NONE', *, *, #74092, .T. ) ;
#11228 = CIRCLE ( 'NONE', #64865, 5.599999999999994316 ) ;
#11229 = VECTOR ( 'NONE', #22249, 1000.000000000000000 ) ;
#11230 = CIRCLE ( 'NONE', #37304, 9.500000000000008882 ) ;
#11231 = EDGE_LOOP ( 'NONE', ( #18068, #22637 ) ) ;
#11232 = VERTEX_POINT ( 'NONE', #11381 ) ;
#11233 = VERTEX_POINT ( 'NONE', #2346 ) ;
#11234 = DIRECTION ( 'NONE',  ( 0.000000000000000000, 1.000000000000000000, 0.000000000000000000 ) ) ;
#11235 = CARTESIAN_POINT ( 'NONE',  ( 100.0240874364964299, -28.99487838171179632, 281.6641967044822650 ) ) ;
#11236 = DIRECTION ( 'NONE',  ( 0.000000000000000000, 1.000000000000000000, 0.000000000000000000 ) ) ;
#11237 = CARTESIAN_POINT ( 'NONE',  ( 144.0665648704335808, -140.6784485900456900, 245.9352930260599805 ) ) ;
#11238 = ADVANCED_FACE ( 'NONE', ( #85481 ), #72280, .F. ) ;
#11239 = VECTOR ( 'NONE', #58018, 1000.000000000000000 ) ;
#11240 = AXIS2_PLACEMENT_3D ( 'NONE', #68589, #75405, #26789 ) ;
#11242 = CARTESIAN_POINT ( 'NONE',  ( 80.06648329127399677, -8.729447159940999512, 293.6356252759119911 ) ) ;
#11241 = LINE ( 'NONE', #38943, #77270 ) ;
#11243 = AXIS2_PLACEMENT_3D ( 'NONE', #14908, #57561, #42571 ) ;
#11244 = CARTESIAN_POINT ( 'NONE',  ( 110.0404421551223209, -45.97207645956791566, 207.2467055423619513 ) ) ;
#11245 = ORIENTED_EDGE ( 'NONE', *, *, #20264, .T. ) ;
#11246 = ORIENTED_EDGE ( 'NONE', *, *, #42075, .F. ) ;
#11247 = ORIENTED_EDGE ( 'NONE', *, *, #9808, .F. ) ;
#11248 = VECTOR ( 'NONE', #80317, 1000.000000000000114 ) ;
#11249 = CYLINDRICAL_SURFACE ( 'NONE', #48480, 2.750000000000002665 ) ;
#11250 = CARTESIAN_POINT ( 'NONE',  ( 97.92338638096642001, -40.78105084111301437, 181.6584144844725870 ) ) ;
#11251 = CARTESIAN_POINT ( 'NONE',  ( 69.56670390244701707, -90.27844715994098124, 51.21780685541800437 ) ) ;
#11252 = CARTESIAN_POINT ( 'NONE',  ( 107.5258121372104227, -46.79223613538503912, 39.04444044875393871 ) ) ;
#11253 = PLANE ( 'NONE',  #83559 ) ;
#11254 = EDGE_CURVE ( 'NONE', #37176, #19054, #18765, .T. ) ;
#11255 = CARTESIAN_POINT ( 'NONE',  ( 57.56670390244829605, -48.82844715994039575, 290.7178068554150627 ) ) ;
#11256 = EDGE_CURVE ( 'NONE', #2257, #59978, #67687, .T. ) ;
#11257 = CARTESIAN_POINT ( 'NONE',  ( 96.02263050233423769, -38.01213896886783061, 236.4184824187689458 ) ) ;
#11258 = DIRECTION ( 'NONE',  ( -0.9254794337955620787, -0.3787978585227822492, 0.000000000000000000 ) ) ;
#11259 = ORIENTED_EDGE ( 'NONE', *, *, #68566, .T. ) ;
#11260 = CARTESIAN_POINT ( 'NONE',  ( 116.3176178399231873, -32.93748434060082531, 55.13562527591098217 ) ) ;
#11261 = VERTEX_POINT ( 'NONE', #39971 ) ;
#11262 = CIRCLE ( 'NONE', #83779, 5.599999999999994316 ) ;
#11263 = DIRECTION ( 'NONE',  ( -0.7071067811865621167, 0.000000000000000000, 0.7071067811865330288 ) ) ;
#11264 = CARTESIAN_POINT ( 'NONE',  ( 98.96120113019971143, -37.69594967233602034, 39.23951894101995919 ) ) ;
#11265 = AXIS2_PLACEMENT_3D ( 'NONE', #55404, #60897, #42236 ) ;
#11266 = CARTESIAN_POINT ( 'NONE',  ( 135.9194882200600318, -16.69035895461892949, 7.660272404628020837 ) ) ;
#11267 = LINE ( 'NONE', #26683, #5554 ) ;
#11268 = DIRECTION ( 'NONE',  ( 1.000000000000000000, 4.163336342344333240E-14, 0.000000000000000000 ) ) ;
#11269 = ORIENTED_EDGE ( 'NONE', *, *, #22738, .T. ) ;
#11270 = DIRECTION ( 'NONE',  ( 0.000000000000000000, -1.000000000000000000, -8.792068030499130893E-15 ) ) ;
#11271 = CARTESIAN_POINT ( 'NONE',  ( 120.4547041627946840, 58.04868223456158915, -50.35440352988698010 ) ) ;
#11272 = ORIENTED_EDGE ( 'NONE', *, *, #449, .F. ) ;
#11273 = CARTESIAN_POINT ( 'NONE',  ( 103.1745875910851851, -27.05783000869472588, 130.3813395616259925 ) ) ;
#11274 = ORIENTED_EDGE ( 'NONE', *, *, #34069, .T. ) ;
#11275 = CARTESIAN_POINT ( 'NONE',  ( 102.1503607674210343, -29.12389592045764530, 69.96765792331494538 ) ) ;
#11276 = CARTESIAN_POINT ( 'NONE',  ( 97.82210220655964861, -40.54279968662331157, 87.63734374981743258 ) ) ;
#11277 = CARTESIAN_POINT ( 'NONE',  ( 102.5140397859015877, -29.09155558458053292, 81.93586902018296314 ) ) ;
#11278 = DIRECTION ( 'NONE',  ( 1.424786214935630051E-15, -4.252453317207020267E-31, -1.000000000000000000 ) ) ;
#11279 = DIRECTION ( 'NONE',  ( 1.000000000000000000, -3.885780586188044357E-13, 0.000000000000000000 ) ) ;
#11280 = CARTESIAN_POINT ( 'NONE',  ( 99.12701999692106369, -43.51930588094383978, 27.88991099019694175 ) ) ;
#11281 = CARTESIAN_POINT ( 'NONE',  ( 57.14999999999999858, 69.84999999999999432, 280.2255000000000109 ) ) ;
#11282 = ORIENTED_EDGE ( 'NONE', *, *, #7022, .T. ) ;
#11283 = CARTESIAN_POINT ( 'NONE',  ( 52.38749999999999574, 94.53880000000000905, 221.4562499999999829 ) ) ;
#11284 = CIRCLE ( 'NONE', #54777, 88.90000000000000568 ) ;
#11285 = ORIENTED_EDGE ( 'NONE', *, *, #34914, .F. ) ;
#11286 = CIRCLE ( 'NONE', #62065, 34.13125000000000142 ) ;
#11287 = CARTESIAN_POINT ( 'NONE',  ( -118.5108917117887444, 70.27763793881261734, -3.294392537550126843 ) ) ;
#11288 = VERTEX_POINT ( 'NONE', #82681 ) ;
#11289 = ORIENTED_EDGE ( 'NONE', *, *, #17583, .F. ) ;
#11290 = ADVANCED_FACE ( 'NONE', ( #54471 ), #75846, .F. ) ;
#11291 = VECTOR ( 'NONE', #54812, 1000.000000000000000 ) ;
#11292 = CYLINDRICAL_SURFACE ( 'NONE', #31071, 0.5000000000000073275 ) ;
#11293 = ORIENTED_EDGE ( 'NONE', *, *, #1714, .T. ) ;
#11294 = CARTESIAN_POINT ( 'NONE',  ( 116.5710038106515611, -34.42130396933979597, 209.0156252759109634 ) ) ;
#11295 = CARTESIAN_POINT ( 'NONE',  ( 101.6182654208066367, -28.31338856567544582, 125.5326905051223321 ) ) ;
#11296 = CARTESIAN_POINT ( 'NONE',  ( 116.8171228686476297, -34.15291832581976195, 190.0314586088004489 ) ) ;
#11297 = CARTESIAN_POINT ( 'NONE',  ( 96.92707254288593788, -39.15325348941441064, 52.51276813305394597 ) ) ;
#11298 = CARTESIAN_POINT ( 'NONE',  ( 115.7830219863385963, -41.80246318181204401, 44.40644472814330612 ) ) ;
#11299 = ORIENTED_EDGE ( 'NONE', *, *, #69395, .F. ) ;
#11300 = CIRCLE ( 'NONE', #22938, 17.33514202138210081 ) ;
#11301 = DIRECTION ( 'NONE',  ( 0.7071067811865835440, 0.000000000000000000, 0.7071067811865114905 ) ) ;
#11302 = AXIS2_PLACEMENT_3D ( 'NONE', #7699, #7258, #27693 ) ;
#11303 = AXIS2_PLACEMENT_3D ( 'NONE', #33436, #5292, #39786 ) ;
#11304 = LINE ( 'NONE', #66716, #4191 ) ;
#11305 = ORIENTED_EDGE ( 'NONE', *, *, #14771, .T. ) ;
#11306 = VECTOR ( 'NONE', #80656, 1000.000000000000000 ) ;
#11307 = CARTESIAN_POINT ( 'NONE',  ( 107.0664832912739257, -18.82844715994099971, 239.5838068554170093 ) ) ;
#11308 = ADVANCED_FACE ( 'NONE', ( #39076 ), #5468, .T. ) ;
#11309 = DIRECTION ( 'NONE',  ( -2.170915417798913418E-16, 0.000000000000000000, -1.000000000000000000 ) ) ;
#11310 = CARTESIAN_POINT ( 'NONE',  ( 96.29057984255072711, -34.37493501460198075, 256.1432443235300980 ) ) ;
#11311 = CARTESIAN_POINT ( 'NONE',  ( 107.0667039024470313, -104.2784471599413934, 2.217806855418003043 ) ) ;
#11312 = CARTESIAN_POINT ( 'NONE',  ( -479.3614999999999782, 18.41194598552320016, 97.63125000000000853 ) ) ;
#11313 = CARTESIAN_POINT ( 'NONE',  ( 121.2221484686747317, -94.95109689075241022, -19.26696060647628528 ) ) ;
#11314 = CARTESIAN_POINT ( 'NONE',  ( 107.8428746604417654, -27.05123223485975714, 264.4352769709337849 ) ) ;
#11316 = CARTESIAN_POINT ( 'NONE',  ( 113.4020503763144063, -27.70036014686462522, 80.57753003781597556 ) ) ;
#11315 = LINE ( 'NONE', #32650, #12742 ) ;
#11317 = CARTESIAN_POINT ( 'NONE',  ( 114.8133063487188963, 71.21048122817593651, 62.15126537821431185 ) ) ;
#11318 = CARTESIAN_POINT ( 'NONE',  ( 113.8721965385452677, -28.72731865945801744, 139.5156252759109634 ) ) ;
#11319 = VERTEX_POINT ( 'NONE', #60406 ) ;
#11320 = CARTESIAN_POINT ( 'NONE',  ( 132.2601441849021455, -20.80290789369900750, 7.687431601936014047 ) ) ;
#11321 = ORIENTED_EDGE ( 'NONE', *, *, #89703, .T. ) ;
#11322 = VECTOR ( 'NONE', #18675, 1000.000000000000000 ) ;
#11323 = EDGE_CURVE ( 'NONE', #37688, #30738, #82235, .T. ) ;
#11324 = DIRECTION ( 'NONE',  ( 1.000000000000000000, 6.145690160522480771E-16, 0.000000000000000000 ) ) ;
#11325 = CARTESIAN_POINT ( 'NONE',  ( 97.81168895331838087, -40.51742574516882200, 287.6356252759109680 ) ) ;
#11326 = DIRECTION ( 'NONE',  ( 0.9068632946707805287, -0.4214249218767882610, 9.493511560072084562E-16 ) ) ;
#11327 = VERTEX_POINT ( 'NONE', #74950 ) ;
#11328 = EDGE_CURVE ( 'NONE', #24990, #69696, #66784, .T. ) ;
#11329 = EDGE_CURVE ( 'NONE', #68446, #27190, #80906, .T. ) ;
#11330 = DIRECTION ( 'NONE',  ( -1.000000000000000000, 0.000000000000000000, -3.491483361109379305E-15 ) ) ;
#11332 = EDGE_LOOP ( 'NONE', ( #81199, #10623, #23643, #83248 ) ) ;
#11331 = CARTESIAN_POINT ( 'NONE',  ( 107.3350830925955961, -26.26357308316309869, 120.0556252759109555 ) ) ;
#11333 = CARTESIAN_POINT ( 'NONE',  ( 1.163414459189986668E-15, 210.0000000000000000, 163.6557476874258441 ) ) ;
#11334 = CARTESIAN_POINT ( 'NONE',  ( -130.0420937742006515, 87.79544278253749212, -11.57361518220400676 ) ) ;
#11335 = CIRCLE ( 'NONE', #80994, 5.599999999999994316 ) ;
#11336 = CIRCLE ( 'NONE', #15763, 5.041900000000001825 ) ;
#11337 = EDGE_CURVE ( 'NONE', #74946, #82764, #40488, .T. ) ;
#11338 = LINE ( 'NONE', #38586, #84367 ) ;
#11339 = VERTEX_POINT ( 'NONE', #54021 ) ;
#11340 = CARTESIAN_POINT ( 'NONE',  ( 108.9889396673064397, -47.63814106062356757, 122.7032443235299723 ) ) ;
#11341 = APPLICATION_PROTOCOL_DEFINITION ( 'draft international standard', 'automotive_design', 1998, #77131 ) ;
#11342 = EDGE_CURVE ( 'NONE', #64560, #53581, #64940, .T. ) ;
#11343 = CARTESIAN_POINT ( 'NONE',  ( 52.65249034007825912, -48.32844715994060181, 300.4678068554150059 ) ) ;
#11344 = CARTESIAN_POINT ( 'NONE',  ( 117.0718954858691774, -35.46248235918008618, 143.9272919423464714 ) ) ;
#11345 = ORIENTED_EDGE ( 'NONE', *, *, #44966, .T. ) ;
#11346 = EDGE_LOOP ( 'NONE', ( #18636, #11869, #11693, #26833 ) ) ;
#11347 = CARTESIAN_POINT ( 'NONE',  ( 168.5667039024482960, -48.82844715993496720, 180.4678068554150059 ) ) ;
#11348 = CARTESIAN_POINT ( 'NONE',  ( 48.45959712129000252, -28.98061976758940617, -5.074374724088000832 ) ) ;
#11349 = LINE ( 'NONE', #39049, #10646 ) ;
#11350 = EDGE_CURVE ( 'NONE', #34909, #12059, #31668, .T. ) ;
#11351 = DIRECTION ( 'NONE',  ( -0.9254794337955620787, -0.3787978585227822492, 0.000000000000000000 ) ) ;
#11353 = CARTESIAN_POINT ( 'NONE',  ( -4.101352651117800896, 70.52330563318118095, -118.4857037620892726 ) ) ;
#11352 = PLANE ( 'NONE',  #32017 ) ;
#11354 = DIRECTION ( 'NONE',  ( 1.000000000000000000, 4.299999999999999979E-14, 1.000000000000000078E-15 ) ) ;
#11355 = CIRCLE ( 'NONE', #59190, 8.636000000000004562 ) ;
#11356 = ORIENTED_EDGE ( 'NONE', *, *, #13761, .F. ) ;
#11357 = FACE_OUTER_BOUND ( 'NONE', #4266, .T. ) ;
#11358 = CARTESIAN_POINT ( 'NONE',  ( 117.2759483237919085, -34.91131378075003511, 194.9546728949579517 ) ) ;
#11360 = ORIENTED_EDGE ( 'NONE', *, *, #63686, .T. ) ;
#11359 = CARTESIAN_POINT ( 'NONE',  ( 0.000000000000000000, 184.0000000000000000, 90.32146847885337593 ) ) ;
#11361 = ADVANCED_FACE ( 'NONE', ( #32257 ), #19531, .F. ) ;
#11362 = AXIS2_PLACEMENT_3D ( 'NONE', #9171, #36870, #44107 ) ;
#11363 = CARTESIAN_POINT ( 'NONE',  ( 117.3137205126583211, -38.32096045344800928, 64.69181575210097890 ) ) ;
#11365 = EDGE_CURVE ( 'NONE', #16163, #28852, #50462, .T. ) ;
#11364 = CARTESIAN_POINT ( 'NONE',  ( 110.8543372361816779, -45.98429251226213665, 52.88561369035437565 ) ) ;
#11366 = CARTESIAN_POINT ( 'NONE',  ( 31.71315051185499811, -33.70561438052111214, -5.074374724088000832 ) ) ;
#11367 = EDGE_CURVE ( 'NONE', #1618, #48508, #40602, .T. ) ;
#11368 = VECTOR ( 'NONE', #17524, 1000.000000000000000 ) ;
#11369 = FACE_BOUND ( 'NONE', #66700, .T. ) ;
#11370 = ORIENTED_EDGE ( 'NONE', *, *, #18081, .F. ) ;
#11371 = DIRECTION ( 'NONE',  ( 2.900000000000000265E-14, -2.000000000000000155E-15, 1.000000000000000000 ) ) ;
#11372 = VECTOR ( 'NONE', #80214, 1000.000000000000000 ) ;
#11373 = EDGE_CURVE ( 'NONE', #51366, #18171, #1342, .T. ) ;
#11374 = VECTOR ( 'NONE', #85875, 1000.000000000000114 ) ;
#11375 = ORIENTED_EDGE ( 'NONE', *, *, #69213, .T. ) ;
#11376 = ORIENTED_EDGE ( 'NONE', *, *, #77592, .F. ) ;
#11377 = B_SPLINE_CURVE_WITH_KNOTS ( 'NONE', 3,
 ( #9143, #31353, #43186, #22778, #10035 ),
 .UNSPECIFIED., .F., .F.,
 ( 4, 1, 4 ),
 ( -7.123703416098150498, -3.135239217345689777, -0.1438962376298542623 ),
 .UNSPECIFIED. ) ;
#11378 = CARTESIAN_POINT ( 'NONE',  ( 115.4467593082293178, -40.97768201889641659, 244.8968214011349573 ) ) ;
#11379 = PLANE ( 'NONE',  #38591 ) ;
#11380 = CARTESIAN_POINT ( 'NONE',  ( -48.67264380398864176, 148.4450814996825443, 66.68100227564391957 ) ) ;
#11381 = CARTESIAN_POINT ( 'NONE',  ( -72.96458098368751166, 101.5999999999999943, 78.00648098368618832 ) ) ;
#11382 = VECTOR ( 'NONE', #24833, 1000.000000000000000 ) ;
#11383 = LINE ( 'NONE', #40424, #60372 ) ;
#11384 = ORIENTED_EDGE ( 'NONE', *, *, #38621, .T. ) ;
#11385 = FACE_OUTER_BOUND ( 'NONE', #8759, .T. ) ;
#11386 = CARTESIAN_POINT ( 'NONE',  ( 121.2221484686747317, -94.95109689075249548, -21.78219314458229405 ) ) ;
#11387 = EDGE_LOOP ( 'NONE', ( #29293, #32623, #67846, #60044, #23685, #87514 ) ) ;
#11388 = CARTESIAN_POINT ( 'NONE',  ( 115.6373213143784398, -30.77082676042341802, 279.3099109901966131 ) ) ;
#11389 = ORIENTED_EDGE ( 'NONE', *, *, #87650, .F. ) ;
#11390 = ORIENTED_EDGE ( 'NONE', *, *, #43835, .T. ) ;
#11391 = CARTESIAN_POINT ( 'NONE',  ( 97.79975852078015919, -37.20246216128834504, 269.1852332267342831 ) ) ;
#11392 = CARTESIAN_POINT ( 'NONE',  ( 51.42025729302669390, -31.94127993907680718, 342.9256252759109884 ) ) ;
#11393 = CARTESIAN_POINT ( 'NONE',  ( 23.04768281101732796, 77.81817409959050735, 302.2712646479865271 ) ) ;
#11394 = CARTESIAN_POINT ( 'NONE',  ( 53.97500000000000142, 95.25000000000000000, 283.4005000000000223 ) ) ;
#11395 = DIRECTION ( 'NONE',  ( 0.000000000000000000, -1.000000000000000000, 0.000000000000000000 ) ) ;
#11396 = VECTOR ( 'NONE', #48569, 1000.000000000000114 ) ;
#11397 = AXIS2_PLACEMENT_3D ( 'NONE', #18514, #89367, #74836 ) ;
#11398 = CARTESIAN_POINT ( 'NONE',  ( 97.88103918441719031, -41.75145834149261503, 217.7241967044829494 ) ) ;
#11399 = DIRECTION ( 'NONE',  ( 0.000000000000000000, 1.000000000000000000, 0.000000000000000000 ) ) ;
#11400 = ORIENTED_EDGE ( 'NONE', *, *, #47403, .T. ) ;
#11401 = CARTESIAN_POINT ( 'NONE',  ( 117.0163018969640376, -33.47459087099611708, 85.07848241876791917 ) ) ;
#11402 = CARTESIAN_POINT ( 'NONE',  ( 51.06648329127400388, 22.62155284005901024, 333.4006252759110112 ) ) ;
#11403 = VERTEX_POINT ( 'NONE', #28125 ) ;
#11404 = ORIENTED_EDGE ( 'NONE', *, *, #32887, .F. ) ;
#11405 = ORIENTED_EDGE ( 'NONE', *, *, #40947, .F. ) ;
#11406 = CARTESIAN_POINT ( 'NONE',  ( 78.92327517541032478, -39.23064218986550600, 8.021355262919639628 ) ) ;
#11407 = CARTESIAN_POINT ( 'NONE',  ( 194.5667039024485803, -47.82844715993405060, 129.9678068554150343 ) ) ;
#11408 = DIRECTION ( 'NONE',  ( 1.000000000000000078E-15, -1.000000000000000083E-30, -1.000000000000000000 ) ) ;
#11409 = CARTESIAN_POINT ( 'NONE',  ( 115.3759468638744181, -39.14889752855258820, 136.4071379886389650 ) ) ;
#11411 = B_SPLINE_CURVE_WITH_KNOTS ( 'NONE', 3,
 ( #40102, #46005, #86937, #66466, #52798, #39216, #12873, #26044, #19229, #24699, #52365, #67818, #18776, #45555, #5609, #40559, #26484, #67358 ),
 .UNSPECIFIED., .F., .F.,
 ( 4, 2, 2, 2, 2, 2, 2, 2, 4 ),
 ( 0.000000000000000000, 0.06249899055469551601, 0.1249979811093910320, 0.1874969716640865480, 0.2499959622187820640, 0.3124949527734776078, 0.3749939433281730961, 0.4374929338828685843, 0.4999919244375641281 ),
 .UNSPECIFIED. ) ;
#11410 = CARTESIAN_POINT ( 'NONE',  ( 117.5124522703044931, -35.85713534702714611, 249.8927681330537780 ) ) ;
#11412 = FACE_OUTER_BOUND ( 'NONE', #55786, .T. ) ;
#11413 = ORIENTED_EDGE ( 'NONE', *, *, #27843, .T. ) ;
#11414 = AXIS2_PLACEMENT_3D ( 'NONE', #56568, #62932, #83395 ) ;
#11415 = DIRECTION ( 'NONE',  ( 0.000000000000000000, 0.000000000000000000, -1.000000000000000000 ) ) ;
#11416 = ORIENTED_EDGE ( 'NONE', *, *, #39381, .F. ) ;
#11417 = ORIENTED_EDGE ( 'NONE', *, *, #20550, .T. ) ;
#11418 = CIRCLE ( 'NONE', #60679, 37.00000000000000711 ) ;
#11419 = AXIS2_PLACEMENT_3D ( 'NONE', #21461, #20567, #48237 ) ;
#11420 = DIRECTION ( 'NONE',  ( 0.7071067811989784069, -0.7071067811741166276, 6.612322855976402389E-17 ) ) ;
#11421 = VERTEX_POINT ( 'NONE', #49459 ) ;
#11422 = ORIENTED_EDGE ( 'NONE', *, *, #62805, .F. ) ;
#11423 = CARTESIAN_POINT ( 'NONE',  ( 109.6445583207592591, -46.47969343970833478, 168.7823647920304211 ) ) ;
#11424 = FACE_OUTER_BOUND ( 'NONE', #41978, .T. ) ;
#11425 = ADVANCED_FACE ( 'NONE', ( #13616, #34497 ), #14523, .F. ) ;
#11426 = FACE_OUTER_BOUND ( 'NONE', #76945, .T. ) ;
#11427 = CARTESIAN_POINT ( 'NONE',  ( 98.50657384982324061, -36.30512124771701821, 170.7095626852199359 ) ) ;
#11428 = CARTESIAN_POINT ( 'NONE',  ( 116.5143565283028266, -32.21898467494469998, 19.18133956162493092 ) ) ;
#11429 = CARTESIAN_POINT ( 'NONE',  ( 80.15209520963914258, -113.0957571362959726, 250.2190963482990185 ) ) ;
#11430 = ORIENTED_EDGE ( 'NONE', *, *, #55064, .F. ) ;
#11432 = ADVANCED_FACE ( 'NONE', ( #22689 ), #64015, .F. ) ;
#11431 = VECTOR ( 'NONE', #56063, 1000.000000000000000 ) ;
#11433 = CARTESIAN_POINT ( 'NONE',  ( -91.26337341211424814, 76.18740257834565455, -75.67519899969691721 ) ) ;
#11434 = VERTEX_POINT ( 'NONE', #83565 ) ;
#11435 = CIRCLE ( 'NONE', #33223, 6.349999999999999645 ) ;
#11436 = ADVANCED_FACE ( 'NONE', ( #41302 ), #84920, .F. ) ;
#11437 = EDGE_CURVE ( 'NONE', #30447, #18949, #70377, .T. ) ;
#11438 = LINE ( 'NONE', #45478, #21441 ) ;
#11439 = ORIENTED_EDGE ( 'NONE', *, *, #65361, .F. ) ;
#11440 = CARTESIAN_POINT ( 'NONE',  ( 97.67427069871116885, -40.16553667892655710, 167.6058069957254872 ) ) ;
#11441 = AXIS2_PLACEMENT_3D ( 'NONE', #82081, #19829, #13464 ) ;
#11442 = CARTESIAN_POINT ( 'NONE',  ( 115.7821352934020780, -41.80395130134588300, 33.40652350832453266 ) ) ;
#11443 = CARTESIAN_POINT ( 'NONE',  ( 110.8537393078288602, -45.98453721465049426, 132.8855622535276098 ) ) ;
#11444 = EDGE_CURVE ( 'NONE', #22928, #36736, #49910, .T. ) ;
#11445 = DIRECTION ( 'NONE',  ( 1.000000000000000000, 4.163336342344333240E-14, 0.000000000000000000 ) ) ;
#11446 = ORIENTED_EDGE ( 'NONE', *, *, #39337, .T. ) ;
#11447 = CARTESIAN_POINT ( 'NONE',  ( 99.74655714901966519, -44.23324885335900802, 21.96133956162593748 ) ) ;
#11448 = CARTESIAN_POINT ( 'NONE',  ( 116.7674666963954309, -31.33607907186020824, 25.24229194257798881 ) ) ;
#11449 =( NAMED_UNIT ( * ) PLANE_ANGLE_UNIT ( ) SI_UNIT ( $, .RADIAN. ) );
#11450 = ADVANCED_FACE ( 'NONE', ( #84016 ), #69932, .F. ) ;
#11452 = CARTESIAN_POINT ( 'NONE',  ( 140.0667039024470455, -118.2784471599408960, 45.21780685541799727 ) ) ;
#11451 = DIRECTION ( 'NONE',  ( -1.825781832977099352E-16, 0.4999999999999998890, 0.8660254037844387076 ) ) ;
#11453 = LINE ( 'NONE', #81417, #17727 ) ;
#11454 = DIRECTION ( 'NONE',  ( 0.000000000000000000, 0.000000000000000000, -1.000000000000000000 ) ) ;
#11455 = CARTESIAN_POINT ( 'NONE',  ( 132.9232751754149149, -39.23064218986716867, 8.021355262921384011 ) ) ;
#11456 = VECTOR ( 'NONE', #66605, 1000.000000000000000 ) ;
#11457 = DIRECTION ( 'NONE',  ( 0.000000000000000000, 0.000000000000000000, -1.000000000000000000 ) ) ;
#11458 = EDGE_CURVE ( 'NONE', #31568, #60190, #57731, .T. ) ;
#11459 = CARTESIAN_POINT ( 'NONE',  ( 147.0667039024469886, -67.87574355753805833, 246.0361703021810058 ) ) ;
#11460 = VERTEX_POINT ( 'NONE', #50360 ) ;
#11461 = CARTESIAN_POINT ( 'NONE',  ( 112.2029234908279562, -27.56599932623266724, 34.66991099019695355 ) ) ;
#11462 = CARTESIAN_POINT ( 'NONE',  ( 113.1000543987032785, -45.99065659369661319, 219.0480062282919960 ) ) ;
#11463 = CARTESIAN_POINT ( 'NONE',  ( 115.5915050065794247, -42.76776344903117888, 49.33562527591095659 ) ) ;
#11465 = CARTESIAN_POINT ( 'NONE',  ( 199.3900000000000148, 52.73749999999999716, -44.45000000000000284 ) ) ;
#11464 = LINE ( 'NONE', #40504, #66774 ) ;
#11466 = CARTESIAN_POINT ( 'NONE',  ( -17.54031676229692849, 65.59999999999998010, 43.71138335376673467 ) ) ;
#11468 = EDGE_CURVE ( 'NONE', #15026, #22617, #19726, .T. ) ;
#11467 = AXIS2_PLACEMENT_3D ( 'NONE', #45749, #4453, #24895 ) ;
#11469 = ORIENTED_EDGE ( 'NONE', *, *, #19737, .F. ) ;
#11470 = FACE_BOUND ( 'NONE', #76767, .T. ) ;
#11471 = ORIENTED_EDGE ( 'NONE', *, *, #47558, .T. ) ;
#11472 = CARTESIAN_POINT ( 'NONE',  ( 118.1720832024964807, -36.20253795304678590, 114.8641967044819694 ) ) ;
#11474 = ORIENTED_EDGE ( 'NONE', *, *, #36868, .T. ) ;
#11473 = CARTESIAN_POINT ( 'NONE',  ( -487.2989999999999782, 21.43125000000029701, 15.23694598552314972 ) ) ;
#11475 = CARTESIAN_POINT ( 'NONE',  ( 115.4997179687694171, -29.61999039777962039, 220.3718157521019521 ) ) ;
#11476 = DIRECTION ( 'NONE',  ( 3.100000000000000258E-29, -3.100000000000000044E-14, -1.000000000000000000 ) ) ;
#11477 = DIRECTION ( 'NONE',  ( -0.7071067811865476838, -0.7071067811865473507, 0.000000000000000000 ) ) ;
#11478 = CARTESIAN_POINT ( 'NONE',  ( 142.8832909413445122, -79.11588146349312467, 543.8623766218582887 ) ) ;
#11479 = FACE_OUTER_BOUND ( 'NONE', #13055, .T. ) ;
#11480 = ADVANCED_FACE ( 'NONE', ( #22239 ), #62658, .T. ) ;
#11481 = AXIS2_PLACEMENT_3D ( 'NONE', #60018, #87753, #80959 ) ;
#11482 = CARTESIAN_POINT ( 'NONE',  ( 131.4004675426832875, -37.42701295172433618, 2.979899338979598689 ) ) ;
#11483 = LINE ( 'NONE', #86895, #2233 ) ;
#11484 = EDGE_CURVE ( 'NONE', #24458, #5511, #8477, .T. ) ;
#11485 = CARTESIAN_POINT ( 'NONE',  ( 113.7965574739370993, -44.62378898692907825, 153.1508633711499670 ) ) ;
#11486 = ORIENTED_EDGE ( 'NONE', *, *, #33703, .T. ) ;
#11487 = ORIENTED_EDGE ( 'NONE', *, *, #58310, .F. ) ;
#11488 = CARTESIAN_POINT ( 'NONE',  ( 112.9486100676287208, -29.40298074535265727, 115.9577737820869601 ) ) ;
#11489 = CIRCLE ( 'NONE', #44925, 8.636000000000004562 ) ;
#11490 = LINE ( 'NONE', #75510, #38517 ) ;
#11492 = CARTESIAN_POINT ( 'NONE',  ( -186.2398777604655038, 0.000000000000000000, -12.69999999999999929 ) ) ;
#11491 = CARTESIAN_POINT ( 'NONE',  ( 117.4208826025846690, -36.15918394849474282, 269.8822919425771829 ) ) ;
#11493 = LINE ( 'NONE', #45982, #63809 ) ;
#11494 = LINE ( 'NONE', #39189, #42317 ) ;
#11495 = FACE_OUTER_BOUND ( 'NONE', #34002, .T. ) ;
#11496 = AXIS2_PLACEMENT_3D ( 'NONE', #71858, #37330, #2818 ) ;
#11497 = CARTESIAN_POINT ( 'NONE',  ( -487.2989999999999782, 93.66249999999999432, 98.73639197104678544 ) ) ;
#11498 = CARTESIAN_POINT ( 'NONE',  ( 107.0667039024479834, -36.72944715994099596, 239.5838068554170093 ) ) ;
#11499 = LINE ( 'NONE', #67799, #41496 ) ;
#11501 = CARTESIAN_POINT ( 'NONE',  ( 113.6005200848514676, -45.61596423689133672, 183.0689586092439640 ) ) ;
#11500 = AXIS2_PLACEMENT_3D ( 'NONE', #65617, #57119, #15815 ) ;
#11502 = VERTEX_POINT ( 'NONE', #10381 ) ;
#11503 = VERTEX_POINT ( 'NONE', #87138 ) ;
#11504 = CARTESIAN_POINT ( 'NONE',  ( -98.60478223830740774, 120.6499999999999915, -1.074461880482445986E-12 ) ) ;
#11505 = CARTESIAN_POINT ( 'NONE',  ( 77.96925277059908410, -16.94806367528691027, 2.376725340793110597 ) ) ;
#11506 = VECTOR ( 'NONE', #50545, 1000.000000000000000 ) ;
#11507 = LINE ( 'NONE', #47344, #60597 ) ;
#11508 = CARTESIAN_POINT ( 'NONE',  ( -72.96458098368600531, 127.0000000000000000, -72.96458098368781009 ) ) ;
#11509 = ADVANCED_FACE ( 'NONE', ( #64902 ), #4009, .F. ) ;
#11510 = VERTEX_POINT ( 'NONE', #86243 ) ;
#11511 = CARTESIAN_POINT ( 'NONE',  ( -12.60000000000000142, 82.54999999999999716, 117.6834004267381744 ) ) ;
#11512 = CARTESIAN_POINT ( 'NONE',  ( 117.4129020423329450, -35.18752443080737891, 218.9441967044829482 ) ) ;
#11514 = VECTOR ( 'NONE', #39679, 1000.000000000000000 ) ;
#11513 = LINE ( 'NONE', #39209, #44408 ) ;
#11515 = ORIENTED_EDGE ( 'NONE', *, *, #24549, .T. ) ;
#11516 = ORIENTED_EDGE ( 'NONE', *, *, #33896, .T. ) ;
#11517 = VECTOR ( 'NONE', #83173, 1000.000000000000000 ) ;
#11518 = B_SPLINE_CURVE_WITH_KNOTS ( 'NONE', 3,
 ( #20807, #75776, #13543, #40344, #83056, #68957, #68063, #26711, #13108, #19015, #46699, #6281, #41227, #73978, #39455, #88957, #74430, #12204 ),
 .UNSPECIFIED., .F., .F.,
 ( 4, 2, 2, 2, 2, 2, 2, 2, 4 ),
 ( 0.4999390761915182280, 0.5624466916675784356, 0.6249543071436386432, 0.6874619226196989619, 0.7499695380957591695, 0.8124771535718193771, 0.8749847690478795847, 0.9374923845239397924, 1.000000000000000000 ),
 .UNSPECIFIED. ) ;
#11519 = CARTESIAN_POINT ( 'NONE',  ( 116.4889884589737363, -40.12238724215244190, 64.55198567951927657 ) ) ;
#11520 = DIRECTION ( 'NONE',  ( 0.000000000000000000, -1.000000000000000000, 0.000000000000000000 ) ) ;
#11521 = CARTESIAN_POINT ( 'NONE',  ( 72.31648329127396835, -9.833000550534366724, 14.92562527591093691 ) ) ;
#11522 = CARTESIAN_POINT ( 'NONE',  ( 106.4288663150950214, -28.56390168778064975, 22.95666179816197072 ) ) ;
#11523 = CARTESIAN_POINT ( 'NONE',  ( 20.03715912545641231, -24.95799193693202156, 180.4678068554150911 ) ) ;
#11524 = ORIENTED_EDGE ( 'NONE', *, *, #45663, .F. ) ;
#11525 = CARTESIAN_POINT ( 'NONE',  ( -27.27158787008326968, 127.0000000000000000, 111.9860621927989826 ) ) ;
#11527 = ADVANCED_FACE ( 'NONE', ( #10818 ), #24907, .F. ) ;
#11526 = CIRCLE ( 'NONE', #7130, 11.45913725231036118 ) ;
#11528 = CARTESIAN_POINT ( 'NONE',  ( 80.80620050782613362, -16.05355276379784968, 8.162233076788782071 ) ) ;
#11529 = EDGE_LOOP ( 'NONE', ( #80455, #62588, #45728, #66153 ) ) ;
#11530 = ORIENTED_EDGE ( 'NONE', *, *, #79037, .T. ) ;
#11531 = DIRECTION ( 'NONE',  ( 0.000000000000000000, 0.000000000000000000, 1.000000000000000000 ) ) ;
#11532 = ORIENTED_EDGE ( 'NONE', *, *, #25998, .T. ) ;
#11533 = VERTEX_POINT ( 'NONE', #59405 ) ;
#11534 = CARTESIAN_POINT ( 'NONE',  ( 51.06648329127400388, -0.2185775633790978945, 330.8831252759119934 ) ) ;
#11535 = EDGE_CURVE ( 'NONE', #74351, #54417, #57629, .T. ) ;
#11536 = EDGE_CURVE ( 'NONE', #3245, #73802, #67915, .T. ) ;
#11537 = CARTESIAN_POINT ( 'NONE',  ( 98.53752338633383090, -37.19093893883378144, 75.79241982807700140 ) ) ;
#11538 = CARTESIAN_POINT ( 'NONE',  ( 117.9557474314311349, -34.69982462793587530, 203.9851490854349549 ) ) ;
#11539 = AXIS2_PLACEMENT_3D ( 'NONE', #32473, #53345, #33380 ) ;
#11540 = EDGE_CURVE ( 'NONE', #45837, #29906, #58079, .T. ) ;
#11541 = CARTESIAN_POINT ( 'NONE',  ( 117.4355769707883468, -40.49052663852281597, 173.5375300378159693 ) ) ;
#11543 = CARTESIAN_POINT ( 'NONE',  ( 100.8484424157226442, -45.14118303587278547, 253.0699109901968882 ) ) ;
#11542 = CARTESIAN_POINT ( 'NONE',  ( 106.1835720340748139, -46.77890140548399955, 22.50653266953309384 ) ) ;
#11544 = CARTESIAN_POINT ( 'NONE',  ( -479.3614999999999782, 53.97500000000000142, 12.69999999999999929 ) ) ;
#11545 = CARTESIAN_POINT ( 'NONE',  ( 31.75000000000000000, 66.67499999999999716, 295.2750000000000341 ) ) ;
#11546 = ORIENTED_EDGE ( 'NONE', *, *, #67266, .F. ) ;
#11547 = AXIS2_PLACEMENT_3D ( 'NONE', #84991, #22762, #10013 ) ;
#11548 = ORIENTED_EDGE ( 'NONE', *, *, #32031, .T. ) ;
#11549 = B_SPLINE_CURVE_WITH_KNOTS ( 'NONE', 3,
 ( #54268, #67031, #19782, #18885, #47909, #80676, #40208, #5257, #32951, #6164, #60649, #67928, #88390, #26150, #82032, #47467, #81586, #19338, #33854, #76087, #55609, #14775, #69730, #71086, #41998, #7944, #7053, #35642, #63813, #50157, #42443, #13864, #62455, #83363, #49260, #35185, #56066, #1135 ),
 .UNSPECIFIED., .F., .F.,
 ( 4, 2, 2, 1, 2, 2, 2, 2, 1, 1, 2, 2, 2, 1, 2, 2, 1, 2, 1, 2, 2, 4 ),
 ( 0.000000000000000000, 0.04166793602364190358, 0.05208492002955231182, 0.05729341203250756104, 0.05989765803398552912, 0.06250190403546351803, 0.08333587204728555575, 0.1041698400591075935, 0.1145868240650192021, 0.1197953160679756379, 0.1223995620694541958, 0.1250038080709327815, 0.1666717440945731377, 0.1770887281004829561, 0.1822972201034377959, 0.1875057121063926635, 0.2083396801182141878, 0.2291736481300356287, 0.2395906321359451141, 0.2447991241388997319, 0.2500076161418543497, 0.3333434881890883217 ),
 .UNSPECIFIED. ) ;
#11550 = B_SPLINE_CURVE_WITH_KNOTS ( 'NONE', 3,
 ( #43432, #71178, #30715, #3013, #10272, #4800, #18414, #24354, #66115, #52463, #58411, #86139, #45651, #25230, #46102, #32045, #38412, #23915 ),
 .UNSPECIFIED., .F., .F.,
 ( 4, 2, 2, 2, 2, 2, 2, 2, 4 ),
 ( 0.000000000000000000, 0.1249999999999989175, 0.1874999999999970024, 0.2499999999999950595, 0.3749999999999940048, 0.4374999999999941158, 0.4999999999999942268, 0.7499999999999970024, 1.000000000000000000 ),
 .UNSPECIFIED. ) ;
#11551 = VECTOR ( 'NONE', #86493, 1000.000000000000000 ) ;
#11552 = ADVANCED_FACE ( 'NONE', ( #78102 ), #9943, .F. ) ;
#11553 = B_SPLINE_CURVE_WITH_KNOTS ( 'NONE', 3,
 ( #8805, #29675, #21074, #49654, #7444, #85110, #77381, #77837, #71027, #8346, #6996, #83307, #48750, #78296, #28316, #36043, #14267, #14716, #63757, #35584, #56009, #1537, #50101, #83760, #69226, #76485, #35132, #70116 ),
 .UNSPECIFIED., .F., .F.,
 ( 4, 2, 2, 2, 2, 2, 2, 2, 2, 2, 1, 1, 1, 1, 2, 4 ),
 ( 0.000000000000000000, 0.06250188926545433010, 0.1250037785309086602, 0.1875056677963629903, 0.2500075570618173204, 0.3125094463272716783, 0.3750113355927259806, 0.4375132248581803385, 0.4687641694909075452, 0.4843896418072711763, 0.4922023779654531306, 0.4961087460445438024, 0.4980619300840890551, 0.4990385221038616259, 0.4995268181137479391, 0.5000151141236341967 ),
 .UNSPECIFIED. ) ;
#11554 = CARTESIAN_POINT ( 'NONE',  ( 97.81168895331838087, -40.51742574516882200, 287.6356252759109680 ) ) ;
#11555 = CARTESIAN_POINT ( 'NONE',  ( 115.4954577264304731, -29.50689403799194110, 229.4022919425779605 ) ) ;
#11556 = VERTEX_POINT ( 'NONE', #65346 ) ;
#11557 = CARTESIAN_POINT ( 'NONE',  ( 106.9749943965245365, -47.15435292659226718, 187.5699109901969734 ) ) ;
#11558 = CARTESIAN_POINT ( 'NONE',  ( 97.06110197059325628, -37.99657418247586804, 266.4273502531260078 ) ) ;
#11559 = CARTESIAN_POINT ( 'NONE',  ( 49.16670390244701139, -26.71338133339240528, -5.074374724088000832 ) ) ;
#11560 = CARTESIAN_POINT ( 'NONE',  ( 28.57499999999999929, 77.96728223830740490, 310.8325000000000387 ) ) ;
#11561 = DIRECTION ( 'NONE',  ( -0.000000000000000000, 1.000000000000000000, -0.000000000000000000 ) ) ;
#11563 = DIRECTION ( 'NONE',  ( 3.339108161477000479E-13, -1.000000000000000000, 4.100000000000000342E-29 ) ) ;
#11562 = CARTESIAN_POINT ( 'NONE',  ( 100.0247289185300588, -32.06647811954630356, 277.6356252759111953 ) ) ;
#11564 = CARTESIAN_POINT ( 'NONE',  ( 97.83886487280460642, -40.58324923297708864, 172.6412926176714393 ) ) ;
#11566 = EDGE_CURVE ( 'NONE', #65338, #81967, #85372, .T. ) ;
#11565 = DIRECTION ( 'NONE',  ( -4.277118011829300531E-15, 0.000000000000000000, -1.000000000000000000 ) ) ;
#11567 = CARTESIAN_POINT ( 'NONE',  ( 128.5492039024480562, -58.72944715994093201, 231.5838068554170093 ) ) ;
#11568 = AXIS2_PLACEMENT_3D ( 'NONE', #81481, #87381, #52368 ) ;
#11569 = DIRECTION ( 'NONE',  ( 1.000000000000000078E-15, -1.000000000000000083E-30, -1.000000000000000000 ) ) ;
#11570 = STYLED_ITEM ( 'NONE', ( #56798 ), #83525 ) ;
#11571 = LINE ( 'NONE', #44725, #83672 ) ;
#11572 = LINE ( 'NONE', #86982, #2827 ) ;
#11573 = EDGE_CURVE ( 'NONE', #70290, #26617, #89647, .T. ) ;
#11575 = VERTEX_POINT ( 'NONE', #38520 ) ;
#11574 = CARTESIAN_POINT ( 'NONE',  ( -10.08084112162953616, 90.28574336371696063, -118.1269349842563088 ) ) ;
#11576 = LINE ( 'NONE', #81968, #71284 ) ;
#11577 = CARTESIAN_POINT ( 'NONE',  ( 116.0742729640735007, -42.02152512393894312, 238.4041967044829562 ) ) ;
#11578 = CARTESIAN_POINT ( 'NONE',  ( 98.84006766826026080, -28.19945879207355688, 111.6870538473389587 ) ) ;
#11579 = CARTESIAN_POINT ( 'NONE',  ( 105.1027920011780452, -26.44660240447466037, 231.2270538473399597 ) ) ;
#11580 = FACE_OUTER_BOUND ( 'NONE', #310, .T. ) ;
#11581 = AXIS2_PLACEMENT_3D ( 'NONE', #12533, #71753, #79018 ) ;
#11582 = CARTESIAN_POINT ( 'NONE',  ( 184.5667039024486087, -48.82844715993447693, 129.9678068554150059 ) ) ;
#11584 = CARTESIAN_POINT ( 'NONE',  ( 116.3216976867776964, -32.94060878512167534, 40.13562527591096796 ) ) ;
#11583 = CARTESIAN_POINT ( 'NONE',  ( -41.60202597009397607, 64.60000000000000853, 50.85338361873603219 ) ) ;
#11585 = DIRECTION ( 'NONE',  ( 0.000000000000000000, 0.000000000000000000, -1.000000000000000000 ) ) ;
#11586 = CARTESIAN_POINT ( 'NONE',  ( 104.0667030381796963, -67.87844715994094713, 93.21780742166239975 ) ) ;
#11587 = AXIS2_PLACEMENT_3D ( 'NONE', #32865, #46926, #31972 ) ;
#11588 = ORIENTED_EDGE ( 'NONE', *, *, #65287, .T. ) ;
#11589 = VERTEX_POINT ( 'NONE', #58955 ) ;
#11590 = CIRCLE ( 'NONE', #21706, 3.249999999999975131 ) ;
#11591 = CARTESIAN_POINT ( 'NONE',  ( 99.46962827726154899, -41.65933777599243371, 146.2190864947439763 ) ) ;
#11593 = EDGE_LOOP ( 'NONE', ( #19158, #83622, #45477, #2774 ) ) ;
#11592 = CARTESIAN_POINT ( 'NONE',  ( 163.1543517358615247, -31.62489322947688919, 313.9678068554149490 ) ) ;
#11594 = CARTESIAN_POINT ( 'NONE',  ( 117.7221270036566807, -41.68118999199129604, 4.925625275910981316 ) ) ;
#11595 = CARTESIAN_POINT ( 'NONE',  ( 108.3168256696638281, -47.05733704442508980, 113.6727681330539639 ) ) ;
#11596 = DIRECTION ( 'NONE',  ( -1.000000000000000000, -4.299999999999999979E-14, -1.000000000000000078E-15 ) ) ;
#11597 = CARTESIAN_POINT ( 'NONE',  ( 77.67297288197553939, -17.37149612621849215, 7.198162082949088436 ) ) ;
#11598 = CARTESIAN_POINT ( 'NONE',  ( 83.06670390244796920, -67.87844715994100397, 213.1838068554149856 ) ) ;
#11599 = DIRECTION ( 'NONE',  ( -1.000000000000000078E-15, 1.000000000000000083E-30, 1.000000000000000000 ) ) ;
#11600 = EDGE_CURVE ( 'NONE', #67868, #77207, #71286, .T. ) ;
#11601 = CARTESIAN_POINT ( 'NONE',  ( 96.86520444330096780, -38.59296402346417665, 51.48229194257797303 ) ) ;
#11602 = EDGE_LOOP ( 'NONE', ( #32295, #56409 ) ) ;
#11603 = VECTOR ( 'NONE', #86913, 1000.000000000000000 ) ;
#11604 = EDGE_LOOP ( 'NONE', ( #29551, #82243, #78779, #43337 ) ) ;
#11605 = ORIENTED_EDGE ( 'NONE', *, *, #61383, .F. ) ;
#11606 = DIRECTION ( 'NONE',  ( 0.000000000000000000, -1.000000000000000000, 0.000000000000000000 ) ) ;
#11608 = DIRECTION ( 'NONE',  ( 1.000000000000000000, 1.175184669633339961E-16, -2.900000000000000265E-14 ) ) ;
#11607 = CARTESIAN_POINT ( 'NONE',  ( 107.6167445103326230, -46.48501816386541208, 148.6213395616249784 ) ) ;
#11609 = DIRECTION ( 'NONE',  ( 0.000000000000000000, 7.536132396315209176E-17, -1.000000000000000000 ) ) ;
#11610 = FACE_OUTER_BOUND ( 'NONE', #64712, .T. ) ;
#11611 = DIRECTION ( 'NONE',  ( -1.000000000000000078E-15, 1.000000000000000000, 0.000000000000000000 ) ) ;
#11612 = VECTOR ( 'NONE', #36961, 1000.000000000000000 ) ;
#11613 = CARTESIAN_POINT ( 'NONE',  ( 92.27768215249926698, 84.21498941703525531, 74.43373480440783396 ) ) ;
#11614 = DIRECTION ( 'NONE',  ( 1.000000000000000000, 0.000000000000000000, 0.000000000000000000 ) ) ;
#11615 = CARTESIAN_POINT ( 'NONE',  ( 98.66494773507966443, -43.87633619481174918, 76.89943479971999807 ) ) ;
#11616 = VERTEX_POINT ( 'NONE', #51247 ) ;
#11617 = ORIENTED_EDGE ( 'NONE', *, *, #59812, .T. ) ;
#11618 = AXIS2_PLACEMENT_3D ( 'NONE', #3422, #38822, #24317 ) ;
#11619 = ADVANCED_FACE ( 'NONE', ( #45323 ), #64455, .T. ) ;
#11620 = DIRECTION ( 'NONE',  ( 0.000000000000000000, 0.000000000000000000, -1.000000000000000000 ) ) ;
#11621 = CARTESIAN_POINT ( 'NONE',  ( 45.77381068350503313, -48.62134037888107230, 300.4678068554150059 ) ) ;
#11622 = FACE_OUTER_BOUND ( 'NONE', #62923, .T. ) ;
#11623 = CARTESIAN_POINT ( 'NONE',  ( 116.3457274436100164, -36.88499157630047165, 151.6309475124489552 ) ) ;
#11624 = VECTOR ( 'NONE', #64177, 1000.000000000000000 ) ;
#11625 = EDGE_CURVE ( 'NONE', #68999, #70410, #86692, .T. ) ;
#11626 = FACE_OUTER_BOUND ( 'NONE', #33127, .T. ) ;
#11627 = ORIENTED_EDGE ( 'NONE', *, *, #68566, .F. ) ;
#11628 = ORIENTED_EDGE ( 'NONE', *, *, #31977, .F. ) ;
#11629 = FACE_OUTER_BOUND ( 'NONE', #19887, .T. ) ;
#11630 = ORIENTED_EDGE ( 'NONE', *, *, #3124, .T. ) ;
#11631 = ORIENTED_EDGE ( 'NONE', *, *, #64470, .T. ) ;
#11632 = DIRECTION ( 'NONE',  ( -3.100000000000000258E-29, 3.100000000000000044E-14, 1.000000000000000000 ) ) ;
#11633 = CARTESIAN_POINT ( 'NONE',  ( 97.82234778274722942, -32.72736474536957019, 207.4330118773259528 ) ) ;
#11634 = CARTESIAN_POINT ( 'NONE',  ( 85.72499999999999432, 69.84999999999999432, 342.8999999999999773 ) ) ;
#11635 = VECTOR ( 'NONE', #44943, 1000.000000000000114 ) ;
#11636 = DIRECTION ( 'NONE',  ( -1.000000000000000000, -1.734723475976808672E-15, 0.000000000000000000 ) ) ;
#11637 = LINE ( 'NONE', #52480, #79332 ) ;
#11638 = ORIENTED_EDGE ( 'NONE', *, *, #70755, .T. ) ;
#11639 = ORIENTED_EDGE ( 'NONE', *, *, #48627, .T. ) ;
#11640 = ORIENTED_EDGE ( 'NONE', *, *, #4463, .F. ) ;
#11641 = ORIENTED_EDGE ( 'NONE', *, *, #2347, .F. ) ;
#11642 = EDGE_CURVE ( 'NONE', #55229, #61739, #78555, .T. ) ;
#11643 = AXIS2_PLACEMENT_3D ( 'NONE', #63391, #84309, #28416 ) ;
#11644 = CARTESIAN_POINT ( 'NONE',  ( 106.6756582537710187, -44.91051946355214852, 245.3566617981629463 ) ) ;
#11645 = CARTESIAN_POINT ( 'NONE',  ( 96.76980119632513322, -38.49712976775982298, 91.46133956162493917 ) ) ;
#11646 = ADVANCED_FACE ( 'NONE', ( #16311 ), #73042, .T. ) ;
#11647 = CARTESIAN_POINT ( 'NONE',  ( 106.8416606513709866, -48.55305329746398257, 77.56133956162491927 ) ) ;
#11648 = CARTESIAN_POINT ( 'NONE',  ( 112.8268282670517237, -28.64838596922752245, 249.5838068554169240 ) ) ;
#11649 = CARTESIAN_POINT ( 'NONE',  ( 90.69304023831777783, -98.97427844173844846, -10.56397404668094353 ) ) ;
#11650 = CARTESIAN_POINT ( 'NONE',  ( 97.81169585860149596, -40.51742224678086046, 106.6356332503197137 ) ) ;
#11651 = CARTESIAN_POINT ( 'NONE',  ( 114.4628154322623033, -28.51554874119783634, 155.5051490854349652 ) ) ;
#11652 = FACE_OUTER_BOUND ( 'NONE', #86235, .T. ) ;
#11653 = ORIENTED_EDGE ( 'NONE', *, *, #37695, .F. ) ;
#11654 = LINE ( 'NONE', #5740, #4674 ) ;
#11655 = EDGE_LOOP ( 'NONE', ( #40444, #75966, #81341, #83460 ) ) ;
#11656 = EDGE_CURVE ( 'NONE', #53776, #41996, #24464, .T. ) ;
#11657 = EDGE_LOOP ( 'NONE', ( #15347, #20222 ) ) ;
#11658 = CARTESIAN_POINT ( 'NONE',  ( 97.81283413487385303, -40.52022386196461667, 132.6362477986331783 ) ) ;
#11659 = LINE ( 'NONE', #39353, #43073 ) ;
#11661 = ORIENTED_EDGE ( 'NONE', *, *, #40449, .F. ) ;
#11660 = CIRCLE ( 'NONE', #2914, 38.10000000000000142 ) ;
#11662 = CARTESIAN_POINT ( 'NONE',  ( 41.56648329127399677, -18.82844715994099971, 81.04262527591200183 ) ) ;
#11663 = EDGE_CURVE ( 'NONE', #26420, #80043, #17646, .T. ) ;
#11664 = EDGE_LOOP ( 'NONE', ( #23371, #83864 ) ) ;
#11665 = CARTESIAN_POINT ( 'NONE',  ( 104.4875610206461971, -26.97946579336972306, 91.28165471780177143 ) ) ;
#11666 = CARTESIAN_POINT ( 'NONE',  ( 96.08737379349030050, -38.00938547453511518, 86.43086337114897333 ) ) ;
#11667 = DIRECTION ( 'NONE',  ( -1.000000000000000000, 0.000000000000000000, 0.000000000000000000 ) ) ;
#11668 = CARTESIAN_POINT ( 'NONE',  ( 111.8298436232616240, -119.0284471599421181, -21.78219314458157285 ) ) ;
#11669 = CARTESIAN_POINT ( 'NONE',  ( 172.5664832912740110, -36.32844715994070839, 198.9256252759119832 ) ) ;
#11670 = CARTESIAN_POINT ( 'NONE',  ( 103.2241971045484092, -45.72390501747114655, 92.25562527591097250 ) ) ;
#11672 = CARTESIAN_POINT ( 'NONE',  ( 113.6717327907683597, -45.56316108038139845, 184.0994347997199725 ) ) ;
#11671 = LINE ( 'NONE', #86188, #28805 ) ;
#11673 = CARTESIAN_POINT ( 'NONE',  ( -3.174999999999664979, 17.78000000000000114, 31.75000000000000000 ) ) ;
#11675 = EDGE_CURVE ( 'NONE', #66477, #63182, #33944, .T. ) ;
#11674 = CARTESIAN_POINT ( 'NONE',  ( 6.938893903907228378E-15, 149.3723753486177088, 183.8826257785461280 ) ) ;
#11676 = ORIENTED_EDGE ( 'NONE', *, *, #83356, .F. ) ;
#11677 = CARTESIAN_POINT ( 'NONE',  ( 173.9900000000000091, 52.73749999999999716, -44.45000000000000284 ) ) ;
#11678 = LINE ( 'NONE', #87978, #58726 ) ;
#11679 = CARTESIAN_POINT ( 'NONE',  ( 115.0907168629284172, -30.61997542873368516, 134.3440372771844977 ) ) ;
#11680 = VECTOR ( 'NONE', #48194, 1000.000000000000000 ) ;
#11681 = CARTESIAN_POINT ( 'NONE',  ( 63.56670390244708813, -40.82844715994014706, 180.4678068554151196 ) ) ;
#11683 = VERTEX_POINT ( 'NONE', #5817 ) ;
#11682 = CARTESIAN_POINT ( 'NONE',  ( 117.5184129516626257, -36.12626193255995588, 228.8727681330539667 ) ) ;
#11684 = CARTESIAN_POINT ( 'NONE',  ( 99.09551545717923204, -30.55067741387680158, 145.8023164730312828 ) ) ;
#11685 = CARTESIAN_POINT ( 'NONE',  ( 116.6018303087422225, -42.36526137987677743, 279.4137205140061724 ) ) ;
#11686 = CARTESIAN_POINT ( 'NONE',  ( 102.0609898346451274, -27.53498505803861107, 141.4727681330539895 ) ) ;
#11687 = DIRECTION ( 'NONE',  ( -2.108231265501709878E-16, 5.463695987328529395E-16, 1.000000000000000000 ) ) ;
#11688 = CARTESIAN_POINT ( 'NONE',  ( 6.714856022345344400, 93.33757043186105307, -130.3836582748265869 ) ) ;
#11689 = DIRECTION ( 'NONE',  ( -2.999999999999999839E-15, 1.000000000000000000, -2.999999999999999900E-30 ) ) ;
#11690 = DIRECTION ( 'NONE',  ( 1.000000000000000000, 0.000000000000000000, 0.000000000000000000 ) ) ;
#11691 = ORIENTED_EDGE ( 'NONE', *, *, #33403, .F. ) ;
#11692 = AXIS2_PLACEMENT_3D ( 'NONE', #88653, #2303, #28646 ) ;
#11693 = ORIENTED_EDGE ( 'NONE', *, *, #68961, .T. ) ;
#11694 = EDGE_LOOP ( 'NONE', ( #49271, #26950, #49740, #17613 ) ) ;
#11695 = VECTOR ( 'NONE', #14565, 1000.000000000000114 ) ;
#11696 = VERTEX_POINT ( 'NONE', #82133 ) ;
#11697 = CARTESIAN_POINT ( 'NONE',  ( 134.0664832912739826, -9.029447159941003775, 4.925625275910997303 ) ) ;
#11698 = CARTESIAN_POINT ( 'NONE',  ( 106.5192459994187715, -25.71289806663804711, 41.12800622829193742 ) ) ;
#11699 = CARTESIAN_POINT ( 'NONE',  ( 50.97905606905892739, -31.62489322948754022, 342.9256252759109884 ) ) ;
#11700 = CARTESIAN_POINT ( 'NONE',  ( 87.66417971789877583, -139.1778880632977575, 247.6203581219589864 ) ) ;
#11702 = CARTESIAN_POINT ( 'NONE',  ( 69.05801668363947954, -139.6697599411332931, 245.6076672521240027 ) ) ;
#11701 = DIRECTION ( 'NONE',  ( 0.000000000000000000, 1.000000000000000000, 0.000000000000000000 ) ) ;
#11703 = ADVANCED_FACE ( 'NONE', ( #13073 ), #47113, .F. ) ;
#11704 = CARTESIAN_POINT ( 'NONE',  ( 114.4310042120387862, -41.05610445278038156, 237.8267055423629586 ) ) ;
#11705 = VERTEX_POINT ( 'NONE', #75297 ) ;
#11706 = VERTEX_POINT ( 'NONE', #53466 ) ;
#11707 = VERTEX_POINT ( 'NONE', #32152 ) ;
#11708 = DIRECTION ( 'NONE',  ( 0.7071067811864693020, 0.7071067811866258435, -2.899137802865049595E-29 ) ) ;
#11709 = CARTESIAN_POINT ( 'NONE',  ( 112.0660841691505993, -45.48830024005852124, 102.9895797908911277 ) ) ;
#11710 = EDGE_CURVE ( 'NONE', #13679, #72194, #30186, .T. ) ;
#11711 = DIRECTION ( 'NONE',  ( 0.2588190451025269012, 0.000000000000000000, -0.9659258262890665359 ) ) ;
#11712 = DIRECTION ( 'NONE',  ( 0.000000000000000000, -1.000000000000000000, 0.000000000000000000 ) ) ;
#11713 = CARTESIAN_POINT ( 'NONE',  ( 98.21984324360056462, -33.56503799257626497, 22.49682140113501561 ) ) ;
#11714 = VECTOR ( 'NONE', #233, 1000.000000000000000 ) ;
#11715 = CARTESIAN_POINT ( 'NONE',  ( 118.0434137139726829, 88.91291927174619047, -11.02232302911373196 ) ) ;
#11716 = FACE_OUTER_BOUND ( 'NONE', #33770, .T. ) ;
#11717 = CARTESIAN_POINT ( 'NONE',  ( 97.51798386322114709, -31.03399775848789233, 280.8984824187687082 ) ) ;
#11718 = DIRECTION ( 'NONE',  ( 0.000000000000000000, 1.000000000000000000, 6.056575390184510167E-15 ) ) ;
#11719 = ORIENTED_EDGE ( 'NONE', *, *, #34908, .T. ) ;
#11720 = CARTESIAN_POINT ( 'NONE',  ( 106.6600009669583358, -26.71630602157825862, 56.10883478359531296 ) ) ;
#11721 = VECTOR ( 'NONE', #12178, 1000.000000000000000 ) ;
#11722 = DIRECTION ( 'NONE',  ( -1.000000000000000078E-15, 1.000000000000000083E-30, 1.000000000000000000 ) ) ;
#11723 = CARTESIAN_POINT ( 'NONE',  ( 116.2008526694824582, -35.09873344310054932, 46.78523322673494533 ) ) ;
#11724 = ADVANCED_FACE ( 'NONE', ( #33503, #39420 ), #61642, .F. ) ;
#11725 = DIRECTION ( 'NONE',  ( 0.000000000000000000, 0.000000000000000000, 1.000000000000000000 ) ) ;
#11726 = DIRECTION ( 'NONE',  ( -0.7071067811865210384, 0.000000000000000000, 0.7071067811865739960 ) ) ;
#11727 = CARTESIAN_POINT ( 'NONE',  ( -11.39789362727886157, 88.16700649416421243, 118.0069991474212259 ) ) ;
#11728 = VERTEX_POINT ( 'NONE', #67126 ) ;
#11729 = DIRECTION ( 'NONE',  ( 0.000000000000000000, 0.000000000000000000, -1.000000000000000000 ) ) ;
#11730 = CARTESIAN_POINT ( 'NONE',  ( 124.5534632449514589, 58.63620287803254882, -39.13237319201113706 ) ) ;
#11731 = ORIENTED_EDGE ( 'NONE', *, *, #39589, .T. ) ;
#11732 = CARTESIAN_POINT ( 'NONE',  ( 103.2053365856880873, -46.45145584090948176, 117.2756252759109543 ) ) ;
#11733 = ORIENTED_EDGE ( 'NONE', *, *, #78019, .F. ) ;
#11734 = CARTESIAN_POINT ( 'NONE',  ( 113.7363519267670995, -42.85525508308114695, 77.64575316141092287 ) ) ;
#11735 = CIRCLE ( 'NONE', #62502, 3.968750000000020872 ) ;
#11736 = CARTESIAN_POINT ( 'NONE',  ( 97.85179084974261343, -40.61417562505091894, 87.64349320109216990 ) ) ;
#11737 = CARTESIAN_POINT ( 'NONE',  ( 103.8469135698534416, -45.55616208374542708, 93.71777378208700782 ) ) ;
#11738 = DIRECTION ( 'NONE',  ( 0.000000000000000000, 0.8660254037844379305, 0.5000000000000011102 ) ) ;
#11739 = CARTESIAN_POINT ( 'NONE',  ( 89.92341034714860371, -67.87844715994096134, 245.7176246637040151 ) ) ;
#11740 = CARTESIAN_POINT ( 'NONE',  ( 95.23451729606020422, -35.71612027476381002, 32.25848241876794020 ) ) ;
#11741 = VECTOR ( 'NONE', #60816, 1000.000000000000000 ) ;
#11742 = CARTESIAN_POINT ( 'NONE',  ( 99.09585084692569978, -30.55024265790509475, 181.8027529189448046 ) ) ;
#11743 = ORIENTED_EDGE ( 'NONE', *, *, #62139, .T. ) ;
#11744 = PLANE ( 'NONE',  #51670 ) ;
#11745 = ORIENTED_EDGE ( 'NONE', *, *, #84214, .T. ) ;
#11746 = CARTESIAN_POINT ( 'NONE',  ( 77.40046754268347229, -19.42701295173674580, 2.979899338979277612 ) ) ;
#11747 = ORIENTED_EDGE ( 'NONE', *, *, #16541, .T. ) ;
#11748 = ORIENTED_EDGE ( 'NONE', *, *, #35730, .T. ) ;
#11749 = ADVANCED_FACE ( 'NONE', ( #40761 ), #74849, .F. ) ;
#11750 = VECTOR ( 'NONE', #15346, 1000.000000000000000 ) ;
#11751 = CARTESIAN_POINT ( 'NONE',  ( 107.0667039024479834, -36.72944715994101017, 239.5838068554170093 ) ) ;
#11752 = ORIENTED_EDGE ( 'NONE', *, *, #74295, .F. ) ;
#11753 = CARTESIAN_POINT ( 'NONE',  ( 105.2318265017783716, -27.12228994480470945, 235.2270538473399313 ) ) ;
#11754 = CARTESIAN_POINT ( 'NONE',  ( 99.37624259870420929, -30.29005673034905044, 125.7706194579988619 ) ) ;
#11755 = CYLINDRICAL_SURFACE ( 'NONE', #44711, 42.54500000000000171 ) ;
#11756 = EDGE_CURVE ( 'NONE', #58495, #26148, #82469, .T. ) ;
#11757 = CARTESIAN_POINT ( 'NONE',  ( 101.1410050838726846, -27.39870825576502966, 61.51467289495899138 ) ) ;
#11758 = VECTOR ( 'NONE', #53734, 1000.000000000000000 ) ;
#11759 = CARTESIAN_POINT ( 'NONE',  ( 46.03715912545425937, -48.62818131006086020, 313.9678068554150059 ) ) ;
#11760 = ORIENTED_EDGE ( 'NONE', *, *, #75430, .T. ) ;
#11761 = DIRECTION ( 'NONE',  ( 0.000000000000000000, 0.000000000000000000, 1.000000000000000000 ) ) ;
#11762 = EDGE_CURVE ( 'NONE', #31158, #15433, #11267, .T. ) ;
#11763 = DIRECTION ( 'NONE',  ( 0.000000000000000000, 0.000000000000000000, 1.000000000000000000 ) ) ;
#11764 = ORIENTED_EDGE ( 'NONE', *, *, #51117, .F. ) ;
#11765 = CARTESIAN_POINT ( 'NONE',  ( -48.02966122971777452, 100.5999999999999659, 106.4272185163641780 ) ) ;
#11766 = CARTESIAN_POINT ( 'NONE',  ( 27.27158787008325902, 127.0000000000000000, -5.920431057502157584E-15 ) ) ;
#11767 = CARTESIAN_POINT ( 'NONE',  ( 96.91023542590092177, -30.67149048741783091, 280.8984824187682534 ) ) ;
#11768 = CARTESIAN_POINT ( 'NONE',  ( 53.06670390244699576, -67.87844715994100397, 222.2178068554179902 ) ) ;
#11769 = CARTESIAN_POINT ( 'NONE',  ( -7.661254700127833495, 69.45253841614081125, 317.6630000000000109 ) ) ;
#11770 = CARTESIAN_POINT ( 'NONE',  ( 69.63919639214307722, 92.07499999999998863, 0.000000000000000000 ) ) ;
#11771 = CARTESIAN_POINT ( 'NONE',  ( 100.7304913082922440, -30.25890808522221320, 270.1276579233149278 ) ) ;
#11773 = CARTESIAN_POINT ( 'NONE',  ( 109.6783822832554591, -47.44587409406599221, 83.75467289495897205 ) ) ;
#11772 = PLANE ( 'NONE',  #63503 ) ;
#11774 = CARTESIAN_POINT ( 'NONE',  ( 113.5620303038072905, 69.49466463746259137, 64.41016170726432222 ) ) ;
#11775 = CARTESIAN_POINT ( 'NONE',  ( 103.4531379826000261, -46.55545292317445671, 142.2956252759109645 ) ) ;
#11776 = ORIENTED_EDGE ( 'NONE', *, *, #45978, .T. ) ;
#11778 = EDGE_CURVE ( 'NONE', #64418, #14919, #19883, .T. ) ;
#11777 = DIRECTION ( 'NONE',  ( 0.000000000000000000, 0.000000000000000000, -1.000000000000000000 ) ) ;
#11779 = ORIENTED_EDGE ( 'NONE', *, *, #64075, .T. ) ;
#11780 = CARTESIAN_POINT ( 'NONE',  ( 83.56670390244801183, -36.72944715994108122, 218.8274735512160589 ) ) ;
#11781 = VECTOR ( 'NONE', #53658, 1000.000000000000000 ) ;
#11782 = LINE ( 'NONE', #11325, #74010 ) ;
#11783 = EDGE_CURVE ( 'NONE', #40177, #77354, #15674, .T. ) ;
#11784 = CARTESIAN_POINT ( 'NONE',  ( 103.1875000000000000, 117.4749999999999943, 3.602774393244745134E-13 ) ) ;
#11785 = ORIENTED_EDGE ( 'NONE', *, *, #56860, .T. ) ;
#11786 = CARTESIAN_POINT ( 'NONE',  ( 41.56648329127398966, -27.82844715994070484, 138.9256252759119832 ) ) ;
#11788 = VERTEX_POINT ( 'NONE', #52571 ) ;
#11787 = CARTESIAN_POINT ( 'NONE',  ( 102.0606772939666627, -27.53441096011033906, 145.4727681330539610 ) ) ;
#11789 = CARTESIAN_POINT ( 'NONE',  ( 0.000000000000000000, 125.7300000000000040, 0.000000000000000000 ) ) ;
#11790 = CARTESIAN_POINT ( 'NONE',  ( -130.3837941446097375, 93.33921197991992358, -6.712224447894871382 ) ) ;
#11791 = AXIS2_PLACEMENT_3D ( 'NONE', #56899, #84637, #21962 ) ;
#11792 = LINE ( 'NONE', #71898, #31486 ) ;
#11793 = DIRECTION ( 'NONE',  ( -1.000000000000000000, -5.800000000000000483E-29, 2.900000000000000265E-14 ) ) ;
#11794 = EDGE_LOOP ( 'NONE', ( #51067, #20486, #70340, #56437 ) ) ;
#11795 = VECTOR ( 'NONE', #46695, 1000.000000000000000 ) ;
#11796 = CARTESIAN_POINT ( 'NONE',  ( 95.75500511041516916, -40.34669435480882527, 131.5727681330539554 ) ) ;
#11797 = APPLICATION_PROTOCOL_DEFINITION ( 'draft international standard', 'automotive_design', 1998, #18985 ) ;
#11798 = CARTESIAN_POINT ( 'NONE',  ( 90.44969454456408187, -20.11243780205710507, 239.5838068554175209 ) ) ;
#11799 = CARTESIAN_POINT ( 'NONE',  ( 46.32460016641721978, -48.34074026909785005, 300.4678068554150059 ) ) ;
#11800 = VERTEX_POINT ( 'NONE', #80778 ) ;
#11801 = ORIENTED_EDGE ( 'NONE', *, *, #67842, .F. ) ;
#11802 = DIRECTION ( 'NONE',  ( 1.000000000000000000, 0.000000000000000000, 0.000000000000000000 ) ) ;
#11803 = PRODUCT_DEFINITION_SHAPE ( 'NONE', 'NONE',  #76646 ) ;
#11804 = CARTESIAN_POINT ( 'NONE',  ( 111.0197563349041872, -27.48142275213628949, 249.7547965408143966 ) ) ;
#11805 = CARTESIAN_POINT ( 'NONE',  ( 113.1782937260175288, -44.75186862798841503, 158.0939586047068985 ) ) ;
#11806 = PLANE ( 'NONE',  #18316 ) ;
#11807 = VECTOR ( 'NONE', #51578, 1000.000000000000000 ) ;
#11809 = CARTESIAN_POINT ( 'NONE',  ( -12.69999999999999929, 81.71107837960109066, -117.8738102209307499 ) ) ;
#11808 = PLANE ( 'NONE',  #37805 ) ;
#11810 = CARTESIAN_POINT ( 'NONE',  ( -129.9368274816651478, 82.54999999999999716, 12.69999999999954809 ) ) ;
#11811 = ORIENTED_EDGE ( 'NONE', *, *, #36868, .F. ) ;
#11812 = DIRECTION ( 'NONE',  ( 1.000000000000000000, 0.000000000000000000, 0.000000000000000000 ) ) ;
#11813 = EDGE_CURVE ( 'NONE', #59337, #80549, #51934, .T. ) ;
#11814 = CARTESIAN_POINT ( 'NONE',  ( 101.5632356570521324, -44.81509498605967678, 193.1013395616249682 ) ) ;
#11815 = VECTOR ( 'NONE', #14581, 1000.000000000000000 ) ;
#11817 = EDGE_LOOP ( 'NONE', ( #27174, #2365, #77163, #58800 ) ) ;
#11816 = LINE ( 'NONE', #60391, #28366 ) ;
#11818 = CARTESIAN_POINT ( 'NONE',  ( 113.9027609268605659, -43.72435554967452731, 69.19276813305297935 ) ) ;
#11819 = CARTESIAN_POINT ( 'NONE',  ( 111.0144279432724232, -45.91752097597848348, 52.89941656328505815 ) ) ;
#11820 = CARTESIAN_POINT ( 'NONE',  ( 69.95483947742927455, -138.0502943369556021, 247.6584922829669893 ) ) ;
#11821 = CIRCLE ( 'NONE', #39373, 16.00000000000000000 ) ;
#11822 = CARTESIAN_POINT ( 'NONE',  ( 97.79819224205189698, -40.48430588183206424, 22.63277894479249142 ) ) ;
#11823 = ORIENTED_EDGE ( 'NONE', *, *, #87471, .T. ) ;
#11824 = CARTESIAN_POINT ( 'NONE',  ( 107.0667039024479834, -36.72944715994101017, 239.5838068554170093 ) ) ;
#11825 = VERTEX_POINT ( 'NONE', #54361 ) ;
#11826 = EDGE_LOOP ( 'NONE', ( #89248, #73908, #7175, #37340 ) ) ;
#11827 = CARTESIAN_POINT ( 'NONE',  ( 106.4165995140572250, -45.56720307917569102, 218.9501547344689527 ) ) ;
#11828 = CARTESIAN_POINT ( 'NONE',  ( 113.1804603017864252, -44.75025694503620599, 54.09380354789409751 ) ) ;
#11829 = ADVANCED_FACE ( 'NONE', ( #40311 ), #27257, .T. ) ;
#11830 = DIRECTION ( 'NONE',  ( 1.000000000000000000, -5.337610695313248426E-16, 0.000000000000000000 ) ) ;
#11831 = DIRECTION ( 'NONE',  ( -0.5000000000000061062, 0.000000000000000000, 0.8660254037844351549 ) ) ;
#11832 = CARTESIAN_POINT ( 'NONE',  ( -41.60202597009397607, 64.60000000000000853, 50.85338361873603219 ) ) ;
#11834 = VERTEX_POINT ( 'NONE', #81235 ) ;
#11833 = CIRCLE ( 'NONE', #62604, 11.57110091390434192 ) ;
#11835 = DIRECTION ( 'NONE',  ( 0.000000000000000000, 0.000000000000000000, 1.000000000000000000 ) ) ;
#11836 = LINE ( 'NONE', #31373, #82193 ) ;
#11837 = ORIENTED_EDGE ( 'NONE', *, *, #65372, .F. ) ;
#11838 = CARTESIAN_POINT ( 'NONE',  ( 98.42358855985509081, -42.06826316073455274, 11.76800622829193799 ) ) ;
#11839 = ORIENTED_EDGE ( 'NONE', *, *, #29925, .T. ) ;
#11840 = ORIENTED_EDGE ( 'NONE', *, *, #23054, .T. ) ;
#11842 = EDGE_CURVE ( 'NONE', #28950, #22788, #24423, .T. ) ;
#11841 = CARTESIAN_POINT ( 'NONE',  ( 98.99928044157054785, -35.48447157832033128, 264.0223760838769635 ) ) ;
#11843 = EDGE_CURVE ( 'NONE', #733, #43944, #18525, .T. ) ;
#11844 = CARTESIAN_POINT ( 'NONE',  ( 191.6377717143134589, -48.82844715994099971, 307.9888746672805269 ) ) ;
#11845 = CARTESIAN_POINT ( 'NONE',  ( 111.8077268321493563, -46.78591733285071541, 137.9270538473399768 ) ) ;
#11846 = CARTESIAN_POINT ( 'NONE',  ( 23.08473575203844064, 77.94038194589714408, 301.6578082054804213 ) ) ;
#11847 = DIRECTION ( 'NONE',  ( -1.000000000000000000, 0.000000000000000000, 0.000000000000000000 ) ) ;
#11848 = DIRECTION ( 'NONE',  ( 0.000000000000000000, 0.5000000000000087708, -0.8660254037844334896 ) ) ;
#11849 = AXIS2_PLACEMENT_3D ( 'NONE', #32217, #73112, #88108 ) ;
#11850 = CARTESIAN_POINT ( 'NONE',  ( 103.8062037941931095, -48.17417041148343060, 213.3556252759109668 ) ) ;
#11851 = CARTESIAN_POINT ( 'NONE',  ( 0.000000000000000000, 65.60000000000000853, -53.97512327982435210 ) ) ;
#11852 = EDGE_LOOP ( 'NONE', ( #9730, #83809 ) ) ;
#11853 = AXIS2_PLACEMENT_3D ( 'NONE', #81263, #79476, #31288 ) ;
#11854 = CARTESIAN_POINT ( 'NONE',  ( 116.7149026195978792, -32.57661448200846621, 75.14991099019697174 ) ) ;
#11855 = DIRECTION ( 'NONE',  ( 0.000000000000000000, 1.000000000000000000, 0.000000000000000000 ) ) ;
#11856 = EDGE_CURVE ( 'NONE', #21233, #1886, #2646, .T. ) ;
#11857 = ORIENTED_EDGE ( 'NONE', *, *, #77098, .F. ) ;
#11858 = VERTEX_POINT ( 'NONE', #12174 ) ;
#11859 = B_SPLINE_CURVE_WITH_KNOTS ( 'NONE', 3,
 ( #4092, #2772, #72251, #36832, #30466, #58165 ),
 .UNSPECIFIED., .F., .F.,
 ( 4, 2, 4 ),
 ( -0.008545295454838610846, -0.004274282335290478449, 0.000000000000000000 ),
 .UNSPECIFIED. ) ;
#11860 = VERTEX_POINT ( 'NONE', #35740 ) ;
#11861 = CARTESIAN_POINT ( 'NONE',  ( 115.8239080364990059, -31.72738345397315385, 159.2397836617124085 ) ) ;
#11862 = DIRECTION ( 'NONE',  ( 0.000000000000000000, 1.000000000000000000, 0.000000000000000000 ) ) ;
#11863 = FACE_OUTER_BOUND ( 'NONE', #31505, .T. ) ;
#11864 = ADVANCED_FACE ( 'NONE', ( #14422 ), #27143, .T. ) ;
#11865 = CARTESIAN_POINT ( 'NONE',  ( 115.0306645585770298, -38.52089976383655312, 146.4680903695919767 ) ) ;
#11866 = CARTESIAN_POINT ( 'NONE',  ( 97.45308667932049218, -40.90817919144255654, 227.6527681330539679 ) ) ;
#11867 = CIRCLE ( 'NONE', #85874, 4.762500000000001066 ) ;
#11868 = DIRECTION ( 'NONE',  ( 0.000000000000000000, 1.000000000000000000, 0.000000000000000000 ) ) ;
#11869 = ORIENTED_EDGE ( 'NONE', *, *, #80273, .T. ) ;
#11870 = CARTESIAN_POINT ( 'NONE',  ( 130.5540562089606738, 95.23006786499114185, 0.8254869398584661067 ) ) ;
#11871 = CARTESIAN_POINT ( 'NONE',  ( 204.2160000000000082, 52.73749999999999716, -48.41875000000000284 ) ) ;
#11872 = ORIENTED_EDGE ( 'NONE', *, *, #2900, .F. ) ;
#11874 = ORIENTED_EDGE ( 'NONE', *, *, #33000, .T. ) ;
#11873 = VECTOR ( 'NONE', #21298, 999.9999999999998863 ) ;
#11875 = AXIS2_PLACEMENT_3D ( 'NONE', #17373, #86429, #45056 ) ;
#11876 = DIRECTION ( 'NONE',  ( 0.000000000000000000, -1.000000000000000000, 0.000000000000000000 ) ) ;
#11877 = ORIENTED_EDGE ( 'NONE', *, *, #84996, .T. ) ;
#11878 = ORIENTED_EDGE ( 'NONE', *, *, #24199, .F. ) ;
#11879 = CARTESIAN_POINT ( 'NONE',  ( 117.0290271953209498, -38.08751257484902908, 9.718958609244278790 ) ) ;
#11880 = CARTESIAN_POINT ( 'NONE',  ( 57.56670390244816815, -42.82844715994040286, 295.7178068554150627 ) ) ;
#11881 = DIRECTION ( 'NONE',  ( 1.000000000000000078E-15, -1.000000000000000000, 0.000000000000000000 ) ) ;
#11882 = CARTESIAN_POINT ( 'NONE',  ( 115.8611420101186269, -34.56920459637935750, 163.4286103042669822 ) ) ;
#11883 = CARTESIAN_POINT ( 'NONE',  ( 97.44607596320715004, -32.59944340835617282, 16.00419670448194154 ) ) ;
#11885 = ADVANCED_FACE ( 'NONE', ( #36199 ), #62996, .T. ) ;
#11884 = CARTESIAN_POINT ( 'NONE',  ( 105.7978665782029282, -26.72425971154408941, 126.1774233227885276 ) ) ;
#11886 = VERTEX_POINT ( 'NONE', #63913 ) ;
#11887 = ADVANCED_FACE ( 'NONE', ( #56627 ), #76184, .F. ) ;
#11888 = DIRECTION ( 'NONE',  ( 0.000000000000000000, 0.000000000000000000, 1.000000000000000000 ) ) ;
#11889 = AXIS2_PLACEMENT_3D ( 'NONE', #160, #603, #28771 ) ;
#11890 = VERTEX_POINT ( 'NONE', #70729 ) ;
#11891 = EDGE_CURVE ( 'NONE', #52784, #11922, #48008, .T. ) ;
#11892 = DIRECTION ( 'NONE',  ( -1.000000000000000078E-15, 1.000000000000000000, 0.000000000000000000 ) ) ;
#11893 = ORIENTED_EDGE ( 'NONE', *, *, #52546, .F. ) ;
#11894 = FACE_OUTER_BOUND ( 'NONE', #30527, .T. ) ;
#11895 = ADVANCED_FACE ( 'NONE', ( #8501 ), #41643, .F. ) ;
#11896 = FACE_OUTER_BOUND ( 'NONE', #87984, .T. ) ;
#11897 = FACE_OUTER_BOUND ( 'NONE', #9444, .T. ) ;
#11898 = CARTESIAN_POINT ( 'NONE',  ( 0.000000000000000000, 17.78000000000000114, 0.000000000000000000 ) ) ;
#11899 = ORIENTED_EDGE ( 'NONE', *, *, #59314, .F. ) ;
#11900 = CARTESIAN_POINT ( 'NONE',  ( 118.0989925035467252, -37.71898322177068508, 33.74324432352998571 ) ) ;
#11901 = CARTESIAN_POINT ( 'NONE',  ( 117.3094150574360128, -38.89169797369248727, 59.66133956162595098 ) ) ;
#11903 = LINE ( 'NONE', #80960, #35481 ) ;
#11902 = DIRECTION ( 'NONE',  ( 0.000000000000000000, 0.000000000000000000, 1.000000000000000000 ) ) ;
#11904 = DIRECTION ( 'NONE',  ( 0.000000000000000000, 0.000000000000000000, 1.000000000000000000 ) ) ;
#11905 = LINE ( 'NONE', #53192, #69913 ) ;
#11906 = CARTESIAN_POINT ( 'NONE',  ( 88.90000000000000568, 69.84999999999999432, 346.0750000000000455 ) ) ;
#11907 = CYLINDRICAL_SURFACE ( 'NONE', #27175, 5.000000000000004441 ) ;
#11908 = DIRECTION ( 'NONE',  ( 0.7071067811865453523, 0.7071067811865496822, 0.000000000000000000 ) ) ;
#11909 = ORIENTED_EDGE ( 'NONE', *, *, #18263, .F. ) ;
#11910 = CARTESIAN_POINT ( 'NONE',  ( 110.5699785786504918, -46.63284631861461804, 37.84705384733994293 ) ) ;
#11911 = CARTESIAN_POINT ( 'NONE',  ( 95.40797249125856183, -38.85400393358575855, 197.4699109901969791 ) ) ;
#11912 = CARTESIAN_POINT ( 'NONE',  ( 98.07812720205548374, -31.40528397058157850, 81.90133956162493689 ) ) ;
#11913 = CIRCLE ( 'NONE', #17682, 3.968749999999992895 ) ;
#11915 = CARTESIAN_POINT ( 'NONE',  ( 134.0664832912740110, -8.350947159940998787, 308.6356252759119911 ) ) ;
#11914 = DIRECTION ( 'NONE',  ( 0.000000000000000000, 1.000000000000000000, 0.000000000000000000 ) ) ;
#11916 = CARTESIAN_POINT ( 'NONE',  ( 50.42303506447345285, 65.60000000000000853, -73.21698938693724301 ) ) ;
#11917 = CARTESIAN_POINT ( 'NONE',  ( 30.48091746481830100, -49.32844715994148288, 300.4678068554150059 ) ) ;
#11918 = VERTEX_POINT ( 'NONE', #69378 ) ;
#11919 = ADVANCED_FACE ( 'NONE', ( #42541 ), #77097, .F. ) ;
#11920 = CARTESIAN_POINT ( 'NONE',  ( 102.0841886111852688, -27.63463957783716651, 96.46324432352997746 ) ) ;
#11922 = VERTEX_POINT ( 'NONE', #41200 ) ;
#11921 = CARTESIAN_POINT ( 'NONE',  ( 10.38443768554948932, 89.86159749365012317, 130.1424040926225132 ) ) ;
#11923 = CARTESIAN_POINT ( 'NONE',  ( 98.85650974919605005, -29.36329775763232774, 231.7565776568629587 ) ) ;
#11924 = CARTESIAN_POINT ( 'NONE',  ( 117.0608242671911512, -38.08101263064929043, 254.7201668676480324 ) ) ;
#11925 = PRODUCT_DEFINITION_SHAPE ( 'NONE', 'NONE',  #89945 ) ;
#11926 = CARTESIAN_POINT ( 'NONE',  ( 111.0139104026190182, -45.91774244734033061, 147.8993717799802994 ) ) ;
#11927 = PLANE ( 'NONE',  #6568 ) ;
#11928 = DIRECTION ( 'NONE',  ( -6.524622321627019585E-16, -3.741823817616790462E-31, -1.000000000000000000 ) ) ;
#11929 = VECTOR ( 'NONE', #47454, 1000.000000000000000 ) ;
#11930 = DIRECTION ( 'NONE',  ( 0.000000000000000000, 0.000000000000000000, 1.000000000000000000 ) ) ;
#11931 = CARTESIAN_POINT ( 'NONE',  ( 173.9900000000000091, 52.73749999999999716, -26.11912895322935313 ) ) ;
#11932 = CARTESIAN_POINT ( 'NONE',  ( 117.1372161989437899, -34.25576096370539148, 164.0061014663879746 ) ) ;
#11933 = ORIENTED_EDGE ( 'NONE', *, *, #78243, .T. ) ;
#11934 = ORIENTED_EDGE ( 'NONE', *, *, #35199, .T. ) ;
#11935 = AXIS2_PLACEMENT_3D ( 'NONE', #37166, #58052, #78963 ) ;
#11936 = CARTESIAN_POINT ( 'NONE',  ( 99.74759560186635099, -41.77880479991928553, 123.2387261630399564 ) ) ;
#11937 = CONICAL_SURFACE ( 'NONE', #61203, 1.624999999999987566, 1.029744258676650093 ) ;
#11938 = DIRECTION ( 'NONE',  ( 4.194175870806139918E-14, -1.000000000000000000, 0.000000000000000000 ) ) ;
#11939 = EDGE_CURVE ( 'NONE', #51458, #35086, #21688, .T. ) ;
#11941 = DIRECTION ( 'NONE',  ( 0.000000000000000000, -1.000000000000000000, 0.000000000000000000 ) ) ;
#11940 = CARTESIAN_POINT ( 'NONE',  ( 105.8561066403589308, -27.02385992090132305, 266.1756252759109884 ) ) ;
#11942 = LINE ( 'NONE', #75061, #75408 ) ;
#11943 = DIRECTION ( 'NONE',  ( 4.299999999999999979E-14, -1.000000000000000000, 0.000000000000000000 ) ) ;
#11944 = ADVANCED_FACE ( 'NONE', ( #62554 ), #20339, .F. ) ;
#11945 = AXIS2_PLACEMENT_3D ( 'NONE', #82521, #20283, #82963 ) ;
#11946 = CARTESIAN_POINT ( 'NONE',  ( 61.00843881761244347, 49.07499999999999574, -53.97512327982435210 ) ) ;
#11947 = EDGE_CURVE ( 'NONE', #30264, #2214, #84372, .T. ) ;
#11948 = DIRECTION ( 'NONE',  ( 1.000000000000000000, 1.314511288311335947E-16, 0.000000000000000000 ) ) ;
#11949 = CARTESIAN_POINT ( 'NONE',  ( 97.81168895331838087, -40.51742574516882200, 287.6356252759109680 ) ) ;
#11950 = CARTESIAN_POINT ( 'NONE',  ( 0.000000000000000000, 184.0000000000000000, 85.23828826961327820 ) ) ;
#11951 = CARTESIAN_POINT ( 'NONE',  ( 97.40233316251681117, -42.04621543282991780, 176.7146728949589658 ) ) ;
#11952 = DIRECTION ( 'NONE',  ( -3.386875084296745512E-15, 0.000000000000000000, 1.000000000000000000 ) ) ;
#11953 = VERTEX_POINT ( 'NONE', #7155 ) ;
#11954 = VERTEX_POINT ( 'NONE', #56168 ) ;
#11955 = ADVANCED_FACE ( 'NONE', ( #35285 ), #15318, .F. ) ;
#11956 = ADVANCED_FACE ( 'NONE', ( #68927 ), #14875, .T. ) ;
#11957 = CARTESIAN_POINT ( 'NONE',  ( -95.16685018566032284, 70.52074417248462623, -89.37727808479068869 ) ) ;
#11958 = CARTESIAN_POINT ( 'NONE',  ( 80.81782300817755527, -21.40255221908232741, 8.160479982078024719 ) ) ;
#11959 = LINE ( 'NONE', #67345, #66433 ) ;
#11960 = CYLINDRICAL_SURFACE ( 'NONE', #58408, 2.117000000000000881 ) ;
#11961 = ADVANCED_FACE ( 'NONE', ( #22143, #28027 ), #77537, .T. ) ;
#11962 = CARTESIAN_POINT ( 'NONE',  ( 97.60805412390877223, -39.98290213189324049, 96.59010508770597880 ) ) ;
#11963 = EDGE_LOOP ( 'NONE', ( #25263, #37882, #61119, #52904 ) ) ;
#11964 = CARTESIAN_POINT ( 'NONE',  ( -29.99999999999998224, 127.0000000000000000, 113.8826257785461280 ) ) ;
#11965 = EDGE_CURVE ( 'NONE', #20160, #8910, #21231, .T. ) ;
#11966 = CARTESIAN_POINT ( 'NONE',  ( 96.13794759894150843, -35.07228238994858316, 221.1946728949589840 ) ) ;
#11967 = DIRECTION ( 'NONE',  ( 0.7071067708032388044, 0.0001211784769831114530, 0.7071067811865423547 ) ) ;
#11968 = ORIENTED_EDGE ( 'NONE', *, *, #24195, .T. ) ;
#11969 = ORIENTED_EDGE ( 'NONE', *, *, #14623, .T. ) ;
#11970 = VECTOR ( 'NONE', #72144, 1000.000000000000000 ) ;
#11971 = CARTESIAN_POINT ( 'NONE',  ( -12.27785138262897924, 85.41117304334655103, 117.9185570544176898 ) ) ;
#11972 = CARTESIAN_POINT ( 'NONE',  ( 177.0371591254545933, -48.62818131005479927, 117.4678068554150485 ) ) ;
#11973 = CARTESIAN_POINT ( 'NONE',  ( 101.9933085522700082, -45.44587970176321789, 167.1565046981921796 ) ) ;
#11974 = EDGE_CURVE ( 'NONE', #49665, #21567, #65244, .T. ) ;
#11975 = CARTESIAN_POINT ( 'NONE',  ( 101.8554017947406862, -30.44658510084856218, 38.44523322673398980 ) ) ;
#11976 = CARTESIAN_POINT ( 'NONE',  ( 98.26250712568560175, -31.04002435091596368, 141.8699109901969564 ) ) ;
#11977 = CARTESIAN_POINT ( 'NONE',  ( 118.5256205435843526, -36.72944715994100306, 293.2242906452868851 ) ) ;
#11978 = EDGE_LOOP ( 'NONE', ( #56740, #68843, #7740, #72861 ) ) ;
#11979 = CARTESIAN_POINT ( 'NONE',  ( 107.0664832912750057, -36.72944715993903486, 0.7256252759109708128 ) ) ;
#11980 = DIRECTION ( 'NONE',  ( 1.000000000000000000, 0.000000000000000000, 0.000000000000000000 ) ) ;
#11981 = ORIENTED_EDGE ( 'NONE', *, *, #17799, .T. ) ;
#11982 = VERTEX_POINT ( 'NONE', #43890 ) ;
#11983 = AXIS2_PLACEMENT_3D ( 'NONE', #87924, #25690, #53368 ) ;
#11984 = LINE ( 'NONE', #79699, #69156 ) ;
#11985 = VERTEX_POINT ( 'NONE', #72515 ) ;
#11986 = ORIENTED_EDGE ( 'NONE', *, *, #21379, .F. ) ;
#11987 = CARTESIAN_POINT ( 'NONE',  ( 56.06670390244700997, -79.67844715994098692, 155.2178068554179902 ) ) ;
#11988 = CARTESIAN_POINT ( 'NONE',  ( 111.0503013157718044, -29.17396400730615369, 59.11241982807696616 ) ) ;
#11989 = CARTESIAN_POINT ( 'NONE',  ( 117.4347420270075730, -35.18426962645584410, 218.9441967044829482 ) ) ;
#11990 = CARTESIAN_POINT ( 'NONE',  ( 108.9412587213991088, -26.46057952311815953, 164.9327681330529742 ) ) ;
#11992 = CARTESIAN_POINT ( 'NONE',  ( 116.5819428025096585, -42.35350697836285860, 279.4137205140061724 ) ) ;
#11991 = FACE_OUTER_BOUND ( 'NONE', #12760, .T. ) ;
#11993 = CARTESIAN_POINT ( 'NONE',  ( 90.06670420047024095, -102.7784471599409670, 222.2178068554179902 ) ) ;
#11994 = CARTESIAN_POINT ( 'NONE',  ( 34.92499999999999716, 66.67499999999999716, 292.1000000000000227 ) ) ;
#11995 = EDGE_LOOP ( 'NONE', ( #40838, #22846, #13113, #42994 ) ) ;
#11996 = CIRCLE ( 'NONE', #83079, 0.2999999999999943823 ) ;
#11997 = EDGE_CURVE ( 'NONE', #20780, #31941, #71624, .T. ) ;
#11998 = VERTEX_POINT ( 'NONE', #46449 ) ;
#11999 = ADVANCED_FACE ( 'NONE', ( #15765 ), #81018, .F. ) ;
#12000 = AXIS2_PLACEMENT_3D ( 'NONE', #33769, #75106, #12895 ) ;
#12001 = FACE_OUTER_BOUND ( 'NONE', #89138, .T. ) ;
#12002 = CARTESIAN_POINT ( 'NONE',  ( 98.90817802506259682, -30.16829472858045591, 240.7870538473399620 ) ) ;
#12003 = ORIENTED_EDGE ( 'NONE', *, *, #9830, .F. ) ;
#12004 = CARTESIAN_POINT ( 'NONE',  ( 101.4252639664679094, -46.23501037223531540, 207.1622919425779514 ) ) ;
#12005 = CYLINDRICAL_SURFACE ( 'NONE', #7957, 4.750000000000004441 ) ;
#12006 = CARTESIAN_POINT ( 'NONE',  ( -23.05114358122109053, 56.73092669637083674, 30.33591271885418905 ) ) ;
#12007 = CYLINDRICAL_SURFACE ( 'NONE', #87054, 2.750000000000002665 ) ;
#12008 = CARTESIAN_POINT ( 'NONE',  ( 82.54999999999999716, 69.84999999999999432, 346.9005000000000223 ) ) ;
#12010 = CARTESIAN_POINT ( 'NONE',  ( 9.261585182541617556, 239.0000000000000000, 152.5407914452011653 ) ) ;
#12009 = CARTESIAN_POINT ( 'NONE',  ( 109.2259222164322523, -28.99876954086582614, 277.6356252759110248 ) ) ;
#12011 = DIRECTION ( 'NONE',  ( -0.1811243269278930978, 0.9834602067165288952, 0.000000000000000000 ) ) ;
#12012 = DIRECTION ( 'NONE',  ( -0.8660254037844377084, -0.5000000000000016653, 1.550000000000002231E-14 ) ) ;
#12013 = CIRCLE ( 'NONE', #43891, 6.999999999999997335 ) ;
#12014 = DIRECTION ( 'NONE',  ( -0.7071067812163264188, 0.7071067811567686157, -7.071067812163272297E-16 ) ) ;
#12015 = DIRECTION ( 'NONE',  ( -0.0001211784769825758164, 0.7071067708032326982, 0.7071067811865484609 ) ) ;
#12016 = LINE ( 'NONE', #86981, #86588 ) ;
#12017 = CARTESIAN_POINT ( 'NONE',  ( 108.4174892589812487, -26.73503592869370493, 75.96895860870016293 ) ) ;
#12019 = VERTEX_POINT ( 'NONE', #44333 ) ;
#12018 = CARTESIAN_POINT ( 'NONE',  ( -12.37521547983011416, 85.43365698736769787, -117.9083787315452412 ) ) ;
#12020 = FACE_OUTER_BOUND ( 'NONE', #40734, .T. ) ;
#12021 = CARTESIAN_POINT ( 'NONE',  ( 116.5468340722667051, -41.20284764396129873, 228.4756252759109714 ) ) ;
#12022 = CARTESIAN_POINT ( 'NONE',  ( 117.3387810265436144, -32.64853063025485369, 95.13943479972097350 ) ) ;
#12023 = CARTESIAN_POINT ( 'NONE',  ( 113.2457357650714727, -45.17988020286173878, 224.0784824187679476 ) ) ;
#12024 = CARTESIAN_POINT ( 'NONE',  ( 44.45000000000000284, 111.1250000000000000, 219.0749999999999886 ) ) ;
#12025 = DIRECTION ( 'NONE',  ( 0.000000000000000000, 0.000000000000000000, -1.000000000000000000 ) ) ;
#12027 = CARTESIAN_POINT ( 'NONE',  ( 116.3212776292296127, -32.94146857471318413, 287.6356252759109680 ) ) ;
#12026 = CARTESIAN_POINT ( 'NONE',  ( 183.5150000000000148, 14.63749999999999929, -52.38749999999999574 ) ) ;
#12028 = CARTESIAN_POINT ( 'NONE',  ( 196.2150000000000034, 30.98800000000000310, 44.45000000000000284 ) ) ;
#12029 = FACE_OUTER_BOUND ( 'NONE', #57904, .T. ) ;
#12030 = ORIENTED_EDGE ( 'NONE', *, *, #53430, .T. ) ;
#12031 = VERTEX_POINT ( 'NONE', #86144 ) ;
#12032 = CARTESIAN_POINT ( 'NONE',  ( 108.4402549024021312, -27.77817906387560143, 144.3657531614099412 ) ) ;
#12034 = VERTEX_POINT ( 'NONE', #16212 ) ;
#12033 = CARTESIAN_POINT ( 'NONE',  ( 107.0667039024470313, -104.2784471599409528, 250.2178068554179902 ) ) ;
#12035 = CARTESIAN_POINT ( 'NONE',  ( -27.27158787008326968, 184.0000000000000000, 111.9860621927989826 ) ) ;
#12036 = CARTESIAN_POINT ( 'NONE',  ( 102.3703197837810848, -46.01248081495474906, 123.2041967044829818 ) ) ;
#12037 = CARTESIAN_POINT ( 'NONE',  ( 105.7809510460201210, -24.27257308096163868, 321.6188579224977389 ) ) ;
#12038 = CARTESIAN_POINT ( 'NONE',  ( 107.0664832912739968, -18.82844715994099971, 330.8831252759119934 ) ) ;
#12039 = CARTESIAN_POINT ( 'NONE',  ( -492.0614999999999668, 93.66249999999999432, 85.72499999999999432 ) ) ;
#12040 = CARTESIAN_POINT ( 'NONE',  ( 117.0718954851608373, -35.46248235549226990, 109.9272919426389734 ) ) ;
#12041 = CARTESIAN_POINT ( 'NONE',  ( 106.9359508110862720, -26.91635713860562973, 60.08705384733998045 ) ) ;
#12042 = ORIENTED_EDGE ( 'NONE', *, *, #42488, .F. ) ;
#12043 = ORIENTED_EDGE ( 'NONE', *, *, #2128, .T. ) ;
#12044 = ORIENTED_EDGE ( 'NONE', *, *, #20064, .F. ) ;
#12045 = CIRCLE ( 'NONE', #26494, 5.500000000000000888 ) ;
#12046 = DIRECTION ( 'NONE',  ( -0.7071067811865175967, -0.7071067811865774377, -7.071067811865168663E-16 ) ) ;
#12048 = DIRECTION ( 'NONE',  ( 0.000000000000000000, -1.000000000000000000, 0.000000000000000000 ) ) ;
#12047 = CARTESIAN_POINT ( 'NONE',  ( 108.5509251780138129, -26.47246927008498929, 145.9737205140059473 ) ) ;
#12049 = DIRECTION ( 'NONE',  ( 0.000000000000000000, 0.000000000000000000, 1.000000000000000000 ) ) ;
#12050 = EDGE_CURVE ( 'NONE', #16560, #9081, #22583, .T. ) ;
#12051 = CARTESIAN_POINT ( 'NONE',  ( 7.399926448127667200, 72.22026871922481916, -130.3465752436562468 ) ) ;
#12052 = EDGE_CURVE ( 'NONE', #18138, #10974, #65881, .T. ) ;
#12053 = LINE ( 'NONE', #12503, #6838 ) ;
#12054 = EDGE_CURVE ( 'NONE', #68641, #88437, #34847, .T. ) ;
#12055 = CARTESIAN_POINT ( 'NONE',  ( 83.54193218351797157, 95.25015226514366873, 84.12159398442744873 ) ) ;
#12056 = CARTESIAN_POINT ( 'NONE',  ( 98.30752360899535347, -41.72884965087872189, 177.7397897205293305 ) ) ;
#12057 = CARTESIAN_POINT ( 'NONE',  ( 96.10063762778146668, -37.91858611869022866, 81.40038718067299328 ) ) ;
#12058 = ORIENTED_EDGE ( 'NONE', *, *, #49569, .F. ) ;
#12059 = VERTEX_POINT ( 'NONE', #30280 ) ;
#12060 = EDGE_CURVE ( 'NONE', #55007, #28894, #51593, .T. ) ;
#12061 = DIRECTION ( 'NONE',  ( 1.000000000000000078E-15, -1.000000000000000083E-30, -1.000000000000000000 ) ) ;
#12062 = CARTESIAN_POINT ( 'NONE',  ( 107.0667039024470313, -104.2784471599409528, 19.21780685541800437 ) ) ;
#12063 = DIRECTION ( 'NONE',  ( -1.000000000000000000, -8.163404592832032979E-16, 0.000000000000000000 ) ) ;
#12064 = CARTESIAN_POINT ( 'NONE',  ( 112.6831787765100898, -43.31780159632685212, 150.9690427505439914 ) ) ;
#12065 = ADVANCED_FACE ( 'NONE', ( #57973 ), #50712, .F. ) ;
#12066 = VECTOR ( 'NONE', #21275, 1000.000000000000114 ) ;
#12067 = CONICAL_SURFACE ( 'NONE', #19326, 17.00000000000090239, 0.7853981633974447263 ) ;
#12068 = EDGE_CURVE ( 'NONE', #85068, #27190, #23036, .T. ) ;
#12069 = VECTOR ( 'NONE', #62899, 1000.000000000000000 ) ;
#12070 = FACE_OUTER_BOUND ( 'NONE', #40045, .T. ) ;
#12071 = ORIENTED_EDGE ( 'NONE', *, *, #9816, .F. ) ;
#12072 = ORIENTED_EDGE ( 'NONE', *, *, #78047, .F. ) ;
#12073 = CARTESIAN_POINT ( 'NONE',  ( 1.387778780781445676E-14, 223.9999999999999716, 90.07542076772557493 ) ) ;
#12074 = ORIENTED_EDGE ( 'NONE', *, *, #67423, .F. ) ;
#12075 = EDGE_LOOP ( 'NONE', ( #50675, #40179 ) ) ;
#12076 = DIRECTION ( 'NONE',  ( 0.000000000000000000, 0.000000000000000000, 1.000000000000000000 ) ) ;
#12077 = ADVANCED_FACE ( 'NONE', ( #6927 ), #20569, .T. ) ;
#12078 = CARTESIAN_POINT ( 'NONE',  ( 97.15642216441104040, -38.53537999780244405, 197.9015833058969633 ) ) ;
#12079 = CARTESIAN_POINT ( 'NONE',  ( 103.1875000000000000, 127.0000000000000000, 5.041900000000359761 ) ) ;
#12080 = CARTESIAN_POINT ( 'NONE',  ( 61.56670390244634916, -23.42844715994043270, 180.4678068554151196 ) ) ;
#12081 = LINE ( 'NONE', #67479, #16942 ) ;
#12082 = ORIENTED_EDGE ( 'NONE', *, *, #49250, .F. ) ;
#12083 = ORIENTED_EDGE ( 'NONE', *, *, #16178, .F. ) ;
#12084 = AXIS2_PLACEMENT_3D ( 'NONE', #85890, #58160, #58589 ) ;
#12085 = ORIENTED_EDGE ( 'NONE', *, *, #68062, .T. ) ;
#12086 = ORIENTED_EDGE ( 'NONE', *, *, #47690, .T. ) ;
#12087 = CARTESIAN_POINT ( 'NONE',  ( 102.5467118750096631, -28.62589253813684209, 253.2995189410198691 ) ) ;
#12089 = CARTESIAN_POINT ( 'NONE',  ( 101.7446525173404979, -27.01484174591878329, 100.4632443235299633 ) ) ;
#12088 = CONICAL_SURFACE ( 'NONE', #41120, 25.39999999999999858, 0.7853981633974984611 ) ;
#12090 = CARTESIAN_POINT ( 'NONE',  ( 97.30890135812528285, -33.12136451854834007, 66.04419670448297097 ) ) ;
#12091 = CARTESIAN_POINT ( 'NONE',  ( 109.3549997033752277, -28.03260486696533249, 249.5838068554168387 ) ) ;
#12092 = CARTESIAN_POINT ( 'NONE',  ( 131.5565945955649170, -17.60518703965928466, 7.068229416970669199 ) ) ;
#12093 = CARTESIAN_POINT ( 'NONE',  ( 51.03742451361726751, -23.42844715994066362, 237.4678068554150059 ) ) ;
#12094 = CARTESIAN_POINT ( 'NONE',  ( 113.0221554258835823, -45.32894145911351558, 199.0584824187679374 ) ) ;
#12095 = PLANE ( 'NONE',  #62523 ) ;
#12096 = ORIENTED_EDGE ( 'NONE', *, *, #36867, .T. ) ;
#12097 = CARTESIAN_POINT ( 'NONE',  ( 130.0003553321328411, 78.46683822717001533, -12.03293382262373612 ) ) ;
#12098 = ORIENTED_EDGE ( 'NONE', *, *, #82021, .T. ) ;
#12099 = ORIENTED_EDGE ( 'NONE', *, *, #44068, .F. ) ;
#12100 = CARTESIAN_POINT ( 'NONE',  ( 31.71315051185382572, -33.70561438052049397, 117.4678068554150485 ) ) ;
#12101 = EDGE_CURVE ( 'NONE', #73956, #6135, #34628, .T. ) ;
#12102 = ORIENTED_EDGE ( 'NONE', *, *, #54447, .T. ) ;
#12103 = AXIS2_PLACEMENT_3D ( 'NONE', #66692, #10396, #87594 ) ;
#12104 = CARTESIAN_POINT ( 'NONE',  ( 0.000000000000000000, 82.54999999999999716, -97.46299999999996544 ) ) ;
#12105 = CARTESIAN_POINT ( 'NONE',  ( 116.8171228671177175, -34.15291832207935130, 179.0314586091353704 ) ) ;
#12106 = CARTESIAN_POINT ( 'NONE',  ( 117.3536837868190332, -38.62665896660388398, 88.68133956162493803 ) ) ;
#12107 = DIRECTION ( 'NONE',  ( 1.000000000000000000, 0.000000000000000000, 0.000000000000000000 ) ) ;
#12108 = DIRECTION ( 'NONE',  ( 0.7071067811864671926, 0.7071067811866279529, 6.612322855854137577E-17 ) ) ;
#12109 = CARTESIAN_POINT ( 'NONE',  ( 97.81170008160388818, -40.51743097690945916, 72.63551179937353197 ) ) ;
#12112 = CARTESIAN_POINT ( 'NONE',  ( 116.3308458273175603, -44.07926308385594183, 194.2927681330539542 ) ) ;
#12111 = CARTESIAN_POINT ( 'NONE',  ( 97.81997189479284316, -40.53760914905940638, 56.63694704664123947 ) ) ;
#12110 = CARTESIAN_POINT ( 'NONE',  ( -187.8075999999999794, 101.5999999999999943, -12.69999999999999929 ) ) ;
#12113 = DIRECTION ( 'NONE',  ( -1.000000000000000000, 0.000000000000000000, 0.000000000000000000 ) ) ;
#12114 = CARTESIAN_POINT ( 'NONE',  ( 37.06648329127298780, 12.92155284005730387, 358.9756252759109998 ) ) ;
#12115 = ORIENTED_EDGE ( 'NONE', *, *, #55593, .T. ) ;
#12116 = FACE_OUTER_BOUND ( 'NONE', #72440, .T. ) ;
#12117 = LINE ( 'NONE', #3075, #32597 ) ;
#12118 = CARTESIAN_POINT ( 'NONE',  ( 97.06386167369745976, -37.34267883451605030, 136.3754845998514043 ) ) ;
#12119 = CARTESIAN_POINT ( 'NONE',  ( 156.5667039024483813, -48.82844715993569196, 254.7178068554149490 ) ) ;
#12120 = EDGE_CURVE ( 'NONE', #74222, #79502, #2109, .T. ) ;
#12122 = ORIENTED_EDGE ( 'NONE', *, *, #88683, .F. ) ;
#12121 = CARTESIAN_POINT ( 'NONE',  ( 103.9260401568723324, -26.74224119611745820, 250.3184824187677577 ) ) ;
#12123 = CARTESIAN_POINT ( 'NONE',  ( -179.6544565346565037, 20.32000000000000028, -9.200237383489920262 ) ) ;
#12124 = CARTESIAN_POINT ( 'NONE',  ( 97.19620376612084556, -33.30704266974938577, 282.0613395616252888 ) ) ;
#12125 = CARTESIAN_POINT ( 'NONE',  ( 116.9452694852055998, -40.19391870447465465, 129.5584824187679658 ) ) ;
#12126 = FACE_OUTER_BOUND ( 'NONE', #72113, .T. ) ;
#12127 = CARTESIAN_POINT ( 'NONE',  ( 2.077912807000529050, 95.08573034283288905, -130.5400978111108543 ) ) ;
#12129 = CARTESIAN_POINT ( 'NONE',  ( 182.6664832912729821, 12.92155284005730387, 355.9756252759109998 ) ) ;
#12128 = CARTESIAN_POINT ( 'NONE',  ( 182.2300522401149863, -33.89581943344511217, -5.074374724088000832 ) ) ;
#12130 = DIRECTION ( 'NONE',  ( 0.000000000000000000, 1.000000000000000000, 0.000000000000000000 ) ) ;
#12131 = CARTESIAN_POINT ( 'NONE',  ( 63.03715912545825262, -46.82818131006018803, 237.4678068554150059 ) ) ;
#12132 = ORIENTED_EDGE ( 'NONE', *, *, #24995, .T. ) ;
#12134 = ADVANCED_FACE ( 'NONE', ( #53702 ), #83247, .T. ) ;
#12133 = VECTOR ( 'NONE', #57575, 1000.000000000000000 ) ;
#12135 = APPLICATION_CONTEXT ( 'automotive_design' ) ;
#12136 = AXIS2_PLACEMENT_3D ( 'NONE', #69080, #33212, #69529 ) ;
#12137 = VERTEX_POINT ( 'NONE', #82807 ) ;
#12138 = EDGE_LOOP ( 'NONE', ( #53444, #41076, #47228, #65655 ) ) ;
#12139 = VERTEX_POINT ( 'NONE', #26035 ) ;
#12140 = DIRECTION ( 'NONE',  ( 0.000000000000000000, 0.000000000000000000, -1.000000000000000000 ) ) ;
#12141 = CARTESIAN_POINT ( 'NONE',  ( 102.7643194828038702, -25.71402177940534983, 16.37276813305293999 ) ) ;
#12142 = DIRECTION ( 'NONE',  ( -0.9254794337955620787, -0.3787978585227822492, 0.000000000000000000 ) ) ;
#12143 = DIRECTION ( 'NONE',  ( 0.000000000000000000, -1.000000000000000000, 0.000000000000000000 ) ) ;
#12144 = CARTESIAN_POINT ( 'NONE',  ( 144.5610809520308351, -138.4343374614282425, 247.5945153064158717 ) ) ;
#12146 = LINE ( 'NONE', #5334, #71870 ) ;
#12145 = DIRECTION ( 'NONE',  ( 0.000000000000000000, -1.000000000000000000, 0.000000000000000000 ) ) ;
#12147 = CARTESIAN_POINT ( 'NONE',  ( 101.9719466847405158, -43.62131184885326007, 256.4924198280769474 ) ) ;
#12148 = EDGE_LOOP ( 'NONE', ( #34251, #50136, #46001, #47466 ) ) ;
#12149 = VERTEX_POINT ( 'NONE', #47347 ) ;
#12150 = ORIENTED_EDGE ( 'NONE', *, *, #9808, .T. ) ;
#12151 = VECTOR ( 'NONE', #60867, 1000.000000000000000 ) ;
#12152 = CARTESIAN_POINT ( 'NONE',  ( 107.0664832912730020, -27.87844715994269862, 361.9756252759109998 ) ) ;
#12153 = AXIS2_PLACEMENT_3D ( 'NONE', #7229, #77168, #62629 ) ;
#12154 = CARTESIAN_POINT ( 'NONE',  ( 115.0687214047011366, -42.78184030945386951, 183.3110242557596905 ) ) ;
#12155 = CARTESIAN_POINT ( 'NONE',  ( 141.0667039024479834, -50.82844715994100682, 10.91780685541499807 ) ) ;
#12156 = CARTESIAN_POINT ( 'NONE',  ( 31.75000000000000000, 8.255000000000000782, -3.174999999999999822 ) ) ;
#12157 = EDGE_CURVE ( 'NONE', #46735, #52987, #76073, .T. ) ;
#12158 = CARTESIAN_POINT ( 'NONE',  ( 116.8454820155364331, -34.32316206775963963, 10.45015473446897403 ) ) ;
#12159 = EDGE_CURVE ( 'NONE', #65845, #39861, #31068, .T. ) ;
#12160 = CARTESIAN_POINT ( 'NONE',  ( 118.3662777621133131, 93.33860577356861654, -6.713439888429178382 ) ) ;
#12161 = CIRCLE ( 'NONE', #77452, 87.89999999999994884 ) ;
#12162 = EDGE_CURVE ( 'NONE', #12424, #61646, #20119, .T. ) ;
#12163 = FACE_OUTER_BOUND ( 'NONE', #78167, .T. ) ;
#12164 = CARTESIAN_POINT ( 'NONE',  ( 110.7503262618283344, -45.78994064700705735, 282.8841967044829744 ) ) ;
#12165 = CARTESIAN_POINT ( 'NONE',  ( -41.60202597009397607, 40.59999999999997300, 47.15338361873602935 ) ) ;
#12166 = ORIENTED_EDGE ( 'NONE', *, *, #64270, .F. ) ;
#12167 = EDGE_CURVE ( 'NONE', #49816, #17557, #76416, .T. ) ;
#12168 = DIRECTION ( 'NONE',  ( 0.000000000000000000, 1.000000000000000000, 0.000000000000000000 ) ) ;
#12169 = B_SPLINE_CURVE_WITH_KNOTS ( 'NONE', 3,
 ( #67831, #86503, #45133, #38330 ),
 .UNSPECIFIED., .F., .F.,
 ( 4, 4 ),
 ( 0.000000000000000000, 0.001501537230210108625 ),
 .UNSPECIFIED. ) ;
#12170 = FACE_OUTER_BOUND ( 'NONE', #45567, .T. ) ;
#12171 = CARTESIAN_POINT ( 'NONE',  ( 110.8736562448416549, -29.50897902285196039, 57.50809036959092424 ) ) ;
#12172 = EDGE_CURVE ( 'NONE', #11460, #68161, #81908, .T. ) ;
#12173 = CARTESIAN_POINT ( 'NONE',  ( 136.7838203269376152, -18.30343833344100801, 6.798133076499780714 ) ) ;
#12174 = CARTESIAN_POINT ( 'NONE',  ( 106.5656518807525117, -24.23945688555024702, 323.2548426863285727 ) ) ;
#12175 = EDGE_CURVE ( 'NONE', #83823, #14890, #27368, .T. ) ;
#12176 = LINE ( 'NONE', #81679, #22796 ) ;
#12177 = ORIENTED_EDGE ( 'NONE', *, *, #66313, .F. ) ;
#12178 = DIRECTION ( 'NONE',  ( 1.000000000000000078E-15, -1.000000000000000083E-30, -1.000000000000000000 ) ) ;
#12179 = CARTESIAN_POINT ( 'NONE',  ( 123.6114559063626928, 60.30978874921765964, -42.01581149136940496 ) ) ;
#12180 = ORIENTED_EDGE ( 'NONE', *, *, #41968, .T. ) ;
#12181 = CARTESIAN_POINT ( 'NONE',  ( 117.6081704542122282, -33.40500446796587397, 129.0575300378159795 ) ) ;
#12182 = VERTEX_POINT ( 'NONE', #14194 ) ;
#12183 = CARTESIAN_POINT ( 'NONE',  ( 109.2109342822782168, -45.52796977871753370, 87.17718173283900285 ) ) ;
#12184 = DIRECTION ( 'NONE',  ( -2.973811673103097665E-16, 0.000000000000000000, -1.000000000000000000 ) ) ;
#12185 = CARTESIAN_POINT ( 'NONE',  ( 112.8380968919016425, -43.45378765227984275, 104.5730118773259534 ) ) ;
#12186 = LINE ( 'NONE', #39870, #37338 ) ;
#12187 = CYLINDRICAL_SURFACE ( 'NONE', #15032, 9.999999999999998224 ) ;
#12188 = CARTESIAN_POINT ( 'NONE',  ( 106.8407189164991706, -48.60257990303799858, 73.56133956162497611 ) ) ;
#12189 = CARTESIAN_POINT ( 'NONE',  ( 152.4409905591762708, -0.9151414768251351362, 542.9756252759101471 ) ) ;
#12190 = AXIS2_PLACEMENT_3D ( 'NONE', #87312, #80963, #25075 ) ;
#12191 = CARTESIAN_POINT ( 'NONE',  ( 154.4439038579832300, -17.91479848270203945, 542.9756252759101471 ) ) ;
#12192 = ORIENTED_EDGE ( 'NONE', *, *, #51682, .T. ) ;
#12193 = CARTESIAN_POINT ( 'NONE',  ( 123.6837132603318707, -20.11243780205705534, 218.8274735512161158 ) ) ;
#12194 = VECTOR ( 'NONE', #28283, 1000.000000000000000 ) ;
#12195 = VERTEX_POINT ( 'NONE', #88277 ) ;
#12196 = ORIENTED_EDGE ( 'NONE', *, *, #23708, .T. ) ;
#12197 = CARTESIAN_POINT ( 'NONE',  ( 162.0667039024470171, -77.67844715994088745, 96.96780685541800437 ) ) ;
#12198 = ORIENTED_EDGE ( 'NONE', *, *, #41724, .T. ) ;
#12199 = CARTESIAN_POINT ( 'NONE',  ( 117.4008144674645280, -32.62901037329574905, 249.1270538473399654 ) ) ;
#12200 = CARTESIAN_POINT ( 'NONE',  ( 116.9247085916874909, -40.18670803819183845, 129.5584824187679658 ) ) ;
#12201 = LINE ( 'NONE', #38552, #17629 ) ;
#12202 = CARTESIAN_POINT ( 'NONE',  ( 127.4058501689330996, -85.76982405743852667, 250.2178068554179902 ) ) ;
#12203 = CARTESIAN_POINT ( 'NONE',  ( 116.5983126044778402, -29.68822244385183140, 105.3327681330539463 ) ) ;
#12204 = CARTESIAN_POINT ( 'NONE',  ( 116.3244028009478797, -32.94573790848593120, 95.13562527591096796 ) ) ;
#12205 = VERTEX_POINT ( 'NONE', #67348 ) ;
#12206 = CARTESIAN_POINT ( 'NONE',  ( 151.0371591254572934, -24.42818131005592974, 300.4678068554149490 ) ) ;
#12207 = CYLINDRICAL_SURFACE ( 'NONE', #86870, 16.00000000000000000 ) ;
#12208 = ADVANCED_FACE ( 'NONE', ( #5136 ), #40991, .T. ) ;
#12209 = ORIENTED_EDGE ( 'NONE', *, *, #39509, .T. ) ;
#12210 = VECTOR ( 'NONE', #21464, 1000.000000000000000 ) ;
#12211 = CARTESIAN_POINT ( 'NONE',  ( 83.73314995794051185, 12.92155284005802685, 334.6228282640713019 ) ) ;
#12212 = CIRCLE ( 'NONE', #7865, 2.517499999999998739 ) ;
#12213 = DIRECTION ( 'NONE',  ( 0.000000000000000000, 0.000000000000000000, -1.000000000000000000 ) ) ;
#12214 = CARTESIAN_POINT ( 'NONE',  ( 115.6373213143784398, -30.77082676042341802, 279.3099109901966131 ) ) ;
#12215 = CARTESIAN_POINT ( 'NONE',  ( -12.69999999999999929, 82.54999999999999716, -179.8908777604655143 ) ) ;
#12216 = VECTOR ( 'NONE', #35329, 1000.000000000000000 ) ;
#12217 = DIRECTION ( 'NONE',  ( -0.000000000000000000, -0.000000000000000000, 1.000000000000000000 ) ) ;
#12218 = CARTESIAN_POINT ( 'NONE',  ( 78.42773927736698170, -38.94013506380486689, 2.060080721665560777 ) ) ;
#12219 = CARTESIAN_POINT ( 'NONE',  ( 109.4611421171680945, -28.53056059958231216, 259.2724198280769770 ) ) ;
#12221 = CARTESIAN_POINT ( 'NONE',  ( 107.8666756518570793, -26.35696637107995954, 66.01562527591097762 ) ) ;
#12220 = CARTESIAN_POINT ( 'NONE',  ( 97.63926207416247394, -40.07016425843875140, 101.5979595511756628 ) ) ;
#12222 = DIRECTION ( 'NONE',  ( -4.237773401492740281E-14, 1.000000000000000000, 0.000000000000000000 ) ) ;
#12223 = CARTESIAN_POINT ( 'NONE',  ( 117.5013794172148351, -40.51439451343497922, 173.5375300378159693 ) ) ;
#12224 = ORIENTED_EDGE ( 'NONE', *, *, #89028, .F. ) ;
#12225 = DIRECTION ( 'NONE',  ( 1.000000000000000000, 0.000000000000000000, 0.000000000000000000 ) ) ;
#12226 = VERTEX_POINT ( 'NONE', #19217 ) ;
#12227 = CARTESIAN_POINT ( 'NONE',  ( 70.63919639214310564, 353.0471713899363522, 56.85413200336923012 ) ) ;
#12228 = CIRCLE ( 'NONE', #15145, 14.00000000000000888 ) ;
#12229 = DIRECTION ( 'NONE',  ( -0.7071067811865453523, -0.7071067811865496822, -7.071067811865460542E-16 ) ) ;
#12230 = LINE ( 'NONE', #66278, #55723 ) ;
#12231 = VERTEX_POINT ( 'NONE', #6477 ) ;
#12232 = DIRECTION ( 'NONE',  ( 0.000000000000000000, 0.000000000000000000, 1.000000000000000000 ) ) ;
#12234 = EDGE_LOOP ( 'NONE', ( #65295, #76282, #6766, #32383 ) ) ;
#12233 = CARTESIAN_POINT ( 'NONE',  ( 117.0754465142714054, -30.29129860725820222, 144.2813395616249750 ) ) ;
#12235 = CARTESIAN_POINT ( 'NONE',  ( 194.5664832912739826, -18.82844715994099971, 342.9256252759119548 ) ) ;
#12236 = CARTESIAN_POINT ( 'NONE',  ( -130.4354318373311514, 93.94566094357735153, -5.621620364686718219 ) ) ;
#12237 = DIRECTION ( 'NONE',  ( -1.000000000000000000, -4.510281037539694659E-14, 0.000000000000000000 ) ) ;
#12238 = CARTESIAN_POINT ( 'NONE',  ( 41.56670390244801894, -27.57844715994070484, 342.9256252759119548 ) ) ;
#12239 = VERTEX_POINT ( 'NONE', #34170 ) ;
#12240 = EDGE_CURVE ( 'NONE', #27718, #23732, #74622, .T. ) ;
#12241 = DIRECTION ( 'NONE',  ( 1.000000000000000078E-15, -1.000000000000000083E-30, -1.000000000000000000 ) ) ;
#12242 = CARTESIAN_POINT ( 'NONE',  ( 20.03715912545645850, -24.95799193693202156, 129.9678068554150627 ) ) ;
#12243 = EDGE_LOOP ( 'NONE', ( #30978, #73389, #51941, #22929 ) ) ;
#12244 = EDGE_LOOP ( 'NONE', ( #20031, #5929, #3263, #39852, #25252, #6395 ) ) ;
#12245 = DIRECTION ( 'NONE',  ( -0.000000000000000000, -0.000000000000000000, 1.000000000000000000 ) ) ;
#12246 = CARTESIAN_POINT ( 'NONE',  ( 72.96458098368701428, 127.0000000000000000, -67.92268098368680285 ) ) ;
#12247 = CARTESIAN_POINT ( 'NONE',  ( 115.0372574787901954, -42.90846260359005271, 158.3022919389477465 ) ) ;
#12248 = DIRECTION ( 'NONE',  ( 1.907762142705490052E-15, 7.167082501179359715E-16, -1.000000000000000000 ) ) ;
#12250 = CARTESIAN_POINT ( 'NONE',  ( 107.0664832912739968, -36.72944715994100306, 287.6356252759109680 ) ) ;
#12249 = LINE ( 'NONE', #61282, #13166 ) ;
#12251 = FACE_BOUND ( 'NONE', #56681, .T. ) ;
#12252 = CIRCLE ( 'NONE', #16613, 1.000000000002049694 ) ;
#12253 = ORIENTED_EDGE ( 'NONE', *, *, #82128, .T. ) ;
#12254 = AXIS2_PLACEMENT_3D ( 'NONE', #85320, #2636, #49410 ) ;
#12255 = CARTESIAN_POINT ( 'NONE',  ( 63.56670390244828184, -47.82844715994016127, 249.9678068554150343 ) ) ;
#12256 = CARTESIAN_POINT ( 'NONE',  ( 101.7025241355417364, -45.60450926735014576, 198.1318157521009482 ) ) ;
#12257 = EDGE_CURVE ( 'NONE', #34233, #17736, #67809, .T. ) ;
#12259 = ORIENTED_EDGE ( 'NONE', *, *, #71760, .T. ) ;
#12258 = LINE ( 'NONE', #39953, #12418 ) ;
#12260 = CARTESIAN_POINT ( 'NONE',  ( 118.0115280580377402, -34.77548253539075063, 44.96705384733895272 ) ) ;
#12261 = ADVANCED_FACE ( 'NONE', ( #60992 ), #88720, .F. ) ;
#12262 = CARTESIAN_POINT ( 'NONE',  ( 116.3183049785035195, -32.94379174720932468, 54.13562527591098217 ) ) ;
#12263 = EDGE_CURVE ( 'NONE', #79263, #26148, #68270, .T. ) ;
#12264 = CARTESIAN_POINT ( 'NONE',  ( 0.000000000000000000, 65.60000000000000853, 118.5560000000000116 ) ) ;
#12265 = CARTESIAN_POINT ( 'NONE',  ( -77.39114642430010349, 120.6499999999999915, 71.77848634863050847 ) ) ;
#12266 = EDGE_LOOP ( 'NONE', ( #62571, #70882, #85295, #36284 ) ) ;
#12267 = CARTESIAN_POINT ( 'NONE',  ( 27.27158787008327678, 184.0000000000000000, 101.0189074266571794 ) ) ;
#12268 = ADVANCED_FACE ( 'NONE', ( #56404 ), #35977, .T. ) ;
#12269 = ORIENTED_EDGE ( 'NONE', *, *, #8100, .T. ) ;
#12270 = ORIENTED_EDGE ( 'NONE', *, *, #35385, .F. ) ;
#12271 = CARTESIAN_POINT ( 'NONE',  ( 113.4748355983601300, -30.60888351595189860, 230.8644404487539816 ) ) ;
#12272 = AXIS2_PLACEMENT_3D ( 'NONE', #63888, #16188, #57947 ) ;
#12273 = DIRECTION ( 'NONE',  ( 0.000000000000000000, -0.8660254037844383745, -0.5000000000000003331 ) ) ;
#12274 = VECTOR ( 'NONE', #30568, 1000.000000000000000 ) ;
#12275 = VECTOR ( 'NONE', #6333, 1000.000000000000000 ) ;
#12276 = CARTESIAN_POINT ( 'NONE',  ( -118.2605848834651709, 92.12496802699141085, -8.385272115321491526 ) ) ;
#12277 = AXIS2_PLACEMENT_3D ( 'NONE', #47943, #41139, #34331 ) ;
#12278 = DIRECTION ( 'NONE',  ( 0.5000000000000015543, -0.8660254037844377084, 2.602085213965216006E-14 ) ) ;
#12279 = EDGE_CURVE ( 'NONE', #28336, #84782, #29611, .T. ) ;
#12280 = CARTESIAN_POINT ( 'NONE',  ( 82.67340060512941591, -37.60624470235564587, 2.902100967938844089 ) ) ;
#12281 = AXIS2_PLACEMENT_3D ( 'NONE', #29659, #76015, #20613 ) ;
#12282 = VERTEX_POINT ( 'NONE', #77770 ) ;
#12283 = CARTESIAN_POINT ( 'NONE',  ( 85.06670390244701707, -80.35669973212957018, 222.2178068554179902 ) ) ;
#12284 = AXIS2_PLACEMENT_3D ( 'NONE', #2336, #51343, #10477 ) ;
#12285 = CARTESIAN_POINT ( 'NONE',  ( 97.12568611773902205, -37.99775231544951737, 37.42709075889258941 ) ) ;
#12286 = EDGE_CURVE ( 'NONE', #53177, #87561, #62776, .T. ) ;
#12287 = ORIENTED_EDGE ( 'NONE', *, *, #45300, .T. ) ;
#12288 = CARTESIAN_POINT ( 'NONE',  ( 110.9847977634196496, -46.36662828626499078, 282.8841967044824628 ) ) ;
#12289 = EDGE_LOOP ( 'NONE', ( #11299, #81159 ) ) ;
#12290 = ORIENTED_EDGE ( 'NONE', *, *, #20468, .T. ) ;
#12291 = CARTESIAN_POINT ( 'NONE',  ( 111.4490224358278994, -43.61588866942526721, 260.8452332267341376 ) ) ;
#12292 = CARTESIAN_POINT ( 'NONE',  ( 85.06670390244700286, -74.11757344603526576, 55.21780685541800437 ) ) ;
#12293 = CARTESIAN_POINT ( 'NONE',  ( 108.8290724220007348, -27.07506712556656936, 164.9327681330539690 ) ) ;
#12294 = CARTESIAN_POINT ( 'NONE',  ( 160.2664750769289697, 0.000000000000000000, 148.0533267522752112 ) ) ;
#12295 = CARTESIAN_POINT ( 'NONE',  ( 20.03715912545730760, -24.42818131006189830, 300.4678068554150059 ) ) ;
#12296 = CARTESIAN_POINT ( 'NONE',  ( 73.06670390244801183, -48.82844715994099971, 179.9178068554149661 ) ) ;
#12297 = CARTESIAN_POINT ( 'NONE',  ( 96.73312529990856490, -40.78150971882554643, 242.6118157521009664 ) ) ;
#12298 = CYLINDRICAL_SURFACE ( 'NONE', #63032, 5.599999999999994316 ) ;
#12299 = ORIENTED_EDGE ( 'NONE', *, *, #83569, .F. ) ;
#12300 = CARTESIAN_POINT ( 'NONE',  ( 109.7813809329710040, -47.49173451690833048, 88.78514908543493789 ) ) ;
#12301 = CARTESIAN_POINT ( 'NONE',  ( 48.79742451362097455, -36.32844715994040996, 342.9256252759109884 ) ) ;
#12302 = ORIENTED_EDGE ( 'NONE', *, *, #14734, .F. ) ;
#12303 = AXIS2_PLACEMENT_3D ( 'NONE', #77815, #49180, #64185 ) ;
#12304 = ORIENTED_EDGE ( 'NONE', *, *, #37775, .F. ) ;
#12305 = ORIENTED_EDGE ( 'NONE', *, *, #20066, .F. ) ;
#12306 = CARTESIAN_POINT ( 'NONE',  ( 177.8371591254542921, -47.82818131005477369, 313.9678068554149490 ) ) ;
#12307 = CARTESIAN_POINT ( 'NONE',  ( 12.60000000000000142, 82.54999999999999716, 89.46299999999996544 ) ) ;
#12308 = CARTESIAN_POINT ( 'NONE',  ( 98.30745628127105817, -41.72868722923796270, 151.7403413731134663 ) ) ;
#12309 = CARTESIAN_POINT ( 'NONE',  ( 103.1635642379172850, -29.56027560196853088, 143.2909475124489518 ) ) ;
#12310 = CARTESIAN_POINT ( 'NONE',  ( 116.9459113946819286, -41.73765103896904805, 244.4651490854349731 ) ) ;
#12311 = DIRECTION ( 'NONE',  ( 0.000000000000000000, -1.000000000000000000, -2.913971193241881161E-15 ) ) ;
#12312 = EDGE_LOOP ( 'NONE', ( #52481, #68052, #68784 ) ) ;
#12313 = CARTESIAN_POINT ( 'NONE',  ( 107.0664832912739541, -23.56278049327425350, 311.6356252759109680 ) ) ;
#12314 = DIRECTION ( 'NONE',  ( 0.000000000000000000, 0.000000000000000000, 1.000000000000000000 ) ) ;
#12315 = EDGE_CURVE ( 'NONE', #43956, #18807, #1471, .T. ) ;
#12316 = EDGE_LOOP ( 'NONE', ( #88395, #50327, #75661, #33760 ) ) ;
#12317 = ORIENTED_EDGE ( 'NONE', *, *, #13689, .F. ) ;
#12318 = AXIS2_PLACEMENT_3D ( 'NONE', #53321, #81086, #19290 ) ;
#12319 = CARTESIAN_POINT ( 'NONE',  ( 31.89136050872134476, -31.76306994223885383, 193.9678068554150911 ) ) ;
#12320 = ORIENTED_EDGE ( 'NONE', *, *, #18118, .F. ) ;
#12321 = ORIENTED_EDGE ( 'NONE', *, *, #11997, .T. ) ;
#12322 = DIRECTION ( 'NONE',  ( 1.000000000000000078E-15, -1.000000000000000000, 0.000000000000000000 ) ) ;
#12323 = AXIS2_PLACEMENT_3D ( 'NONE', #6207, #33895, #35686 ) ;
#12324 = PLANE ( 'NONE',  #777 ) ;
#12325 = EDGE_CURVE ( 'NONE', #83557, #61431, #35513, .T. ) ;
#12326 = PLANE ( 'NONE',  #43177 ) ;
#12327 = CARTESIAN_POINT ( 'NONE',  ( 111.7477409549918690, -43.87381266066567775, 177.4609912566479579 ) ) ;
#12328 = CARTESIAN_POINT ( 'NONE',  ( 101.9388778781502509, -27.60177885026046596, 60.48419670448296159 ) ) ;
#12329 = PLANE ( 'NONE',  #33594 ) ;
#12330 = ORIENTED_EDGE ( 'NONE', *, *, #72769, .T. ) ;
#12331 = DIRECTION ( 'NONE',  ( 0.7071067811868666508, 0.7071067811862283836, 7.071067811868659373E-16 ) ) ;
#12332 = VERTEX_POINT ( 'NONE', #77317 ) ;
#12333 = FACE_OUTER_BOUND ( 'NONE', #80855, .T. ) ;
#12334 = EDGE_LOOP ( 'NONE', ( #87606, #70527, #72973, #8282 ) ) ;
#12335 = CARTESIAN_POINT ( 'NONE',  ( 107.0222341398176127, -26.64422208933962821, 166.0788337594356676 ) ) ;
#12336 = DIRECTION ( 'NONE',  ( -0.7071067811865604513, 0.000000000000000000, 0.7071067811865345831 ) ) ;
#12337 = CARTESIAN_POINT ( 'NONE',  ( 113.2919313540066071, -44.57100634757310331, 133.1104735366473903 ) ) ;
#12339 = VECTOR ( 'NONE', #22785, 1000.000000000000000 ) ;
#12338 = LINE ( 'NONE', #38248, #66885 ) ;
#12340 = VERTEX_POINT ( 'NONE', #78235 ) ;
#12341 = EDGE_CURVE ( 'NONE', #22595, #36659, #35067, .T. ) ;
#12342 = CARTESIAN_POINT ( 'NONE',  ( 116.1397716810727303, -31.55208187140975795, 289.2384824187681716 ) ) ;
#12343 = AXIS2_PLACEMENT_3D ( 'NONE', #30024, #44073, #16397 ) ;
#12344 = CARTESIAN_POINT ( 'NONE',  ( 101.1162363742629253, -27.35970543535582422, 61.51467289495899138 ) ) ;
#12345 = VECTOR ( 'NONE', #38394, 1000.000000000000000 ) ;
#12346 =( NAMED_UNIT ( * ) PLANE_ANGLE_UNIT ( ) SI_UNIT ( $, .RADIAN. ) );
#12347 = AXIS2_PLACEMENT_3D ( 'NONE', #6829, #34071, #34532 ) ;
#12349 = LINE ( 'NONE', #40038, #38466 ) ;
#12348 = CARTESIAN_POINT ( 'NONE',  ( 134.0664832912740110, -8.350947159940998787, 2.408125275911999097 ) ) ;
#12350 = DIRECTION ( 'NONE',  ( 1.000000000000000078E-15, 1.000000000000000083E-30, -1.000000000000000000 ) ) ;
#12351 = FACE_OUTER_BOUND ( 'NONE', #1558, .T. ) ;
#12352 = DIRECTION ( 'NONE',  ( 0.000000000000000000, 0.000000000000000000, 1.000000000000000000 ) ) ;
#12353 = DIRECTION ( 'NONE',  ( 0.000000000000000000, 1.000000000000000000, 0.000000000000000000 ) ) ;
#12354 = ADVANCED_FACE ( 'NONE', ( #41871 ), #70506, .T. ) ;
#12355 = ORIENTED_EDGE ( 'NONE', *, *, #14313, .F. ) ;
#12356 = CARTESIAN_POINT ( 'NONE',  ( 114.8522965031571630, -43.72857415363870359, 38.24419670448192221 ) ) ;
#12357 = CARTESIAN_POINT ( 'NONE',  ( 113.4285887376619968, -27.66253919562607422, 80.57753003781597556 ) ) ;
#12359 = CARTESIAN_POINT ( 'NONE',  ( 0.000000000000000000, 198.8420489685532004, 0.000000000000000000 ) ) ;
#12358 = CARTESIAN_POINT ( 'NONE',  ( 163.0822201311030142, 20.32000000000000028, -75.92468371870729982 ) ) ;
#12360 = CARTESIAN_POINT ( 'NONE',  ( -105.4788588808462038, 120.6499999999999915, -3.968750000001139977 ) ) ;
#12361 = VECTOR ( 'NONE', #82323, 1000.000000000000000 ) ;
#12362 = AXIS2_PLACEMENT_3D ( 'NONE', #17378, #43278, #31437 ) ;
#12363 = CARTESIAN_POINT ( 'NONE',  ( 139.8778540137985829, -131.0224759750418286, 248.3919668373590071 ) ) ;
#12364 = EDGE_LOOP ( 'NONE', ( #70931, #84166, #13544, #37573 ) ) ;
#12365 = CARTESIAN_POINT ( 'NONE',  ( 108.2420053567034017, -46.43931755893575541, 113.6727681330529691 ) ) ;
#12367 = ORIENTED_EDGE ( 'NONE', *, *, #69463, .F. ) ;
#12366 = LINE ( 'NONE', #67774, #41389 ) ;
#12368 = CARTESIAN_POINT ( 'NONE',  ( 112.4005920293389948, -46.38403708128146974, 248.9661014663869878 ) ) ;
#12369 = CARTESIAN_POINT ( 'NONE',  ( 183.5150000000000148, 52.73749999999999716, -34.92499999999999716 ) ) ;
#12370 = FACE_BOUND ( 'NONE', #26881, .T. ) ;
#12371 = DIRECTION ( 'NONE',  ( 1.000000000000000000, 0.000000000000000000, 0.000000000000000000 ) ) ;
#12372 = ADVANCED_FACE ( 'NONE', ( #7822 ), #28719, .F. ) ;
#12373 = DIRECTION ( 'NONE',  ( 0.000000000000000000, 1.000000000000000000, 0.000000000000000000 ) ) ;
#12374 = CARTESIAN_POINT ( 'NONE',  ( 131.5359215223105309, -37.80596063775243465, 2.807537029280252838 ) ) ;
#12375 = LINE ( 'NONE', #40065, #42784 ) ;
#12376 = CARTESIAN_POINT ( 'NONE',  ( 99.36405074150913208, -30.70139697576582805, 155.7984824187689412 ) ) ;
#12377 = ORIENTED_EDGE ( 'NONE', *, *, #56017, .T. ) ;
#12378 = EDGE_LOOP ( 'NONE', ( #345, #76654, #83196, #65193 ) ) ;
#12379 = AXIS2_PLACEMENT_3D ( 'NONE', #5059, #39568, #32757 ) ;
#12380 = CARTESIAN_POINT ( 'NONE',  ( 99.34829255622855726, -41.08350393070648465, 133.1672975916119697 ) ) ;
#12381 = LINE ( 'NONE', #53682, #50126 ) ;
#12383 = CARTESIAN_POINT ( 'NONE',  ( 165.2748236753145932, -30.08671355699731720, 237.4678068554150059 ) ) ;
#12382 = CARTESIAN_POINT ( 'NONE',  ( 115.4101910119109533, -30.57141770992062035, 255.3203871806724123 ) ) ;
#12384 = AXIS2_PLACEMENT_3D ( 'NONE', #50089, #41927, #7877 ) ;
#12385 = LINE ( 'NONE', #40078, #39151 ) ;
#12386 = FACE_OUTER_BOUND ( 'NONE', #674, .T. ) ;
#12387 = EDGE_CURVE ( 'NONE', #46735, #72562, #64139, .T. ) ;
#12388 = DIRECTION ( 'NONE',  ( 0.000000000000000000, 1.000000000000000000, 0.000000000000000000 ) ) ;
#12389 = DIRECTION ( 'NONE',  ( 1.000000000000000000, 0.000000000000000000, 9.462128050782575008E-16 ) ) ;
#12390 = DIRECTION ( 'NONE',  ( -1.000000000000000078E-15, 1.000000000000000083E-30, 1.000000000000000000 ) ) ;
#12391 = EDGE_CURVE ( 'NONE', #18839, #6555, #56855, .T. ) ;
#12392 = CARTESIAN_POINT ( 'NONE',  ( 107.9164806882189396, -47.13338536194959971, 177.6413395616249886 ) ) ;
#12393 = PLANE ( 'NONE',  #44562 ) ;
#12394 = VERTEX_POINT ( 'NONE', #28251 ) ;
#12395 = ORIENTED_EDGE ( 'NONE', *, *, #80768, .F. ) ;
#12396 = CARTESIAN_POINT ( 'NONE',  ( 31.78666935232957869, -29.62846900982343001, 237.4678068554150059 ) ) ;
#12397 = CARTESIAN_POINT ( 'NONE',  ( 82.59390026529925422, -19.81452881270899269, 7.047625865520877220 ) ) ;
#12398 = CARTESIAN_POINT ( 'NONE',  ( 34.92499999999999716, 82.54999999999999716, 290.4490000000000123 ) ) ;
#12400 = CARTESIAN_POINT ( 'NONE',  ( 116.3212776292296127, -32.94146857471318413, 287.6356252759109680 ) ) ;
#12399 = AXIS2_PLACEMENT_3D ( 'NONE', #70366, #8599, #36296 ) ;
#12401 = ORIENTED_EDGE ( 'NONE', *, *, #1084, .T. ) ;
#12402 = VECTOR ( 'NONE', #59601, 1000.000000000000000 ) ;
#12403 = LINE ( 'NONE', #11964, #52330 ) ;
#12404 = AXIS2_PLACEMENT_3D ( 'NONE', #13833, #48777, #77405 ) ;
#12405 = AXIS2_PLACEMENT_3D ( 'NONE', #53458, #5350, #52562 ) ;
#12406 = CARTESIAN_POINT ( 'NONE',  ( 113.1555140577670215, -26.56262906569767068, 204.6470538473399756 ) ) ;
#12407 = DIRECTION ( 'NONE',  ( -1.000000000000000000, 0.000000000000000000, 0.000000000000000000 ) ) ;
#12408 = ORIENTED_EDGE ( 'NONE', *, *, #19175, .F. ) ;
#12409 = CONICAL_SURFACE ( 'NONE', #58821, 9.571100913904478702, 0.7853981633974539411 ) ;
#12410 = CARTESIAN_POINT ( 'NONE',  ( -9.749037034254357081, 238.5000000000000000, 152.4294779587682456 ) ) ;
#12411 = DIRECTION ( 'NONE',  ( 0.9586846635221889512, 0.000000000000000000, -0.2844709403917162205 ) ) ;
#12412 = CARTESIAN_POINT ( 'NONE',  ( 28.57499999999999929, 77.96728223830730542, 294.9574999999999818 ) ) ;
#12413 = CARTESIAN_POINT ( 'NONE',  ( 110.2473415405206083, -44.77823998140315354, 20.70618560768600247 ) ) ;
#12415 = VECTOR ( 'NONE', #88569, 1000.000000000000000 ) ;
#12414 = CARTESIAN_POINT ( 'NONE',  ( 95.65143945485090171, -33.45545561978638460, 137.1041967044819501 ) ) ;
#12416 = CARTESIAN_POINT ( 'NONE',  ( 204.2160000000000082, 52.73749999999999716, -48.41875000000000284 ) ) ;
#12417 = ORIENTED_EDGE ( 'NONE', *, *, #84066, .F. ) ;
#12418 = VECTOR ( 'NONE', #4554, 1000.000000000000000 ) ;
#12419 = CARTESIAN_POINT ( 'NONE',  ( 172.5664832912729878, -27.82844715994070484, 14.17562527591199917 ) ) ;
#12420 = CARTESIAN_POINT ( 'NONE',  ( 82.58878920443973470, -17.63370978841311754, 7.053538376721526504 ) ) ;
#12421 = VERTEX_POINT ( 'NONE', #84597 ) ;
#12422 = VERTEX_POINT ( 'NONE', #69609 ) ;
#12423 = PLANE ( 'NONE',  #28488 ) ;
#12424 = VERTEX_POINT ( 'NONE', #57300 ) ;
#12425 = ORIENTED_EDGE ( 'NONE', *, *, #79443, .T. ) ;
#12426 = DIRECTION ( 'NONE',  ( 0.000000000000000000, 0.000000000000000000, -1.000000000000000000 ) ) ;
#12427 = EDGE_CURVE ( 'NONE', #65668, #62636, #70966, .T. ) ;
#12428 = CARTESIAN_POINT ( 'NONE',  ( 115.2492312947614437, -32.84933048162275071, 63.61337220902895950 ) ) ;
#12429 = CARTESIAN_POINT ( 'NONE',  ( 96.62214413241265731, -36.48016117738031738, 196.3070538473399438 ) ) ;
#12430 = CARTESIAN_POINT ( 'NONE',  ( 114.9485010938853975, -29.93956786141545834, 184.3927681330539770 ) ) ;
#12432 = CARTESIAN_POINT ( 'NONE',  ( 97.12559377168382468, -39.79659400623918231, 17.56419670448195092 ) ) ;
#12431 = CARTESIAN_POINT ( 'NONE',  ( 97.82822030858592655, -40.55762851625022591, 21.63876279231929445 ) ) ;
#12433 = CARTESIAN_POINT ( 'NONE',  ( 146.0667039024470171, -94.02844715994091018, 55.21780685541800437 ) ) ;
#12434 = VECTOR ( 'NONE', #17400, 1000.000000000000000 ) ;
#12435 = CARTESIAN_POINT ( 'NONE',  ( 183.5150000000000148, 68.61249999999999716, -71.94630657015589748 ) ) ;
#12436 = EDGE_LOOP ( 'NONE', ( #74058, #58884, #77020, #26816 ) ) ;
#12437 = ORIENTED_EDGE ( 'NONE', *, *, #60849, .T. ) ;
#12438 = VECTOR ( 'NONE', #70391, 1000.000000000000000 ) ;
#12439 = VECTOR ( 'NONE', #24947, 1000.000000000000000 ) ;
#12440 = DIRECTION ( 'NONE',  ( -0.000000000000000000, -0.000000000000000000, -1.000000000000000000 ) ) ;
#12441 = CARTESIAN_POINT ( 'NONE',  ( 103.8060002238608774, -48.17488501466909412, 217.3556252759109668 ) ) ;
#12442 = EDGE_LOOP ( 'NONE', ( #18103, #71966, #76608, #40160 ) ) ;
#12443 = EDGE_CURVE ( 'NONE', #70167, #69623, #42724, .T. ) ;
#12444 = CARTESIAN_POINT ( 'NONE',  ( 103.7231215738078163, -26.19374500585225363, 205.3089586092439731 ) ) ;
#12445 = CARTESIAN_POINT ( 'NONE',  ( -17.13243906362141900, 64.60000000000000853, 42.79834678115690849 ) ) ;
#12446 = VECTOR ( 'NONE', #78464, 1000.000000000000000 ) ;
#12447 = DIRECTION ( 'NONE',  ( 0.000000000000000000, -0.000000000000000000, 1.000000000000000000 ) ) ;
#12448 = CARTESIAN_POINT ( 'NONE',  ( 109.6421639904622936, -46.48030490558162597, 23.78138826461756139 ) ) ;
#12449 = CARTESIAN_POINT ( 'NONE',  ( 151.0371591254583450, -46.82818131005583240, 300.4678068554149490 ) ) ;
#12450 = EDGE_CURVE ( 'NONE', #22374, #30549, #48983, .T. ) ;
#12452 = DIRECTION ( 'NONE',  ( 0.000000000000000000, 0.000000000000000000, 1.000000000000000000 ) ) ;
#12451 = CARTESIAN_POINT ( 'NONE',  ( 98.10142885082893827, -36.98438604582442224, 277.6356252759110816 ) ) ;
#12453 = CARTESIAN_POINT ( 'NONE',  ( 98.54766419607773287, -41.97700047869818718, 172.7658057784116750 ) ) ;
#12454 = DIRECTION ( 'NONE',  ( -3.100000000000000258E-29, 3.100000000000000044E-14, 1.000000000000000000 ) ) ;
#12455 = DIRECTION ( 'NONE',  ( -1.000000000000000078E-15, 1.000000000000000083E-30, 1.000000000000000000 ) ) ;
#12456 = EDGE_CURVE ( 'NONE', #59338, #79094, #65470, .T. ) ;
#12457 = DIRECTION ( 'NONE',  ( -0.000000000000000000, -0.000000000000000000, 1.000000000000000000 ) ) ;
#12458 = FACE_OUTER_BOUND ( 'NONE', #84785, .T. ) ;
#12459 = ADVANCED_FACE ( 'NONE', ( #85939 ), #87702, .F. ) ;
#12460 = CARTESIAN_POINT ( 'NONE',  ( -71.77848634863190114, 127.0000000000000000, 77.39114642429879609 ) ) ;
#12462 = EDGE_LOOP ( 'NONE', ( #37127, #40691, #85433, #10745 ) ) ;
#12461 = LINE ( 'NONE', #40146, #8029 ) ;
#12463 = EDGE_CURVE ( 'NONE', #17992, #69275, #53138, .T. ) ;
#12464 = CARTESIAN_POINT ( 'NONE',  ( 204.2160000000000082, 52.73749999999999716, -39.68750000000000000 ) ) ;
#12465 = CARTESIAN_POINT ( 'NONE',  ( 118.0640922190486890, -35.40731289736847032, 238.9337205140059552 ) ) ;
#12466 = CARTESIAN_POINT ( 'NONE',  ( 112.8017646537355176, -47.09965271489118521, 98.97848241876793907 ) ) ;
#12467 = CARTESIAN_POINT ( 'NONE',  ( 111.7585843298372197, -27.37117935058896379, 275.7070538473396937 ) ) ;
#12468 = DIRECTION ( 'NONE',  ( -1.058811598242755461E-16, 0.5150380749100580413, -0.8571673007021100021 ) ) ;
#12469 = DIRECTION ( 'NONE',  ( -0.9659258262890677571, 0.000000000000000000, 0.2588190451025230154 ) ) ;
#12471 = DIRECTION ( 'NONE',  ( 0.000000000000000000, 0.000000000000000000, 1.000000000000000000 ) ) ;
#12470 = FACE_OUTER_BOUND ( 'NONE', #60850, .T. ) ;
#12472 = DIRECTION ( 'NONE',  ( -0.1041461484700691442, 0.008931931031208454816, 0.9945218953682739560 ) ) ;
#12473 = EDGE_CURVE ( 'NONE', #66028, #64424, #52875, .T. ) ;
#12474 = CARTESIAN_POINT ( 'NONE',  ( 132.8008218761707724, -21.17731672736086423, 1.873071027759226626 ) ) ;
#12475 = AXIS2_PLACEMENT_3D ( 'NONE', #33834, #4794, #61525 ) ;
#12476 = EDGE_CURVE ( 'NONE', #7688, #45185, #26782, .T. ) ;
#12477 = AXIS2_PLACEMENT_3D ( 'NONE', #16417, #64121, #37301 ) ;
#12478 = AXIS2_PLACEMENT_3D ( 'NONE', #47334, #73718, #32363 ) ;
#12479 = EDGE_CURVE ( 'NONE', #76165, #41047, #76143, .T. ) ;
#12480 = ORIENTED_EDGE ( 'NONE', *, *, #88901, .F. ) ;
#12481 = VERTEX_POINT ( 'NONE', #80450 ) ;
#12482 = CARTESIAN_POINT ( 'NONE',  ( 99.86829443779211601, -32.07773762820211516, 145.2924198280769872 ) ) ;
#12484 = EDGE_LOOP ( 'NONE', ( #29628, #23889, #41178, #51518, #74712, #88733, #35280, #62937 ) ) ;
#12483 = CARTESIAN_POINT ( 'NONE',  ( 21.53388387833662065, 46.83799769796173251, 31.43192935164580604 ) ) ;
#12485 = DIRECTION ( 'NONE',  ( 0.9068632946707808618, -0.4214249218767877059, 0.000000000000000000 ) ) ;
#12486 = CARTESIAN_POINT ( 'NONE',  ( 97.76587557681025942, -42.65924729906315349, 137.7661014663869992 ) ) ;
#12487 = CARTESIAN_POINT ( 'NONE',  ( 151.0371591254576060, -24.95799193692592155, 129.9678068554149775 ) ) ;
#12488 = EDGE_CURVE ( 'NONE', #41468, #89588, #44111, .T. ) ;
#12489 = PLANE ( 'NONE',  #3724 ) ;
#12490 = DIRECTION ( 'NONE',  ( 0.000000000000000000, 1.000000000000000000, 0.000000000000000000 ) ) ;
#12491 = LINE ( 'NONE', #66995, #30907 ) ;
#12493 = CARTESIAN_POINT ( 'NONE',  ( 97.30000116515907393, -37.25789978020652882, 76.36991099019796536 ) ) ;
#12492 = CIRCLE ( 'NONE', #85062, 13.44999999999999396 ) ;
#12494 = VERTEX_POINT ( 'NONE', #10067 ) ;
#12495 = EDGE_LOOP ( 'NONE', ( #81947, #78584, #62352, #51503 ) ) ;
#12496 = ORIENTED_EDGE ( 'NONE', *, *, #68896, .T. ) ;
#12497 = CARTESIAN_POINT ( 'NONE',  ( 22.49563609058251146, -48.82844715994099971, 307.9888746672805269 ) ) ;
#12499 = DIRECTION ( 'NONE',  ( -1.000000000000000000, 8.775353200852647323E-16, 0.000000000000000000 ) ) ;
#12498 = CARTESIAN_POINT ( 'NONE',  ( 97.26456095925938428, -36.24355304347524509, 167.2870538473389672 ) ) ;
#12500 = AXIS2_PLACEMENT_3D ( 'NONE', #56130, #28913, #16619 ) ;
#12501 = CARTESIAN_POINT ( 'NONE',  ( 0.000000000000000000, 103.1240000000000236, 0.000000000000000000 ) ) ;
#12502 = CARTESIAN_POINT ( 'NONE',  ( -55.95243198108136085, 55.97500000000000142, 70.69974874213239957 ) ) ;
#12503 = CARTESIAN_POINT ( 'NONE',  ( 49.56670390244799762, -50.82844715994100682, 310.9178068554150514 ) ) ;
#12504 = EDGE_CURVE ( 'NONE', #85180, #13373, #47072, .T. ) ;
#12505 = DIRECTION ( 'NONE',  ( 0.000000000000000000, 0.000000000000000000, -1.000000000000000000 ) ) ;
#12506 = DIRECTION ( 'NONE',  ( -1.000000000000000000, 0.000000000000000000, 0.000000000000000000 ) ) ;
#12507 = EDGE_CURVE ( 'NONE', #44520, #38912, #45889, .T. ) ;
#12508 = CARTESIAN_POINT ( 'NONE',  ( 103.3702027031294506, -47.12181610991865455, 102.3165776568629752 ) ) ;
#12509 = ORIENTED_EDGE ( 'NONE', *, *, #29743, .F. ) ;
#12510 = ORIENTED_EDGE ( 'NONE', *, *, #49148, .T. ) ;
#12511 = EDGE_CURVE ( 'NONE', #74649, #30366, #66802, .T. ) ;
#12512 = DIRECTION ( 'NONE',  ( -0.9254794337955620787, -0.3787978585227822492, 0.000000000000000000 ) ) ;
#12513 = PLANE ( 'NONE',  #66401 ) ;
#12514 = ADVANCED_FACE ( 'NONE', ( #2810 ), #16882, .F. ) ;
#12515 = CARTESIAN_POINT ( 'NONE',  ( 31.89136050872298966, -31.76306994223740432, -5.074374724088000832 ) ) ;
#12516 = CARTESIAN_POINT ( 'NONE',  ( 114.6928066196564515, -42.01481596195104373, 161.1623760838769783 ) ) ;
#12517 = CARTESIAN_POINT ( 'NONE',  ( 20.56670390244743984, -48.82844715994200158, 180.4678068554150911 ) ) ;
#12518 = VERTEX_POINT ( 'NONE', #37323 ) ;
#12519 = ORIENTED_EDGE ( 'NONE', *, *, #74224, .F. ) ;
#12520 = CARTESIAN_POINT ( 'NONE',  ( 95.05156358570199870, -41.69348830286664764, 293.6369201390379544 ) ) ;
#12521 = CARTESIAN_POINT ( 'NONE',  ( 136.2737402105998967, -20.37320971850501650, 2.471387388698214060 ) ) ;
#12522 = EDGE_LOOP ( 'NONE', ( #37000, #71430, #23849, #81883 ) ) ;
#12523 = ORIENTED_EDGE ( 'NONE', *, *, #22939, .T. ) ;
#12524 = CARTESIAN_POINT ( 'NONE',  ( 106.0361919388305409, -11.55049677724511881, 323.5352776872487652 ) ) ;
#12525 = CARTESIAN_POINT ( 'NONE',  ( 114.2499829074921820, -30.67355260991839216, 220.8034880678019647 ) ) ;
#12526 = CIRCLE ( 'NONE', #89373, 1.000000000000000888 ) ;
#12527 = CARTESIAN_POINT ( 'NONE',  ( 41.56670390244804025, -42.82844715994103524, 300.4678068554150059 ) ) ;
#12528 = CARTESIAN_POINT ( 'NONE',  ( -111.5512539134624888, 65.62907064895924236, 67.83205493406804010 ) ) ;
#12529 = EDGE_LOOP ( 'NONE', ( #716, #23097, #41804 ) ) ;
#12530 = ORIENTED_EDGE ( 'NONE', *, *, #72949, .F. ) ;
#12531 = VECTOR ( 'NONE', #5534, 1000.000000000000000 ) ;
#12532 = AXIS2_PLACEMENT_3D ( 'NONE', #6150, #89267, #69261 ) ;
#12533 = CARTESIAN_POINT ( 'NONE',  ( 173.9900000000000091, 52.73749999999999716, -44.45000000000000284 ) ) ;
#12534 = VECTOR ( 'NONE', #30935, 1000.000000000000000 ) ;
#12535 = VERTEX_POINT ( 'NONE', #79568 ) ;
#12536 = ORIENTED_EDGE ( 'NONE', *, *, #70949, .T. ) ;
#12537 = CARTESIAN_POINT ( 'NONE',  ( 115.1064843935641022, -35.31944421942311862, 241.7823760838769545 ) ) ;
#12538 = CARTESIAN_POINT ( 'NONE',  ( 116.5534958752826213, -32.35418074550542400, 104.1699109901969535 ) ) ;
#12539 = CARTESIAN_POINT ( 'NONE',  ( 100.9560042165379059, -28.30978499293925310, 75.57562527591093726 ) ) ;
#12540 = CARTESIAN_POINT ( 'NONE',  ( 99.08163574056251832, -37.52321402124415783, 249.5838068554173503 ) ) ;
#12541 = B_SPLINE_SURFACE_WITH_KNOTS ( 'NONE', 3, 3, ( 
 ( #61617, #13047, #66648, #11700, #38942, #61177 ),
 ( #4437, #88905, #67099, #4880, #26657, #54337 ),
 ( #82103, #19851, #60271, #81205, #88002, #47537 ),
 ( #11237, #45732, #75270, #68454, #89353, #80305 ),
 ( #18054, #73460, #32124, #59821, #52982, #8016 ) ),
 .UNSPECIFIED., .F., .F., .F.,
 ( 4, 1, 4 ),
 ( 4, 1, 1, 4 ),
 ( -2.453700414991130114E-06, 0.5714285714285709528, 1.000002453700419958 ),
 ( 0.1139507740808489988, 4.342301322120899698, 5.399388959130909882, 7.513564233150940019 ),
 .UNSPECIFIED. ) ;
#12542 = CARTESIAN_POINT ( 'NONE',  ( 131.3325395364354904, -18.38432368373458559, 6.774690158158469089 ) ) ;
#12543 = PLANE ( 'NONE',  #63480 ) ;
#12544 = CARTESIAN_POINT ( 'NONE',  ( 110.4988674196275014, -26.88560509280327082, 205.8099109901969541 ) ) ;
#12545 = DIRECTION ( 'NONE',  ( 1.000000000000000078E-15, -1.000000000000000083E-30, -1.000000000000000000 ) ) ;
#12546 = VERTEX_POINT ( 'NONE', #73622 ) ;
#12547 = CARTESIAN_POINT ( 'NONE',  ( 130.2063869749195248, 74.16976894168006140, -9.551794474070780083 ) ) ;
#12548 = ORIENTED_EDGE ( 'NONE', *, *, #37517, .T. ) ;
#12549 = EDGE_LOOP ( 'NONE', ( #27039, #57655, #74008, #63057 ) ) ;
#12550 = DIRECTION ( 'NONE',  ( -1.000000000000000000, 0.000000000000000000, 0.000000000000000000 ) ) ;
#12551 = CIRCLE ( 'NONE', #14043, 179.8898777604655095 ) ;
#12552 = ORIENTED_EDGE ( 'NONE', *, *, #3450, .T. ) ;
#12553 = DIRECTION ( 'NONE',  ( 0.000000000000000000, -1.000000000000000000, 0.000000000000000000 ) ) ;
#12554 =( BOUNDED_CURVE ( )  B_SPLINE_CURVE ( 3, ( #74126, #39591, #18709, #4637 ),
 .UNSPECIFIED., .F., .T. ) 
 B_SPLINE_CURVE_WITH_KNOTS ( ( 4, 4 ),
 ( 4.647722573419573955, 4.714015861847076216 ),
 .UNSPECIFIED. ) 
 CURVE ( )  GEOMETRIC_REPRESENTATION_ITEM ( )  RATIONAL_B_SPLINE_CURVE ( ( 1.000000000000000000, 0.9996338001896092340, 0.9996338001896092340, 1.000000000000000000 ) ) 
 REPRESENTATION_ITEM ( '' )  );
#12555 = CARTESIAN_POINT ( 'NONE',  ( 3.968750000000000000, 127.0000000000000000, -105.4788588808464027 ) ) ;
#12556 = CARTESIAN_POINT ( 'NONE',  ( 96.64175856332744274, -36.61924367559645788, 111.3184824187679567 ) ) ;
#12557 = CARTESIAN_POINT ( 'NONE',  ( -11.54220284826591758, 77.25119473389790414, 130.0448154359650630 ) ) ;
#12558 = ADVANCED_FACE ( 'NONE', ( #80014 ), #2167, .F. ) ;
#12559 = CARTESIAN_POINT ( 'NONE',  ( 136.8164806451553659, -36.72944715939129168, 6.749772901088312516 ) ) ;
#12560 = DIRECTION ( 'NONE',  ( 0.000000000000000000, -1.000000000000000000, 0.000000000000000000 ) ) ;
#12561 = EDGE_CURVE ( 'NONE', #15404, #21921, #38209, .T. ) ;
#12564 = CARTESIAN_POINT ( 'NONE',  ( 106.9407056411434951, -47.75886249174716625, 228.5794347997199907 ) ) ;
#12563 = CARTESIAN_POINT ( 'NONE',  ( 25.56670390244797275, -58.35344715994099829, 139.9678068554150059 ) ) ;
#12562 = DIRECTION ( 'NONE',  ( 1.000000000000000000, 4.163336342344333240E-14, 0.000000000000000000 ) ) ;
#12565 = DIRECTION ( 'NONE',  ( 1.000000000000000000, 0.000000000000000000, 0.000000000000000000 ) ) ;
#12566 = CARTESIAN_POINT ( 'NONE',  ( -462.0260000000000105, 53.97500000000000142, -3.174999999999999822 ) ) ;
#12567 = EDGE_LOOP ( 'NONE', ( #64618, #38153, #83468, #53760 ) ) ;
#12568 = CARTESIAN_POINT ( 'NONE',  ( 59.56670390244699576, -67.87844715994098976, 155.2178068554179902 ) ) ;
#12569 = EDGE_CURVE ( 'NONE', #47365, #46362, #3692, .T. ) ;
#12570 = CARTESIAN_POINT ( 'NONE',  ( -3.175000000000120171, 104.3431970271541900, 33.98325472291460159 ) ) ;
#12571 = DIRECTION ( 'NONE',  ( 0.000000000000000000, 1.000000000000000000, 0.000000000000000000 ) ) ;
#12572 = EDGE_CURVE ( 'NONE', #28045, #55376, #59079, .T. ) ;
#12573 = CARTESIAN_POINT ( 'NONE',  ( 72.06648329127401098, -45.72944715994106701, 14.67562527591093513 ) ) ;
#12575 = ORIENTED_EDGE ( 'NONE', *, *, #26072, .F. ) ;
#12574 = CARTESIAN_POINT ( 'NONE',  ( 112.5123584215844659, -46.40184746663635451, 257.9965776568634510 ) ) ;
#12576 = EDGE_CURVE ( 'NONE', #87213, #6718, #80911, .T. ) ;
#12577 = DIRECTION ( 'NONE',  ( 0.000000000000000000, 1.000000000000000000, 0.000000000000000000 ) ) ;
#12578 = CARTESIAN_POINT ( 'NONE',  ( 105.0174007254451567, -25.84429900004466063, 276.2365776568634033 ) ) ;
#12579 = CARTESIAN_POINT ( 'NONE',  ( 101.7473938980672870, -45.74611303501656323, 158.1527681330539963 ) ) ;
#12580 = CARTESIAN_POINT ( 'NONE',  ( 151.5667039024534120, -48.82844715994099971, 300.4678068554149490 ) ) ;
#12581 = CARTESIAN_POINT ( 'NONE',  ( 0.000000000000000000, 101.5999999999999943, 0.000000000000000000 ) ) ;
#12583 = DIRECTION ( 'NONE',  ( 4.299999999999999979E-14, -1.000000000000000000, 4.400000000000000367E-29 ) ) ;
#12582 = CARTESIAN_POINT ( 'NONE',  ( 182.0667039024478981, -32.29483332967958376, 117.4678068554150627 ) ) ;
#12584 = DIRECTION ( 'NONE',  ( 0.000000000000000000, 0.000000000000000000, -1.000000000000000000 ) ) ;
#12585 = CARTESIAN_POINT ( 'NONE',  ( 63.06670390244711655, -40.32844715994016838, 129.9678068554150911 ) ) ;
#12586 = ORIENTED_EDGE ( 'NONE', *, *, #63026, .T. ) ;
#12587 = ADVANCED_FACE ( 'NONE', ( #33185 ), #27262, .F. ) ;
#12588 = EDGE_CURVE ( 'NONE', #43667, #38868, #54936, .T. ) ;
#12589 = ORIENTED_EDGE ( 'NONE', *, *, #82675, .F. ) ;
#12590 = EDGE_LOOP ( 'NONE', ( #79288, #27943, #364, #35638 ) ) ;
#12591 = ORIENTED_EDGE ( 'NONE', *, *, #73202, .T. ) ;
#12592 = LINE ( 'NONE', #6666, #4474 ) ;
#12593 = CARTESIAN_POINT ( 'NONE',  ( 115.8731522275743089, -31.19128430790907913, 30.27276813305396175 ) ) ;
#12594 = DIRECTION ( 'NONE',  ( 1.639958061481212836E-42, -4.100000000000000342E-29, -1.000000000000000000 ) ) ;
#12595 = ADVANCED_FACE ( 'NONE', ( #40440 ), #68609, .T. ) ;
#12596 = CARTESIAN_POINT ( 'NONE',  ( 145.1753220238131519, -139.0425770237959284, 246.8297448300953079 ) ) ;
#12598 = CARTESIAN_POINT ( 'NONE',  ( 68.87339889186067410, -139.0446803891145748, 247.0600586179500056 ) ) ;
#12597 = DIRECTION ( 'NONE',  ( -1.047445008332813989E-14, 0.000000000000000000, 1.000000000000000000 ) ) ;
#12599 = AXIS2_PLACEMENT_3D ( 'NONE', #12191, #5833, #87160 ) ;
#12600 = CARTESIAN_POINT ( 'NONE',  ( 105.8912501276363543, -45.18964566429946217, 256.8895626852198006 ) ) ;
#12601 = ORIENTED_EDGE ( 'NONE', *, *, #4887, .T. ) ;
#12602 = ADVANCED_FACE ( 'NONE', ( #75423 ), #12298, .F. ) ;
#12603 = ORIENTED_EDGE ( 'NONE', *, *, #56028, .F. ) ;
#12604 = VERTEX_POINT ( 'NONE', #5489 ) ;
#12605 = AXIS2_PLACEMENT_3D ( 'NONE', #72892, #45598, #38811 ) ;
#12606 = CARTESIAN_POINT ( 'NONE',  ( 45.76696975232822950, -48.62818131006091704, 129.9678068554150911 ) ) ;
#12607 = AXIS2_PLACEMENT_3D ( 'NONE', #15319, #8958, #30722 ) ;
#12608 = DIRECTION ( 'NONE',  ( -1.000000000000000000, 0.000000000000000000, 0.000000000000000000 ) ) ;
#12609 = CARTESIAN_POINT ( 'NONE',  ( 107.0664832912750057, -36.72944715993903486, 9.125625275910969947 ) ) ;
#12610 = CARTESIAN_POINT ( 'NONE',  ( 63.03715912545737865, -24.89890238295017966, 249.9678068554150343 ) ) ;
#12611 = CARTESIAN_POINT ( 'NONE',  ( 116.2961902049681697, -40.76469377450285947, 54.93015473446794061 ) ) ;
#12612 = DIRECTION ( 'NONE',  ( 0.000000000000000000, 1.000000000000000000, 0.000000000000000000 ) ) ;
#12613 = CARTESIAN_POINT ( 'NONE',  ( 97.81170212845945855, -40.51743756719207568, 176.6354241348688277 ) ) ;
#12614 = CARTESIAN_POINT ( 'NONE',  ( 100.4593435015893164, -29.47291325643525184, 285.6641967044828334 ) ) ;
#12615 = CARTESIAN_POINT ( 'NONE',  ( 97.81168895331838087, -40.51742574516882200, 287.6356252759109680 ) ) ;
#12616 = ORIENTED_EDGE ( 'NONE', *, *, #40558, .T. ) ;
#12617 = ADVANCED_FACE ( 'NONE', ( #48130 ), #27711, .T. ) ;
#12618 = DIRECTION ( 'NONE',  ( 0.000000000000000000, 1.000000000000000000, 0.000000000000000000 ) ) ;
#12619 = ADVANCED_FACE ( 'NONE', ( #69049 ), #18660, .F. ) ;
#12620 = AXIS2_PLACEMENT_3D ( 'NONE', #932, #56315, #64503 ) ;
#12621 = DIRECTION ( 'NONE',  ( -4.554376769437570034E-14, 1.000000000000000000, 0.000000000000000000 ) ) ;
#12622 = CARTESIAN_POINT ( 'NONE',  ( 102.4269143325283835, -29.42360532460997291, 63.33285227435298026 ) ) ;
#12623 = CARTESIAN_POINT ( 'NONE',  ( 134.8062005078452614, -16.05355276379774310, 8.162233076783889985 ) ) ;
#12624 = DIRECTION ( 'NONE',  ( 4.194175870806139918E-14, -1.000000000000000000, 0.000000000000000000 ) ) ;
#12625 = CARTESIAN_POINT ( 'NONE',  ( 168.0371591254545649, -48.62818131005509059, 180.4678068554150059 ) ) ;
#12626 = ORIENTED_EDGE ( 'NONE', *, *, #30594, .F. ) ;
#12627 = CARTESIAN_POINT ( 'NONE',  ( 77.58678459498918301, -35.53883969337057636, 7.103318745425301728 ) ) ;
#12628 = ORIENTED_EDGE ( 'NONE', *, *, #85798, .T. ) ;
#12629 = CARTESIAN_POINT ( 'NONE',  ( 99.68446536626322541, -46.00016974189506413, 122.0413395616249659 ) ) ;
#12630 = ORIENTED_EDGE ( 'NONE', *, *, #76388, .T. ) ;
#12631 = CARTESIAN_POINT ( 'NONE',  ( 98.07131787375925569, -37.77809840677601017, 85.85337220902894728 ) ) ;
#12632 = CARTESIAN_POINT ( 'NONE',  ( 179.7974245136200011, -36.32844715994040996, -5.074374724088000832 ) ) ;
#12633 = CARTESIAN_POINT ( 'NONE',  ( 103.9179606659962616, -45.58175368509670733, 98.74824997256392578 ) ) ;
#12634 = DIRECTION ( 'NONE',  ( -0.7071067811865794361, 0.7071067811865157093, -7.071067811865492096E-16 ) ) ;
#12635 = LINE ( 'NONE', #60768, #45465 ) ;
#12636 = VECTOR ( 'NONE', #11278, 1000.000000000000000 ) ;
#12637 = CARTESIAN_POINT ( 'NONE',  ( 104.0364404988798270, -47.38327494250712135, 63.36800622829197494 ) ) ;
#12638 = VECTOR ( 'NONE', #7421, 1000.000000000000000 ) ;
#12639 = CARTESIAN_POINT ( 'NONE',  ( 115.5439452383991892, -99.96145986183427112, -19.78219314458215550 ) ) ;
#12640 = ADVANCED_FACE ( 'NONE', ( #53596 ), #40882, .F. ) ;
#12641 = CARTESIAN_POINT ( 'NONE',  ( 97.81399847929220925, -40.51646572127298640, 256.6355814287313137 ) ) ;
#12642 = ORIENTED_EDGE ( 'NONE', *, *, #26714, .F. ) ;
#12643 = CARTESIAN_POINT ( 'NONE',  ( 72.26648329127297643, -1.929447159941394263, 342.9256252759109884 ) ) ;
#12644 = ORIENTED_EDGE ( 'NONE', *, *, #72510, .F. ) ;
#12645 = ORIENTED_EDGE ( 'NONE', *, *, #44877, .T. ) ;
#12646 = CARTESIAN_POINT ( 'NONE',  ( 103.8797721312301405, -101.8611209747507189, 2.217806855417919998 ) ) ;
#12647 = EDGE_LOOP ( 'NONE', ( #29385, #6494, #23836, #88821 ) ) ;
#12648 = CARTESIAN_POINT ( 'NONE',  ( 106.5981863181247462, -46.53222597210214673, 247.5384824187689787 ) ) ;
#12649 = CARTESIAN_POINT ( 'NONE',  ( 108.2803420215754500, -47.73912846947793298, 153.6518157521009584 ) ) ;
#12650 = CARTESIAN_POINT ( 'NONE',  ( 3.286821707691937711, 70.27560252132435892, -118.5111027017741776 ) ) ;
#12651 = DIRECTION ( 'NONE',  ( 0.9068632946707807507, -0.4214249218767881500, 9.028300618466658994E-16 ) ) ;
#12652 = CARTESIAN_POINT ( 'NONE',  ( 117.1064219673475719, -39.53695830471063744, 94.60991099019693706 ) ) ;
#12653 = EDGE_LOOP ( 'NONE', ( #8756, #14881, #65348, #49049 ) ) ;
#12654 = LINE ( 'NONE', #4940, #13371 ) ;
#12655 = VECTOR ( 'NONE', #37496, 1000.000000000000000 ) ;
#12656 = CIRCLE ( 'NONE', #44534, 218.1859999999999786 ) ;
#12657 = CARTESIAN_POINT ( 'NONE',  ( 98.30754538652605845, -41.72890334347444252, 157.7395978512973613 ) ) ;
#12659 = VERTEX_POINT ( 'NONE', #75865 ) ;
#12658 = EDGE_CURVE ( 'NONE', #76744, #17700, #5032, .T. ) ;
#12660 = AXIS2_PLACEMENT_3D ( 'NONE', #88669, #55446, #46840 ) ;
#12661 = DIRECTION ( 'NONE',  ( -0.000000000000000000, 1.000000000000000000, -0.000000000000000000 ) ) ;
#12662 = VECTOR ( 'NONE', #40626, 1000.000000000000000 ) ;
#12663 = DIRECTION ( 'NONE',  ( -0.8660253910675250744, -0.0001484127182099123339, -0.5000000000000052180 ) ) ;
#12664 = CARTESIAN_POINT ( 'NONE',  ( 114.3996560367811810, -27.45190519937920470, 274.5441967044824878 ) ) ;
#12665 = CARTESIAN_POINT ( 'NONE',  ( 46.03715912545427358, -48.62818131006086020, 300.4678068554150059 ) ) ;
#12666 = EDGE_CURVE ( 'NONE', #56235, #83503, #29724, .T. ) ;
#12667 = DIRECTION ( 'NONE',  ( 1.000000000000000000, 0.000000000000000000, 0.000000000000000000 ) ) ;
#12668 = CARTESIAN_POINT ( 'NONE',  ( 47.62500000000000000, 66.67499999999999716, 260.3500000000000227 ) ) ;
#12669 = EDGE_CURVE ( 'NONE', #877, #19584, #13636, .T. ) ;
#12670 = CARTESIAN_POINT ( 'NONE',  ( 108.8243102715920685, -46.27830423087877421, 277.1438483995053161 ) ) ;
#12672 = CARTESIAN_POINT ( 'NONE',  ( 98.35456548258461851, -42.41549619454038123, 97.78705384733993355 ) ) ;
#12671 = CARTESIAN_POINT ( 'NONE',  ( 99.98384727107165304, -29.55937221596129305, 100.6969498110766210 ) ) ;
#12673 = DIRECTION ( 'NONE',  ( -0.9999999853157766072, -0.0001713722456134502174, 0.000000000000000000 ) ) ;
#12674 = CARTESIAN_POINT ( 'NONE',  ( 97.34100429996045989, -42.07995573552675950, 176.7146728949589658 ) ) ;
#12675 = VERTEX_POINT ( 'NONE', #60884 ) ;
#12676 = CYLINDRICAL_SURFACE ( 'NONE', #36533, 1.000000000000000888 ) ;
#12677 = ORIENTED_EDGE ( 'NONE', *, *, #40616, .T. ) ;
#12678 = DIRECTION ( 'NONE',  ( 0.000000000000000000, 0.000000000000000000, -1.000000000000000000 ) ) ;
#12679 = EDGE_CURVE ( 'NONE', #75690, #9436, #48809, .T. ) ;
#12680 = LINE ( 'NONE', #74901, #10207 ) ;
#12681 = CARTESIAN_POINT ( 'NONE',  ( 136.5461822395192826, -35.53884010536734905, 2.747932095377162209 ) ) ;
#12682 = ORIENTED_EDGE ( 'NONE', *, *, #51796, .T. ) ;
#12683 = VECTOR ( 'NONE', #85644, 1000.000000000000000 ) ;
#12684 = CARTESIAN_POINT ( 'NONE',  ( 97.07216744069562253, -35.37760030334273864, 62.21925782715792508 ) ) ;
#12685 = EDGE_CURVE ( 'NONE', #25045, #40273, #76759, .T. ) ;
#12687 = ORIENTED_EDGE ( 'NONE', *, *, #75604, .F. ) ;
#12686 = CARTESIAN_POINT ( 'NONE',  ( 113.3579092357397542, -45.09751872455207433, 143.0899109901969553 ) ) ;
#12688 = DIRECTION ( 'NONE',  ( -1.000000000000000000, 0.000000000000000000, 0.000000000000000000 ) ) ;
#12689 = CIRCLE ( 'NONE', #27137, 5.600000000000000533 ) ;
#12690 = B_SPLINE_CURVE_WITH_KNOTS ( 'NONE', 3,
 ( #83786, #28345, #15183, #1562, #7020, #13836, #63328, #29704, #15639, #21559, #56039, #14746, #29263, #56946, #20658, #1106, #84689, #28817 ),
 .UNSPECIFIED., .F., .F.,
 ( 4, 2, 2, 2, 2, 2, 2, 2, 4 ),
 ( 0.5000000020452582961, 0.5625000017896010229, 0.6250000015339437498, 0.6875000012782863656, 0.7500000010226290925, 0.8125000007669718194, 0.8750000005113145463, 0.9375000002556572731, 1.000000000000000000 ),
 .UNSPECIFIED. ) ;
#12691 = DIRECTION ( 'NONE',  ( 1.000000000000000078E-15, 1.000000000000000083E-30, -1.000000000000000000 ) ) ;
#12692 = AXIS2_PLACEMENT_3D ( 'NONE', #46707, #74436, #39901 ) ;
#12693 = DIRECTION ( 'NONE',  ( -1.000000000000000000, -8.163404592832032979E-16, 0.000000000000000000 ) ) ;
#12694 = CARTESIAN_POINT ( 'NONE',  ( 0.000000000000000000, 101.5999999999999943, 130.5560000000000116 ) ) ;
#12695 = ORIENTED_EDGE ( 'NONE', *, *, #43324, .F. ) ;
#12697 = EDGE_CURVE ( 'NONE', #83795, #49158, #72654, .T. ) ;
#12696 = CONICAL_SURFACE ( 'NONE', #6843, 9.571100913904325935, 0.7853981633974543852 ) ;
#12698 = DIRECTION ( 'NONE',  ( 1.000000000000000000, 0.000000000000000000, 0.000000000000000000 ) ) ;
#12699 = CARTESIAN_POINT ( 'NONE',  ( 88.79221564186276794, -137.6784471599409585, 55.21780685541800437 ) ) ;
#12700 = ORIENTED_EDGE ( 'NONE', *, *, #64862, .F. ) ;
#12701 = EDGE_CURVE ( 'NONE', #22201, #18085, #49995, .T. ) ;
#12702 = ORIENTED_EDGE ( 'NONE', *, *, #49028, .T. ) ;
#12703 = CARTESIAN_POINT ( 'NONE',  ( 163.0667039024477276, -33.35206098992141222, 237.4678068554150059 ) ) ;
#12704 = DIRECTION ( 'NONE',  ( -3.100000000000000258E-29, 3.100000000000000044E-14, 1.000000000000000000 ) ) ;
#12705 = FACE_BOUND ( 'NONE', #29529, .T. ) ;
#12706 = DIRECTION ( 'NONE',  ( 0.000000000000000000, 1.000000000000000000, 0.000000000000000000 ) ) ;
#12708 = CARTESIAN_POINT ( 'NONE',  ( 153.0667039024470739, -124.7784471599408960, 222.2178068554179902 ) ) ;
#12707 = CARTESIAN_POINT ( 'NONE',  ( 182.4202572930269923, -31.94127993907680718, 117.4678068554150627 ) ) ;
#12709 = DIRECTION ( 'NONE',  ( -1.000000000000000000, 0.000000000000000000, 0.000000000000000000 ) ) ;
#12710 = CIRCLE ( 'NONE', #64900, 11.45913725231036118 ) ;
#12711 = EDGE_LOOP ( 'NONE', ( #1448, #27234, #35622, #26456 ) ) ;
#12712 = LINE ( 'NONE', #71269, #38395 ) ;
#12713 = LINE ( 'NONE', #60389, #36127 ) ;
#12714 = CARTESIAN_POINT ( 'NONE',  ( 96.12852455334832769, -38.72269610271986551, 197.4699109901959844 ) ) ;
#12716 = ORIENTED_EDGE ( 'NONE', *, *, #18622, .T. ) ;
#12715 = LINE ( 'NONE', #25434, #41442 ) ;
#12717 = CARTESIAN_POINT ( 'NONE',  ( 99.16769444712207360, -43.44866735504064081, 72.89943479971999807 ) ) ;
#12718 = DIRECTION ( 'NONE',  ( 0.000000000000000000, 0.000000000000000000, 1.000000000000000000 ) ) ;
#12719 = DIRECTION ( 'NONE',  ( -0.7071067811856560636, -0.7071067811874389708, 0.000000000000000000 ) ) ;
#12720 = FACE_OUTER_BOUND ( 'NONE', #76447, .T. ) ;
#12721 = ORIENTED_EDGE ( 'NONE', *, *, #82221, .F. ) ;
#12722 = LINE ( 'NONE', #20872, #71933 ) ;
#12723 = VECTOR ( 'NONE', #66144, 1000.000000000000000 ) ;
#12724 = EDGE_LOOP ( 'NONE', ( #60446, #17744 ) ) ;
#12725 = VERTEX_POINT ( 'NONE', #68903 ) ;
#12726 = EDGE_CURVE ( 'NONE', #26573, #20221, #75717, .T. ) ;
#12727 = CARTESIAN_POINT ( 'NONE',  ( 104.7356562592608498, -27.62759180600148667, 241.7196785439919609 ) ) ;
#12728 = AXIS2_PLACEMENT_3D ( 'NONE', #77167, #14944, #42613 ) ;
#12729 = DIRECTION ( 'NONE',  ( 1.821231995776179916E-16, 0.000000000000000000, 1.000000000000000000 ) ) ;
#12730 = AXIS2_PLACEMENT_3D ( 'NONE', #62409, #56021, #76041 ) ;
#12731 = CARTESIAN_POINT ( 'NONE',  ( -118.4880192609368947, 94.60304557064718267, -4.087421425392933294 ) ) ;
#12732 = DIRECTION ( 'NONE',  ( 1.000000000000000078E-15, -1.000000000000000083E-30, -1.000000000000000000 ) ) ;
#12733 = CARTESIAN_POINT ( 'NONE',  ( 182.3467384525650061, -36.02818131005800950, 342.9256252759119548 ) ) ;
#12734 = VERTEX_POINT ( 'NONE', #62074 ) ;
#12735 = CARTESIAN_POINT ( 'NONE',  ( -12.69999999999999929, 82.54999999999999716, 206.3750000000000000 ) ) ;
#12736 = CIRCLE ( 'NONE', #83810, 3.000000000000002665 ) ;
#12737 = CARTESIAN_POINT ( 'NONE',  ( 4.665904304751420031E-15, 95.25000000000000000, -38.10000000000000142 ) ) ;
#12738 = VERTEX_POINT ( 'NONE', #68001 ) ;
#12739 = CARTESIAN_POINT ( 'NONE',  ( 111.1290374500119498, -47.00926920395730235, 22.88800622829195675 ) ) ;
#12740 = EDGE_LOOP ( 'NONE', ( #37958, #5268, #57873, #66298 ) ) ;
#12741 = CARTESIAN_POINT ( 'NONE',  ( 109.3549613941650875, -28.89410453886290142, 257.6680903695913685 ) ) ;
#12742 = VECTOR ( 'NONE', #88084, 1000.000000000000000 ) ;
#12743 = DIRECTION ( 'NONE',  ( 0.000000000000000000, -1.000000000000000000, 0.000000000000000000 ) ) ;
#12744 = CARTESIAN_POINT ( 'NONE',  ( 107.9488082096507213, -26.98745991040259895, 155.0041967044829505 ) ) ;
#12745 = CARTESIAN_POINT ( 'NONE',  ( 80.06648329127398256, -9.029447159941060619, 4.925625275910944012 ) ) ;
#12746 = DIRECTION ( 'NONE',  ( -3.360405532702990443E-14, 1.000000000000000000, 0.000000000000000000 ) ) ;
#12747 = VECTOR ( 'NONE', #15978, 1000.000000000000000 ) ;
#12748 = CYLINDRICAL_SURFACE ( 'NONE', #81145, 0.5000000000000104361 ) ;
#12749 = AXIS2_PLACEMENT_3D ( 'NONE', #12104, #40242, #54747 ) ;
#12750 = CARTESIAN_POINT ( 'NONE',  ( 136.8164832912739826, -18.72944715994099951, -5.074374724088999145 ) ) ;
#12751 = CARTESIAN_POINT ( 'NONE',  ( 118.0968619800241299, -35.49322535880637020, 229.9032443235299468 ) ) ;
#12752 = CARTESIAN_POINT ( 'NONE',  ( 92.32962665258611423, 82.96450994655477018, -74.36911441044638593 ) ) ;
#12753 = VECTOR ( 'NONE', #82566, 1000.000000000000000 ) ;
#12754 = ORIENTED_EDGE ( 'NONE', *, *, #19837, .T. ) ;
#12755 = ADVANCED_FACE ( 'NONE', ( #27562 ), #7125, .T. ) ;
#12756 = CARTESIAN_POINT ( 'NONE',  ( 95.98963492482539550, -41.07853246264400582, 92.62419670448296927 ) ) ;
#12757 = CARTESIAN_POINT ( 'NONE',  ( 119.0814029968458811, -31.76540601701525901, 289.6356252759107406 ) ) ;
#12758 = VERTEX_POINT ( 'NONE', #26658 ) ;
#12759 = VERTEX_POINT ( 'NONE', #47540 ) ;
#12760 = EDGE_LOOP ( 'NONE', ( #59513, #85069, #54529, #76186 ) ) ;
#12761 = DIRECTION ( 'NONE',  ( 0.000000000000000000, 1.000000000000000000, 0.000000000000000000 ) ) ;
#12762 = DIRECTION ( 'NONE',  ( 1.000000000000000078E-15, 0.000000000000000000, -1.000000000000000000 ) ) ;
#12763 = DIRECTION ( 'NONE',  ( -1.000000000000000078E-15, 1.000000000000000083E-30, 1.000000000000000000 ) ) ;
#12764 = LINE ( 'NONE', #61777, #5512 ) ;
#12765 = CARTESIAN_POINT ( 'NONE',  ( 108.5685384152640864, -45.25263643686804471, 120.5214237029249915 ) ) ;
#12766 = CARTESIAN_POINT ( 'NONE',  ( 117.4513846513745960, -35.59318846168486772, 274.9127681330539872 ) ) ;
#12767 = LINE ( 'NONE', #74535, #17458 ) ;
#12768 = VERTEX_POINT ( 'NONE', #47084 ) ;
#12769 = CARTESIAN_POINT ( 'NONE',  ( 130.5169520046878802, 94.84315624882771090, 3.295103719955264410 ) ) ;
#12770 = VECTOR ( 'NONE', #35972, 1000.000000000000000 ) ;
#12771 = CARTESIAN_POINT ( 'NONE',  ( 172.5667039024480118, -36.32844715993499563, 180.4678068554150059 ) ) ;
#12772 = ORIENTED_EDGE ( 'NONE', *, *, #52901, .F. ) ;
#12774 = ORIENTED_EDGE ( 'NONE', *, *, #21146, .T. ) ;
#12773 = AXIS2_PLACEMENT_3D ( 'NONE', #83599, #47251, #26820 ) ;
#12775 = PLANE ( 'NONE',  #44503 ) ;
#12776 = ORIENTED_EDGE ( 'NONE', *, *, #58820, .T. ) ;
#12777 = ORIENTED_EDGE ( 'NONE', *, *, #1942, .T. ) ;
#12778 = DIRECTION ( 'NONE',  ( 1.000000000000000000, 4.299999999999999979E-14, 1.000000000000000078E-15 ) ) ;
#12779 = DIRECTION ( 'NONE',  ( -1.000000000000000078E-15, 1.000000000000000083E-30, 1.000000000000000000 ) ) ;
#12780 = DIRECTION ( 'NONE',  ( -1.000000000000000000, -1.206764157201257538E-15, 0.000000000000000000 ) ) ;
#12781 = CYLINDRICAL_SURFACE ( 'NONE', #17131, 8.636000000000004562 ) ;
#12782 = EDGE_CURVE ( 'NONE', #51228, #27673, #54272, .T. ) ;
#12783 = CARTESIAN_POINT ( 'NONE',  ( 100.3400348588553328, -31.46521817125301368, 155.2209912566479488 ) ) ;
#12784 = CARTESIAN_POINT ( 'NONE',  ( 117.5318583147471401, -37.01683481156648980, 43.80419670448293346 ) ) ;
#12785 = CARTESIAN_POINT ( 'NONE',  ( 25.56670390244797275, -67.87844715994100397, 257.2178068554150059 ) ) ;
#12786 = ORIENTED_EDGE ( 'NONE', *, *, #51122, .F. ) ;
#12787 = EDGE_CURVE ( 'NONE', #84106, #18961, #25357, .T. ) ;
#12788 = DIRECTION ( 'NONE',  ( 0.000000000000000000, 0.000000000000000000, 1.000000000000000000 ) ) ;
#12789 = EDGE_CURVE ( 'NONE', #77070, #72856, #19852, .T. ) ;
#12790 = VERTEX_POINT ( 'NONE', #84788 ) ;
#12791 = DIRECTION ( 'NONE',  ( -1.000000000000000000, -8.163404592832032979E-16, 0.000000000000000000 ) ) ;
#12792 = EDGE_CURVE ( 'NONE', #12340, #76826, #28211, .T. ) ;
#12793 = ORIENTED_EDGE ( 'NONE', *, *, #87035, .F. ) ;
#12794 = DIRECTION ( 'NONE',  ( 1.000000000000000000, -3.418174336900117128E-15, 0.000000000000000000 ) ) ;
#12795 = CIRCLE ( 'NONE', #75160, 10.00000000000000711 ) ;
#12796 = CARTESIAN_POINT ( 'NONE',  ( -12.57992038868342810, 81.72639488118660722, 117.8866931554271247 ) ) ;
#12797 = CARTESIAN_POINT ( 'NONE',  ( 81.84766347661002328, -83.77844715994096703, 55.21780685541800437 ) ) ;
#12798 = B_SPLINE_CURVE_WITH_KNOTS ( 'NONE', 3,
 ( #53580, #18646, #39975, #25457 ),
 .UNSPECIFIED., .F., .F.,
 ( 4, 4 ),
 ( 0.000000000000000000, 0.001454366796625762874 ),
 .UNSPECIFIED. ) ;
#12800 = CARTESIAN_POINT ( 'NONE',  ( 141.8545562996767444, -1.932463243632623229, 361.9756252759100335 ) ) ;
#12799 = AXIS2_PLACEMENT_3D ( 'NONE', #51006, #86002, #49208 ) ;
#12801 = ORIENTED_EDGE ( 'NONE', *, *, #8272, .T. ) ;
#12802 = AXIS2_PLACEMENT_3D ( 'NONE', #86757, #66287, #78174 ) ;
#12803 = CARTESIAN_POINT ( 'NONE',  ( 118.2322726120735155, -40.77409347166903331, 23.54991099019593292 ) ) ;
#12804 = CARTESIAN_POINT ( 'NONE',  ( 103.4621965996249600, -25.38836122657986394, 51.32133956162493149 ) ) ;
#12805 =( NAMED_UNIT ( * ) PLANE_ANGLE_UNIT ( ) SI_UNIT ( $, .RADIAN. ) );
#12807 = PLANE ( 'NONE',  #32565 ) ;
#12806 = CYLINDRICAL_SURFACE ( 'NONE', #27488, 8.999999999999994671 ) ;
#12808 = CARTESIAN_POINT ( 'NONE',  ( 102.0670646858952040, -27.97049243879484237, 146.4902315787838347 ) ) ;
#12809 = CARTESIAN_POINT ( 'NONE',  ( 131.5094688080979211, -17.71735499139275305, 2.839545688279645042 ) ) ;
#12810 = VERTEX_POINT ( 'NONE', #15738 ) ;
#12811 = EDGE_CURVE ( 'NONE', #36283, #73560, #50684, .T. ) ;
#12812 = VECTOR ( 'NONE', #24579, 999.9999999999998863 ) ;
#12813 = CARTESIAN_POINT ( 'NONE',  ( 25.56670390244797275, -62.87844715994099687, 137.2178068554150059 ) ) ;
#12814 = VECTOR ( 'NONE', #41519, 1000.000000000000000 ) ;
#12815 = CARTESIAN_POINT ( 'NONE',  ( 147.0667039024470171, -101.1152392874521126, 245.7200378389940170 ) ) ;
#12816 = CARTESIAN_POINT ( 'NONE',  ( 38.10000000000000142, 82.54999999999999716, 315.3410000000000082 ) ) ;
#12817 = ORIENTED_EDGE ( 'NONE', *, *, #54071, .F. ) ;
#12818 = CARTESIAN_POINT ( 'NONE',  ( 106.6048964044850607, -25.63891871564037928, 40.09753003781596448 ) ) ;
#12819 = CARTESIAN_POINT ( 'NONE',  ( 95.32466046839788021, -34.95410283156319053, 67.20705384733894050 ) ) ;
#12820 = VECTOR ( 'NONE', #20833, 1000.000000000000000 ) ;
#12822 = FACE_OUTER_BOUND ( 'NONE', #71197, .T. ) ;
#12821 = CARTESIAN_POINT ( 'NONE',  ( 116.8163290874346529, -34.14984622352434940, 174.0307337802608743 ) ) ;
#12823 = DIRECTION ( 'NONE',  ( 0.000000000000000000, -1.000000000000000000, 0.000000000000000000 ) ) ;
#12824 = CARTESIAN_POINT ( 'NONE',  ( 145.4713219652040834, -135.8544957252408949, 247.4783998280190076 ) ) ;
#12825 = EDGE_LOOP ( 'NONE', ( #44983, #30253, #88553, #3980 ) ) ;
#12826 = CARTESIAN_POINT ( 'NONE',  ( 97.28626111821324685, -36.62605694204433604, 107.3184824187669619 ) ) ;
#12827 = AXIS2_PLACEMENT_3D ( 'NONE', #28627, #50403, #72209 ) ;
#12829 = ORIENTED_EDGE ( 'NONE', *, *, #28589, .T. ) ;
#12828 = CARTESIAN_POINT ( 'NONE',  ( 7.568530249623516504, 92.75688873515042587, 130.3366983285493461 ) ) ;
#12830 = CARTESIAN_POINT ( 'NONE',  ( 112.4430884738663394, -45.67687932769430859, 234.0070538473389377 ) ) ;
#12831 = CARTESIAN_POINT ( 'NONE',  ( 97.81310256251512669, -40.52087785597539948, 252.6358801373274048 ) ) ;
#12832 = CARTESIAN_POINT ( 'NONE',  ( 116.9155271266333642, -38.71841217917236122, 148.6681463939105754 ) ) ;
#12833 = CYLINDRICAL_SURFACE ( 'NONE', #66078, 4.874999999999990230 ) ;
#12834 = DIRECTION ( 'NONE',  ( 1.000000000000000000, 6.145690160522439356E-16, 0.000000000000000000 ) ) ;
#12835 = CARTESIAN_POINT ( 'NONE',  ( 75.31670390244798341, -67.87844715994100397, 86.31780685541500020 ) ) ;
#12836 = CARTESIAN_POINT ( 'NONE',  ( -100.4321520267694723, 78.46444036551649504, 83.41622542100928683 ) ) ;
#12837 = CARTESIAN_POINT ( 'NONE',  ( 99.89458030379213938, -28.23347241844141919, 150.6356252759109680 ) ) ;
#12838 = CIRCLE ( 'NONE', #56310, 12.44599999999999795 ) ;
#12839 = VERTEX_POINT ( 'NONE', #70244 ) ;
#12840 = EDGE_LOOP ( 'NONE', ( #86570, #72475, #26590, #31340 ) ) ;
#12841 = ADVANCED_FACE ( 'NONE', ( #62969 ), #43412, .F. ) ;
#12842 = AXIS2_PLACEMENT_3D ( 'NONE', #88803, #54227, #61509 ) ;
#12843 = CARTESIAN_POINT ( 'NONE',  ( 112.1755263188685205, -29.48886997617658423, 126.0187261630399718 ) ) ;
#12844 = LINE ( 'NONE', #60058, #28343 ) ;
#12846 = CARTESIAN_POINT ( 'NONE',  ( -215.9010000000000105, 52.73749999999999716, -44.45000000000000284 ) ) ;
#12845 = CARTESIAN_POINT ( 'NONE',  ( 117.4008144674644285, -32.62901037329578458, 245.1270538473389706 ) ) ;
#12847 = CARTESIAN_POINT ( 'NONE',  ( 57.56670390244804736, -42.82844715994040286, 293.2178068554150627 ) ) ;
#12848 = EDGE_CURVE ( 'NONE', #78132, #21144, #36631, .T. ) ;
#12849 = DIRECTION ( 'NONE',  ( 0.000000000000000000, -1.000000000000000000, 0.000000000000000000 ) ) ;
#12850 = CARTESIAN_POINT ( 'NONE',  ( 47.62500000000000000, 94.53880000000000905, 229.3937500000000114 ) ) ;
#12851 = DIRECTION ( 'NONE',  ( 0.000000000000000000, -1.000000000000000000, 0.000000000000000000 ) ) ;
#12852 = DIRECTION ( 'NONE',  ( 1.000000000000000078E-15, 0.000000000000000000, -1.000000000000000000 ) ) ;
#12853 = CARTESIAN_POINT ( 'NONE',  ( 98.27975524859421341, -42.29919363830190804, 186.7756252759109543 ) ) ;
#12854 = LINE ( 'NONE', #40540, #86675 ) ;
#12855 = VERTEX_POINT ( 'NONE', #78425 ) ;
#12856 = ORIENTED_EDGE ( 'NONE', *, *, #86441, .T. ) ;
#12857 = VECTOR ( 'NONE', #13900, 1000.000000000000000 ) ;
#12858 = CARTESIAN_POINT ( 'NONE',  ( 69.56670390244704549, -118.2784471599409812, 45.21780685541799727 ) ) ;
#12859 = DIRECTION ( 'NONE',  ( -3.100000000000000258E-29, 3.100000000000000044E-14, 1.000000000000000000 ) ) ;
#12860 = DIRECTION ( 'NONE',  ( -3.999999999999999995E-14, 1.000000000000000000, -4.100000000000000342E-29 ) ) ;
#12861 = DIRECTION ( 'NONE',  ( 1.000000000000000078E-15, -1.000000000000000083E-30, -1.000000000000000000 ) ) ;
#12863 = CARTESIAN_POINT ( 'NONE',  ( 44.45000000000000284, 66.67499999999999716, 257.1750000000000114 ) ) ;
#12862 = CIRCLE ( 'NONE', #66532, 4.762500000000002842 ) ;
#12864 = VECTOR ( 'NONE', #85937, 1000.000000000000000 ) ;
#12865 = ORIENTED_EDGE ( 'NONE', *, *, #57036, .T. ) ;
#12866 = ADVANCED_FACE ( 'NONE', ( #64331 ), #49781, .T. ) ;
#12867 = FACE_OUTER_BOUND ( 'NONE', #28910, .T. ) ;
#12868 = CARTESIAN_POINT ( 'NONE',  ( 103.6385507868184277, -26.22095696399066966, 210.3394347997209763 ) ) ;
#12869 = VERTEX_POINT ( 'NONE', #28450 ) ;
#12870 = AXIS2_PLACEMENT_3D ( 'NONE', #15663, #71083, #43790 ) ;
#12871 = FACE_OUTER_BOUND ( 'NONE', #84976, .T. ) ;
#12872 = DIRECTION ( 'NONE',  ( -1.000000000000000000, 0.000000000000000000, 0.000000000000000000 ) ) ;
#12873 = CARTESIAN_POINT ( 'NONE',  ( 115.0365168329930867, -42.90940218011385809, 164.3021974415819670 ) ) ;
#12874 = CARTESIAN_POINT ( 'NONE',  ( 113.7569007282865101, -30.30027569836345336, 37.25380465530597718 ) ) ;
#12876 = CARTESIAN_POINT ( 'NONE',  ( 109.3632651814324817, -25.89385771158341853, 180.9222919425779708 ) ) ;
#12875 = AXIS2_PLACEMENT_3D ( 'NONE', #2897, #66440, #86469 ) ;
#12877 = CARTESIAN_POINT ( 'NONE',  ( 162.7131505118679797, -31.94127993907790852, 193.9678068554150059 ) ) ;
#12878 = ORIENTED_EDGE ( 'NONE', *, *, #10171, .F. ) ;
#12879 = LINE ( 'NONE', #42338, #1606 ) ;
#12880 = CARTESIAN_POINT ( 'NONE',  ( 111.7624441058946871, -45.65476495282741354, 67.96418635338669390 ) ) ;
#12881 = EDGE_LOOP ( 'NONE', ( #59775, #24980, #5869, #15207 ) ) ;
#12882 = ORIENTED_EDGE ( 'NONE', *, *, #21949, .T. ) ;
#12883 = DIRECTION ( 'NONE',  ( -0.7071067811869841124, 0.7071067811861110330, 0.000000000000000000 ) ) ;
#12884 = EDGE_LOOP ( 'NONE', ( #60433, #2226, #21209, #83447 ) ) ;
#12885 = ORIENTED_EDGE ( 'NONE', *, *, #5497, .F. ) ;
#12886 = DIRECTION ( 'NONE',  ( 0.000000000000000000, -1.000000000000000000, 0.000000000000000000 ) ) ;
#12887 = ADVANCED_FACE ( 'NONE', ( #21203 ), #37068, .F. ) ;
#12888 = CARTESIAN_POINT ( 'NONE',  ( 112.3043975166656736, -44.90470753876829235, 67.45241982807698378 ) ) ;
#12889 = CARTESIAN_POINT ( 'NONE',  ( 118.8150946519381250, -38.46269469016341702, 223.7099109901969598 ) ) ;
#12890 = CARTESIAN_POINT ( 'NONE',  ( 96.07698540226623152, -35.78353028925530310, 186.2461014663869889 ) ) ;
#12892 = CARTESIAN_POINT ( 'NONE',  ( 110.2773916389477478, -46.62487827714361543, 8.827053847339950465 ) ) ;
#12891 = CARTESIAN_POINT ( 'NONE',  ( 84.06648329127399677, -18.82844715994099971, 239.5838068554169809 ) ) ;
#12893 = CARTESIAN_POINT ( 'NONE',  ( 194.0371591254573502, -24.89890238294407965, 249.9678068554149775 ) ) ;
#12894 = EDGE_CURVE ( 'NONE', #8142, #5023, #2102, .T. ) ;
#12895 = DIRECTION ( 'NONE',  ( -1.000000000000000000, -5.512527431108013646E-15, 0.000000000000000000 ) ) ;
#12896 = ORIENTED_EDGE ( 'NONE', *, *, #62593, .T. ) ;
#12897 = VECTOR ( 'NONE', #46421, 1000.000000000000000 ) ;
#12898 = DIRECTION ( 'NONE',  ( 0.000000000000000000, 0.000000000000000000, -1.000000000000000000 ) ) ;
#12899 = CARTESIAN_POINT ( 'NONE',  ( 105.6259887305572676, -47.09919361126699044, 257.4670538473392298 ) ) ;
#12900 = ORIENTED_EDGE ( 'NONE', *, *, #49047, .T. ) ;
#12901 = CARTESIAN_POINT ( 'NONE',  ( 114.1248632939498719, -29.05700933358840032, 199.4841967044819739 ) ) ;
#12902 = DIRECTION ( 'NONE',  ( 0.000000000000000000, -1.000000000000000000, 0.000000000000000000 ) ) ;
#12903 = CARTESIAN_POINT ( 'NONE',  ( -23.27731929905159802, 54.32390312253606623, 30.16249999999998366 ) ) ;
#12904 = FILL_AREA_STYLE ('',( #67855 ) ) ;
#12905 = CARTESIAN_POINT ( 'NONE',  ( 112.5286436197554849, -45.20754988127118423, 29.03387687458365818 ) ) ;
#12907 = LINE ( 'NONE', #89211, #2184 ) ;
#12906 = CARTESIAN_POINT ( 'NONE',  ( 99.40665670852901314, -32.99082215312059674, 277.6356252759109680 ) ) ;
#12908 = CARTESIAN_POINT ( 'NONE',  ( 97.86658801961326049, -40.64925014044468554, 172.6469892981851615 ) ) ;
#12909 = DIRECTION ( 'NONE',  ( 1.000000000000000000, 0.000000000000000000, -9.299908063537909262E-17 ) ) ;
#12910 = DIRECTION ( 'NONE',  ( 9.860761315262647568E-31, -0.7071067811865480168, 0.7071067811865470176 ) ) ;
#12911 = ADVANCED_FACE ( 'NONE', ( #22558 ), #48546, .T. ) ;
#12912 = DIRECTION ( 'NONE',  ( -1.000000000000000078E-15, -1.000000000000000083E-30, 1.000000000000000000 ) ) ;
#12913 = EDGE_CURVE ( 'NONE', #8428, #21819, #79008, .T. ) ;
#12914 = DIRECTION ( 'NONE',  ( 0.000000000000000000, 0.000000000000000000, -1.000000000000000000 ) ) ;
#12915 = DIRECTION ( 'NONE',  ( 1.000000000000000078E-15, -1.000000000000000000, 0.000000000000000000 ) ) ;
#12917 = ORIENTED_EDGE ( 'NONE', *, *, #76897, .T. ) ;
#12916 = CARTESIAN_POINT ( 'NONE',  ( 107.0667039024479834, -36.72944715994099596, 239.5838068554170093 ) ) ;
#12918 = VECTOR ( 'NONE', #43721, 1000.000000000000000 ) ;
#12919 = CARTESIAN_POINT ( 'NONE',  ( 107.0667039024470313, -104.2784471599420755, -19.78219314458201694 ) ) ;
#12920 = CARTESIAN_POINT ( 'NONE',  ( 106.9401735163927611, -47.80552439772274909, 232.5794347997199907 ) ) ;
#12921 = CARTESIAN_POINT ( 'NONE',  ( 98.14961424977839499, -43.26117181588809757, 102.8175300378159847 ) ) ;
#12922 = CARTESIAN_POINT ( 'NONE',  ( 114.4457317200277089, -27.39361268404408634, 270.5441967044823741 ) ) ;
#12923 = CARTESIAN_POINT ( 'NONE',  ( 115.8254323940822843, -31.73001883404345236, 154.2397919421239010 ) ) ;
#12924 = CARTESIAN_POINT ( 'NONE',  ( 167.6524903400753601, -48.32844715993521589, 249.9678068554149775 ) ) ;
#12926 = DIRECTION ( 'NONE',  ( 3.100000000000000258E-29, -3.100000000000000044E-14, -1.000000000000000000 ) ) ;
#12925 = CARTESIAN_POINT ( 'NONE',  ( 164.9190312289449878, -35.91149509761181235, -5.074374724088000832 ) ) ;
#12927 = CARTESIAN_POINT ( 'NONE',  ( -462.0260000000000105, 53.97500000000000142, -3.174999999999999822 ) ) ;
#12928 = CARTESIAN_POINT ( 'NONE',  ( 131.4524275574070487, -19.60567372263979280, 2.908038864009617086 ) ) ;
#12929 = AXIS2_PLACEMENT_3D ( 'NONE', #80757, #46195, #39841 ) ;
#12930 = CIRCLE ( 'NONE', #76785, 7.874000000000005883 ) ;
#12931 = ORIENTED_EDGE ( 'NONE', *, *, #61487, .T. ) ;
#12932 = ORIENTED_EDGE ( 'NONE', *, *, #8710, .F. ) ;
#12933 = CARTESIAN_POINT ( 'NONE',  ( 108.8156685800011303, -28.36903548837926792, 139.3352769709339896 ) ) ;
#12934 = CIRCLE ( 'NONE', #65186, 0.9999999999991942001 ) ;
#12936 = ORIENTED_EDGE ( 'NONE', *, *, #52027, .F. ) ;
#12935 = DIRECTION ( 'NONE',  ( 1.000000000000000000, 0.000000000000000000, -0.000000000000000000 ) ) ;
#12937 = CARTESIAN_POINT ( 'NONE',  ( 72.25757238336811383, -1.944390235229867425, 394.9756252759101471 ) ) ;
#12938 = CARTESIAN_POINT ( 'NONE',  ( 108.2741602056595269, -26.36093993100608657, 125.9841967044819597 ) ) ;
#12939 = PLANE ( 'NONE',  #75829 ) ;
#12940 = VECTOR ( 'NONE', #19423, 1000.000000000000000 ) ;
#12941 = CARTESIAN_POINT ( 'NONE',  ( 49.21437657594998427, -35.91149509761070391, 342.9256252759119548 ) ) ;
#12942 = DIRECTION ( 'NONE',  ( -0.7071067811865501263, 0.7071067811865449082, -7.071067811865501957E-16 ) ) ;
#12943 = FACE_BOUND ( 'NONE', #47307, .T. ) ;
#12944 = AXIS2_PLACEMENT_3D ( 'NONE', #38260, #16051, #86432 ) ;
#12945 = CARTESIAN_POINT ( 'NONE',  ( 104.2296407737279509, -46.70397019442136610, 67.36800622829292706 ) ) ;
#12946 = ORIENTED_EDGE ( 'NONE', *, *, #27353, .F. ) ;
#12947 = ORIENTED_EDGE ( 'NONE', *, *, #40397, .T. ) ;
#12948 = ORIENTED_EDGE ( 'NONE', *, *, #31545, .T. ) ;
#12949 = DIRECTION ( 'NONE',  ( 0.000000000000000000, 1.000000000000000000, 0.000000000000000000 ) ) ;
#12951 = FACE_OUTER_BOUND ( 'NONE', #39964, .T. ) ;
#12950 = CARTESIAN_POINT ( 'NONE',  ( 98.51953950620418254, -30.85675296092865239, 161.8594347997199918 ) ) ;
#12952 = DIRECTION ( 'NONE',  ( 1.000000000000000078E-15, 0.000000000000000000, -1.000000000000000000 ) ) ;
#12954 = ADVANCED_FACE ( 'NONE', ( #57503 ), #76614, .T. ) ;
#12953 = FACE_OUTER_BOUND ( 'NONE', #25311, .T. ) ;
#12955 = VECTOR ( 'NONE', #46711, 1000.000000000000000 ) ;
#12956 = CARTESIAN_POINT ( 'NONE',  ( 173.9900000000000091, 53.21300000000000097, 41.63456447661469895 ) ) ;
#12957 = CARTESIAN_POINT ( 'NONE',  ( 82.65057572782268380, 95.14807216649717247, 84.99753727674189463 ) ) ;
#12958 = CARTESIAN_POINT ( 'NONE',  ( 107.0664832912739968, -36.72944715994100306, 277.6356252759110248 ) ) ;
#12959 = CARTESIAN_POINT ( 'NONE',  ( 97.56228874418788166, -32.49873190831181802, 100.9927681330539713 ) ) ;
#12960 = ORIENTED_EDGE ( 'NONE', *, *, #1943, .F. ) ;
#12961 = EDGE_LOOP ( 'NONE', ( #46566, #51561, #86350, #44808, #22333, #89842 ) ) ;
#12962 = ORIENTED_EDGE ( 'NONE', *, *, #60322, .T. ) ;
#12963 = LINE ( 'NONE', #40652, #42983 ) ;
#12964 = CARTESIAN_POINT ( 'NONE',  ( -83.76986456925402535, 87.79544278253753475, -100.1374281256143774 ) ) ;
#12965 = CYLINDRICAL_SURFACE ( 'NONE', #39481, 2.030000000002079918 ) ;
#12966 = CARTESIAN_POINT ( 'NONE',  ( 103.7603453811189667, -44.19263536178414142, 175.0623760838769840 ) ) ;
#12967 = VECTOR ( 'NONE', #53800, 1000.000000000000000 ) ;
#12968 = EDGE_CURVE ( 'NONE', #23436, #61346, #22113, .T. ) ;
#12969 = B_SPLINE_CURVE_WITH_KNOTS ( 'NONE', 3,
 ( #9810, #31572, #66093, #64333, #43867, #36632, #10252, #71600, #65653, #72485, #78427, #72915, #87005, #59278, #58392, #37069, #16189, #9362 ),
 .UNSPECIFIED., .F., .F.,
 ( 4, 2, 2, 2, 2, 2, 2, 2, 4 ),
 ( 0.4999946744394294096, 0.5624953401345007542, 0.6249960058295720433, 0.6874966715246433324, 0.7499973372197146215, 0.8124980029147859106, 0.8749986686098573108, 0.9374993343049287109, 1.000000000000000000 ),
 .UNSPECIFIED. ) ;
#12970 = CARTESIAN_POINT ( 'NONE',  ( 102.0676263548437248, -27.97016309701666614, 26.48917362245403240 ) ) ;
#12971 = ORIENTED_EDGE ( 'NONE', *, *, #41562, .F. ) ;
#12973 = ORIENTED_EDGE ( 'NONE', *, *, #38401, .T. ) ;
#12972 = ORIENTED_EDGE ( 'NONE', *, *, #9622, .F. ) ;
#12974 = DIRECTION ( 'NONE',  ( 0.000000000000000000, -1.000000000000000000, 0.000000000000000000 ) ) ;
#12975 = CARTESIAN_POINT ( 'NONE',  ( 135.2096185787404181, -21.23068377182193345, 1.829869271364342076 ) ) ;
#12976 = ORIENTED_EDGE ( 'NONE', *, *, #38644, .T. ) ;
#12977 = ORIENTED_EDGE ( 'NONE', *, *, #46724, .T. ) ;
#12978 = CARTESIAN_POINT ( 'NONE',  ( 34.67381068362099228, -26.00627455219321860, -5.074374724088000832 ) ) ;
#12979 = EDGE_CURVE ( 'NONE', #16028, #25661, #7574, .T. ) ;
#12980 = CARTESIAN_POINT ( 'NONE',  ( 97.76609424928555825, -35.39554716186696481, 222.6568214011349767 ) ) ;
#12981 = VECTOR ( 'NONE', #20950, 1000.000000000000000 ) ;
#12982 = EDGE_CURVE ( 'NONE', #2549, #31941, #31188, .T. ) ;
#12983 = CARTESIAN_POINT ( 'NONE',  ( 52.99265158129180264, 69.84999999999999432, 346.9005000000000223 ) ) ;
#12984 = CARTESIAN_POINT ( 'NONE',  ( -122.8759924518541169, 73.50212837636460961, 44.11811403647472929 ) ) ;
#12985 = VECTOR ( 'NONE', #64178, 1000.000000000000000 ) ;
#12986 = ORIENTED_EDGE ( 'NONE', *, *, #49151, .T. ) ;
#12987 = VERTEX_POINT ( 'NONE', #49333 ) ;
#12988 = LINE ( 'NONE', #62906, #59399 ) ;
#12989 = VERTEX_POINT ( 'NONE', #77067 ) ;
#12990 = ORIENTED_EDGE ( 'NONE', *, *, #25793, .F. ) ;
#12991 = EDGE_CURVE ( 'NONE', #49825, #8449, #14846, .T. ) ;
#12992 = CARTESIAN_POINT ( 'NONE',  ( 108.8441613132982155, -28.76266695291210951, 222.7195189410199703 ) ) ;
#12993 = CIRCLE ( 'NONE', #24592, 188.9759999999999991 ) ;
#12994 = CARTESIAN_POINT ( 'NONE',  ( 109.2059698035850914, -26.50355049596284118, 139.9127681330539872 ) ) ;
#12995 = CARTESIAN_POINT ( 'NONE',  ( 96.11054930851071276, -38.00668368623060189, 86.43086337114897333 ) ) ;
#12996 = CARTESIAN_POINT ( 'NONE',  ( 101.8644741850226580, -30.26426668629352079, 249.5838068554171514 ) ) ;
#12997 = PLANE ( 'NONE',  #17684 ) ;
#12998 = CARTESIAN_POINT ( 'NONE',  ( 107.9469797351305118, -25.30413091219610422, 322.6728824914080747 ) ) ;
#12999 = CARTESIAN_POINT ( 'NONE',  ( 101.9845378472182773, -45.87248622144053911, 183.1727681330539781 ) ) ;
#13000 = EDGE_CURVE ( 'NONE', #9037, #88384, #15292, .T. ) ;
#13001 = CARTESIAN_POINT ( 'NONE',  ( 116.3265940946004378, -32.93621273019581253, 125.1356252759109680 ) ) ;
#13002 = EDGE_LOOP ( 'NONE', ( #24227, #62900, #16556, #47310, #32080 ) ) ;
#13003 = CARTESIAN_POINT ( 'NONE',  ( 1.387778780781445676E-14, 239.0000000000000000, 97.27542076772557778 ) ) ;
#13004 = ORIENTED_EDGE ( 'NONE', *, *, #43647, .F. ) ;
#13005 = ORIENTED_EDGE ( 'NONE', *, *, #85904, .F. ) ;
#13006 = CARTESIAN_POINT ( 'NONE',  ( 208.9149999999999920, 28.98850000000000193, -58.73749999999999716 ) ) ;
#13007 = EDGE_LOOP ( 'NONE', ( #61397, #49239, #14174, #50224 ) ) ;
#13008 = CARTESIAN_POINT ( 'NONE',  ( 87.06648329127403940, -46.72944715994105280, -4.824374724089049771 ) ) ;
#13009 = CARTESIAN_POINT ( 'NONE',  ( 99.50153220775246155, -43.90290835836871253, 81.92991099019597812 ) ) ;
#13010 = CARTESIAN_POINT ( 'NONE',  ( -4.771202963297667132, 70.78025357177421029, 130.4687910435467018 ) ) ;
#13011 = CYLINDRICAL_SURFACE ( 'NONE', #2901, 0.2499999999999941991 ) ;
#13012 = CARTESIAN_POINT ( 'NONE',  ( 152.0371591254585724, -47.82818131005588214, 129.9678068554149775 ) ) ;
#13015 = CARTESIAN_POINT ( 'NONE',  ( 105.1150531980676561, -26.51080800785444680, 231.2270538473399597 ) ) ;
#13014 = FACE_OUTER_BOUND ( 'NONE', #73364, .T. ) ;
#13013 = CARTESIAN_POINT ( 'NONE',  ( 97.81169461453751524, -40.51741999607308742, 142.6356648221729131 ) ) ;
#13016 = FACE_OUTER_BOUND ( 'NONE', #8873, .T. ) ;
#13017 = DIRECTION ( 'NONE',  ( 1.000000000000000000, 0.000000000000000000, 0.000000000000000000 ) ) ;
#13018 = EDGE_LOOP ( 'NONE', ( #68121, #68080, #77595, #20230 ) ) ;
#13019 = AXIS2_PLACEMENT_3D ( 'NONE', #70313, #84412, #8542 ) ;
#13020 = CARTESIAN_POINT ( 'NONE',  ( 107.0664832912739257, -52.42944715994095617, 311.3356252759109566 ) ) ;
#13021 = EDGE_CURVE ( 'NONE', #7162, #31385, #36172, .T. ) ;
#13022 = DIRECTION ( 'NONE',  ( 0.000000000000000000, 1.000000000000000000, 0.000000000000000000 ) ) ;
#13023 = EDGE_CURVE ( 'NONE', #13042, #28081, #23459, .T. ) ;
#13024 = DIRECTION ( 'NONE',  ( 0.000000000000000000, -1.000000000000000000, 0.000000000000000000 ) ) ;
#13025 = EDGE_CURVE ( 'NONE', #54266, #86672, #3651, .T. ) ;
#13026 = LINE ( 'NONE', #7101, #70918 ) ;
#13028 = ORIENTED_EDGE ( 'NONE', *, *, #779, .F. ) ;
#13027 = CARTESIAN_POINT ( 'NONE',  ( 104.3127904766024443, -25.97630531626002437, 245.2880062282919482 ) ) ;
#13029 = CARTESIAN_POINT ( 'NONE',  ( -33.98325472291460159, 104.3431970271541900, -3.175000000000234746 ) ) ;
#13030 = CARTESIAN_POINT ( 'NONE',  ( 104.2409529242390391, -46.76432966167102023, 18.35848241876792031 ) ) ;
#13031 = CARTESIAN_POINT ( 'NONE',  ( 95.52146136750830863, -39.61450893497475079, 162.5213395616259788 ) ) ;
#13032 = EDGE_CURVE ( 'NONE', #9271, #67598, #37519, .T. ) ;
#13033 = CARTESIAN_POINT ( 'NONE',  ( -41.60202597009397607, 40.59999999999997300, 54.66767516814134353 ) ) ;
#13034 = CARTESIAN_POINT ( 'NONE',  ( 172.5664832912740110, -27.82844715994070484, 143.6756252759119832 ) ) ;
#13035 = VECTOR ( 'NONE', #6039, 1000.000000000000000 ) ;
#13037 = CARTESIAN_POINT ( 'NONE',  ( 107.0664832912739968, -36.72944715994100306, 287.6356252759109680 ) ) ;
#13036 = DIRECTION ( 'NONE',  ( -6.493183223601999383E-14, 1.000000000000000000, -6.593183223602000791E-29 ) ) ;
#13038 = CARTESIAN_POINT ( 'NONE',  ( 130.5667039024480118, -34.21194715994094082, 229.5838068554170093 ) ) ;
#13039 = DIRECTION ( 'NONE',  ( -1.000000000000000078E-15, 1.000000000000000083E-30, 1.000000000000000000 ) ) ;
#13040 = VERTEX_POINT ( 'NONE', #24329 ) ;
#13041 = ORIENTED_EDGE ( 'NONE', *, *, #40952, .F. ) ;
#13042 = VERTEX_POINT ( 'NONE', #87450 ) ;
#13043 = CONICAL_SURFACE ( 'NONE', #47820, 13.31607168056649826, 0.1047197551196538678 ) ;
#13044 = ORIENTED_EDGE ( 'NONE', *, *, #29691, .F. ) ;
#13045 = CARTESIAN_POINT ( 'NONE',  ( -24.79284581386642827, 184.0000000000000000, 101.0189074266571794 ) ) ;
#13046 = CARTESIAN_POINT ( 'NONE',  ( 117.4903696573863385, -37.28369426754698424, 14.78419670448294454 ) ) ;
#13047 = CARTESIAN_POINT ( 'NONE',  ( 129.9879594898645792, -139.1139133488901223, 247.5865165982399958 ) ) ;
#13049 = CARTESIAN_POINT ( 'NONE',  ( 19.56670390244739721, -25.42844715994192129, 249.9678068554150059 ) ) ;
#13048 = AXIS2_PLACEMENT_3D ( 'NONE', #72468, #45178, #31558 ) ;
#13050 = DIRECTION ( 'NONE',  ( 0.000000000000000000, 0.000000000000000000, 1.000000000000000000 ) ) ;
#13051 = CARTESIAN_POINT ( 'NONE',  ( 105.4642979808546670, -28.33962392264099250, 234.6495626852199621 ) ) ;
#13052 = VERTEX_POINT ( 'NONE', #72484 ) ;
#13053 = EDGE_LOOP ( 'NONE', ( #34545, #22263, #52889, #21784 ) ) ;
#13055 = EDGE_LOOP ( 'NONE', ( #87640, #42209, #52577, #32292, #64777, #16734 ) ) ;
#13054 = VECTOR ( 'NONE', #88419, 1000.000000000000000 ) ;
#13056 = FACE_OUTER_BOUND ( 'NONE', #25871, .T. ) ;
#13057 = CARTESIAN_POINT ( 'NONE',  ( 104.4081941772929980, -46.45811691506909114, 102.3647646864374110 ) ) ;
#13058 = DIRECTION ( 'NONE',  ( 1.000000000000000078E-15, 1.000000000000000083E-30, -1.000000000000000000 ) ) ;
#13059 = DIRECTION ( 'NONE',  ( 1.067522139062650671E-15, 1.000000000000000000, 0.000000000000000000 ) ) ;
#13060 = FACE_OUTER_BOUND ( 'NONE', #65277, .T. ) ;
#13061 = AXIS2_PLACEMENT_3D ( 'NONE', #27828, #48250, #27380 ) ;
#13062 = FACE_OUTER_BOUND ( 'NONE', #63818, .T. ) ;
#13063 = CARTESIAN_POINT ( 'NONE',  ( 100.6033219294167793, -44.83909144599476804, 272.0289586092449667 ) ) ;
#13064 = DIRECTION ( 'NONE',  ( 0.000000000000000000, 0.000000000000000000, -1.000000000000000000 ) ) ;
#13065 = ORIENTED_EDGE ( 'NONE', *, *, #46185, .F. ) ;
#13066 = LINE ( 'NONE', #74392, #78048 ) ;
#13067 = CIRCLE ( 'NONE', #85640, 0.5000000000000004441 ) ;
#13068 = CYLINDRICAL_SURFACE ( 'NONE', #61261, 13.44999999999999396 ) ;
#13069 = CARTESIAN_POINT ( 'NONE',  ( 114.1581430127411352, -30.74577825543392606, 72.20237608387697037 ) ) ;
#13070 = EDGE_CURVE ( 'NONE', #9306, #87803, #69443, .T. ) ;
#13071 = CARTESIAN_POINT ( 'NONE',  ( -100.8961411191535973, 120.6499999999999915, -3.968750000001104894 ) ) ;
#13072 = EDGE_CURVE ( 'NONE', #65138, #31678, #72914, .T. ) ;
#13073 = FACE_OUTER_BOUND ( 'NONE', #35394, .T. ) ;
#13074 = VECTOR ( 'NONE', #74780, 1000.000000000000000 ) ;
#13075 = DIRECTION ( 'NONE',  ( -2.900000000000000265E-14, 2.000000000000000155E-15, -1.000000000000000000 ) ) ;
#13076 = ORIENTED_EDGE ( 'NONE', *, *, #9927, .F. ) ;
#13077 = EDGE_CURVE ( 'NONE', #31310, #81967, #18390, .T. ) ;
#13078 = DIRECTION ( 'NONE',  ( 0.000000000000000000, 0.000000000000000000, 1.000000000000000000 ) ) ;
#13079 = ORIENTED_EDGE ( 'NONE', *, *, #2915, .F. ) ;
#13080 = CARTESIAN_POINT ( 'NONE',  ( 114.2535261088984981, -44.28147934099003180, 158.1813395616249807 ) ) ;
#13081 = VERTEX_POINT ( 'NONE', #51126 ) ;
#13082 = EDGE_CURVE ( 'NONE', #21703, #28403, #83467, .T. ) ;
#13083 = LINE ( 'NONE', #87151, #85251 ) ;
#13084 = CARTESIAN_POINT ( 'NONE',  ( 103.2343105203340201, -28.73928255177903068, 91.86444044875396742 ) ) ;
#13085 = EDGE_CURVE ( 'NONE', #85412, #21246, #78866, .T. ) ;
#13086 = DIRECTION ( 'NONE',  ( 0.7071067811865514585, -0.7071067811865435759, 7.071067811865522665E-16 ) ) ;
#13087 = PLANE ( 'NONE',  #39711 ) ;
#13088 = CIRCLE ( 'NONE', #62419, 5.562599999999973122 ) ;
#13089 = CARTESIAN_POINT ( 'NONE',  ( 101.9498695335308014, -27.62134513440381411, 56.48419670448296159 ) ) ;
#13090 = EDGE_CURVE ( 'NONE', #85887, #48350, #59715, .T. ) ;
#13091 = EDGE_CURVE ( 'NONE', #22706, #70290, #46076, .T. ) ;
#13092 = CARTESIAN_POINT ( 'NONE',  ( 0.000000000000000000, 92.07499999999998863, 38.10000000000000142 ) ) ;
#13093 = ORIENTED_EDGE ( 'NONE', *, *, #16668, .F. ) ;
#13094 = CARTESIAN_POINT ( 'NONE',  ( -118.0068565116053492, 76.93600387762168680, -11.39936611905761765 ) ) ;
#13095 =( BOUNDED_CURVE ( )  B_SPLINE_CURVE ( 3, ( #72017, #66066, #9338, #59692 ),
 .UNSPECIFIED., .F., .T. ) 
 B_SPLINE_CURVE_WITH_KNOTS ( ( 4, 4 ),
 ( 1.570796326794220432, 3.141592653588994200 ),
 .UNSPECIFIED. ) 
 CURVE ( )  GEOMETRIC_REPRESENTATION_ITEM ( )  RATIONAL_B_SPLINE_CURVE ( ( 1.000000000000000000, 0.8047378541243939143, 0.8047378541243939143, 1.000000000000000000 ) ) 
 REPRESENTATION_ITEM ( '' )  );
#13096 = ORIENTED_EDGE ( 'NONE', *, *, #40952, .T. ) ;
#13097 = EDGE_LOOP ( 'NONE', ( #86654, #8755, #61773, #34359, #41546, #31577 ) ) ;
#13098 = EDGE_CURVE ( 'NONE', #36775, #1670, #54379, .T. ) ;
#13099 = CIRCLE ( 'NONE', #46394, 0.5000000000000004441 ) ;
#13100 = CARTESIAN_POINT ( 'NONE',  ( 138.8167039024479834, -50.82844715994100682, 35.51780685541480409 ) ) ;
#13101 = ORIENTED_EDGE ( 'NONE', *, *, #23588, .F. ) ;
#13102 = CARTESIAN_POINT ( 'NONE',  ( 96.91794407517402021, -34.59732685048006573, 261.1737205140070159 ) ) ;
#13103 = CARTESIAN_POINT ( 'NONE',  ( 96.62828407576300549, -37.15518013270143172, 157.3584824187679487 ) ) ;
#13104 = CARTESIAN_POINT ( 'NONE',  ( 57.56670390244744340, -48.82844715994040286, 173.2178068554150911 ) ) ;
#13105 = DIRECTION ( 'NONE',  ( -0.8660254037844351549, 0.5000000000000061062, 0.000000000000000000 ) ) ;
#13106 = CARTESIAN_POINT ( 'NONE',  ( 97.54238320567634446, -32.48987111900922997, 96.99276813305395706 ) ) ;
#13107 = EDGE_CURVE ( 'NONE', #41269, #52484, #16961, .T. ) ;
#13108 = CARTESIAN_POINT ( 'NONE',  ( 102.0691103994968643, -27.96929322877106117, 96.48882554008449119 ) ) ;
#13109 = ORIENTED_EDGE ( 'NONE', *, *, #36764, .F. ) ;
#13110 = LINE ( 'NONE', #88959, #10452 ) ;
#13111 = CIRCLE ( 'NONE', #34875, 7.937500000000000000 ) ;
#13112 = FACE_OUTER_BOUND ( 'NONE', #30753, .T. ) ;
#13113 = ORIENTED_EDGE ( 'NONE', *, *, #41255, .T. ) ;
#13114 = AXIS2_PLACEMENT_3D ( 'NONE', #43159, #70901, #51310 ) ;
#13115 = DIRECTION ( 'NONE',  ( 1.000000000000000000, 2.999999999999999839E-15, 1.000000000000000078E-15 ) ) ;
#13116 = CARTESIAN_POINT ( 'NONE',  ( 41.56670390244783420, -36.32844715994104234, 249.9678068554150343 ) ) ;
#13117 = CARTESIAN_POINT ( 'NONE',  ( 116.1206117333611871, -31.56300607074027909, 289.2384824187681716 ) ) ;
#13118 = CARTESIAN_POINT ( 'NONE',  ( 41.56648329127398966, -18.82844715994071194, 318.9256252759120116 ) ) ;
#13119 = CARTESIAN_POINT ( 'NONE',  ( -179.8898777604655095, 0.000000000000000000, -12.69999999999999929 ) ) ;
#13120 = PLANE ( 'NONE',  #48994 ) ;
#13121 = CARTESIAN_POINT ( 'NONE',  ( 107.1874307469290386, -26.94942635195914349, 35.06705384733993469 ) ) ;
#13123 = CARTESIAN_POINT ( 'NONE',  ( 113.8422018911646774, -44.62364141802220985, 104.1413395616249744 ) ) ;
#13122 = CARTESIAN_POINT ( 'NONE',  ( 116.0344360784154532, -32.23950325226218183, 99.19648518757557554 ) ) ;
#13124 = DIRECTION ( 'NONE',  ( 3.999999999999999995E-14, -1.000000000000000000, 4.100000000000000342E-29 ) ) ;
#13125 = CARTESIAN_POINT ( 'NONE',  ( 117.8245512228195224, -33.99506276729055543, 169.0365776568629599 ) ) ;
#13126 = DIRECTION ( 'NONE',  ( 1.000000000000000000, -0.000000000000000000, 2.108231265501710124E-16 ) ) ;
#13127 = ORIENTED_EDGE ( 'NONE', *, *, #65988, .T. ) ;
#13128 = CIRCLE ( 'NONE', #14615, 2.750000000000002665 ) ;
#13129 = DIRECTION ( 'NONE',  ( 0.000000000000000000, 0.000000000000000000, 1.000000000000000000 ) ) ;
#13130 = LINE ( 'NONE', #40814, #18888 ) ;
#13131 = CARTESIAN_POINT ( 'NONE',  ( 136.4174407532110251, -35.29868422067971778, 2.608896314047598253 ) ) ;
#13132 = ORIENTED_EDGE ( 'NONE', *, *, #87637, .F. ) ;
#13133 = ADVANCED_FACE ( 'NONE', ( #79204 ), #65106, .F. ) ;
#13134 = FACE_OUTER_BOUND ( 'NONE', #47120, .T. ) ;
#13136 = ORIENTED_EDGE ( 'NONE', *, *, #33389, .T. ) ;
#13135 = CARTESIAN_POINT ( 'NONE',  ( 97.70685376065341643, -42.69687791250295561, 141.7661014663869707 ) ) ;
#13137 = CARTESIAN_POINT ( 'NONE',  ( 107.0667039024470313, -104.2784471599418197, -11.78219314458200984 ) ) ;
#13138 = EDGE_CURVE ( 'NONE', #88437, #26589, #80224, .T. ) ;
#13139 = DIRECTION ( 'NONE',  ( 1.000000000000000000, 4.163336342344333240E-14, 0.000000000000000000 ) ) ;
#13140 = CARTESIAN_POINT ( 'NONE',  ( 193.0371591254583450, -47.82818131005411999, 237.4678068554150059 ) ) ;
#13141 = DIRECTION ( 'NONE',  ( 0.000000000000000000, 0.000000000000000000, -1.000000000000000000 ) ) ;
#13142 = EDGE_LOOP ( 'NONE', ( #76348, #845, #5066, #62903 ) ) ;
#13143 = APPLICATION_PROTOCOL_DEFINITION ( 'draft international standard', 'automotive_design', 1998, #89874 ) ;
#13144 = ORIENTED_EDGE ( 'NONE', *, *, #78014, .F. ) ;
#13146 = EDGE_LOOP ( 'NONE', ( #17835, #64598, #80995, #87025 ) ) ;
#13145 = AXIS2_PLACEMENT_3D ( 'NONE', #8781, #35112, #1516 ) ;
#13147 = AXIS2_PLACEMENT_3D ( 'NONE', #65533, #51438, #85998 ) ;
#13148 = EDGE_LOOP ( 'NONE', ( #12408, #89748, #39042, #38993 ) ) ;
#13149 = CARTESIAN_POINT ( 'NONE',  ( 7.778756678762479992E-15, 50.79999999999999716, 222.8849999999999909 ) ) ;
#13150 = CARTESIAN_POINT ( 'NONE',  ( 88.25806911646408537, 93.94653598907717651, -96.20559720633534084 ) ) ;
#13151 = CARTESIAN_POINT ( 'NONE',  ( 116.3214453605167478, -32.94026287388232532, 159.1356252759109680 ) ) ;
#13152 = DIRECTION ( 'NONE',  ( 0.000000000000000000, 0.000000000000000000, -1.000000000000000000 ) ) ;
#13154 = CARTESIAN_POINT ( 'NONE',  ( -12.37563412544579045, 79.66819247178165142, -117.9083347083516173 ) ) ;
#13153 = FACE_OUTER_BOUND ( 'NONE', #11604, .T. ) ;
#13155 = DIRECTION ( 'NONE',  ( -1.000000000000000000, 0.000000000000000000, -2.108231265501709878E-16 ) ) ;
#13156 = EDGE_LOOP ( 'NONE', ( #58346, #12716, #28827, #19212 ) ) ;
#13157 = ORIENTED_EDGE ( 'NONE', *, *, #57972, .T. ) ;
#13158 = CARTESIAN_POINT ( 'NONE',  ( -254.0000000000000000, 3.174999999999999822, -41.27499999999999858 ) ) ;
#13159 = CARTESIAN_POINT ( 'NONE',  ( 135.5667039024470455, -118.2784471599408960, 45.21780685541799727 ) ) ;
#13160 = CARTESIAN_POINT ( 'NONE',  ( 97.78144721833434971, -39.80378292816723018, 237.5813395616249579 ) ) ;
#13161 = DIRECTION ( 'NONE',  ( 0.000000000000000000, 0.000000000000000000, -1.000000000000000000 ) ) ;
#13162 = CARTESIAN_POINT ( 'NONE',  ( 98.84777479348176144, -29.24180311599948467, 76.73848241876795839 ) ) ;
#13163 = CARTESIAN_POINT ( 'NONE',  ( 114.5898276930936532, -43.34969010434090819, 53.25228543077692933 ) ) ;
#13164 = AXIS2_PLACEMENT_3D ( 'NONE', #12501, #46545, #40183 ) ;
#13165 = CARTESIAN_POINT ( 'NONE',  ( 103.3333906439367098, -27.45234650783311636, 21.38091191696080529 ) ) ;
#13166 = VECTOR ( 'NONE', #39942, 1000.000000000000114 ) ;
#13167 = ORIENTED_EDGE ( 'NONE', *, *, #64796, .T. ) ;
#13168 = LINE ( 'NONE', #81292, #69009 ) ;
#13169 = ORIENTED_EDGE ( 'NONE', *, *, #48854, .F. ) ;
#13170 = ORIENTED_EDGE ( 'NONE', *, *, #5285, .T. ) ;
#13171 = ADVANCED_FACE ( 'NONE', ( #72813 ), #24224, .T. ) ;
#13172 = CARTESIAN_POINT ( 'NONE',  ( 97.76609424928555825, -35.39554716186696481, 222.6568214011349767 ) ) ;
#13173 = VECTOR ( 'NONE', #44842, 1000.000000000000114 ) ;
#13174 = PLANE ( 'NONE',  #5265 ) ;
#13175 = CARTESIAN_POINT ( 'NONE',  ( 97.33780952251225926, -34.07119382363175220, 141.1148024095264759 ) ) ;
#13176 = EDGE_CURVE ( 'NONE', #77621, #67060, #22442, .T. ) ;
#13177 = ADVANCED_FACE ( 'NONE', ( #32350 ), #53676, .F. ) ;
#13178 = CARTESIAN_POINT ( 'NONE',  ( 113.1782937241120806, -44.75186862947914079, 154.0939586045162173 ) ) ;
#13179 = AXIS2_PLACEMENT_3D ( 'NONE', #13990, #8075, #7626 ) ;
#13180 = CARTESIAN_POINT ( 'NONE',  ( 81.30995888129169202, -39.18301917769736065, 1.868341932361629265 ) ) ;
#13181 = ORIENTED_EDGE ( 'NONE', *, *, #19258, .T. ) ;
#13182 = FACE_OUTER_BOUND ( 'NONE', #45910, .T. ) ;
#13183 = ADVANCED_FACE ( 'NONE', ( #88695, #46863, #31461, #74155 ), #26007, .T. ) ;
#13184 = CARTESIAN_POINT ( 'NONE',  ( 99.04388270494561652, -42.84098838056963388, 182.8444536297417073 ) ) ;
#13185 = ORIENTED_EDGE ( 'NONE', *, *, #10117, .T. ) ;
#13186 = CARTESIAN_POINT ( 'NONE',  ( 103.9573432206533283, -47.33663036165624050, 62.33753003781600199 ) ) ;
#13187 = ORIENTED_EDGE ( 'NONE', *, *, #30943, .T. ) ;
#13188 = CARTESIAN_POINT ( 'NONE',  ( 110.0029149558365305, -28.58829895313488834, 247.6071379886389821 ) ) ;
#13189 = EDGE_CURVE ( 'NONE', #20374, #15487, #55808, .T. ) ;
#13190 = LINE ( 'NONE', #5934, #43055 ) ;
#13191 = CARTESIAN_POINT ( 'NONE',  ( 116.6093774848466325, -38.87601340171674025, 148.6499109901969859 ) ) ;
#13192 = CARTESIAN_POINT ( 'NONE',  ( 23.71365514520064011, 81.30718046324925297, 307.5032745394355516 ) ) ;
#13193 = PLANE ( 'NONE',  #24441 ) ;
#13194 = CARTESIAN_POINT ( 'NONE',  ( 122.2221484686747459, -107.5284471599419192, -21.78219314458190681 ) ) ;
#13195 = CARTESIAN_POINT ( 'NONE',  ( 5.011961811782480680, 70.88063028345509053, 130.4597710397083858 ) ) ;
#13196 = CARTESIAN_POINT ( 'NONE',  ( 115.8919449742516861, -44.71207447090664999, 229.2413395616249545 ) ) ;
#13197 = DIRECTION ( 'NONE',  ( 0.7071067811865671127, 0.7071067811865279218, 7.071067811865664660E-16 ) ) ;
#13198 = EDGE_CURVE ( 'NONE', #31817, #394, #16687, .T. ) ;
#13199 = ORIENTED_EDGE ( 'NONE', *, *, #37585, .T. ) ;
#13200 = CARTESIAN_POINT ( 'NONE',  ( 103.1584010082818850, -27.01760528431355368, 126.3813395616259783 ) ) ;
#13201 = CARTESIAN_POINT ( 'NONE',  ( 121.2668985255015031, 45.81534544650252627, -48.36754857886660375 ) ) ;
#13202 = ORIENTED_EDGE ( 'NONE', *, *, #7479, .T. ) ;
#13203 = ORIENTED_EDGE ( 'NONE', *, *, #22035, .F. ) ;
#13204 = VERTEX_POINT ( 'NONE', #25545 ) ;
#13205 = EDGE_CURVE ( 'NONE', #26848, #23939, #18283, .T. ) ;
#13206 = DIRECTION ( 'NONE',  ( 0.000000000000000000, 1.000000000000000000, 0.000000000000000000 ) ) ;
#13207 = LINE ( 'NONE', #40891, #35614 ) ;
#13208 = DIRECTION ( 'NONE',  ( 1.000000000000000000, 4.299999999999999979E-14, 1.000000000000000078E-15 ) ) ;
#13209 = CARTESIAN_POINT ( 'NONE',  ( 242.3160000000000025, 65.43750000000000000, -63.94449999999999790 ) ) ;
#13210 = VECTOR ( 'NONE', #62515, 1000.000000000000000 ) ;
#13211 = CARTESIAN_POINT ( 'NONE',  ( 107.8028422452843387, -28.59910946728008341, 152.8223760838769749 ) ) ;
#13212 = CARTESIAN_POINT ( 'NONE',  ( 108.0160737019250377, -24.89219542061752577, 261.0127681330534415 ) ) ;
#13213 = EDGE_CURVE ( 'NONE', #84792, #28839, #11483, .T. ) ;
#13214 = FACE_OUTER_BOUND ( 'NONE', #45863, .T. ) ;
#13215 = VERTEX_POINT ( 'NONE', #80992 ) ;
#13216 = FACE_OUTER_BOUND ( 'NONE', #32481, .T. ) ;
#13217 = AXIS2_PLACEMENT_3D ( 'NONE', #45484, #18251, #11445 ) ;
#13218 = ORIENTED_EDGE ( 'NONE', *, *, #8596, .F. ) ;
#13219 = EDGE_LOOP ( 'NONE', ( #68624, #25882, #64166, #1591 ) ) ;
#13220 = CIRCLE ( 'NONE', #49639, 4.762500000000000178 ) ;
#13221 = CARTESIAN_POINT ( 'NONE',  ( 91.91125933621934507, -111.8737466215625744, -11.78219314458178779 ) ) ;
#13222 = ORIENTED_EDGE ( 'NONE', *, *, #32541, .T. ) ;
#13223 = VERTEX_POINT ( 'NONE', #11931 ) ;
#13224 = CARTESIAN_POINT ( 'NONE',  ( 182.2420472961719895, -31.76306994223730840, -5.074374724088000832 ) ) ;
#13225 = CARTESIAN_POINT ( 'NONE',  ( 97.75831510205337338, -40.38470820808293382, 16.62424145675636922 ) ) ;
#13226 = FACE_BOUND ( 'NONE', #87368, .T. ) ;
#13227 = DIRECTION ( 'NONE',  ( 1.000000000000000078E-15, 1.000000000000000083E-30, -1.000000000000000000 ) ) ;
#13228 = CARTESIAN_POINT ( 'NONE',  ( 114.6950545185401609, -40.57145610743049247, 202.8781341137909635 ) ) ;
#13229 = CARTESIAN_POINT ( 'NONE',  ( 96.67089207319645539, -38.24056507437282448, 66.44133956162495735 ) ) ;
#13230 = CARTESIAN_POINT ( 'NONE',  ( 1.523316295016020135E-15, 71.21114727940270939, 265.5569999999999595 ) ) ;
#13231 = ORIENTED_EDGE ( 'NONE', *, *, #24360, .T. ) ;
#13232 = CARTESIAN_POINT ( 'NONE',  ( -74.43211355457115985, 80.89685143461889538, -92.27899210470897629 ) ) ;
#13233 = ORIENTED_EDGE ( 'NONE', *, *, #32084, .F. ) ;
#13234 = CIRCLE ( 'NONE', #194, 3.814291549405317117 ) ;
#13235 = CARTESIAN_POINT ( 'NONE',  ( 87.06648329127402519, -54.72944906728955061, 14.67562527591094934 ) ) ;
#13236 = ORIENTED_EDGE ( 'NONE', *, *, #6085, .F. ) ;
#13237 = LINE ( 'NONE', #54085, #37812 ) ;
#13238 = CARTESIAN_POINT ( 'NONE',  ( 121.3693057586265809, -136.8327113968526305, 248.4142799812389910 ) ) ;
#13239 = EDGE_CURVE ( 'NONE', #49274, #27685, #12375, .T. ) ;
#13240 = CARTESIAN_POINT ( 'NONE',  ( 110.8543353071601558, -45.98429331485927918, 132.8856134878540729 ) ) ;
#13241 = AXIS2_PLACEMENT_3D ( 'NONE', #69328, #25744, #54315 ) ;
#13242 = DIRECTION ( 'NONE',  ( -0.9659258262890683122, 0.000000000000000000, -0.2588190451025206285 ) ) ;
#13243 = ORIENTED_EDGE ( 'NONE', *, *, #20579, .F. ) ;
#13244 = CARTESIAN_POINT ( 'NONE',  ( 115.7470646134707266, -43.61006842878475709, 48.30514908543492680 ) ) ;
#13246 = CARTESIAN_POINT ( 'NONE',  ( 110.7536356736639078, -102.7271463785358492, -19.78219314458207378 ) ) ;
#13245 = DIRECTION ( 'NONE',  ( 0.000000000000000000, 0.000000000000000000, 1.000000000000000000 ) ) ;
#13247 = DIRECTION ( 'NONE',  ( 0.7071067811865597852, -0.7071067811865354713, 0.000000000000000000 ) ) ;
#13248 = CARTESIAN_POINT ( 'NONE',  ( 131.4836309258849667, -17.78502016655529161, 2.871594975603859456 ) ) ;
#13249 = ORIENTED_EDGE ( 'NONE', *, *, #19436, .F. ) ;
#13250 = AXIS2_PLACEMENT_3D ( 'NONE', #20705, #56088, #22502 ) ;
#13251 = CARTESIAN_POINT ( 'NONE',  ( 179.7974245136200295, -36.32844715994041707, 342.9256252759109884 ) ) ;
#13252 = CIRCLE ( 'NONE', #43646, 2.749999999999974687 ) ;
#13253 = DIRECTION ( 'NONE',  ( 0.9329458799396118662, 0.000000000000000000, -0.3600166455925385423 ) ) ;
#13254 = CARTESIAN_POINT ( 'NONE',  ( 52.99265158129170317, 95.25000000000000000, 358.0130000000000337 ) ) ;
#13255 = ORIENTED_EDGE ( 'NONE', *, *, #51396, .F. ) ;
#13256 = EDGE_CURVE ( 'NONE', #5960, #51180, #24661, .T. ) ;
#13257 = CARTESIAN_POINT ( 'NONE',  ( 102.9625221110550513, -46.33646342331733337, 88.25562527591095829 ) ) ;
#13259 = DIRECTION ( 'NONE',  ( 0.000000000000000000, 0.000000000000000000, -1.000000000000000000 ) ) ;
#13258 = DIRECTION ( 'NONE',  ( 0.08544974978095688789, 0.9963424814100680926, 0.000000000000000000 ) ) ;
#13260 = DIRECTION ( 'NONE',  ( -4.649954031768924432E-17, -0.8660254037844390407, -0.4999999999999995004 ) ) ;
#13261 = EDGE_CURVE ( 'NONE', #50282, #59961, #67782, .T. ) ;
#13262 = CARTESIAN_POINT ( 'NONE',  ( 145.3578527675120142, -69.40277113351952210, 247.4783998280190076 ) ) ;
#13263 = EDGE_LOOP ( 'NONE', ( #48150, #2153 ) ) ;
#13264 = CARTESIAN_POINT ( 'NONE',  ( 102.6819511611811180, -27.33185899950651887, 131.4118157521009778 ) ) ;
#13266 = EDGE_LOOP ( 'NONE', ( #57137, #5513, #77517, #65801 ) ) ;
#13265 = CARTESIAN_POINT ( 'NONE',  ( 1.154229608196380665E-15, 12.27000000000000313, 9.425000000000000711 ) ) ;
#13267 = VECTOR ( 'NONE', #83638, 1000.000000000000114 ) ;
#13268 = CARTESIAN_POINT ( 'NONE',  ( 111.4711666614668673, -26.61707918639095993, 280.7375300378156453 ) ) ;
#13269 = DIRECTION ( 'NONE',  ( 0.000000000000000000, 0.000000000000000000, -1.000000000000000000 ) ) ;
#13270 = FACE_OUTER_BOUND ( 'NONE', #11963, .T. ) ;
#13271 = DIRECTION ( 'NONE',  ( 0.9242245927363033076, 0.3818493186865917766, 0.000000000000000000 ) ) ;
#13272 = CARTESIAN_POINT ( 'NONE',  ( 107.0664832912739968, -36.72944715994100306, 293.2242906452868851 ) ) ;
#13273 = FACE_OUTER_BOUND ( 'NONE', #43905, .T. ) ;
#13274 = CARTESIAN_POINT ( 'NONE',  ( 75.31670390244798341, -67.87844715994100397, 35.51780685541480409 ) ) ;
#13275 = CARTESIAN_POINT ( 'NONE',  ( 106.5196382177906855, -25.62481104856546565, 195.1156252759109861 ) ) ;
#13276 = EDGE_LOOP ( 'NONE', ( #40660, #668, #69729, #15122 ) ) ;
#13277 = VECTOR ( 'NONE', #20055, 1000.000000000000000 ) ;
#13278 = ORIENTED_EDGE ( 'NONE', *, *, #83229, .T. ) ;
#13279 = CARTESIAN_POINT ( 'NONE',  ( 100.0737993132363783, -29.47871783549896918, 112.1187261630399661 ) ) ;
#13280 = CIRCLE ( 'NONE', #48078, 2.500000000000002220 ) ;
#13281 = DIRECTION ( 'NONE',  ( 1.000000000000000000, 0.000000000000000000, 0.000000000000000000 ) ) ;
#13283 = CARTESIAN_POINT ( 'NONE',  ( 172.5664832912740110, -9.303447159940999356, 141.0426252759120018 ) ) ;
#13282 = CARTESIAN_POINT ( 'NONE',  ( 109.2301907924558009, -26.89130329018268739, 26.33586902018297948 ) ) ;
#13284 = CARTESIAN_POINT ( 'NONE',  ( 141.8664832912740223, -71.52944715994085811, 394.9756252759100903 ) ) ;
#13285 = ADVANCED_FACE ( 'NONE', ( #80530 ), #45521, .F. ) ;
#13286 = EDGE_CURVE ( 'NONE', #89067, #69114, #54123, .T. ) ;
#13287 = DIRECTION ( 'NONE',  ( 0.4999999926578935772, 8.568612280667725471E-05, -0.8660254037844357100 ) ) ;
#13288 = DIRECTION ( 'NONE',  ( 1.000000000000000000, 4.163336342344333240E-14, 0.000000000000000000 ) ) ;
#13289 = DIRECTION ( 'NONE',  ( 0.000000000000000000, 0.000000000000000000, -1.000000000000000000 ) ) ;
#13290 = EDGE_CURVE ( 'NONE', #6003, #28799, #71869, .T. ) ;
#13291 = DIRECTION ( 'NONE',  ( -2.900000000000000265E-14, 2.000000000000000155E-15, -1.000000000000000000 ) ) ;
#13292 = CARTESIAN_POINT ( 'NONE',  ( 113.7851844261090264, -26.99768152489561501, 239.5956252759109759 ) ) ;
#13293 = DIRECTION ( 'NONE',  ( 1.000000000000000000, 0.000000000000000000, 3.386875084296745512E-15 ) ) ;
#13294 = ORIENTED_EDGE ( 'NONE', *, *, #64465, .T. ) ;
#13295 = ORIENTED_EDGE ( 'NONE', *, *, #64773, .T. ) ;
#13296 = AXIS2_PLACEMENT_3D ( 'NONE', #13611, #68584, #66894 ) ;
#13297 = EDGE_CURVE ( 'NONE', #38056, #18286, #41263, .T. ) ;
#13298 = CARTESIAN_POINT ( 'NONE',  ( -89.95878776288222411, 70.27756284692561906, -94.61736061587636470 ) ) ;
#13299 = DIRECTION ( 'NONE',  ( -1.000000000000000000, -3.999999999999999995E-14, -1.000000000000000078E-15 ) ) ;
#13300 = CARTESIAN_POINT ( 'NONE',  ( 113.2462366615943381, -28.75923750785663557, 184.5526495355683494 ) ) ;
#13301 = CARTESIAN_POINT ( 'NONE',  ( -179.6544565346565037, 20.32000000000000028, -9.200237383489920262 ) ) ;
#13302 = VECTOR ( 'NONE', #41048, 1000.000000000000114 ) ;
#13303 = CARTESIAN_POINT ( 'NONE',  ( 31.85959712127300847, -23.19206098994090581, -5.074374724088000832 ) ) ;
#13304 = ORIENTED_EDGE ( 'NONE', *, *, #83230, .F. ) ;
#13305 = DIRECTION ( 'NONE',  ( 0.000000000000000000, 0.000000000000000000, -1.000000000000000000 ) ) ;
#13306 = CARTESIAN_POINT ( 'NONE',  ( 117.1924066864372520, -41.16168844948898453, 208.4861014663869696 ) ) ;
#13307 = VERTEX_POINT ( 'NONE', #89583 ) ;
#13308 = EDGE_CURVE ( 'NONE', #22291, #15780, #83665, .T. ) ;
#13309 = VECTOR ( 'NONE', #56674, 1000.000000000000000 ) ;
#13310 = LINE ( 'NONE', #46457, #62190 ) ;
#13311 = CARTESIAN_POINT ( 'NONE',  ( 51.24204729617191845, -31.76306994223782709, 117.4678068554150485 ) ) ;
#13312 = CARTESIAN_POINT ( 'NONE',  ( 117.0903339436451347, -37.63109343375219140, 168.7546943088809996 ) ) ;
#13313 = CIRCLE ( 'NONE', #30693, 0.1500000000000008271 ) ;
#13314 = CARTESIAN_POINT ( 'NONE',  ( 112.0375358597863027, -29.64498801284190321, 82.39570941720997155 ) ) ;
#13315 = CARTESIAN_POINT ( 'NONE',  ( 103.8005819418147411, -26.80618422321597194, 161.3299109901969643 ) ) ;
#13316 = CARTESIAN_POINT ( 'NONE',  ( -479.3614999999999782, 86.51875000000001137, 94.61194598552339130 ) ) ;
#13317 = ORIENTED_EDGE ( 'NONE', *, *, #23098, .F. ) ;
#13318 = DIRECTION ( 'NONE',  ( -1.000000000000000000, -1.181088324069315053E-15, 0.000000000000000000 ) ) ;
#13319 = CARTESIAN_POINT ( 'NONE',  ( 97.84153879744087590, -40.58974903926429789, 66.64233031300194909 ) ) ;
#13320 = EDGE_LOOP ( 'NONE', ( #89844, #38638, #7047, #74510 ) ) ;
#13321 = ORIENTED_EDGE ( 'NONE', *, *, #49065, .F. ) ;
#13322 = LINE ( 'NONE', #62353, #32835 ) ;
#13323 = ORIENTED_EDGE ( 'NONE', *, *, #26929, .T. ) ;
#13324 = ORIENTED_EDGE ( 'NONE', *, *, #54781, .T. ) ;
#13325 = CARTESIAN_POINT ( 'NONE',  ( 172.5664832912740110, -36.32844715994070839, 78.92562527591199739 ) ) ;
#13326 = CARTESIAN_POINT ( 'NONE',  ( 100.1216203692562630, -42.54163687813885275, 71.29146744712500094 ) ) ;
#13327 = CARTESIAN_POINT ( 'NONE',  ( 105.1067973254952790, -26.46757623491196298, 235.2270538473399313 ) ) ;
#13328 = CIRCLE ( 'NONE', #64108, 2.999999999999947153 ) ;
#13329 = CARTESIAN_POINT ( 'NONE',  ( 110.0457755916377778, -26.10929462018208369, 219.8708633711489711 ) ) ;
#13331 = CARTESIAN_POINT ( 'NONE',  ( 102.3792474187797694, -47.61030217832540501, 283.2527681330539053 ) ) ;
#13330 = DIRECTION ( 'NONE',  ( 0.000000000000000000, 0.000000000000000000, -1.000000000000000000 ) ) ;
#13332 = DIRECTION ( 'NONE',  ( -4.237773401492740281E-14, 1.000000000000000000, 0.000000000000000000 ) ) ;
#13333 = FACE_OUTER_BOUND ( 'NONE', #49159, .T. ) ;
#13334 = CARTESIAN_POINT ( 'NONE',  ( 125.0664832912740110, -14.47844715994100007, 284.9256252759119548 ) ) ;
#13335 = ORIENTED_EDGE ( 'NONE', *, *, #31363, .T. ) ;
#13336 = ORIENTED_EDGE ( 'NONE', *, *, #384, .F. ) ;
#13337 = CIRCLE ( 'NONE', #42354, 2.116999999999993776 ) ;
#13338 = ADVANCED_FACE ( 'NONE', ( #20984 ), #35489, .F. ) ;
#13339 = CIRCLE ( 'NONE', #85857, 2.500000000000002220 ) ;
#13340 = CARTESIAN_POINT ( 'NONE',  ( 117.3261810260836597, -38.23854875528750341, 73.72229194257801055 ) ) ;
#13341 = CARTESIAN_POINT ( 'NONE',  ( 98.82309110046458045, -43.24084327085208912, 91.85848241876892928 ) ) ;
#13342 = CARTESIAN_POINT ( 'NONE',  ( 110.9088526855213388, -26.95253601363527807, 269.7784824187680783 ) ) ;
#13343 = ORIENTED_EDGE ( 'NONE', *, *, #80925, .F. ) ;
#13344 = CARTESIAN_POINT ( 'NONE',  ( 118.0409265538620787, -35.41009787725452185, 238.9337205140059552 ) ) ;
#13345 = DIRECTION ( 'NONE',  ( -0.000000000000000000, -0.000000000000000000, 1.000000000000000000 ) ) ;
#13346 = CARTESIAN_POINT ( 'NONE',  ( 107.0667039024470313, -104.2784471599409528, 45.21780685541799727 ) ) ;
#13347 = EDGE_CURVE ( 'NONE', #1145, #7741, #34109, .T. ) ;
#13348 = CARTESIAN_POINT ( 'NONE',  ( 1.475953350320055108E-14, 239.0000000000000000, 104.4754207677255806 ) ) ;
#13349 = DIRECTION ( 'NONE',  ( 1.000000000000000000, 4.299999999999999979E-14, 1.000000000000000078E-15 ) ) ;
#13351 = FACE_BOUND ( 'NONE', #43356, .T. ) ;
#13350 = CARTESIAN_POINT ( 'NONE',  ( 115.2577283620428545, -37.00732651667798478, 277.6356252759109680 ) ) ;
#13352 = DIRECTION ( 'NONE',  ( 0.000000000000000000, -1.000000000000000000, 4.100000000000000342E-29 ) ) ;
#13353 = DIRECTION ( 'NONE',  ( 0.4999999999999998890, -0.8660254037844387076, 0.000000000000000000 ) ) ;
#13354 = LINE ( 'NONE', #7874, #89095 ) ;
#13355 = LINE ( 'NONE', #6533, #87857 ) ;
#13356 = DIRECTION ( 'NONE',  ( 0.000000000000000000, 0.000000000000000000, -1.000000000000000000 ) ) ;
#13357 = CARTESIAN_POINT ( 'NONE',  ( 98.34985891999399144, -31.65658479692842064, 76.90645860808798773 ) ) ;
#13358 = AXIS2_PLACEMENT_3D ( 'NONE', #36651, #64352, #57523 ) ;
#13360 = ORIENTED_EDGE ( 'NONE', *, *, #73947, .F. ) ;
#13359 = CARTESIAN_POINT ( 'NONE',  ( 97.33784130179184046, -34.07106456304081377, 261.1147919453016470 ) ) ;
#13361 = CARTESIAN_POINT ( 'NONE',  ( -74.15067561874160162, 120.6499999999999915, -68.53801554307528932 ) ) ;
#13362 = CARTESIAN_POINT ( 'NONE',  ( 102.2269548454591046, -45.98824451103227062, 212.1927681330539599 ) ) ;
#13363 = CARTESIAN_POINT ( 'NONE',  ( 98.28086921530724851, -31.05189054518432101, 141.8699109901969564 ) ) ;
#13364 = CARTESIAN_POINT ( 'NONE',  ( 112.5120184049100089, -46.40124356417671692, 253.9965776568635647 ) ) ;
#13365 = DIRECTION ( 'NONE',  ( 0.7071067811862239427, 0.7071067811868709807, 0.000000000000000000 ) ) ;
#13367 = CARTESIAN_POINT ( 'NONE',  ( 134.0664832912740110, -46.72944715994100306, 10.42562527591099553 ) ) ;
#13366 = CARTESIAN_POINT ( 'NONE',  ( 192.5667039024474434, -23.42844715993413374, 180.4678068554150343 ) ) ;
#13368 = DIRECTION ( 'NONE',  ( 1.000000000000000078E-15, -1.000000000000000000, 0.000000000000000000 ) ) ;
#13369 = VECTOR ( 'NONE', #68773, 1000.000000000000000 ) ;
#13370 = CARTESIAN_POINT ( 'NONE',  ( 147.4575741623270062, 0.000000000000000000, -135.2444258376734183 ) ) ;
#13372 = ADVANCED_FACE ( 'NONE', ( #76839 ), #7797, .T. ) ;
#13371 = VECTOR ( 'NONE', #75329, 1000.000000000000000 ) ;
#13373 = VERTEX_POINT ( 'NONE', #55017 ) ;
#13374 = EDGE_LOOP ( 'NONE', ( #79789, #46053, #73118, #6610 ) ) ;
#13375 = AXIS2_PLACEMENT_3D ( 'NONE', #36601, #35230, #83399 ) ;
#13376 = CARTESIAN_POINT ( 'NONE',  ( 115.7815527111783069, -39.19119195442627301, 143.0419436376009799 ) ) ;
#13378 = ORIENTED_EDGE ( 'NONE', *, *, #18812, .F. ) ;
#13377 = CARTESIAN_POINT ( 'NONE',  ( 19.89663890320305839, 44.45000000000000284, 32.49205688096009936 ) ) ;
#13379 = CARTESIAN_POINT ( 'NONE',  ( 107.2792697713003776, -24.20934055526686279, 321.5865679059475610 ) ) ;
#13380 = CARTESIAN_POINT ( 'NONE',  ( 108.9412587213990804, -26.46057952311826611, 160.9327681330539690 ) ) ;
#13381 = LINE ( 'NONE', #61958, #80195 ) ;
#13382 = CIRCLE ( 'NONE', #77187, 17.00000000000000000 ) ;
#13383 = CARTESIAN_POINT ( 'NONE',  ( -47.04228170325576031, 92.15829462204605704, 74.35109477667292310 ) ) ;
#13384 = CARTESIAN_POINT ( 'NONE',  ( -91.90683392111071726, 78.46407912418315789, 74.89107914305792235 ) ) ;
#13385 = DIRECTION ( 'NONE',  ( 0.000000000000000000, 1.000000000000000000, 1.541976423090495239E-15 ) ) ;
#13386 = CARTESIAN_POINT ( 'NONE',  ( 116.3126599349421895, -33.43976754494798342, 114.0984824187689668 ) ) ;
#13387 = ORIENTED_EDGE ( 'NONE', *, *, #44959, .T. ) ;
#13388 = ORIENTED_EDGE ( 'NONE', *, *, #88668, .F. ) ;
#13389 = ORIENTED_EDGE ( 'NONE', *, *, #2224, .T. ) ;
#13390 = CARTESIAN_POINT ( 'NONE',  ( 181.9790560690451855, -31.62489322948519543, 342.9256252759109884 ) ) ;
#13392 = CARTESIAN_POINT ( 'NONE',  ( 70.06796229133446730, -140.6784471599409869, 245.5026818104030042 ) ) ;
#13391 = CARTESIAN_POINT ( 'NONE',  ( 118.1851208724671238, -36.91582462397654751, 149.8127681330539644 ) ) ;
#13393 = CARTESIAN_POINT ( 'NONE',  ( 115.0894923806533967, -30.61840087513353836, 54.34358037573613842 ) ) ;
#13394 = LINE ( 'NONE', #21561, #85805 ) ;
#13395 = EDGE_CURVE ( 'NONE', #19112, #29616, #14169, .T. ) ;
#13396 = LINE ( 'NONE', #82901, #85196 ) ;
#13397 = VECTOR ( 'NONE', #69455, 1000.000000000000000 ) ;
#13398 = CARTESIAN_POINT ( 'NONE',  ( 61.56670390244727287, -23.42844715994043980, 300.4678068554150627 ) ) ;
#13399 = EDGE_CURVE ( 'NONE', #72149, #24293, #735, .T. ) ;
#13400 = FACE_OUTER_BOUND ( 'NONE', #64661, .T. ) ;
#13401 = CARTESIAN_POINT ( 'NONE',  ( 115.2499566122393588, -44.12502604085376134, 83.25372051400698581 ) ) ;
#13402 = ORIENTED_EDGE ( 'NONE', *, *, #6584, .F. ) ;
#13403 = EDGE_CURVE ( 'NONE', #23728, #39686, #40965, .T. ) ;
#13404 = VERTEX_POINT ( 'NONE', #21889 ) ;
#13405 = ORIENTED_EDGE ( 'NONE', *, *, #72997, .T. ) ;
#13406 = EDGE_CURVE ( 'NONE', #89397, #54515, #73269, .T. ) ;
#13407 = CARTESIAN_POINT ( 'NONE',  ( 46.83715912545343940, -47.82818131006086304, 129.9678068554150911 ) ) ;
#13408 = CARTESIAN_POINT ( 'NONE',  ( 62.03715912545748523, -47.82818131006020934, 193.9678068554150911 ) ) ;
#13409 = AXIS2_PLACEMENT_3D ( 'NONE', #85776, #23985, #40721 ) ;
#13410 = DIRECTION ( 'NONE',  ( 0.000000000000000000, 0.000000000000000000, 1.000000000000000000 ) ) ;
#13411 = CARTESIAN_POINT ( 'NONE',  ( 114.6839398542181101, -39.73893943580953447, 191.3452332267339671 ) ) ;
#13412 = CIRCLE ( 'NONE', #59811, 9.525000000000000355 ) ;
#13413 = CARTESIAN_POINT ( 'NONE',  ( 62.03715912545744260, -47.82818131006020934, 129.9678068554150911 ) ) ;
#13414 = ORIENTED_EDGE ( 'NONE', *, *, #76159, .T. ) ;
#13416 = EDGE_LOOP ( 'NONE', ( #1671, #34448, #3937, #43491 ) ) ;
#13415 = ORIENTED_EDGE ( 'NONE', *, *, #34709, .F. ) ;
#13417 = ADVANCED_FACE ( 'NONE', ( #36846 ), #65001, .T. ) ;
#13418 = LINE ( 'NONE', #27042, #4718 ) ;
#13419 = CARTESIAN_POINT ( 'NONE',  ( 107.0667039024479834, -48.82844715994099971, 160.9178068554150229 ) ) ;
#13420 = ORIENTED_EDGE ( 'NONE', *, *, #74747, .F. ) ;
#13421 = VERTEX_POINT ( 'NONE', #51346 ) ;
#13422 = FACE_OUTER_BOUND ( 'NONE', #84147, .T. ) ;
#13423 = CARTESIAN_POINT ( 'NONE',  ( 103.6867908865108916, -46.21882986916993730, 248.7358690201829745 ) ) ;
#13424 = EDGE_LOOP ( 'NONE', ( #3513, #52034, #18567, #39323 ) ) ;
#13425 = FACE_OUTER_BOUND ( 'NONE', #10685, .T. ) ;
#13426 = CARTESIAN_POINT ( 'NONE',  ( -114.2735689154193750, 70.52307754910606263, 63.13935773474766222 ) ) ;
#13427 = VERTEX_POINT ( 'NONE', #37748 ) ;
#13428 = ORIENTED_EDGE ( 'NONE', *, *, #65899, .F. ) ;
#13429 = AXIS2_PLACEMENT_3D ( 'NONE', #40689, #69305, #21613 ) ;
#13430 = DIRECTION ( 'NONE',  ( 1.000000000000000000, 0.000000000000000000, 0.000000000000000000 ) ) ;
#13431 = VERTEX_POINT ( 'NONE', #24120 ) ;
#13432 = ORIENTED_EDGE ( 'NONE', *, *, #87176, .F. ) ;
#13433 = VECTOR ( 'NONE', #12909, 1000.000000000000000 ) ;
#13434 = CARTESIAN_POINT ( 'NONE',  ( 100.6713832604498577, -30.89818480590637861, 228.5442808457819979 ) ) ;
#13435 = CARTESIAN_POINT ( 'NONE',  ( 108.9889396673064397, -47.63814106062356757, 122.7032443235299723 ) ) ;
#13436 = CARTESIAN_POINT ( 'NONE',  ( 98.16825066461156268, -43.24752039522714142, 106.8175300378159704 ) ) ;
#13437 = CARTESIAN_POINT ( 'NONE',  ( 104.1307268678290683, -28.83426272247936240, 249.5838068554171798 ) ) ;
#13438 = CARTESIAN_POINT ( 'NONE',  ( 133.0522658619983360, -16.17316201338587689, 8.065992442478552960 ) ) ;
#13439 = CARTESIAN_POINT ( 'NONE',  ( 98.55127668717894096, -44.97116251829300637, 187.9384824187679612 ) ) ;
#13440 = CARTESIAN_POINT ( 'NONE',  ( 183.5150000000000148, 37.33800000000000097, 32.46912895322940074 ) ) ;
#13441 = VERTEX_POINT ( 'NONE', #9149 ) ;
#13442 = CARTESIAN_POINT ( 'NONE',  ( 130.4667014434020587, 70.80031561532533146, -4.873084245995139341 ) ) ;
#13443 = EDGE_LOOP ( 'NONE', ( #17025, #32213, #86020, #87037, #31067 ) ) ;
#13444 = VERTEX_POINT ( 'NONE', #16853 ) ;
#13445 = DIRECTION ( 'NONE',  ( 0.000000000000000000, 1.000000000000000000, 0.000000000000000000 ) ) ;
#13446 = ORIENTED_EDGE ( 'NONE', *, *, #73220, .F. ) ;
#13447 = EDGE_CURVE ( 'NONE', #2655, #82610, #6567, .T. ) ;
#13448 = LINE ( 'NONE', #61577, #9900 ) ;
#13449 = CARTESIAN_POINT ( 'NONE',  ( 117.3714642245996629, -32.73114059124436892, 94.10895860924395606 ) ) ;
#13450 = CARTESIAN_POINT ( 'NONE',  ( -10.45593524471656721, 75.34132956249517576, 130.1366506729525554 ) ) ;
#13451 = EDGE_CURVE ( 'NONE', #59655, #72639, #78658, .T. ) ;
#13452 = LINE ( 'NONE', #89318, #66679 ) ;
#13453 = FACE_OUTER_BOUND ( 'NONE', #60971, .T. ) ;
#13456 = CARTESIAN_POINT ( 'NONE',  ( 106.8520627977276973, -47.75749532952657006, 223.5489586092439538 ) ) ;
#13455 = CARTESIAN_POINT ( 'NONE',  ( 1.387778780781445676E-14, 239.0000000000000000, 97.27542076772557778 ) ) ;
#13454 = CARTESIAN_POINT ( 'NONE',  ( -465.6921742093550165, 47.62500000000000000, 3.174999999999999822 ) ) ;
#13457 = CARTESIAN_POINT ( 'NONE',  ( 107.0664832912739399, -36.72944715994095333, 302.7856252759109452 ) ) ;
#13458 = CARTESIAN_POINT ( 'NONE',  ( 48.16670390244701139, -26.71338133339251542, 237.4678068554150059 ) ) ;
#13459 = VERTEX_POINT ( 'NONE', #29583 ) ;
#13460 = DIRECTION ( 'NONE',  ( -2.900000000000000265E-14, 2.000000000000000155E-15, -1.000000000000000000 ) ) ;
#13461 = AXIS2_PLACEMENT_3D ( 'NONE', #23891, #31127, #58826 ) ;
#13462 = CARTESIAN_POINT ( 'NONE',  ( -3.174999999999664979, 8.255000000000000782, 31.75000000000000000 ) ) ;
#13463 = DIRECTION ( 'NONE',  ( 1.748382715945130353E-14, 0.000000000000000000, -1.000000000000000000 ) ) ;
#13464 = DIRECTION ( 'NONE',  ( 0.000000000000000000, 1.000000000000000000, 0.000000000000000000 ) ) ;
#13466 = ORIENTED_EDGE ( 'NONE', *, *, #41999, .F. ) ;
#13465 = CARTESIAN_POINT ( 'NONE',  ( 97.12779447186500192, -40.02021159927672755, 241.5813395616249863 ) ) ;
#13467 = CARTESIAN_POINT ( 'NONE',  ( 0.000000000000000000, 127.0000000000000000, -103.1875000000000000 ) ) ;
#13468 = CARTESIAN_POINT ( 'NONE',  ( 108.3221154657901337, -47.10103102204929826, 117.6727681330539639 ) ) ;
#13469 = CARTESIAN_POINT ( 'NONE',  ( 101.1417250294410337, -28.10862513908322313, 46.55562527591094835 ) ) ;
#13470 = CARTESIAN_POINT ( 'NONE',  ( 98.82232569344716921, -30.27743405825323464, 151.7984824187679465 ) ) ;
#13471 = CARTESIAN_POINT ( 'NONE',  ( 3.174999999999879918, 8.255000000000000782, -33.98325472291465132 ) ) ;
#13472 = CARTESIAN_POINT ( 'NONE',  ( 100.9547954897877702, -28.70692885872499289, 101.5939034364447338 ) ) ;
#13474 = DIRECTION ( 'NONE',  ( 1.000000000000000000, 4.299999999999999979E-14, 1.000000000000000078E-15 ) ) ;
#13473 = DIRECTION ( 'NONE',  ( 1.000000000000000000, 0.000000000000000000, 0.000000000000000000 ) ) ;
#13475 = PLANE ( 'NONE',  #20536 ) ;
#13476 = CARTESIAN_POINT ( 'NONE',  ( 192.5667039024473013, -23.42844715993434335, 249.9678068554149775 ) ) ;
#13477 = VERTEX_POINT ( 'NONE', #77745 ) ;
#13478 = VECTOR ( 'NONE', #18663, 1000.000000000000000 ) ;
#13479 = B_SPLINE_CURVE_WITH_KNOTS ( 'NONE', 3,
 ( #59942, #46309, #82224, #11820, #19978, #47659 ),
 .UNSPECIFIED., .F., .F.,
 ( 4, 2, 4 ),
 ( 1.223758863293699992E-06, 0.0009153852925891950649, 0.001829959312313299931 ),
 .UNSPECIFIED. ) ;
#13480 = EDGE_CURVE ( 'NONE', #28839, #2851, #23248, .T. ) ;
#13481 = ORIENTED_EDGE ( 'NONE', *, *, #61280, .F. ) ;
#13482 = ORIENTED_EDGE ( 'NONE', *, *, #61178, .T. ) ;
#13483 = EDGE_LOOP ( 'NONE', ( #10610, #59710, #31499, #63498 ) ) ;
#13484 = CARTESIAN_POINT ( 'NONE',  ( -127.0239848601436563, 53.14309343562469934, 30.16249999999989839 ) ) ;
#13485 = CARTESIAN_POINT ( 'NONE',  ( 116.7068942081671423, -31.36975501082244477, 25.24229194257798881 ) ) ;
#13486 = CARTESIAN_POINT ( 'NONE',  ( 96.41083957889333078, -31.77770432788677013, 4.925625275910959999 ) ) ;
#13487 = CARTESIAN_POINT ( 'NONE',  ( 107.0664832912739968, 12.92155284005902516, 330.1506252759110680 ) ) ;
#13488 = EDGE_CURVE ( 'NONE', #26370, #68689, #56824, .T. ) ;
#13489 = CARTESIAN_POINT ( 'NONE',  ( 102.9499971297430250, -26.42158413985995580, 171.3908633711489813 ) ) ;
#13490 = LINE ( 'NONE', #33922, #6963 ) ;
#13491 = CARTESIAN_POINT ( 'NONE',  ( 101.9513324583280962, -44.20259256747556975, 241.5333722090289825 ) ) ;
#13492 = ORIENTED_EDGE ( 'NONE', *, *, #31313, .F. ) ;
#13493 = ORIENTED_EDGE ( 'NONE', *, *, #19893, .T. ) ;
#13494 = ORIENTED_EDGE ( 'NONE', *, *, #27474, .F. ) ;
#13495 = VECTOR ( 'NONE', #13129, 1000.000000000000000 ) ;
#13496 = DIRECTION ( 'NONE',  ( 0.000000000000000000, 0.000000000000000000, -1.000000000000000000 ) ) ;
#13499 = EDGE_CURVE ( 'NONE', #22883, #76315, #68940, .T. ) ;
#13498 = CIRCLE ( 'NONE', #86065, 7.873999999999991672 ) ;
#13497 = CARTESIAN_POINT ( 'NONE',  ( 115.7832426263078958, -41.80208187097057504, 103.4062359794634176 ) ) ;
#13500 = CARTESIAN_POINT ( 'NONE',  ( -546.0365000000000464, 53.97500000000000142, 12.69999999999999929 ) ) ;
#13501 = CARTESIAN_POINT ( 'NONE',  ( -68.53801554307499089, 127.0000000000000000, 74.15067561874188584 ) ) ;
#13502 = DIRECTION ( 'NONE',  ( -1.000000000000000000, -8.843517682682131024E-16, -1.000000000000000078E-15 ) ) ;
#13503 = CONICAL_SURFACE ( 'NONE', #7729, 1.571100913904388552, 1.047197551196592302 ) ;
#13504 = CARTESIAN_POINT ( 'NONE',  ( 48.45959712127301344, -26.00627455219131789, 237.4678068554150059 ) ) ;
#13505 = DIRECTION ( 'NONE',  ( 5.512527431108029424E-15, -1.000000000000000000, 0.000000000000000000 ) ) ;
#13506 = CARTESIAN_POINT ( 'NONE',  ( 97.54182784580959265, -34.36413255816223966, 276.1327681330543555 ) ) ;
#13507 = EDGE_CURVE ( 'NONE', #7448, #58550, #36772, .T. ) ;
#13508 = LINE ( 'NONE', #27133, #86470 ) ;
#13509 = ORIENTED_EDGE ( 'NONE', *, *, #41356, .F. ) ;
#13510 = FACE_OUTER_BOUND ( 'NONE', #63363, .T. ) ;
#13511 = B_SPLINE_CURVE_WITH_KNOTS ( 'NONE', 3,
 ( #19048, #67645, #5430, #33126, #54429, #60820, #82192, #22200, #7661, #36718, #77157, #78514, #2650, #16274, #48965, #77601, #42600, #63064 ),
 .UNSPECIFIED., .F., .F.,
 ( 4, 2, 2, 2, 2, 2, 2, 2, 4 ),
 ( 0.5000000002356785878, 0.5625000002062188198, 0.6250000001767589408, 0.6875000001472990618, 0.7500000001178392939, 0.8125000000883795259, 0.8750000000589196469, 0.9375000000294597680, 1.000000000000000000 ),
 .UNSPECIFIED. ) ;
#13512 = CARTESIAN_POINT ( 'NONE',  ( 141.8664832912739939, -71.52944715994085811, 361.9756252759100335 ) ) ;
#13513 = CARTESIAN_POINT ( 'NONE',  ( 98.47016933319702048, -37.73160053143655546, 84.24904275054394986 ) ) ;
#13514 = AXIS2_PLACEMENT_3D ( 'NONE', #9132, #36829, #29565 ) ;
#13515 = DIRECTION ( 'NONE',  ( -0.9999999853157766072, -0.0001713722456150811827, 0.000000000000000000 ) ) ;
#13516 = CARTESIAN_POINT ( 'NONE',  ( 168.0371591254545649, -48.62818131005499112, 180.4678068554150059 ) ) ;
#13517 = ORIENTED_EDGE ( 'NONE', *, *, #37307, .T. ) ;
#13518 = ADVANCED_FACE ( 'NONE', ( #37293 ), #63662, .T. ) ;
#13519 = CARTESIAN_POINT ( 'NONE',  ( 79.41328093383648934, -34.05633243510678909, 8.161687850944868927 ) ) ;
#13520 = AXIS2_PLACEMENT_3D ( 'NONE', #69574, #42291, #13269 ) ;
#13521 = ORIENTED_EDGE ( 'NONE', *, *, #35833, .F. ) ;
#13522 = CARTESIAN_POINT ( 'NONE',  ( 97.83587340921722841, -31.88353427759474457, 135.9413395616259947 ) ) ;
#13523 = ORIENTED_EDGE ( 'NONE', *, *, #72969, .F. ) ;
#13524 = EDGE_CURVE ( 'NONE', #78255, #30086, #37055, .T. ) ;
#13525 = CARTESIAN_POINT ( 'NONE',  ( 145.3076464064830873, -69.48838775773263876, 247.4862654744191843 ) ) ;
#13526 = CARTESIAN_POINT ( 'NONE',  ( 105.2783438540041061, -26.81616000048136428, 121.6501547344689698 ) ) ;
#13527 = PLANE ( 'NONE',  #57700 ) ;
#13528 = CARTESIAN_POINT ( 'NONE',  ( 89.89786210216969664, -69.33318169163436551, 247.6453889683499767 ) ) ;
#13529 = CARTESIAN_POINT ( 'NONE',  ( 96.69317630666223806, -38.23732580652426094, 62.44133956162495025 ) ) ;
#13530 = AXIS2_PLACEMENT_3D ( 'NONE', #32167, #59862, #11279 ) ;
#13531 = CARTESIAN_POINT ( 'NONE',  ( 115.7831076651936257, -41.80230951900219338, 84.40645860845914683 ) ) ;
#13532 = VERTEX_POINT ( 'NONE', #70481 ) ;
#13533 = CARTESIAN_POINT ( 'NONE',  ( 188.5667039024480971, -42.82844715993431350, 293.2178068554150059 ) ) ;
#13534 = ORIENTED_EDGE ( 'NONE', *, *, #29495, .F. ) ;
#13535 = ORIENTED_EDGE ( 'NONE', *, *, #42767, .F. ) ;
#13536 = FACE_OUTER_BOUND ( 'NONE', #56481, .T. ) ;
#13537 = ORIENTED_EDGE ( 'NONE', *, *, #73590, .T. ) ;
#13538 = CARTESIAN_POINT ( 'NONE',  ( 100.6687104586878547, -44.89077600197693130, 277.0594347997210889 ) ) ;
#13539 = CARTESIAN_POINT ( 'NONE',  ( 108.9491117623569636, -26.41756539094687639, 160.9327681330539690 ) ) ;
#13540 = DIRECTION ( 'NONE',  ( -0.9254794337955620787, -0.3787978585227822492, 0.000000000000000000 ) ) ;
#13541 = CARTESIAN_POINT ( 'NONE',  ( 99.09570908213733276, -30.55043174551792262, 141.8022919418074821 ) ) ;
#13542 = CARTESIAN_POINT ( 'NONE',  ( 115.2072660578295284, -44.20618685261739245, 74.22324432352993995 ) ) ;
#13543 = CARTESIAN_POINT ( 'NONE',  ( 97.06098806315000616, -37.99597704668403253, 97.42732106492178445 ) ) ;
#13544 = ORIENTED_EDGE ( 'NONE', *, *, #41461, .F. ) ;
#13545 = DIRECTION ( 'NONE',  ( -1.000000000000000078E-15, 1.000000000000000083E-30, 1.000000000000000000 ) ) ;
#13546 = CARTESIAN_POINT ( 'NONE',  ( 100.8875641163020873, -44.70030114050455694, 158.0521118432647825 ) ) ;
#13547 = ORIENTED_EDGE ( 'NONE', *, *, #62194, .T. ) ;
#13548 = AXIS2_PLACEMENT_3D ( 'NONE', #80722, #89326, #60245 ) ;
#13549 = DIRECTION ( 'NONE',  ( 1.000000000000000078E-15, 0.000000000000000000, -1.000000000000000000 ) ) ;
#13550 = DIRECTION ( 'NONE',  ( 1.000000000000000078E-15, -1.000000000000000083E-30, -1.000000000000000000 ) ) ;
#13551 = CARTESIAN_POINT ( 'NONE',  ( 100.2624651760415304, -28.85963121439194623, 260.6441967044822263 ) ) ;
#13552 = CYLINDRICAL_SURFACE ( 'NONE', #60568, 0.2499999999999941991 ) ;
#13553 = AXIS2_PLACEMENT_3D ( 'NONE', #5518, #76336, #81387 ) ;
#13554 = CARTESIAN_POINT ( 'NONE',  ( 69.39078715552076915, 92.39984138453077378, 54.48432155457955162 ) ) ;
#13555 = LINE ( 'NONE', #69868, #39754 ) ;
#13556 = CARTESIAN_POINT ( 'NONE',  ( 116.1300133678986413, -31.69047823903573047, 29.24229194257799236 ) ) ;
#13558 = CARTESIAN_POINT ( 'NONE',  ( 116.8835868046512587, -40.17228670562622739, 129.5584824187679658 ) ) ;
#13557 = CARTESIAN_POINT ( 'NONE',  ( 97.76673074818263842, -40.40594551311712479, 101.6265170135205409 ) ) ;
#13559 = CARTESIAN_POINT ( 'NONE',  ( 168.0371591254546217, -48.62818131005519007, 129.9678068554150059 ) ) ;
#13560 = CARTESIAN_POINT ( 'NONE',  ( 99.38968898744698777, -27.63536841754259044, 150.6356252759109680 ) ) ;
#13561 = FACE_OUTER_BOUND ( 'NONE', #51610, .T. ) ;
#13562 = ORIENTED_EDGE ( 'NONE', *, *, #2308, .T. ) ;
#13563 = DIRECTION ( 'NONE',  ( -0.9254794337955620787, -0.3787978585227822492, 0.000000000000000000 ) ) ;
#13564 = DIRECTION ( 'NONE',  ( 1.000000000000000000, 0.000000000000000000, 0.000000000000000000 ) ) ;
#13565 = CARTESIAN_POINT ( 'NONE',  ( 135.7756147485175688, -34.57277681851078199, 2.101554741580191621 ) ) ;
#13566 = VERTEX_POINT ( 'NONE', #1445 ) ;
#13567 = CARTESIAN_POINT ( 'NONE',  ( 51.23005224011609471, -33.89581943344337134, 193.9678068554150911 ) ) ;
#13569 = ORIENTED_EDGE ( 'NONE', *, *, #51953, .T. ) ;
#13568 = CARTESIAN_POINT ( 'NONE',  ( 98.24359417337518607, -31.02780217081950909, 145.8699109901969848 ) ) ;
#13570 = CYLINDRICAL_SURFACE ( 'NONE', #87157, 4.762500000000001066 ) ;
#13571 = CARTESIAN_POINT ( 'NONE',  ( 95.16685018565972598, 70.52074417248462623, 89.37727808479131397 ) ) ;
#13572 = FACE_OUTER_BOUND ( 'NONE', #398, .T. ) ;
#13573 = DIRECTION ( 'NONE',  ( 0.000000000000000000, 1.000000000000000000, -0.000000000000000000 ) ) ;
#13574 = EDGE_LOOP ( 'NONE', ( #43306, #47920, #79196, #7578 ) ) ;
#13575 = ADVANCED_FACE ( 'NONE', ( #22331, #50011, #15519, #43194, #8712 ), #36414, .F. ) ;
#13576 = AXIS2_PLACEMENT_3D ( 'NONE', #20317, #27116, #47542 ) ;
#13577 = ADVANCED_FACE ( 'NONE', ( #17304 ), #44984, .F. ) ;
#13578 = ORIENTED_EDGE ( 'NONE', *, *, #14395, .T. ) ;
#13579 = EDGE_LOOP ( 'NONE', ( #31062, #17886, #80557, #88713 ) ) ;
#13580 = ADVANCED_FACE ( 'NONE', ( #17743, #10921 ), #73138, .T. ) ;
#13581 = AXIS2_PLACEMENT_3D ( 'NONE', #8028, #55252, #7136 ) ;
#13582 = VERTEX_POINT ( 'NONE', #38624 ) ;
#13583 = DIRECTION ( 'NONE',  ( 1.000000000000000078E-15, 1.000000000000000083E-30, -1.000000000000000000 ) ) ;
#13584 = CARTESIAN_POINT ( 'NONE',  ( 98.43498668633466764, -29.82501040932825020, 191.7775300378159784 ) ) ;
#13585 = CARTESIAN_POINT ( 'NONE',  ( 89.37916159652658621, 94.58014758961626001, -95.16508291382855589 ) ) ;
#13586 = CARTESIAN_POINT ( 'NONE',  ( -47.13180528695278326, 100.9330007194059675, 75.77065372412548072 ) ) ;
#13587 = ADVANCED_FACE ( 'NONE', ( #60399 ), #29853, .T. ) ;
#13588 = EDGE_CURVE ( 'NONE', #15679, #21569, #88136, .T. ) ;
#13590 = CARTESIAN_POINT ( 'NONE',  ( 92.32962665258456525, 82.54999999999999716, 74.36911441044829019 ) ) ;
#13589 = FACE_OUTER_BOUND ( 'NONE', #4339, .T. ) ;
#13591 = DIRECTION ( 'NONE',  ( 0.000000000000000000, 0.000000000000000000, -1.000000000000000000 ) ) ;
#13592 = ORIENTED_EDGE ( 'NONE', *, *, #88566, .T. ) ;
#13593 = EDGE_CURVE ( 'NONE', #50094, #81819, #82060, .T. ) ;
#13594 = VECTOR ( 'NONE', #56979, 1000.000000000000000 ) ;
#13595 = ADVANCED_FACE ( 'NONE', ( #67678 ), #46313, .F. ) ;
#13596 = EDGE_LOOP ( 'NONE', ( #82709, #84404 ) ) ;
#13597 = CARTESIAN_POINT ( 'NONE',  ( 37.56670390244833158, -48.82844715994119866, 249.9678068554150343 ) ) ;
#13599 = EDGE_CURVE ( 'NONE', #24899, #81994, #72714, .T. ) ;
#13598 = DIRECTION ( 'NONE',  ( -1.000000000000000000, 0.000000000000000000, 6.982966722218760189E-15 ) ) ;
#13600 = CARTESIAN_POINT ( 'NONE',  ( 111.3277751695582651, -45.53312973143654574, 243.9356252759109509 ) ) ;
#13601 = LINE ( 'NONE', #76727, #42879 ) ;
#13602 = CARTESIAN_POINT ( 'NONE',  ( 97.42673588038243793, -38.38435052442952866, 87.46133956162493917 ) ) ;
#13603 = EDGE_CURVE ( 'NONE', #89615, #5243, #80878, .T. ) ;
#13604 = CARTESIAN_POINT ( 'NONE',  ( 110.9562181391215745, -45.94203628685212237, 52.89439067654506488 ) ) ;
#13605 = EDGE_CURVE ( 'NONE', #53038, #87166, #31362, .T. ) ;
#13606 = CARTESIAN_POINT ( 'NONE',  ( 103.4003208981030753, -27.42560052542062721, 21.37517646364080903 ) ) ;
#13607 = VERTEX_POINT ( 'NONE', #81338 ) ;
#13608 = DIRECTION ( 'NONE',  ( 0.000000000000000000, -1.000000000000000000, 0.000000000000000000 ) ) ;
#13609 = EDGE_LOOP ( 'NONE', ( #37790, #66839, #87375, #40221, #13870 ) ) ;
#13610 = EDGE_LOOP ( 'NONE', ( #3963, #71787, #56089, #16214 ) ) ;
#13611 = CARTESIAN_POINT ( 'NONE',  ( 180.1667039024475230, -28.27351298636767396, 237.4678068554150059 ) ) ;
#13612 = CARTESIAN_POINT ( 'NONE',  ( 100.6682639674293114, -30.55490919580550013, 247.1472975916109647 ) ) ;
#13613 = CIRCLE ( 'NONE', #51331, 7.143750000000004263 ) ;
#13614 = CARTESIAN_POINT ( 'NONE',  ( 100.8874677989195447, -44.70022130964055407, 192.0522919340818362 ) ) ;
#13615 = DIRECTION ( 'NONE',  ( 0.000000000000000000, 1.000000000000000000, 0.000000000000000000 ) ) ;
#13616 = FACE_BOUND ( 'NONE', #83998, .T. ) ;
#13617 = FACE_OUTER_BOUND ( 'NONE', #16548, .T. ) ;
#13618 = ORIENTED_EDGE ( 'NONE', *, *, #89695, .T. ) ;
#13619 = DIRECTION ( 'NONE',  ( 0.000000000000000000, 0.000000000000000000, -1.000000000000000000 ) ) ;
#13620 = ADVANCED_FACE ( 'NONE', ( #79541 ), #18634, .F. ) ;
#13621 = CARTESIAN_POINT ( 'NONE',  ( 112.0640919193708243, -45.48941087331174771, 183.9901923727738620 ) ) ;
#13622 = ORIENTED_EDGE ( 'NONE', *, *, #75159, .F. ) ;
#13623 = CARTESIAN_POINT ( 'NONE',  ( 96.17734138947662359, -38.62830894954290528, 46.45181575210094138 ) ) ;
#13624 = ORIENTED_EDGE ( 'NONE', *, *, #65176, .T. ) ;
#13625 = EDGE_CURVE ( 'NONE', #40317, #1757, #39068, .T. ) ;
#13626 = CARTESIAN_POINT ( 'NONE',  ( 105.1260075982565212, -28.80065313513137326, 283.0852332267343172 ) ) ;
#13627 = EDGE_CURVE ( 'NONE', #44525, #64446, #65876, .T. ) ;
#13628 = CARTESIAN_POINT ( 'NONE',  ( -117.8738102209307925, 82.54999999999999716, 12.69999999999959073 ) ) ;
#13629 = CARTESIAN_POINT ( 'NONE',  ( 98.32242264099468798, -42.30440888850458947, 141.7661014663879655 ) ) ;
#13630 = CARTESIAN_POINT ( 'NONE',  ( 107.0664832912739968, -8.729447159940999512, 6.425625275911999168 ) ) ;
#13631 = DIRECTION ( 'NONE',  ( -1.175184669632759901E-16, 1.000000000000000000, 2.000000000000003705E-15 ) ) ;
#13633 = EDGE_CURVE ( 'NONE', #84986, #66271, #66077, .T. ) ;
#13632 = CARTESIAN_POINT ( 'NONE',  ( 94.86917197795300183, -31.06128196069623471, 25.56312527591095574 ) ) ;
#13634 = CARTESIAN_POINT ( 'NONE',  ( 7.082822281873440318, 72.00847419435602603, 130.3637323515569904 ) ) ;
#13635 = CARTESIAN_POINT ( 'NONE',  ( 114.6369858128092858, -29.49892357452570124, 230.4327681330539690 ) ) ;
#13636 = LINE ( 'NONE', #20011, #5008 ) ;
#13637 = ORIENTED_EDGE ( 'NONE', *, *, #72460, .F. ) ;
#13638 = CIRCLE ( 'NONE', #31007, 2.030000000000003801 ) ;
#13639 = ORIENTED_EDGE ( 'NONE', *, *, #6931, .T. ) ;
#13640 = CARTESIAN_POINT ( 'NONE',  ( 95.43962894333766656, -34.19422119854147013, 102.1556252759109640 ) ) ;
#13641 = CARTESIAN_POINT ( 'NONE',  ( 121.9957511497836578, 45.05269096688547137, -46.49927299628500776 ) ) ;
#13642 = AXIS2_PLACEMENT_3D ( 'NONE', #68055, #19903, #61228 ) ;
#13643 = VECTOR ( 'NONE', #32988, 1000.000000000000000 ) ;
#13644 = ORIENTED_EDGE ( 'NONE', *, *, #8097, .T. ) ;
#13645 = VERTEX_POINT ( 'NONE', #74493 ) ;
#13646 = ORIENTED_EDGE ( 'NONE', *, *, #50507, .F. ) ;
#13647 = AXIS2_PLACEMENT_3D ( 'NONE', #86574, #43876, #71168 ) ;
#13648 = FACE_OUTER_BOUND ( 'NONE', #9871, .T. ) ;
#13649 = DIRECTION ( 'NONE',  ( 1.000000000000000000, 0.000000000000000000, 0.000000000000000000 ) ) ;
#13650 = LINE ( 'NONE', #7733, #59612 ) ;
#13651 = CYLINDRICAL_SURFACE ( 'NONE', #41727, 8.636000000000004562 ) ;
#13652 = CARTESIAN_POINT ( 'NONE',  ( 103.6346955097220643, -29.32319583828803999, 178.2395189410199805 ) ) ;
#13653 = CARTESIAN_POINT ( 'NONE',  ( 110.7407540106703010, -26.28028736477551419, 250.8194347997206819 ) ) ;
#13654 = DIRECTION ( 'NONE',  ( -1.000000000000000000, -4.163336342344333240E-14, 0.000000000000000000 ) ) ;
#13655 = ORIENTED_EDGE ( 'NONE', *, *, #63390, .T. ) ;
#13656 = CARTESIAN_POINT ( 'NONE',  ( 106.0988357118831118, -121.2196481995798507, -19.23816774841949240 ) ) ;
#13657 = DIRECTION ( 'NONE',  ( -0.000000000000000000, 0.000000000000000000, -1.000000000000000000 ) ) ;
#13658 = ORIENTED_EDGE ( 'NONE', *, *, #66431, .F. ) ;
#13659 = ORIENTED_EDGE ( 'NONE', *, *, #32760, .F. ) ;
#13660 = DIRECTION ( 'NONE',  ( 1.000000000000000000, 4.163336342344333240E-14, 0.000000000000000000 ) ) ;
#13661 = ORIENTED_EDGE ( 'NONE', *, *, #11215, .F. ) ;
#13662 = DIRECTION ( 'NONE',  ( 1.000000000000000078E-15, -1.000000000000000083E-30, -1.000000000000000000 ) ) ;
#13663 = CARTESIAN_POINT ( 'NONE',  ( 102.0669959706335561, -27.97053095873570427, 15.48979716230626913 ) ) ;
#13664 = DIRECTION ( 'NONE',  ( 1.000000000000000000, -5.337610695313248426E-16, 0.000000000000000000 ) ) ;
#13665 = DIRECTION ( 'NONE',  ( -0.7071067811571960515, 0.7071067812158990940, 0.000000000000000000 ) ) ;
#13666 = CARTESIAN_POINT ( 'NONE',  ( 107.5482541545970605, -45.77270802984816811, 197.0533722090289643 ) ) ;
#13667 = CARTESIAN_POINT ( 'NONE',  ( 118.0484485056734769, -38.34478726580598362, 73.72229194257801055 ) ) ;
#13668 = VERTEX_POINT ( 'NONE', #10480 ) ;
#13669 = CARTESIAN_POINT ( 'NONE',  ( 182.4202572930265660, -31.94127993907054730, 313.9678068554149490 ) ) ;
#13670 = ORIENTED_EDGE ( 'NONE', *, *, #82936, .F. ) ;
#13671 = CARTESIAN_POINT ( 'NONE',  ( -85.85227416678151258, 70.17658267799284033, -81.76234319299396702 ) ) ;
#13672 = ORIENTED_EDGE ( 'NONE', *, *, #18764, .T. ) ;
#13673 = DIRECTION ( 'NONE',  ( 0.000000000000000000, 0.000000000000000000, -1.000000000000000000 ) ) ;
#13674 = ORIENTED_EDGE ( 'NONE', *, *, #43727, .T. ) ;
#13675 = LINE ( 'NONE', #41362, #74047 ) ;
#13676 = CARTESIAN_POINT ( 'NONE',  ( 103.6786524251748460, -132.6284614801578243, 250.2203867545810283 ) ) ;
#13677 = CARTESIAN_POINT ( 'NONE',  ( 194.0371591254575776, -24.89890238294407254, 129.9678068554150343 ) ) ;
#13678 = CYLINDRICAL_SURFACE ( 'NONE', #14713, 12.70000000000000107 ) ;
#13679 = VERTEX_POINT ( 'NONE', #38181 ) ;
#13680 = CARTESIAN_POINT ( 'NONE',  ( 101.1290945223330198, -28.09024711436062915, 50.55562527591095545 ) ) ;
#13681 = VECTOR ( 'NONE', #86406, 1000.000000000000000 ) ;
#13682 = ADVANCED_FACE ( 'NONE', ( #80424 ), #66776, .T. ) ;
#13684 = CARTESIAN_POINT ( 'NONE',  ( 98.83784439188674753, 74.16222525595216553, -85.30119219530038777 ) ) ;
#13683 = DIRECTION ( 'NONE',  ( -0.000000000000000000, 1.000000000000000000, 0.000000000000000000 ) ) ;
#13685 = CARTESIAN_POINT ( 'NONE',  ( 68.69857366530352749, -82.21785355595537226, 247.5323269625177716 ) ) ;
#13686 = ADVANCED_FACE ( 'NONE', ( #73593 ), #4563, .F. ) ;
#13687 = DIRECTION ( 'NONE',  ( 0.000000000000000000, 1.000000000000000000, 0.000000000000000000 ) ) ;
#13688 = ORIENTED_EDGE ( 'NONE', *, *, #17723, .F. ) ;
#13689 = EDGE_CURVE ( 'NONE', #77431, #13215, #47213, .T. ) ;
#13690 = DIRECTION ( 'NONE',  ( 0.000000000000000000, -1.000000000000000000, 0.000000000000000000 ) ) ;
#13691 = CARTESIAN_POINT ( 'NONE',  ( -462.0260000000000105, 53.97500000000000142, -3.174999999999999822 ) ) ;
#13692 = CARTESIAN_POINT ( 'NONE',  ( 5.627926923415666138, 71.15750911566317427, 118.4229113093306438 ) ) ;
#13693 = EDGE_CURVE ( 'NONE', #12149, #40524, #28339, .T. ) ;
#13694 = VERTEX_POINT ( 'NONE', #34938 ) ;
#13695 = CARTESIAN_POINT ( 'NONE',  ( 96.06465719955961902, -38.01203376208108153, 82.43086337114895912 ) ) ;
#13697 = PLANE ( 'NONE',  #10841 ) ;
#13696 = CARTESIAN_POINT ( 'NONE',  ( 20.03715912545736799, -24.42818131006189830, 237.4678068554150059 ) ) ;
#13698 = CARTESIAN_POINT ( 'NONE',  ( 103.1875000000000000, 127.0000000000000000, 7.937500000000360600 ) ) ;
#13699 = EDGE_CURVE ( 'NONE', #42802, #3897, #51552, .T. ) ;
#13700 = AXIS2_PLACEMENT_3D ( 'NONE', #84146, #22360, #85497 ) ;
#13701 = AXIS2_PLACEMENT_3D ( 'NONE', #11915, #39163, #48195 ) ;
#13702 = AXIS2_PLACEMENT_3D ( 'NONE', #34416, #48034, #27162 ) ;
#13703 = AXIS2_PLACEMENT_3D ( 'NONE', #22972, #57011, #22081 ) ;
#13705 = EDGE_CURVE ( 'NONE', #85160, #36866, #12722, .T. ) ;
#13704 = CARTESIAN_POINT ( 'NONE',  ( 141.2325875157518453, -122.8456360496983137, 248.3919668373590071 ) ) ;
#13706 = ORIENTED_EDGE ( 'NONE', *, *, #52741, .F. ) ;
#13707 = CARTESIAN_POINT ( 'NONE',  ( 114.0519814166326995, -29.87813257090978070, 145.4441967044819819 ) ) ;
#13709 = VERTEX_POINT ( 'NONE', #75835 ) ;
#13708 = CARTESIAN_POINT ( 'NONE',  ( 25.56670390244820368, -42.82844715994167473, 259.7178068554150059 ) ) ;
#13710 = VECTOR ( 'NONE', #86534, 1000.000000000000000 ) ;
#13711 = VECTOR ( 'NONE', #36949, 1000.000000000000000 ) ;
#13712 = CARTESIAN_POINT ( 'NONE',  ( 100.0388059118473052, -29.01104360887439526, 281.6641967044822650 ) ) ;
#13713 = CARTESIAN_POINT ( 'NONE',  ( 0.000000000000000000, 2.031999999999865025, 0.000000000000000000 ) ) ;
#13714 = DIRECTION ( 'NONE',  ( 0.000000000000000000, 0.000000000000000000, 1.000000000000000000 ) ) ;
#13715 = DIRECTION ( 'NONE',  ( 0.000000000000000000, 0.000000000000000000, 1.000000000000000000 ) ) ;
#13716 = DIRECTION ( 'NONE',  ( 0.000000000000000000, 0.000000000000000000, -1.000000000000000000 ) ) ;
#13717 = ADVANCED_FACE ( 'NONE', ( #69474 ), #48541, .F. ) ;
#13718 = CARTESIAN_POINT ( 'NONE',  ( 138.8664832912740223, -71.52944715994085811, 394.9756252759100903 ) ) ;
#13719 = CARTESIAN_POINT ( 'NONE',  ( -98.83784439188610804, 74.16222525595216553, 85.30119219530108410 ) ) ;
#13720 = CARTESIAN_POINT ( 'NONE',  ( 112.6571330189593141, -45.46348522128867131, 218.0175300378159591 ) ) ;
#13721 = VERTEX_POINT ( 'NONE', #76734 ) ;
#13722 = ORIENTED_EDGE ( 'NONE', *, *, #6307, .F. ) ;
#13723 = ADVANCED_FACE ( 'NONE', ( #68127 ), #14515, .F. ) ;
#13724 = CARTESIAN_POINT ( 'NONE',  ( 110.7647657470428157, -46.09926102310604534, 169.3072975916109613 ) ) ;
#13725 = DIRECTION ( 'NONE',  ( -1.000000000000000000, 6.745093096447288888E-17, -9.693101022688619289E-16 ) ) ;
#13727 = CARTESIAN_POINT ( 'NONE',  ( 97.79819076598835181, -40.48430223427173757, 57.63277862058793488 ) ) ;
#13726 = CARTESIAN_POINT ( 'NONE',  ( 100.3317924633492737, -42.48897995906190772, 28.32158330589695794 ) ) ;
#13728 = LINE ( 'NONE', #7361, #10115 ) ;
#13729 = LINE ( 'NONE', #55029, #51872 ) ;
#13730 = FACE_OUTER_BOUND ( 'NONE', #77812, .T. ) ;
#13731 = CARTESIAN_POINT ( 'NONE',  ( 108.4174892490654258, -26.73503592719089639, 105.9689586094897038 ) ) ;
#13732 = DIRECTION ( 'NONE',  ( 1.000000000000000000, 1.000000000000000078E-15, 0.000000000000000000 ) ) ;
#13733 = CARTESIAN_POINT ( 'NONE',  ( 96.79426660377257008, -34.87310936442964504, 241.1841967044819626 ) ) ;
#13734 = CARTESIAN_POINT ( 'NONE',  ( 105.8002857911943977, -26.72392027096438127, 170.1763073387932934 ) ) ;
#13735 = EDGE_LOOP ( 'NONE', ( #88204, #30000 ) ) ;
#13736 = ORIENTED_EDGE ( 'NONE', *, *, #69065, .T. ) ;
#13737 = ADVANCED_FACE ( 'NONE', ( #42193 ), #82227, .F. ) ;
#13738 = CARTESIAN_POINT ( 'NONE',  ( -99.78212687779739554, 76.18750001922978754, -84.19388261208001722 ) ) ;
#13739 = CARTESIAN_POINT ( 'NONE',  ( -74.49778344313841671, 84.62843115047675724, -92.22587532767836649 ) ) ;
#13740 = LINE ( 'NONE', #64135, #28716 ) ;
#13742 = EDGE_CURVE ( 'NONE', #50282, #62015, #26778, .T. ) ;
#13741 = LINE ( 'NONE', #54594, #65111 ) ;
#13743 = PRESENTATION_LAYER_ASSIGNMENT (  '', '', ( #2145 ) ) ;
#13744 = DIRECTION ( 'NONE',  ( -0.5000000000000015543, 0.8660254037844377084, -2.602085213965216006E-14 ) ) ;
#13745 = ORIENTED_EDGE ( 'NONE', *, *, #47930, .F. ) ;
#13746 = DIRECTION ( 'NONE',  ( 0.000000000000000000, 0.000000000000000000, 1.000000000000000000 ) ) ;
#13747 = VECTOR ( 'NONE', #57120, 1000.000000000000000 ) ;
#13748 = CARTESIAN_POINT ( 'NONE',  ( 116.9255123305063222, -41.72731008894000837, 248.4651490854349731 ) ) ;
#13749 = EDGE_LOOP ( 'NONE', ( #54289, #3885, #44677, #62248 ) ) ;
#13750 = CARTESIAN_POINT ( 'NONE',  ( -8.621918145265579980, 91.74735363741767458, 118.2424309765198416 ) ) ;
#13751 = CARTESIAN_POINT ( 'NONE',  ( 107.0664832912739968, -36.72944715994100306, 287.6356252759109680 ) ) ;
#13752 = CARTESIAN_POINT ( 'NONE',  ( 105.7149151130501536, -46.72377363291952435, 167.4689823453068698 ) ) ;
#13753 = CARTESIAN_POINT ( 'NONE',  ( 99.12283442819817481, -33.29442637601800214, 58.83189989340093007 ) ) ;
#13754 = CARTESIAN_POINT ( 'NONE',  ( 102.9047493514100893, -27.10917607469848178, 151.4013395616249511 ) ) ;
#13755 = DIRECTION ( 'NONE',  ( 0.000000000000000000, -1.000000000000000000, 0.000000000000000000 ) ) ;
#13756 = ORIENTED_EDGE ( 'NONE', *, *, #16033, .F. ) ;
#13757 = EDGE_CURVE ( 'NONE', #58541, #20859, #70446, .T. ) ;
#13758 = FACE_OUTER_BOUND ( 'NONE', #47870, .T. ) ;
#13759 = ORIENTED_EDGE ( 'NONE', *, *, #80876, .T. ) ;
#13760 = ORIENTED_EDGE ( 'NONE', *, *, #49151, .F. ) ;
#13761 = EDGE_CURVE ( 'NONE', #33523, #62846, #89312, .T. ) ;
#13762 = AXIS2_PLACEMENT_3D ( 'NONE', #88458, #6231, #5332 ) ;
#13763 = FACE_OUTER_BOUND ( 'NONE', #20797, .T. ) ;
#13764 = AXIS2_PLACEMENT_3D ( 'NONE', #28925, #15301, #1673 ) ;
#13765 = EDGE_LOOP ( 'NONE', ( #5284, #70786 ) ) ;
#13766 = ORIENTED_EDGE ( 'NONE', *, *, #3035, .F. ) ;
#13767 = DIRECTION ( 'NONE',  ( 0.000000000000000000, -1.000000000000000000, 0.000000000000000000 ) ) ;
#13768 = VECTOR ( 'NONE', #19117, 1000.000000000000000 ) ;
#13769 = CARTESIAN_POINT ( 'NONE',  ( 99.26324148224303201, -33.25589724784042289, 100.4152769709339736 ) ) ;
#13771 = CARTESIAN_POINT ( 'NONE',  ( 117.4964429983690337, -36.12752982774328103, 228.8727681330539667 ) ) ;
#13770 = VECTOR ( 'NONE', #41923, 1000.000000000000000 ) ;
#13772 = AXIS2_PLACEMENT_3D ( 'NONE', #74490, #4558, #80420 ) ;
#13773 = CARTESIAN_POINT ( 'NONE',  ( 98.56907362037662779, -44.95393718666142746, 191.9384824187679612 ) ) ;
#13774 = CARTESIAN_POINT ( 'NONE',  ( 96.73644666290624627, -38.23103596604165233, 62.44133956162495025 ) ) ;
#13775 = LINE ( 'NONE', #1039, #12194 ) ;
#13776 = DIRECTION ( 'NONE',  ( 1.000000000000000000, 0.000000000000000000, 0.000000000000000000 ) ) ;
#13777 = ORIENTED_EDGE ( 'NONE', *, *, #44758, .F. ) ;
#13778 = VECTOR ( 'NONE', #69235, 1000.000000000000000 ) ;
#13779 = CARTESIAN_POINT ( 'NONE',  ( 116.0091996907507905, -30.12340400999213941, 109.3327681330539605 ) ) ;
#13780 = CARTESIAN_POINT ( 'NONE',  ( 107.3221093067165128, -25.63226107660779007, 75.04610146638695767 ) ) ;
#13781 = CARTESIAN_POINT ( 'NONE',  ( 97.51966259852430596, -43.83486848311488160, 261.8356252759109566 ) ) ;
#13782 = ORIENTED_EDGE ( 'NONE', *, *, #85177, .T. ) ;
#13783 = CARTESIAN_POINT ( 'NONE',  ( 98.03659727384791722, -44.40418782976336587, 226.8870538473399563 ) ) ;
#13784 = CARTESIAN_POINT ( 'NONE',  ( 113.2454986814590683, -28.75867293103612710, 34.55229194428200401 ) ) ;
#13785 =( NAMED_UNIT ( * ) SI_UNIT ( $, .STERADIAN. ) SOLID_ANGLE_UNIT ( ) );
#13786 = CARTESIAN_POINT ( 'NONE',  ( 113.1774878185915298, -44.75247536050181907, 24.09387774641090729 ) ) ;
#13787 = DIRECTION ( 'NONE',  ( 1.000000000000000078E-15, -1.000000000000000083E-30, -1.000000000000000000 ) ) ;
#13788 = AXIS2_PLACEMENT_3D ( 'NONE', #76460, #50081, #29652 ) ;
#13789 = ADVANCED_FACE ( 'NONE', ( #48101 ), #63091, .T. ) ;
#13791 = PLANE ( 'NONE',  #44166 ) ;
#13790 = LINE ( 'NONE', #41474, #4217 ) ;
#13792 = CARTESIAN_POINT ( 'NONE',  ( -487.2989999999999782, 93.66249999999999432, 90.48749999999999716 ) ) ;
#13793 = ADVANCED_FACE ( 'NONE', ( #62198 ), #74944, .T. ) ;
#13794 = CARTESIAN_POINT ( 'NONE',  ( 0.000000000000000000, 101.5999999999999943, 0.000000000000000000 ) ) ;
#13795 = PLANE ( 'NONE',  #49907 ) ;
#13796 = EDGE_CURVE ( 'NONE', #19, #26777, #35379, .T. ) ;
#13797 = DIRECTION ( 'NONE',  ( -4.237773401492740281E-14, 1.000000000000000000, 0.000000000000000000 ) ) ;
#13798 = CARTESIAN_POINT ( 'NONE',  ( 37.06648329127400388, 12.92155284005802685, 349.2756252759108406 ) ) ;
#13799 = DIRECTION ( 'NONE',  ( -0.7071067812159675947, -0.7071067811571274397, -7.071067812159980775E-16 ) ) ;
#13801 = ORIENTED_EDGE ( 'NONE', *, *, #81440, .T. ) ;
#13800 = CARTESIAN_POINT ( 'NONE',  ( 99.09570905812269359, -30.55043177598640369, 260.8022919448715697 ) ) ;
#13802 = ADVANCED_FACE ( 'NONE', ( #26344 ), #54013, .F. ) ;
#13803 = CARTESIAN_POINT ( 'NONE',  ( 12.69999999999999929, 82.54999999999999716, 206.3750000000000000 ) ) ;
#13804 = CARTESIAN_POINT ( 'NONE',  ( 118.1265197682042327, -36.12032134488166690, 273.8822919425775808 ) ) ;
#13805 = CARTESIAN_POINT ( 'NONE',  ( 102.3931144830280715, -26.71278082505766704, 131.4118157521009778 ) ) ;
#13806 = CARTESIAN_POINT ( 'NONE',  ( 97.52025866034094292, -43.83442485161933178, 257.8356252759109566 ) ) ;
#13807 = LINE ( 'NONE', #88339, #25791 ) ;
#13809 = DIRECTION ( 'NONE',  ( 0.000000000000000000, 0.000000000000000000, -1.000000000000000000 ) ) ;
#13808 = PLANE ( 'NONE',  #47828 ) ;
#13810 = LINE ( 'NONE', #53319, #26230 ) ;
#13811 = VECTOR ( 'NONE', #87286, 1000.000000000000000 ) ;
#13812 = DIRECTION ( 'NONE',  ( 4.299999999999999979E-14, -1.000000000000000000, 4.400000000000000367E-29 ) ) ;
#13813 = EDGE_CURVE ( 'NONE', #56525, #67362, #13168, .T. ) ;
#13814 = ORIENTED_EDGE ( 'NONE', *, *, #82838, .T. ) ;
#13815 = CARTESIAN_POINT ( 'NONE',  ( 45.56670390244706681, -48.82844715994099971, 300.4678068554150059 ) ) ;
#13816 = EDGE_LOOP ( 'NONE', ( #38162, #26585, #7727, #15936, #5199, #56535, #72831, #11748, #36994, #7467, #61449, #89653, #85354, #6857 ) ) ;
#13817 = EDGE_CURVE ( 'NONE', #48257, #49936, #6344, .T. ) ;
#13818 = CARTESIAN_POINT ( 'NONE',  ( 102.9027671602101037, -44.22047980607887752, 186.5952769709339805 ) ) ;
#13820 = VERTEX_POINT ( 'NONE', #84467 ) ;
#13819 = CARTESIAN_POINT ( 'NONE',  ( 151.0371591254573502, -24.42818131005592974, 249.9678068554149490 ) ) ;
#13821 = DIRECTION ( 'NONE',  ( 1.000000000000000000, 4.237773401492740281E-14, 0.000000000000000000 ) ) ;
#13822 = CARTESIAN_POINT ( 'NONE',  ( 96.67182511810091228, -37.15340426533111895, 157.3584824187679487 ) ) ;
#13823 = CARTESIAN_POINT ( 'NONE',  ( 56.06670390244700997, -79.67844715994098692, 190.2178068554179902 ) ) ;
#13824 = FACE_OUTER_BOUND ( 'NONE', #65494, .T. ) ;
#13825 = CARTESIAN_POINT ( 'NONE',  ( -89.12695577293538918, 72.47328848629025799, 78.17938156622544454 ) ) ;
#13826 = CARTESIAN_POINT ( 'NONE',  ( 53.56670390244833158, -48.82844715994055917, 249.9678068554150343 ) ) ;
#13827 = CARTESIAN_POINT ( 'NONE',  ( 114.6661721138975025, -42.88640786233948887, 88.28419670448295165 ) ) ;
#13828 = ORIENTED_EDGE ( 'NONE', *, *, #58596, .F. ) ;
#13829 = EDGE_LOOP ( 'NONE', ( #60495, #25691, #51213, #8760 ) ) ;
#13830 = ORIENTED_EDGE ( 'NONE', *, *, #58217, .T. ) ;
#13831 = VECTOR ( 'NONE', #5571, 1000.000000000000000 ) ;
#13832 = VECTOR ( 'NONE', #65103, 1000.000000000000000 ) ;
#13833 = CARTESIAN_POINT ( 'NONE',  ( 44.45000000000000284, 50.79999999999999716, 257.1750000000000114 ) ) ;
#13834 = VECTOR ( 'NONE', #4225, 1000.000000000000000 ) ;
#13836 = CARTESIAN_POINT ( 'NONE',  ( 104.4081007499953984, -46.45808916365906782, 37.36479194982128149 ) ) ;
#13835 = CARTESIAN_POINT ( 'NONE',  ( 104.7173522264389618, -47.59653351925012288, 178.4070538473389718 ) ) ;
#13837 = VECTOR ( 'NONE', #26235, 1000.000000000000000 ) ;
#13838 = CARTESIAN_POINT ( 'NONE',  ( 161.0667039024469886, -67.87844715994089029, 55.21780685541800437 ) ) ;
#13839 = DIRECTION ( 'NONE',  ( 0.000000000000000000, 0.000000000000000000, -1.000000000000000000 ) ) ;
#13841 = DIRECTION ( 'NONE',  ( 0.000000000000000000, 1.000000000000000000, 0.000000000000000000 ) ) ;
#13840 = AXIS2_PLACEMENT_3D ( 'NONE', #82984, #48406, #76139 ) ;
#13842 = CARTESIAN_POINT ( 'NONE',  ( 0.000000000000000000, 60.82030000000000314, 265.5569999999999595 ) ) ;
#13843 = CARTESIAN_POINT ( 'NONE',  ( 68.20141520875638719, -68.96305191817310742, 247.2983592438824587 ) ) ;
#13844 = CARTESIAN_POINT ( 'NONE',  ( 97.85535806214033983, -31.89376338832682123, 135.9413395616259947 ) ) ;
#13845 = ORIENTED_EDGE ( 'NONE', *, *, #87637, .T. ) ;
#13846 = EDGE_LOOP ( 'NONE', ( #65648, #6170, #76256, #12115 ) ) ;
#13847 = EDGE_LOOP ( 'NONE', ( #23848, #42094, #39662, #70734 ) ) ;
#13848 = CIRCLE ( 'NONE', #29812, 0.5000000000000004441 ) ;
#13849 = DIRECTION ( 'NONE',  ( 1.000000000000000000, 2.999999999999999839E-15, 1.000000000000000078E-15 ) ) ;
#13850 = CARTESIAN_POINT ( 'NONE',  ( -87.71306776503853087, 93.55256755804782642, -96.70275196374447546 ) ) ;
#13852 = EDGE_CURVE ( 'NONE', #73470, #28852, #2227, .T. ) ;
#13851 = CARTESIAN_POINT ( 'NONE',  ( 183.6524903400783160, -48.32844715993452667, 300.4678068554149490 ) ) ;
#13853 = CARTESIAN_POINT ( 'NONE',  ( 113.3093514795881589, -30.73549005055465955, 187.2414237029249477 ) ) ;
#13854 = APPLICATION_CONTEXT ( 'automotive_design' ) ;
#13855 = DIRECTION ( 'NONE',  ( 0.4214249218767882055, 0.9068632946707806397, 4.214249218767890910E-16 ) ) ;
#13856 = AXIS2_PLACEMENT_3D ( 'NONE', #6537, #168, #82864 ) ;
#13857 = CARTESIAN_POINT ( 'NONE',  ( 146.0042039024470171, -68.87844715994090450, 222.2178068554179902 ) ) ;
#13858 = ORIENTED_EDGE ( 'NONE', *, *, #41190, .T. ) ;
#13860 = ORIENTED_EDGE ( 'NONE', *, *, #58196, .F. ) ;
#13859 = VERTEX_POINT ( 'NONE', #3894 ) ;
#13861 = CARTESIAN_POINT ( 'NONE',  ( 144.1829449321824654, -138.0544793359106848, 247.6577929143110168 ) ) ;
#13862 = ORIENTED_EDGE ( 'NONE', *, *, #57502, .T. ) ;
#13863 = ORIENTED_EDGE ( 'NONE', *, *, #8956, .F. ) ;
#13864 = CARTESIAN_POINT ( 'NONE',  ( 78.82227874343284668, -21.18254450372301534, 7.982620440116730443 ) ) ;
#13865 = CARTESIAN_POINT ( 'NONE',  ( 111.8242684682981718, -44.20552626741085334, 259.4587261630397848 ) ) ;
#13866 = ORIENTED_EDGE ( 'NONE', *, *, #18307, .T. ) ;
#13867 = DIRECTION ( 'NONE',  ( 1.000000000000000000, 0.000000000000000000, 9.462128050782575008E-16 ) ) ;
#13868 = AXIS2_PLACEMENT_3D ( 'NONE', #2285, #64062, #29989 ) ;
#13869 = CARTESIAN_POINT ( 'NONE',  ( -124.2531446105977011, 71.60797102361802047, 40.07553659477990493 ) ) ;
#13870 = ORIENTED_EDGE ( 'NONE', *, *, #35319, .F. ) ;
#13871 = EDGE_LOOP ( 'NONE', ( #69010, #25676 ) ) ;
#13872 = EDGE_CURVE ( 'NONE', #1794, #14083, #54445, .T. ) ;
#13873 = LINE ( 'NONE', #41555, #53613 ) ;
#13874 = AXIS2_PLACEMENT_3D ( 'NONE', #11798, #74469, #31782 ) ;
#13875 = ORIENTED_EDGE ( 'NONE', *, *, #40200, .T. ) ;
#13876 = VERTEX_POINT ( 'NONE', #43082 ) ;
#13877 = B_SPLINE_CURVE_WITH_KNOTS ( 'NONE', 3,
 ( #51987, #10673, #24756, #43854, #65642, #85231, #9351, #30244, #79745, #44741, #51551, #17503, #31563, #51114, #36623, #72473, #2983, #79302, #17061, #3427, #45183, #38377, #66076, #59266, #17937, #45614, #8924 ),
 .UNSPECIFIED., .F., .F.,
 ( 4, 2, 2, 2, 2, 2, 2, 2, 2, 2, 1, 1, 1, 2, 4 ),
 ( 0.000000000000000000, 0.06251142862490606522, 0.1250228572498121304, 0.1875342858747182095, 0.2500457144996242609, 0.3125571431245303122, 0.3750685717494364191, 0.4375800003743421374, 0.4688357146867948577, 0.4844635718430209126, 0.4922775004211341066, 0.4961844647101908423, 0.4981379468547192380, 0.4991146879269833803, 0.5000914289992475226 ),
 .UNSPECIFIED. ) ;
#13878 = CARTESIAN_POINT ( 'NONE',  ( 103.3964814340166498, -45.24903370896166876, 285.0709475124485266 ) ) ;
#13879 = CARTESIAN_POINT ( 'NONE',  ( 98.44037697964694189, -30.83566621160791144, 120.8499109901969604 ) ) ;
#13880 = CARTESIAN_POINT ( 'NONE',  ( 96.66103594285301881, -37.56076609107802255, 101.3899109901969524 ) ) ;
#13881 = CARTESIAN_POINT ( 'NONE',  ( 109.8023483073639710, -28.09558655615849787, 249.5838068554169240 ) ) ;
#13882 = CARTESIAN_POINT ( 'NONE',  ( 131.4004675426832023, -18.03188136815630216, 6.871351212842276901 ) ) ;
#13883 = CARTESIAN_POINT ( 'NONE',  ( 108.1817661827909376, -47.09470796318245078, 198.6613395616249989 ) ) ;
#13884 = LINE ( 'NONE', #15691, #82014 ) ;
#13885 = CARTESIAN_POINT ( 'NONE',  ( -9.749037034254357081, 224.4999999999999432, 152.4294779587682456 ) ) ;
#13886 = EDGE_LOOP ( 'NONE', ( #29873, #68371, #76620, #44301 ) ) ;
#13887 = DIRECTION ( 'NONE',  ( 0.000000000000000000, 0.000000000000000000, 1.000000000000000000 ) ) ;
#13888 = ORIENTED_EDGE ( 'NONE', *, *, #20174, .T. ) ;
#13889 = ORIENTED_EDGE ( 'NONE', *, *, #59013, .F. ) ;
#13890 = DIRECTION ( 'NONE',  ( -0.1858654557293184517, 0.9825752044329902901, 0.000000000000000000 ) ) ;
#13891 = AXIS2_PLACEMENT_3D ( 'NONE', #64005, #23136, #17962 ) ;
#13892 = CARTESIAN_POINT ( 'NONE',  ( 103.3014603440054628, -27.46527934327819054, 136.3836531168635702 ) ) ;
#13893 = VECTOR ( 'NONE', #84570, 1000.000000000000000 ) ;
#13894 = CIRCLE ( 'NONE', #28411, 2.030000000001807248 ) ;
#13895 = CARTESIAN_POINT ( 'NONE',  ( 108.7432494476977922, -25.80391683235395917, 144.9432443235299672 ) ) ;
#13896 = CARTESIAN_POINT ( 'NONE',  ( -6.118449702233622389, 71.41905655665884467, 130.4126312001327221 ) ) ;
#13897 = AXIS2_PLACEMENT_3D ( 'NONE', #76632, #33937, #89828 ) ;
#13898 = CARTESIAN_POINT ( 'NONE',  ( 97.81169182074827972, -40.51741433969252881, 77.63574375254798099 ) ) ;
#13899 = CARTESIAN_POINT ( 'NONE',  ( 124.0667039024470313, -104.2784471599417486, -9.937637710810031777 ) ) ;
#13902 = CARTESIAN_POINT ( 'NONE',  ( 117.1759530674218865, -34.27439392744689428, 205.0156252759109634 ) ) ;
#13901 = CARTESIAN_POINT ( 'NONE',  ( 5.878304635907259698E-16, 239.0000000000000000, 159.4557476874258271 ) ) ;
#13900 = DIRECTION ( 'NONE',  ( 0.000000000000000000, 0.000000000000000000, 1.000000000000000000 ) ) ;
#13903 = CARTESIAN_POINT ( 'NONE',  ( 165.9667039024459996, -28.27351298637401200, 193.9678068554150059 ) ) ;
#13904 = ADVANCED_FACE ( 'NONE', ( #52455 ), #43536, .F. ) ;
#13905 = LINE ( 'NONE', #29336, #330 ) ;
#13906 = EDGE_LOOP ( 'NONE', ( #29408, #62715 ) ) ;
#13907 = CARTESIAN_POINT ( 'NONE',  ( 68.12920390244700286, -68.87844715994098976, 55.21780685541800437 ) ) ;
#13908 = EDGE_CURVE ( 'NONE', #26420, #28268, #63172, .T. ) ;
#13909 = CARTESIAN_POINT ( 'NONE',  ( -7.205548786489490269E-13, 117.4749999999999943, 103.1875000000000000 ) ) ;
#13910 = EDGE_CURVE ( 'NONE', #19, #84869, #45645, .T. ) ;
#13911 = DIRECTION ( 'NONE',  ( 0.000000000000000000, 0.000000000000000000, -1.000000000000000000 ) ) ;
#13912 = FACE_BOUND ( 'NONE', #9842, .T. ) ;
#13914 = VERTEX_POINT ( 'NONE', #21782 ) ;
#13913 = CARTESIAN_POINT ( 'NONE',  ( 109.2210686807619453, -48.43357285789136313, 277.7213395616254843 ) ) ;
#13915 = ADVANCED_FACE ( 'NONE', ( #38852 ), #63548, .F. ) ;
#13916 = LINE ( 'NONE', #41595, #82893 ) ;
#13917 = CARTESIAN_POINT ( 'NONE',  ( 108.6520877210037952, -25.77347123183324484, 149.9737205140059473 ) ) ;
#13918 = CARTESIAN_POINT ( 'NONE',  ( 115.5737247207382552, -42.75516958203532880, 49.33562527591095659 ) ) ;
#13919 = CARTESIAN_POINT ( 'NONE',  ( 99.39016829297771949, -27.63593621212785933, 146.6356252759109395 ) ) ;
#13920 = PLANE ( 'NONE',  #60482 ) ;
#13921 = CARTESIAN_POINT ( 'NONE',  ( 97.81151828220572497, -40.51700876243793203, 102.6355898084469942 ) ) ;
#13922 = VECTOR ( 'NONE', #47201, 1000.000000000000114 ) ;
#13924 = CARTESIAN_POINT ( 'NONE',  ( 107.0664832912739968, -36.72944715994100306, 9.635625275910941312 ) ) ;
#13923 = CARTESIAN_POINT ( 'NONE',  ( 183.6524903400785718, -48.32844715993451956, 129.9678068554150059 ) ) ;
#13925 = CARTESIAN_POINT ( 'NONE',  ( 71.24189083761808661, -0.9290567490904538817, 396.9756252759102040 ) ) ;
#13926 = DIRECTION ( 'NONE',  ( -3.100000000000000258E-29, 3.100000000000000044E-14, 1.000000000000000000 ) ) ;
#13927 = ORIENTED_EDGE ( 'NONE', *, *, #64050, .T. ) ;
#13928 = AXIS2_PLACEMENT_3D ( 'NONE', #80860, #53997, #79972 ) ;
#13929 = VERTEX_POINT ( 'NONE', #50352 ) ;
#13930 = ORIENTED_EDGE ( 'NONE', *, *, #41872, .T. ) ;
#13931 = ADVANCED_FACE ( 'NONE', ( #1332, #57163 ), #875, .F. ) ;
#13932 = ORIENTED_EDGE ( 'NONE', *, *, #53641, .F. ) ;
#13933 = CARTESIAN_POINT ( 'NONE',  ( 0.000000000000000000, 127.0000000000000000, -103.1875000000000000 ) ) ;
#13934 = CARTESIAN_POINT ( 'NONE',  ( 103.8480726019013645, -46.65951555449685628, 78.32705384733995402 ) ) ;
#13935 = CARTESIAN_POINT ( 'NONE',  ( 143.5667039024469886, -67.87844715994090450, 55.21780685541800437 ) ) ;
#13936 = CARTESIAN_POINT ( 'NONE',  ( 145.2632846747241899, -139.1299635158950423, 246.6334900878847520 ) ) ;
#13937 = CARTESIAN_POINT ( 'NONE',  ( 109.3680554845995232, -25.87125837001184081, 180.9222919425779708 ) ) ;
#13938 = LINE ( 'NONE', #41617, #27252 ) ;
#13939 = CARTESIAN_POINT ( 'NONE',  ( 114.1362055435773613, -41.52268812998874381, 272.7752769709339304 ) ) ;
#13940 = ORIENTED_EDGE ( 'NONE', *, *, #59139, .T. ) ;
#13941 = ORIENTED_EDGE ( 'NONE', *, *, #7988, .T. ) ;
#13942 = VERTEX_POINT ( 'NONE', #66110 ) ;
#13943 = CARTESIAN_POINT ( 'NONE',  ( 116.3195061320206207, -32.94150711290046729, 139.1356252759109680 ) ) ;
#13944 = CARTESIAN_POINT ( 'NONE',  ( 172.5664832912740110, 0.2215528400590013880, 138.9256252759119832 ) ) ;
#13945 = CARTESIAN_POINT ( 'NONE',  ( 112.1405389099331984, -28.01350764861801323, 19.65586982525807613 ) ) ;
#13946 = FACE_OUTER_BOUND ( 'NONE', #67810, .T. ) ;
#13947 = CARTESIAN_POINT ( 'NONE',  ( 184.5667039024480118, -67.87844715994100397, 10.91780685541479734 ) ) ;
#13948 = CARTESIAN_POINT ( 'NONE',  ( 188.5667039024479834, -48.82844715994099971, 173.2178068554149775 ) ) ;
#13949 = DIRECTION ( 'NONE',  ( 0.000000000000000000, 1.000000000000000000, 0.000000000000000000 ) ) ;
#13950 = CARTESIAN_POINT ( 'NONE',  ( 102.7643194828038276, -25.71402177940525746, 20.37276813305294354 ) ) ;
#13951 = CARTESIAN_POINT ( 'NONE',  ( 140.0667039024470171, -90.27844715994091018, 45.21780685541799727 ) ) ;
#13952 = ORIENTED_EDGE ( 'NONE', *, *, #80198, .T. ) ;
#13953 = CARTESIAN_POINT ( 'NONE',  ( 95.64925804648841279, -35.75026674902539980, 300.2406250056037038 ) ) ;
#13954 = VECTOR ( 'NONE', #46000, 1000.000000000000000 ) ;
#13956 = EDGE_CURVE ( 'NONE', #57074, #75399, #80216, .T. ) ;
#13955 = CARTESIAN_POINT ( 'NONE',  ( 75.61066417432020614, 0.000000000000000000, 177.0380000000000109 ) ) ;
#13957 = CARTESIAN_POINT ( 'NONE',  ( 100.4295600883690014, -42.28392062234677695, 69.68713798863895192 ) ) ;
#13958 = AXIS2_PLACEMENT_3D ( 'NONE', #18866, #46990, #20219 ) ;
#13959 = VECTOR ( 'NONE', #68432, 1000.000000000000000 ) ;
#13960 = CIRCLE ( 'NONE', #24209, 11.57110091390439699 ) ;
#13961 = AXIS2_PLACEMENT_3D ( 'NONE', #11832, #67232, #45871 ) ;
#13962 = EDGE_CURVE ( 'NONE', #8744, #83042, #71714, .T. ) ;
#13963 = DIRECTION ( 'NONE',  ( 0.000000000000000000, 1.000000000000000000, 0.000000000000000000 ) ) ;
#13964 = CARTESIAN_POINT ( 'NONE',  ( 52.38749999999999574, 94.53880000000000905, 254.7937499999999886 ) ) ;
#13965 = ORIENTED_EDGE ( 'NONE', *, *, #50558, .T. ) ;
#13966 = ORIENTED_EDGE ( 'NONE', *, *, #52227, .T. ) ;
#13967 = CARTESIAN_POINT ( 'NONE',  ( 80.06648329127399677, -33.97944715994105991, 8.225625275910942946 ) ) ;
#13968 = VERTEX_POINT ( 'NONE', #84910 ) ;
#13969 = CARTESIAN_POINT ( 'NONE',  ( 105.3162203493976676, -48.44985994433862686, 147.4584824187679715 ) ) ;
#13970 = ORIENTED_EDGE ( 'NONE', *, *, #12286, .F. ) ;
#13971 = FACE_BOUND ( 'NONE', #43662, .T. ) ;
#13972 = CARTESIAN_POINT ( 'NONE',  ( 116.0270257299131487, -33.90363670229466919, 125.4892023535159638 ) ) ;
#13973 = CARTESIAN_POINT ( 'NONE',  ( 98.36549455146187881, -40.29075363668734155, 11.63562527591094309 ) ) ;
#13974 = AXIS2_PLACEMENT_3D ( 'NONE', #33329, #87852, #12898 ) ;
#13975 = CARTESIAN_POINT ( 'NONE',  ( 101.1293421793351968, -28.09060746778665418, 46.55562527591094835 ) ) ;
#13976 = CARTESIAN_POINT ( 'NONE',  ( 95.05156358570199870, -41.69348830286664764, 292.6356252759106837 ) ) ;
#13977 = EDGE_LOOP ( 'NONE', ( #47423, #8101, #68931, #35770 ) ) ;
#13978 = EDGE_CURVE ( 'NONE', #82359, #18397, #10699, .T. ) ;
#13979 = CARTESIAN_POINT ( 'NONE',  ( -117.8825533107840329, 80.89685143461892380, -12.61964884581497692 ) ) ;
#13980 = VERTEX_POINT ( 'NONE', #59293 ) ;
#13981 = VECTOR ( 'NONE', #89004, 1000.000000000000000 ) ;
#13982 = ORIENTED_EDGE ( 'NONE', *, *, #84179, .F. ) ;
#13983 = DIRECTION ( 'NONE',  ( 1.000000000000000000, -7.570719237730591757E-15, 0.000000000000000000 ) ) ;
#13984 = ORIENTED_EDGE ( 'NONE', *, *, #36236, .T. ) ;
#13985 = CARTESIAN_POINT ( 'NONE',  ( 96.36668125800717633, -39.40815171121898430, 16.53372051400597798 ) ) ;
#13986 = CARTESIAN_POINT ( 'NONE',  ( 102.6884963789050289, -46.90384819475383438, 133.2651490854349561 ) ) ;
#13987 = CARTESIAN_POINT ( 'NONE',  ( 108.0667039024470455, -121.2010968907524529, -19.26696060647547881 ) ) ;
#13988 = CARTESIAN_POINT ( 'NONE',  ( 115.0889047246291454, -30.61763668101085045, 140.3439586091480464 ) ) ;
#13989 = CARTESIAN_POINT ( 'NONE',  ( 97.26643838138058129, -31.61739275409173544, 86.93181575210095957 ) ) ;
#13990 = CARTESIAN_POINT ( 'NONE',  ( 173.9899999999999807, 52.73749999999999716, -44.45000000000000284 ) ) ;
#13991 = EDGE_LOOP ( 'NONE', ( #15162, #31055, #55037, #24336 ) ) ;
#13992 = FACE_OUTER_BOUND ( 'NONE', #7627, .T. ) ;
#13993 = EDGE_CURVE ( 'NONE', #76533, #83920, #5209, .T. ) ;
#13994 = DIRECTION ( 'NONE',  ( 8.673617379884035472E-16, 1.000000000000000000, 0.000000000000000000 ) ) ;
#13995 = VECTOR ( 'NONE', #50834, 1000.000000000000000 ) ;
#13996 = EDGE_LOOP ( 'NONE', ( #52890, #24026 ) ) ;
#13997 = DIRECTION ( 'NONE',  ( 0.000000000000000000, 0.000000000000000000, -1.000000000000000000 ) ) ;
#13998 = CARTESIAN_POINT ( 'NONE',  ( 163.5667039024460223, -18.82844715994111340, -5.074374724088000832 ) ) ;
#13999 = CARTESIAN_POINT ( 'NONE',  ( 97.35142178662984236, -32.85085377626895564, 41.02419670448193045 ) ) ;
#14000 = CARTESIAN_POINT ( 'NONE',  ( 154.5667039024469886, -67.87844715994090450, 120.2178068554179902 ) ) ;
#14001 = FACE_OUTER_BOUND ( 'NONE', #38225, .T. ) ;
#14002 = CARTESIAN_POINT ( 'NONE',  ( 116.3229784443844324, -32.93528945216412041, 94.13562527591096796 ) ) ;
#14003 = CARTESIAN_POINT ( 'NONE',  ( 117.8597870418416562, -34.07357964055000821, 14.01848241876896317 ) ) ;
#14005 = CARTESIAN_POINT ( 'NONE',  ( 97.95167206076199307, -31.64175201202211341, 106.9213395616259703 ) ) ;
#14004 = CARTESIAN_POINT ( 'NONE',  ( 97.81413224952068219, -40.51639846094042952, 101.6360726122380100 ) ) ;
#14006 = LINE ( 'NONE', #55315, #84345 ) ;
#14007 = CARTESIAN_POINT ( 'NONE',  ( 101.9504156919933280, -46.58027128656367921, 167.1832443235299763 ) ) ;
#14008 = LINE ( 'NONE', #75347, #78634 ) ;
#14009 = ORIENTED_EDGE ( 'NONE', *, *, #59501, .F. ) ;
#14010 = CARTESIAN_POINT ( 'NONE',  ( -47.02966122971772478, 92.07499999999998863, -43.25671021339634592 ) ) ;
#14011 = DIRECTION ( 'NONE',  ( 0.000000000000000000, 0.000000000000000000, -1.000000000000000000 ) ) ;
#14012 = FACE_OUTER_BOUND ( 'NONE', #7785, .T. ) ;
#14014 = ORIENTED_EDGE ( 'NONE', *, *, #29820, .T. ) ;
#14013 = EDGE_CURVE ( 'NONE', #50621, #60674, #56259, .T. ) ;
#14015 = CARTESIAN_POINT ( 'NONE',  ( 104.4919955313450686, -26.97824969402968875, 61.28156387838701136 ) ) ;
#14017 = VERTEX_POINT ( 'NONE', #36748 ) ;
#14016 = CARTESIAN_POINT ( 'NONE',  ( 97.38432216341050207, -42.15794967186695175, 181.7451490854349743 ) ) ;
#14018 = LINE ( 'NONE', #75805, #61078 ) ;
#14019 = CARTESIAN_POINT ( 'NONE',  ( 99.06932979199925171, -29.95266829982950441, 211.7670538473399517 ) ) ;
#14020 = VECTOR ( 'NONE', #66581, 1000.000000000000000 ) ;
#14021 = CARTESIAN_POINT ( 'NONE',  ( 112.0840054422653935, -139.4321760210394814, 247.7260698222571307 ) ) ;
#14022 = B_SPLINE_CURVE_WITH_KNOTS ( 'NONE', 3,
 ( #66429, #19193, #59605, #87782, #17842, #45520, #32806, #25544, #53220, #65980, #88694, #52326, #87342, #80091, #88248, #25103, #46862, #5112, #73242, #60965, #3772, #26451, #31460, #60052, #12374, #52765, #80990, #11482, #18737, #26005, #40064 ),
 .UNSPECIFIED., .F., .F.,
 ( 4, 2, 2, 1, 2, 2, 2, 2, 2, 2, 2, 1, 1, 2, 2, 2, 4 ),
 ( 0.000000000000000000, 0.1249999999999613920, 0.1874999999999421019, 0.2187499999999242273, 0.2343749999999238942, 0.2499999999999235611, 0.3749999999998904765, 0.4374999999998728795, 0.4999999999998552269, 0.6249999999998172573, 0.6874999999997966071, 0.7187499999997883915, 0.7343749999997789546, 0.7421874999997795097, 0.7499999999997800648, 0.8749999999998900879, 1.000000000000000000 ),
 .UNSPECIFIED. ) ;
#14023 = CARTESIAN_POINT ( 'NONE',  ( -24.20305689751608824, 53.97499999999997300, 58.62596543806478877 ) ) ;
#14025 = VECTOR ( 'NONE', #28705, 999.9999999999998863 ) ;
#14024 = LINE ( 'NONE', #5881, #16272 ) ;
#14026 = ORIENTED_EDGE ( 'NONE', *, *, #54049, .T. ) ;
#14027 = AXIS2_PLACEMENT_3D ( 'NONE', #46949, #32890, #74679 ) ;
#14028 = MECHANICAL_DESIGN_GEOMETRIC_PRESENTATION_REPRESENTATION (  '', ( #72065 ), #32875 ) ;
#14029 = ITEM_DEFINED_TRANSFORMATION ( 'NONE', 'NONE', #37711,  #50656 ) ;
#14030 = CIRCLE ( 'NONE', #64800, 4.762500000000002842 ) ;
#14031 = ORIENTED_EDGE ( 'NONE', *, *, #78336, .F. ) ;
#14032 = VERTEX_POINT ( 'NONE', #11147 ) ;
#14033 = ADVANCED_FACE ( 'NONE', ( #29937 ), #49451, .F. ) ;
#14034 = ORIENTED_EDGE ( 'NONE', *, *, #6318, .T. ) ;
#14035 = DIRECTION ( 'NONE',  ( 0.000000000000000000, 0.000000000000000000, -1.000000000000000000 ) ) ;
#14036 = CARTESIAN_POINT ( 'NONE',  ( 109.9601702690906677, -48.22123515106449787, 238.7727681330539724 ) ) ;
#14037 = DIRECTION ( 'NONE',  ( 0.000000000000000000, -1.000000000000000000, 0.000000000000000000 ) ) ;
#14038 = EDGE_CURVE ( 'NONE', #59995, #24816, #24789, .T. ) ;
#14039 = CARTESIAN_POINT ( 'NONE',  ( 134.4427611689604589, -15.99866847873243714, 1.641799428526213855 ) ) ;
#14041 = DIRECTION ( 'NONE',  ( -3.100000000000000258E-29, 3.100000000000000044E-14, 1.000000000000000000 ) ) ;
#14040 = CARTESIAN_POINT ( 'NONE',  ( 89.06648329127401098, -18.82844715994099971, 17.92562527591199739 ) ) ;
#14042 = CARTESIAN_POINT ( 'NONE',  ( 31.56670390244700641, -22.48495420874110806, -5.074374724088000832 ) ) ;
#14043 = AXIS2_PLACEMENT_3D ( 'NONE', #17452, #80583, #11531 ) ;
#14044 = CARTESIAN_POINT ( 'NONE',  ( 112.1280348295452001, -26.87672238358117127, 19.71086337114896736 ) ) ;
#14045 = VERTEX_POINT ( 'NONE', #42630 ) ;
#14046 = EDGE_LOOP ( 'NONE', ( #50918, #79053, #78945, #23507 ) ) ;
#14047 = AXIS2_PLACEMENT_3D ( 'NONE', #79820, #13445, #6190 ) ;
#14048 = PLANE ( 'NONE',  #76076 ) ;
#14049 = DIRECTION ( 'NONE',  ( 0.000000000000000000, 0.000000000000000000, 1.000000000000000000 ) ) ;
#14050 = CARTESIAN_POINT ( 'NONE',  ( 99.34779341711927714, -29.80408710710938891, 231.7565776568629587 ) ) ;
#14051 = DIRECTION ( 'NONE',  ( 0.9242245927363033076, 0.3818493186865917766, 0.000000000000000000 ) ) ;
#14052 = CARTESIAN_POINT ( 'NONE',  ( 112.9545114599701492, -28.19305977888952697, 85.60800622829195561 ) ) ;
#14053 = CYLINDRICAL_SURFACE ( 'NONE', #16826, 190.5000000000000000 ) ;
#14054 = CARTESIAN_POINT ( 'NONE',  ( 97.53183037146393985, -39.74891120937812872, 22.57051295153732440 ) ) ;
#14055 = ORIENTED_EDGE ( 'NONE', *, *, #59325, .F. ) ;
#14056 = DIRECTION ( 'NONE',  ( 0.000000000000000000, -1.000000000000000000, 0.000000000000000000 ) ) ;
#14057 = ORIENTED_EDGE ( 'NONE', *, *, #71275, .F. ) ;
#14058 = EDGE_LOOP ( 'NONE', ( #70968, #6189, #41636, #19399 ) ) ;
#14059 = CARTESIAN_POINT ( 'NONE',  ( -92.32962665258561685, 82.96450994655479860, 74.36911441044702542 ) ) ;
#14060 = CARTESIAN_POINT ( 'NONE',  ( 106.0694874169909809, -45.56507127853855366, 278.9187261630399917 ) ) ;
#14061 = CARTESIAN_POINT ( 'NONE',  ( 97.81170999939396893, -40.51745679428447744, 191.6351607553995393 ) ) ;
#14062 = CARTESIAN_POINT ( 'NONE',  ( 97.81315821180474757, -40.51681016098617505, 66.63608906629065132 ) ) ;
#14063 = EDGE_CURVE ( 'NONE', #36866, #13081, #57339, .T. ) ;
#14064 = CARTESIAN_POINT ( 'NONE',  ( 97.07207206230401653, -35.37844117569200364, 86.21895860738254669 ) ) ;
#14065 = CARTESIAN_POINT ( 'NONE',  ( 79.76251016565943530, 71.15456258041353976, -87.71317827224403629 ) ) ;
#14066 = ORIENTED_EDGE ( 'NONE', *, *, #38915, .T. ) ;
#14067 = CARTESIAN_POINT ( 'NONE',  ( 80.06648329127399677, -8.350947159940998787, 4.925625275911999168 ) ) ;
#14068 = CARTESIAN_POINT ( 'NONE',  ( 115.0356694214038242, -42.91047690283549798, 184.3026665754189821 ) ) ;
#14069 = ORIENTED_EDGE ( 'NONE', *, *, #65061, .F. ) ;
#14070 = CARTESIAN_POINT ( 'NONE',  ( 112.9632928630424402, -28.13208318394687524, 44.59848241876795782 ) ) ;
#14071 = ORIENTED_EDGE ( 'NONE', *, *, #86810, .F. ) ;
#14072 = CARTESIAN_POINT ( 'NONE',  ( 114.1709767417603132, -32.67596046159766132, 287.0566617981627360 ) ) ;
#14073 = DIRECTION ( 'NONE',  ( 0.000000000000000000, -1.000000000000000000, 0.000000000000000000 ) ) ;
#14074 = CARTESIAN_POINT ( 'NONE',  ( 97.26456095925928480, -36.24355304347522377, 171.2870538473399620 ) ) ;
#14075 = LINE ( 'NONE', #63573, #43318 ) ;
#14076 = AXIS2_PLACEMENT_3D ( 'NONE', #42055, #76597, #288 ) ;
#14077 = DIRECTION ( 'NONE',  ( 0.000000000000000000, 0.000000000000000000, 1.000000000000000000 ) ) ;
#14078 = DIRECTION ( 'NONE',  ( 0.000000000000000000, -1.000000000000000000, 0.000000000000000000 ) ) ;
#14079 = AXIS2_PLACEMENT_3D ( 'NONE', #9412, #8981, #21713 ) ;
#14080 = CARTESIAN_POINT ( 'NONE',  ( 8.223282282254929854, 72.86292289192388694, 130.2970040361317103 ) ) ;
#14081 = CARTESIAN_POINT ( 'NONE',  ( 116.6456181429820447, -40.95237922671789477, 249.4956252759109532 ) ) ;
#14082 = CARTESIAN_POINT ( 'NONE',  ( 74.62309654709210349, 85.43299024555683729, -92.12450916458674044 ) ) ;
#14083 = VERTEX_POINT ( 'NONE', #19316 ) ;
#14084 = DIRECTION ( 'NONE',  ( 0.000000000000000000, 0.000000000000000000, 1.000000000000000000 ) ) ;
#14085 = VECTOR ( 'NONE', #47746, 1000.000000000000000 ) ;
#14086 = ORIENTED_EDGE ( 'NONE', *, *, #85955, .T. ) ;
#14087 = CARTESIAN_POINT ( 'NONE',  ( 102.2824096876565108, -27.37794169069978523, 116.4527681330539650 ) ) ;
#14089 = EDGE_CURVE ( 'NONE', #19776, #89932, #70505, .T. ) ;
#14088 = AXIS2_PLACEMENT_3D ( 'NONE', #28592, #55827, #77209 ) ;
#14090 = DIRECTION ( 'NONE',  ( 1.000000000000000000, 0.000000000000000000, 0.000000000000000000 ) ) ;
#14091 = CIRCLE ( 'NONE', #64867, 3.500000000000003109 ) ;
#14092 = B_SPLINE_CURVE_WITH_KNOTS ( 'NONE', 3,
 ( #31741, #11296, #53498, #38999, #60329, #66708, #87169, #24935, #24496, #18558, #39453, #17676, #87609, #73976, #25829, #24055, #4495, #3161 ),
 .UNSPECIFIED., .F., .F.,
 ( 4, 2, 2, 2, 2, 2, 2, 2, 4 ),
 ( 0.000000000000000000, 0.06250000026632723804, 0.1250000005326544761, 0.1875000007989817141, 0.2500000010653089522, 0.3125000013316361902, 0.3750000015979634282, 0.4375000018642906663, 0.5000000021306179043 ),
 .UNSPECIFIED. ) ;
#14093 = ORIENTED_EDGE ( 'NONE', *, *, #15043, .F. ) ;
#14094 = ORIENTED_EDGE ( 'NONE', *, *, #86196, .T. ) ;
#14095 = VERTEX_POINT ( 'NONE', #61089 ) ;
#14096 = EDGE_CURVE ( 'NONE', #26687, #29557, #89376, .T. ) ;
#14097 = CARTESIAN_POINT ( 'NONE',  ( 98.34986732099139317, -31.65657060954530522, 266.9064573084277754 ) ) ;
#14098 = DIRECTION ( 'NONE',  ( 0.000000000000000000, -0.5000000000000007772, 0.8660254037844381525 ) ) ;
#14099 = CYLINDRICAL_SURFACE ( 'NONE', #74161, 3.250000000000002665 ) ;
#14100 = CARTESIAN_POINT ( 'NONE',  ( 77.06670390244703128, -118.2784471599409812, 51.21780685541800437 ) ) ;
#14101 = CARTESIAN_POINT ( 'NONE',  ( 100.8299159177638984, -43.59960581930123880, 154.8080903695919801 ) ) ;
#14102 = CARTESIAN_POINT ( 'NONE',  ( 105.7736751693905148, -26.36287077168075754, 266.1756252759109884 ) ) ;
#14103 = EDGE_CURVE ( 'NONE', #34773, #15887, #87936, .T. ) ;
#14104 = CARTESIAN_POINT ( 'NONE',  ( 97.92328980544225203, -40.78083263938301428, 57.65839077251143863 ) ) ;
#14105 = EDGE_LOOP ( 'NONE', ( #29053, #48716, #25942, #87535 ) ) ;
#14106 = CARTESIAN_POINT ( 'NONE',  ( 177.0664832912730162, 12.92155284005730387, 361.9756252759109998 ) ) ;
#14107 = EDGE_CURVE ( 'NONE', #41873, #2797, #18406, .T. ) ;
#14108 = AXIS2_PLACEMENT_3D ( 'NONE', #20217, #34273, #61087 ) ;
#14109 = CIRCLE ( 'NONE', #21306, 0.5000000000000104361 ) ;
#14110 = CYLINDRICAL_SURFACE ( 'NONE', #17173, 2.517500000000005844 ) ;
#14111 = VERTEX_POINT ( 'NONE', #88817 ) ;
#14112 = ORIENTED_EDGE ( 'NONE', *, *, #84101, .F. ) ;
#14113 = EDGE_CURVE ( 'NONE', #68597, #84959, #32812, .T. ) ;
#14114 = CARTESIAN_POINT ( 'NONE',  ( 123.6837132603318992, -50.04645651782490745, 239.5838068554164693 ) ) ;
#14115 = LINE ( 'NONE', #54963, #20819 ) ;
#14116 = CARTESIAN_POINT ( 'NONE',  ( -0.8390482630167189759, 69.85000000000000853, -130.5560000000000400 ) ) ;
#14117 = EDGE_CURVE ( 'NONE', #63602, #58568, #76331, .T. ) ;
#14118 = DIRECTION ( 'NONE',  ( -0.7071067811865475727, 0.7071067811865475727, 0.000000000000000000 ) ) ;
#14119 = LINE ( 'NONE', #34550, #64915 ) ;
#14120 = CARTESIAN_POINT ( 'NONE',  ( 100.1837753934783990, -31.62254652264567767, 180.2409912566479591 ) ) ;
#14121 = CARTESIAN_POINT ( 'NONE',  ( 99.26081945853924537, -43.75962541195023903, 56.90991099019593236 ) ) ;
#14122 = ORIENTED_EDGE ( 'NONE', *, *, #5605, .F. ) ;
#14123 = LINE ( 'NONE', #47722, #61152 ) ;
#14124 = ORIENTED_EDGE ( 'NONE', *, *, #4379, .T. ) ;
#14125 = CARTESIAN_POINT ( 'NONE',  ( -75.68572508987513459, 76.20320268897033600, -91.25368348339026170 ) ) ;
#14127 = VERTEX_POINT ( 'NONE', #25673 ) ;
#14126 = ADVANCED_FACE ( 'NONE', ( #68365 ), #6145, .F. ) ;
#14128 = CARTESIAN_POINT ( 'NONE',  ( 107.0667039024470313, -104.2784471599414502, 0.2178068554180012661 ) ) ;
#14129 = VERTEX_POINT ( 'NONE', #89261 ) ;
#14130 = DIRECTION ( 'NONE',  ( 0.000000000000000000, 0.000000000000000000, 1.000000000000000000 ) ) ;
#14131 = CARTESIAN_POINT ( 'NONE',  ( 193.0371591254584587, -47.82818131005411999, 237.4678068554150059 ) ) ;
#14132 = CARTESIAN_POINT ( 'NONE',  ( 68.24424899846859205, -67.86899452490857243, 247.3945403487729777 ) ) ;
#14133 = VECTOR ( 'NONE', #64752, 1000.000000000000000 ) ;
#14134 = DIRECTION ( 'NONE',  ( 0.7071067811739274456, -0.7071067811991676999, 0.000000000000000000 ) ) ;
#14135 = VERTEX_POINT ( 'NONE', #40187 ) ;
#14136 = CARTESIAN_POINT ( 'NONE',  ( 116.2511270133230283, -31.75062363771698770, 69.22133956162495849 ) ) ;
#14138 = CARTESIAN_POINT ( 'NONE',  ( 97.62852612868790914, 72.47310549519059464, -86.68128281353502018 ) ) ;
#14137 = DIRECTION ( 'NONE',  ( 0.000000000000000000, 1.000000000000000000, 0.000000000000000000 ) ) ;
#14139 = DIRECTION ( 'NONE',  ( 0.7071067811989784069, -0.7071067811741166276, 7.071067811989480323E-16 ) ) ;
#14140 = DIRECTION ( 'NONE',  ( 1.000000000000000078E-15, -1.000000000000000083E-30, -1.000000000000000000 ) ) ;
#14141 = ORIENTED_EDGE ( 'NONE', *, *, #19561, .T. ) ;
#14142 = EDGE_CURVE ( 'NONE', #88900, #48200, #37177, .T. ) ;
#14143 = LINE ( 'NONE', #9130, #51793 ) ;
#14144 = EDGE_CURVE ( 'NONE', #21144, #55523, #75631, .T. ) ;
#14145 = ADVANCED_FACE ( 'NONE', ( #13400 ), #87466, .T. ) ;
#14146 = PLANE ( 'NONE',  #42882 ) ;
#14147 = CARTESIAN_POINT ( 'NONE',  ( 11.41378189430731993, 76.91903266065129685, 118.0057337156638653 ) ) ;
#14148 = EDGE_LOOP ( 'NONE', ( #14951, #87998, #56877, #40889 ) ) ;
#14149 = CARTESIAN_POINT ( 'NONE',  ( 96.67756931115832231, -37.82841265861588909, 122.4099109901969626 ) ) ;
#14150 = EDGE_CURVE ( 'NONE', #12139, #71132, #75864, .T. ) ;
#14151 = VECTOR ( 'NONE', #31179, 1000.000000000000000 ) ;
#14153 = CYLINDRICAL_SURFACE ( 'NONE', #42726, 1.000000000000000888 ) ;
#14152 = LINE ( 'NONE', #41386, #37746 ) ;
#14154 = CARTESIAN_POINT ( 'NONE',  ( 107.0664832912739541, -21.02944715994095759, 311.3356252759109566 ) ) ;
#14155 = VECTOR ( 'NONE', #45401, 1000.000000000000000 ) ;
#14156 = CIRCLE ( 'NONE', #64924, 3.000000000000002665 ) ;
#14157 = CARTESIAN_POINT ( 'NONE',  ( 127.3855721265797456, -122.7922957798182324, 250.2191008560389776 ) ) ;
#14158 = ORIENTED_EDGE ( 'NONE', *, *, #25443, .F. ) ;
#14159 = CARTESIAN_POINT ( 'NONE',  ( 103.6907823165633289, -45.90921117331522083, 138.2956252759109645 ) ) ;
#14161 = ORIENTED_EDGE ( 'NONE', *, *, #32658, .F. ) ;
#14160 = CARTESIAN_POINT ( 'NONE',  ( 97.81168895331838087, -40.51742574516882200, 287.6356252759109680 ) ) ;
#14162 = CARTESIAN_POINT ( 'NONE',  ( 101.0991643652557599, -45.25116564454916102, 278.0899109901965858 ) ) ;
#14163 = DIRECTION ( 'NONE',  ( -1.000000000000000000, 0.000000000000000000, -2.108231265501709878E-16 ) ) ;
#14164 = PLANE ( 'NONE',  #30127 ) ;
#14165 = CARTESIAN_POINT ( 'NONE',  ( 86.72755763596092038, -85.76982405743865456, 250.2178068554179902 ) ) ;
#14166 = DIRECTION ( 'NONE',  ( 0.7071067811866279529, -0.7071067811864671926, 7.071067811866286874E-16 ) ) ;
#14167 = AXIS2_PLACEMENT_3D ( 'NONE', #53054, #88079, #46253 ) ;
#14168 = CARTESIAN_POINT ( 'NONE',  ( 46.83715912545430626, -47.82818131006082751, 237.4678068554150059 ) ) ;
#14169 = LINE ( 'NONE', #20094, #52937 ) ;
#14170 = AXIS2_PLACEMENT_3D ( 'NONE', #59953, #12732, #87686 ) ;
#14172 = CARTESIAN_POINT ( 'NONE',  ( 100.4443968677459083, -27.79860430499261881, 185.5841967044829630 ) ) ;
#14171 = CIRCLE ( 'NONE', #28626, 3.174999999999983391 ) ;
#14173 = VERTEX_POINT ( 'NONE', #83338 ) ;
#14174 = ORIENTED_EDGE ( 'NONE', *, *, #21162, .T. ) ;
#14175 = CARTESIAN_POINT ( 'NONE',  ( 115.8726827828676704, -31.83848043880258061, 175.6615833058969827 ) ) ;
#14176 = VECTOR ( 'NONE', #77287, 1000.000000000000000 ) ;
#14177 = DIRECTION ( 'NONE',  ( -1.000000000000000000, -5.512527431108013646E-15, 0.000000000000000000 ) ) ;
#14178 = CARTESIAN_POINT ( 'NONE',  ( 97.51798391995397708, -31.03399779358258215, 276.8984824187675713 ) ) ;
#14179 = DIRECTION ( 'NONE',  ( 1.000000000000000078E-15, 1.000000000000000083E-30, -1.000000000000000000 ) ) ;
#14180 = CARTESIAN_POINT ( 'NONE',  ( 113.1775979644639278, -44.75238856601268367, 268.0940785184301944 ) ) ;
#14181 = DIRECTION ( 'NONE',  ( 0.2588190451025229599, 0.000000000000000000, 0.9659258262890676461 ) ) ;
#14182 = CARTESIAN_POINT ( 'NONE',  ( 116.3212776292292716, -32.94146857471233147, 105.1356252759109680 ) ) ;
#14183 = DIRECTION ( 'NONE',  ( 4.299999999999999979E-14, -1.000000000000000000, 4.400000000000000367E-29 ) ) ;
#14184 = B_SPLINE_CURVE_WITH_KNOTS ( 'NONE', 3,
 ( #21054, #19704, #61926, #89657, #88321, #33779, #82850, #13786, #53744, #12448, #33335, #54193, #55534, #41472, #32880, #6091, #81513, #76462, #39690, #34669, #62375, #83288, #40135, #47388, #19266, #68309, #67393, #75120, #46940 ),
 .UNSPECIFIED., .F., .F.,
 ( 4, 2, 2, 2, 2, 2, 2, 2, 2, 2, 1, 1, 1, 1, 1, 2, 4 ),
 ( 0.000000000000000000, 0.06250185527508492211, 0.1250037105501698442, 0.1875055658252547663, 0.2500074211003396885, 0.3125092763754245828, 0.3750111316505095327, 0.4375129869255944826, 0.4687639145631368187, 0.4843893783819079868, 0.4922021102912934598, 0.4961084762459861408, 0.4980616592233322870, 0.4990382507120053046, 0.4995265464563418689, 0.4997706943285100678, 0.5000148422006782667 ),
 .UNSPECIFIED. ) ;
#14185 = CARTESIAN_POINT ( 'NONE',  ( 100.6510976905701824, -26.79511100149714764, 220.5327681330539633 ) ) ;
#14186 = ORIENTED_EDGE ( 'NONE', *, *, #23186, .T. ) ;
#14187 = ORIENTED_EDGE ( 'NONE', *, *, #55005, .T. ) ;
#14188 = CARTESIAN_POINT ( 'NONE',  ( 41.56648329127499153, -32.07844715994070839, 74.17562527591199739 ) ) ;
#14189 = CARTESIAN_POINT ( 'NONE',  ( -74.44936585838399878, 84.21376545118704371, -92.26493792250069248 ) ) ;
#14190 = DIRECTION ( 'NONE',  ( 0.000000000000000000, 0.000000000000000000, -1.000000000000000000 ) ) ;
#14191 = DIRECTION ( 'NONE',  ( 0.000000000000000000, 0.000000000000000000, 1.000000000000000000 ) ) ;
#14192 = AXIS2_PLACEMENT_3D ( 'NONE', #66691, #46682, #4478 ) ;
#14193 = AXIS2_PLACEMENT_3D ( 'NONE', #64934, #56764, #1825 ) ;
#14194 = CARTESIAN_POINT ( 'NONE',  ( -487.2989999999999782, 89.53805401447691281, 18.25625000000039933 ) ) ;
#14195 = EDGE_LOOP ( 'NONE', ( #60445, #33314, #41552, #62789 ) ) ;
#14196 = DIRECTION ( 'NONE',  ( 0.000000000000000000, 1.000000000000000000, 0.000000000000000000 ) ) ;
#14197 = CARTESIAN_POINT ( 'NONE',  ( 106.2268934648462420, -47.75097955688366369, 267.5280062282920994 ) ) ;
#14198 = EDGE_CURVE ( 'NONE', #19079, #33965, #28407, .T. ) ;
#14199 = ORIENTED_EDGE ( 'NONE', *, *, #13488, .F. ) ;
#14200 = EDGE_CURVE ( 'NONE', #75737, #77463, #36078, .T. ) ;
#14201 = CARTESIAN_POINT ( 'NONE',  ( 77.43469508765247156, -37.52719034724768932, 6.916533740478608472 ) ) ;
#14202 = DIRECTION ( 'NONE',  ( 0.000000000000000000, 0.000000000000000000, -1.000000000000000000 ) ) ;
#14203 = DIRECTION ( 'NONE',  ( 0.000000000000000000, 0.000000000000000000, -1.000000000000000000 ) ) ;
#14204 = CARTESIAN_POINT ( 'NONE',  ( 105.2602129278706400, -44.68979347096200883, 70.21666179816293152 ) ) ;
#14205 = CARTESIAN_POINT ( 'NONE',  ( 99.99340640592768636, -27.19037833420660277, 181.5841967044829630 ) ) ;
#14206 = EDGE_CURVE ( 'NONE', #40315, #14995, #55588, .T. ) ;
#14207 = CARTESIAN_POINT ( 'NONE',  ( 36.65249034007535300, -49.32844715994124130, 249.9678068554150343 ) ) ;
#14208 = VERTEX_POINT ( 'NONE', #56505 ) ;
#14209 = EDGE_CURVE ( 'NONE', #13373, #85180, #53078, .T. ) ;
#14210 = VECTOR ( 'NONE', #46712, 1000.000000000000000 ) ;
#14211 = LINE ( 'NONE', #62790, #36423 ) ;
#14212 = ORIENTED_EDGE ( 'NONE', *, *, #85904, .T. ) ;
#14213 = EDGE_LOOP ( 'NONE', ( #20466, #87746 ) ) ;
#14214 = EDGE_CURVE ( 'NONE', #72016, #25675, #56954, .T. ) ;
#14215 = VECTOR ( 'NONE', #63073, 1000.000000000000000 ) ;
#14216 = AXIS2_PLACEMENT_3D ( 'NONE', #80490, #73658, #9650 ) ;
#14217 = FACE_OUTER_BOUND ( 'NONE', #34020, .T. ) ;
#14218 = ORIENTED_EDGE ( 'NONE', *, *, #47383, .F. ) ;
#14219 = EDGE_LOOP ( 'NONE', ( #27452, #71069, #70419, #4770 ) ) ;
#14220 = DIRECTION ( 'NONE',  ( 0.000000000000000000, 0.000000000000000000, -1.000000000000000000 ) ) ;
#14221 = EDGE_CURVE ( 'NONE', #22206, #12340, #74844, .T. ) ;
#14222 = CARTESIAN_POINT ( 'NONE',  ( 115.9223471279375843, -38.62321220144315248, 108.0933722090289564 ) ) ;
#14223 = CARTESIAN_POINT ( 'NONE',  ( 98.01753632367962155, -44.42038823906860756, 226.8870538473399563 ) ) ;
#14224 = CIRCLE ( 'NONE', #76609, 32.50000000000000711 ) ;
#14225 = CARTESIAN_POINT ( 'NONE',  ( 113.0129699484216133, -46.01939436189644539, 218.0175300378159591 ) ) ;
#14226 = CARTESIAN_POINT ( 'NONE',  ( 97.37192905580968727, -32.85904099757684804, 37.02419670448292521 ) ) ;
#14227 = CARTESIAN_POINT ( 'NONE',  ( -68.53801554307339927, 120.6499999999999915, -74.15067561874339219 ) ) ;
#14228 = FACE_OUTER_BOUND ( 'NONE', #85742, .T. ) ;
#14229 = EDGE_CURVE ( 'NONE', #60536, #75621, #15403, .T. ) ;
#14230 = CIRCLE ( 'NONE', #76613, 1.999999999999995781 ) ;
#14231 = ORIENTED_EDGE ( 'NONE', *, *, #88605, .F. ) ;
#14232 = CARTESIAN_POINT ( 'NONE',  ( 181.8884939055940038, -32.11662333284530746, 342.9256252759119548 ) ) ;
#14233 = VECTOR ( 'NONE', #35671, 1000.000000000000114 ) ;
#14234 = LINE ( 'NONE', #69642, #75362 ) ;
#14235 = LINE ( 'NONE', #69643, #9248 ) ;
#14236 = EDGE_CURVE ( 'NONE', #228, #43691, #71996, .T. ) ;
#14237 = CARTESIAN_POINT ( 'NONE',  ( 106.1376555893193228, -47.80867374849579221, 112.5099109901969712 ) ) ;
#14238 = CARTESIAN_POINT ( 'NONE',  ( 107.8717536863088640, -26.29114242999935769, 70.01562527591099183 ) ) ;
#14239 = CARTESIAN_POINT ( 'NONE',  ( 103.0736367338192139, -47.94042275923426644, 252.3041967044822798 ) ) ;
#14240 = ORIENTED_EDGE ( 'NONE', *, *, #16071, .T. ) ;
#14241 = CARTESIAN_POINT ( 'NONE',  ( 106.3019233867144351, -47.12668134090281313, 222.5184824187679453 ) ) ;
#14242 = DIRECTION ( 'NONE',  ( 0.04216478779797398074, -0.9991106698809455455, 0.000000000000000000 ) ) ;
#14243 = DIRECTION ( 'NONE',  ( 0.000000000000000000, 0.000000000000000000, 1.000000000000000000 ) ) ;
#14244 = CARTESIAN_POINT ( 'NONE',  ( 11.87295884493951625, 78.03960220850400731, 130.0150426351353588 ) ) ;
#14245 = PLANE ( 'NONE',  #19896 ) ;
#14247 = DIRECTION ( 'NONE',  ( 0.000000000000000000, 0.000000000000000000, -1.000000000000000000 ) ) ;
#14246 = DIRECTION ( 'NONE',  ( 0.7071067811865459074, 0.7071067811865491270, 7.071067811865459556E-16 ) ) ;
#14248 = PLANE ( 'NONE',  #30750 ) ;
#14249 = DIRECTION ( 'NONE',  ( 0.000000000000000000, 0.000000000000000000, -1.000000000000000000 ) ) ;
#14250 = DIRECTION ( 'NONE',  ( 0.000000000000000000, -0.000000000000000000, 1.000000000000000000 ) ) ;
#14251 = AXIS2_PLACEMENT_3D ( 'NONE', #29086, #56770, #23625 ) ;
#14252 = DIRECTION ( 'NONE',  ( 0.000000000000000000, 0.000000000000000000, 1.000000000000000000 ) ) ;
#14253 = CARTESIAN_POINT ( 'NONE',  ( 115.8196581495599986, -31.72004586281034477, 39.23976723453453275 ) ) ;
#14254 = CARTESIAN_POINT ( 'NONE',  ( 92.84710890992452903, -94.98933252893162660, -19.21044887263828471 ) ) ;
#14255 = EDGE_CURVE ( 'NONE', #76109, #24458, #22021, .T. ) ;
#14257 = ORIENTED_EDGE ( 'NONE', *, *, #41456, .T. ) ;
#14256 = CARTESIAN_POINT ( 'NONE',  ( 61.56670390244730839, -23.42844715994043980, 249.9678068554150343 ) ) ;
#14258 = CARTESIAN_POINT ( 'NONE',  ( 150.5667039024476139, -25.42844715993593852, 129.9678068554149775 ) ) ;
#14259 = CARTESIAN_POINT ( 'NONE',  ( 106.5662725644766908, -47.20027100765710060, 247.5384824187679556 ) ) ;
#14260 = CARTESIAN_POINT ( 'NONE',  ( 105.3162569294398168, -48.44961499074708655, 143.4584824187689662 ) ) ;
#14261 = CARTESIAN_POINT ( 'NONE',  ( 99.36487284946518628, -28.73678208742278173, 261.6746728949589169 ) ) ;
#14262 = EDGE_CURVE ( 'NONE', #52873, #75590, #36536, .T. ) ;
#14263 = DIRECTION ( 'NONE',  ( 1.000000000000000000, -9.073094938289460781E-13, 0.000000000000000000 ) ) ;
#14264 = AXIS2_PLACEMENT_3D ( 'NONE', #30946, #31829, #17325 ) ;
#14266 = CARTESIAN_POINT ( 'NONE',  ( 82.57621891718092400, -35.60488046388260841, 7.068409955837002379 ) ) ;
#14265 = CARTESIAN_POINT ( 'NONE',  ( 88.17226027475719263, -58.72944715994110254, 249.5838068554174924 ) ) ;
#14267 = CARTESIAN_POINT ( 'NONE',  ( 99.08975728047121834, -42.79576521077569851, 137.8439474464609589 ) ) ;
#14268 = VECTOR ( 'NONE', #19301, 1000.000000000000000 ) ;
#14269 = DIRECTION ( 'NONE',  ( 0.000000000000000000, 0.000000000000000000, 1.000000000000000000 ) ) ;
#14270 = ORIENTED_EDGE ( 'NONE', *, *, #63910, .F. ) ;
#14271 = CARTESIAN_POINT ( 'NONE',  ( 83.56670559755329464, -36.73837296219065252, 239.5838068554176914 ) ) ;
#14272 = ORIENTED_EDGE ( 'NONE', *, *, #81395, .F. ) ;
#14273 = CARTESIAN_POINT ( 'NONE',  ( 115.2610577610831655, -39.13882072599808026, 183.0209912566479602 ) ) ;
#14275 = ORIENTED_EDGE ( 'NONE', *, *, #56675, .F. ) ;
#14274 = CARTESIAN_POINT ( 'NONE',  ( 100.8864776678791344, -44.69940107073664848, 187.0527194606352168 ) ) ;
#14276 = DIRECTION ( 'NONE',  ( -0.9254794337955620787, -0.3787978585227822492, 0.000000000000000000 ) ) ;
#14277 = CARTESIAN_POINT ( 'NONE',  ( 112.4747680694540293, -26.21285726233897506, 165.6984824187679521 ) ) ;
#14278 = CARTESIAN_POINT ( 'NONE',  ( 24.79284581386643183, 184.0000000000000000, 85.23828826961327820 ) ) ;
#14279 = DIRECTION ( 'NONE',  ( -1.000000000000000078E-15, 0.000000000000000000, 1.000000000000000000 ) ) ;
#14280 = DIRECTION ( 'NONE',  ( -0.7071067812160263255, 0.7071067811570687089, -7.071067812160270681E-16 ) ) ;
#14281 = AXIS2_PLACEMENT_3D ( 'NONE', #73323, #24299, #51965 ) ;
#14282 = CARTESIAN_POINT ( 'NONE',  ( -89.55259891852560372, 73.00424585431356661, 77.69145367648832234 ) ) ;
#14283 = FACE_OUTER_BOUND ( 'NONE', #77955, .T. ) ;
#14284 = CARTESIAN_POINT ( 'NONE',  ( 112.9545114599701918, -28.19305977888944525, 89.60800622829296458 ) ) ;
#14285 = EDGE_LOOP ( 'NONE', ( #59879, #43495, #7838, #64131 ) ) ;
#14286 = ORIENTED_EDGE ( 'NONE', *, *, #30524, .F. ) ;
#14287 = VERTEX_POINT ( 'NONE', #16094 ) ;
#14288 = EDGE_CURVE ( 'NONE', #67926, #30523, #31042, .T. ) ;
#14289 = AXIS2_PLACEMENT_3D ( 'NONE', #5100, #73692, #46408 ) ;
#14290 = CARTESIAN_POINT ( 'NONE',  ( 98.75489364002905290, -33.65605228111792968, 62.47586902018298360 ) ) ;
#14291 = VECTOR ( 'NONE', #60704, 1000.000000000000000 ) ;
#14292 = CARTESIAN_POINT ( 'NONE',  ( 19.56670390244796920, -48.82844715994099971, 10.91780685541479734 ) ) ;
#14294 = DIRECTION ( 'NONE',  ( 0.000000000000000000, 0.8660254037844445918, -0.4999999999999897304 ) ) ;
#14293 = CARTESIAN_POINT ( 'NONE',  ( 114.4888877093245583, -29.48743791597858177, 190.4537205140059655 ) ) ;
#14295 = CARTESIAN_POINT ( 'NONE',  ( 97.81443832832722762, -40.51607714565724905, 56.63519146330476417 ) ) ;
#14296 = DIRECTION ( 'NONE',  ( 0.000000000000000000, 0.000000000000000000, -1.000000000000000000 ) ) ;
#14297 = CARTESIAN_POINT ( 'NONE',  ( 0.000000000000000000, 100.5999999999999659, 118.5560000000000116 ) ) ;
#14298 = VECTOR ( 'NONE', #8165, 999.9999999999998863 ) ;
#14299 = DIRECTION ( 'NONE',  ( 0.000000000000000000, 0.000000000000000000, 1.000000000000000000 ) ) ;
#14300 = CARTESIAN_POINT ( 'NONE',  ( 71.24189083761808661, -0.9290567490904538817, 542.9756252759101471 ) ) ;
#14301 = CARTESIAN_POINT ( 'NONE',  ( 112.1095002620001821, -47.42599740258513208, 137.9270538473389820 ) ) ;
#14302 = ORIENTED_EDGE ( 'NONE', *, *, #5852, .F. ) ;
#14303 = ORIENTED_EDGE ( 'NONE', *, *, #33517, .F. ) ;
#14304 = ORIENTED_EDGE ( 'NONE', *, *, #89055, .T. ) ;
#14305 = AXIS2_PLACEMENT_3D ( 'NONE', #46981, #81562, #74720 ) ;
#14306 = CARTESIAN_POINT ( 'NONE',  ( 8.398107354775891764, 72.98722500879387098, 130.2869324835649536 ) ) ;
#14307 = CARTESIAN_POINT ( 'NONE',  ( -98.64044413062988781, 91.23859726994547259, -85.52787878288694401 ) ) ;
#14308 = LINE ( 'NONE', #7928, #46779 ) ;
#14309 = CARTESIAN_POINT ( 'NONE',  ( 103.6346955097220643, -29.32319583828803999, 178.2395189410199805 ) ) ;
#14310 = EDGE_CURVE ( 'NONE', #27454, #17964, #63235, .T. ) ;
#14311 = FACE_OUTER_BOUND ( 'NONE', #10241, .T. ) ;
#14312 = EDGE_CURVE ( 'NONE', #24458, #77970, #43774, .T. ) ;
#14313 = EDGE_CURVE ( 'NONE', #80899, #18726, #82127, .T. ) ;
#14314 = FACE_OUTER_BOUND ( 'NONE', #346, .T. ) ;
#14315 = VERTEX_POINT ( 'NONE', #15644 ) ;
#14317 = ORIENTED_EDGE ( 'NONE', *, *, #46579, .T. ) ;
#14316 = ORIENTED_EDGE ( 'NONE', *, *, #24868, .T. ) ;
#14318 = VECTOR ( 'NONE', #69414, 1000.000000000000000 ) ;
#14319 = EDGE_CURVE ( 'NONE', #17076, #76315, #86914, .T. ) ;
#14320 = CARTESIAN_POINT ( 'NONE',  ( 107.0667039024470313, -104.2784471599420755, -19.78219314458201694 ) ) ;
#14321 = ORIENTED_EDGE ( 'NONE', *, *, #16459, .T. ) ;
#14322 = VERTEX_POINT ( 'NONE', #86476 ) ;
#14323 = DIRECTION ( 'NONE',  ( 1.000000000000000000, 0.000000000000000000, 0.000000000000000000 ) ) ;
#14324 = CARTESIAN_POINT ( 'NONE',  ( 98.91186986371705814, -40.27407823153063759, 228.0844404487539805 ) ) ;
#14325 = LINE ( 'NONE', #7503, #12069 ) ;
#14326 = ORIENTED_EDGE ( 'NONE', *, *, #59416, .T. ) ;
#14327 = CARTESIAN_POINT ( 'NONE',  ( 3.174999999999889688, 8.255000000000000782, -31.75000000000000000 ) ) ;
#14328 = CIRCLE ( 'NONE', #82559, 1.000000000000003775 ) ;
#14329 = CARTESIAN_POINT ( 'NONE',  ( -114.7490242460955159, 71.13177641138574359, 62.26986715482768631 ) ) ;
#14330 = ORIENTED_EDGE ( 'NONE', *, *, #41970, .T. ) ;
#14331 = ORIENTED_EDGE ( 'NONE', *, *, #29872, .F. ) ;
#14332 = EDGE_CURVE ( 'NONE', #47179, #87166, #31477, .T. ) ;
#14333 = CARTESIAN_POINT ( 'NONE',  ( 107.0664832912749915, -36.72944715993903486, 25.56312527591096995 ) ) ;
#14334 = ORIENTED_EDGE ( 'NONE', *, *, #1089, .F. ) ;
#14335 = ORIENTED_EDGE ( 'NONE', *, *, #30920, .F. ) ;
#14336 = EDGE_CURVE ( 'NONE', #69712, #32370, #37869, .T. ) ;
#14337 = CARTESIAN_POINT ( 'NONE',  ( 99.66640463149437323, -40.17452507577532117, 254.4909475124484857 ) ) ;
#14338 = CARTESIAN_POINT ( 'NONE',  ( 117.6304226258691727, -33.39798698885631012, 129.0575300378159795 ) ) ;
#14339 = CARTESIAN_POINT ( 'NONE',  ( 103.3702027031294506, -47.12181610991865455, 102.3165776568629752 ) ) ;
#14340 = CARTESIAN_POINT ( 'NONE',  ( 164.7830935719630361, -29.99615139349950965, -5.074374724088000832 ) ) ;
#14341 = PLANE ( 'NONE',  #37977 ) ;
#14342 = CARTESIAN_POINT ( 'NONE',  ( 96.77275252345162926, -34.86922145964237529, 237.1841967044819626 ) ) ;
#14343 = DIRECTION ( 'NONE',  ( 0.000000000000000000, 0.000000000000000000, -1.000000000000000000 ) ) ;
#14344 = DIRECTION ( 'NONE',  ( 2.900000000000000265E-14, -2.000000000000000155E-15, 1.000000000000000000 ) ) ;
#14345 = ORIENTED_EDGE ( 'NONE', *, *, #49820, .T. ) ;
#14346 = CARTESIAN_POINT ( 'NONE',  ( 130.5246120830809957, 70.17656663518269511, -2.891956274606212407 ) ) ;
#14347 = EDGE_LOOP ( 'NONE', ( #67237, #34461, #37117, #41499 ) ) ;
#14348 = EDGE_CURVE ( 'NONE', #77176, #19859, #86034, .T. ) ;
#14349 = VECTOR ( 'NONE', #36921, 1000.000000000000000 ) ;
#14350 = ORIENTED_EDGE ( 'NONE', *, *, #74881, .F. ) ;
#14351 = DIRECTION ( 'NONE',  ( -0.4999999999999998890, -0.8660254037844387076, 0.000000000000000000 ) ) ;
#14352 = AXIS2_PLACEMENT_3D ( 'NONE', #28215, #70018, #66764 ) ;
#14353 = CARTESIAN_POINT ( 'NONE',  ( 98.34965401982358912, -31.65695195725486855, 136.9064172575153862 ) ) ;
#14354 = AXIS2_PLACEMENT_3D ( 'NONE', #68709, #34168, #70052 ) ;
#14355 = ORIENTED_EDGE ( 'NONE', *, *, #48232, .F. ) ;
#14356 = CARTESIAN_POINT ( 'NONE',  ( 117.2223540064780991, -42.83671953415140621, 128.3956252759109873 ) ) ;
#14357 = LINE ( 'NONE', #36133, #39843 ) ;
#14358 = DIRECTION ( 'NONE',  ( 0.000000000000000000, -1.000000000000000000, 0.000000000000000000 ) ) ;
#14359 = FACE_OUTER_BOUND ( 'NONE', #5325, .T. ) ;
#14362 = CARTESIAN_POINT ( 'NONE',  ( 99.76842024043818924, -29.31547782932927859, 221.6956252759109702 ) ) ;
#14361 = DIRECTION ( 'NONE',  ( 0.000000000000000000, 0.000000000000000000, -1.000000000000000000 ) ) ;
#14360 = CARTESIAN_POINT ( 'NONE',  ( 34.67381068360400320, -28.98061976758901892, 237.4678068554150059 ) ) ;
#14363 = DIRECTION ( 'NONE',  ( 0.000000000000000000, 0.000000000000000000, 1.000000000000000000 ) ) ;
#14365 = FACE_OUTER_BOUND ( 'NONE', #27570, .T. ) ;
#14364 = APPLICATION_CONTEXT ( 'automotive_design' ) ;
#14366 = ORIENTED_EDGE ( 'NONE', *, *, #11144, .T. ) ;
#14367 = DIRECTION ( 'NONE',  ( -0.000000000000000000, -0.000000000000000000, -1.000000000000000000 ) ) ;
#14368 = CIRCLE ( 'NONE', #86848, 20.63750000000000284 ) ;
#14369 = LINE ( 'NONE', #84317, #34090 ) ;
#14370 = PLANE ( 'NONE',  #83610 ) ;
#14371 = DIRECTION ( 'NONE',  ( 0.000000000000000000, 0.000000000000000000, -1.000000000000000000 ) ) ;
#14373 = ORIENTED_EDGE ( 'NONE', *, *, #58591, .F. ) ;
#14372 = CARTESIAN_POINT ( 'NONE',  ( 106.2233489284451338, -47.79750968570053971, 267.5280062282920994 ) ) ;
#14374 = LINE ( 'NONE', #22986, #29259 ) ;
#14375 = CARTESIAN_POINT ( 'NONE',  ( 114.5434305778746733, -28.56033675696621899, 154.4746728949589851 ) ) ;
#14376 = CARTESIAN_POINT ( 'NONE',  ( 97.80922128671791427, -29.33095300656633597, 41.78991099019596334 ) ) ;
#14377 = CARTESIAN_POINT ( 'NONE',  ( 98.63080892621665896, -30.47026088752560824, 176.8184824187679567 ) ) ;
#14378 = DIRECTION ( 'NONE',  ( -3.100000000000000258E-29, 3.100000000000000044E-14, 1.000000000000000000 ) ) ;
#14379 = AXIS2_PLACEMENT_3D ( 'NONE', #88435, #27535, #20291 ) ;
#14380 = ADVANCED_FACE ( 'NONE', ( #24678, #79666 ), #30603, .T. ) ;
#14381 = CARTESIAN_POINT ( 'NONE',  ( 97.53181802940885348, -39.74887296861906805, 102.5705099596000593 ) ) ;
#14383 = CARTESIAN_POINT ( 'NONE',  ( 19.56670390244740076, -47.82844715994204421, 180.4678068554150911 ) ) ;
#14382 = DIRECTION ( 'NONE',  ( 1.000000000000000078E-15, -1.000000000000000083E-30, -1.000000000000000000 ) ) ;
#14384 = CARTESIAN_POINT ( 'NONE',  ( 4.665904304751416087E-15, 44.45000000000000284, -38.10000000000000142 ) ) ;
#14385 = CARTESIAN_POINT ( 'NONE',  ( 130.0664832912740110, -18.82844715994099971, 226.9256252759120116 ) ) ;
#14386 = EDGE_LOOP ( 'NONE', ( #71538, #47212, #12973, #39532 ) ) ;
#14387 = DIRECTION ( 'NONE',  ( 1.000000000000000000, -0.000000000000000000, -0.000000000000000000 ) ) ;
#14388 = ORIENTED_EDGE ( 'NONE', *, *, #39819, .F. ) ;
#14389 = ORIENTED_EDGE ( 'NONE', *, *, #12488, .T. ) ;
#14390 = VECTOR ( 'NONE', #35895, 1000.000000000000000 ) ;
#14391 = ORIENTED_EDGE ( 'NONE', *, *, #38001, .T. ) ;
#14392 = CARTESIAN_POINT ( 'NONE',  ( 117.4257108620837329, -37.68603989742253191, 74.75276813305397638 ) ) ;
#14393 = CARTESIAN_POINT ( 'NONE',  ( 0.000000000000000000, 44.45000000000000284, 0.000000000000000000 ) ) ;
#14394 = DIRECTION ( 'NONE',  ( 1.000000000000000000, 3.999999999999999995E-14, 1.000000000000000078E-15 ) ) ;
#14395 = EDGE_CURVE ( 'NONE', #1129, #44353, #881, .T. ) ;
#14396 = CARTESIAN_POINT ( 'NONE',  ( 96.57517526037739231, -36.20937929227457630, 167.2870538473399620 ) ) ;
#14397 = CARTESIAN_POINT ( 'NONE',  ( 112.5471327968798221, -30.46552556802231138, 288.9257531614101708 ) ) ;
#14398 = EDGE_LOOP ( 'NONE', ( #74465, #24288, #47089, #35873 ) ) ;
#14399 = CIRCLE ( 'NONE', #89870, 2.500000000000002220 ) ;
#14400 = ORIENTED_EDGE ( 'NONE', *, *, #38917, .F. ) ;
#14401 = VERTEX_POINT ( 'NONE', #78330 ) ;
#14402 = ADVANCED_FACE ( 'NONE', ( #39194 ), #5126, .T. ) ;
#14403 = ORIENTED_EDGE ( 'NONE', *, *, #65601, .T. ) ;
#14404 = CARTESIAN_POINT ( 'NONE',  ( -89.60916260784479448, 223.9999999999999716, 134.1927865330827103 ) ) ;
#14405 = DIRECTION ( 'NONE',  ( 0.000000000000000000, 0.000000000000000000, -1.000000000000000000 ) ) ;
#14406 = CARTESIAN_POINT ( 'NONE',  ( 99.09555428360187079, -30.55063820098889593, 161.8023122570933765 ) ) ;
#14407 = CARTESIAN_POINT ( 'NONE',  ( 97.33795622581291695, -34.07061224223205897, 21.11392868892265540 ) ) ;
#14408 = CARTESIAN_POINT ( 'NONE',  ( 99.17062120112595380, 90.28418055714728041, 84.91247172076124627 ) ) ;
#14409 = DIRECTION ( 'NONE',  ( 0.000000000000000000, 0.000000000000000000, 1.000000000000000000 ) ) ;
#14410 = CARTESIAN_POINT ( 'NONE',  ( 33.96670390244699433, -26.71338133339301635, -5.074374724088000832 ) ) ;
#14411 = CYLINDRICAL_SURFACE ( 'NONE', #52885, 6.350000000000659561 ) ;
#14412 = LINE ( 'NONE', #83443, #63726 ) ;
#14413 = CARTESIAN_POINT ( 'NONE',  ( 99.16013801855501697, -43.49098322490566204, 31.88991099019594699 ) ) ;
#14414 = DIRECTION ( 'NONE',  ( -3.100000000000000258E-29, 3.100000000000000044E-14, 1.000000000000000000 ) ) ;
#14415 = ORIENTED_EDGE ( 'NONE', *, *, #59147, .F. ) ;
#14416 = CYLINDRICAL_SURFACE ( 'NONE', #30176, 7.143750000000004263 ) ;
#14417 = CARTESIAN_POINT ( 'NONE',  ( 107.0667039024479834, -58.72944715994110254, 160.9178068554150229 ) ) ;
#14418 = CARTESIAN_POINT ( 'NONE',  ( 108.5688297718456852, -44.75270591617022831, 80.54237608387698799 ) ) ;
#14419 = CIRCLE ( 'NONE', #24528, 7.999999999999992895 ) ;
#14420 = VECTOR ( 'NONE', #61321, 1000.000000000000000 ) ;
#14421 = SHAPE_REPRESENTATION ( 'Drilling Spindle Head', ( #50656 ), #4304 ) ;
#14422 = FACE_OUTER_BOUND ( 'NONE', #79861, .T. ) ;
#14423 = EDGE_CURVE ( 'NONE', #35871, #66630, #73720, .T. ) ;
#14424 = CARTESIAN_POINT ( 'NONE',  ( 108.4174892506360663, -26.73503592742903834, 44.96895860936416511 ) ) ;
#14425 = ORIENTED_EDGE ( 'NONE', *, *, #85804, .F. ) ;
#14426 = ORIENTED_EDGE ( 'NONE', *, *, #23054, .F. ) ;
#14427 = VECTOR ( 'NONE', #88622, 1000.000000000000000 ) ;
#14428 = DIRECTION ( 'NONE',  ( -1.000000000000000000, 1.011922027653136551E-15, 0.000000000000000000 ) ) ;
#14429 = EDGE_CURVE ( 'NONE', #16194, #78995, #54511, .T. ) ;
#14430 = EDGE_LOOP ( 'NONE', ( #48414, #26964, #36417, #86479 ) ) ;
#14431 = EDGE_LOOP ( 'NONE', ( #80269, #20958 ) ) ;
#14432 =( GEOMETRIC_REPRESENTATION_CONTEXT ( 3 ) GLOBAL_UNCERTAINTY_ASSIGNED_CONTEXT ( ( #68092 ) ) GLOBAL_UNIT_ASSIGNED_CONTEXT ( ( #72782, #38252, #57803 ) ) REPRESENTATION_CONTEXT ( 'NONE', 'WORKASPACE' ) );
#14433 = CARTESIAN_POINT ( 'NONE',  ( 112.0659116485927456, -45.48839624525916747, 68.98979194496561718 ) ) ;
#14434 = CARTESIAN_POINT ( 'NONE',  ( 113.1755435565086998, -43.14875213554007161, 154.6130118773249649 ) ) ;
#14435 = EDGE_CURVE ( 'NONE', #2385, #6056, #74611, .T. ) ;
#14436 = DIRECTION ( 'NONE',  ( 1.000000000000000000, 3.999999999999999995E-14, 1.000000000000000078E-15 ) ) ;
#14437 = CARTESIAN_POINT ( 'NONE',  ( 97.24595611328004452, -31.60670846949429347, 86.93181575210095957 ) ) ;
#14438 = DIRECTION ( 'NONE',  ( 0.000000000000000000, -0.7071067811864968355, -0.7071067811865981989 ) ) ;
#14439 = ORIENTED_EDGE ( 'NONE', *, *, #43696, .F. ) ;
#14440 = CARTESIAN_POINT ( 'NONE',  ( -117.9723322394570886, 77.68452076096554038, -11.75283433610015393 ) ) ;
#14441 = ORIENTED_EDGE ( 'NONE', *, *, #2403, .F. ) ;
#14442 = VERTEX_POINT ( 'NONE', #4234 ) ;
#14443 = EDGE_CURVE ( 'NONE', #85594, #40569, #67337, .T. ) ;
#14444 = VECTOR ( 'NONE', #88423, 1000.000000000000000 ) ;
#14445 = DIRECTION ( 'NONE',  ( 1.000000000000000000, 2.999999999999999839E-15, 1.000000000000000078E-15 ) ) ;
#14446 = ORIENTED_EDGE ( 'NONE', *, *, #19754, .T. ) ;
#14447 = CARTESIAN_POINT ( 'NONE',  ( 97.81168895331671820, -40.51742574516950413, 11.63562527591094309 ) ) ;
#14448 = CARTESIAN_POINT ( 'NONE',  ( 114.3591167413298280, -29.19972650290871030, 170.4641967044829585 ) ) ;
#14449 = CARTESIAN_POINT ( 'NONE',  ( 136.8164832912740110, -36.72944715994100306, -5.074374724088999145 ) ) ;
#14450 = CARTESIAN_POINT ( 'NONE',  ( 7.661254700127844153, 66.45253841614081125, 275.4630000000000223 ) ) ;
#14451 = CARTESIAN_POINT ( 'NONE',  ( 117.3638278218041364, -38.35646377537064211, 109.7013395616249767 ) ) ;
#14452 = CARTESIAN_POINT ( 'NONE',  ( 24.79284581386643183, 184.0000000000000000, 101.0189074266571794 ) ) ;
#14453 = ORIENTED_EDGE ( 'NONE', *, *, #89292, .F. ) ;
#14454 = CARTESIAN_POINT ( 'NONE',  ( 97.31323063254396288, -38.96129955496207486, 116.5061487331113881 ) ) ;
#14455 = LINE ( 'NONE', #85301, #30272 ) ;
#14457 = EDGE_LOOP ( 'NONE', ( #17782, #82727, #21581, #73000, #19185 ) ) ;
#14456 = AXIS2_PLACEMENT_3D ( 'NONE', #31928, #89146, #26908 ) ;
#14458 = CARTESIAN_POINT ( 'NONE',  ( 127.0667052882549797, -69.62844715994091871, 222.2178068554179902 ) ) ;
#14459 = DIRECTION ( 'NONE',  ( 0.000000000000000000, 0.000000000000000000, 1.000000000000000000 ) ) ;
#14460 = CARTESIAN_POINT ( 'NONE',  ( 118.5710604172009965, -33.89858672578665733, 14.01848241876796308 ) ) ;
#14461 = CARTESIAN_POINT ( 'NONE',  ( -462.0260000000000105, 53.97500000000000142, -1.387778780781445991E-14 ) ) ;
#14462 = CARTESIAN_POINT ( 'NONE',  ( 0.000000000000000000, 101.5999999999999943, 0.000000000000000000 ) ) ;
#14463 = DIRECTION ( 'NONE',  ( 1.000000000000000000, 4.299999999999999979E-14, 1.000000000000000078E-15 ) ) ;
#14464 = CARTESIAN_POINT ( 'NONE',  ( 117.3951115944451402, -37.65585020919953507, 33.74324432352998571 ) ) ;
#14466 = CARTESIAN_POINT ( 'NONE',  ( 106.0785370228625055, -48.51385081415330092, 108.5099109901969712 ) ) ;
#14465 = CARTESIAN_POINT ( 'NONE',  ( 97.70673715082763522, -40.25178540000793959, 111.6128956075913550 ) ) ;
#14467 = PLANE ( 'NONE',  #50913 ) ;
#14468 = DIRECTION ( 'NONE',  ( 0.000000000000000000, -1.000000000000000000, 0.000000000000000000 ) ) ;
#14469 = VERTEX_POINT ( 'NONE', #47336 ) ;
#14470 = DIRECTION ( 'NONE',  ( 1.000000000000000000, 1.000000000000000078E-15, 0.000000000000000000 ) ) ;
#14471 = VECTOR ( 'NONE', #70948, 1000.000000000000000 ) ;
#14472 = DIRECTION ( 'NONE',  ( 1.000000000000000000, 0.000000000000000000, 0.000000000000000000 ) ) ;
#14473 = DIRECTION ( 'NONE',  ( 0.000000000000000000, 1.365923996832131856E-16, -1.000000000000000000 ) ) ;
#14474 = VERTEX_POINT ( 'NONE', #60067 ) ;
#14475 = AXIS2_PLACEMENT_3D ( 'NONE', #33802, #26100, #26993 ) ;
#14476 = DIRECTION ( 'NONE',  ( 0.000000000000000000, 1.000000000000000000, 0.000000000000000000 ) ) ;
#14478 = ORIENTED_EDGE ( 'NONE', *, *, #72954, .F. ) ;
#14477 = CARTESIAN_POINT ( 'NONE',  ( 113.6422709061198049, -28.58293356745306824, 164.5356252759109736 ) ) ;
#14479 = CARTESIAN_POINT ( 'NONE',  ( 131.0667039024480118, -42.97311385573999587, 231.5838068554170093 ) ) ;
#14480 = CARTESIAN_POINT ( 'NONE',  ( 97.07541381888600540, -41.51105113164680915, 212.6937205140059461 ) ) ;
#14481 = CARTESIAN_POINT ( 'NONE',  ( 116.2698991418618419, -31.74044761805202342, 65.22133956162595325 ) ) ;
#14482 = LINE ( 'NONE', #48962, #22999 ) ;
#14483 = EDGE_CURVE ( 'NONE', #9211, #834, #11499, .T. ) ;
#14484 = DIRECTION ( 'NONE',  ( -0.000000000000000000, 1.000000000000000000, -0.000000000000000000 ) ) ;
#14486 = DIRECTION ( 'NONE',  ( 0.000000000000000000, -1.000000000000000000, 0.000000000000000000 ) ) ;
#14485 = CIRCLE ( 'NONE', #5721, 7.874000000000005883 ) ;
#14487 = VERTEX_POINT ( 'NONE', #5586 ) ;
#14488 = VECTOR ( 'NONE', #65141, 1000.000000000000000 ) ;
#14489 = EDGE_CURVE ( 'NONE', #71741, #83417, #87799, .T. ) ;
#14490 = VERTEX_POINT ( 'NONE', #81895 ) ;
#14491 = EDGE_LOOP ( 'NONE', ( #63711, #38033, #31133, #40883, #25757, #61120, #48992, #39101, #78134, #88008, #46204, #24166, #35264, #35702, #89487, #8154, #47794, #17875, #9176, #75874, #59865, #55822 ) ) ;
#14492 = VECTOR ( 'NONE', #30414, 1000.000000000000000 ) ;
#14493 = VERTEX_POINT ( 'NONE', #32366 ) ;
#14494 = DIRECTION ( 'NONE',  ( -0.1858654557293184517, 0.9825752044329902901, 0.000000000000000000 ) ) ;
#14495 = CARTESIAN_POINT ( 'NONE',  ( 103.0905057572046672, -47.89305850247227880, 248.3041967044829619 ) ) ;
#14496 = LINE ( 'NONE', #8120, #14215 ) ;
#14497 = CARTESIAN_POINT ( 'NONE',  ( 6.812220284937080487E-16, 67.86880000000000734, 271.1195999999999913 ) ) ;
#14498 = AXIS2_PLACEMENT_3D ( 'NONE', #40674, #68396, #42011 ) ;
#14500 = FACE_OUTER_BOUND ( 'NONE', #13374, .T. ) ;
#14499 = CYLINDRICAL_SURFACE ( 'NONE', #42420, 0.4999999999999932832 ) ;
#14501 = CARTESIAN_POINT ( 'NONE',  ( 143.0664832912740110, -18.82844715994099971, 17.92562527591199739 ) ) ;
#14502 = CARTESIAN_POINT ( 'NONE',  ( 112.8299879122683791, -27.27019477826133453, 49.62895860924498947 ) ) ;
#14503 = ORIENTED_EDGE ( 'NONE', *, *, #57742, .F. ) ;
#14504 = ORIENTED_EDGE ( 'NONE', *, *, #16889, .F. ) ;
#14505 = ADVANCED_FACE ( 'NONE', ( #40537 ), #26467, .F. ) ;
#14506 = DIRECTION ( 'NONE',  ( 0.000000000000000000, 0.000000000000000000, 1.000000000000000000 ) ) ;
#14507 = FACE_BOUND ( 'NONE', #88844, .T. ) ;
#14508 = CARTESIAN_POINT ( 'NONE',  ( 117.3720538532506623, -35.57445771113446398, 229.9032443235289520 ) ) ;
#14509 = AXIS2_PLACEMENT_3D ( 'NONE', #31984, #59678, #65177 ) ;
#14510 = CYLINDRICAL_SURFACE ( 'NONE', #31275, 13.00000000000000355 ) ;
#14511 = CARTESIAN_POINT ( 'NONE',  ( 109.9668656698224538, -46.07028316908876775, 93.81562527591097478 ) ) ;
#14512 = PLANE ( 'NONE',  #31330 ) ;
#14513 = CARTESIAN_POINT ( 'NONE',  ( 98.34954641256851460, -31.65714432329926709, 21.90643418995717795 ) ) ;
#14514 = VERTEX_POINT ( 'NONE', #53239 ) ;
#14515 = CYLINDRICAL_SURFACE ( 'NONE', #9561, 2.116999999999993776 ) ;
#14516 = ORIENTED_EDGE ( 'NONE', *, *, #7054, .T. ) ;
#14517 = EDGE_LOOP ( 'NONE', ( #23403, #54023, #12865, #48013, #61076, #42978 ) ) ;
#14518 = VECTOR ( 'NONE', #4121, 1000.000000000000000 ) ;
#14519 = CARTESIAN_POINT ( 'NONE',  ( -82.65294504194682190, 95.16897323824359489, 84.99816483510906551 ) ) ;
#14520 = CARTESIAN_POINT ( 'NONE',  ( 111.6760726031484978, -44.91652306731177902, 254.4282499725637479 ) ) ;
#14521 = CARTESIAN_POINT ( 'NONE',  ( 107.0664832912739968, -36.72944715994100306, 9.635625275910941312 ) ) ;
#14522 = CARTESIAN_POINT ( 'NONE',  ( 97.31585367440334267, -39.30600031747468392, 141.5314607004144705 ) ) ;
#14523 = PLANE ( 'NONE',  #79542 ) ;
#14524 = EDGE_CURVE ( 'NONE', #55444, #67055, #32825, .T. ) ;
#14525 = CARTESIAN_POINT ( 'NONE',  ( 91.25368348339054592, 76.20320268897036442, -75.68572508987483616 ) ) ;
#14526 = ORIENTED_EDGE ( 'NONE', *, *, #35214, .F. ) ;
#14527 = DIRECTION ( 'NONE',  ( 1.147230458779309805E-16, 3.204747427460360459E-31, 1.000000000000000000 ) ) ;
#14528 = PLANE ( 'NONE',  #49871 ) ;
#14529 = ORIENTED_EDGE ( 'NONE', *, *, #18781, .F. ) ;
#14530 = CARTESIAN_POINT ( 'NONE',  ( 100.4790876285538275, -27.85333844968608830, 35.59657765686397113 ) ) ;
#14531 = EDGE_LOOP ( 'NONE', ( #36126, #84180 ) ) ;
#14532 = B_SPLINE_CURVE_WITH_KNOTS ( 'NONE', 3,
 ( #22210, #56701, #14039, #43063, #14945, #84445, #27665, #83099, #49884, #48518, #20852, #70802, #63986, #28098, #21762, #28548, #853, #83990, #36274, #49432, #77613, #41720, #29463, #55781, #6771, #15394, #50332, #42614, #42172, #69902, #8574 ),
 .UNSPECIFIED., .F., .F.,
 ( 4, 2, 2, 1, 2, 2, 2, 2, 2, 2, 2, 1, 1, 2, 2, 2, 4 ),
 ( 0.000000000000000000, 0.06250000000001065814, 0.09375000000001587619, 0.1093750000000143774, 0.1171875000000136280, 0.1250000000000128786, 0.1875000000000279499, 0.2187500000000324185, 0.2500000000000368594, 0.3125000000000400235, 0.3437500000000436873, 0.3593750000000451306, 0.3671875000000462963, 0.3710937500000464073, 0.3750000000000465183, 0.4375000000000232592, 0.5000000000000000000 ),
 .UNSPECIFIED. ) ;
#14533 = EDGE_CURVE ( 'NONE', #53830, #89358, #16823, .T. ) ;
#14534 = CARTESIAN_POINT ( 'NONE',  ( 114.7745679063646378, -33.04956858091291139, 18.60384839950496172 ) ) ;
#14535 = DIRECTION ( 'NONE',  ( 0.000000000000000000, -1.000000000000000000, 0.000000000000000000 ) ) ;
#14536 = CARTESIAN_POINT ( 'NONE',  ( 98.71823956546961654, -31.63334453281603587, 170.8899109901969950 ) ) ;
#14537 = LINE ( 'NONE', #42216, #59271 ) ;
#14538 = EDGE_CURVE ( 'NONE', #7104, #54166, #75065, .T. ) ;
#14539 = DIRECTION ( 'NONE',  ( 0.000000000000000000, 2.135044278125299371E-15, -1.000000000000000000 ) ) ;
#14540 = DIRECTION ( 'NONE',  ( -0.7071067811865192621, -0.7071067811865758834, -7.071067811865185427E-16 ) ) ;
#14541 = CARTESIAN_POINT ( 'NONE',  ( 5.567800219335068412, 71.13383842984607952, 130.4373048777247561 ) ) ;
#14542 = CARTESIAN_POINT ( 'NONE',  ( 100.5841487926172277, -28.49196697857695781, 11.60705384733995515 ) ) ;
#14543 = CARTESIAN_POINT ( 'NONE',  ( 76.39920031718088467, 90.28416741362499920, -90.65736737572389359 ) ) ;
#14544 = AXIS2_PLACEMENT_3D ( 'NONE', #1274, #62590, #28979 ) ;
#14545 = ORIENTED_EDGE ( 'NONE', *, *, #57221, .T. ) ;
#14546 = CARTESIAN_POINT ( 'NONE',  ( 136.7635286919469593, -37.26660482608871661, 6.827192804310227459 ) ) ;
#14547 = EDGE_LOOP ( 'NONE', ( #2048, #87689, #56691, #27971, #54275 ) ) ;
#14548 = CARTESIAN_POINT ( 'NONE',  ( 96.65590158217011663, -37.83070472558634378, 122.4099109901969626 ) ) ;
#14549 = CARTESIAN_POINT ( 'NONE',  ( 120.2492451804830011, 48.02562542861102202, -50.84303487544575262 ) ) ;
#14550 = VERTEX_POINT ( 'NONE', #66900 ) ;
#14551 = DIRECTION ( 'NONE',  ( 1.054009200593500181E-15, 1.000000000000000000, 0.000000000000000000 ) ) ;
#14552 = ORIENTED_EDGE ( 'NONE', *, *, #3874, .T. ) ;
#14553 = EDGE_LOOP ( 'NONE', ( #22669, #38238, #34357, #26263 ) ) ;
#14554 = EDGE_CURVE ( 'NONE', #7464, #63748, #77769, .T. ) ;
#14555 = VECTOR ( 'NONE', #79134, 1000.000000000000000 ) ;
#14556 = CARTESIAN_POINT ( 'NONE',  ( 151.0667039024469886, -67.87844715994090450, 190.2178068554179902 ) ) ;
#14557 = DIRECTION ( 'NONE',  ( -0.9659258262890697555, 0.000000000000000000, 0.2588190451025154659 ) ) ;
#14559 = ADVANCED_FACE ( 'NONE', ( #68260 ), #88265, .T. ) ;
#14558 = CARTESIAN_POINT ( 'NONE',  ( 38.10000000000000142, 69.84999999999999432, 346.9005000000000223 ) ) ;
#14560 = AXIS2_PLACEMENT_3D ( 'NONE', #17276, #72689, #38155 ) ;
#14561 = CARTESIAN_POINT ( 'NONE',  ( 126.0667039024479266, -14.72944715994094977, 239.5838068554170377 ) ) ;
#14562 = CARTESIAN_POINT ( 'NONE',  ( 138.8664832912739939, -71.52944715994085811, 361.9756252759100335 ) ) ;
#14563 = CARTESIAN_POINT ( 'NONE',  ( 115.4543170047500098, -34.59750657913997429, 166.8547570362579506 ) ) ;
#14564 = CARTESIAN_POINT ( 'NONE',  ( 114.4303731589454998, -27.41304352248915777, 270.5441967044823741 ) ) ;
#14565 = DIRECTION ( 'NONE',  ( -0.5000000000000129896, -0.8660254037844311581, 0.000000000000000000 ) ) ;
#14566 = VERTEX_POINT ( 'NONE', #89147 ) ;
#14567 = DIRECTION ( 'NONE',  ( -1.000000000000000078E-15, 1.000000000000000083E-30, 1.000000000000000000 ) ) ;
#14568 = AXIS2_PLACEMENT_3D ( 'NONE', #75660, #13430, #24080 ) ;
#14569 = LINE ( 'NONE', #42242, #8490 ) ;
#14570 = EDGE_LOOP ( 'NONE', ( #54012, #5837, #6315 ) ) ;
#14571 = ORIENTED_EDGE ( 'NONE', *, *, #19847, .F. ) ;
#14572 = CARTESIAN_POINT ( 'NONE',  ( 82.81651833456541567, -18.90056224776904159, 3.101534470965027435 ) ) ;
#14573 = PLANE ( 'NONE',  #89027 ) ;
#14574 = CARTESIAN_POINT ( 'NONE',  ( 104.4898988706324445, -26.97882157938011360, 15.28146304136766354 ) ) ;
#14575 = PLANE ( 'NONE',  #40498 ) ;
#14576 = CARTESIAN_POINT ( 'NONE',  ( 125.0664851986225159, -56.72944715994083964, 14.82207188531762654 ) ) ;
#14577 = VECTOR ( 'NONE', #16325, 1000.000000000000000 ) ;
#14578 = CARTESIAN_POINT ( 'NONE',  ( 107.4755550402934148, -45.77628807984756065, 192.0228960185529559 ) ) ;
#14579 = CARTESIAN_POINT ( 'NONE',  ( 110.1710482807090585, -46.72786414817543488, 97.81562527591097478 ) ) ;
#14580 = ORIENTED_EDGE ( 'NONE', *, *, #39762, .T. ) ;
#14581 = DIRECTION ( 'NONE',  ( 0.000000000000000000, -1.000000000000000000, 0.000000000000000000 ) ) ;
#14582 = VERTEX_POINT ( 'NONE', #26909 ) ;
#14583 = CARTESIAN_POINT ( 'NONE',  ( -77.45828646618646474, 73.28361289573329884, -89.75424775947691103 ) ) ;
#14584 = ORIENTED_EDGE ( 'NONE', *, *, #5103, .F. ) ;
#14585 = DIRECTION ( 'NONE',  ( 0.000000000000000000, 0.000000000000000000, 1.000000000000000000 ) ) ;
#14586 = ORIENTED_EDGE ( 'NONE', *, *, #48016, .T. ) ;
#14587 = CARTESIAN_POINT ( 'NONE',  ( -75.61066417432020614, 0.000000000000000000, 177.0380000000000109 ) ) ;
#14588 = CARTESIAN_POINT ( 'NONE',  ( 41.56648329127398966, -27.57844715994070484, 78.92562527591199739 ) ) ;
#14589 = CARTESIAN_POINT ( 'NONE',  ( 73.06648329127399677, -8.729447159941065237, -4.824374724089063982 ) ) ;
#14590 = CONICAL_SURFACE ( 'NONE', #49373, 10.66799999999999748, 0.08726646259971625186 ) ;
#14591 = CARTESIAN_POINT ( 'NONE',  ( 113.7313622454167046, -108.7036397175020994, -19.78219314458187839 ) ) ;
#14592 = EDGE_LOOP ( 'NONE', ( #48302, #21990, #89799, #10258 ) ) ;
#14593 = CARTESIAN_POINT ( 'NONE',  ( 117.5098600993040066, -37.01623072280121107, 43.80419670448293346 ) ) ;
#14596 = ADVANCED_FACE ( 'NONE', ( #38744 ), #80109, .T. ) ;
#14595 = CYLINDRICAL_SURFACE ( 'NONE', #5086, 5.599999999999994316 ) ;
#14594 = CARTESIAN_POINT ( 'NONE',  ( 63.50000000000000000, 66.67499999999999716, 219.0749999999999886 ) ) ;
#14597 = CARTESIAN_POINT ( 'NONE',  ( 4.788368984666157546E-15, 92.07499999999998863, -39.10000000000005116 ) ) ;
#14598 = CARTESIAN_POINT ( 'NONE',  ( 128.2504969244201334, -12.91928723231331588, 361.9756252759100903 ) ) ;
#14599 = VERTEX_POINT ( 'NONE', #46438 ) ;
#14600 = CIRCLE ( 'NONE', #81328, 4.762500000000002842 ) ;
#14601 = CARTESIAN_POINT ( 'NONE',  ( 105.6559524084447617, -26.80454636418725656, 121.1869003628085579 ) ) ;
#14602 = LINE ( 'NONE', #36388, #49809 ) ;
#14603 = CARTESIAN_POINT ( 'NONE',  ( 90.44969454456422397, -23.41243780205712710, 249.5838068554174924 ) ) ;
#14604 = VECTOR ( 'NONE', #73122, 1000.000000000000000 ) ;
#14605 = CARTESIAN_POINT ( 'NONE',  ( 96.00479252368074867, -37.29883552165912874, 117.3794347997199594 ) ) ;
#14607 = DIRECTION ( 'NONE',  ( 0.000000000000000000, 1.000000000000000000, 0.000000000000000000 ) ) ;
#14606 = LINE ( 'NONE', #7339, #10182 ) ;
#14608 = FACE_OUTER_BOUND ( 'NONE', #66225, .T. ) ;
#14609 = AXIS2_PLACEMENT_3D ( 'NONE', #7763, #58146, #64966 ) ;
#14610 = ORIENTED_EDGE ( 'NONE', *, *, #58596, .T. ) ;
#14611 = ADVANCED_FACE ( 'NONE', ( #87359 ), #80547, .F. ) ;
#14612 = B_SPLINE_CURVE_WITH_KNOTS ( 'NONE', 3,
 ( #16676, #38009, #80697, #39344, #44362, #44811 ),
 .UNSPECIFIED., .F., .F.,
 ( 4, 2, 4 ),
 ( 0.9103247092270834173, 0.9551623546135417087, 1.000000000000000000 ),
 .UNSPECIFIED. ) ;
#14613 = DIRECTION ( 'NONE',  ( 0.000000000000000000, 0.000000000000000000, -1.000000000000000000 ) ) ;
#14614 = CARTESIAN_POINT ( 'NONE',  ( 113.4935171807053536, -28.59114140144097860, 120.5565776568629559 ) ) ;
#14615 = AXIS2_PLACEMENT_3D ( 'NONE', #50397, #78143, #15901 ) ;
#14617 = ORIENTED_EDGE ( 'NONE', *, *, #48232, .T. ) ;
#14616 = CARTESIAN_POINT ( 'NONE',  ( 29.00000000000001421, 172.0000000000000000, 113.8826257785461280 ) ) ;
#14618 = CARTESIAN_POINT ( 'NONE',  ( 106.2286657330468245, -47.72771449247510844, 263.5280062282920994 ) ) ;
#14619 = CARTESIAN_POINT ( 'NONE',  ( 97.81399931465544739, -40.51646775427786196, 252.6355816051047896 ) ) ;
#14620 = PLANE ( 'NONE',  #85268 ) ;
#14621 = CARTESIAN_POINT ( 'NONE',  ( 107.5667039024470313, -108.2470741265382799, 2.217806855418114065 ) ) ;
#14622 = LINE ( 'NONE', #50010, #39824 ) ;
#14623 = EDGE_CURVE ( 'NONE', #80786, #28614, #21453, .T. ) ;
#14624 = DIRECTION ( 'NONE',  ( -1.175184669632759901E-16, 1.000000000000000000, 2.000000000000003705E-15 ) ) ;
#14625 = CARTESIAN_POINT ( 'NONE',  ( -89.37727808479034763, 70.52074417248462623, 95.16685018566064969 ) ) ;
#14626 = CARTESIAN_POINT ( 'NONE',  ( 99.07755742602699911, -44.46178485432853478, 191.9384824187689560 ) ) ;
#14627 = ORIENTED_EDGE ( 'NONE', *, *, #84152, .T. ) ;
#14628 = EDGE_LOOP ( 'NONE', ( #34198, #63678, #83983, #8222 ) ) ;
#14629 = CARTESIAN_POINT ( 'NONE',  ( 105.5787418010314695, -46.69191849206237066, 143.8901547344689789 ) ) ;
#14630 = CARTESIAN_POINT ( 'NONE',  ( 71.09939861440099662, 101.5999999999999943, 177.8662485265279827 ) ) ;
#14631 = CARTESIAN_POINT ( 'NONE',  ( 97.82556271424805061, -33.52526948863204126, 282.0613395616247772 ) ) ;
#14632 = CARTESIAN_POINT ( 'NONE',  ( 147.0667039027857470, -137.6784471596013191, 245.4218662566959779 ) ) ;
#14633 = EDGE_CURVE ( 'NONE', #85887, #77884, #69597, .T. ) ;
#14634 = CIRCLE ( 'NONE', #71251, 32.50000000000000711 ) ;
#14635 = CARTESIAN_POINT ( 'NONE',  ( 116.8174800920801317, -34.15430197086818254, 269.0316147097951216 ) ) ;
#14636 = DIRECTION ( 'NONE',  ( 0.000000000000000000, 0.000000000000000000, -1.000000000000000000 ) ) ;
#14637 = AXIS2_PLACEMENT_3D ( 'NONE', #44738, #38824, #3869 ) ;
#14638 = CARTESIAN_POINT ( 'NONE',  ( 90.44969454456416713, -53.34645651782494724, 219.5838068554169809 ) ) ;
#14639 = LINE ( 'NONE', #70495, #89443 ) ;
#14640 = B_SPLINE_CURVE_WITH_KNOTS ( 'NONE', 3,
 ( #16224, #56297, #31614, #10288, #86601, #30291, #23050, #71635, #44799, #24373, #58864, #65689, #43901, #30733, #37993, #9400, #2595, #72953 ),
 .UNSPECIFIED., .F., .F.,
 ( 4, 2, 2, 2, 2, 2, 2, 2, 4 ),
 ( 0.000000000000000000, 0.06249999963049208268, 0.1249999992609841654, 0.1874999988914762550, 0.2499999985219683307, 0.3124999981524604342, 0.3749999977829525100, 0.4374999974134445857, 0.4999999970439366614 ),
 .UNSPECIFIED. ) ;
#14641 = CARTESIAN_POINT ( 'NONE',  ( 96.70388795518319114, -35.81005419191407668, 231.2556252759109725 ) ) ;
#14642 = CARTESIAN_POINT ( 'NONE',  ( 128.5492039024480277, -43.72944715994093912, 231.5838068554170093 ) ) ;
#14643 = ORIENTED_EDGE ( 'NONE', *, *, #71655, .T. ) ;
#14645 = ORIENTED_EDGE ( 'NONE', *, *, #37613, .F. ) ;
#14644 = EDGE_CURVE ( 'NONE', #60102, #45673, #35056, .T. ) ;
#14646 = CARTESIAN_POINT ( 'NONE',  ( 6.349999999999999645, 82.54999999999999716, 307.6574999999999704 ) ) ;
#14647 = CARTESIAN_POINT ( 'NONE',  ( 82.77657790094413315, -19.19711456032067787, 6.808568500765782794 ) ) ;
#14648 = FACE_OUTER_BOUND ( 'NONE', #39241, .T. ) ;
#14649 = CARTESIAN_POINT ( 'NONE',  ( 21.03715912545738220, -47.82818131006197149, 193.9678068554150627 ) ) ;
#14650 = AXIS2_PLACEMENT_3D ( 'NONE', #44599, #72336, #49628 ) ;
#14651 = DIRECTION ( 'NONE',  ( 1.000000000000000000, 0.000000000000000000, 0.000000000000000000 ) ) ;
#14652 = EDGE_LOOP ( 'NONE', ( #51595, #8383, #21193, #70880, #37394 ) ) ;
#14653 = AXIS2_PLACEMENT_3D ( 'NONE', #43686, #71422, #36884 ) ;
#14654 = CARTESIAN_POINT ( 'NONE',  ( -2.861372676390278258, 94.82780855858955249, 118.3221063943049813 ) ) ;
#14655 = CARTESIAN_POINT ( 'NONE',  ( 96.77253738264830929, -34.86918258059447595, 241.1841967044819626 ) ) ;
#14656 = ORIENTED_EDGE ( 'NONE', *, *, #5838, .T. ) ;
#14657 = ADVANCED_FACE ( 'NONE', ( #82347 ), #35964, .F. ) ;
#14658 = CYLINDRICAL_SURFACE ( 'NONE', #79663, 9.999999999999998224 ) ;
#14660 = EDGE_CURVE ( 'NONE', #60222, #11985, #84134, .T. ) ;
#14659 = CARTESIAN_POINT ( 'NONE',  ( 97.81168895331838087, -40.51742574516882200, 287.6356252759109680 ) ) ;
#14661 = CARTESIAN_POINT ( 'NONE',  ( 31.75000000000000000, 17.78000000000000114, 3.174999999999999822 ) ) ;
#14662 = ADVANCED_FACE ( 'NONE', ( #27802 ), #543, .T. ) ;
#14663 = CARTESIAN_POINT ( 'NONE',  ( 109.9854453146643039, -44.35239847312019634, 60.68523322673397047 ) ) ;
#14664 = CARTESIAN_POINT ( 'NONE',  ( 112.7920458925406422, -45.46759294451666022, 174.0384824187679556 ) ) ;
#14665 = CIRCLE ( 'NONE', #36588, 7.937500000000000000 ) ;
#14666 = DIRECTION ( 'NONE',  ( 3.100000000000000258E-29, -3.100000000000000044E-14, -1.000000000000000000 ) ) ;
#14667 = VERTEX_POINT ( 'NONE', #48227 ) ;
#14668 = EDGE_CURVE ( 'NONE', #2787, #9116, #70044, .T. ) ;
#14669 = DIRECTION ( 'NONE',  ( 0.9242245927363031965, 0.3818493186865917766, 0.000000000000000000 ) ) ;
#14670 = ORIENTED_EDGE ( 'NONE', *, *, #14902, .F. ) ;
#14672 = VERTEX_POINT ( 'NONE', #82798 ) ;
#14671 = AXIS2_PLACEMENT_3D ( 'NONE', #40378, #39923, #53981 ) ;
#14673 = DIRECTION ( 'NONE',  ( 1.000000000000000000, 4.299999999999999979E-14, 1.000000000000000078E-15 ) ) ;
#14674 = ORIENTED_EDGE ( 'NONE', *, *, #21687, .T. ) ;
#14675 = ORIENTED_EDGE ( 'NONE', *, *, #77567, .F. ) ;
#14676 = CARTESIAN_POINT ( 'NONE',  ( 107.0664832912730020, -27.87844715994269862, 361.9756252759109998 ) ) ;
#14677 = DIRECTION ( 'NONE',  ( -1.000000000000000000, -1.075267683398002218E-15, 2.333298185338067508E-30 ) ) ;
#14678 = CARTESIAN_POINT ( 'NONE',  ( 115.4827349520354858, -33.38588942772360468, 98.56194363760096167 ) ) ;
#14679 = CIRCLE ( 'NONE', #87165, 1.219499999999975159 ) ;
#14680 = CARTESIAN_POINT ( 'NONE',  ( 118.3649377238561300, -33.07154184081399961, 284.0756252759109657 ) ) ;
#14681 = CARTESIAN_POINT ( 'NONE',  ( 99.10268845779062019, -29.98093639561593449, 215.7670538473399517 ) ) ;
#14682 = DIRECTION ( 'NONE',  ( -2.283216351027200160E-14, 0.000000000000000000, 1.000000000000000000 ) ) ;
#14683 = DIRECTION ( 'NONE',  ( 0.000000000000000000, 1.000000000000000000, 0.000000000000000000 ) ) ;
#14684 = VERTEX_POINT ( 'NONE', #55482 ) ;
#14685 = LINE ( 'NONE', #62809, #31897 ) ;
#14686 = FACE_OUTER_BOUND ( 'NONE', #23476, .T. ) ;
#14687 = CARTESIAN_POINT ( 'NONE',  ( 70.42775326414512449, -140.0375196470091055, 247.0014259009493856 ) ) ;
#14688 = CARTESIAN_POINT ( 'NONE',  ( 108.8662857618680562, -46.94215964495590043, 122.7032443235309671 ) ) ;
#14689 = CARTESIAN_POINT ( 'NONE',  ( 106.9267615183890854, -26.22553017860169433, 60.08705384733897858 ) ) ;
#14690 = CARTESIAN_POINT ( 'NONE',  ( 112.5123584215844659, -46.40184746663635451, 257.9965776568634510 ) ) ;
#14691 = EDGE_LOOP ( 'NONE', ( #28356, #4205 ) ) ;
#14692 = CARTESIAN_POINT ( 'NONE',  ( 106.5673262220758772, -47.17821497701651623, 247.5384824187679556 ) ) ;
#14693 = DIRECTION ( 'NONE',  ( 1.000000000000000000, -1.000000000000000078E-15, 0.000000000000000000 ) ) ;
#14694 =( NAMED_UNIT ( * ) SI_UNIT ( $, .STERADIAN. ) SOLID_ANGLE_UNIT ( ) );
#14695 =( NAMED_UNIT ( * ) PLANE_ANGLE_UNIT ( ) SI_UNIT ( $, .RADIAN. ) );
#14696 = CARTESIAN_POINT ( 'NONE',  ( 99.18883298691498851, -42.92813836781478898, 27.85781585569052154 ) ) ;
#14698 = LINE ( 'NONE', #69206, #10846 ) ;
#14697 = CARTESIAN_POINT ( 'NONE',  ( 134.0664832912740110, -8.350947159940998787, 7.443125275912000127 ) ) ;
#14699 = CARTESIAN_POINT ( 'NONE',  ( -487.2989999999999782, 14.28750000000036025, 2.863608028952925100 ) ) ;
#14700 = CARTESIAN_POINT ( 'NONE',  ( 51.42025729302500281, -31.94127993907734719, 117.4678068554150485 ) ) ;
#14701 = CARTESIAN_POINT ( 'NONE',  ( 2.078103260390294693, 95.08570091005915970, -118.5384849238115947 ) ) ;
#14702 = AXIS2_PLACEMENT_3D ( 'NONE', #73124, #51330, #44518 ) ;
#14703 = CARTESIAN_POINT ( 'NONE',  ( -479.3614999999999782, 53.97500000000000142, 88.90000000000000568 ) ) ;
#14704 = CARTESIAN_POINT ( 'NONE',  ( 104.4899544214444944, -26.97880759237127180, 11.28145861166093766 ) ) ;
#14705 = DIRECTION ( 'NONE',  ( -0.7071067811865475727, 0.7071067811865475727, 0.000000000000000000 ) ) ;
#14707 = ORIENTED_EDGE ( 'NONE', *, *, #2548, .F. ) ;
#14706 = CARTESIAN_POINT ( 'NONE',  ( 108.4174892377433252, -26.73503592547494634, 259.9689586103912688 ) ) ;
#14708 = CARTESIAN_POINT ( 'NONE',  ( 127.4058501689331280, -122.7870702624433221, 250.2178068554179902 ) ) ;
#14709 = CARTESIAN_POINT ( 'NONE',  ( 96.22633597390384352, -34.45202597047101278, 261.1737205140064475 ) ) ;
#14710 = CARTESIAN_POINT ( 'NONE',  ( 103.4684036848089050, -46.51393990267121836, 138.2956252759109645 ) ) ;
#14711 = CARTESIAN_POINT ( 'NONE',  ( 118.5948618896802742, -33.89272371608580414, 10.01848241876795953 ) ) ;
#14712 = DIRECTION ( 'NONE',  ( 0.000000000000000000, 0.000000000000000000, 1.000000000000000000 ) ) ;
#14713 = AXIS2_PLACEMENT_3D ( 'NONE', #42267, #48616, #20512 ) ;
#14715 = CARTESIAN_POINT ( 'NONE',  ( 81.63820548406727085, -34.47341874818841490, 7.827313014938356517 ) ) ;
#14714 = DIRECTION ( 'NONE',  ( 0.6544127834855474335, 0.2678505344604093508, 0.7071067811865271446 ) ) ;
#14716 = CARTESIAN_POINT ( 'NONE',  ( 98.54777178369499779, -41.97717499081849013, 137.7658220778284317 ) ) ;
#14717 = VECTOR ( 'NONE', #35309, 1000.000000000000000 ) ;
#14718 = EDGE_CURVE ( 'NONE', #770, #54421, #61864, .T. ) ;
#14719 = ORIENTED_EDGE ( 'NONE', *, *, #53939, .F. ) ;
#14720 = EDGE_CURVE ( 'NONE', #12518, #87053, #73469, .T. ) ;
#14721 = LINE ( 'NONE', #56475, #33073 ) ;
#14722 = ORIENTED_EDGE ( 'NONE', *, *, #62400, .F. ) ;
#14723 = CARTESIAN_POINT ( 'NONE',  ( 109.3519496323076083, -28.49945473430254950, 174.2838483995049899 ) ) ;
#14724 = EDGE_CURVE ( 'NONE', #7172, #40430, #63224, .T. ) ;
#14726 = ORIENTED_EDGE ( 'NONE', *, *, #59704, .F. ) ;
#14725 = DIRECTION ( 'NONE',  ( 1.000000000000000000, 4.299999999999999979E-14, 1.000000000000000078E-15 ) ) ;
#14727 = LINE ( 'NONE', #42400, #73663 ) ;
#14728 = CARTESIAN_POINT ( 'NONE',  ( 113.6008039948045649, -28.63430547549730676, 160.5356252759109736 ) ) ;
#14729 = CARTESIAN_POINT ( 'NONE',  ( 172.5664832912740110, -18.82844715994099971, 18.92562527591200094 ) ) ;
#14730 = FACE_OUTER_BOUND ( 'NONE', #77515, .T. ) ;
#14731 = CARTESIAN_POINT ( 'NONE',  ( 107.7705136438765550, -26.73286797099179424, 86.02129597068410760 ) ) ;
#14732 = EDGE_CURVE ( 'NONE', #74795, #76086, #14639, .T. ) ;
#14733 = AXIS2_PLACEMENT_3D ( 'NONE', #46546, #68359, #59289 ) ;
#14734 = EDGE_CURVE ( 'NONE', #88862, #46552, #42982, .T. ) ;
#14735 = CARTESIAN_POINT ( 'NONE',  ( -87.72765544449595154, 71.14137858619484689, 79.74945239053533896 ) ) ;
#14736 = LINE ( 'NONE', #63319, #25128 ) ;
#14737 = CARTESIAN_POINT ( 'NONE',  ( 106.6854394624702707, -26.95610377642487165, 85.10705384733996937 ) ) ;
#14738 = ORIENTED_EDGE ( 'NONE', *, *, #85717, .F. ) ;
#14739 = VERTEX_POINT ( 'NONE', #21905 ) ;
#14741 = VERTEX_POINT ( 'NONE', #89599 ) ;
#14740 = CIRCLE ( 'NONE', #61138, 2.517500000000005844 ) ;
#14742 = EDGE_CURVE ( 'NONE', #35450, #37737, #55935, .T. ) ;
#14743 = CARTESIAN_POINT ( 'NONE',  ( 115.7370193921850898, -38.55977017368898174, 60.09301187732596361 ) ) ;
#14744 = DIRECTION ( 'NONE',  ( 0.7071067811868717579, 0.7071067811862232766, 7.071067811868711635E-16 ) ) ;
#14746 = CARTESIAN_POINT ( 'NONE',  ( 115.0372575324259401, -42.90846253205904759, 38.30229194598641129 ) ) ;
#14745 = CARTESIAN_POINT ( 'NONE',  ( 116.7742277529939230, -35.53649587948896027, 189.9241967044819717 ) ) ;
#14747 = CARTESIAN_POINT ( 'NONE',  ( 172.5664832912740110, -36.32844715994070839, 143.6756252759119832 ) ) ;
#14748 = ADVANCED_FACE ( 'NONE', ( #8267 ), #27356, .T. ) ;
#14749 = DIRECTION ( 'NONE',  ( 0.000000000000000000, 0.000000000000000000, -1.000000000000000000 ) ) ;
#14750 = AXIS2_PLACEMENT_3D ( 'NONE', #53626, #88201, #66833 ) ;
#14751 = DIRECTION ( 'NONE',  ( 7.076552332833900719E-16, -1.000000000000000000, 3.100000000000000044E-14 ) ) ;
#14752 = DIRECTION ( 'NONE',  ( 1.000000000000000000, 3.999999999999999995E-14, 1.000000000000000078E-15 ) ) ;
#14753 = CARTESIAN_POINT ( 'NONE',  ( 67.20685546831352042, -68.01262586362689433, 246.2275592078436546 ) ) ;
#14754 = ADVANCED_FACE ( 'NONE', ( #1459 ), #20558, .T. ) ;
#14755 = CARTESIAN_POINT ( 'NONE',  ( 109.2504006710444315, -46.93703897017543625, 107.7441967044829880 ) ) ;
#14756 = VERTEX_POINT ( 'NONE', #6914 ) ;
#14757 = VERTEX_POINT ( 'NONE', #83236 ) ;
#14759 = ORIENTED_EDGE ( 'NONE', *, *, #35705, .T. ) ;
#14758 = EDGE_CURVE ( 'NONE', #86303, #37134, #930, .T. ) ;
#14760 = LINE ( 'NONE', #64241, #58936 ) ;
#14761 = LINE ( 'NONE', #42876, #79534 ) ;
#14762 = CARTESIAN_POINT ( 'NONE',  ( 108.4158484965001890, -26.73482408474558270, 129.9690911813341927 ) ) ;
#14763 = CARTESIAN_POINT ( 'NONE',  ( 116.3212776292292716, -32.94146857471233147, 105.1356252759109680 ) ) ;
#14764 = CARTESIAN_POINT ( 'NONE',  ( 114.3567987304369495, -40.40109894280344349, 201.2738046553059803 ) ) ;
#14765 = CARTESIAN_POINT ( 'NONE',  ( 37.03715912545425937, -48.62818131006122258, 313.9678068554150059 ) ) ;
#14766 = CARTESIAN_POINT ( 'NONE',  ( 109.7258523471263914, -27.00106681210123938, 25.86424884311490047 ) ) ;
#14767 = VERTEX_POINT ( 'NONE', #9602 ) ;
#14769 = ORIENTED_EDGE ( 'NONE', *, *, #88491, .T. ) ;
#14768 = ORIENTED_EDGE ( 'NONE', *, *, #39603, .T. ) ;
#14770 = VECTOR ( 'NONE', #48626, 1000.000000000000000 ) ;
#14771 = EDGE_CURVE ( 'NONE', #65869, #69742, #47323, .T. ) ;
#14772 = CARTESIAN_POINT ( 'NONE',  ( 107.9747653995834327, -87.30271670975442078, -11.78219314458253741 ) ) ;
#14773 = VERTEX_POINT ( 'NONE', #1900 ) ;
#14774 = ORIENTED_EDGE ( 'NONE', *, *, #76149, .T. ) ;
#14776 = EDGE_CURVE ( 'NONE', #59253, #28372, #2426, .T. ) ;
#14775 = CARTESIAN_POINT ( 'NONE',  ( 77.97204591021541376, -20.52018918698335170, 7.480061334675825790 ) ) ;
#14777 = ADVANCED_FACE ( 'NONE', ( #71400 ), #36428, .T. ) ;
#14778 = CARTESIAN_POINT ( 'NONE',  ( 111.6760726031484978, -44.91652306731177902, 254.4282499725637479 ) ) ;
#14779 = CARTESIAN_POINT ( 'NONE',  ( 105.7999286771159149, -26.72397919236279762, 181.1777144871696237 ) ) ;
#14780 = ORIENTED_EDGE ( 'NONE', *, *, #30314, .F. ) ;
#14781 = EDGE_CURVE ( 'NONE', #89690, #46099, #57748, .T. ) ;
#14782 = AXIS2_PLACEMENT_3D ( 'NONE', #68098, #40383, #33568 ) ;
#14783 = DIRECTION ( 'NONE',  ( 0.000000000000000000, 3.785359618865284342E-16, 1.000000000000000000 ) ) ;
#14784 = CARTESIAN_POINT ( 'NONE',  ( -123.0153672541236176, 73.36296953743759275, 43.72751329226351658 ) ) ;
#14785 = VERTEX_POINT ( 'NONE', #64571 ) ;
#14786 = ORIENTED_EDGE ( 'NONE', *, *, #68942, .F. ) ;
#14787 = CYLINDRICAL_SURFACE ( 'NONE', #69668, 2.030000000002086580 ) ;
#14788 = EDGE_LOOP ( 'NONE', ( #22564, #68338, #81411, #43003 ) ) ;
#14789 = ORIENTED_EDGE ( 'NONE', *, *, #37987, .F. ) ;
#14790 = CARTESIAN_POINT ( 'NONE',  ( 114.0298635175061008, -31.59016113260716097, 257.1385665600676589 ) ) ;
#14791 = CARTESIAN_POINT ( 'NONE',  ( 98.26213988389305598, -31.03978702703054537, 145.8699109901969848 ) ) ;
#14792 = CARTESIAN_POINT ( 'NONE',  ( 114.5517459224756749, -44.00510994954056088, 98.21276813305395592 ) ) ;
#14793 = DIRECTION ( 'NONE',  ( 0.000000000000000000, 0.000000000000000000, 1.000000000000000000 ) ) ;
#14794 = FILL_AREA_STYLE_COLOUR ( '', #80074 ) ;
#14795 = CARTESIAN_POINT ( 'NONE',  ( 98.94264532560653436, -30.19601435972772308, 236.7870538473399336 ) ) ;
#14796 = CARTESIAN_POINT ( 'NONE',  ( 147.0667039024469886, -67.87844715994090450, 222.2178068554179902 ) ) ;
#14797 = DIRECTION ( 'NONE',  ( 0.000000000000000000, -1.000000000000000000, 0.000000000000000000 ) ) ;
#14798 = ORIENTED_EDGE ( 'NONE', *, *, #35421, .F. ) ;
#14799 = LINE ( 'NONE', #7968, #58414 ) ;
#14800 = ORIENTED_EDGE ( 'NONE', *, *, #71834, .T. ) ;
#14801 = CIRCLE ( 'NONE', #51020, 9.525000000000000355 ) ;
#14802 = ORIENTED_EDGE ( 'NONE', *, *, #4790, .T. ) ;
#14803 = LINE ( 'NONE', #69309, #63452 ) ;
#14804 = CARTESIAN_POINT ( 'NONE',  ( 110.1409620311622604, -27.17888879385625600, 135.8284909550441455 ) ) ;
#14805 = VECTOR ( 'NONE', #86173, 1000.000000000000000 ) ;
#14806 = ORIENTED_EDGE ( 'NONE', *, *, #8903, .T. ) ;
#14807 = CARTESIAN_POINT ( 'NONE',  ( 99.68446536626322541, -46.00016974189506413, 122.0413395616249659 ) ) ;
#14808 = PLANE ( 'NONE',  #41700 ) ;
#14809 = CARTESIAN_POINT ( 'NONE',  ( 135.7892066358211594, -34.57943358557326263, 7.744922197164725297 ) ) ;
#14810 = CARTESIAN_POINT ( 'NONE',  ( 107.0667039024470313, -104.2784471599420897, -20.48315503890502143 ) ) ;
#14813 = CARTESIAN_POINT ( 'NONE',  ( 100.1532602078033278, -44.50350736857013345, 262.9984824187678782 ) ) ;
#14812 = DIRECTION ( 'NONE',  ( 0.000000000000000000, 1.000000000000000000, 0.000000000000000000 ) ) ;
#14811 = CARTESIAN_POINT ( 'NONE',  ( 107.0667039024470313, -104.2784471599409102, 17.71780685541799016 ) ) ;
#14814 = FACE_OUTER_BOUND ( 'NONE', #8504, .T. ) ;
#14815 = PLANE ( 'NONE',  #46740 ) ;
#14816 = VECTOR ( 'NONE', #41246, 1000.000000000000000 ) ;
#14817 = CARTESIAN_POINT ( 'NONE',  ( 1.166476076187854022E-15, 92.07499999999998863, -9.525000000000000355 ) ) ;
#14818 = DIRECTION ( 'NONE',  ( 0.000000000000000000, -1.000000000000000000, 0.000000000000000000 ) ) ;
#14819 = DIRECTION ( 'NONE',  ( -1.000000000000000078E-15, 0.000000000000000000, -1.000000000000000000 ) ) ;
#14820 = CIRCLE ( 'NONE', #59714, 2.500000000000002220 ) ;
#14821 = CARTESIAN_POINT ( 'NONE',  ( 144.8664832912739939, -71.52944715994085811, 361.9756252759100335 ) ) ;
#14823 = ORIENTED_EDGE ( 'NONE', *, *, #11065, .T. ) ;
#14822 = CARTESIAN_POINT ( 'NONE',  ( 96.93601811142059432, -39.37148068186442629, 276.5299109901966403 ) ) ;
#14824 = VECTOR ( 'NONE', #43450, 1000.000000000000000 ) ;
#14825 = CARTESIAN_POINT ( 'NONE',  ( 208.9149999999999920, 30.98800000000000310, 44.45000000000000284 ) ) ;
#14826 = CARTESIAN_POINT ( 'NONE',  ( 117.8019377669635190, -34.00081044253764162, 169.0365776568629599 ) ) ;
#14827 = CARTESIAN_POINT ( 'NONE',  ( 100.9411170126626587, -46.87412574091977291, 48.14419670448194211 ) ) ;
#14828 = CARTESIAN_POINT ( 'NONE',  ( 117.2345208925008109, -41.18012235578145663, 204.4861014663869696 ) ) ;
#14829 = DIRECTION ( 'NONE',  ( 1.000000000000000000, 9.408669700213195533E-16, 0.000000000000000000 ) ) ;
#14830 = CARTESIAN_POINT ( 'NONE',  ( 30.48091746481826192, -48.32844715994148999, 300.4678068554150059 ) ) ;
#14832 = DIRECTION ( 'NONE',  ( 1.000000000000000000, 4.163336342344333240E-14, 0.000000000000000000 ) ) ;
#14831 = CYLINDRICAL_SURFACE ( 'NONE', #39156, 1.000000000000000888 ) ;
#14833 = CARTESIAN_POINT ( 'NONE',  ( 109.7248659280113827, -27.00080518171892052, 69.86479194203108989 ) ) ;
#14834 = CARTESIAN_POINT ( 'NONE',  ( 144.0667039004811443, -140.6784471619068029, 245.4415720117440003 ) ) ;
#14835 = ORIENTED_EDGE ( 'NONE', *, *, #17689, .F. ) ;
#14836 = CARTESIAN_POINT ( 'NONE',  ( 40.31648329127299490, 12.92155284005730387, 355.9756252759109998 ) ) ;
#14837 = EDGE_CURVE ( 'NONE', #18507, #28799, #65016, .T. ) ;
#14838 = ORIENTED_EDGE ( 'NONE', *, *, #51929, .T. ) ;
#14839 = EDGE_CURVE ( 'NONE', #877, #23402, #16868, .T. ) ;
#14840 = ORIENTED_EDGE ( 'NONE', *, *, #16190, .T. ) ;
#14841 = ADVANCED_FACE ( 'NONE', ( #37311 ), #57525, .F. ) ;
#14843 = ORIENTED_EDGE ( 'NONE', *, *, #10985, .T. ) ;
#14842 = DIRECTION ( 'NONE',  ( 0.000000000000000000, 0.000000000000000000, -1.000000000000000000 ) ) ;
#14844 = CARTESIAN_POINT ( 'NONE',  ( 110.4495079430909357, -47.22796928374258130, 53.83657765686300678 ) ) ;
#14845 = DIRECTION ( 'NONE',  ( 0.1858654558203195195, -0.9825752044157765042, 0.000000000000000000 ) ) ;
#14846 = LINE ( 'NONE', #63424, #66006 ) ;
#14847 = EDGE_CURVE ( 'NONE', #33225, #16017, #2799, .T. ) ;
#14848 = CARTESIAN_POINT ( 'NONE',  ( 98.63080892621665896, -30.47026088752560824, 176.8184824187679567 ) ) ;
#14849 = AXIS2_PLACEMENT_3D ( 'NONE', #80734, #18484, #11690 ) ;
#14850 = CARTESIAN_POINT ( 'NONE',  ( 98.20387719113243463, -34.86749027545791080, 260.5962293518865636 ) ) ;
#14851 = ORIENTED_EDGE ( 'NONE', *, *, #60535, .F. ) ;
#14852 = ORIENTED_EDGE ( 'NONE', *, *, #40949, .T. ) ;
#14853 = ORIENTED_EDGE ( 'NONE', *, *, #79427, .T. ) ;
#14854 = ADVANCED_FACE ( 'NONE', ( #85032 ), #29600, .T. ) ;
#14855 = AXIS2_PLACEMENT_3D ( 'NONE', #49366, #77102, #70273 ) ;
#14856 = EDGE_LOOP ( 'NONE', ( #40368, #33154, #4123, #80140 ) ) ;
#14857 = LINE ( 'NONE', #42968, #67444 ) ;
#14858 = FACE_OUTER_BOUND ( 'NONE', #81382, .T. ) ;
#14859 = CARTESIAN_POINT ( 'NONE',  ( -69.72411017812909506, 127.0000000000000000, -69.72411017813089984 ) ) ;
#14860 = CARTESIAN_POINT ( 'NONE',  ( 188.5667039024479834, -67.87844715994100397, 173.2178068554149775 ) ) ;
#14861 = CARTESIAN_POINT ( 'NONE',  ( 100.8594679592200833, 82.54999999999999716, 82.89895571708400723 ) ) ;
#14862 = LINE ( 'NONE', #63440, #84320 ) ;
#14863 = EDGE_CURVE ( 'NONE', #45672, #66449, #53137, .T. ) ;
#14864 = CARTESIAN_POINT ( 'NONE',  ( 32.25690895536984470, -33.54226604285049262, 117.4678068554150485 ) ) ;
#14865 = FACE_OUTER_BOUND ( 'NONE', #38446, .T. ) ;
#14866 = CARTESIAN_POINT ( 'NONE',  ( 118.0525141433398773, -37.71481444994964960, 33.74324432352998571 ) ) ;
#14867 = DIRECTION ( 'NONE',  ( 0.000000000000000000, -1.000000000000000000, 0.000000000000000000 ) ) ;
#14870 = EDGE_LOOP ( 'NONE', ( #8174, #45344, #70957, #8858 ) ) ;
#14869 = ADVANCED_FACE ( 'NONE', ( #58626 ), #85927, .F. ) ;
#14868 = AXIS2_PLACEMENT_3D ( 'NONE', #4904, #32593, #46207 ) ;
#14871 = DIRECTION ( 'NONE',  ( 2.900000000000000265E-14, -2.000000000000000155E-15, 1.000000000000000000 ) ) ;
#14872 = FACE_BOUND ( 'NONE', #49170, .T. ) ;
#14873 = CARTESIAN_POINT ( 'NONE',  ( 115.1946057043837328, -37.48001498139237953, 76.57094751244896713 ) ) ;
#14874 = VECTOR ( 'NONE', #11080, 1000.000000000000114 ) ;
#14875 = CYLINDRICAL_SURFACE ( 'NONE', #39752, 1.999999999999995781 ) ;
#14876 = CIRCLE ( 'NONE', #17775, 0.5000000000000004441 ) ;
#14877 = FACE_OUTER_BOUND ( 'NONE', #14347, .T. ) ;
#14878 = VERTEX_POINT ( 'NONE', #72285 ) ;
#14879 = ORIENTED_EDGE ( 'NONE', *, *, #54997, .T. ) ;
#14880 = CARTESIAN_POINT ( 'NONE',  ( 108.3336695260893094, -46.73483522987581296, 137.6750204624211733 ) ) ;
#14881 = ORIENTED_EDGE ( 'NONE', *, *, #24337, .F. ) ;
#14882 = VERTEX_POINT ( 'NONE', #44996 ) ;
#14883 = CARTESIAN_POINT ( 'NONE',  ( 115.7125814391468737, -38.67428926243481158, 145.0815833058969702 ) ) ;
#14884 = CARTESIAN_POINT ( 'NONE',  ( -10.78716141056406208, 89.26551436951578467, 118.0644550036098224 ) ) ;
#14885 = EDGE_CURVE ( 'NONE', #46008, #39822, #10054, .T. ) ;
#14886 = CARTESIAN_POINT ( 'NONE',  ( 108.3220630915710530, -47.10059840840933987, 113.6727681330539639 ) ) ;
#14887 = DIRECTION ( 'NONE',  ( 1.000000000000000078E-15, -1.000000000000000000, 0.000000000000000000 ) ) ;
#14888 = ORIENTED_EDGE ( 'NONE', *, *, #85729, .T. ) ;
#14889 = VERTEX_POINT ( 'NONE', #86362 ) ;
#14890 = VERTEX_POINT ( 'NONE', #8726 ) ;
#14892 = CARTESIAN_POINT ( 'NONE',  ( 130.5667039024479834, -36.72944715994093912, 239.5838068554170377 ) ) ;
#14891 = AXIS2_PLACEMENT_3D ( 'NONE', #78076, #43517, #36730 ) ;
#14893 = ORIENTED_EDGE ( 'NONE', *, *, #43004, .F. ) ;
#14894 = CARTESIAN_POINT ( 'NONE',  ( 97.21286698537356585, -39.96429565625729907, 286.5908633711495668 ) ) ;
#14895 = CARTESIAN_POINT ( 'NONE',  ( 113.5786777234211939, -44.94349119991360197, 164.1099109901969655 ) ) ;
#14896 = CARTESIAN_POINT ( 'NONE',  ( 193.0371591254586008, -47.82818131005411999, 193.9678068554150343 ) ) ;
#14897 = LINE ( 'NONE', #15344, #11153 ) ;
#14898 = CARTESIAN_POINT ( 'NONE',  ( 97.83606632657298974, -31.88363555591887533, 131.9413395616259947 ) ) ;
#14899 = DIRECTION ( 'NONE',  ( 0.000000000000000000, 0.000000000000000000, 1.000000000000000000 ) ) ;
#14900 = ORIENTED_EDGE ( 'NONE', *, *, #33359, .F. ) ;
#14901 = CARTESIAN_POINT ( 'NONE',  ( 25.56670390244797275, -67.87844715994100397, 132.3428068554150343 ) ) ;
#14902 = EDGE_CURVE ( 'NONE', #48061, #63918, #63302, .T. ) ;
#14903 = ORIENTED_EDGE ( 'NONE', *, *, #72157, .T. ) ;
#14904 = CARTESIAN_POINT ( 'NONE',  ( 20.03715912545826328, -46.82818131006190043, 237.4678068554150059 ) ) ;
#14905 = ORIENTED_EDGE ( 'NONE', *, *, #23526, .F. ) ;
#14906 = AXIS2_PLACEMENT_3D ( 'NONE', #66353, #46791, #11855 ) ;
#14907 = EDGE_CURVE ( 'NONE', #78010, #5742, #35632, .T. ) ;
#14908 = CARTESIAN_POINT ( 'NONE',  ( 89.60916260784479448, 238.5000000000000000, 134.1927865330827103 ) ) ;
#14909 = LINE ( 'NONE', #42572, #58047 ) ;
#14910 = CARTESIAN_POINT ( 'NONE',  ( 115.6114045197296178, -28.51818617053012161, 39.43562527591099354 ) ) ;
#14911 = CARTESIAN_POINT ( 'NONE',  ( 117.8738102209308920, 82.54999999999999716, -12.69999999999876827 ) ) ;
#14912 = CARTESIAN_POINT ( 'NONE',  ( 108.0667039024470171, -87.35579742913164125, -19.26696060647653397 ) ) ;
#14913 = LINE ( 'NONE', #77578, #49935 ) ;
#14914 = CARTESIAN_POINT ( 'NONE',  ( 111.0600676157742726, -27.80113716294804505, 24.74133956162494030 ) ) ;
#14916 = CARTESIAN_POINT ( 'NONE',  ( 105.3199149336540046, -48.42511963160323774, 143.4584824187689662 ) ) ;
#14915 = CYLINDRICAL_SURFACE ( 'NONE', #62309, 9.999999999999998224 ) ;
#14917 = FACE_BOUND ( 'NONE', #64909, .T. ) ;
#14918 = LINE ( 'NONE', #78499, #49593 ) ;
#14919 = VERTEX_POINT ( 'NONE', #25015 ) ;
#14920 = LINE ( 'NONE', #83504, #12066 ) ;
#14921 = CARTESIAN_POINT ( 'NONE',  ( 109.6604454188727402, 49.07786898089018734, 70.84811965973803183 ) ) ;
#14922 = DIRECTION ( 'NONE',  ( 1.000000000000000000, 0.000000000000000000, 2.108231265501709878E-16 ) ) ;
#14923 = ORIENTED_EDGE ( 'NONE', *, *, #9101, .F. ) ;
#14924 = PLANE ( 'NONE',  #82471 ) ;
#14926 = ORIENTED_EDGE ( 'NONE', *, *, #58792, .F. ) ;
#14925 = CARTESIAN_POINT ( 'NONE',  ( 115.0734612967709722, -29.04171753102041365, 189.4232443235299570 ) ) ;
#14927 = DIRECTION ( 'NONE',  ( 0.000000000000000000, 0.000000000000000000, 1.000000000000000000 ) ) ;
#14928 = CARTESIAN_POINT ( 'NONE',  ( 96.66048121734328902, -35.80620304765527351, 227.2556252759109725 ) ) ;
#14929 = CARTESIAN_POINT ( 'NONE',  ( 101.1169593292293598, -28.07258979649007102, 46.55562527591094835 ) ) ;
#14930 = CARTESIAN_POINT ( 'NONE',  ( 29.77381068363477112, -48.62134037875501491, 300.4678068554150059 ) ) ;
#14931 = CARTESIAN_POINT ( 'NONE',  ( 95.60734603896362671, -36.72944715994100306, 293.2242906452868851 ) ) ;
#14932 = DIRECTION ( 'NONE',  ( 2.775557561562888827E-14, -1.000000000000000000, 0.000000000000000000 ) ) ;
#14933 = EDGE_LOOP ( 'NONE', ( #56234, #50532 ) ) ;
#14934 = VECTOR ( 'NONE', #50067, 1000.000000000000000 ) ;
#14935 = EDGE_CURVE ( 'NONE', #53803, #53776, #47227, .T. ) ;
#14936 = EDGE_LOOP ( 'NONE', ( #74851, #58832 ) ) ;
#14937 = ADVANCED_FACE ( 'NONE', ( #87251 ), #73606, .T. ) ;
#14938 = EDGE_LOOP ( 'NONE', ( #57231, #35001, #27329, #12496 ) ) ;
#14939 = AXIS2_PLACEMENT_3D ( 'NONE', #1521, #22410, #50087 ) ;
#14940 = EDGE_CURVE ( 'NONE', #31872, #39210, #11836, .T. ) ;
#14941 = ORIENTED_EDGE ( 'NONE', *, *, #55507, .F. ) ;
#14942 = CARTESIAN_POINT ( 'NONE',  ( -74.15067561874319324, 127.0000000000000000, 68.53801554307369770 ) ) ;
#14943 = CARTESIAN_POINT ( 'NONE',  ( 101.6506511131177461, -45.63737897744897509, 243.1413395616249886 ) ) ;
#14944 = DIRECTION ( 'NONE',  ( 3.100000000000000258E-29, -3.100000000000000044E-14, -1.000000000000000000 ) ) ;
#14945 = CARTESIAN_POINT ( 'NONE',  ( 134.8111839727964139, -16.08035908359601507, 1.709393751552864993 ) ) ;
#14946 = ADVANCED_FACE ( 'NONE', ( #4575 ), #25914, .T. ) ;
#14948 = CYLINDRICAL_SURFACE ( 'NONE', #19597, 7.937500000000000000 ) ;
#14947 = DIRECTION ( 'NONE',  ( 0.000000000000000000, 1.000000000000000000, 0.000000000000000000 ) ) ;
#14949 = CARTESIAN_POINT ( 'NONE',  ( 91.06648329127391150, -36.72944715993925513, -5.074374724089045330 ) ) ;
#14950 = CARTESIAN_POINT ( 'NONE',  ( 104.2349294074198411, -46.78572220631293277, 22.35848241876792031 ) ) ;
#14951 = ORIENTED_EDGE ( 'NONE', *, *, #84885, .F. ) ;
#14952 = ORIENTED_EDGE ( 'NONE', *, *, #55209, .T. ) ;
#14953 = EDGE_CURVE ( 'NONE', #70548, #87213, #59957, .T. ) ;
#14954 = SURFACE_STYLE_USAGE ( .BOTH. , #43526 ) ;
#14955 = CARTESIAN_POINT ( 'NONE',  ( 97.78098940324528598, -40.44159231346958450, 17.62882595293030619 ) ) ;
#14956 = CARTESIAN_POINT ( 'NONE',  ( 107.2379402074490855, -25.61267671046461558, 226.0641967044819580 ) ) ;
#14957 = EDGE_CURVE ( 'NONE', #24976, #2162, #12798, .T. ) ;
#14958 = DIRECTION ( 'NONE',  ( 4.012088370409549976E-14, -1.000000000000000000, 0.000000000000000000 ) ) ;
#14959 = CIRCLE ( 'NONE', #25057, 2.517500000000005844 ) ;
#14960 = CARTESIAN_POINT ( 'NONE',  ( 116.5944731948637809, -42.45914096480943556, 124.3956252759109731 ) ) ;
#14961 = CARTESIAN_POINT ( 'NONE',  ( -479.3614999999999782, 7.143750000000339995, 6.988054014476278830 ) ) ;
#14962 = CARTESIAN_POINT ( 'NONE',  ( 103.2794297788319966, -27.47427420437042755, 21.38554664520359694 ) ) ;
#14963 = VERTEX_POINT ( 'NONE', #12737 ) ;
#14964 = DIRECTION ( 'NONE',  ( 0.000000000000000000, 0.000000000000000000, -1.000000000000000000 ) ) ;
#14965 = EDGE_LOOP ( 'NONE', ( #51442, #55438, #12986, #29966 ) ) ;
#14966 = ORIENTED_EDGE ( 'NONE', *, *, #48849, .T. ) ;
#14967 = DIRECTION ( 'NONE',  ( 0.000000000000000000, -0.5000000000000003331, -0.8660254037844384856 ) ) ;
#14968 = CARTESIAN_POINT ( 'NONE',  ( 101.7809741706781921, -43.87965855000975068, 253.5015833058971850 ) ) ;
#14969 = CARTESIAN_POINT ( 'NONE',  ( 105.7154772450396081, -46.72385838138438174, 192.4689586024476853 ) ) ;
#14970 = CYLINDRICAL_SURFACE ( 'NONE', #81259, 4.874999999999990230 ) ;
#14971 = CARTESIAN_POINT ( 'NONE',  ( 255.9983484187079910, 40.03750000000000142, -2.032000000000000028 ) ) ;
#14972 = CARTESIAN_POINT ( 'NONE',  ( 80.31601416995117404, 70.80054593973557076, -87.20837843453648475 ) ) ;
#14973 = ORIENTED_EDGE ( 'NONE', *, *, #22510, .T. ) ;
#14974 = DIRECTION ( 'NONE',  ( -0.8660254037844382635, -0.5000000000000008882, 1.550000000000000022E-14 ) ) ;
#14975 = CARTESIAN_POINT ( 'NONE',  ( 105.7142056743471557, -46.72366556389629011, 183.4694020350319477 ) ) ;
#14976 = ORIENTED_EDGE ( 'NONE', *, *, #8436, .T. ) ;
#14977 = CARTESIAN_POINT ( 'NONE',  ( 118.7327907441706571, -34.64671908090114272, 48.96705384733895983 ) ) ;
#14978 = VERTEX_POINT ( 'NONE', #17756 ) ;
#14979 = CARTESIAN_POINT ( 'NONE',  ( 98.53948418117370522, -33.67937232826720617, 25.48765792331497693 ) ) ;
#14980 = CARTESIAN_POINT ( 'NONE',  ( 71.06648329127399677, -8.729447159940999512, 284.9256252759119548 ) ) ;
#14981 = CARTESIAN_POINT ( 'NONE',  ( 116.8150918559700813, -40.26546416881835455, 173.5375300378159693 ) ) ;
#14982 = CARTESIAN_POINT ( 'NONE',  ( 41.56648329127499153, -36.32844715994070839, 258.9256252759120116 ) ) ;
#14983 = CARTESIAN_POINT ( 'NONE',  ( 86.06670390244796920, -48.82844715994099971, 198.9178068554149945 ) ) ;
#14984 = DIRECTION ( 'NONE',  ( -0.8660254037844387076, 0.4999999999999998890, 0.000000000000000000 ) ) ;
#14985 = EDGE_CURVE ( 'NONE', #16276, #56405, #46326, .T. ) ;
#14986 = CARTESIAN_POINT ( 'NONE',  ( 68.87418703512655327, -69.52506677730903561, 247.4937269829859758 ) ) ;
#14987 = CARTESIAN_POINT ( 'NONE',  ( 115.3579863298411254, -45.26537652146382840, 264.1899109901965517 ) ) ;
#14988 = CARTESIAN_POINT ( 'NONE',  ( 87.71311422381590717, 93.94553785444269067, -79.76258624986799362 ) ) ;
#14989 = VERTEX_POINT ( 'NONE', #81784 ) ;
#14990 = AXIS2_PLACEMENT_3D ( 'NONE', #72563, #78502, #16261 ) ;
#14991 = DIRECTION ( 'NONE',  ( 0.7071067811865389130, 0.000000000000000000, 0.7071067811865561215 ) ) ;
#14992 = ORIENTED_EDGE ( 'NONE', *, *, #24770, .F. ) ;
#14993 = CARTESIAN_POINT ( 'NONE',  ( 99.65376319600918009, -46.03872712633670972, 118.0413395616259606 ) ) ;
#14994 = DIRECTION ( 'NONE',  ( 1.000000000000000078E-15, 1.000000000000000083E-30, -1.000000000000000000 ) ) ;
#14995 = VERTEX_POINT ( 'NONE', #81351 ) ;
#14996 = ORIENTED_EDGE ( 'NONE', *, *, #16535, .T. ) ;
#14997 = ORIENTED_EDGE ( 'NONE', *, *, #70535, .F. ) ;
#14998 = CARTESIAN_POINT ( 'NONE',  ( 116.8171228694637733, -34.15291832781043979, 124.0314586086284692 ) ) ;
#14999 = CARTESIAN_POINT ( 'NONE',  ( 113.2455016744213765, -28.75867540999941241, 265.5522916365027299 ) ) ;
#15000 = DIRECTION ( 'NONE',  ( 3.340531404218880531E-13, -1.000000000000000000, 3.350531404218880242E-28 ) ) ;
#15001 = CARTESIAN_POINT ( 'NONE',  ( 163.0959832912770082, -23.42844715993521021, 313.9678068554149490 ) ) ;
#15002 = CARTESIAN_POINT ( 'NONE',  ( 41.56648329127398966, -18.82844715994071194, 138.9256252759119832 ) ) ;
#15003 = CARTESIAN_POINT ( 'NONE',  ( 118.0831039394318083, -37.62836316206458065, 34.77372051400695341 ) ) ;
#15004 = CARTESIAN_POINT ( 'NONE',  ( 131.0667039024480118, -43.72944715994093201, 231.5838068554170093 ) ) ;
#15005 = ORIENTED_EDGE ( 'NONE', *, *, #88579, .T. ) ;
#15006 = PLANE ( 'NONE',  #26830 ) ;
#15007 = CARTESIAN_POINT ( 'NONE',  ( 101.9936095392775712, -45.44606507104835202, 42.15594039548825123 ) ) ;
#15008 = ORIENTED_EDGE ( 'NONE', *, *, #56837, .F. ) ;
#15009 = EDGE_LOOP ( 'NONE', ( #79896, #18947, #7004, #46323 ) ) ;
#15010 = EDGE_CURVE ( 'NONE', #7509, #27470, #19090, .T. ) ;
#15011 = CARTESIAN_POINT ( 'NONE',  ( 82.67340060512943012, -19.60624470235704564, 2.902100967938844533 ) ) ;
#15012 = VECTOR ( 'NONE', #2319, 1000.000000000000000 ) ;
#15013 = DIRECTION ( 'NONE',  ( 0.000000000000000000, 0.000000000000000000, 1.000000000000000000 ) ) ;
#15014 = FACE_BOUND ( 'NONE', #21812, .T. ) ;
#15015 = CYLINDRICAL_SURFACE ( 'NONE', #4253, 2.117000000000000881 ) ;
#15016 = DIRECTION ( 'NONE',  ( 0.7071067811865671127, 0.7071067811865279218, 7.071067811865664660E-16 ) ) ;
#15017 = CARTESIAN_POINT ( 'NONE',  ( 101.2834890806669677, -28.93024170975123255, 185.0067055423629938 ) ) ;
#15018 = FACE_OUTER_BOUND ( 'NONE', #68595, .T. ) ;
#15019 = CARTESIAN_POINT ( 'NONE',  ( 125.1553824804045547, 69.48256747448400006, 37.16550212950143361 ) ) ;
#15020 = CARTESIAN_POINT ( 'NONE',  ( 108.9933628702935238, -47.01991853554855538, 82.72419670448194040 ) ) ;
#15021 = EDGE_LOOP ( 'NONE', ( #71099, #38880 ) ) ;
#15022 = LINE ( 'NONE', #70437, #53861 ) ;
#15023 = ORIENTED_EDGE ( 'NONE', *, *, #59717, .T. ) ;
#15024 = AXIS2_PLACEMENT_3D ( 'NONE', #22781, #85906, #23678 ) ;
#15025 = CARTESIAN_POINT ( 'NONE',  ( 103.3136250034697099, -27.46033481550304600, 276.3826084592540724 ) ) ;
#15026 = VERTEX_POINT ( 'NONE', #5019 ) ;
#15027 = CARTESIAN_POINT ( 'NONE',  ( 105.7993347760366021, -26.72405582829313531, 50.17730648672989702 ) ) ;
#15028 = ORIENTED_EDGE ( 'NONE', *, *, #41444, .T. ) ;
#15029 = LINE ( 'NONE', #22754, #42134 ) ;
#15030 = DIRECTION ( 'NONE',  ( 1.000000000000000000, 0.000000000000000000, 0.000000000000000000 ) ) ;
#15031 = CARTESIAN_POINT ( 'NONE',  ( 68.23087527387866658, -137.6857029198856992, 247.4029867184769955 ) ) ;
#15032 = AXIS2_PLACEMENT_3D ( 'NONE', #88503, #26256, #53934 ) ;
#15033 = CARTESIAN_POINT ( 'NONE',  ( -44.45000000000000284, 50.79999999999999716, 257.1750000000000114 ) ) ;
#15034 = ORIENTED_EDGE ( 'NONE', *, *, #59782, .T. ) ;
#15035 = CARTESIAN_POINT ( 'NONE',  ( 96.93519779220999055, -32.25144590123284161, 55.98324432352897162 ) ) ;
#15036 =( LENGTH_UNIT ( ) NAMED_UNIT ( * ) SI_UNIT ( .MILLI., .METRE. ) );
#15038 = CARTESIAN_POINT ( 'NONE',  ( 131.0667039024480118, -58.35344715994099829, 234.8338068554150198 ) ) ;
#15037 = CARTESIAN_POINT ( 'NONE',  ( 109.7241730775608062, -27.00061873284944269, 164.8648492007025652 ) ) ;
#15039 = CARTESIAN_POINT ( 'NONE',  ( 179.1667039024475230, -28.27351298636771659, 237.4678068554150059 ) ) ;
#15040 = CARTESIAN_POINT ( 'NONE',  ( 98.30753417366616986, -41.72887546178495910, 141.7397919399187458 ) ) ;
#15041 = ORIENTED_EDGE ( 'NONE', *, *, #66403, .F. ) ;
#15042 = ADVANCED_FACE ( 'NONE', ( #26356 ), #5473, .T. ) ;
#15043 = EDGE_CURVE ( 'NONE', #35953, #47474, #74520, .T. ) ;
#15044 = CARTESIAN_POINT ( 'NONE',  ( 110.0236307522814911, -27.14727356840723971, 120.8367254748248598 ) ) ;
#15045 = CARTESIAN_POINT ( 'NONE',  ( 170.2205283966864897, 101.5999999999999943, -71.37400000000000944 ) ) ;
#15046 = EDGE_CURVE ( 'NONE', #39094, #29668, #50752, .T. ) ;
#15047 = CARTESIAN_POINT ( 'NONE',  ( -31.75000000000000000, 24.56180297284579694, 3.175000000000219647 ) ) ;
#15048 = CARTESIAN_POINT ( 'NONE',  ( 117.6299819888065912, -33.39812594883869679, 125.0575300378149706 ) ) ;
#15049 = EDGE_CURVE ( 'NONE', #83484, #5931, #20842, .T. ) ;
#15051 = FACE_OUTER_BOUND ( 'NONE', #71151, .T. ) ;
#15050 = DIRECTION ( 'NONE',  ( 0.9347835805883503157, 0.000000000000000000, -0.3552177606235690788 ) ) ;
#15052 = DIRECTION ( 'NONE',  ( -1.907762142705490052E-15, -7.167082501179359715E-16, 1.000000000000000000 ) ) ;
#15053 = AXIS2_PLACEMENT_3D ( 'NONE', #4854, #61590, #54309 ) ;
#15054 = ORIENTED_EDGE ( 'NONE', *, *, #61694, .F. ) ;
#15055 = AXIS2_PLACEMENT_3D ( 'NONE', #70884, #9099, #8654 ) ;
#15056 = DIRECTION ( 'NONE',  ( 0.4999999999999986122, 0.000000000000000000, 0.8660254037844394848 ) ) ;
#15057 = CARTESIAN_POINT ( 'NONE',  ( 116.9310496459149391, -33.53114825773884178, 130.0880062282909648 ) ) ;
#15058 = EDGE_CURVE ( 'NONE', #9292, #82261, #35393, .T. ) ;
#15060 = ORIENTED_EDGE ( 'NONE', *, *, #62433, .F. ) ;
#15059 = LINE ( 'NONE', #62294, #76161 ) ;
#15061 = CARTESIAN_POINT ( 'NONE',  ( 97.63514171170974976, -41.12017164899855715, 252.6727681330536655 ) ) ;
#15062 = DIRECTION ( 'NONE',  ( 0.000000000000000000, 1.000000000000000000, 0.000000000000000000 ) ) ;
#15063 = CARTESIAN_POINT ( 'NONE',  ( 172.5664832912740110, -36.32844715994070839, 83.67562527591201160 ) ) ;
#15064 = LINE ( 'NONE', #71381, #24092 ) ;
#15065 = PLANE ( 'NONE',  #45643 ) ;
#15066 = CARTESIAN_POINT ( 'NONE',  ( 226.4410000000000025, 52.73749999999999716, -56.89600000000000080 ) ) ;
#15067 = DIRECTION ( 'NONE',  ( -1.000000000000000000, -1.541976423090496028E-15, 0.000000000000000000 ) ) ;
#15068 = CARTESIAN_POINT ( 'NONE',  ( 117.2759483237920080, -34.91131378075001379, 198.9546728949589749 ) ) ;
#15069 = ORIENTED_EDGE ( 'NONE', *, *, #77282, .T. ) ;
#15070 = VERTEX_POINT ( 'NONE', #82240 ) ;
#15071 = CARTESIAN_POINT ( 'NONE',  ( 99.43677639672335999, -41.29559517668970869, 158.1872975916109567 ) ) ;
#15072 = CIRCLE ( 'NONE', #22121, 0.5000000000000004441 ) ;
#15073 = CARTESIAN_POINT ( 'NONE',  ( 163.0667039024470171, -33.35206098992711077, 342.9256252759119548 ) ) ;
#15074 = CARTESIAN_POINT ( 'NONE',  ( 111.4279401658702682, -28.40658880358809668, 11.11205949637394852 ) ) ;
#15075 = VECTOR ( 'NONE', #78075, 999.9999999999998863 ) ;
#15076 = CARTESIAN_POINT ( 'NONE',  ( 162.5667039024470171, -32.29483332968611364, 117.4678068554150485 ) ) ;
#15077 = CARTESIAN_POINT ( 'NONE',  ( 167.6524903400753885, -49.32844715993521589, 249.9678068554149775 ) ) ;
#15078 = DIRECTION ( 'NONE',  ( 0.000000000000000000, 0.000000000000000000, -1.000000000000000000 ) ) ;
#15079 = AXIS2_PLACEMENT_3D ( 'NONE', #26670, #13058, #88471 ) ;
#15080 = DIRECTION ( 'NONE',  ( -0.9254794337955623007, -0.3787978585227819162, 0.000000000000000000 ) ) ;
#15081 = CARTESIAN_POINT ( 'NONE',  ( -107.7702177616926065, 127.0000000000000000, -1.170464777364108012E-12 ) ) ;
#15082 = CARTESIAN_POINT ( 'NONE',  ( 96.14807755961376756, -35.16348456217429685, 226.2251490854349640 ) ) ;
#15083 = CARTESIAN_POINT ( 'NONE',  ( 8.321939743097969355, 92.04720212734648044, 118.0645406551164029 ) ) ;
#15084 = VERTEX_POINT ( 'NONE', #83570 ) ;
#15085 = EDGE_LOOP ( 'NONE', ( #86110, #30093, #53087, #47246 ) ) ;
#15086 = CARTESIAN_POINT ( 'NONE',  ( 112.0659116112372402, -45.48839626716342366, 87.98979194155364780 ) ) ;
#15087 = DIRECTION ( 'NONE',  ( 1.000000000000000000, 0.000000000000000000, 3.902639990948949304E-17 ) ) ;
#15088 = LINE ( 'NONE', #69154, #40306 ) ;
#15089 = CARTESIAN_POINT ( 'NONE',  ( -27.27158787008326968, 184.0000000000000000, 80.02307622376218887 ) ) ;
#15090 = EDGE_CURVE ( 'NONE', #17736, #33658, #62662, .T. ) ;
#15091 = CARTESIAN_POINT ( 'NONE',  ( 110.3395589168170545, -45.98151452051992294, 33.84705384733993583 ) ) ;
#15092 = DIRECTION ( 'NONE',  ( 0.000000000000000000, 0.000000000000000000, 1.000000000000000000 ) ) ;
#15093 = VERTEX_POINT ( 'NONE', #27697 ) ;
#15094 = CARTESIAN_POINT ( 'NONE',  ( 106.2487395568334421, -26.25713557174866253, 21.13848241876792144 ) ) ;
#15095 = LINE ( 'NONE', #53814, #58334 ) ;
#15096 = EDGE_CURVE ( 'NONE', #23774, #15841, #26665, .T. ) ;
#15097 = CARTESIAN_POINT ( 'NONE',  ( 115.2518872279481030, -30.21599423016839836, 244.3613395616249875 ) ) ;
#15098 = ORIENTED_EDGE ( 'NONE', *, *, #1498, .T. ) ;
#15099 = DIRECTION ( 'NONE',  ( 0.000000000000000000, -1.000000000000000000, 0.000000000000000000 ) ) ;
#15100 = LINE ( 'NONE', #82814, #19600 ) ;
#15101 = CARTESIAN_POINT ( 'NONE',  ( 108.3327516424870964, -46.73493878462306128, 167.6772798019345032 ) ) ;
#15102 = CARTESIAN_POINT ( 'NONE',  ( 98.91570299145236334, -37.17047609451836365, 74.18809036959095238 ) ) ;
#15103 = CARTESIAN_POINT ( 'NONE',  ( 116.3968524479345348, -41.42853965253563331, 199.4556252759109611 ) ) ;
#15104 = CARTESIAN_POINT ( 'NONE',  ( 0.000000000000000000, 127.0000000000000000, 85.23828826961327820 ) ) ;
#15105 = ORIENTED_EDGE ( 'NONE', *, *, #47383, .T. ) ;
#15106 = LINE ( 'NONE', #85517, #69743 ) ;
#15107 = ORIENTED_EDGE ( 'NONE', *, *, #64811, .T. ) ;
#15108 = ORIENTED_EDGE ( 'NONE', *, *, #53290, .T. ) ;
#15109 = VECTOR ( 'NONE', #68316, 1000.000000000000000 ) ;
#15110 = EDGE_CURVE ( 'NONE', #56957, #60012, #49009, .T. ) ;
#15111 = DIRECTION ( 'NONE',  ( 0.000000000000000000, 0.000000000000000000, 1.000000000000000000 ) ) ;
#15112 = VERTEX_POINT ( 'NONE', #48116 ) ;
#15113 = ORIENTED_EDGE ( 'NONE', *, *, #46264, .F. ) ;
#15114 = FACE_OUTER_BOUND ( 'NONE', #75080, .T. ) ;
#15115 = VECTOR ( 'NONE', #73196, 1000.000000000000000 ) ;
#15116 = B_SPLINE_CURVE_WITH_KNOTS ( 'NONE', 3,
 ( #27754, #55436, #84540, #83187, #48615, #77709, #8674, #7321, #56338, #28648, #35453, #84085, #36373, #21856, #22298, #29553, #22755, #76355 ),
 .UNSPECIFIED., .F., .F.,
 ( 4, 2, 2, 2, 2, 2, 2, 2, 4 ),
 ( 0.000000000000000000, 0.06250903880341492080, 0.1250180776068298416, 0.1875271164102447763, 0.2500361552136596832, 0.3125451940170745901, 0.3750542328204895526, 0.4375632716239044595, 0.5000723104273193664 ),
 .UNSPECIFIED. ) ;
#15117 = CARTESIAN_POINT ( 'NONE',  ( 97.80977108376971785, -40.51273747973604600, 42.63522248069732967 ) ) ;
#15118 = CARTESIAN_POINT ( 'NONE',  ( 116.7149163912777396, -35.64392129247566032, 83.33813411379098568 ) ) ;
#15119 = CARTESIAN_POINT ( 'NONE',  ( 96.54134661961150243, -40.18473915001016650, 286.5908633711491120 ) ) ;
#15120 = DIRECTION ( 'NONE',  ( -1.000000000000000000, -4.554376769437570034E-14, 0.000000000000000000 ) ) ;
#15121 = DIRECTION ( 'NONE',  ( 0.000000000000000000, 1.000000000000000000, -0.000000000000000000 ) ) ;
#15122 = ORIENTED_EDGE ( 'NONE', *, *, #83763, .T. ) ;
#15123 = EDGE_CURVE ( 'NONE', #74222, #44952, #34950, .T. ) ;
#15124 = VERTEX_POINT ( 'NONE', #55375 ) ;
#15125 = CARTESIAN_POINT ( 'NONE',  ( -492.0614999999999668, 93.66249999999999432, 90.48749999999999716 ) ) ;
#15126 = DIRECTION ( 'NONE',  ( -4.237773401492740281E-14, 1.000000000000000000, 0.000000000000000000 ) ) ;
#15127 = CARTESIAN_POINT ( 'NONE',  ( 70.74335932947460037, -139.3331411919284619, 247.4266426818775244 ) ) ;
#15128 = CARTESIAN_POINT ( 'NONE',  ( 114.2351621074132879, -44.22269940884951467, 113.1718157521019776 ) ) ;
#15129 = CARTESIAN_POINT ( 'NONE',  ( 98.05881815954255387, -31.39384645160161469, 85.90133956162493689 ) ) ;
#15131 = AXIS2_PLACEMENT_3D ( 'NONE', #69828, #7601, #34848 ) ;
#15130 = DIRECTION ( 'NONE',  ( 1.000000000000000000, 0.000000000000000000, 0.000000000000000000 ) ) ;
#15132 = ORIENTED_EDGE ( 'NONE', *, *, #20117, .F. ) ;
#15133 = UNCERTAINTY_MEASURE_WITH_UNIT (LENGTH_MEASURE( 1.000000000000000082E-05 ), #74466, 'distance_accuracy_value', 'NONE');
#15134 = CARTESIAN_POINT ( 'NONE',  ( 113.1001805014122255, -45.99085015462044623, 223.0480062282919675 ) ) ;
#15135 = AXIS2_PLACEMENT_3D ( 'NONE', #2424, #16944, #44623 ) ;
#15136 = AXIS2_PLACEMENT_3D ( 'NONE', #10238, #31114, #3425 ) ;
#15138 = SURFACE_STYLE_USAGE ( .BOTH. , #61475 ) ;
#15137 = CIRCLE ( 'NONE', #26724, 16.33514202138210791 ) ;
#15139 = DIRECTION ( 'NONE',  ( 1.000000000000000078E-15, -1.000000000000000083E-30, -1.000000000000000000 ) ) ;
#15141 = PLANE ( 'NONE',  #12281 ) ;
#15140 = LINE ( 'NONE', #77818, #30288 ) ;
#15142 = DIRECTION ( 'NONE',  ( 1.000000000000000000, 0.000000000000000000, 0.000000000000000000 ) ) ;
#15143 = DIRECTION ( 'NONE',  ( 0.000000000000000000, 0.000000000000000000, 1.000000000000000000 ) ) ;
#15144 = CARTESIAN_POINT ( 'NONE',  ( 1.663885868249273425, 95.14749804389164467, -118.5450564992233780 ) ) ;
#15145 = AXIS2_PLACEMENT_3D ( 'NONE', #22974, #14361, #42039 ) ;
#15146 = CARTESIAN_POINT ( 'NONE',  ( 182.3467384525650061, -36.02818131005800950, -5.074374724088000832 ) ) ;
#15147 = DIRECTION ( 'NONE',  ( 1.000000000000000000, 0.000000000000000000, 0.000000000000000000 ) ) ;
#15148 = ADVANCED_FACE ( 'NONE', ( #34048 ), #89486, .F. ) ;
#15149 = CARTESIAN_POINT ( 'NONE',  ( 97.06670390244703128, -109.9573555057410772, 19.21780685541815714 ) ) ;
#15151 = ORIENTED_EDGE ( 'NONE', *, *, #67570, .F. ) ;
#15150 = DIRECTION ( 'NONE',  ( 0.000000000000000000, 0.000000000000000000, -1.000000000000000000 ) ) ;
#15152 = CARTESIAN_POINT ( 'NONE',  ( 119.9305508289311888, -128.6589936823970106, 250.2178068554180470 ) ) ;
#15153 = CARTESIAN_POINT ( 'NONE',  ( 96.49566810458604493, -31.31724962161759507, 245.9499109901969689 ) ) ;
#15154 = CARTESIAN_POINT ( 'NONE',  ( 116.9041476981693677, -40.17949737190902937, 129.5584824187679658 ) ) ;
#15155 = CARTESIAN_POINT ( 'NONE',  ( 118.3880299729056276, -33.06406546148816261, 280.0756252759109657 ) ) ;
#15156 = FACE_OUTER_BOUND ( 'NONE', #54490, .T. ) ;
#15158 = CARTESIAN_POINT ( 'NONE',  ( 82.77273044669095725, -36.23917853419808210, 6.814128304791553070 ) ) ;
#15157 = LINE ( 'NONE', #78294, #2927 ) ;
#15159 = CARTESIAN_POINT ( 'NONE',  ( 177.8371591254543205, -47.82818131005477369, 300.4678068554149490 ) ) ;
#15160 = ORIENTED_EDGE ( 'NONE', *, *, #41027, .T. ) ;
#15161 = DIRECTION ( 'NONE',  ( 0.000000000000000000, 0.000000000000000000, 1.000000000000000000 ) ) ;
#15162 = ORIENTED_EDGE ( 'NONE', *, *, #19149, .F. ) ;
#15163 = CARTESIAN_POINT ( 'NONE',  ( 115.5545030166667146, -32.01519760825960503, 178.6524198280769724 ) ) ;
#15164 = ADVANCED_FACE ( 'NONE', ( #76746 ), #14528, .F. ) ;
#15166 = EDGE_LOOP ( 'NONE', ( #52501, #60148, #42608, #5339 ) ) ;
#15165 = DIRECTION ( 'NONE',  ( 4.299999999999999979E-14, -1.000000000000000000, 4.400000000000000367E-29 ) ) ;
#15167 = DIRECTION ( 'NONE',  ( 0.000000000000000000, 0.000000000000000000, 1.000000000000000000 ) ) ;
#15168 = CARTESIAN_POINT ( 'NONE',  ( 117.4047238282098249, -30.98758422922437106, 175.2299109901969700 ) ) ;
#15169 = CARTESIAN_POINT ( 'NONE',  ( 109.6407380183136837, -46.48065911288304619, 148.7819440279659489 ) ) ;
#15170 = EDGE_CURVE ( 'NONE', #58498, #77150, #13638, .T. ) ;
#15171 = CARTESIAN_POINT ( 'NONE',  ( 104.0667030381801936, -67.87844715994094713, 173.2178086137559774 ) ) ;
#15172 = CARTESIAN_POINT ( 'NONE',  ( 97.31540730480230650, -39.30489313201859858, 87.53094125324652452 ) ) ;
#15173 = CYLINDRICAL_SURFACE ( 'NONE', #53377, 3.299999999999997158 ) ;
#15174 = CYLINDRICAL_SURFACE ( 'NONE', #17868, 0.5000000000000172085 ) ;
#15175 = CARTESIAN_POINT ( 'NONE',  ( 97.28626111821314737, -36.62605694204433604, 111.3184824187689657 ) ) ;
#15176 = VERTEX_POINT ( 'NONE', #28585 ) ;
#15177 = ORIENTED_EDGE ( 'NONE', *, *, #45132, .T. ) ;
#15178 = ORIENTED_EDGE ( 'NONE', *, *, #84720, .F. ) ;
#15179 = AXIS2_PLACEMENT_3D ( 'NONE', #66297, #4536, #32224 ) ;
#15180 = CARTESIAN_POINT ( 'NONE',  ( 98.47292639957201743, -32.93111785796080682, 52.41491663922997901 ) ) ;
#15181 = CARTESIAN_POINT ( 'NONE',  ( 125.0664851986225159, -56.72944715994101728, 14.92562527591098842 ) ) ;
#15183 = CARTESIAN_POINT ( 'NONE',  ( 99.04406193110015977, -42.84125773391240699, 36.84395861861840871 ) ) ;
#15182 = CARTESIAN_POINT ( 'NONE',  ( 98.91665286848252947, -30.31703347128394910, 196.8080062282909637 ) ) ;
#15184 = CIRCLE ( 'NONE', #25279, 2.116999999999980009 ) ;
#15185 = FACE_OUTER_BOUND ( 'NONE', #63484, .T. ) ;
#15186 = CARTESIAN_POINT ( 'NONE',  ( 163.0664832912739826, 19.62155284005901024, 330.1506252759110680 ) ) ;
#15187 = DIRECTION ( 'NONE',  ( 0.000000000000000000, 0.000000000000000000, -1.000000000000000000 ) ) ;
#15188 = DIRECTION ( 'NONE',  ( 0.000000000000000000, 0.000000000000000000, -1.000000000000000000 ) ) ;
#15189 = CARTESIAN_POINT ( 'NONE',  ( 67.06824679800834588, -67.87939406239482310, 245.5735631681239397 ) ) ;
#15190 = CARTESIAN_POINT ( 'NONE',  ( 101.5125196766230289, -27.93273449574867229, 110.5241967044819944 ) ) ;
#15191 = ORIENTED_EDGE ( 'NONE', *, *, #30986, .T. ) ;
#15192 = ORIENTED_EDGE ( 'NONE', *, *, #43096, .T. ) ;
#15193 = ORIENTED_EDGE ( 'NONE', *, *, #72427, .F. ) ;
#15194 = CARTESIAN_POINT ( 'NONE',  ( 9.720633968232110273E-16, 117.4749999999999943, -111.1250000000000000 ) ) ;
#15195 = CARTESIAN_POINT ( 'NONE',  ( -48.02966122971776741, 353.0471713899363522, 75.53254848357481421 ) ) ;
#15196 = CARTESIAN_POINT ( 'NONE',  ( 97.31313350590980349, -38.96086997259878615, 131.5054597300594423 ) ) ;
#15197 = DIRECTION ( 'NONE',  ( -1.000000000000000000, -4.299999999999999979E-14, -1.000000000000000078E-15 ) ) ;
#15198 = CARTESIAN_POINT ( 'NONE',  ( 99.23015118009998048, -40.40270512654389279, 209.4814237029249568 ) ) ;
#15199 = VECTOR ( 'NONE', #67704, 1000.000000000000000 ) ;
#15200 = VECTOR ( 'NONE', #38607, 1000.000000000000000 ) ;
#15201 = DIRECTION ( 'NONE',  ( -1.000000000000000078E-15, 1.000000000000000083E-30, 1.000000000000000000 ) ) ;
#15202 = AXIS2_PLACEMENT_3D ( 'NONE', #59832, #87563, #52990 ) ;
#15203 = VECTOR ( 'NONE', #42476, 1000.000000000000000 ) ;
#15204 = EDGE_CURVE ( 'NONE', #2549, #18180, #84021, .T. ) ;
#15205 = DIRECTION ( 'NONE',  ( -1.000000000000000078E-15, 1.000000000000000000, 0.000000000000000000 ) ) ;
#15206 = VERTEX_POINT ( 'NONE', #49465 ) ;
#15208 = ORIENTED_EDGE ( 'NONE', *, *, #31641, .T. ) ;
#15207 = ORIENTED_EDGE ( 'NONE', *, *, #46643, .T. ) ;
#15209 = VECTOR ( 'NONE', #55992, 1000.000000000000114 ) ;
#15210 = VECTOR ( 'NONE', #45416, 1000.000000000000000 ) ;
#15211 = DIRECTION ( 'NONE',  ( 0.000000000000000000, -1.000000000000000000, 0.000000000000000000 ) ) ;
#15212 = ORIENTED_EDGE ( 'NONE', *, *, #58715, .F. ) ;
#15213 = ORIENTED_EDGE ( 'NONE', *, *, #41855, .T. ) ;
#15214 = LINE ( 'NONE', #20682, #43436 ) ;
#15215 = FACE_OUTER_BOUND ( 'NONE', #12590, .T. ) ;
#15216 = CARTESIAN_POINT ( 'NONE',  ( 114.5371455856629694, -43.48665885088448135, 229.6730118773259619 ) ) ;
#15217 = DIRECTION ( 'NONE',  ( 9.713237310806269221E-16, 0.000000000000000000, -1.000000000000000000 ) ) ;
#15218 = ORIENTED_EDGE ( 'NONE', *, *, #56331, .T. ) ;
#15219 = FACE_OUTER_BOUND ( 'NONE', #88697, .T. ) ;
#15220 = FACE_OUTER_BOUND ( 'NONE', #83704, .T. ) ;
#15221 = VERTEX_POINT ( 'NONE', #77204 ) ;
#15222 = VERTEX_POINT ( 'NONE', #68143 ) ;
#15223 = EDGE_CURVE ( 'NONE', #82107, #62559, #55617, .T. ) ;
#15224 = DIRECTION ( 'NONE',  ( 0.8660254037844390407, 0.000000000000000000, -0.4999999999999995004 ) ) ;
#15225 = ORIENTED_EDGE ( 'NONE', *, *, #24887, .T. ) ;
#15226 = EDGE_LOOP ( 'NONE', ( #86021, #2447, #48391, #73749, #61310, #59737 ) ) ;
#15227 = VECTOR ( 'NONE', #51524, 1000.000000000000114 ) ;
#15228 = EDGE_CURVE ( 'NONE', #37616, #85174, #89034, .T. ) ;
#15229 = CARTESIAN_POINT ( 'NONE',  ( 98.82205551832399237, -39.36200594543229414, 279.3785665600675543 ) ) ;
#15230 = ADVANCED_FACE ( 'NONE', ( #51251, #79447 ), #16315, .F. ) ;
#15231 = CARTESIAN_POINT ( 'NONE',  ( 96.59657429157336139, -36.21044007025302136, 171.2870538473399620 ) ) ;
#15232 = CARTESIAN_POINT ( 'NONE',  ( 103.2867953297129588, -47.09177226061144239, 97.28610146638693834 ) ) ;
#15233 = DIRECTION ( 'NONE',  ( 1.000000000000000000, 3.999999999999999995E-14, 1.000000000000000078E-15 ) ) ;
#15234 = CARTESIAN_POINT ( 'NONE',  ( 176.5667039024485518, -48.82844715993482509, 180.4678068554150059 ) ) ;
#15235 = CARTESIAN_POINT ( 'NONE',  ( 97.16978355702093495, -40.00630874038032658, 237.5813395616249579 ) ) ;
#15236 = DIRECTION ( 'NONE',  ( 0.000000000000000000, 0.000000000000000000, 1.000000000000000000 ) ) ;
#15237 = CARTESIAN_POINT ( 'NONE',  ( 41.56670390244689628, -36.32844715994109208, 180.4678068554150911 ) ) ;
#15238 = ORIENTED_EDGE ( 'NONE', *, *, #11663, .T. ) ;
#15239 = CARTESIAN_POINT ( 'NONE',  ( 34.67381068362099228, -26.00627455219321860, 313.9678068554150059 ) ) ;
#15241 = ORIENTED_EDGE ( 'NONE', *, *, #87729, .T. ) ;
#15240 = EDGE_CURVE ( 'NONE', #64922, #14514, #58520, .T. ) ;
#15242 = ADVANCED_FACE ( 'NONE', ( #29949 ), #42644, .F. ) ;
#15243 = ORIENTED_EDGE ( 'NONE', *, *, #23777, .T. ) ;
#15244 = PLANE ( 'NONE',  #54728 ) ;
#15245 = ADVANCED_FACE ( 'NONE', ( #1347 ), #64020, .F. ) ;
#15246 = AXIS2_PLACEMENT_3D ( 'NONE', #20633, #83761, #14269 ) ;
#15247 = ORIENTED_EDGE ( 'NONE', *, *, #78270, .T. ) ;
#15248 = CARTESIAN_POINT ( 'NONE',  ( 95.77883191840808763, -40.33907488607122360, 131.5727681330539554 ) ) ;
#15249 = DIRECTION ( 'NONE',  ( 1.000000000000000078E-15, -1.000000000000000083E-30, -1.000000000000000000 ) ) ;
#15250 = VECTOR ( 'NONE', #84760, 1000.000000000000000 ) ;
#15251 = EDGE_CURVE ( 'NONE', #42066, #23612, #50364, .T. ) ;
#15252 = CARTESIAN_POINT ( 'NONE',  ( 147.4575741623265799, 101.5999999999999943, 135.2444258376725941 ) ) ;
#15253 = PLANE ( 'NONE',  #42728 ) ;
#15256 = CARTESIAN_POINT ( 'NONE',  ( 118.0585799961420577, -32.36802338489823683, 245.1270538473389706 ) ) ;
#15255 = FACE_OUTER_BOUND ( 'NONE', #22397, .T. ) ;
#15254 = CARTESIAN_POINT ( 'NONE',  ( 94.06648329127393993, -36.72944715994093912, 315.6356252759111953 ) ) ;
#15257 = PLANE ( 'NONE',  #37952 ) ;
#15258 = DIRECTION ( 'NONE',  ( 0.000000000000000000, 0.000000000000000000, -1.000000000000000000 ) ) ;
#15259 = CARTESIAN_POINT ( 'NONE',  ( -24.79284581386642827, 127.0000000000000000, 106.1020876358972771 ) ) ;
#15260 = DIRECTION ( 'NONE',  ( 1.000000000000000078E-15, 0.000000000000000000, -1.000000000000000000 ) ) ;
#15261 = CARTESIAN_POINT ( 'NONE',  ( 100.9546727936483848, -28.70702574047548339, 256.5939586109827246 ) ) ;
#15262 = EDGE_CURVE ( 'NONE', #9337, #44647, #2044, .T. ) ;
#15263 = CARTESIAN_POINT ( 'NONE',  ( 167.6524903400753033, -48.32844715993521589, 300.4678068554149490 ) ) ;
#15265 = EDGE_LOOP ( 'NONE', ( #5874, #41309, #88595, #82572 ) ) ;
#15264 = CARTESIAN_POINT ( 'NONE',  ( 96.49234500119369784, -40.10591448887350197, 281.5603871806727625 ) ) ;
#15266 = CARTESIAN_POINT ( 'NONE',  ( 86.06670390244796920, -48.82844715994099971, 250.9178068554150514 ) ) ;
#15267 = CARTESIAN_POINT ( 'NONE',  ( 108.7467888895124162, -25.78085441620226348, 144.9432443235299672 ) ) ;
#15268 = CARTESIAN_POINT ( 'NONE',  ( 118.0755232325510917, -37.71687819837586630, 29.74324432352998215 ) ) ;
#15269 = CARTESIAN_POINT ( 'NONE',  ( 110.1502920506493552, -26.06700738780482141, 210.8403871806729626 ) ) ;
#15270 = PLANE ( 'NONE',  #2487 ) ;
#15271 = DIRECTION ( 'NONE',  ( -2.106816776397999944E-14, 1.000000000000000000, -2.206816776398000223E-29 ) ) ;
#15273 = DIRECTION ( 'NONE',  ( -0.000000000000000000, 1.000000000000000000, -0.000000000000000000 ) ) ;
#15272 = FACE_OUTER_BOUND ( 'NONE', #40276, .T. ) ;
#15274 = CARTESIAN_POINT ( 'NONE',  ( 99.09570908588736415, -30.55043174076017820, 70.80229194132837733 ) ) ;
#15275 = CARTESIAN_POINT ( 'NONE',  ( 116.3212776292296127, -32.94146857471318413, 287.6356252759109680 ) ) ;
#15276 = ORIENTED_EDGE ( 'NONE', *, *, #30535, .F. ) ;
#15277 = CARTESIAN_POINT ( 'NONE',  ( 140.9629299006807059, -46.47944715994099596, -5.074374724088994704 ) ) ;
#15278 = AXIS2_PLACEMENT_3D ( 'NONE', #76390, #528, #41403 ) ;
#15279 = AXIS2_PLACEMENT_3D ( 'NONE', #79976, #17730, #64985 ) ;
#15280 = VECTOR ( 'NONE', #45203, 1000.000000000000000 ) ;
#15281 = ORIENTED_EDGE ( 'NONE', *, *, #68593, .F. ) ;
#15282 = ORIENTED_EDGE ( 'NONE', *, *, #66383, .T. ) ;
#15283 = VECTOR ( 'NONE', #19839, 1000.000000000000000 ) ;
#15284 = EDGE_CURVE ( 'NONE', #29629, #33210, #84731, .T. ) ;
#15286 = ORIENTED_EDGE ( 'NONE', *, *, #23094, .T. ) ;
#15285 = CYLINDRICAL_SURFACE ( 'NONE', #9640, 4.750000000000004441 ) ;
#15287 = CARTESIAN_POINT ( 'NONE',  ( 96.94236579736397630, -32.35154040576534840, 57.01372051400599616 ) ) ;
#15288 = LINE ( 'NONE', #63423, #19413 ) ;
#15289 = ADVANCED_FACE ( 'NONE', ( #22693 ), #44440, .F. ) ;
#15290 = ADVANCED_FACE ( 'NONE', ( #9948 ), #57633, .T. ) ;
#15291 = CIRCLE ( 'NONE', #5152, 34.13125000000000142 ) ;
#15292 = LINE ( 'NONE', #42961, #48617 ) ;
#15293 = CARTESIAN_POINT ( 'NONE',  ( 109.4552518484143206, -25.89010755186295754, 175.8918157521009391 ) ) ;
#15294 = EDGE_CURVE ( 'NONE', #78195, #41311, #56737, .T. ) ;
#15296 = CARTESIAN_POINT ( 'NONE',  ( 110.8947914379136961, -29.09399076817903662, 279.1295626852197529 ) ) ;
#15295 = AXIS2_PLACEMENT_3D ( 'NONE', #56368, #84109, #21881 ) ;
#15297 = ORIENTED_EDGE ( 'NONE', *, *, #72673, .T. ) ;
#15298 = ORIENTED_EDGE ( 'NONE', *, *, #51185, .F. ) ;
#15299 = VERTEX_POINT ( 'NONE', #8157 ) ;
#15300 = VERTEX_POINT ( 'NONE', #8613 ) ;
#15301 = DIRECTION ( 'NONE',  ( -3.100000000000000258E-29, 3.100000000000000044E-14, 1.000000000000000000 ) ) ;
#15302 = DIRECTION ( 'NONE',  ( 0.000000000000000000, 0.000000000000000000, 1.000000000000000000 ) ) ;
#15303 = CARTESIAN_POINT ( 'NONE',  ( 102.0667490476481589, -27.97067744669410061, 161.4898198796698239 ) ) ;
#15304 = CARTESIAN_POINT ( 'NONE',  ( 97.33784130791669043, -34.07106454120959427, 76.11479194351055355 ) ) ;
#15305 = CONICAL_SURFACE ( 'NONE', #77670, 1.258750000000002922, 1.029744258676650093 ) ;
#15306 = CARTESIAN_POINT ( 'NONE',  ( 95.69832483115182242, 94.30053025434482095, 88.80956239834469557 ) ) ;
#15307 = PLANE ( 'NONE',  #65428 ) ;
#15308 = CYLINDRICAL_SURFACE ( 'NONE', #66471, 7.143750000000004263 ) ;
#15309 = CARTESIAN_POINT ( 'NONE',  ( -12.69999999999999929, 82.54999999999999716, 129.9368274816650057 ) ) ;
#15310 = CARTESIAN_POINT ( 'NONE',  ( 109.6066175024219973, -25.17973177368032012, 29.90419670448196854 ) ) ;
#15311 = CARTESIAN_POINT ( 'NONE',  ( 148.0533267522752112, 20.32000000000000028, 160.2664750769284865 ) ) ;
#15312 = ORIENTED_EDGE ( 'NONE', *, *, #44683, .T. ) ;
#15313 = CARTESIAN_POINT ( 'NONE',  ( 57.14999999999999858, 95.25000000000000000, 297.6879999999999882 ) ) ;
#15314 = FACE_OUTER_BOUND ( 'NONE', #1490, .T. ) ;
#15315 = CARTESIAN_POINT ( 'NONE',  ( 115.0083044075158654, -38.73198694842640322, 121.4480903695919807 ) ) ;
#15316 = VECTOR ( 'NONE', #46812, 1000.000000000000000 ) ;
#15317 = AXIS2_PLACEMENT_3D ( 'NONE', #38427, #44346, #912 ) ;
#15318 = PLANE ( 'NONE',  #57194 ) ;
#15319 = CARTESIAN_POINT ( 'NONE',  ( 0.000000000000000000, 65.60000000000000853, 0.000000000000000000 ) ) ;
#15320 = ORIENTED_EDGE ( 'NONE', *, *, #29409, .T. ) ;
#15321 = VERTEX_POINT ( 'NONE', #70841 ) ;
#15322 = CARTESIAN_POINT ( 'NONE',  ( -7.301849239715819957E-13, 127.0000000000000000, 98.60478223830740774 ) ) ;
#15323 = VERTEX_POINT ( 'NONE', #22244 ) ;
#15324 = ORIENTED_EDGE ( 'NONE', *, *, #24595, .T. ) ;
#15325 = CARTESIAN_POINT ( 'NONE',  ( 100.5685618138929271, -29.03188392736010570, 147.0672975916109806 ) ) ;
#15326 = LINE ( 'NONE', #9398, #23517 ) ;
#15327 = CARTESIAN_POINT ( 'NONE',  ( 103.3547197592076969, -47.16534756318074528, 98.31657765686297523 ) ) ;
#15328 = DIRECTION ( 'NONE',  ( 0.000000000000000000, 0.000000000000000000, 1.000000000000000000 ) ) ;
#15329 = AXIS2_PLACEMENT_3D ( 'NONE', #11824, #11371, #75397 ) ;
#15330 = ORIENTED_EDGE ( 'NONE', *, *, #48704, .F. ) ;
#15331 = AXIS2_PLACEMENT_3D ( 'NONE', #62856, #14279, #84674 ) ;
#15332 = AXIS2_PLACEMENT_3D ( 'NONE', #36069, #49681, #21102 ) ;
#15333 = AXIS2_PLACEMENT_3D ( 'NONE', #7732, #89514, #62689 ) ;
#15334 = ORIENTED_EDGE ( 'NONE', *, *, #80783, .F. ) ;
#15335 = EDGE_LOOP ( 'NONE', ( #62864, #30950, #9122, #50751 ) ) ;
#15336 = EDGE_CURVE ( 'NONE', #79139, #29190, #36310, .T. ) ;
#15337 = VECTOR ( 'NONE', #15722, 1000.000000000000000 ) ;
#15338 = EDGE_CURVE ( 'NONE', #9815, #81510, #64419, .T. ) ;
#15339 = CARTESIAN_POINT ( 'NONE',  ( 96.17000221327154463, -38.71995997157278424, 51.48229194257797303 ) ) ;
#15340 = ORIENTED_EDGE ( 'NONE', *, *, #26915, .F. ) ;
#15341 = CARTESIAN_POINT ( 'NONE',  ( 109.0793648114890715, -47.66380995969711876, 277.7213395616258822 ) ) ;
#15342 = CARTESIAN_POINT ( 'NONE',  ( 116.8155376854491720, -40.58108761943747567, 189.5270538473389479 ) ) ;
#15343 = CARTESIAN_POINT ( 'NONE',  ( 128.0667039024480118, -58.35344715994099829, 10.91780685541479734 ) ) ;
#15344 = CARTESIAN_POINT ( 'NONE',  ( 3.968750000000000000, 120.6499999999999915, -105.4788588808464027 ) ) ;
#15345 = CARTESIAN_POINT ( 'NONE',  ( 97.74639642956380214, -42.67166664343270099, 137.7661014663869992 ) ) ;
#15346 = DIRECTION ( 'NONE',  ( -0.0001713722456127401463, 0.9999999853157766072, 1.713722456137401502E-19 ) ) ;
#15347 = ORIENTED_EDGE ( 'NONE', *, *, #16459, .F. ) ;
#15348 = LINE ( 'NONE', #35314, #83019 ) ;
#15349 = ADVANCED_FACE ( 'NONE', ( #37652 ), #35353, .F. ) ;
#15350 = EDGE_CURVE ( 'NONE', #52647, #77884, #35847, .T. ) ;
#15351 = ORIENTED_EDGE ( 'NONE', *, *, #1230, .T. ) ;
#15352 = CARTESIAN_POINT ( 'NONE',  ( 98.38043711079399145, -41.69530130865705786, 132.7403033756623074 ) ) ;
#15353 = ORIENTED_EDGE ( 'NONE', *, *, #44445, .F. ) ;
#15354 = VECTOR ( 'NONE', #57157, 1000.000000000000000 ) ;
#15355 = ORIENTED_EDGE ( 'NONE', *, *, #11783, .F. ) ;
#15356 = EDGE_CURVE ( 'NONE', #66809, #43116, #46934, .T. ) ;
#15357 = DIRECTION ( 'NONE',  ( 0.000000000000000000, 1.000000000000000000, 0.000000000000000000 ) ) ;
#15358 = CARTESIAN_POINT ( 'NONE',  ( 46.83715912545422100, -47.82818131006082751, 313.9678068554150059 ) ) ;
#15359 = CARTESIAN_POINT ( 'NONE',  ( 117.4878618838608872, -37.01562663403593234, 43.80419670448293346 ) ) ;
#15360 = CARTESIAN_POINT ( 'NONE',  ( 21.94694372886773337, 60.27287744939596337, 31.14430251170410457 ) ) ;
#15361 = AXIS2_PLACEMENT_3D ( 'NONE', #6001, #32787, #19608 ) ;
#15362 = ADVANCED_FACE ( 'NONE', ( #2690 ), #16760, .F. ) ;
#15363 = PLANE ( 'NONE',  #53559 ) ;
#15364 = PLANE ( 'NONE',  #17972 ) ;
#15365 = CARTESIAN_POINT ( 'NONE',  ( 116.8435662018514307, -36.99793375417353758, 43.80419670448193159 ) ) ;
#15367 = CARTESIAN_POINT ( 'NONE',  ( 117.0123300003820646, -30.33189756676014426, 140.2813395616249750 ) ) ;
#15366 = PLANE ( 'NONE',  #44870 ) ;
#15368 = CARTESIAN_POINT ( 'NONE',  ( 97.06107109872726824, -37.99641197594983311, 72.42729194355847255 ) ) ;
#15369 = CARTESIAN_POINT ( 'NONE',  ( 33.92127028473484529, -29.73316016639607184, 193.9678068554150911 ) ) ;
#15370 = ORIENTED_EDGE ( 'NONE', *, *, #41530, .T. ) ;
#15371 = CARTESIAN_POINT ( 'NONE',  ( 274.0659999999999741, 40.03750000000000142, -7.937500000000000000 ) ) ;
#15372 = CARTESIAN_POINT ( 'NONE',  ( -18.25522102001837155, 65.15566424648996247, 33.44615533302457777 ) ) ;
#15373 = CARTESIAN_POINT ( 'NONE',  ( 34.92499999999999716, 69.79919999999999902, 346.9005000000000223 ) ) ;
#15374 = ORIENTED_EDGE ( 'NONE', *, *, #68578, .F. ) ;
#15375 = EDGE_CURVE ( 'NONE', #87925, #64058, #32158, .T. ) ;
#15376 = DIRECTION ( 'NONE',  ( 4.299999999999999979E-14, -1.000000000000000000, 4.400000000000000367E-29 ) ) ;
#15378 = VERTEX_POINT ( 'NONE', #5362 ) ;
#15377 = CARTESIAN_POINT ( 'NONE',  ( 103.0327258024342427, -26.38818591439425632, 170.3603871806729444 ) ) ;
#15379 = DIRECTION ( 'NONE',  ( 1.000000000000000078E-15, 1.000000000000000083E-30, -1.000000000000000000 ) ) ;
#15380 = CARTESIAN_POINT ( 'NONE',  ( 117.4960079497888472, -36.12755493457860467, 224.8727681330539667 ) ) ;
#15381 = CARTESIAN_POINT ( 'NONE',  ( 107.6053842629478794, -26.23908965751013156, 91.03562527591097364 ) ) ;
#15382 = CARTESIAN_POINT ( 'NONE',  ( 51.42025729302798709, -31.94127993907680718, -5.074374724088000832 ) ) ;
#15383 = CARTESIAN_POINT ( 'NONE',  ( 115.0868436454567387, -30.61496486536007211, 190.3439483173824556 ) ) ;
#15384 = EDGE_CURVE ( 'NONE', #733, #34697, #38090, .T. ) ;
#15385 = CARTESIAN_POINT ( 'NONE',  ( 183.5150000000000148, 52.73749999999999716, -53.97500000000000142 ) ) ;
#15386 = ORIENTED_EDGE ( 'NONE', *, *, #86162, .F. ) ;
#15387 = AXIS2_PLACEMENT_3D ( 'NONE', #81045, #51943, #60103 ) ;
#15388 = ORIENTED_EDGE ( 'NONE', *, *, #33916, .T. ) ;
#15389 = ORIENTED_EDGE ( 'NONE', *, *, #53251, .F. ) ;
#15390 = EDGE_LOOP ( 'NONE', ( #59169, #61700, #18042, #8296, #4412 ) ) ;
#15391 = DIRECTION ( 'NONE',  ( 1.000000000000000000, 4.299999999999999979E-14, 1.000000000000000078E-15 ) ) ;
#15392 = CARTESIAN_POINT ( 'NONE',  ( 104.8412801004068058, -26.50840007386317509, 256.2470538473397141 ) ) ;
#15393 = LINE ( 'NONE', #41719, #1123 ) ;
#15394 = CARTESIAN_POINT ( 'NONE',  ( 136.6003823147689786, -17.66080131299353795, 2.811527311783424743 ) ) ;
#15395 = ADVANCED_FACE ( 'NONE', ( #31715 ), #73497, .T. ) ;
#15398 = EDGE_CURVE ( 'NONE', #47018, #31056, #72313, .T. ) ;
#15397 = DIRECTION ( 'NONE',  ( 0.7071067811578790607, 0.7071067812152160847, 0.000000000000000000 ) ) ;
#15396 = CARTESIAN_POINT ( 'NONE',  ( 182.0374245136142406, -23.42844715993458848, 193.9678068554150059 ) ) ;
#15399 = CIRCLE ( 'NONE', #77767, 3.000000000000002665 ) ;
#15400 = CARTESIAN_POINT ( 'NONE',  ( 107.0667039024470313, -104.2784471599418197, -11.78219314458200984 ) ) ;
#15401 = CARTESIAN_POINT ( 'NONE',  ( 112.9757402841042904, -28.11393523324086985, 44.59848241876795782 ) ) ;
#15402 = ORIENTED_EDGE ( 'NONE', *, *, #21318, .T. ) ;
#15403 = CIRCLE ( 'NONE', #859, 0.5000000000000004441 ) ;
#15404 = VERTEX_POINT ( 'NONE', #45769 ) ;
#15405 = VECTOR ( 'NONE', #3662, 1000.000000000000000 ) ;
#15406 = VECTOR ( 'NONE', #12273, 1000.000000000000114 ) ;
#15407 = SURFACE_STYLE_FILL_AREA ( #15846 ) ;
#15408 = CIRCLE ( 'NONE', #51609, 3.250000000000002665 ) ;
#15409 = LINE ( 'NONE', #1774, #59318 ) ;
#15410 = CARTESIAN_POINT ( 'NONE',  ( 97.21282778982880757, -39.96427141005798234, 282.5908633711484867 ) ) ;
#15411 = PLANE ( 'NONE',  #74801 ) ;
#15412 = CARTESIAN_POINT ( 'NONE',  ( 113.4935171807053536, -28.59114140144097860, 120.5565776568629559 ) ) ;
#15413 = FACE_OUTER_BOUND ( 'NONE', #23540, .T. ) ;
#15414 = CARTESIAN_POINT ( 'NONE',  ( 108.3327080255635622, -46.73494336040992181, 27.67723307863499826 ) ) ;
#15415 = ORIENTED_EDGE ( 'NONE', *, *, #6131, .F. ) ;
#15416 = DIRECTION ( 'NONE',  ( 0.7071067811865259234, -0.7071067811865692221, 2.899137802865049595E-29 ) ) ;
#15417 = CARTESIAN_POINT ( 'NONE',  ( 78.35491772849390202, -34.56918551488853097, 2.099346190924665567 ) ) ;
#15418 = ORIENTED_EDGE ( 'NONE', *, *, #17702, .F. ) ;
#15419 = ORIENTED_EDGE ( 'NONE', *, *, #60662, .T. ) ;
#15420 = AXIS2_PLACEMENT_3D ( 'NONE', #3835, #4734, #81508 ) ;
#15421 = CARTESIAN_POINT ( 'NONE',  ( 97.95250717983367394, -32.49412669507731266, 9.425625275910961776 ) ) ;
#15422 = CARTESIAN_POINT ( 'NONE',  ( 98.67113652751868358, -38.83122756767168227, 14.35189989340096517 ) ) ;
#15423 = EDGE_CURVE ( 'NONE', #78070, #46083, #83224, .T. ) ;
#15424 = CARTESIAN_POINT ( 'NONE',  ( 6.938893903907229955E-15, 67.86880000000000734, 216.0269999999999868 ) ) ;
#15425 = CARTESIAN_POINT ( 'NONE',  ( 177.0664832912730162, 12.92155284005730387, 358.9756252759109998 ) ) ;
#15426 = CARTESIAN_POINT ( 'NONE',  ( 135.3838309168194201, -60.54606547621062163, 361.9756252759100335 ) ) ;
#15427 = CARTESIAN_POINT ( 'NONE',  ( 88.21655330423281782, 71.53193882405247450, -79.20758933349323172 ) ) ;
#15428 = ORIENTED_EDGE ( 'NONE', *, *, #78336, .T. ) ;
#15429 = FACE_OUTER_BOUND ( 'NONE', #75796, .T. ) ;
#15430 = CARTESIAN_POINT ( 'NONE',  ( 21.03715912545744615, -47.82818131006197149, 129.9678068554150627 ) ) ;
#15431 = ORIENTED_EDGE ( 'NONE', *, *, #87474, .F. ) ;
#15432 = CARTESIAN_POINT ( 'NONE',  ( 113.5062182464826748, -28.53085922249196216, 79.54705384733995288 ) ) ;
#15433 = VERTEX_POINT ( 'NONE', #5820 ) ;
#15434 = CARTESIAN_POINT ( 'NONE',  ( 110.7520593201813597, -44.56232478875543990, 285.7328522743533767 ) ) ;
#15435 = CARTESIAN_POINT ( 'NONE',  ( 74.06670390244704549, -118.2784471599409812, 51.21780685541800437 ) ) ;
#15436 = CARTESIAN_POINT ( 'NONE',  ( 98.02110346605346081, -41.80092515478916937, 181.7451490854359974 ) ) ;
#15437 = CARTESIAN_POINT ( 'NONE',  ( 31.75000000000000000, 69.84999999999999432, 295.2750000000000341 ) ) ;
#15438 = DIRECTION ( 'NONE',  ( 0.000000000000000000, 1.000000000000000000, 1.598363122120870523E-15 ) ) ;
#15439 = CYLINDRICAL_SURFACE ( 'NONE', #62250, 9.999999999999998224 ) ;
#15440 = CARTESIAN_POINT ( 'NONE',  ( 68.86273219497338971, -69.51591775960335440, 247.4919776621595418 ) ) ;
#15441 = ADVANCED_FACE ( 'NONE', ( #33507, #20343 ), #20782, .T. ) ;
#15442 = CARTESIAN_POINT ( 'NONE',  ( 118.1536727146126395, -36.20817079386891635, 264.8518157521014587 ) ) ;
#15443 = CARTESIAN_POINT ( 'NONE',  ( 80.88915705228910724, 94.58006533271583294, -86.67541640318093243 ) ) ;
#15444 = ORIENTED_EDGE ( 'NONE', *, *, #84282, .F. ) ;
#15445 = DIRECTION ( 'NONE',  ( 3.100000000000000258E-29, -3.100000000000000044E-14, -1.000000000000000000 ) ) ;
#15446 = VERTEX_POINT ( 'NONE', #48012 ) ;
#15447 = CARTESIAN_POINT ( 'NONE',  ( 96.56348986465089013, -36.88801538493378018, 132.3384824187679669 ) ) ;
#15448 = CARTESIAN_POINT ( 'NONE',  ( 125.0134529257903893, 48.65659782722526217, -37.63673439681842581 ) ) ;
#15449 = ORIENTED_EDGE ( 'NONE', *, *, #29747, .F. ) ;
#15451 = EDGE_CURVE ( 'NONE', #26947, #58383, #19411, .T. ) ;
#15450 = ORIENTED_EDGE ( 'NONE', *, *, #26345, .T. ) ;
#15453 = VERTEX_POINT ( 'NONE', #89383 ) ;
#15452 = EDGE_CURVE ( 'NONE', #58845, #37060, #36619, .T. ) ;
#15454 = CARTESIAN_POINT ( 'NONE',  ( 142.8698897858160421, -0.9167816978817300289, 361.9756252759100335 ) ) ;
#15455 = ADVANCED_FACE ( 'NONE', ( #28032 ), #83028, .F. ) ;
#15456 = DIRECTION ( 'NONE',  ( -1.000000000000000000, 0.000000000000000000, 0.000000000000000000 ) ) ;
#15457 = CARTESIAN_POINT ( 'NONE',  ( 0.000000000000000000, 215.0000000000000000, 154.6557476874258441 ) ) ;
#15458 = CARTESIAN_POINT ( 'NONE',  ( -72.96458098368751166, 117.4749999999999943, 80.10833098368618721 ) ) ;
#15459 = DIRECTION ( 'NONE',  ( 1.067522139062650671E-15, 1.000000000000000000, 0.000000000000000000 ) ) ;
#15460 = CARTESIAN_POINT ( 'NONE',  ( 107.1953983157108041, -26.30515493630308654, 31.06705384733893283 ) ) ;
#15461 = DIRECTION ( 'NONE',  ( -4.237773401492740281E-14, 1.000000000000000000, 0.000000000000000000 ) ) ;
#15462 = ORIENTED_EDGE ( 'NONE', *, *, #31086, .F. ) ;
#15463 = CARTESIAN_POINT ( 'NONE',  ( 12.70000000000000107, 81.71003749631398705, 117.8738102209307925 ) ) ;
#15464 = EDGE_CURVE ( 'NONE', #43342, #41931, #4888, .T. ) ;
#15465 = AXIS2_PLACEMENT_3D ( 'NONE', #15888, #72638, #86260 ) ;
#15466 = PLANE ( 'NONE',  #53367 ) ;
#15467 = EDGE_LOOP ( 'NONE', ( #60413, #81927, #77958, #1377 ) ) ;
#15468 = VERTEX_POINT ( 'NONE', #75301 ) ;
#15469 = ADVANCED_FACE ( 'NONE', ( #47117 ), #82137, .F. ) ;
#15470 = AXIS2_PLACEMENT_3D ( 'NONE', #28187, #7320, #64851 ) ;
#15471 = CARTESIAN_POINT ( 'NONE',  ( 82.16371341590115662, -20.51083119283027045, 2.376725019074904743 ) ) ;
#15472 = LINE ( 'NONE', #2282, #64343 ) ;
#15473 = CARTESIAN_POINT ( 'NONE',  ( 172.5664832912740110, -18.82844715994099971, 321.0426252759119734 ) ) ;
#15474 = AXIS2_PLACEMENT_3D ( 'NONE', #6912, #62765, #70042 ) ;
#15475 = FACE_OUTER_BOUND ( 'NONE', #44425, .T. ) ;
#15476 = LINE ( 'NONE', #30434, #73656 ) ;
#15477 = EDGE_CURVE ( 'NONE', #69462, #48907, #15072, .T. ) ;
#15478 = CARTESIAN_POINT ( 'NONE',  ( 112.5827476457113079, -28.73936235024410024, 239.0181341137909783 ) ) ;
#15479 = CARTESIAN_POINT ( 'NONE',  ( 151.0371591254582881, -46.82818131005593187, 237.4678068554150059 ) ) ;
#15480 = CARTESIAN_POINT ( 'NONE',  ( 126.4548149396404710, 63.48030817387711977, 32.46806497751565956 ) ) ;
#15481 = CARTESIAN_POINT ( 'NONE',  ( 98.82309110046458045, -43.24084327085208912, 91.85848241876892928 ) ) ;
#15482 = ORIENTED_EDGE ( 'NONE', *, *, #31641, .F. ) ;
#15483 = LINE ( 'NONE', #7754, #84339 ) ;
#15484 = EDGE_LOOP ( 'NONE', ( #88387, #11627, #49828, #77762 ) ) ;
#15485 = CARTESIAN_POINT ( 'NONE',  ( 176.7738106835696499, -48.62134037881071436, 129.9678068554150059 ) ) ;
#15486 = CARTESIAN_POINT ( 'NONE',  ( 99.09397582248948311, -30.55267087576145357, 276.8024460130702664 ) ) ;
#15487 = VERTEX_POINT ( 'NONE', #74852 ) ;
#15488 = CARTESIAN_POINT ( 'NONE',  ( 44.45000000000000284, 111.1250000000000000, 257.1750000000000114 ) ) ;
#15489 = ORIENTED_EDGE ( 'NONE', *, *, #19957, .T. ) ;
#15490 = DIRECTION ( 'NONE',  ( 0.000000000000000000, -1.000000000000000000, 0.000000000000000000 ) ) ;
#15491 = CARTESIAN_POINT ( 'NONE',  ( 67.36333724445186988, -137.6828925929944774, 246.8602380403289942 ) ) ;
#15492 = AXIS2_PLACEMENT_3D ( 'NONE', #24273, #31509, #18788 ) ;
#15493 = DIRECTION ( 'NONE',  ( -0.5000000000000015543, 0.8660254037844377084, -2.688821387764056676E-14 ) ) ;
#15494 = ORIENTED_EDGE ( 'NONE', *, *, #76391, .F. ) ;
#15495 = CARTESIAN_POINT ( 'NONE',  ( 96.76980119632513322, -38.49712976775982298, 91.46133956162493917 ) ) ;
#15497 = CARTESIAN_POINT ( 'NONE',  ( 84.19388261208037250, 76.18750001922980175, -99.78212687779711132 ) ) ;
#15496 = CARTESIAN_POINT ( 'NONE',  ( 108.4167997317111372, -26.73494551780935069, 164.9690142253840577 ) ) ;
#15498 = CARTESIAN_POINT ( 'NONE',  ( 103.3797721312301405, -102.7271463785358492, -19.78219314458207378 ) ) ;
#15499 = CARTESIAN_POINT ( 'NONE',  ( -9.487324347909602551, 74.21786271237625954, 117.9765759210854554 ) ) ;
#15500 = VERTEX_POINT ( 'NONE', #23041 ) ;
#15501 = CARTESIAN_POINT ( 'NONE',  ( 112.1400524529204148, -28.07738699070645438, 120.6531484116016912 ) ) ;
#15502 = CARTESIAN_POINT ( 'NONE',  ( 93.91125933621933086, -96.68314769832107913, -11.78219314458223188 ) ) ;
#15503 = CARTESIAN_POINT ( 'NONE',  ( 95.75547692839532488, -40.34654347423973775, 127.5727681330539554 ) ) ;
#15506 = ADVANCED_FACE ( 'NONE', ( #50717 ), #50260, .T. ) ;
#15505 = CARTESIAN_POINT ( 'NONE',  ( 30.48091746481745901, -49.32844715994156815, 180.4678068554150911 ) ) ;
#15504 = DIRECTION ( 'NONE',  ( -0.2588190451025281225, 0.000000000000000000, 0.9659258262890663138 ) ) ;
#15507 = DIRECTION ( 'NONE',  ( -3.100000000000000258E-29, 3.100000000000000044E-14, 1.000000000000000000 ) ) ;
#15508 = AXIS2_PLACEMENT_3D ( 'NONE', #64861, #44396, #65309 ) ;
#15509 = ORIENTED_EDGE ( 'NONE', *, *, #22282, .T. ) ;
#15510 = CARTESIAN_POINT ( 'NONE',  ( 107.0664832912739399, -36.72944715994095333, 315.1356252759112522 ) ) ;
#15511 = CARTESIAN_POINT ( 'NONE',  ( 107.8656169629272341, -46.51081515578102454, 173.6413395616249886 ) ) ;
#15513 = ORIENTED_EDGE ( 'NONE', *, *, #67656, .F. ) ;
#15512 = CARTESIAN_POINT ( 'NONE',  ( 106.5646857698207981, -25.28130207810567498, 321.1698005525342978 ) ) ;
#15514 = CARTESIAN_POINT ( 'NONE',  ( 95.98894198207693762, -35.78073158428682632, 32.25848241876694544 ) ) ;
#15515 = PLANE ( 'NONE',  #22292 ) ;
#15516 = DIRECTION ( 'NONE',  ( -3.100000000000000258E-29, 3.100000000000000044E-14, 1.000000000000000000 ) ) ;
#15517 = LINE ( 'NONE', #35486, #42920 ) ;
#15518 = CARTESIAN_POINT ( 'NONE',  ( -100.8961411191535973, 127.0000000000000000, -3.968750000001104894 ) ) ;
#15519 = FACE_BOUND ( 'NONE', #72991, .T. ) ;
#15520 = AXIS2_PLACEMENT_3D ( 'NONE', #16123, #65594, #42897 ) ;
#15521 = CARTESIAN_POINT ( 'NONE',  ( 97.40895461294492463, -34.98419235835273611, 241.1841967044829573 ) ) ;
#15522 = VERTEX_POINT ( 'NONE', #78455 ) ;
#15523 = EDGE_LOOP ( 'NONE', ( #66561, #7753, #50453, #34741 ) ) ;
#15524 = CARTESIAN_POINT ( 'NONE',  ( 108.1711956065674229, -46.05983505851052229, 159.1139642582779459 ) ) ;
#15525 = EDGE_CURVE ( 'NONE', #23402, #22043, #35744, .T. ) ;
#15526 = VECTOR ( 'NONE', #36031, 1000.000000000000000 ) ;
#15527 = DIRECTION ( 'NONE',  ( -0.7071067812162686872, -0.7071067811568263473, 2.899137802742872063E-29 ) ) ;
#15528 = CIRCLE ( 'NONE', #11157, 7.937500000000000000 ) ;
#15529 = CARTESIAN_POINT ( 'NONE',  ( 101.4092135025303776, -29.90862777007100703, 37.05872616303995670 ) ) ;
#15530 = AXIS2_PLACEMENT_3D ( 'NONE', #10819, #53010, #80779 ) ;
#15531 = CARTESIAN_POINT ( 'NONE',  ( 23.68729270147990462, 84.09221149220967106, 298.3783288177381792 ) ) ;
#15532 = B_SPLINE_CURVE_WITH_KNOTS ( 'NONE', 3,
 ( #70256, #759, #15749, #22125, #28460, #83004, #14406, #36183, #15303, #49346, #83901, #21213, #28927, #77976, #29378, #41628, #21672, #27572 ),
 .UNSPECIFIED., .F., .F.,
 ( 4, 2, 2, 2, 2, 2, 2, 2, 4 ),
 ( 0.4999919244375641281, 0.5624929338828685843, 0.6249939433281730405, 0.6874949527734776078, 0.7499959622187820640, 0.8124969716640865203, 0.8749979811093910875, 0.9374989905546955438, 1.000000000000000000 ),
 .UNSPECIFIED. ) ;
#15533 = CARTESIAN_POINT ( 'NONE',  ( 48.16670390244661348, -28.27351298637380950, 117.4678068554150485 ) ) ;
#15534 = DIRECTION ( 'NONE',  ( 3.596091637922019804E-15, 0.000000000000000000, 1.000000000000000000 ) ) ;
#15535 = CARTESIAN_POINT ( 'NONE',  ( 73.06648329127402519, -46.47944715994106701, -5.074374724089063982 ) ) ;
#15536 = DIRECTION ( 'NONE',  ( -1.000000000000000000, 0.000000000000000000, 0.000000000000000000 ) ) ;
#15537 = CARTESIAN_POINT ( 'NONE',  ( 105.1131368864170241, -25.87365329830167937, 275.2061014663871674 ) ) ;
#15538 = CARTESIAN_POINT ( 'NONE',  ( 97.79668209375444121, -40.48056570805522369, 171.6327272062056295 ) ) ;
#15539 = ORIENTED_EDGE ( 'NONE', *, *, #72068, .T. ) ;
#15540 = EDGE_LOOP ( 'NONE', ( #19777, #4377 ) ) ;
#15541 = CARTESIAN_POINT ( 'NONE',  ( 101.9936209214569516, -45.44607152756502444, 87.15645860747564200 ) ) ;
#15542 = CARTESIAN_POINT ( 'NONE',  ( -75.24778849303618244, 87.79588542099533299, -91.61507027739561693 ) ) ;
#15543 = CYLINDRICAL_SURFACE ( 'NONE', #57757, 5.599999999999994316 ) ;
#15544 = VECTOR ( 'NONE', #62428, 1000.000000000000000 ) ;
#15545 = DIRECTION ( 'NONE',  ( 0.000000000000000000, 1.000000000000000000, 0.000000000000000000 ) ) ;
#15546 = VECTOR ( 'NONE', #4503, 1000.000000000000000 ) ;
#15547 = CARTESIAN_POINT ( 'NONE',  ( 98.38136461969652657, -29.78821554292439444, 41.78991099019696520 ) ) ;
#15548 = DIRECTION ( 'NONE',  ( 1.000000000000000000, -0.000000000000000000, 2.108231265501710124E-16 ) ) ;
#15549 = CLOSED_SHELL ( 'NONE', ( #74468, #26821, #67375, #13285, #28353, #65151, #33795, #77184, #84683, #31319, #24361, #16466, #24022, #52408, #17074, #83080, #48006, #23673, #10635, #83086, #25602, #76205, #35146, #77355, #26934, #26632, #869, #34880, #8374, #85557, #82623, #34634, #56960, #17157, #49843, #28210, #2234, #55795, #57273, #26920, #79966, #49808, #74242, #12595, #63022, #84677, #74077, #32482, #54691, #52567, #12459, #30017, #66107, #13802, #21394, #13682, #16914, #38862, #73046, #31934, #60432, #16702, #81389, #44852, #52770, #28853, #35826, #11829, #34859, #80259, #48452, #23756, #75841, #33007 ) ) ;
#15550 = VERTEX_POINT ( 'NONE', #8049 ) ;
#15551 = DIRECTION ( 'NONE',  ( 1.000000000000000000, 4.194175870806139918E-14, 0.000000000000000000 ) ) ;
#15552 = CARTESIAN_POINT ( 'NONE',  ( 32.06670390244676128, -33.35206098992750157, 193.9678068554150911 ) ) ;
#15553 = CARTESIAN_POINT ( 'NONE',  ( 112.4894639655092305, -46.36118470102660183, 257.9965776568635647 ) ) ;
#15555 = VERTEX_POINT ( 'NONE', #29844 ) ;
#15554 = EDGE_CURVE ( 'NONE', #14550, #27150, #61241, .T. ) ;
#15556 = EDGE_CURVE ( 'NONE', #21297, #73197, #43444, .T. ) ;
#15557 = LINE ( 'NONE', #16003, #37564 ) ;
#15558 = LINE ( 'NONE', #57309, #77643 ) ;
#15559 = EDGE_CURVE ( 'NONE', #71324, #82436, #85713, .T. ) ;
#15560 = CYLINDRICAL_SURFACE ( 'NONE', #66888, 3.299999999999999822 ) ;
#15561 = CARTESIAN_POINT ( 'NONE',  ( 114.5297761857384415, -31.21626383854846765, 107.1509475124489654 ) ) ;
#15562 = CARTESIAN_POINT ( 'NONE',  ( 106.4823958901525458, -24.86854109859944373, 191.1156252759109861 ) ) ;
#15563 = DIRECTION ( 'NONE',  ( -1.000000000000000000, 9.376883653928684652E-16, 1.500301384628589584E-15 ) ) ;
#15564 = EDGE_LOOP ( 'NONE', ( #40992, #83711, #76749, #66777 ) ) ;
#15565 = EDGE_CURVE ( 'NONE', #61198, #58395, #2138, .T. ) ;
#15566 = CARTESIAN_POINT ( 'NONE',  ( 41.56648329127399677, -9.303447159940999356, 78.92562527591199739 ) ) ;
#15567 = EDGE_LOOP ( 'NONE', ( #45739, #14034, #26057 ) ) ;
#15569 = ORIENTED_EDGE ( 'NONE', *, *, #68094, .F. ) ;
#15568 = VECTOR ( 'NONE', #15139, 1000.000000000000000 ) ;
#15570 = EDGE_CURVE ( 'NONE', #32982, #48113, #10523, .T. ) ;
#15571 = FACE_BOUND ( 'NONE', #35193, .T. ) ;
#15572 = ORIENTED_EDGE ( 'NONE', *, *, #27601, .F. ) ;
#15573 = EDGE_LOOP ( 'NONE', ( #83420, #65712, #19462, #50343, #53812 ) ) ;
#15574 = FACE_OUTER_BOUND ( 'NONE', #2043, .T. ) ;
#15575 = CARTESIAN_POINT ( 'NONE',  ( 97.78479357905025893, -40.45113604636035376, 42.62993149403730797 ) ) ;
#15576 = EDGE_CURVE ( 'NONE', #30851, #39116, #9073, .T. ) ;
#15577 = CARTESIAN_POINT ( 'NONE',  ( 100.8685319560204050, -42.60665150962044123, 81.35241982807694683 ) ) ;
#15578 = CARTESIAN_POINT ( 'NONE',  ( 97.20287302226383019, -40.27875065248429820, 266.6013395616254797 ) ) ;
#15579 = CARTESIAN_POINT ( 'NONE',  ( 28.57499999999999929, 73.38456447661469895, 302.8950000000000387 ) ) ;
#15580 = DIRECTION ( 'NONE',  ( 0.000000000000000000, 1.000000000000000000, 0.000000000000000000 ) ) ;
#15581 = ORIENTED_EDGE ( 'NONE', *, *, #19918, .F. ) ;
#15582 = ORIENTED_EDGE ( 'NONE', *, *, #10942, .F. ) ;
#15583 = DIRECTION ( 'NONE',  ( 3.100000000000000258E-29, -3.100000000000000044E-14, -1.000000000000000000 ) ) ;
#15584 = CIRCLE ( 'NONE', #53202, 7.937500000000000000 ) ;
#15585 = DIRECTION ( 'NONE',  ( 0.000000000000000000, 1.000000000000000000, -2.731847993664264698E-16 ) ) ;
#15586 = CARTESIAN_POINT ( 'NONE',  ( 70.98999999999998067, 52.73749999999999716, -52.28750000000002274 ) ) ;
#15587 = CARTESIAN_POINT ( 'NONE',  ( 114.7398264468854592, -44.75021323582976862, 113.1718157521009687 ) ) ;
#15589 = DIRECTION ( 'NONE',  ( 0.0001713722456127401463, -0.9999999853157766072, -1.713722456137401502E-19 ) ) ;
#15588 = AXIS2_PLACEMENT_3D ( 'NONE', #23228, #65854, #24100 ) ;
#15590 = ORIENTED_EDGE ( 'NONE', *, *, #49985, .F. ) ;
#15591 = VECTOR ( 'NONE', #18537, 1000.000000000000000 ) ;
#15592 = CARTESIAN_POINT ( 'NONE',  ( 105.0216316738932107, -25.86677467614671500, 280.2365776568631759 ) ) ;
#15593 = CARTESIAN_POINT ( 'NONE',  ( 97.75353936551157119, -40.54122631656009190, 7.635625275910939536 ) ) ;
#15594 = VECTOR ( 'NONE', #42436, 1000.000000000000000 ) ;
#15595 = CARTESIAN_POINT ( 'NONE',  ( 97.87053931029933551, -40.65856329638635458, 27.64823128951286080 ) ) ;
#15597 = CARTESIAN_POINT ( 'NONE',  ( 68.69838760978726100, -139.2979692165780818, 245.8480134095270557 ) ) ;
#15596 = DIRECTION ( 'NONE',  ( 0.7071067811865415775, 0.000000000000000000, 0.7071067811865535679 ) ) ;
#15598 = DIRECTION ( 'NONE',  ( 0.000000000000000000, 1.000000000000000000, 0.000000000000000000 ) ) ;
#15599 = CARTESIAN_POINT ( 'NONE',  ( 86.06670390244796920, -50.82844715994100682, 151.9178068554149945 ) ) ;
#15600 = CARTESIAN_POINT ( 'NONE',  ( 132.6453213455613991, -39.08531275930689475, 7.905164235259871219 ) ) ;
#15601 = CARTESIAN_POINT ( 'NONE',  ( -9.572882853229330635, 90.93765695308124464, 130.2059221945669947 ) ) ;
#15602 = CARTESIAN_POINT ( 'NONE',  ( 194.0667039024475287, -24.92844715993407334, 180.4678068554150343 ) ) ;
#15603 = LINE ( 'NONE', #21064, #60832 ) ;
#15604 = CIRCLE ( 'NONE', #47469, 20.63750000000000284 ) ;
#15606 = ORIENTED_EDGE ( 'NONE', *, *, #28959, .F. ) ;
#15605 = DIRECTION ( 'NONE',  ( 1.000000000000000078E-15, -1.000000000000000000, 0.000000000000000000 ) ) ;
#15607 = CARTESIAN_POINT ( 'NONE',  ( 114.6154092934514495, -130.7908339518063769, 250.2178068554180470 ) ) ;
#15608 = CARTESIAN_POINT ( 'NONE',  ( 97.59524074137092953, -41.13874739096760891, 256.6727681330537507 ) ) ;
#15609 = CARTESIAN_POINT ( 'NONE',  ( 117.7791004155048853, -34.00661502546044801, 165.0365776568629315 ) ) ;
#15610 = CARTESIAN_POINT ( 'NONE',  ( 97.17561725847181719, -33.29990440931864271, 282.0613395616252888 ) ) ;
#15611 = VECTOR ( 'NONE', #41679, 999.9999999999998863 ) ;
#15614 = EDGE_CURVE ( 'NONE', #61529, #35450, #85273, .T. ) ;
#15613 = CARTESIAN_POINT ( 'NONE',  ( 101.9936209440171240, -45.44607154049054998, 47.15645860952901813 ) ) ;
#15612 = FACE_OUTER_BOUND ( 'NONE', #63369, .T. ) ;
#15615 = CARTESIAN_POINT ( 'NONE',  ( 165.9667039024474491, -26.71338133338714016, 237.4678068554150059 ) ) ;
#15616 = TOROIDAL_SURFACE ( 'NONE', #73561, 15.84999999999999964, 0.1499999999999999944 ) ;
#15617 = ADVANCED_FACE ( 'NONE', ( #21693 ), #84377, .T. ) ;
#15618 = ORIENTED_EDGE ( 'NONE', *, *, #58609, .T. ) ;
#15619 = DIRECTION ( 'NONE',  ( 1.000000000000000000, 1.110223024625155531E-13, 0.000000000000000000 ) ) ;
#15620 = ORIENTED_EDGE ( 'NONE', *, *, #87795, .T. ) ;
#15621 = CARTESIAN_POINT ( 'NONE',  ( 104.3962608544918993, -28.61612207615715775, 164.7524198280769667 ) ) ;
#15623 = VERTEX_POINT ( 'NONE', #44790 ) ;
#15622 = PLANE ( 'NONE',  #26877 ) ;
#15624 = DIRECTION ( 'NONE',  ( 1.000000000000000000, 0.000000000000000000, 0.000000000000000000 ) ) ;
#15625 = CARTESIAN_POINT ( 'NONE',  ( 107.5647246096319094, -47.74832088493814553, 188.6003871806729535 ) ) ;
#15626 = DIRECTION ( 'NONE',  ( -1.000000000000000000, -1.000000000000000078E-15, 0.000000000000000000 ) ) ;
#15627 = DIRECTION ( 'NONE',  ( 4.299999999999999979E-14, -1.000000000000000000, 4.400000000000000367E-29 ) ) ;
#15628 = CARTESIAN_POINT ( 'NONE',  ( 97.81373435033219721, -40.51654435448209313, 87.63515866765291662 ) ) ;
#15629 = CARTESIAN_POINT ( 'NONE',  ( 144.7726661055232853, -137.4541655641505145, 247.5777877757870158 ) ) ;
#15630 = CARTESIAN_POINT ( 'NONE',  ( 110.8522644532615828, -45.98514059693295053, 97.88543543875454134 ) ) ;
#15631 = CARTESIAN_POINT ( 'NONE',  ( 102.6513375509277495, -45.45698538002856282, 127.2041967044829960 ) ) ;
#15632 = ORIENTED_EDGE ( 'NONE', *, *, #58322, .F. ) ;
#15633 = ORIENTED_EDGE ( 'NONE', *, *, #50626, .F. ) ;
#15634 = VECTOR ( 'NONE', #16169, 1000.000000000000000 ) ;
#15635 = CARTESIAN_POINT ( 'NONE',  ( 109.8762032759827321, -45.69504804023497968, 49.23777378208799149 ) ) ;
#15636 = ADVANCED_FACE ( 'NONE', ( #4809 ), #60192, .F. ) ;
#15637 = DIRECTION ( 'NONE',  ( -1.000000000000000000, -1.541976423090496028E-15, 0.000000000000000000 ) ) ;
#15639 = CARTESIAN_POINT ( 'NONE',  ( 109.6430121981732952, -46.48008671661597191, 37.78145861478355272 ) ) ;
#15638 = CARTESIAN_POINT ( 'NONE',  ( 101.7025241355417364, -45.60450926735014576, 198.1318157521009482 ) ) ;
#15640 = CYLINDRICAL_SURFACE ( 'NONE', #37676, 2.750000000000002665 ) ;
#15641 = CARTESIAN_POINT ( 'NONE',  ( 97.80791547859365664, -40.51903635482080546, 112.6360621818907077 ) ) ;
#15642 = CARTESIAN_POINT ( 'NONE',  ( 144.0667039024470455, -124.7784471599409102, 55.21780685541800437 ) ) ;
#15643 = PLANE ( 'NONE',  #28921 ) ;
#15644 = CARTESIAN_POINT ( 'NONE',  ( 131.3164832912739826, -18.72944715994100662, 3.101481641215524832 ) ) ;
#15645 = CARTESIAN_POINT ( 'NONE',  ( 97.63679352021414104, -31.00714225716590278, 125.8803871806719599 ) ) ;
#15646 = VERTEX_POINT ( 'NONE', #17977 ) ;
#15647 = ORIENTED_EDGE ( 'NONE', *, *, #73537, .F. ) ;
#15648 = EDGE_LOOP ( 'NONE', ( #3668, #11072, #80898, #25802 ) ) ;
#15649 = LINE ( 'NONE', #16101, #2689 ) ;
#15650 = AXIS2_PLACEMENT_3D ( 'NONE', #73864, #4830, #38438 ) ;
#15651 = CARTESIAN_POINT ( 'NONE',  ( 97.33763304300855168, -34.07186372398516028, 131.1148582292631772 ) ) ;
#15652 = CARTESIAN_POINT ( 'NONE',  ( 104.4075942973239393, -46.45795486759642046, 103.3647508459505246 ) ) ;
#15653 = CARTESIAN_POINT ( 'NONE',  ( 104.8109701446277171, -28.85573464981227687, 223.1166617981629656 ) ) ;
#15654 = VECTOR ( 'NONE', #67201, 1000.000000000000000 ) ;
#15655 = AXIS2_PLACEMENT_3D ( 'NONE', #35143, #20644, #14276 ) ;
#15656 = CARTESIAN_POINT ( 'NONE',  ( 21.03715912545823130, -47.82818131006186491, 313.9678068554150059 ) ) ;
#15657 = CARTESIAN_POINT ( 'NONE',  ( 114.5123156819773698, -29.42664080734638787, 149.4441967044819819 ) ) ;
#15658 = DIRECTION ( 'NONE',  ( 0.000000000000000000, 0.000000000000000000, -1.000000000000000000 ) ) ;
#15659 = ORIENTED_EDGE ( 'NONE', *, *, #39941, .F. ) ;
#15662 = VERTEX_POINT ( 'NONE', #46113 ) ;
#15661 = ORIENTED_EDGE ( 'NONE', *, *, #8102, .F. ) ;
#15660 = EDGE_CURVE ( 'NONE', #20369, #80721, #65597, .T. ) ;
#15663 = CARTESIAN_POINT ( 'NONE',  ( 123.6837132603319560, -53.34645651782485487, 218.8274735512161158 ) ) ;
#15664 = EDGE_LOOP ( 'NONE', ( #38777, #45392, #61313, #4338 ) ) ;
#15665 = ORIENTED_EDGE ( 'NONE', *, *, #25606, .F. ) ;
#15666 = DIRECTION ( 'NONE',  ( -0.7071067811865101582, -0.7071067811865849873, 0.000000000000000000 ) ) ;
#15667 = ADVANCED_FACE ( 'NONE', ( #10715 ), #24803, .F. ) ;
#15668 = CARTESIAN_POINT ( 'NONE',  ( 132.4277392773736040, -34.51875925606939433, 7.791169830160155740 ) ) ;
#15669 = CARTESIAN_POINT ( 'NONE',  ( 98.49168440212470443, -38.96576165349271292, 272.9615833058970225 ) ) ;
#15670 = AXIS2_PLACEMENT_3D ( 'NONE', #20750, #48422, #76160 ) ;
#15671 = DIRECTION ( 'NONE',  ( -1.047445008332813989E-14, 0.000000000000000000, 1.000000000000000000 ) ) ;
#15672 = ORIENTED_EDGE ( 'NONE', *, *, #53197, .T. ) ;
#15673 = ADVANCED_FACE ( 'NONE', ( #11629 ), #52536, .F. ) ;
#15674 = CIRCLE ( 'NONE', #28753, 2.999999999999919176 ) ;
#15675 = VECTOR ( 'NONE', #73653, 1000.000000000000000 ) ;
#15676 = CARTESIAN_POINT ( 'NONE',  ( 115.9158992903809633, -39.94991172188729678, 9.635625275910943088 ) ) ;
#15677 = LINE ( 'NONE', #58761, #53135 ) ;
#15678 = ORIENTED_EDGE ( 'NONE', *, *, #77160, .T. ) ;
#15679 = VERTEX_POINT ( 'NONE', #73391 ) ;
#15680 = AXIS2_PLACEMENT_3D ( 'NONE', #54804, #47552, #76170 ) ;
#15681 = CARTESIAN_POINT ( 'NONE',  ( 110.8545889635279309, -45.98418948027816811, 112.8856353431071398 ) ) ;
#15682 = ORIENTED_EDGE ( 'NONE', *, *, #57440, .F. ) ;
#15683 = ORIENTED_EDGE ( 'NONE', *, *, #22398, .T. ) ;
#15684 = EDGE_CURVE ( 'NONE', #13968, #19262, #85918, .T. ) ;
#15685 = CARTESIAN_POINT ( 'NONE',  ( 111.3125147634731462, -44.27080922411229835, 255.8147570362582712 ) ) ;
#15686 = CARTESIAN_POINT ( 'NONE',  ( 101.9611696646907433, -46.55956485693801028, 167.1832443235299763 ) ) ;
#15687 = CARTESIAN_POINT ( 'NONE',  ( 108.5866130067098538, -47.05677245125747277, 142.6927681330539883 ) ) ;
#15688 = EDGE_CURVE ( 'NONE', #60205, #2787, #32054, .T. ) ;
#15689 = CYLINDRICAL_SURFACE ( 'NONE', #10422, 1.000000000000000888 ) ;
#15690 = CARTESIAN_POINT ( 'NONE',  ( 113.0254242409527308, -46.03885118181761982, 214.0175300378159591 ) ) ;
#15691 = CARTESIAN_POINT ( 'NONE',  ( 1.088711004441995877E-14, 92.07499999999998863, -88.90000000000000568 ) ) ;
#15692 = DIRECTION ( 'NONE',  ( 0.000000000000000000, 0.000000000000000000, -1.000000000000000000 ) ) ;
#15693 = ORIENTED_EDGE ( 'NONE', *, *, #62002, .T. ) ;
#15694 = DIRECTION ( 'NONE',  ( 1.000000000000000000, 8.163404592831600092E-16, 1.020425574103949962E-15 ) ) ;
#15695 = ORIENTED_EDGE ( 'NONE', *, *, #20376, .F. ) ;
#15696 = ORIENTED_EDGE ( 'NONE', *, *, #38610, .F. ) ;
#15697 = AXIS2_PLACEMENT_3D ( 'NONE', #83304, #5205, #41491 ) ;
#15698 = CARTESIAN_POINT ( 'NONE',  ( 101.1758151987629333, -45.38431258166273352, 197.1013395616249966 ) ) ;
#15699 = ORIENTED_EDGE ( 'NONE', *, *, #54699, .F. ) ;
#15700 = CARTESIAN_POINT ( 'NONE',  ( 102.6160711382646156, -46.84739750188308705, 132.2346728949579528 ) ) ;
#15701 = FACE_OUTER_BOUND ( 'NONE', #66639, .T. ) ;
#15702 = CARTESIAN_POINT ( 'NONE',  ( 136.3178028891369422, -35.14744377621116200, 7.339349742409597255 ) ) ;
#15703 = DIRECTION ( 'NONE',  ( -3.100000000000000258E-29, 3.100000000000000044E-14, 1.000000000000000000 ) ) ;
#15706 = CARTESIAN_POINT ( 'NONE',  ( 97.57986484199628308, -43.79006170206856297, 257.8356252759109566 ) ) ;
#15705 = CYLINDRICAL_SURFACE ( 'NONE', #57204, 4.762500000000001066 ) ;
#15704 = CARTESIAN_POINT ( 'NONE',  ( 143.9834832912729894, -71.52944715994142655, 342.9256252759109884 ) ) ;
#15707 = CARTESIAN_POINT ( 'NONE',  ( 72.96458098368650269, 117.4749999999999943, 65.82083098368730134 ) ) ;
#15708 = DIRECTION ( 'NONE',  ( 0.000000000000000000, 0.000000000000000000, 1.000000000000000000 ) ) ;
#15709 = FACE_OUTER_BOUND ( 'NONE', #84617, .T. ) ;
#15710 = DIRECTION ( 'NONE',  ( -0.7071067811865779928, 0.7071067811865171526, -7.071067811865476319E-16 ) ) ;
#15711 = CARTESIAN_POINT ( 'NONE',  ( 109.7248659108412170, -27.00080517668511249, 255.8647919434466473 ) ) ;
#15712 = DIRECTION ( 'NONE',  ( 1.000000000000000000, 4.237773401492740281E-14, 0.000000000000000000 ) ) ;
#15714 = ORIENTED_EDGE ( 'NONE', *, *, #23337, .F. ) ;
#15713 = CARTESIAN_POINT ( 'NONE',  ( 99.34894212307516170, -29.65511154620466172, 275.7356252759109907 ) ) ;
#15715 = DIRECTION ( 'NONE',  ( 0.000000000000000000, 0.000000000000000000, -1.000000000000000000 ) ) ;
#15716 = CARTESIAN_POINT ( 'NONE',  ( 114.5280328947845732, -29.41122550446140949, 149.4441967044819819 ) ) ;
#15717 = CARTESIAN_POINT ( 'NONE',  ( 98.30635682897023742, -28.74854496012902771, 76.73848241876795839 ) ) ;
#15718 = CARTESIAN_POINT ( 'NONE',  ( 116.4163124136858443, -41.43834035574819552, 199.4556252759109611 ) ) ;
#15719 = DIRECTION ( 'NONE',  ( 0.000000000000000000, -1.000000000000000000, 0.000000000000000000 ) ) ;
#15720 = LINE ( 'NONE', #14830, #17060 ) ;
#15722 = DIRECTION ( 'NONE',  ( 1.000000000000000078E-15, -1.000000000000000000, 0.000000000000000000 ) ) ;
#15721 = CYLINDRICAL_SURFACE ( 'NONE', #26004, 3.000000000000002665 ) ;
#15723 = CARTESIAN_POINT ( 'NONE',  ( 182.2420472961719895, -31.76306994223730840, -5.074374724088000832 ) ) ;
#15724 = DIRECTION ( 'NONE',  ( 0.000000000000000000, 1.000000000000000000, 0.000000000000000000 ) ) ;
#15725 = VERTEX_POINT ( 'NONE', #87483 ) ;
#15726 = FACE_OUTER_BOUND ( 'NONE', #87837, .T. ) ;
#15727 = AXIS2_PLACEMENT_3D ( 'NONE', #16062, #84664, #15619 ) ;
#15728 = AXIS2_PLACEMENT_3D ( 'NONE', #37719, #65415, #64967 ) ;
#15729 = ADVANCED_FACE ( 'NONE', ( #65681 ), #17106, .T. ) ;
#15730 = ORIENTED_EDGE ( 'NONE', *, *, #61073, .T. ) ;
#15731 = ORIENTED_EDGE ( 'NONE', *, *, #36963, .T. ) ;
#15732 = AXIS2_PLACEMENT_3D ( 'NONE', #58633, #51368, #79112 ) ;
#15734 = ORIENTED_EDGE ( 'NONE', *, *, #3028, .T. ) ;
#15733 = DIRECTION ( 'NONE',  ( 0.000000000000000000, 0.000000000000000000, -1.000000000000000000 ) ) ;
#15735 = CARTESIAN_POINT ( 'NONE',  ( 116.1047473792919504, -29.10330858331350612, 70.38419670448192278 ) ) ;
#15736 = CARTESIAN_POINT ( 'NONE',  ( 31.56670390244800828, -32.29483332968611364, 117.4678068554150485 ) ) ;
#15737 = VECTOR ( 'NONE', #23902, 1000.000000000000000 ) ;
#15738 = CARTESIAN_POINT ( 'NONE',  ( -76.20505178924449297, 120.6499999999999915, 76.20505178924310030 ) ) ;
#15739 = CARTESIAN_POINT ( 'NONE',  ( 13.86911000615387302, 238.5000000000000000, 102.9892450244911686 ) ) ;
#15740 = AXIS2_PLACEMENT_3D ( 'NONE', #70714, #8491, #29382 ) ;
#15741 = AXIS2_PLACEMENT_3D ( 'NONE', #84537, #16375, #72231 ) ;
#15742 = CARTESIAN_POINT ( 'NONE',  ( 100.7700969181924506, -30.95782257301981488, 275.1581341137911068 ) ) ;
#15743 = ORIENTED_EDGE ( 'NONE', *, *, #28252, .T. ) ;
#15744 = EDGE_LOOP ( 'NONE', ( #2204, #44855, #5039, #49619 ) ) ;
#15745 = EDGE_LOOP ( 'NONE', ( #39573, #6649, #40203, #1587, #1818 ) ) ;
#15746 = EDGE_CURVE ( 'NONE', #12182, #58138, #18881, .T. ) ;
#15747 = CARTESIAN_POINT ( 'NONE',  ( 117.0718954852079605, -35.46248235573542473, 108.9272919426195614 ) ) ;
#15748 = DIRECTION ( 'NONE',  ( 0.000000000000000000, -1.000000000000000000, 0.000000000000000000 ) ) ;
#15749 = CARTESIAN_POINT ( 'NONE',  ( 97.06108334801497506, -37.99647572000111495, 162.4272970119406523 ) ) ;
#15750 = CARTESIAN_POINT ( 'NONE',  ( 97.31578350476630135, -39.30578092224938302, 21.53098511257883274 ) ) ;
#15751 = DIRECTION ( 'NONE',  ( 0.000000000000000000, 0.000000000000000000, 1.000000000000000000 ) ) ;
#15752 = DIRECTION ( 'NONE',  ( -0.9963424814100679816, 0.08544974978095716545, 0.000000000000000000 ) ) ;
#15753 = DIRECTION ( 'NONE',  ( 9.351236661543306751E-17, -3.725950533538267725E-29, -1.000000000000000000 ) ) ;
#15754 = CARTESIAN_POINT ( 'NONE',  ( 64.68306507141299733, -72.55818180160879649, 394.9756252759101471 ) ) ;
#15755 = CARTESIAN_POINT ( 'NONE',  ( 107.1951288810177090, -26.32694189238797833, 35.06705384733893283 ) ) ;
#15756 = EDGE_CURVE ( 'NONE', #51663, #21659, #13412, .T. ) ;
#15757 = ORIENTED_EDGE ( 'NONE', *, *, #50914, .T. ) ;
#15758 = EDGE_CURVE ( 'NONE', #75933, #52977, #86148, .T. ) ;
#15759 = CARTESIAN_POINT ( 'NONE',  ( 76.20505178924389611, 120.6499999999999915, -76.20505178924359768 ) ) ;
#15760 = VECTOR ( 'NONE', #81793, 1000.000000000000000 ) ;
#15761 = DIRECTION ( 'NONE',  ( 9.032638163712999905E-13, -1.000000000000000000, 4.100000000000000342E-29 ) ) ;
#15762 = CARTESIAN_POINT ( 'NONE',  ( 99.91476266851738330, -32.73750773393640401, 108.7395189410199663 ) ) ;
#15763 = AXIS2_PLACEMENT_3D ( 'NONE', #61072, #12490, #53786 ) ;
#15764 = EDGE_CURVE ( 'NONE', #1830, #57751, #46564, .T. ) ;
#15765 = FACE_OUTER_BOUND ( 'NONE', #19033, .T. ) ;
#15766 = ORIENTED_EDGE ( 'NONE', *, *, #3352, .T. ) ;
#15767 = ORIENTED_EDGE ( 'NONE', *, *, #74202, .F. ) ;
#15768 = CARTESIAN_POINT ( 'NONE',  ( 117.0718258217757466, -35.46190141227904746, 138.9264153952272807 ) ) ;
#15769 = EDGE_LOOP ( 'NONE', ( #70176, #75321 ) ) ;
#15770 = ORIENTED_EDGE ( 'NONE', *, *, #10799, .T. ) ;
#15771 = EDGE_CURVE ( 'NONE', #28030, #11013, #46706, .T. ) ;
#15772 = CARTESIAN_POINT ( 'NONE',  ( 108.0951925567892431, -27.89746624773302841, 126.4158690201829813 ) ) ;
#15773 = AXIS2_PLACEMENT_3D ( 'NONE', #15254, #29775, #2070 ) ;
#15774 = PLANE ( 'NONE',  #46681 ) ;
#15775 = CARTESIAN_POINT ( 'NONE',  ( 104.2081133107797228, -25.20330419090194951, 86.26991099019699050 ) ) ;
#15776 = CARTESIAN_POINT ( 'NONE',  ( 114.6097843884836323, -43.32694117741820605, 18.25468785797279025 ) ) ;
#15777 = AXIS2_PLACEMENT_3D ( 'NONE', #72705, #31351, #73582 ) ;
#15778 = VERTEX_POINT ( 'NONE', #12073 ) ;
#15779 = AXIS2_PLACEMENT_3D ( 'NONE', #38643, #19100, #46785 ) ;
#15780 = VERTEX_POINT ( 'NONE', #58858 ) ;
#15781 = ORIENTED_EDGE ( 'NONE', *, *, #11179, .T. ) ;
#15782 = EDGE_CURVE ( 'NONE', #29833, #32371, #40948, .T. ) ;
#15783 = CARTESIAN_POINT ( 'NONE',  ( 108.9893125699443175, -46.99828796752551341, 82.72419670448194040 ) ) ;
#15784 = ORIENTED_EDGE ( 'NONE', *, *, #18613, .T. ) ;
#15785 = CARTESIAN_POINT ( 'NONE',  ( 99.99555918775621421, -44.36035129061385618, 46.98133956162592284 ) ) ;
#15786 = CARTESIAN_POINT ( 'NONE',  ( 96.02367466659750050, -35.86829477906547226, 187.2765776568629406 ) ) ;
#15787 = EDGE_CURVE ( 'NONE', #223, #13942, #58421, .T. ) ;
#15788 = CARTESIAN_POINT ( 'NONE',  ( 12.27293249669208919, 79.25788962028573792, -117.9191036749242301 ) ) ;
#15789 = CARTESIAN_POINT ( 'NONE',  ( 100.8868993066867432, -44.69975041575762020, 128.0522334713024293 ) ) ;
#15790 = CARTESIAN_POINT ( 'NONE',  ( 107.3339483091110225, -26.30778942656879948, 116.0556252759109555 ) ) ;
#15792 = ADVANCED_FACE ( 'NONE', ( #45224 ), #24365, .F. ) ;
#15791 = CARTESIAN_POINT ( 'NONE',  ( 31.89136050872298966, -31.76306994223740432, 342.9256252759109884 ) ) ;
#15793 = EDGE_LOOP ( 'NONE', ( #81798, #28043, #70438, #46268, #46084 ) ) ;
#15794 = AXIS2_PLACEMENT_3D ( 'NONE', #86905, #79213, #72385 ) ;
#15795 = FACE_BOUND ( 'NONE', #58103, .T. ) ;
#15796 = EDGE_CURVE ( 'NONE', #73048, #25675, #52471, .T. ) ;
#15797 = ORIENTED_EDGE ( 'NONE', *, *, #36475, .T. ) ;
#15798 = VECTOR ( 'NONE', #60698, 1000.000000000000000 ) ;
#15799 = CARTESIAN_POINT ( 'NONE',  ( 97.82514972460828062, -40.55017182310744062, 132.6388286205130385 ) ) ;
#15800 = ORIENTED_EDGE ( 'NONE', *, *, #76985, .T. ) ;
#15801 = ORIENTED_EDGE ( 'NONE', *, *, #13633, .F. ) ;
#15802 = CARTESIAN_POINT ( 'NONE',  ( 52.38749999999999574, 94.53880000000000905, 254.7937499999999886 ) ) ;
#15803 = LINE ( 'NONE', #76679, #8718 ) ;
#15804 = CARTESIAN_POINT ( 'NONE',  ( 116.7272869458707305, -31.35841744470506498, 29.24229194257799236 ) ) ;
#15805 = CARTESIAN_POINT ( 'NONE',  ( 23.27731929905161223, 53.97500000000000142, 30.16249999999999076 ) ) ;
#15806 = CARTESIAN_POINT ( 'NONE',  ( 172.5664832912740110, -36.32844715994070839, 138.9256252759119832 ) ) ;
#15807 = LINE ( 'NONE', #50759, #598 ) ;
#15808 = CARTESIAN_POINT ( 'NONE',  ( 99.77418633167435758, -43.29726106931981633, 56.90991099019693422 ) ) ;
#15810 = CARTESIAN_POINT ( 'NONE',  ( 97.76587557681025942, -42.65924729906315349, 137.7661014663869992 ) ) ;
#15809 = DIRECTION ( 'NONE',  ( 0.000000000000000000, 0.000000000000000000, -1.000000000000000000 ) ) ;
#15811 = PLANE ( 'NONE',  #23393 ) ;
#15812 = CARTESIAN_POINT ( 'NONE',  ( -544.5124999999999318, 53.97500000000000142, 50.79999999999999716 ) ) ;
#15813 = ORIENTED_EDGE ( 'NONE', *, *, #63632, .T. ) ;
#15814 = CARTESIAN_POINT ( 'NONE',  ( 71.77848634863140376, 127.0000000000000000, -77.39114642429929347 ) ) ;
#15815 = DIRECTION ( 'NONE',  ( 1.000000000000000000, 4.163336342344333240E-14, 0.000000000000000000 ) ) ;
#15816 = LINE ( 'NONE', #9890, #2148 ) ;
#15817 = ORIENTED_EDGE ( 'NONE', *, *, #62008, .T. ) ;
#15818 = DIRECTION ( 'NONE',  ( -1.000000000000000078E-15, -1.000000000000000083E-30, 1.000000000000000000 ) ) ;
#15820 = ORIENTED_EDGE ( 'NONE', *, *, #71493, .F. ) ;
#15819 = CARTESIAN_POINT ( 'NONE',  ( 109.3681991936945508, -25.87058038976459429, 184.9222919425779708 ) ) ;
#15821 = LINE ( 'NONE', #43496, #23380 ) ;
#15822 = CARTESIAN_POINT ( 'NONE',  ( 116.0738972362454149, -42.02130438377608357, 234.4041967044819899 ) ) ;
#15823 = CARTESIAN_POINT ( 'NONE',  ( 117.9015171282527916, -39.13767059441630636, 99.64038718067195077 ) ) ;
#15824 = CARTESIAN_POINT ( 'NONE',  ( 91.12500358871285755, -35.36225116344564157, 302.4856252759109907 ) ) ;
#15825 = CYLINDRICAL_SURFACE ( 'NONE', #56125, 9.999999999999998224 ) ;
#15826 = CIRCLE ( 'NONE', #40438, 2.116999999999993776 ) ;
#15827 = LINE ( 'NONE', #8564, #74290 ) ;
#15828 = ORIENTED_EDGE ( 'NONE', *, *, #19246, .T. ) ;
#15829 = ORIENTED_EDGE ( 'NONE', *, *, #71382, .T. ) ;
#15830 = ORIENTED_EDGE ( 'NONE', *, *, #52196, .F. ) ;
#15831 = ORIENTED_EDGE ( 'NONE', *, *, #25316, .T. ) ;
#15832 = CARTESIAN_POINT ( 'NONE',  ( 0.000000000000000000, 117.4749999999999943, -103.1875000000000000 ) ) ;
#15833 = CARTESIAN_POINT ( 'NONE',  ( 100.8232821092315845, -45.85065428865130599, 238.1108633711489517 ) ) ;
#15834 = DIRECTION ( 'NONE',  ( 0.000000000000000000, 1.000000000000000000, 0.000000000000000000 ) ) ;
#15835 = CARTESIAN_POINT ( 'NONE',  ( 107.3428450438784694, -25.27364292152175551, 322.4523926293242653 ) ) ;
#15836 = VECTOR ( 'NONE', #60472, 1000.000000000000000 ) ;
#15838 = CARTESIAN_POINT ( 'NONE',  ( 3.110602869834275287E-15, 2.031999999999865025, -25.39999999999999858 ) ) ;
#15837 = DIRECTION ( 'NONE',  ( 1.000000000000000078E-15, 1.000000000000000083E-30, -1.000000000000000000 ) ) ;
#15839 = DIRECTION ( 'NONE',  ( 0.000000000000000000, -1.000000000000000000, 0.000000000000000000 ) ) ;
#15840 = CARTESIAN_POINT ( 'NONE',  ( 105.4174756516424054, -47.04580008967651850, 37.44991099019695469 ) ) ;
#15841 = VERTEX_POINT ( 'NONE', #56859 ) ;
#15842 = ORIENTED_EDGE ( 'NONE', *, *, #59501, .T. ) ;
#15843 = VECTOR ( 'NONE', #60284, 1000.000000000000000 ) ;
#15844 = EDGE_LOOP ( 'NONE', ( #51855, #87941, #47340, #61937, #19238 ) ) ;
#15845 = ADVANCED_FACE ( 'NONE', ( #35980 ), #30788, .T. ) ;
#15846 = FILL_AREA_STYLE ('',( #57153 ) ) ;
#15847 = CARTESIAN_POINT ( 'NONE',  ( 116.3181387014812458, -32.94505625723229514, 15.13562527591094664 ) ) ;
#15848 = EDGE_CURVE ( 'NONE', #46344, #21324, #68827, .T. ) ;
#15849 = CARTESIAN_POINT ( 'NONE',  ( 116.8725690376871569, -36.55701438716827312, 284.8413395616245793 ) ) ;
#15850 = DIRECTION ( 'NONE',  ( -0.7071067811869841124, 0.7071067811861110330, 0.000000000000000000 ) ) ;
#15852 = EDGE_CURVE ( 'NONE', #56233, #72479, #72858, .T. ) ;
#15851 = AXIS2_PLACEMENT_3D ( 'NONE', #28159, #28616, #35875 ) ;
#15853 = CARTESIAN_POINT ( 'NONE',  ( 101.8448680821487642, -28.45912855063591351, 106.5241967044819944 ) ) ;
#15854 = LINE ( 'NONE', #23577, #6813 ) ;
#15855 = EDGE_CURVE ( 'NONE', #36904, #3733, #63242, .T. ) ;
#15856 = ORIENTED_EDGE ( 'NONE', *, *, #54472, .F. ) ;
#15857 = CARTESIAN_POINT ( 'NONE',  ( -487.2989999999999782, 21.43125000000029701, 15.23694598552314972 ) ) ;
#15858 = EDGE_CURVE ( 'NONE', #42921, #18344, #10485, .T. ) ;
#15859 = CARTESIAN_POINT ( 'NONE',  ( 78.02982435611764345, -34.87939921900456142, 2.327894594453169042 ) ) ;
#15860 = AXIS2_PLACEMENT_3D ( 'NONE', #52845, #79286, #85656 ) ;
#15861 = ORIENTED_EDGE ( 'NONE', *, *, #40284, .T. ) ;
#15862 = DIRECTION ( 'NONE',  ( -1.047445008332813989E-14, 0.000000000000000000, 1.000000000000000000 ) ) ;
#15863 = CARTESIAN_POINT ( 'NONE',  ( 98.91757684337089529, -33.81461462136097396, 23.88332846482899186 ) ) ;
#15864 = ADVANCED_FACE ( 'NONE', ( #75646 ), #49590, .T. ) ;
#15865 = DIRECTION ( 'NONE',  ( 2.900000000000000265E-14, -2.000000000000000155E-15, 1.000000000000000000 ) ) ;
#15866 = EDGE_CURVE ( 'NONE', #88862, #32266, #13418, .T. ) ;
#15867 = AXIS2_PLACEMENT_3D ( 'NONE', #5632, #25157, #46482 ) ;
#15868 = CARTESIAN_POINT ( 'NONE',  ( 0.000000000000000000, 114.2999999999999972, 0.000000000000000000 ) ) ;
#15869 = AXIS2_PLACEMENT_3D ( 'NONE', #68635, #54965, #41350 ) ;
#15870 = LINE ( 'NONE', #51248, #69142 ) ;
#15871 = ORIENTED_EDGE ( 'NONE', *, *, #23886, .T. ) ;
#15872 = LINE ( 'NONE', #57178, #47937 ) ;
#15873 = DIRECTION ( 'NONE',  ( 0.000000000000000000, 0.000000000000000000, -1.000000000000000000 ) ) ;
#15874 = ORIENTED_EDGE ( 'NONE', *, *, #1230, .F. ) ;
#15875 = CARTESIAN_POINT ( 'NONE',  ( 116.9750915152277884, -33.48807190773455034, 89.07848241876791917 ) ) ;
#15876 = EDGE_LOOP ( 'NONE', ( #25160, #49711, #11893 ) ) ;
#15877 = CARTESIAN_POINT ( 'NONE',  ( 100.5751258508236674, -42.28088033547287949, 31.31241982807697610 ) ) ;
#15878 = EDGE_CURVE ( 'NONE', #84869, #1472, #88834, .T. ) ;
#15879 = FACE_OUTER_BOUND ( 'NONE', #43991, .T. ) ;
#15880 = CARTESIAN_POINT ( 'NONE',  ( 96.59955023297820276, -32.98040794253977737, 176.0527681330549683 ) ) ;
#15881 = CARTESIAN_POINT ( 'NONE',  ( -21.12245462538188079, 46.12462447032474699, 31.70988376339461112 ) ) ;
#15882 = LINE ( 'NONE', #79458, #82231 ) ;
#15883 = DIRECTION ( 'NONE',  ( 0.000000000000000000, 0.000000000000000000, 1.000000000000000000 ) ) ;
#15884 = CARTESIAN_POINT ( 'NONE',  ( 114.6444261855607891, -91.15344715994180547, -11.78219314458242550 ) ) ;
#15885 = AXIS2_PLACEMENT_3D ( 'NONE', #22573, #63442, #84807 ) ;
#15886 = CARTESIAN_POINT ( 'NONE',  ( 102.3596500697202174, -47.65578173298946751, 283.2527681330539053 ) ) ;
#15887 = VERTEX_POINT ( 'NONE', #5711 ) ;
#15888 = CARTESIAN_POINT ( 'NONE',  ( 107.0667039024470171, -89.08784823670062281, -21.78219314458248945 ) ) ;
#15889 = ORIENTED_EDGE ( 'NONE', *, *, #242, .F. ) ;
#15890 = CARTESIAN_POINT ( 'NONE',  ( 117.1680251128577908, -33.85633223813928794, 145.0470538473399529 ) ) ;
#15891 = CARTESIAN_POINT ( 'NONE',  ( 74.15067561874269586, 120.6499999999999915, -68.53801554307419508 ) ) ;
#15892 = ORIENTED_EDGE ( 'NONE', *, *, #87439, .F. ) ;
#15893 = EDGE_LOOP ( 'NONE', ( #17638, #5431, #19091, #83818, #40563, #76163, #41694, #68287, #84775, #36747, #59765, #35654 ) ) ;
#15894 = VERTEX_POINT ( 'NONE', #21924 ) ;
#15895 = CARTESIAN_POINT ( 'NONE',  ( 101.9936208123286150, -45.44607146504151274, 122.1564585975432067 ) ) ;
#15896 = DIRECTION ( 'NONE',  ( 0.000000000000000000, -1.000000000000000000, 0.000000000000000000 ) ) ;
#15897 = LINE ( 'NONE', #23617, #32693 ) ;
#15898 = CARTESIAN_POINT ( 'NONE',  ( 41.56648329127381203, -18.82844715994071194, 321.9256252759119548 ) ) ;
#15899 = CARTESIAN_POINT ( 'NONE',  ( 142.8687636814962616, 5.654319119531167281, 361.9756252759100335 ) ) ;
#15900 = CARTESIAN_POINT ( 'NONE',  ( 115.9451031845006099, -42.19318012571019949, 14.38705384733995984 ) ) ;
#15902 = EDGE_CURVE ( 'NONE', #78335, #35491, #45291, .T. ) ;
#15901 = DIRECTION ( 'NONE',  ( 0.000000000000000000, 0.000000000000000000, -1.000000000000000000 ) ) ;
#15903 = ORIENTED_EDGE ( 'NONE', *, *, #79250, .F. ) ;
#15904 = DIRECTION ( 'NONE',  ( -4.237773401492740281E-14, 1.000000000000000000, 0.000000000000000000 ) ) ;
#15905 = AXIS2_PLACEMENT_3D ( 'NONE', #55887, #83636, #29114 ) ;
#15906 = EDGE_CURVE ( 'NONE', #25266, #11985, #6155, .T. ) ;
#15907 = CARTESIAN_POINT ( 'NONE',  ( 117.0718948736623020, -35.46247637142937492, 43.92702797836822981 ) ) ;
#15908 = VERTEX_POINT ( 'NONE', #20233 ) ;
#15909 = ORIENTED_EDGE ( 'NONE', *, *, #7417, .F. ) ;
#15910 = AXIS2_PLACEMENT_3D ( 'NONE', #29644, #49623, #1950 ) ;
#15911 = AXIS2_PLACEMENT_3D ( 'NONE', #43793, #9734, #10613 ) ;
#15912 = DIRECTION ( 'NONE',  ( 1.000000000000000078E-15, 0.000000000000000000, -1.000000000000000000 ) ) ;
#15913 = PLANE ( 'NONE',  #74500 ) ;
#15914 = DIRECTION ( 'NONE',  ( 0.02992792722492259097, 0.000000000000000000, 0.9995520592605567911 ) ) ;
#15915 = DIRECTION ( 'NONE',  ( -0.000000000000000000, 1.000000000000000000, 0.000000000000000000 ) ) ;
#15916 = FACE_OUTER_BOUND ( 'NONE', #86387, .T. ) ;
#15917 = CARTESIAN_POINT ( 'NONE',  ( 109.5825779133427460, -28.02991049533996204, 214.2628960185529365 ) ) ;
#15919 = CARTESIAN_POINT ( 'NONE',  ( 95.28387218206130171, -35.72034718286344912, 32.25848241876794020 ) ) ;
#15918 = LINE ( 'NONE', #44039, #70783 ) ;
#15920 = CARTESIAN_POINT ( 'NONE',  ( 125.9597867034675573, 66.44223047789067493, 34.33911078552125673 ) ) ;
#15921 = CARTESIAN_POINT ( 'NONE',  ( 96.04102276344947597, -38.01478905114413465, 86.43086337114897333 ) ) ;
#15922 = ORIENTED_EDGE ( 'NONE', *, *, #38302, .F. ) ;
#15923 = CARTESIAN_POINT ( 'NONE',  ( 131.3164832912739826, -18.72944715994100662, 6.749768910606465333 ) ) ;
#15924 = ORIENTED_EDGE ( 'NONE', *, *, #22345, .F. ) ;
#15925 = AXIS2_PLACEMENT_3D ( 'NONE', #16784, #44465, #9083 ) ;
#15926 = DIRECTION ( 'NONE',  ( -0.000000000000000000, 1.000000000000000000, 0.000000000000000000 ) ) ;
#15927 = AXIS2_PLACEMENT_3D ( 'NONE', #22761, #2312, #51317 ) ;
#15928 = DIRECTION ( 'NONE',  ( 1.000000000000000000, -6.745093096447288888E-17, 9.693101022688619289E-16 ) ) ;
#15929 = EDGE_LOOP ( 'NONE', ( #86961, #51835, #66029, #6377 ) ) ;
#15930 = DIRECTION ( 'NONE',  ( 0.9068632946707807507, -0.4214249218767880945, 8.673617379884035472E-16 ) ) ;
#15931 = ORIENTED_EDGE ( 'NONE', *, *, #23588, .T. ) ;
#15932 = FACE_OUTER_BOUND ( 'NONE', #81469, .T. ) ;
#15933 = CIRCLE ( 'NONE', #50724, 6.571100913904396990 ) ;
#15934 = CARTESIAN_POINT ( 'NONE',  ( 152.0371591254585155, -47.82818131005588214, 180.4678068554149775 ) ) ;
#15935 = LINE ( 'NONE', #29556, #53822 ) ;
#15936 = ORIENTED_EDGE ( 'NONE', *, *, #59644, .T. ) ;
#15937 = CARTESIAN_POINT ( 'NONE',  ( 97.20468889015201341, -31.68559423518837193, 95.96229194257799122 ) ) ;
#15938 = DIRECTION ( 'NONE',  ( -1.000000000000000000, 0.000000000000000000, -2.544367396927093358E-16 ) ) ;
#15939 = CARTESIAN_POINT ( 'NONE',  ( 97.39138288182120107, -39.27886290962566562, 166.5314880106770659 ) ) ;
#15940 = DIRECTION ( 'NONE',  ( 0.000000000000000000, 0.000000000000000000, 1.000000000000000000 ) ) ;
#15941 = PLANE ( 'NONE',  #18010 ) ;
#15942 = ORIENTED_EDGE ( 'NONE', *, *, #70178, .F. ) ;
#15943 = CIRCLE ( 'NONE', #60841, 2.117000000000000881 ) ;
#15944 = LINE ( 'NONE', #62733, #48881 ) ;
#15945 = CARTESIAN_POINT ( 'NONE',  ( 97.33784134059621351, -34.07106442472682772, 156.1147919339565817 ) ) ;
#15946 = DIRECTION ( 'NONE',  ( -0.4999999999999989453, -0.8660254037844392627, 2.684678751731760294E-14 ) ) ;
#15948 = LINE ( 'NONE', #44968, #22470 ) ;
#15947 = DIRECTION ( 'NONE',  ( 5.512527431108029424E-15, -1.000000000000000000, 0.000000000000000000 ) ) ;
#15949 = CARTESIAN_POINT ( 'NONE',  ( 180.1667039024460166, -26.71338133339240528, -5.074374724088000832 ) ) ;
#15951 = EDGE_CURVE ( 'NONE', #64336, #42621, #15095, .T. ) ;
#15950 = VECTOR ( 'NONE', #21904, 1000.000000000000000 ) ;
#15952 = ORIENTED_EDGE ( 'NONE', *, *, #9927, .T. ) ;
#15953 = EDGE_CURVE ( 'NONE', #2317, #20780, #81582, .T. ) ;
#15954 = LINE ( 'NONE', #77736, #70903 ) ;
#15955 = EDGE_CURVE ( 'NONE', #68627, #34761, #42770, .T. ) ;
#15956 = CARTESIAN_POINT ( 'NONE',  ( 97.38117110781249153, -35.36630255995241612, 177.2156252759109805 ) ) ;
#15958 = ORIENTED_EDGE ( 'NONE', *, *, #60966, .T. ) ;
#15957 = CARTESIAN_POINT ( 'NONE',  ( -147.4575741623270062, 0.000000000000000000, 135.2444258376732193 ) ) ;
#15959 = AXIS2_PLACEMENT_3D ( 'NONE', #60061, #32820, #87352 ) ;
#15960 = EDGE_CURVE ( 'NONE', #26855, #7253, #33405, .T. ) ;
#15961 = CARTESIAN_POINT ( 'NONE',  ( 110.8778723966665751, -46.37372517157803742, 18.88800622829095488 ) ) ;
#15962 = DIRECTION ( 'NONE',  ( 0.000000000000000000, 0.000000000000000000, 1.000000000000000000 ) ) ;
#15963 = CARTESIAN_POINT ( 'NONE',  ( 70.63919639214310564, 91.07499999999996021, 53.63573739454427880 ) ) ;
#15964 = CARTESIAN_POINT ( 'NONE',  ( 70.56670390244700286, -68.87844715994098976, 222.2178068554179902 ) ) ;
#15965 = CARTESIAN_POINT ( 'NONE',  ( 6.938893903907229955E-15, 67.86880000000000734, 216.0269999999999868 ) ) ;
#15966 = ADVANCED_FACE ( 'NONE', ( #47905 ), #33850, .T. ) ;
#15967 = CARTESIAN_POINT ( 'NONE',  ( 100.9552578586416018, -28.70656802983730671, 30.59412679818443337 ) ) ;
#15968 = CARTESIAN_POINT ( 'NONE',  ( 99.44473759953881142, -30.59981194223813361, 240.7870538473399620 ) ) ;
#15969 = ORIENTED_EDGE ( 'NONE', *, *, #75883, .F. ) ;
#15970 = ORIENTED_EDGE ( 'NONE', *, *, #71995, .F. ) ;
#15971 = CARTESIAN_POINT ( 'NONE',  ( 97.15642216441104040, -38.53537999780244405, 197.9015833058969633 ) ) ;
#15972 = CIRCLE ( 'NONE', #1451, 0.5000000000000004441 ) ;
#15973 = ADVANCED_FACE ( 'NONE', ( #54713 ), #29173, .F. ) ;
#15974 = CARTESIAN_POINT ( 'NONE',  ( 116.8159028922284648, -34.14818352781880151, 55.03137681045001273 ) ) ;
#15975 = CARTESIAN_POINT ( 'NONE',  ( 101.8597501770084364, -45.35270844728685802, 48.57586902018196184 ) ) ;
#15976 = CARTESIAN_POINT ( 'NONE',  ( -90.25311968877612401, 94.92443974548203300, 94.33669211993731096 ) ) ;
#15977 = EDGE_CURVE ( 'NONE', #23851, #1382, #39524, .T. ) ;
#15978 = DIRECTION ( 'NONE',  ( 1.000000000000000078E-15, -1.000000000000000000, 0.000000000000000000 ) ) ;
#15979 = VECTOR ( 'NONE', #58225, 1000.000000000000000 ) ;
#15980 = FACE_OUTER_BOUND ( 'NONE', #38316, .T. ) ;
#15981 = ORIENTED_EDGE ( 'NONE', *, *, #18249, .T. ) ;
#15982 = DIRECTION ( 'NONE',  ( 1.000000000000000000, 1.000000000000000078E-15, 0.000000000000000000 ) ) ;
#15983 = DIRECTION ( 'NONE',  ( 0.000000000000000000, 0.000000000000000000, 1.000000000000000000 ) ) ;
#15984 = DIRECTION ( 'NONE',  ( -1.514143847546114723E-15, -0.8660254037844387076, 0.4999999999999998890 ) ) ;
#15985 = CARTESIAN_POINT ( 'NONE',  ( 115.2346088729120339, -30.22974330756297690, 244.3613395616249875 ) ) ;
#15986 = CARTESIAN_POINT ( 'NONE',  ( 122.2189888861420286, -96.57077177932983147, -11.78219314458225853 ) ) ;
#15987 = VERTEX_POINT ( 'NONE', #88386 ) ;
#15988 = ORIENTED_EDGE ( 'NONE', *, *, #36853, .F. ) ;
#15989 = EDGE_CURVE ( 'NONE', #27698, #29421, #30510, .T. ) ;
#15990 = CARTESIAN_POINT ( 'NONE',  ( 105.7154773210734220, -46.72385839103964855, 82.46895860850119675 ) ) ;
#15991 = FACE_OUTER_BOUND ( 'NONE', #84926, .T. ) ;
#15992 = AXIS2_PLACEMENT_3D ( 'NONE', #74453, #79947, #45382 ) ;
#15993 = DIRECTION ( 'NONE',  ( 1.000000000000000000, 6.145690160522439356E-16, 0.000000000000000000 ) ) ;
#15994 = CARTESIAN_POINT ( 'NONE',  ( 122.2221484686747459, -111.8737466215628729, -21.78219314458179667 ) ) ;
#15995 = CARTESIAN_POINT ( 'NONE',  ( 110.1676348244934331, -46.62498374987613659, 48.80610146638597513 ) ) ;
#15996 = CARTESIAN_POINT ( 'NONE',  ( 51.56670390244699576, -19.82844715994031048, -5.074374724088000832 ) ) ;
#15997 = VERTEX_POINT ( 'NONE', #64144 ) ;
#15998 = CARTESIAN_POINT ( 'NONE',  ( 118.1291538054787509, -37.63212066291781355, 34.77372051400695341 ) ) ;
#15999 = PLANE ( 'NONE',  #77278 ) ;
#16000 = CARTESIAN_POINT ( 'NONE',  ( 99.33304576907053729, -28.83178728225833609, 270.7051490854348685 ) ) ;
#16001 = VERTEX_POINT ( 'NONE', #58214 ) ;
#16002 = CIRCLE ( 'NONE', #30461, 10.00000000000000888 ) ;
#16003 = CARTESIAN_POINT ( 'NONE',  ( 37.35959712141530531, -48.62134037890907479, 180.4678068554150911 ) ) ;
#16004 = DIRECTION ( 'NONE',  ( 1.000000000000000000, 0.000000000000000000, 0.000000000000000000 ) ) ;
#16005 = CYLINDRICAL_SURFACE ( 'NONE', #14653, 4.500000000000003553 ) ;
#16006 = CARTESIAN_POINT ( 'NONE',  ( 110.2109830224615052, -27.99972479296931382, 97.61951894101994753 ) ) ;
#16007 = CARTESIAN_POINT ( 'NONE',  ( 102.2271567091324158, -45.98785831331388607, 208.1927681330539599 ) ) ;
#16008 = CARTESIAN_POINT ( 'NONE',  ( 107.0664832912739399, -36.72944715994095333, 302.6356252759109680 ) ) ;
#16009 = EDGE_LOOP ( 'NONE', ( #36790, #50827, #20500, #17506 ) ) ;
#16010 = EDGE_CURVE ( 'NONE', #73246, #61299, #27994, .T. ) ;
#16011 = DIRECTION ( 'NONE',  ( -0.000000000000000000, 1.000000000000000000, -0.000000000000000000 ) ) ;
#16012 = VECTOR ( 'NONE', #80001, 1000.000000000000000 ) ;
#16013 = ORIENTED_EDGE ( 'NONE', *, *, #1081, .T. ) ;
#16014 = ORIENTED_EDGE ( 'NONE', *, *, #24103, .F. ) ;
#16015 = DIRECTION ( 'NONE',  ( 1.000000000000000000, 0.000000000000000000, 0.000000000000000000 ) ) ;
#16016 =( BOUNDED_CURVE ( )  B_SPLINE_CURVE ( 3, ( #49072, #35007, #76806, #14589 ),
 .UNSPECIFIED., .F., .T. ) 
 B_SPLINE_CURVE_WITH_KNOTS ( ( 4, 4 ),
 ( 4.712388980378937831, 6.283185307174309564 ),
 .UNSPECIFIED. ) 
 CURVE ( )  GEOMETRIC_REPRESENTATION_ITEM ( )  RATIONAL_B_SPLINE_CURVE ( ( 1.000000000000000000, 0.8047378541230092441, 0.8047378541230092441, 1.000000000000000000 ) ) 
 REPRESENTATION_ITEM ( '' )  );
#16017 = VERTEX_POINT ( 'NONE', #86375 ) ;
#16018 = VERTEX_POINT ( 'NONE', #22819 ) ;
#16019 = PLANE ( 'NONE',  #9158 ) ;
#16020 = CARTESIAN_POINT ( 'NONE',  ( 97.81136857603131318, -40.51756142711754194, 161.6353372277744143 ) ) ;
#16021 = CARTESIAN_POINT ( 'NONE',  ( 107.2856214976012552, -28.19082255356615008, 119.4781341137909578 ) ) ;
#16022 = CARTESIAN_POINT ( 'NONE',  ( 100.2327115992702176, -45.44695862323239055, 277.0594347997204068 ) ) ;
#16023 = AXIS2_PLACEMENT_3D ( 'NONE', #59509, #39526, #33162 ) ;
#16024 = DIRECTION ( 'NONE',  ( 0.000000000000000000, 1.000000000000000000, 0.000000000000000000 ) ) ;
#16025 = EDGE_LOOP ( 'NONE', ( #87482, #78346, #31251, #55620 ) ) ;
#16026 = CIRCLE ( 'NONE', #65301, 16.00000000000000000 ) ;
#16027 = EDGE_CURVE ( 'NONE', #29809, #16028, #43681, .T. ) ;
#16028 = VERTEX_POINT ( 'NONE', #72301 ) ;
#16029 = DIRECTION ( 'NONE',  ( -1.000000000000000000, 0.000000000000000000, 0.000000000000000000 ) ) ;
#16030 = CARTESIAN_POINT ( 'NONE',  ( -215.9000000000000057, 3.174999999999999822, 142.8750000000000000 ) ) ;
#16031 = FACE_OUTER_BOUND ( 'NONE', #32850, .T. ) ;
#16032 = VECTOR ( 'NONE', #32667, 1000.000000000000000 ) ;
#16033 = EDGE_CURVE ( 'NONE', #73048, #56141, #24149, .T. ) ;
#16034 = CARTESIAN_POINT ( 'NONE',  ( 98.16479183632776540, -43.36064410082828857, 111.8480062282919647 ) ) ;
#16035 = CARTESIAN_POINT ( 'NONE',  ( 111.0096634661633885, -46.42778601040829045, 282.8841967044824628 ) ) ;
#16036 = ORIENTED_EDGE ( 'NONE', *, *, #55495, .F. ) ;
#16037 = UNCERTAINTY_MEASURE_WITH_UNIT (LENGTH_MEASURE( 1.000000000000000082E-05 ), #48823, 'distance_accuracy_value', 'NONE');
#16038 = CARTESIAN_POINT ( 'NONE',  ( 96.24916995763402383, -34.45682319295006124, 261.1737205140064475 ) ) ;
#16039 = CARTESIAN_POINT ( 'NONE',  ( 0.000000000000000000, 50.79999999999999716, 265.5569999999999595 ) ) ;
#16040 = PRESENTATION_STYLE_ASSIGNMENT (( #3299 ) ) ;
#16041 = CARTESIAN_POINT ( 'NONE',  ( 11.80314539778289529, 77.86161004085525406, 130.0213727849707368 ) ) ;
#16042 = CARTESIAN_POINT ( 'NONE',  ( 97.81193178031652735, -40.51732023384165160, 27.63604381180012837 ) ) ;
#16044 = DIRECTION ( 'NONE',  ( 0.000000000000000000, 0.000000000000000000, 1.000000000000000000 ) ) ;
#16043 = LINE ( 'NONE', #2408, #12918 ) ;
#16045 = CARTESIAN_POINT ( 'NONE',  ( 106.6155744189988326, -25.27918481551454732, 323.5352776872487652 ) ) ;
#16046 = FACE_OUTER_BOUND ( 'NONE', #42275, .T. ) ;
#16047 = CARTESIAN_POINT ( 'NONE',  ( 20.03715912545737510, -24.95799193693189721, 249.9678068554150059 ) ) ;
#16048 = AXIS2_PLACEMENT_3D ( 'NONE', #52262, #65486, #80028 ) ;
#16049 = FACE_OUTER_BOUND ( 'NONE', #54944, .T. ) ;
#16050 = CARTESIAN_POINT ( 'NONE',  ( 95.60734603896362671, -36.72944715994100306, 293.2242906452868851 ) ) ;
#16051 = DIRECTION ( 'NONE',  ( -0.9988791501868375944, -0.04215501712985142424, 0.02152667770007998804 ) ) ;
#16052 = DIRECTION ( 'NONE',  ( 0.000000000000000000, 0.000000000000000000, 1.000000000000000000 ) ) ;
#16053 = DIRECTION ( 'NONE',  ( 0.000000000000000000, 1.000000000000000000, 0.000000000000000000 ) ) ;
#16054 = CARTESIAN_POINT ( 'NONE',  ( 115.4801557161918311, -43.01927310766588874, 28.31562527591097123 ) ) ;
#16055 = CARTESIAN_POINT ( 'NONE',  ( 113.6142049395107421, -45.63457611473454989, 179.0689586092439640 ) ) ;
#16056 = CARTESIAN_POINT ( 'NONE',  ( 116.7902211891048694, -31.42528581690661582, 20.21181575210195902 ) ) ;
#16058 = CARTESIAN_POINT ( 'NONE',  ( 82.81648064515525220, -36.72944715939136273, 6.749772901088423538 ) ) ;
#16057 = DIRECTION ( 'NONE',  ( 4.299999999999999979E-14, -1.000000000000000000, 4.400000000000000367E-29 ) ) ;
#16059 = PLANE ( 'NONE',  #50876 ) ;
#16060 = EDGE_LOOP ( 'NONE', ( #25568, #20622, #17062, #21051 ) ) ;
#16061 = ADVANCED_FACE ( 'NONE', ( #79571 ), #65474, .F. ) ;
#16062 = CARTESIAN_POINT ( 'NONE',  ( 163.0667039024479550, -33.35206098992140511, 117.4678068554150485 ) ) ;
#16063 = VERTEX_POINT ( 'NONE', #80018 ) ;
#16064 = EDGE_CURVE ( 'NONE', #28268, #5970, #79121, .T. ) ;
#16065 = CIRCLE ( 'NONE', #45015, 2.117000000000007987 ) ;
#16066 = CARTESIAN_POINT ( 'NONE',  ( 113.0229309284916184, -28.24065945027253477, 80.57753003781498080 ) ) ;
#16068 = ORIENTED_EDGE ( 'NONE', *, *, #53027, .T. ) ;
#16067 = CARTESIAN_POINT ( 'NONE',  ( 7.008108505301582802, 93.14135335536794003, 130.3677710664748020 ) ) ;
#16069 = VECTOR ( 'NONE', #6112, 1000.000000000000000 ) ;
#16070 = CARTESIAN_POINT ( 'NONE',  ( -254.0000000000000000, 104.7749999999999915, 142.8750000000000000 ) ) ;
#16071 = EDGE_CURVE ( 'NONE', #48691, #73197, #44565, .T. ) ;
#16072 = CARTESIAN_POINT ( 'NONE',  ( 97.78191787992085438, -41.50032452247405246, 192.7041967044819728 ) ) ;
#16073 = DIRECTION ( 'NONE',  ( 0.000000000000000000, 0.000000000000000000, -1.000000000000000000 ) ) ;
#16074 = CARTESIAN_POINT ( 'NONE',  ( 97.81847858979224952, -40.53397798444700584, 146.6370489193171238 ) ) ;
#16075 = CARTESIAN_POINT ( 'NONE',  ( 105.8001069787651716, -26.72395502425483826, 150.1776541679874128 ) ) ;
#16076 = CARTESIAN_POINT ( 'NONE',  ( 188.5667039024479834, -65.37844715994100397, 173.2178068554149775 ) ) ;
#16077 = CARTESIAN_POINT ( 'NONE',  ( 0.000000000000000000, 1.270000000000000018, 0.000000000000000000 ) ) ;
#16078 = EDGE_CURVE ( 'NONE', #45292, #58396, #59866, .T. ) ;
#16079 = CARTESIAN_POINT ( 'NONE',  ( 105.7137601602295121, -46.72359881362813638, 97.46889204442247490 ) ) ;
#16080 = CARTESIAN_POINT ( 'NONE',  ( 113.7357275853186991, -44.67049210939298831, 148.1203871806729353 ) ) ;
#16081 = ORIENTED_EDGE ( 'NONE', *, *, #67460, .T. ) ;
#16082 = AXIS2_PLACEMENT_3D ( 'NONE', #38973, #26246, #39862 ) ;
#16083 = ORIENTED_EDGE ( 'NONE', *, *, #66274, .T. ) ;
#16084 = CARTESIAN_POINT ( 'NONE',  ( 115.1688055144990415, -30.74420868983300537, 105.7644404487539589 ) ) ;
#16085 = DIRECTION ( 'NONE',  ( 0.000000000000000000, 0.000000000000000000, -1.000000000000000000 ) ) ;
#16087 = CARTESIAN_POINT ( 'NONE',  ( 116.3167039024470029, -67.87844715994093292, 222.2178068554179902 ) ) ;
#16086 = CARTESIAN_POINT ( 'NONE',  ( 113.3831382903590566, -27.58002901871528323, 235.5956252759109759 ) ) ;
#16088 = CARTESIAN_POINT ( 'NONE',  ( 108.0667039024470171, -87.35579742913164125, -19.26696060647653397 ) ) ;
#16089 = CARTESIAN_POINT ( 'NONE',  ( 98.34985026692173449, -31.65659937734086071, 111.9069137705935901 ) ) ;
#16090 = B_SPLINE_CURVE_WITH_KNOTS ( 'NONE', 3,
 ( #72126, #9448, #36715, #58472, #3087, #37607, #65308, #30782, #2195, #38047, #24424, #52088, #79848, #45285, #73005, #1749, #84876, #43499 ),
 .UNSPECIFIED., .F., .F.,
 ( 4, 2, 2, 2, 2, 2, 2, 2, 4 ),
 ( 0.5000305911332758591, 0.5625267672416163212, 0.6250229433499568943, 0.6875191194582974674, 0.7500152955666379295, 0.8125114716749783916, 0.8750076477833189648, 0.9375038238916595379, 1.000000000000000000 ),
 .UNSPECIFIED. ) ;
#16091 = EDGE_CURVE ( 'NONE', #30574, #56233, #50946, .T. ) ;
#16092 = LINE ( 'NONE', #56044, #77921 ) ;
#16093 = DIRECTION ( 'NONE',  ( 1.000000000000000000, 0.000000000000000000, 0.000000000000000000 ) ) ;
#16094 = CARTESIAN_POINT ( 'NONE',  ( 82.54999999999999716, 95.25000000000000000, 346.9005000000000223 ) ) ;
#16095 = CARTESIAN_POINT ( 'NONE',  ( 98.10941331148539746, -42.08998169807674117, 161.7556252759109725 ) ) ;
#16096 = EDGE_LOOP ( 'NONE', ( #5525, #58037, #7164, #78025 ) ) ;
#16097 = VERTEX_POINT ( 'NONE', #44115 ) ;
#16098 = ORIENTED_EDGE ( 'NONE', *, *, #86305, .F. ) ;
#16099 = AXIS2_PLACEMENT_3D ( 'NONE', #18493, #3532, #17616 ) ;
#16100 = CARTESIAN_POINT ( 'NONE',  ( 62.03715912545739286, -47.82818131006020934, 180.4678068554151196 ) ) ;
#16101 = CARTESIAN_POINT ( 'NONE',  ( 47.62500000000000000, 66.67499999999999716, 260.3500000000000227 ) ) ;
#16102 = CARTESIAN_POINT ( 'NONE',  ( 112.1377149357240341, -28.01188520256706482, 129.6566085857481596 ) ) ;
#16103 = CARTESIAN_POINT ( 'NONE',  ( 97.81528920454944398, -40.52621084845757338, 102.6363811929704895 ) ) ;
#16104 = CARTESIAN_POINT ( 'NONE',  ( 100.6247221172615127, -30.94977259965520844, 233.5747570362579495 ) ) ;
#16105 = LINE ( 'NONE', #30615, #63991 ) ;
#16106 = CARTESIAN_POINT ( 'NONE',  ( 114.9780134700875180, -29.01019993736734293, 194.4537205140059370 ) ) ;
#16107 = DIRECTION ( 'NONE',  ( 0.7071067811865178188, 0.7071067811865773267, 7.071067811865170636E-16 ) ) ;
#16108 = EDGE_LOOP ( 'NONE', ( #23608, #37814, #18155, #18883 ) ) ;
#16110 = VERTEX_POINT ( 'NONE', #10508 ) ;
#16109 = ORIENTED_EDGE ( 'NONE', *, *, #64099, .F. ) ;
#16111 = VECTOR ( 'NONE', #82501, 999.9999999999998863 ) ;
#16112 = CARTESIAN_POINT ( 'NONE',  ( 25.56670390244797275, -62.87844715994099687, 298.0928068554150627 ) ) ;
#16113 = ORIENTED_EDGE ( 'NONE', *, *, #44683, .F. ) ;
#16114 = ORIENTED_EDGE ( 'NONE', *, *, #9605, .F. ) ;
#16115 = FACE_OUTER_BOUND ( 'NONE', #31716, .T. ) ;
#16116 = CARTESIAN_POINT ( 'NONE',  ( 50.97905606905900555, -31.62489322948711035, -5.074374724088000832 ) ) ;
#16117 = VECTOR ( 'NONE', #89775, 1000.000000000000000 ) ;
#16118 = CARTESIAN_POINT ( 'NONE',  ( 98.41530666024773666, -31.56922914487509502, 277.3301547344686355 ) ) ;
#16119 = CARTESIAN_POINT ( 'NONE',  ( 116.7951251982872662, -39.38783008756426085, 273.6147919184925854 ) ) ;
#16120 = ORIENTED_EDGE ( 'NONE', *, *, #74615, .F. ) ;
#16121 = EDGE_CURVE ( 'NONE', #60085, #4611, #57764, .T. ) ;
#16122 = CARTESIAN_POINT ( 'NONE',  ( 109.1587844380377277, -44.82492231645672121, 9.635625275910939536 ) ) ;
#16123 = CARTESIAN_POINT ( 'NONE',  ( 41.56648329127499153, -36.32844715994070839, 318.9256252759120116 ) ) ;
#16124 = ORIENTED_EDGE ( 'NONE', *, *, #24370, .T. ) ;
#16125 = VERTEX_POINT ( 'NONE', #29614 ) ;
#16126 = CARTESIAN_POINT ( 'NONE',  ( 117.0527731729269476, -35.95361413649180093, 113.8882183681226081 ) ) ;
#16127 = EDGE_LOOP ( 'NONE', ( #44050, #58211, #73365 ) ) ;
#16128 = ORIENTED_EDGE ( 'NONE', *, *, #10848, .T. ) ;
#16129 = ADVANCED_FACE ( 'NONE', ( #71854 ), #37777, .T. ) ;
#16130 = VECTOR ( 'NONE', #18782, 1000.000000000000000 ) ;
#16131 = CARTESIAN_POINT ( 'NONE',  ( 107.5092159716399181, -46.42865411040452273, 42.03527697093395687 ) ) ;
#16132 = CARTESIAN_POINT ( 'NONE',  ( 113.6284486023480724, -28.60005753680112761, 164.5356252759109736 ) ) ;
#16133 = VECTOR ( 'NONE', #6881, 1000.000000000000000 ) ;
#16134 = CARTESIAN_POINT ( 'NONE',  ( 116.8835868046513582, -40.17228670562625581, 133.5584824187679658 ) ) ;
#16135 =( NAMED_UNIT ( * ) PLANE_ANGLE_UNIT ( ) SI_UNIT ( $, .RADIAN. ) );
#16136 = CARTESIAN_POINT ( 'NONE',  ( 116.0551108448461264, -42.01026737563550029, 234.4041967044819899 ) ) ;
#16137 = FACE_OUTER_BOUND ( 'NONE', #16234, .T. ) ;
#16138 = CARTESIAN_POINT ( 'NONE',  ( 85.44094044773511598, -87.19737211520767062, 250.2190963482990185 ) ) ;
#16139 = VERTEX_POINT ( 'NONE', #58641 ) ;
#16140 = CARTESIAN_POINT ( 'NONE',  ( -130.2867309503044453, 73.00415124681445889, -8.386992461123011111 ) ) ;
#16141 = ORIENTED_EDGE ( 'NONE', *, *, #23023, .T. ) ;
#16142 = ORIENTED_EDGE ( 'NONE', *, *, #82831, .T. ) ;
#16143 = VECTOR ( 'NONE', #71893, 1000.000000000000000 ) ;
#16144 = CIRCLE ( 'NONE', #5967, 5.041900000000001825 ) ;
#16145 = EDGE_CURVE ( 'NONE', #84879, #26178, #22378, .T. ) ;
#16146 = CARTESIAN_POINT ( 'NONE',  ( 101.4014481618761181, -46.27514046166531614, 207.1622919425779514 ) ) ;
#16147 = ORIENTED_EDGE ( 'NONE', *, *, #69483, .T. ) ;
#16148 = CARTESIAN_POINT ( 'NONE',  ( 101.7694246217487972, -45.70876760617753831, 162.1527681330539679 ) ) ;
#16149 = CARTESIAN_POINT ( 'NONE',  ( 99.09686023256277565, -30.54889700294794963, 255.8022268357593703 ) ) ;
#16150 = CARTESIAN_POINT ( 'NONE',  ( 147.0665874381622018, -67.87844715994090450, 245.5130140176639770 ) ) ;
#16151 = CARTESIAN_POINT ( 'NONE',  ( 41.56648329127399677, 0.2215528400590013880, 198.9256252759119832 ) ) ;
#16154 = CARTESIAN_POINT ( 'NONE',  ( 116.1995025514323316, -41.78438384397597360, 259.4241967044825969 ) ) ;
#16153 = CARTESIAN_POINT ( 'NONE',  ( 104.9367214363761889, -46.52192551884516547, 57.40585424230521028 ) ) ;
#16152 = CARTESIAN_POINT ( 'NONE',  ( 226.4410000000000025, 40.03750000000000142, -2.032000000000000028 ) ) ;
#16155 = DIRECTION ( 'NONE',  ( -0.000000000000000000, -0.000000000000000000, 1.000000000000000000 ) ) ;
#16156 = CARTESIAN_POINT ( 'NONE',  ( 0.000000000000000000, 215.0000000000000000, 154.6557476874258441 ) ) ;
#16157 = CARTESIAN_POINT ( 'NONE',  ( 104.4871749466126545, -26.97957198089209641, 271.2812583532387407 ) ) ;
#16158 = CARTESIAN_POINT ( 'NONE',  ( 0.000000000000000000, 172.0000000000000000, 0.000000000000000000 ) ) ;
#16159 = CARTESIAN_POINT ( 'NONE',  ( 117.0718954847100122, -35.46248235314624253, 259.9272919428255477 ) ) ;
#16160 = CARTESIAN_POINT ( 'NONE',  ( 146.3069282193933986, -137.2669017349363685, 247.0814054964307616 ) ) ;
#16161 = AXIS2_PLACEMENT_3D ( 'NONE', #66555, #81564, #32926 ) ;
#16163 = VERTEX_POINT ( 'NONE', #38213 ) ;
#16162 = CARTESIAN_POINT ( 'NONE',  ( 99.49891107524048550, -31.87110612240238439, 195.5838068554173219 ) ) ;
#16164 = DIRECTION ( 'NONE',  ( 0.000000000000000000, -1.000000000000000000, 0.000000000000000000 ) ) ;
#16165 = CARTESIAN_POINT ( 'NONE',  ( 117.9717084303226500, -34.78741065070708061, 198.9546728949589749 ) ) ;
#16166 = CARTESIAN_POINT ( 'NONE',  ( 98.72253030179433608, -42.97932203522270100, 62.83848241876793850 ) ) ;
#16167 = CARTESIAN_POINT ( 'NONE',  ( 114.8463700017591407, -29.67172957150665979, 205.4127681330539872 ) ) ;
#16168 = CARTESIAN_POINT ( 'NONE',  ( 21.03715912545744615, -47.82818131006197149, 129.9678068554150627 ) ) ;
#16169 = DIRECTION ( 'NONE',  ( -1.000000000000000000, -4.299999999999999979E-14, -1.000000000000000078E-15 ) ) ;
#16171 = CARTESIAN_POINT ( 'NONE',  ( 41.56648329127398966, -27.82844715994070484, 258.9256252759120116 ) ) ;
#16170 = DIRECTION ( 'NONE',  ( 9.172741847159597097E-17, 0.1045284632676476005, -0.9945218953682739560 ) ) ;
#16172 = DIRECTION ( 'NONE',  ( 1.000000000000000000, 4.012088370409549976E-14, 0.000000000000000000 ) ) ;
#16173 = LINE ( 'NONE', #71143, #49622 ) ;
#16174 = ORIENTED_EDGE ( 'NONE', *, *, #38639, .T. ) ;
#16175 = CARTESIAN_POINT ( 'NONE',  ( 34.92499999999999716, 66.67499999999999716, 346.0750000000000455 ) ) ;
#16176 = EDGE_LOOP ( 'NONE', ( #88158, #64869, #57427, #48957 ) ) ;
#16177 = ORIENTED_EDGE ( 'NONE', *, *, #76388, .F. ) ;
#16178 = EDGE_CURVE ( 'NONE', #58180, #15623, #24588, .T. ) ;
#16179 = AXIS2_PLACEMENT_3D ( 'NONE', #697, #21154, #36121 ) ;
#16180 = CARTESIAN_POINT ( 'NONE',  ( 115.3767887321059789, -38.82490071601502990, 123.0524198280769639 ) ) ;
#16182 = ORIENTED_EDGE ( 'NONE', *, *, #14940, .T. ) ;
#16181 = DIRECTION ( 'NONE',  ( 0.000000000000000000, 0.000000000000000000, -1.000000000000000000 ) ) ;
#16183 = ADVANCED_FACE ( 'NONE', ( #8742 ), #15999, .F. ) ;
#16184 = CARTESIAN_POINT ( 'NONE',  ( 96.04673288144557830, -37.20790665022158805, 112.3489586092449599 ) ) ;
#16185 = FACE_OUTER_BOUND ( 'NONE', #81981, .T. ) ;
#16186 = EDGE_CURVE ( 'NONE', #25689, #28894, #30069, .T. ) ;
#16187 = VECTOR ( 'NONE', #22085, 999.9999999999998863 ) ;
#16188 = DIRECTION ( 'NONE',  ( 0.000000000000000000, 0.000000000000000000, -1.000000000000000000 ) ) ;
#16189 = CARTESIAN_POINT ( 'NONE',  ( 115.8254323925114875, -31.73001883020303637, 175.2397919424540760 ) ) ;
#16190 = EDGE_CURVE ( 'NONE', #50856, #27885, #88617, .T. ) ;
#16191 = CARTESIAN_POINT ( 'NONE',  ( 99.61812512063040970, -43.94476044465314857, 41.95086337115000674 ) ) ;
#16192 = ORIENTED_EDGE ( 'NONE', *, *, #71259, .T. ) ;
#16193 = ORIENTED_EDGE ( 'NONE', *, *, #44119, .T. ) ;
#16194 = VERTEX_POINT ( 'NONE', #33189 ) ;
#16195 = CARTESIAN_POINT ( 'NONE',  ( 41.56648329127398966, -27.82844715994070484, 134.1756252759119832 ) ) ;
#16196 = CARTESIAN_POINT ( 'NONE',  ( 173.9900000000000091, 20.32000000000000028, 131.6533725204182019 ) ) ;
#16197 = CARTESIAN_POINT ( 'NONE',  ( 116.3191307872214821, -32.94748812527954840, 115.1356252759109822 ) ) ;
#16198 = DIRECTION ( 'NONE',  ( -0.000000000000000000, 1.000000000000000000, -0.000000000000000000 ) ) ;
#16199 = CARTESIAN_POINT ( 'NONE',  ( 84.37439091330263352, 89.26666702275852572, 99.62873342662707898 ) ) ;
#16200 = CARTESIAN_POINT ( 'NONE',  ( 223.2659999999999911, 52.73749999999999716, -55.11800000000000210 ) ) ;
#16201 = EDGE_CURVE ( 'NONE', #69025, #20236, #60888, .T. ) ;
#16202 = DIRECTION ( 'NONE',  ( 0.000000000000000000, 0.000000000000000000, -1.000000000000000000 ) ) ;
#16203 = AXIS2_PLACEMENT_3D ( 'NONE', #86319, #71360, #24096 ) ;
#16204 = CARTESIAN_POINT ( 'NONE',  ( -7.061405134937971617, 93.10587809510549562, 130.3648943659824795 ) ) ;
#16205 = CARTESIAN_POINT ( 'NONE',  ( 98.60777729073571152, -43.80857954853296121, 71.86895860924397539 ) ) ;
#16206 = EDGE_LOOP ( 'NONE', ( #71656, #89570, #47362, #27556 ) ) ;
#16207 = LINE ( 'NONE', #57067, #19994 ) ;
#16208 = AXIS2_PLACEMENT_3D ( 'NONE', #68205, #41366, #75911 ) ;
#16209 = CARTESIAN_POINT ( 'NONE',  ( 82.02983075842483629, -115.7792181415380668, 250.2178068554180470 ) ) ;
#16210 = CARTESIAN_POINT ( 'NONE',  ( 103.4072989863811074, -28.88653346237834185, 133.2299951314959685 ) ) ;
#16211 = VECTOR ( 'NONE', #18901, 1000.000000000000000 ) ;
#16212 = CARTESIAN_POINT ( 'NONE',  ( 9.331435647859348646E-23, 95.25000000000000000, 130.5560000000000116 ) ) ;
#16213 = CARTESIAN_POINT ( 'NONE',  ( 73.06648329127402519, -46.72944715994106701, -4.824374724089063982 ) ) ;
#16214 = ORIENTED_EDGE ( 'NONE', *, *, #15764, .T. ) ;
#16215 = ORIENTED_EDGE ( 'NONE', *, *, #87928, .T. ) ;
#16216 = DIRECTION ( 'NONE',  ( 0.000000000000000000, 0.000000000000000000, -1.000000000000000000 ) ) ;
#16217 = ORIENTED_EDGE ( 'NONE', *, *, #18842, .F. ) ;
#16218 = EDGE_LOOP ( 'NONE', ( #52284, #21553, #20591, #73108 ) ) ;
#16219 = AXIS2_PLACEMENT_3D ( 'NONE', #34035, #73716, #56550 ) ;
#16220 = CARTESIAN_POINT ( 'NONE',  ( 112.7482059764288778, -43.52991081625548020, 189.5615833058969883 ) ) ;
#16221 = DIRECTION ( 'NONE',  ( 0.000000000000000000, 0.000000000000000000, 1.000000000000000000 ) ) ;
#16223 = EDGE_CURVE ( 'NONE', #34951, #89277, #87267, .T. ) ;
#16222 = CARTESIAN_POINT ( 'NONE',  ( 101.4892552882362793, -27.89588691190665060, 106.5241967044819944 ) ) ;
#16224 = CARTESIAN_POINT ( 'NONE',  ( 116.3183510266638336, -32.94967450325654568, 119.1356252759109537 ) ) ;
#16225 = CIRCLE ( 'NONE', #78622, 7.873999999999991672 ) ;
#16226 = CARTESIAN_POINT ( 'NONE',  ( 115.0850347510768330, -42.76005057245251351, 18.31318323247893076 ) ) ;
#16227 = ORIENTED_EDGE ( 'NONE', *, *, #17770, .T. ) ;
#16228 = ORIENTED_EDGE ( 'NONE', *, *, #61121, .F. ) ;
#16229 = VERTEX_POINT ( 'NONE', #12301 ) ;
#16230 = EDGE_CURVE ( 'NONE', #22054, #28950, #67144, .T. ) ;
#16231 = AXIS2_PLACEMENT_3D ( 'NONE', #25397, #67177, #80833 ) ;
#16232 = CARTESIAN_POINT ( 'NONE',  ( 102.0328030160422230, -28.93470572416599751, 218.3509475124479593 ) ) ;
#16233 = CARTESIAN_POINT ( 'NONE',  ( 96.31560519187928548, -41.77450771427546528, 61.67562527591097421 ) ) ;
#16234 = EDGE_LOOP ( 'NONE', ( #3955, #12132, #26248, #16328, #81672, #67220, #80584, #59459, #19538, #12196, #19407, #50809 ) ) ;
#16235 = CARTESIAN_POINT ( 'NONE',  ( 106.5192459994187715, -25.71289806663794408, 45.12800622829193742 ) ) ;
#16236 = CARTESIAN_POINT ( 'NONE',  ( 106.4823958901525458, -24.86854109859944373, 191.1156252759109861 ) ) ;
#16237 = CARTESIAN_POINT ( 'NONE',  ( 83.06670390244796920, -61.87844715994100397, 207.5838068554149913 ) ) ;
#16238 = DIRECTION ( 'NONE',  ( 0.000000000000000000, 1.000000000000000000, 0.000000000000000000 ) ) ;
#16239 = CARTESIAN_POINT ( 'NONE',  ( 102.3604841619309411, -46.03192315517718214, 123.2041967044829818 ) ) ;
#16240 = CIRCLE ( 'NONE', #33669, 11.45913725231036118 ) ;
#16241 = CARTESIAN_POINT ( 'NONE',  ( 182.5667039024480118, -32.29483332968450782, -5.074374724088000832 ) ) ;
#16242 = VERTEX_POINT ( 'NONE', #45446 ) ;
#16243 = DIRECTION ( 'NONE',  ( -0.000000000000000000, -1.000000000000000000, -0.000000000000000000 ) ) ;
#16244 = ORIENTED_EDGE ( 'NONE', *, *, #86288, .T. ) ;
#16245 = CARTESIAN_POINT ( 'NONE',  ( 115.0378464896363795, -42.90772034720064454, 134.3033616519834368 ) ) ;
#16246 = VERTEX_POINT ( 'NONE', #5035 ) ;
#16247 = EDGE_LOOP ( 'NONE', ( #39045, #54599 ) ) ;
#16248 = LINE ( 'NONE', #76678, #22878 ) ;
#16249 = ADVANCED_FACE ( 'NONE', ( #52694 ), #26373, .F. ) ;
#16250 = CARTESIAN_POINT ( 'NONE',  ( -160.2664750769294812, 20.32000000000000028, -148.0533267522755807 ) ) ;
#16251 = CARTESIAN_POINT ( 'NONE',  ( 107.2322097935746541, -25.67722466037449536, 80.07657765686299456 ) ) ;
#16252 = DIRECTION ( 'NONE',  ( 0.000000000000000000, 0.000000000000000000, -1.000000000000000000 ) ) ;
#16253 = DIRECTION ( 'NONE',  ( -0.9068632946707806397, 0.4214249218767882055, -9.068632946707802473E-16 ) ) ;
#16254 = CARTESIAN_POINT ( 'NONE',  ( 106.6155744189988326, -25.27918481551454732, 323.5352776872487652 ) ) ;
#16255 = CARTESIAN_POINT ( 'NONE',  ( 95.98894198207682393, -35.78073158428679790, 36.25848241876794731 ) ) ;
#16257 = CARTESIAN_POINT ( 'NONE',  ( 113.8292797163801851, -28.77778007523028947, 135.5156252759109634 ) ) ;
#16256 = CARTESIAN_POINT ( 'NONE',  ( 115.8254209475894072, -31.72999086795746848, 109.2397943467912995 ) ) ;
#16258 = DIRECTION ( 'NONE',  ( -7.723290606088049820E-15, 0.000000000000000000, 1.000000000000000000 ) ) ;
#16259 = DIRECTION ( 'NONE',  ( 0.000000000000000000, 0.000000000000000000, 1.000000000000000000 ) ) ;
#16260 = VERTEX_POINT ( 'NONE', #12757 ) ;
#16261 = DIRECTION ( 'NONE',  ( 1.387778780781444492E-15, 0.000000000000000000, -1.000000000000000000 ) ) ;
#16262 = DIRECTION ( 'NONE',  ( 0.000000000000000000, 0.000000000000000000, 1.000000000000000000 ) ) ;
#16263 = EDGE_LOOP ( 'NONE', ( #11068, #18857 ) ) ;
#16264 = ADVANCED_FACE ( 'NONE', ( #39548 ), #54492, .T. ) ;
#16265 = CARTESIAN_POINT ( 'NONE',  ( 100.8961411191535973, 120.6499999999999915, 3.968750000000400124 ) ) ;
#16267 = ORIENTED_EDGE ( 'NONE', *, *, #37185, .T. ) ;
#16266 = CARTESIAN_POINT ( 'NONE',  ( 103.8060002238608774, -48.17488501466909412, 217.3556252759109668 ) ) ;
#16268 = CARTESIAN_POINT ( 'NONE',  ( -3.174999999999664979, 124.5870000000000033, -31.75000000000000000 ) ) ;
#16269 = CARTESIAN_POINT ( 'NONE',  ( 112.5006845157638651, -46.38111348219169372, 253.9965776568635647 ) ) ;
#16270 = CARTESIAN_POINT ( 'NONE',  ( 111.0993040117788979, -25.53357873718133320, 95.80133956162495679 ) ) ;
#16271 = DIRECTION ( 'NONE',  ( 1.000000000000000000, 0.000000000000000000, -1.047445008332813989E-14 ) ) ;
#16272 = VECTOR ( 'NONE', #75363, 1000.000000000000000 ) ;
#16273 = DIRECTION ( 'NONE',  ( 1.000000000000000078E-15, 0.000000000000000000, -1.000000000000000000 ) ) ;
#16274 = CARTESIAN_POINT ( 'NONE',  ( 116.7951252721859987, -39.38782978701362936, 78.61479194282316030 ) ) ;
#16275 = ORIENTED_EDGE ( 'NONE', *, *, #76357, .F. ) ;
#16276 = VERTEX_POINT ( 'NONE', #80453 ) ;
#16277 = ORIENTED_EDGE ( 'NONE', *, *, #29983, .T. ) ;
#16278 = ORIENTED_EDGE ( 'NONE', *, *, #11144, .F. ) ;
#16279 = DIRECTION ( 'NONE',  ( -1.000000000000000078E-15, 1.000000000000000083E-30, 1.000000000000000000 ) ) ;
#16280 = CARTESIAN_POINT ( 'NONE',  ( 114.4150145978633049, -27.43247436093422920, 270.5441967044823741 ) ) ;
#16281 = CARTESIAN_POINT ( 'NONE',  ( 107.0664832912739968, -36.72944715994100306, 312.6356252759112522 ) ) ;
#16282 = CARTESIAN_POINT ( 'NONE',  ( 131.5094688080979495, -35.71735499139286674, 2.839545688279668578 ) ) ;
#16283 = EDGE_CURVE ( 'NONE', #73924, #6162, #6222, .T. ) ;
#16284 = AXIS2_PLACEMENT_3D ( 'NONE', #83016, #56624, #84368 ) ;
#16286 = CARTESIAN_POINT ( 'NONE',  ( 71.47170404114027065, -139.6113389983086961, 247.4111996305669834 ) ) ;
#16285 = CARTESIAN_POINT ( 'NONE',  ( 51.06648329127400388, 12.92155284005902516, 330.1506252759110680 ) ) ;
#16287 = DIRECTION ( 'NONE',  ( 1.346944695195362088E-15, -1.000000000000000000, 3.469446951953620425E-31 ) ) ;
#16288 = CARTESIAN_POINT ( 'NONE',  ( 108.9266419529017327, -28.39302457734394736, 224.3238483995049819 ) ) ;
#16289 = EDGE_LOOP ( 'NONE', ( #47531, #68337, #26250, #18840 ) ) ;
#16290 = AXIS2_PLACEMENT_3D ( 'NONE', #38938, #3981, #18954 ) ;
#16291 = ORIENTED_EDGE ( 'NONE', *, *, #29682, .F. ) ;
#16292 = EDGE_LOOP ( 'NONE', ( #37617, #27209, #62572, #45790 ) ) ;
#16293 = AXIS2_PLACEMENT_3D ( 'NONE', #69858, #7186, #89867 ) ;
#16294 = CARTESIAN_POINT ( 'NONE',  ( 118.5667039024470313, -104.2784471599411376, 0.2178068554180012661 ) ) ;
#16295 = CARTESIAN_POINT ( 'NONE',  ( 97.83899935994767816, -40.58357122989591659, 181.6413209514236371 ) ) ;
#16296 = CARTESIAN_POINT ( 'NONE',  ( 105.7207279102414077, -46.41719084699259668, 253.4670538473389740 ) ) ;
#16297 = VECTOR ( 'NONE', #25287, 1000.000000000000114 ) ;
#16298 = LINE ( 'NONE', #43976, #35697 ) ;
#16299 = EDGE_CURVE ( 'NONE', #58534, #74550, #59529, .T. ) ;
#16300 = CARTESIAN_POINT ( 'NONE',  ( 108.9483104351207174, -46.92736419409149562, 123.7337205140059666 ) ) ;
#16301 = EDGE_CURVE ( 'NONE', #4381, #63654, #58397, .T. ) ;
#16302 = AXIS2_PLACEMENT_3D ( 'NONE', #5995, #11904, #54542 ) ;
#16303 = CARTESIAN_POINT ( 'NONE',  ( 116.8175521666927779, -34.15458112805423951, 29.03132320540886724 ) ) ;
#16304 = VERTEX_POINT ( 'NONE', #68163 ) ;
#16305 = DIRECTION ( 'NONE',  ( 0.000000000000000000, 6.982966722218760189E-15, -1.000000000000000000 ) ) ;
#16306 = CARTESIAN_POINT ( 'NONE',  ( 71.24189083761808661, -0.9290567490904538817, 542.9756252759101471 ) ) ;
#16307 = ORIENTED_EDGE ( 'NONE', *, *, #81098, .T. ) ;
#16308 = CARTESIAN_POINT ( 'NONE',  ( 177.1649999999999920, 25.81350000000000477, -58.73749999999999716 ) ) ;
#16309 = CARTESIAN_POINT ( 'NONE',  ( 98.13886466857337609, -39.66030079267085995, 283.0225356868493805 ) ) ;
#16310 = CARTESIAN_POINT ( 'NONE',  ( 25.56670390244832802, -48.82844715994168183, 254.7178068554150059 ) ) ;
#16311 = FACE_OUTER_BOUND ( 'NONE', #24153, .T. ) ;
#16312 = CYLINDRICAL_SURFACE ( 'NONE', #70639, 9.999999999999998224 ) ;
#16313 = ORIENTED_EDGE ( 'NONE', *, *, #22132, .T. ) ;
#16314 = DIRECTION ( 'NONE',  ( 0.000000000000000000, 1.000000000000000000, 0.000000000000000000 ) ) ;
#16315 = PLANE ( 'NONE',  #45503 ) ;
#16316 = VECTOR ( 'NONE', #43965, 1000.000000000000000 ) ;
#16317 = ORIENTED_EDGE ( 'NONE', *, *, #66487, .T. ) ;
#16318 = CARTESIAN_POINT ( 'NONE',  ( 96.65640405957751113, -37.29272404675901242, 76.36991099019697060 ) ) ;
#16319 = ORIENTED_EDGE ( 'NONE', *, *, #9309, .F. ) ;
#16320 = CARTESIAN_POINT ( 'NONE',  ( 113.4185696802295809, -42.43971249784851096, 37.66670554236295487 ) ) ;
#16321 = CARTESIAN_POINT ( 'NONE',  ( 116.9299238147201692, -38.64270279391814711, 89.67301604876226406 ) ) ;
#16322 = CARTESIAN_POINT ( 'NONE',  ( 115.4889021248300196, -33.97424487988631370, 85.51015473446898341 ) ) ;
#16323 = CARTESIAN_POINT ( 'NONE',  ( 4.665904304751416087E-15, 65.60000000000000853, -38.10000000000000142 ) ) ;
#16324 = DIRECTION ( 'NONE',  ( 0.000000000000000000, 0.000000000000000000, 1.000000000000000000 ) ) ;
#16325 = DIRECTION ( 'NONE',  ( 3.100000000000000258E-29, -3.100000000000000044E-14, -1.000000000000000000 ) ) ;
#16326 = CARTESIAN_POINT ( 'NONE',  ( 95.18190931754610062, -37.33608887137841492, 267.3670538473396618 ) ) ;
#16327 = DIRECTION ( 'NONE',  ( 0.000000000000000000, 0.000000000000000000, 1.000000000000000000 ) ) ;
#16328 = ORIENTED_EDGE ( 'NONE', *, *, #20803, .T. ) ;
#16329 = VECTOR ( 'NONE', #12974, 1000.000000000000000 ) ;
#16330 = DIRECTION ( 'NONE',  ( -0.000000000000000000, 1.000000000000000000, 0.000000000000000000 ) ) ;
#16331 = ORIENTED_EDGE ( 'NONE', *, *, #87439, .T. ) ;
#16332 = CARTESIAN_POINT ( 'NONE',  ( 98.82232569344716921, -30.27743405825323464, 151.7984824187679465 ) ) ;
#16333 = CARTESIAN_POINT ( 'NONE',  ( 172.5664832912740110, -32.07844715994070839, 318.9256252759120116 ) ) ;
#16334 = EDGE_LOOP ( 'NONE', ( #27733, #63292, #3365, #1032, #78598, #40445, #653, #39430 ) ) ;
#16335 = VERTEX_POINT ( 'NONE', #31837 ) ;
#16336 = EDGE_CURVE ( 'NONE', #40569, #9390, #56037, .T. ) ;
#16337 = ORIENTED_EDGE ( 'NONE', *, *, #88097, .F. ) ;
#16338 = CARTESIAN_POINT ( 'NONE',  ( 107.0664832912739968, -36.72944715994100306, 287.6356252759109680 ) ) ;
#16339 = CARTESIAN_POINT ( 'NONE',  ( -179.8898777604655095, 0.000000000000000000, 114.2999999999999972 ) ) ;
#16340 = CARTESIAN_POINT ( 'NONE',  ( 96.80143343076635176, -35.25719154489700458, 226.2251490854349640 ) ) ;
#16341 = DIRECTION ( 'NONE',  ( 0.000000000000000000, 2.135044278125299371E-15, -1.000000000000000000 ) ) ;
#16342 = CARTESIAN_POINT ( 'NONE',  ( 143.5625297611475730, -139.4754646311774877, 247.4327973477450087 ) ) ;
#16343 = DIRECTION ( 'NONE',  ( 0.000000000000000000, 0.000000000000000000, 1.000000000000000000 ) ) ;
#16344 = CARTESIAN_POINT ( 'NONE',  ( 115.4446095375818970, -42.99269977972175383, 24.31562527591096767 ) ) ;
#16345 = VECTOR ( 'NONE', #50143, 1000.000000000000000 ) ;
#16346 = CARTESIAN_POINT ( 'NONE',  ( 121.2542802781108406, -113.5872461203042292, -19.23816774841974464 ) ) ;
#16347 = ORIENTED_EDGE ( 'NONE', *, *, #4171, .F. ) ;
#16348 = CARTESIAN_POINT ( 'NONE',  ( 106.5738132885318379, -26.72017395369831405, 171.1156838945207710 ) ) ;
#16349 = DIRECTION ( 'NONE',  ( 0.000000000000000000, 0.000000000000000000, 1.000000000000000000 ) ) ;
#16350 = ORIENTED_EDGE ( 'NONE', *, *, #46365, .F. ) ;
#16351 = CIRCLE ( 'NONE', #39546, 0.5000000000000079936 ) ;
#16352 = CARTESIAN_POINT ( 'NONE',  ( 82.64938057483486489, -19.67376371870454932, 2.871651383883025321 ) ) ;
#16353 = EDGE_CURVE ( 'NONE', #27831, #18963, #64247, .T. ) ;
#16354 = PLANE ( 'NONE',  #17956 ) ;
#16355 = CARTESIAN_POINT ( 'NONE',  ( 97.63514171170966449, -41.12017164899860688, 256.6727681330537507 ) ) ;
#16356 = CARTESIAN_POINT ( 'NONE',  ( 48.16670390244647137, -26.71338133339281029, 193.9678068554150911 ) ) ;
#16357 = EDGE_CURVE ( 'NONE', #63459, #27672, #12045, .T. ) ;
#16358 = DIRECTION ( 'NONE',  ( -0.000000000000000000, 1.000000000000000000, 0.000000000000000000 ) ) ;
#16359 = CARTESIAN_POINT ( 'NONE',  ( 83.06670390244806867, -51.22944715994108122, 207.5838068554169809 ) ) ;
#16360 = CARTESIAN_POINT ( 'NONE',  ( 109.4373255760682611, -46.14484595950412427, 242.1952769709339464 ) ) ;
#16363 = CARTESIAN_POINT ( 'NONE',  ( 115.0059970501926330, -43.50650750775896825, 59.26419670448196086 ) ) ;
#16362 = DIRECTION ( 'NONE',  ( 1.000000000000000000, 1.000000000000000078E-15, 1.000000000000000078E-15 ) ) ;
#16361 = VECTOR ( 'NONE', #79725, 1000.000000000000000 ) ;
#16364 = CARTESIAN_POINT ( 'NONE',  ( 127.0154160123110927, 55.38930970734350723, 30.19865483100764791 ) ) ;
#16365 = CARTESIAN_POINT ( 'NONE',  ( 116.5734795788845020, -32.34496456428597355, 104.1699109901969535 ) ) ;
#16366 = ORIENTED_EDGE ( 'NONE', *, *, #45145, .F. ) ;
#16367 = DIRECTION ( 'NONE',  ( 1.000000000000000000, 0.000000000000000000, 0.000000000000000000 ) ) ;
#16368 = ORIENTED_EDGE ( 'NONE', *, *, #47014, .F. ) ;
#16369 = ADVANCED_FACE ( 'NONE', ( #80915 ), #86043, .F. ) ;
#16370 = DIRECTION ( 'NONE',  ( -0.9254794337955620787, -0.3787978585227822492, 0.000000000000000000 ) ) ;
#16371 = LINE ( 'NONE', #30887, #52735 ) ;
#16372 = VERTEX_POINT ( 'NONE', #25931 ) ;
#16373 = EDGE_CURVE ( 'NONE', #30447, #6360, #89051, .T. ) ;
#16374 = EDGE_CURVE ( 'NONE', #84699, #64009, #19241, .T. ) ;
#16375 = DIRECTION ( 'NONE',  ( 1.000000000000000078E-15, -1.000000000000000000, 0.000000000000000000 ) ) ;
#16376 = ORIENTED_EDGE ( 'NONE', *, *, #11373, .F. ) ;
#16377 = DIRECTION ( 'NONE',  ( 1.000000000000000000, 0.000000000000000000, 0.000000000000000000 ) ) ;
#16378 = CYLINDRICAL_SURFACE ( 'NONE', #37506, 20.63750000000000284 ) ;
#16379 = ADVANCED_FACE ( 'NONE', ( #74071 ), #53600, .T. ) ;
#16380 = CYLINDRICAL_SURFACE ( 'NONE', #74223, 10.00000000000000711 ) ;
#16381 = EDGE_CURVE ( 'NONE', #39961, #33407, #70402, .T. ) ;
#16382 = EDGE_LOOP ( 'NONE', ( #40606, #30699 ) ) ;
#16383 = CARTESIAN_POINT ( 'NONE',  ( 118.8678016624199358, -35.40170448615204890, 83.91562527591095488 ) ) ;
#16384 = DIRECTION ( 'NONE',  ( 1.000000000000000000, 0.000000000000000000, 0.000000000000000000 ) ) ;
#16385 = EDGE_CURVE ( 'NONE', #11556, #24002, #63130, .T. ) ;
#16386 = CARTESIAN_POINT ( 'NONE',  ( 84.32545390244804651, -42.97311385574013087, 207.5838068554169809 ) ) ;
#16387 = CARTESIAN_POINT ( 'NONE',  ( -141.3509999999999991, 0.000000000000000000, 141.3509999999999991 ) ) ;
#16388 = DIRECTION ( 'NONE',  ( 0.000000000000000000, 1.000000000000000000, 0.000000000000000000 ) ) ;
#16389 = VERTEX_POINT ( 'NONE', #77222 ) ;
#16390 = AXIS2_PLACEMENT_3D ( 'NONE', #2883, #78757, #85570 ) ;
#16391 = EDGE_CURVE ( 'NONE', #48080, #51651, #22175, .T. ) ;
#16392 = CARTESIAN_POINT ( 'NONE',  ( 100.4448767513723624, 86.64186789594792515, -83.40142812120552662 ) ) ;
#16393 = DIRECTION ( 'NONE',  ( 1.000000000000000000, 0.000000000000000000, 0.000000000000000000 ) ) ;
#16394 = EDGE_CURVE ( 'NONE', #30630, #20434, #49703, .T. ) ;
#16395 = CARTESIAN_POINT ( 'NONE',  ( 32.24491389930098251, -32.11662333284611748, -5.074374724088000832 ) ) ;
#16397 = DIRECTION ( 'NONE',  ( -0.9254794337955620787, -0.3787978585227822492, 0.000000000000000000 ) ) ;
#16396 = LINE ( 'NONE', #22771, #14604 ) ;
#16398 = CARTESIAN_POINT ( 'NONE',  ( 179.1667039024460166, -26.71338133339251542, -5.074374724088000832 ) ) ;
#16399 = ORIENTED_EDGE ( 'NONE', *, *, #18606, .F. ) ;
#16400 = FACE_OUTER_BOUND ( 'NONE', #10058, .T. ) ;
#16401 = CARTESIAN_POINT ( 'NONE',  ( 114.5468542906242391, -29.54732804739400365, 185.4232443235299570 ) ) ;
#16403 = EDGE_LOOP ( 'NONE', ( #54477, #13493, #21274, #67542 ) ) ;
#16402 = CARTESIAN_POINT ( 'NONE',  ( 95.60734603896362671, -36.72944715994100306, 292.6356252759106837 ) ) ;
#16404 = EDGE_CURVE ( 'NONE', #35731, #75012, #55840, .T. ) ;
#16405 = CARTESIAN_POINT ( 'NONE',  ( 97.69287098190334007, -33.93680905855630670, 27.09562527591097236 ) ) ;
#16406 = LINE ( 'NONE', #65441, #48308 ) ;
#16407 = CARTESIAN_POINT ( 'NONE',  ( 20.03715912545735378, -24.42818131006189830, 249.9678068554150059 ) ) ;
#16408 = DIRECTION ( 'NONE',  ( 1.000000000000000000, 3.987088437185090195E-11, 0.000000000000000000 ) ) ;
#16409 = EDGE_CURVE ( 'NONE', #21876, #45628, #6822, .T. ) ;
#16410 = CARTESIAN_POINT ( 'NONE',  ( 115.8262887155365632, -31.73150010602303439, 29.23988951266790082 ) ) ;
#16411 = EDGE_CURVE ( 'NONE', #45509, #40177, #42664, .T. ) ;
#16412 = CARTESIAN_POINT ( 'NONE',  ( 107.2379402074490429, -25.61267671046441308, 230.0641967044829812 ) ) ;
#16413 = ORIENTED_EDGE ( 'NONE', *, *, #51953, .F. ) ;
#16414 = ORIENTED_EDGE ( 'NONE', *, *, #40552, .F. ) ;
#16415 = CARTESIAN_POINT ( 'NONE',  ( 104.0709181822855243, -28.35754658334662182, 186.7815833058969872 ) ) ;
#16416 = CIRCLE ( 'NONE', #52606, 11.49999999999999645 ) ;
#16417 = CARTESIAN_POINT ( 'NONE',  ( 140.0667039024470171, -90.27844715994091018, 45.21780685541799727 ) ) ;
#16418 = CARTESIAN_POINT ( 'NONE',  ( 105.6677623720644306, -45.47998190943052066, 33.88158330589596545 ) ) ;
#16419 = CARTESIAN_POINT ( 'NONE',  ( 23.74735168769544913, 83.17465673267136594, 307.6189677106137310 ) ) ;
#16420 = CIRCLE ( 'NONE', #81721, 1.000000000000000888 ) ;
#16421 = AXIS2_PLACEMENT_3D ( 'NONE', #39149, #87311, #32323 ) ;
#16422 = CARTESIAN_POINT ( 'NONE',  ( 116.3212776292269552, -32.94146857470667555, 79.13562527591095375 ) ) ;
#16423 = CARTESIAN_POINT ( 'NONE',  ( 131.0667039024480118, -58.35344715994099829, 207.5838068554149913 ) ) ;
#16424 = ORIENTED_EDGE ( 'NONE', *, *, #20016, .T. ) ;
#16425 = CARTESIAN_POINT ( 'NONE',  ( 120.2221484686747317, -96.68314769832136335, -21.78219314458224076 ) ) ;
#16426 = CARTESIAN_POINT ( 'NONE',  ( 131.0667039024480403, -42.97311385573999587, 207.5838068554170377 ) ) ;
#16427 = CARTESIAN_POINT ( 'NONE',  ( 117.3134009501235795, -34.93240959161192194, 243.9641967044819637 ) ) ;
#16428 = CARTESIAN_POINT ( 'NONE',  ( 4.081702869980341042, 94.58342596962857840, 118.4863875214337838 ) ) ;
#16429 = ORIENTED_EDGE ( 'NONE', *, *, #43175, .T. ) ;
#16430 = DIRECTION ( 'NONE',  ( 1.000000000000000078E-15, -1.000000000000000000, 0.000000000000000000 ) ) ;
#16431 = CARTESIAN_POINT ( 'NONE',  ( 149.4512091874903206, -60.54365471797113685, 394.9756252759100903 ) ) ;
#16432 = DIRECTION ( 'NONE',  ( -0.9834602067153815907, -0.1811243269341220596, 0.000000000000000000 ) ) ;
#16433 = CARTESIAN_POINT ( 'NONE',  ( 36.74138383868164226, -48.33240602328862678, 300.4678068554150059 ) ) ;
#16434 = CARTESIAN_POINT ( 'NONE',  ( 113.6564618781686136, -45.68400828401183844, 29.08133956162495082 ) ) ;
#16435 = DIRECTION ( 'NONE',  ( 0.000000000000000000, 0.000000000000000000, 1.000000000000000000 ) ) ;
#16436 = ORIENTED_EDGE ( 'NONE', *, *, #28710, .T. ) ;
#16437 = CARTESIAN_POINT ( 'NONE',  ( 105.9839165226978110, -26.31690525417204540, 46.15848241876796720 ) ) ;
#16438 = CARTESIAN_POINT ( 'NONE',  ( 130.5667039024479834, -33.42944715994100591, 239.5838068554162987 ) ) ;
#16439 = VECTOR ( 'NONE', #25190, 1000.000000000000000 ) ;
#16440 = CARTESIAN_POINT ( 'NONE',  ( 112.2083724274664291, -26.91728527761779333, 14.68038718067299442 ) ) ;
#16441 = ORIENTED_EDGE ( 'NONE', *, *, #49686, .T. ) ;
#16442 = AXIS2_PLACEMENT_3D ( 'NONE', #48205, #35038, #55462 ) ;
#16443 = CARTESIAN_POINT ( 'NONE',  ( -24.79284581386642827, 127.0000000000000000, 90.32146847885337593 ) ) ;
#16444 = DIRECTION ( 'NONE',  ( 0.000000000000000000, 0.000000000000000000, 1.000000000000000000 ) ) ;
#16445 = CARTESIAN_POINT ( 'NONE',  ( 75.31670390244798341, -67.87844715994100397, 86.31780685541500020 ) ) ;
#16446 = CARTESIAN_POINT ( 'NONE',  ( 103.5365535965830475, -29.36946602085958702, 93.25094751244894553 ) ) ;
#16447 = CARTESIAN_POINT ( 'NONE',  ( 117.9712535577395869, -34.78749165583555225, 194.9546728949589749 ) ) ;
#16448 = FACE_OUTER_BOUND ( 'NONE', #45875, .T. ) ;
#16449 = ORIENTED_EDGE ( 'NONE', *, *, #32258, .T. ) ;
#16450 = CARTESIAN_POINT ( 'NONE',  ( 183.5150000000000148, 36.86249999999999716, -53.61543552338530105 ) ) ;
#16451 = EDGE_LOOP ( 'NONE', ( #47586, #22505, #29842, #439 ) ) ;
#16452 = ORIENTED_EDGE ( 'NONE', *, *, #30625, .T. ) ;
#16453 = VECTOR ( 'NONE', #82598, 1000.000000000000114 ) ;
#16454 = CARTESIAN_POINT ( 'NONE',  ( 134.0664832912740110, -41.22944715994101017, -0.5743747240890021422 ) ) ;
#16455 = ORIENTED_EDGE ( 'NONE', *, *, #84615, .F. ) ;
#16456 = EDGE_LOOP ( 'NONE', ( #5722, #86819, #87283, #17706 ) ) ;
#16457 = CARTESIAN_POINT ( 'NONE',  ( 59.56670390244699576, -67.87844715994098976, 120.2178068554179902 ) ) ;
#16458 = EDGE_CURVE ( 'NONE', #53148, #35758, #40886, .T. ) ;
#16459 = EDGE_CURVE ( 'NONE', #31056, #47018, #53695, .T. ) ;
#16460 = CARTESIAN_POINT ( 'NONE',  ( 97.31302290375664654, -38.96038935385655577, 42.50539279665081693 ) ) ;
#16461 = CARTESIAN_POINT ( 'NONE',  ( 115.1266331755855958, -39.55612640683342107, 132.9809912566479397 ) ) ;
#16462 = CARTESIAN_POINT ( 'NONE',  ( 101.2817000042767148, -26.35783695576231267, 255.4813395616251626 ) ) ;
#16463 = EDGE_CURVE ( 'NONE', #80081, #57023, #78581, .T. ) ;
#16464 = DIRECTION ( 'NONE',  ( 1.000000000000000000, 1.000000000000000078E-15, -0.000000000000000000 ) ) ;
#16465 = ORIENTED_EDGE ( 'NONE', *, *, #8287, .T. ) ;
#16466 = ADVANCED_FACE ( 'NONE', ( #23173 ), #72192, .T. ) ;
#16467 = ADVANCED_FACE ( 'NONE', ( #84945 ), #64039, .F. ) ;
#16468 = DIRECTION ( 'NONE',  ( 1.000000000000000078E-15, -1.000000000000000083E-30, -1.000000000000000000 ) ) ;
#16469 = ORIENTED_EDGE ( 'NONE', *, *, #63270, .F. ) ;
#16470 = DIRECTION ( 'NONE',  ( 0.000000000000000000, 1.000000000000000000, 0.000000000000000000 ) ) ;
#16471 = LINE ( 'NONE', #45045, #11031 ) ;
#16472 = CARTESIAN_POINT ( 'NONE',  ( 97.86672365782918348, -40.64956839743646100, 131.6470187837300330 ) ) ;
#16473 = EDGE_CURVE ( 'NONE', #2012, #82307, #64479, .T. ) ;
#16474 = AXIS2_PLACEMENT_3D ( 'NONE', #30665, #44274, #44723 ) ;
#16475 = CARTESIAN_POINT ( 'NONE',  ( 131.0667039024480971, -58.72944715994092491, 207.5838068554170377 ) ) ;
#16476 = ORIENTED_EDGE ( 'NONE', *, *, #23576, .F. ) ;
#16477 = CARTESIAN_POINT ( 'NONE',  ( 96.26778515314977369, -34.36995442310919202, 256.1432443235300980 ) ) ;
#16478 = CARTESIAN_POINT ( 'NONE',  ( 96.61551125061282619, -32.99117460050268846, 22.06514908543494258 ) ) ;
#16479 =( NAMED_UNIT ( * ) PLANE_ANGLE_UNIT ( ) SI_UNIT ( $, .RADIAN. ) );
#16480 = AXIS2_PLACEMENT_3D ( 'NONE', #44032, #64504, #78153 ) ;
#16481 = B_SPLINE_CURVE_WITH_KNOTS ( 'NONE', 3,
 ( #49402, #16256, #21270, #85314, #55752, #48943, #42581, #71669, #8998, #77581, #35331, #7642, #70316, #37143, #50761, #56671, #70773, #57113, #63043, #825, #50301, #14465, #83959, #76685, #78041, #84415, #42142, #71226, #21730, #77138 ),
 .UNSPECIFIED., .F., .F.,
 ( 4, 2, 2, 2, 2, 2, 2, 2, 2, 2, 1, 1, 1, 1, 1, 1, 2, 4 ),
 ( 0.000000000000000000, 0.06250190528924848277, 0.1250038105784969655, 0.1875057158677454483, 0.2500076211569939311, 0.3125095264462424138, 0.3750114317354908966, 0.4375133370247393794, 0.4687642896693638428, 0.4843897659916759912, 0.4922025041528320100, 0.4961088732334101858, 0.4980620577736992183, 0.4990386500438436235, 0.4995269461789159093, 0.4997710942464516637, 0.4998931682802195686, 0.5000152423139874180 ),
 .UNSPECIFIED. ) ;
#16482 = CARTESIAN_POINT ( 'NONE',  ( 130.5667039024480118, -39.24694715994083793, 219.5838068554170093 ) ) ;
#16483 = ADVANCED_FACE ( 'NONE', ( #8634 ), #1816, .T. ) ;
#16485 = CARTESIAN_POINT ( 'NONE',  ( 69.37738364949149172, -138.6267510924388944, 247.3762624300263155 ) ) ;
#16484 = DIRECTION ( 'NONE',  ( -0.9963424814100680926, 0.08544974978095698503, 0.000000000000000000 ) ) ;
#16486 = DIRECTION ( 'NONE',  ( -0.000000000000000000, -0.000000000000000000, -1.000000000000000000 ) ) ;
#16487 = PLANE ( 'NONE',  #27815 ) ;
#16488 = CARTESIAN_POINT ( 'NONE',  ( 131.4905132191207997, -37.69637952317774676, 6.988870342676155367 ) ) ;
#16489 = LINE ( 'NONE', #44168, #80752 ) ;
#16490 = CARTESIAN_POINT ( 'NONE',  ( 109.6433924709448888, -46.47999098159603903, 162.7813146523185424 ) ) ;
#16491 = ADVANCED_FACE ( 'NONE', ( #22262 ), #44909, .F. ) ;
#16492 = DIRECTION ( 'NONE',  ( 1.000000000000000000, 4.299999999999999979E-14, 1.000000000000000078E-15 ) ) ;
#16493 = FACE_OUTER_BOUND ( 'NONE', #14938, .T. ) ;
#16494 = CARTESIAN_POINT ( 'NONE',  ( 97.06250871634010480, -39.81605817309107920, 21.56419670448195092 ) ) ;
#16495 = CARTESIAN_POINT ( 'NONE',  ( 96.74313874428034410, -35.27650366090898615, 177.2156252759109805 ) ) ;
#16496 = CARTESIAN_POINT ( 'NONE',  ( 101.5975885682485398, -47.27054607199826819, 13.19562527591094891 ) ) ;
#16498 = LINE ( 'NONE', #71913, #12274 ) ;
#16497 = CARTESIAN_POINT ( 'NONE',  ( 97.81167943543778165, -40.51737693692245301, 166.6360185166829808 ) ) ;
#16499 = CARTESIAN_POINT ( 'NONE',  ( 82.73250004807572111, -36.03188439719672687, 2.979900720421668758 ) ) ;
#16500 = EDGE_CURVE ( 'NONE', #42802, #74968, #70862, .T. ) ;
#16501 = CIRCLE ( 'NONE', #70180, 2.517500000000005844 ) ;
#16502 = ORIENTED_EDGE ( 'NONE', *, *, #29490, .T. ) ;
#16503 = CARTESIAN_POINT ( 'NONE',  ( 74.36911441044604487, 82.54999999999999716, 92.32962665258637003 ) ) ;
#16504 = VERTEX_POINT ( 'NONE', #9078 ) ;
#16505 = CARTESIAN_POINT ( 'NONE',  ( 116.4365193811696457, -32.28633913640747011, 60.19086337114898555 ) ) ;
#16507 = ORIENTED_EDGE ( 'NONE', *, *, #66609, .F. ) ;
#16506 = CARTESIAN_POINT ( 'NONE',  ( 0.7862675091416512219, 95.25000000000004263, 130.5560000000000684 ) ) ;
#16508 = AXIS2_PLACEMENT_3D ( 'NONE', #9822, #16637, #23905 ) ;
#16509 = CARTESIAN_POINT ( 'NONE',  ( 116.8173832505959666, -34.15392672464852808, 50.03137649336521520 ) ) ;
#16510 = CARTESIAN_POINT ( 'NONE',  ( 96.07698540226633099, -35.78353028925530310, 182.2461014663869889 ) ) ;
#16511 = CARTESIAN_POINT ( 'NONE',  ( 184.5667039024480118, -67.87844715994100397, 20.91780685541479912 ) ) ;
#16512 = CARTESIAN_POINT ( 'NONE',  ( 97.82529570206294522, -40.55052488149144096, 146.6384733909613090 ) ) ;
#16513 = CARTESIAN_POINT ( 'NONE',  ( 126.0667039024479266, -14.72944715994094977, 239.5838068554170377 ) ) ;
#16514 = DIRECTION ( 'NONE',  ( -1.000000000000000078E-15, 1.000000000000000000, 0.000000000000000000 ) ) ;
#16515 = EDGE_CURVE ( 'NONE', #35035, #85102, #22711, .T. ) ;
#16516 = CARTESIAN_POINT ( 'NONE',  ( 63.06670390244794078, -40.32844715994017548, 300.4678068554150627 ) ) ;
#16517 = CARTESIAN_POINT ( 'NONE',  ( 116.9402674190077391, -38.58240887119603713, 98.67907853902740101 ) ) ;
#16518 = EDGE_CURVE ( 'NONE', #2985, #13223, #2261, .T. ) ;
#16519 = CARTESIAN_POINT ( 'NONE',  ( 108.2018929880948832, -26.98138995270364759, 129.9841967044829687 ) ) ;
#16520 = ORIENTED_EDGE ( 'NONE', *, *, #12476, .F. ) ;
#16521 = ORIENTED_EDGE ( 'NONE', *, *, #65904, .F. ) ;
#16522 = VECTOR ( 'NONE', #81918, 1000.000000000000114 ) ;
#16523 = CARTESIAN_POINT ( 'NONE',  ( 103.5852769812406535, -44.87864842379759978, 88.68729759161098514 ) ) ;
#16524 = DIRECTION ( 'NONE',  ( -1.000000000000000000, 7.570719237730541270E-15, 0.000000000000000000 ) ) ;
#16526 = DIRECTION ( 'NONE',  ( -4.237773401492740281E-14, 1.000000000000000000, 0.000000000000000000 ) ) ;
#16525 = CARTESIAN_POINT ( 'NONE',  ( 99.57924082623978279, -30.38476633542330774, 211.7670538473389570 ) ) ;
#16527 = CARTESIAN_POINT ( 'NONE',  ( 100.8594679592200833, 82.54999999999999716, 82.89895571708400723 ) ) ;
#16528 = DIRECTION ( 'NONE',  ( 1.986798540846734824E-16, 0.000000000000000000, -1.000000000000000000 ) ) ;
#16529 = LINE ( 'NONE', #31039, #33027 ) ;
#16530 = DIRECTION ( 'NONE',  ( 0.7071067811865660024, 0.000000000000000000, 0.7071067811865291430 ) ) ;
#16531 = CARTESIAN_POINT ( 'NONE',  ( 12.27767421224444533, 79.68862222894867386, 117.9185750741009429 ) ) ;
#16532 = CARTESIAN_POINT ( 'NONE',  ( 108.8451227504523331, -46.97957433935484772, 167.7127681330539701 ) ) ;
#16533 = VERTEX_POINT ( 'NONE', #37220 ) ;
#16534 = ORIENTED_EDGE ( 'NONE', *, *, #78333, .T. ) ;
#16535 = EDGE_CURVE ( 'NONE', #86596, #22588, #44460, .T. ) ;
#16536 = DIRECTION ( 'NONE',  ( 1.000000000000000000, 1.000000000000000078E-15, 0.000000000000000000 ) ) ;
#16537 = CARTESIAN_POINT ( 'NONE',  ( 77.50946880809777895, -17.71735499139141723, 2.839545688279708546 ) ) ;
#16538 = DIRECTION ( 'NONE',  ( 4.299999999999999979E-14, -1.000000000000000000, 4.400000000000000367E-29 ) ) ;
#16539 = LINE ( 'NONE', #44214, #68538 ) ;
#16540 = CARTESIAN_POINT ( 'NONE',  ( 112.3381529121750191, -29.09364788469061480, 237.4138046553059951 ) ) ;
#16541 = EDGE_CURVE ( 'NONE', #4843, #47987, #48395, .T. ) ;
#16542 = FACE_OUTER_BOUND ( 'NONE', #36307, .T. ) ;
#16543 =( BOUNDED_CURVE ( )  B_SPLINE_CURVE ( 3, ( #62640, #414, #28106, #55789 ),
 .UNSPECIFIED., .F., .T. ) 
 B_SPLINE_CURVE_WITH_KNOTS ( ( 4, 4 ),
 ( 4.712388980381146730, 6.283185307176318624 ),
 .UNSPECIFIED. ) 
 CURVE ( )  GEOMETRIC_REPRESENTATION_ITEM ( )  RATIONAL_B_SPLINE_CURVE ( ( 1.000000000000000000, 0.8047378541235299387, 0.8047378541235299387, 1.000000000000000000 ) ) 
 REPRESENTATION_ITEM ( '' )  );
#16544 = AXIS2_PLACEMENT_3D ( 'NONE', #74551, #25962, #5065 ) ;
#16545 = CARTESIAN_POINT ( 'NONE',  ( 107.6545119506432258, -47.76725988480858121, 197.6308633711489620 ) ) ;
#16546 = LINE ( 'NONE', #1127, #40199 ) ;
#16547 = VERTEX_POINT ( 'NONE', #59869 ) ;
#16549 = EDGE_LOOP ( 'NONE', ( #71824, #71644, #19254, #24499 ) ) ;
#16548 = EDGE_LOOP ( 'NONE', ( #2970, #46441, #85163, #86715, #18199, #74772 ) ) ;
#16550 = CARTESIAN_POINT ( 'NONE',  ( 97.85750890579558359, -40.62776002508964268, 62.64559988044219807 ) ) ;
#16551 = EDGE_LOOP ( 'NONE', ( #56364, #60554 ) ) ;
#16552 = DIRECTION ( 'NONE',  ( -2.108231265501709878E-16, 0.000000000000000000, 1.000000000000000000 ) ) ;
#16553 = CARTESIAN_POINT ( 'NONE',  ( 131.8552587341498281, -35.08426237659745084, 7.378668740724780406 ) ) ;
#16554 = CARTESIAN_POINT ( 'NONE',  ( 98.13886466857337609, -39.66030079267085995, 283.0225356868493805 ) ) ;
#16555 = CARTESIAN_POINT ( 'NONE',  ( 83.06670390244796920, -61.87844715994100397, 237.1838068554150141 ) ) ;
#16556 = ORIENTED_EDGE ( 'NONE', *, *, #60221, .T. ) ;
#16557 = CARTESIAN_POINT ( 'NONE',  ( 114.2248125149048263, -42.04901104171000270, 9.635625275910941312 ) ) ;
#16558 = ADVANCED_FACE ( 'NONE', ( #79914 ), #32376, .F. ) ;
#16559 = CARTESIAN_POINT ( 'NONE',  ( 105.4788588808462038, 120.6499999999999915, -3.968749999999580336 ) ) ;
#16560 = VERTEX_POINT ( 'NONE', #18550 ) ;
#16561 = VERTEX_POINT ( 'NONE', #39878 ) ;
#16562 = AXIS2_PLACEMENT_3D ( 'NONE', #329, #20778, #82581 ) ;
#16563 = CARTESIAN_POINT ( 'NONE',  ( 111.2307140782278765, -45.82263013567369825, 112.9182118773837118 ) ) ;
#16564 = AXIS2_PLACEMENT_3D ( 'NONE', #35024, #47299, #510 ) ;
#16565 = VERTEX_POINT ( 'NONE', #32173 ) ;
#16566 = ORIENTED_EDGE ( 'NONE', *, *, #68493, .F. ) ;
#16567 = AXIS2_PLACEMENT_3D ( 'NONE', #78039, #77136, #56206 ) ;
#16568 = EDGE_CURVE ( 'NONE', #79504, #63431, #35296, .T. ) ;
#16569 = ADVANCED_FACE ( 'NONE', ( #26262 ), #32619, .F. ) ;
#16570 = CARTESIAN_POINT ( 'NONE',  ( 98.90470121413369498, -39.24767091914073802, 20.98670554236298358 ) ) ;
#16572 = CARTESIAN_POINT ( 'NONE',  ( 102.9583934913338652, -26.44260899983745006, 175.3908633711489813 ) ) ;
#16571 = AXIS2_PLACEMENT_3D ( 'NONE', #64300, #36137, #83396 ) ;
#16573 = EDGE_CURVE ( 'NONE', #50785, #6249, #27827, .T. ) ;
#16574 = CARTESIAN_POINT ( 'NONE',  ( 108.6454077996538530, -25.81962716842089378, 149.9737205140059473 ) ) ;
#16575 = CARTESIAN_POINT ( 'NONE',  ( 25.56670390244797275, -48.82844715994099971, 259.9678068554150059 ) ) ;
#16576 = CARTESIAN_POINT ( 'NONE',  ( 106.1383564330493812, -47.74364531592736682, 258.4975300378158636 ) ) ;
#16577 = CARTESIAN_POINT ( 'NONE',  ( 59.68306514483415270, -72.55903866283681225, 542.9756252759101471 ) ) ;
#16578 = CARTESIAN_POINT ( 'NONE',  ( 108.4156033759623909, -26.73479662881522856, 125.9691087597593082 ) ) ;
#16579 = DIRECTION ( 'NONE',  ( 0.000000000000000000, 0.000000000000000000, 1.000000000000000000 ) ) ;
#16580 = VERTEX_POINT ( 'NONE', #34412 ) ;
#16581 = EDGE_CURVE ( 'NONE', #27442, #78823, #40778, .T. ) ;
#16582 = ORIENTED_EDGE ( 'NONE', *, *, #60901, .F. ) ;
#16583 = EDGE_CURVE ( 'NONE', #72917, #31310, #89853, .T. ) ;
#16584 = CARTESIAN_POINT ( 'NONE',  ( 101.9629764938643035, -45.91127772325894085, 187.1727681330539781 ) ) ;
#16585 = ORIENTED_EDGE ( 'NONE', *, *, #63824, .T. ) ;
#16586 = CARTESIAN_POINT ( 'NONE',  ( 117.4575111195971857, -40.49848259682686802, 173.5375300378159693 ) ) ;
#16587 = CARTESIAN_POINT ( 'NONE',  ( 104.4889533838567104, -26.97908276470762701, 265.2814877645184879 ) ) ;
#16588 = DIRECTION ( 'NONE',  ( -1.000000000000000000, -8.163404592832032979E-16, 0.000000000000000000 ) ) ;
#16589 = DIRECTION ( 'NONE',  ( -1.000000000000000000, 0.000000000000000000, 0.000000000000000000 ) ) ;
#16592 = CARTESIAN_POINT ( 'NONE',  ( 98.07879728544668296, -32.87107120142745487, 12.00419670448193976 ) ) ;
#16591 = LINE ( 'NONE', #37921, #3529 ) ;
#16590 = CARTESIAN_POINT ( 'NONE',  ( 97.99254151483945918, -40.00862495256633622, 277.6356252759111385 ) ) ;
#16593 = DIRECTION ( 'NONE',  ( 0.000000000000000000, 1.000000000000000000, 0.000000000000000000 ) ) ;
#16595 = EDGE_CURVE ( 'NONE', #8519, #7620, #43986, .T. ) ;
#16594 = LINE ( 'NONE', #44273, #88850 ) ;
#16596 = CARTESIAN_POINT ( 'NONE',  ( 179.4595971212889651, -28.98061976758942748, 342.9256252759109884 ) ) ;
#16597 = DIRECTION ( 'NONE',  ( 0.000000000000000000, 0.000000000000000000, 1.000000000000000000 ) ) ;
#16598 = LINE ( 'NONE', #49755, #32872 ) ;
#16599 = DIRECTION ( 'NONE',  ( 2.127927463864879951E-15, 1.848892746611749922E-31, 1.000000000000000000 ) ) ;
#16601 = VERTEX_POINT ( 'NONE', #34863 ) ;
#16600 = CARTESIAN_POINT ( 'NONE',  ( 111.4101316090540479, -43.50011782763849055, 195.5838068554169809 ) ) ;
#16602 = FACE_OUTER_BOUND ( 'NONE', #19699, .T. ) ;
#16603 = CARTESIAN_POINT ( 'NONE',  ( 98.24258143063333648, -42.32275744278853580, 186.7756252759109543 ) ) ;
#16604 = CARTESIAN_POINT ( 'NONE',  ( 106.8411897839350786, -48.57781660025092663, 73.56133956162497611 ) ) ;
#16605 = CARTESIAN_POINT ( 'NONE',  ( 96.00064313654479520, -35.86649870909684523, 187.2765776568629406 ) ) ;
#16606 = DIRECTION ( 'NONE',  ( 0.000000000000000000, -1.000000000000000000, 0.000000000000000000 ) ) ;
#16607 = DIRECTION ( 'NONE',  ( 1.000000000000000078E-15, -1.000000000000000083E-30, -1.000000000000000000 ) ) ;
#16609 = CYLINDRICAL_SURFACE ( 'NONE', #31261, 4.762500000000001066 ) ;
#16608 = DIRECTION ( 'NONE',  ( -4.237773401492740281E-14, 1.000000000000000000, 0.000000000000000000 ) ) ;
#16610 = LINE ( 'NONE', #72026, #30579 ) ;
#16611 = CARTESIAN_POINT ( 'NONE',  ( 46.48091746482130304, -49.32844715994084339, 300.4678068554150059 ) ) ;
#16612 = ORIENTED_EDGE ( 'NONE', *, *, #62941, .T. ) ;
#16613 = AXIS2_PLACEMENT_3D ( 'NONE', #19605, #83195, #63181 ) ;
#16614 = CARTESIAN_POINT ( 'NONE',  ( 6.938893903907229955E-15, 60.82030000000000314, 209.4690212008904950 ) ) ;
#16615 = VECTOR ( 'NONE', #78940, 1000.000000000000000 ) ;
#16616 = ORIENTED_EDGE ( 'NONE', *, *, #69735, .F. ) ;
#16617 = EDGE_LOOP ( 'NONE', ( #1369, #24263, #19534, #70022 ) ) ;
#16618 = CARTESIAN_POINT ( 'NONE',  ( 108.8595479556035599, -45.11020018309576329, 107.1667055423619672 ) ) ;
#16620 = ORIENTED_EDGE ( 'NONE', *, *, #78011, .F. ) ;
#16619 = DIRECTION ( 'NONE',  ( 0.7071067811865473507, 0.000000000000000000, -0.7071067811865476838 ) ) ;
#16621 = CARTESIAN_POINT ( 'NONE',  ( 113.3292761056178648, -27.64973082387879444, 85.60800622829195561 ) ) ;
#16622 = CYLINDRICAL_SURFACE ( 'NONE', #68642, 2.517499999999998739 ) ;
#16623 = CARTESIAN_POINT ( 'NONE',  ( 48.45959712129000252, -28.98061976758940617, -5.074374724088000832 ) ) ;
#16624 = DIRECTION ( 'NONE',  ( -1.000000000000000078E-15, 1.000000000000000000, 0.000000000000000000 ) ) ;
#16625 = ADVANCED_FACE ( 'NONE', ( #20795 ), #69844, .F. ) ;
#16626 = CARTESIAN_POINT ( 'NONE',  ( 109.4837483930865574, -46.20680252518646114, 47.77562527591094721 ) ) ;
#16627 = ORIENTED_EDGE ( 'NONE', *, *, #35363, .T. ) ;
#16628 = VERTEX_POINT ( 'NONE', #55283 ) ;
#16629 = ORIENTED_EDGE ( 'NONE', *, *, #2128, .F. ) ;
#16630 = VECTOR ( 'NONE', #6669, 1000.000000000000000 ) ;
#16631 = AXIS2_PLACEMENT_3D ( 'NONE', #46404, #33697, #13259 ) ;
#16632 = DIRECTION ( 'NONE',  ( -0.7071067812163244204, 0.7071067811567707251, -7.071067812163251589E-16 ) ) ;
#16633 = VECTOR ( 'NONE', #11708, 1000.000000000000114 ) ;
#16634 = LINE ( 'NONE', #72045, #78114 ) ;
#16635 = CARTESIAN_POINT ( 'NONE',  ( 100.9546728166709215, -28.70702572326774416, 116.5939586087175286 ) ) ;
#16636 = AXIS2_PLACEMENT_3D ( 'NONE', #18811, #27408, #69204 ) ;
#16637 = DIRECTION ( 'NONE',  ( -0.7071067811866279529, 0.7071067811864671926, -7.071067811866286874E-16 ) ) ;
#16638 = CARTESIAN_POINT ( 'NONE',  ( 30.48091746481746611, -48.32844715994156815, 129.9678068554150627 ) ) ;
#16639 = DIRECTION ( 'NONE',  ( -0.000000000000000000, 1.000000000000000000, -0.000000000000000000 ) ) ;
#16641 = DIRECTION ( 'NONE',  ( 1.000000000000000078E-15, -1.000000000000000083E-30, -1.000000000000000000 ) ) ;
#16640 = AXIS2_PLACEMENT_3D ( 'NONE', #86866, #45490, #71901 ) ;
#16642 = AXIS2_PLACEMENT_3D ( 'NONE', #13272, #81439, #68683 ) ;
#16643 = CARTESIAN_POINT ( 'NONE',  ( -5.570957693668114885, 93.96460761459663047, 130.4371699319834761 ) ) ;
#16644 = CARTESIAN_POINT ( 'NONE',  ( 96.36089708107958529, -41.75325360632975702, 61.67562527591097421 ) ) ;
#16645 = ORIENTED_EDGE ( 'NONE', *, *, #34064, .T. ) ;
#16646 = DIRECTION ( 'NONE',  ( 0.000000000000000000, 0.000000000000000000, 1.000000000000000000 ) ) ;
#16647 = DIRECTION ( 'NONE',  ( -0.000000000000000000, -0.000000000000000000, -1.000000000000000000 ) ) ;
#16648 = CARTESIAN_POINT ( 'NONE',  ( 110.7682021097048306, -28.22102727396991284, 132.5680903695919710 ) ) ;
#16649 = EDGE_CURVE ( 'NONE', #56710, #43418, #6269, .T. ) ;
#16650 = CIRCLE ( 'NONE', #26814, 5.041900000000000048 ) ;
#16651 = CARTESIAN_POINT ( 'NONE',  ( 36.74138383868164226, -48.33240602328862678, 300.4678068554150059 ) ) ;
#16652 = FACE_OUTER_BOUND ( 'NONE', #39322, .T. ) ;
#16653 = ORIENTED_EDGE ( 'NONE', *, *, #14489, .F. ) ;
#16654 = VERTEX_POINT ( 'NONE', #61658 ) ;
#16655 = DIRECTION ( 'NONE',  ( 0.000000000000000000, 0.000000000000000000, 1.000000000000000000 ) ) ;
#16656 = ORIENTED_EDGE ( 'NONE', *, *, #74199, .T. ) ;
#16657 = ORIENTED_EDGE ( 'NONE', *, *, #14935, .F. ) ;
#16658 = CARTESIAN_POINT ( 'NONE',  ( 98.29135092237498839, -35.49440443996801520, 177.6472975916109647 ) ) ;
#16659 = FACE_OUTER_BOUND ( 'NONE', #42642, .T. ) ;
#16660 = CARTESIAN_POINT ( 'NONE',  ( 96.64920772548965999, -35.94453432339758336, 142.2670538473399517 ) ) ;
#16661 = CARTESIAN_POINT ( 'NONE',  ( 147.0667039024457665, -137.6758868153238780, 245.5072646551060132 ) ) ;
#16662 = AXIS2_PLACEMENT_3D ( 'NONE', #44292, #2547, #65206 ) ;
#16663 = CARTESIAN_POINT ( 'NONE',  ( 97.81170008160388818, -40.51743097690945916, 72.63551179937353197 ) ) ;
#16664 = VERTEX_POINT ( 'NONE', #76200 ) ;
#16665 = VECTOR ( 'NONE', #69323, 1000.000000000000000 ) ;
#16666 = VERTEX_POINT ( 'NONE', #27159 ) ;
#16667 = ORIENTED_EDGE ( 'NONE', *, *, #53549, .T. ) ;
#16668 = EDGE_CURVE ( 'NONE', #57023, #65340, #83043, .T. ) ;
#16669 = CARTESIAN_POINT ( 'NONE',  ( 98.55143180905920985, -33.04300857791147195, 208.8195189410199646 ) ) ;
#16670 = CARTESIAN_POINT ( 'NONE',  ( 115.2246207261642894, -44.22212590188486558, 78.22324432352995416 ) ) ;
#16671 = ORIENTED_EDGE ( 'NONE', *, *, #86852, .T. ) ;
#16672 = EDGE_CURVE ( 'NONE', #84699, #54126, #41658, .T. ) ;
#16673 = CARTESIAN_POINT ( 'NONE',  ( 118.1852327621007532, -40.75705396371412803, 23.54991099019593292 ) ) ;
#16674 = CARTESIAN_POINT ( 'NONE',  ( 117.0725227226916587, -35.46769152344445786, 253.9273137617209954 ) ) ;
#16675 = DIRECTION ( 'NONE',  ( 1.000000000000000000, 8.673617379883546378E-16, 9.757819552368989676E-16 ) ) ;
#16676 = CARTESIAN_POINT ( 'NONE',  ( 112.8675307907708287, -28.58609239232746546, 195.5838076129389833 ) ) ;
#16677 = ADVANCED_FACE ( 'NONE', ( #54833 ), #41215, .F. ) ;
#16678 = CARTESIAN_POINT ( 'NONE',  ( 108.7432144037193922, -25.80414517310806488, 140.9432443235299672 ) ) ;
#16679 = LINE ( 'NONE', #16241, #26266 ) ;
#16680 = ORIENTED_EDGE ( 'NONE', *, *, #6399, .T. ) ;
#16681 = CARTESIAN_POINT ( 'NONE',  ( 64.68306507141299733, -72.55818180160879649, 394.9756252759101471 ) ) ;
#16682 = EDGE_CURVE ( 'NONE', #70782, #11886, #38170, .T. ) ;
#16683 = EDGE_LOOP ( 'NONE', ( #34049, #13492, #37190, #33205 ) ) ;
#16684 = CARTESIAN_POINT ( 'NONE',  ( 107.0667039024479834, -36.72944715994099596, 239.5838068554170093 ) ) ;
#16685 = VERTEX_POINT ( 'NONE', #7615 ) ;
#16686 = ORIENTED_EDGE ( 'NONE', *, *, #71571, .F. ) ;
#16687 = CIRCLE ( 'NONE', #8007, 2.116999999999993776 ) ;
#16688 = CARTESIAN_POINT ( 'NONE',  ( 258.9276602595319901, 52.73749999999999716, -2.903194600000015502 ) ) ;
#16689 = TOROIDAL_SURFACE ( 'NONE', #15279, 13.50000000000000000, 0.5000000000000000000 ) ;
#16690 = VECTOR ( 'NONE', #79766, 1000.000000000000000 ) ;
#16691 = CARTESIAN_POINT ( 'NONE',  ( 75.31670390244798341, -67.87844715994100397, 88.43480685541499042 ) ) ;
#16692 = CARTESIAN_POINT ( 'NONE',  ( 112.7417948769132039, -27.24419935825454431, 54.65943479971996055 ) ) ;
#16693 = CARTESIAN_POINT ( 'NONE',  ( 132.2857443282839824, -83.77844715994092439, 55.21780685541800437 ) ) ;
#16694 = AXIS2_PLACEMENT_3D ( 'NONE', #35876, #6382, #54946 ) ;
#16695 = DIRECTION ( 'NONE',  ( 0.000000000000000000, 0.000000000000000000, 1.000000000000000000 ) ) ;
#16696 = CARTESIAN_POINT ( 'NONE',  ( 116.8171228663217533, -34.15291832013626561, 75.03145860928886179 ) ) ;
#16697 = CARTESIAN_POINT ( 'NONE',  ( 107.5734549334945456, -47.83597508069291138, 42.61276813305398292 ) ) ;
#16699 = CARTESIAN_POINT ( 'NONE',  ( 114.5119312840559473, -28.59475203354334027, 150.4746728949579619 ) ) ;
#16698 = DIRECTION ( 'NONE',  ( 0.000000000000000000, 0.000000000000000000, -1.000000000000000000 ) ) ;
#16700 = CARTESIAN_POINT ( 'NONE',  ( 63.03715912545646205, -24.89890238295017255, 129.9678068554150911 ) ) ;
#16702 = ADVANCED_FACE ( 'NONE', ( #33371, #12943 ), #67891, .F. ) ;
#16701 = DIRECTION ( 'NONE',  ( 0.000000000000000000, 0.000000000000000000, -1.000000000000000000 ) ) ;
#16703 = ORIENTED_EDGE ( 'NONE', *, *, #19132, .F. ) ;
#16704 = PLANE ( 'NONE',  #43953 ) ;
#16705 = AXIS2_PLACEMENT_3D ( 'NONE', #1194, #1652, #7561 ) ;
#16706 = AXIS2_PLACEMENT_3D ( 'NONE', #50698, #36645, #62986 ) ;
#16707 = PLANE ( 'NONE',  #23883 ) ;
#16708 = DIRECTION ( 'NONE',  ( -0.000000000000000000, 1.000000000000000000, 0.000000000000000000 ) ) ;
#16709 = CARTESIAN_POINT ( 'NONE',  ( 242.3160000000000025, 65.43750000000000000, -63.94449999999999790 ) ) ;
#16711 = EDGE_LOOP ( 'NONE', ( #43254, #18882, #69436, #71434, #4625, #62122, #22296, #3354 ) ) ;
#16710 = CARTESIAN_POINT ( 'NONE',  ( 98.39836552415940218, -29.79571670633027836, 195.7775300378159784 ) ) ;
#16712 = DIRECTION ( 'NONE',  ( 1.514143847546114723E-15, -0.8660254037844387076, -0.4999999999999998890 ) ) ;
#16713 = CARTESIAN_POINT ( 'NONE',  ( 96.78746529907793672, -40.85582509469530521, 247.6422919425769749 ) ) ;
#16714 = CARTESIAN_POINT ( 'NONE',  ( 98.82360578189442890, -43.24043672769812474, 87.85848241876792031 ) ) ;
#16715 = DIRECTION ( 'NONE',  ( -1.000000000000000078E-15, 1.000000000000000083E-30, 1.000000000000000000 ) ) ;
#16716 = CARTESIAN_POINT ( 'NONE',  ( 87.06648329127401098, -46.72944715994105280, 14.67562527591094934 ) ) ;
#16717 = VECTOR ( 'NONE', #23240, 1000.000000000000000 ) ;
#16718 = DIRECTION ( 'NONE',  ( 1.387778780781444492E-15, 0.000000000000000000, -1.000000000000000000 ) ) ;
#16719 = EDGE_LOOP ( 'NONE', ( #76085, #35168, #71841, #32705, #70531, #45877 ) ) ;
#16720 = CIRCLE ( 'NONE', #21123, 5.035202529042187791 ) ;
#16721 = ORIENTED_EDGE ( 'NONE', *, *, #53914, .F. ) ;
#16722 = EDGE_LOOP ( 'NONE', ( #69601, #8350 ) ) ;
#16723 = ORIENTED_EDGE ( 'NONE', *, *, #33251, .T. ) ;
#16724 = CARTESIAN_POINT ( 'NONE',  ( 126.0667039024479266, -14.72944715994094977, 239.5838068554170377 ) ) ;
#16725 = CARTESIAN_POINT ( 'NONE',  ( 100.2472489666992743, -45.42841400796814355, 273.0594347997205773 ) ) ;
#16726 = DIRECTION ( 'NONE',  ( -1.000000000000000078E-15, 1.000000000000000083E-30, 1.000000000000000000 ) ) ;
#16727 = CARTESIAN_POINT ( 'NONE',  ( 33.92127028473601769, -29.73316016639540749, -5.074374724088000832 ) ) ;
#16729 = PLANE ( 'NONE',  #3653 ) ;
#16728 = DIRECTION ( 'NONE',  ( 0.9068632946707807507, -0.4214249218767880945, 9.080193194566099635E-16 ) ) ;
#16730 = CARTESIAN_POINT ( 'NONE',  ( 183.5150000000000148, 53.21300000000000097, 41.63456447661469895 ) ) ;
#16731 = EDGE_CURVE ( 'NONE', #12987, #48763, #12491, .T. ) ;
#16732 = CARTESIAN_POINT ( 'NONE',  ( 103.1098180292659947, -44.29918505015107399, 211.6152769709339623 ) ) ;
#16733 = ORIENTED_EDGE ( 'NONE', *, *, #69802, .T. ) ;
#16734 = ORIENTED_EDGE ( 'NONE', *, *, #5625, .F. ) ;
#16735 = VECTOR ( 'NONE', #51173, 1000.000000000000114 ) ;
#16736 = ORIENTED_EDGE ( 'NONE', *, *, #4045, .F. ) ;
#16737 = CARTESIAN_POINT ( 'NONE',  ( 142.8838050580815775, -82.11588141944041297, 542.9756252759101471 ) ) ;
#16738 = VECTOR ( 'NONE', #73565, 999.9999999999998863 ) ;
#16739 = DIRECTION ( 'NONE',  ( -1.000000000000000000, -1.734723475976808672E-15, 0.000000000000000000 ) ) ;
#16740 = EDGE_CURVE ( 'NONE', #13307, #17048, #75909, .T. ) ;
#16741 = CARTESIAN_POINT ( 'NONE',  ( 115.1244435615320612, -31.12738976831575144, 275.3099109901961015 ) ) ;
#16742 = CARTESIAN_POINT ( 'NONE',  ( 38.10000000000000142, 69.84999999999999432, 346.0750000000000455 ) ) ;
#16743 = LINE ( 'NONE', #8249, #37544 ) ;
#16744 = CARTESIAN_POINT ( 'NONE',  ( 113.1774560752732839, -44.75249464381799669, 28.09387619456539653 ) ) ;
#16745 = ORIENTED_EDGE ( 'NONE', *, *, #1368, .F. ) ;
#16746 = DIRECTION ( 'NONE',  ( -0.000000000000000000, -0.000000000000000000, 1.000000000000000000 ) ) ;
#16747 = ORIENTED_EDGE ( 'NONE', *, *, #40872, .F. ) ;
#16748 = DIRECTION ( 'NONE',  ( -0.7071067811865779928, 0.7071067811865171526, -2.899137802864836037E-29 ) ) ;
#16749 = CARTESIAN_POINT ( 'NONE',  ( 101.3472728536945198, -42.59232338312836674, 19.77951894102097796 ) ) ;
#16750 = AXIS2_PLACEMENT_3D ( 'NONE', #49901, #22229, #77631 ) ;
#16751 = EDGE_CURVE ( 'NONE', #37281, #78352, #25210, .T. ) ;
#16752 = AXIS2_PLACEMENT_3D ( 'NONE', #17402, #4661, #11019 ) ;
#16753 = VECTOR ( 'NONE', #2451, 1000.000000000000000 ) ;
#16754 = CARTESIAN_POINT ( 'NONE',  ( 38.69148329127400388, 12.92155284005802685, 335.5992267699910485 ) ) ;
#16755 = CIRCLE ( 'NONE', #12405, 2.517500000000005844 ) ;
#16756 = DIRECTION ( 'NONE',  ( 1.000000000000000078E-15, 1.000000000000000083E-30, -1.000000000000000000 ) ) ;
#16757 = DIRECTION ( 'NONE',  ( 0.000000000000000000, 0.000000000000000000, 1.000000000000000000 ) ) ;
#16758 = EDGE_LOOP ( 'NONE', ( #61347, #88175, #56874, #54711 ) ) ;
#16759 = LINE ( 'NONE', #35846, #43610 ) ;
#16760 = CYLINDRICAL_SURFACE ( 'NONE', #87616, 3.174999999999997158 ) ;
#16761 = ORIENTED_EDGE ( 'NONE', *, *, #77263, .F. ) ;
#16762 = CARTESIAN_POINT ( 'NONE',  ( 101.0660769631361688, -27.44644056990073366, 70.54514908543497143 ) ) ;
#16763 = VERTEX_POINT ( 'NONE', #40631 ) ;
#16764 = CARTESIAN_POINT ( 'NONE',  ( 106.9524907322914089, -28.15978509997144741, 59.50956268521995440 ) ) ;
#16765 = AXIS2_PLACEMENT_3D ( 'NONE', #21153, #42911, #55631 ) ;
#16766 = EDGE_CURVE ( 'NONE', #82989, #76109, #22236, .T. ) ;
#16767 = CARTESIAN_POINT ( 'NONE',  ( 210.2301280605339855, 25.81350000000000477, -7.937500000000000000 ) ) ;
#16768 = CARTESIAN_POINT ( 'NONE',  ( 113.8294273123088374, -42.50220367264088139, 59.69586902018298247 ) ) ;
#16769 = CARTESIAN_POINT ( 'NONE',  ( 0.000000000000000000, 127.0000000000000000, -103.1875000000000000 ) ) ;
#16770 = CARTESIAN_POINT ( 'NONE',  ( -77.89700433585372252, 82.54999999999999716, 59.93649209371516662 ) ) ;
#16771 = DIRECTION ( 'NONE',  ( 0.000000000000000000, -1.000000000000000000, 0.000000000000000000 ) ) ;
#16772 = CIRCLE ( 'NONE', #29876, 13.44999999999999396 ) ;
#16773 = CARTESIAN_POINT ( 'NONE',  ( 104.6438654950096350, -47.53759819287119370, 23.38895860924494841 ) ) ;
#16774 = CARTESIAN_POINT ( 'NONE',  ( 68.91674821478504498, 82.54999999999999716, -68.91674821478385127 ) ) ;
#16775 = VERTEX_POINT ( 'NONE', #32021 ) ;
#16776 = DIRECTION ( 'NONE',  ( 0.000000000000000000, 1.000000000000000000, 0.000000000000000000 ) ) ;
#16777 = EDGE_LOOP ( 'NONE', ( #49209, #1265, #63031, #32085 ) ) ;
#16778 = CARTESIAN_POINT ( 'NONE',  ( 114.1102230946791707, -44.52199131239810015, 129.1613395616249704 ) ) ;
#16779 = CARTESIAN_POINT ( 'NONE',  ( 79.32178306374994747, -21.37853523628605501, 1.709393643969079113 ) ) ;
#16780 = VERTEX_POINT ( 'NONE', #68349 ) ;
#16781 = AXIS2_PLACEMENT_3D ( 'NONE', #4640, #19170, #18262 ) ;
#16782 = ORIENTED_EDGE ( 'NONE', *, *, #70207, .F. ) ;
#16783 = CARTESIAN_POINT ( 'NONE',  ( 103.1875000000000000, 127.0000000000000000, 3.602774393244745134E-13 ) ) ;
#16784 = CARTESIAN_POINT ( 'NONE',  ( 71.25614885437424562, -84.12815644128085069, 396.9756252759102040 ) ) ;
#16785 = CARTESIAN_POINT ( 'NONE',  ( 111.8874393434638250, -45.23954810143646910, 212.9870538473399506 ) ) ;
#16786 = CARTESIAN_POINT ( 'NONE',  ( 80.06648329127401098, -41.22944715994105280, 8.225625275910942946 ) ) ;
#16787 = CARTESIAN_POINT ( 'NONE',  ( 143.7322224575774783, -140.5784730598227839, 246.8085536723579878 ) ) ;
#16788 = CARTESIAN_POINT ( 'NONE',  ( 106.5667039024470313, -100.3098201933445068, 2.217806855417892020 ) ) ;
#16789 = AXIS2_PLACEMENT_3D ( 'NONE', #11634, #53821, #52039 ) ;
#16790 = EDGE_CURVE ( 'NONE', #36098, #54865, #61074, .T. ) ;
#16791 = CARTESIAN_POINT ( 'NONE',  ( 116.7270850375765576, -31.35852969783502786, 25.24229194257798881 ) ) ;
#16792 = PLANE ( 'NONE',  #71172 ) ;
#16793 = ORIENTED_EDGE ( 'NONE', *, *, #69893, .F. ) ;
#16794 = CARTESIAN_POINT ( 'NONE',  ( 103.2823872499383668, -27.47306433781803037, 171.3852924192453884 ) ) ;
#16795 = CARTESIAN_POINT ( 'NONE',  ( 63.06670390244641311, -24.92844715994017335, 180.4678068554151196 ) ) ;
#16796 = VERTEX_POINT ( 'NONE', #32916 ) ;
#16797 = CIRCLE ( 'NONE', #28385, 2.750000000000002665 ) ;
#16798 = CARTESIAN_POINT ( 'NONE',  ( 0.000000000000000000, 8.255000000000000782, 0.000000000000000000 ) ) ;
#16799 = CARTESIAN_POINT ( 'NONE',  ( 99.04384646079246579, -42.84093120032608226, 112.8445491430621246 ) ) ;
#16801 = AXIS2_PLACEMENT_3D ( 'NONE', #86156, #51163, #66130 ) ;
#16800 = CARTESIAN_POINT ( 'NONE',  ( 96.79426660377257008, -34.87310936442964504, 241.1841967044819626 ) ) ;
#16802 = SURFACE_STYLE_FILL_AREA ( #58127 ) ;
#16803 = FACE_BOUND ( 'NONE', #83057, .T. ) ;
#16804 = DIRECTION ( 'NONE',  ( -0.7071067811865476838, -0.7071067811865473507, 0.000000000000000000 ) ) ;
#16805 = CARTESIAN_POINT ( 'NONE',  ( 108.9266419529017327, -28.39302457734394736, 224.3238483995049819 ) ) ;
#16807 = CARTESIAN_POINT ( 'NONE',  ( 115.5559444348970857, -42.74257571503945741, 49.33562527591095659 ) ) ;
#16806 = LINE ( 'NONE', #66267, #85323 ) ;
#16808 = CARTESIAN_POINT ( 'NONE',  ( 113.3231070055411323, 69.11259796942169942, 64.82881333974782478 ) ) ;
#16809 = CARTESIAN_POINT ( 'NONE',  ( 117.2063690954211808, -34.12380291655402687, 124.0270538473399426 ) ) ;
#16810 = ORIENTED_EDGE ( 'NONE', *, *, #89292, .T. ) ;
#16812 = EDGE_CURVE ( 'NONE', #61339, #30803, #33821, .T. ) ;
#16811 = CARTESIAN_POINT ( 'NONE',  ( 132.9421938897428674, -21.23922437001909103, 8.028287874532244572 ) ) ;
#16813 = ORIENTED_EDGE ( 'NONE', *, *, #72500, .F. ) ;
#16814 = CARTESIAN_POINT ( 'NONE',  ( 97.33784129700110554, -34.07106458011696759, 67.11479194670231152 ) ) ;
#16815 = EDGE_CURVE ( 'NONE', #75367, #51539, #67207, .T. ) ;
#16816 = CARTESIAN_POINT ( 'NONE',  ( 103.3429861031523842, -27.44848569022927975, 276.3800890687926994 ) ) ;
#16817 = ORIENTED_EDGE ( 'NONE', *, *, #88605, .T. ) ;
#16818 = DIRECTION ( 'NONE',  ( 1.000000000000000078E-15, 1.000000000000000083E-30, -1.000000000000000000 ) ) ;
#16819 = ORIENTED_EDGE ( 'NONE', *, *, #14209, .T. ) ;
#16820 = DIRECTION ( 'NONE',  ( 0.000000000000000000, 1.000000000000000000, 0.000000000000000000 ) ) ;
#16821 = CARTESIAN_POINT ( 'NONE',  ( 164.9667039024459996, -28.27351298637401200, -5.074374724088000832 ) ) ;
#16823 = CIRCLE ( 'NONE', #66132, 1.000000000000000888 ) ;
#16822 = PLANE ( 'NONE',  #46642 ) ;
#16824 = ORIENTED_EDGE ( 'NONE', *, *, #45758, .T. ) ;
#16825 = CARTESIAN_POINT ( 'NONE',  ( 104.2079940790944477, -25.20282339889105927, 90.26991099019693365 ) ) ;
#16826 = AXIS2_PLACEMENT_3D ( 'NONE', #41735, #29032, #28111 ) ;
#16827 = CIRCLE ( 'NONE', #3781, 0.5000000000000004441 ) ;
#16828 = SURFACE_STYLE_USAGE ( .BOTH. , #59024 ) ;
#16829 = DIRECTION ( 'NONE',  ( 6.524622321627019585E-16, 3.741823817616790462E-31, 1.000000000000000000 ) ) ;
#16830 = LINE ( 'NONE', #44510, #75647 ) ;
#16831 = CARTESIAN_POINT ( 'NONE',  ( -446.0240000000000009, 93.66249999999999432, 11.11250000000040217 ) ) ;
#16832 = ORIENTED_EDGE ( 'NONE', *, *, #77825, .T. ) ;
#16833 = B_SPLINE_CURVE_WITH_KNOTS ( 'NONE', 3,
 ( #62023, #89757, #69303, #251, #9316, #19145, #78818, #29762, #43814, #9760, #11884, #16578, #5063, #53172, #80941, #39572, #37463, #60458 ),
 .UNSPECIFIED., .F., .F.,
 ( 4, 2, 2, 2, 2, 2, 2, 2, 4 ),
 ( 0.4999874473045213263, 0.5624890163914562091, 0.6249905854783910364, 0.6874921545653258637, 0.7499937236522606909, 0.8124952927391955182, 0.8749968618261303455, 0.9374984309130651727, 1.000000000000000000 ),
 .UNSPECIFIED. ) ;
#16834 = CYLINDRICAL_SURFACE ( 'NONE', #37358, 12.60000000000000142 ) ;
#16835 = DIRECTION ( 'NONE',  ( 4.299999999999999979E-14, -1.000000000000000000, 4.400000000000000367E-29 ) ) ;
#16836 = DIRECTION ( 'NONE',  ( 0.5773502691896258421, -0.5773502691896255090, -0.5773502691896258421 ) ) ;
#16838 = DIRECTION ( 'NONE',  ( 0.000000000000000000, 1.000000000000000000, 0.000000000000000000 ) ) ;
#16837 = LINE ( 'NONE', #79975, #5908 ) ;
#16839 = DIRECTION ( 'NONE',  ( -0.7071067811865516806, 0.7071067811865434649, -7.071067811865511818E-16 ) ) ;
#16840 = AXIS2_PLACEMENT_3D ( 'NONE', #50348, #8592, #84460 ) ;
#16841 = ORIENTED_EDGE ( 'NONE', *, *, #12576, .T. ) ;
#16842 = VECTOR ( 'NONE', #49989, 1000.000000000000000 ) ;
#16843 = DIRECTION ( 'NONE',  ( 1.000000000000000000, -3.885780586188044357E-13, 0.000000000000000000 ) ) ;
#16844 = ADVANCED_FACE ( 'NONE', ( #46079 ), #52870, .F. ) ;
#16845 = CARTESIAN_POINT ( 'NONE',  ( 98.25516505653069999, -40.97492784622581041, 167.6841967044819626 ) ) ;
#16847 = ORIENTED_EDGE ( 'NONE', *, *, #88739, .T. ) ;
#16846 = CARTESIAN_POINT ( 'NONE',  ( 51.06648329127330044, -0.7548456658612000547, 333.4006252759120343 ) ) ;
#16848 = CARTESIAN_POINT ( 'NONE',  ( 111.8651074766111293, -28.16866562884743885, 30.66991099019594813 ) ) ;
#16849 = DIRECTION ( 'NONE',  ( 0.7071067811864980568, 0.7071067811865969777, 0.000000000000000000 ) ) ;
#16850 = CARTESIAN_POINT ( 'NONE',  ( 20.03715912545830236, -46.82818131006180096, 300.4678068554150059 ) ) ;
#16851 = FACE_OUTER_BOUND ( 'NONE', #23170, .T. ) ;
#16852 = ORIENTED_EDGE ( 'NONE', *, *, #44445, .T. ) ;
#16853 = CARTESIAN_POINT ( 'NONE',  ( 136.8164832912739826, -18.72944715994099951, 3.101481641215532825 ) ) ;
#16854 = B_SPLINE_CURVE_WITH_KNOTS ( 'NONE', 3,
 ( #75418, #60418, #47683, #13192, #33179, #60877, #88608, #47234, #26364, #54033, #40875, #32725, #81792, #6364, #34055, #73615, #61759, #19545, #88163, #25022, #11393, #11846, #39087, #66798, #4583, #25465, #49017, #22251, #84490, #62670, #48568, #55382, #70390, #77211, #43105, #445 ),
 .UNSPECIFIED., .F., .F.,
 ( 4, 2, 2, 2, 2, 2, 2, 2, 2, 2, 2, 2, 2, 2, 2, 2, 2, 4 ),
 ( 0.01497400908950941197, 0.01590963194845458270, 0.01684525480739975517, 0.01778087766634492417, 0.01871650052529009664, 0.01965212338423526911, 0.02058774624318043811, 0.02152336910212561405, 0.02199118053159819508, 0.02245899196107077611, 0.02339461482001610471, 0.02433023767896143330, 0.02526586053790676190, 0.02620148339685209049, 0.02713710625579741909, 0.02807272911474275115, 0.02900835197368807974, 0.02994397483263340834 ),
 .UNSPECIFIED. ) ;
#16855 = CARTESIAN_POINT ( 'NONE',  ( 114.9950743857441608, -30.04541929558963886, 224.3718157521019521 ) ) ;
#16856 = VERTEX_POINT ( 'NONE', #32463 ) ;
#16857 = ORIENTED_EDGE ( 'NONE', *, *, #14483, .T. ) ;
#16858 = CARTESIAN_POINT ( 'NONE',  ( 104.2245914675057321, -27.77399204033938318, 201.7406309249449521 ) ) ;
#16859 = CARTESIAN_POINT ( 'NONE',  ( 75.31670390244798341, -67.87844715994100397, 84.20080685541500998 ) ) ;
#16860 = EDGE_CURVE ( 'NONE', #78803, #48612, #88805, .T. ) ;
#16861 = CARTESIAN_POINT ( 'NONE',  ( 104.8770057419572908, -45.34735396192071732, 43.81015473446897346 ) ) ;
#16862 = CARTESIAN_POINT ( 'NONE',  ( -87.44839512528793080, 93.33885111288432768, 96.94208673523014852 ) ) ;
#16863 = DIRECTION ( 'NONE',  ( -0.000000000000000000, 1.000000000000000000, 0.000000000000000000 ) ) ;
#16864 = EDGE_CURVE ( 'NONE', #137, #88945, #53334, .T. ) ;
#16865 = DIRECTION ( 'NONE',  ( -1.000000000000000078E-15, 1.000000000000000083E-30, 1.000000000000000000 ) ) ;
#16866 = ORIENTED_EDGE ( 'NONE', *, *, #13032, .T. ) ;
#16867 = DIRECTION ( 'NONE',  ( 0.000000000000000000, 0.000000000000000000, 1.000000000000000000 ) ) ;
#16868 = LINE ( 'NONE', #3244, #22728 ) ;
#16869 = ORIENTED_EDGE ( 'NONE', *, *, #42244, .T. ) ;
#16870 = CARTESIAN_POINT ( 'NONE',  ( 99.34937008002594894, -28.84845824588779095, 270.7051490854348685 ) ) ;
#16871 = CARTESIAN_POINT ( 'NONE',  ( 3.284115064261067030, 94.82510599261892992, 118.5111763271416692 ) ) ;
#16872 = ORIENTED_EDGE ( 'NONE', *, *, #56541, .T. ) ;
#16873 = EDGE_CURVE ( 'NONE', #71994, #77969, #57035, .T. ) ;
#16874 = EDGE_CURVE ( 'NONE', #6482, #68461, #8214, .T. ) ;
#16875 = CARTESIAN_POINT ( 'NONE',  ( -74.36911441044730964, 82.54999999999999716, 92.32962665258534685 ) ) ;
#16876 = CARTESIAN_POINT ( 'NONE',  ( 114.6444261855608744, -117.4034471599418055, -11.78219314458159239 ) ) ;
#16877 = CARTESIAN_POINT ( 'NONE',  ( 152.0368932755772562, -23.42844715993587812, 193.9678068554149775 ) ) ;
#16878 = AXIS2_PLACEMENT_3D ( 'NONE', #59867, #46231, #18546 ) ;
#16879 = EDGE_CURVE ( 'NONE', #42339, #83669, #48770, .T. ) ;
#16880 = CARTESIAN_POINT ( 'NONE',  ( 115.8115096128641284, -32.27542772465451293, 40.20133956162496958 ) ) ;
#16882 = CYLINDRICAL_SURFACE ( 'NONE', #18098, 12.69999999999998863 ) ;
#16881 = AXIS2_PLACEMENT_3D ( 'NONE', #11950, #39635, #26024 ) ;
#16883 = VERTEX_POINT ( 'NONE', #34260 ) ;
#16884 = AXIS2_PLACEMENT_3D ( 'NONE', #47954, #74791, #33897 ) ;
#16885 = CARTESIAN_POINT ( 'NONE',  ( 115.6469432611725665, -28.48403513818922761, 35.43562527591098643 ) ) ;
#16886 = AXIS2_PLACEMENT_3D ( 'NONE', #67461, #18871, #89722 ) ;
#16887 = DIRECTION ( 'NONE',  ( 1.000000000000000078E-15, 1.000000000000000083E-30, -1.000000000000000000 ) ) ;
#16888 = AXIS2_PLACEMENT_3D ( 'NONE', #62210, #21792, #35390 ) ;
#16889 = EDGE_CURVE ( 'NONE', #46304, #54672, #49770, .T. ) ;
#16890 = CARTESIAN_POINT ( 'NONE',  ( 117.5190927476815119, -36.54584727635032237, 288.8413395616252615 ) ) ;
#16891 = VERTEX_POINT ( 'NONE', #68794 ) ;
#16892 = CARTESIAN_POINT ( 'NONE',  ( 78.76282073104860615, -39.15113447711711103, 7.957506268071020017 ) ) ;
#16893 = CYLINDRICAL_SURFACE ( 'NONE', #31196, 118.5560000000000116 ) ;
#16894 = CARTESIAN_POINT ( 'NONE',  ( 107.0664832912739968, -36.72944715994100306, 287.6356252759109680 ) ) ;
#16895 = EDGE_CURVE ( 'NONE', #37024, #67223, #6561, .T. ) ;
#16896 = CARTESIAN_POINT ( 'NONE',  ( 109.1833626410332130, -45.12109460632434121, 90.60332846482899072 ) ) ;
#16897 = CARTESIAN_POINT ( 'NONE',  ( 103.6314581395739793, -26.19921411638948427, 206.3394347997209763 ) ) ;
#16898 = DIRECTION ( 'NONE',  ( 1.000000000000000078E-15, -1.000000000000000000, 0.000000000000000000 ) ) ;
#16899 = DIRECTION ( 'NONE',  ( -1.000000000000000000, 0.000000000000000000, 0.000000000000000000 ) ) ;
#16900 = EDGE_LOOP ( 'NONE', ( #86491, #65153, #66775, #32797 ) ) ;
#16901 = AXIS2_PLACEMENT_3D ( 'NONE', #49610, #71871, #15111 ) ;
#16902 = CARTESIAN_POINT ( 'NONE',  ( 51.23005224011772185, -33.89581943344268211, 237.4678068554150059 ) ) ;
#16903 = EDGE_LOOP ( 'NONE', ( #17615, #19858, #43502, #81109 ) ) ;
#16904 = ORIENTED_EDGE ( 'NONE', *, *, #41190, .F. ) ;
#16905 = CARTESIAN_POINT ( 'NONE',  ( 165.9667039024478754, -28.27351298636806831, 313.9678068554149490 ) ) ;
#16906 = ORIENTED_EDGE ( 'NONE', *, *, #60403, .T. ) ;
#16907 = ORIENTED_EDGE ( 'NONE', *, *, #36377, .F. ) ;
#16908 = DIRECTION ( 'NONE',  ( 1.000000000000000078E-15, -1.000000000000000083E-30, -1.000000000000000000 ) ) ;
#16909 = VECTOR ( 'NONE', #53092, 1000.000000000000000 ) ;
#16910 = CARTESIAN_POINT ( 'NONE',  ( 103.2785244713985833, -27.47464473206936830, 41.38562443853131612 ) ) ;
#16911 = CARTESIAN_POINT ( 'NONE',  ( 103.4202683135912650, -45.01906637089264507, 131.6571817328389784 ) ) ;
#16912 = CARTESIAN_POINT ( 'NONE',  ( 106.6048964044850607, -25.63891871564037928, 40.09753003781596448 ) ) ;
#16913 = ADVANCED_FACE ( 'NONE', ( #54680 ), #8362, .F. ) ;
#16914 = ADVANCED_FACE ( 'NONE', ( #14283 ), #41957, .T. ) ;
#16915 = FACE_OUTER_BOUND ( 'NONE', #33808, .T. ) ;
#16916 = ORIENTED_EDGE ( 'NONE', *, *, #48847, .F. ) ;
#16917 = EDGE_CURVE ( 'NONE', #14173, #47689, #14736, .T. ) ;
#16918 = CARTESIAN_POINT ( 'NONE',  ( 116.0743685831884733, -32.33849391669360784, 135.1874756336685834 ) ) ;
#16919 = EDGE_LOOP ( 'NONE', ( #51925, #4766, #8568 ) ) ;
#16920 = LINE ( 'NONE', #85972, #7278 ) ;
#16921 = EDGE_CURVE ( 'NONE', #88540, #20676, #69692, .T. ) ;
#16922 = DIRECTION ( 'NONE',  ( 0.000000000000000000, 0.000000000000000000, 1.000000000000000000 ) ) ;
#16923 = DIRECTION ( 'NONE',  ( -1.000000000000000000, 0.000000000000000000, 0.000000000000000000 ) ) ;
#16924 = LINE ( 'NONE', #85977, #42176 ) ;
#16925 = ORIENTED_EDGE ( 'NONE', *, *, #29847, .F. ) ;
#16926 = UNCERTAINTY_MEASURE_WITH_UNIT (LENGTH_MEASURE( 1.000000000000000082E-05 ), #37244, 'distance_accuracy_value', 'NONE');
#16927 = CARTESIAN_POINT ( 'NONE',  ( 115.3236443966936235, -45.23002221789283084, 268.1899109901965517 ) ) ;
#16928 = CARTESIAN_POINT ( 'NONE',  ( 100.4516903307928573, -27.81642228345825885, 31.59657765686396758 ) ) ;
#16929 = FACE_OUTER_BOUND ( 'NONE', #31119, .T. ) ;
#16931 = CARTESIAN_POINT ( 'NONE',  ( 68.86296241111062955, -139.1369832984686354, 246.6149457656773052 ) ) ;
#16930 = CARTESIAN_POINT ( 'NONE',  ( 152.0368932755770288, -23.42844715993588522, 300.4678068554149490 ) ) ;
#16932 = CARTESIAN_POINT ( 'NONE',  ( 105.6962374661776209, -25.35223018209148194, 323.2475121285344244 ) ) ;
#16933 = CARTESIAN_POINT ( 'NONE',  ( 107.0664832912739399, -36.72944715994096754, 298.1356252759109680 ) ) ;
#16934 = CARTESIAN_POINT ( 'NONE',  ( 132.1198940698338902, -38.67261125154126233, 7.590611884332613357 ) ) ;
#16935 = CARTESIAN_POINT ( 'NONE',  ( 116.3212776292296127, -32.94146857471318413, 287.6356252759109680 ) ) ;
#16936 = PLANE ( 'NONE',  #12944 ) ;
#16937 = CARTESIAN_POINT ( 'NONE',  ( 138.0667039024479550, -26.72944715994091069, 239.5838068554170377 ) ) ;
#16938 = DIRECTION ( 'NONE',  ( 1.000000000000000078E-15, -1.000000000000000000, 0.000000000000000000 ) ) ;
#16939 = CARTESIAN_POINT ( 'NONE',  ( 97.75295786963341982, -40.54146432227403807, 11.63562527591094309 ) ) ;
#16940 = CARTESIAN_POINT ( 'NONE',  ( 97.95649862111255857, -30.46988169760521359, 161.8594347997199918 ) ) ;
#16941 = CARTESIAN_POINT ( 'NONE',  ( 110.8022603587792219, -46.48553390388831019, 58.86705384733998159 ) ) ;
#16942 = VECTOR ( 'NONE', #32503, 1000.000000000000000 ) ;
#16944 = DIRECTION ( 'NONE',  ( 0.000000000000000000, -1.000000000000000000, 0.000000000000000000 ) ) ;
#16943 = DIRECTION ( 'NONE',  ( 1.000000000000000078E-15, 1.000000000000000083E-30, -1.000000000000000000 ) ) ;
#16945 = PLANE ( 'NONE',  #49427 ) ;
#16946 = VECTOR ( 'NONE', #66515, 1000.000000000000000 ) ;
#16947 = AXIS2_PLACEMENT_3D ( 'NONE', #48903, #83454, #19884 ) ;
#16948 = ORIENTED_EDGE ( 'NONE', *, *, #50705, .T. ) ;
#16949 = DIRECTION ( 'NONE',  ( 1.000000000000000078E-15, -1.000000000000000083E-30, -1.000000000000000000 ) ) ;
#16950 = ORIENTED_EDGE ( 'NONE', *, *, #30512, .F. ) ;
#16951 = CARTESIAN_POINT ( 'NONE',  ( 96.07333748454176714, -35.06730156692550793, 67.20705384733894050 ) ) ;
#16953 = VERTEX_POINT ( 'NONE', #1096 ) ;
#16952 = CARTESIAN_POINT ( 'NONE',  ( 116.8189785850517524, -34.16011448583248722, 189.0314799851472287 ) ) ;
#16954 = DIRECTION ( 'NONE',  ( 1.327617956749545812E-15, -0.7071067811865480168, -0.7071067811865470176 ) ) ;
#16955 = CARTESIAN_POINT ( 'NONE',  ( 114.9613132280021830, -29.02649429439055595, 190.4537205140059655 ) ) ;
#16956 = FACE_OUTER_BOUND ( 'NONE', #3189, .T. ) ;
#16957 = CARTESIAN_POINT ( 'NONE',  ( 98.15100683351592181, -41.26167086457207489, 146.7007424152079409 ) ) ;
#16958 = DIRECTION ( 'NONE',  ( 0.000000000000000000, 0.000000000000000000, -1.000000000000000000 ) ) ;
#16959 = LINE ( 'NONE', #79643, #29870 ) ;
#16960 = CARTESIAN_POINT ( 'NONE',  ( 146.9537589533094888, -137.3494371116456989, 246.8018929578719849 ) ) ;
#16961 = LINE ( 'NONE', #78314, #79076 ) ;
#16963 = CARTESIAN_POINT ( 'NONE',  ( 109.0694692412632492, -27.15596902575777349, 139.9127681330539872 ) ) ;
#16962 = AXIS2_PLACEMENT_3D ( 'NONE', #18680, #67270, #46359 ) ;
#16964 = ORIENTED_EDGE ( 'NONE', *, *, #19038, .T. ) ;
#16965 = VERTEX_POINT ( 'NONE', #89698 ) ;
#16966 = CARTESIAN_POINT ( 'NONE',  ( 97.22447099779657265, -34.58340453033963513, 102.5872975916109482 ) ) ;
#16967 = CARTESIAN_POINT ( 'NONE',  ( 72.31648329127401098, -45.62589376934781882, 14.92562527591093691 ) ) ;
#16968 = ADVANCED_FACE ( 'NONE', ( #62859, #47876 ), #42407, .T. ) ;
#16970 = CARTESIAN_POINT ( 'NONE',  ( 100.8961411191535973, 120.6499999999999915, 3.968750000000400124 ) ) ;
#16969 = CARTESIAN_POINT ( 'NONE',  ( 97.32398421004042177, -35.86507053846868587, 227.2556252759109725 ) ) ;
#16971 = DIRECTION ( 'NONE',  ( -1.000000000000000078E-15, -1.000000000000000083E-30, 1.000000000000000000 ) ) ;
#16972 = LINE ( 'NONE', #44657, #43756 ) ;
#16973 = ADVANCED_FACE ( 'NONE', ( #7462 ), #15174, .T. ) ;
#16974 = CARTESIAN_POINT ( 'NONE',  ( 118.5559323284754782, 69.85063172184841562, 0.8489616598202707198 ) ) ;
#16975 = ADVANCED_FACE ( 'NONE', ( #48314 ), #35150, .T. ) ;
#16976 = CYLINDRICAL_SURFACE ( 'NONE', #864, 4.750000000000000888 ) ;
#16977 = FACE_OUTER_BOUND ( 'NONE', #30134, .T. ) ;
#16978 = CARTESIAN_POINT ( 'NONE',  ( 12.17775809732705028, 79.28909450904312450, 117.9289698252223815 ) ) ;
#16979 = CARTESIAN_POINT ( 'NONE',  ( 102.0615167388204725, -46.55869598106830409, 172.2137205140059564 ) ) ;
#16980 = VERTEX_POINT ( 'NONE', #56029 ) ;
#16981 = ORIENTED_EDGE ( 'NONE', *, *, #9718, .F. ) ;
#16982 = ADVANCED_FACE ( 'NONE', ( #22003 ), #83777, .T. ) ;
#16983 = ADVANCED_FACE ( 'NONE', ( #34712 ), #70589, .F. ) ;
#16984 = DIRECTION ( 'NONE',  ( -4.237773401492740281E-14, 1.000000000000000000, 0.000000000000000000 ) ) ;
#16985 = CARTESIAN_POINT ( 'NONE',  ( 77.31648329127399677, -18.72944715994106346, 3.101481641215480867 ) ) ;
#16986 = CARTESIAN_POINT ( 'NONE',  ( -492.0614999999999668, 93.66249999999999432, 90.48749999999999716 ) ) ;
#16987 = CARTESIAN_POINT ( 'NONE',  ( 107.0667039024470313, -104.2784471599420755, -19.78219314458201694 ) ) ;
#16988 = AXIS2_PLACEMENT_3D ( 'NONE', #53481, #18539, #31724 ) ;
#16989 = AXIS2_PLACEMENT_3D ( 'NONE', #36920, #27857, #21513 ) ;
#16990 = EDGE_CURVE ( 'NONE', #46739, #78957, #68650, .T. ) ;
#16991 = LINE ( 'NONE', #58742, #40754 ) ;
#16992 = EDGE_CURVE ( 'NONE', #44371, #44076, #20650, .T. ) ;
#16993 = CARTESIAN_POINT ( 'NONE',  ( 100.0080109101350985, -27.21007462382121744, 185.5841967044829630 ) ) ;
#16994 = DIRECTION ( 'NONE',  ( 0.000000000000000000, 0.000000000000000000, -1.000000000000000000 ) ) ;
#16995 = ORIENTED_EDGE ( 'NONE', *, *, #30084, .T. ) ;
#16997 = ORIENTED_EDGE ( 'NONE', *, *, #62518, .T. ) ;
#16996 = ORIENTED_EDGE ( 'NONE', *, *, #23217, .T. ) ;
#16998 = CARTESIAN_POINT ( 'NONE',  ( -5.635505087355097587, 71.13841253056517644, 118.4244851085658468 ) ) ;
#16999 = LINE ( 'NONE', #31058, #11551 ) ;
#17000 = DIRECTION ( 'NONE',  ( -1.000000000000000078E-15, 1.000000000000000000, 0.000000000000000000 ) ) ;
#17001 = EDGE_CURVE ( 'NONE', #64475, #75853, #55572, .T. ) ;
#17002 = CARTESIAN_POINT ( 'NONE',  ( 113.3129409812876389, -28.82675956000495887, 270.9758690201826425 ) ) ;
#17003 = CARTESIAN_POINT ( 'NONE',  ( 108.3334472470058785, -46.73485946926888346, 272.6772918751394172 ) ) ;
#17004 = ORIENTED_EDGE ( 'NONE', *, *, #8057, .T. ) ;
#17005 = CIRCLE ( 'NONE', #40192, 9.425000000000000711 ) ;
#17006 = AXIS2_PLACEMENT_3D ( 'NONE', #48469, #41668, #82607 ) ;
#17007 = CARTESIAN_POINT ( 'NONE',  ( 115.0813998565176774, -41.07721658520456742, 9.635625275910943088 ) ) ;
#17008 = DIRECTION ( 'NONE',  ( 4.299999999999999979E-14, -1.000000000000000000, 0.000000000000000000 ) ) ;
#17009 = ORIENTED_EDGE ( 'NONE', *, *, #23364, .T. ) ;
#17010 = EDGE_LOOP ( 'NONE', ( #66539, #87674, #88983, #65753 ) ) ;
#17011 = AXIS2_PLACEMENT_3D ( 'NONE', #30998, #86431, #11457 ) ;
#17012 = VECTOR ( 'NONE', #68789, 1000.000000000000000 ) ;
#17013 = CARTESIAN_POINT ( 'NONE',  ( 100.8875017264671783, -44.70024944885620499, 112.0523634285323453 ) ) ;
#17014 = CIRCLE ( 'NONE', #89568, 1.000000000002049694 ) ;
#17015 = EDGE_LOOP ( 'NONE', ( #24708, #77608, #40015, #80000, #222, #58409 ) ) ;
#17016 = ORIENTED_EDGE ( 'NONE', *, *, #65216, .F. ) ;
#17017 = CARTESIAN_POINT ( 'NONE',  ( 101.7664832247249365, -29.99442739451795958, 15.02956268521998773 ) ) ;
#17018 = CARTESIAN_POINT ( 'NONE',  ( 98.14931896820920088, -31.28605259387051518, 170.8899109901960003 ) ) ;
#17019 = CARTESIAN_POINT ( 'NONE',  ( 114.5119312840560184, -28.59475203354325501, 154.4746728949589851 ) ) ;
#17020 = CARTESIAN_POINT ( 'NONE',  ( 72.96458098368701428, 117.4749999999999943, -72.96458098368670164 ) ) ;
#17021 = CARTESIAN_POINT ( 'NONE',  ( 115.0547525607699697, -30.03093676393617173, 265.3813395616251682 ) ) ;
#17022 = LINE ( 'NONE', #31082, #26869 ) ;
#17023 = CARTESIAN_POINT ( 'NONE',  ( 68.20286926358554069, -119.2990514172772833, 247.4783998280180128 ) ) ;
#17024 = CARTESIAN_POINT ( 'NONE',  ( -130.5246035444015718, 70.17666187254643262, -2.891673250712901044 ) ) ;
#17025 = ORIENTED_EDGE ( 'NONE', *, *, #24549, .F. ) ;
#17026 = ADVANCED_FACE ( 'NONE', ( #65792 ), #73058, .T. ) ;
#17027 = VECTOR ( 'NONE', #6291, 1000.000000000000000 ) ;
#17028 = ORIENTED_EDGE ( 'NONE', *, *, #47415, .T. ) ;
#17029 = CIRCLE ( 'NONE', #28625, 6.557978799109520196 ) ;
#17030 = ADVANCED_FACE ( 'NONE', ( #4023 ), #3143, .T. ) ;
#17031 = CIRCLE ( 'NONE', #8410, 10.00000000000000711 ) ;
#17032 = CARTESIAN_POINT ( 'NONE',  ( 117.9946794957619431, -34.78331989172042427, 198.9546728949589749 ) ) ;
#17033 = EDGE_LOOP ( 'NONE', ( #77103, #1915 ) ) ;
#17034 = CARTESIAN_POINT ( 'NONE',  ( 117.0233241640237338, -39.93681227152024604, 158.5784824187679476 ) ) ;
#17035 = DIRECTION ( 'NONE',  ( 0.000000000000000000, -1.000000000000000000, 0.000000000000000000 ) ) ;
#17036 = DIRECTION ( 'NONE',  ( 0.000000000000000000, -1.682382052829014912E-15, -1.000000000000000000 ) ) ;
#17037 = CARTESIAN_POINT ( 'NONE',  ( 143.4594029887166471, -139.4935159556384860, 247.3653129605272056 ) ) ;
#17040 = CARTESIAN_POINT ( 'NONE',  ( 100.8736165617014677, -44.32606212243579336, 8.032768133052980986 ) ) ;
#17039 = DIRECTION ( 'NONE',  ( 0.000000000000000000, 0.000000000000000000, 1.000000000000000000 ) ) ;
#17038 = CARTESIAN_POINT ( 'NONE',  ( 183.5150000000000148, 52.73749999999999716, -62.78087104677060637 ) ) ;
#17041 = DIRECTION ( 'NONE',  ( -9.073094938289460781E-13, -1.000000000000000000, 0.000000000000000000 ) ) ;
#17042 = DIRECTION ( 'NONE',  ( 0.7071067811865453523, 0.7071067811865496822, 7.071067811865460542E-16 ) ) ;
#17043 = PLANE ( 'NONE',  #16474 ) ;
#17044 = CARTESIAN_POINT ( 'NONE',  ( 67.06670403371455791, -137.6620872545493341, 245.7334057579663238 ) ) ;
#17045 = DIRECTION ( 'NONE',  ( 1.000000000000000078E-15, -1.000000000000000083E-30, -1.000000000000000000 ) ) ;
#17046 = FACE_OUTER_BOUND ( 'NONE', #82432, .T. ) ;
#17048 = VERTEX_POINT ( 'NONE', #72632 ) ;
#17047 = CARTESIAN_POINT ( 'NONE',  ( 113.1460701246578680, -29.40654960323831801, 195.5838068554210452 ) ) ;
#17049 = CARTESIAN_POINT ( 'NONE',  ( 136.1031364520983686, -20.57950990141002379, 7.523361336352738959 ) ) ;
#17050 = CARTESIAN_POINT ( 'NONE',  ( 104.5572623809163701, -48.33710955716689028, 182.4070538473399665 ) ) ;
#17051 = CARTESIAN_POINT ( 'NONE',  ( 116.6747397658760832, -32.59390121112949856, 75.14991099019697174 ) ) ;
#17052 = CARTESIAN_POINT ( 'NONE',  ( 113.8273992703627044, -26.93653503804465288, 235.5956252759109759 ) ) ;
#17053 = LINE ( 'NONE', #58806, #88070 ) ;
#17054 = DIRECTION ( 'NONE',  ( -4.237773401492740281E-14, 1.000000000000000000, 0.000000000000000000 ) ) ;
#17056 = CARTESIAN_POINT ( 'NONE',  ( 97.86387113231445767, -40.64285381717150614, 37.64614471822871167 ) ) ;
#17055 = DIRECTION ( 'NONE',  ( 1.000000000000000000, 4.443626637970137948E-14, 0.000000000000000000 ) ) ;
#17057 = LINE ( 'NONE', #25194, #29102 ) ;
#17058 = PLANE ( 'NONE',  #1616 ) ;
#17059 = ORIENTED_EDGE ( 'NONE', *, *, #80815, .F. ) ;
#17060 = VECTOR ( 'NONE', #57485, 1000.000000000000000 ) ;
#17061 = CARTESIAN_POINT ( 'NONE',  ( 97.39135791878592840, -39.27877462570257450, 66.53211423348820119 ) ) ;
#17062 = ORIENTED_EDGE ( 'NONE', *, *, #29495, .T. ) ;
#17063 = ORIENTED_EDGE ( 'NONE', *, *, #66949, .T. ) ;
#17064 = CARTESIAN_POINT ( 'NONE',  ( 113.3421067344362996, -42.52364098839497331, 122.6552769709339827 ) ) ;
#17066 = VERTEX_POINT ( 'NONE', #4479 ) ;
#17065 = CARTESIAN_POINT ( 'NONE',  ( -4.087661814003488381, 94.58137602904392338, -130.4926000606902505 ) ) ;
#17067 = CARTESIAN_POINT ( 'NONE',  ( 104.1140010245780729, -46.70499295924809502, 103.3470538473389411 ) ) ;
#17068 = CARTESIAN_POINT ( 'NONE',  ( 0.000000000000000000, 61.59999999999999432, 0.000000000000000000 ) ) ;
#17069 = CARTESIAN_POINT ( 'NONE',  ( 77.54412859703477068, -17.63380991825937016, 7.053480412781051534 ) ) ;
#17070 = CARTESIAN_POINT ( 'NONE',  ( 0.000000000000000000, 1.270000000000000018, 24.63800000000000168 ) ) ;
#17071 = AXIS2_PLACEMENT_3D ( 'NONE', #26400, #47272, #38235 ) ;
#17072 = CARTESIAN_POINT ( 'NONE',  ( 110.8002668817294847, -46.40403677370081681, 17.85753003781598380 ) ) ;
#17073 = VERTEX_POINT ( 'NONE', #51708 ) ;
#17074 = ADVANCED_FACE ( 'NONE', ( #4921 ), #87155, .T. ) ;
#17075 = ORIENTED_EDGE ( 'NONE', *, *, #73566, .T. ) ;
#17076 = VERTEX_POINT ( 'NONE', #53024 ) ;
#17077 = AXIS2_PLACEMENT_3D ( 'NONE', #87659, #46291, #6323 ) ;
#17078 = PLANE ( 'NONE',  #54383 ) ;
#17079 = CARTESIAN_POINT ( 'NONE',  ( 73.06670390244801183, -50.82844715994100682, 198.9178068554149945 ) ) ;
#17080 = CARTESIAN_POINT ( 'NONE',  ( 99.09570908081879281, -30.55043174719083510, 116.8022919419756107 ) ) ;
#17081 = CARTESIAN_POINT ( 'NONE',  ( 24.79284581386643893, 127.0000000000000000, 106.1020876358972629 ) ) ;
#17082 = CARTESIAN_POINT ( 'NONE',  ( 210.5660000000000025, 52.73749999999999716, -44.45000000000000284 ) ) ;
#17083 = ADVANCED_FACE ( 'NONE', ( #25351 ), #62865, .T. ) ;
#17084 = DIRECTION ( 'NONE',  ( -0.7071067811865360264, 0.000000000000000000, 0.7071067811865588970 ) ) ;
#17085 = ADVANCED_FACE ( 'NONE', ( #18542 ), #59423, .F. ) ;
#17086 = LINE ( 'NONE', #17530, #35885 ) ;
#17087 = EDGE_CURVE ( 'NONE', #82750, #52712, #24483, .T. ) ;
#17088 = CARTESIAN_POINT ( 'NONE',  ( -7.079787210858614621, 93.09356445001880331, 130.3638972052411589 ) ) ;
#17089 = CARTESIAN_POINT ( 'NONE',  ( 116.7246412902989903, -32.86309880586077270, 54.12991099019698282 ) ) ;
#17090 = VERTEX_POINT ( 'NONE', #46227 ) ;
#17091 = ORIENTED_EDGE ( 'NONE', *, *, #46147, .F. ) ;
#17092 = AXIS2_PLACEMENT_3D ( 'NONE', #35899, #8206, #43148 ) ;
#17093 = EDGE_CURVE ( 'NONE', #16780, #72546, #17223, .T. ) ;
#17094 = LINE ( 'NONE', #88822, #56013 ) ;
#17095 = FACE_OUTER_BOUND ( 'NONE', #15540, .T. ) ;
#17096 = VECTOR ( 'NONE', #69144, 1000.000000000000000 ) ;
#17097 = AXIS2_PLACEMENT_3D ( 'NONE', #40695, #88865, #34326 ) ;
#17098 = DIRECTION ( 'NONE',  ( 1.000000000000000000, 0.000000000000000000, 0.000000000000000000 ) ) ;
#17099 = CARTESIAN_POINT ( 'NONE',  ( 104.0433210460927000, -44.34148882339519560, 115.0938046553049503 ) ) ;
#17100 = ADVANCED_FACE ( 'NONE', ( #25811 ), #61126, .F. ) ;
#17101 = CARTESIAN_POINT ( 'NONE',  ( 97.12565827820864683, -37.99761304849175758, 96.42736898879877572 ) ) ;
#17102 = EDGE_CURVE ( 'NONE', #84365, #88986, #68044, .T. ) ;
#17103 = DIRECTION ( 'NONE',  ( 1.000000000000000000, 0.000000000000000000, 0.000000000000000000 ) ) ;
#17104 = ORIENTED_EDGE ( 'NONE', *, *, #75206, .T. ) ;
#17105 = EDGE_LOOP ( 'NONE', ( #35930, #23139 ) ) ;
#17106 = CYLINDRICAL_SURFACE ( 'NONE', #83061, 2.000000000000001776 ) ;
#17107 = ORIENTED_EDGE ( 'NONE', *, *, #70642, .F. ) ;
#17108 = ORIENTED_EDGE ( 'NONE', *, *, #17802, .T. ) ;
#17109 = EDGE_CURVE ( 'NONE', #274, #45431, #89008, .T. ) ;
#17110 = CARTESIAN_POINT ( 'NONE',  ( 113.8438844162330810, -30.22226962059244215, 185.8549166392299696 ) ) ;
#17111 = DIRECTION ( 'NONE',  ( -0.000000000000000000, -0.000000000000000000, -1.000000000000000000 ) ) ;
#17112 = VECTOR ( 'NONE', #36435, 1000.000000000000000 ) ;
#17113 = CARTESIAN_POINT ( 'NONE',  ( 95.28708132950120557, -38.28245711228485959, 147.4299109901969871 ) ) ;
#17114 = LINE ( 'NONE', #79801, #86443 ) ;
#17115 = VECTOR ( 'NONE', #63141, 1000.000000000000000 ) ;
#17116 = CARTESIAN_POINT ( 'NONE',  ( 104.4081006377808620, -46.45808913390618500, 83.36479194067089793 ) ) ;
#17117 = VERTEX_POINT ( 'NONE', #68937 ) ;
#17118 = EDGE_LOOP ( 'NONE', ( #46126, #80367 ) ) ;
#17119 = ORIENTED_EDGE ( 'NONE', *, *, #81628, .F. ) ;
#17120 = CARTESIAN_POINT ( 'NONE',  ( 114.9947780803761503, -40.19975936245594283, 206.3042808457819604 ) ) ;
#17121 = CARTESIAN_POINT ( 'NONE',  ( 116.2511270133230283, -31.75062363771698770, 69.22133956162495849 ) ) ;
#17122 = ORIENTED_EDGE ( 'NONE', *, *, #3577, .F. ) ;
#17123 = CARTESIAN_POINT ( 'NONE',  ( 117.3629797429381654, -38.21633193987523214, 28.71276813305395592 ) ) ;
#17124 = CARTESIAN_POINT ( 'NONE',  ( -3.686187674308976980, 145.6861876743087691, 113.8826257785461280 ) ) ;
#17125 = CARTESIAN_POINT ( 'NONE',  ( 70.06968321367156705, -140.6784088069870222, 245.5331728854790185 ) ) ;
#17126 = CARTESIAN_POINT ( 'NONE',  ( 156.5667039024485518, -48.82844715993568485, 173.2178068554149775 ) ) ;
#17127 = CARTESIAN_POINT ( 'NONE',  ( 108.2778103265350893, -47.71616603169876214, 153.6518157521009584 ) ) ;
#17128 = DIRECTION ( 'NONE',  ( -0.7071067811865580088, 0.000000000000000000, -0.7071067811865370256 ) ) ;
#17129 = EDGE_LOOP ( 'NONE', ( #79545, #85673, #55337, #5424 ) ) ;
#17130 = CARTESIAN_POINT ( 'NONE',  ( 194.0667039024475287, -24.92844715993407334, 180.4678068554150343 ) ) ;
#17131 = AXIS2_PLACEMENT_3D ( 'NONE', #40473, #68636, #26838 ) ;
#17132 = VERTEX_POINT ( 'NONE', #5370 ) ;
#17133 = FACE_OUTER_BOUND ( 'NONE', #47625, .T. ) ;
#17134 = DIRECTION ( 'NONE',  ( 0.000000000000000000, 1.000000000000000000, 0.000000000000000000 ) ) ;
#17135 = ADVANCED_FACE ( 'NONE', ( #48023 ), #34407, .T. ) ;
#17136 = VERTEX_POINT ( 'NONE', #27599 ) ;
#17137 = CIRCLE ( 'NONE', #25881, 7.937500000000000000 ) ;
#17138 = CARTESIAN_POINT ( 'NONE',  ( 50.88849390559499142, -32.11662333284530746, -5.074374724088000832 ) ) ;
#17139 = VECTOR ( 'NONE', #87096, 1000.000000000000000 ) ;
#17140 = LINE ( 'NONE', #45264, #78363 ) ;
#17141 = CARTESIAN_POINT ( 'NONE',  ( 109.9110735108787793, -46.79593677437021881, 72.79562527591099297 ) ) ;
#17142 = LINE ( 'NONE', #72552, #66341 ) ;
#17143 = DIRECTION ( 'NONE',  ( 0.000000000000000000, 1.000000000000000000, 0.000000000000000000 ) ) ;
#17144 = CARTESIAN_POINT ( 'NONE',  ( 107.0664832912739968, -36.72944715994100306, 9.635625275910941312 ) ) ;
#17145 = CARTESIAN_POINT ( 'NONE',  ( 115.8115096128642136, -32.27542772465447030, 44.20133956162592170 ) ) ;
#17147 = CARTESIAN_POINT ( 'NONE',  ( 107.5647246096319094, -47.74832088493814553, 188.6003871806729535 ) ) ;
#17146 = DIRECTION ( 'NONE',  ( 0.000000000000000000, 0.000000000000000000, 1.000000000000000000 ) ) ;
#17148 = CARTESIAN_POINT ( 'NONE',  ( 97.81170051792484799, -40.51743816602341752, 61.63542871443850402 ) ) ;
#17149 = DIRECTION ( 'NONE',  ( 0.000000000000000000, 0.000000000000000000, 1.000000000000000000 ) ) ;
#17150 = EDGE_LOOP ( 'NONE', ( #58977, #52125, #61979, #28480 ) ) ;
#17151 = CARTESIAN_POINT ( 'NONE',  ( 94.58945128933383728, -41.88441296220994303, 293.6356252759107974 ) ) ;
#17152 = VECTOR ( 'NONE', #15087, 1000.000000000000000 ) ;
#17153 = CARTESIAN_POINT ( 'NONE',  ( 1.451892259197136103E-14, 101.5999999999999943, -118.5560000000000116 ) ) ;
#17154 = CARTESIAN_POINT ( 'NONE',  ( 156.5667039024483813, -48.82844715993569196, 254.7178068554149490 ) ) ;
#17155 = VECTOR ( 'NONE', #32924, 1000.000000000000114 ) ;
#17156 = FACE_OUTER_BOUND ( 'NONE', #24997, .T. ) ;
#17157 = ADVANCED_FACE ( 'NONE', ( #39872 ), #13087, .F. ) ;
#17159 = ORIENTED_EDGE ( 'NONE', *, *, #80759, .T. ) ;
#17158 = CARTESIAN_POINT ( 'NONE',  ( 101.3806489482690694, -45.56251468762313550, 222.1213395616249784 ) ) ;
#17160 = DIRECTION ( 'NONE',  ( 0.000000000000000000, 1.000000000000000000, 0.000000000000000000 ) ) ;
#17161 = CARTESIAN_POINT ( 'NONE',  ( 97.54012738755939438, -43.81963713510241121, 257.8356252759109566 ) ) ;
#17162 = CARTESIAN_POINT ( 'NONE',  ( 109.0806625061526205, -47.64460086702110431, 123.7337205140059666 ) ) ;
#17163 = AXIS2_PLACEMENT_3D ( 'NONE', #69482, #69033, #21332 ) ;
#17164 = CARTESIAN_POINT ( 'NONE',  ( 82.89895571708156297, 82.54999999999999716, 100.8594679592221155 ) ) ;
#17165 = CIRCLE ( 'NONE', #4110, 0.5000000000000004441 ) ;
#17166 = CARTESIAN_POINT ( 'NONE',  ( 0.000000000000000000, 223.9999999999999716, 154.6557476874258441 ) ) ;
#17167 = CARTESIAN_POINT ( 'NONE',  ( 100.6522392491104938, 79.66749569656609253, -83.15048135366419046 ) ) ;
#17168 = CARTESIAN_POINT ( 'NONE',  ( 112.0652232319741586, -45.48878010129285343, 263.9899091037361814 ) ) ;
#17169 = VERTEX_POINT ( 'NONE', #55279 ) ;
#17170 = EDGE_CURVE ( 'NONE', #56556, #83896, #74413, .T. ) ;
#17171 = ORIENTED_EDGE ( 'NONE', *, *, #64251, .T. ) ;
#17172 = VERTEX_POINT ( 'NONE', #88940 ) ;
#17173 = AXIS2_PLACEMENT_3D ( 'NONE', #89070, #40461, #69524 ) ;
#17174 = ORIENTED_EDGE ( 'NONE', *, *, #77090, .F. ) ;
#17175 = CARTESIAN_POINT ( 'NONE',  ( 98.30753417922522885, -41.72887547139915654, 71.73979194078179944 ) ) ;
#17176 = CARTESIAN_POINT ( 'NONE',  ( 112.6636929512762180, -45.52454417301038347, 259.0270538473393458 ) ) ;
#17177 = DIRECTION ( 'NONE',  ( 3.100000000000000258E-29, -3.100000000000000044E-14, -1.000000000000000000 ) ) ;
#17178 = CARTESIAN_POINT ( 'NONE',  ( 131.4450127212694781, -35.89730640218696323, 2.921034946745736605 ) ) ;
#17180 = CARTESIAN_POINT ( 'NONE',  ( 79.20758933349287645, 71.53193882405246029, 88.21655330423307362 ) ) ;
#17179 = FACE_OUTER_BOUND ( 'NONE', #20857, .T. ) ;
#17181 = LINE ( 'NONE', #44866, #74792 ) ;
#17182 = CARTESIAN_POINT ( 'NONE',  ( 112.0098809771561577, -44.31729861111978153, 222.4705150661719983 ) ) ;
#17183 = ORIENTED_EDGE ( 'NONE', *, *, #67633, .F. ) ;
#17184 = AXIS2_PLACEMENT_3D ( 'NONE', #79759, #50685, #23893 ) ;
#17185 = ORIENTED_EDGE ( 'NONE', *, *, #89626, .F. ) ;
#17186 = EDGE_LOOP ( 'NONE', ( #85674, #84190, #69258, #62878 ) ) ;
#17187 = CARTESIAN_POINT ( 'NONE',  ( -469.3583484187089994, 53.97500000000000142, 3.174999999999999822 ) ) ;
#17188 = CARTESIAN_POINT ( 'NONE',  ( 101.9934930118830749, -45.44599331293795785, 182.1565212684371033 ) ) ;
#17189 = EDGE_CURVE ( 'NONE', #36762, #81558, #89393, .T. ) ;
#17190 = CARTESIAN_POINT ( 'NONE',  ( 105.1480534186857483, -26.53835308478808130, 276.2365776568628917 ) ) ;
#17191 = EDGE_CURVE ( 'NONE', #61623, #59070, #52710, .T. ) ;
#17192 = DIRECTION ( 'NONE',  ( 1.000000000000000000, 4.163336342344333240E-14, 0.000000000000000000 ) ) ;
#17193 = EDGE_CURVE ( 'NONE', #35428, #83920, #1593, .T. ) ;
#17194 = DIRECTION ( 'NONE',  ( 1.000000000000000078E-15, -1.000000000000000083E-30, -1.000000000000000000 ) ) ;
#17195 = CARTESIAN_POINT ( 'NONE',  ( 101.9933023703032262, -45.44587501993174072, 27.15642918372197556 ) ) ;
#17196 = ORIENTED_EDGE ( 'NONE', *, *, #24315, .F. ) ;
#17197 = AXIS2_PLACEMENT_3D ( 'NONE', #2628, #31651, #59351 ) ;
#17198 = ADVANCED_FACE ( 'NONE', ( #15215 ), #26693, .F. ) ;
#17199 = CARTESIAN_POINT ( 'NONE',  ( 112.7925898505289979, -28.47466936393675851, 55.59362532201837581 ) ) ;
#17200 = ORIENTED_EDGE ( 'NONE', *, *, #58489, .F. ) ;
#17201 = FACE_OUTER_BOUND ( 'NONE', #6372, .T. ) ;
#17202 = CARTESIAN_POINT ( 'NONE',  ( 114.0183221777719638, -41.00747610084435024, 16.20523322673395228 ) ) ;
#17203 = AXIS2_PLACEMENT_3D ( 'NONE', #87367, #45995, #25127 ) ;
#17204 = DIRECTION ( 'NONE',  ( 0.000000000000000000, -1.000000000000000000, 0.000000000000000000 ) ) ;
#17205 = B_SPLINE_CURVE_WITH_KNOTS ( 'NONE', 3,
 ( #66745, #4527, #81743, #46732, #74461, #68543, #47627, #11334, #18593, #73557, #47175, #53530, #39033, #68095, #74011, #11790, #81302, #12236, #39486, #39924, #67643, #40821, #75359, #33122, #19045, #67187, #59912, #19492, #53982, #4970, #32668, #60363, #53076, #25863, #54426, #5427, #74909, #88988, #6312, #32215, #40379, #5879, #34004, #88550, #33565, #26747, #82190, #61705, #24967 ),
 .UNSPECIFIED., .F., .F.,
 ( 4, 2, 2, 2, 2, 2, 2, 2, 2, 2, 2, 2, 2, 2, 2, 1, 2, 2, 2, 2, 2, 2, 2, 2, 4 ),
 ( 0.01986933033599076401, 0.02111088875730814801, 0.02235244717862553548, 0.02483556402126030349, 0.02607712244257766668, 0.02731868086389502986, 0.02980179770652975971, 0.03228491454916448955, 0.03352647297048184927, 0.03476803139179920898, 0.03725114823443394924, 0.03849270665575131589, 0.03973426507706868949, 0.04221738191970342974, 0.04345894034102079639, 0.04470049876233816999, 0.04594205718365554358, 0.04718361560497291718, 0.04966673244760767825, 0.05090829086892507960, 0.05214984929024249483, 0.05463296613287728365, 0.05587452455419468500, 0.05711608297551208635, 0.05959919981814688905 ),
 .UNSPECIFIED. ) ;
#17206 = DIRECTION ( 'NONE',  ( 1.000000000000000000, 4.299999999999999979E-14, 1.000000000000000078E-15 ) ) ;
#17207 = EDGE_CURVE ( 'NONE', #16775, #82312, #12635, .T. ) ;
#17208 = CARTESIAN_POINT ( 'NONE',  ( 125.8897075496517317, -55.55267141831851774, -5.074374724089010691 ) ) ;
#17209 = ORIENTED_EDGE ( 'NONE', *, *, #42767, .T. ) ;
#17210 = DIRECTION ( 'NONE',  ( 0.000000000000000000, 0.000000000000000000, -1.000000000000000000 ) ) ;
#17211 = CIRCLE ( 'NONE', #67974, 11.45913725231036118 ) ;
#17212 = DIRECTION ( 'NONE',  ( -0.7071067811866279529, 0.7071067811864671926, -7.071067811866286874E-16 ) ) ;
#17213 = ORIENTED_EDGE ( 'NONE', *, *, #82058, .T. ) ;
#17214 = CARTESIAN_POINT ( 'NONE',  ( 116.1238663722925253, -29.08717671455551468, 74.38419670448293175 ) ) ;
#17215 = ORIENTED_EDGE ( 'NONE', *, *, #31943, .T. ) ;
#17216 = CARTESIAN_POINT ( 'NONE',  ( 99.10695020771697727, -33.55172231072156563, 40.44670554236296312 ) ) ;
#17217 = VECTOR ( 'NONE', #16526, 1000.000000000000000 ) ;
#17218 = CARTESIAN_POINT ( 'NONE',  ( 37.03715912545434463, -48.62818131006122258, 237.4678068554150059 ) ) ;
#17219 = CARTESIAN_POINT ( 'NONE',  ( 98.33263373320089329, -38.22883053613415427, 87.89301187732596077 ) ) ;
#17220 = DIRECTION ( 'NONE',  ( 0.000000000000000000, 0.000000000000000000, 1.000000000000000000 ) ) ;
#17221 = FACE_BOUND ( 'NONE', #82489, .T. ) ;
#17222 = CIRCLE ( 'NONE', #73815, 12.59999999999999964 ) ;
#17223 = LINE ( 'NONE', #79460, #17936 ) ;
#17224 = CARTESIAN_POINT ( 'NONE',  ( 97.05449064767977063, -33.74661928051879300, 27.09562527591097236 ) ) ;
#17225 = CARTESIAN_POINT ( 'NONE',  ( 142.8824340801165249, -74.11588153691421610, 540.9756252759101471 ) ) ;
#17226 = ORIENTED_EDGE ( 'NONE', *, *, #64872, .F. ) ;
#17227 = PLANE ( 'NONE',  #86520 ) ;
#17228 = VERTEX_POINT ( 'NONE', #68498 ) ;
#17229 = CARTESIAN_POINT ( 'NONE',  ( 78.22143491580683872, -20.77077206072207360, 2.188418444514117489 ) ) ;
#17230 = ORIENTED_EDGE ( 'NONE', *, *, #15123, .F. ) ;
#17231 = EDGE_LOOP ( 'NONE', ( #87583, #28167, #87644, #11857 ) ) ;
#17232 = AXIS2_PLACEMENT_3D ( 'NONE', #73081, #80817, #59882 ) ;
#17233 = DIRECTION ( 'NONE',  ( 0.000000000000000000, 0.000000000000000000, -1.000000000000000000 ) ) ;
#17234 = PLANE ( 'NONE',  #63766 ) ;
#17235 = CARTESIAN_POINT ( 'NONE',  ( 101.0525363619397012, -44.44280425155412217, 232.0499109901969632 ) ) ;
#17236 = CARTESIAN_POINT ( 'NONE',  ( 135.3838309168194201, -60.54606547621062163, 361.9756252759100335 ) ) ;
#17237 = DIRECTION ( 'NONE',  ( 1.000000000000000000, 4.163336342344333240E-14, 0.000000000000000000 ) ) ;
#17238 = CARTESIAN_POINT ( 'NONE',  ( 116.1236770753320542, -29.08733643602844054, 70.38419670448192278 ) ) ;
#17239 = CARTESIAN_POINT ( 'NONE',  ( 100.8870673645827480, -44.69991497499172084, 43.05225246011283247 ) ) ;
#17240 = ORIENTED_EDGE ( 'NONE', *, *, #32059, .T. ) ;
#17241 = CARTESIAN_POINT ( 'NONE',  ( 97.31305002966453799, -38.96050384283260826, 172.5054018742519020 ) ) ;
#17242 = LINE ( 'NONE', #19018, #25910 ) ;
#17243 = EDGE_CURVE ( 'NONE', #73652, #54474, #77403, .T. ) ;
#17245 = ORIENTED_EDGE ( 'NONE', *, *, #12991, .T. ) ;
#17244 = AXIS2_PLACEMENT_3D ( 'NONE', #18282, #66881, #24660 ) ;
#17246 = CARTESIAN_POINT ( 'NONE',  ( 219.9639999999999986, 40.03750000000000142, -58.73749999999999716 ) ) ;
#17247 = CARTESIAN_POINT ( 'NONE',  ( 25.56670390244797275, -48.82844715994099971, 134.4678068554150059 ) ) ;
#17248 = CARTESIAN_POINT ( 'NONE',  ( 116.0363244534468805, -41.99923036749497385, 238.4041967044829562 ) ) ;
#17249 = FACE_OUTER_BOUND ( 'NONE', #20584, .T. ) ;
#17250 = EDGE_CURVE ( 'NONE', #41991, #79223, #75759, .T. ) ;
#17251 = DIRECTION ( 'NONE',  ( 3.100000000000000258E-29, -3.100000000000000044E-14, -1.000000000000000000 ) ) ;
#17252 = DIRECTION ( 'NONE',  ( 0.000000000000000000, 1.000000000000000000, 0.000000000000000000 ) ) ;
#17253 = CARTESIAN_POINT ( 'NONE',  ( 106.6575247680289777, -45.29010455595041407, 246.9609912566479579 ) ) ;
#17255 = CARTESIAN_POINT ( 'NONE',  ( 110.1514708964275684, -46.66481413883387575, 93.81562527591097478 ) ) ;
#17254 = DIRECTION ( 'NONE',  ( 0.000000000000000000, 0.000000000000000000, 1.000000000000000000 ) ) ;
#17256 = CARTESIAN_POINT ( 'NONE',  ( 111.6005515524849017, 65.74677178836266478, 67.75091760821770492 ) ) ;
#17257 = CARTESIAN_POINT ( 'NONE',  ( 102.3405178495751215, -46.07139110582879482, 127.2041967044829960 ) ) ;
#17258 = ORIENTED_EDGE ( 'NONE', *, *, #24105, .T. ) ;
#17259 = LINE ( 'NONE', #24516, #59640 ) ;
#17260 = VERTEX_POINT ( 'NONE', #18999 ) ;
#17261 = LINE ( 'NONE', #9998, #62759 ) ;
#17262 = LINE ( 'NONE', #71342, #42097 ) ;
#17263 = CARTESIAN_POINT ( 'NONE',  ( 130.0664832912740110, -14.47844715994100007, 17.92562527591199739 ) ) ;
#17264 = ORIENTED_EDGE ( 'NONE', *, *, #42381, .F. ) ;
#17265 = VECTOR ( 'NONE', #601, 1000.000000000000000 ) ;
#17266 = DIRECTION ( 'NONE',  ( -1.000000000000000078E-15, 1.000000000000000000, -3.100000000000000044E-14 ) ) ;
#17267 = EDGE_LOOP ( 'NONE', ( #42679, #16113, #33606, #18306 ) ) ;
#17268 = CARTESIAN_POINT ( 'NONE',  ( 72.96458098368650269, 127.0000000000000000, 80.10833098368729566 ) ) ;
#17269 = CARTESIAN_POINT ( 'NONE',  ( -12.60000000000000142, 82.54999999999999716, 92.46299999999996544 ) ) ;
#17271 = CARTESIAN_POINT ( 'NONE',  ( 156.5667039024485803, -48.82844715993568485, 137.2178068554149775 ) ) ;
#17270 = VECTOR ( 'NONE', #57054, 1000.000000000000000 ) ;
#17272 = ORIENTED_EDGE ( 'NONE', *, *, #83532, .F. ) ;
#17273 = VECTOR ( 'NONE', #7, 1000.000000000000000 ) ;
#17274 = ADVANCED_FACE ( 'NONE', ( #46683 ), #12187, .T. ) ;
#17275 = CARTESIAN_POINT ( 'NONE',  ( 114.3686432469292527, -44.20104832357726110, 73.19276813305397411 ) ) ;
#17276 = CARTESIAN_POINT ( 'NONE',  ( -295.6978641014171671, 7.710689432856530360E-60, 1.032479058483546304E-12 ) ) ;
#17277 = DIRECTION ( 'NONE',  ( 0.000000000000000000, 1.000000000000000000, 0.000000000000000000 ) ) ;
#17278 = DIRECTION ( 'NONE',  ( 0.7071067811739274456, -0.7071067811991676999, 0.000000000000000000 ) ) ;
#17279 = CARTESIAN_POINT ( 'NONE',  ( 72.26648329127297643, -1.929447159941394263, 361.9756252759109998 ) ) ;
#17280 = EDGE_LOOP ( 'NONE', ( #37562, #66032 ) ) ;
#17281 = VECTOR ( 'NONE', #42233, 1000.000000000000000 ) ;
#17282 = ORIENTED_EDGE ( 'NONE', *, *, #15046, .F. ) ;
#17283 = CYLINDRICAL_SURFACE ( 'NONE', #46015, 16.00000000000000000 ) ;
#17284 = DIRECTION ( 'NONE',  ( 1.000000000000000000, 0.000000000000000000, 0.000000000000000000 ) ) ;
#17285 = CIRCLE ( 'NONE', #72400, 8.928099999999993486 ) ;
#17286 = FACE_OUTER_BOUND ( 'NONE', #5378, .T. ) ;
#17287 = VECTOR ( 'NONE', #1066, 1000.000000000000000 ) ;
#17289 = CARTESIAN_POINT ( 'NONE',  ( -103.1875000000000000, 101.5999999999999943, -1.080832317973422076E-12 ) ) ;
#17288 = DIRECTION ( 'NONE',  ( 0.000000000000000000, 0.000000000000000000, -1.000000000000000000 ) ) ;
#17290 = LINE ( 'NONE', #9578, #81434 ) ;
#17291 = ORIENTED_EDGE ( 'NONE', *, *, #85400, .F. ) ;
#17292 = DIRECTION ( 'NONE',  ( 0.2884130866282238470, 0.7071067811865494601, -0.6456143519637539407 ) ) ;
#17293 = CARTESIAN_POINT ( 'NONE',  ( 113.1634500054121872, -44.41975088505036240, 164.1099109901959707 ) ) ;
#17294 = EDGE_CURVE ( 'NONE', #16097, #3936, #48379, .T. ) ;
#17295 = VECTOR ( 'NONE', #69420, 1000.000000000000000 ) ;
#17297 = ORIENTED_EDGE ( 'NONE', *, *, #2460, .F. ) ;
#17296 = LINE ( 'NONE', #44975, #45781 ) ;
#17298 = CARTESIAN_POINT ( 'NONE',  ( 97.32756240345236165, -42.09278592124177010, 22.72705384733897205 ) ) ;
#17299 = FACE_OUTER_BOUND ( 'NONE', #49097, .T. ) ;
#17300 = DIRECTION ( 'NONE',  ( -0.1858654557293118459, 0.9825752044329915114, 0.000000000000000000 ) ) ;
#17301 = EDGE_CURVE ( 'NONE', #50227, #8645, #50158, .T. ) ;
#17302 = CARTESIAN_POINT ( 'NONE',  ( 138.8167039024479834, -67.87844715994100397, 35.51780685541480409 ) ) ;
#17303 = VERTEX_POINT ( 'NONE', #9294 ) ;
#17304 = FACE_OUTER_BOUND ( 'NONE', #66015, .T. ) ;
#17305 = EDGE_CURVE ( 'NONE', #69846, #59397, #61429, .T. ) ;
#17306 = EDGE_LOOP ( 'NONE', ( #49870, #68354, #75192, #76379 ) ) ;
#17307 = EDGE_LOOP ( 'NONE', ( #76641, #10717, #55680, #67993 ) ) ;
#17308 = CIRCLE ( 'NONE', #53504, 2.116999999999993776 ) ;
#17309 = CARTESIAN_POINT ( 'NONE',  ( 106.9887167903908392, -45.59072421142732168, 184.0015833058969577 ) ) ;
#17310 = CARTESIAN_POINT ( 'NONE',  ( 51.34673845256598668, -29.62846900982231446, -5.074374724088000832 ) ) ;
#17311 = CARTESIAN_POINT ( 'NONE',  ( 23.58194362415510881, 84.94332446042855622, 307.0240855191376568 ) ) ;
#17312 = DIRECTION ( 'NONE',  ( 0.000000000000000000, 1.000000000000000000, 0.000000000000000000 ) ) ;
#17313 = EDGE_CURVE ( 'NONE', #23155, #66915, #51928, .T. ) ;
#17314 = CARTESIAN_POINT ( 'NONE',  ( 173.9900000000000091, 5.112500000000000711, -7.937500000000000000 ) ) ;
#17315 = ORIENTED_EDGE ( 'NONE', *, *, #85399, .F. ) ;
#17316 = DIRECTION ( 'NONE',  ( 3.100000000000000258E-29, -3.100000000000000044E-14, -1.000000000000000000 ) ) ;
#17317 = CARTESIAN_POINT ( 'NONE',  ( 32.25690895537100289, -33.54226604285010893, -5.074374724088000832 ) ) ;
#17318 = ADVANCED_FACE ( 'NONE', ( #77891 ), #51491, .T. ) ;
#17319 = ORIENTED_EDGE ( 'NONE', *, *, #42991, .T. ) ;
#17320 = CARTESIAN_POINT ( 'NONE',  ( 106.8369185487093063, -47.13021470646874178, 272.5584824187680510 ) ) ;
#17321 = DIRECTION ( 'NONE',  ( 1.000000000000000000, 0.000000000000000000, 0.000000000000000000 ) ) ;
#17322 = VERTEX_POINT ( 'NONE', #16116 ) ;
#17323 = CARTESIAN_POINT ( 'NONE',  ( 98.30753418384445297, -41.72887547938789510, 81.73979194150940941 ) ) ;
#17324 = DIRECTION ( 'NONE',  ( 0.000000000000000000, 0.000000000000000000, 1.000000000000000000 ) ) ;
#17325 = DIRECTION ( 'NONE',  ( 1.000000000000000000, 0.000000000000000000, 0.000000000000000000 ) ) ;
#17326 = CARTESIAN_POINT ( 'NONE',  ( 107.0664832912739968, -36.72944715994103149, 14.92562527591097066 ) ) ;
#17327 = CARTESIAN_POINT ( 'NONE',  ( 114.8463700017591407, -29.67172957150665979, 205.4127681330539872 ) ) ;
#17329 = DIRECTION ( 'NONE',  ( -1.000000000000000078E-15, 0.000000000000000000, 1.000000000000000000 ) ) ;
#17328 = CIRCLE ( 'NONE', #40525, 11.49999999999999645 ) ;
#17330 = CIRCLE ( 'NONE', #59386, 3.299999999999997158 ) ;
#17331 = ORIENTED_EDGE ( 'NONE', *, *, #27418, .T. ) ;
#17332 = CARTESIAN_POINT ( 'NONE',  ( 100.4516903307928573, -27.81642228345825885, 31.59657765686396758 ) ) ;
#17333 = CARTESIAN_POINT ( 'NONE',  ( 180.2121375201594731, -29.73316016638963433, 313.9678068554149490 ) ) ;
#17334 = CARTESIAN_POINT ( 'NONE',  ( 98.40533970481327231, -42.07952101345657780, 11.76800622829193799 ) ) ;
#17335 = ORIENTED_EDGE ( 'NONE', *, *, #62400, .T. ) ;
#17336 = VECTOR ( 'NONE', #79244, 1000.000000000000000 ) ;
#17337 = CARTESIAN_POINT ( 'NONE',  ( 78.64532134553982701, -39.08531275929848903, 7.905164235249591442 ) ) ;
#17338 = DIRECTION ( 'NONE',  ( -0.000000000000000000, 1.000000000000000000, -0.000000000000000000 ) ) ;
#17339 = FACE_OUTER_BOUND ( 'NONE', #87785, .T. ) ;
#17340 = CARTESIAN_POINT ( 'NONE',  ( 102.7086973628091187, -29.82731503872160417, 108.3423760838769851 ) ) ;
#17341 = CARTESIAN_POINT ( 'NONE',  ( 103.0821958934680111, -47.91639064866039632, 248.3041967044829619 ) ) ;
#17342 = PLANE ( 'NONE',  #72519 ) ;
#17343 = ORIENTED_EDGE ( 'NONE', *, *, #84167, .T. ) ;
#17344 = CARTESIAN_POINT ( 'NONE',  ( 172.5664832912729878, -27.82844715994070484, 198.9256252759119832 ) ) ;
#17345 = ORIENTED_EDGE ( 'NONE', *, *, #87436, .F. ) ;
#17346 = VERTEX_POINT ( 'NONE', #71972 ) ;
#17347 = DIRECTION ( 'NONE',  ( 1.000000000000000000, -2.098553464303459752E-16, 0.000000000000000000 ) ) ;
#17348 = ORIENTED_EDGE ( 'NONE', *, *, #60344, .F. ) ;
#17349 = EDGE_LOOP ( 'NONE', ( #43058, #27216, #83326, #34467 ) ) ;
#17350 = CARTESIAN_POINT ( 'NONE',  ( 192.5667039024474434, -23.42844715993433624, 180.4678068554150343 ) ) ;
#17351 = CARTESIAN_POINT ( 'NONE',  ( 31.75000000000000000, 104.3431970271542042, 3.174999999999999822 ) ) ;
#17352 = EDGE_CURVE ( 'NONE', #44183, #30803, #47204, .T. ) ;
#17353 = CARTESIAN_POINT ( 'NONE',  ( 103.3178953596948162, -27.45860474605225221, 41.38224140060551548 ) ) ;
#17354 = VECTOR ( 'NONE', #17584, 1000.000000000000000 ) ;
#17355 = CARTESIAN_POINT ( 'NONE',  ( 100.5019087779429015, -42.19410572027086914, 116.3009912566479471 ) ) ;
#17356 = CARTESIAN_POINT ( 'NONE',  ( 112.3495078575228376, -28.18909723048616911, 289.6356252759109680 ) ) ;
#17357 = CARTESIAN_POINT ( 'NONE',  ( -12.27300924177314911, 79.25817979229439914, 129.9779100289732696 ) ) ;
#17358 = ORIENTED_EDGE ( 'NONE', *, *, #27290, .T. ) ;
#17359 = DIRECTION ( 'NONE',  ( 0.000000000000000000, 1.000000000000000000, 0.000000000000000000 ) ) ;
#17360 = EDGE_LOOP ( 'NONE', ( #68460, #2038, #40057, #84735 ) ) ;
#17361 = CARTESIAN_POINT ( 'NONE',  ( 97.03930911280052385, -36.38725636255255580, 167.2994274293335195 ) ) ;
#17362 = CARTESIAN_POINT ( 'NONE',  ( -194.1576000000000022, 101.5999999999999943, 114.2999999999999972 ) ) ;
#17363 = CARTESIAN_POINT ( 'NONE',  ( 75.31670390244798341, -50.82844715994100682, 33.40080685541480676 ) ) ;
#17364 = VECTOR ( 'NONE', #41416, 1000.000000000000000 ) ;
#17365 = LINE ( 'NONE', #24186, #50940 ) ;
#17366 = ORIENTED_EDGE ( 'NONE', *, *, #22416, .F. ) ;
#17367 = EDGE_CURVE ( 'NONE', #17066, #14490, #31059, .T. ) ;
#17368 = CARTESIAN_POINT ( 'NONE',  ( 111.4804840314119758, -26.59568808167472653, 284.7375300378156453 ) ) ;
#17369 = CARTESIAN_POINT ( 'NONE',  ( 99.11046098610404442, -43.53346720896296773, 27.88991099019694175 ) ) ;
#17371 = CARTESIAN_POINT ( 'NONE',  ( 69.20747379336683025, -138.7952845549384904, 247.2071845478467083 ) ) ;
#17370 = LINE ( 'NONE', #72783, #88333 ) ;
#17372 = LINE ( 'NONE', #17815, #75754 ) ;
#17373 = CARTESIAN_POINT ( 'NONE',  ( 70.98999999999998067, 52.73749999999999716, -44.45000000000002416 ) ) ;
#17374 = CARTESIAN_POINT ( 'NONE',  ( 131.7676426598725072, -38.23887630717962338, 7.293197373621404189 ) ) ;
#17375 = VECTOR ( 'NONE', #69143, 1000.000000000000000 ) ;
#17376 = FACE_OUTER_BOUND ( 'NONE', #51550, .T. ) ;
#17377 = FACE_OUTER_BOUND ( 'NONE', #65926, .T. ) ;
#17378 = CARTESIAN_POINT ( 'NONE',  ( -103.1875000000000000, 127.0000000000000000, -1.080832317973422076E-12 ) ) ;
#17379 = AXIS2_PLACEMENT_3D ( 'NONE', #53317, #34241, #55110 ) ;
#17380 = EDGE_CURVE ( 'NONE', #7662, #61259, #64370, .T. ) ;
#17381 = CARTESIAN_POINT ( 'NONE',  ( 106.2486884972880432, -26.25648168547507311, 25.13848241876792855 ) ) ;
#17382 = CARTESIAN_POINT ( 'NONE',  ( 114.9778481211559154, -29.01036126763497336, 190.4537205140059655 ) ) ;
#17383 = CARTESIAN_POINT ( 'NONE',  ( 100.3971814656068915, -28.68844771884695888, 36.62705384733894221 ) ) ;
#17385 = CARTESIAN_POINT ( 'NONE',  ( 117.0608945236349143, -38.08045312005563687, 48.71895860930425926 ) ) ;
#17384 = DIRECTION ( 'NONE',  ( 0.000000000000000000, -1.000000000000000000, 0.000000000000000000 ) ) ;
#17386 = CARTESIAN_POINT ( 'NONE',  ( 80.44276116895382245, -33.99866847873249753, 1.641799428525402504 ) ) ;
#17387 = AXIS2_PLACEMENT_3D ( 'NONE', #2958, #9773, #37477 ) ;
#17388 = AXIS2_PLACEMENT_3D ( 'NONE', #17877, #45553, #23821 ) ;
#17389 = EDGE_CURVE ( 'NONE', #44246, #75012, #87579, .T. ) ;
#17390 = ORIENTED_EDGE ( 'NONE', *, *, #48267, .T. ) ;
#17391 = DIRECTION ( 'NONE',  ( -1.000000000000000078E-15, 1.000000000000000000, 0.000000000000000000 ) ) ;
#17392 = VERTEX_POINT ( 'NONE', #58753 ) ;
#17393 = CARTESIAN_POINT ( 'NONE',  ( 114.7041265136727901, -43.74408836545391921, 74.22324432352993995 ) ) ;
#17394 = VECTOR ( 'NONE', #11868, 1000.000000000000000 ) ;
#17396 = ORIENTED_EDGE ( 'NONE', *, *, #37857, .T. ) ;
#17395 = CARTESIAN_POINT ( 'NONE',  ( -47.18030668273772221, 93.07500000000001705, 75.34738655934135920 ) ) ;
#17397 = DIRECTION ( 'NONE',  ( 0.000000000000000000, -1.000000000000000000, 0.000000000000000000 ) ) ;
#17398 = CARTESIAN_POINT ( 'NONE',  ( 102.2473430764597282, -45.94923854148469644, 208.1927681330539599 ) ) ;
#17399 = CARTESIAN_POINT ( 'NONE',  ( 100.8864929060172528, -44.69947222835936884, 253.0533978726845419 ) ) ;
#17400 = DIRECTION ( 'NONE',  ( 0.000000000000000000, -1.000000000000000000, 0.000000000000000000 ) ) ;
#17401 = PRODUCT_DEFINITION_FORMATION_WITH_SPECIFIED_SOURCE ( 'ANY', '', #73550, .NOT_KNOWN. ) ;
#17402 = CARTESIAN_POINT ( 'NONE',  ( 128.5664832912740110, -41.22944715994101017, 4.925625275910991974 ) ) ;
#17403 = EDGE_CURVE ( 'NONE', #74897, #62421, #6331, .T. ) ;
#17404 = DIRECTION ( 'NONE',  ( 0.7071067811864666375, 0.7071067811866283970, 7.071067811864971448E-16 ) ) ;
#17405 = CARTESIAN_POINT ( 'NONE',  ( 145.3708670603641622, -136.8623670038712987, 247.4903216359130056 ) ) ;
#17406 = CARTESIAN_POINT ( 'NONE',  ( 109.6407163665292046, -46.48066509518846345, 97.78129702168313031 ) ) ;
#17407 = AXIS2_PLACEMENT_3D ( 'NONE', #9971, #44912, #82041 ) ;
#17408 = CARTESIAN_POINT ( 'NONE',  ( 113.5587197313314505, -28.64306037466250743, 119.5261014663879564 ) ) ;
#17409 = ORIENTED_EDGE ( 'NONE', *, *, #5608, .T. ) ;
#17410 = ORIENTED_EDGE ( 'NONE', *, *, #66796, .F. ) ;
#17411 = CARTESIAN_POINT ( 'NONE',  ( 109.2913206311583707, -45.85778897805103327, 84.18634521065892784 ) ) ;
#17412 = DIRECTION ( 'NONE',  ( 0.000000000000000000, -1.000000000000000000, 0.000000000000000000 ) ) ;
#17414 = CARTESIAN_POINT ( 'NONE',  ( 51.42025729302664416, -31.94127993907661178, 237.4678068554150059 ) ) ;
#17413 = CARTESIAN_POINT ( 'NONE',  ( 96.86352172870826394, -32.31225822881506815, 207.0013395616249738 ) ) ;
#17415 = CARTESIAN_POINT ( 'NONE',  ( 141.0664832912739826, -8.729447159940995959, 14.67562527591100441 ) ) ;
#17416 = LINE ( 'NONE', #3342, #22070 ) ;
#17417 = VECTOR ( 'NONE', #80607, 1000.000000000000000 ) ;
#17418 = CARTESIAN_POINT ( 'NONE',  ( 117.9439354154377924, 78.46407912418312947, 12.03195559056957187 ) ) ;
#17419 = EDGE_CURVE ( 'NONE', #60827, #83591, #44055, .T. ) ;
#17420 = DIRECTION ( 'NONE',  ( -4.237773401492740281E-14, 1.000000000000000000, 0.000000000000000000 ) ) ;
#17421 = CARTESIAN_POINT ( 'NONE',  ( 188.5667039024483529, -42.82844715993430640, 134.7178068554150059 ) ) ;
#17422 = CARTESIAN_POINT ( 'NONE',  ( 12.59999999999999964, 82.54999999999999716, 117.8845415480757595 ) ) ;
#17423 = EDGE_CURVE ( 'NONE', #19595, #19378, #77550, .T. ) ;
#17424 = CARTESIAN_POINT ( 'NONE',  ( 99.11802762103501152, -45.48540990049890809, 156.9899109901969609 ) ) ;
#17425 = ORIENTED_EDGE ( 'NONE', *, *, #65942, .F. ) ;
#17426 = ORIENTED_EDGE ( 'NONE', *, *, #30752, .T. ) ;
#17427 = EDGE_CURVE ( 'NONE', #75163, #64560, #53711, .T. ) ;
#17428 = DIRECTION ( 'NONE',  ( -0.4999999999999990563, 0.000000000000000000, -0.8660254037844392627 ) ) ;
#17429 = CARTESIAN_POINT ( 'NONE',  ( 146.7254745405287224, -68.20551812416188397, 246.6136140996082702 ) ) ;
#17430 = EDGE_CURVE ( 'NONE', #74275, #17303, #19671, .T. ) ;
#17431 = FACE_OUTER_BOUND ( 'NONE', #59777, .T. ) ;
#17432 = CIRCLE ( 'NONE', #52211, 10.26166025953211758 ) ;
#17433 = DIRECTION ( 'NONE',  ( 0.7071067811862279395, -0.7071067811868672059, 7.071067811862286363E-16 ) ) ;
#17434 = CARTESIAN_POINT ( 'NONE',  ( 108.6750451637706618, -26.42898313331718541, 189.9527681330539792 ) ) ;
#17435 = LINE ( 'NONE', #19223, #70568 ) ;
#17436 = ORIENTED_EDGE ( 'NONE', *, *, #87304, .T. ) ;
#17438 = EDGE_LOOP ( 'NONE', ( #18891, #47908, #77129, #14345 ) ) ;
#17437 = VERTEX_POINT ( 'NONE', #88728 ) ;
#17439 = VECTOR ( 'NONE', #2236, 1000.000000000000000 ) ;
#17440 = LINE ( 'NONE', #37439, #83937 ) ;
#17441 = DIRECTION ( 'NONE',  ( -1.000000000000000000, -1.000000000000000078E-15, 0.000000000000000000 ) ) ;
#17442 = CARTESIAN_POINT ( 'NONE',  ( 132.3573525511357332, -34.57277629268848074, 7.749696248598098691 ) ) ;
#17443 = CARTESIAN_POINT ( 'NONE',  ( 98.69396380956492010, -33.82637249272325164, 282.4930118773256709 ) ) ;
#17444 = CIRCLE ( 'NONE', #24702, 4.750000000000004441 ) ;
#17445 = LINE ( 'NONE', #72851, #5730 ) ;
#17446 = ORIENTED_EDGE ( 'NONE', *, *, #83021, .F. ) ;
#17447 = CARTESIAN_POINT ( 'NONE',  ( 104.9952014352892888, -44.61589190275481798, 9.635625275910941312 ) ) ;
#17448 = CARTESIAN_POINT ( 'NONE',  ( 82.15318967143088003, -16.93816060012580138, 7.482180659745496065 ) ) ;
#17449 = EDGE_LOOP ( 'NONE', ( #71921, #3563, #15276, #18992 ) ) ;
#17451 = EDGE_LOOP ( 'NONE', ( #57177, #1723, #942, #79560, #48969, #129 ) ) ;
#17450 = CIRCLE ( 'NONE', #30488, 0.5000000000000079936 ) ;
#17452 = CARTESIAN_POINT ( 'NONE',  ( 0.000000000000000000, 20.32000000000000028, 0.000000000000000000 ) ) ;
#17453 = ORIENTED_EDGE ( 'NONE', *, *, #46897, .F. ) ;
#17454 = ORIENTED_EDGE ( 'NONE', *, *, #12789, .F. ) ;
#17455 = CARTESIAN_POINT ( 'NONE',  ( 115.0871287824179348, -30.61533435494355970, 155.3439420463051590 ) ) ;
#17456 = EDGE_CURVE ( 'NONE', #65898, #76316, #67269, .T. ) ;
#17457 = CARTESIAN_POINT ( 'NONE',  ( 106.3992821860680635, -28.18503700880033236, 24.56099125664901095 ) ) ;
#17458 = VECTOR ( 'NONE', #40004, 1000.000000000000000 ) ;
#17459 = CARTESIAN_POINT ( 'NONE',  ( 101.4133560641720067, -46.25507541695031222, 207.1622919425779514 ) ) ;
#17460 = CARTESIAN_POINT ( 'NONE',  ( 117.6812658759005217, -39.72780374360938538, 143.6194347997209775 ) ) ;
#17461 = DIRECTION ( 'NONE',  ( 0.000000000000000000, 0.000000000000000000, -1.000000000000000000 ) ) ;
#17462 = CARTESIAN_POINT ( 'NONE',  ( 96.97881741550158097, -39.36031858868991407, 272.5299109901966972 ) ) ;
#17463 = FACE_OUTER_BOUND ( 'NONE', #69926, .T. ) ;
#17464 = CARTESIAN_POINT ( 'NONE',  ( 164.7812970173241922, -35.65087443489296248, 313.9678068554149490 ) ) ;
#17465 = ORIENTED_EDGE ( 'NONE', *, *, #68368, .F. ) ;
#17466 = ORIENTED_EDGE ( 'NONE', *, *, #6672, .F. ) ;
#17467 = VECTOR ( 'NONE', #58140, 1000.000000000000000 ) ;
#17468 = CARTESIAN_POINT ( 'NONE',  ( 116.9264758816979537, -41.82782236628663242, 243.4346728949589647 ) ) ;
#17469 = EDGE_LOOP ( 'NONE', ( #51203, #28483 ) ) ;
#17470 = ADVANCED_FACE ( 'NONE', ( #88288 ), #81477, .F. ) ;
#17471 = CARTESIAN_POINT ( 'NONE',  ( 97.38189020833135601, -42.05746220039552696, 176.7146728949589658 ) ) ;
#17472 = CARTESIAN_POINT ( 'NONE',  ( 116.3216976867776964, -32.94060878512167534, 40.13562527591096796 ) ) ;
#17473 = LINE ( 'NONE', #22189, #43387 ) ;
#17474 = CARTESIAN_POINT ( 'NONE',  ( 46.83715912545343940, -47.82818131006086304, 129.9678068554150911 ) ) ;
#17475 = DIRECTION ( 'NONE',  ( 0.000000000000000000, 0.000000000000000000, -1.000000000000000000 ) ) ;
#17476 = EDGE_CURVE ( 'NONE', #44525, #88514, #33302, .T. ) ;
#17479 = CARTESIAN_POINT ( 'NONE',  ( 115.6772654923306902, -42.56752007954064965, 269.3527681330536439 ) ) ;
#17478 = DIRECTION ( 'NONE',  ( 0.000000000000000000, 1.000000000000000000, 0.000000000000000000 ) ) ;
#17477 = CARTESIAN_POINT ( 'NONE',  ( 70.06670390244703128, -96.32844715994099261, 222.2178068554179902 ) ) ;
#17480 = LINE ( 'NONE', #11099, #68492 ) ;
#17481 = DIRECTION ( 'NONE',  ( 1.000000000000000000, 0.000000000000000000, 2.108231265501709878E-16 ) ) ;
#17482 = VECTOR ( 'NONE', #25594, 1000.000000000000000 ) ;
#17483 = CARTESIAN_POINT ( 'NONE',  ( 25.56670390244722668, -42.82844715994178131, 134.7178068554150627 ) ) ;
#17484 = EDGE_CURVE ( 'NONE', #51994, #29546, #11411, .T. ) ;
#17485 = CARTESIAN_POINT ( 'NONE',  ( 68.48770573954575980, -136.9758359881863896, 247.4278779589974135 ) ) ;
#17486 = LINE ( 'NONE', #73330, #60424 ) ;
#17487 = EDGE_CURVE ( 'NONE', #49481, #19751, #54146, .T. ) ;
#17488 = CARTESIAN_POINT ( 'NONE',  ( 97.31584371105238063, -39.30597598001633486, 77.53145860767988040 ) ) ;
#17490 = VERTEX_POINT ( 'NONE', #17878 ) ;
#17489 = CARTESIAN_POINT ( 'NONE',  ( 110.2163081462844900, -44.10521182743453039, 195.5838068554167819 ) ) ;
#17491 = EDGE_CURVE ( 'NONE', #66455, #50481, #27666, .T. ) ;
#17492 = CARTESIAN_POINT ( 'NONE',  ( 136.6795104150337750, -19.60592655292144926, 6.943955837743826187 ) ) ;
#17493 = CARTESIAN_POINT ( 'NONE',  ( 103.7160641590222809, -26.17150546779393494, 205.3089586092439731 ) ) ;
#17494 = CARTESIAN_POINT ( 'NONE',  ( 104.7595845749942782, -46.89609389129499561, 68.39848241876794077 ) ) ;
#17495 = CARTESIAN_POINT ( 'NONE',  ( 97.05457585776278506, -41.52102392564493272, 212.6937205140059461 ) ) ;
#17496 = CARTESIAN_POINT ( 'NONE',  ( 33.92127028473601769, -29.73316016639540749, 237.4678068554150059 ) ) ;
#17497 = DIRECTION ( 'NONE',  ( 1.000000000000000000, 1.000000000000000078E-15, 0.000000000000000000 ) ) ;
#17499 = CARTESIAN_POINT ( 'NONE',  ( 97.91933391361872907, -40.77183597370108004, 37.65731701089936223 ) ) ;
#17498 = DIRECTION ( 'NONE',  ( 1.000000000000000078E-15, -1.000000000000000083E-30, -1.000000000000000000 ) ) ;
#17500 = CARTESIAN_POINT ( 'NONE',  ( 84.06648329127399677, -18.72966777111500036, 239.5838068554169809 ) ) ;
#17501 = LINE ( 'NONE', #38375, #26720 ) ;
#17502 = EDGE_CURVE ( 'NONE', #52020, #36552, #83255, .T. ) ;
#17503 = CARTESIAN_POINT ( 'NONE',  ( 99.09629730216126120, -30.54963492062786656, 65.80361837691383187 ) ) ;
#17504 = ADVANCED_FACE ( 'NONE', ( #7830 ), #56413, .F. ) ;
#17505 = ORIENTED_EDGE ( 'NONE', *, *, #60540, .F. ) ;
#17506 = ORIENTED_EDGE ( 'NONE', *, *, #60447, .T. ) ;
#17507 = CARTESIAN_POINT ( 'NONE',  ( 98.01892258562502036, -37.12227740767932715, 115.7714674471239675 ) ) ;
#17509 = VERTEX_POINT ( 'NONE', #48694 ) ;
#17508 = CYLINDRICAL_SURFACE ( 'NONE', #6714, 11.45913725231036118 ) ;
#17510 = CARTESIAN_POINT ( 'NONE',  ( 96.81317962367450036, -38.48968277746985933, 87.46133956162493917 ) ) ;
#17511 = EDGE_CURVE ( 'NONE', #33965, #19776, #77326, .T. ) ;
#17512 = CARTESIAN_POINT ( 'NONE',  ( -7.205548786489490269E-13, 117.4749999999999943, 103.1875000000000000 ) ) ;
#17513 = VECTOR ( 'NONE', #11609, 1000.000000000000000 ) ;
#17514 = EDGE_CURVE ( 'NONE', #12332, #2162, #81759, .T. ) ;
#17516 = CARTESIAN_POINT ( 'NONE',  ( 77.53258422225751190, -17.66080143920404666, 7.039723185228972113 ) ) ;
#17515 = AXIS2_PLACEMENT_3D ( 'NONE', #63644, #56809, #84557 ) ;
#17517 = FACE_OUTER_BOUND ( 'NONE', #35623, .T. ) ;
#17518 = CARTESIAN_POINT ( 'NONE',  ( 111.8051047218221896, -27.50533234054179843, 19.71086337114996567 ) ) ;
#17519 = ORIENTED_EDGE ( 'NONE', *, *, #78101, .F. ) ;
#17520 = ORIENTED_EDGE ( 'NONE', *, *, #11323, .T. ) ;
#17522 = EDGE_LOOP ( 'NONE', ( #53775, #76330 ) ) ;
#17521 = AXIS2_PLACEMENT_3D ( 'NONE', #36817, #16820, #18592 ) ;
#17523 = CARTESIAN_POINT ( 'NONE',  ( 76.06670390244799762, -26.72944715994109899, 199.5838068554169524 ) ) ;
#17524 = DIRECTION ( 'NONE',  ( 0.000000000000000000, 0.000000000000000000, 1.000000000000000000 ) ) ;
#17525 = DIRECTION ( 'NONE',  ( -0.9254794337955620787, -0.3787978585227822492, 0.000000000000000000 ) ) ;
#17526 = LINE ( 'NONE', #45206, #26673 ) ;
#17527 = LINE ( 'NONE', #17957, #73689 ) ;
#17528 = CARTESIAN_POINT ( 'NONE',  ( 115.0439452383991892, -99.09543445804915507, 2.217806855417836509 ) ) ;
#17529 = AXIS2_PLACEMENT_3D ( 'NONE', #19359, #39346, #67052 ) ;
#17530 = CARTESIAN_POINT ( 'NONE',  ( 90.44969454456408187, -16.81243780205710436, 239.5838068554175209 ) ) ;
#17531 = EDGE_CURVE ( 'NONE', #28246, #72639, #7387, .T. ) ;
#17532 = CARTESIAN_POINT ( 'NONE',  ( 79.21650378603776232, 93.55239623846831876, 88.20661029664658770 ) ) ;
#17533 = ADVANCED_FACE ( 'NONE', ( #21471 ), #562, .F. ) ;
#17534 = CARTESIAN_POINT ( 'NONE',  ( 96.94236579736387682, -32.35154040576531997, 61.01372051400599616 ) ) ;
#17535 = EDGE_LOOP ( 'NONE', ( #9638, #44247 ) ) ;
#17536 = ORIENTED_EDGE ( 'NONE', *, *, #52510, .T. ) ;
#17537 = EDGE_CURVE ( 'NONE', #63665, #80398, #68335, .T. ) ;
#17538 = CARTESIAN_POINT ( 'NONE',  ( 4.087661814003508809, 94.58137602904389496, 130.4926000606901937 ) ) ;
#17539 = CARTESIAN_POINT ( 'NONE',  ( 80.06648329127402519, -46.72944715994105991, 4.925625275910944012 ) ) ;
#17540 = EDGE_CURVE ( 'NONE', #11232, #41269, #16144, .T. ) ;
#17541 = CARTESIAN_POINT ( 'NONE',  ( 0.000000000000000000, 125.4759999999999991, 0.000000000000000000 ) ) ;
#17542 = CARTESIAN_POINT ( 'NONE',  ( 111.3099657731024337, -28.47785412639777647, 167.5166617981629713 ) ) ;
#17543 = AXIS2_PLACEMENT_3D ( 'NONE', #15566, #51386, #44580 ) ;
#17544 = LINE ( 'NONE', #12517, #3976 ) ;
#17545 = ORIENTED_EDGE ( 'NONE', *, *, #54603, .F. ) ;
#17546 = ORIENTED_EDGE ( 'NONE', *, *, #55940, .T. ) ;
#17547 = DIRECTION ( 'NONE',  ( 1.000000000000000000, 0.000000000000000000, 0.000000000000000000 ) ) ;
#17548 = VERTEX_POINT ( 'NONE', #14661 ) ;
#17549 = EDGE_LOOP ( 'NONE', ( #75019, #29396, #2763, #8367, #88791 ) ) ;
#17550 = DIRECTION ( 'NONE',  ( -0.9254794337955620787, -0.3787978585227822492, 0.000000000000000000 ) ) ;
#17551 = VECTOR ( 'NONE', #72905, 999.9999999999998863 ) ;
#17552 = CARTESIAN_POINT ( 'NONE',  ( 112.6928898907800090, -44.25407833457246909, 184.5311071154209799 ) ) ;
#17553 = CARTESIAN_POINT ( 'NONE',  ( 8.462210198923249696E-15, 71.21114727940270939, 216.0269999999999868 ) ) ;
#17554 = AXIS2_PLACEMENT_3D ( 'NONE', #80491, #72778, #10545 ) ;
#17555 = DIRECTION ( 'NONE',  ( 0.000000000000000000, 0.000000000000000000, 1.000000000000000000 ) ) ;
#17556 = CARTESIAN_POINT ( 'NONE',  ( 110.8778075460668617, -45.97466301617711792, 17.88763232902943301 ) ) ;
#17557 = VERTEX_POINT ( 'NONE', #35525 ) ;
#17558 = AXIS2_PLACEMENT_3D ( 'NONE', #46350, #52702, #17778 ) ;
#17559 = ORIENTED_EDGE ( 'NONE', *, *, #83652, .T. ) ;
#17560 = ORIENTED_EDGE ( 'NONE', *, *, #61272, .T. ) ;
#17561 = CARTESIAN_POINT ( 'NONE',  ( 116.3142130228717264, -37.48801553205211690, 186.5795189410199555 ) ) ;
#17562 = CARTESIAN_POINT ( 'NONE',  ( 96.61701384456422659, -37.56428313387978335, 101.3899109901969524 ) ) ;
#17563 = CARTESIAN_POINT ( 'NONE',  ( 116.7246412902989903, -32.86309880586077270, 54.12991099019698282 ) ) ;
#17564 = CARTESIAN_POINT ( 'NONE',  ( 115.0348970223676872, -42.91145613756582833, 253.3023792191510495 ) ) ;
#17565 = CARTESIAN_POINT ( 'NONE',  ( 112.3521431160374675, -140.6784471599409301, 245.8674624188659834 ) ) ;
#17566 = CARTESIAN_POINT ( 'NONE',  ( 85.72499999999999432, 66.67499999999999716, 346.0750000000000455 ) ) ;
#17567 = CARTESIAN_POINT ( 'NONE',  ( 103.8073934974285066, -26.82688076304711444, 161.3299109901969643 ) ) ;
#17568 = CARTESIAN_POINT ( 'NONE',  ( 213.4642805167760002, 52.73749999999999716, -54.26046066215670294 ) ) ;
#17569 = ORIENTED_EDGE ( 'NONE', *, *, #4425, .T. ) ;
#17570 = CARTESIAN_POINT ( 'NONE',  ( 151.5667039024483245, -48.82844715993591223, 300.4678068554149490 ) ) ;
#17571 = VERTEX_POINT ( 'NONE', #29621 ) ;
#17572 = AXIS2_PLACEMENT_3D ( 'NONE', #74724, #61084, #40184 ) ;
#17573 = ORIENTED_EDGE ( 'NONE', *, *, #9055, .T. ) ;
#17574 = CARTESIAN_POINT ( 'NONE',  ( 97.81168895331838087, -40.51742574516882200, 287.6356252759109680 ) ) ;
#17575 = EDGE_LOOP ( 'NONE', ( #24474, #55854, #89084, #38228 ) ) ;
#17576 = ORIENTED_EDGE ( 'NONE', *, *, #10799, .F. ) ;
#17577 = AXIS2_PLACEMENT_3D ( 'NONE', #13137, #34453, #27647 ) ;
#17578 = FACE_BOUND ( 'NONE', #77234, .T. ) ;
#17579 = ORIENTED_EDGE ( 'NONE', *, *, #20266, .F. ) ;
#17580 = DIRECTION ( 'NONE',  ( 1.000000000000000000, 0.000000000000000000, 0.000000000000000000 ) ) ;
#17581 = CARTESIAN_POINT ( 'NONE',  ( 104.7595363604009435, -46.89630637601933927, 72.39848241876795498 ) ) ;
#17582 = CARTESIAN_POINT ( 'NONE',  ( -123.4696824136392053, 101.5999999999999943, -179.8898777604655095 ) ) ;
#17583 = EDGE_CURVE ( 'NONE', #56759, #61997, #78696, .T. ) ;
#17584 = DIRECTION ( 'NONE',  ( 0.000000000000000000, 0.000000000000000000, 1.000000000000000000 ) ) ;
#17585 = DIRECTION ( 'NONE',  ( 0.000000000000000000, -1.000000000000000000, 0.000000000000000000 ) ) ;
#17586 = EDGE_CURVE ( 'NONE', #49295, #26572, #77027, .T. ) ;
#17587 = CARTESIAN_POINT ( 'NONE',  ( 102.0418483691416469, -28.29933337693050532, 85.50419670448295051 ) ) ;
#17589 = CARTESIAN_POINT ( 'NONE',  ( 103.5497706991577189, -26.90106182813410740, 186.3499109901969746 ) ) ;
#17588 = DIRECTION ( 'NONE',  ( 0.8660254037844392627, 0.000000000000000000, 0.4999999999999990563 ) ) ;
#17590 = PLANE ( 'NONE',  #68370 ) ;
#17591 = CARTESIAN_POINT ( 'NONE',  ( 107.0664832912739541, -36.72944715994095333, 305.7008218191032256 ) ) ;
#17592 = ORIENTED_EDGE ( 'NONE', *, *, #20803, .F. ) ;
#17593 = VECTOR ( 'NONE', #49965, 1000.000000000000000 ) ;
#17594 = DIRECTION ( 'NONE',  ( 0.000000000000000000, 0.000000000000000000, -1.000000000000000000 ) ) ;
#17595 = ADVANCED_FACE ( 'NONE', ( #17339 ), #85949, .F. ) ;
#17596 = CARTESIAN_POINT ( 'NONE',  ( 74.38348329127296665, -1.929447159941392931, 361.9756252759109998 ) ) ;
#17597 = CARTESIAN_POINT ( 'NONE',  ( 97.81469011401388514, -40.51612824417846070, 136.6360017533206417 ) ) ;
#17598 = VECTOR ( 'NONE', #78935, 1000.000000000000000 ) ;
#17599 = EDGE_CURVE ( 'NONE', #21095, #78359, #50944, .T. ) ;
#17600 = FACE_OUTER_BOUND ( 'NONE', #42409, .T. ) ;
#17602 = ORIENTED_EDGE ( 'NONE', *, *, #32291, .F. ) ;
#17601 = CARTESIAN_POINT ( 'NONE',  ( 108.1864980337677764, -47.13868502929719284, 202.6613395616249704 ) ) ;
#17603 = DIRECTION ( 'NONE',  ( 0.8571673007021091140, -8.250245410175212261E-16, 0.5150380749100597066 ) ) ;
#17604 = CARTESIAN_POINT ( 'NONE',  ( 106.1364166314141499, -47.76666518589912869, 258.4975300378158636 ) ) ;
#17605 = CARTESIAN_POINT ( 'NONE',  ( 113.3575164265628672, -45.09699625868619677, 139.0899109901969553 ) ) ;
#17606 = PLANE ( 'NONE',  #7017 ) ;
#17607 = CARTESIAN_POINT ( 'NONE',  ( 82.76352869194737139, -37.26660482608630076, 6.827192804309592411 ) ) ;
#17608 = DIRECTION ( 'NONE',  ( -3.999999999999999995E-14, 1.000000000000000000, -4.100000000000000342E-29 ) ) ;
#17609 = DIRECTION ( 'NONE',  ( -0.000000000000000000, -0.000000000000000000, -1.000000000000000000 ) ) ;
#17610 = ORIENTED_EDGE ( 'NONE', *, *, #70053, .T. ) ;
#17611 = ADVANCED_FACE ( 'NONE', ( #51380, #77782 ), #51826, .T. ) ;
#17612 = ORIENTED_EDGE ( 'NONE', *, *, #86231, .T. ) ;
#17613 = ORIENTED_EDGE ( 'NONE', *, *, #25792, .F. ) ;
#17614 = CONICAL_SURFACE ( 'NONE', #68383, 5.800000000000000711, 0.7853981633974476129 ) ;
#17615 = ORIENTED_EDGE ( 'NONE', *, *, #40574, .F. ) ;
#17616 = DIRECTION ( 'NONE',  ( 0.000000000000000000, 0.000000000000000000, -1.000000000000000000 ) ) ;
#17617 = CARTESIAN_POINT ( 'NONE',  ( 118.3409026158823281, -33.07932318167559060, 280.0756252759109657 ) ) ;
#17618 = DIRECTION ( 'NONE',  ( 1.000000000000000078E-15, -1.000000000000000083E-30, -1.000000000000000000 ) ) ;
#17619 = DIRECTION ( 'NONE',  ( 1.000000000000000000, -5.337610695313248426E-16, 0.000000000000000000 ) ) ;
#17620 = ADVANCED_FACE ( 'NONE', ( #1480 ), #15560, .F. ) ;
#17622 = CARTESIAN_POINT ( 'NONE',  ( 90.81844170390269255, 75.15251084995274766, 76.20754074253750332 ) ) ;
#17621 = DIRECTION ( 'NONE',  ( 1.000000000000000000, 3.999999999999999995E-14, -4.193851878741028267E-47 ) ) ;
#17623 = CIRCLE ( 'NONE', #58266, 16.00000000000000000 ) ;
#17624 = CARTESIAN_POINT ( 'NONE',  ( 115.9822952273240304, -35.14169155943780964, 198.3771817328379825 ) ) ;
#17625 = EDGE_LOOP ( 'NONE', ( #6405, #75395 ) ) ;
#17626 = EDGE_CURVE ( 'NONE', #121, #39820, #58646, .T. ) ;
#17627 = ORIENTED_EDGE ( 'NONE', *, *, #10631, .T. ) ;
#17628 = ORIENTED_EDGE ( 'NONE', *, *, #1906, .F. ) ;
#17629 = VECTOR ( 'NONE', #53040, 1000.000000000000000 ) ;
#17630 = CARTESIAN_POINT ( 'NONE',  ( 116.3212776292296127, -32.94146857471318413, 287.6356252759109680 ) ) ;
#17631 = CARTESIAN_POINT ( 'NONE',  ( 97.81555862303321192, -40.52686724714011746, 181.6364370671610118 ) ) ;
#17632 = LINE ( 'NONE', #31695, #21446 ) ;
#17633 = CARTESIAN_POINT ( 'NONE',  ( 111.4141554795631492, -28.97316737322958957, 31.10158330589696263 ) ) ;
#17634 = CARTESIAN_POINT ( 'NONE',  ( 117.9583070260533901, 87.03046781249440755, -11.89069406032356824 ) ) ;
#17635 = DIRECTION ( 'NONE',  ( 0.000000000000000000, 0.000000000000000000, 1.000000000000000000 ) ) ;
#17636 = CARTESIAN_POINT ( 'NONE',  ( 107.0664832912739968, -36.72944715994100306, 287.6356252759109680 ) ) ;
#17638 = ORIENTED_EDGE ( 'NONE', *, *, #39096, .F. ) ;
#17637 = VECTOR ( 'NONE', #18296, 1000.000000000000000 ) ;
#17639 = DIRECTION ( 'NONE',  ( 0.000000000000000000, 0.8660254037844387076, 0.4999999999999998890 ) ) ;
#17640 = ORIENTED_EDGE ( 'NONE', *, *, #62, .F. ) ;
#17641 = ADVANCED_FACE ( 'NONE', ( #35986 ), #30518, .T. ) ;
#17642 = PLANE ( 'NONE',  #40833 ) ;
#17643 = CARTESIAN_POINT ( 'NONE',  ( 113.7275377883433549, -41.44750597731145092, 51.15380465530594734 ) ) ;
#17644 = AXIS2_PLACEMENT_3D ( 'NONE', #12919, #18827, #32894 ) ;
#17645 = LINE ( 'NONE', #24463, #31949 ) ;
#17646 = LINE ( 'NONE', #18077, #43195 ) ;
#17647 = CIRCLE ( 'NONE', #85888, 24.50000000000000711 ) ;
#17648 = DIRECTION ( 'NONE',  ( 0.000000000000000000, 1.000000000000000000, 0.000000000000000000 ) ) ;
#17649 = ORIENTED_EDGE ( 'NONE', *, *, #83046, .T. ) ;
#17650 = LINE ( 'NONE', #66223, #76955 ) ;
#17651 = CARTESIAN_POINT ( 'NONE',  ( 119.9576544348878713, 56.34114634768905461, -51.52716989460228802 ) ) ;
#17652 = VERTEX_POINT ( 'NONE', #63699 ) ;
#17653 = CARTESIAN_POINT ( 'NONE',  ( 98.33613682261365341, -42.42752411612296015, 101.7870538473399620 ) ) ;
#17654 = ORIENTED_EDGE ( 'NONE', *, *, #1705, .F. ) ;
#17656 = VECTOR ( 'NONE', #27969, 1000.000000000000000 ) ;
#17655 = CARTESIAN_POINT ( 'NONE',  ( 107.5092159716399181, -46.42865411040452273, 42.03527697093395687 ) ) ;
#17657 = CARTESIAN_POINT ( 'NONE',  ( 76.06670390244796920, -26.72944715994109899, 239.5838068554169809 ) ) ;
#17658 = CARTESIAN_POINT ( 'NONE',  ( 99.90998525089342763, -42.81722683197487811, 73.33110711542096283 ) ) ;
#17659 = ADVANCED_FACE ( 'NONE', ( #9188 ), #1625, .F. ) ;
#17660 = CARTESIAN_POINT ( 'NONE',  ( 82.54999999999999716, 69.84999999999999432, 358.0130000000000337 ) ) ;
#17661 = PLANE ( 'NONE',  #21207 ) ;
#17662 = CARTESIAN_POINT ( 'NONE',  ( 74.67462176122349149, -68.26729679194136224, 247.0134555675329864 ) ) ;
#17663 = CARTESIAN_POINT ( 'NONE',  ( 99.04917799727566319, -44.37196124675453746, 32.92038718067297509 ) ) ;
#17664 = LINE ( 'NONE', #23166, #59895 ) ;
#17665 = ORIENTED_EDGE ( 'NONE', *, *, #9983, .T. ) ;
#17666 = EDGE_CURVE ( 'NONE', #26264, #54446, #22824, .T. ) ;
#17667 = FACE_OUTER_BOUND ( 'NONE', #43199, .T. ) ;
#17668 = ORIENTED_EDGE ( 'NONE', *, *, #57985, .F. ) ;
#17669 = CARTESIAN_POINT ( 'NONE',  ( 77.96454488116506809, -20.51222316633940679, 2.376608873914837439 ) ) ;
#17670 = ORIENTED_EDGE ( 'NONE', *, *, #47105, .T. ) ;
#17671 = ORIENTED_EDGE ( 'NONE', *, *, #67570, .T. ) ;
#17672 = LINE ( 'NONE', #65803, #68180 ) ;
#17673 = ORIENTED_EDGE ( 'NONE', *, *, #51338, .T. ) ;
#17674 = CARTESIAN_POINT ( 'NONE',  ( 116.7732407090126827, -35.28285290846962141, 218.9441967044829482 ) ) ;
#17675 = DIRECTION ( 'NONE',  ( 6.745093096447288888E-17, 1.000000000000000000, 0.000000000000000000 ) ) ;
#17676 = CARTESIAN_POINT ( 'NONE',  ( 105.7154772411971209, -46.72385838089639520, 188.4689586021422087 ) ) ;
#17677 = CARTESIAN_POINT ( 'NONE',  ( 101.9605410436089699, -27.64034152677590583, 56.48419670448296159 ) ) ;
#17678 = CARTESIAN_POINT ( 'NONE',  ( 97.83877808327316927, -40.58304141722473446, 42.64127468446370983 ) ) ;
#17679 = ORIENTED_EDGE ( 'NONE', *, *, #64355, .F. ) ;
#17680 = CARTESIAN_POINT ( 'NONE',  ( 103.2774353142084038, -27.47509059510596074, 171.3857181134776226 ) ) ;
#17681 = CARTESIAN_POINT ( 'NONE',  ( 107.0667036193247696, -67.87844715994094713, 90.21780599115064092 ) ) ;
#17682 = AXIS2_PLACEMENT_3D ( 'NONE', #76251, #34906, #62167 ) ;
#17683 = ORIENTED_EDGE ( 'NONE', *, *, #61112, .T. ) ;
#17684 = AXIS2_PLACEMENT_3D ( 'NONE', #61127, #19356, #47928 ) ;
#17685 = DIRECTION ( 'NONE',  ( 5.512527431108029424E-15, -1.000000000000000000, 0.000000000000000000 ) ) ;
#17686 = CARTESIAN_POINT ( 'NONE',  ( 109.6408376098527242, -46.48063368938936435, 113.7820702227787137 ) ) ;
#17687 = CARTESIAN_POINT ( 'NONE',  ( 96.83034234600413015, -40.83861266248845823, 251.6422919425777138 ) ) ;
#17688 = CARTESIAN_POINT ( 'NONE',  ( 177.4809174648213741, -49.32844715993478957, 300.4678068554149490 ) ) ;
#17689 = EDGE_CURVE ( 'NONE', #27267, #2214, #78248, .T. ) ;
#17690 = CARTESIAN_POINT ( 'NONE',  ( -446.0240000000000009, 104.7749999999999915, -1.387778780781445991E-14 ) ) ;
#17691 = CARTESIAN_POINT ( 'NONE',  ( 77.53258422225754032, -37.79809288067778539, 2.811527366592890154 ) ) ;
#17692 = EDGE_CURVE ( 'NONE', #80451, #19992, #29170, .T. ) ;
#17693 = CARTESIAN_POINT ( 'NONE',  ( 110.8947914379136961, -29.09399076817903662, 279.1295626852197529 ) ) ;
#17695 = CARTESIAN_POINT ( 'NONE',  ( 98.66494773507974969, -43.87633619481167102, 72.89943479972099283 ) ) ;
#17694 = DIRECTION ( 'NONE',  ( 0.000000000000000000, -0.4999999999999921174, -0.8660254037844431485 ) ) ;
#17696 = CARTESIAN_POINT ( 'NONE',  ( 109.5717151936057689, 58.27256190523081614, 70.98527193250401979 ) ) ;
#17697 = CARTESIAN_POINT ( 'NONE',  ( 116.9635770353169733, -33.20817898692279613, 114.0984824187679720 ) ) ;
#17698 = EDGE_LOOP ( 'NONE', ( #32069, #70301, #73547, #29112, #75800 ) ) ;
#17699 = LINE ( 'NONE', #45379, #20521 ) ;
#17700 = VERTEX_POINT ( 'NONE', #44574 ) ;
#17701 = DIRECTION ( 'NONE',  ( 0.000000000000000000, 0.000000000000000000, -1.000000000000000000 ) ) ;
#17702 = EDGE_CURVE ( 'NONE', #60793, #45550, #57310, .T. ) ;
#17703 = CARTESIAN_POINT ( 'NONE',  ( 172.5664832912729878, -27.82844715994070484, 138.9256252759119832 ) ) ;
#17704 = PRODUCT_DEFINITION_SHAPE ( 'NONE', 'NONE',  #89938 ) ;
#17705 = DIRECTION ( 'NONE',  ( 0.000000000000000000, 1.000000000000000000, 0.000000000000000000 ) ) ;
#17706 = ORIENTED_EDGE ( 'NONE', *, *, #20153, .F. ) ;
#17707 = LINE ( 'NONE', #67183, #21574 ) ;
#17708 = EDGE_CURVE ( 'NONE', #27001, #10481, #65482, .T. ) ;
#17710 = ORIENTED_EDGE ( 'NONE', *, *, #23651, .T. ) ;
#17709 = CARTESIAN_POINT ( 'NONE',  ( 114.8040440383551157, -44.68828107661028781, 118.2022919425779719 ) ) ;
#17711 = CARTESIAN_POINT ( 'NONE',  ( 0.000000000000000000, 1.270000000000000018, 0.000000000000000000 ) ) ;
#17712 = CARTESIAN_POINT ( 'NONE',  ( 131.3179999999999836, 53.97500000000000142, 50.79999999999999716 ) ) ;
#17713 = VECTOR ( 'NONE', #2418, 999.9999999999998863 ) ;
#17714 = DIRECTION ( 'NONE',  ( 0.000000000000000000, 3.785359618865284342E-16, -1.000000000000000000 ) ) ;
#17715 = ORIENTED_EDGE ( 'NONE', *, *, #59116, .T. ) ;
#17716 = ADVANCED_FACE ( 'NONE', ( #30959 ), #16005, .F. ) ;
#17717 = AXIS2_PLACEMENT_3D ( 'NONE', #38892, #80701, #87506 ) ;
#17718 = CARTESIAN_POINT ( 'NONE',  ( 117.1850550582282580, -34.12927998004249730, 124.0270538473399426 ) ) ;
#17719 = DIRECTION ( 'NONE',  ( 1.000000000000000000, 0.000000000000000000, 7.237399417378975455E-15 ) ) ;
#17720 = DIRECTION ( 'NONE',  ( 1.000000000000000000, 4.299999999999999979E-14, 1.000000000000000078E-15 ) ) ;
#17721 = CARTESIAN_POINT ( 'NONE',  ( 44.45000000000000284, 111.1250000000000000, 219.0749999999999886 ) ) ;
#17722 = EDGE_LOOP ( 'NONE', ( #29195, #59870, #40794, #35210 ) ) ;
#17723 = EDGE_CURVE ( 'NONE', #89397, #4393, #64594, .T. ) ;
#17724 = ORIENTED_EDGE ( 'NONE', *, *, #59489, .T. ) ;
#17725 = CARTESIAN_POINT ( 'NONE',  ( 107.0667039024470313, -104.2784471599420755, -19.78219314458201694 ) ) ;
#17726 = LINE ( 'NONE', #51325, #78826 ) ;
#17727 = VECTOR ( 'NONE', #18707, 1000.000000000000114 ) ;
#17728 = CARTESIAN_POINT ( 'NONE',  ( 107.0664832912739968, -36.72944715994100306, 287.6356252759109680 ) ) ;
#17730 = DIRECTION ( 'NONE',  ( 0.000000000000000000, 0.000000000000000000, -1.000000000000000000 ) ) ;
#17729 = CARTESIAN_POINT ( 'NONE',  ( 97.95250717983367394, -32.49412669507730556, 3.024967495036141596 ) ) ;
#17731 = CARTESIAN_POINT ( 'NONE',  ( 0.000000000000000000, 61.59999999999999432, 130.5560000000000116 ) ) ;
#17732 = EDGE_LOOP ( 'NONE', ( #46371, #44226, #64199, #31171 ) ) ;
#17733 = FACE_OUTER_BOUND ( 'NONE', #11346, .T. ) ;
#17734 = CARTESIAN_POINT ( 'NONE',  ( 112.6571330189592430, -45.46348522128858605, 214.0175300378159591 ) ) ;
#17736 = VERTEX_POINT ( 'NONE', #33196 ) ;
#17735 = LINE ( 'NONE', #31800, #13922 ) ;
#17737 = AXIS2_PLACEMENT_3D ( 'NONE', #30361, #85786, #23560 ) ;
#17738 = CARTESIAN_POINT ( 'NONE',  ( 97.54819157151555942, -32.61351373332772852, 57.01372051400599616 ) ) ;
#17739 = CARTESIAN_POINT ( 'NONE',  ( 99.08981029112005956, -42.79583336390666659, 51.84399569144299136 ) ) ;
#17740 = LINE ( 'NONE', #66317, #15210 ) ;
#17741 = DIRECTION ( 'NONE',  ( 0.000000000000000000, -1.000000000000000000, 0.000000000000000000 ) ) ;
#17742 = VERTEX_POINT ( 'NONE', #25481 ) ;
#17743 = FACE_BOUND ( 'NONE', #37019, .T. ) ;
#17744 = ORIENTED_EDGE ( 'NONE', *, *, #35761, .T. ) ;
#17745 = VECTOR ( 'NONE', #732, 1000.000000000000000 ) ;
#17746 = ORIENTED_EDGE ( 'NONE', *, *, #12991, .F. ) ;
#17747 = ADVANCED_FACE ( 'NONE', ( #66359 ), #31845, .F. ) ;
#17748 = CARTESIAN_POINT ( 'NONE',  ( 99.68253537205306714, -30.91964177047806217, 197.2396785439919711 ) ) ;
#17749 = VECTOR ( 'NONE', #40204, 1000.000000000000000 ) ;
#17750 = DIRECTION ( 'NONE',  ( 0.000000000000000000, 0.000000000000000000, 1.000000000000000000 ) ) ;
#17751 = CARTESIAN_POINT ( 'NONE',  ( -98.83759631548484492, 90.93932679091001603, 85.30153658290403484 ) ) ;
#17752 = DIRECTION ( 'NONE',  ( -4.299999999999999979E-14, 1.000000000000000000, 0.000000000000000000 ) ) ;
#17753 = PLANE ( 'NONE',  #19795 ) ;
#17754 = ORIENTED_EDGE ( 'NONE', *, *, #67015, .F. ) ;
#17755 = LINE ( 'NONE', #19535, #16012 ) ;
#17756 = CARTESIAN_POINT ( 'NONE',  ( 31.56670390244800117, -33.35206098992711077, 342.9256252759109884 ) ) ;
#17757 = ORIENTED_EDGE ( 'NONE', *, *, #49169, .F. ) ;
#17758 = CARTESIAN_POINT ( 'NONE',  ( 113.7419942178973287, -29.10023054337252546, 289.5032443235301116 ) ) ;
#17759 = CARTESIAN_POINT ( 'NONE',  ( 0.8389232435964502077, 95.25000000000004263, 118.5560000000000542 ) ) ;
#17760 = ORIENTED_EDGE ( 'NONE', *, *, #25131, .F. ) ;
#17761 = CIRCLE ( 'NONE', #6165, 9.425000000000000711 ) ;
#17762 = CARTESIAN_POINT ( 'NONE',  ( 113.1782937666078510, -44.75186859622988322, 83.09395860877987161 ) ) ;
#17763 = CARTESIAN_POINT ( 'NONE',  ( 124.9629318080292393, -56.47944715994101728, -5.074374724089012467 ) ) ;
#17764 = CARTESIAN_POINT ( 'NONE',  ( 156.5667039024484666, -48.82844715993568485, 139.7178068554149775 ) ) ;
#17765 = DIRECTION ( 'NONE',  ( 0.000000000000000000, 0.000000000000000000, -1.000000000000000000 ) ) ;
#17766 = CARTESIAN_POINT ( 'NONE',  ( 101.4018018619443922, -46.27454447023805528, 203.1622919425779514 ) ) ;
#17767 = CARTESIAN_POINT ( 'NONE',  ( 82.56670390244703128, -104.2784471599409670, 24.21780685541800082 ) ) ;
#17768 = ORIENTED_EDGE ( 'NONE', *, *, #11444, .T. ) ;
#17770 = EDGE_CURVE ( 'NONE', #14401, #67672, #29639, .T. ) ;
#17769 = VECTOR ( 'NONE', #33875, 1000.000000000000000 ) ;
#17771 = CARTESIAN_POINT ( 'NONE',  ( 97.77052560236188583, -29.30002703792375485, 41.78991099019596334 ) ) ;
#17772 = CARTESIAN_POINT ( 'NONE',  ( 194.5667039024479834, -67.87844715994100397, 310.9178068554150514 ) ) ;
#17773 = VERTEX_POINT ( 'NONE', #87712 ) ;
#17774 = ORIENTED_EDGE ( 'NONE', *, *, #42250, .T. ) ;
#17775 = AXIS2_PLACEMENT_3D ( 'NONE', #56572, #715, #41586 ) ;
#17776 = CARTESIAN_POINT ( 'NONE',  ( 82.16842210270853286, -16.94667169166570986, 2.376609173400793473 ) ) ;
#17777 = DIRECTION ( 'NONE',  ( -4.237773401492740281E-14, 1.000000000000000000, 0.000000000000000000 ) ) ;
#17778 = DIRECTION ( 'NONE',  ( 0.000000000000000000, 0.000000000000000000, 1.000000000000000000 ) ) ;
#17779 = CARTESIAN_POINT ( 'NONE',  ( 98.14730025337767927, -34.17130281729839680, 138.9223760838769692 ) ) ;
#17780 = CARTESIAN_POINT ( 'NONE',  ( 104.1798084317939725, -26.65242854998196265, 221.2984824187679465 ) ) ;
#17781 = FACE_OUTER_BOUND ( 'NONE', #34322, .T. ) ;
#17782 = ORIENTED_EDGE ( 'NONE', *, *, #69912, .F. ) ;
#17783 = CYLINDRICAL_SURFACE ( 'NONE', #31677, 12.44600000000001216 ) ;
#17784 = EDGE_LOOP ( 'NONE', ( #25929, #58481, #51569, #80238, #15178, #88658 ) ) ;
#17785 = ORIENTED_EDGE ( 'NONE', *, *, #27463, .T. ) ;
#17786 = FACE_OUTER_BOUND ( 'NONE', #62534, .T. ) ;
#17787 = EDGE_LOOP ( 'NONE', ( #23547, #11676, #2105, #23295 ) ) ;
#17788 = VERTEX_POINT ( 'NONE', #72747 ) ;
#17789 = CARTESIAN_POINT ( 'NONE',  ( -27.27158787008326968, 184.0000000000000000, 90.32146847885337593 ) ) ;
#17790 = DIRECTION ( 'NONE',  ( -0.7071067811865490160, 0.000000000000000000, 0.7071067811865461294 ) ) ;
#17791 = CARTESIAN_POINT ( 'NONE',  ( 162.7866693523280048, -29.62846900982320264, -5.074374724088000832 ) ) ;
#17792 = EDGE_CURVE ( 'NONE', #49775, #29846, #3701, .T. ) ;
#17793 = CARTESIAN_POINT ( 'NONE',  ( 102.7266122873206768, -44.08618886718738139, 161.5752769709339702 ) ) ;
#17794 = CARTESIAN_POINT ( 'NONE',  ( 113.7702145813751571, -29.06794043779556347, 289.5032443235301116 ) ) ;
#17795 = ORIENTED_EDGE ( 'NONE', *, *, #83860, .F. ) ;
#17796 = CIRCLE ( 'NONE', #80125, 5.599999999999994316 ) ;
#17797 = ADVANCED_FACE ( 'NONE', ( #87273 ), #81810, .T. ) ;
#17798 = CARTESIAN_POINT ( 'NONE',  ( 44.45000000000000284, 69.84999999999999432, 260.3500000000000227 ) ) ;
#17799 = EDGE_CURVE ( 'NONE', #30283, #18647, #69759, .T. ) ;
#17800 = ORIENTED_EDGE ( 'NONE', *, *, #63562, .T. ) ;
#17801 = CARTESIAN_POINT ( 'NONE',  ( 61.68306511546568061, -72.55869591834559174, 394.9756252759102040 ) ) ;
#17802 = EDGE_CURVE ( 'NONE', #34850, #58230, #30593, .T. ) ;
#17803 = VERTEX_POINT ( 'NONE', #18669 ) ;
#17804 = CARTESIAN_POINT ( 'NONE',  ( 163.0664832912739826, 12.92155284005902516, 333.4006252759110112 ) ) ;
#17805 = CARTESIAN_POINT ( 'NONE',  ( 116.8177678418650771, -34.15541691211213760, 34.03146788054147720 ) ) ;
#17806 = DIRECTION ( 'NONE',  ( 0.000000000000000000, 0.000000000000000000, -1.000000000000000000 ) ) ;
#17807 = AXIS2_PLACEMENT_3D ( 'NONE', #43570, #29515, #71746 ) ;
#17808 = FACE_OUTER_BOUND ( 'NONE', #3589, .T. ) ;
#17809 = EDGE_LOOP ( 'NONE', ( #25507, #53310, #62024, #63467 ) ) ;
#17810 = CARTESIAN_POINT ( 'NONE',  ( 100.4651824673786393, -27.83460210401261747, 35.59657765686397113 ) ) ;
#17811 = CARTESIAN_POINT ( 'NONE',  ( 111.4336192290781753, -46.24370506310440732, 23.91848241876792969 ) ) ;
#17812 = SURFACE_SIDE_STYLE ('',( #87307 ) ) ;
#17814 = CARTESIAN_POINT ( 'NONE',  ( 68.96386331618904819, -139.0368364878925718, 246.8410557163890076 ) ) ;
#17813 = LINE ( 'NONE', #3301, #60742 ) ;
#17815 = CARTESIAN_POINT ( 'NONE',  ( 82.10814995794051185, 12.92155284005802685, 335.5992267699911054 ) ) ;
#17816 = DIRECTION ( 'NONE',  ( 0.000000000000000000, 0.000000000000000000, -1.000000000000000000 ) ) ;
#17817 = LINE ( 'NONE', #74127, #29571 ) ;
#17818 = ADVANCED_FACE ( 'NONE', ( #80921 ), #4600, .F. ) ;
#17819 = CARTESIAN_POINT ( 'NONE',  ( 107.0664832912739257, -50.72944715994096043, 315.1356252759112522 ) ) ;
#17820 = FACE_BOUND ( 'NONE', #72094, .T. ) ;
#17821 = DIRECTION ( 'NONE',  ( 0.000000000000000000, -1.000000000000000000, 0.000000000000000000 ) ) ;
#17822 = CARTESIAN_POINT ( 'NONE',  ( 115.9827728363227664, -42.21636132903250171, 18.38705384733896153 ) ) ;
#17823 = CARTESIAN_POINT ( 'NONE',  ( 117.7763469108053869, -31.65663365956905650, 210.1784824187679703 ) ) ;
#17824 = CARTESIAN_POINT ( 'NONE',  ( 112.7535375185862705, -27.22457367525289129, 50.65943479972101215 ) ) ;
#17826 = DIRECTION ( 'NONE',  ( 1.000000000000000000, 0.000000000000000000, 0.000000000000000000 ) ) ;
#17825 = LINE ( 'NONE', #2423, #68219 ) ;
#17827 = CARTESIAN_POINT ( 'NONE',  ( 80.06648329127401098, -33.97944715994105991, 1.625625275910943746 ) ) ;
#17828 = AXIS2_PLACEMENT_3D ( 'NONE', #50306, #1738, #55319 ) ;
#17829 = VERTEX_POINT ( 'NONE', #18221 ) ;
#17830 = DIRECTION ( 'NONE',  ( 0.000000000000000000, 0.000000000000000000, -1.000000000000000000 ) ) ;
#17831 = ORIENTED_EDGE ( 'NONE', *, *, #18606, .T. ) ;
#17832 = VECTOR ( 'NONE', #12454, 1000.000000000000000 ) ;
#17833 = CARTESIAN_POINT ( 'NONE',  ( 117.3261810260835603, -38.23854875528750341, 69.72229194257801055 ) ) ;
#17835 = ORIENTED_EDGE ( 'NONE', *, *, #54579, .F. ) ;
#17834 = CARTESIAN_POINT ( 'NONE',  ( 172.5664832912740110, -32.07844715994070839, 138.9256252759119832 ) ) ;
#17836 = CARTESIAN_POINT ( 'NONE',  ( 107.0667039024470313, -104.2784471599409528, 25.71780685541800437 ) ) ;
#17837 = CARTESIAN_POINT ( 'NONE',  ( 116.8642987764956160, -41.79567201640973195, 239.4346728949589647 ) ) ;
#17838 = DIRECTION ( 'NONE',  ( -1.000000000000000000, -8.163404592832032979E-16, 0.000000000000000000 ) ) ;
#17839 = DIRECTION ( 'NONE',  ( -0.000000000000000000, 1.000000000000000000, 0.000000000000000000 ) ) ;
#17840 = DIRECTION ( 'NONE',  ( 0.0001713722456127291687, -0.9999999853157766072, -1.713722456127291814E-19 ) ) ;
#17841 = CARTESIAN_POINT ( 'NONE',  ( 82.89895571708365196, 82.54999999999999716, -100.8594679592203818 ) ) ;
#17842 = CARTESIAN_POINT ( 'NONE',  ( 133.3217830637533439, -39.37853523628599106, 1.709393643968337706 ) ) ;
#17843 = DIRECTION ( 'NONE',  ( 0.7071067811989691920, 0.7071067811741258424, -2.899137802813799626E-29 ) ) ;
#17844 = CARTESIAN_POINT ( 'NONE',  ( 99.59366209610195142, -44.96145431533982162, 156.9899109901969609 ) ) ;
#17845 = ORIENTED_EDGE ( 'NONE', *, *, #79684, .F. ) ;
#17846 = EDGE_LOOP ( 'NONE', ( #40483, #39610, #4578, #48191, #88738, #81816, #59550, #36097 ) ) ;
#17847 = ADVANCED_FACE ( 'NONE', ( #11863 ), #39556, .F. ) ;
#17848 = CARTESIAN_POINT ( 'NONE',  ( 116.0163176773587708, -41.35234337494321721, 89.87872616303998541 ) ) ;
#17849 = CARTESIAN_POINT ( 'NONE',  ( 107.0664832912739968, -36.72944715994100306, 287.6356252759109680 ) ) ;
#17851 = CARTESIAN_POINT ( 'NONE',  ( 168.0371591254543375, -48.62818131005509770, 300.4678068554149490 ) ) ;
#17850 = CARTESIAN_POINT ( 'NONE',  ( 118.0655259830058270, -38.35211242607483939, 219.7099109901959935 ) ) ;
#17852 = CIRCLE ( 'NONE', #58500, 0.5000000000000004441 ) ;
#17853 = CARTESIAN_POINT ( 'NONE',  ( 59.56670390244700997, -79.67844715994098692, 85.21780685541799016 ) ) ;
#17855 = EDGE_CURVE ( 'NONE', #52976, #14490, #54052, .T. ) ;
#17854 = LINE ( 'NONE', #46433, #4603 ) ;
#17856 = CARTESIAN_POINT ( 'NONE',  ( 194.5667039024483529, -47.82844715993405771, 249.9678068554149775 ) ) ;
#17857 = LINE ( 'NONE', #23801, #37114 ) ;
#17858 = AXIS2_PLACEMENT_3D ( 'NONE', #60612, #88355, #19742 ) ;
#17859 = CARTESIAN_POINT ( 'NONE',  ( 173.9900000000000091, 101.5999999999999943, 131.6533725204182019 ) ) ;
#17860 = DIRECTION ( 'NONE',  ( 0.000000000000000000, 0.000000000000000000, -1.000000000000000000 ) ) ;
#17861 = CARTESIAN_POINT ( 'NONE',  ( 103.8142050530422438, -26.84757730287814326, 165.3299109901969643 ) ) ;
#17862 = VERTEX_POINT ( 'NONE', #19118 ) ;
#17863 = VERTEX_POINT ( 'NONE', #46798 ) ;
#17864 = CARTESIAN_POINT ( 'NONE',  ( 110.4543776057972053, -75.92700761993931735, 250.2201230397200220 ) ) ;
#17865 = CARTESIAN_POINT ( 'NONE',  ( 146.4725015627529103, -68.45085798094062568, 246.9176224039437386 ) ) ;
#17866 = CARTESIAN_POINT ( 'NONE',  ( 38.10000000000000142, 95.25000000000000000, 346.9005000000000223 ) ) ;
#17867 = CARTESIAN_POINT ( 'NONE',  ( 92.81932083335591699, -95.00417761012948858, -11.78219314458228695 ) ) ;
#17868 = AXIS2_PLACEMENT_3D ( 'NONE', #75616, #28334, #70134 ) ;
#17869 = EDGE_CURVE ( 'NONE', #83824, #7721, #32067, .T. ) ;
#17870 = DIRECTION ( 'NONE',  ( 4.299999999999999979E-14, -1.000000000000000000, 0.000000000000000000 ) ) ;
#17871 = CARTESIAN_POINT ( 'NONE',  ( 96.05373888820416539, -35.78152935435744553, 186.2461014663869889 ) ) ;
#17872 = LINE ( 'NONE', #81024, #22663 ) ;
#17873 = ORIENTED_EDGE ( 'NONE', *, *, #35940, .F. ) ;
#17875 = ORIENTED_EDGE ( 'NONE', *, *, #37377, .T. ) ;
#17874 = ORIENTED_EDGE ( 'NONE', *, *, #80174, .F. ) ;
#17876 = CARTESIAN_POINT ( 'NONE',  ( 106.2078554787763522, -46.73095241849994608, 63.50879164150141776 ) ) ;
#17877 = CARTESIAN_POINT ( 'NONE',  ( 142.8698897858160706, -0.9167816978817300289, 396.9756252759102040 ) ) ;
#17878 = CARTESIAN_POINT ( 'NONE',  ( 23.27731929905161223, 53.97500000000000142, 30.16249999999999076 ) ) ;
#17879 = CARTESIAN_POINT ( 'NONE',  ( 103.6908924260029607, -28.08645471411401928, 18.19094751244793073 ) ) ;
#17880 = EDGE_CURVE ( 'NONE', #87303, #11589, #10954, .T. ) ;
#17881 = LINE ( 'NONE', #38765, #69594 ) ;
#17882 = ORIENTED_EDGE ( 'NONE', *, *, #4708, .T. ) ;
#17883 = DIRECTION ( 'NONE',  ( 0.000000000000000000, 0.000000000000000000, -1.000000000000000000 ) ) ;
#17884 = CARTESIAN_POINT ( 'NONE',  ( 182.5667039024469886, -33.35206098992650681, 117.4678068554150627 ) ) ;
#17885 = VERTEX_POINT ( 'NONE', #20022 ) ;
#17886 = ORIENTED_EDGE ( 'NONE', *, *, #32967, .T. ) ;
#17887 = CONICAL_SURFACE ( 'NONE', #83206, 15.00000000000000000, 0.7853981633974691512 ) ;
#17888 = DIRECTION ( 'NONE',  ( 0.000000000000000000, 0.000000000000000000, 1.000000000000000000 ) ) ;
#17889 = VERTEX_POINT ( 'NONE', #69964 ) ;
#17890 = VERTEX_POINT ( 'NONE', #83598 ) ;
#17891 = DIRECTION ( 'NONE',  ( 0.000000000000000000, 0.000000000000000000, 1.000000000000000000 ) ) ;
#17892 = VECTOR ( 'NONE', #61903, 1000.000000000000000 ) ;
#17893 = CARTESIAN_POINT ( 'NONE',  ( 113.4185696802295809, -42.43971249784851096, 37.66670554236295487 ) ) ;
#17894 = CARTESIAN_POINT ( 'NONE',  ( 96.65194983638532733, -35.53535514585328059, 206.2356252759109623 ) ) ;
#17895 = CARTESIAN_POINT ( 'NONE',  ( 97.69433714244404143, -41.24514667321086847, 171.6841967044819626 ) ) ;
#17896 = CARTESIAN_POINT ( 'NONE',  ( 107.3864418959535527, -26.30668689864625875, 322.4523926293242653 ) ) ;
#17897 = CARTESIAN_POINT ( 'NONE',  ( 110.8926193997603065, -26.99384161864454157, 265.7784824187680783 ) ) ;
#17898 = CARTESIAN_POINT ( 'NONE',  ( 72.96458098368650269, 127.0000000000000000, 72.96458098368729850 ) ) ;
#17899 = ADVANCED_FACE ( 'NONE', ( #68172 ), #5953, .T. ) ;
#17900 = DIRECTION ( 'NONE',  ( -0.000000000000000000, -0.000000000000000000, -1.000000000000000000 ) ) ;
#17901 = ORIENTED_EDGE ( 'NONE', *, *, #70688, .F. ) ;
#17902 = ORIENTED_EDGE ( 'NONE', *, *, #16409, .T. ) ;
#17903 = CARTESIAN_POINT ( 'NONE',  ( 97.81169822462854313, -40.51742973538109993, 111.6355314416972391 ) ) ;
#17904 = CARTESIAN_POINT ( 'NONE',  ( 113.8278214188052999, -26.93592357317604424, 239.5956252759109759 ) ) ;
#17905 = VERTEX_POINT ( 'NONE', #40892 ) ;
#17906 = CARTESIAN_POINT ( 'NONE',  ( 107.6545119506432258, -47.76725988480858121, 197.6308633711489620 ) ) ;
#17907 = CARTESIAN_POINT ( 'NONE',  ( 270.8910000000000196, 65.43750000000000000, -67.11950000000000216 ) ) ;
#17908 = AXIS2_PLACEMENT_3D ( 'NONE', #7124, #36170, #14845 ) ;
#17909 = CARTESIAN_POINT ( 'NONE',  ( 138.0667039024479834, -26.72944715994091069, 199.5838068554170093 ) ) ;
#17910 = CARTESIAN_POINT ( 'NONE',  ( 91.06648329127391150, -36.72944715993925513, -5.074374724089045330 ) ) ;
#17911 = LINE ( 'NONE', #4741, #70311 ) ;
#17914 = CARTESIAN_POINT ( 'NONE',  ( 116.2977993645975232, -41.52656014244012539, 284.4441967044824082 ) ) ;
#17913 = CARTESIAN_POINT ( 'NONE',  ( 127.0667052882549797, -71.37844715994091871, 55.21780685541800437 ) ) ;
#17912 = LINE ( 'NONE', #16152, #82574 ) ;
#17915 = DIRECTION ( 'NONE',  ( 0.000000000000000000, 0.000000000000000000, -1.000000000000000000 ) ) ;
#17916 = DIRECTION ( 'NONE',  ( -4.299999999999999979E-14, 1.000000000000000000, 0.000000000000000000 ) ) ;
#17917 = FACE_OUTER_BOUND ( 'NONE', #32518, .T. ) ;
#17918 = EDGE_CURVE ( 'NONE', #4456, #18085, #75438, .T. ) ;
#17919 = VECTOR ( 'NONE', #28683, 1000.000000000000000 ) ;
#17920 = CARTESIAN_POINT ( 'NONE',  ( 67.90006995966258785, -137.2348498917707218, 247.1319224459439852 ) ) ;
#17921 = ADVANCED_FACE ( 'NONE', ( #75878 ), #33643, .F. ) ;
#17922 = CARTESIAN_POINT ( 'NONE',  ( 90.06670420047026937, -131.9777253117771636, 55.21780685541800437 ) ) ;
#17923 = CARTESIAN_POINT ( 'NONE',  ( 245.4909999999999854, 40.03750000000000142, -67.11950000000000216 ) ) ;
#17925 = ORIENTED_EDGE ( 'NONE', *, *, #70835, .F. ) ;
#17924 = CARTESIAN_POINT ( 'NONE',  ( 114.8707465414360058, -39.51320248554598180, 195.5838068554167251 ) ) ;
#17926 = CARTESIAN_POINT ( 'NONE',  ( 134.8178230081367133, -21.40255221908221372, 8.160479982092603279 ) ) ;
#17927 = CARTESIAN_POINT ( 'NONE',  ( 113.6281634912633223, -45.65356023013480780, 183.0689586092439640 ) ) ;
#17928 = CARTESIAN_POINT ( 'NONE',  ( 97.54238320567634446, -32.48987111900922997, 96.99276813305395706 ) ) ;
#17929 = CARTESIAN_POINT ( 'NONE',  ( 117.5177603787924170, -36.12629959281294134, 224.8727681330539667 ) ) ;
#17930 = CARTESIAN_POINT ( 'NONE',  ( 163.0664832912739826, -0.7548456658610993575, 331.7756252759120343 ) ) ;
#17931 = DIRECTION ( 'NONE',  ( -1.000000000000000000, 0.000000000000000000, 0.000000000000000000 ) ) ;
#17933 = CARTESIAN_POINT ( 'NONE',  ( 98.03457007761814168, -41.02703092026990817, 37.67959706312523593 ) ) ;
#17932 = CARTESIAN_POINT ( 'NONE',  ( 156.5667039024485518, -48.82844715993568485, 170.7178068554149775 ) ) ;
#17934 = CARTESIAN_POINT ( 'NONE',  ( 150.5667039024482960, -47.82844715993594775, 300.4678068554149490 ) ) ;
#17935 = LINE ( 'NONE', #66530, #32489 ) ;
#17936 = VECTOR ( 'NONE', #72183, 1000.000000000000000 ) ;
#17937 = CARTESIAN_POINT ( 'NONE',  ( 97.79642245614456897, -40.47996586491548499, 66.63287571918958463 ) ) ;
#17938 = EDGE_LOOP ( 'NONE', ( #78958, #17505, #66065, #56078, #48089, #39248, #24614, #31806, #20654, #31676, #4538, #69752 ) ) ;
#17939 = ORIENTED_EDGE ( 'NONE', *, *, #60959, .T. ) ;
#17940 = CARTESIAN_POINT ( 'NONE',  ( 98.52552435659306695, -36.63915763587115038, 110.7409912566489680 ) ) ;
#17942 = ORIENTED_EDGE ( 'NONE', *, *, #50924, .F. ) ;
#17941 = DIRECTION ( 'NONE',  ( 0.000000000000000000, 1.000000000000000000, 0.000000000000000000 ) ) ;
#17943 = CARTESIAN_POINT ( 'NONE',  ( 96.11054930851091171, -38.00668368623056637, 82.43086337114895912 ) ) ;
#17944 = CARTESIAN_POINT ( 'NONE',  ( 105.8881231706732962, -26.36991942434103819, 322.4846826458744431 ) ) ;
#17945 = CARTESIAN_POINT ( 'NONE',  ( 144.0667039024470739, -137.6784471599409017, 55.21780685541800437 ) ) ;
#17946 = LINE ( 'NONE', #11131, #22966 ) ;
#17947 = CARTESIAN_POINT ( 'NONE',  ( 115.0372575083174524, -42.90846256421102822, 109.3022919428230182 ) ) ;
#17948 = CARTESIAN_POINT ( 'NONE',  ( 117.4022237771662276, -37.57280582802028590, 38.77372051400595865 ) ) ;
#17949 = ORIENTED_EDGE ( 'NONE', *, *, #5222, .F. ) ;
#17950 = VERTEX_POINT ( 'NONE', #89516 ) ;
#17951 = ORIENTED_EDGE ( 'NONE', *, *, #2813, .T. ) ;
#17952 = VECTOR ( 'NONE', #23324, 1000.000000000000000 ) ;
#17953 = DIRECTION ( 'NONE',  ( -0.5000000000000069944, 0.8660254037844344888, -2.684678751731748934E-14 ) ) ;
#17955 = DIRECTION ( 'NONE',  ( -0.7071067811865187069, -0.7071067811865764385, -7.071067811865181482E-16 ) ) ;
#17954 = CARTESIAN_POINT ( 'NONE',  ( 117.0231039428182385, -39.62849705588580917, 134.5889586092439743 ) ) ;
#17956 = AXIS2_PLACEMENT_3D ( 'NONE', #55862, #71328, #84524 ) ;
#17957 = CARTESIAN_POINT ( 'NONE',  ( 71.06648329127399677, -18.82844715994099971, 17.92562527591199739 ) ) ;
#17959 = EDGE_CURVE ( 'NONE', #51171, #14599, #13220, .T. ) ;
#17958 = CARTESIAN_POINT ( 'NONE',  ( 12.27300924177314911, 79.25817979229439914, -129.9779100289732696 ) ) ;
#17960 = CARTESIAN_POINT ( 'NONE',  ( 188.5667039024485518, -48.82844715993430640, 170.7178068554150059 ) ) ;
#17961 = CARTESIAN_POINT ( 'NONE',  ( 199.3900000000000148, 59.08750000000000568, -38.10000000000000142 ) ) ;
#17962 = DIRECTION ( 'NONE',  ( -1.000000000000000000, -2.756263715554006823E-15, 0.000000000000000000 ) ) ;
#17963 = CARTESIAN_POINT ( 'NONE',  ( 96.73644666290614680, -38.23103596604165944, 66.44133956162495735 ) ) ;
#17964 = VERTEX_POINT ( 'NONE', #62690 ) ;
#17965 = EDGE_LOOP ( 'NONE', ( #29754, #51494, #5620, #89830 ) ) ;
#17966 = CARTESIAN_POINT ( 'NONE',  ( 12.03249045273852502, 86.63451674300237926, 130.0003965276981432 ) ) ;
#17967 = FACE_OUTER_BOUND ( 'NONE', #86658, .T. ) ;
#17968 = CARTESIAN_POINT ( 'NONE',  ( 80.80881079632693798, -95.93364041391161834, 250.2178068554180470 ) ) ;
#17969 = CARTESIAN_POINT ( 'NONE',  ( 112.1934831763302896, -30.37778608165438854, 162.3538046553059644 ) ) ;
#17970 = EDGE_CURVE ( 'NONE', #5764, #34865, #24818, .T. ) ;
#17971 = AXIS2_PLACEMENT_3D ( 'NONE', #20071, #6002, #68220 ) ;
#17972 = AXIS2_PLACEMENT_3D ( 'NONE', #51190, #37587, #85312 ) ;
#17973 = LINE ( 'NONE', #59745, #56149 ) ;
#17974 = ORIENTED_EDGE ( 'NONE', *, *, #61376, .T. ) ;
#17975 = ORIENTED_EDGE ( 'NONE', *, *, #50001, .T. ) ;
#17976 = EDGE_CURVE ( 'NONE', #48576, #33376, #61334, .T. ) ;
#17977 = CARTESIAN_POINT ( 'NONE',  ( 33.78129701733065815, -35.65087443492598140, 342.9256252759109884 ) ) ;
#17978 = VECTOR ( 'NONE', #73931, 1000.000000000000000 ) ;
#17979 = VERTEX_POINT ( 'NONE', #28161 ) ;
#17980 = ORIENTED_EDGE ( 'NONE', *, *, #86116, .F. ) ;
#17981 = FACE_OUTER_BOUND ( 'NONE', #58106, .T. ) ;
#17982 = ADVANCED_FACE ( 'NONE', ( #6830 ), #89061, .T. ) ;
#17983 = CARTESIAN_POINT ( 'NONE',  ( 108.6634326348915351, -27.98234008310821608, 161.3644404487539816 ) ) ;
#17984 = EDGE_CURVE ( 'NONE', #62096, #9843, #27724, .T. ) ;
#17985 = CARTESIAN_POINT ( 'NONE',  ( 122.2221484686747743, -98.95301919085950715, -21.02845593540943270 ) ) ;
#17986 = FACE_OUTER_BOUND ( 'NONE', #57390, .T. ) ;
#17987 = EDGE_CURVE ( 'NONE', #21680, #79544, #82264, .T. ) ;
#17988 = CARTESIAN_POINT ( 'NONE',  ( -111.4783850760235566, 65.45264025789361995, 67.95177877341511419 ) ) ;
#17989 = EDGE_LOOP ( 'NONE', ( #80834, #14852, #18785, #73172, #80311, #36282 ) ) ;
#17990 = ORIENTED_EDGE ( 'NONE', *, *, #12666, .F. ) ;
#17991 = ORIENTED_EDGE ( 'NONE', *, *, #1946, .F. ) ;
#17992 = VERTEX_POINT ( 'NONE', #24 ) ;
#17993 = EDGE_CURVE ( 'NONE', #77147, #51227, #55848, .T. ) ;
#17994 = CARTESIAN_POINT ( 'NONE',  ( 115.1682430951150735, -35.73384980259207566, 191.7423760838769908 ) ) ;
#17995 = CARTESIAN_POINT ( 'NONE',  ( 108.5410937779726623, -26.38672566707733225, 104.9641967044819779 ) ) ;
#17996 = CARTESIAN_POINT ( 'NONE',  ( 101.0787430638808928, -27.46603582566399027, 70.54514908543497143 ) ) ;
#17997 = CARTESIAN_POINT ( 'NONE',  ( 99.04379977427080917, -42.84086283679705076, 251.8441986198212703 ) ) ;
#17998 = DIRECTION ( 'NONE',  ( -3.100000000000000258E-29, 3.100000000000000044E-14, 1.000000000000000000 ) ) ;
#17999 = CARTESIAN_POINT ( 'NONE',  ( 107.9025279714727787, -25.30072614498174488, 322.7599154420194623 ) ) ;
#18000 = CARTESIAN_POINT ( 'NONE',  ( 95.91002759172351944, -32.73343517516348555, 172.0527681330539735 ) ) ;
#18001 = EDGE_CURVE ( 'NONE', #69846, #22712, #62237, .T. ) ;
#18002 = CYLINDRICAL_SURFACE ( 'NONE', #71232, 5.041900000000001825 ) ;
#18003 = ORIENTED_EDGE ( 'NONE', *, *, #34700, .T. ) ;
#18004 = CARTESIAN_POINT ( 'NONE',  ( 49.21437657594998427, -35.91149509761070391, 313.9678068554150059 ) ) ;
#18005 = ORIENTED_EDGE ( 'NONE', *, *, #21294, .F. ) ;
#18006 = EDGE_LOOP ( 'NONE', ( #56020, #64269, #29766, #45568 ) ) ;
#18007 = CARTESIAN_POINT ( 'NONE',  ( 192.5667039024472444, -23.42844715993434335, 300.4678068554149490 ) ) ;
#18008 = VERTEX_POINT ( 'NONE', #918 ) ;
#18009 = ORIENTED_EDGE ( 'NONE', *, *, #72361, .T. ) ;
#18010 = AXIS2_PLACEMENT_3D ( 'NONE', #36826, #50891, #56802 ) ;
#18011 = LINE ( 'NONE', #51184, #34516 ) ;
#18012 = ORIENTED_EDGE ( 'NONE', *, *, #78784, .F. ) ;
#18013 = DIRECTION ( 'NONE',  ( -0.9419738712670565617, 0.000000000000000000, -0.3356862014592719157 ) ) ;
#18014 = CARTESIAN_POINT ( 'NONE',  ( 95.34890500915419409, -34.95776856631113105, 71.20705384733993526 ) ) ;
#18015 = CARTESIAN_POINT ( 'NONE',  ( -0.7859308033515303160, 69.84999999999996589, 130.5560000000000684 ) ) ;
#18016 = VECTOR ( 'NONE', #11888, 1000.000000000000000 ) ;
#18017 = DIRECTION ( 'NONE',  ( 0.000000000000000000, 0.000000000000000000, 1.000000000000000000 ) ) ;
#18018 = FACE_OUTER_BOUND ( 'NONE', #67178, .T. ) ;
#18019 = CARTESIAN_POINT ( 'NONE',  ( 102.8368274790082921, -27.91052165842129185, 95.43276813305395478 ) ) ;
#18021 = CARTESIAN_POINT ( 'NONE',  ( 96.06973772670292533, -35.87188691900273341, 187.2765776568629406 ) ) ;
#18020 = DIRECTION ( 'NONE',  ( 0.000000000000000000, 1.000000000000000000, 0.000000000000000000 ) ) ;
#18022 = CARTESIAN_POINT ( 'NONE',  ( 105.7963566878966191, -26.72446537362054286, 60.17754341170855525 ) ) ;
#18023 = CARTESIAN_POINT ( 'NONE',  ( 41.56648329127399677, -18.82844715994099971, 201.0426252759120018 ) ) ;
#18024 = ORIENTED_EDGE ( 'NONE', *, *, #41562, .T. ) ;
#18025 = LINE ( 'NONE', #52954, #77426 ) ;
#18026 = EDGE_CURVE ( 'NONE', #78421, #55155, #20475, .T. ) ;
#18027 = CARTESIAN_POINT ( 'NONE',  ( 20.03715912545639100, -24.42818131006202265, 180.4678068554150911 ) ) ;
#18028 = EDGE_CURVE ( 'NONE', #47532, #51892, #13650, .T. ) ;
#18029 = CARTESIAN_POINT ( 'NONE',  ( 48.85858412958099706, -30.08671355700241179, -5.074374724088000832 ) ) ;
#18030 = EDGE_CURVE ( 'NONE', #71705, #81882, #75603, .T. ) ;
#18031 = DIRECTION ( 'NONE',  ( 0.000000000000000000, -1.000000000000000000, 0.000000000000000000 ) ) ;
#18033 = ORIENTED_EDGE ( 'NONE', *, *, #65451, .T. ) ;
#18032 = CARTESIAN_POINT ( 'NONE',  ( 116.5668037432639608, -41.21227053747742985, 228.4756252759109714 ) ) ;
#18034 = CARTESIAN_POINT ( 'NONE',  ( 132.0248166246069843, 12.92155284005802685, 335.5992267699912190 ) ) ;
#18035 = CARTESIAN_POINT ( 'NONE',  ( 114.4303731589454998, -27.41304352248915777, 270.5441967044823741 ) ) ;
#18036 = CARTESIAN_POINT ( 'NONE',  ( 108.3246818025246654, -47.12222909040148267, 113.6727681330539639 ) ) ;
#18037 = EDGE_CURVE ( 'NONE', #44520, #47420, #82875, .T. ) ;
#18038 = DIRECTION ( 'NONE',  ( 1.000000000000000000, 4.163336342344333240E-14, 0.000000000000000000 ) ) ;
#18039 = DIRECTION ( 'NONE',  ( 0.000000000000000000, 0.000000000000000000, 1.000000000000000000 ) ) ;
#18040 = FACE_OUTER_BOUND ( 'NONE', #53598, .T. ) ;
#18041 = CARTESIAN_POINT ( 'NONE',  ( 115.7825805894831888, -41.80319946571558631, 264.4065922469304724 ) ) ;
#18042 = ORIENTED_EDGE ( 'NONE', *, *, #2308, .F. ) ;
#18043 = AXIS2_PLACEMENT_3D ( 'NONE', #21008, #26922, #13744 ) ;
#18044 = CIRCLE ( 'NONE', #86265, 1.000000000000000888 ) ;
#18045 = AXIS2_PLACEMENT_3D ( 'NONE', #48985, #78538, #863 ) ;
#18046 = CIRCLE ( 'NONE', #29655, 5.041900000000001825 ) ;
#18047 = ORIENTED_EDGE ( 'NONE', *, *, #14013, .F. ) ;
#18048 = ORIENTED_EDGE ( 'NONE', *, *, #20287, .T. ) ;
#18049 = VECTOR ( 'NONE', #23351, 1000.000000000000000 ) ;
#18050 = ORIENTED_EDGE ( 'NONE', *, *, #58987, .F. ) ;
#18051 = CARTESIAN_POINT ( 'NONE',  ( 107.0667039024470313, -104.2784471599409528, 55.21780685541800437 ) ) ;
#18052 = CARTESIAN_POINT ( 'NONE',  ( 97.55999611477783162, -43.80484941858547643, 257.8356252759109566 ) ) ;
#18053 = DIRECTION ( 'NONE',  ( 1.000000000000000000, 1.000000000000000078E-15, 0.000000000000000000 ) ) ;
#18054 = CARTESIAN_POINT ( 'NONE',  ( 144.0637627337163735, -140.6784471599286235, 245.5331643397809671 ) ) ;
#18056 = CARTESIAN_POINT ( 'NONE',  ( 108.4181602030399461, -26.73512120126024882, 149.9692933348216854 ) ) ;
#18055 = FACE_OUTER_BOUND ( 'NONE', #25861, .T. ) ;
#18057 = CARTESIAN_POINT ( 'NONE',  ( 109.1470148533826432, -28.41539336262556503, 199.3038483995049717 ) ) ;
#18058 = ORIENTED_EDGE ( 'NONE', *, *, #3137, .T. ) ;
#18059 = VERTEX_POINT ( 'NONE', #28618 ) ;
#18060 = VERTEX_POINT ( 'NONE', #14561 ) ;
#18061 = DIRECTION ( 'NONE',  ( -0.7071067811987160612, -0.7071067811743789733, 0.000000000000000000 ) ) ;
#18062 = CARTESIAN_POINT ( 'NONE',  ( 110.9568920020971348, -45.94175259203705508, 182.8944488436118831 ) ) ;
#18063 = DIRECTION ( 'NONE',  ( 0.000000000000000000, 5.463695987328529395E-16, -1.000000000000000000 ) ) ;
#18064 = CARTESIAN_POINT ( 'NONE',  ( 109.2301907924558009, -26.89130329018268739, 26.33586902018297948 ) ) ;
#18065 = CARTESIAN_POINT ( 'NONE',  ( 118.1052286201201724, 89.94786999841838337, -10.33119577496741925 ) ) ;
#18066 = DIRECTION ( 'NONE',  ( 0.7071067811862258301, -0.7071067811868692043, 7.071067811862265655E-16 ) ) ;
#18067 = CARTESIAN_POINT ( 'NONE',  ( 179.1667039024477504, -28.27351298636770949, 117.4678068554150627 ) ) ;
#18068 = ORIENTED_EDGE ( 'NONE', *, *, #9718, .T. ) ;
#18069 = CARTESIAN_POINT ( 'NONE',  ( 115.1583939375015291, -30.74836612253984569, 55.33262535118461045 ) ) ;
#18070 = ORIENTED_EDGE ( 'NONE', *, *, #22845, .T. ) ;
#18071 = LINE ( 'NONE', #80326, #59689 ) ;
#18072 = CARTESIAN_POINT ( 'NONE',  ( 99.45988105884268293, -33.69262468827373169, 38.84237608387697094 ) ) ;
#18073 = CONICAL_SURFACE ( 'NONE', #21007, 3.299999999999999822, 0.7853981633974602694 ) ;
#18074 = CARTESIAN_POINT ( 'NONE',  ( 136.4578062354350152, -17.36823420010915342, 7.200493380636948437 ) ) ;
#18075 = AXIS2_PLACEMENT_3D ( 'NONE', #88544, #67181, #53522 ) ;
#18076 = ADVANCED_FACE ( 'NONE', ( #76320 ), #14099, .F. ) ;
#18077 = CARTESIAN_POINT ( 'NONE',  ( 80.54920390244802775, -51.22944715994108833, 231.5838068554169524 ) ) ;
#18078 = CARTESIAN_POINT ( 'NONE',  ( 108.3333593921743301, -46.73486949315721262, 193.6772316444348974 ) ) ;
#18079 = ORIENTED_EDGE ( 'NONE', *, *, #22138, .F. ) ;
#18080 = FACE_BOUND ( 'NONE', #69293, .T. ) ;
#18081 = EDGE_CURVE ( 'NONE', #9481, #36458, #51276, .T. ) ;
#18082 = CARTESIAN_POINT ( 'NONE',  ( 119.5843592605237120, 52.73749999999999716, -52.38749999999991758 ) ) ;
#18083 = VERTEX_POINT ( 'NONE', #35877 ) ;
#18084 = CARTESIAN_POINT ( 'NONE',  ( 98.45613130301506999, -42.66979608177781813, 126.8070538473389490 ) ) ;
#18085 = VERTEX_POINT ( 'NONE', #79023 ) ;
#18086 = CARTESIAN_POINT ( 'NONE',  ( 106.8818968526635160, -46.43699862984655624, 76.98384839950495007 ) ) ;
#18087 = ADVANCED_FACE ( 'NONE', ( #8184 ), #72200, .F. ) ;
#18088 = CARTESIAN_POINT ( 'NONE',  ( -29.00000000000002842, 172.0000000000000000, 8.624053851998991955E-15 ) ) ;
#18089 = CARTESIAN_POINT ( 'NONE',  ( 107.2828545668587878, -27.33638008851531609, 71.47777378208797927 ) ) ;
#18090 = EDGE_CURVE ( 'NONE', #3666, #52538, #23618, .T. ) ;
#18091 = DIRECTION ( 'NONE',  ( 0.000000000000000000, 0.000000000000000000, -1.000000000000000000 ) ) ;
#18092 = DIRECTION ( 'NONE',  ( 0.000000000000000000, 0.000000000000000000, 1.000000000000000000 ) ) ;
#18093 = CARTESIAN_POINT ( 'NONE',  ( 117.5340331363998985, -37.28601590683526723, 14.78419670448294454 ) ) ;
#18095 = ADVANCED_FACE ( 'NONE', ( #70870 ), #4540, .F. ) ;
#18094 = LINE ( 'NONE', #45783, #30933 ) ;
#18096 = ORIENTED_EDGE ( 'NONE', *, *, #28357, .F. ) ;
#18097 = DIRECTION ( 'NONE',  ( -0.000000000000000000, 1.000000000000000000, 0.000000000000000000 ) ) ;
#18098 = AXIS2_PLACEMENT_3D ( 'NONE', #51817, #9613, #66349 ) ;
#18099 = EDGE_LOOP ( 'NONE', ( #43509, #77113 ) ) ;
#18100 = CARTESIAN_POINT ( 'NONE',  ( -118.5472164932298256, 69.93120980984942037, 1.660430599529278295 ) ) ;
#18101 = VECTOR ( 'NONE', #71700, 1000.000000000000000 ) ;
#18102 = VECTOR ( 'NONE', #74717, 1000.000000000000000 ) ;
#18103 = ORIENTED_EDGE ( 'NONE', *, *, #17419, .F. ) ;
#18104 = EDGE_LOOP ( 'NONE', ( #54063, #62998, #16847, #11360, #10470, #70484 ) ) ;
#18105 = EDGE_CURVE ( 'NONE', #74932, #11705, #84512, .T. ) ;
#18106 = CIRCLE ( 'NONE', #74654, 29.00000000000000000 ) ;
#18107 = VECTOR ( 'NONE', #86787, 1000.000000000000000 ) ;
#18108 = ORIENTED_EDGE ( 'NONE', *, *, #32821, .F. ) ;
#18109 = CARTESIAN_POINT ( 'NONE',  ( 115.8019334949658798, -41.12891815432281817, 203.4556252759109611 ) ) ;
#18110 = CARTESIAN_POINT ( 'NONE',  ( 116.1804594027163375, -40.96476762480074996, 25.56312527591098060 ) ) ;
#18111 = DIRECTION ( 'NONE',  ( 0.000000000000000000, 0.000000000000000000, 1.000000000000000000 ) ) ;
#18112 = CARTESIAN_POINT ( 'NONE',  ( 115.6731346838618464, -43.66482979471727077, 39.27467289495895386 ) ) ;
#18113 = EDGE_CURVE ( 'NONE', #88467, #20221, #59671, .T. ) ;
#18114 = LINE ( 'NONE', #58118, #85696 ) ;
#18115 = VERTEX_POINT ( 'NONE', #56763 ) ;
#18116 = LINE ( 'NONE', #73980, #23568 ) ;
#18117 = FACE_OUTER_BOUND ( 'NONE', #11794, .T. ) ;
#18119 = VERTEX_POINT ( 'NONE', #15898 ) ;
#18118 = EDGE_CURVE ( 'NONE', #80487, #51959, #22269, .T. ) ;
#18120 = CARTESIAN_POINT ( 'NONE',  ( 6.174546696621020337E-16, 101.5999999999999943, -108.2293999999999983 ) ) ;
#18121 = CARTESIAN_POINT ( 'NONE',  ( 78.56670390244704549, -118.2784471599409812, 45.21780685541799727 ) ) ;
#18122 = CARTESIAN_POINT ( 'NONE',  ( 114.5897159479186342, -29.54407062678533791, 234.4327681330539690 ) ) ;
#18123 = DIRECTION ( 'NONE',  ( 1.000000000000000000, 4.163336342344333240E-14, 0.000000000000000000 ) ) ;
#18124 = VECTOR ( 'NONE', #83847, 1000.000000000000000 ) ;
#18125 = DIRECTION ( 'NONE',  ( 1.000000000000000000, 0.000000000000000000, 0.000000000000000000 ) ) ;
#18126 = CARTESIAN_POINT ( 'NONE',  ( 79.69020591994934932, -39.46022584114963649, 1.641799370504630984 ) ) ;
#18127 = CARTESIAN_POINT ( 'NONE',  ( 116.5602560931381220, -38.76387722282552062, 258.0809912566484741 ) ) ;
#18129 = CARTESIAN_POINT ( 'NONE',  ( 101.0787430638809496, -27.46603582566407908, 66.54514908543495721 ) ) ;
#18128 = CARTESIAN_POINT ( 'NONE',  ( 0.000000000000000000, 95.25000000000000000, 0.000000000000000000 ) ) ;
#18130 = CARTESIAN_POINT ( 'NONE',  ( 109.2774118001977541, 55.39176648947218240, 71.43749999999998579 ) ) ;
#18131 = CARTESIAN_POINT ( 'NONE',  ( 98.16479183632776540, -43.36064410082828857, 111.8480062282919647 ) ) ;
#18132 = VERTEX_POINT ( 'NONE', #71758 ) ;
#18133 = PLANE ( 'NONE',  #78556 ) ;
#18134 = ORIENTED_EDGE ( 'NONE', *, *, #61640, .F. ) ;
#18135 = PLANE ( 'NONE',  #68611 ) ;
#18136 = DIRECTION ( 'NONE',  ( -1.000000000000000078E-15, 1.000000000000000083E-30, 1.000000000000000000 ) ) ;
#18137 = DIRECTION ( 'NONE',  ( 0.000000000000000000, 0.000000000000000000, -1.000000000000000000 ) ) ;
#18138 = VERTEX_POINT ( 'NONE', #15458 ) ;
#18139 = ADVANCED_FACE ( 'NONE', ( #21824, #85846 ), #8641, .T. ) ;
#18140 = PLANE ( 'NONE',  #49093 ) ;
#18142 = ORIENTED_EDGE ( 'NONE', *, *, #87828, .F. ) ;
#18141 = CARTESIAN_POINT ( 'NONE',  ( 112.5373769503831625, -27.80330641407773840, 94.63848241876793566 ) ) ;
#18143 = CYLINDRICAL_SURFACE ( 'NONE', #71217, 4.875000000000017764 ) ;
#18144 = ADVANCED_FACE ( 'NONE', ( #64047, #1824 ), #23183, .T. ) ;
#18145 = FACE_OUTER_BOUND ( 'NONE', #36541, .T. ) ;
#18146 =( GEOMETRIC_REPRESENTATION_CONTEXT ( 3 ) GLOBAL_UNCERTAINTY_ASSIGNED_CONTEXT ( ( #63277 ) ) GLOBAL_UNIT_ASSIGNED_CONTEXT ( ( #42909, #21607, #1612 ) ) REPRESENTATION_CONTEXT ( 'NONE', 'WORKASPACE' ) );
#18147 = CARTESIAN_POINT ( 'NONE',  ( 123.6837132603318707, -21.37118780205705448, 218.8274735512161158 ) ) ;
#18148 = EDGE_LOOP ( 'NONE', ( #42222, #83624, #41113, #5619 ) ) ;
#18149 = CARTESIAN_POINT ( 'NONE',  ( 102.3504518276437523, -46.05175434220414132, 127.2041967044829960 ) ) ;
#18150 = PRODUCT_CONTEXT ( 'NONE', #35322, 'mechanical' ) ;
#18151 = AXIS2_PLACEMENT_3D ( 'NONE', #87530, #25739, #24414 ) ;
#18152 = CARTESIAN_POINT ( 'NONE',  ( 107.0664832912730020, -36.72944715994189835, 342.9256252759109884 ) ) ;
#18153 = CARTESIAN_POINT ( 'NONE',  ( 33.96670390244699433, -28.27351298637401200, -5.074374724088000832 ) ) ;
#18154 = ORIENTED_EDGE ( 'NONE', *, *, #75028, .F. ) ;
#18155 = ORIENTED_EDGE ( 'NONE', *, *, #37979, .T. ) ;
#18156 = CARTESIAN_POINT ( 'NONE',  ( 62.03715912545749944, -47.82818131006020934, 180.4678068554151196 ) ) ;
#18157 = DIRECTION ( 'NONE',  ( 0.000000000000000000, 0.000000000000000000, 1.000000000000000000 ) ) ;
#18158 = DIRECTION ( 'NONE',  ( 0.000000000000000000, 0.000000000000000000, 1.000000000000000000 ) ) ;
#18160 = DIRECTION ( 'NONE',  ( 1.000000000000000000, 1.000000000000000078E-15, 0.000000000000000000 ) ) ;
#18159 = DIRECTION ( 'NONE',  ( 0.7071067811865671127, 0.7071067811865279218, 7.071067811865664660E-16 ) ) ;
#18161 = CARTESIAN_POINT ( 'NONE',  ( 97.80411235625082611, -40.49886499406813556, 181.6340295426134048 ) ) ;
#18162 = ADVANCED_FACE ( 'NONE', ( #44020 ), #78139, .T. ) ;
#18163 = VECTOR ( 'NONE', #85019, 1000.000000000000000 ) ;
#18164 = ORIENTED_EDGE ( 'NONE', *, *, #86404, .F. ) ;
#18165 = VECTOR ( 'NONE', #32346, 1000.000000000000000 ) ;
#18166 = AXIS2_PLACEMENT_3D ( 'NONE', #6569, #67443, #11606 ) ;
#18167 = CIRCLE ( 'NONE', #45763, 4.762500000000001066 ) ;
#18168 = CARTESIAN_POINT ( 'NONE',  ( 113.1782938590851160, -44.75186852387405168, 34.09395861806017081 ) ) ;
#18169 = CARTESIAN_POINT ( 'NONE',  ( 116.7742277529939230, -35.53649587948896027, 189.9241967044819717 ) ) ;
#18171 = VERTEX_POINT ( 'NONE', #17236 ) ;
#18170 = PLANE ( 'NONE',  #87831 ) ;
#18172 = AXIS2_PLACEMENT_3D ( 'NONE', #20301, #47970, #62513 ) ;
#18173 = CARTESIAN_POINT ( 'NONE',  ( 110.5640613610537883, -45.86347053068958246, 58.86705384733897972 ) ) ;
#18174 = CARTESIAN_POINT ( 'NONE',  ( 97.81169138727440782, -40.51741131469341184, 51.63568823874075520 ) ) ;
#18175 = DIRECTION ( 'NONE',  ( -0.7071067811874389708, 0.7071067811856560636, 0.000000000000000000 ) ) ;
#18176 = AXIS2_PLACEMENT_3D ( 'NONE', #41567, #69302, #69750 ) ;
#18177 = DIRECTION ( 'NONE',  ( 1.000000000000000000, 0.000000000000000000, 0.000000000000000000 ) ) ;
#18178 = ORIENTED_EDGE ( 'NONE', *, *, #25773, .T. ) ;
#18179 = DIRECTION ( 'NONE',  ( 0.000000000000000000, 0.000000000000000000, -1.000000000000000000 ) ) ;
#18180 = VERTEX_POINT ( 'NONE', #79921 ) ;
#18181 = EDGE_LOOP ( 'NONE', ( #86446, #60153 ) ) ;
#18182 = CIRCLE ( 'NONE', #86352, 10.66799999999999748 ) ;
#18183 = EDGE_CURVE ( 'NONE', #4939, #38575, #81449, .T. ) ;
#18184 = CARTESIAN_POINT ( 'NONE',  ( 107.4435086560219474, -45.58304137281263024, 234.0415833058969781 ) ) ;
#18185 = CARTESIAN_POINT ( 'NONE',  ( 97.82697590662368725, -40.55461666880389515, 52.63840751606506529 ) ) ;
#18186 = LINE ( 'NONE', #82234, #21794 ) ;
#18187 = AXIS2_PLACEMENT_3D ( 'NONE', #12916, #4308, #89220 ) ;
#18188 = EDGE_CURVE ( 'NONE', #27566, #1599, #12201, .T. ) ;
#18189 = EDGE_CURVE ( 'NONE', #23638, #9163, #52157, .T. ) ;
#18190 = CARTESIAN_POINT ( 'NONE',  ( 25.56670390244797275, -62.87844715994099687, 139.9678068554150059 ) ) ;
#18191 = DIRECTION ( 'NONE',  ( 0.000000000000000000, 0.000000000000000000, -1.000000000000000000 ) ) ;
#18192 = VERTEX_POINT ( 'NONE', #24495 ) ;
#18193 = CYLINDRICAL_SURFACE ( 'NONE', #49319, 88.90000000000000568 ) ;
#18194 = ADVANCED_FACE ( 'NONE', ( #19012 ), #67607, .T. ) ;
#18195 = CARTESIAN_POINT ( 'NONE',  ( 102.0622438148563873, -27.97331942483490508, 36.48982574705384252 ) ) ;
#18196 = EDGE_LOOP ( 'NONE', ( #53323, #40352, #78466, #56754 ) ) ;
#18197 = CARTESIAN_POINT ( 'NONE',  ( 111.7292870705843768, -27.42961193919077445, 279.7070538473396937 ) ) ;
#18198 = CARTESIAN_POINT ( 'NONE',  ( 12.70000000000000107, 82.54999999999999716, 117.8738102209307641 ) ) ;
#18199 = ORIENTED_EDGE ( 'NONE', *, *, #83252, .F. ) ;
#18200 = CARTESIAN_POINT ( 'NONE',  ( 115.1064843935641022, -35.31944421942311862, 241.7823760838769545 ) ) ;
#18201 = EDGE_CURVE ( 'NONE', #69678, #26649, #32630, .T. ) ;
#18202 = LINE ( 'NONE', #4582, #30045 ) ;
#18203 = CARTESIAN_POINT ( 'NONE',  ( 162.7131505118679797, -31.94127993907790852, -5.074374724088000832 ) ) ;
#18204 = LINE ( 'NONE', #11394, #44710 ) ;
#18205 = CARTESIAN_POINT ( 'NONE',  ( 21.56670390244726576, -23.42844715994183957, 237.4678068554150059 ) ) ;
#18207 = CARTESIAN_POINT ( 'NONE',  ( 96.09249528944252461, -35.06539016137039511, 217.1946728949589840 ) ) ;
#18206 = AXIS2_PLACEMENT_3D ( 'NONE', #32643, #73989, #87621 ) ;
#18208 = DIRECTION ( 'NONE',  ( 0.000000000000000000, 1.000000000000000000, 0.000000000000000000 ) ) ;
#18209 = EDGE_CURVE ( 'NONE', #82784, #62066, #52456, .T. ) ;
#18210 = ORIENTED_EDGE ( 'NONE', *, *, #52235, .F. ) ;
#18211 = CARTESIAN_POINT ( 'NONE',  ( 97.18453276023305420, -31.67528530451021851, 91.96229194257693962 ) ) ;
#18212 = CARTESIAN_POINT ( 'NONE',  ( 87.17003668186745813, -46.62589376934782592, 14.92562527591089783 ) ) ;
#18213 = B_SPLINE_CURVE_WITH_KNOTS ( 'NONE', 3,
 ( #14763, #35629, #50599, #72406, #57415, #24246, #86041, #10167, #71073, #43332, #65577, #29721, #15652, #51916, #45111, #78340, #64244, #23810, #2470, #2018, #30165, #31049, #3359, #85151, #58314, #37877, #16103, #43781, #2912, #72838 ),
 .UNSPECIFIED., .F., .F.,
 ( 4, 2, 2, 2, 2, 2, 2, 2, 2, 2, 1, 1, 1, 1, 1, 1, 2, 4 ),
 ( 0.000000000000000000, 0.06250180076269364060, 0.1250036015253872812, 0.1875054022880809357, 0.2500072030507745624, 0.3125090038134681891, 0.3750108045761618714, 0.4375126053388554981, 0.4687635057202020894, 0.4843889559108754961, 0.4922016810062120884, 0.4961080435538803846, 0.4980612248277145326, 0.4990378154646316622, 0.4995261107830904490, 0.4997702584423199257, 0.4998923322719344697, 0.5000144061015490138 ),
 .UNSPECIFIED. ) ;
#18214 = AXIS2_PLACEMENT_3D ( 'NONE', #15146, #14252, #83295 ) ;
#18215 = EDGE_LOOP ( 'NONE', ( #22273, #7530, #4736, #87669, #68379, #59101, #5946, #59310, #88269, #5037, #15988, #19917, #34475, #22008, #87223, #39521, #1139, #45306, #72150, #17348, #10628, #52187, #40735, #9746, #2372, #49938 ) ) ;
#18216 = ORIENTED_EDGE ( 'NONE', *, *, #30299, .F. ) ;
#18217 = ORIENTED_EDGE ( 'NONE', *, *, #51420, .F. ) ;
#18218 = EDGE_CURVE ( 'NONE', #2953, #22107, #62553, .T. ) ;
#18219 = CARTESIAN_POINT ( 'NONE',  ( 82.51836309791794122, -17.48272428399696210, 2.716753546982734857 ) ) ;
#18220 = CARTESIAN_POINT ( 'NONE',  ( 130.5667039024480118, -36.72944715994093912, 229.5838068554170093 ) ) ;
#18221 = CARTESIAN_POINT ( 'NONE',  ( 52.99265158129180264, 69.84999999999999432, 358.0130000000000337 ) ) ;
#18222 = CARTESIAN_POINT ( 'NONE',  ( 108.7381085716129263, -28.73974155568626898, 137.7309475124479548 ) ) ;
#18223 = CARTESIAN_POINT ( 'NONE',  ( 99.73785018541691727, -29.28442226721861275, 221.6956252759109702 ) ) ;
#18224 = EDGE_CURVE ( 'NONE', #43116, #31632, #86721, .T. ) ;
#18225 = CARTESIAN_POINT ( 'NONE',  ( 70.63919639214310564, 49.07499999999999574, -33.74458626278666884 ) ) ;
#18226 = VERTEX_POINT ( 'NONE', #54393 ) ;
#18227 = CARTESIAN_POINT ( 'NONE',  ( 136.5411229421764006, -37.94037323192798539, 2.740176903235941097 ) ) ;
#18228 = ORIENTED_EDGE ( 'NONE', *, *, #39298, .T. ) ;
#18229 = VERTEX_POINT ( 'NONE', #40788 ) ;
#18230 = AXIS2_PLACEMENT_3D ( 'NONE', #25004, #5004, #45420 ) ;
#18231 = AXIS2_PLACEMENT_3D ( 'NONE', #33150, #54009, #40410 ) ;
#18232 = DIRECTION ( 'NONE',  ( 1.000000000000000000, 0.000000000000000000, 0.000000000000000000 ) ) ;
#18233 = VECTOR ( 'NONE', #39185, 1000.000000000000000 ) ;
#18234 = VERTEX_POINT ( 'NONE', #61671 ) ;
#18235 = EDGE_LOOP ( 'NONE', ( #62111, #42683, #87549, #20574 ) ) ;
#18236 = CARTESIAN_POINT ( 'NONE',  ( 3.175000000000334666, 124.5870000000000033, -31.75000000000000000 ) ) ;
#18237 = PLANE ( 'NONE',  #50102 ) ;
#18238 = DIRECTION ( 'NONE',  ( 0.000000000000000000, 1.000000000000000000, 0.000000000000000000 ) ) ;
#18239 = CARTESIAN_POINT ( 'NONE',  ( 112.8906599442021275, -43.66427313951261624, 147.5428960185529661 ) ) ;
#18240 = CARTESIAN_POINT ( 'NONE',  ( 111.0631195717115673, -47.08511319755631774, 17.85753003781598380 ) ) ;
#18241 = ORIENTED_EDGE ( 'NONE', *, *, #34718, .T. ) ;
#18242 = DIRECTION ( 'NONE',  ( 0.000000000000000000, -1.000000000000000000, 0.000000000000000000 ) ) ;
#18243 = VERTEX_POINT ( 'NONE', #82158 ) ;
#18244 = CIRCLE ( 'NONE', #65893, 13.63963572536219715 ) ;
#18245 = DIRECTION ( 'NONE',  ( 1.000000000000000000, 1.132880637372608296E-15, 0.000000000000000000 ) ) ;
#18246 = ORIENTED_EDGE ( 'NONE', *, *, #39821, .T. ) ;
#18247 = CARTESIAN_POINT ( 'NONE',  ( 97.22634975616455222, -34.77161965005227273, 167.1698970065834828 ) ) ;
#18248 = LINE ( 'NONE', #17362, #77773 ) ;
#18249 = EDGE_CURVE ( 'NONE', #61102, #83340, #21254, .T. ) ;
#18250 = CARTESIAN_POINT ( 'NONE',  ( 97.81168839172025287, -40.51739946886939947, 131.6358419732753475 ) ) ;
#18251 = DIRECTION ( 'NONE',  ( 1.000000000000000078E-15, -1.000000000000000083E-30, -1.000000000000000000 ) ) ;
#18252 = ORIENTED_EDGE ( 'NONE', *, *, #30569, .T. ) ;
#18253 = CARTESIAN_POINT ( 'NONE',  ( 116.3173282457959345, -41.53670860177669510, 288.4441967044823514 ) ) ;
#18254 = CARTESIAN_POINT ( 'NONE',  ( 109.6225776363756950, -25.10716277166327615, 25.90419670448196143 ) ) ;
#18255 = AXIS2_PLACEMENT_3D ( 'NONE', #16395, #71802, #44965 ) ;
#18257 = CARTESIAN_POINT ( 'NONE',  ( -69.72411017813060141, 120.6499999999999915, 69.72411017812929401 ) ) ;
#18256 = PLANE ( 'NONE',  #55015 ) ;
#18258 = PLANE ( 'NONE',  #88801 ) ;
#18259 = CARTESIAN_POINT ( 'NONE',  ( 97.81399847929220925, -40.51646572127298640, 256.6355814287313137 ) ) ;
#18260 = DIRECTION ( 'NONE',  ( 1.000000000000000078E-15, -1.000000000000000083E-30, -1.000000000000000000 ) ) ;
#18261 = LINE ( 'NONE', #45940, #56144 ) ;
#18262 = DIRECTION ( 'NONE',  ( 0.000000000000000000, 0.000000000000000000, 1.000000000000000000 ) ) ;
#18263 = EDGE_CURVE ( 'NONE', #20018, #61103, #31644, .T. ) ;
#18264 = CARTESIAN_POINT ( 'NONE',  ( 112.9881877051661263, -28.09578728253486446, 44.59848241876795782 ) ) ;
#18265 = CARTESIAN_POINT ( 'NONE',  ( 110.6962928707952756, -48.01036458606073865, 203.8241967044819489 ) ) ;
#18266 = CARTESIAN_POINT ( 'NONE',  ( 101.0536616762676374, -27.42723333900414318, 66.54514908543495721 ) ) ;
#18268 = DIRECTION ( 'NONE',  ( -0.7071067812164788524, 0.7071067811566160710, 0.000000000000000000 ) ) ;
#18267 = DIRECTION ( 'NONE',  ( 1.000000000000000000, 4.299999999999999979E-14, 1.000000000000000078E-15 ) ) ;
#18269 = CYLINDRICAL_SURFACE ( 'NONE', #163, 3.174999999999983391 ) ;
#18270 = EDGE_CURVE ( 'NONE', #88009, #71659, #20549, .T. ) ;
#18271 = VERTEX_POINT ( 'NONE', #81706 ) ;
#18272 = FACE_OUTER_BOUND ( 'NONE', #58014, .T. ) ;
#18273 = ORIENTED_EDGE ( 'NONE', *, *, #27630, .T. ) ;
#18274 = CARTESIAN_POINT ( 'NONE',  ( 113.5922197990810645, -29.44396856740777224, 110.4956252759109816 ) ) ;
#18276 = VERTEX_POINT ( 'NONE', #7181 ) ;
#18275 = CARTESIAN_POINT ( 'NONE',  ( 31.56670390244700641, -19.82844715994111340, -5.074374724088000832 ) ) ;
#18277 = CARTESIAN_POINT ( 'NONE',  ( 96.54020141486705597, -31.34005042439575561, 241.9499109901969689 ) ) ;
#18278 = LINE ( 'NONE', #53215, #4825 ) ;
#18279 = CARTESIAN_POINT ( 'NONE',  ( 41.56648329127399677, -9.303447159940999356, 81.04262527591200183 ) ) ;
#18280 = FACE_OUTER_BOUND ( 'NONE', #19384, .T. ) ;
#18281 = CARTESIAN_POINT ( 'NONE',  ( 108.0015324895207129, -121.2375264746780488, -19.21046202161247152 ) ) ;
#18282 = CARTESIAN_POINT ( 'NONE',  ( 107.0664832912739968, -36.72944715994100306, 287.6356252759109680 ) ) ;
#18283 = LINE ( 'NONE', #19194, #86329 ) ;
#18284 = VECTOR ( 'NONE', #74628, 1000.000000000000000 ) ;
#18285 = CARTESIAN_POINT ( 'NONE',  ( 117.1170091337237551, -34.17489915221370467, 169.0365776568639831 ) ) ;
#18286 = VERTEX_POINT ( 'NONE', #33532 ) ;
#18287 = VERTEX_POINT ( 'NONE', #47589 ) ;
#18288 = CARTESIAN_POINT ( 'NONE',  ( 97.38361328163530573, -33.95226689236985607, 137.5358690201829575 ) ) ;
#18289 = AXIS2_PLACEMENT_3D ( 'NONE', #42188, #76730, #69470 ) ;
#18290 = DIRECTION ( 'NONE',  ( 0.000000000000000000, 0.000000000000000000, 1.000000000000000000 ) ) ;
#18291 = AXIS2_PLACEMENT_3D ( 'NONE', #76739, #48107, #62205 ) ;
#18293 = DIRECTION ( 'NONE',  ( 0.9999999853157766072, 0.0001713722456133601202, -9.999999853157765648E-16 ) ) ;
#18292 = CARTESIAN_POINT ( 'NONE',  ( 115.1619974903459251, -42.21817061296636808, 269.3527681330531891 ) ) ;
#18294 = AXIS2_PLACEMENT_3D ( 'NONE', #62319, #43208, #20556 ) ;
#18295 = DIRECTION ( 'NONE',  ( -0.000000000000000000, 1.000000000000000000, -0.000000000000000000 ) ) ;
#18296 = DIRECTION ( 'NONE',  ( -3.100000000000000258E-29, 3.100000000000000044E-14, 1.000000000000000000 ) ) ;
#18297 = ADVANCED_FACE ( 'NONE', ( #60783 ), #19458, .T. ) ;
#18298 = CARTESIAN_POINT ( 'NONE',  ( 118.3867465934798560, 71.53193882405243187, 6.370299515175424254 ) ) ;
#18299 = CARTESIAN_POINT ( 'NONE',  ( 138.8167039024479834, -67.87844715994100397, 84.20080685541500998 ) ) ;
#18300 = DIRECTION ( 'NONE',  ( 1.000000000000000078E-15, 1.000000000000000083E-30, -1.000000000000000000 ) ) ;
#18301 = EDGE_CURVE ( 'NONE', #64730, #54616, #13280, .T. ) ;
#18302 = DIRECTION ( 'NONE',  ( -1.000000000000000000, 0.000000000000000000, 0.000000000000000000 ) ) ;
#18303 = CARTESIAN_POINT ( 'NONE',  ( 103.5497706991576905, -26.90106182813401503, 190.3499109901969746 ) ) ;
#18304 = EDGE_CURVE ( 'NONE', #29424, #28847, #88517, .T. ) ;
#18305 = VERTEX_POINT ( 'NONE', #74875 ) ;
#18306 = ORIENTED_EDGE ( 'NONE', *, *, #17301, .F. ) ;
#18307 = EDGE_CURVE ( 'NONE', #58766, #41861, #34988, .T. ) ;
#18308 = LINE ( 'NONE', #51044, #76399 ) ;
#18309 = CARTESIAN_POINT ( 'NONE',  ( 147.0048854145641144, -67.93494677174348340, 245.9788996868301751 ) ) ;
#18310 = CARTESIAN_POINT ( 'NONE',  ( 5.041899999999280624, 117.4749999999999943, 103.1875000000000000 ) ) ;
#18311 = CARTESIAN_POINT ( 'NONE',  ( 100.6318841171118379, -87.59835267194286246, -9.274842254011147702 ) ) ;
#18312 = CIRCLE ( 'NONE', #44370, 2.750000000000002665 ) ;
#18314 = ORIENTED_EDGE ( 'NONE', *, *, #3814, .T. ) ;
#18313 = EDGE_CURVE ( 'NONE', #54780, #43708, #51003, .T. ) ;
#18315 = CARTESIAN_POINT ( 'NONE',  ( 117.0723199711336946, -35.46600488634853576, 63.92701177807728641 ) ) ;
#18316 = AXIS2_PLACEMENT_3D ( 'NONE', #39940, #39504, #24544 ) ;
#18317 = CARTESIAN_POINT ( 'NONE',  ( 108.1817894924016770, -47.09492459897622751, 202.6613395616249704 ) ) ;
#18318 = CARTESIAN_POINT ( 'NONE',  ( 160.2664750769284865, 0.000000000000000000, -148.0533267522753818 ) ) ;
#18319 = VERTEX_POINT ( 'NONE', #6277 ) ;
#18320 = ORIENTED_EDGE ( 'NONE', *, *, #39272, .F. ) ;
#18321 = EDGE_CURVE ( 'NONE', #63793, #49742, #1687, .T. ) ;
#18322 = CARTESIAN_POINT ( 'NONE',  ( 107.9598221976452521, -46.72791177985842381, 63.64822525680465048 ) ) ;
#18323 = LINE ( 'NONE', #11972, #63759 ) ;
#18324 = DIRECTION ( 'NONE',  ( 1.000000000000000078E-15, -1.000000000000000083E-30, -1.000000000000000000 ) ) ;
#18325 = CARTESIAN_POINT ( 'NONE',  ( 98.55283614654496205, -38.28467619158744384, 49.30047132197196191 ) ) ;
#18326 = LINE ( 'NONE', #45557, #60826 ) ;
#18327 = ORIENTED_EDGE ( 'NONE', *, *, #24868, .F. ) ;
#18328 = CARTESIAN_POINT ( 'NONE',  ( 173.9900000000000091, 36.86249999999999716, -53.61543552338530105 ) ) ;
#18329 = CARTESIAN_POINT ( 'NONE',  ( 81.62727349186526737, -16.46583755400498106, 7.833212107638633626 ) ) ;
#18330 = ORIENTED_EDGE ( 'NONE', *, *, #18764, .F. ) ;
#18331 = ORIENTED_EDGE ( 'NONE', *, *, #2093, .F. ) ;
#18332 = CARTESIAN_POINT ( 'NONE',  ( 1.598849875094818280E-14, 61.59999999999999432, -130.5560000000000116 ) ) ;
#18333 = ORIENTED_EDGE ( 'NONE', *, *, #32140, .F. ) ;
#18334 = EDGE_LOOP ( 'NONE', ( #47621, #31957, #59427, #72956 ) ) ;
#18335 = FACE_OUTER_BOUND ( 'NONE', #75633, .T. ) ;
#18336 = CARTESIAN_POINT ( 'NONE',  ( 99.05520249114191245, -33.76709814885239780, 65.46670554236195017 ) ) ;
#18337 = CARTESIAN_POINT ( 'NONE',  ( 97.03688691280343903, -41.43079139552996537, 211.6632443235299945 ) ) ;
#18338 = CARTESIAN_POINT ( 'NONE',  ( 97.97553865104310944, -30.48296430071270535, 165.8594347997199634 ) ) ;
#18340 = CARTESIAN_POINT ( 'NONE',  ( 96.91437895093065436, -34.20831442473366479, 272.1327681330538439 ) ) ;
#18339 = CARTESIAN_POINT ( 'NONE',  ( 102.2973125513888988, -45.62237811309391589, 22.18432667138703707 ) ) ;
#18341 = LINE ( 'NONE', #4279, #62336 ) ;
#18342 = CARTESIAN_POINT ( 'NONE',  ( -9.749037034254357081, 223.9999999999999716, 152.4294779587682456 ) ) ;
#18343 = ORIENTED_EDGE ( 'NONE', *, *, #89695, .F. ) ;
#18344 = VERTEX_POINT ( 'NONE', #6722 ) ;
#18345 = VECTOR ( 'NONE', #60200, 1000.000000000000000 ) ;
#18346 = AXIS2_PLACEMENT_3D ( 'NONE', #45988, #42755, #7368 ) ;
#18347 = CARTESIAN_POINT ( 'NONE',  ( 193.0374249753377001, -23.42844715993431848, 129.9678068554150343 ) ) ;
#18349 = CARTESIAN_POINT ( 'NONE',  ( 117.4565820116822010, -35.18101482210430930, 218.9441967044829482 ) ) ;
#18348 = AXIS2_PLACEMENT_3D ( 'NONE', #85766, #23973, #55877 ) ;
#18350 = ORIENTED_EDGE ( 'NONE', *, *, #38708, .F. ) ;
#18351 = AXIS2_PLACEMENT_3D ( 'NONE', #80665, #11620, #87472 ) ;
#18352 = CARTESIAN_POINT ( 'NONE',  ( 114.9780134700875180, -29.01019993736734293, 194.4537205140059370 ) ) ;
#18353 = CARTESIAN_POINT ( 'NONE',  ( 98.34958594534221277, -31.65707425133572173, 265.9065036673953273 ) ) ;
#18354 = CARTESIAN_POINT ( 'NONE',  ( -0.6929090906571917508, 70.24203434096085630, 38.09999999999997300 ) ) ;
#18355 = EDGE_CURVE ( 'NONE', #81510, #21246, #76211, .T. ) ;
#18356 = CARTESIAN_POINT ( 'NONE',  ( 152.4532656103850456, -72.54314042502360849, 394.9756252759102040 ) ) ;
#18357 = DIRECTION ( 'NONE',  ( 1.000000000000000000, 1.000000000000000078E-15, 0.000000000000000000 ) ) ;
#18360 = CARTESIAN_POINT ( 'NONE',  ( 100.9974690995740190, -29.01719307973645812, 11.60705384733895507 ) ) ;
#18359 = DIRECTION ( 'NONE',  ( 1.000000000000000000, 0.000000000000000000, 0.000000000000000000 ) ) ;
#18358 = CARTESIAN_POINT ( 'NONE',  ( 112.0046464180979200, -30.41912573431281075, 277.6356252759109680 ) ) ;
#18361 = CARTESIAN_POINT ( 'NONE',  ( 75.31670390244798341, -57.40094715994099772, 58.80080685541479824 ) ) ;
#18362 = CARTESIAN_POINT ( 'NONE',  ( -458.3598257906459708, 47.62500000000000000, -3.174999999999999822 ) ) ;
#18363 = DIRECTION ( 'NONE',  ( -1.000000000000000078E-15, 1.000000000000000083E-30, 1.000000000000000000 ) ) ;
#18364 = DIRECTION ( 'NONE',  ( -1.000000000000000078E-15, 0.000000000000000000, 1.000000000000000000 ) ) ;
#18365 = PLANE ( 'NONE',  #2427 ) ;
#18366 = CARTESIAN_POINT ( 'NONE',  ( 55.48342271751659638, 20.32000000000000028, 171.1197181046785261 ) ) ;
#18368 = ORIENTED_EDGE ( 'NONE', *, *, #45683, .T. ) ;
#18367 = CARTESIAN_POINT ( 'NONE',  ( -0.8293608286808433760, 95.25000000000002842, -118.5560000000000400 ) ) ;
#18369 = FACE_OUTER_BOUND ( 'NONE', #53928, .T. ) ;
#18370 = CARTESIAN_POINT ( 'NONE',  ( 118.0743634110212383, -35.49574686983337557, 233.9032443235299752 ) ) ;
#18371 = CARTESIAN_POINT ( 'NONE',  ( 108.0341493669268260, -25.71865232712709215, 105.9946728949589811 ) ) ;
#18372 = CARTESIAN_POINT ( 'NONE',  ( 100.7237713325202861, -45.83809708005067307, 233.0803871806729717 ) ) ;
#18373 = DIRECTION ( 'NONE',  ( -0.7071067811865671127, -0.7071067811865279218, -7.071067811865664660E-16 ) ) ;
#18374 = LINE ( 'NONE', #72901, #67808 ) ;
#18375 = CIRCLE ( 'NONE', #35750, 4.762500000000001066 ) ;
#18377 = CARTESIAN_POINT ( 'NONE',  ( 98.14055758736320456, -41.24087220378398655, 37.69858362254909423 ) ) ;
#18376 = CARTESIAN_POINT ( 'NONE',  ( 91.12500358871285755, -35.36225116344564157, 293.9356252759109793 ) ) ;
#18378 = CARTESIAN_POINT ( 'NONE',  ( 103.1875000000000000, 117.4749999999999943, -7.937499999999639400 ) ) ;
#18379 = LINE ( 'NONE', #11586, #35511 ) ;
#18380 = VECTOR ( 'NONE', #32083, 1000.000000000000000 ) ;
#18381 = EDGE_CURVE ( 'NONE', #35298, #73407, #39451, .T. ) ;
#18382 = ORIENTED_EDGE ( 'NONE', *, *, #65874, .F. ) ;
#18383 = VERTEX_POINT ( 'NONE', #37123 ) ;
#18384 = CARTESIAN_POINT ( 'NONE',  ( 112.8135049847298461, -43.08742197748514968, 132.5838483995059676 ) ) ;
#18386 = VERTEX_POINT ( 'NONE', #22606 ) ;
#18385 = FACE_OUTER_BOUND ( 'NONE', #53887, .T. ) ;
#18387 = DIRECTION ( 'NONE',  ( -0.4214249218767883165, -0.9068632946707806397, -4.214249218767892389E-16 ) ) ;
#18388 = CARTESIAN_POINT ( 'NONE',  ( 117.0123300003820646, -30.33189756676014426, 140.2813395616249750 ) ) ;
#18389 = CARTESIAN_POINT ( 'NONE',  ( 91.91125933621933086, -101.0284471599423739, -21.78219314458213063 ) ) ;
#18390 = LINE ( 'NONE', #58391, #35534 ) ;
#18391 = CARTESIAN_POINT ( 'NONE',  ( -74.70173812346030218, 79.26437155269049128, 92.06079644778199622 ) ) ;
#18392 = DIRECTION ( 'NONE',  ( -0.7071067811865765496, 0.7071067811865185959, -7.071067811865461528E-16 ) ) ;
#18393 = CARTESIAN_POINT ( 'NONE',  ( 110.5640613610538168, -45.86347053068967483, 62.86705384733992474 ) ) ;
#18394 = ORIENTED_EDGE ( 'NONE', *, *, #57568, .T. ) ;
#18395 = ORIENTED_EDGE ( 'NONE', *, *, #32327, .F. ) ;
#18397 = VERTEX_POINT ( 'NONE', #78474 ) ;
#18396 = VECTOR ( 'NONE', #83088, 1000.000000000000000 ) ;
#18398 = CARTESIAN_POINT ( 'NONE',  ( 204.2160000000000082, 52.73749999999999716, -44.45000000000000284 ) ) ;
#18400 = LINE ( 'NONE', #65660, #11368 ) ;
#18399 = CARTESIAN_POINT ( 'NONE',  ( 116.0678243078410787, -40.55558035091540603, 164.5070538473389661 ) ) ;
#18401 = LINE ( 'NONE', #57958, #82816 ) ;
#18402 = PLANE ( 'NONE',  #17572 ) ;
#18403 = ADVANCED_FACE ( 'NONE', ( #57093, #805 ), #29865, .T. ) ;
#18404 = DIRECTION ( 'NONE',  ( 0.000000000000000000, 0.000000000000000000, 1.000000000000000000 ) ) ;
#18405 = CARTESIAN_POINT ( 'NONE',  ( 86.13037352894073706, 94.82191660594808980, 81.46927207886326983 ) ) ;
#18406 = LINE ( 'NONE', #52887, #57454 ) ;
#18407 = CARTESIAN_POINT ( 'NONE',  ( 99.51750086509213133, -43.88776608678593760, 81.92991099019597812 ) ) ;
#18408 = EDGE_LOOP ( 'NONE', ( #3469, #61408, #43326, #25107 ) ) ;
#18409 = EDGE_CURVE ( 'NONE', #39122, #8508, #78915, .T. ) ;
#18410 = ORIENTED_EDGE ( 'NONE', *, *, #47826, .F. ) ;
#18411 = EDGE_CURVE ( 'NONE', #78071, #82260, #8525, .T. ) ;
#18412 = CARTESIAN_POINT ( 'NONE',  ( 20.03715912545730760, -24.42818131006189830, 300.4678068554150059 ) ) ;
#18413 = AXIS2_PLACEMENT_3D ( 'NONE', #62056, #20298, #47967 ) ;
#18414 = CARTESIAN_POINT ( 'NONE',  ( 126.6848757172646884, 46.51586155035142411, 31.55656739648512854 ) ) ;
#18415 = CIRCLE ( 'NONE', #69192, 3.249999999999975131 ) ;
#18416 = DIRECTION ( 'NONE',  ( 0.000000000000000000, 0.000000000000000000, 1.000000000000000000 ) ) ;
#18417 = CARTESIAN_POINT ( 'NONE',  ( 99.76898186052154927, -41.38212431049157658, 139.5842808457819615 ) ) ;
#18418 = AXIS2_PLACEMENT_3D ( 'NONE', #31434, #58259, #2862 ) ;
#18419 = VECTOR ( 'NONE', #63116, 1000.000000000000000 ) ;
#18420 = VECTOR ( 'NONE', #4909, 1000.000000000000114 ) ;
#18421 = DIRECTION ( 'NONE',  ( 0.000000000000000000, 0.000000000000000000, -1.000000000000000000 ) ) ;
#18422 = VERTEX_POINT ( 'NONE', #8980 ) ;
#18423 = VERTEX_POINT ( 'NONE', #85736 ) ;
#18424 = EDGE_CURVE ( 'NONE', #24618, #85625, #50739, .T. ) ;
#18425 = DIRECTION ( 'NONE',  ( 1.000000000000000078E-15, -1.000000000000000000, 0.000000000000000000 ) ) ;
#18426 = EDGE_LOOP ( 'NONE', ( #26895, #13101, #15695, #36841 ) ) ;
#18427 = PRODUCT_DEFINITION_SHAPE ( 'NONE', 'NONE',  #89947 ) ;
#18428 = EDGE_LOOP ( 'NONE', ( #36816, #31576 ) ) ;
#18429 = ADVANCED_FACE ( 'NONE', ( #35762, #36679 ), #51174, .F. ) ;
#18430 = DIRECTION ( 'NONE',  ( -3.100000000000000258E-29, 3.100000000000000044E-14, 1.000000000000000000 ) ) ;
#18431 = CARTESIAN_POINT ( 'NONE',  ( 115.6736222539786638, -40.49689781175994341, 204.9177737820879486 ) ) ;
#18432 = FACE_OUTER_BOUND ( 'NONE', #51674, .T. ) ;
#18433 = VECTOR ( 'NONE', #40642, 1000.000000000000000 ) ;
#18434 = VECTOR ( 'NONE', #46249, 1000.000000000000000 ) ;
#18435 = CARTESIAN_POINT ( 'NONE',  ( 19.56648329127400032, 25.62155284005901379, 323.8756252759109202 ) ) ;
#18436 = CARTESIAN_POINT ( 'NONE',  ( 97.81483072311490901, -40.51614641965803543, 17.63529977666319937 ) ) ;
#18437 = ORIENTED_EDGE ( 'NONE', *, *, #55100, .F. ) ;
#18438 = ORIENTED_EDGE ( 'NONE', *, *, #15953, .T. ) ;
#18439 = AXIS2_PLACEMENT_3D ( 'NONE', #23268, #65463, #51365 ) ;
#18440 = EDGE_LOOP ( 'NONE', ( #68546, #74741 ) ) ;
#18441 = ORIENTED_EDGE ( 'NONE', *, *, #28406, .F. ) ;
#18442 = CARTESIAN_POINT ( 'NONE',  ( 99.31750181266291122, -39.29518527230509051, 239.3995189410199487 ) ) ;
#18443 = CARTESIAN_POINT ( 'NONE',  ( 97.52207955639441650, -32.48083311392049666, 100.9927681330539713 ) ) ;
#18444 = CARTESIAN_POINT ( 'NONE',  ( 110.3472192523918380, -25.36789009815977636, 64.85276813305395649 ) ) ;
#18445 = DIRECTION ( 'NONE',  ( 0.000000000000000000, 0.000000000000000000, 1.000000000000000000 ) ) ;
#18446 = CYLINDRICAL_SURFACE ( 'NONE', #28668, 4.749999999999976907 ) ;
#18447 = CARTESIAN_POINT ( 'NONE',  ( 116.6607991934174322, -40.80763178269008762, 164.5070538473399608 ) ) ;
#18448 = FACE_BOUND ( 'NONE', #51598, .T. ) ;
#18449 = EDGE_LOOP ( 'NONE', ( #77330, #13655, #36587, #26913 ) ) ;
#18450 = CARTESIAN_POINT ( 'NONE',  ( 129.9449656991351105, 80.88456863959032717, -12.61750076990764313 ) ) ;
#18451 = ORIENTED_EDGE ( 'NONE', *, *, #2764, .F. ) ;
#18452 = ORIENTED_EDGE ( 'NONE', *, *, #45751, .F. ) ;
#18453 = LINE ( 'NONE', #72545, #33166 ) ;
#18454 = CARTESIAN_POINT ( 'NONE',  ( 48.86082318535700608, -35.55794170701751256, -5.074374724088000832 ) ) ;
#18455 = ORIENTED_EDGE ( 'NONE', *, *, #12511, .T. ) ;
#18456 = AXIS2_PLACEMENT_3D ( 'NONE', #79740, #24750, #60142 ) ;
#18457 = DIRECTION ( 'NONE',  ( -1.000000000000000000, 0.000000000000000000, 0.000000000000000000 ) ) ;
#18458 = VERTEX_POINT ( 'NONE', #14896 ) ;
#18459 = CARTESIAN_POINT ( 'NONE',  ( 116.3201542697790529, -32.94256427661516540, 65.13562527591099638 ) ) ;
#18460 = CARTESIAN_POINT ( 'NONE',  ( 109.7701363090614990, -47.44715903388583200, 92.78514908543495210 ) ) ;
#18461 = CARTESIAN_POINT ( 'NONE',  ( -3.228675327066591105, 70.25984576160145423, 130.5164141216791904 ) ) ;
#18462 = ADVANCED_FACE ( 'NONE', ( #85291 ), #42560, .T. ) ;
#18463 = LINE ( 'NONE', #87968, #55052 ) ;
#18464 = CARTESIAN_POINT ( 'NONE',  ( 138.8167039024479834, -57.40094715994099772, 58.80080685541479824 ) ) ;
#18465 = CARTESIAN_POINT ( 'NONE',  ( 99.96923091713365750, -43.45941328387855407, 81.92991099019697288 ) ) ;
#18467 = CARTESIAN_POINT ( 'NONE',  ( 100.0229104548316883, -27.23016881827670943, 181.5841967044829630 ) ) ;
#18466 = FACE_OUTER_BOUND ( 'NONE', #19659, .T. ) ;
#18468 = CARTESIAN_POINT ( 'NONE',  ( 108.4138796129811055, -26.73457821205273532, 59.96924600114584081 ) ) ;
#18469 = CARTESIAN_POINT ( 'NONE',  ( -55.95243198108136085, 55.97500000000000142, 70.69974874213239957 ) ) ;
#18470 = ORIENTED_EDGE ( 'NONE', *, *, #65431, .T. ) ;
#18471 = LINE ( 'NONE', #39370, #84635 ) ;
#18472 = CARTESIAN_POINT ( 'NONE',  ( 52.38749999999999574, 94.53880000000000905, 250.8250000000000171 ) ) ;
#18473 = CARTESIAN_POINT ( 'NONE',  ( 31.56670390244800828, -33.35206098992711077, -5.074374724088000832 ) ) ;
#18474 = DIRECTION ( 'NONE',  ( -2.973811673103097665E-16, 0.000000000000000000, -1.000000000000000000 ) ) ;
#18476 = VERTEX_POINT ( 'NONE', #84836 ) ;
#18475 = CARTESIAN_POINT ( 'NONE',  ( 97.43243490695729747, -40.91715606259069204, 231.6527681330539679 ) ) ;
#18477 = CARTESIAN_POINT ( 'NONE',  ( 172.5664832912740110, -32.07844715994070839, 254.1756252759120400 ) ) ;
#18478 = CARTESIAN_POINT ( 'NONE',  ( 99.36548562555644537, -29.67027625815665104, 271.7356252759109907 ) ) ;
#18479 = CARTESIAN_POINT ( 'NONE',  ( 108.5961642634028692, -47.12166094979025388, 138.6927681330539883 ) ) ;
#18480 = VECTOR ( 'NONE', #45916, 1000.000000000000000 ) ;
#18481 = CARTESIAN_POINT ( 'NONE',  ( 144.0667052733537901, -83.77844715994089597, 55.21780685541800437 ) ) ;
#18482 = CARTESIAN_POINT ( 'NONE',  ( 82.67951041503442866, -37.60592655292794007, 6.943955837742791459 ) ) ;
#18483 = CARTESIAN_POINT ( 'NONE',  ( 76.06670390244799762, -26.72944715994109899, 199.5838068554169524 ) ) ;
#18484 = DIRECTION ( 'NONE',  ( 0.000000000000000000, 0.000000000000000000, 1.000000000000000000 ) ) ;
#18485 = ORIENTED_EDGE ( 'NONE', *, *, #26714, .T. ) ;
#18486 = AXIS2_PLACEMENT_3D ( 'NONE', #52205, #30902, #79519 ) ;
#18488 = ADVANCED_FACE ( 'NONE', ( #50278, #49831 ), #56649, .F. ) ;
#18487 = VECTOR ( 'NONE', #89845, 1000.000000000000000 ) ;
#18489 = VECTOR ( 'NONE', #21124, 1000.000000000000000 ) ;
#18490 = ORIENTED_EDGE ( 'NONE', *, *, #42090, .F. ) ;
#18491 = VERTEX_POINT ( 'NONE', #22164 ) ;
#18492 = VERTEX_POINT ( 'NONE', #9411 ) ;
#18493 = CARTESIAN_POINT ( 'NONE',  ( -72.96458098368751166, 117.4749999999999943, 72.96458098368620426 ) ) ;
#18494 = CARTESIAN_POINT ( 'NONE',  ( 112.9508454419805332, -28.15023113465295879, 40.59848241876795782 ) ) ;
#18495 = DIRECTION ( 'NONE',  ( 0.000000000000000000, -1.000000000000000000, 0.000000000000000000 ) ) ;
#18496 = LINE ( 'NONE', #80743, #73026 ) ;
#18497 = ADVANCED_FACE ( 'NONE', ( #63933 ), #56189, .F. ) ;
#18498 = AXIS2_PLACEMENT_3D ( 'NONE', #33982, #76225, #369 ) ;
#18499 = EDGE_CURVE ( 'NONE', #79518, #4931, #64824, .T. ) ;
#18500 = AXIS2_PLACEMENT_3D ( 'NONE', #15077, #71396, #49570 ) ;
#18502 = CARTESIAN_POINT ( 'NONE',  ( 69.38289674479436542, -139.5561639417483946, 246.9828236755479907 ) ) ;
#18501 = CYLINDRICAL_SURFACE ( 'NONE', #19226, 37.00000000000000711 ) ;
#18503 = AXIS2_PLACEMENT_3D ( 'NONE', #43924, #366, #28062 ) ;
#18504 = CARTESIAN_POINT ( 'NONE',  ( 113.2432932581317289, -30.83002766685618923, 233.8552769709339429 ) ) ;
#18505 = VERTEX_POINT ( 'NONE', #63023 ) ;
#18506 = EDGE_LOOP ( 'NONE', ( #73529, #3805, #56889, #17980, #67408, #60986, #88347, #23072, #84249, #62651, #61028, #55724, #38617, #55939, #59556, #51472, #10404, #34878, #64833, #43406, #46098, #7046, #89817, #72942, #21283, #75753, #77220, #67640, #51155, #37548, #66227, #88587, #69410, #87281 ) ) ;
#18507 = VERTEX_POINT ( 'NONE', #83942 ) ;
#18508 = CARTESIAN_POINT ( 'NONE',  ( 80.06648329127399677, -18.72944715994105991, -5.074374724089057764 ) ) ;
#18510 = EDGE_CURVE ( 'NONE', #60827, #53045, #30307, .T. ) ;
#18509 = FACE_OUTER_BOUND ( 'NONE', #7337, .T. ) ;
#18511 = DIRECTION ( 'NONE',  ( 0.000000000000000000, 0.000000000000000000, 1.000000000000000000 ) ) ;
#18512 = CARTESIAN_POINT ( 'NONE',  ( 98.92341559625380398, -33.23365848574461268, 12.43586902018295426 ) ) ;
#18513 = CARTESIAN_POINT ( 'NONE',  ( 122.2221484686747317, -96.64604508066639710, -19.23816774842027044 ) ) ;
#18514 = CARTESIAN_POINT ( 'NONE',  ( -544.5124999999999318, 53.97500000000000142, 50.79999999999999716 ) ) ;
#18515 = B_SPLINE_CURVE_WITH_KNOTS ( 'NONE', 3,
 ( #65146, #58330, #22488, #71093, #2039, #45128, #71977, #86057, #2930, #29302, #31064, #51936, #57885, #15676, #8867, #23827, #36564, #30188, #50162, #77897, #30632, #51496, #79246, #64266, #10185, #58760, #17007, #23397, #78360, #79694, #50618, #16557, #85619, #56984, #2489, #44692, #51064, #84727, #29748, #57433, #85171, #86498, #72420, #44240, #37894, #22944, #43349, #3374, #9744, #16122, #24266, #43800, #71536, #9299, #37002, #65593, #64709, #17447, #8411, #78801, #37448, #36105, #63819, #1597, #24706 ),
 .UNSPECIFIED., .F., .F.,
 ( 4, 1, 1, 1, 1, 1, 2, 2, 1, 1, 1, 1, 2, 2, 1, 1, 1, 1, 1, 1, 2, 2, 1, 1, 1, 1, 1, 2, 2, 1, 1, 1, 1, 1, 2, 2, 1, 2, 2, 1, 2, 2, 2, 2, 2, 4 ),
 ( 0.000000000000000000, 0.03124999999989700600, 0.04687499999984345161, 0.05468749999981731974, 0.05859374999980424686, 0.06054687499979771736, 0.06152343749979605203, 0.06249999999979438670, 0.09374999999972724596, 0.1093749999996942862, 0.1171874999996784794, 0.1210937499996705830, 0.1230468749996672245, 0.1249999999996638522, 0.1562499999996239120, 0.1718749999996045941, 0.1796874999995961286, 0.1835937499995913824, 0.1855468749995903555, 0.1865234374995903555, 0.1870117187495903555, 0.1874999999995903555, 0.2187499999995501099, 0.2343749999995297095, 0.2421874999995189126, 0.2460937499995125566, 0.2480468749995090594, 0.2490234374995082822, 0.2499999999995075051, 0.3124999999995169420, 0.3437499999995223265, 0.3593749999995249911, 0.3671874999995263233, 0.3710937499995269895, 0.3730468749995266009, 0.3749999999995262123, 0.4374999999995722311, 0.4687499999995950462, 0.4999999999996179723, 0.5624999999996637134, 0.5937499999996874722, 0.6249999999997112310, 0.6874999999997587485, 0.7499999999998061551, 0.8749999999999031886, 1.000000000000000000 ),
 .UNSPECIFIED. ) ;
#18516 = CARTESIAN_POINT ( 'NONE',  ( 112.8396959964676682, -44.62460075896473910, 228.0784824187689708 ) ) ;
#18517 = EDGE_CURVE ( 'NONE', #19610, #34249, #32132, .T. ) ;
#18518 = PLANE ( 'NONE',  #89317 ) ;
#18519 = EDGE_LOOP ( 'NONE', ( #66584, #87890 ) ) ;
#18520 = CARTESIAN_POINT ( 'NONE',  ( 194.0371591254575776, -24.89890238294407254, 129.9678068554150343 ) ) ;
#18521 = DIRECTION ( 'NONE',  ( -1.000000000000000000, 0.000000000000000000, 0.000000000000000000 ) ) ;
#18522 = CARTESIAN_POINT ( 'NONE',  ( 106.9575452361726491, -28.53976946500068124, 57.90523322673496409 ) ) ;
#18523 = AXIS2_PLACEMENT_3D ( 'NONE', #28619, #85409, #9086 ) ;
#18524 = CARTESIAN_POINT ( 'NONE',  ( 97.81170999939396893, -40.51745679428447744, 191.6351607553995393 ) ) ;
#18525 = LINE ( 'NONE', #59848, #47596 ) ;
#18526 = DIRECTION ( 'NONE',  ( 1.000000000000000000, 4.163336342344333240E-14, 0.000000000000000000 ) ) ;
#18527 = EDGE_LOOP ( 'NONE', ( #57992, #55530, #54668, #76475 ) ) ;
#18528 = PLANE ( 'NONE',  #8826 ) ;
#18529 = EDGE_CURVE ( 'NONE', #611, #32172, #43742, .T. ) ;
#18530 = CARTESIAN_POINT ( 'NONE',  ( 122.5474368815848578, 60.65832587247668783, -45.02295694080569888 ) ) ;
#18531 = ORIENTED_EDGE ( 'NONE', *, *, #68420, .T. ) ;
#18532 = CARTESIAN_POINT ( 'NONE',  ( 106.0764471815382279, -48.53877882342441552, 112.5099109901969712 ) ) ;
#18533 = ORIENTED_EDGE ( 'NONE', *, *, #79747, .T. ) ;
#18534 = EDGE_CURVE ( 'NONE', #35180, #87084, #23942, .T. ) ;
#18535 = CARTESIAN_POINT ( 'NONE',  ( 99.05520249114191245, -33.76709814885239780, 65.46670554236195017 ) ) ;
#18536 = EDGE_CURVE ( 'NONE', #65691, #60056, #39343, .T. ) ;
#18537 = DIRECTION ( 'NONE',  ( -4.299999999999999979E-14, 1.000000000000000000, -4.100000000000000342E-29 ) ) ;
#18538 = CARTESIAN_POINT ( 'NONE',  ( 108.3172770934737628, -27.95654607328577868, 101.3958690201829711 ) ) ;
#18539 = DIRECTION ( 'NONE',  ( 0.000000000000000000, 1.000000000000000000, 0.000000000000000000 ) ) ;
#18540 = ADVANCED_FACE ( 'NONE', ( #65269, #31178, #52925, #73412 ), #11184, .T. ) ;
#18541 = AXIS2_PLACEMENT_3D ( 'NONE', #89081, #69085, #28635 ) ;
#18542 = FACE_OUTER_BOUND ( 'NONE', #4420, .T. ) ;
#18543 = CARTESIAN_POINT ( 'NONE',  ( 96.32186211137589282, -39.41937243639647903, 12.53372051400597442 ) ) ;
#18544 = CARTESIAN_POINT ( 'NONE',  ( 53.97500000000000142, 66.67499999999999716, 209.5499999999999829 ) ) ;
#18545 = ORIENTED_EDGE ( 'NONE', *, *, #80377, .T. ) ;
#18546 = DIRECTION ( 'NONE',  ( 1.000000000000000000, 4.163336342344333240E-14, 0.000000000000000000 ) ) ;
#18547 = CIRCLE ( 'NONE', #80953, 1.000000000000000888 ) ;
#18548 = ORIENTED_EDGE ( 'NONE', *, *, #31423, .F. ) ;
#18549 = VECTOR ( 'NONE', #85535, 1000.000000000000000 ) ;
#18550 = CARTESIAN_POINT ( 'NONE',  ( 90.44969454456403923, -17.59493780205715652, 239.5838068554169809 ) ) ;
#18551 = ORIENTED_EDGE ( 'NONE', *, *, #80815, .T. ) ;
#18552 = ORIENTED_EDGE ( 'NONE', *, *, #15123, .T. ) ;
#18553 = CIRCLE ( 'NONE', #69346, 5.035202529042104302 ) ;
#18554 = DIRECTION ( 'NONE',  ( 0.000000000000000000, 0.000000000000000000, 1.000000000000000000 ) ) ;
#18555 = ORIENTED_EDGE ( 'NONE', *, *, #67638, .F. ) ;
#18556 = CARTESIAN_POINT ( 'NONE',  ( 104.9788083641148688, -27.14010996210884485, 260.2470538473402826 ) ) ;
#18557 = CARTESIAN_POINT ( 'NONE',  ( 105.4983833033492715, -26.83149777197436592, 125.2004868081602353 ) ) ;
#18558 = CARTESIAN_POINT ( 'NONE',  ( 109.6430120601289957, -46.48008675456071614, 188.7814586034739364 ) ) ;
#18559 = CARTESIAN_POINT ( 'NONE',  ( 112.9631696212496905, -28.13226286662721165, 40.59848241876795782 ) ) ;
#18560 = CARTESIAN_POINT ( 'NONE',  ( 104.4076862809217516, -46.45797926106136799, 43.36475834774724802 ) ) ;
#18561 = ORIENTED_EDGE ( 'NONE', *, *, #57502, .F. ) ;
#18562 = VECTOR ( 'NONE', #85864, 1000.000000000000000 ) ;
#18563 = DIRECTION ( 'NONE',  ( 0.000000000000000000, 0.000000000000000000, 1.000000000000000000 ) ) ;
#18564 = AXIS2_PLACEMENT_3D ( 'NONE', #39527, #32712, #77644 ) ;
#18565 = AXIS2_PLACEMENT_3D ( 'NONE', #4624, #25061, #46824 ) ;
#18566 = CARTESIAN_POINT ( 'NONE',  ( 177.0371591254543659, -48.62818131005480637, 249.9678068554149775 ) ) ;
#18567 = ORIENTED_EDGE ( 'NONE', *, *, #81184, .T. ) ;
#18568 = AXIS2_PLACEMENT_3D ( 'NONE', #70712, #36185, #8944 ) ;
#18569 = DIRECTION ( 'NONE',  ( 0.000000000000000000, 0.000000000000000000, -1.000000000000000000 ) ) ;
#18570 = DIRECTION ( 'NONE',  ( 0.000000000000000000, 1.000000000000000000, 0.000000000000000000 ) ) ;
#18571 = CARTESIAN_POINT ( 'NONE',  ( 100.1919508713739049, -45.35525880799018239, 272.0289586092443415 ) ) ;
#18572 = CARTESIAN_POINT ( 'NONE',  ( -446.0240000000000009, 93.66249999999999432, 15.87500000000039968 ) ) ;
#18573 = EDGE_CURVE ( 'NONE', #4156, #8582, #87059, .T. ) ;
#18574 = DIRECTION ( 'NONE',  ( 3.999999999999999995E-14, -1.000000000000000000, 4.100000000000000342E-29 ) ) ;
#18575 = CARTESIAN_POINT ( 'NONE',  ( 79.05226586199937344, -39.28573230649617187, 1.785258109343057731 ) ) ;
#18576 = CARTESIAN_POINT ( 'NONE',  ( 100.8994401894200053, -30.77800351108903598, 250.1381341137912671 ) ) ;
#18578 = CARTESIAN_POINT ( 'NONE',  ( 102.5676158828201778, -27.34920955258912301, 91.43276813305395478 ) ) ;
#18577 = DIRECTION ( 'NONE',  ( 0.000000000000000000, 0.000000000000000000, -1.000000000000000000 ) ) ;
#18579 = CARTESIAN_POINT ( 'NONE',  ( 111.6427491051048122, 65.84630886252570292, 67.68135981035700866 ) ) ;
#18580 = CARTESIAN_POINT ( 'NONE',  ( 97.70685376065341643, -42.69687791250295561, 141.7661014663869707 ) ) ;
#18581 = ORIENTED_EDGE ( 'NONE', *, *, #6616, .F. ) ;
#18582 = FACE_OUTER_BOUND ( 'NONE', #17989, .T. ) ;
#18583 = EDGE_LOOP ( 'NONE', ( #68301, #16449, #47907 ) ) ;
#18584 = CIRCLE ( 'NONE', #50542, 0.4999999999999982236 ) ;
#18585 = CARTESIAN_POINT ( 'NONE',  ( 177.4809174648215730, -49.32844715993478246, 180.4678068554150059 ) ) ;
#18586 = CARTESIAN_POINT ( 'NONE',  ( 127.0664832912740394, -46.72944715994101017, -5.074374724089008915 ) ) ;
#18587 = CARTESIAN_POINT ( 'NONE',  ( 177.8371591254543205, -47.82818131005477369, 300.4678068554149490 ) ) ;
#18588 = ORIENTED_EDGE ( 'NONE', *, *, #58998, .F. ) ;
#18589 = CARTESIAN_POINT ( 'NONE',  ( 97.70663789874652139, -40.25152162066777350, 51.61287317870858260 ) ) ;
#18591 = ORIENTED_EDGE ( 'NONE', *, *, #51497, .F. ) ;
#18590 = CARTESIAN_POINT ( 'NONE',  ( 107.6554820827327461, -47.17179587048914158, 152.6213395616249500 ) ) ;
#18592 = DIRECTION ( 'NONE',  ( 0.000000000000000000, 0.000000000000000000, 1.000000000000000000 ) ) ;
#18593 = CARTESIAN_POINT ( 'NONE',  ( -130.0580535164678508, 88.17609398443093482, -11.39345613590910666 ) ) ;
#18594 = AXIS2_PLACEMENT_3D ( 'NONE', #31937, #10166, #87366 ) ;
#18595 = CYLINDRICAL_SURFACE ( 'NONE', #48866, 2.517499999999998739 ) ;
#18596 = AXIS2_PLACEMENT_3D ( 'NONE', #51127, #78867, #81551 ) ;
#18597 = LINE ( 'NONE', #67189, #75719 ) ;
#18598 = ORIENTED_EDGE ( 'NONE', *, *, #23271, .F. ) ;
#18599 = CARTESIAN_POINT ( 'NONE',  ( 117.2310933634200012, -39.29246586887208537, 123.6299109901969615 ) ) ;
#18600 = EDGE_CURVE ( 'NONE', #67104, #37337, #77436, .T. ) ;
#18601 = APPLICATION_PROTOCOL_DEFINITION ( 'draft international standard', 'automotive_design', 1998, #23172 ) ;
#18602 = DIRECTION ( 'NONE',  ( 0.000000000000000000, 0.000000000000000000, 1.000000000000000000 ) ) ;
#18603 = EDGE_CURVE ( 'NONE', #43538, #2385, #9862, .T. ) ;
#18604 = CARTESIAN_POINT ( 'NONE',  ( 86.06670390244796920, -50.82844715994100682, 295.9178068554149945 ) ) ;
#18605 = EDGE_LOOP ( 'NONE', ( #21370, #89509, #4564, #14187 ) ) ;
#18606 = EDGE_CURVE ( 'NONE', #26947, #63793, #72738, .T. ) ;
#18607 = ORIENTED_EDGE ( 'NONE', *, *, #22118, .T. ) ;
#18608 = FACE_OUTER_BOUND ( 'NONE', #20848, .T. ) ;
#18609 = CARTESIAN_POINT ( 'NONE',  ( 82.89895571708365196, 83.38918798244688446, -100.8594679592203676 ) ) ;
#18610 = DIRECTION ( 'NONE',  ( 0.000000000000000000, 0.000000000000000000, -1.000000000000000000 ) ) ;
#18611 = CARTESIAN_POINT ( 'NONE',  ( 184.5664832912729878, -81.37844715994266664, 342.9256252759109884 ) ) ;
#18612 = ADVANCED_FACE ( 'NONE', ( #80253 ), #30747, .F. ) ;
#18613 = EDGE_CURVE ( 'NONE', #13215, #63081, #58877, .T. ) ;
#18615 = CARTESIAN_POINT ( 'NONE',  ( -3.306873253463332496, 70.28105300984509540, -118.5105382607468130 ) ) ;
#18614 = CARTESIAN_POINT ( 'NONE',  ( 105.7992971826924986, -26.72406505859367698, 105.1773095432808987 ) ) ;
#18616 = DIRECTION ( 'NONE',  ( 1.825781832977094175E-16, -0.4999999999999998890, -0.8660254037844387076 ) ) ;
#18617 = EDGE_CURVE ( 'NONE', #6412, #70634, #6031, .T. ) ;
#18618 = AXIS2_PLACEMENT_3D ( 'NONE', #18956, #21079, #6551 ) ;
#18619 = ORIENTED_EDGE ( 'NONE', *, *, #9386, .F. ) ;
#18620 = AXIS2_PLACEMENT_3D ( 'NONE', #19835, #88441, #61163 ) ;
#18622 = EDGE_CURVE ( 'NONE', #67362, #61554, #86168, .T. ) ;
#18621 = CARTESIAN_POINT ( 'NONE',  ( 100.8874680621459987, -44.70022151100008756, 33.05229196020944471 ) ) ;
#18623 = CARTESIAN_POINT ( 'NONE',  ( 97.31640351007386869, -35.61153895465465524, 202.2356252759109623 ) ) ;
#18625 = EDGE_LOOP ( 'NONE', ( #22835, #86146 ) ) ;
#18624 = FACE_BOUND ( 'NONE', #80207, .T. ) ;
#18626 = AXIS2_PLACEMENT_3D ( 'NONE', #30059, #57754, #45002 ) ;
#18627 = CARTESIAN_POINT ( 'NONE',  ( 110.1676348244934331, -46.62498374987613659, 48.80610146638597513 ) ) ;
#18628 = FACE_OUTER_BOUND ( 'NONE', #82184, .T. ) ;
#18629 = FACE_OUTER_BOUND ( 'NONE', #40672, .T. ) ;
#18630 = ADVANCED_FACE ( 'NONE', ( #44810 ), #86613, .F. ) ;
#18631 = VECTOR ( 'NONE', #10691, 1000.000000000000000 ) ;
#18632 = CARTESIAN_POINT ( 'NONE',  ( 107.0664832912739968, -0.2185775633790978945, 335.9181252759120184 ) ) ;
#18633 = ORIENTED_EDGE ( 'NONE', *, *, #60357, .F. ) ;
#18634 = CYLINDRICAL_SURFACE ( 'NONE', #22594, 3.500000000000003109 ) ;
#18635 = CIRCLE ( 'NONE', #44691, 5.599999999999994316 ) ;
#18636 = ORIENTED_EDGE ( 'NONE', *, *, #59029, .F. ) ;
#18637 = ORIENTED_EDGE ( 'NONE', *, *, #89661, .F. ) ;
#18638 = CARTESIAN_POINT ( 'NONE',  ( 97.06047953529140671, -37.89159766150721964, 232.8501547344689584 ) ) ;
#18639 = CARTESIAN_POINT ( 'NONE',  ( 177.4809174648213173, -48.32844715993478957, 300.4678068554149490 ) ) ;
#18640 = CARTESIAN_POINT ( 'NONE',  ( -117.9423201497065321, 86.64222086580515736, -12.05142355921143960 ) ) ;
#18641 = CARTESIAN_POINT ( 'NONE',  ( 101.9936208421809454, -45.44607148214490877, 153.1564586002609190 ) ) ;
#18642 = VECTOR ( 'NONE', #84405, 1000.000000000000000 ) ;
#18643 = CARTESIAN_POINT ( 'NONE',  ( 63.03715912545637678, -24.42818131006026761, 193.9678068554150911 ) ) ;
#18644 = ORIENTED_EDGE ( 'NONE', *, *, #53180, .T. ) ;
#18645 = CARTESIAN_POINT ( 'NONE',  ( 0.000000000000000000, 44.45000000000000284, 0.000000000000000000 ) ) ;
#18646 = CARTESIAN_POINT ( 'NONE',  ( 69.97247222095467123, 91.74172417118840883, -53.74920436177191618 ) ) ;
#18647 = VERTEX_POINT ( 'NONE', #24387 ) ;
#18648 = CARTESIAN_POINT ( 'NONE',  ( 97.07516343140007109, -33.75277822987297327, 31.09562527591097592 ) ) ;
#18649 = ORIENTED_EDGE ( 'NONE', *, *, #85976, .F. ) ;
#18650 = ORIENTED_EDGE ( 'NONE', *, *, #89495, .F. ) ;
#18651 = CARTESIAN_POINT ( 'NONE',  ( 103.9533468823514823, -45.47040322110986210, 250.1223760838773273 ) ) ;
#18652 = EDGE_CURVE ( 'NONE', #296, #27915, #45246, .T. ) ;
#18653 = DIRECTION ( 'NONE',  ( 0.000000000000000000, 0.000000000000000000, -1.000000000000000000 ) ) ;
#18654 = CARTESIAN_POINT ( 'NONE',  ( 71.25443513191777356, -74.12815658812309039, 540.9756252759101471 ) ) ;
#18655 = DIRECTION ( 'NONE',  ( 0.000000000000000000, 1.000000000000000000, 0.000000000000000000 ) ) ;
#18657 = EDGE_CURVE ( 'NONE', #17073, #22233, #78098, .T. ) ;
#18656 = DIRECTION ( 'NONE',  ( -4.237773401492740281E-14, 1.000000000000000000, 0.000000000000000000 ) ) ;
#18658 = CIRCLE ( 'NONE', #86815, 20.63750000000000284 ) ;
#18659 = CARTESIAN_POINT ( 'NONE',  ( 117.8211145215647946, -31.63542911875440211, 210.1784824187679703 ) ) ;
#18660 = CYLINDRICAL_SURFACE ( 'NONE', #10838, 4.500000000000003553 ) ;
#18661 = ORIENTED_EDGE ( 'NONE', *, *, #49475, .F. ) ;
#18662 = CARTESIAN_POINT ( 'NONE',  ( 110.3678327243794541, -25.29650332976257943, 60.85276813305395649 ) ) ;
#18663 = DIRECTION ( 'NONE',  ( -4.237773401492740281E-14, 1.000000000000000000, 0.000000000000000000 ) ) ;
#18664 = ORIENTED_EDGE ( 'NONE', *, *, #17367, .F. ) ;
#18665 = ORIENTED_EDGE ( 'NONE', *, *, #80365, .F. ) ;
#18666 = VERTEX_POINT ( 'NONE', #59770 ) ;
#18667 = CARTESIAN_POINT ( 'NONE',  ( 36.74138383868084645, -48.33240602328870494, 129.9678068554150911 ) ) ;
#18668 = DIRECTION ( 'NONE',  ( 0.1858654558203329255, -0.9825752044157738396, 0.000000000000000000 ) ) ;
#18669 = CARTESIAN_POINT ( 'NONE',  ( 103.3797721312301547, -105.8297479413476196, 2.217806855418058554 ) ) ;
#18670 = CARTESIAN_POINT ( 'NONE',  ( 115.0182259351703777, -41.51125854152899564, 126.2138046553059638 ) ) ;
#18671 = CARTESIAN_POINT ( 'NONE',  ( 103.9327720845255669, -26.76365000536165439, 246.3184824187679567 ) ) ;
#18672 = FACE_OUTER_BOUND ( 'NONE', #73604, .T. ) ;
#18673 = ORIENTED_EDGE ( 'NONE', *, *, #39658, .F. ) ;
#18674 = VECTOR ( 'NONE', #24734, 1000.000000000000000 ) ;
#18675 = DIRECTION ( 'NONE',  ( 1.000000000000000000, -2.098553464303459752E-16, 0.000000000000000000 ) ) ;
#18676 = VERTEX_POINT ( 'NONE', #38437 ) ;
#18677 = ORIENTED_EDGE ( 'NONE', *, *, #11566, .T. ) ;
#18678 = CIRCLE ( 'NONE', #47647, 9.524999999999998579 ) ;
#18679 = VECTOR ( 'NONE', #21916, 1000.000000000000000 ) ;
#18680 = CARTESIAN_POINT ( 'NONE',  ( 0.000000000000000000, 92.07499999999998863, 0.000000000000000000 ) ) ;
#18681 = ORIENTED_EDGE ( 'NONE', *, *, #75951, .F. ) ;
#18682 = ORIENTED_EDGE ( 'NONE', *, *, #1668, .F. ) ;
#18683 = DIRECTION ( 'NONE',  ( 1.000000000000000078E-15, 1.000000000000000083E-30, -1.000000000000000000 ) ) ;
#18684 = DIRECTION ( 'NONE',  ( 3.100000000000000258E-29, -3.100000000000000044E-14, -1.000000000000000000 ) ) ;
#18685 = DIRECTION ( 'NONE',  ( -0.7071067812160284349, 0.7071067811570665995, -7.071067812160292375E-16 ) ) ;
#18686 = CARTESIAN_POINT ( 'NONE',  ( 109.3519496323076083, -28.49945473430254950, 174.2838483995049899 ) ) ;
#18687 = CARTESIAN_POINT ( 'NONE',  ( 112.2029234908279562, -27.56599932623266724, 34.66991099019695355 ) ) ;
#18688 = CARTESIAN_POINT ( 'NONE',  ( 107.0664832912739968, -18.82844715994099971, 335.9181252759120184 ) ) ;
#18689 = ORIENTED_EDGE ( 'NONE', *, *, #85215, .F. ) ;
#18690 = VECTOR ( 'NONE', #54930, 1000.000000000000000 ) ;
#18691 = CARTESIAN_POINT ( 'NONE',  ( -40.89999999999999858, 53.97500000000000142, 50.79999999999999716 ) ) ;
#18692 = ORIENTED_EDGE ( 'NONE', *, *, #71780, .T. ) ;
#18693 = AXIS2_PLACEMENT_3D ( 'NONE', #36530, #64230, #2001 ) ;
#18694 = FACE_OUTER_BOUND ( 'NONE', #10293, .T. ) ;
#18695 = VERTEX_POINT ( 'NONE', #46133 ) ;
#18696 = CARTESIAN_POINT ( 'NONE',  ( 97.80987186915811549, -40.51298665854582737, 167.6355175185183839 ) ) ;
#18697 = AXIS2_PLACEMENT_3D ( 'NONE', #31662, #73442, #38920 ) ;
#18698 = CARTESIAN_POINT ( 'NONE',  ( -8.321932579531722496, 73.05279115126568001, 118.2650340428489812 ) ) ;
#18699 = CARTESIAN_POINT ( 'NONE',  ( 111.0490742293896318, -45.90261773848913407, 132.9024169551198895 ) ) ;
#18700 = DIRECTION ( 'NONE',  ( 0.000000000000000000, -1.000000000000000000, 0.000000000000000000 ) ) ;
#18701 = VERTEX_POINT ( 'NONE', #73863 ) ;
#18702 = CARTESIAN_POINT ( 'NONE',  ( 116.1776873554136813, -43.03363693755514419, 13.35657765686298859 ) ) ;
#18703 = CARTESIAN_POINT ( 'NONE',  ( 113.4862441490110427, -46.74931658189198913, 64.02991099019695298 ) ) ;
#18704 = ADVANCED_FACE ( 'NONE', ( #32512 ), #12997, .F. ) ;
#18706 = DIRECTION ( 'NONE',  ( 0.000000000000000000, 0.000000000000000000, -1.000000000000000000 ) ) ;
#18705 = LINE ( 'NONE', #47739, #63681 ) ;
#18707 = DIRECTION ( 'NONE',  ( 0.7071067811874264253, -0.7071067811856686092, 7.071067811874271132E-16 ) ) ;
#18708 = ADVANCED_FACE ( 'NONE', ( #74323 ), #88406, .F. ) ;
#18709 = CARTESIAN_POINT ( 'NONE',  ( 106.3488784333137289, -25.28999724522163461, 322.7624077768622328 ) ) ;
#18710 = CARTESIAN_POINT ( 'NONE',  ( 41.56670390244695312, -36.32844715994109208, 129.9678068554150911 ) ) ;
#18711 = VECTOR ( 'NONE', #7747, 1000.000000000000000 ) ;
#18712 = ADVANCED_FACE ( 'NONE', ( #61566 ), #27504, .F. ) ;
#18713 = FACE_OUTER_BOUND ( 'NONE', #8426, .T. ) ;
#18714 = CARTESIAN_POINT ( 'NONE',  ( 145.8009859422575119, -77.83856765075479700, 247.4449540823549967 ) ) ;
#18715 = ADVANCED_FACE ( 'NONE', ( #5277 ), #20702, .F. ) ;
#18716 = ORIENTED_EDGE ( 'NONE', *, *, #53539, .T. ) ;
#18717 = CARTESIAN_POINT ( 'NONE',  ( 105.9838489277333480, -26.31625509990853828, 50.15848241876796720 ) ) ;
#18718 = CARTESIAN_POINT ( 'NONE',  ( 113.0254242409527308, -46.03885118181761982, 214.0175300378159591 ) ) ;
#18719 = CARTESIAN_POINT ( 'NONE',  ( 117.4691034930615103, -37.69004686371126667, 74.75276813305397638 ) ) ;
#18721 = CARTESIAN_POINT ( 'NONE',  ( 135.3756687995053483, -12.91806617559082504, 361.9756252759100335 ) ) ;
#18720 = CARTESIAN_POINT ( 'NONE',  ( 97.81944477327695608, -40.53632314921513569, 171.6375141567590674 ) ) ;
#18722 = CARTESIAN_POINT ( 'NONE',  ( 194.0371591254583166, -46.82818131005407736, 236.4678068554149775 ) ) ;
#18723 = VECTOR ( 'NONE', #77982, 999.9999999999998863 ) ;
#18724 = EDGE_CURVE ( 'NONE', #46977, #15780, #23066, .T. ) ;
#18725 = DIRECTION ( 'NONE',  ( -0.000000000000000000, 1.000000000000000000, 0.000000000000000000 ) ) ;
#18726 = VERTEX_POINT ( 'NONE', #41565 ) ;
#18727 = EDGE_CURVE ( 'NONE', #79957, #32858, #69300, .T. ) ;
#18728 = CARTESIAN_POINT ( 'NONE',  ( 114.2951562036312936, -44.16484043540973659, 114.2022919425769771 ) ) ;
#18730 = EDGE_LOOP ( 'NONE', ( #10747, #11305, #25473, #63166 ) ) ;
#18729 = LINE ( 'NONE', #54557, #12361 ) ;
#18731 = CARTESIAN_POINT ( 'NONE',  ( 118.0279888096067396, -35.50094427011356402, 229.9032443235299468 ) ) ;
#18732 = CARTESIAN_POINT ( 'NONE',  ( 117.0719613561143433, -35.46296010572103086, 254.9279646184726573 ) ) ;
#18733 = DIRECTION ( 'NONE',  ( 2.900000000000000265E-14, -2.000000000000000155E-15, 1.000000000000000000 ) ) ;
#18734 = CARTESIAN_POINT ( 'NONE',  ( 78.00648098368699834, 117.4749999999999943, -72.96458098368670164 ) ) ;
#18735 = DIRECTION ( 'NONE',  ( -4.299999999999999979E-14, 1.000000000000000000, -4.400000000000000367E-29 ) ) ;
#18736 = EDGE_CURVE ( 'NONE', #34428, #37855, #82049, .T. ) ;
#18737 = CARTESIAN_POINT ( 'NONE',  ( 131.3325395364355472, -37.07457063614607762, 3.076560393663394510 ) ) ;
#18738 = CARTESIAN_POINT ( 'NONE',  ( 107.0667039024470313, -104.2784471599420755, -19.78219314458201694 ) ) ;
#18739 = CARTESIAN_POINT ( 'NONE',  ( 97.29384000864233428, -37.12803473146956890, 161.3584824187679487 ) ) ;
#18740 = ORIENTED_EDGE ( 'NONE', *, *, #21390, .T. ) ;
#18741 = VERTEX_POINT ( 'NONE', #19803 ) ;
#18742 = VECTOR ( 'NONE', #27675, 999.9999999999998863 ) ;
#18743 = CARTESIAN_POINT ( 'NONE',  ( 115.8195149170444296, -38.11245691049232676, 110.1330118773259699 ) ) ;
#18744 = AXIS2_PLACEMENT_3D ( 'NONE', #33628, #6366, #68154 ) ;
#18745 = CARTESIAN_POINT ( 'NONE',  ( 20.03715912545730760, -24.42818131006189830, 300.4678068554150059 ) ) ;
#18747 = DIRECTION ( 'NONE',  ( 1.000000000000000000, 0.000000000000000000, 0.000000000000000000 ) ) ;
#18746 = CARTESIAN_POINT ( 'NONE',  ( 114.8131502045275880, -44.70447909941016462, 264.1899109901960401 ) ) ;
#18748 = CARTESIAN_POINT ( 'NONE',  ( -240.5296158183964792, 93.66249999999999432, 15.87500000000039968 ) ) ;
#18749 = DIRECTION ( 'NONE',  ( -1.000000000000000000, 0.000000000000000000, -7.867884063170659983E-16 ) ) ;
#18750 = DIRECTION ( 'NONE',  ( -0.000000000000000000, 1.000000000000000000, -0.000000000000000000 ) ) ;
#18751 = CONICAL_SURFACE ( 'NONE', #78244, 1.258750000000002922, 1.029744258676650093 ) ;
#18752 = CARTESIAN_POINT ( 'NONE',  ( 120.2221484686747317, -111.8737466215628871, -21.78219314458179667 ) ) ;
#18753 = DIRECTION ( 'NONE',  ( 0.000000000000000000, 0.000000000000000000, 1.000000000000000000 ) ) ;
#18754 = CARTESIAN_POINT ( 'NONE',  ( 107.0664832912739968, -36.72944715994100306, 287.6356252759109680 ) ) ;
#18755 = CARTESIAN_POINT ( 'NONE',  ( 97.44537786355540732, -42.12371753947140007, 181.7451490854349743 ) ) ;
#18756 = CARTESIAN_POINT ( 'NONE',  ( 0.000000000000000000, 0.000000000000000000, 0.000000000000000000 ) ) ;
#18757 = ORIENTED_EDGE ( 'NONE', *, *, #36290, .F. ) ;
#18758 = VERTEX_POINT ( 'NONE', #82499 ) ;
#18759 = CARTESIAN_POINT ( 'NONE',  ( -100.3415888741737376, 78.07027470200928576, -83.52520760052931337 ) ) ;
#18760 = DIRECTION ( 'NONE',  ( 0.000000000000000000, 0.000000000000000000, 1.000000000000000000 ) ) ;
#18761 = VECTOR ( 'NONE', #57359, 1000.000000000000000 ) ;
#18762 = DIRECTION ( 'NONE',  ( 1.000000000000000000, 0.000000000000000000, -9.299908063537919123E-17 ) ) ;
#18764 = EDGE_CURVE ( 'NONE', #30005, #85483, #35049, .T. ) ;
#18763 = CARTESIAN_POINT ( 'NONE',  ( 20.56670390244828184, -48.82844715994187368, 300.4678068554150059 ) ) ;
#18765 = B_SPLINE_CURVE_WITH_KNOTS ( 'NONE', 3,
 ( #16422, #58192, #10050, #44097, #71832, #65455, #3239, #9598, #30934, #58621, #51799, #79550, #53575, #54918, #6353, #67230, #34042, #33165 ),
 .UNSPECIFIED., .F., .F.,
 ( 4, 2, 2, 2, 2, 2, 2, 2, 4 ),
 ( 0.000000000000000000, 0.06249999997213293024, 0.1249999999442658605, 0.1874999999163987907, 0.2499999998885317209, 0.3124999998606646789, 0.3749999998327975814, 0.4374999998049304839, 0.4999999997770634419 ),
 .UNSPECIFIED. ) ;
#18766 = DIRECTION ( 'NONE',  ( 0.000000000000000000, 0.000000000000000000, -1.000000000000000000 ) ) ;
#18767 = ORIENTED_EDGE ( 'NONE', *, *, #12263, .F. ) ;
#18768 = CARTESIAN_POINT ( 'NONE',  ( -12.17775636522063643, 85.81091203684010793, 117.7279047925309925 ) ) ;
#18769 = CARTESIAN_POINT ( 'NONE',  ( 117.9328099866778246, -34.70409988052399086, 203.9851490854349549 ) ) ;
#18770 = CYLINDRICAL_SURFACE ( 'NONE', #53274, 9.999999999999998224 ) ;
#18771 = ORIENTED_EDGE ( 'NONE', *, *, #3742, .T. ) ;
#18772 = ORIENTED_EDGE ( 'NONE', *, *, #21719, .F. ) ;
#18773 = AXIS2_PLACEMENT_3D ( 'NONE', #5860, #41239, #48053 ) ;
#18774 = CARTESIAN_POINT ( 'NONE',  ( 51.56670390244899238, -32.29483332968450782, 313.9678068554150059 ) ) ;
#18775 = DIRECTION ( 'NONE',  ( -1.000000000000000000, -4.299999999999999979E-14, -9.351236661543306751E-17 ) ) ;
#18776 = CARTESIAN_POINT ( 'NONE',  ( 104.4075988886342401, -46.45794203021185353, 163.3647505914425153 ) ) ;
#18777 = CARTESIAN_POINT ( 'NONE',  ( 113.6264423535256043, -41.63348889605062908, 26.13380465530496011 ) ) ;
#18778 = CARTESIAN_POINT ( 'NONE',  ( 97.55141575199942849, -31.05946519635597269, 126.9108633711489915 ) ) ;
#18779 = CARTESIAN_POINT ( 'NONE',  ( 127.0667052882550365, -78.66107132697010229, 222.2178068554179902 ) ) ;
#18780 = ORIENTED_EDGE ( 'NONE', *, *, #67114, .F. ) ;
#18781 = EDGE_CURVE ( 'NONE', #42224, #69089, #46648, .T. ) ;
#18782 = DIRECTION ( 'NONE',  ( 0.000000000000000000, 0.8660254037844387076, -0.4999999999999998890 ) ) ;
#18783 = AXIS2_PLACEMENT_3D ( 'NONE', #47335, #4233, #75064 ) ;
#18784 = CARTESIAN_POINT ( 'NONE',  ( 81.78920663581700978, -16.57943358557456293, 7.744922197166920874 ) ) ;
#18785 = ORIENTED_EDGE ( 'NONE', *, *, #4992, .T. ) ;
#18786 = ORIENTED_EDGE ( 'NONE', *, *, #13023, .F. ) ;
#18787 = EDGE_CURVE ( 'NONE', #18458, #41728, #2054, .T. ) ;
#18788 = DIRECTION ( 'NONE',  ( 1.000000000000000000, 0.000000000000000000, 0.000000000000000000 ) ) ;
#18789 = ORIENTED_EDGE ( 'NONE', *, *, #44854, .F. ) ;
#18790 = EDGE_LOOP ( 'NONE', ( #29323, #29305, #83369, #77542 ) ) ;
#18791 = CARTESIAN_POINT ( 'NONE',  ( 98.34940958104215269, -31.65739082969130180, 156.9063178242618051 ) ) ;
#18792 = CARTESIAN_POINT ( 'NONE',  ( 115.2801527212906336, -32.91522314707135166, 58.58289601855292972 ) ) ;
#18793 = CARTESIAN_POINT ( 'NONE',  ( 97.74263787230347589, -41.52050856888216401, 196.7041967044819728 ) ) ;
#18794 = CIRCLE ( 'NONE', #57961, 2.750000000000002665 ) ;
#18795 = CARTESIAN_POINT ( 'NONE',  ( 109.4403364888817123, -25.95778788316468422, 179.8918157521019339 ) ) ;
#18797 = CARTESIAN_POINT ( 'NONE',  ( 112.1067112481348431, -26.91823048478340397, 15.71086337114896381 ) ) ;
#18796 = CARTESIAN_POINT ( 'NONE',  ( 97.81477617152367543, -40.51601309134415629, 21.63528831556280707 ) ) ;
#18798 = FACE_OUTER_BOUND ( 'NONE', #81740, .T. ) ;
#18799 = PLANE ( 'NONE',  #85999 ) ;
#18800 = ORIENTED_EDGE ( 'NONE', *, *, #33116, .F. ) ;
#18801 = VECTOR ( 'NONE', #26541, 999.9999999999998863 ) ;
#18802 = EDGE_LOOP ( 'NONE', ( #4522, #46646, #64036, #1412 ) ) ;
#18803 = CIRCLE ( 'NONE', #88465, 3.250000000000002665 ) ;
#18804 = AXIS2_PLACEMENT_3D ( 'NONE', #48352, #89736, #14323 ) ;
#18805 = CARTESIAN_POINT ( 'NONE',  ( 62.03715912545840183, -47.82818131006021645, 237.4678068554150059 ) ) ;
#18806 = CARTESIAN_POINT ( 'NONE',  ( 100.7233752965418034, -45.83866581990632483, 237.0803871806729717 ) ) ;
#18807 = VERTEX_POINT ( 'NONE', #22957 ) ;
#18808 = CARTESIAN_POINT ( 'NONE',  ( 117.2917222856570447, -34.52255020207628888, 183.9956252759109532 ) ) ;
#18809 = DIRECTION ( 'NONE',  ( -1.000000000000000000, 0.000000000000000000, 0.000000000000000000 ) ) ;
#18810 = DIRECTION ( 'NONE',  ( 1.000000000000000078E-15, 1.000000000000000083E-30, -1.000000000000000000 ) ) ;
#18811 = CARTESIAN_POINT ( 'NONE',  ( 188.5667039024479834, -62.87844715994099687, 137.2178068554150059 ) ) ;
#18812 = EDGE_CURVE ( 'NONE', #71344, #61557, #36118, .T. ) ;
#18814 = DIRECTION ( 'NONE',  ( 1.000000000000000078E-15, 1.000000000000000083E-30, -1.000000000000000000 ) ) ;
#18813 = CARTESIAN_POINT ( 'NONE',  ( 114.4830409211623419, -33.53596877257181319, 277.6356252759111385 ) ) ;
#18815 = CARTESIAN_POINT ( 'NONE',  ( 162.7131505118679797, -31.94127993907790852, 342.9256252759119548 ) ) ;
#18816 = ADVANCED_FACE ( 'NONE', ( #85186 ), #14341, .F. ) ;
#18817 = LINE ( 'NONE', #33340, #83094 ) ;
#18818 = DIRECTION ( 'NONE',  ( 0.000000000000000000, 1.000000000000000000, 0.000000000000000000 ) ) ;
#18819 = VECTOR ( 'NONE', #15302, 1000.000000000000000 ) ;
#18820 = EDGE_CURVE ( 'NONE', #60117, #29891, #64282, .T. ) ;
#18821 = CARTESIAN_POINT ( 'NONE',  ( 161.4809174648183330, -48.32844715993547879, 300.4678068554149490 ) ) ;
#18822 = CARTESIAN_POINT ( 'NONE',  ( 164.9667039024459996, -26.71338133339301635, -5.074374724088000832 ) ) ;
#18823 = CARTESIAN_POINT ( 'NONE',  ( 83.06670390244808289, -58.72944715994108122, 207.5838068554169809 ) ) ;
#18825 = ORIENTED_EDGE ( 'NONE', *, *, #41989, .F. ) ;
#18824 = CARTESIAN_POINT ( 'NONE',  ( 100.3694914525244712, -30.29371855352183118, 195.5838068554172651 ) ) ;
#18826 = EDGE_CURVE ( 'NONE', #77606, #5064, #62916, .T. ) ;
#18827 = DIRECTION ( 'NONE',  ( 3.100000000000000258E-29, -3.100000000000000044E-14, -1.000000000000000000 ) ) ;
#18828 = CARTESIAN_POINT ( 'NONE',  ( 113.2331319966886412, -45.16264392691098806, 228.0784824187679760 ) ) ;
#18829 = CARTESIAN_POINT ( 'NONE',  ( 108.9848500582430404, -47.61493517985451973, 118.7032443235299723 ) ) ;
#18830 = CARTESIAN_POINT ( 'NONE',  ( 101.3810039469494200, -45.56196318943892010, 218.1213395616249784 ) ) ;
#18831 = CARTESIAN_POINT ( 'NONE',  ( 3.174999999999879918, 111.1250000000000000, 33.98325472291465132 ) ) ;
#18832 = AXIS2_PLACEMENT_3D ( 'NONE', #57659, #70411, #84949 ) ;
#18833 = LINE ( 'NONE', #11582, #88124 ) ;
#18835 = DIRECTION ( 'NONE',  ( -0.4999999926578924114, -8.568612279970206714E-05, -0.8660254037844363761 ) ) ;
#18834 = CYLINDRICAL_SURFACE ( 'NONE', #71089, 0.5000000000000197620 ) ;
#18836 = DIRECTION ( 'NONE',  ( 0.000000000000000000, 0.000000000000000000, -1.000000000000000000 ) ) ;
#18837 = CARTESIAN_POINT ( 'NONE',  ( 86.06670390244796920, -58.72944715994112386, 198.9178068554149945 ) ) ;
#18838 = ADVANCED_FACE ( 'NONE', ( #77912 ), #68463, .T. ) ;
#18839 = VERTEX_POINT ( 'NONE', #42020 ) ;
#18840 = ORIENTED_EDGE ( 'NONE', *, *, #33959, .F. ) ;
#18841 = BREP_WITH_VOIDS ( 'NONE', #86604, ( #7833, #81688, #8987, #10099, #67821, #23948, #66688, #35626, #89470, #65572, #72248, #25060, #50594 ) );
#18842 = EDGE_CURVE ( 'NONE', #65875, #11800, #37014, .T. ) ;
#18843 = AXIS2_PLACEMENT_3D ( 'NONE', #2956, #31538, #59241 ) ;
#18844 = CARTESIAN_POINT ( 'NONE',  ( 100.3400348588553328, -31.46521817125301368, 155.2209912566479488 ) ) ;
#18846 = ORIENTED_EDGE ( 'NONE', *, *, #11468, .F. ) ;
#18845 = CARTESIAN_POINT ( 'NONE',  ( -77.39114642430010349, 127.0000000000000000, 71.77848634863050847 ) ) ;
#18847 = CARTESIAN_POINT ( 'NONE',  ( 102.0669781233241196, -27.97054301683326116, 90.48814389190501117 ) ) ;
#18848 = CARTESIAN_POINT ( 'NONE',  ( 118.8789388927531974, -36.16900092901214947, 114.8641967044819694 ) ) ;
#18849 = CARTESIAN_POINT ( 'NONE',  ( 71.25614885437424562, -84.12815644128087911, 396.9756252759102040 ) ) ;
#18850 = FACE_OUTER_BOUND ( 'NONE', #36342, .T. ) ;
#18851 = LINE ( 'NONE', #26555, #4132 ) ;
#18852 = CARTESIAN_POINT ( 'NONE',  ( 113.1782937742881927, -44.75186859022056751, 109.0939586095510805 ) ) ;
#18853 = CARTESIAN_POINT ( 'NONE',  ( 102.2761128416349123, -28.20209198692209185, 60.48419670448296159 ) ) ;
#18854 = EDGE_LOOP ( 'NONE', ( #41657, #65091, #60815, #18164 ) ) ;
#18855 = AXIS2_PLACEMENT_3D ( 'NONE', #19089, #26355, #11835 ) ;
#18856 = ORIENTED_EDGE ( 'NONE', *, *, #70728, .T. ) ;
#18857 = ORIENTED_EDGE ( 'NONE', *, *, #17487, .T. ) ;
#18858 = DIRECTION ( 'NONE',  ( 0.000000000000000000, 0.000000000000000000, 1.000000000000000000 ) ) ;
#18860 = DIRECTION ( 'NONE',  ( 0.000000000000000000, 1.000000000000000000, 0.000000000000000000 ) ) ;
#18859 = CARTESIAN_POINT ( 'NONE',  ( 108.2857792741417597, -47.02760743735399984, 158.6822919425769669 ) ) ;
#18861 = CARTESIAN_POINT ( 'NONE',  ( -450.8499999999999659, 53.97500000000000142, -1.387778780781445991E-14 ) ) ;
#18862 = CARTESIAN_POINT ( 'NONE',  ( 6.364581335559162056, 71.52860519235655090, -130.4026037055029690 ) ) ;
#18863 = CARTESIAN_POINT ( 'NONE',  ( 142.8821648370248170, -72.54478064608022692, 540.9756252759101471 ) ) ;
#18864 = CIRCLE ( 'NONE', #69634, 0.5000000000000031086 ) ;
#18865 = CARTESIAN_POINT ( 'NONE',  ( 91.26325766987402233, 88.91291927174620469, 75.67533895324436344 ) ) ;
#18866 = CARTESIAN_POINT ( 'NONE',  ( 107.0667039024470313, -104.2784471599409528, 24.21780685541800082 ) ) ;
#18867 = CARTESIAN_POINT ( 'NONE',  ( 106.8416606513709866, -48.55305329746398257, 77.56133956162491927 ) ) ;
#18868 = ORIENTED_EDGE ( 'NONE', *, *, #10614, .F. ) ;
#18869 = ORIENTED_EDGE ( 'NONE', *, *, #61272, .F. ) ;
#18870 = AXIS2_PLACEMENT_3D ( 'NONE', #52420, #73340, #9790 ) ;
#18871 = DIRECTION ( 'NONE',  ( 1.000000000000000078E-15, -1.000000000000000083E-30, -1.000000000000000000 ) ) ;
#18872 = CARTESIAN_POINT ( 'NONE',  ( -85.30153658290372221, 90.93932679091004445, -98.83759631548520019 ) ) ;
#18874 = ADVANCED_FACE ( 'NONE', ( #28397 ), #15689, .F. ) ;
#18873 = CARTESIAN_POINT ( 'NONE',  ( 31.78666935232998725, -36.02818131005891189, -5.074374724088000832 ) ) ;
#18875 = CARTESIAN_POINT ( 'NONE',  ( 114.8702562078425160, -31.70976148532177064, 142.0995189410209605 ) ) ;
#18876 = AXIS2_PLACEMENT_3D ( 'NONE', #3495, #3061, #18013 ) ;
#18877 = DIRECTION ( 'NONE',  ( 0.000000000000000000, 0.000000000000000000, -1.000000000000000000 ) ) ;
#18878 = EDGE_LOOP ( 'NONE', ( #44458, #7500, #66585 ) ) ;
#18879 = ORIENTED_EDGE ( 'NONE', *, *, #47208, .F. ) ;
#18880 = CIRCLE ( 'NONE', #36269, 24.50000000000000711 ) ;
#18881 = LINE ( 'NONE', #11162, #29374 ) ;
#18882 = ORIENTED_EDGE ( 'NONE', *, *, #11328, .T. ) ;
#18883 = ORIENTED_EDGE ( 'NONE', *, *, #32975, .T. ) ;
#18884 = CARTESIAN_POINT ( 'NONE',  ( 50.87649884952499946, -33.54226604284930602, -5.074374724088000832 ) ) ;
#18885 = CARTESIAN_POINT ( 'NONE',  ( 77.37801896924341349, -19.30949827216399939, 6.839365140900691920 ) ) ;
#18886 = CARTESIAN_POINT ( 'NONE',  ( 98.55918112442081735, -40.71722039560211925, 208.0949166392299787 ) ) ;
#18887 = CARTESIAN_POINT ( 'NONE',  ( 127.0664832912740394, -46.47944715994101017, -5.074374724089008915 ) ) ;
#18888 = VECTOR ( 'NONE', #68535, 1000.000000000000000 ) ;
#18889 = CARTESIAN_POINT ( 'NONE',  ( 173.9900000000000091, 5.112500000000000711, -7.937500000000000000 ) ) ;
#18890 = DIRECTION ( 'NONE',  ( 1.000000000000000000, 9.408669700213195533E-16, 0.000000000000000000 ) ) ;
#18891 = ORIENTED_EDGE ( 'NONE', *, *, #27144, .F. ) ;
#18892 = VERTEX_POINT ( 'NONE', #2503 ) ;
#18893 = EDGE_CURVE ( 'NONE', #59306, #69327, #40884, .T. ) ;
#18894 = ORIENTED_EDGE ( 'NONE', *, *, #20630, .T. ) ;
#18895 = VERTEX_POINT ( 'NONE', #57896 ) ;
#18896 = VECTOR ( 'NONE', #7506, 1000.000000000000000 ) ;
#18897 = CARTESIAN_POINT ( 'NONE',  ( 99.00663190570655559, -35.27291570150341471, 239.0023760838769817 ) ) ;
#18898 = CARTESIAN_POINT ( 'NONE',  ( 104.1015100224914960, -46.74719628246504044, 107.3470538473389411 ) ) ;
#18899 = CARTESIAN_POINT ( 'NONE',  ( 101.9712125536870957, -27.65933791914790874, 60.48419670448296159 ) ) ;
#18900 = CARTESIAN_POINT ( 'NONE',  ( 99.08156578439323425, -35.73259618917102642, 249.5838068554173503 ) ) ;
#18901 = DIRECTION ( 'NONE',  ( 0.000000000000000000, 0.000000000000000000, -1.000000000000000000 ) ) ;
#18902 = DIRECTION ( 'NONE',  ( 0.5000000000000015543, 0.8660254037844377084, -2.602085213965216006E-14 ) ) ;
#18903 = CARTESIAN_POINT ( 'NONE',  ( 96.05396905170981370, -35.78154916559406473, 182.2461014663869889 ) ) ;
#18904 = DIRECTION ( 'NONE',  ( -1.000000000000000000, 0.000000000000000000, -0.000000000000000000 ) ) ;
#18905 = ORIENTED_EDGE ( 'NONE', *, *, #46406, .T. ) ;
#18906 = LINE ( 'NONE', #60218, #39492 ) ;
#18907 = ORIENTED_EDGE ( 'NONE', *, *, #74700, .F. ) ;
#18908 = ORIENTED_EDGE ( 'NONE', *, *, #55362, .F. ) ;
#18909 = FACE_OUTER_BOUND ( 'NONE', #54619, .T. ) ;
#18910 = LINE ( 'NONE', #87959, #80775 ) ;
#18912 = ORIENTED_EDGE ( 'NONE', *, *, #81598, .F. ) ;
#18911 = AXIS2_PLACEMENT_3D ( 'NONE', #41536, #43334, #64248 ) ;
#18913 = CARTESIAN_POINT ( 'NONE',  ( 75.31670390244798341, -50.82844715994100682, 63.03480685541479289 ) ) ;
#18914 =( BOUNDED_CURVE ( )  B_SPLINE_CURVE ( 3, ( #46629, #53881, #67536, #5323 ),
 .UNSPECIFIED., .F., .T. ) 
 B_SPLINE_CURVE_WITH_KNOTS ( ( 4, 4 ),
 ( 8.874879220657207072E-12, 1.570796326806122467 ),
 .UNSPECIFIED. ) 
 CURVE ( )  GEOMETRIC_REPRESENTATION_ITEM ( )  RATIONAL_B_SPLINE_CURVE ( ( 1.000000000000000000, 0.8047378541238108252, 0.8047378541238108252, 1.000000000000000000 ) ) 
 REPRESENTATION_ITEM ( '' )  );
#18915 = LINE ( 'NONE', #69641, #13054 ) ;
#18916 = CARTESIAN_POINT ( 'NONE',  ( 101.7558625676976618, -27.03530485730228250, 100.4632443235299633 ) ) ;
#18917 = FACE_OUTER_BOUND ( 'NONE', #79591, .T. ) ;
#18918 = FACE_OUTER_BOUND ( 'NONE', #50933, .T. ) ;
#18919 = CARTESIAN_POINT ( 'NONE',  ( 107.0664832912739968, -36.72944715994100306, 287.6356252759109680 ) ) ;
#18922 = CARTESIAN_POINT ( 'NONE',  ( 115.0229693000240303, -29.09019634776603169, 185.4232443235299570 ) ) ;
#18921 = CARTESIAN_POINT ( 'NONE',  ( 97.81371332943018615, -40.52236848741042508, 56.63563370667147012 ) ) ;
#18920 = CARTESIAN_POINT ( 'NONE',  ( 62.56670390244752156, -48.82844715994099971, 249.9678068554150343 ) ) ;
#18923 = PLANE ( 'NONE',  #53868 ) ;
#18924 = EDGE_CURVE ( 'NONE', #27372, #17890, #13339, .T. ) ;
#18925 = CARTESIAN_POINT ( 'NONE',  ( 116.3167039024470029, -67.87844715994093292, 55.21780685541800437 ) ) ;
#18926 = ORIENTED_EDGE ( 'NONE', *, *, #75353, .F. ) ;
#18927 = CARTESIAN_POINT ( 'NONE',  ( 51.42025729302798709, -31.94127993907680718, -5.074374724088000832 ) ) ;
#18928 = VECTOR ( 'NONE', #42432, 1000.000000000000000 ) ;
#18929 = ADVANCED_FACE ( 'NONE', ( #83833 ), #49282, .F. ) ;
#18930 = CARTESIAN_POINT ( 'NONE',  ( -185.9961463128564958, 101.5999999999999943, -3.174999999999514877 ) ) ;
#18931 = ADVANCED_FACE ( 'NONE', ( #49733 ), #31520, .F. ) ;
#18932 = CARTESIAN_POINT ( 'NONE',  ( 97.33774252606986011, -34.07133272141320646, 136.1149023111836129 ) ) ;
#18933 = CIRCLE ( 'NONE', #30480, 10.00000000000002665 ) ;
#18934 = FACE_BOUND ( 'NONE', #58436, .T. ) ;
#18936 = ORIENTED_EDGE ( 'NONE', *, *, #82128, .F. ) ;
#18935 = CARTESIAN_POINT ( 'NONE',  ( 115.2864439380202271, -30.18849607537921997, 244.3613395616249875 ) ) ;
#18937 = EDGE_CURVE ( 'NONE', #15221, #2107, #51068, .T. ) ;
#18938 = DIRECTION ( 'NONE',  ( 1.000000000000000000, 4.163336342344333240E-14, 0.000000000000000000 ) ) ;
#18939 = CARTESIAN_POINT ( 'NONE',  ( 116.1584918543541960, -31.54133664852386332, 285.2384824187680579 ) ) ;
#18940 = CARTESIAN_POINT ( 'NONE',  ( 102.6793653923444651, -46.92506852294805952, 133.2651490854349561 ) ) ;
#18941 = CARTESIAN_POINT ( 'NONE',  ( 0.000000000000000000, 114.2999999999999972, -9.525000000000000355 ) ) ;
#18942 = CARTESIAN_POINT ( 'NONE',  ( 81.30994157254338006, -39.18303583363594100, 7.982915248818332365 ) ) ;
#18944 = DIRECTION ( 'NONE',  ( 0.9586846635221889512, 0.000000000000000000, -0.2844709403917162205 ) ) ;
#18943 = PLANE ( 'NONE',  #43431 ) ;
#18945 = FACE_OUTER_BOUND ( 'NONE', #81649, .T. ) ;
#18946 = LINE ( 'NONE', #6220, #26435 ) ;
#18947 = ORIENTED_EDGE ( 'NONE', *, *, #51517, .T. ) ;
#18948 = VECTOR ( 'NONE', #34105, 1000.000000000000000 ) ;
#18949 = VERTEX_POINT ( 'NONE', #67732 ) ;
#18950 = VERTEX_POINT ( 'NONE', #54072 ) ;
#18951 = EDGE_CURVE ( 'NONE', #87720, #72723, #5520, .T. ) ;
#18952 = AXIS2_PLACEMENT_3D ( 'NONE', #15004, #84516, #1376 ) ;
#18953 = ORIENTED_EDGE ( 'NONE', *, *, #32996, .T. ) ;
#18954 = DIRECTION ( 'NONE',  ( -1.000000000000000000, 0.000000000000000000, 0.000000000000000000 ) ) ;
#18955 = CARTESIAN_POINT ( 'NONE',  ( 118.7081646409640427, -34.65111545711814500, 44.96705384733895272 ) ) ;
#18956 = CARTESIAN_POINT ( 'NONE',  ( -487.2989999999999782, 14.28750000000036025, 2.863608028952925100 ) ) ;
#18957 = DIRECTION ( 'NONE',  ( -5.551115123125777653E-14, -1.000000000000000000, 0.000000000000000000 ) ) ;
#18959 = DIRECTION ( 'NONE',  ( -3.100000000000000258E-29, 3.100000000000000044E-14, 1.000000000000000000 ) ) ;
#18958 = DIRECTION ( 'NONE',  ( -1.000000000000000000, 9.376883653928684652E-16, 1.500301384628589584E-15 ) ) ;
#18960 = CARTESIAN_POINT ( 'NONE',  ( 100.8994401894200053, -30.77800351108903598, 250.1381341137912671 ) ) ;
#18961 = VERTEX_POINT ( 'NONE', #23408 ) ;
#18962 = ORIENTED_EDGE ( 'NONE', *, *, #20117, .T. ) ;
#18963 = VERTEX_POINT ( 'NONE', #16575 ) ;
#18964 = PLANE ( 'NONE',  #25361 ) ;
#18965 = CARTESIAN_POINT ( 'NONE',  ( 112.4094413778908148, -45.19673273518448298, 183.0243865414169022 ) ) ;
#18966 = DIRECTION ( 'NONE',  ( -4.237773401492740281E-14, 1.000000000000000000, 0.000000000000000000 ) ) ;
#18967 = LINE ( 'NONE', #13501, #12753 ) ;
#18968 = CARTESIAN_POINT ( 'NONE',  ( 100.3317924633492737, -42.48897995906190772, 28.32158330589695794 ) ) ;
#18969 = CIRCLE ( 'NONE', #52256, 2.117000000000007987 ) ;
#18970 = CARTESIAN_POINT ( 'NONE',  ( 118.4577320646419594, 94.30044247306076954, -4.871303722668521630 ) ) ;
#18971 = AXIS2_PLACEMENT_3D ( 'NONE', #72798, #57823, #78744 ) ;
#18972 = DIRECTION ( 'NONE',  ( 0.000000000000000000, 0.000000000000000000, 1.000000000000000000 ) ) ;
#18973 = CARTESIAN_POINT ( 'NONE',  ( 105.1480534446306621, -26.53835310083740850, 280.2365776568638580 ) ) ;
#18974 = DIRECTION ( 'NONE',  ( 0.000000000000000000, 0.000000000000000000, 1.000000000000000000 ) ) ;
#18975 = ORIENTED_EDGE ( 'NONE', *, *, #34612, .T. ) ;
#18976 = CARTESIAN_POINT ( 'NONE',  ( 111.1099401812523979, -27.53270267244794667, 55.74708093204620241 ) ) ;
#18977 = VECTOR ( 'NONE', #65349, 1000.000000000000000 ) ;
#18979 = ADVANCED_FACE ( 'NONE', ( #60914 ), #86513, .T. ) ;
#18978 = DIRECTION ( 'NONE',  ( -0.7071067811578587436, 0.7071067812152364018, 0.000000000000000000 ) ) ;
#18980 = CARTESIAN_POINT ( 'NONE',  ( 111.5100823108406587, -29.30278217496053017, 52.47761417911495130 ) ) ;
#18981 = AXIS2_PLACEMENT_3D ( 'NONE', #45019, #65037, #23720 ) ;
#18982 = DIRECTION ( 'NONE',  ( 0.4999999999999998890, 0.8660254037844387076, 0.000000000000000000 ) ) ;
#18983 = EDGE_CURVE ( 'NONE', #18305, #70548, #81507, .T. ) ;
#18984 = CARTESIAN_POINT ( 'NONE',  ( 188.5667039024479834, -62.87844715994099687, 257.2178068554150059 ) ) ;
#18985 = APPLICATION_CONTEXT ( 'automotive_design' ) ;
#18986 = CARTESIAN_POINT ( 'NONE',  ( 1.154229608196380665E-15, 125.7300000000000040, 9.425000000000000711 ) ) ;
#18987 = ORIENTED_EDGE ( 'NONE', *, *, #40043, .F. ) ;
#18988 = DIRECTION ( 'NONE',  ( 0.0001713722456129695634, -0.9999999853157764962, 0.000000000000000000 ) ) ;
#18989 = CARTESIAN_POINT ( 'NONE',  ( 124.3618578197163771, 59.12976082637415942, -39.73717948323967164 ) ) ;
#18990 = ORIENTED_EDGE ( 'NONE', *, *, #73779, .T. ) ;
#18991 = CARTESIAN_POINT ( 'NONE',  ( 117.8755673099929453, -39.04089478637848032, 108.6708633711489824 ) ) ;
#18992 = ORIENTED_EDGE ( 'NONE', *, *, #12894, .T. ) ;
#18993 = CARTESIAN_POINT ( 'NONE',  ( 107.7234663162357151, -28.21331511381966806, 69.43813411379096578 ) ) ;
#18994 = CIRCLE ( 'NONE', #47955, 0.5000000000000004441 ) ;
#18995 = AXIS2_PLACEMENT_3D ( 'NONE', #20328, #69367, #35725 ) ;
#18996 = CARTESIAN_POINT ( 'NONE',  ( 182.4202572930400095, -33.70561438051981185, -5.074374724088000832 ) ) ;
#18997 = CARTESIAN_POINT ( 'NONE',  ( 98.20303647727408247, -37.43757155718014928, 97.82158330589696504 ) ) ;
#18998 = PLANE ( 'NONE',  #11194 ) ;
#18999 = CARTESIAN_POINT ( 'NONE',  ( 71.06670390244701707, -90.27844715994098124, 51.21780685541800437 ) ) ;
#19000 = CARTESIAN_POINT ( 'NONE',  ( 106.9270610292626742, -26.24804662171751346, 56.08705384733997334 ) ) ;
#19001 = CARTESIAN_POINT ( 'NONE',  ( 184.5667039024485518, -48.82844715993447693, 180.4678068554150343 ) ) ;
#19002 = CARTESIAN_POINT ( 'NONE',  ( 99.04403941723640514, -42.84122471778974983, 256.8438871033408191 ) ) ;
#19003 = VERTEX_POINT ( 'NONE', #23843 ) ;
#19004 = ADVANCED_FACE ( 'NONE', ( #72431 ), #81826, .T. ) ;
#19005 = CARTESIAN_POINT ( 'NONE',  ( -117.8827794761417493, 80.88465057165902294, 12.61751953376163549 ) ) ;
#19006 = ORIENTED_EDGE ( 'NONE', *, *, #21294, .T. ) ;
#19007 = ORIENTED_EDGE ( 'NONE', *, *, #11540, .T. ) ;
#19008 = VECTOR ( 'NONE', #28056, 1000.000000000000000 ) ;
#19009 = FACE_OUTER_BOUND ( 'NONE', #48921, .T. ) ;
#19010 = ORIENTED_EDGE ( 'NONE', *, *, #7154, .F. ) ;
#19011 = CARTESIAN_POINT ( 'NONE',  ( 115.6529839569025455, -41.48189714014875307, 263.4241967044829948 ) ) ;
#19012 = FACE_OUTER_BOUND ( 'NONE', #39565, .T. ) ;
#19013 = CARTESIAN_POINT ( 'NONE',  ( 107.8683515708180636, -26.33524229811608919, 66.01562527591097762 ) ) ;
#19014 = AXIS2_PLACEMENT_3D ( 'NONE', #33989, #54413, #12673 ) ;
#19015 = CARTESIAN_POINT ( 'NONE',  ( 104.4926606602381014, -26.97806419231898545, 96.28046078532923957 ) ) ;
#19016 = ORIENTED_EDGE ( 'NONE', *, *, #82429, .F. ) ;
#19017 = DIRECTION ( 'NONE',  ( -1.000000000000000078E-15, 1.000000000000000083E-30, 1.000000000000000000 ) ) ;
#19018 = CARTESIAN_POINT ( 'NONE',  ( -7.941868552260229762E-13, 120.6499999999999915, 107.7702177616926065 ) ) ;
#19019 = EDGE_LOOP ( 'NONE', ( #59989, #42503, #34045, #7970 ) ) ;
#19020 = CYLINDRICAL_SURFACE ( 'NONE', #57671, 118.3560000000000088 ) ;
#19021 = CARTESIAN_POINT ( 'NONE',  ( 107.0664832912739399, -36.72944715994095333, 293.6356252759109680 ) ) ;
#19022 = CARTESIAN_POINT ( 'NONE',  ( 95.25611604350963546, -37.33230102880722967, 271.3670538473393776 ) ) ;
#19023 = DIRECTION ( 'NONE',  ( 0.000000000000000000, 0.000000000000000000, 1.000000000000000000 ) ) ;
#19024 = DIRECTION ( 'NONE',  ( -1.000000000000000078E-15, 1.000000000000000083E-30, 1.000000000000000000 ) ) ;
#19025 = CARTESIAN_POINT ( 'NONE',  ( 100.8881267872233707, -44.70076677403937282, 92.05261961146344163 ) ) ;
#19026 = CARTESIAN_POINT ( 'NONE',  ( 105.2433400634091925, -28.35518594498741507, 259.6695626852197734 ) ) ;
#19028 = CARTESIAN_POINT ( 'NONE',  ( 96.81317962367450036, -38.48968277746985933, 87.46133956162493917 ) ) ;
#19027 = CARTESIAN_POINT ( 'NONE',  ( 108.6549043256371618, -26.75500537441465099, 99.95237438151097820 ) ) ;
#19029 = CARTESIAN_POINT ( 'NONE',  ( 165.9667039024459996, -26.71338133339301635, -5.074374724088000832 ) ) ;
#19030 = CARTESIAN_POINT ( 'NONE',  ( 117.3534821530742107, -34.78408995979881269, 158.9756252759109714 ) ) ;
#19031 = ORIENTED_EDGE ( 'NONE', *, *, #70012, .F. ) ;
#19032 = PLANE ( 'NONE',  #81542 ) ;
#19033 = EDGE_LOOP ( 'NONE', ( #81166, #85326, #20636, #41377 ) ) ;
#19034 = DIRECTION ( 'NONE',  ( 0.3356862014592719712, 0.000000000000000000, -0.9419738712670565617 ) ) ;
#19035 = VECTOR ( 'NONE', #46405, 1000.000000000000000 ) ;
#19036 = LINE ( 'NONE', #80388, #49356 ) ;
#19037 = CARTESIAN_POINT ( 'NONE',  ( 134.2548946453517260, -33.97944715994100306, 1.625625275910998147 ) ) ;
#19039 = VERTEX_POINT ( 'NONE', #38340 ) ;
#19038 = EDGE_CURVE ( 'NONE', #68139, #41462, #71392, .T. ) ;
#19040 = CARTESIAN_POINT ( 'NONE',  ( 9.749037034254362410, 223.9999999999999716, 152.4294779587682740 ) ) ;
#19042 = VERTEX_POINT ( 'NONE', #44253 ) ;
#19041 = CARTESIAN_POINT ( 'NONE',  ( 102.3405178495751215, -46.07139110582879482, 127.2041967044829960 ) ) ;
#19044 = LINE ( 'NONE', #4969, #43565 ) ;
#19043 = UNCERTAINTY_MEASURE_WITH_UNIT (LENGTH_MEASURE( 1.000000000000000082E-05 ), #73666, 'distance_accuracy_value', 'NONE');
#19045 = CARTESIAN_POINT ( 'NONE',  ( -130.5560151749589295, 95.25015599858942039, -0.4097429349699925338 ) ) ;
#19046 = CIRCLE ( 'NONE', #24813, 3.174999999999997158 ) ;
#19047 = CARTESIAN_POINT ( 'NONE',  ( 109.6430121245902853, -46.48008673684198300, 118.7814586087551447 ) ) ;
#19048 = CARTESIAN_POINT ( 'NONE',  ( 97.81169962758427516, -40.51743340529665005, 76.63548575323150658 ) ) ;
#19049 = ORIENTED_EDGE ( 'NONE', *, *, #58787, .T. ) ;
#19050 = AXIS2_PLACEMENT_3D ( 'NONE', #75773, #355, #40341 ) ;
#19051 = DIRECTION ( 'NONE',  ( -1.573642578468252655E-16, -2.847986909583865776E-33, -1.000000000000000000 ) ) ;
#19052 = LINE ( 'NONE', #45396, #8042 ) ;
#19053 = FACE_OUTER_BOUND ( 'NONE', #62649, .T. ) ;
#19054 = VERTEX_POINT ( 'NONE', #61351 ) ;
#19055 = EDGE_CURVE ( 'NONE', #26390, #29421, #67022, .T. ) ;
#19056 = ORIENTED_EDGE ( 'NONE', *, *, #4980, .T. ) ;
#19057 = DIRECTION ( 'NONE',  ( 0.000000000000000000, 1.000000000000000000, 0.000000000000000000 ) ) ;
#19058 = PRODUCT ( 'BR-Y-104', 'BR-Y-104', '', ( #32675 ) ) ;
#19059 = CARTESIAN_POINT ( 'NONE',  ( 91.72735010416676005, 95.24968527363472504, -92.90667244829690219 ) ) ;
#19060 = EDGE_CURVE ( 'NONE', #25721, #54206, #19579, .T. ) ;
#19061 = CARTESIAN_POINT ( 'NONE',  ( -47.18030668273772221, 100.5999999999999659, 75.34738655934135920 ) ) ;
#19062 = PLANE ( 'NONE',  #87967 ) ;
#19064 = DIRECTION ( 'NONE',  ( 0.000000000000000000, 0.000000000000000000, -1.000000000000000000 ) ) ;
#19063 = DIRECTION ( 'NONE',  ( 0.000000000000000000, -1.000000000000000000, 0.000000000000000000 ) ) ;
#19065 = CARTESIAN_POINT ( 'NONE',  ( 97.70662569943051778, -40.25148919734539277, 181.6128704218694168 ) ) ;
#19066 = ORIENTED_EDGE ( 'NONE', *, *, #40506, .T. ) ;
#19067 = LINE ( 'NONE', #27220, #56340 ) ;
#19068 = CARTESIAN_POINT ( 'NONE',  ( 109.4488926988246504, -27.20905326525217660, 195.8813395616249977 ) ) ;
#19069 = AXIS2_PLACEMENT_3D ( 'NONE', #60919, #68194, #27743 ) ;
#19071 = EDGE_LOOP ( 'NONE', ( #33926, #89221, #42956, #86525 ) ) ;
#19070 = CARTESIAN_POINT ( 'NONE',  ( -29.99999999999998224, 172.0000000000000000, 113.8826257785461280 ) ) ;
#19072 = CARTESIAN_POINT ( 'NONE',  ( 103.6990349130722677, -26.13358598113153164, 51.32133956162493149 ) ) ;
#19073 = CARTESIAN_POINT ( 'NONE',  ( 112.4075703148740644, -45.19790706062806862, 53.02421102707163669 ) ) ;
#19074 = LINE ( 'NONE', #81768, #44167 ) ;
#19075 = VECTOR ( 'NONE', #37480, 1000.000000000000000 ) ;
#19076 = DIRECTION ( 'NONE',  ( -0.000000000000000000, 1.000000000000000000, 0.000000000000000000 ) ) ;
#19077 = EDGE_LOOP ( 'NONE', ( #2687, #27498, #81556, #75523 ) ) ;
#19078 = DIRECTION ( 'NONE',  ( 1.000000000000000078E-15, -1.000000000000000000, 0.000000000000000000 ) ) ;
#19079 = VERTEX_POINT ( 'NONE', #44703 ) ;
#19080 = ORIENTED_EDGE ( 'NONE', *, *, #65080, .T. ) ;
#19081 = CARTESIAN_POINT ( 'NONE',  ( 100.1609931986295976, -31.17584605865120295, 237.2187261630399746 ) ) ;
#19082 = CARTESIAN_POINT ( 'NONE',  ( 115.0392291604921127, -42.90596946611127294, 54.30216204422613657 ) ) ;
#19083 = CARTESIAN_POINT ( 'NONE',  ( -118.0645351272586936, 89.26692529358285810, -10.78628659036711035 ) ) ;
#19084 = ADVANCED_FACE ( 'NONE', ( #51511 ), #79706, .T. ) ;
#19085 = CARTESIAN_POINT ( 'NONE',  ( 25.56670390244797275, -65.37844715994100397, 142.0928068554150059 ) ) ;
#19086 = CARTESIAN_POINT ( 'NONE',  ( 165.9667039024476196, -26.71338133338713305, 193.9678068554149775 ) ) ;
#19088 = EDGE_LOOP ( 'NONE', ( #1798, #60811, #79950, #16627, #39719, #71983, #40549, #60676, #10131 ) ) ;
#19087 = AXIS2_PLACEMENT_3D ( 'NONE', #2089, #29794, #22539 ) ;
#19089 = CARTESIAN_POINT ( 'NONE',  ( -215.9000000000000057, 53.97500000000000142, 50.79999999999999716 ) ) ;
#19090 = LINE ( 'NONE', #40427, #12151 ) ;
#19091 = ORIENTED_EDGE ( 'NONE', *, *, #67463, .F. ) ;
#19092 = CARTESIAN_POINT ( 'NONE',  ( 109.2074818670226222, -48.35976665079991221, 277.7213395616254843 ) ) ;
#19093 = VERTEX_POINT ( 'NONE', #5972 ) ;
#19094 = ORIENTED_EDGE ( 'NONE', *, *, #38245, .F. ) ;
#19095 = CARTESIAN_POINT ( 'NONE',  ( 104.6179474607139213, -28.94263790944830106, 248.1366617981629474 ) ) ;
#19096 = CARTESIAN_POINT ( 'NONE',  ( 31.75000000000000000, 111.1250000000000000, -3.174999999999999822 ) ) ;
#19097 = CARTESIAN_POINT ( 'NONE',  ( 113.2097911582632861, -29.11871762112820150, 164.5356252759109736 ) ) ;
#19098 = CARTESIAN_POINT ( 'NONE',  ( 196.2150000000000034, 30.98800000000000310, 57.14999999999999858 ) ) ;
#19099 = CARTESIAN_POINT ( 'NONE',  ( 49.16670390244647137, -26.71338133339277121, 193.9678068554150911 ) ) ;
#19100 = DIRECTION ( 'NONE',  ( -0.5000000000000012212, 0.8660254037844379305, -2.684678751731759663E-14 ) ) ;
#19101 = AXIS2_PLACEMENT_3D ( 'NONE', #64969, #85879, #51313 ) ;
#19102 = B_SPLINE_CURVE_WITH_KNOTS ( 'NONE', 3,
 ( #3397, #52831, #87856, #51961, #31090, #86528, #59676, #66503, #16587, #79717, #87407, #52394, #18353, #46039, #80160, #11558, #24295, #2955 ),
 .UNSPECIFIED., .F., .F.,
 ( 4, 2, 2, 2, 2, 2, 2, 2, 4 ),
 ( 0.000000000000000000, 0.06249958877818252018, 0.1249991775563650404, 0.1874987663345475675, 0.2499983551127300807, 0.3124979438909126217, 0.3749975326690951349, 0.4374971214472776482, 0.4999967102254601614 ),
 .UNSPECIFIED. ) ;
#19103 = CARTESIAN_POINT ( 'NONE',  ( 115.5527055449870772, -29.57532036350955806, 220.3718157521019521 ) ) ;
#19104 = CARTESIAN_POINT ( 'NONE',  ( 89.55214429302422730, 92.12496802699136822, -77.69357874334680503 ) ) ;
#19105 = EDGE_LOOP ( 'NONE', ( #29358, #64834, #54730, #59920 ) ) ;
#19106 = VECTOR ( 'NONE', #29759, 1000.000000000000000 ) ;
#19107 = B_SPLINE_CURVE_WITH_KNOTS ( 'NONE', 3,
 ( #17827, #31006, #17386, #58700, #80073, #23336, #80514, #25085, #24208, #38267, #9239, #86440, #11004, #52749, #85558, #3315, #71914, #43740, #71477, #30126, #65089, #51002, #37836, #23770, #36937, #51875, #65963, #16499, #2872, #30570, #58269 ),
 .UNSPECIFIED., .F., .F.,
 ( 4, 2, 2, 1, 2, 2, 2, 2, 2, 2, 2, 1, 1, 2, 2, 2, 4 ),
 ( 0.000000000000000000, 0.06249999999999088229, 0.09374999999998391564, 0.1093749999999804184, 0.1171874999999810013, 0.1249999999999815842, 0.1874999999999718558, 0.2187499999999680811, 0.2499999999999643063, 0.3124999999999580891, 0.3437499999999560907, 0.3593749999999550915, 0.3671874999999563682, 0.3710937499999579225, 0.3749999999999594213, 0.4374999999999796829, 0.5000000000000000000 ),
 .UNSPECIFIED. ) ;
#19108 = CARTESIAN_POINT ( 'NONE',  ( 96.04171114508396556, -38.01470880000633201, 82.43086337114895912 ) ) ;
#19109 = EDGE_CURVE ( 'NONE', #4210, #89451, #72799, .T. ) ;
#19110 = CARTESIAN_POINT ( 'NONE',  ( -446.0240000000000009, 53.97500000000000142, 50.79999999999999716 ) ) ;
#19111 = VERTEX_POINT ( 'NONE', #37905 ) ;
#19113 = ADVANCED_FACE ( 'NONE', ( #68189 ), #33214, .T. ) ;
#19112 = VERTEX_POINT ( 'NONE', #74997 ) ;
#19114 = ORIENTED_EDGE ( 'NONE', *, *, #26850, .T. ) ;
#19115 = EDGE_CURVE ( 'NONE', #87454, #71894, #30645, .T. ) ;
#19116 = CARTESIAN_POINT ( 'NONE',  ( 29.56670390244797630, -48.82844715994099971, 300.9178068554150514 ) ) ;
#19117 = DIRECTION ( 'NONE',  ( 1.000000000000000078E-15, -1.000000000000000083E-30, -1.000000000000000000 ) ) ;
#19118 = CARTESIAN_POINT ( 'NONE',  ( 188.5667039024479834, -62.87844715994099687, 290.4678068554150627 ) ) ;
#19119 = CARTESIAN_POINT ( 'NONE',  ( 108.0140583617620820, -28.59404368299928123, 127.8023760838769505 ) ) ;
#19120 = CARTESIAN_POINT ( 'NONE',  ( 116.5464386332369600, -41.20266105201044127, 224.4756252759109714 ) ) ;
#19121 = EDGE_CURVE ( 'NONE', #13980, #48446, #47271, .T. ) ;
#19122 = AXIS2_PLACEMENT_3D ( 'NONE', #4680, #32360, #60062 ) ;
#19123 = CARTESIAN_POINT ( 'NONE',  ( 90.06670420047024095, -102.7784471599409670, 55.21780685541800437 ) ) ;
#19124 = EDGE_LOOP ( 'NONE', ( #34824, #36264 ) ) ;
#19125 = CARTESIAN_POINT ( 'NONE',  ( 130.2877996231769941, 92.12504059357186748, 8.385216644675763220 ) ) ;
#19126 = EDGE_CURVE ( 'NONE', #17346, #30864, #45220, .T. ) ;
#19127 = DIRECTION ( 'NONE',  ( 0.000000000000000000, 1.000000000000000000, 0.000000000000000000 ) ) ;
#19128 = ORIENTED_EDGE ( 'NONE', *, *, #78023, .T. ) ;
#19130 = ORIENTED_EDGE ( 'NONE', *, *, #1498, .F. ) ;
#19129 = VECTOR ( 'NONE', #19057, 1000.000000000000000 ) ;
#19131 = ADVANCED_FACE ( 'NONE', ( #20495, #55865 ), #14575, .T. ) ;
#19132 = EDGE_CURVE ( 'NONE', #15662, #10687, #75455, .T. ) ;
#19133 = AXIS2_PLACEMENT_3D ( 'NONE', #79462, #72185, #24485 ) ;
#19134 = PLANE ( 'NONE',  #41575 ) ;
#19135 = ORIENTED_EDGE ( 'NONE', *, *, #45799, .T. ) ;
#19136 = VERTEX_POINT ( 'NONE', #28175 ) ;
#19137 = FACE_OUTER_BOUND ( 'NONE', #35719, .T. ) ;
#19138 = DIRECTION ( 'NONE',  ( 1.000000000000000000, 0.000000000000000000, 0.000000000000000000 ) ) ;
#19139 = ADVANCED_FACE ( 'NONE', ( #42251, #77245, #13226 ), #89080, .T. ) ;
#19140 = DIRECTION ( 'NONE',  ( 0.8660254037844389297, -0.4999999999999993894, 1.550000000000000968E-14 ) ) ;
#19141 = CARTESIAN_POINT ( 'NONE',  ( 99.37165735872611094, -40.43697808898449608, 171.1067055423629597 ) ) ;
#19142 = CIRCLE ( 'NONE', #69918, 130.5560000000000116 ) ;
#19143 = CARTESIAN_POINT ( 'NONE',  ( 106.5157732221739195, -25.64298685704507363, 45.12800622829193742 ) ) ;
#19144 = ORIENTED_EDGE ( 'NONE', *, *, #37020, .F. ) ;
#19145 = CARTESIAN_POINT ( 'NONE',  ( 98.34945445922909357, -31.65731027460955005, 126.9065242933907456 ) ) ;
#19146 = ORIENTED_EDGE ( 'NONE', *, *, #78631, .T. ) ;
#19147 = FACE_OUTER_BOUND ( 'NONE', #79873, .T. ) ;
#19148 = AXIS2_PLACEMENT_3D ( 'NONE', #50988, #58255, #78729 ) ;
#19150 = ORIENTED_EDGE ( 'NONE', *, *, #7988, .F. ) ;
#19149 = EDGE_CURVE ( 'NONE', #50592, #74753, #21383, .T. ) ;
#19151 = CARTESIAN_POINT ( 'NONE',  ( 97.31587469922506273, -39.30605313450122651, 262.5315195711698379 ) ) ;
#19152 = AXIS2_PLACEMENT_3D ( 'NONE', #72077, #85719, #8966 ) ;
#19153 = EDGE_LOOP ( 'NONE', ( #59815, #10726, #75228, #16436, #58537 ) ) ;
#19154 = CARTESIAN_POINT ( 'NONE',  ( 105.0763451348094861, -26.90764585894701710, 166.2350905474758065 ) ) ;
#19155 = CARTESIAN_POINT ( 'NONE',  ( 133.3464018318852595, -128.1369193926091157, 249.3173333679100097 ) ) ;
#19156 = LINE ( 'NONE', #12797, #8392 ) ;
#19157 = DIRECTION ( 'NONE',  ( 0.000000000000000000, 0.000000000000000000, -1.000000000000000000 ) ) ;
#19158 = ORIENTED_EDGE ( 'NONE', *, *, #39739, .F. ) ;
#19159 = CARTESIAN_POINT ( 'NONE',  ( 111.1376129892989013, -47.03096861136451423, 22.88800622829195675 ) ) ;
#19160 = CARTESIAN_POINT ( 'NONE',  ( 115.0558824863888390, -43.54908903376227158, 59.26419670448196086 ) ) ;
#19161 =( LENGTH_UNIT ( ) NAMED_UNIT ( * ) SI_UNIT ( .MILLI., .METRE. ) );
#19163 = PLANE ( 'NONE',  #68949 ) ;
#19162 = CARTESIAN_POINT ( 'NONE',  ( 151.0371591254585155, -46.82818131005592477, 117.4678068554150485 ) ) ;
#19164 = CARTESIAN_POINT ( 'NONE',  ( 97.31584198560500454, -39.30596968595895646, 147.5320030024637674 ) ) ;
#19165 = FACE_OUTER_BOUND ( 'NONE', #26560, .T. ) ;
#19166 = EDGE_CURVE ( 'NONE', #4210, #3366, #70429, .T. ) ;
#19167 = CARTESIAN_POINT ( 'NONE',  ( 100.2650085812441461, -33.56876024586312468, 9.125625275910969947 ) ) ;
#19168 = ADVANCED_FACE ( 'NONE', ( #34993 ), #15015, .F. ) ;
#19169 = ADVANCED_FACE ( 'NONE', ( #82730 ), #69531, .T. ) ;
#19170 = DIRECTION ( 'NONE',  ( 0.000000000000000000, -1.000000000000000000, 0.000000000000000000 ) ) ;
#19171 = ORIENTED_EDGE ( 'NONE', *, *, #15398, .T. ) ;
#19172 = CARTESIAN_POINT ( 'NONE',  ( 104.7257947241298979, -47.57997989614905521, 32.41943479972098174 ) ) ;
#19173 = CARTESIAN_POINT ( 'NONE',  ( 116.8574199659429098, -40.30995640862995799, 214.5470538473389581 ) ) ;
#19174 = CARTESIAN_POINT ( 'NONE',  ( 112.5256494142567192, -27.82244069900259476, 90.63848241876793566 ) ) ;
#19175 = EDGE_CURVE ( 'NONE', #70797, #79957, #8203, .T. ) ;
#19176 = VECTOR ( 'NONE', #78066, 1000.000000000000000 ) ;
#19178 = CARTESIAN_POINT ( 'NONE',  ( 134.0664832912740110, -46.42944715994100591, 4.925625275910997303 ) ) ;
#19177 = CARTESIAN_POINT ( 'NONE',  ( 98.38064376042838433, -41.69566365478069514, 171.7393974040084288 ) ) ;
#19179 = DIRECTION ( 'NONE',  ( 1.000000000000000000, 0.000000000000000000, 0.000000000000000000 ) ) ;
#19180 = VECTOR ( 'NONE', #79344, 1000.000000000000000 ) ;
#19181 = CARTESIAN_POINT ( 'NONE',  ( 133.3763347640258417, -80.31065270615032148, 249.3055338466990065 ) ) ;
#19182 = ORIENTED_EDGE ( 'NONE', *, *, #40334, .T. ) ;
#19183 = CARTESIAN_POINT ( 'NONE',  ( 113.4367438382843716, -44.15125393826585309, 104.1413395616249744 ) ) ;
#19185 = ORIENTED_EDGE ( 'NONE', *, *, #71219, .F. ) ;
#19184 = CARTESIAN_POINT ( 'NONE',  ( -479.3614999999999782, 97.78694598552370110, 18.25625000000050235 ) ) ;
#19186 = CARTESIAN_POINT ( 'NONE',  ( 118.0585799961420577, -32.36802338489823683, 245.1270538473389706 ) ) ;
#19187 = LINE ( 'NONE', #74150, #57077 ) ;
#19188 = PRODUCT_DEFINITION_SHAPE ( 'NONE', 'NONE',  #89933 ) ;
#19189 = CARTESIAN_POINT ( 'NONE',  ( 67.06670390244707392, -140.6784471599409869, 247.2178068554179902 ) ) ;
#19190 = DIRECTION ( 'NONE',  ( 0.000000000000000000, -1.000000000000000000, 0.000000000000000000 ) ) ;
#19191 = CARTESIAN_POINT ( 'NONE',  ( 71.23990787207000608, 10.64204399490126463, 396.9756252759102040 ) ) ;
#19192 = AXIS2_PLACEMENT_3D ( 'NONE', #34845, #35734, #7150 ) ;
#19193 = CARTESIAN_POINT ( 'NONE',  ( 133.8780722764277868, -39.47944715994101728, 1.625625275910997258 ) ) ;
#19194 = CARTESIAN_POINT ( 'NONE',  ( 13.86911000615387302, 223.9999999999999716, 102.9892450244911686 ) ) ;
#19195 = CARTESIAN_POINT ( 'NONE',  ( 96.03815445040686427, -38.18343476501375022, 151.4299109901969871 ) ) ;
#19196 = EDGE_LOOP ( 'NONE', ( #83103, #4620, #74826, #20047 ) ) ;
#19197 = ORIENTED_EDGE ( 'NONE', *, *, #18304, .T. ) ;
#19198 = CARTESIAN_POINT ( 'NONE',  ( 115.6883067454668463, -38.90345035940969609, 120.0615833058969457 ) ) ;
#19199 = VECTOR ( 'NONE', #28058, 1000.000000000000000 ) ;
#19200 = DIRECTION ( 'NONE',  ( 3.665114028111779382E-18, -0.9995520592605569021, 0.02992792722492374630 ) ) ;
#19202 = DIRECTION ( 'NONE',  ( 1.000000000000000000, 0.000000000000000000, 0.000000000000000000 ) ) ;
#19201 = CARTESIAN_POINT ( 'NONE',  ( 109.0793648129487678, -47.66380996059997699, 273.7213395616246885 ) ) ;
#19203 = FACE_OUTER_BOUND ( 'NONE', #46220, .T. ) ;
#19204 = AXIS2_PLACEMENT_3D ( 'NONE', #59354, #87083, #46158 ) ;
#19205 = CARTESIAN_POINT ( 'NONE',  ( 1.166476076187854022E-15, 1.270000000000000018, 9.525000000000000355 ) ) ;
#19206 = DIRECTION ( 'NONE',  ( 0.000000000000000000, 0.000000000000000000, 1.000000000000000000 ) ) ;
#19207 = CARTESIAN_POINT ( 'NONE',  ( 194.5664832912729878, -71.37844715994266664, 342.9256252759109884 ) ) ;
#19208 = DIRECTION ( 'NONE',  ( -0.000000000000000000, -0.000000000000000000, 1.000000000000000000 ) ) ;
#19209 = CARTESIAN_POINT ( 'NONE',  ( 118.8526415125689937, -37.69623653580512723, 188.7613395616259595 ) ) ;
#19210 = CARTESIAN_POINT ( 'NONE',  ( 112.1406058298522197, -28.01353614044138496, 169.6558318805149668 ) ) ;
#19211 = ORIENTED_EDGE ( 'NONE', *, *, #23257, .T. ) ;
#19212 = ORIENTED_EDGE ( 'NONE', *, *, #73254, .F. ) ;
#19213 = CARTESIAN_POINT ( 'NONE',  ( -85.96437953530681852, 73.28356282573680858, -98.26026929335846205 ) ) ;
#19214 = LINE ( 'NONE', #5132, #33080 ) ;
#19215 = LINE ( 'NONE', #54593, #30211 ) ;
#19216 = DIRECTION ( 'NONE',  ( 0.000000000000000000, 0.000000000000000000, 1.000000000000000000 ) ) ;
#19217 = CARTESIAN_POINT ( 'NONE',  ( -179.8898777604659927, 20.32000000000000028, -123.4696824136383952 ) ) ;
#19218 = ORIENTED_EDGE ( 'NONE', *, *, #48741, .T. ) ;
#19219 = CARTESIAN_POINT ( 'NONE',  ( 38.10000000000000142, 82.54999999999999716, 302.8950000000000387 ) ) ;
#19220 = EDGE_CURVE ( 'NONE', #77666, #40553, #56430, .T. ) ;
#19221 = CARTESIAN_POINT ( 'NONE',  ( 116.3775870818408151, -41.41883695635522145, 203.4556252759109611 ) ) ;
#19222 = EDGE_CURVE ( 'NONE', #11460, #82260, #483, .T. ) ;
#19223 = CARTESIAN_POINT ( 'NONE',  ( 59.67079009362632291, -0.9310397146383332379, 540.9756252759101471 ) ) ;
#19224 = ORIENTED_EDGE ( 'NONE', *, *, #73141, .T. ) ;
#19225 = EDGE_CURVE ( 'NONE', #50035, #22899, #8608, .T. ) ;
#19226 = AXIS2_PLACEMENT_3D ( 'NONE', #47085, #40288, #18958 ) ;
#19227 = LINE ( 'NONE', #46901, #2817 ) ;
#19228 = DIRECTION ( 'NONE',  ( 0.000000000000000000, 0.000000000000000000, 1.000000000000000000 ) ) ;
#19229 = CARTESIAN_POINT ( 'NONE',  ( 112.0650627701821094, -45.48886962380960597, 163.9897151582021593 ) ) ;
#19230 = CARTESIAN_POINT ( 'NONE',  ( 115.6864120445923163, -37.50259225211298286, 31.56142370292397459 ) ) ;
#19231 = CARTESIAN_POINT ( 'NONE',  ( 109.0764703591063522, -47.62188296335364157, 123.7337205140059666 ) ) ;
#19232 = EDGE_CURVE ( 'NONE', #66717, #8294, #28634, .T. ) ;
#19233 = DIRECTION ( 'NONE',  ( 0.000000000000000000, 0.000000000000000000, 1.000000000000000000 ) ) ;
#19234 = VERTEX_POINT ( 'NONE', #84067 ) ;
#19235 = EDGE_CURVE ( 'NONE', #64042, #72016, #6400, .T. ) ;
#19236 = DIRECTION ( 'NONE',  ( -1.000000000000000078E-15, 0.000000000000000000, 1.000000000000000000 ) ) ;
#19237 = CARTESIAN_POINT ( 'NONE',  ( 121.3178890780284434, -113.5468731908974291, -21.78219314458173983 ) ) ;
#19238 = ORIENTED_EDGE ( 'NONE', *, *, #88478, .F. ) ;
#19239 = ORIENTED_EDGE ( 'NONE', *, *, #22071, .T. ) ;
#19240 = ADVANCED_FACE ( 'NONE', ( #61797 ), #89534, .F. ) ;
#19241 = CIRCLE ( 'NONE', #61305, 5.041900000000001825 ) ;
#19242 = CARTESIAN_POINT ( 'NONE',  ( 172.5664832912740110, -18.82844715994099971, 16.80862527591200006 ) ) ;
#19243 = ORIENTED_EDGE ( 'NONE', *, *, #63985, .T. ) ;
#19244 = VERTEX_POINT ( 'NONE', #6848 ) ;
#19245 = DIRECTION ( 'NONE',  ( 0.000000000000000000, 1.000000000000000000, 2.000000000000000155E-15 ) ) ;
#19246 = EDGE_CURVE ( 'NONE', #48350, #66137, #34549, .T. ) ;
#19247 = CARTESIAN_POINT ( 'NONE',  ( 104.5891003629744631, -45.44008686965874944, 66.79051506617194889 ) ) ;
#19248 = CARTESIAN_POINT ( 'NONE',  ( 98.51948014227190242, -30.72152729218522538, 205.8384824187679669 ) ) ;
#19249 = CARTESIAN_POINT ( 'NONE',  ( 108.3633857348901586, -47.68307073960303910, 162.6822919425769669 ) ) ;
#19251 = CARTESIAN_POINT ( 'NONE',  ( 105.8935855965125938, -47.12395608077676457, 278.4870538473395527 ) ) ;
#19250 = CARTESIAN_POINT ( 'NONE',  ( 115.3155962437203073, -42.52683630334157527, 23.33992995560114991 ) ) ;
#19252 = CARTESIAN_POINT ( 'NONE',  ( 140.0667039024470455, -118.2784471599408960, 51.21780685541800437 ) ) ;
#19253 = CARTESIAN_POINT ( 'NONE',  ( 194.0371591254575208, -24.89890238294407254, 180.4678068554150343 ) ) ;
#19254 = ORIENTED_EDGE ( 'NONE', *, *, #52021, .F. ) ;
#19256 = EDGE_CURVE ( 'NONE', #18423, #39686, #55421, .T. ) ;
#19255 = AXIS2_PLACEMENT_3D ( 'NONE', #13851, #6587, #70156 ) ;
#19257 = ORIENTED_EDGE ( 'NONE', *, *, #3317, .F. ) ;
#19258 = EDGE_CURVE ( 'NONE', #14322, #33917, #1343, .T. ) ;
#19259 = VECTOR ( 'NONE', #87848, 1000.000000000000114 ) ;
#19260 = DIRECTION ( 'NONE',  ( 0.000000000000000000, 0.000000000000000000, -1.000000000000000000 ) ) ;
#19261 = CARTESIAN_POINT ( 'NONE',  ( 101.3806489482690694, -45.56251468762313550, 222.1213395616249784 ) ) ;
#19262 = VERTEX_POINT ( 'NONE', #43591 ) ;
#19263 = CARTESIAN_POINT ( 'NONE',  ( 102.2371489609593880, -45.96874152625851906, 212.1927681330539599 ) ) ;
#19264 = DIRECTION ( 'NONE',  ( 0.000000000000000000, 0.000000000000000000, 1.000000000000000000 ) ) ;
#19265 = DIRECTION ( 'NONE',  ( 0.000000000000000000, 0.000000000000000000, 1.000000000000000000 ) ) ;
#19266 = CARTESIAN_POINT ( 'NONE',  ( 97.82515092478139707, -40.55017472135673984, 22.63844333753277738 ) ) ;
#19267 = LINE ( 'NONE', #6976, #35476 ) ;
#19269 = DIRECTION ( 'NONE',  ( 0.6893610196960192615, -0.7071067811865284769, -0.1574210421884302824 ) ) ;
#19268 = CARTESIAN_POINT ( 'NONE',  ( 101.9785357346435148, -30.23611602480990257, 277.6356252759111385 ) ) ;
#19270 = CARTESIAN_POINT ( 'NONE',  ( 129.9368274816652331, 82.54999999999999716, -12.69999999999864038 ) ) ;
#19271 = CARTESIAN_POINT ( 'NONE',  ( 33.91903122894598965, -35.91149509761181235, 237.4678068554150059 ) ) ;
#19272 = AXIS2_PLACEMENT_3D ( 'NONE', #56453, #21060, #48733 ) ;
#19273 = PLANE ( 'NONE',  #54233 ) ;
#19274 = LINE ( 'NONE', #18821, #778 ) ;
#19275 = CARTESIAN_POINT ( 'NONE',  ( 115.0821792353001740, -30.60892512433434831, 39.34390919315809043 ) ) ;
#19276 = FACE_OUTER_BOUND ( 'NONE', #65541, .T. ) ;
#19277 = ADVANCED_FACE ( 'NONE', ( #44931 ), #44485, .T. ) ;
#19279 = EDGE_LOOP ( 'NONE', ( #7297, #1817, #13644, #7665 ) ) ;
#19278 = CARTESIAN_POINT ( 'NONE',  ( 101.1531192966442347, -28.75920026314567934, 195.5838068554172082 ) ) ;
#19280 = CARTESIAN_POINT ( 'NONE',  ( 136.7765779009448579, -19.19711456031681251, 6.808568500764772935 ) ) ;
#19281 = CARTESIAN_POINT ( 'NONE',  ( 99.06899620534126427, -29.95238561887155981, 215.7670538473399517 ) ) ;
#19282 = CARTESIAN_POINT ( 'NONE',  ( 104.9628592394672069, -25.06714115267218546, 121.2184824187679766 ) ) ;
#19283 = CARTESIAN_POINT ( 'NONE',  ( 110.0014563237810137, -26.68062070874399438, 255.8499109901966051 ) ) ;
#19284 = DIRECTION ( 'NONE',  ( -1.000000000000000078E-15, -1.000000000000000083E-30, 1.000000000000000000 ) ) ;
#19285 = ADVANCED_FACE ( 'NONE', ( #64064, #15475 ), #43145, .F. ) ;
#19286 = DIRECTION ( 'NONE',  ( 0.7071067811865561215, -0.000000000000000000, -0.7071067811865389130 ) ) ;
#19288 = DIRECTION ( 'NONE',  ( 0.000000000000000000, 2.135044278125299371E-15, -1.000000000000000000 ) ) ;
#19287 = FACE_OUTER_BOUND ( 'NONE', #77885, .T. ) ;
#19289 = DIRECTION ( 'NONE',  ( 0.000000000000000000, 0.000000000000000000, 1.000000000000000000 ) ) ;
#19290 = DIRECTION ( 'NONE',  ( 1.000000000000000000, 0.000000000000000000, 0.000000000000000000 ) ) ;
#19291 = ORIENTED_EDGE ( 'NONE', *, *, #25713, .T. ) ;
#19292 = ORIENTED_EDGE ( 'NONE', *, *, #34732, .F. ) ;
#19293 = CARTESIAN_POINT ( 'NONE',  ( 100.0120368033278311, -41.59636475471172901, 126.2295626852199746 ) ) ;
#19295 = ORIENTED_EDGE ( 'NONE', *, *, #64704, .T. ) ;
#19294 = CARTESIAN_POINT ( 'NONE',  ( 30.00000000000001776, 172.0000000000000000, 114.8826257785461280 ) ) ;
#19296 = VECTOR ( 'NONE', #26553, 1000.000000000000000 ) ;
#19297 = CARTESIAN_POINT ( 'NONE',  ( -187.8075999999999794, 0.000000000000000000, 107.9500000000000028 ) ) ;
#19298 = CARTESIAN_POINT ( 'NONE',  ( 97.63679352021421209, -31.00714225716596673, 121.8803871806729546 ) ) ;
#19299 = FACE_OUTER_BOUND ( 'NONE', #56508, .T. ) ;
#19300 = DIRECTION ( 'NONE',  ( -0.000000000000000000, -0.000000000000000000, 1.000000000000000000 ) ) ;
#19301 = DIRECTION ( 'NONE',  ( 0.000000000000000000, 0.000000000000000000, -1.000000000000000000 ) ) ;
#19302 = CARTESIAN_POINT ( 'NONE',  ( 116.8171228663878907, -34.15291832029765828, 110.0314586092749778 ) ) ;
#19303 = CARTESIAN_POINT ( 'NONE',  ( 99.96923091713365750, -43.45941328387855407, 81.92991099019697288 ) ) ;
#19304 = VERTEX_POINT ( 'NONE', #71331 ) ;
#19305 = ORIENTED_EDGE ( 'NONE', *, *, #52274, .T. ) ;
#19306 = ORIENTED_EDGE ( 'NONE', *, *, #57290, .T. ) ;
#19307 = VECTOR ( 'NONE', #77398, 1000.000000000000000 ) ;
#19308 = ADVANCED_FACE ( 'NONE', ( #71771, #86289, #57222, #72660, #51291, #56777, #23199, #50866, #79038, #78604, #16803, #10427, #65394, #37247, #22283, #70886, #30433, #49958, #72217 ), #2733, .F. ) ;
#19309 = CARTESIAN_POINT ( 'NONE',  ( 177.8371591254544910, -47.82818131005477369, 193.9678068554150059 ) ) ;
#19311 = CARTESIAN_POINT ( 'NONE',  ( 97.81169789812091153, -40.51742632959496859, 107.6355761348045519 ) ) ;
#19310 = CARTESIAN_POINT ( 'NONE',  ( 116.4020974974655047, -33.81230083437814216, 170.0670538473389684 ) ) ;
#19312 = CARTESIAN_POINT ( 'NONE',  ( -27.27158787008326968, 127.0000000000000000, 80.02307622376218887 ) ) ;
#19313 = CARTESIAN_POINT ( 'NONE',  ( 11.39831192919941927, 76.93384533283848725, -130.0576265831481635 ) ) ;
#19314 = CARTESIAN_POINT ( 'NONE',  ( 31.89136050872298966, -31.76306994223740432, 237.4678068554150059 ) ) ;
#19315 = CARTESIAN_POINT ( 'NONE',  ( 116.1804594027163660, -40.96476762480074996, 3.024967495036159804 ) ) ;
#19316 = CARTESIAN_POINT ( 'NONE',  ( -103.1875000000000000, 117.4749999999999943, 7.937499999998919087 ) ) ;
#19317 = CARTESIAN_POINT ( 'NONE',  ( 117.0854383170106559, -39.53109055650223524, 98.60991099019594230 ) ) ;
#19318 = ORIENTED_EDGE ( 'NONE', *, *, #66289, .T. ) ;
#19319 = ORIENTED_EDGE ( 'NONE', *, *, #88046, .F. ) ;
#19320 = CARTESIAN_POINT ( 'NONE',  ( 19.56648329127400032, -18.82844715994099971, 342.9256252759119548 ) ) ;
#19321 = DIRECTION ( 'NONE',  ( 1.000000000000000000, 0.000000000000000000, 0.000000000000000000 ) ) ;
#19322 = DIRECTION ( 'NONE',  ( 0.000000000000000000, -0.000000000000000000, 1.000000000000000000 ) ) ;
#19323 = CARTESIAN_POINT ( 'NONE',  ( 106.0125404296577045, -27.51070622278902533, 157.9852332267339534 ) ) ;
#19324 = EDGE_CURVE ( 'NONE', #26264, #48691, #3176, .T. ) ;
#19325 = AXIS2_PLACEMENT_3D ( 'NONE', #18585, #60353, #53065 ) ;
#19326 = AXIS2_PLACEMENT_3D ( 'NONE', #48259, #54172, #33315 ) ;
#19327 = ADVANCED_FACE ( 'NONE', ( #8656, #36799 ), #84967, .F. ) ;
#19328 = EDGE_CURVE ( 'NONE', #36508, #24432, #64507, .T. ) ;
#19329 = VECTOR ( 'NONE', #24193, 1000.000000000000000 ) ;
#19330 = CARTESIAN_POINT ( 'NONE',  ( -29.99999999999996092, 172.0000000000000000, 183.8826257785461280 ) ) ;
#19331 = ORIENTED_EDGE ( 'NONE', *, *, #77723, .T. ) ;
#19332 = ORIENTED_EDGE ( 'NONE', *, *, #52908, .F. ) ;
#19333 = DIRECTION ( 'NONE',  ( 3.999999999999999995E-14, -1.000000000000000000, 4.100000000000000342E-29 ) ) ;
#19334 = ADVANCED_FACE ( 'NONE', ( #51739 ), #50411, .T. ) ;
#19335 = CARTESIAN_POINT ( 'NONE',  ( 136.6368519841215345, -19.70758306363340395, 2.855952960430312881 ) ) ;
#19336 = ORIENTED_EDGE ( 'NONE', *, *, #84686, .T. ) ;
#19337 = VERTEX_POINT ( 'NONE', #9102 ) ;
#19338 = CARTESIAN_POINT ( 'NONE',  ( 77.74802179993506002, -20.20859666167768154, 7.273989459507554933 ) ) ;
#19339 = CARTESIAN_POINT ( 'NONE',  ( 99.29109958770327182, -40.98052783126505005, 218.1558690201829620 ) ) ;
#19340 = ADVANCED_FACE ( 'NONE', ( #44036 ), #2287, .F. ) ;
#19341 = DIRECTION ( 'NONE',  ( -0.000000000000000000, -0.000000000000000000, -1.000000000000000000 ) ) ;
#19342 = CARTESIAN_POINT ( 'NONE',  ( -111.1819842745013460, 64.70253472953531571, 68.43619979767439077 ) ) ;
#19343 = ORIENTED_EDGE ( 'NONE', *, *, #83635, .T. ) ;
#19344 = EDGE_LOOP ( 'NONE', ( #57050, #83683, #27603, #62389 ) ) ;
#19345 = EDGE_CURVE ( 'NONE', #46288, #14095, #41897, .T. ) ;
#19346 = CYLINDRICAL_SURFACE ( 'NONE', #24601, 8.636000000000004562 ) ;
#19347 = TOROIDAL_SURFACE ( 'NONE', #12084, 11.75000000000000000, 2.125000000000000000 ) ;
#19348 = ORIENTED_EDGE ( 'NONE', *, *, #34238, .T. ) ;
#19349 = ORIENTED_EDGE ( 'NONE', *, *, #3163, .T. ) ;
#19350 = EDGE_CURVE ( 'NONE', #47179, #72757, #46254, .T. ) ;
#19351 = CARTESIAN_POINT ( 'NONE',  ( 116.2459175369934172, -38.08366948007849118, 221.5280903695909842 ) ) ;
#19353 = CARTESIAN_POINT ( 'NONE',  ( 96.06419827846988824, -38.01208726283962847, 86.43086337114897333 ) ) ;
#19352 = VECTOR ( 'NONE', #64554, 1000.000000000000000 ) ;
#19354 = CARTESIAN_POINT ( 'NONE',  ( 107.2318599658364207, -25.70055450771768690, 80.07657765686299456 ) ) ;
#19355 = CARTESIAN_POINT ( 'NONE',  ( 113.1205385969929438, -43.14583419566791633, 249.5838068554168672 ) ) ;
#19356 = DIRECTION ( 'NONE',  ( -0.000000000000000000, 1.000000000000000000, 0.000000000000000000 ) ) ;
#19357 = DIRECTION ( 'NONE',  ( 1.000000000000000000, 1.806816776397999960E-14, 8.991631831580328678E-43 ) ) ;
#19358 = CARTESIAN_POINT ( 'NONE',  ( 116.3773924821832111, -41.41873894932305689, 199.4556252759109611 ) ) ;
#19359 = CARTESIAN_POINT ( 'NONE',  ( 0.000000000000000000, 2.270000000000000462, 0.000000000000000000 ) ) ;
#19360 = ORIENTED_EDGE ( 'NONE', *, *, #41587, .T. ) ;
#19361 = CARTESIAN_POINT ( 'NONE',  ( 130.1663562161751884, 74.81660785136577374, -10.08264331121358381 ) ) ;
#19362 = EDGE_LOOP ( 'NONE', ( #20520, #73083, #15418, #44545 ) ) ;
#19363 = ORIENTED_EDGE ( 'NONE', *, *, #69578, .T. ) ;
#19364 = DIRECTION ( 'NONE',  ( 0.000000000000000000, 0.000000000000000000, -1.000000000000000000 ) ) ;
#19365 = VERTEX_POINT ( 'NONE', #39905 ) ;
#19366 = AXIS2_PLACEMENT_3D ( 'NONE', #12643, #67599, #80799 ) ;
#19367 = FACE_OUTER_BOUND ( 'NONE', #76430, .T. ) ;
#19368 = DIRECTION ( 'NONE',  ( -1.000000000000000000, 0.000000000000000000, 0.000000000000000000 ) ) ;
#19369 = CARTESIAN_POINT ( 'NONE',  ( 113.8565348333340665, -44.64034031543166492, 108.1413395616249744 ) ) ;
#19370 = CARTESIAN_POINT ( 'NONE',  ( 116.3186249068845939, -32.94868901192853627, 254.1356252759109395 ) ) ;
#19371 = DIRECTION ( 'NONE',  ( -0.7071067811865336949, -0.7071067811865614505, 0.000000000000000000 ) ) ;
#19372 = CARTESIAN_POINT ( 'NONE',  ( 123.4403675665762705, -98.97427844173840583, -10.56397404668093998 ) ) ;
#19375 = CARTESIAN_POINT ( 'NONE',  ( 97.11708974113240345, -41.49110554365059045, 212.6937205140059461 ) ) ;
#19374 = DIRECTION ( 'NONE',  ( 0.000000000000000000, 0.000000000000000000, -1.000000000000000000 ) ) ;
#19373 = CARTESIAN_POINT ( 'NONE',  ( 115.0372575035121940, -42.90846257061950553, 144.3022919421925678 ) ) ;
#19376 = DIRECTION ( 'NONE',  ( -0.7071067811855830110, -0.7071067811875120235, 0.000000000000000000 ) ) ;
#19377 = DIRECTION ( 'NONE',  ( 1.000000000000000000, 0.000000000000000000, 0.000000000000000000 ) ) ;
#19378 = VERTEX_POINT ( 'NONE', #73990 ) ;
#19379 = CARTESIAN_POINT ( 'NONE',  ( 106.5139905941028360, -24.40372801450956430, 320.5359728645732389 ) ) ;
#19380 = LINE ( 'NONE', #82078, #36960 ) ;
#19381 = DIRECTION ( 'NONE',  ( -4.237773401492740281E-14, 1.000000000000000000, 0.000000000000000000 ) ) ;
#19382 = CARTESIAN_POINT ( 'NONE',  ( 47.62500000000000000, 69.84999999999999432, 288.9250000000000114 ) ) ;
#19384 = EDGE_LOOP ( 'NONE', ( #34254, #11933 ) ) ;
#19383 = CARTESIAN_POINT ( 'NONE',  ( 110.8326918741827711, -26.28777313046090569, 249.7889586092445882 ) ) ;
#19385 = CARTESIAN_POINT ( 'NONE',  ( 107.0664832912748068, -36.72944715993923381, -5.074374724089029343 ) ) ;
#19386 = CARTESIAN_POINT ( 'NONE',  ( 118.3644662943939636, -33.07169432158188727, 280.0756252759109657 ) ) ;
#19387 = CARTESIAN_POINT ( 'NONE',  ( 117.2805452986850412, -39.02698501918706597, 144.6499109901969859 ) ) ;
#19388 = FACE_OUTER_BOUND ( 'NONE', #84022, .T. ) ;
#19389 = EDGE_CURVE ( 'NONE', #23550, #32370, #59892, .T. ) ;
#19390 = CARTESIAN_POINT ( 'NONE',  ( 71.24162159452610865, 0.6420441417434794573, 540.9756252759101471 ) ) ;
#19392 = LINE ( 'NONE', #54773, #15283 ) ;
#19391 = CARTESIAN_POINT ( 'NONE',  ( 51.06648329127400388, -8.350947159940998787, 330.8831252759119934 ) ) ;
#19393 = FACE_OUTER_BOUND ( 'NONE', #38199, .T. ) ;
#19394 = CARTESIAN_POINT ( 'NONE',  ( 80.06648329127399677, -8.729447159940999512, 296.1531252759119752 ) ) ;
#19395 = ORIENTED_EDGE ( 'NONE', *, *, #53557, .F. ) ;
#19396 = AXIS2_PLACEMENT_3D ( 'NONE', #4413, #32100, #27089 ) ;
#19397 = ORIENTED_EDGE ( 'NONE', *, *, #58122, .F. ) ;
#19398 = ORIENTED_EDGE ( 'NONE', *, *, #89619, .T. ) ;
#19399 = ORIENTED_EDGE ( 'NONE', *, *, #54686, .T. ) ;
#19400 = DIRECTION ( 'NONE',  ( 0.000000000000000000, 0.000000000000000000, -1.000000000000000000 ) ) ;
#19401 = CARTESIAN_POINT ( 'NONE',  ( 117.3629797429380659, -38.21633193987522503, 24.71276813305395237 ) ) ;
#19402 = CARTESIAN_POINT ( 'NONE',  ( 77.31648329127399677, -18.72944715994106346, -5.074374724089059541 ) ) ;
#19403 = CARTESIAN_POINT ( 'NONE',  ( 117.0707351141037833, -37.57509454027182016, 118.7609861400189715 ) ) ;
#19405 = CARTESIAN_POINT ( 'NONE',  ( 107.0664832912739399, -36.72944715994095333, 315.6356252759111953 ) ) ;
#19404 = CARTESIAN_POINT ( 'NONE',  ( -487.2989999999999782, 85.41360802895360393, 11.11250000000036131 ) ) ;
#19406 = CARTESIAN_POINT ( 'NONE',  ( 98.63267121701338169, -35.20533560836722131, 240.6067055423629597 ) ) ;
#19407 = ORIENTED_EDGE ( 'NONE', *, *, #922, .T. ) ;
#19408 = VERTEX_POINT ( 'NONE', #59450 ) ;
#19409 = ORIENTED_EDGE ( 'NONE', *, *, #21492, .F. ) ;
#19410 = EDGE_CURVE ( 'NONE', #83042, #71543, #88531, .T. ) ;
#19411 = CIRCLE ( 'NONE', #70177, 13.44999999999999396 ) ;
#19412 = CARTESIAN_POINT ( 'NONE',  ( 51.06648329127400388, -8.350947159940998787, 333.4006252759120343 ) ) ;
#19413 = VECTOR ( 'NONE', #42069, 1000.000000000000114 ) ;
#19414 = CARTESIAN_POINT ( 'NONE',  ( 116.9901879630660630, -35.35324060233794796, 183.9360659761157990 ) ) ;
#19415 = CARTESIAN_POINT ( 'NONE',  ( 29.56670390244797630, -67.87844715994100397, 20.91780685541479912 ) ) ;
#19416 = DIRECTION ( 'NONE',  ( 3.999999999999999995E-14, -1.000000000000000000, 4.100000000000000342E-29 ) ) ;
#19417 = CARTESIAN_POINT ( 'NONE',  ( 115.9456366428866119, -37.20155953748186306, 15.21586902018295895 ) ) ;
#19418 = CARTESIAN_POINT ( 'NONE',  ( 118.4860461769942361, 94.58006533271583294, -4.091503224719446941 ) ) ;
#19419 = CARTESIAN_POINT ( 'NONE',  ( 107.0664832912739399, -36.72944715994095333, 315.6356252759111953 ) ) ;
#19420 = CARTESIAN_POINT ( 'NONE',  ( 104.7413500955949672, -27.22895272701804359, 285.2670538473402075 ) ) ;
#19421 = DIRECTION ( 'NONE',  ( -1.000000000000000078E-15, 1.000000000000000083E-30, 1.000000000000000000 ) ) ;
#19422 = ORIENTED_EDGE ( 'NONE', *, *, #51301, .T. ) ;
#19423 = DIRECTION ( 'NONE',  ( -1.000000000000000000, -4.299999999999999979E-14, -1.000000000000000078E-15 ) ) ;
#19424 = CYLINDRICAL_SURFACE ( 'NONE', #1762, 0.5000000000000104361 ) ;
#19425 = CARTESIAN_POINT ( 'NONE',  ( 100.8503319422675020, -42.75110701849109063, 39.76904275054393878 ) ) ;
#19426 = CARTESIAN_POINT ( 'NONE',  ( 105.8259002483207922, -25.33766151058717142, 321.6188579224977389 ) ) ;
#19427 = DIRECTION ( 'NONE',  ( 0.000000000000000000, -1.000000000000000000, 0.000000000000000000 ) ) ;
#19428 = ADVANCED_FACE ( 'NONE', ( #87183 ), #80825, .T. ) ;
#19429 = CARTESIAN_POINT ( 'NONE',  ( 129.8079539024480482, -42.97311385574000298, 207.5838068554170377 ) ) ;
#19430 = VERTEX_POINT ( 'NONE', #17690 ) ;
#19431 = CARTESIAN_POINT ( 'NONE',  ( 78.22143491581488206, -34.68812225914982861, 7.662832107313313657 ) ) ;
#19432 = EDGE_CURVE ( 'NONE', #78028, #17169, #3608, .T. ) ;
#19433 = ORIENTED_EDGE ( 'NONE', *, *, #60736, .F. ) ;
#19434 = CARTESIAN_POINT ( 'NONE',  ( 113.3148160382734773, -28.33991531616941728, 104.5670538473399347 ) ) ;
#19435 = ORIENTED_EDGE ( 'NONE', *, *, #15262, .F. ) ;
#19436 = EDGE_CURVE ( 'NONE', #31238, #52939, #79683, .T. ) ;
#19437 = CARTESIAN_POINT ( 'NONE',  ( 102.2116477823090293, -29.08462914334738869, 64.93718173283896533 ) ) ;
#19438 = CARTESIAN_POINT ( 'NONE',  ( 98.22417599084440099, -41.40637017319168933, 87.71314181957467326 ) ) ;
#19439 = CARTESIAN_POINT ( 'NONE',  ( 113.5614835896806625, -43.51851901557028413, 109.6034880678019618 ) ) ;
#19440 = EDGE_CURVE ( 'NONE', #23818, #24431, #67621, .T. ) ;
#19441 = DIRECTION ( 'NONE',  ( 0.000000000000000000, 0.000000000000000000, -1.000000000000000000 ) ) ;
#19442 = DIRECTION ( 'NONE',  ( 0.000000000000000000, 0.000000000000000000, -1.000000000000000000 ) ) ;
#19443 = CARTESIAN_POINT ( 'NONE',  ( 115.0392540076567656, -43.53489519176116573, 59.26419670448196086 ) ) ;
#19444 = DIRECTION ( 'NONE',  ( -4.440892098500319985E-16, -3.100000000000000044E-14, -1.000000000000000000 ) ) ;
#19445 = AXIS2_PLACEMENT_3D ( 'NONE', #10553, #18260, #52740 ) ;
#19446 = CARTESIAN_POINT ( 'NONE',  ( 116.7950397785617156, -39.38813467484644093, 258.6147150626158577 ) ) ;
#19447 = ORIENTED_EDGE ( 'NONE', *, *, #11573, .F. ) ;
#19448 = CARTESIAN_POINT ( 'NONE',  ( 77.67297288198761862, -20.08739819368273061, 2.653088468860025362 ) ) ;
#19449 = SHAPE_REPRESENTATION ( 'Pneumatic Toggle Clamp Unit', ( #50656 ), #23133 ) ;
#19450 = VECTOR ( 'NONE', #16024, 1000.000000000000000 ) ;
#19451 = ORIENTED_EDGE ( 'NONE', *, *, #45869, .T. ) ;
#19452 = ORIENTED_EDGE ( 'NONE', *, *, #48032, .T. ) ;
#19453 = EDGE_CURVE ( 'NONE', #34012, #42178, #70990, .T. ) ;
#19454 = DIRECTION ( 'NONE',  ( -3.360405532702990443E-14, 1.000000000000000000, 0.000000000000000000 ) ) ;
#19455 = ORIENTED_EDGE ( 'NONE', *, *, #81503, .T. ) ;
#19456 = CARTESIAN_POINT ( 'NONE',  ( 107.9555263298577330, -25.64695713395843413, 265.0127681330543510 ) ) ;
#19457 = CARTESIAN_POINT ( 'NONE',  ( 102.9047493514100893, -27.10917607469848178, 151.4013395616249511 ) ) ;
#19458 = CYLINDRICAL_SURFACE ( 'NONE', #39401, 9.999999999999998224 ) ;
#19459 = CARTESIAN_POINT ( 'NONE',  ( 0.000000000000000000, 20.32000000000000028, 0.000000000000000000 ) ) ;
#19460 = CARTESIAN_POINT ( 'NONE',  ( 117.4474071775726287, -37.68804338056689573, 74.75276813305397638 ) ) ;
#19461 = DIRECTION ( 'NONE',  ( -0.000000000000000000, -0.000000000000000000, -1.000000000000000000 ) ) ;
#19462 = ORIENTED_EDGE ( 'NONE', *, *, #57492, .F. ) ;
#19463 = CARTESIAN_POINT ( 'NONE',  ( -148.0533267522759786, 0.000000000000000000, -160.2664750769289697 ) ) ;
#19464 = CARTESIAN_POINT ( 'NONE',  ( 116.8169405894235808, -34.15221262904118049, 160.0313671257249837 ) ) ;
#19465 = ORIENTED_EDGE ( 'NONE', *, *, #28710, .F. ) ;
#19466 = AXIS2_PLACEMENT_3D ( 'NONE', #13303, #61877, #48238 ) ;
#19467 = FACE_OUTER_BOUND ( 'NONE', #34851, .T. ) ;
#19468 = VECTOR ( 'NONE', #12471, 1000.000000000000000 ) ;
#19469 = AXIS2_PLACEMENT_3D ( 'NONE', #59265, #10671, #44290 ) ;
#19470 = DIRECTION ( 'NONE',  ( 0.000000000000000000, -1.000000000000000000, 0.000000000000000000 ) ) ;
#19471 = CARTESIAN_POINT ( 'NONE',  ( 118.0799254396265923, -36.12288750354066735, 273.8822919425776945 ) ) ;
#19472 = DIRECTION ( 'NONE',  ( 0.000000000000000000, 0.000000000000000000, -1.000000000000000000 ) ) ;
#19473 = AXIS2_PLACEMENT_3D ( 'NONE', #23085, #43479, #71224 ) ;
#19474 = LINE ( 'NONE', #47157, #69484 ) ;
#19475 = CARTESIAN_POINT ( 'NONE',  ( 116.8158949166094658, -34.14816870754088285, 94.03160469597915494 ) ) ;
#19476 = CARTESIAN_POINT ( 'NONE',  ( 98.74870792914448714, -34.66384430100242753, 275.5552769709340737 ) ) ;
#19478 = CARTESIAN_POINT ( 'NONE',  ( 113.0643619202157453, -28.22920495858477352, 125.5870538473399591 ) ) ;
#19477 = CARTESIAN_POINT ( 'NONE',  ( 116.3247715116346939, -32.94624160847306626, 99.13562527591096796 ) ) ;
#19479 = DIRECTION ( 'NONE',  ( 1.000000000000000000, 2.775557561562888827E-14, 0.000000000000000000 ) ) ;
#19480 = CARTESIAN_POINT ( 'NONE',  ( 103.0327258024342427, -26.38818591439425632, 170.3603871806729444 ) ) ;
#19481 = ORIENTED_EDGE ( 'NONE', *, *, #78573, .F. ) ;
#19482 = CARTESIAN_POINT ( 'NONE',  ( 70.98999999999998067, 52.73749999999999716, -44.45000000000002416 ) ) ;
#19483 = VERTEX_POINT ( 'NONE', #4951 ) ;
#19484 = PLANE ( 'NONE',  #78805 ) ;
#19485 = DIRECTION ( 'NONE',  ( 1.000000000000000000, 0.000000000000000000, 0.000000000000000000 ) ) ;
#19486 = CARTESIAN_POINT ( 'NONE',  ( 107.0664832912750057, -36.72944715993903486, 9.125625275910969947 ) ) ;
#19487 = ORIENTED_EDGE ( 'NONE', *, *, #4153, .T. ) ;
#19488 = CARTESIAN_POINT ( 'NONE',  ( 141.0664832912740110, -46.72944715994102438, 14.82207188531771358 ) ) ;
#19490 = ORIENTED_EDGE ( 'NONE', *, *, #7117, .T. ) ;
#19489 = CARTESIAN_POINT ( 'NONE',  ( 116.9458863120112539, -40.19413502446316500, 133.5584824187679658 ) ) ;
#19491 = FACE_OUTER_BOUND ( 'NONE', #29064, .T. ) ;
#19492 = CARTESIAN_POINT ( 'NONE',  ( -130.5247076678899134, 94.92443974548204721, 2.887521757540267409 ) ) ;
#19493 = EDGE_CURVE ( 'NONE', #25402, #61470, #37595, .T. ) ;
#19494 = CARTESIAN_POINT ( 'NONE',  ( 100.8874678769283264, -44.70022136931469703, 118.0522919418250893 ) ) ;
#19495 = PLANE ( 'NONE',  #14782 ) ;
#19496 = VERTEX_POINT ( 'NONE', #53510 ) ;
#19497 = CARTESIAN_POINT ( 'NONE',  ( -107.0569861830068845, 79.12155284006277611, -201.8896130469582317 ) ) ;
#19498 = EDGE_CURVE ( 'NONE', #31238, #25043, #88081, .T. ) ;
#19499 = CARTESIAN_POINT ( 'NONE',  ( 183.5150000000000148, 37.33800000000000097, 32.46912895322940074 ) ) ;
#19500 = ORIENTED_EDGE ( 'NONE', *, *, #80467, .T. ) ;
#19501 = ORIENTED_EDGE ( 'NONE', *, *, #20765, .T. ) ;
#19502 = CARTESIAN_POINT ( 'NONE',  ( 1.451892259197136103E-14, 61.59999999999999432, -118.5560000000000116 ) ) ;
#19503 = CARTESIAN_POINT ( 'NONE',  ( 96.94152442043744600, 93.33921197991993779, -87.44900557253130557 ) ) ;
#19504 = CARTESIAN_POINT ( 'NONE',  ( 101.9936208461673459, -45.44607148442891287, 157.1564586006232389 ) ) ;
#19505 = CYLINDRICAL_SURFACE ( 'NONE', #71962, 9.999999999999998224 ) ;
#19506 = AXIS2_PLACEMENT_3D ( 'NONE', #66481, #60556, #32399 ) ;
#19508 = CARTESIAN_POINT ( 'NONE',  ( -6.360060842339565923, 71.54945291875249325, -118.3858484385471286 ) ) ;
#19507 = CARTESIAN_POINT ( 'NONE',  ( -186.2398777604655038, 101.5999999999999943, -6.349999999999999645 ) ) ;
#19509 = CARTESIAN_POINT ( 'NONE',  ( 172.5667039024480118, -36.32844715993499563, 180.4678068554150059 ) ) ;
#19510 = ORIENTED_EDGE ( 'NONE', *, *, #62831, .T. ) ;
#19511 = EDGE_CURVE ( 'NONE', #23819, #29231, #52172, .T. ) ;
#19512 = CARTESIAN_POINT ( 'NONE',  ( 188.5667039024479834, -62.87844715994099687, 137.2178068554150059 ) ) ;
#19513 = AXIS2_PLACEMENT_3D ( 'NONE', #66738, #87197, #18137 ) ;
#19514 = CARTESIAN_POINT ( 'NONE',  ( 193.5667039024485803, -48.82844715993409324, 180.4678068554150343 ) ) ;
#19515 = CARTESIAN_POINT ( 'NONE',  ( 114.4888877093245583, -29.48743791597858177, 190.4537205140059655 ) ) ;
#19517 = ORIENTED_EDGE ( 'NONE', *, *, #28654, .F. ) ;
#19516 = DIRECTION ( 'NONE',  ( 0.000000000000000000, 0.000000000000000000, 1.000000000000000000 ) ) ;
#19518 = CARTESIAN_POINT ( 'NONE',  ( 109.4837483930865289, -46.20680252518636166, 43.77562527591094721 ) ) ;
#19519 = CARTESIAN_POINT ( 'NONE',  ( -27.27158787008326968, 184.0000000000000000, 0.000000000000000000 ) ) ;
#19520 = CARTESIAN_POINT ( 'NONE',  ( 98.60478223830740774, 120.6499999999999915, 3.859079674607175002E-13 ) ) ;
#19521 = DIRECTION ( 'NONE',  ( 0.000000000000000000, 1.000000000000000000, 0.000000000000000000 ) ) ;
#19522 = EDGE_LOOP ( 'NONE', ( #69663, #26815 ) ) ;
#19523 = CARTESIAN_POINT ( 'NONE',  ( 110.0667047667142953, -67.87844715994094713, 93.21780685541800437 ) ) ;
#19524 = VERTEX_POINT ( 'NONE', #53055 ) ;
#19525 = VERTEX_POINT ( 'NONE', #45809 ) ;
#19526 = CARTESIAN_POINT ( 'NONE',  ( 99.39098736499681763, -43.25305561222647555, 223.3187261630399689 ) ) ;
#19527 = VECTOR ( 'NONE', #11399, 1000.000000000000000 ) ;
#19528 = CARTESIAN_POINT ( 'NONE',  ( 31.75000000000000000, 66.67499999999999716, 292.1000000000000227 ) ) ;
#19529 = CARTESIAN_POINT ( 'NONE',  ( -7.940696711283829426E-13, 127.0000000000000000, 107.7702177616926065 ) ) ;
#19530 = CONICAL_SURFACE ( 'NONE', #64482, 16.25000000000000000, 0.5235987755982992597 ) ;
#19531 = PLANE ( 'NONE',  #75184 ) ;
#19532 = CYLINDRICAL_SURFACE ( 'NONE', #21230, 9.999999999999998224 ) ;
#19533 = AXIS2_PLACEMENT_3D ( 'NONE', #9328, #18814, #27410 ) ;
#19534 = ORIENTED_EDGE ( 'NONE', *, *, #71378, .F. ) ;
#19535 = CARTESIAN_POINT ( 'NONE',  ( 226.4410000000000025, 65.43750000000000000, -2.032000000000000028 ) ) ;
#19536 = CIRCLE ( 'NONE', #41307, 2.117000000000000881 ) ;
#19537 = DIRECTION ( 'NONE',  ( -0.000000000000000000, 1.000000000000000000, -0.000000000000000000 ) ) ;
#19538 = ORIENTED_EDGE ( 'NONE', *, *, #18937, .T. ) ;
#19539 = CARTESIAN_POINT ( 'NONE',  ( 116.7701435943788653, -31.43623786049258584, 24.21181575210196257 ) ) ;
#19540 = EDGE_LOOP ( 'NONE', ( #74056, #14055, #89349, #13941 ) ) ;
#19541 = EDGE_CURVE ( 'NONE', #59761, #13459, #19474, .T. ) ;
#19542 = CARTESIAN_POINT ( 'NONE',  ( 110.6228153916969603, -44.07670705792993715, 245.7538046553059701 ) ) ;
#19543 =( NAMED_UNIT ( * ) SI_UNIT ( $, .STERADIAN. ) SOLID_ANGLE_UNIT ( ) );
#19544 = CARTESIAN_POINT ( 'NONE',  ( 96.03815445040686427, -38.18343476501375022, 151.4299109901969871 ) ) ;
#19545 = CARTESIAN_POINT ( 'NONE',  ( 23.04053976455417185, 77.79540997170535377, 303.2111662390294669 ) ) ;
#19546 = LINE ( 'NONE', #80905, #60653 ) ;
#19547 = CYLINDRICAL_SURFACE ( 'NONE', #5668, 9.425000000000000711 ) ;
#19548 = CARTESIAN_POINT ( 'NONE',  ( 7.069959413120197489, 71.99984796920048780, 130.3644307161663107 ) ) ;
#19549 = CARTESIAN_POINT ( 'NONE',  ( 116.9665165100108908, -41.74809644303882550, 244.4651490854349731 ) ) ;
#19550 = DIRECTION ( 'NONE',  ( 1.000000000000000000, 0.000000000000000000, 0.000000000000000000 ) ) ;
#19551 = VERTEX_POINT ( 'NONE', #73090 ) ;
#19552 = CARTESIAN_POINT ( 'NONE',  ( 117.6393638915270827, -42.19070237429166070, 89.44705384733997278 ) ) ;
#19553 = CARTESIAN_POINT ( 'NONE',  ( 172.5664832912740110, -32.07844715994070839, 74.17562527591199739 ) ) ;
#19554 = EDGE_LOOP ( 'NONE', ( #49125, #22023, #6702, #17230 ) ) ;
#19555 = VECTOR ( 'NONE', #77927, 999.9999999999998863 ) ;
#19556 = ORIENTED_EDGE ( 'NONE', *, *, #81004, .F. ) ;
#19557 = VERTEX_POINT ( 'NONE', #38130 ) ;
#19558 = EDGE_CURVE ( 'NONE', #57167, #31769, #30335, .T. ) ;
#19559 = CARTESIAN_POINT ( 'NONE',  ( 115.0871287824145242, -30.61533435493911526, 159.3439420475139059 ) ) ;
#19561 = EDGE_CURVE ( 'NONE', #17346, #84744, #81118, .T. ) ;
#19560 = CARTESIAN_POINT ( 'NONE',  ( 163.0664832912739826, -18.82844715994099971, 330.8831252759119934 ) ) ;
#19562 = DIRECTION ( 'NONE',  ( 0.000000000000000000, 1.000000000000000000, 0.000000000000000000 ) ) ;
#19563 = LINE ( 'NONE', #40893, #76571 ) ;
#19564 = CARTESIAN_POINT ( 'NONE',  ( 98.87701435734486211, -36.85308710711977653, 134.1566617981629577 ) ) ;
#19565 = CARTESIAN_POINT ( 'NONE',  ( 111.8740745592753427, -46.04428811464656945, 268.9556252759110180 ) ) ;
#19566 = CARTESIAN_POINT ( 'NONE',  ( -487.2989999999999782, 6.038608028953049711, 90.48749999999999716 ) ) ;
#19567 = VERTEX_POINT ( 'NONE', #73538 ) ;
#19568 = CARTESIAN_POINT ( 'NONE',  ( 130.1658227983197662, 90.29814575435203494, 10.09656535537147803 ) ) ;
#19569 = FACE_OUTER_BOUND ( 'NONE', #5390, .T. ) ;
#19570 = ORIENTED_EDGE ( 'NONE', *, *, #29193, .F. ) ;
#19571 = VERTEX_POINT ( 'NONE', #11312 ) ;
#19572 = MECHANICAL_DESIGN_GEOMETRIC_PRESENTATION_REPRESENTATION (  '', ( #25336 ), #29699 ) ;
#19573 = CARTESIAN_POINT ( 'NONE',  ( 20.03715912545645850, -24.95799193693202156, 129.9678068554150627 ) ) ;
#19574 = EDGE_LOOP ( 'NONE', ( #24145, #63521, #45305 ) ) ;
#19575 = ORIENTED_EDGE ( 'NONE', *, *, #81409, .T. ) ;
#19576 = CARTESIAN_POINT ( 'NONE',  ( 136.8164832912740110, -36.72944715994100306, 3.101481641215515950 ) ) ;
#19577 = AXIS2_PLACEMENT_3D ( 'NONE', #36143, #15710, #22980 ) ;
#19578 = CARTESIAN_POINT ( 'NONE',  ( -11.41387019979801387, 76.91918732108555901, -130.0565070412864372 ) ) ;
#19579 = LINE ( 'NONE', #80146, #49565 ) ;
#19580 = DIRECTION ( 'NONE',  ( 0.000000000000000000, -1.000000000000000000, 0.000000000000000000 ) ) ;
#19581 = CARTESIAN_POINT ( 'NONE',  ( 108.1312808730283166, -45.72271566404705112, 162.1048007804579640 ) ) ;
#19582 = CARTESIAN_POINT ( 'NONE',  ( 112.7657546104280044, -27.20415503536211688, 54.65943479971996055 ) ) ;
#19583 = LINE ( 'NONE', #81831, #33527 ) ;
#19584 = VERTEX_POINT ( 'NONE', #39013 ) ;
#19585 = CARTESIAN_POINT ( 'NONE',  ( -91.81719692706842295, 78.06989712577870932, -75.00102098090771108 ) ) ;
#19586 = EDGE_LOOP ( 'NONE', ( #1771, #13482, #72548, #28674 ) ) ;
#19587 = CARTESIAN_POINT ( 'NONE',  ( 97.06110197060442601, -37.99657418256868624, 262.4273502539846845 ) ) ;
#19588 = ORIENTED_EDGE ( 'NONE', *, *, #88140, .F. ) ;
#19589 = B_SPLINE_CURVE_WITH_KNOTS ( 'NONE', 3,
 ( #86582, #52891, #3457, #9833, #3898, #17538, #37539, #59738, #58410, #65238, #3012, #72932, #31595, #10704, #67016, #24353, #46101, #73832, #80220, #17966, #45215, #38411, #59297, #30714, #45650 ),
 .UNSPECIFIED., .F., .F.,
 ( 4, 2, 2, 1, 2, 2, 2, 2, 2, 2, 2, 2, 4 ),
 ( 0.03972946622853323895, 0.04221318292723492960, 0.04345504127658578186, 0.04469689962593662719, 0.04593875797528747251, 0.04718061632463831784, 0.04966433302334004318, 0.05090619137269088851, 0.05214804972204173383, 0.05463176642074343836, 0.05587362477009429063, 0.05711548311944514289, 0.05959919981814688211 ),
 .UNSPECIFIED. ) ;
#19590 = DIRECTION ( 'NONE',  ( -0.2884130866282236250, -0.7071067811865507924, 0.6456143519637524975 ) ) ;
#19591 = CARTESIAN_POINT ( 'NONE',  ( -12.19523605228628682, 79.27667993837064842, 117.9272132121709689 ) ) ;
#19592 = CARTESIAN_POINT ( 'NONE',  ( 110.9148046014321523, -45.95934737500046907, 132.8908183948595934 ) ) ;
#19594 = AXIS2_PLACEMENT_3D ( 'NONE', #53221, #19632, #87783 ) ;
#19593 = LINE ( 'NONE', #33676, #232 ) ;
#19595 = VERTEX_POINT ( 'NONE', #66723 ) ;
#19596 = CARTESIAN_POINT ( 'NONE',  ( 100.0239399080498544, -28.99471651683304785, 285.6641967044823787 ) ) ;
#19597 = AXIS2_PLACEMENT_3D ( 'NONE', #6773, #41722, #63531 ) ;
#19598 = CARTESIAN_POINT ( 'NONE',  ( 116.7853252867327996, -32.83880582269000570, 50.12991099019698282 ) ) ;
#19599 = VECTOR ( 'NONE', #16632, 999.9999999999998863 ) ;
#19600 = VECTOR ( 'NONE', #21015, 1000.000000000000000 ) ;
#19603 = EDGE_CURVE ( 'NONE', #57294, #87995, #4507, .T. ) ;
#19602 = CARTESIAN_POINT ( 'NONE',  ( 107.0667039024470313, -104.2784471599420755, -19.78219314458201694 ) ) ;
#19601 = DIRECTION ( 'NONE',  ( 0.000000000000000000, -1.000000000000000000, 0.000000000000000000 ) ) ;
#19604 = CARTESIAN_POINT ( 'NONE',  ( 98.34986356287390663, -31.65657669940653207, 146.9069401482558419 ) ) ;
#19605 = CARTESIAN_POINT ( 'NONE',  ( 49.16670390244701139, -26.71338133339240528, -5.074374724088000832 ) ) ;
#19606 = VECTOR ( 'NONE', #80294, 1000.000000000000000 ) ;
#19607 = CARTESIAN_POINT ( 'NONE',  ( 0.000000000000000000, 215.0000000000000000, 154.6557476874258441 ) ) ;
#19608 = DIRECTION ( 'NONE',  ( 0.9068632946707805287, -0.4214249218767880389, 9.068632946707802473E-16 ) ) ;
#19609 = DIRECTION ( 'NONE',  ( -1.000000000000000000, -4.299999999999999979E-14, -1.000000000000000078E-15 ) ) ;
#19610 = VERTEX_POINT ( 'NONE', #89878 ) ;
#19611 = CARTESIAN_POINT ( 'NONE',  ( 100.9151287000745896, -46.91716693487881429, 52.14419670448194921 ) ) ;
#19612 = CARTESIAN_POINT ( 'NONE',  ( 109.7757303681923418, -47.46933477669593771, 88.78514908543493789 ) ) ;
#19614 = CARTESIAN_POINT ( 'NONE',  ( 34.96670390244699433, -26.71338133339301635, -5.074374724088000832 ) ) ;
#19613 = CARTESIAN_POINT ( 'NONE',  ( -451.6120000000000232, 53.97500000000000142, -3.174999999999999822 ) ) ;
#19615 = DIRECTION ( 'NONE',  ( 0.000000000000000000, 6.920681583949466031E-15, -1.000000000000000000 ) ) ;
#19616 = AXIS2_PLACEMENT_3D ( 'NONE', #64214, #22887, #30133 ) ;
#19617 = EDGE_CURVE ( 'NONE', #46374, #47812, #54989, .T. ) ;
#19618 = CIRCLE ( 'NONE', #82022, 3.000000864267354572 ) ;
#19619 = CARTESIAN_POINT ( 'NONE',  ( -487.2989999999999782, 93.66249999999999432, 15.87500000000039968 ) ) ;
#19620 = ORIENTED_EDGE ( 'NONE', *, *, #24666, .F. ) ;
#19621 = CARTESIAN_POINT ( 'NONE',  ( 115.9482186066388749, -32.63332544795709111, 100.1699109901959588 ) ) ;
#19623 = ORIENTED_EDGE ( 'NONE', *, *, #58031, .F. ) ;
#19622 = CARTESIAN_POINT ( 'NONE',  ( 10.54391646024738627, 89.62925550596948199, 130.1295316605823871 ) ) ;
#19624 = CARTESIAN_POINT ( 'NONE',  ( 98.91597900623165174, -29.29754952351882480, 226.7261014663869503 ) ) ;
#19625 = CARTESIAN_POINT ( 'NONE',  ( 98.37992361594359636, -41.69440232629470700, 252.7399961474531835 ) ) ;
#19626 = CARTESIAN_POINT ( 'NONE',  ( 116.9903668002740602, -35.35439823643719137, 148.9359728826448759 ) ) ;
#19627 = CARTESIAN_POINT ( 'NONE',  ( -186.2398777604655038, 0.000000000000000000, 114.2999999999999972 ) ) ;
#19628 = CARTESIAN_POINT ( 'NONE',  ( 100.9546728272766956, -28.70702571534067005, 81.59395860767402553 ) ) ;
#19629 = EDGE_CURVE ( 'NONE', #43244, #79697, #68525, .T. ) ;
#19630 = EDGE_CURVE ( 'NONE', #70136, #39283, #53493, .T. ) ;
#19631 = CYLINDRICAL_SURFACE ( 'NONE', #17244, 9.999999999999998224 ) ;
#19632 = DIRECTION ( 'NONE',  ( -0.000000000000000000, 1.000000000000000000, -0.000000000000000000 ) ) ;
#19633 = CARTESIAN_POINT ( 'NONE',  ( 108.2029444874846007, -47.03713394308636708, 157.6518157521019532 ) ) ;
#19634 = ORIENTED_EDGE ( 'NONE', *, *, #72155, .T. ) ;
#19635 = ORIENTED_EDGE ( 'NONE', *, *, #37807, .T. ) ;
#19636 = AXIS2_PLACEMENT_3D ( 'NONE', #79593, #76559, #14793 ) ;
#19637 = CARTESIAN_POINT ( 'NONE',  ( 99.14414808984345484, -41.78050036225572228, 138.1977737820869834 ) ) ;
#19638 = CARTESIAN_POINT ( 'NONE',  ( 177.1649999999999920, 25.81350000000000477, -58.73749999999999716 ) ) ;
#19640 = CARTESIAN_POINT ( 'NONE',  ( 180.1667039024474377, -26.71338133338667831, 237.4678068554150059 ) ) ;
#19639 = CARTESIAN_POINT ( 'NONE',  ( 96.93540839703301515, -34.51582869190843894, 252.1432443235293590 ) ) ;
#19641 = AXIS2_PLACEMENT_3D ( 'NONE', #11343, #39040, #64814 ) ;
#19642 = PLANE ( 'NONE',  #15959 ) ;
#19643 = EDGE_CURVE ( 'NONE', #1830, #17950, #68801, .T. ) ;
#19644 = DIRECTION ( 'NONE',  ( 0.000000000000000000, 0.000000000000000000, -1.000000000000000000 ) ) ;
#19645 = DIRECTION ( 'NONE',  ( -0.000000000000000000, -1.000000000000000000, -0.000000000000000000 ) ) ;
#19646 = DIRECTION ( 'NONE',  ( 0.000000000000000000, 0.000000000000000000, 1.000000000000000000 ) ) ;
#19647 = DIRECTION ( 'NONE',  ( 1.000000000000000000, 4.163336342344333240E-14, 0.000000000000000000 ) ) ;
#19648 = CARTESIAN_POINT ( 'NONE',  ( 109.6005296801413351, -26.60309369064632534, 199.8813395616249977 ) ) ;
#19649 = LINE ( 'NONE', #69149, #83762 ) ;
#19650 = ORIENTED_EDGE ( 'NONE', *, *, #70518, .T. ) ;
#19652 = ORIENTED_EDGE ( 'NONE', *, *, #63569, .F. ) ;
#19651 = EDGE_CURVE ( 'NONE', #79764, #36007, #25120, .T. ) ;
#19653 = CARTESIAN_POINT ( 'NONE',  ( -98.06260288352387988, 72.98383416765814502, -86.19129576945131532 ) ) ;
#19654 = CARTESIAN_POINT ( 'NONE',  ( 107.0667039024470313, -104.2784471599421323, -21.78219314458201694 ) ) ;
#19655 = FACE_BOUND ( 'NONE', #78267, .T. ) ;
#19656 = DIRECTION ( 'NONE',  ( 0.000000000000000000, 0.000000000000000000, 1.000000000000000000 ) ) ;
#19658 = CARTESIAN_POINT ( 'NONE',  ( 143.0664832912740110, -18.82844715994099971, 93.42562527591199739 ) ) ;
#19657 = AXIS2_PLACEMENT_3D ( 'NONE', #62650, #13608, #425 ) ;
#19659 = EDGE_LOOP ( 'NONE', ( #47366, #44146, #56014, #57976, #87404 ) ) ;
#19660 = AXIS2_PLACEMENT_3D ( 'NONE', #45518, #10577, #3769 ) ;
#19661 = CARTESIAN_POINT ( 'NONE',  ( -158.9822249764580135, 20.32000000000000028, 107.9500000000000028 ) ) ;
#19662 = AXIS2_PLACEMENT_3D ( 'NONE', #67329, #25109, #88256 ) ;
#19663 = CIRCLE ( 'NONE', #79147, 88.90000000000000568 ) ;
#19664 = CARTESIAN_POINT ( 'NONE',  ( 116.5268644012694637, -41.19342475044518181, 228.4756252759109714 ) ) ;
#19665 = ORIENTED_EDGE ( 'NONE', *, *, #85297, .F. ) ;
#19666 = VECTOR ( 'NONE', #58810, 1000.000000000000114 ) ;
#19667 = ADVANCED_FACE ( 'NONE', ( #27182 ), #60776, .T. ) ;
#19668 = LINE ( 'NONE', #27374, #69538 ) ;
#19670 = EDGE_CURVE ( 'NONE', #84394, #25618, #35328, .T. ) ;
#19669 = CARTESIAN_POINT ( 'NONE',  ( -492.0614999999999668, 14.28749999999982201, 90.48749999999999716 ) ) ;
#19671 = LINE ( 'NONE', #25138, #3426 ) ;
#19672 = ADVANCED_FACE ( 'NONE', ( #371 ), #42139, .T. ) ;
#19673 = CARTESIAN_POINT ( 'NONE',  ( 114.6306032519149198, -32.52409173292234357, 27.06047132197198124 ) ) ;
#19675 = VECTOR ( 'NONE', #5680, 1000.000000000000000 ) ;
#19674 = CARTESIAN_POINT ( 'NONE',  ( 108.9888594788934029, -47.63768604335348300, 118.7032443235299723 ) ) ;
#19676 = CARTESIAN_POINT ( 'NONE',  ( 94.86917197795300183, -31.06128196069623471, 25.56312527591095574 ) ) ;
#19677 = VERTEX_POINT ( 'NONE', #20820 ) ;
#19678 = EDGE_CURVE ( 'NONE', #83074, #36562, #63040, .T. ) ;
#19679 = VECTOR ( 'NONE', #7683, 1000.000000000000000 ) ;
#19680 = CARTESIAN_POINT ( 'NONE',  ( 41.56648329127398966, -27.82844715994070484, 198.9256252759119832 ) ) ;
#19681 = CARTESIAN_POINT ( 'NONE',  ( 101.7972116522101089, -45.32445798590094199, 67.13961389132575164 ) ) ;
#19682 = VERTEX_POINT ( 'NONE', #54408 ) ;
#19683 = EDGE_LOOP ( 'NONE', ( #27110, #64326, #44908, #45773 ) ) ;
#19684 = LINE ( 'NONE', #41892, #11113 ) ;
#19685 = ORIENTED_EDGE ( 'NONE', *, *, #83186, .T. ) ;
#19686 = ORIENTED_EDGE ( 'NONE', *, *, #46876, .T. ) ;
#19687 = CARTESIAN_POINT ( 'NONE',  ( 28.57499999999999929, 87.13271776169270311, 294.9574999999999818 ) ) ;
#19688 = AXIS2_PLACEMENT_3D ( 'NONE', #5550, #52743, #66405 ) ;
#19689 = CARTESIAN_POINT ( 'NONE',  ( 102.8831062096190436, -29.28260300185988996, 59.90670554236199052 ) ) ;
#19690 = CARTESIAN_POINT ( 'NONE',  ( 116.6260796636124155, -40.94376574832517690, 253.4956252759109532 ) ) ;
#19691 = CARTESIAN_POINT ( 'NONE',  ( 114.2383551682310525, -44.26553795382362466, 158.1813395616249807 ) ) ;
#19693 = CARTESIAN_POINT ( 'NONE',  ( 116.1395517938576347, -31.55217135963209785, 285.2384824187680579 ) ) ;
#19692 = CARTESIAN_POINT ( 'NONE',  ( 117.0881497372581634, -37.78494053717825096, 23.74254566645982933 ) ) ;
#19694 = DIRECTION ( 'NONE',  ( 0.000000000000000000, 0.000000000000000000, 1.000000000000000000 ) ) ;
#19695 = CARTESIAN_POINT ( 'NONE',  ( 112.0634802680675222, -45.48975181846424931, 93.98957202063608918 ) ) ;
#19696 = EDGE_LOOP ( 'NONE', ( #8160, #25756, #38094, #60392 ) ) ;
#19697 = CARTESIAN_POINT ( 'NONE',  ( 83.56670390244801183, -36.72944715994108122, 218.0711402470150801 ) ) ;
#19698 = CARTESIAN_POINT ( 'NONE',  ( 110.0016395821292292, -26.67999326470393839, 259.8499109901964630 ) ) ;
#19699 = EDGE_LOOP ( 'NONE', ( #39221, #65552, #12962, #5741 ) ) ;
#19700 = CARTESIAN_POINT ( 'NONE',  ( 114.8141470925876462, -29.70096138442027112, 209.4127681330539872 ) ) ;
#19701 = DIRECTION ( 'NONE',  ( 0.000000000000000000, 1.000000000000000000, 0.000000000000000000 ) ) ;
#19702 = AXIS2_PLACEMENT_3D ( 'NONE', #38333, #26059, #73298 ) ;
#19703 = FACE_OUTER_BOUND ( 'NONE', #22834, .T. ) ;
#19704 = CARTESIAN_POINT ( 'NONE',  ( 116.8174769680534979, -34.15428111572317249, 25.03134733120764821 ) ) ;
#19705 = DIRECTION ( 'NONE',  ( -0.7071067811865170416, -0.7071067811865778818, -7.071067811865162747E-16 ) ) ;
#19707 = CARTESIAN_POINT ( 'NONE',  ( -487.2989999999999782, 7.143750000000339995, 6.988054014476278830 ) ) ;
#19706 = CARTESIAN_POINT ( 'NONE',  ( 113.4524916730000825, -42.42761561582053531, 277.6356252759110248 ) ) ;
#19708 = DIRECTION ( 'NONE',  ( -0.7071067811865671127, -0.7071067811865279218, -7.071067811865664660E-16 ) ) ;
#19709 = PLANE ( 'NONE',  #71483 ) ;
#19710 = CARTESIAN_POINT ( 'NONE',  ( 92.84712468462734591, -113.5675721218997865, -19.21046202161272376 ) ) ;
#19711 = DIRECTION ( 'NONE',  ( -3.100000000000000258E-29, 3.100000000000000044E-14, 1.000000000000000000 ) ) ;
#19712 = DIRECTION ( 'NONE',  ( 1.000000000000000000, 0.000000000000000000, 6.982966722218760189E-15 ) ) ;
#19713 = DIRECTION ( 'NONE',  ( 1.000000000000000000, 2.106816776397999944E-14, 9.351236661543306751E-17 ) ) ;
#19715 = ORIENTED_EDGE ( 'NONE', *, *, #72937, .F. ) ;
#19714 = CARTESIAN_POINT ( 'NONE',  ( 101.0178098607260893, -29.23851721486679267, 195.5838068554161282 ) ) ;
#19716 = LINE ( 'NONE', #40607, #84386 ) ;
#19717 = CARTESIAN_POINT ( 'NONE',  ( 96.66004714996478242, -35.80616453621266970, 231.2556252759109725 ) ) ;
#19718 = CARTESIAN_POINT ( 'NONE',  ( 109.7700798034136511, -47.44693503648352362, 88.78514908543493789 ) ) ;
#19719 = CARTESIAN_POINT ( 'NONE',  ( 118.1536727146126395, -36.20817079386891635, 264.8518157521014587 ) ) ;
#19720 = CARTESIAN_POINT ( 'NONE',  ( 97.07207207514328218, -35.37844108510153518, 156.2189586001694579 ) ) ;
#19721 = CARTESIAN_POINT ( 'NONE',  ( 182.0374245136142406, -23.42844715993458848, 193.9678068554150059 ) ) ;
#19722 = B_SPLINE_CURVE_WITH_KNOTS ( 'NONE', 3,
 ( #68731, #82827, #27833, #54617, #6070, #61448, #6949, #61012, #34650, #76890, #54169, #42341, #47813, #68290, #55512, #48705, #6497, #21482, #82377, #70072, #81929, #75553, #69628, #49157, #34197 ),
 .UNSPECIFIED., .F., .F.,
 ( 4, 2, 2, 1, 2, 2, 2, 2, 2, 2, 2, 2, 4 ),
 ( 0.03973448063954120035, 0.04221847903031247795, 0.04346047822569811675, 0.04470247742108374861, 0.04594447661646938741, 0.04718647581185502621, 0.04967047420262627605, 0.05091247339801188709, 0.05215447259339749814, 0.05463847098416872022, 0.05588047017955435208, 0.05712246937493997700, 0.05960646776571127542 ),
 .UNSPECIFIED. ) ;
#19724 = CARTESIAN_POINT ( 'NONE',  ( 0.000000000000000000, 0.000000000000000000, 0.000000000000000000 ) ) ;
#19723 = CARTESIAN_POINT ( 'NONE',  ( 107.0664832912739399, -36.72944715994096754, 298.1356252759109680 ) ) ;
#19725 = DIRECTION ( 'NONE',  ( 0.7071067811865536790, 0.000000000000000000, -0.7071067811865414665 ) ) ;
#19726 = B_SPLINE_CURVE_WITH_KNOTS ( 'NONE', 3,
 ( #43092, #49004, #29489, #83125, #70836, #20884, #36305, #56732, #35389, #21791, #77199, #48552, #76293, #8607, #14064, #29045, #41748, #35843 ),
 .UNSPECIFIED., .F., .F.,
 ( 4, 2, 2, 2, 2, 2, 2, 2, 4 ),
 ( 0.000000000000000000, 0.06249999994414716376, 0.1249999998882943275, 0.1874999998324414774, 0.2499999997765886550, 0.3124999997207358327, 0.3749999996648829548, 0.4374999996090297993, 0.4999999995531766439 ),
 .UNSPECIFIED. ) ;
#19727 = CARTESIAN_POINT ( 'NONE',  ( 131.5867845949916557, -19.92005462651755110, 2.747931806393766774 ) ) ;
#19728 = AXIS2_PLACEMENT_3D ( 'NONE', #12958, #40645, #12506 ) ;
#19729 = AXIS2_PLACEMENT_3D ( 'NONE', #49898, #1326, #871 ) ;
#19731 = EDGE_CURVE ( 'NONE', #25758, #54218, #82621, .T. ) ;
#19730 = VECTOR ( 'NONE', #13725, 1000.000000000000000 ) ;
#19732 = AXIS2_PLACEMENT_3D ( 'NONE', #89597, #26907, #13288 ) ;
#19733 = ORIENTED_EDGE ( 'NONE', *, *, #71655, .F. ) ;
#19734 = ADVANCED_FACE ( 'NONE', ( #14001 ), #822, .T. ) ;
#19735 = ORIENTED_EDGE ( 'NONE', *, *, #16518, .F. ) ;
#19736 = CARTESIAN_POINT ( 'NONE',  ( 108.0580239150950774, -28.21657753114420331, 129.4067055423629711 ) ) ;
#19737 = EDGE_CURVE ( 'NONE', #84886, #2655, #56205, .T. ) ;
#19739 = ORIENTED_EDGE ( 'NONE', *, *, #58084, .T. ) ;
#19738 = DIRECTION ( 'NONE',  ( -0.7396053187813123042, -0.6730408400909958511, 0.000000000000000000 ) ) ;
#19740 = CARTESIAN_POINT ( 'NONE',  ( 116.3191775144681515, -32.94222376661483764, 89.13562527591095375 ) ) ;
#19741 = CARTESIAN_POINT ( 'NONE',  ( 108.9808406375926779, -47.59218431635552093, 118.7032443235299723 ) ) ;
#19742 = DIRECTION ( 'NONE',  ( 0.000000000000000000, 0.000000000000000000, 1.000000000000000000 ) ) ;
#19743 = FACE_OUTER_BOUND ( 'NONE', #66476, .T. ) ;
#19744 = EDGE_CURVE ( 'NONE', #14095, #70385, #65209, .T. ) ;
#19745 = ADVANCED_FACE ( 'NONE', ( #47606 ), #68073, .F. ) ;
#19746 = PLANE ( 'NONE',  #28791 ) ;
#19747 = CARTESIAN_POINT ( 'NONE',  ( 112.0659116261392541, -45.48839625842523304, 108.9897919429150761 ) ) ;
#19749 = CARTESIAN_POINT ( 'NONE',  ( 116.4365193811697310, -32.28633913640743458, 64.19086337114998742 ) ) ;
#19748 = AXIS2_PLACEMENT_3D ( 'NONE', #58335, #2495, #86062 ) ;
#19750 = ORIENTED_EDGE ( 'NONE', *, *, #25941, .F. ) ;
#19751 = VERTEX_POINT ( 'NONE', #68970 ) ;
#19752 = EDGE_CURVE ( 'NONE', #18741, #28403, #49232, .T. ) ;
#19753 = VERTEX_POINT ( 'NONE', #43028 ) ;
#19754 = EDGE_CURVE ( 'NONE', #56065, #87130, #30327, .T. ) ;
#19755 = CARTESIAN_POINT ( 'NONE',  ( 145.4513818679876920, -123.8420284488499306, 247.5435765132629626 ) ) ;
#19757 = DIRECTION ( 'NONE',  ( -4.237773401492740281E-14, 1.000000000000000000, 0.000000000000000000 ) ) ;
#19756 = CARTESIAN_POINT ( 'NONE',  ( 112.9441315310008918, -44.54716313336194844, 139.0899109901959605 ) ) ;
#19758 = CIRCLE ( 'NONE', #58892, 7.143750000000001599 ) ;
#19759 = LINE ( 'NONE', #68358, #66838 ) ;
#19760 = EDGE_CURVE ( 'NONE', #86449, #43505, #79749, .T. ) ;
#19761 = DIRECTION ( 'NONE',  ( 0.000000000000000000, 0.000000000000000000, -1.000000000000000000 ) ) ;
#19762 = LINE ( 'NONE', #47440, #8341 ) ;
#19763 = CARTESIAN_POINT ( 'NONE',  ( 90.13147184857858463, 91.23868085022587593, 77.01901799881319732 ) ) ;
#19764 = CARTESIAN_POINT ( 'NONE',  ( 112.0655926785064906, -45.48857413222889079, 178.9897630915276352 ) ) ;
#19765 = CARTESIAN_POINT ( 'NONE',  ( 116.5135284680788175, -32.37261310794432490, 104.1699109901969535 ) ) ;
#19766 = ORIENTED_EDGE ( 'NONE', *, *, #16581, .T. ) ;
#19767 = ORIENTED_EDGE ( 'NONE', *, *, #49788, .F. ) ;
#19769 = ORIENTED_EDGE ( 'NONE', *, *, #50297, .T. ) ;
#19768 = ADVANCED_FACE ( 'NONE', ( #50758 ), #2175, .T. ) ;
#19770 = FACE_OUTER_BOUND ( 'NONE', #5476, .T. ) ;
#19771 = CYLINDRICAL_SURFACE ( 'NONE', #86784, 2.117000000000000881 ) ;
#19772 = CARTESIAN_POINT ( 'NONE',  ( 172.5664832912729878, -27.57844715994070484, 81.92562527591199739 ) ) ;
#19773 = CARTESIAN_POINT ( 'NONE',  ( 98.92939184154955967, -35.79647825066581390, 204.0538046553059814 ) ) ;
#19774 = CARTESIAN_POINT ( 'NONE',  ( 113.2464514564345706, -28.75940189997899310, 25.55195518195452564 ) ) ;
#19775 = ORIENTED_EDGE ( 'NONE', *, *, #78663, .F. ) ;
#19777 = ORIENTED_EDGE ( 'NONE', *, *, #82841, .T. ) ;
#19776 = VERTEX_POINT ( 'NONE', #30765 ) ;
#19778 = DIRECTION ( 'NONE',  ( 0.000000000000000000, -0.8660254037844351549, -0.5000000000000061062 ) ) ;
#19779 = CARTESIAN_POINT ( 'NONE',  ( 136.7495928495827400, -19.33856210725350167, 3.004220725469440634 ) ) ;
#19780 = EDGE_LOOP ( 'NONE', ( #76760, #49996, #27041, #45898 ) ) ;
#19781 = ORIENTED_EDGE ( 'NONE', *, *, #3499, .T. ) ;
#19782 = CARTESIAN_POINT ( 'NONE',  ( 77.33333279747650124, -19.08363404521308482, 6.775960187534255219 ) ) ;
#19783 = ADVANCED_FACE ( 'NONE', ( #77577 ), #29884, .F. ) ;
#19784 = CARTESIAN_POINT ( 'NONE',  ( 108.0145050256332979, -45.54020952213421936, 199.0930118773259778 ) ) ;
#19785 = EDGE_CURVE ( 'NONE', #1301, #51309, #37586, .T. ) ;
#19786 = VECTOR ( 'NONE', #87818, 1000.000000000000000 ) ;
#19787 = CARTESIAN_POINT ( 'NONE',  ( 31.75000000000000000, 66.67499999999999716, 342.8999999999999773 ) ) ;
#19788 = CARTESIAN_POINT ( 'NONE',  ( -109.6498392670675628, 58.85328883199191097, 70.86473263594878347 ) ) ;
#19789 = AXIS2_PLACEMENT_3D ( 'NONE', #11386, #4122, #39080 ) ;
#19790 = ORIENTED_EDGE ( 'NONE', *, *, #32577, .T. ) ;
#19791 = EDGE_LOOP ( 'NONE', ( #50703, #21020, #23262, #77874 ) ) ;
#19792 = VECTOR ( 'NONE', #24854, 1000.000000000000000 ) ;
#19793 = AXIS2_PLACEMENT_3D ( 'NONE', #4799, #32483, #60183 ) ;
#19794 = PLANE ( 'NONE',  #14498 ) ;
#19795 = AXIS2_PLACEMENT_3D ( 'NONE', #73150, #78218, #38631 ) ;
#19796 = ORIENTED_EDGE ( 'NONE', *, *, #53717, .T. ) ;
#19797 = ORIENTED_EDGE ( 'NONE', *, *, #18424, .F. ) ;
#19798 = CARTESIAN_POINT ( 'NONE',  ( 110.0029149558365305, -28.58829895313488834, 247.6071379886389821 ) ) ;
#19799 = CARTESIAN_POINT ( 'NONE',  ( 97.72652769937234041, -42.68433437468970482, 141.7661014663869707 ) ) ;
#19800 = CARTESIAN_POINT ( 'NONE',  ( 96.97787942770413849, -32.27031107066116533, 55.98324432352897162 ) ) ;
#19801 = CARTESIAN_POINT ( 'NONE',  ( 104.2046607136328191, -44.36613767402425879, 249.5838068554171230 ) ) ;
#19802 = B_SPLINE_SURFACE_WITH_KNOTS ( 'NONE', 3, 3, ( 
 ( #33674, #39580, #19155, #40925 ),
 ( #89093, #54531, #46828, #75468 ),
 ( #67286, #13238, #68648, #6414 ),
 ( #34106, #61812, #75908, #13676 ),
 ( #4627, #74556, #40029, #32311 ),
 ( #62268, #72116, #3077, #35006 ),
 ( #41808, #51648, #21398, #79391 ) ),
 .UNSPECIFIED., .F., .F., .F.,
 ( 4, 1, 1, 1, 4 ),
 ( 4, 4 ),
 ( -0.0008599663877943859985, 0.2857142857142860315, 0.5714285714285709528, 0.8571428571428569843, 1.000859966387789957 ),
 ( 0.09780657971653439198, 1.000859966387789957 ),
 .UNSPECIFIED. ) ;
#19803 = CARTESIAN_POINT ( 'NONE',  ( 33.78309357195659146, -29.99615139352317428, 117.4678068554150485 ) ) ;
#19804 = CARTESIAN_POINT ( 'NONE',  ( 97.81138037892189629, -40.51667183916828918, 42.63556083456600732 ) ) ;
#19805 = CARTESIAN_POINT ( 'NONE',  ( 117.2915085808104436, -34.52259632565112213, 179.9956252759109532 ) ) ;
#19806 = DIRECTION ( 'NONE',  ( 0.000000000000000000, 0.000000000000000000, 1.000000000000000000 ) ) ;
#19807 = VERTEX_POINT ( 'NONE', #8995 ) ;
#19808 = DIRECTION ( 'NONE',  ( 0.000000000000000000, -1.000000000000000000, 0.000000000000000000 ) ) ;
#19809 = ORIENTED_EDGE ( 'NONE', *, *, #63859, .F. ) ;
#19810 = VERTEX_POINT ( 'NONE', #1729 ) ;
#19811 = DIRECTION ( 'NONE',  ( 0.000000000000000000, 0.000000000000000000, 1.000000000000000000 ) ) ;
#19812 = VECTOR ( 'NONE', #26056, 1000.000000000000000 ) ;
#19813 = ORIENTED_EDGE ( 'NONE', *, *, #73659, .F. ) ;
#19814 = CARTESIAN_POINT ( 'NONE',  ( 150.5667039024473297, -25.42844715993594562, 300.4678068554149490 ) ) ;
#19815 = CARTESIAN_POINT ( 'NONE',  ( 102.0652380361773339, -27.97156370417384608, 91.48995787984884487 ) ) ;
#19816 = CARTESIAN_POINT ( 'NONE',  ( 113.4154522487949919, -27.68126056648907252, 84.57753003781698453 ) ) ;
#19817 = CARTESIAN_POINT ( 'NONE',  ( -11.66942133526382008, 77.53815898108125282, 130.0334386654385526 ) ) ;
#19818 = LINE ( 'NONE', #20277, #46434 ) ;
#19819 = FACE_OUTER_BOUND ( 'NONE', #80935, .T. ) ;
#19822 = CARTESIAN_POINT ( 'NONE',  ( 117.1710321396410421, -41.15233254730026147, 204.4861014663869696 ) ) ;
#19821 = DIRECTION ( 'NONE',  ( 0.000000000000000000, 0.000000000000000000, -1.000000000000000000 ) ) ;
#19820 = CARTESIAN_POINT ( 'NONE',  ( 115.7831076679527058, -41.80230951405372508, 144.4064586089073714 ) ) ;
#19823 = DIRECTION ( 'NONE',  ( -0.7071067811865480168, 0.000000000000000000, 0.7071067811865470176 ) ) ;
#19824 = LINE ( 'NONE', #67073, #1777 ) ;
#19825 = ORIENTED_EDGE ( 'NONE', *, *, #52535, .T. ) ;
#19826 = CARTESIAN_POINT ( 'NONE',  ( 226.4410000000000025, 40.03750000000000142, 10.66800000000000104 ) ) ;
#19827 = CARTESIAN_POINT ( 'NONE',  ( 37.56670390244828184, -48.82844715994119866, 300.4678068554150059 ) ) ;
#19828 = CARTESIAN_POINT ( 'NONE',  ( 97.81171235735017433, -40.51746255502365557, 257.6350867217079212 ) ) ;
#19829 = DIRECTION ( 'NONE',  ( 1.000000000000000000, 0.000000000000000000, 0.000000000000000000 ) ) ;
#19831 = VERTEX_POINT ( 'NONE', #84856 ) ;
#19830 = CARTESIAN_POINT ( 'NONE',  ( 110.0016395821292292, -26.67999326470393839, 259.8499109901964630 ) ) ;
#19832 = CARTESIAN_POINT ( 'NONE',  ( 112.5227400616102500, -28.31493319190477109, 194.6183074944887039 ) ) ;
#19833 = CARTESIAN_POINT ( 'NONE',  ( 115.7133342524696360, -42.59197454220085177, 269.3527681330536439 ) ) ;
#19834 = CARTESIAN_POINT ( 'NONE',  ( 114.2698949211017663, -45.17901133753223064, 149.1508633711489722 ) ) ;
#19835 = CARTESIAN_POINT ( 'NONE',  ( 107.0664832912739399, -36.72944715994095333, 293.9356252759109793 ) ) ;
#19836 = CARTESIAN_POINT ( 'NONE',  ( 99.09577730710090293, -30.55033931252097545, 101.8022151059804656 ) ) ;
#19837 = EDGE_CURVE ( 'NONE', #1672, #58534, #41971, .T. ) ;
#19839 = DIRECTION ( 'NONE',  ( 4.012088370409549976E-14, -1.000000000000000000, 0.000000000000000000 ) ) ;
#19838 = LINE ( 'NONE', #54772, #44862 ) ;
#19840 = CARTESIAN_POINT ( 'NONE',  ( -48.02966122971776741, 100.5999999999999659, 75.53254848357481421 ) ) ;
#19841 = DIRECTION ( 'NONE',  ( 1.000000000000000000, 0.000000000000000000, 0.000000000000000000 ) ) ;
#19842 = ORIENTED_EDGE ( 'NONE', *, *, #73612, .T. ) ;
#19843 = ADVANCED_FACE ( 'NONE', ( #85311, #43928 ), #15363, .T. ) ;
#19844 = EDGE_LOOP ( 'NONE', ( #38656, #35369, #9969, #71080, #39318 ) ) ;
#19845 = ADVANCED_FACE ( 'NONE', ( #22624 ), #36696, .F. ) ;
#19846 = ORIENTED_EDGE ( 'NONE', *, *, #30209, .F. ) ;
#19847 = EDGE_CURVE ( 'NONE', #72244, #59868, #85755, .T. ) ;
#19848 = EDGE_LOOP ( 'NONE', ( #1244, #80048, #472, #59054 ) ) ;
#19849 = CARTESIAN_POINT ( 'NONE',  ( 5.210259806972410633E-15, 111.1250000000000000, -42.54500000000000171 ) ) ;
#19850 = CARTESIAN_POINT ( 'NONE',  ( 116.3681181406586518, -31.99193570193499525, 40.20133956162496958 ) ) ;
#19851 = CARTESIAN_POINT ( 'NONE',  ( 129.9817983987124705, -140.4109954690793245, 246.9195128019829895 ) ) ;
#19852 = LINE ( 'NONE', #13049, #23898 ) ;
#19853 = ADVANCED_FACE ( 'NONE', ( #65288 ), #78930, .F. ) ;
#19854 = DIRECTION ( 'NONE',  ( 0.000000000000000000, 1.000000000000000000, 0.000000000000000000 ) ) ;
#19855 = VECTOR ( 'NONE', #28957, 1000.000000000000000 ) ;
#19856 = CARTESIAN_POINT ( 'NONE',  ( 116.0662231142348162, -35.72080775710429634, 233.3257531614099776 ) ) ;
#19857 = EDGE_LOOP ( 'NONE', ( #37642, #36610, #30655, #41023, #19031, #85076 ) ) ;
#19858 = ORIENTED_EDGE ( 'NONE', *, *, #43562, .T. ) ;
#19859 = VERTEX_POINT ( 'NONE', #1277 ) ;
#19860 = ADVANCED_FACE ( 'NONE', ( #44377 ), #43458, .F. ) ;
#19861 = AXIS2_PLACEMENT_3D ( 'NONE', #50657, #78398, #14819 ) ;
#19862 = AXIS2_PLACEMENT_3D ( 'NONE', #2804, #72730, #10499 ) ;
#19863 = DIRECTION ( 'NONE',  ( 1.151873470568221791E-31, -1.000000000000000000, -5.463695987328529395E-16 ) ) ;
#19864 = VECTOR ( 'NONE', #36306, 1000.000000000000000 ) ;
#19865 = B_SPLINE_CURVE_WITH_KNOTS ( 'NONE', 3,
 ( #72572, #79396, #10766, #9896, #32108, #85771, #59802, #3083, #32549, #73900, #24859, #11684, #23541, #51204, #52965, #46169, #37604, #45282, #44391, #78947, #58910, #73445, #24420, #39377, #38043, #3514, #72122, #73001, #80289 ),
 .UNSPECIFIED., .F., .F.,
 ( 4, 2, 2, 2, 2, 2, 2, 2, 2, 2, 1, 1, 1, 1, 1, 2, 4 ),
 ( 0.000000000000000000, 0.06250189640743901431, 0.1250037928148780286, 0.1875056892223170568, 0.2500075856297560573, 0.3125094820371950854, 0.3750113784446341136, 0.4375132748520730863, 0.4687642230557926837, 0.4843896971576525656, 0.4922024342085823956, 0.4961088027340472273, 0.4980619869967797819, 0.4990385791281458094, 0.4995268751938287122, 0.4997710232266699970, 0.5000151712595112263 ),
 .UNSPECIFIED. ) ;
#19866 = CARTESIAN_POINT ( 'NONE',  ( 100.8875041660994043, -44.70025221268588211, 102.0524332644927057 ) ) ;
#19867 = CARTESIAN_POINT ( 'NONE',  ( 20.03715912545735023, -46.82818131006202123, 180.4678068554150911 ) ) ;
#19868 = CARTESIAN_POINT ( 'NONE',  ( 100.9529263511984141, -28.70839242354088583, 275.5937037153142910 ) ) ;
#19869 = EDGE_CURVE ( 'NONE', #87491, #1864, #2298, .T. ) ;
#19870 = DIRECTION ( 'NONE',  ( 0.7071067811865533459, 0.000000000000000000, -0.7071067811865416886 ) ) ;
#19871 = CARTESIAN_POINT ( 'NONE',  ( 107.0664832912739257, -50.22944715994096043, 311.6356252759109680 ) ) ;
#19872 = CARTESIAN_POINT ( 'NONE',  ( 96.93540839703290146, -34.51582869190840341, 256.1432443235307232 ) ) ;
#19873 = LINE ( 'NONE', #49353, #3784 ) ;
#19875 = EDGE_LOOP ( 'NONE', ( #86948, #58834, #44181, #2147 ) ) ;
#19874 = EDGE_CURVE ( 'NONE', #34264, #65898, #23227, .T. ) ;
#19876 = DIRECTION ( 'NONE',  ( -0.000000000000000000, -0.000000000000000000, 1.000000000000000000 ) ) ;
#19877 = CIRCLE ( 'NONE', #30061, 12.44600000000001216 ) ;
#19878 = VECTOR ( 'NONE', #41791, 1000.000000000000000 ) ;
#19879 = FACE_OUTER_BOUND ( 'NONE', #2657, .T. ) ;
#19880 = CARTESIAN_POINT ( 'NONE',  ( 100.2308834438963174, -41.19087078291441628, 99.60523322673398638 ) ) ;
#19881 = CIRCLE ( 'NONE', #27078, 1.571100913904333041 ) ;
#19882 = CARTESIAN_POINT ( 'NONE',  ( 115.8243402359382657, -31.72812547371020031, 129.2399646760175074 ) ) ;
#19883 = LINE ( 'NONE', #4462, #76616 ) ;
#19884 = DIRECTION ( 'NONE',  ( -1.000000000000000078E-15, 1.000000000000000083E-30, 1.000000000000000000 ) ) ;
#19885 = EDGE_LOOP ( 'NONE', ( #43858, #53294 ) ) ;
#19886 = CARTESIAN_POINT ( 'NONE',  ( 107.0664832912739541, -23.22944715994095688, 315.1356252759112522 ) ) ;
#19887 = EDGE_LOOP ( 'NONE', ( #48358, #62696, #17649, #63253 ) ) ;
#19888 = CARTESIAN_POINT ( 'NONE',  ( 113.6146262985763258, -28.61718150614917633, 164.5356252759109736 ) ) ;
#19889 = ORIENTED_EDGE ( 'NONE', *, *, #1736, .T. ) ;
#19890 = CARTESIAN_POINT ( 'NONE',  ( 99.08946256649485917, -109.4614598618336174, 2.217806855418169576 ) ) ;
#19891 = CARTESIAN_POINT ( 'NONE',  ( 112.3776303481765950, -29.59825886299321951, 100.9987261630399757 ) ) ;
#19892 = FACE_BOUND ( 'NONE', #54899, .T. ) ;
#19893 = EDGE_CURVE ( 'NONE', #22477, #47420, #50298, .T. ) ;
#19894 = DIRECTION ( 'NONE',  ( 0.000000000000000000, -1.000000000000000000, 0.000000000000000000 ) ) ;
#19895 = CARTESIAN_POINT ( 'NONE',  ( 98.70509129169590778, -42.99238438483101987, 62.83848241876793850 ) ) ;
#19896 = AXIS2_PLACEMENT_3D ( 'NONE', #83735, #41921, #77817 ) ;
#19897 = CARTESIAN_POINT ( 'NONE',  ( 112.0657206150906120, -45.48850286296052303, 257.9896703071129878 ) ) ;
#19898 = EDGE_LOOP ( 'NONE', ( #77055, #38976, #70055, #88686, #2996 ) ) ;
#19899 = CARTESIAN_POINT ( 'NONE',  ( -118.1704280561597358, 74.16215221268205937, -9.571784452933755460 ) ) ;
#19900 = VERTEX_POINT ( 'NONE', #43478 ) ;
#19901 = B_SPLINE_CURVE_WITH_KNOTS ( 'NONE', 3,
 ( #88082, #31304, #81279, #19025, #89879, #48054, #75789, #75341, #34886, #55750, #33985, #76228, #372, #42140, #40359, #55311, #19475, #14002 ),
 .UNSPECIFIED., .F., .F.,
 ( 4, 2, 2, 2, 2, 2, 2, 2, 4 ),
 ( 0.4999390785766987810, 0.5624466937546114265, 0.6249543089325240164, 0.6874619241104367173, 0.7499695392883494183, 0.8124771544662620082, 0.8749847696441745981, 0.9374923848220872991, 1.000000000000000000 ),
 .UNSPECIFIED. ) ;
#19902 = EDGE_LOOP ( 'NONE', ( #47170, #20652 ) ) ;
#19903 = DIRECTION ( 'NONE',  ( 0.4999999999999989453, 0.8660254037844392627, -2.684678751731760294E-14 ) ) ;
#19904 = ORIENTED_EDGE ( 'NONE', *, *, #64878, .F. ) ;
#19905 = CARTESIAN_POINT ( 'NONE',  ( 104.1325824198641499, -27.39908484284267587, 250.3184824187684683 ) ) ;
#19906 = CARTESIAN_POINT ( 'NONE',  ( 95.65143945485090171, -33.45545561978638460, 137.1041967044819501 ) ) ;
#19907 = CARTESIAN_POINT ( 'NONE',  ( 123.6837132603321692, -20.11243780205712639, 249.5838068554165261 ) ) ;
#19908 = CARTESIAN_POINT ( 'NONE',  ( 97.33784131423797703, -34.07106451867782226, 142.1147919416630430 ) ) ;
#19909 = CARTESIAN_POINT ( 'NONE',  ( 113.3423928682155406, -27.63071431045342763, 85.60800622829195561 ) ) ;
#19910 = DIRECTION ( 'NONE',  ( -0.7071067811865753283, 0.7071067811865197061, -7.071067811865760309E-16 ) ) ;
#19911 = VERTEX_POINT ( 'NONE', #71223 ) ;
#19912 = CARTESIAN_POINT ( 'NONE',  ( 1.387778780781445676E-14, 238.8000000000000114, 104.4754207677255806 ) ) ;
#19913 = EDGE_CURVE ( 'NONE', #24486, #35637, #10094, .T. ) ;
#19914 = CIRCLE ( 'NONE', #64855, 29.49999999999998579 ) ;
#19915 = AXIS2_PLACEMENT_3D ( 'NONE', #66773, #47211, #4560 ) ;
#19916 = CARTESIAN_POINT ( 'NONE',  ( 113.1786488514148061, -44.75160319904480843, 159.0938251498227771 ) ) ;
#19917 = ORIENTED_EDGE ( 'NONE', *, *, #81304, .F. ) ;
#19918 = EDGE_CURVE ( 'NONE', #63276, #74286, #66614, .T. ) ;
#19919 = CIRCLE ( 'NONE', #47456, 2.750000000000002665 ) ;
#19920 = CARTESIAN_POINT ( 'NONE',  ( 44.45000000000000284, 66.67499999999999716, 219.0749999999999886 ) ) ;
#19921 = CIRCLE ( 'NONE', #44540, 4.750000000000004441 ) ;
#19922 = DIRECTION ( 'NONE',  ( 0.000000000000000000, 0.000000000000000000, 1.000000000000000000 ) ) ;
#19923 = CARTESIAN_POINT ( 'NONE',  ( 111.7292870705843768, -27.42961193919077445, 279.7070538473396937 ) ) ;
#19924 = DIRECTION ( 'NONE',  ( 0.000000000000000000, 0.000000000000000000, 1.000000000000000000 ) ) ;
#19925 = AXIS2_PLACEMENT_3D ( 'NONE', #49251, #62447, #20229 ) ;
#19926 = DIRECTION ( 'NONE',  ( 0.000000000000000000, -1.000000000000000000, 0.000000000000000000 ) ) ;
#19927 = FACE_OUTER_BOUND ( 'NONE', #89247, .T. ) ;
#19928 = CARTESIAN_POINT ( 'NONE',  ( 116.8666057829012033, -37.25052826422871277, 18.78419670448294809 ) ) ;
#19930 = CARTESIAN_POINT ( 'NONE',  ( 103.1828028919049984, -27.07824557232550688, 126.3813395616259783 ) ) ;
#19929 = CARTESIAN_POINT ( 'NONE',  ( 97.11097791331823714, -37.83202729851629442, 101.4149069316836602 ) ) ;
#19931 = LINE ( 'NONE', #74895, #30627 ) ;
#19932 = CARTESIAN_POINT ( 'NONE',  ( 96.60586043895887087, -37.15609470439714102, 161.3584824187679487 ) ) ;
#19933 = ORIENTED_EDGE ( 'NONE', *, *, #70421, .F. ) ;
#19934 = LINE ( 'NONE', #33991, #65563 ) ;
#19935 = EDGE_LOOP ( 'NONE', ( #51596, #56197, #56446, #87269 ) ) ;
#19936 = DIRECTION ( 'NONE',  ( 0.000000000000000000, -1.000000000000000000, 0.000000000000000000 ) ) ;
#19937 = CARTESIAN_POINT ( 'NONE',  ( 110.7653435595065901, 44.45000000000000284, 69.10794311903988785 ) ) ;
#19938 = CARTESIAN_POINT ( 'NONE',  ( -186.2398777604659870, 0.000000000000000000, 107.9500000000000028 ) ) ;
#19939 = EDGE_LOOP ( 'NONE', ( #9731, #401, #30128, #14218 ) ) ;
#19940 = CIRCLE ( 'NONE', #85263, 11.17600000000001970 ) ;
#19941 = CARTESIAN_POINT ( 'NONE',  ( 115.8271982374479592, -31.73307718988874271, 60.23988603985338841 ) ) ;
#19943 = ORIENTED_EDGE ( 'NONE', *, *, #38767, .F. ) ;
#19942 = CARTESIAN_POINT ( 'NONE',  ( 117.3534821530742107, -34.78408995979881269, 158.9756252759109714 ) ) ;
#19944 = DIRECTION ( 'NONE',  ( -4.237773401492740281E-14, 1.000000000000000000, 0.000000000000000000 ) ) ;
#19945 = AXIS2_PLACEMENT_3D ( 'NONE', #29267, #23365, #36075 ) ;
#19946 = DIRECTION ( 'NONE',  ( 0.9068632946707805287, -0.4214249218767882055, 9.081056412856297650E-16 ) ) ;
#19947 = CIRCLE ( 'NONE', #11243, 81.91591158490091118 ) ;
#19948 = CARTESIAN_POINT ( 'NONE',  ( 8.960875259515155733, 209.9608752595157455, 75.92175051903043936 ) ) ;
#19949 = FACE_OUTER_BOUND ( 'NONE', #62014, .T. ) ;
#19950 = ORIENTED_EDGE ( 'NONE', *, *, #16672, .T. ) ;
#19951 = AXIS2_PLACEMENT_3D ( 'NONE', #18756, #33283, #82350 ) ;
#19952 = DIRECTION ( 'NONE',  ( 1.000000000000000000, 0.000000000000000000, -5.551115123125780853E-17 ) ) ;
#19953 = EDGE_CURVE ( 'NONE', #2949, #36750, #58893, .T. ) ;
#19954 = ORIENTED_EDGE ( 'NONE', *, *, #41078, .F. ) ;
#19955 = EDGE_CURVE ( 'NONE', #16565, #83000, #18463, .T. ) ;
#19956 = ORIENTED_EDGE ( 'NONE', *, *, #38532, .F. ) ;
#19957 = EDGE_CURVE ( 'NONE', #88399, #5757, #60685, .T. ) ;
#19958 = ORIENTED_EDGE ( 'NONE', *, *, #46799, .T. ) ;
#19959 = FACE_OUTER_BOUND ( 'NONE', #50813, .T. ) ;
#19960 = CARTESIAN_POINT ( 'NONE',  ( 86.19179098795335392, 92.11674985319540099, -98.06216817836228472 ) ) ;
#19961 = CARTESIAN_POINT ( 'NONE',  ( 108.3334480150830501, -46.73485936483547931, 157.6772919362252310 ) ) ;
#19962 = CARTESIAN_POINT ( 'NONE',  ( 63.56670390244739366, -47.82844715994014706, 180.4678068554151196 ) ) ;
#19963 = EDGE_CURVE ( 'NONE', #18192, #64715, #44827, .T. ) ;
#19965 = DIRECTION ( 'NONE',  ( -0.9254794337955620787, -0.3787978585227822492, 0.000000000000000000 ) ) ;
#19964 = DIRECTION ( 'NONE',  ( 0.000000000000000000, 0.000000000000000000, -1.000000000000000000 ) ) ;
#19966 = CARTESIAN_POINT ( 'NONE',  ( 98.34971108053937883, -31.65683447307292298, 180.9064812817925372 ) ) ;
#19967 = AXIS2_PLACEMENT_3D ( 'NONE', #63463, #48022, #7168 ) ;
#19968 = VERTEX_POINT ( 'NONE', #52508 ) ;
#19969 = CIRCLE ( 'NONE', #11197, 2.029999999999997140 ) ;
#19970 = ORIENTED_EDGE ( 'NONE', *, *, #76468, .T. ) ;
#19971 = DIRECTION ( 'NONE',  ( 4.299999999999999979E-14, -1.000000000000000000, 0.000000000000000000 ) ) ;
#19972 = CARTESIAN_POINT ( 'NONE',  ( 97.44287158780967673, -40.59272077381804422, 247.6422919425769749 ) ) ;
#19973 = EDGE_CURVE ( 'NONE', #42178, #36122, #25281, .T. ) ;
#19975 = VERTEX_POINT ( 'NONE', #72554 ) ;
#19974 = CARTESIAN_POINT ( 'NONE',  ( 147.0667039024469886, -67.87844715994090450, 222.2178068554179902 ) ) ;
#19976 = CARTESIAN_POINT ( 'NONE',  ( 113.0229309284916184, -28.24065945027253477, 80.57753003781498080 ) ) ;
#19977 = CARTESIAN_POINT ( 'NONE',  ( 116.7486982854288726, -34.15480232083102408, 54.03335171816377169 ) ) ;
#19978 = CARTESIAN_POINT ( 'NONE',  ( 69.95705417202927379, -138.0482284146212635, 247.6588381008699855 ) ) ;
#19979 = CARTESIAN_POINT ( 'NONE',  ( 100.9539600449370766, -28.70758302638736836, 21.59398670790487884 ) ) ;
#19980 = ORIENTED_EDGE ( 'NONE', *, *, #78936, .T. ) ;
#19981 = DIRECTION ( 'NONE',  ( -4.299999999999999979E-14, 1.000000000000000000, -4.400000000000000367E-29 ) ) ;
#19982 = AXIS2_PLACEMENT_3D ( 'NONE', #28744, #47029, #61128 ) ;
#19983 = ORIENTED_EDGE ( 'NONE', *, *, #65709, .T. ) ;
#19984 = ORIENTED_EDGE ( 'NONE', *, *, #82440, .F. ) ;
#19985 = CARTESIAN_POINT ( 'NONE',  ( 100.0731593717985106, -30.45489967868845227, 232.1882499725639661 ) ) ;
#19986 = VECTOR ( 'NONE', #48517, 1000.000000000000000 ) ;
#19987 = CARTESIAN_POINT ( 'NONE',  ( 97.81452210549078075, -40.51628237377364883, 52.63520911028864901 ) ) ;
#19988 = CIRCLE ( 'NONE', #12730, 2.117000000000000881 ) ;
#19989 = CARTESIAN_POINT ( 'NONE',  ( -118.4407179355509356, 94.12556101775334128, -5.241146580996161930 ) ) ;
#19990 = CARTESIAN_POINT ( 'NONE',  ( 112.0659115654917599, -45.48839629398710827, 153.9897919373767081 ) ) ;
#19991 = CARTESIAN_POINT ( 'NONE',  ( 81.48476992305924682, -39.08750326150863685, 1.944748881527252893 ) ) ;
#19992 = VERTEX_POINT ( 'NONE', #67507 ) ;
#19993 = DIRECTION ( 'NONE',  ( -0.000000000000000000, -0.000000000000000000, 1.000000000000000000 ) ) ;
#19994 = VECTOR ( 'NONE', #14871, 1000.000000000000000 ) ;
#19995 = CARTESIAN_POINT ( 'NONE',  ( 0.000000000000000000, 101.5999999999999943, 0.000000000000000000 ) ) ;
#19996 = VERTEX_POINT ( 'NONE', #59788 ) ;
#19997 = CARTESIAN_POINT ( 'NONE',  ( 96.33825113647944249, -41.76388066030261115, 61.67562527591097421 ) ) ;
#19998 = VERTEX_POINT ( 'NONE', #52946 ) ;
#19999 = CARTESIAN_POINT ( 'NONE',  ( 114.5355946289170390, -40.02218186577253789, 251.3138046553057734 ) ) ;
#20000 = VECTOR ( 'NONE', #74658, 999.9999999999998863 ) ;
#20001 = CARTESIAN_POINT ( 'NONE',  ( 62.03715912545755629, -47.82818131006020934, 117.4678068554150485 ) ) ;
#20002 = CARTESIAN_POINT ( 'NONE',  ( 98.54774150848822956, -41.53511815344526070, 136.7356252759109623 ) ) ;
#20003 = LINE ( 'NONE', #18203, #41878 ) ;
#20004 = CARTESIAN_POINT ( 'NONE',  ( 41.56648329127398966, -27.82844715994070484, 198.9256252759119832 ) ) ;
#20005 = AXIS2_PLACEMENT_3D ( 'NONE', #48223, #89144, #33277 ) ;
#20006 = CARTESIAN_POINT ( 'NONE',  ( 50.03799999999999670, 20.32000000000000028, 191.3008000794699797 ) ) ;
#20007 = AXIS2_PLACEMENT_3D ( 'NONE', #38241, #80946, #18245 ) ;
#20008 = EDGE_CURVE ( 'NONE', #42564, #48576, #39361, .T. ) ;
#20009 = DIRECTION ( 'NONE',  ( 0.000000000000000000, -1.000000000000000000, 0.000000000000000000 ) ) ;
#20010 = CARTESIAN_POINT ( 'NONE',  ( 103.9262362324350590, -26.74286475366834281, 246.3184824187679567 ) ) ;
#20011 = CARTESIAN_POINT ( 'NONE',  ( -31.27367473141074683, 54.97499999999995879, 74.45358409497265484 ) ) ;
#20012 = CIRCLE ( 'NONE', #82394, 5.500000000000000888 ) ;
#20013 = ORIENTED_EDGE ( 'NONE', *, *, #64808, .T. ) ;
#20014 = CARTESIAN_POINT ( 'NONE',  ( 103.8278507311454177, -46.72190801433284690, 78.32705384733995402 ) ) ;
#20015 = DIRECTION ( 'NONE',  ( 1.907762142705490052E-15, 7.167082501179359715E-16, -1.000000000000000000 ) ) ;
#20016 = EDGE_CURVE ( 'NONE', #45281, #65225, #80714, .T. ) ;
#20017 = ORIENTED_EDGE ( 'NONE', *, *, #52036, .F. ) ;
#20018 = VERTEX_POINT ( 'NONE', #11668 ) ;
#20019 = ORIENTED_EDGE ( 'NONE', *, *, #5285, .F. ) ;
#20020 = DIRECTION ( 'NONE',  ( 0.000000000000000000, 0.000000000000000000, -1.000000000000000000 ) ) ;
#20021 = FACE_OUTER_BOUND ( 'NONE', #63811, .T. ) ;
#20022 = CARTESIAN_POINT ( 'NONE',  ( 0.000000000000000000, 11.98343896644750117, -160.4955849403809793 ) ) ;
#20023 = DIRECTION ( 'NONE',  ( 3.491483361109380094E-15, 0.000000000000000000, -1.000000000000000000 ) ) ;
#20024 = CARTESIAN_POINT ( 'NONE',  ( 114.8977050226898484, -39.03198754188770891, 181.4166617981629486 ) ) ;
#20025 = CARTESIAN_POINT ( 'NONE',  ( 118.1305967499472160, -36.20925573564677791, 264.8518157521014587 ) ) ;
#20026 = CARTESIAN_POINT ( 'NONE',  ( 48.79742451362098166, -36.32844715994040996, 313.9678068554150059 ) ) ;
#20027 = ORIENTED_EDGE ( 'NONE', *, *, #48704, .T. ) ;
#20028 = CARTESIAN_POINT ( 'NONE',  ( 130.3837601098275059, 93.33885111288434189, -6.713053715882820960 ) ) ;
#20029 = AXIS2_PLACEMENT_3D ( 'NONE', #41424, #21005, #83688 ) ;
#20030 = CARTESIAN_POINT ( 'NONE',  ( 21.03689327557705369, -23.42844715994186089, 313.9678068554150059 ) ) ;
#20031 = ORIENTED_EDGE ( 'NONE', *, *, #46827, .F. ) ;
#20033 = ORIENTED_EDGE ( 'NONE', *, *, #63740, .F. ) ;
#20032 = VECTOR ( 'NONE', #13365, 1000.000000000000000 ) ;
#20034 = EDGE_CURVE ( 'NONE', #35135, #23413, #38026, .T. ) ;
#20035 = DIRECTION ( 'NONE',  ( -1.000000000000000078E-15, 1.000000000000000083E-30, 1.000000000000000000 ) ) ;
#20036 = ORIENTED_EDGE ( 'NONE', *, *, #30363, .F. ) ;
#20037 = ORIENTED_EDGE ( 'NONE', *, *, #24983, .F. ) ;
#20038 = CARTESIAN_POINT ( 'NONE',  ( 67.06670390244704549, -104.2784471599409812, 234.7178068554179902 ) ) ;
#20039 = CARTESIAN_POINT ( 'NONE',  ( -4.879617406430184268, 70.80304812169737261, -130.4664555583633501 ) ) ;
#20040 = CARTESIAN_POINT ( 'NONE',  ( 90.44969454456416713, -52.08770651782494809, 218.8274735512160589 ) ) ;
#20041 = CARTESIAN_POINT ( 'NONE',  ( -50.03799999999999670, 101.5999999999999943, 178.6098374884404905 ) ) ;
#20042 = CARTESIAN_POINT ( 'NONE',  ( 104.1791519563360993, -28.66003454886012136, 189.7724198280769770 ) ) ;
#20043 = CARTESIAN_POINT ( 'NONE',  ( 110.3680388590993573, -25.29578946207851331, 64.85276813305395649 ) ) ;
#20044 = CARTESIAN_POINT ( 'NONE',  ( 107.5667039024470313, -102.2941336766436251, -19.78219314458207378 ) ) ;
#20045 = VERTEX_POINT ( 'NONE', #86631 ) ;
#20046 = CARTESIAN_POINT ( 'NONE',  ( -84.41866557162670404, 69.84937538953985836, -83.24493215373384203 ) ) ;
#20047 = ORIENTED_EDGE ( 'NONE', *, *, #85745, .T. ) ;
#20048 = CARTESIAN_POINT ( 'NONE',  ( 105.7984081882107006, -26.72418595413192577, 261.1773184477624454 ) ) ;
#20049 = VERTEX_POINT ( 'NONE', #31648 ) ;
#20050 = CARTESIAN_POINT ( 'NONE',  ( 57.14999999999999858, 69.84999999999999432, 300.8629999999999995 ) ) ;
#20051 = VECTOR ( 'NONE', #5861, 1000.000000000000000 ) ;
#20052 = FACE_OUTER_BOUND ( 'NONE', #85822, .T. ) ;
#20053 = DIRECTION ( 'NONE',  ( 1.000000000000000000, -5.337610695313248426E-16, 0.000000000000000000 ) ) ;
#20055 = DIRECTION ( 'NONE',  ( -0.7071067811865165975, -0.7071067811865784369, -7.071067811865158803E-16 ) ) ;
#20054 = VECTOR ( 'NONE', #52981, 1000.000000000000000 ) ;
#20056 = ORIENTED_EDGE ( 'NONE', *, *, #33572, .F. ) ;
#20057 = AXIS2_PLACEMENT_3D ( 'NONE', #60817, #46276, #88105 ) ;
#20058 = CARTESIAN_POINT ( 'NONE',  ( 106.6058666599951152, -25.66223100340348040, 40.09753003781596448 ) ) ;
#20060 = CARTESIAN_POINT ( 'NONE',  ( 99.08946256649485917, -109.4614598618343138, -19.78219314458184996 ) ) ;
#20059 = FACE_OUTER_BOUND ( 'NONE', #20874, .T. ) ;
#20061 = CARTESIAN_POINT ( 'NONE',  ( 107.0664832912739399, -36.72944715994095333, 302.6356252759109680 ) ) ;
#20062 = CARTESIAN_POINT ( 'NONE',  ( -4.049533659350667669, 70.61131560177412325, 118.2873649127880071 ) ) ;
#20063 = EDGE_LOOP ( 'NONE', ( #67385, #68428, #18664, #71091 ) ) ;
#20064 = EDGE_CURVE ( 'NONE', #7066, #57830, #20285, .T. ) ;
#20065 = VECTOR ( 'NONE', #3686, 1000.000000000000000 ) ;
#20066 = EDGE_CURVE ( 'NONE', #76506, #16372, #50731, .T. ) ;
#20067 = DIRECTION ( 'NONE',  ( 0.000000000000000000, 1.000000000000000000, 0.000000000000000000 ) ) ;
#20068 = ADVANCED_FACE ( 'NONE', ( #18918 ), #53405, .F. ) ;
#20069 = CIRCLE ( 'NONE', #50524, 2.124999999999998224 ) ;
#20070 = FACE_OUTER_BOUND ( 'NONE', #44945, .T. ) ;
#20071 = CARTESIAN_POINT ( 'NONE',  ( 25.56670390244797275, -65.37844715994100397, 257.2178068554150059 ) ) ;
#20072 = ORIENTED_EDGE ( 'NONE', *, *, #18424, .T. ) ;
#20073 = CARTESIAN_POINT ( 'NONE',  ( 116.6948211927369812, -32.58525784656897883, 75.14991099019697174 ) ) ;
#20074 = EDGE_CURVE ( 'NONE', #79794, #71248, #79829, .T. ) ;
#20075 = VECTOR ( 'NONE', #56270, 1000.000000000000000 ) ;
#20076 = AXIS2_PLACEMENT_3D ( 'NONE', #68539, #34000, #7210 ) ;
#20078 = FACE_OUTER_BOUND ( 'NONE', #30967, .T. ) ;
#20077 = DIRECTION ( 'NONE',  ( 1.000000000000000000, 0.000000000000000000, 0.000000000000000000 ) ) ;
#20079 = FACE_OUTER_BOUND ( 'NONE', #65388, .T. ) ;
#20080 = CARTESIAN_POINT ( 'NONE',  ( 131.3179999999999836, 53.97500000000000142, 50.79999999999999716 ) ) ;
#20081 = ORIENTED_EDGE ( 'NONE', *, *, #18529, .F. ) ;
#20082 = CARTESIAN_POINT ( 'NONE',  ( 103.2241971045484519, -45.72390501747104707, 88.25562527591095829 ) ) ;
#20083 = EDGE_CURVE ( 'NONE', #66137, #71741, #45700, .T. ) ;
#20084 = CIRCLE ( 'NONE', #57744, 3.000000000000002665 ) ;
#20086 = VERTEX_POINT ( 'NONE', #51637 ) ;
#20085 = CARTESIAN_POINT ( 'NONE',  ( 7.037613089623343754, 93.12175551049465128, 130.3661809698470506 ) ) ;
#20087 = CARTESIAN_POINT ( 'NONE',  ( 105.0259480979001552, -25.88970440745778134, 276.2365776568634033 ) ) ;
#20088 = DIRECTION ( 'NONE',  ( 0.000000000000000000, 0.000000000000000000, -1.000000000000000000 ) ) ;
#20089 = DIRECTION ( 'NONE',  ( 1.000000000000000078E-15, -1.000000000000000083E-30, -1.000000000000000000 ) ) ;
#20090 = EDGE_CURVE ( 'NONE', #29287, #6713, #15943, .T. ) ;
#20091 = FACE_OUTER_BOUND ( 'NONE', #427, .T. ) ;
#20092 = CARTESIAN_POINT ( 'NONE',  ( 74.19170390244705970, -127.9034471599409812, 45.21780685541799727 ) ) ;
#20093 = DIRECTION ( 'NONE',  ( -0.000000000000000000, 1.000000000000000000, -0.000000000000000000 ) ) ;
#20094 = CARTESIAN_POINT ( 'NONE',  ( 177.0371591254545933, -48.62818131005479927, 129.9678068554150059 ) ) ;
#20095 = CARTESIAN_POINT ( 'NONE',  ( 99.76930146980365066, -30.21680002102808515, 190.7470538473399415 ) ) ;
#20096 = AXIS2_PLACEMENT_3D ( 'NONE', #83580, #63119, #7273 ) ;
#20097 = VERTEX_POINT ( 'NONE', #72984 ) ;
#20098 = ORIENTED_EDGE ( 'NONE', *, *, #64665, .F. ) ;
#20099 = CARTESIAN_POINT ( 'NONE',  ( 112.8895349442155265, -29.35594087158844445, 120.9882499725639633 ) ) ;
#20100 = DIRECTION ( 'NONE',  ( -4.012088370409549976E-14, 1.000000000000000000, 0.000000000000000000 ) ) ;
#20102 = CARTESIAN_POINT ( 'NONE',  ( 182.0374245136174522, -23.42844715993458848, 117.4678068554150627 ) ) ;
#20101 = CARTESIAN_POINT ( 'NONE',  ( 100.6696166679599713, -29.33055989933774299, 256.6441967044817147 ) ) ;
#20103 = FACE_OUTER_BOUND ( 'NONE', #5516, .T. ) ;
#20104 = CYLINDRICAL_SURFACE ( 'NONE', #56225, 9.999999999999998224 ) ;
#20105 = CARTESIAN_POINT ( 'NONE',  ( 0.000000000000000000, 101.5999999999999943, 0.000000000000000000 ) ) ;
#20106 = CARTESIAN_POINT ( 'NONE',  ( 97.31584371825169910, -39.30597600789160140, 107.5314586099498229 ) ) ;
#20107 = DIRECTION ( 'NONE',  ( 0.000000000000000000, 0.000000000000000000, 1.000000000000000000 ) ) ;
#20108 = CARTESIAN_POINT ( 'NONE',  ( 96.06973772670281164, -35.87188691900273341, 191.2765776568629690 ) ) ;
#20109 = FACE_BOUND ( 'NONE', #18625, .T. ) ;
#20110 = ORIENTED_EDGE ( 'NONE', *, *, #11891, .F. ) ;
#20111 = VERTEX_POINT ( 'NONE', #59348 ) ;
#20112 = VECTOR ( 'NONE', #17588, 999.9999999999998863 ) ;
#20113 = DIRECTION ( 'NONE',  ( 0.000000000000000000, 0.000000000000000000, 1.000000000000000000 ) ) ;
#20114 = CARTESIAN_POINT ( 'NONE',  ( 77.52387074034942316, -17.68172011937453192, 2.822018711114674172 ) ) ;
#20115 = CARTESIAN_POINT ( 'NONE',  ( 117.0612157011691750, -38.07822042050563027, 124.7180529556605109 ) ) ;
#20116 = CARTESIAN_POINT ( 'NONE',  ( -47.02966122971776031, 65.60000000000000853, 108.8289304395572401 ) ) ;
#20117 = EDGE_CURVE ( 'NONE', #86172, #49620, #11590, .T. ) ;
#20119 = LINE ( 'NONE', #12863, #84796 ) ;
#20118 = AXIS2_PLACEMENT_3D ( 'NONE', #10907, #79979, #52656 ) ;
#20120 = VECTOR ( 'NONE', #67807, 1000.000000000000114 ) ;
#20121 = ORIENTED_EDGE ( 'NONE', *, *, #46752, .F. ) ;
#20122 = CARTESIAN_POINT ( 'NONE',  ( -11.79654564977231779, 86.99658319087748737, 117.7667590573388026 ) ) ;
#20123 = ADVANCED_FACE ( 'NONE', ( #27964 ), #69763, .T. ) ;
#20124 = CARTESIAN_POINT ( 'NONE',  ( 98.89873792621239090, -29.28182854020744230, 230.7261014663869503 ) ) ;
#20125 = ORIENTED_EDGE ( 'NONE', *, *, #37660, .F. ) ;
#20126 = AXIS2_PLACEMENT_3D ( 'NONE', #21343, #28594, #36318 ) ;
#20127 = CARTESIAN_POINT ( 'NONE',  ( 0.000000000000000000, 101.5999999999999943, 0.000000000000000000 ) ) ;
#20128 = CARTESIAN_POINT ( 'NONE',  ( 177.8371591254542921, -47.82818131005477369, 313.9678068554149490 ) ) ;
#20129 = CARTESIAN_POINT ( 'NONE',  ( 110.8799455303576593, -45.97378286453075447, 167.8878162705527188 ) ) ;
#20130 = CARTESIAN_POINT ( 'NONE',  ( 99.15069935661746570, -33.23069170325895527, 53.80142370292495713 ) ) ;
#20132 = CARTESIAN_POINT ( 'NONE',  ( 97.36185206511996171, -42.06848625969246314, 172.7146728949589942 ) ) ;
#20131 = AXIS2_PLACEMENT_3D ( 'NONE', #29938, #16746, #58071 ) ;
#20133 = DIRECTION ( 'NONE',  ( 0.7071067811865344721, 0.000000000000000000, -0.7071067811865604513 ) ) ;
#20134 = ORIENTED_EDGE ( 'NONE', *, *, #69676, .F. ) ;
#20135 = AXIS2_PLACEMENT_3D ( 'NONE', #55215, #33898, #48396 ) ;
#20136 = DIRECTION ( 'NONE',  ( -0.000000000000000000, -0.000000000000000000, -1.000000000000000000 ) ) ;
#20137 = CARTESIAN_POINT ( 'NONE',  ( 97.87203513630441876, -40.66183252246401025, 66.64857268046317529 ) ) ;
#20138 = ORIENTED_EDGE ( 'NONE', *, *, #16541, .F. ) ;
#20139 = ORIENTED_EDGE ( 'NONE', *, *, #11129, .F. ) ;
#20140 = EDGE_CURVE ( 'NONE', #85724, #78112, #13452, .T. ) ;
#20141 = CARTESIAN_POINT ( 'NONE',  ( 107.0664832912739968, -18.82844715994099971, 168.9256252759119832 ) ) ;
#20142 = ORIENTED_EDGE ( 'NONE', *, *, #36386, .T. ) ;
#20143 = VERTEX_POINT ( 'NONE', #76577 ) ;
#20144 = FACE_OUTER_BOUND ( 'NONE', #64502, .T. ) ;
#20145 = CIRCLE ( 'NONE', #28840, 5.599999999999994316 ) ;
#20146 = CARTESIAN_POINT ( 'NONE',  ( 109.8440526342893975, -45.34906309516006928, 57.25908649474392575 ) ) ;
#20147 = CARTESIAN_POINT ( 'NONE',  ( 116.5468340722667051, -41.20284764396129873, 228.4756252759109714 ) ) ;
#20148 = CARTESIAN_POINT ( 'NONE',  ( 118.7655994573051714, -38.45539276985795851, 223.7099109901969598 ) ) ;
#20150 = CARTESIAN_POINT ( 'NONE',  ( 109.6066175024219831, -25.17973177368044801, 25.90419670448196143 ) ) ;
#20149 = LINE ( 'NONE', #81050, #65000 ) ;
#20151 = DIRECTION ( 'NONE',  ( 0.000000000000000000, 0.000000000000000000, 1.000000000000000000 ) ) ;
#20152 = CARTESIAN_POINT ( 'NONE',  ( 97.81169266289590780, -40.51741659614882707, 92.63571255866972365 ) ) ;
#20153 = EDGE_CURVE ( 'NONE', #81352, #88467, #41580, .T. ) ;
#20154 = ORIENTED_EDGE ( 'NONE', *, *, #76976, .F. ) ;
#20155 = VERTEX_POINT ( 'NONE', #48384 ) ;
#20156 = VECTOR ( 'NONE', #56938, 1000.000000000000000 ) ;
#20157 = CARTESIAN_POINT ( 'NONE',  ( 112.4472966703649348, -46.45872411559678028, 102.9784824187679817 ) ) ;
#20158 = CARTESIAN_POINT ( 'NONE',  ( 98.61163144626758026, -43.92169047526947168, 76.89943479971999807 ) ) ;
#20159 = CARTESIAN_POINT ( 'NONE',  ( 96.20350199017366322, -34.44722874799195722, 261.1737205140063338 ) ) ;
#20160 = VERTEX_POINT ( 'NONE', #7088 ) ;
#20161 = CARTESIAN_POINT ( 'NONE',  ( 100.7500417190893245, -45.80037066963202363, 237.0803871806729717 ) ) ;
#20162 = CARTESIAN_POINT ( 'NONE',  ( 105.7995184340200581, -26.72403497198984113, 35.17729194683857941 ) ) ;
#20163 = CARTESIAN_POINT ( 'NONE',  ( 75.25757238336811383, -1.944390235229870978, 394.9756252759101471 ) ) ;
#20164 = EDGE_CURVE ( 'NONE', #21258, #6226, #63788, .T. ) ;
#20165 = DIRECTION ( 'NONE',  ( 0.9963424814100680926, -0.08544974978095698503, 0.000000000000000000 ) ) ;
#20166 = CARTESIAN_POINT ( 'NONE',  ( 51.34673845256460112, -29.62846900982267329, 193.9678068554150911 ) ) ;
#20168 = FACE_OUTER_BOUND ( 'NONE', #81385, .T. ) ;
#20167 = CARTESIAN_POINT ( 'NONE',  ( 114.3906737664497371, -40.90796621566182267, 277.6356252759109111 ) ) ;
#20169 = CARTESIAN_POINT ( 'NONE',  ( 98.15085007322062438, -41.26136264609154125, 172.7007008575214400 ) ) ;
#20170 = DIRECTION ( 'NONE',  ( 0.0001713722456127401463, -0.9999999853157766072, -1.713722456137401502E-19 ) ) ;
#20171 = CARTESIAN_POINT ( 'NONE',  ( 11.00058663074870324, 88.91008943578141555, -118.0447001808843766 ) ) ;
#20172 = CARTESIAN_POINT ( 'NONE',  ( 87.06648329127403940, -46.72944715994105280, -5.074374724089050659 ) ) ;
#20173 = DIRECTION ( 'NONE',  ( 0.000000000000000000, -1.000000000000000000, 0.000000000000000000 ) ) ;
#20174 = EDGE_CURVE ( 'NONE', #31769, #76607, #36218, .T. ) ;
#20175 = FACE_OUTER_BOUND ( 'NONE', #49723, .T. ) ;
#20177 = ORIENTED_EDGE ( 'NONE', *, *, #68762, .T. ) ;
#20176 = LINE ( 'NONE', #56460, #50083 ) ;
#20178 = VECTOR ( 'NONE', #48729, 1000.000000000000114 ) ;
#20179 = CARTESIAN_POINT ( 'NONE',  ( 78.13314995793999174, 12.92155284005730387, 355.9756252759109998 ) ) ;
#20180 = CARTESIAN_POINT ( 'NONE',  ( 115.5353962700893788, -29.58991257470437120, 224.3718157521009573 ) ) ;
#20181 = CARTESIAN_POINT ( 'NONE',  ( 112.1200623320449097, -47.44840020502576294, 133.9270538473399768 ) ) ;
#20182 = CARTESIAN_POINT ( 'NONE',  ( 116.5760347145385367, -42.45360038892302157, 274.3832443235299365 ) ) ;
#20183 = CARTESIAN_POINT ( 'NONE',  ( 115.0889047303822110, -30.61763668965400598, 154.3439586083368624 ) ) ;
#20184 = DIRECTION ( 'NONE',  ( 0.7071067811865165975, 0.7071067811865784369, 7.071067811865158803E-16 ) ) ;
#20186 = CARTESIAN_POINT ( 'NONE',  ( 89.06648138392549185, -56.72944715994095333, -4.970821333495735850 ) ) ;
#20185 = DIRECTION ( 'NONE',  ( 0.000000000000000000, 0.000000000000000000, 1.000000000000000000 ) ) ;
#20187 = CARTESIAN_POINT ( 'NONE',  ( 107.0664832912739968, -36.72944715994100306, 292.6356252759106837 ) ) ;
#20188 = FACE_OUTER_BOUND ( 'NONE', #75179, .T. ) ;
#20189 = VECTOR ( 'NONE', #69812, 1000.000000000000227 ) ;
#20190 = VECTOR ( 'NONE', #27046, 1000.000000000000000 ) ;
#20191 = ORIENTED_EDGE ( 'NONE', *, *, #31926, .F. ) ;
#20192 = VERTEX_POINT ( 'NONE', #13898 ) ;
#20193 = CARTESIAN_POINT ( 'NONE',  ( 99.50386058399449496, -32.75919911893461034, 135.3638483995049739 ) ) ;
#20194 = EDGE_CURVE ( 'NONE', #4612, #68436, #76118, .T. ) ;
#20195 = VECTOR ( 'NONE', #40890, 1000.000000000000000 ) ;
#20197 = ORIENTED_EDGE ( 'NONE', *, *, #73394, .F. ) ;
#20196 = CARTESIAN_POINT ( 'NONE',  ( 23.12708505997960629, 51.75119301488568624, 30.27798919810780731 ) ) ;
#20198 = DIRECTION ( 'NONE',  ( 0.000000000000000000, 0.000000000000000000, -1.000000000000000000 ) ) ;
#20199 = CARTESIAN_POINT ( 'NONE',  ( 104.5678333644584228, -48.28820816006142991, 178.4070538473399665 ) ) ;
#20200 = CARTESIAN_POINT ( 'NONE',  ( 70.14948329127297200, -71.52944715994141234, 361.9756252759109998 ) ) ;
#20201 = EDGE_CURVE ( 'NONE', #40235, #24929, #83394, .T. ) ;
#20202 = EDGE_CURVE ( 'NONE', #78334, #73595, #73949, .T. ) ;
#20203 = DIRECTION ( 'NONE',  ( -0.4634479843259246556, -0.000000000000000000, -0.8861241255175470455 ) ) ;
#20204 = CARTESIAN_POINT ( 'NONE',  ( -86.94609723791337785, 70.66242608954387094, 80.59807192910960794 ) ) ;
#20205 = CARTESIAN_POINT ( 'NONE',  ( 45.77381068350418758, -48.62134037888111493, 180.4678068554150911 ) ) ;
#20206 = EDGE_CURVE ( 'NONE', #83591, #36007, #42036, .T. ) ;
#20207 = CARTESIAN_POINT ( 'NONE',  ( 113.9027609268606369, -43.72435554967460547, 73.19276813305496887 ) ) ;
#20208 = ORIENTED_EDGE ( 'NONE', *, *, #62208, .F. ) ;
#20209 = ORIENTED_EDGE ( 'NONE', *, *, #50469, .T. ) ;
#20210 = EDGE_LOOP ( 'NONE', ( #6499, #58419, #3758, #47021 ) ) ;
#20211 = DIRECTION ( 'NONE',  ( -6.524622321627019585E-16, -4.013151879589939944E-16, -1.000000000000000000 ) ) ;
#20213 = DIRECTION ( 'NONE',  ( 0.000000000000000000, 1.000000000000000000, 0.000000000000000000 ) ) ;
#20212 = CARTESIAN_POINT ( 'NONE',  ( 116.5042510202518571, -34.04512512578506289, 145.0470538473389581 ) ) ;
#20214 = CARTESIAN_POINT ( 'NONE',  ( 116.3183049785035195, -32.94379174720932468, 54.13562527591098217 ) ) ;
#20215 = FACE_OUTER_BOUND ( 'NONE', #71868, .T. ) ;
#20216 = AXIS2_PLACEMENT_3D ( 'NONE', #24508, #38566, #31754 ) ;
#20217 = CARTESIAN_POINT ( 'NONE',  ( 0.000000000000000000, 0.000000000000000000, 0.000000000000000000 ) ) ;
#20218 = CARTESIAN_POINT ( 'NONE',  ( 85.84941893669208923, 94.92435932957491218, 81.76533775135520443 ) ) ;
#20219 = DIRECTION ( 'NONE',  ( -1.000000000000000000, -1.181088324069315053E-15, 0.000000000000000000 ) ) ;
#20220 = CARTESIAN_POINT ( 'NONE',  ( 113.4020503763144632, -27.70036014686454351, 84.57753003781698453 ) ) ;
#20221 = VERTEX_POINT ( 'NONE', #26184 ) ;
#20222 = ORIENTED_EDGE ( 'NONE', *, *, #15398, .F. ) ;
#20223 = ORIENTED_EDGE ( 'NONE', *, *, #49169, .T. ) ;
#20224 = LINE ( 'NONE', #34734, #54574 ) ;
#20225 = CARTESIAN_POINT ( 'NONE',  ( -93.48397507443814902, 95.16896684734908263, -91.13883569058478429 ) ) ;
#20226 = CARTESIAN_POINT ( 'NONE',  ( 162.7131505118539962, -33.70561438052090608, 117.4678068554150627 ) ) ;
#20227 = CARTESIAN_POINT ( 'NONE',  ( 109.0547627366692041, -28.78404389176943212, 197.6995189410199600 ) ) ;
#20228 = VECTOR ( 'NONE', #68808, 1000.000000000000000 ) ;
#20229 = DIRECTION ( 'NONE',  ( -1.000000000000000000, -1.541976423090496028E-15, 0.000000000000000000 ) ) ;
#20230 = ORIENTED_EDGE ( 'NONE', *, *, #37098, .F. ) ;
#20232 = EDGE_LOOP ( 'NONE', ( #79898, #61902 ) ) ;
#20231 = ORIENTED_EDGE ( 'NONE', *, *, #56043, .T. ) ;
#20233 = CARTESIAN_POINT ( 'NONE',  ( 143.0664832912740110, -8.729447159940999512, 284.9256252759119548 ) ) ;
#20234 = CARTESIAN_POINT ( 'NONE',  ( 135.2499137886320284, -21.21189172703428483, 1.845048092482432400 ) ) ;
#20235 = ORIENTED_EDGE ( 'NONE', *, *, #5558, .F. ) ;
#20236 = VERTEX_POINT ( 'NONE', #53852 ) ;
#20237 = DIRECTION ( 'NONE',  ( 0.000000000000000000, 0.000000000000000000, -1.000000000000000000 ) ) ;
#20238 = CARTESIAN_POINT ( 'NONE',  ( 115.9133815579708937, -36.21888896485111076, 225.3044404487539794 ) ) ;
#20239 = AXIS2_PLACEMENT_3D ( 'NONE', #7771, #13683, #41373 ) ;
#20240 = ORIENTED_EDGE ( 'NONE', *, *, #50407, .T. ) ;
#20241 = CARTESIAN_POINT ( 'NONE',  ( 0.000000000000000000, 125.7300000000000040, 0.000000000000000000 ) ) ;
#20242 = CARTESIAN_POINT ( 'NONE',  ( -115.0751651833283233, 71.53075230113380201, 61.66802841283988101 ) ) ;
#20243 = AXIS2_PLACEMENT_3D ( 'NONE', #37961, #45205, #23019 ) ;
#20244 = ORIENTED_EDGE ( 'NONE', *, *, #739, .F. ) ;
#20246 = ORIENTED_EDGE ( 'NONE', *, *, #32952, .T. ) ;
#20245 = VECTOR ( 'NONE', #79686, 1000.000000000000000 ) ;
#20247 = ADVANCED_FACE ( 'NONE', ( #81621 ), #13011, .T. ) ;
#20248 = DIRECTION ( 'NONE',  ( 0.9825752044328148749, 0.1858654557302456822, 0.000000000000000000 ) ) ;
#20249 = ORIENTED_EDGE ( 'NONE', *, *, #4650, .F. ) ;
#20250 = ORIENTED_EDGE ( 'NONE', *, *, #75210, .T. ) ;
#20251 = EDGE_CURVE ( 'NONE', #44627, #3441, #68421, .T. ) ;
#20252 = CARTESIAN_POINT ( 'NONE',  ( 107.2095755159442376, -27.45176125347251173, 227.8823760838769488 ) ) ;
#20254 = EDGE_CURVE ( 'NONE', #63483, #21337, #89770, .T. ) ;
#20253 = AXIS2_PLACEMENT_3D ( 'NONE', #24262, #39220, #4260 ) ;
#20255 = CARTESIAN_POINT ( 'NONE',  ( 113.3446846601215441, -45.07992904040708737, 143.0899109901969553 ) ) ;
#20256 = CARTESIAN_POINT ( 'NONE',  ( 104.2200364793041274, -25.25138339198301907, 90.26991099019693365 ) ) ;
#20257 = CARTESIAN_POINT ( 'NONE',  ( 102.9521648518240085, -29.48031188516382528, 249.5838068554170661 ) ) ;
#20258 = DIRECTION ( 'NONE',  ( 0.000000000000000000, 0.000000000000000000, -1.000000000000000000 ) ) ;
#20259 = COLOUR_RGB ( '', 0.72549020, 0.75294118, 0.79215686) ;
#20260 = CARTESIAN_POINT ( 'NONE',  ( 117.1971262914088499, -34.26925207598063849, 205.0156252759109634 ) ) ;
#20261 = CARTESIAN_POINT ( 'NONE',  ( -50.03799999999999670, 20.32000000000000028, 191.3008000794699797 ) ) ;
#20262 = VERTEX_POINT ( 'NONE', #6197 ) ;
#20263 = CARTESIAN_POINT ( 'NONE',  ( 116.3212776292296127, -32.94146857471318413, 287.6356252759109680 ) ) ;
#20265 = ORIENTED_EDGE ( 'NONE', *, *, #51821, .F. ) ;
#20264 = EDGE_CURVE ( 'NONE', #69134, #34414, #19818, .T. ) ;
#20266 = EDGE_CURVE ( 'NONE', #28847, #44183, #56485, .T. ) ;
#20267 = ORIENTED_EDGE ( 'NONE', *, *, #22458, .F. ) ;
#20268 = CARTESIAN_POINT ( 'NONE',  ( 50.03799999999999670, 20.32000000000000028, 178.6098374884404905 ) ) ;
#20269 = EDGE_LOOP ( 'NONE', ( #26210, #64600, #59087, #87899 ) ) ;
#20270 = EDGE_CURVE ( 'NONE', #56526, #13876, #65344, .T. ) ;
#20271 = EDGE_CURVE ( 'NONE', #6343, #5474, #29330, .T. ) ;
#20272 = CARTESIAN_POINT ( 'NONE',  ( 152.0371591254583450, -47.82818131005588214, 237.4678068554150059 ) ) ;
#20273 = AXIS2_PLACEMENT_3D ( 'NONE', #74591, #87779, #11018 ) ;
#20274 = CARTESIAN_POINT ( 'NONE',  ( 100.2985985360463843, -46.45756217656626319, 87.09276813305393716 ) ) ;
#20275 = CARTESIAN_POINT ( 'NONE',  ( -10.38944306109878646, 75.24551383372960345, 130.1420047866670870 ) ) ;
#20276 = ADVANCED_FACE ( 'NONE', ( #709 ), #70208, .T. ) ;
#20277 = CARTESIAN_POINT ( 'NONE',  ( 99.08946256649487339, -99.09543445804918349, 2.217806855417836509 ) ) ;
#20278 = LINE ( 'NONE', #76119, #84801 ) ;
#20281 = CARTESIAN_POINT ( 'NONE',  ( 117.3910620576582318, -35.19077923515893502, 214.9441967044829767 ) ) ;
#20280 = CARTESIAN_POINT ( 'NONE',  ( 80.06648329127402519, -36.72944715994107412, -5.074374724089057764 ) ) ;
#20279 = CARTESIAN_POINT ( 'NONE',  ( -179.6544565346565037, 101.5999999999999943, -9.200237383489920262 ) ) ;
#20282 = CARTESIAN_POINT ( 'NONE',  ( 37.03715912545425937, -48.62818131006122258, 313.9678068554150059 ) ) ;
#20283 = DIRECTION ( 'NONE',  ( 1.000000000000000078E-15, -1.000000000000000000, 0.000000000000000000 ) ) ;
#20284 = ORIENTED_EDGE ( 'NONE', *, *, #4986, .F. ) ;
#20285 = CIRCLE ( 'NONE', #37648, 2.124999999999994227 ) ;
#20286 = CARTESIAN_POINT ( 'NONE',  ( -55.11501535285000131, 20.32000000000000028, 183.9403141659174992 ) ) ;
#20287 = EDGE_CURVE ( 'NONE', #79701, #47173, #27589, .T. ) ;
#20288 = DIRECTION ( 'NONE',  ( 0.000000000000000000, 0.000000000000000000, 1.000000000000000000 ) ) ;
#20289 = CARTESIAN_POINT ( 'NONE',  ( 47.62500000000000000, 66.67499999999999716, 257.1750000000000114 ) ) ;
#20290 = EDGE_CURVE ( 'NONE', #89556, #58657, #16002, .T. ) ;
#20291 = DIRECTION ( 'NONE',  ( 8.673617379884035472E-16, 1.000000000000000000, 0.000000000000000000 ) ) ;
#20293 = ORIENTED_EDGE ( 'NONE', *, *, #8281, .T. ) ;
#20292 = CARTESIAN_POINT ( 'NONE',  ( 98.90817802506259682, -30.16829472858045591, 240.7870538473399620 ) ) ;
#20294 = DIRECTION ( 'NONE',  ( 0.000000000000000000, 1.000000000000000000, 0.000000000000000000 ) ) ;
#20295 = CARTESIAN_POINT ( 'NONE',  ( 113.8578909311569305, -28.74413913138208088, 139.5156252759109634 ) ) ;
#20296 = CARTESIAN_POINT ( 'NONE',  ( 118.7325469213664633, -34.64676260937859098, 44.96705384733895272 ) ) ;
#20297 = CARTESIAN_POINT ( 'NONE',  ( 108.8562982717690062, -47.04397778784520057, 163.7127681330539701 ) ) ;
#20298 = DIRECTION ( 'NONE',  ( 0.000000000000000000, 0.000000000000000000, -1.000000000000000000 ) ) ;
#20299 = CARTESIAN_POINT ( 'NONE',  ( 97.80977320450685397, -40.51274266863887874, 102.6352229270316627 ) ) ;
#20301 = CARTESIAN_POINT ( 'NONE',  ( 172.5664832912729878, -27.57844715994070484, 198.9256252759119832 ) ) ;
#20300 = DIRECTION ( 'NONE',  ( -1.000000000000000000, 0.000000000000000000, 0.000000000000000000 ) ) ;
#20302 = LINE ( 'NONE', #47971, #53886 ) ;
#20303 = LINE ( 'NONE', #88896, #56702 ) ;
#20304 = ORIENTED_EDGE ( 'NONE', *, *, #47223, .T. ) ;
#20305 = EDGE_LOOP ( 'NONE', ( #9869, #66279, #85436, #87470 ) ) ;
#20306 = ORIENTED_EDGE ( 'NONE', *, *, #22653, .T. ) ;
#20307 = AXIS2_PLACEMENT_3D ( 'NONE', #86027, #65992, #57850 ) ;
#20308 = EDGE_CURVE ( 'NONE', #53776, #19, #36134, .T. ) ;
#20309 = ORIENTED_EDGE ( 'NONE', *, *, #63000, .F. ) ;
#20310 = FACE_OUTER_BOUND ( 'NONE', #22832, .T. ) ;
#20311 = CARTESIAN_POINT ( 'NONE',  ( 97.09625384711495144, -33.75906160244647936, 27.09562527591097236 ) ) ;
#20312 = CARTESIAN_POINT ( 'NONE',  ( -487.2989999999999782, 7.143750000000280487, 15.23694598552305024 ) ) ;
#20313 = ADVANCED_FACE ( 'NONE', ( #7978 ), #56100, .F. ) ;
#20314 = EDGE_CURVE ( 'NONE', #69306, #36268, #43825, .T. ) ;
#20316 = CARTESIAN_POINT ( 'NONE',  ( 116.6941949105806060, -33.85593710834429260, 119.0581585122466635 ) ) ;
#20315 = VECTOR ( 'NONE', #32443, 1000.000000000000000 ) ;
#20318 = EDGE_CURVE ( 'NONE', #10839, #46235, #20340, .T. ) ;
#20317 = CARTESIAN_POINT ( 'NONE',  ( 141.3509999999999991, 20.32000000000000028, 141.3509999999999991 ) ) ;
#20319 = CARTESIAN_POINT ( 'NONE',  ( 111.4459538621439805, -44.65616828817710626, 252.3886103042673028 ) ) ;
#20320 = ORIENTED_EDGE ( 'NONE', *, *, #5379, .F. ) ;
#20321 = VERTEX_POINT ( 'NONE', #64734 ) ;
#20323 = EDGE_LOOP ( 'NONE', ( #56591, #7381, #48830, #14786 ) ) ;
#20322 = AXIS2_PLACEMENT_3D ( 'NONE', #13116, #13550, #32641 ) ;
#20324 = CARTESIAN_POINT ( 'NONE',  ( 46.48091746482135278, -49.32844715994084339, 249.9678068554150343 ) ) ;
#20325 = PLANE ( 'NONE',  #12929 ) ;
#20326 = DIRECTION ( 'NONE',  ( 0.000000000000000000, 0.000000000000000000, 1.000000000000000000 ) ) ;
#20327 = CARTESIAN_POINT ( 'NONE',  ( 97.81252181335722184, -40.51708140359354360, 276.6353344664656220 ) ) ;
#20328 = CARTESIAN_POINT ( 'NONE',  ( 37.06648329127298780, 12.92155284005730387, 355.9756252759109998 ) ) ;
#20329 = PLANE ( 'NONE',  #57486 ) ;
#20330 = VECTOR ( 'NONE', #32389, 1000.000000000000000 ) ;
#20331 = CARTESIAN_POINT ( 'NONE',  ( 0.000000000000000000, 67.86880000000000734, 259.9944000000000415 ) ) ;
#20332 = CARTESIAN_POINT ( 'NONE',  ( 112.1541913332956710, -45.76570811864968391, 257.9965776568639626 ) ) ;
#20333 = FACE_OUTER_BOUND ( 'NONE', #18148, .T. ) ;
#20334 = VERTEX_POINT ( 'NONE', #83848 ) ;
#20335 = DIRECTION ( 'NONE',  ( 0.000000000000000000, 0.000000000000000000, 1.000000000000000000 ) ) ;
#20336 = CONICAL_SURFACE ( 'NONE', #59469, 14.49999999999997158, 0.7853981633974743692 ) ;
#20337 = CARTESIAN_POINT ( 'NONE',  ( 34.96670390244699433, -28.27351298637401200, -5.074374724088000832 ) ) ;
#20338 = CARTESIAN_POINT ( 'NONE',  ( 115.6288848908637732, -37.98889302744424867, 71.54047132197199232 ) ) ;
#20339 = CYLINDRICAL_SURFACE ( 'NONE', #15131, 7.937500000000000000 ) ;
#20340 = CIRCLE ( 'NONE', #85652, 130.5560000000000116 ) ;
#20341 = LINE ( 'NONE', #41644, #47387 ) ;
#20342 = EDGE_LOOP ( 'NONE', ( #63834, #25274, #83668, #29038 ) ) ;
#20343 = FACE_OUTER_BOUND ( 'NONE', #62895, .T. ) ;
#20344 = ORIENTED_EDGE ( 'NONE', *, *, #67949, .F. ) ;
#20345 = CARTESIAN_POINT ( 'NONE',  ( 101.9719236373881444, -46.53885842731235556, 167.1832443235299763 ) ) ;
#20346 = VERTEX_POINT ( 'NONE', #16150 ) ;
#20347 = CARTESIAN_POINT ( 'NONE',  ( 145.2378574334098005, -69.54310811732223385, 247.4968681563179871 ) ) ;
#20348 = CARTESIAN_POINT ( 'NONE',  ( 99.74964917879287896, -31.73022550229359595, 117.2815833058969446 ) ) ;
#20349 = CARTESIAN_POINT ( 'NONE',  ( 130.3998166246059895, 12.92155284005730387, 361.9756252759109998 ) ) ;
#20350 = DIRECTION ( 'NONE',  ( 0.000000000000000000, 0.000000000000000000, 1.000000000000000000 ) ) ;
#20351 = CARTESIAN_POINT ( 'NONE',  ( 110.3788355960759162, -47.29890920647816444, 48.80610146638797175 ) ) ;
#20352 = CARTESIAN_POINT ( 'NONE',  ( 116.7951252697354363, -39.38782979697960940, 84.61479194201683640 ) ) ;
#20353 = EDGE_LOOP ( 'NONE', ( #35288, #87052, #24323, #67711 ) ) ;
#20354 = CARTESIAN_POINT ( 'NONE',  ( -72.96458098368600531, 127.0000000000000000, -78.00648098368779415 ) ) ;
#20355 = VERTEX_POINT ( 'NONE', #57910 ) ;
#20357 = EDGE_CURVE ( 'NONE', #3053, #36009, #10156, .T. ) ;
#20356 = ORIENTED_EDGE ( 'NONE', *, *, #77000, .T. ) ;
#20358 = EDGE_CURVE ( 'NONE', #54044, #71630, #44267, .T. ) ;
#20359 = VECTOR ( 'NONE', #39419, 1000.000000000000000 ) ;
#20360 = ADVANCED_FACE ( 'NONE', ( #52833 ), #58356, .T. ) ;
#20361 = CARTESIAN_POINT ( 'NONE',  ( 148.0533267522749838, 101.5999999999999943, -160.2664750769289697 ) ) ;
#20362 = ORIENTED_EDGE ( 'NONE', *, *, #56626, .F. ) ;
#20363 = CARTESIAN_POINT ( 'NONE',  ( 114.1395267584829867, -29.97404255306813781, 234.4327681330549638 ) ) ;
#20364 = CARTESIAN_POINT ( 'NONE',  ( 118.9423443782970082, -36.92851767163586629, 149.8127681330539644 ) ) ;
#20365 = CARTESIAN_POINT ( 'NONE',  ( 94.58945128933383728, -41.88441296220994303, 290.1356252759106837 ) ) ;
#20366 = CARTESIAN_POINT ( 'NONE',  ( 115.0354244594187065, -42.91078753811923718, 129.3020580932306416 ) ) ;
#20367 = CARTESIAN_POINT ( 'NONE',  ( 116.6747397658760832, -32.59390121112949856, 75.14991099019697174 ) ) ;
#20368 = DIRECTION ( 'NONE',  ( -1.000000000000000078E-15, -1.000000000000000083E-30, 1.000000000000000000 ) ) ;
#20369 = VERTEX_POINT ( 'NONE', #24732 ) ;
#20370 = CARTESIAN_POINT ( 'NONE',  ( 90.06670390244703128, -104.2784471599414644, 0.2178068554180012661 ) ) ;
#20371 = AXIS2_PLACEMENT_3D ( 'NONE', #76375, #56361, #41828 ) ;
#20372 = EDGE_CURVE ( 'NONE', #76842, #15468, #44716, .T. ) ;
#20373 = CARTESIAN_POINT ( 'NONE',  ( 107.0664832912750057, -36.72944715993903486, 9.125625275910969947 ) ) ;
#20374 = VERTEX_POINT ( 'NONE', #86083 ) ;
#20375 = AXIS2_PLACEMENT_3D ( 'NONE', #1856, #78172, #84082 ) ;
#20376 = EDGE_CURVE ( 'NONE', #15300, #71038, #3401, .T. ) ;
#20377 = FACE_OUTER_BOUND ( 'NONE', #49900, .T. ) ;
#20378 = CARTESIAN_POINT ( 'NONE',  ( 86.06670390244796920, -58.72944715994110254, 250.9178068554150514 ) ) ;
#20379 = CARTESIAN_POINT ( 'NONE',  ( 112.6519946835718855, -45.50616226388166297, 263.0270538473394595 ) ) ;
#20380 = DIRECTION ( 'NONE',  ( -1.000000000000000000, 0.000000000000000000, 0.000000000000000000 ) ) ;
#20381 = EDGE_CURVE ( 'NONE', #88157, #67349, #23854, .T. ) ;
#20382 = B_SPLINE_CURVE_WITH_KNOTS ( 'NONE', 3,
 ( #18174, #9587, #31357, #78655, #57727, #64998, #52221, #65872, #10476, #79986, #87232, #37290, #3224, #17739, #73134, #10915, #2782, #38619, #66315, #4103, #59497, #52661, #80419, #45857, #73588, #11364, #2334, #30034, #61733, #26337, #82222, #20427, #13604, #11819, #74489, #26774, #74038, #19073, #40847, #53563, #13163, #88132, #54458, #68123, #25438, #67216, #4557, #66771, #19977, #81767, #12262 ),
 .UNSPECIFIED., .F., .F.,
 ( 4, 2, 1, 1, 1, 1, 1, 1, 2, 2, 2, 2, 2, 2, 2, 1, 1, 1, 1, 1, 1, 1, 2, 2, 2, 2, 2, 2, 2, 2, 2, 4 ),
 ( 0.5000150356002270868, 0.5001371022419210943, 0.5002591688836151018, 0.5005033021670026727, 0.5009915687337783696, 0.5019681018673299855, 0.5039211681344335503, 0.5078273006686406799, 0.5156395657370546060, 0.5312640958738821251, 0.5625131561475371633, 0.6250112766948475729, 0.6875093972421580935, 0.7500075177894686140, 0.7500685511103151182, 0.7501295844311617333, 0.7502516510728743926, 0.7504957843562853892, 0.7509840509230981676, 0.7519605840567150645, 0.7539136503239830533, 0.7578197828585190310, 0.7656320479275997570, 0.7812565780657612091, 0.8125056383420810047, 0.8437546986184008002, 0.8750037588947205958, 0.9062528191710403913, 0.9375018794473601869, 0.9687509397236802045, 0.9843754698618401022, 1.000000000000000000 ),
 .UNSPECIFIED. ) ;
#20383 = DIRECTION ( 'NONE',  ( -0.000000000000000000, -0.000000000000000000, -1.000000000000000000 ) ) ;
#20384 = CARTESIAN_POINT ( 'NONE',  ( 165.9667039024459996, -28.27351298637401200, -5.074374724088000832 ) ) ;
#20385 = CARTESIAN_POINT ( 'NONE',  ( 100.2135729635196242, -43.75450166755856429, 21.96133956162593748 ) ) ;
#20387 = CARTESIAN_POINT ( 'NONE',  ( 98.85726102317303798, -28.21728661942041683, 111.6870538473389587 ) ) ;
#20386 = CARTESIAN_POINT ( 'NONE',  ( 112.6101834458390556, -28.37539859851495905, 99.61086039997772446 ) ) ;
#20388 = DIRECTION ( 'NONE',  ( 0.000000000000000000, 0.000000000000000000, 1.000000000000000000 ) ) ;
#20389 = CARTESIAN_POINT ( 'NONE',  ( 113.6422709061198049, -28.58293356745306824, 164.5356252759109736 ) ) ;
#20390 = CARTESIAN_POINT ( 'NONE',  ( 6.162975822039154730E-30, 95.25000000000000000, 118.5560000000000116 ) ) ;
#20391 = VERTEX_POINT ( 'NONE', #18356 ) ;
#20392 = CIRCLE ( 'NONE', #39234, 3.250000000000002665 ) ;
#20393 = DIRECTION ( 'NONE',  ( 0.000000000000000000, 0.000000000000000000, -1.000000000000000000 ) ) ;
#20394 = CARTESIAN_POINT ( 'NONE',  ( 80.06648329127398256, -8.729447159941058132, 8.525625275910952539 ) ) ;
#20395 = FACE_OUTER_BOUND ( 'NONE', #6015, .T. ) ;
#20396 = VERTEX_POINT ( 'NONE', #65618 ) ;
#20397 = EDGE_CURVE ( 'NONE', #62972, #47787, #41, .T. ) ;
#20398 = CARTESIAN_POINT ( 'NONE',  ( 165.6738106836199904, -26.00627455219321860, 193.9678068554150059 ) ) ;
#20400 = EDGE_LOOP ( 'NONE', ( #81403, #77497 ) ) ;
#20399 = CARTESIAN_POINT ( 'NONE',  ( 102.3732866125132688, -26.67028275327534814, 135.4118157521009493 ) ) ;
#20401 = FACE_OUTER_BOUND ( 'NONE', #52084, .T. ) ;
#20402 = CARTESIAN_POINT ( 'NONE',  ( 89.37861919290365620, 70.52006616879377532, 95.16559702356724415 ) ) ;
#20403 = DIRECTION ( 'NONE',  ( 0.000000000000000000, 1.000000000000000000, 0.000000000000000000 ) ) ;
#20404 = EDGE_CURVE ( 'NONE', #81215, #3837, #46041, .T. ) ;
#20405 = FACE_OUTER_BOUND ( 'NONE', #21941, .T. ) ;
#20406 = ORIENTED_EDGE ( 'NONE', *, *, #84582, .F. ) ;
#20407 = ORIENTED_EDGE ( 'NONE', *, *, #48351, .F. ) ;
#20408 = EDGE_LOOP ( 'NONE', ( #29922, #47811 ) ) ;
#20409 = VECTOR ( 'NONE', #26995, 1000.000000000000000 ) ;
#20410 = VERTEX_POINT ( 'NONE', #52396 ) ;
#20411 = CARTESIAN_POINT ( 'NONE',  ( -78.57724105935571401, 120.6499999999999915, 67.35192090801800191 ) ) ;
#20412 = CARTESIAN_POINT ( 'NONE',  ( 93.48344774443344818, 95.14808745951977187, -91.13664476550651727 ) ) ;
#20413 = PLANE ( 'NONE',  #54131 ) ;
#20414 = EDGE_CURVE ( 'NONE', #59817, #65595, #79276, .T. ) ;
#20417 = EDGE_CURVE ( 'NONE', #22058, #89758, #80163, .T. ) ;
#20416 = FACE_OUTER_BOUND ( 'NONE', #1245, .T. ) ;
#20415 = DIRECTION ( 'NONE',  ( -0.000000000000000000, 1.000000000000000000, 0.000000000000000000 ) ) ;
#20418 = DIRECTION ( 'NONE',  ( -3.100000000000000258E-29, 3.100000000000000044E-14, 1.000000000000000000 ) ) ;
#20419 = AXIS2_PLACEMENT_3D ( 'NONE', #2688, #16314, #58083 ) ;
#20420 = EDGE_LOOP ( 'NONE', ( #7496, #73416, #27926, #55671 ) ) ;
#20421 = ORIENTED_EDGE ( 'NONE', *, *, #65032, .F. ) ;
#20422 = CARTESIAN_POINT ( 'NONE',  ( 172.5664832912728457, -27.82844715994070484, 321.9256252759120116 ) ) ;
#20423 = DIRECTION ( 'NONE',  ( 1.067522139062650671E-15, 1.000000000000000000, 0.000000000000000000 ) ) ;
#20424 = CARTESIAN_POINT ( 'NONE',  ( 101.1405520526760284, -45.23956608920054379, 233.0803871806719769 ) ) ;
#20425 = DIRECTION ( 'NONE',  ( -0.4999999999999998890, 0.000000000000000000, -0.8660254037844387076 ) ) ;
#20426 = CARTESIAN_POINT ( 'NONE',  ( 109.5220866130624700, -46.80460460589462457, 83.75467289495797729 ) ) ;
#20427 = CARTESIAN_POINT ( 'NONE',  ( 110.8969065101373701, -45.96677993874423152, 52.88927660374830708 ) ) ;
#20428 = CIRCLE ( 'NONE', #50699, 7.999999999999992895 ) ;
#20429 = CARTESIAN_POINT ( 'NONE',  ( 110.1781312709696863, -27.19109411000012244, 20.82538979885751473 ) ) ;
#20431 = ORIENTED_EDGE ( 'NONE', *, *, #75245, .F. ) ;
#20430 = CIRCLE ( 'NONE', #27682, 3.250000000000002665 ) ;
#20432 = EDGE_CURVE ( 'NONE', #50014, #57432, #7309, .T. ) ;
#20433 = CARTESIAN_POINT ( 'NONE',  ( -186.2398777604655038, 20.32000000000000028, 114.2999999999999972 ) ) ;
#20434 = VERTEX_POINT ( 'NONE', #31092 ) ;
#20435 = ORIENTED_EDGE ( 'NONE', *, *, #48849, .F. ) ;
#20436 = LINE ( 'NONE', #59177, #7524 ) ;
#20437 = CARTESIAN_POINT ( 'NONE',  ( 115.8755296135227724, -35.76560983836216678, 275.3444404487542556 ) ) ;
#20438 = EDGE_CURVE ( 'NONE', #28826, #30158, #79806, .T. ) ;
#20439 = CARTESIAN_POINT ( 'NONE',  ( 117.0608945213714946, -38.08045314215456045, 193.7189586075451473 ) ) ;
#20440 = CARTESIAN_POINT ( 'NONE',  ( 109.7244294343027633, -27.00068945919879582, 139.8648275368623501 ) ) ;
#20441 = CARTESIAN_POINT ( 'NONE',  ( 99.04406177815982915, -42.84125753558077321, 152.8439585988425051 ) ) ;
#20442 = CIRCLE ( 'NONE', #56677, 1.000000000000000888 ) ;
#20443 = CYLINDRICAL_SURFACE ( 'NONE', #69082, 10.00000000000002665 ) ;
#20444 = VERTEX_POINT ( 'NONE', #25171 ) ;
#20445 = DIRECTION ( 'NONE',  ( -0.000000000000000000, -1.000000000000000000, -0.000000000000000000 ) ) ;
#20446 = DIRECTION ( 'NONE',  ( 0.000000000000000000, 0.000000000000000000, 1.000000000000000000 ) ) ;
#20447 = ORIENTED_EDGE ( 'NONE', *, *, #21605, .T. ) ;
#20448 = CARTESIAN_POINT ( 'NONE',  ( 105.9884003220067399, -26.36003215364494423, 50.15848241876796720 ) ) ;
#20449 = ORIENTED_EDGE ( 'NONE', *, *, #71148, .T. ) ;
#20451 = AXIS2_PLACEMENT_3D ( 'NONE', #34890, #60803, #47612 ) ;
#20450 = CARTESIAN_POINT ( 'NONE',  ( 115.8942015304759252, -33.87145029861233070, 281.8938046553057575 ) ) ;
#20452 = DIRECTION ( 'NONE',  ( 0.000000000000000000, 0.000000000000000000, -1.000000000000000000 ) ) ;
#20453 = CARTESIAN_POINT ( 'NONE',  ( 99.89458030379213938, -28.23347241844141919, 150.6356252759109680 ) ) ;
#20454 = FACE_BOUND ( 'NONE', #58985, .T. ) ;
#20455 = DIRECTION ( 'NONE',  ( -1.000000000000000000, -4.299999999999999979E-14, -1.000000000000000078E-15 ) ) ;
#20456 = LINE ( 'NONE', #34057, #34692 ) ;
#20457 = B_SPLINE_CURVE_WITH_KNOTS ( 'NONE', 3,
 ( #37535, #57962, #3009, #71615, #45644, #38851, #73375, #58405, #72501, #85698, #37088, #9380, #65666, #86578, #52017, #64788, #17532, #11146, #23473, #32477, #67907, #53350, #12957, #33833, #12055, #54242, #68363, #20218, #18405, #33385, #87465, #82008, #5695, #39305, #81120, #81566, #19763, #89260, #59732, #88372, #18865, #61088, #47442, #52886, #25224, #75175, #11613, #80659, #6144 ),
 .UNSPECIFIED., .F., .F.,
 ( 4, 2, 2, 2, 2, 2, 2, 2, 2, 2, 2, 2, 2, 2, 2, 1, 2, 2, 2, 2, 2, 2, 2, 2, 4 ),
 ( 0.01987186023414423339, 0.02111356671950569489, 0.02235527320486715638, 0.02483868617559007591, 0.02608039266095154782, 0.02732209914631301972, 0.02980551211703596354, 0.03228892508775890735, 0.03353063157312035497, 0.03477233805848180259, 0.03725575102920469783, 0.03849745751456616627, 0.03973916399992762083, 0.04222257697065059934, 0.04346428345601208165, 0.04470598994137357785, 0.04594769642673506016, 0.04718940291209654941, 0.04967281588281953486, 0.05091452236818098942, 0.05215622885354243010, 0.05463964182426538085, 0.05588134830962686317, 0.05712305479498833161, 0.05960646776571133787 ),
 .UNSPECIFIED. ) ;
#20458 = CARTESIAN_POINT ( 'NONE',  ( 5.749594899366220702, 71.22412605658588802, 130.4294147092975606 ) ) ;
#20459 = CARTESIAN_POINT ( 'NONE',  ( 96.63877784842330243, -35.80427747552585060, 227.2556252759109725 ) ) ;
#20460 = DIRECTION ( 'NONE',  ( 0.000000000000000000, -0.000000000000000000, 1.000000000000000000 ) ) ;
#20461 = ORIENTED_EDGE ( 'NONE', *, *, #80248, .F. ) ;
#20462 = ORIENTED_EDGE ( 'NONE', *, *, #22981, .F. ) ;
#20463 = CARTESIAN_POINT ( 'NONE',  ( 96.59840162804212582, -36.61878533396502888, 107.3184824187679567 ) ) ;
#20464 = DIRECTION ( 'NONE',  ( 0.000000000000000000, 0.000000000000000000, -1.000000000000000000 ) ) ;
#20465 = VERTEX_POINT ( 'NONE', #81064 ) ;
#20467 = ADVANCED_FACE ( 'NONE', ( #38799 ), #66960, .T. ) ;
#20466 = ORIENTED_EDGE ( 'NONE', *, *, #17380, .T. ) ;
#20469 = ORIENTED_EDGE ( 'NONE', *, *, #88184, .F. ) ;
#20468 = EDGE_CURVE ( 'NONE', #38670, #20086, #24297, .T. ) ;
#20470 = AXIS2_PLACEMENT_3D ( 'NONE', #54164, #81924, #38325 ) ;
#20471 = AXIS2_PLACEMENT_3D ( 'NONE', #70467, #49544, #28671 ) ;
#20472 = ADVANCED_FACE ( 'NONE', ( #72880 ), #32420, .F. ) ;
#20473 = DIRECTION ( 'NONE',  ( -0.000000000000000000, 1.000000000000000000, 0.000000000000000000 ) ) ;
#20474 = DIRECTION ( 'NONE',  ( -0.8660253910675250744, -0.0001484127182077903334, 0.5000000000000052180 ) ) ;
#20475 = LINE ( 'NONE', #48587, #8889 ) ;
#20476 = CARTESIAN_POINT ( 'NONE',  ( 132.2857443282839824, -83.77844715994092439, 45.21780685541799727 ) ) ;
#20477 = CARTESIAN_POINT ( 'NONE',  ( 115.1781387256201725, -32.22423048609648788, 177.0480903695909660 ) ) ;
#20478 = CARTESIAN_POINT ( 'NONE',  ( 111.7488185767529245, -27.39065688012293265, 275.7070538473396937 ) ) ;
#20479 = CARTESIAN_POINT ( 'NONE',  ( 98.04142522629925338, -41.04166024399867041, 57.68117463785360144 ) ) ;
#20480 = ORIENTED_EDGE ( 'NONE', *, *, #72583, .F. ) ;
#20481 = CARTESIAN_POINT ( 'NONE',  ( 130.1664033068597064, 90.28418055714726620, -10.08203418473755164 ) ) ;
#20482 = ADVANCED_FACE ( 'NONE', ( #10647 ), #12007, .F. ) ;
#20483 = CARTESIAN_POINT ( 'NONE',  ( 126.4481529151155996, 44.45000000000000284, 32.49205688096009936 ) ) ;
#20484 = AXIS2_PLACEMENT_3D ( 'NONE', #5599, #40550, #88280 ) ;
#20485 = ORIENTED_EDGE ( 'NONE', *, *, #58303, .F. ) ;
#20486 = ORIENTED_EDGE ( 'NONE', *, *, #33276, .T. ) ;
#20487 = ADVANCED_FACE ( 'NONE', ( #66052 ), #26107, .T. ) ;
#20488 = AXIS2_PLACEMENT_3D ( 'NONE', #41332, #69061, #83158 ) ;
#20489 = CARTESIAN_POINT ( 'NONE',  ( 177.3246001664172695, -48.34074026909179622, 300.4678068554149490 ) ) ;
#20490 = ORIENTED_EDGE ( 'NONE', *, *, #30631, .T. ) ;
#20491 = VERTEX_POINT ( 'NONE', #86971 ) ;
#20492 = DIRECTION ( 'NONE',  ( -1.000000000000000000, -2.756263715554006823E-15, 0.000000000000000000 ) ) ;
#20493 = CARTESIAN_POINT ( 'NONE',  ( 97.31303930280388670, -38.96046111533910050, 16.50542592143737508 ) ) ;
#20494 = B_SPLINE_CURVE_WITH_KNOTS ( 'NONE', 3,
 ( #41818, #21410, #34573, #34119, #69106, #75918, #28659, #13248, #60, #12809, #49081, #42274, #75477, #6426, #82306, #959, #61822, #33686, #82756, #35462, #506, #28199, #41376, #70002, #35015, #83640, #20519, #7774, #48185, #7330 ),
 .UNSPECIFIED., .F., .F.,
 ( 4, 2, 2, 2, 1, 2, 2, 2, 2, 2, 2, 2, 1, 2, 2, 4 ),
 ( 0.000000000000000000, 0.1250000000000000555, 0.1875000000000011935, 0.2187500000000017764, 0.2343750000000021094, 0.2421874999999987510, 0.2499999999999953926, 0.3750000000000031641, 0.4375000000000122125, 0.5000000000000212053, 0.6250000000000273115, 0.6875000000000297540, 0.7187500000000239808, 0.7343750000000210942, 0.7500000000000182077, 1.000000000000000000 ),
 .UNSPECIFIED. ) ;
#20495 = FACE_BOUND ( 'NONE', #12724, .T. ) ;
#20496 = CARTESIAN_POINT ( 'NONE',  ( 31.71315051186898870, -31.94127993907790852, -5.074374724088000832 ) ) ;
#20497 = EDGE_CURVE ( 'NONE', #39861, #65845, #46367, .T. ) ;
#20498 = CARTESIAN_POINT ( 'NONE',  ( 106.9915265980828849, -45.27055441931952373, 186.9924198280769758 ) ) ;
#20499 = CARTESIAN_POINT ( 'NONE',  ( 106.9267615183890854, -26.22553017860169433, 60.08705384733897858 ) ) ;
#20500 = ORIENTED_EDGE ( 'NONE', *, *, #12968, .F. ) ;
#20501 = LINE ( 'NONE', #6852, #87227 ) ;
#20502 = ORIENTED_EDGE ( 'NONE', *, *, #54800, .F. ) ;
#20503 = CARTESIAN_POINT ( 'NONE',  ( -75.38287938185001735, 76.93600387762164416, -91.50401754987797176 ) ) ;
#20504 = ORIENTED_EDGE ( 'NONE', *, *, #32140, .T. ) ;
#20505 = VECTOR ( 'NONE', #77409, 1000.000000000000000 ) ;
#20506 = CARTESIAN_POINT ( 'NONE',  ( 97.33774478693185017, -34.07145668260515237, 262.1148423024291105 ) ) ;
#20507 = ORIENTED_EDGE ( 'NONE', *, *, #77383, .T. ) ;
#20508 = CARTESIAN_POINT ( 'NONE',  ( 115.9865316739811476, -32.12318019333122265, 165.2061833773214801 ) ) ;
#20509 = DIRECTION ( 'NONE',  ( -0.7071067811865336949, -0.7071067811865614505, 0.000000000000000000 ) ) ;
#20510 = CARTESIAN_POINT ( 'NONE',  ( 37.06648329127400388, 12.92155284005802685, 349.2756252759108406 ) ) ;
#20511 = CIRCLE ( 'NONE', #26328, 5.599999999999994316 ) ;
#20512 = DIRECTION ( 'NONE',  ( 1.000000000000000000, 0.000000000000000000, 0.000000000000000000 ) ) ;
#20513 = ORIENTED_EDGE ( 'NONE', *, *, #63338, .T. ) ;
#20514 = CARTESIAN_POINT ( 'NONE',  ( 96.69266203715996255, -37.96645829736812061, 41.42133956162496844 ) ) ;
#20515 =( LENGTH_UNIT ( ) NAMED_UNIT ( * ) SI_UNIT ( .MILLI., .METRE. ) );
#20517 = CARTESIAN_POINT ( 'NONE',  ( 97.40459591070923295, 72.22361908171431821, -86.93292302958576556 ) ) ;
#20516 = CARTESIAN_POINT ( 'NONE',  ( 112.1386878447022042, -28.01244317163742892, 164.6565191118704661 ) ) ;
#20518 = CARTESIAN_POINT ( 'NONE',  ( 68.70120400217622603, -127.1654454912769836, 247.5297809874748793 ) ) ;
#20519 = CARTESIAN_POINT ( 'NONE',  ( 132.9420963948872725, -16.21971364483387035, 1.822997995689119133 ) ) ;
#20520 = ORIENTED_EDGE ( 'NONE', *, *, #16223, .T. ) ;
#20521 = VECTOR ( 'NONE', #44939, 1000.000000000000000 ) ;
#20522 = DIRECTION ( 'NONE',  ( 0.000000000000000000, 1.000000000000000000, 0.000000000000000000 ) ) ;
#20523 = DIRECTION ( 'NONE',  ( -1.000000000000000000, 0.000000000000000000, 0.000000000000000000 ) ) ;
#20524 = CARTESIAN_POINT ( 'NONE',  ( 8.398302923777746898, 72.98741371662136146, 118.2596197875572415 ) ) ;
#20525 = VERTEX_POINT ( 'NONE', #48278 ) ;
#20526 = CARTESIAN_POINT ( 'NONE',  ( 107.3215613407866584, -25.65604926530302166, 71.04610146638795243 ) ) ;
#20529 = EDGE_CURVE ( 'NONE', #45331, #53161, #76877, .T. ) ;
#20528 = DIRECTION ( 'NONE',  ( 0.000000000000000000, 0.000000000000000000, -1.000000000000000000 ) ) ;
#20527 = CARTESIAN_POINT ( 'NONE',  ( 33.91903122894598965, -35.91149509761181235, -5.074374724088000832 ) ) ;
#20530 = CARTESIAN_POINT ( 'NONE',  ( -31.75000000000000000, 111.1250000000000000, -3.175000000000219647 ) ) ;
#20531 = CARTESIAN_POINT ( 'NONE',  ( 142.4374377537056660, -108.6105248799684233, 248.3919668373590071 ) ) ;
#20532 = ORIENTED_EDGE ( 'NONE', *, *, #11625, .T. ) ;
#20533 = CARTESIAN_POINT ( 'NONE',  ( 100.1408543393099393, -45.42701269980175738, 118.0413395616249659 ) ) ;
#20535 = VERTEX_POINT ( 'NONE', #75577 ) ;
#20534 = FACE_OUTER_BOUND ( 'NONE', #59547, .T. ) ;
#20536 = AXIS2_PLACEMENT_3D ( 'NONE', #41160, #6659, #34353 ) ;
#20537 = CARTESIAN_POINT ( 'NONE',  ( 96.78489722101822679, -35.14273565208915073, 262.2041967044821149 ) ) ;
#20538 = DIRECTION ( 'NONE',  ( -1.000000000000000000, 0.000000000000000000, 0.000000000000000000 ) ) ;
#20539 = DIRECTION ( 'NONE',  ( 0.7071067811865490160, 0.000000000000000000, 0.7071067811865461294 ) ) ;
#20540 = DIRECTION ( 'NONE',  ( 0.000000000000000000, 1.000000000000000000, 0.000000000000000000 ) ) ;
#20541 = CARTESIAN_POINT ( 'NONE',  ( 108.4174892634158027, -26.73503592936582152, 80.96895860834700898 ) ) ;
#20542 = CARTESIAN_POINT ( 'NONE',  ( 68.24270753389627941, -138.8544507913902066, 245.5998607319569942 ) ) ;
#20543 = DIRECTION ( 'NONE',  ( 1.000000000000000078E-15, 1.000000000000000083E-30, -1.000000000000000000 ) ) ;
#20544 = CARTESIAN_POINT ( 'NONE',  ( 103.5361331145922890, -27.60804031003065262, 215.3699109901969848 ) ) ;
#20545 = EDGE_LOOP ( 'NONE', ( #75381, #81751, #26586, #50981 ) ) ;
#20546 = VECTOR ( 'NONE', #40928, 1000.000000000000000 ) ;
#20547 = EDGE_LOOP ( 'NONE', ( #9259, #39798 ) ) ;
#20548 = CARTESIAN_POINT ( 'NONE',  ( 100.0878889097611335, -31.26788461136058217, 152.2301547344689538 ) ) ;
#20549 = CIRCLE ( 'NONE', #27794, 3.300000000000000711 ) ;
#20550 = EDGE_CURVE ( 'NONE', #58010, #63589, #48726, .T. ) ;
#20551 = LINE ( 'NONE', #993, #25494 ) ;
#20553 = CARTESIAN_POINT ( 'NONE',  ( 97.81170508561586985, -40.51744524251693491, 57.63550115181184452 ) ) ;
#20552 = CARTESIAN_POINT ( 'NONE',  ( 110.7503267229639476, -45.78994093226354778, 278.8841967044818375 ) ) ;
#20554 = DIRECTION ( 'NONE',  ( 0.000000000000000000, 0.000000000000000000, 1.000000000000000000 ) ) ;
#20555 = FACE_OUTER_BOUND ( 'NONE', #28795, .T. ) ;
#20556 = DIRECTION ( 'NONE',  ( 0.000000000000000000, 0.000000000000000000, 1.000000000000000000 ) ) ;
#20557 = DIRECTION ( 'NONE',  ( 0.7071067811865279218, -0.7071067811865670016, 2.899137802865041747E-29 ) ) ;
#20558 = CYLINDRICAL_SURFACE ( 'NONE', #29982, 3.700000000000001954 ) ;
#20559 = CARTESIAN_POINT ( 'NONE',  ( 101.4165038149807003, -45.50681337102575696, 222.1213395616249784 ) ) ;
#20560 = CARTESIAN_POINT ( 'NONE',  ( 113.2467642917647623, -28.75963215629028369, 169.5517896119323780 ) ) ;
#20561 = ORIENTED_EDGE ( 'NONE', *, *, #36965, .T. ) ;
#20562 = VERTEX_POINT ( 'NONE', #26974 ) ;
#20563 = AXIS2_PLACEMENT_3D ( 'NONE', #48003, #88924, #75740 ) ;
#20564 = CARTESIAN_POINT ( 'NONE',  ( 97.81168895331838087, -40.51742574516882200, 287.6356252759109680 ) ) ;
#20565 = CARTESIAN_POINT ( 'NONE',  ( 81.44716491658451218, -21.11090284774729042, 7.925007058935930715 ) ) ;
#20566 = LINE ( 'NONE', #40090, #85351 ) ;
#20567 = DIRECTION ( 'NONE',  ( -0.000000000000000000, 1.000000000000000000, -0.000000000000000000 ) ) ;
#20568 = AXIS2_PLACEMENT_3D ( 'NONE', #43733, #87658, #32682 ) ;
#20569 = PLANE ( 'NONE',  #19466 ) ;
#20570 = ORIENTED_EDGE ( 'NONE', *, *, #16091, .T. ) ;
#20571 = CARTESIAN_POINT ( 'NONE',  ( 102.7372881883638058, -25.64480981559214712, 16.37276813305293999 ) ) ;
#20572 = CARTESIAN_POINT ( 'NONE',  ( 101.2938852305094173, -26.37968400006201719, 255.4813395616251626 ) ) ;
#20574 = ORIENTED_EDGE ( 'NONE', *, *, #39026, .T. ) ;
#20573 = EDGE_CURVE ( 'NONE', #89037, #47853, #5187, .T. ) ;
#20575 = AXIS2_PLACEMENT_3D ( 'NONE', #48946, #76688, #42145 ) ;
#20576 = EDGE_CURVE ( 'NONE', #58675, #1366, #61031, .T. ) ;
#20577 = CARTESIAN_POINT ( 'NONE',  ( -12.60000000000000497, 83.37282639406460305, 117.8845415480758021 ) ) ;
#20578 = CARTESIAN_POINT ( 'NONE',  ( 0.000000000000000000, 223.9999999999999716, 159.6557476874258441 ) ) ;
#20579 = EDGE_CURVE ( 'NONE', #54148, #83421, #88761, .T. ) ;
#20580 = CARTESIAN_POINT ( 'NONE',  ( 110.8543953957528032, -45.98426871307141539, 167.8856186728536386 ) ) ;
#20581 = CARTESIAN_POINT ( 'NONE',  ( 98.66659878002396056, -40.67125783036974696, 59.49380465530595785 ) ) ;
#20582 = CARTESIAN_POINT ( 'NONE',  ( 114.3591167413298280, -29.19972650290871030, 170.4641967044829585 ) ) ;
#20583 = DIRECTION ( 'NONE',  ( -1.000000000000000078E-15, 1.000000000000000000, 0.000000000000000000 ) ) ;
#20584 = EDGE_LOOP ( 'NONE', ( #80849, #54973, #56212, #68716 ) ) ;
#20585 = EDGE_CURVE ( 'NONE', #11707, #45346, #26520, .T. ) ;
#20586 = DIRECTION ( 'NONE',  ( 1.000000000000000000, 0.000000000000000000, -1.047445008332813989E-14 ) ) ;
#20587 = ORIENTED_EDGE ( 'NONE', *, *, #19115, .F. ) ;
#20588 = ORIENTED_EDGE ( 'NONE', *, *, #14255, .F. ) ;
#20589 = CARTESIAN_POINT ( 'NONE',  ( 172.5664832912729878, -18.82844715994071194, 75.92562527591206845 ) ) ;
#20590 = ORIENTED_EDGE ( 'NONE', *, *, #70758, .T. ) ;
#20591 = ORIENTED_EDGE ( 'NONE', *, *, #45770, .F. ) ;
#20592 = DIRECTION ( 'NONE',  ( 1.000000000000000000, 0.000000000000000000, -9.299908063537909262E-17 ) ) ;
#20593 = EDGE_CURVE ( 'NONE', #81558, #83603, #76012, .T. ) ;
#20594 = CARTESIAN_POINT ( 'NONE',  ( 97.58007606596183336, -34.66094392094686327, 105.5781341137909664 ) ) ;
#20595 = CARTESIAN_POINT ( 'NONE',  ( 109.3417050147583041, -26.53289234591626311, 224.9013395616249511 ) ) ;
#20596 = CARTESIAN_POINT ( 'NONE',  ( 117.7539631054257967, -31.66723592997632863, 214.1784824187679419 ) ) ;
#20597 = CARTESIAN_POINT ( 'NONE',  ( 101.3960830062750631, -28.00733582429768376, 21.53562527591096298 ) ) ;
#20598 = CARTESIAN_POINT ( 'NONE',  ( 97.81262911421374895, -40.51702269960655656, 122.6351715870756323 ) ) ;
#20599 = DIRECTION ( 'NONE',  ( 0.000000000000000000, 0.000000000000000000, 1.000000000000000000 ) ) ;
#20600 = ORIENTED_EDGE ( 'NONE', *, *, #76617, .F. ) ;
#20601 = AXIS2_PLACEMENT_3D ( 'NONE', #75808, #47178, #61269 ) ;
#20602 = AXIS2_PLACEMENT_3D ( 'NONE', #86954, #3387, #72866 ) ;
#20603 = CARTESIAN_POINT ( 'NONE',  ( 116.5944731948638804, -42.45914096480947819, 128.3956252759109873 ) ) ;
#20604 = CARTESIAN_POINT ( 'NONE',  ( 95.29943635023701631, -34.95028898632038050, 71.20705384733993526 ) ) ;
#20605 = CARTESIAN_POINT ( 'NONE',  ( 112.4344423749254531, -46.44530527459760805, 252.9661014663871015 ) ) ;
#20606 = ORIENTED_EDGE ( 'NONE', *, *, #22071, .F. ) ;
#20607 = CARTESIAN_POINT ( 'NONE',  ( 112.4544618167839332, -45.69580618038663999, 238.0070538473389377 ) ) ;
#20608 = CARTESIAN_POINT ( 'NONE',  ( 124.0667039024470313, -104.2784471599417202, 0.2178068554180012661 ) ) ;
#20609 = DIRECTION ( 'NONE',  ( 1.000000000000000000, 1.261617073437676668E-15, 9.462128050782575008E-16 ) ) ;
#20610 = DIRECTION ( 'NONE',  ( 0.000000000000000000, 1.000000000000000000, 0.000000000000000000 ) ) ;
#20611 = DIRECTION ( 'NONE',  ( -0.7071067811865774377, 0.7071067811865175967, -7.071067811865782003E-16 ) ) ;
#20613 = DIRECTION ( 'NONE',  ( -1.000000000000000078E-15, 1.000000000000000083E-30, 1.000000000000000000 ) ) ;
#20612 = CARTESIAN_POINT ( 'NONE',  ( 108.6893337760746334, -46.06423824197239725, 277.6356252759110248 ) ) ;
#20614 = DIRECTION ( 'NONE',  ( 1.000000000000000000, 3.999999999999999995E-14, 1.000000000000000078E-15 ) ) ;
#20615 = CARTESIAN_POINT ( 'NONE',  ( -48.02966122971777452, 66.60000000000003695, 106.4272185163641780 ) ) ;
#20616 = CYLINDRICAL_SURFACE ( 'NONE', #20879, 13.44999999999999396 ) ;
#20617 = DIRECTION ( 'NONE',  ( 0.000000000000000000, 1.000000000000000000, 0.000000000000000000 ) ) ;
#20618 = CARTESIAN_POINT ( 'NONE',  ( -215.9000000000000057, 53.97500000000000142, 71.43750000000000000 ) ) ;
#20619 = CARTESIAN_POINT ( 'NONE',  ( 104.4899544611976836, -26.97880758236209786, 76.28145860849610926 ) ) ;
#20620 = AXIS2_PLACEMENT_3D ( 'NONE', #2130, #38413, #45652 ) ;
#20622 = ORIENTED_EDGE ( 'NONE', *, *, #31360, .T. ) ;
#20621 = CARTESIAN_POINT ( 'NONE',  ( -479.3614999999999782, 18.41194598552320016, 97.63125000000000853 ) ) ;
#20623 = CARTESIAN_POINT ( 'NONE',  ( 177.8371591254543489, -47.82818131005477369, 249.9678068554149775 ) ) ;
#20624 = CARTESIAN_POINT ( 'NONE',  ( 100.1628669375702714, -45.39175184048325917, 272.0289586092442278 ) ) ;
#20625 = CARTESIAN_POINT ( 'NONE',  ( 97.98655846647217516, -41.85169789442448263, 132.7356252759109623 ) ) ;
#20626 = CARTESIAN_POINT ( 'NONE',  ( 101.0616705854173460, -45.30470917520826646, 278.0899109901965858 ) ) ;
#20627 = CARTESIAN_POINT ( 'NONE',  ( 116.3212776292296127, -32.94146857471318413, 287.6356252759109680 ) ) ;
#20630 = EDGE_CURVE ( 'NONE', #10962, #88157, #54640, .T. ) ;
#20629 = LINE ( 'NONE', #13367, #3719 ) ;
#20628 = DIRECTION ( 'NONE',  ( 1.000000000000000000, 0.000000000000000000, 0.000000000000000000 ) ) ;
#20631 = DIRECTION ( 'NONE',  ( 0.000000000000000000, 0.000000000000000000, 1.000000000000000000 ) ) ;
#20632 = CIRCLE ( 'NONE', #34936, 11.49999999999999645 ) ;
#20633 = CARTESIAN_POINT ( 'NONE',  ( 131.3179999999999836, 53.97500000000000142, 50.79999999999999716 ) ) ;
#20634 = VECTOR ( 'NONE', #86619, 1000.000000000000000 ) ;
#20635 = EDGE_CURVE ( 'NONE', #66334, #51011, #14184, .T. ) ;
#20636 = ORIENTED_EDGE ( 'NONE', *, *, #5186, .T. ) ;
#20637 = LINE ( 'NONE', #48303, #89704 ) ;
#20638 = ORIENTED_EDGE ( 'NONE', *, *, #30260, .T. ) ;
#20639 = MANIFOLD_SOLID_BREP ( 'Stock-Rail and drilling-1', #21310 ) ;
#20640 = CIRCLE ( 'NONE', #48165, 3.174999999999983391 ) ;
#20641 = CARTESIAN_POINT ( 'NONE',  ( 115.2191710476659665, -34.18193581181276386, 173.4895626852199371 ) ) ;
#20643 = ORIENTED_EDGE ( 'NONE', *, *, #59816, .T. ) ;
#20642 = LINE ( 'NONE', #42842, #67465 ) ;
#20644 = DIRECTION ( 'NONE',  ( 0.000000000000000000, 0.000000000000000000, -1.000000000000000000 ) ) ;
#20645 = CARTESIAN_POINT ( 'NONE',  ( 97.97553865104319470, -30.48296430071277641, 161.8594347997199918 ) ) ;
#20646 = CARTESIAN_POINT ( 'NONE',  ( -68.53801554307339927, 127.0000000000000000, -74.15067561874339219 ) ) ;
#20647 = VECTOR ( 'NONE', #7329, 1000.000000000000000 ) ;
#20648 = FACE_OUTER_BOUND ( 'NONE', #11817, .T. ) ;
#20649 = LINE ( 'NONE', #69691, #1238 ) ;
#20650 = LINE ( 'NONE', #13826, #29487 ) ;
#20651 = CARTESIAN_POINT ( 'NONE',  ( 116.7274023843879718, -38.25590632018516857, 113.7013395616259857 ) ) ;
#20652 = ORIENTED_EDGE ( 'NONE', *, *, #76718, .F. ) ;
#20653 = ORIENTED_EDGE ( 'NONE', *, *, #20771, .T. ) ;
#20654 = ORIENTED_EDGE ( 'NONE', *, *, #26154, .F. ) ;
#20655 = ADVANCED_FACE ( 'NONE', ( #74670, #22405 ), #36022, .T. ) ;
#20656 = DIRECTION ( 'NONE',  ( 0.000000000000000000, 0.000000000000000000, -1.000000000000000000 ) ) ;
#20658 = CARTESIAN_POINT ( 'NONE',  ( 117.0608945257504985, -38.08045309939960532, 38.71895861094868252 ) ) ;
#20657 = CARTESIAN_POINT ( 'NONE',  ( 108.1128363339379490, -46.45408497333508535, 198.6613395616249989 ) ) ;
#20659 = CARTESIAN_POINT ( 'NONE',  ( 102.0675651188745832, -27.97020183595695997, 55.48833508751222610 ) ) ;
#20660 = LINE ( 'NONE', #89712, #15544 ) ;
#20661 = VECTOR ( 'NONE', #38493, 1000.000000000000000 ) ;
#20662 = LINE ( 'NONE', #48327, #62290 ) ;
#20663 = CARTESIAN_POINT ( 'NONE',  ( 67.09903452484594766, -67.90769682686300257, 245.8492538885293186 ) ) ;
#20664 = CARTESIAN_POINT ( 'NONE',  ( 116.8835868046513582, -40.17228670562625581, 133.5584824187679658 ) ) ;
#20665 = EDGE_LOOP ( 'NONE', ( #56738, #20209, #27388, #88489 ) ) ;
#20666 = EDGE_LOOP ( 'NONE', ( #46450, #58883, #75676, #16507 ) ) ;
#20667 = ORIENTED_EDGE ( 'NONE', *, *, #69334, .F. ) ;
#20668 = EDGE_CURVE ( 'NONE', #8418, #79915, #71008, .T. ) ;
#20669 = CARTESIAN_POINT ( 'NONE',  ( 151.0371591254575208, -24.42818131005592264, 180.4678068554149775 ) ) ;
#20670 = DIRECTION ( 'NONE',  ( 1.000000000000000078E-15, -1.000000000000000083E-30, -1.000000000000000000 ) ) ;
#20671 = CARTESIAN_POINT ( 'NONE',  ( 118.5667039024470313, -104.2784471599411376, 19.21780685541799016 ) ) ;
#20672 = CARTESIAN_POINT ( 'NONE',  ( 115.0725392204758890, -35.00151292932243052, 181.8138046553059723 ) ) ;
#20673 = VECTOR ( 'NONE', #72945, 1000.000000000000000 ) ;
#20674 = DIRECTION ( 'NONE',  ( 1.000000000000000000, 4.163336342344333240E-14, 0.000000000000000000 ) ) ;
#20675 = CARTESIAN_POINT ( 'NONE',  ( 105.8003522596126516, -26.72392167762159332, 26.17665498994805517 ) ) ;
#20676 = VERTEX_POINT ( 'NONE', #22859 ) ;
#20678 = ORIENTED_EDGE ( 'NONE', *, *, #39495, .F. ) ;
#20677 = EDGE_LOOP ( 'NONE', ( #10525, #65682, #33607, #50844, #38276 ) ) ;
#20679 = CARTESIAN_POINT ( 'NONE',  ( -19.89663890320305839, 44.45000000000000284, 32.49205688096009936 ) ) ;
#20680 = ORIENTED_EDGE ( 'NONE', *, *, #8509, .F. ) ;
#20681 = VERTEX_POINT ( 'NONE', #76916 ) ;
#20682 = CARTESIAN_POINT ( 'NONE',  ( 71.25614885437424562, -84.12815644128085069, 540.9756252759101471 ) ) ;
#20683 = EDGE_CURVE ( 'NONE', #37688, #76536, #65334, .T. ) ;
#20684 = VECTOR ( 'NONE', #77424, 1000.000000000000000 ) ;
#20685 = CARTESIAN_POINT ( 'NONE',  ( 101.2707639275114815, -30.02587231748817231, 257.0758690201828927 ) ) ;
#20686 = ORIENTED_EDGE ( 'NONE', *, *, #739, .T. ) ;
#20687 = DIRECTION ( 'NONE',  ( -9.073094938289460781E-13, -1.000000000000000000, 0.000000000000000000 ) ) ;
#20688 = CARTESIAN_POINT ( 'NONE',  ( -126.0120328259609863, 66.16239491992259047, 34.14452143064587375 ) ) ;
#20689 = EDGE_LOOP ( 'NONE', ( #61137, #54078, #56247, #31840 ) ) ;
#20690 = ORIENTED_EDGE ( 'NONE', *, *, #76279, .F. ) ;
#20691 = AXIS2_PLACEMENT_3D ( 'NONE', #7522, #56555, #1161 ) ;
#20692 = CARTESIAN_POINT ( 'NONE',  ( 70.63919639214310564, 93.07500000000001705, 56.85413200336923012 ) ) ;
#20693 = ORIENTED_EDGE ( 'NONE', *, *, #65049, .T. ) ;
#20694 = ORIENTED_EDGE ( 'NONE', *, *, #21002, .T. ) ;
#20695 = AXIS2_PLACEMENT_3D ( 'NONE', #72451, #58793, #9331 ) ;
#20696 = EDGE_CURVE ( 'NONE', #89471, #36163, #16065, .T. ) ;
#20697 = CARTESIAN_POINT ( 'NONE',  ( 99.11752347482735104, -34.75543446931638414, 273.9509475124486357 ) ) ;
#20698 = CARTESIAN_POINT ( 'NONE',  ( 111.8042541167996546, -25.83965636698058432, 134.7499109901969518 ) ) ;
#20699 = CARTESIAN_POINT ( 'NONE',  ( 99.07096106853131801, -43.38529345585687480, 116.8784824187679732 ) ) ;
#20700 = CARTESIAN_POINT ( 'NONE',  ( 99.03962527909632740, -36.84879970159397544, 249.5838068554172082 ) ) ;
#20701 = EDGE_CURVE ( 'NONE', #40497, #22712, #51016, .T. ) ;
#20702 = PLANE ( 'NONE',  #77159 ) ;
#20703 = CARTESIAN_POINT ( 'NONE',  ( 113.1553867986010857, -26.56284154956258092, 200.6470538473399756 ) ) ;
#20704 = CARTESIAN_POINT ( 'NONE',  ( 107.0667039024470313, -104.2784471599418197, -11.78219314458200984 ) ) ;
#20705 = CARTESIAN_POINT ( 'NONE',  ( 34.27258461953899626, -35.55794170701810941, -5.074374724088000832 ) ) ;
#20706 = ORIENTED_EDGE ( 'NONE', *, *, #50808, .F. ) ;
#20707 = CARTESIAN_POINT ( 'NONE',  ( 130.5246035444014581, 70.17666187254641841, 2.891673250713812759 ) ) ;
#20708 = EDGE_LOOP ( 'NONE', ( #1692, #14141, #18665, #58748 ) ) ;
#20709 = VERTEX_POINT ( 'NONE', #7275 ) ;
#20710 = FACE_OUTER_BOUND ( 'NONE', #32965, .T. ) ;
#20711 = CARTESIAN_POINT ( 'NONE',  ( 0.000000000000000000, 101.5999999999999943, 0.000000000000000000 ) ) ;
#20712 = CARTESIAN_POINT ( 'NONE',  ( 117.0333688383452397, -30.31836458025946968, 144.2813395616249750 ) ) ;
#20713 = CARTESIAN_POINT ( 'NONE',  ( -4.834503460661677465, 70.80616061483986812, 130.4664586724606750 ) ) ;
#20714 = DIRECTION ( 'NONE',  ( 0.000000000000000000, 0.000000000000000000, 1.000000000000000000 ) ) ;
#20715 = CARTESIAN_POINT ( 'NONE',  ( 128.0667039024480118, -48.82844715994099971, 250.9178068554150514 ) ) ;
#20718 = CARTESIAN_POINT ( 'NONE',  ( 103.3114313307234085, -27.02747569519259230, 211.3699109901969848 ) ) ;
#20717 = CARTESIAN_POINT ( 'NONE',  ( 97.81443832832722762, -40.51607714565724905, 56.63519146330476417 ) ) ;
#20716 = LINE ( 'NONE', #88871, #12857 ) ;
#20719 = DIRECTION ( 'NONE',  ( 0.000000000000000000, 1.000000000000000000, 0.000000000000000000 ) ) ;
#20720 = DIRECTION ( 'NONE',  ( -6.831565154159360295E-14, 1.000000000000000000, 0.000000000000000000 ) ) ;
#20721 = ORIENTED_EDGE ( 'NONE', *, *, #23450, .T. ) ;
#20722 = CARTESIAN_POINT ( 'NONE',  ( -141.3509999999999991, 20.32000000000000028, -141.3509999999999991 ) ) ;
#20723 = AXIS2_PLACEMENT_3D ( 'NONE', #31021, #37847, #16073 ) ;
#20724 = CYLINDRICAL_SURFACE ( 'NONE', #708, 0.5000000000000079936 ) ;
#20725 = DIRECTION ( 'NONE',  ( 0.7071067811865475727, -0.7071067811865475727, 0.000000000000000000 ) ) ;
#20726 = LINE ( 'NONE', #76129, #72404 ) ;
#20728 = ORIENTED_EDGE ( 'NONE', *, *, #44628, .F. ) ;
#20727 = DIRECTION ( 'NONE',  ( 0.000000000000000000, -1.000000000000000000, 0.000000000000000000 ) ) ;
#20729 = CARTESIAN_POINT ( 'NONE',  ( 116.0324533029107670, -32.23654553487196495, 194.1959605532332489 ) ) ;
#20730 = CARTESIAN_POINT ( 'NONE',  ( 95.99055855653007541, -36.58346519971924948, 156.3280062282919687 ) ) ;
#20731 = CARTESIAN_POINT ( 'NONE',  ( 115.8915968718629017, -31.17968520675552924, 30.27276813305396175 ) ) ;
#20732 = CARTESIAN_POINT ( 'NONE',  ( 112.8039874620816789, -45.48581773443041953, 174.0384824187679556 ) ) ;
#20733 = FACE_OUTER_BOUND ( 'NONE', #76723, .T. ) ;
#20734 = CARTESIAN_POINT ( 'NONE',  ( 105.7996235970844907, -26.72402767612700103, 101.1773280814526430 ) ) ;
#20736 = DIRECTION ( 'NONE',  ( 0.000000000000000000, 0.000000000000000000, -1.000000000000000000 ) ) ;
#20735 = CARTESIAN_POINT ( 'NONE',  ( 181.9694315774339941, -34.03355364505720360, -5.074374724088000832 ) ) ;
#20737 = DIRECTION ( 'NONE',  ( 1.000000000000000000, -4.163336342344339393E-15, -2.775557561562892929E-14 ) ) ;
#20738 = CARTESIAN_POINT ( 'NONE',  ( 37.03715912545427358, -48.62818131006122258, 300.4678068554150059 ) ) ;
#20739 = ORIENTED_EDGE ( 'NONE', *, *, #4382, .F. ) ;
#20740 = VECTOR ( 'NONE', #70970, 1000.000000000000000 ) ;
#20741 = EDGE_CURVE ( 'NONE', #78070, #54444, #88612, .T. ) ;
#20742 = ORIENTED_EDGE ( 'NONE', *, *, #31144, .F. ) ;
#20743 = ORIENTED_EDGE ( 'NONE', *, *, #56491, .F. ) ;
#20744 = EDGE_LOOP ( 'NONE', ( #66354, #89764, #22353, #39640 ) ) ;
#20745 = CARTESIAN_POINT ( 'NONE',  ( 130.5667039024482960, -33.42944715994102722, 249.5838068554162987 ) ) ;
#20746 = CARTESIAN_POINT ( 'NONE',  ( 114.3378803067696197, -44.16957155219873243, 69.19276813305397411 ) ) ;
#20747 = CARTESIAN_POINT ( 'NONE',  ( 151.0371591254572934, -24.42818131005592974, 300.4678068554149490 ) ) ;
#20748 = CARTESIAN_POINT ( 'NONE',  ( 145.4217101158483842, -139.2854844008623445, 245.9863971430950187 ) ) ;
#20749 = CARTESIAN_POINT ( 'NONE',  ( 103.5276745422693523, -26.83930826182397311, 186.3499109901969746 ) ) ;
#20750 = CARTESIAN_POINT ( 'NONE',  ( -187.8075999999999794, 0.000000000000000000, 114.2999999999999972 ) ) ;
#20751 = CARTESIAN_POINT ( 'NONE',  ( 98.80150335516665905, -38.88496061976939444, 275.9524198280767564 ) ) ;
#20752 = ORIENTED_EDGE ( 'NONE', *, *, #77998, .T. ) ;
#20753 = ORIENTED_EDGE ( 'NONE', *, *, #84722, .T. ) ;
#20754 = ORIENTED_EDGE ( 'NONE', *, *, #29707, .T. ) ;
#20755 = VECTOR ( 'NONE', #77586, 999.9999999999998863 ) ;
#20756 = ADVANCED_FACE ( 'NONE', ( #62674 ), #89499, .F. ) ;
#20757 = DIRECTION ( 'NONE',  ( 1.000000000000000000, 4.163336342344333240E-14, 0.000000000000000000 ) ) ;
#20759 = TOROIDAL_SURFACE ( 'NONE', #55533, 13.50000000000000000, 0.5000000000000000000 ) ;
#20758 = DIRECTION ( 'NONE',  ( 1.000000000000000078E-15, -1.000000000000000000, 0.000000000000000000 ) ) ;
#20760 = DIRECTION ( 'NONE',  ( 1.000000000000000000, 0.000000000000000000, 0.000000000000000000 ) ) ;
#20761 = CARTESIAN_POINT ( 'NONE',  ( 108.4139696804844846, -26.73458958342868996, 274.9688129555700584 ) ) ;
#20762 = FACE_OUTER_BOUND ( 'NONE', #78808, .T. ) ;
#20763 = VECTOR ( 'NONE', #81712, 1000.000000000000000 ) ;
#20764 = CARTESIAN_POINT ( 'NONE',  ( 0.000000000000000000, 101.5999999999999943, 0.000000000000000000 ) ) ;
#20765 = EDGE_CURVE ( 'NONE', #33950, #17073, #23341, .T. ) ;
#20766 = FACE_OUTER_BOUND ( 'NONE', #24540, .T. ) ;
#20767 = CARTESIAN_POINT ( 'NONE',  ( 100.6687104586878547, -44.89077600197693130, 277.0594347997210889 ) ) ;
#20768 = DIRECTION ( 'NONE',  ( 1.000000000000000078E-15, 0.000000000000000000, -1.000000000000000000 ) ) ;
#20769 = EDGE_CURVE ( 'NONE', #25006, #78471, #31991, .T. ) ;
#20770 = ORIENTED_EDGE ( 'NONE', *, *, #39825, .T. ) ;
#20771 = EDGE_CURVE ( 'NONE', #8503, #35967, #54036, .T. ) ;
#20772 = DIRECTION ( 'NONE',  ( -1.000000000000000078E-15, 1.000000000000000083E-30, 1.000000000000000000 ) ) ;
#20773 = CARTESIAN_POINT ( 'NONE',  ( 49.16670390244701139, -28.27351298637340093, -5.074374724088000832 ) ) ;
#20774 = CARTESIAN_POINT ( 'NONE',  ( 114.5896176151078976, -33.49137084947443554, 76.96809036959095351 ) ) ;
#20775 = EDGE_CURVE ( 'NONE', #78144, #75163, #36355, .T. ) ;
#20776 = VECTOR ( 'NONE', #84097, 1000.000000000000000 ) ;
#20777 = ADVANCED_FACE ( 'NONE', ( #6367 ), #34058, .F. ) ;
#20778 = DIRECTION ( 'NONE',  ( 4.299999999999999979E-14, -1.000000000000000000, 4.400000000000000367E-29 ) ) ;
#20779 = CYLINDRICAL_SURFACE ( 'NONE', #28539, 3.249999999999975131 ) ;
#20780 = VERTEX_POINT ( 'NONE', #50835 ) ;
#20781 = ORIENTED_EDGE ( 'NONE', *, *, #6337, .T. ) ;
#20782 = PLANE ( 'NONE',  #58554 ) ;
#20783 = VECTOR ( 'NONE', #30582, 1000.000000000000000 ) ;
#20784 = ORIENTED_EDGE ( 'NONE', *, *, #80759, .F. ) ;
#20785 = CARTESIAN_POINT ( 'NONE',  ( 113.3314600845033482, -45.06233935626208620, 143.0899109901969553 ) ) ;
#20786 = ORIENTED_EDGE ( 'NONE', *, *, #46720, .F. ) ;
#20787 = EDGE_CURVE ( 'NONE', #81489, #24432, #70855, .T. ) ;
#20788 = CARTESIAN_POINT ( 'NONE',  ( 97.81169160209351787, -40.51741184665055329, 67.63577596198375375 ) ) ;
#20789 = CARTESIAN_POINT ( 'NONE',  ( 97.07454461617307118, -38.04679588918885713, 147.8615833058969713 ) ) ;
#20790 = CARTESIAN_POINT ( 'NONE',  ( 97.81168895331838087, -40.51742574516882200, 11.63562527591094309 ) ) ;
#20791 = DIRECTION ( 'NONE',  ( 0.000000000000000000, 1.000000000000000000, 0.000000000000000000 ) ) ;
#20792 = CARTESIAN_POINT ( 'NONE',  ( 115.2242804385497976, -44.22181337150698255, 74.22324432352993995 ) ) ;
#20793 = CARTESIAN_POINT ( 'NONE',  ( -147.4575741623271767, 20.32000000000000028, -135.2444258376735888 ) ) ;
#20794 = ORIENTED_EDGE ( 'NONE', *, *, #1327, .F. ) ;
#20795 = FACE_OUTER_BOUND ( 'NONE', #26395, .T. ) ;
#20796 = ORIENTED_EDGE ( 'NONE', *, *, #36586, .F. ) ;
#20797 = EDGE_LOOP ( 'NONE', ( #50639, #7122 ) ) ;
#20798 = EDGE_CURVE ( 'NONE', #7104, #65312, #903, .T. ) ;
#20799 = FACE_OUTER_BOUND ( 'NONE', #80113, .T. ) ;
#20800 = VERTEX_POINT ( 'NONE', #69948 ) ;
#20801 = CARTESIAN_POINT ( 'NONE',  ( 117.4251315444616353, -36.24242395571270237, 268.8518157521021408 ) ) ;
#20802 = CARTESIAN_POINT ( 'NONE',  ( 95.99102054923815786, -36.58347128883620059, 152.3280062282919971 ) ) ;
#20803 = EDGE_CURVE ( 'NONE', #65259, #69797, #7714, .T. ) ;
#20804 = CARTESIAN_POINT ( 'NONE',  ( 9.568977433314790559, 74.15890990428199814, -118.1706578929490377 ) ) ;
#20805 = CARTESIAN_POINT ( 'NONE',  ( 113.2454986999111100, -28.75867294631898829, 140.5522919423851249 ) ) ;
#20806 = CARTESIAN_POINT ( 'NONE',  ( 98.14961424977839499, -43.26117181588809757, 102.8175300378159847 ) ) ;
#20808 = EDGE_CURVE ( 'NONE', #10687, #76744, #1357, .T. ) ;
#20807 = CARTESIAN_POINT ( 'NONE',  ( 97.81413651554109379, -40.51640884438177181, 97.63607350422876152 ) ) ;
#20809 = EDGE_LOOP ( 'NONE', ( #44462, #30470, #44697, #64404 ) ) ;
#20810 = LINE ( 'NONE', #35768, #59763 ) ;
#20811 = EDGE_CURVE ( 'NONE', #65595, #22170, #29060, .T. ) ;
#20812 = CARTESIAN_POINT ( 'NONE',  ( 21.03715912545745326, -47.82818131006196438, 117.4678068554150485 ) ) ;
#20813 = VERTEX_POINT ( 'NONE', #29958 ) ;
#20814 = AXIS2_PLACEMENT_3D ( 'NONE', #12568, #38913, #73439 ) ;
#20815 = DIRECTION ( 'NONE',  ( 0.7071067810573886669, 0.7071067813157063675, 7.071067810573880276E-16 ) ) ;
#20816 = DIRECTION ( 'NONE',  ( 1.000000000000000000, 6.145690160522480771E-16, 0.000000000000000000 ) ) ;
#20817 = CARTESIAN_POINT ( 'NONE',  ( 118.0833341887621373, -37.62838194956883342, 38.77372051400595865 ) ) ;
#20818 = FACE_OUTER_BOUND ( 'NONE', #37628, .T. ) ;
#20819 = VECTOR ( 'NONE', #89532, 1000.000000000000000 ) ;
#20820 = CARTESIAN_POINT ( 'NONE',  ( 183.5150000000000148, 14.63749999999999929, -19.05000000000000071 ) ) ;
#20821 = DIRECTION ( 'NONE',  ( 0.7071067811865460184, 0.000000000000000000, 0.7071067811865487940 ) ) ;
#20822 = CARTESIAN_POINT ( 'NONE',  ( 111.8803212371932148, -27.54331830560560590, 14.68038718067299442 ) ) ;
#20824 = CARTESIAN_POINT ( 'NONE',  ( 114.7100688122352494, -43.78666090992606996, 119.2327681330539804 ) ) ;
#20823 = FACE_OUTER_BOUND ( 'NONE', #84354, .T. ) ;
#20825 = DIRECTION ( 'NONE',  ( 0.000000000000000000, 1.000000000000000000, 0.000000000000000000 ) ) ;
#20826 = CARTESIAN_POINT ( 'NONE',  ( 102.8958089960464690, -27.08850953439599962, 155.4013395616249795 ) ) ;
#20827 = LINE ( 'NONE', #54864, #14816 ) ;
#20828 = EDGE_LOOP ( 'NONE', ( #82522, #34178, #62990, #21024 ) ) ;
#20829 = FACE_OUTER_BOUND ( 'NONE', #70398, .T. ) ;
#20830 = CARTESIAN_POINT ( 'NONE',  ( 194.0667039024473297, -24.92844715993408045, 300.4678068554149490 ) ) ;
#20831 = CARTESIAN_POINT ( 'NONE',  ( 135.9115321082789194, -34.68812259377269669, 2.188418746640047541 ) ) ;
#20832 = EDGE_LOOP ( 'NONE', ( #19575, #27056, #48449, #8046 ) ) ;
#20833 = DIRECTION ( 'NONE',  ( -1.000000000000000078E-15, 1.000000000000000083E-30, 1.000000000000000000 ) ) ;
#20835 = EDGE_LOOP ( 'NONE', ( #38625, #83523, #59184, #79105 ) ) ;
#20834 = CARTESIAN_POINT ( 'NONE',  ( 113.5926674049485854, -44.96113684323219672, 168.1099109901969939 ) ) ;
#20836 = FACE_OUTER_BOUND ( 'NONE', #84614, .T. ) ;
#20837 = CARTESIAN_POINT ( 'NONE',  ( 97.45308667932049218, -40.90817919144255654, 227.6527681330539679 ) ) ;
#20838 = CARTESIAN_POINT ( 'NONE',  ( 70.88111044991026688, -139.0101909505960691, 247.5112285516309782 ) ) ;
#20839 = LINE ( 'NONE', #27202, #86626 ) ;
#20840 = DIRECTION ( 'NONE',  ( 0.000000000000000000, 0.000000000000000000, 1.000000000000000000 ) ) ;
#20841 = EDGE_LOOP ( 'NONE', ( #6825, #49452, #36267, #32628 ) ) ;
#20842 = CIRCLE ( 'NONE', #48359, 5.799999999999998934 ) ;
#20843 = ITEM_DEFINED_TRANSFORMATION ( 'NONE', 'NONE', #85572,  #50656 ) ;
#20844 = VECTOR ( 'NONE', #30358, 1000.000000000000227 ) ;
#20845 = EDGE_LOOP ( 'NONE', ( #31904, #81782, #17974, #63107 ) ) ;
#20846 = ORIENTED_EDGE ( 'NONE', *, *, #83155, .T. ) ;
#20847 = CIRCLE ( 'NONE', #71629, 16.33514202138213633 ) ;
#20848 = EDGE_LOOP ( 'NONE', ( #69792, #38632, #55869, #14926 ) ) ;
#20849 = CARTESIAN_POINT ( 'NONE',  ( -50.03799999999999670, 101.5999999999999943, 206.3750000000000000 ) ) ;
#20850 = CARTESIAN_POINT ( 'NONE',  ( 115.8552077933167794, -44.67884570232850194, 229.2413395616249545 ) ) ;
#20851 = DIRECTION ( 'NONE',  ( -0.7071067812160258814, 0.7071067811570692641, -2.899137802744100161E-29 ) ) ;
#20852 = CARTESIAN_POINT ( 'NONE',  ( 135.3321452824298774, -16.28157797494703374, 1.873071231934059444 ) ) ;
#20854 = PLANE ( 'NONE',  #45633 ) ;
#20853 = CARTESIAN_POINT ( 'NONE',  ( 147.0667039024469886, -67.87844715994090450, 222.2178068554179902 ) ) ;
#20855 = DIRECTION ( 'NONE',  ( -0.9254794337955620787, -0.3787978585227822492, 0.000000000000000000 ) ) ;
#20856 = CARTESIAN_POINT ( 'NONE',  ( 100.5368863760760973, -27.78183265877541430, 30.56610146638794134 ) ) ;
#20857 = EDGE_LOOP ( 'NONE', ( #24503, #41992, #43822, #49207, #19735, #60700 ) ) ;
#20858 = AXIS2_PLACEMENT_3D ( 'NONE', #67592, #41210, #74861 ) ;
#20859 = VERTEX_POINT ( 'NONE', #63579 ) ;
#20860 = EDGE_CURVE ( 'NONE', #22586, #29395, #35403, .T. ) ;
#20861 = FACE_OUTER_BOUND ( 'NONE', #25933, .T. ) ;
#20862 = CARTESIAN_POINT ( 'NONE',  ( 2.849336855536075284E-14, 127.0000000000000000, 111.9860621927989683 ) ) ;
#20863 = EDGE_CURVE ( 'NONE', #9020, #63589, #26163, .T. ) ;
#20864 = CARTESIAN_POINT ( 'NONE',  ( 98.06605190618653012, -40.64173669134672906, 227.6527681330529731 ) ) ;
#20865 = CARTESIAN_POINT ( 'NONE',  ( 130.3998166246070127, 12.92155284005802685, 334.6228282640714156 ) ) ;
#20866 = EDGE_CURVE ( 'NONE', #46484, #13532, #84495, .T. ) ;
#20867 = CARTESIAN_POINT ( 'NONE',  ( 98.65123886609836745, -31.74476095556103061, 81.90133956162493689 ) ) ;
#20868 = CARTESIAN_POINT ( 'NONE',  ( 172.5664832912729878, -27.82844715994070484, 314.1756252759120116 ) ) ;
#20869 = CARTESIAN_POINT ( 'NONE',  ( 103.2775828556913211, -27.47503018801354457, 21.38570542117368234 ) ) ;
#20870 = EDGE_CURVE ( 'NONE', #36562, #20391, #22704, .T. ) ;
#20871 = VERTEX_POINT ( 'NONE', #28600 ) ;
#20872 = CARTESIAN_POINT ( 'NONE',  ( 116.3212776292296127, -32.94146857471318413, 287.6356252759109680 ) ) ;
#20873 = EDGE_CURVE ( 'NONE', #40469, #13431, #44002, .T. ) ;
#20874 = EDGE_LOOP ( 'NONE', ( #59520, #45755, #35073, #15191 ) ) ;
#20875 = VERTEX_POINT ( 'NONE', #71738 ) ;
#20876 = FACE_OUTER_BOUND ( 'NONE', #57860, .T. ) ;
#20877 = CARTESIAN_POINT ( 'NONE',  ( 116.9161372654479578, -38.84013935494854763, 255.0901547344684559 ) ) ;
#20878 = EDGE_CURVE ( 'NONE', #60824, #30264, #46500, .T. ) ;
#20879 = AXIS2_PLACEMENT_3D ( 'NONE', #48285, #27863, #48734 ) ;
#20880 = DIRECTION ( 'NONE',  ( 0.000000000000000000, 0.000000000000000000, 1.000000000000000000 ) ) ;
#20881 = CARTESIAN_POINT ( 'NONE',  ( 193.5667039024416454, -48.82844715994099971, 180.4678068554150343 ) ) ;
#20882 = CIRCLE ( 'NONE', #36836, 5.041900000000001825 ) ;
#20883 = ADVANCED_FACE ( 'NONE', ( #43109 ), #70393, .F. ) ;
#20884 = CARTESIAN_POINT ( 'NONE',  ( 109.7248659292862385, -27.00080518209267311, 84.86479194192601483 ) ) ;
#20885 = CARTESIAN_POINT ( 'NONE',  ( 78.94931995840801164, 71.76236341257997253, -88.44575049335516326 ) ) ;
#20886 = VERTEX_POINT ( 'NONE', #37213 ) ;
#20887 = DIRECTION ( 'NONE',  ( 0.000000000000000000, -1.000000000000000000, 0.000000000000000000 ) ) ;
#20888 = CARTESIAN_POINT ( 'NONE',  ( 30.48091746481826192, -48.32844715994148999, 300.4678068554150059 ) ) ;
#20889 = EDGE_LOOP ( 'NONE', ( #25129, #42965, #21541, #52933 ) ) ;
#20890 = CARTESIAN_POINT ( 'NONE',  ( 101.1416012009399026, -28.10844496237015733, 50.55562527591095545 ) ) ;
#20891 = ORIENTED_EDGE ( 'NONE', *, *, #76871, .F. ) ;
#20892 = CARTESIAN_POINT ( 'NONE',  ( 105.5073833390055853, -45.15143093073633196, 11.85241982807799843 ) ) ;
#20893 = EDGE_CURVE ( 'NONE', #71132, #64360, #23842, .T. ) ;
#20894 = FACE_OUTER_BOUND ( 'NONE', #52033, .T. ) ;
#20895 = CARTESIAN_POINT ( 'NONE',  ( 114.0663967180213803, -29.08153105160599949, 154.4746728949589851 ) ) ;
#20896 = DIRECTION ( 'NONE',  ( -4.237773401492740281E-14, 1.000000000000000000, 0.000000000000000000 ) ) ;
#20897 = CARTESIAN_POINT ( 'NONE',  ( -46.60773131249376178, 91.07499999999996021, -44.42500552774628630 ) ) ;
#20898 = CARTESIAN_POINT ( 'NONE',  ( 97.81168895331838087, -40.51742574516882200, 9.635625275910941312 ) ) ;
#20899 = CARTESIAN_POINT ( 'NONE',  ( 4.935589585849590399, 70.84825094496120812, 130.4626753348074999 ) ) ;
#20900 = EDGE_CURVE ( 'NONE', #70808, #11319, #78123, .T. ) ;
#20901 = CARTESIAN_POINT ( 'NONE',  ( 117.5177603787924170, -36.12629959281294134, 224.8727681330539667 ) ) ;
#20902 = CARTESIAN_POINT ( 'NONE',  ( 75.00112839233754869, 87.03046781249436492, -91.81710919847664343 ) ) ;
#20903 = EDGE_LOOP ( 'NONE', ( #53382, #81746, #14366, #61792 ) ) ;
#20904 = CARTESIAN_POINT ( 'NONE',  ( 136.5663465660554721, -37.87725565067738387, 7.080220459966729329 ) ) ;
#20905 = EDGE_LOOP ( 'NONE', ( #71215, #52244, #63093, #24713 ) ) ;
#20906 = CARTESIAN_POINT ( 'NONE',  ( 95.98172161192206886, -37.30002307145830542, 117.3794347997199594 ) ) ;
#20907 = CARTESIAN_POINT ( 'NONE',  ( 121.4441796687513744, 45.58144993709862547, -47.92108811332148832 ) ) ;
#20908 = AXIS2_PLACEMENT_3D ( 'NONE', #42121, #6273, #63018 ) ;
#20909 = VECTOR ( 'NONE', #54302, 1000.000000000000000 ) ;
#20910 = ORIENTED_EDGE ( 'NONE', *, *, #79874, .T. ) ;
#20911 = EDGE_LOOP ( 'NONE', ( #38548, #39768, #27936 ) ) ;
#20912 = ORIENTED_EDGE ( 'NONE', *, *, #41642, .T. ) ;
#20913 = CIRCLE ( 'NONE', #52816, 2.517499999999998739 ) ;
#20914 = DIRECTION ( 'NONE',  ( 0.000000000000000000, 1.000000000000000000, 0.000000000000000000 ) ) ;
#20915 = CARTESIAN_POINT ( 'NONE',  ( 182.2420472961719895, -31.76306994223730840, -5.074374724088000832 ) ) ;
#20916 = CARTESIAN_POINT ( 'NONE',  ( 0.000000000000000000, 44.45000000000000284, 130.5560000000000116 ) ) ;
#20917 = LINE ( 'NONE', #48588, #28717 ) ;
#20918 = CARTESIAN_POINT ( 'NONE',  ( 106.9948502263972188, -44.89183619263916825, 185.3880903695919642 ) ) ;
#20919 = CARTESIAN_POINT ( 'NONE',  ( 100.0093689611455687, -28.97871315454919028, 281.6641967044822650 ) ) ;
#20921 = EDGE_CURVE ( 'NONE', #14315, #19682, #84278, .T. ) ;
#20920 = CARTESIAN_POINT ( 'NONE',  ( 113.1765051245399860, -44.75320790169451612, 59.09377906252450430 ) ) ;
#20922 = EDGE_LOOP ( 'NONE', ( #14212, #38232 ) ) ;
#20923 = DIRECTION ( 'NONE',  ( 0.000000000000000000, -1.000000000000000000, 0.000000000000000000 ) ) ;
#20924 = ADVANCED_FACE ( 'NONE', ( #13425 ), #6603, .T. ) ;
#20925 = DIRECTION ( 'NONE',  ( 0.7071067811865389130, 0.000000000000000000, 0.7071067811865561215 ) ) ;
#20926 = ORIENTED_EDGE ( 'NONE', *, *, #46869, .F. ) ;
#20927 = ORIENTED_EDGE ( 'NONE', *, *, #51395, .F. ) ;
#20928 = CARTESIAN_POINT ( 'NONE',  ( 31.56670390244800828, -32.29483332968611364, -5.074374724088000832 ) ) ;
#20929 = LINE ( 'NONE', #40470, #58479 ) ;
#20930 = CARTESIAN_POINT ( 'NONE',  ( 97.78482178150787263, -40.45120638126190471, 16.62993809196701989 ) ) ;
#20931 = DIRECTION ( 'NONE',  ( 0.000000000000000000, 1.000000000000000000, 0.000000000000000000 ) ) ;
#20932 = CARTESIAN_POINT ( 'NONE',  ( 107.0664832912750057, -36.72944715993903486, 0.4256252759109709349 ) ) ;
#20933 = CARTESIAN_POINT ( 'NONE',  ( 115.3666750469823938, -34.71377145672549602, 208.4381341137909658 ) ) ;
#20934 = CARTESIAN_POINT ( 'NONE',  ( 97.24697957573494023, -33.09846756419045022, 66.04419670448297097 ) ) ;
#20935 = FACE_BOUND ( 'NONE', #62365, .T. ) ;
#20936 = VERTEX_POINT ( 'NONE', #82486 ) ;
#20937 = CARTESIAN_POINT ( 'NONE',  ( 91.06648329127391150, -36.72944715993925513, -4.074374724089044442 ) ) ;
#20938 = EDGE_LOOP ( 'NONE', ( #16192, #20912 ) ) ;
#20939 = DIRECTION ( 'NONE',  ( 0.000000000000000000, 0.000000000000000000, 1.000000000000000000 ) ) ;
#20940 = ORIENTED_EDGE ( 'NONE', *, *, #36965, .F. ) ;
#20941 = DIRECTION ( 'NONE',  ( -6.524622321627019585E-16, -4.013151879589939944E-16, -1.000000000000000000 ) ) ;
#20942 = CARTESIAN_POINT ( 'NONE',  ( 149.4532656544376721, -72.54365454176046057, 361.9756252759100335 ) ) ;
#20943 = CARTESIAN_POINT ( 'NONE',  ( 67.06670390244700286, -67.87641945813885513, 245.9001325644979659 ) ) ;
#20945 = EDGE_CURVE ( 'NONE', #20334, #56957, #48355, .T. ) ;
#20944 = CIRCLE ( 'NONE', #49974, 2.116999999999993776 ) ;
#20946 = PLANE ( 'NONE',  #87261 ) ;
#20947 = EDGE_LOOP ( 'NONE', ( #76052, #52346, #22493, #87440 ) ) ;
#20948 = CARTESIAN_POINT ( 'NONE',  ( 98.70474251149389033, -42.99264563182325816, 66.83848241876793850 ) ) ;
#20949 = AXIS2_PLACEMENT_3D ( 'NONE', #7207, #68536, #41252 ) ;
#20951 = CARTESIAN_POINT ( 'NONE',  ( -479.3614999999999782, 100.8062500000000057, 94.61194598552329182 ) ) ;
#20950 = DIRECTION ( 'NONE',  ( -0.000000000000000000, -1.000000000000000000, -0.000000000000000000 ) ) ;
#20952 = CARTESIAN_POINT ( 'NONE',  ( 50.96943157740487607, -34.03355364506408165, 193.9678068554150911 ) ) ;
#20953 = CARTESIAN_POINT ( 'NONE',  ( 177.4809174648213173, -48.32844715993478957, 300.4678068554149490 ) ) ;
#20954 = ORIENTED_EDGE ( 'NONE', *, *, #26490, .F. ) ;
#20955 = CARTESIAN_POINT ( 'NONE',  ( 114.6040617491220246, -30.10671728496298627, 120.3995749443976706 ) ) ;
#20956 = LINE ( 'NONE', #27768, #38547 ) ;
#20957 = CARTESIAN_POINT ( 'NONE',  ( -194.1576000000000022, 0.000000000000000000, 146.9389999999999930 ) ) ;
#20958 = ORIENTED_EDGE ( 'NONE', *, *, #39616, .T. ) ;
#20959 = CARTESIAN_POINT ( 'NONE',  ( 117.1846329980857178, -34.12938843674525202, 120.0270538473389479 ) ) ;
#20961 = DIRECTION ( 'NONE',  ( 0.000000000000000000, -0.8660254037844382635, -0.5000000000000008882 ) ) ;
#20960 = CARTESIAN_POINT ( 'NONE',  ( 53.97500000000000142, 95.25000000000000000, 283.4005000000000223 ) ) ;
#20962 = DIRECTION ( 'NONE',  ( -1.000000000000000000, 0.000000000000000000, 0.000000000000000000 ) ) ;
#20963 = EDGE_CURVE ( 'NONE', #75262, #25396, #62459, .T. ) ;
#20964 = VECTOR ( 'NONE', #54038, 1000.000000000000000 ) ;
#20965 = CIRCLE ( 'NONE', #79013, 3.249999999999975131 ) ;
#20966 = AXIS2_PLACEMENT_3D ( 'NONE', #82664, #40839, #68116 ) ;
#20967 = AXIS2_PLACEMENT_3D ( 'NONE', #59679, #86084, #72005 ) ;
#20968 = EDGE_CURVE ( 'NONE', #85809, #1145, #56071, .T. ) ;
#20969 = CARTESIAN_POINT ( 'NONE',  ( 67.06673837846007302, -137.6758525980020806, 245.5072637273240161 ) ) ;
#20970 = ORIENTED_EDGE ( 'NONE', *, *, #17666, .F. ) ;
#20971 = EDGE_CURVE ( 'NONE', #35428, #23949, #39258, .T. ) ;
#20972 = CARTESIAN_POINT ( 'NONE',  ( 102.8912152862170188, -46.22186109533342346, 128.2346728949579528 ) ) ;
#20974 = EDGE_LOOP ( 'NONE', ( #41322, #18545, #1289, #74943 ) ) ;
#20973 = CARTESIAN_POINT ( 'NONE',  ( 32.16397622746000451, -34.03355364505800651, 237.4678068554150059 ) ) ;
#20975 = AXIS2_PLACEMENT_3D ( 'NONE', #82304, #45936, #18706 ) ;
#20977 = ADVANCED_FACE ( 'NONE', ( #1143 ), #89742, .F. ) ;
#20976 = AXIS2_PLACEMENT_3D ( 'NONE', #17302, #23680, #78656 ) ;
#20978 = CARTESIAN_POINT ( 'NONE',  ( 115.7579298488886224, -31.01215564512775558, 250.2899109901966028 ) ) ;
#20979 = CARTESIAN_POINT ( 'NONE',  ( 162.5667039024470171, -32.29483332968611364, -5.074374724088000832 ) ) ;
#20980 = DIRECTION ( 'NONE',  ( 0.000000000000000000, 0.000000000000000000, -1.000000000000000000 ) ) ;
#20981 = CARTESIAN_POINT ( 'NONE',  ( 92.53858863555680614, -80.85146542362646471, 250.2178068554180470 ) ) ;
#20982 = DIRECTION ( 'NONE',  ( 0.000000000000000000, -1.000000000000000000, 0.000000000000000000 ) ) ;
#20983 = DIRECTION ( 'NONE',  ( 0.000000000000000000, 0.000000000000000000, -1.000000000000000000 ) ) ;
#20984 = FACE_OUTER_BOUND ( 'NONE', #55248, .T. ) ;
#20985 = CARTESIAN_POINT ( 'NONE',  ( 107.6181574201208662, -47.08485352040301564, 197.6308633711499567 ) ) ;
#20986 = EDGE_LOOP ( 'NONE', ( #21669, #76286, #23296, #57582 ) ) ;
#20987 = ORIENTED_EDGE ( 'NONE', *, *, #68381, .F. ) ;
#20988 = CARTESIAN_POINT ( 'NONE',  ( 115.8989637469753831, -39.93316602039875107, 169.9692023535169483 ) ) ;
#20989 = EDGE_CURVE ( 'NONE', #24368, #74810, #18969, .T. ) ;
#20990 = CYLINDRICAL_SURFACE ( 'NONE', #11033, 7.937500000000000000 ) ;
#20991 = CARTESIAN_POINT ( 'NONE',  ( 110.4493835822141676, -45.49486465592072904, 14.28920235351599466 ) ) ;
#20992 = DIRECTION ( 'NONE',  ( 0.000000000000000000, 1.000000000000000000, 0.000000000000000000 ) ) ;
#20993 = ADVANCED_FACE ( 'NONE', ( #48808 ), #83366, .T. ) ;
#20994 = CARTESIAN_POINT ( 'NONE',  ( 108.3328345498486414, -46.73492894964222444, 267.6773957667126069 ) ) ;
#20995 = CARTESIAN_POINT ( 'NONE',  ( -24.20305689751608824, 53.97499999999997300, 58.62596543806478877 ) ) ;
#20996 = FACE_OUTER_BOUND ( 'NONE', #80597, .T. ) ;
#20997 = CARTESIAN_POINT ( 'NONE',  ( 107.0667039024470313, -104.2784471599409528, 25.71780685541800437 ) ) ;
#20998 = CARTESIAN_POINT ( 'NONE',  ( 96.87985868497418096, -34.61725761836211035, 216.1641967044819808 ) ) ;
#20999 = CARTESIAN_POINT ( 'NONE',  ( 86.06670390244796920, -50.82844715994100682, 198.9178068554149945 ) ) ;
#21000 = ORIENTED_EDGE ( 'NONE', *, *, #19752, .T. ) ;
#21001 = EDGE_LOOP ( 'NONE', ( #63353, #80425, #64683, #36779 ) ) ;
#21002 = EDGE_CURVE ( 'NONE', #73956, #12535, #33856, .T. ) ;
#21003 = DIRECTION ( 'NONE',  ( -1.000000000000000000, 0.000000000000000000, 0.000000000000000000 ) ) ;
#21004 = CARTESIAN_POINT ( 'NONE',  ( -90.81826664112017511, 89.94786999841838337, -76.20774946062876154 ) ) ;
#21005 = DIRECTION ( 'NONE',  ( 0.000000000000000000, -1.000000000000000000, 0.000000000000000000 ) ) ;
#21006 = LINE ( 'NONE', #61874, #47648 ) ;
#21007 = AXIS2_PLACEMENT_3D ( 'NONE', #37054, #24321, #2094 ) ;
#21008 = CARTESIAN_POINT ( 'NONE',  ( 107.0667039024470313, -119.4690460831836276, -21.78219314458154798 ) ) ;
#21009 = ORIENTED_EDGE ( 'NONE', *, *, #39155, .T. ) ;
#21010 = DIRECTION ( 'NONE',  ( -4.194175870806139918E-14, 1.000000000000000000, 0.000000000000000000 ) ) ;
#21011 = AXIS2_PLACEMENT_3D ( 'NONE', #38036, #65727, #3509 ) ;
#21012 = CARTESIAN_POINT ( 'NONE',  ( 112.4544618167839332, -45.69580618038663999, 238.0070538473389377 ) ) ;
#21013 = ORIENTED_EDGE ( 'NONE', *, *, #78008, .T. ) ;
#21014 = CARTESIAN_POINT ( 'NONE',  ( -254.0000000000000000, 14.28749999999982201, 95.25000000000000000 ) ) ;
#21015 = DIRECTION ( 'NONE',  ( -1.000000000000000078E-15, 1.000000000000000083E-30, 1.000000000000000000 ) ) ;
#21016 = DIRECTION ( 'NONE',  ( -6.878358445406130340E-15, 0.000000000000000000, 1.000000000000000000 ) ) ;
#21017 = CARTESIAN_POINT ( 'NONE',  ( 112.7718126367562093, -42.56716444297848767, 71.01094751244896486 ) ) ;
#21018 = CARTESIAN_POINT ( 'NONE',  ( 109.8617963350518920, -26.66349048206837580, 170.8613395616249591 ) ) ;
#21019 = DIRECTION ( 'NONE',  ( -0.000000000000000000, -0.000000000000000000, 1.000000000000000000 ) ) ;
#21020 = ORIENTED_EDGE ( 'NONE', *, *, #76862, .T. ) ;
#21021 = B_SPLINE_CURVE_WITH_KNOTS ( 'NONE', 3,
 ( #781, #55708, #75298, #83024, #56169, #28478, #14424, #42104, #33945, #83919, #40762, #70270, #68484, #34849, #27145, #82582, #49363, #48009 ),
 .UNSPECIFIED., .F., .F.,
 ( 4, 2, 2, 2, 2, 2, 2, 2, 4 ),
 ( 0.000000000000000000, 0.06250000000899012809, 0.1250000000179802562, 0.1875000000269703704, 0.2500000000359605123, 0.3125000000449506543, 0.3750000000539407408, 0.4375000000629308827, 0.5000000000719210247 ),
 .UNSPECIFIED. ) ;
#21022 = ADVANCED_FACE ( 'NONE', ( #49266, #15219 ), #21593, .F. ) ;
#21023 = DIRECTION ( 'NONE',  ( 0.000000000000000000, 0.000000000000000000, -1.000000000000000000 ) ) ;
#21024 = ORIENTED_EDGE ( 'NONE', *, *, #4534, .F. ) ;
#21025 = ORIENTED_EDGE ( 'NONE', *, *, #67620, .T. ) ;
#21026 = VECTOR ( 'NONE', #45008, 1000.000000000000000 ) ;
#21027 = CIRCLE ( 'NONE', #84850, 2.000000000000007550 ) ;
#21028 = PLANE ( 'NONE',  #8220 ) ;
#21029 = VECTOR ( 'NONE', #73367, 1000.000000000000000 ) ;
#21030 = EDGE_LOOP ( 'NONE', ( #81612, #49676, #4868, #40425 ) ) ;
#21031 = VERTEX_POINT ( 'NONE', #14327 ) ;
#21032 = DIRECTION ( 'NONE',  ( 0.7071067811578790607, 0.7071067812152160847, 0.000000000000000000 ) ) ;
#21033 = AXIS2_PLACEMENT_3D ( 'NONE', #18220, #40000, #81372 ) ;
#21034 = CARTESIAN_POINT ( 'NONE',  ( 102.7155009198991280, -28.78705314239651969, 99.88575316140996563 ) ) ;
#21036 = CARTESIAN_POINT ( 'NONE',  ( 97.14868559305091367, -40.01329441332335790, 241.5813395616249863 ) ) ;
#21035 = CIRCLE ( 'NONE', #25436, 3.174999999999983391 ) ;
#21037 = VECTOR ( 'NONE', #76836, 1000.000000000000000 ) ;
#21038 = CARTESIAN_POINT ( 'NONE',  ( 96.69582475441069391, -35.54038568221476879, 206.2356252759109623 ) ) ;
#21039 = CARTESIAN_POINT ( 'NONE',  ( 117.9019101119219357, -41.46671778014663801, 54.49848241876792088 ) ) ;
#21040 = DIRECTION ( 'NONE',  ( -4.554376769437570034E-14, 1.000000000000000000, 0.000000000000000000 ) ) ;
#21041 = CARTESIAN_POINT ( 'NONE',  ( 126.0667039024479550, -14.72944715994094977, 199.5838068554170093 ) ) ;
#21042 = EDGE_CURVE ( 'NONE', #46235, #10839, #76942, .T. ) ;
#21043 = VERTEX_POINT ( 'NONE', #62007 ) ;
#21044 = CARTESIAN_POINT ( 'NONE',  ( 92.91125933621933086, -94.95109689075242443, -19.26696060647628528 ) ) ;
#21045 = CARTESIAN_POINT ( 'NONE',  ( 70.06968321367156705, -140.6784088069870222, 245.5331728854790185 ) ) ;
#21046 = VECTOR ( 'NONE', #75495, 1000.000000000000000 ) ;
#21047 = CARTESIAN_POINT ( 'NONE',  ( 102.0112516875887252, -27.67497761899947406, 105.4937205140069665 ) ) ;
#21048 = ADVANCED_FACE ( 'NONE', ( #56532 ), #680, .F. ) ;
#21049 = CARTESIAN_POINT ( 'NONE',  ( 99.46959489307312197, -43.93319290153426238, 81.92991099019597812 ) ) ;
#21050 = CARTESIAN_POINT ( 'NONE',  ( 106.5652189068774902, -47.22232703829767786, 247.5384824187679556 ) ) ;
#21051 = ORIENTED_EDGE ( 'NONE', *, *, #54255, .F. ) ;
#21052 = CARTESIAN_POINT ( 'NONE',  ( 107.2492389712779612, -24.88009754917498739, 230.0641967044819580 ) ) ;
#21053 = DIRECTION ( 'NONE',  ( -1.000000000000000000, 0.000000000000000000, 0.000000000000000000 ) ) ;
#21054 = CARTESIAN_POINT ( 'NONE',  ( 116.3274949261486881, -32.94048995676258329, 25.13562527591095375 ) ) ;
#21055 = CARTESIAN_POINT ( 'NONE',  ( 98.05794652679882972, -41.07680959571720081, 27.68475610168817269 ) ) ;
#21056 = CIRCLE ( 'NONE', #3607, 3.174999999999983391 ) ;
#21058 = CYLINDRICAL_SURFACE ( 'NONE', #51426, 2.517500000000000071 ) ;
#21057 = CARTESIAN_POINT ( 'NONE',  ( 107.8140391369254019, -46.65806076900804555, 277.6356252759110816 ) ) ;
#21059 = CARTESIAN_POINT ( 'NONE',  ( 25.56670390244829250, -48.82844715994168183, 290.7178068554150059 ) ) ;
#21060 = DIRECTION ( 'NONE',  ( -0.7071067811865433539, -0.7071067811865516806, -7.071067811865440820E-16 ) ) ;
#21061 = PLANE ( 'NONE',  #60010 ) ;
#21062 = CARTESIAN_POINT ( 'NONE',  ( -64.50026246089650783, 148.4450814996825443, 59.61038444174924678 ) ) ;
#21063 = CARTESIAN_POINT ( 'NONE',  ( 105.7925720156200384, -26.72498208092823546, 40.17704486214662296 ) ) ;
#21064 = CARTESIAN_POINT ( 'NONE',  ( 33.92127028473601769, -29.73316016639540749, -5.074374724088000832 ) ) ;
#21066 = EDGE_LOOP ( 'NONE', ( #68230, #31169 ) ) ;
#21065 = DIRECTION ( 'NONE',  ( 1.000000000000000078E-15, -1.000000000000000000, 0.000000000000000000 ) ) ;
#21067 = DIRECTION ( 'NONE',  ( -1.000000000000000078E-15, 1.000000000000000083E-30, 1.000000000000000000 ) ) ;
#21068 = CARTESIAN_POINT ( 'NONE',  ( 97.20287302226383019, -40.27875065248429820, 266.6013395616254797 ) ) ;
#21069 = CARTESIAN_POINT ( 'NONE',  ( 96.67093460706618657, -35.94617138369610387, 142.2670538473399517 ) ) ;
#21070 = CARTESIAN_POINT ( 'NONE',  ( 96.76602677561474763, -40.86443131079876423, 247.6422919425769749 ) ) ;
#21071 = DIRECTION ( 'NONE',  ( 0.000000000000000000, -1.000000000000000000, 5.463695987328529395E-16 ) ) ;
#21073 = CARTESIAN_POINT ( 'NONE',  ( 82.15318967142708573, -34.93816060011965163, 7.482180659748648210 ) ) ;
#21072 = CARTESIAN_POINT ( 'NONE',  ( 128.0667039024480118, -50.82844715994100682, 57.91780685541508689 ) ) ;
#21074 = CARTESIAN_POINT ( 'NONE',  ( 117.0718980089568078, -35.46249550098277581, 139.9272908994846034 ) ) ;
#21075 = VECTOR ( 'NONE', #7961, 1000.000000000000000 ) ;
#21076 = FACE_OUTER_BOUND ( 'NONE', #17438, .T. ) ;
#21077 = AXIS2_PLACEMENT_3D ( 'NONE', #53538, #12241, #17720 ) ;
#21078 = EDGE_LOOP ( 'NONE', ( #63838, #10809 ) ) ;
#21079 = DIRECTION ( 'NONE',  ( -0.000000000000000000, 0.4999999999999985567, 0.8660254037844394848 ) ) ;
#21080 = ORIENTED_EDGE ( 'NONE', *, *, #6616, .T. ) ;
#21081 = EDGE_CURVE ( 'NONE', #79856, #26963, #42103, .T. ) ;
#21082 = CARTESIAN_POINT ( 'NONE',  ( 107.4755550402934148, -45.77628807984756065, 192.0228960185529559 ) ) ;
#21084 = ORIENTED_EDGE ( 'NONE', *, *, #18409, .T. ) ;
#21083 = CARTESIAN_POINT ( 'NONE',  ( 91.91125933621933086, -96.68314769832132072, -19.26696060647622843 ) ) ;
#21085 = DIRECTION ( 'NONE',  ( -3.100000000000000258E-29, 3.100000000000000044E-14, 1.000000000000000000 ) ) ;
#21086 = EDGE_CURVE ( 'NONE', #22615, #7080, #41548, .T. ) ;
#21087 = CARTESIAN_POINT ( 'NONE',  ( 116.7861719071672155, -43.46560779248400763, 159.3441967044829539 ) ) ;
#21088 = FACE_OUTER_BOUND ( 'NONE', #42471, .T. ) ;
#21089 = CARTESIAN_POINT ( 'NONE',  ( 70.96339109104607701, -139.0938916433960912, 247.5000110694289788 ) ) ;
#21090 = PLANE ( 'NONE',  #34186 ) ;
#21091 = CARTESIAN_POINT ( 'NONE',  ( -91.11526841082567785, 75.84278307195157254, 75.85240403722379199 ) ) ;
#21092 = EDGE_CURVE ( 'NONE', #32624, #3091, #27937, .T. ) ;
#21093 = CARTESIAN_POINT ( 'NONE',  ( -28.99999999999997513, 127.0000000000000000, 183.8826257785461280 ) ) ;
#21094 = CARTESIAN_POINT ( 'NONE',  ( 102.8368274790082921, -27.91052165842129185, 95.43276813305395478 ) ) ;
#21095 = VERTEX_POINT ( 'NONE', #35190 ) ;
#21096 = ORIENTED_EDGE ( 'NONE', *, *, #30413, .F. ) ;
#21097 = ORIENTED_EDGE ( 'NONE', *, *, #20630, .F. ) ;
#21098 = AXIS2_PLACEMENT_3D ( 'NONE', #18738, #39179, #73706 ) ;
#21099 = CARTESIAN_POINT ( 'NONE',  ( 99.16631175631914630, -32.71502711089942039, 47.38444044875394923 ) ) ;
#21100 = EDGE_CURVE ( 'NONE', #22667, #18476, #18515, .T. ) ;
#21101 = AXIS2_PLACEMENT_3D ( 'NONE', #15171, #1990, #35599 ) ;
#21102 = DIRECTION ( 'NONE',  ( -9.437404618277395057E-08, 0.000000000000000000, -0.9999999999999955591 ) ) ;
#21103 = AXIS2_PLACEMENT_3D ( 'NONE', #49227, #35156, #41964 ) ;
#21105 = PLANE ( 'NONE',  #81102 ) ;
#21104 = CARTESIAN_POINT ( 'NONE',  ( 109.2982854457139297, -26.60236246699155416, 175.8918157521009391 ) ) ;
#21106 = CARTESIAN_POINT ( 'NONE',  ( 70.56670390244700286, -67.87844715994098976, 222.2178068554179902 ) ) ;
#21107 = DIRECTION ( 'NONE',  ( 0.000000000000000000, -1.000000000000000000, 0.000000000000000000 ) ) ;
#21108 = ADVANCED_FACE ( 'NONE', ( #26050 ), #60093, .F. ) ;
#21110 = DIRECTION ( 'NONE',  ( 1.000000000000000000, 3.083952846180989689E-15, 1.541976423090494844E-15 ) ) ;
#21109 = AXIS2_PLACEMENT_3D ( 'NONE', #81084, #18835, #46517 ) ;
#21111 = CARTESIAN_POINT ( 'NONE',  ( 67.84300328633237598, -68.62291849891890649, 247.0791910793475381 ) ) ;
#21112 = CARTESIAN_POINT ( 'NONE',  ( 95.80265872640100611, -40.33145541733363615, 131.5727681330539554 ) ) ;
#21113 = EDGE_LOOP ( 'NONE', ( #62877, #63981, #18552, #20693 ) ) ;
#21114 = ORIENTED_EDGE ( 'NONE', *, *, #4713, .T. ) ;
#21115 = EDGE_LOOP ( 'NONE', ( #12510, #9408, #70796, #26825 ) ) ;
#21116 = VECTOR ( 'NONE', #1314, 1000.000000000000114 ) ;
#21117 = CARTESIAN_POINT ( 'NONE',  ( -41.60202597009397607, 65.59999999999998010, 50.85338361873603219 ) ) ;
#21118 = CARTESIAN_POINT ( 'NONE',  ( 145.6879805935534478, -69.19066990707743514, 247.4001512595007739 ) ) ;
#21119 = DIRECTION ( 'NONE',  ( -3.100000000000000258E-29, 3.100000000000000044E-14, 1.000000000000000000 ) ) ;
#21121 = CARTESIAN_POINT ( 'NONE',  ( 102.4736563324128440, -43.47745920372498318, 194.9195189410199589 ) ) ;
#21120 = AXIS2_PLACEMENT_3D ( 'NONE', #41284, #28109, #75388 ) ;
#21122 = CARTESIAN_POINT ( 'NONE',  ( 49.21213752016101495, -29.73316016639650172, -5.074374724088000832 ) ) ;
#21123 = AXIS2_PLACEMENT_3D ( 'NONE', #41484, #70107, #49193 ) ;
#21124 = DIRECTION ( 'NONE',  ( 1.000000000000000000, 2.999999999999999839E-15, 1.000000000000000078E-15 ) ) ;
#21125 = ORIENTED_EDGE ( 'NONE', *, *, #70831, .F. ) ;
#21127 = ORIENTED_EDGE ( 'NONE', *, *, #31423, .T. ) ;
#21126 = VERTEX_POINT ( 'NONE', #52370 ) ;
#21128 = CARTESIAN_POINT ( 'NONE',  ( 20.03715912545735378, -24.42818131006189830, 249.9678068554150059 ) ) ;
#21129 = ORIENTED_EDGE ( 'NONE', *, *, #35470, .F. ) ;
#21130 = VERTEX_POINT ( 'NONE', #4714 ) ;
#21131 = CARTESIAN_POINT ( 'NONE',  ( 162.5667039024460223, -19.82844715994111340, 342.9256252759119548 ) ) ;
#21132 = VECTOR ( 'NONE', #57382, 1000.000000000000000 ) ;
#21133 = CARTESIAN_POINT ( 'NONE',  ( 114.5810018449060834, -31.08954144758037685, 260.7825356868496556 ) ) ;
#21134 = CARTESIAN_POINT ( 'NONE',  ( 115.0893015243264443, -30.61815127115607638, 180.3443299114694582 ) ) ;
#21135 = VERTEX_POINT ( 'NONE', #12419 ) ;
#21136 = ADVANCED_FACE ( 'NONE', ( #33307 ), #53686, .F. ) ;
#21137 = CARTESIAN_POINT ( 'NONE',  ( 131.3164832912739826, -18.72944715994100662, -5.074374724089004474 ) ) ;
#21138 = VECTOR ( 'NONE', #52170, 1000.000000000000000 ) ;
#21139 = CARTESIAN_POINT ( 'NONE',  ( -120.0114297908194203, 74.60389011813707327, 51.40169094214619605 ) ) ;
#21140 = ORIENTED_EDGE ( 'NONE', *, *, #63109, .T. ) ;
#21141 = EDGE_LOOP ( 'NONE', ( #37884, #6611, #89541, #30408 ) ) ;
#21142 = CARTESIAN_POINT ( 'NONE',  ( 63.03715912545730760, -24.42818131006027826, 300.4678068554150627 ) ) ;
#21143 = VECTOR ( 'NONE', #54271, 1000.000000000000000 ) ;
#21144 = VERTEX_POINT ( 'NONE', #86942 ) ;
#21145 = EDGE_LOOP ( 'NONE', ( #9357, #70152, #76040, #52596 ) ) ;
#21146 = EDGE_CURVE ( 'NONE', #53629, #3324, #88558, .T. ) ;
#21147 = CARTESIAN_POINT ( 'NONE',  ( 109.3549613941650875, -28.89410453886290142, 257.6680903695913685 ) ) ;
#21148 = CARTESIAN_POINT ( 'NONE',  ( 117.2310933634200012, -39.29246586887208537, 123.6299109901969615 ) ) ;
#21149 = CARTESIAN_POINT ( 'NONE',  ( 117.3423061886548879, -38.35306328171704848, 113.7013395616249767 ) ) ;
#21150 = CARTESIAN_POINT ( 'NONE',  ( 204.2160000000000082, 52.73749999999999716, -44.45000000000000284 ) ) ;
#21151 = DIRECTION ( 'NONE',  ( 0.7071067811865560104, 0.000000000000000000, -0.7071067811865391350 ) ) ;
#21152 = CARTESIAN_POINT ( 'NONE',  ( 112.2050260072902290, -45.80016191694880234, 208.9870538473389558 ) ) ;
#21153 = CARTESIAN_POINT ( 'NONE',  ( 41.56670390244783420, -36.32844715994104234, 249.9678068554150343 ) ) ;
#21154 = DIRECTION ( 'NONE',  ( 0.000000000000000000, 0.000000000000000000, -1.000000000000000000 ) ) ;
#21155 = EDGE_LOOP ( 'NONE', ( #56642, #50261, #64458, #32963 ) ) ;
#21156 = CARTESIAN_POINT ( 'NONE',  ( -130.1663562161751599, 74.81660785136578795, 10.08264331121449153 ) ) ;
#21157 = ORIENTED_EDGE ( 'NONE', *, *, #53457, .T. ) ;
#21158 = ORIENTED_EDGE ( 'NONE', *, *, #24792, .F. ) ;
#21159 = CARTESIAN_POINT ( 'NONE',  ( 41.56648329127399677, 0.2215528400590013880, 78.92562527591199739 ) ) ;
#21160 = VECTOR ( 'NONE', #25899, 1000.000000000000000 ) ;
#21161 = CARTESIAN_POINT ( 'NONE',  ( 97.07204692338113716, -35.37868373995705440, 137.2189094707525783 ) ) ;
#21162 = EDGE_CURVE ( 'NONE', #61542, #63618, #40108, .T. ) ;
#21163 = AXIS2_PLACEMENT_3D ( 'NONE', #39957, #25893, #89016 ) ;
#21164 = VECTOR ( 'NONE', #5920, 1000.000000000000000 ) ;
#21165 = CARTESIAN_POINT ( 'NONE',  ( 102.0817216996469483, -27.57306688727539168, 145.4727681330539610 ) ) ;
#21166 = CARTESIAN_POINT ( 'NONE',  ( -8.235690233012341821, 72.87934159340741758, 130.2959689530747767 ) ) ;
#21167 = AXIS2_PLACEMENT_3D ( 'NONE', #74609, #88707, #4683 ) ;
#21168 = CARTESIAN_POINT ( 'NONE',  ( 130.5667039024480118, -35.47069715994093997, 218.8274735512161158 ) ) ;
#21169 = CARTESIAN_POINT ( 'NONE',  ( 152.0371591254583450, -47.82818131005588214, 249.9678068554149490 ) ) ;
#21172 = CARTESIAN_POINT ( 'NONE',  ( 112.1942863616535817, -45.78120396183486918, 208.9870538473389558 ) ) ;
#21171 = DIRECTION ( 'NONE',  ( -1.000000000000000000, 0.000000000000000000, -1.748382715945130353E-14 ) ) ;
#21170 = CARTESIAN_POINT ( 'NONE',  ( 125.0664832912740110, -18.82844715994099971, 284.9256252759119548 ) ) ;
#21173 = CARTESIAN_POINT ( 'NONE',  ( 138.0667039024480403, -58.72944715994091069, 239.5838068554170377 ) ) ;
#21174 = DIRECTION ( 'NONE',  ( 0.000000000000000000, -1.000000000000000000, 0.000000000000000000 ) ) ;
#21175 = ORIENTED_EDGE ( 'NONE', *, *, #40460, .T. ) ;
#21176 = B_SPLINE_CURVE_WITH_KNOTS ( 'NONE', 3,
 ( #67950, #87953, #47931, #75671 ),
 .UNSPECIFIED., .F., .F.,
 ( 4, 4 ),
 ( -0.6035999334370389935, -0.5903216970416030884 ),
 .UNSPECIFIED. ) ;
#21177 = LINE ( 'NONE', #34791, #48340 ) ;
#21178 = CARTESIAN_POINT ( 'NONE',  ( 91.91441891875214765, -111.9861225405538505, -11.78219314458175937 ) ) ;
#21179 = PLANE ( 'NONE',  #931 ) ;
#21180 = CARTESIAN_POINT ( 'NONE',  ( 141.0664832912739826, -8.729447159940995959, 14.67562527591100441 ) ) ;
#21182 = VERTEX_POINT ( 'NONE', #31958 ) ;
#21181 = CARTESIAN_POINT ( 'NONE',  ( 111.7588773036880383, -27.37059502548119028, 279.7070538473396937 ) ) ;
#21183 = FACE_OUTER_BOUND ( 'NONE', #81932, .T. ) ;
#21184 = CARTESIAN_POINT ( 'NONE',  ( 114.2686970495659295, -44.29742072815643184, 158.1813395616249807 ) ) ;
#21185 = CARTESIAN_POINT ( 'NONE',  ( 100.5507766775973835, -27.80086676837388637, 26.56610146638793779 ) ) ;
#21186 = CARTESIAN_POINT ( 'NONE',  ( 117.4696809092536256, -30.95150704042223211, 175.2299109901969700 ) ) ;
#21187 = CARTESIAN_POINT ( 'NONE',  ( -31.75000000000000000, 111.1250000000000000, -3.175000000000219647 ) ) ;
#21188 = DIRECTION ( 'NONE',  ( 0.000000000000000000, -1.000000000000000000, 0.000000000000000000 ) ) ;
#21190 = CARTESIAN_POINT ( 'NONE',  ( 77.39114642429960611, 120.6499999999999915, -71.77848634863110533 ) ) ;
#21189 = CARTESIAN_POINT ( 'NONE',  ( 208.9149999999999920, 28.98850000000000193, -7.937500000000000000 ) ) ;
#21191 = CARTESIAN_POINT ( 'NONE',  ( 193.0371591254584303, -47.82818131005411999, 249.9678068554149775 ) ) ;
#21192 = CARTESIAN_POINT ( 'NONE',  ( 116.3212776292296127, -32.94146857471318413, 287.6356252759109680 ) ) ;
#21193 = ORIENTED_EDGE ( 'NONE', *, *, #19744, .F. ) ;
#21194 = DIRECTION ( 'NONE',  ( 0.000000000000000000, 0.000000000000000000, -1.000000000000000000 ) ) ;
#21195 = VECTOR ( 'NONE', #53548, 1000.000000000000000 ) ;
#21196 = ORIENTED_EDGE ( 'NONE', *, *, #62757, .F. ) ;
#21197 = ORIENTED_EDGE ( 'NONE', *, *, #42362, .F. ) ;
#21198 = ADVANCED_FACE ( 'NONE', ( #46465 ), #46910, .T. ) ;
#21199 = EDGE_LOOP ( 'NONE', ( #15903, #28115, #63679, #5551 ) ) ;
#21200 = CARTESIAN_POINT ( 'NONE',  ( 117.2454586689011364, -38.87819698039182015, 59.66133956162595098 ) ) ;
#21201 = CARTESIAN_POINT ( 'NONE',  ( 107.0667039024470313, -104.2784471599413791, 2.217806855418003043 ) ) ;
#21202 = EDGE_CURVE ( 'NONE', #84828, #55699, #66932, .T. ) ;
#21203 = FACE_OUTER_BOUND ( 'NONE', #6442, .T. ) ;
#21204 = CARTESIAN_POINT ( 'NONE',  ( 111.4354466870268539, -47.79847022207366081, 168.8756252759109486 ) ) ;
#21205 = ADVANCED_FACE ( 'NONE', ( #74203 ), #67825, .F. ) ;
#21206 = CARTESIAN_POINT ( 'NONE',  ( 105.0359719168109933, -28.43277227512634298, 284.6895626852196415 ) ) ;
#21207 = AXIS2_PLACEMENT_3D ( 'NONE', #44900, #23162, #38101 ) ;
#21208 = ORIENTED_EDGE ( 'NONE', *, *, #23044, .T. ) ;
#21209 = ORIENTED_EDGE ( 'NONE', *, *, #9520, .T. ) ;
#21210 = ORIENTED_EDGE ( 'NONE', *, *, #58909, .F. ) ;
#21211 = CARTESIAN_POINT ( 'NONE',  ( 115.0372575077159212, -42.90846256501347966, 108.3022919427452138 ) ) ;
#21212 = DIRECTION ( 'NONE',  ( -1.000000000000000000, 0.000000000000000000, 0.000000000000000000 ) ) ;
#21213 = CARTESIAN_POINT ( 'NONE',  ( 108.4169788036852964, -26.73497112227234140, 160.9689992506304748 ) ) ;
#21214 = CARTESIAN_POINT ( 'NONE',  ( 173.9900000000000091, 5.112500000000000711, -58.73749999999999716 ) ) ;
#21215 = DIRECTION ( 'NONE',  ( 1.000000000000000000, 4.163336342344333240E-14, 0.000000000000000000 ) ) ;
#21216 = DIRECTION ( 'NONE',  ( 0.000000000000000000, -0.000000000000000000, -1.000000000000000000 ) ) ;
#21217 = CARTESIAN_POINT ( 'NONE',  ( -72.96458098368600531, 101.5999999999999943, -78.00648098368779415 ) ) ;
#21218 = ADVANCED_FACE ( 'NONE', ( #87832 ), #5617, .F. ) ;
#21219 = LINE ( 'NONE', #29383, #79695 ) ;
#21220 = EDGE_CURVE ( 'NONE', #50419, #21337, #4262, .T. ) ;
#21221 = CARTESIAN_POINT ( 'NONE',  ( 112.1867106929447999, -26.95862322015887358, 14.68038718067299442 ) ) ;
#21222 = FACE_OUTER_BOUND ( 'NONE', #42262, .T. ) ;
#21223 = VERTEX_POINT ( 'NONE', #11525 ) ;
#21224 = LINE ( 'NONE', #68476, #31588 ) ;
#21225 = CIRCLE ( 'NONE', #16878, 1.000000000000000888 ) ;
#21226 = LINE ( 'NONE', #70725, #3249 ) ;
#21227 = CARTESIAN_POINT ( 'NONE',  ( 102.3683448235669715, -29.46113098739592928, 68.36332846482901004 ) ) ;
#21228 = AXIS2_PLACEMENT_3D ( 'NONE', #65998, #3790, #58304 ) ;
#21229 = AXIS2_PLACEMENT_3D ( 'NONE', #5761, #12571, #68875 ) ;
#21230 = AXIS2_PLACEMENT_3D ( 'NONE', #88594, #5469, #73603 ) ;
#21231 = LINE ( 'NONE', #48902, #58615 ) ;
#21232 = CARTESIAN_POINT ( 'NONE',  ( 80.06648329127399677, -8.729447159940999512, 306.1181252759120071 ) ) ;
#21233 = VERTEX_POINT ( 'NONE', #53267 ) ;
#21234 = EDGE_LOOP ( 'NONE', ( #7974, #48995, #26305, #29271 ) ) ;
#21235 = DIRECTION ( 'NONE',  ( -1.000000000000000078E-15, -1.000000000000000083E-30, 1.000000000000000000 ) ) ;
#21236 = VERTEX_POINT ( 'NONE', #66473 ) ;
#21237 = EDGE_LOOP ( 'NONE', ( #55679, #72269, #83434, #21702 ) ) ;
#21238 = CARTESIAN_POINT ( 'NONE',  ( 34.96670390244654669, -26.71338133339238041, 117.4678068554150485 ) ) ;
#21239 = CARTESIAN_POINT ( 'NONE',  ( 100.2959224756171466, -44.18784923124425035, 153.4215833058969736 ) ) ;
#21240 = DIRECTION ( 'NONE',  ( 1.000000000000000078E-15, -1.000000000000000000, 0.000000000000000000 ) ) ;
#21241 = AXIS2_PLACEMENT_3D ( 'NONE', #60099, #73751, #73295 ) ;
#21242 = CARTESIAN_POINT ( 'NONE',  ( 96.77023068570494502, -38.49705603518268049, 87.46133956162493917 ) ) ;
#21243 = CARTESIAN_POINT ( 'NONE',  ( 188.5667039024479834, -62.87844715994099687, 134.4678068554150059 ) ) ;
#21244 = ORIENTED_EDGE ( 'NONE', *, *, #79068, .T. ) ;
#21245 = CARTESIAN_POINT ( 'NONE',  ( 107.0667039024467613, -36.72944715994091780, 196.8538068554170195 ) ) ;
#21246 = VERTEX_POINT ( 'NONE', #31502 ) ;
#21247 = AXIS2_PLACEMENT_3D ( 'NONE', #66538, #87000, #59709 ) ;
#21248 = ORIENTED_EDGE ( 'NONE', *, *, #27932, .F. ) ;
#21249 = EDGE_CURVE ( 'NONE', #7062, #38828, #8875, .T. ) ;
#21250 = CARTESIAN_POINT ( 'NONE',  ( 72.26648329127297643, -1.929447159941394263, 352.4506252759079530 ) ) ;
#21251 = EDGE_LOOP ( 'NONE', ( #333, #32516, #1053, #37883 ) ) ;
#21252 = CARTESIAN_POINT ( 'NONE',  ( 115.9938418408662244, -42.00591315737207054, 283.4137205140066271 ) ) ;
#21253 = CARTESIAN_POINT ( 'NONE',  ( 96.58534993179142703, -36.88768535406505578, 132.3384824187679669 ) ) ;
#21254 = LINE ( 'NONE', #83480, #237 ) ;
#21255 = DIRECTION ( 'NONE',  ( -3.100000000000000258E-29, 3.100000000000000044E-14, 1.000000000000000000 ) ) ;
#21256 = CARTESIAN_POINT ( 'NONE',  ( 101.7108440984968212, -27.74398881808361850, 81.50419670448295051 ) ) ;
#21257 = CARTESIAN_POINT ( 'NONE',  ( 107.0664832912750057, -36.72944715993903486, 9.425625275910970657 ) ) ;
#21258 = VERTEX_POINT ( 'NONE', #25142 ) ;
#21259 = CARTESIAN_POINT ( 'NONE',  ( 97.12564716885088956, -37.99759042466634895, 116.4282268054463145 ) ) ;
#21260 = CARTESIAN_POINT ( 'NONE',  ( 97.81136857581559241, -40.51756142658395987, 157.6353372204761456 ) ) ;
#21261 = EDGE_LOOP ( 'NONE', ( #17991, #9895, #22157, #22934 ) ) ;
#21262 = DIRECTION ( 'NONE',  ( 0.000000000000000000, 0.000000000000000000, 1.000000000000000000 ) ) ;
#21263 = EDGE_CURVE ( 'NONE', #64803, #11195, #52803, .T. ) ;
#21264 = CARTESIAN_POINT ( 'NONE',  ( 12.60000000000000142, 83.38255235285211597, 117.8845415480757595 ) ) ;
#21265 = CARTESIAN_POINT ( 'NONE',  ( 112.1975415602056216, -26.93795424888832812, 14.68038718067299442 ) ) ;
#21266 = CARTESIAN_POINT ( 'NONE',  ( 70.14948329127297200, -71.52944715994141234, 352.4506252759078961 ) ) ;
#21267 = CARTESIAN_POINT ( 'NONE',  ( 77.61670390244702844, -103.2284471599409841, 222.2178068554179902 ) ) ;
#21268 = PLANE ( 'NONE',  #28732 ) ;
#21269 = CARTESIAN_POINT ( 'NONE',  ( 111.3857387752846790, -29.74709210828544670, 289.0581341137911409 ) ) ;
#21271 = CARTESIAN_POINT ( 'NONE',  ( 98.47430666977648173, -42.65725675464086919, 122.8070538473389490 ) ) ;
#21270 = CARTESIAN_POINT ( 'NONE',  ( 115.0888706016519905, -30.61758542023168062, 109.3439634156283091 ) ) ;
#21272 = CARTESIAN_POINT ( 'NONE',  ( 104.4899544459507865, -26.97880758620100750, 71.28145860973472736 ) ) ;
#21273 = CARTESIAN_POINT ( 'NONE',  ( 172.5664832912729878, -27.82844715994070484, 134.1756252759119832 ) ) ;
#21274 = ORIENTED_EDGE ( 'NONE', *, *, #67160, .T. ) ;
#21275 = DIRECTION ( 'NONE',  ( 0.7071067811865779928, -0.7071067811865171526, 7.071067811865785947E-16 ) ) ;
#21276 = FACE_BOUND ( 'NONE', #23135, .T. ) ;
#21277 = CARTESIAN_POINT ( 'NONE',  ( 46.83715912545339677, -47.82818131006086304, 180.4678068554150911 ) ) ;
#21278 = ORIENTED_EDGE ( 'NONE', *, *, #78565, .T. ) ;
#21279 = EDGE_CURVE ( 'NONE', #50783, #8428, #68315, .T. ) ;
#21280 = ADVANCED_FACE ( 'NONE', ( #10621 ), #32852, .F. ) ;
#21281 = DIRECTION ( 'NONE',  ( 1.000000000000000000, 0.000000000000000000, 0.000000000000000000 ) ) ;
#21283 = ORIENTED_EDGE ( 'NONE', *, *, #66622, .T. ) ;
#21282 = CARTESIAN_POINT ( 'NONE',  ( 103.7935660395325073, -26.78486678718983072, 165.3299109901969643 ) ) ;
#21284 = CARTESIAN_POINT ( 'NONE',  ( 63.03715912545735023, -24.42818131006027826, 249.9678068554150343 ) ) ;
#21285 = CARTESIAN_POINT ( 'NONE',  ( 103.7162039098101332, -26.17194585468624624, 201.3089586092439731 ) ) ;
#21286 = CARTESIAN_POINT ( 'NONE',  ( 98.61215933031529346, -43.92124142298762735, 72.89943479972099283 ) ) ;
#21287 = VECTOR ( 'NONE', #31504, 1000.000000000000000 ) ;
#21288 = CARTESIAN_POINT ( 'NONE',  ( 92.90380151374968420, 69.84937019662268654, 91.73035097708832097 ) ) ;
#21289 = CARTESIAN_POINT ( 'NONE',  ( 62.56670390244747892, -48.82844715994099971, 300.4678068554150627 ) ) ;
#21290 = LINE ( 'NONE', #9019, #19176 ) ;
#21291 = ORIENTED_EDGE ( 'NONE', *, *, #50205, .T. ) ;
#21292 = AXIS2_PLACEMENT_3D ( 'NONE', #31994, #3412, #52844 ) ;
#21293 = AXIS2_PLACEMENT_3D ( 'NONE', #86811, #58203, #64577 ) ;
#21294 = EDGE_CURVE ( 'NONE', #19859, #51458, #66026, .T. ) ;
#21295 = ORIENTED_EDGE ( 'NONE', *, *, #54603, .T. ) ;
#21296 = ORIENTED_EDGE ( 'NONE', *, *, #67431, .F. ) ;
#21297 = VERTEX_POINT ( 'NONE', #130 ) ;
#21298 = DIRECTION ( 'NONE',  ( 3.665114028111779382E-18, -0.9995520592605569021, 0.02992792722492374630 ) ) ;
#21299 = CARTESIAN_POINT ( 'NONE',  ( 114.6054725695487946, -29.52902160936550047, 230.4327681330539690 ) ) ;
#21300 = FACE_OUTER_BOUND ( 'NONE', #61229, .T. ) ;
#21301 = LINE ( 'NONE', #38490, #86143 ) ;
#21302 = EDGE_CURVE ( 'NONE', #44089, #4100, #14634, .T. ) ;
#21304 = CARTESIAN_POINT ( 'NONE',  ( 92.06079644778121462, 79.26437155269051971, 74.70173812346128273 ) ) ;
#21303 = DIRECTION ( 'NONE',  ( 0.000000000000000000, 0.000000000000000000, 1.000000000000000000 ) ) ;
#21305 = CARTESIAN_POINT ( 'NONE',  ( -1.790903581468949841E-22, 95.14999999999999147, 118.3560000000000088 ) ) ;
#21306 = AXIS2_PLACEMENT_3D ( 'NONE', #61344, #26831, #69528 ) ;
#21307 = CARTESIAN_POINT ( 'NONE',  ( 106.6058666599951152, -25.66223100340348040, 40.09753003781596448 ) ) ;
#21308 = ORIENTED_EDGE ( 'NONE', *, *, #63417, .F. ) ;
#21309 = ORIENTED_EDGE ( 'NONE', *, *, #71238, .F. ) ;
#21310 = CLOSED_SHELL ( 'NONE', ( #62528, #16625, #46388, #49679, #26784, #65133, #28374, #8925, #8821, #57060, #56557, #12619, #87231, #55910, #15973, #77797, #60844, #26322, #74973, #80867, #166, #45363, #79765, #86219, #33513, #49715, #83428, #67112, #13417, #25822, #88826, #62442, #50114, #61870, #23559, #36703, #28665, #10064, #84486, #59842, #73894, #42376, #58587, #18095, #53777, #42535, #82466, #51897, #17100, #39934, #64276, #17030, #82470, #9204, #8048, #42579, #79785, #25644, #25836, #26602, #72259, #17085, #80890, #13620, #55416, #24873, #38217, #15636, #48020, #22908, #46075, #58694, #48636, #13737, #47270, #50460, #87018, #30207, #73782, #42472, #64761, #60557, #10733, #29291, #26295, #75945, #67540, #4137, #82738, #4359, #37053, #29837, #70201, #70105, #47337, #59036, #33056, #64779, #69400, #35065, #41109, #58490, #72889, #1573, #34814, #54959, #17716, #5825, #34402, #87656, #74839, #14559, #74380, #65211, #82533, #66998, #53645, #15441, #15506, #51506, #72474, #44778, #66243, #70004, #45167, #18462, #88502, #14748, #50148, #38530, #38295, #34284, #82967, #39333, #27225, #13177, #88554, #75402, #56573, #23551, #78843, #10585, #12887, #11450, #82751, #13577, #47287, #23040, #82858, #77907, #32146, #56562, #48519, #28537, #70877, #10335, #58854, #30321, #26959, #5848, #45062, #57326, #53828, #68661, #19334, #18816, #7637, #45453, #11955, #30349, #29832, #56883, #30806, #76175, #17847, #13595, #57264, #77823, #65880, #43859, #19667, #61728, #39810, #62092, #26049, #6928, #53354, #7545, #43958, #36576, #15729, #38210, #34640, #12134, #11956, #10562, #12354, #14937, #11308, #4008, #55301, #56868, #75663, #42031, #44035, #79644, #75154, #46925, #40144, #16129, #63764, #61744, #54182, #79971, #65742, #80456, #8577, #86077, #51312, #54152, #3367, #71152, #6729, #14946, #78053, #84477, #87069, #80909, #71855, #44138, #68654, #83526, #46448, #49719, #87028 ) ) ;
#21311 = CARTESIAN_POINT ( 'NONE',  ( 57.56670390244819657, -48.82844715994039575, 259.7178068554150627 ) ) ;
#21312 = CARTESIAN_POINT ( 'NONE',  ( 107.0667039024470313, -104.2784471599420755, -19.78219314458201694 ) ) ;
#21313 = CARTESIAN_POINT ( 'NONE',  ( 110.5064767540468011, -26.94654216138288660, 250.8194347997200850 ) ) ;
#21314 = CARTESIAN_POINT ( 'NONE',  ( 61.56670390244727287, -23.42844715994043980, 300.4678068554150627 ) ) ;
#21315 = EDGE_CURVE ( 'NONE', #37451, #88467, #14211, .T. ) ;
#21316 = CARTESIAN_POINT ( 'NONE',  ( 97.87212830949614784, -31.93334231290201330, 86.93181575210095957 ) ) ;
#21318 = EDGE_CURVE ( 'NONE', #36953, #21752, #55508, .T. ) ;
#21317 = CARTESIAN_POINT ( 'NONE',  ( 221.2791280605339921, 36.86249999999999716, -7.937500000000000000 ) ) ;
#21319 = EDGE_CURVE ( 'NONE', #83706, #77060, #35084, .T. ) ;
#21320 = CARTESIAN_POINT ( 'NONE',  ( -9.749037034254353529, 224.4999999999999432, 152.4294779587682456 ) ) ;
#21321 = VERTEX_POINT ( 'NONE', #41889 ) ;
#21322 = DIRECTION ( 'NONE',  ( 0.000000000000000000, 0.000000000000000000, 1.000000000000000000 ) ) ;
#21323 = EDGE_CURVE ( 'NONE', #14083, #41448, #69625, .T. ) ;
#21324 = VERTEX_POINT ( 'NONE', #56420 ) ;
#21325 = EDGE_LOOP ( 'NONE', ( #54742, #51933, #87938, #63322 ) ) ;
#21326 = CARTESIAN_POINT ( 'NONE',  ( -77.68727430814968216, 92.11680164986013608, 89.55756476669517951 ) ) ;
#21327 = CARTESIAN_POINT ( 'NONE',  ( 110.1832024441707460, -27.86589328696400969, 251.2511071154212061 ) ) ;
#21328 = VECTOR ( 'NONE', #5880, 1000.000000000000000 ) ;
#21329 = CARTESIAN_POINT ( 'NONE',  ( 117.0718954873599671, -35.46248236694560063, 193.9272919417280718 ) ) ;
#21330 = CARTESIAN_POINT ( 'NONE',  ( -118.4232890149586552, 93.94641470820113227, 5.620000134943238024 ) ) ;
#21331 = B_SPLINE_CURVE_WITH_KNOTS ( 'NONE', 3,
 ( #6534, #14253, #19275, #41928, #34229, #33791, #61934, #21063, #48737, #89667, #26982, #26530, #67865, #27417, #55099, #54202, #81964, #75128 ),
 .UNSPECIFIED., .F., .F.,
 ( 4, 2, 2, 2, 2, 2, 2, 2, 4 ),
 ( 0.000000000000000000, 0.06248810027333082107, 0.1249762005466616421, 0.1874643008199924632, 0.2499524010933232843, 0.3124405013666541331, 0.3749286016399849264, 0.4374167019133153866, 0.4999048021866459024 ),
 .UNSPECIFIED. ) ;
#21332 = DIRECTION ( 'NONE',  ( -0.7967329428042217998, 0.6043315462976631691, -1.908195823574488750E-14 ) ) ;
#21333 = CARTESIAN_POINT ( 'NONE',  ( 86.94609723791393208, 70.66242608954389937, -80.59807192910901108 ) ) ;
#21334 = EDGE_LOOP ( 'NONE', ( #61897, #87495, #17185, #84543, #36399, #86501 ) ) ;
#21335 = DIRECTION ( 'NONE',  ( 0.000000000000000000, 1.000000000000000000, 0.000000000000000000 ) ) ;
#21336 = DIRECTION ( 'NONE',  ( 3.309108161477000101E-13, -1.000000000000000000, 4.100000000000000342E-29 ) ) ;
#21337 = VERTEX_POINT ( 'NONE', #62349 ) ;
#21338 = CARTESIAN_POINT ( 'NONE',  ( 99.98060178585627966, -44.37649324013435859, 46.98133956162592284 ) ) ;
#21339 = ORIENTED_EDGE ( 'NONE', *, *, #54480, .T. ) ;
#21340 = CARTESIAN_POINT ( 'NONE',  ( 98.28161005395152472, -38.92874716189901818, 15.95622935188595370 ) ) ;
#21341 = DIRECTION ( 'NONE',  ( 0.000000000000000000, 0.000000000000000000, -1.000000000000000000 ) ) ;
#21342 = CARTESIAN_POINT ( 'NONE',  ( 98.80555182512723889, -41.96590078842033478, 186.7756252759109543 ) ) ;
#21343 = CARTESIAN_POINT ( 'NONE',  ( 57.56670390244829605, -48.82844715994039575, 293.2178068554150627 ) ) ;
#21344 = CARTESIAN_POINT ( 'NONE',  ( 172.5664832912740110, -9.303447159940999356, 81.04262527591200183 ) ) ;
#21345 = DIRECTION ( 'NONE',  ( 4.299999999999999979E-14, -1.000000000000000000, 0.000000000000000000 ) ) ;
#21346 = AXIS2_PLACEMENT_3D ( 'NONE', #38622, #81335, #25896 ) ;
#21347 = CARTESIAN_POINT ( 'NONE',  ( 4.902965529469843986, 70.83457992324913732, 130.4639032678012995 ) ) ;
#21348 = CARTESIAN_POINT ( 'NONE',  ( 118.5948618896802742, -33.89272371608580414, 10.01848241876795953 ) ) ;
#21349 = CARTESIAN_POINT ( 'NONE',  ( 77.68727430815029322, 92.11680164986012187, -89.55756476669462529 ) ) ;
#21350 = ORIENTED_EDGE ( 'NONE', *, *, #75910, .F. ) ;
#21351 = CARTESIAN_POINT ( 'NONE',  ( 77.89700433585288408, 82.54999999999999716, 59.93649209371626085 ) ) ;
#21352 = AXIS2_PLACEMENT_3D ( 'NONE', #32786, #5999, #69109 ) ;
#21353 = ORIENTED_EDGE ( 'NONE', *, *, #67419, .F. ) ;
#21354 = CARTESIAN_POINT ( 'NONE',  ( 96.59565658895887452, -37.56598942197172164, 97.38991099019594344 ) ) ;
#21355 = AXIS2_PLACEMENT_3D ( 'NONE', #67429, #5219, #6556 ) ;
#21356 = DIRECTION ( 'NONE',  ( -2.900000000000000265E-14, 2.000000000000000155E-15, -1.000000000000000000 ) ) ;
#21357 = AXIS2_PLACEMENT_3D ( 'NONE', #51485, #16994, #44675 ) ;
#21358 = VERTEX_POINT ( 'NONE', #21477 ) ;
#21359 = CARTESIAN_POINT ( 'NONE',  ( 76.31670390244799762, -50.82844715994100682, 198.9178068554149945 ) ) ;
#21360 = ORIENTED_EDGE ( 'NONE', *, *, #31742, .T. ) ;
#21361 = ORIENTED_EDGE ( 'NONE', *, *, #88171, .T. ) ;
#21362 = CARTESIAN_POINT ( 'NONE',  ( 97.95250717983365973, -32.49412669507731266, 25.56312527591095929 ) ) ;
#21363 = LINE ( 'NONE', #49037, #39044 ) ;
#21364 = CYLINDRICAL_SURFACE ( 'NONE', #84919, 0.5000000000000073275 ) ;
#21365 = DIRECTION ( 'NONE',  ( -1.000000000000000000, 0.000000000000000000, 0.000000000000000000 ) ) ;
#21366 = DIRECTION ( 'NONE',  ( 1.000000000000000000, 4.163336342344333240E-14, 0.000000000000000000 ) ) ;
#21367 = CARTESIAN_POINT ( 'NONE',  ( 108.5374814027631203, -28.67222352762033211, 162.7509475124489597 ) ) ;
#21368 = CARTESIAN_POINT ( 'NONE',  ( 116.2377588530493995, -41.80555791324388082, 259.4241967044827106 ) ) ;
#21369 = LINE ( 'NONE', #49044, #11695 ) ;
#21370 = ORIENTED_EDGE ( 'NONE', *, *, #14742, .T. ) ;
#21371 = CARTESIAN_POINT ( 'NONE',  ( 8.391117282579658720, 72.98104651172248225, 118.2601343779861622 ) ) ;
#21372 = AXIS2_PLACEMENT_3D ( 'NONE', #46987, #33383, #27462 ) ;
#21373 = AXIS2_PLACEMENT_3D ( 'NONE', #8083, #817, #71218 ) ;
#21374 = CYLINDRICAL_SURFACE ( 'NONE', #40369, 12.69999999999999574 ) ;
#21375 = ORIENTED_EDGE ( 'NONE', *, *, #72949, .T. ) ;
#21376 = ORIENTED_EDGE ( 'NONE', *, *, #50501, .F. ) ;
#21377 = CIRCLE ( 'NONE', #40217, 10.26166025953212468 ) ;
#21378 = DIRECTION ( 'NONE',  ( 1.000000000000000078E-15, -1.000000000000000083E-30, -1.000000000000000000 ) ) ;
#21379 = EDGE_CURVE ( 'NONE', #3248, #67028, #84164, .T. ) ;
#21380 = DIRECTION ( 'NONE',  ( -0.4808135048159887792, -0.02029144519433677407, 0.8765880622267739897 ) ) ;
#21381 = CARTESIAN_POINT ( 'NONE',  ( 112.1393234202593590, -28.01280907429307732, 14.65646064512042912 ) ) ;
#21382 = ADVANCED_FACE ( 'NONE', ( #76886, #55963 ), #75089, .T. ) ;
#21383 = LINE ( 'NONE', #26837, #39060 ) ;
#21384 = DIRECTION ( 'NONE',  ( 0.7071067811865514585, -0.7071067811865435759, 7.071067811865211065E-16 ) ) ;
#21385 = CARTESIAN_POINT ( 'NONE',  ( 113.5990078486005217, -30.45738264864434441, 188.8457531614099594 ) ) ;
#21386 = CARTESIAN_POINT ( 'NONE',  ( 117.0169231590003562, -33.47438763928646210, 89.07848241876791917 ) ) ;
#21387 = ORIENTED_EDGE ( 'NONE', *, *, #80871, .T. ) ;
#21388 = FACE_OUTER_BOUND ( 'NONE', #72096, .T. ) ;
#21389 = ORIENTED_EDGE ( 'NONE', *, *, #36573, .F. ) ;
#21390 = EDGE_CURVE ( 'NONE', #16883, #64854, #88621, .T. ) ;
#21391 = CARTESIAN_POINT ( 'NONE',  ( -74.70281015415449133, 79.25941250729455589, -92.05992619857326531 ) ) ;
#21392 = EDGE_LOOP ( 'NONE', ( #8614, #12946, #73187, #67248 ) ) ;
#21393 = ADVANCED_FACE ( 'NONE', ( #1030 ), #54612, .T. ) ;
#21394 = ADVANCED_FACE ( 'NONE', ( #89174 ), #28733, .T. ) ;
#21395 = DIRECTION ( 'NONE',  ( -3.100000000000000258E-29, 3.100000000000000044E-14, 1.000000000000000000 ) ) ;
#21396 = ORIENTED_EDGE ( 'NONE', *, *, #73574, .T. ) ;
#21397 = CARTESIAN_POINT ( 'NONE',  ( 3.110602869834275287E-15, 124.9679999999999893, 25.39999999999999858 ) ) ;
#21398 = CARTESIAN_POINT ( 'NONE',  ( 80.78702870777534883, -128.1369015726494922, 249.3173333679100097 ) ) ;
#21399 = DIRECTION ( 'NONE',  ( 0.7071067811865779928, -0.7071067811865171526, 7.071067811865785947E-16 ) ) ;
#21400 = VECTOR ( 'NONE', #38821, 1000.000000000000000 ) ;
#21401 = EDGE_CURVE ( 'NONE', #75109, #12810, #12879, .T. ) ;
#21402 = FACE_OUTER_BOUND ( 'NONE', #54082, .T. ) ;
#21403 = EDGE_LOOP ( 'NONE', ( #22104, #78884, #37129, #38666, #745, #52148, #29845 ) ) ;
#21404 = CARTESIAN_POINT ( 'NONE',  ( 96.15435578470099642, -38.63231720721949358, 46.45181575210094138 ) ) ;
#21405 =( NAMED_UNIT ( * ) PLANE_ANGLE_UNIT ( ) SI_UNIT ( $, .RADIAN. ) );
#21406 = ADVANCED_FACE ( 'NONE', ( #40565 ), #48701, .F. ) ;
#21408 = PLANE ( 'NONE',  #47137 ) ;
#21407 = PLANE ( 'NONE',  #20239 ) ;
#21409 = FACE_OUTER_BOUND ( 'NONE', #8796, .T. ) ;
#21410 = CARTESIAN_POINT ( 'NONE',  ( 131.3165191078497855, -18.55813574389560117, 3.101427645695946644 ) ) ;
#21411 = ORIENTED_EDGE ( 'NONE', *, *, #20811, .T. ) ;
#21412 = ADVANCED_FACE ( 'NONE', ( #75548 ), #68725, .F. ) ;
#21413 = CARTESIAN_POINT ( 'NONE',  ( 116.3199495083284347, -32.94194616109231077, 85.13562527591095375 ) ) ;
#21414 = ADVANCED_FACE ( 'NONE', ( #89628 ), #27383, .T. ) ;
#21415 = LINE ( 'NONE', #26870, #3737 ) ;
#21416 = FACE_OUTER_BOUND ( 'NONE', #5727, .T. ) ;
#21417 = CARTESIAN_POINT ( 'NONE',  ( 116.9423613927432939, -33.21572726007214271, 110.0984824187679578 ) ) ;
#21418 = AXIS2_PLACEMENT_3D ( 'NONE', #83617, #75456, #5973 ) ;
#21420 = DIRECTION ( 'NONE',  ( 0.000000000000000000, 0.000000000000000000, 1.000000000000000000 ) ) ;
#21419 = CARTESIAN_POINT ( 'NONE',  ( 85.72499999999999432, 66.67499999999999716, 342.8999999999999773 ) ) ;
#21421 = CARTESIAN_POINT ( 'NONE',  ( 182.2738106836199563, -23.19206098993945275, 342.9256252759109884 ) ) ;
#21422 = CONICAL_SURFACE ( 'NONE', #24338, 10.66800000000000459, 0.02993239667170383839 ) ;
#21423 = APPLICATION_CONTEXT ( 'automotive_design' ) ;
#21424 = VECTOR ( 'NONE', #78307, 1000.000000000000000 ) ;
#21425 = LINE ( 'NONE', #78648, #62182 ) ;
#21426 = CARTESIAN_POINT ( 'NONE',  ( 109.0694692412632207, -27.15596902575785876, 135.9127681330529640 ) ) ;
#21428 = EDGE_LOOP ( 'NONE', ( #64290, #3278, #68899, #23075 ) ) ;
#21427 = DIRECTION ( 'NONE',  ( -3.100000000000000258E-29, 3.100000000000000044E-14, 1.000000000000000000 ) ) ;
#21429 = VECTOR ( 'NONE', #55701, 1000.000000000000000 ) ;
#21430 = CARTESIAN_POINT ( 'NONE',  ( 110.7254274611715630, -26.32387412717039155, 250.8194347997206819 ) ) ;
#21431 = CARTESIAN_POINT ( 'NONE',  ( 107.0664832912739683, -23.41197657318947378, 305.7008218191032256 ) ) ;
#21432 = DIRECTION ( 'NONE',  ( 0.000000000000000000, -1.000000000000000000, 0.000000000000000000 ) ) ;
#21433 = DIRECTION ( 'NONE',  ( 0.9068632946707805287, -0.4214249218767882610, 8.630465054610985966E-16 ) ) ;
#21434 = CARTESIAN_POINT ( 'NONE',  ( -103.1875000000000000, 117.4749999999999943, 5.041899999998910253 ) ) ;
#21435 = ADVANCED_FACE ( 'NONE', ( #13758 ), #41443, .T. ) ;
#21436 = AXIS2_PLACEMENT_3D ( 'NONE', #70310, #71222, #8086 ) ;
#21437 = CARTESIAN_POINT ( 'NONE',  ( 46.83715912545424231, -47.82818131006082751, 300.4678068554150059 ) ) ;
#21438 = CARTESIAN_POINT ( 'NONE',  ( 74.15067561874209900, 120.6499999999999915, 68.53801554307469246 ) ) ;
#21439 = VECTOR ( 'NONE', #73717, 1000.000000000000000 ) ;
#21440 = ADVANCED_FACE ( 'NONE', ( #78254 ), #3273, .F. ) ;
#21442 = CARTESIAN_POINT ( 'NONE',  ( 103.7602102885707183, -27.48919103108766748, 190.3499109901969746 ) ) ;
#21441 = VECTOR ( 'NONE', #17359, 1000.000000000000000 ) ;
#21443 = ORIENTED_EDGE ( 'NONE', *, *, #46594, .T. ) ;
#21444 = ORIENTED_EDGE ( 'NONE', *, *, #86284, .F. ) ;
#21445 = CARTESIAN_POINT ( 'NONE',  ( 99.18485448662231363, -41.84413841198986006, 143.2282499725629634 ) ) ;
#21446 = VECTOR ( 'NONE', #45311, 1000.000000000000000 ) ;
#21447 = DIRECTION ( 'NONE',  ( -1.000000000000000078E-15, 1.000000000000000083E-30, 1.000000000000000000 ) ) ;
#21448 = CARTESIAN_POINT ( 'NONE',  ( 97.21282778982880757, -39.96427141005798234, 282.5908633711484867 ) ) ;
#21449 = LINE ( 'NONE', #89594, #30412 ) ;
#21450 = CARTESIAN_POINT ( 'NONE',  ( 116.7948070112746422, -39.38896383652134858, 268.6149319580774204 ) ) ;
#21451 = CARTESIAN_POINT ( 'NONE',  ( 162.5667039024486087, -33.35206098992175328, 237.4678068554150059 ) ) ;
#21452 = DIRECTION ( 'NONE',  ( 0.000000000000000000, 1.000000000000000000, 0.000000000000000000 ) ) ;
#21453 = LINE ( 'NONE', #7812, #40070 ) ;
#21454 = CARTESIAN_POINT ( 'NONE',  ( 106.8520627977276831, -47.75749532952668375, 227.5489586092439538 ) ) ;
#21455 = CARTESIAN_POINT ( 'NONE',  ( 97.07197674641710705, -35.37901635621462759, 171.2185788321773430 ) ) ;
#21456 = EDGE_LOOP ( 'NONE', ( #83881, #70150 ) ) ;
#21457 = VERTEX_POINT ( 'NONE', #42781 ) ;
#21458 = CARTESIAN_POINT ( 'NONE',  ( -83.90387289223363609, 76.93632333215536789, -100.0252357601324462 ) ) ;
#21459 = CARTESIAN_POINT ( 'NONE',  ( -77.69357874334708924, 92.12496802699139664, -89.55214429302399992 ) ) ;
#21460 = CARTESIAN_POINT ( 'NONE',  ( 104.4083715469849523, -46.45818331703511461, 123.3633132816207336 ) ) ;
#21461 = CARTESIAN_POINT ( 'NONE',  ( 0.000000000000000000, 224.4999999999999432, 154.6557476874258441 ) ) ;
#21462 = AXIS2_PLACEMENT_3D ( 'NONE', #72837, #2911, #72405 ) ;
#21463 = AXIS2_PLACEMENT_3D ( 'NONE', #5661, #12469, #41937 ) ;
#21464 = DIRECTION ( 'NONE',  ( 0.000000000000000000, 1.000000000000000000, 0.000000000000000000 ) ) ;
#21465 = ORIENTED_EDGE ( 'NONE', *, *, #53865, .F. ) ;
#21466 = CARTESIAN_POINT ( 'NONE',  ( 100.4377198651835101, -44.85950937921091253, 8.032768133053981074 ) ) ;
#21467 = CARTESIAN_POINT ( 'NONE',  ( 113.7993967570077700, -26.97709554098909024, 239.5956252759109759 ) ) ;
#21468 = ORIENTED_EDGE ( 'NONE', *, *, #21318, .F. ) ;
#21469 = LINE ( 'NONE', #63247, #7160 ) ;
#21470 = DIRECTION ( 'NONE',  ( 0.000000000000000000, 0.000000000000000000, -1.000000000000000000 ) ) ;
#21471 = FACE_OUTER_BOUND ( 'NONE', #74159, .T. ) ;
#21472 = CARTESIAN_POINT ( 'NONE',  ( 100.4295600883690014, -42.28392062234677695, 69.68713798863895192 ) ) ;
#21473 = CARTESIAN_POINT ( 'NONE',  ( 102.9585648456520772, -26.44303807861259870, 171.3908633711489813 ) ) ;
#21474 = LINE ( 'NONE', #1483, #63829 ) ;
#21475 = ORIENTED_EDGE ( 'NONE', *, *, #50674, .T. ) ;
#21476 = AXIS2_PLACEMENT_3D ( 'NONE', #27183, #6738, #83067 ) ;
#21477 = CARTESIAN_POINT ( 'NONE',  ( 41.56648329127381203, -18.82844715994071194, 21.92562527591192989 ) ) ;
#21478 = ORIENTED_EDGE ( 'NONE', *, *, #52911, .T. ) ;
#21479 = ORIENTED_EDGE ( 'NONE', *, *, #53371, .T. ) ;
#21480 = CIRCLE ( 'NONE', #15727, 0.5000000000000004441 ) ;
#21481 = AXIS2_PLACEMENT_3D ( 'NONE', #52635, #87646, #80396 ) ;
#21482 = CARTESIAN_POINT ( 'NONE',  ( 11.41184330286787940, 88.18497404666861428, 118.0059224074909849 ) ) ;
#21483 = EDGE_LOOP ( 'NONE', ( #89236, #31328, #21248, #29244 ) ) ;
#21484 = ORIENTED_EDGE ( 'NONE', *, *, #77422, .T. ) ;
#21485 = FACE_BOUND ( 'NONE', #73555, .T. ) ;
#21486 = EDGE_CURVE ( 'NONE', #12604, #8963, #55255, .T. ) ;
#21487 = ADVANCED_FACE ( 'NONE', ( #70526 ), #1931, .T. ) ;
#21488 = CARTESIAN_POINT ( 'NONE',  ( 105.8382827194499640, -25.33631814701313445, 322.1960590088103800 ) ) ;
#21489 = CARTESIAN_POINT ( 'NONE',  ( 115.4947688602672997, -38.28382951093581710, 88.10384839950596358 ) ) ;
#21490 = CARTESIAN_POINT ( 'NONE',  ( 104.3185787381473375, -25.99890841748068482, 245.2880062282919482 ) ) ;
#21492 = EDGE_CURVE ( 'NONE', #28894, #71248, #15106, .T. ) ;
#21491 = VECTOR ( 'NONE', #46334, 1000.000000000000114 ) ;
#21493 = CARTESIAN_POINT ( 'NONE',  ( 116.7748712849171966, -40.56502120445013304, 193.5270538473389479 ) ) ;
#21494 = PLANE ( 'NONE',  #7844 ) ;
#21495 = CARTESIAN_POINT ( 'NONE',  ( 274.0659999999999741, 36.86249999999999716, -58.73749999999999716 ) ) ;
#21496 = CIRCLE ( 'NONE', #30183, 5.041900000000001825 ) ;
#21497 = ADVANCED_FACE ( 'NONE', ( #9632 ), #21937, .F. ) ;
#21498 = ORIENTED_EDGE ( 'NONE', *, *, #26510, .T. ) ;
#21499 = DIRECTION ( 'NONE',  ( 0.000000000000000000, 0.000000000000000000, 1.000000000000000000 ) ) ;
#21500 = AXIS2_PLACEMENT_3D ( 'NONE', #81780, #27241, #48111 ) ;
#21501 = AXIS2_PLACEMENT_3D ( 'NONE', #47939, #61139, #75680 ) ;
#21502 = CARTESIAN_POINT ( 'NONE',  ( 107.0667039024470313, -104.2784471599420755, -19.78219314458201694 ) ) ;
#21503 = CARTESIAN_POINT ( 'NONE',  ( 70.44731575448797400, -139.9957943335142545, 247.0389897592665989 ) ) ;
#21504 = EDGE_CURVE ( 'NONE', #24976, #58319, #81370, .T. ) ;
#21505 = CARTESIAN_POINT ( 'NONE',  ( 112.9285164932676224, -28.85859325239445994, 104.5670538473399347 ) ) ;
#21506 = CARTESIAN_POINT ( 'NONE',  ( 113.4866449958868770, -46.74994221786862880, 68.02991099019695298 ) ) ;
#21507 = CARTESIAN_POINT ( 'NONE',  ( 99.34894212307516170, -29.65511154620466172, 275.7356252759109907 ) ) ;
#21508 = ORIENTED_EDGE ( 'NONE', *, *, #78168, .F. ) ;
#21509 = UNCERTAINTY_MEASURE_WITH_UNIT (LENGTH_MEASURE( 1.000000000000000082E-05 ), #51859, 'distance_accuracy_value', 'NONE');
#21510 = CARTESIAN_POINT ( 'NONE',  ( 117.4129020423329450, -35.18752443080737891, 218.9441967044829482 ) ) ;
#21511 = CARTESIAN_POINT ( 'NONE',  ( -186.2398777604655038, 101.5999999999999943, 114.2999999999999972 ) ) ;
#21512 = FILL_AREA_STYLE_COLOUR ( '', #78446 ) ;
#21513 = DIRECTION ( 'NONE',  ( 0.000000000000000000, -1.000000000000000000, 0.000000000000000000 ) ) ;
#21515 = CARTESIAN_POINT ( 'NONE',  ( 68.70199213936925275, -139.2946332222375361, 245.8922333760937136 ) ) ;
#21514 = CARTESIAN_POINT ( 'NONE',  ( 107.8430805769216931, -46.60421432495259353, 277.6356252759110816 ) ) ;
#21516 = CARTESIAN_POINT ( 'NONE',  ( 105.3684880140626063, -25.39599743441489821, 321.1394118018684480 ) ) ;
#21518 = EDGE_CURVE ( 'NONE', #13566, #64462, #58652, .T. ) ;
#21517 = CARTESIAN_POINT ( 'NONE',  ( -12.59999999999999964, 82.54999999999999716, 206.3750000000000000 ) ) ;
#21519 = DIRECTION ( 'NONE',  ( 1.000000000000000000, 4.299999999999999979E-14, 1.000000000000000078E-15 ) ) ;
#21520 = AXIS2_PLACEMENT_3D ( 'NONE', #79482, #38558, #87614 ) ;
#21521 = DIRECTION ( 'NONE',  ( -0.9130365726098600421, 0.000000000000000000, -0.4078776986755215939 ) ) ;
#21522 = CARTESIAN_POINT ( 'NONE',  ( 102.0670549276872521, -27.97049807736920002, 11.48979194543367477 ) ) ;
#21523 = LINE ( 'NONE', #1969, #4241 ) ;
#21524 = EDGE_CURVE ( 'NONE', #3733, #16260, #5949, .T. ) ;
#21526 = ORIENTED_EDGE ( 'NONE', *, *, #65389, .T. ) ;
#21525 = CARTESIAN_POINT ( 'NONE',  ( 41.56648329127499153, -32.07844715994070839, 318.9256252759120116 ) ) ;
#21527 = DIRECTION ( 'NONE',  ( 1.000000000000000078E-15, -1.000000000000000000, 0.000000000000000000 ) ) ;
#21528 = CARTESIAN_POINT ( 'NONE',  ( 96.24499046374883449, -34.36497383161641039, 256.1432443235299843 ) ) ;
#21529 = CARTESIAN_POINT ( 'NONE',  ( 114.4628154322623033, -28.51554874119783634, 155.5051490854349652 ) ) ;
#21530 = CARTESIAN_POINT ( 'NONE',  ( 99.12701999692106369, -43.51930588094383978, 27.88991099019694175 ) ) ;
#21531 = CARTESIAN_POINT ( 'NONE',  ( 179.4595971212889935, -28.98061976758940617, -5.074374724088000832 ) ) ;
#21532 = AXIS2_PLACEMENT_3D ( 'NONE', #75859, #13631, #14539 ) ;
#21534 = CARTESIAN_POINT ( 'NONE',  ( 117.4590087478601248, -92.77844715994211811, -21.78219314458237932 ) ) ;
#21533 = DIRECTION ( 'NONE',  ( 1.821299053822143307E-16, 0.000000000000000000, -1.000000000000000000 ) ) ;
#21535 = DIRECTION ( 'NONE',  ( -0.7071067811865779928, 0.7071067811865171526, -7.071067811865786933E-16 ) ) ;
#21536 = ORIENTED_EDGE ( 'NONE', *, *, #27567, .F. ) ;
#21537 = DIRECTION ( 'NONE',  ( 0.000000000000000000, 1.000000000000000000, 0.000000000000000000 ) ) ;
#21538 = ORIENTED_EDGE ( 'NONE', *, *, #36979, .T. ) ;
#21539 = CARTESIAN_POINT ( 'NONE',  ( 112.4313655287739948, -30.08308194412713021, 163.9581341137909476 ) ) ;
#21541 = ORIENTED_EDGE ( 'NONE', *, *, #23708, .F. ) ;
#21540 = DIRECTION ( 'NONE',  ( 1.000000000000000000, 4.163336342344333240E-14, 0.000000000000000000 ) ) ;
#21542 = DIRECTION ( 'NONE',  ( 0.7071067809773443624, -0.7071067813957507830, 7.071067809773451711E-16 ) ) ;
#21543 = CARTESIAN_POINT ( 'NONE',  ( 102.9757002774702102, -26.48594595611790581, 171.3908633711489813 ) ) ;
#21544 = CARTESIAN_POINT ( 'NONE',  ( 165.3359832912750278, -36.32844715993530826, 180.4678068554150059 ) ) ;
#21545 = LINE ( 'NONE', #80527, #12402 ) ;
#21546 = CARTESIAN_POINT ( 'NONE',  ( 97.07253791766775919, -35.37391747781727247, 87.21837571989119908 ) ) ;
#21547 = VECTOR ( 'NONE', #44269, 1000.000000000000114 ) ;
#21548 = LINE ( 'NONE', #36059, #78149 ) ;
#21549 = CARTESIAN_POINT ( 'NONE',  ( 41.56670390244783420, -36.32844715994104234, 249.9678068554150343 ) ) ;
#21550 = ADVANCED_FACE ( 'NONE', ( #50958 ), #2828, .F. ) ;
#21551 = CARTESIAN_POINT ( 'NONE',  ( 104.2906771502715628, -46.10805769451172864, 107.3470538473399500 ) ) ;
#21552 = ORIENTED_EDGE ( 'NONE', *, *, #16731, .T. ) ;
#21553 = ORIENTED_EDGE ( 'NONE', *, *, #42090, .T. ) ;
#21554 = ORIENTED_EDGE ( 'NONE', *, *, #59519, .T. ) ;
#21555 = CARTESIAN_POINT ( 'NONE',  ( 111.9552019894765493, -28.70592206014574543, 46.06063092494500211 ) ) ;
#21556 = CIRCLE ( 'NONE', #22217, 0.5000000000000004441 ) ;
#21557 = LINE ( 'NONE', #1104, #39948 ) ;
#21559 = CARTESIAN_POINT ( 'NONE',  ( 112.0659116737735559, -45.48839623049394731, 37.98979194726469188 ) ) ;
#21558 = CARTESIAN_POINT ( 'NONE',  ( 117.2610056464982904, -34.82931580038573571, 199.9851490854349549 ) ) ;
#21560 = CARTESIAN_POINT ( 'NONE',  ( 97.33793862645453032, -34.07069176642836794, 56.11362873108982541 ) ) ;
#21561 = CARTESIAN_POINT ( 'NONE',  ( 80.06648329127399677, -8.350947159940998787, 7.443125275912000127 ) ) ;
#21562 = CARTESIAN_POINT ( 'NONE',  ( 0.000000000000000000, 60.82030000000000314, 265.5569999999999595 ) ) ;
#21563 = VECTOR ( 'NONE', #23389, 1000.000000000000000 ) ;
#21564 = DIRECTION ( 'NONE',  ( 0.000000000000000000, 0.000000000000000000, 1.000000000000000000 ) ) ;
#21565 = CARTESIAN_POINT ( 'NONE',  ( 68.06662902182972630, -68.83619408334048728, 247.2278077909978151 ) ) ;
#21566 = CARTESIAN_POINT ( 'NONE',  ( 102.3226935662337098, -26.77152163616654335, 140.4422919425769578 ) ) ;
#21567 = VERTEX_POINT ( 'NONE', #35993 ) ;
#21568 = ORIENTED_EDGE ( 'NONE', *, *, #5499, .F. ) ;
#21569 = VERTEX_POINT ( 'NONE', #43238 ) ;
#21570 = VECTOR ( 'NONE', #49229, 1000.000000000000000 ) ;
#21571 = ADVANCED_FACE ( 'NONE', ( #70982 ), #8753, .F. ) ;
#21572 = CARTESIAN_POINT ( 'NONE',  ( 3.306647731859349904, 70.28099577563533273, 130.5147235605103617 ) ) ;
#21573 = FACE_OUTER_BOUND ( 'NONE', #44057, .T. ) ;
#21574 = VECTOR ( 'NONE', #79503, 1000.000000000000000 ) ;
#21575 = CARTESIAN_POINT ( 'NONE',  ( 188.5667039024479834, -48.82844715994099971, 257.2178068554150059 ) ) ;
#21576 = DIRECTION ( 'NONE',  ( 0.9068632946707755327, -0.4214249218767993077, 0.000000000000000000 ) ) ;
#21577 = CARTESIAN_POINT ( 'NONE',  ( 106.6101046285737510, -27.46188816740816918, 192.9338046553059485 ) ) ;
#21578 = ADVANCED_FACE ( 'NONE', ( #36453 ), #49607, .T. ) ;
#21579 = CARTESIAN_POINT ( 'NONE',  ( 107.0664832912739399, -36.72944715994095333, 247.7440089327910755 ) ) ;
#21580 = DIRECTION ( 'NONE',  ( -1.000000000000000000, 9.376883653928684652E-16, 1.500301384628589584E-15 ) ) ;
#21581 = ORIENTED_EDGE ( 'NONE', *, *, #7156, .T. ) ;
#21583 = ORIENTED_EDGE ( 'NONE', *, *, #3017, .F. ) ;
#21582 = ORIENTED_EDGE ( 'NONE', *, *, #6781, .T. ) ;
#21584 = VECTOR ( 'NONE', #24061, 1000.000000000000000 ) ;
#21585 = FACE_OUTER_BOUND ( 'NONE', #20832, .T. ) ;
#21586 = ORIENTED_EDGE ( 'NONE', *, *, #10521, .F. ) ;
#21587 = ORIENTED_EDGE ( 'NONE', *, *, #77656, .T. ) ;
#21588 = CARTESIAN_POINT ( 'NONE',  ( 82.81648329127398256, -18.72944715994105636, 3.101481641215461327 ) ) ;
#21589 = B_SPLINE_CURVE_WITH_KNOTS ( 'NONE', 3,
 ( #3413, #17488, #45168, #3856, #52409, #13357, #54649, #33792, #60588, #20619, #4750, #12017, #89218, #75130, #26531, #26983, #34230, #32433 ),
 .UNSPECIFIED., .F., .F.,
 ( 4, 2, 2, 2, 2, 2, 2, 2, 4 ),
 ( 0.5000000003264866155, 0.5625000002856758163, 0.6250000002448650172, 0.6875000002040541069, 0.7500000001632433078, 0.8125000001224325086, 0.8750000000816215984, 0.9375000000408107992, 1.000000000000000000 ),
 .UNSPECIFIED. ) ;
#21590 = CARTESIAN_POINT ( 'NONE',  ( 113.4748355983601300, -30.60888351595189860, 230.8644404487539816 ) ) ;
#21591 = CARTESIAN_POINT ( 'NONE',  ( 115.8257729668916909, -31.73060787271685257, 180.2401568395068807 ) ) ;
#21592 = ORIENTED_EDGE ( 'NONE', *, *, #62872, .F. ) ;
#21593 = PLANE ( 'NONE',  #5884 ) ;
#21594 = AXIS2_PLACEMENT_3D ( 'NONE', #5803, #62093, #13505 ) ;
#21595 = CARTESIAN_POINT ( 'NONE',  ( -112.6202530838359479, 67.89471438008003190, 66.04292222482025920 ) ) ;
#21596 = ORIENTED_EDGE ( 'NONE', *, *, #35027, .F. ) ;
#21597 = VERTEX_POINT ( 'NONE', #29188 ) ;
#21598 = CARTESIAN_POINT ( 'NONE',  ( 172.5664832912729878, -27.82844715994070484, 135.9256252759119832 ) ) ;
#21599 = ORIENTED_EDGE ( 'NONE', *, *, #63956, .F. ) ;
#21600 = ORIENTED_EDGE ( 'NONE', *, *, #29310, .F. ) ;
#21601 = EDGE_CURVE ( 'NONE', #80351, #84792, #50508, .T. ) ;
#21602 = EDGE_CURVE ( 'NONE', #62736, #32451, #89665, .T. ) ;
#21603 = CARTESIAN_POINT ( 'NONE',  ( 113.3211896355758057, -31.48460449655562954, 267.1995189410199600 ) ) ;
#21604 = CARTESIAN_POINT ( 'NONE',  ( 114.0958560388892380, -44.50609692678638396, 133.1613395616249989 ) ) ;
#21605 = EDGE_CURVE ( 'NONE', #60711, #57212, #44129, .T. ) ;
#21606 = CARTESIAN_POINT ( 'NONE',  ( 95.51222647996974047, -34.21005103128000968, 106.1556252759109640 ) ) ;
#21607 =( NAMED_UNIT ( * ) PLANE_ANGLE_UNIT ( ) SI_UNIT ( $, .RADIAN. ) );
#21608 = FILL_AREA_STYLE ('',( #14794 ) ) ;
#21609 = CARTESIAN_POINT ( 'NONE',  ( 117.3348620442827865, -34.92864588493001321, 239.9641967044819637 ) ) ;
#21610 = CARTESIAN_POINT ( 'NONE',  ( -76.20505178924449297, 120.6499999999999915, 76.20505178924310030 ) ) ;
#21611 = DIRECTION ( 'NONE',  ( 0.7071067811865969777, -0.7071067811864980568, 0.000000000000000000 ) ) ;
#21612 = ORIENTED_EDGE ( 'NONE', *, *, #20529, .T. ) ;
#21613 = DIRECTION ( 'NONE',  ( 0.000000000000000000, 0.000000000000000000, -1.000000000000000000 ) ) ;
#21614 = VERTEX_POINT ( 'NONE', #71866 ) ;
#21615 = CIRCLE ( 'NONE', #76714, 3.000000000000002665 ) ;
#21616 = ADVANCED_FACE ( 'NONE', ( #72312 ), #10085, .T. ) ;
#21617 = ORIENTED_EDGE ( 'NONE', *, *, #79360, .T. ) ;
#21618 = DIRECTION ( 'NONE',  ( -0.000000000000000000, 1.000000000000000000, -0.000000000000000000 ) ) ;
#21619 = CARTESIAN_POINT ( 'NONE',  ( 97.31303194613644791, -38.96042662333031359, 137.5053956884336230 ) ) ;
#21620 = AXIS2_PLACEMENT_3D ( 'NONE', #48682, #41868, #84144 ) ;
#21621 = EDGE_CURVE ( 'NONE', #45509, #40542, #20084, .T. ) ;
#21622 = ORIENTED_EDGE ( 'NONE', *, *, #1227, .T. ) ;
#21623 = CARTESIAN_POINT ( 'NONE',  ( 97.83587340921722841, -31.88353427759474457, 135.9413395616259947 ) ) ;
#21624 = CARTESIAN_POINT ( 'NONE',  ( 36.65249034007441509, -48.32844715994130524, 180.4678068554150911 ) ) ;
#21625 = CARTESIAN_POINT ( 'NONE',  ( 92.81551872686561921, -95.01002112898683549, -21.78219314458229405 ) ) ;
#21626 = CARTESIAN_POINT ( 'NONE',  ( 57.56670390244718760, -42.82844715994040996, 173.2178068554150911 ) ) ;
#21629 = CARTESIAN_POINT ( 'NONE',  ( 112.4430884738663394, -45.67687932769430859, 234.0070538473389377 ) ) ;
#21628 = DIRECTION ( 'NONE',  ( 0.000000000000000000, 0.000000000000000000, 1.000000000000000000 ) ) ;
#21627 = PLANE ( 'NONE',  #15773 ) ;
#21630 = DIRECTION ( 'NONE',  ( -1.000000000000000078E-15, 1.000000000000000000, 0.000000000000000000 ) ) ;
#21632 = ADVANCED_FACE ( 'NONE', ( #39115 ), #80468, .F. ) ;
#21631 = CARTESIAN_POINT ( 'NONE',  ( 0.000000000000000000, 2.269999999999994245, 0.000000000000000000 ) ) ;
#21633 = ORIENTED_EDGE ( 'NONE', *, *, #80162, .T. ) ;
#21634 = DIRECTION ( 'NONE',  ( 0.000000000000000000, 1.000000000000000000, 0.000000000000000000 ) ) ;
#21635 = VECTOR ( 'NONE', #62688, 1000.000000000000000 ) ;
#21636 = DIRECTION ( 'NONE',  ( 0.000000000000000000, 0.000000000000000000, -1.000000000000000000 ) ) ;
#21637 = CARTESIAN_POINT ( 'NONE',  ( 112.1393456349457551, -28.01282277704235568, 255.6564586098648988 ) ) ;
#21638 = AXIS2_PLACEMENT_3D ( 'NONE', #12846, #19202, #46431 ) ;
#21639 = DIRECTION ( 'NONE',  ( -4.237773401492740281E-14, 1.000000000000000000, 0.000000000000000000 ) ) ;
#21641 = ORIENTED_EDGE ( 'NONE', *, *, #1436, .T. ) ;
#21640 = CARTESIAN_POINT ( 'NONE',  ( 172.5664832912740110, 0.2215528400590013880, 141.0426252759120018 ) ) ;
#21642 = DIRECTION ( 'NONE',  ( 1.000000000000000000, 2.999999999999999839E-15, 1.000000000000000078E-15 ) ) ;
#21643 = CARTESIAN_POINT ( 'NONE',  ( 95.28658997325378266, -38.28252189325972665, 151.4299109901969871 ) ) ;
#21644 = CARTESIAN_POINT ( 'NONE',  ( 101.3842069476886394, -27.98906827703155642, 21.53562527591096298 ) ) ;
#21645 = CARTESIAN_POINT ( 'NONE',  ( 97.36167283409557172, -40.65495779399346077, 202.6327681330539860 ) ) ;
#21646 = DIRECTION ( 'NONE',  ( 0.000000000000000000, -1.000000000000000000, 0.000000000000000000 ) ) ;
#21647 = AXIS2_PLACEMENT_3D ( 'NONE', #54761, #82530, #5311 ) ;
#21648 = CARTESIAN_POINT ( 'NONE',  ( 83.06670390244796920, -61.87844715994100397, 231.5838068554150198 ) ) ;
#21650 = FACE_OUTER_BOUND ( 'NONE', #6581, .T. ) ;
#21649 = DIRECTION ( 'NONE',  ( 0.000000000000000000, 1.000000000000000000, 0.000000000000000000 ) ) ;
#21651 = DIRECTION ( 'NONE',  ( 4.194175870806139918E-14, -1.000000000000000000, 0.000000000000000000 ) ) ;
#21652 = CARTESIAN_POINT ( 'NONE',  ( 83.06670390244796920, -61.87844715994100397, 228.3338068554150198 ) ) ;
#21653 = ORIENTED_EDGE ( 'NONE', *, *, #5798, .F. ) ;
#21654 = DIRECTION ( 'NONE',  ( 1.000000000000000078E-15, -1.000000000000000083E-30, -1.000000000000000000 ) ) ;
#21655 = ORIENTED_EDGE ( 'NONE', *, *, #83654, .F. ) ;
#21656 = VERTEX_POINT ( 'NONE', #25488 ) ;
#21657 = AXIS2_PLACEMENT_3D ( 'NONE', #81278, #12217, #25388 ) ;
#21659 = VERTEX_POINT ( 'NONE', #46356 ) ;
#21658 = CARTESIAN_POINT ( 'NONE',  ( -7.205548786489490269E-13, 127.0000000000000000, 103.1875000000000000 ) ) ;
#21660 = CARTESIAN_POINT ( 'NONE',  ( 111.9186950350129877, -27.52701776748444473, 55.68991099019693536 ) ) ;
#21661 = DIRECTION ( 'NONE',  ( -1.000000000000000078E-15, 1.000000000000000083E-30, 1.000000000000000000 ) ) ;
#21662 = DIRECTION ( 'NONE',  ( 1.000000000000000078E-15, -1.000000000000000083E-30, -1.000000000000000000 ) ) ;
#21663 = CARTESIAN_POINT ( 'NONE',  ( 106.9746138897780696, -47.19771061482636298, 183.5699109901969734 ) ) ;
#21664 = CARTESIAN_POINT ( 'NONE',  ( 101.4801710200817126, -30.26808144278882651, 260.0667055423624561 ) ) ;
#21665 = ORIENTED_EDGE ( 'NONE', *, *, #84795, .T. ) ;
#21666 = AXIS2_PLACEMENT_3D ( 'NONE', #56953, #84246, #76968 ) ;
#21667 = ORIENTED_EDGE ( 'NONE', *, *, #58002, .T. ) ;
#21668 = VERTEX_POINT ( 'NONE', #11871 ) ;
#21669 = ORIENTED_EDGE ( 'NONE', *, *, #87288, .T. ) ;
#21670 = DIRECTION ( 'NONE',  ( 0.000000000000000000, 0.000000000000000000, -1.000000000000000000 ) ) ;
#21671 = DIRECTION ( 'NONE',  ( 6.831565154159360295E-14, -1.000000000000000000, 0.000000000000000000 ) ) ;
#21672 = CARTESIAN_POINT ( 'NONE',  ( 115.8250614324014549, -31.72937732619463702, 160.2398503699754144 ) ) ;
#21673 = CARTESIAN_POINT ( 'NONE',  ( 104.4899544453328559, -26.97880758635668030, 75.28145860978439430 ) ) ;
#21674 = CARTESIAN_POINT ( 'NONE',  ( 98.06216817836198629, 92.11674985319542941, 86.19179098795370919 ) ) ;
#21675 = DIRECTION ( 'NONE',  ( -1.000000000000000000, 0.000000000000000000, -2.108231265501709878E-16 ) ) ;
#21676 = CARTESIAN_POINT ( 'NONE',  ( 85.06670390244703128, -80.35669973212958439, 55.21780685541800437 ) ) ;
#21677 = CYLINDRICAL_SURFACE ( 'NONE', #82613, 5.599999999999994316 ) ;
#21678 = CARTESIAN_POINT ( 'NONE',  ( 112.1067112481348858, -26.91823048478329738, 19.71086337114896736 ) ) ;
#21679 = DIRECTION ( 'NONE',  ( 0.7071067811865540120, 0.000000000000000000, -0.7071067811865410224 ) ) ;
#21680 = VERTEX_POINT ( 'NONE', #60444 ) ;
#21681 = CIRCLE ( 'NONE', #10059, 5.800000000000000711 ) ;
#21682 = CARTESIAN_POINT ( 'NONE',  ( 113.2454988854073576, -28.75867309995891574, 269.5522919233096104 ) ) ;
#21683 = DIRECTION ( 'NONE',  ( -0.000000000000000000, -0.000000000000000000, -1.000000000000000000 ) ) ;
#21684 = CARTESIAN_POINT ( 'NONE',  ( 112.9396172237807860, -42.43812354398048114, 96.03094751244795191 ) ) ;
#21685 = VECTOR ( 'NONE', #26728, 1000.000000000000000 ) ;
#21686 = AXIS2_PLACEMENT_3D ( 'NONE', #22253, #14984, #29506 ) ;
#21687 = EDGE_CURVE ( 'NONE', #70548, #18305, #67923, .T. ) ;
#21688 = LINE ( 'NONE', #62104, #49930 ) ;
#21689 = DIRECTION ( 'NONE',  ( -0.000000000000000000, 0.4999999999999995004, 0.8660254037844390407 ) ) ;
#21690 = ORIENTED_EDGE ( 'NONE', *, *, #66596, .T. ) ;
#21691 = ORIENTED_EDGE ( 'NONE', *, *, #15756, .T. ) ;
#21692 = VECTOR ( 'NONE', #50693, 1000.000000000000000 ) ;
#21693 = FACE_OUTER_BOUND ( 'NONE', #40232, .T. ) ;
#21694 = ORIENTED_EDGE ( 'NONE', *, *, #50225, .T. ) ;
#21695 = EDGE_LOOP ( 'NONE', ( #46912, #87206, #32661, #33172, #82373, #5269, #22490, #89749 ) ) ;
#21696 = COLOUR_RGB ( '', 0.09019608, 0.27058824, 0.51372549) ;
#21697 = CARTESIAN_POINT ( 'NONE',  ( 112.8270896756726671, -29.95615083465972006, 135.9472975916109476 ) ) ;
#21698 = CARTESIAN_POINT ( 'NONE',  ( -5.244287019405542871, 94.12413552026930574, 118.4405785268131410 ) ) ;
#21699 = CIRCLE ( 'NONE', #28901, 10.00000000000000888 ) ;
#21700 = CARTESIAN_POINT ( 'NONE',  ( 109.6893229801689813, -47.49076295823797267, 83.75467289495897205 ) ) ;
#21701 = CARTESIAN_POINT ( 'NONE',  ( 106.5667039024470455, -113.7784471599420613, -19.78219314458171141 ) ) ;
#21702 = ORIENTED_EDGE ( 'NONE', *, *, #46278, .T. ) ;
#21703 = VERTEX_POINT ( 'NONE', #59988 ) ;
#21704 = ORIENTED_EDGE ( 'NONE', *, *, #59724, .F. ) ;
#21705 = ADVANCED_FACE ( 'NONE', ( #4606 ), #25946, .F. ) ;
#21706 = AXIS2_PLACEMENT_3D ( 'NONE', #87077, #24843, #18017 ) ;
#21707 = CARTESIAN_POINT ( 'NONE',  ( 144.0667039004811443, -140.6784471619068029, 245.4415720117440003 ) ) ;
#21708 = ORIENTED_EDGE ( 'NONE', *, *, #2040, .F. ) ;
#21709 = ADVANCED_FACE ( 'NONE', ( #32748 ), #17783, .T. ) ;
#21710 = CARTESIAN_POINT ( 'NONE',  ( 96.71096103112829212, -32.93116260832594122, 21.03467289495897319 ) ) ;
#21711 = CARTESIAN_POINT ( 'NONE',  ( 109.8617963350518920, -26.66349048206837580, 170.8613395616249591 ) ) ;
#21712 = CARTESIAN_POINT ( 'NONE',  ( 0.000000000000000000, 101.6000000000000227, 89.90000000000000568 ) ) ;
#21713 = DIRECTION ( 'NONE',  ( -1.000000000000000000, -1.181088324069315053E-15, 0.000000000000000000 ) ) ;
#21714 = EDGE_CURVE ( 'NONE', #78417, #75698, #88240, .T. ) ;
#21715 = CARTESIAN_POINT ( 'NONE',  ( 102.3023240427231570, -27.41686860022338124, 116.4527681330539650 ) ) ;
#21716 = CARTESIAN_POINT ( 'NONE',  ( 27.27158787008327678, 127.0000000000000000, 80.02307622376218887 ) ) ;
#21717 = ORIENTED_EDGE ( 'NONE', *, *, #83027, .T. ) ;
#21718 = DIRECTION ( 'NONE',  ( 4.811757763307910244E-15, 0.000000000000000000, -1.000000000000000000 ) ) ;
#21719 = EDGE_CURVE ( 'NONE', #44015, #42989, #5049, .T. ) ;
#21720 = CARTESIAN_POINT ( 'NONE',  ( 112.0665211874434988, -45.48806074044107106, 133.9910299359918895 ) ) ;
#21722 = EDGE_LOOP ( 'NONE', ( #9831, #61514, #9794, #77707 ) ) ;
#21721 = AXIS2_PLACEMENT_3D ( 'NONE', #56839, #9601, #16867 ) ;
#21723 = LINE ( 'NONE', #63033, #53289 ) ;
#21724 = CARTESIAN_POINT ( 'NONE',  ( 12.59999999999999964, 82.54999999999999716, 117.8845415480757595 ) ) ;
#21725 = CARTESIAN_POINT ( 'NONE',  ( 96.65879732087768161, -33.00665786158104709, 26.06514908543494613 ) ) ;
#21726 = CARTESIAN_POINT ( 'NONE',  ( 16.74114328162335141, 66.32651888666420348, 34.24720710913430821 ) ) ;
#21727 = CARTESIAN_POINT ( 'NONE',  ( -7.661254700127833495, 82.54999999999999716, 317.6630000000000109 ) ) ;
#21728 = DIRECTION ( 'NONE',  ( 0.000000000000000000, 1.000000000000000000, 0.000000000000000000 ) ) ;
#21729 = CARTESIAN_POINT ( 'NONE',  ( 97.00695627739551696, -39.24785929248557892, 16.53372051400697629 ) ) ;
#21731 = CARTESIAN_POINT ( 'NONE',  ( 116.7751801856527152, -32.99181816784840748, 135.1184824187679396 ) ) ;
#21730 = CARTESIAN_POINT ( 'NONE',  ( 97.81145390679880336, -40.51685147915726048, 111.6355755005379962 ) ) ;
#21732 = FACE_BOUND ( 'NONE', #48592, .T. ) ;
#21734 = EDGE_CURVE ( 'NONE', #67541, #976, #88188, .T. ) ;
#21733 = FACE_OUTER_BOUND ( 'NONE', #86851, .T. ) ;
#21735 = ORIENTED_EDGE ( 'NONE', *, *, #26965, .T. ) ;
#21736 = CARTESIAN_POINT ( 'NONE',  ( 91.00420390244700286, -68.87844715994096134, 55.21780685541800437 ) ) ;
#21737 = AXIS2_PLACEMENT_3D ( 'NONE', #65115, #2898, #51465 ) ;
#21738 = DIRECTION ( 'NONE',  ( 0.000000000000000000, 0.000000000000000000, 1.000000000000000000 ) ) ;
#21739 = EDGE_CURVE ( 'NONE', #25932, #72034, #10786, .T. ) ;
#21740 = DIRECTION ( 'NONE',  ( -1.000000000000000000, -1.734723475976808672E-15, 0.000000000000000000 ) ) ;
#21741 = ORIENTED_EDGE ( 'NONE', *, *, #24060, .F. ) ;
#21742 = AXIS2_PLACEMENT_3D ( 'NONE', #64318, #2087, #56587 ) ;
#21743 = CARTESIAN_POINT ( 'NONE',  ( 0.000000000000000000, -71.84204896855320044, 0.000000000000000000 ) ) ;
#21745 = ORIENTED_EDGE ( 'NONE', *, *, #81339, .T. ) ;
#21744 = CARTESIAN_POINT ( 'NONE',  ( 98.63028220664102719, -30.46987006685205657, 180.8184824187679567 ) ) ;
#21746 = CARTESIAN_POINT ( 'NONE',  ( 41.56670390244695312, -36.32844715994109208, 129.9678068554150911 ) ) ;
#21747 = CARTESIAN_POINT ( 'NONE',  ( 117.9552932246042332, -34.69990928640298478, 199.9851490854349549 ) ) ;
#21748 = CARTESIAN_POINT ( 'NONE',  ( 112.8417677104678063, -27.25086138798909374, 45.62895860924398761 ) ) ;
#21749 = CARTESIAN_POINT ( 'NONE',  ( 100.0338904447220898, 76.91670260214424104, 83.89393544538398828 ) ) ;
#21750 = DIRECTION ( 'NONE',  ( 1.000000000000000000, 0.000000000000000000, 8.465970413060558704E-17 ) ) ;
#21751 = DIRECTION ( 'NONE',  ( 4.299999999999999979E-14, -1.000000000000000000, 4.400000000000000367E-29 ) ) ;
#21752 = VERTEX_POINT ( 'NONE', #60906 ) ;
#21753 = VECTOR ( 'NONE', #41106, 1000.000000000000000 ) ;
#21754 = CONTEXT_DEPENDENT_SHAPE_REPRESENTATION ( #85728, #87336 ) ;
#21755 = EDGE_LOOP ( 'NONE', ( #55841, #42288, #81367, #3152 ) ) ;
#21756 = ORIENTED_EDGE ( 'NONE', *, *, #12286, .T. ) ;
#21757 = AXIS2_PLACEMENT_3D ( 'NONE', #49149, #14666, #29185 ) ;
#21758 = ORIENTED_EDGE ( 'NONE', *, *, #71952, .F. ) ;
#21759 = DIRECTION ( 'NONE',  ( -0.7071067811734105257, 0.7071067811996846197, 0.000000000000000000 ) ) ;
#21760 = CARTESIAN_POINT ( 'NONE',  ( 100.8484424157226442, -45.14118303587278547, 253.0699109901968882 ) ) ;
#21761 = DIRECTION ( 'NONE',  ( 0.000000000000000000, 0.8660254037844387076, 0.4999999999999998890 ) ) ;
#21762 = CARTESIAN_POINT ( 'NONE',  ( 135.9115321082997809, -16.68812259378463025, 2.188418746654308578 ) ) ;
#21763 = PRODUCT_DEFINITION_FORMATION_WITH_SPECIFIED_SOURCE ( 'ANY', '', #60378, .NOT_KNOWN. ) ;
#21764 = CIRCLE ( 'NONE', #26098, 29.00000000000000000 ) ;
#21766 = DIRECTION ( 'NONE',  ( -3.100000000000000258E-29, 3.100000000000000044E-14, 1.000000000000000000 ) ) ;
#21765 = CYLINDRICAL_SURFACE ( 'NONE', #55445, 3.300000000000000711 ) ;
#21767 = CARTESIAN_POINT ( 'NONE',  ( 121.5762960060074960, -43.47224590996763993, 0.7256252759109853567 ) ) ;
#21768 = EDGE_CURVE ( 'NONE', #14135, #76504, #22953, .T. ) ;
#21769 = CARTESIAN_POINT ( 'NONE',  ( 116.4944971008961261, -32.22846566477972630, 19.18133956162493092 ) ) ;
#21770 = VERTEX_POINT ( 'NONE', #20483 ) ;
#21771 = ORIENTED_EDGE ( 'NONE', *, *, #36074, .F. ) ;
#21772 =( NAMED_UNIT ( * ) PLANE_ANGLE_UNIT ( ) SI_UNIT ( $, .RADIAN. ) );
#21773 = CARTESIAN_POINT ( 'NONE',  ( 97.33794773618596707, -34.07063109094482201, 17.11683259552636116 ) ) ;
#21774 = ADVANCED_FACE ( 'NONE', ( #68626, #34984 ), #27731, .F. ) ;
#21775 = CARTESIAN_POINT ( 'NONE',  ( 104.5747221139661605, -26.66317121150818892, 236.2575300378149734 ) ) ;
#21776 = COLOUR_RGB ( '', 0.66274510, 0.83137255, 0.94901961) ;
#21777 = DIRECTION ( 'NONE',  ( 0.3818493186865920541, -0.9242245927363030855, 0.000000000000000000 ) ) ;
#21778 = CARTESIAN_POINT ( 'NONE',  ( 109.0694692412632207, -27.15596902575785876, 135.9127681330529640 ) ) ;
#21779 = DIRECTION ( 'NONE',  ( -3.278217592397115468E-15, 0.000000000000000000, 1.000000000000000000 ) ) ;
#21780 = CARTESIAN_POINT ( 'NONE',  ( -76.55155505517849690, 55.04324208698172782, 30.82815564505935768 ) ) ;
#21781 = ORIENTED_EDGE ( 'NONE', *, *, #13189, .T. ) ;
#21782 = CARTESIAN_POINT ( 'NONE',  ( 208.9149999999999920, 43.68799999999999528, 57.14999999999999858 ) ) ;
#21783 = ORIENTED_EDGE ( 'NONE', *, *, #38100, .T. ) ;
#21784 = ORIENTED_EDGE ( 'NONE', *, *, #2758, .T. ) ;
#21785 = AXIS2_PLACEMENT_3D ( 'NONE', #85926, #50021, #44546 ) ;
#21786 = CARTESIAN_POINT ( 'NONE',  ( -85.28591416242345247, 95.08639429146514033, 82.35292268805530114 ) ) ;
#21787 = CARTESIAN_POINT ( 'NONE',  ( 110.3188062821955242, -28.45390942821411429, 266.2101547344684604 ) ) ;
#21788 = DIRECTION ( 'NONE',  ( -0.7071067811869841124, 0.7071067811861110330, 0.000000000000000000 ) ) ;
#21789 = EDGE_CURVE ( 'NONE', #30320, #62271, #33651, .T. ) ;
#21790 = LINE ( 'NONE', #49458, #23304 ) ;
#21791 = CARTESIAN_POINT ( 'NONE',  ( 102.0670549734760044, -27.97049805183234383, 85.48979194136749982 ) ) ;
#21792 = DIRECTION ( 'NONE',  ( 0.000000000000000000, 0.000000000000000000, -1.000000000000000000 ) ) ;
#21793 = EDGE_LOOP ( 'NONE', ( #15374, #13661, #27751, #58767 ) ) ;
#21794 = VECTOR ( 'NONE', #54019, 1000.000000000000000 ) ;
#21795 = LINE ( 'NONE', #83128, #72547 ) ;
#21796 = DIRECTION ( 'NONE',  ( -1.000000000000000000, -3.999999999999999995E-14, -1.000000000000000078E-15 ) ) ;
#21797 = ORIENTED_EDGE ( 'NONE', *, *, #17918, .F. ) ;
#21798 = CARTESIAN_POINT ( 'NONE',  ( 99.29363446503140267, -43.73007054641615809, 56.90991099019593236 ) ) ;
#21799 = ORIENTED_EDGE ( 'NONE', *, *, #5922, .T. ) ;
#21800 = CARTESIAN_POINT ( 'NONE',  ( 104.7514827670518684, -44.95118086569023319, 21.78099125664900626 ) ) ;
#21801 = AXIS2_PLACEMENT_3D ( 'NONE', #41938, #1535, #49202 ) ;
#21802 = EDGE_CURVE ( 'NONE', #4000, #45258, #65012, .T. ) ;
#21803 = DIRECTION ( 'NONE',  ( -1.000000000000000000, 0.000000000000000000, 1.047445008332813989E-14 ) ) ;
#21804 = CARTESIAN_POINT ( 'NONE',  ( 116.1939227058878714, -40.33550099034470549, 193.5270538473399426 ) ) ;
#21805 = CARTESIAN_POINT ( 'NONE',  ( -160.2664750769294812, 101.5999999999999943, -148.0533267522755807 ) ) ;
#21806 = LINE ( 'NONE', #21344, #47628 ) ;
#21807 = CARTESIAN_POINT ( 'NONE',  ( 170.2205283966864897, 20.32000000000000028, -79.24800000000000466 ) ) ;
#21808 = CARTESIAN_POINT ( 'NONE',  ( 68.77377604071689632, -69.45229246467815187, 247.4784000562319761 ) ) ;
#21809 = CARTESIAN_POINT ( 'NONE',  ( 98.40574028604457624, -42.07939390257583767, 7.768006228291934434 ) ) ;
#21810 = CARTESIAN_POINT ( 'NONE',  ( 87.45628510944675327, 94.12556101775332706, -80.04418453221570928 ) ) ;
#21811 = AXIS2_PLACEMENT_3D ( 'NONE', #36472, #79160, #77807 ) ;
#21812 = EDGE_LOOP ( 'NONE', ( #911, #50003 ) ) ;
#21813 = DIRECTION ( 'NONE',  ( -1.000000000000000000, -8.163404592832032979E-16, 0.000000000000000000 ) ) ;
#21814 = EDGE_LOOP ( 'NONE', ( #15661, #27160, #61091, #46522 ) ) ;
#21815 = CARTESIAN_POINT ( 'NONE',  ( 114.7393473568293700, -44.74971245420289279, 109.1718157521009687 ) ) ;
#21816 = CARTESIAN_POINT ( 'NONE',  ( 124.8806136228746482, 48.00086824241649452, -38.07526654068476546 ) ) ;
#21817 = ORIENTED_EDGE ( 'NONE', *, *, #71496, .T. ) ;
#21818 = ORIENTED_EDGE ( 'NONE', *, *, #42477, .F. ) ;
#21819 = VERTEX_POINT ( 'NONE', #62245 ) ;
#21820 = VECTOR ( 'NONE', #46802, 1000.000000000000000 ) ;
#21821 = CARTESIAN_POINT ( 'NONE',  ( 115.7831076434849251, -41.80230955793731340, 123.4064586049333485 ) ) ;
#21822 = DIRECTION ( 'NONE',  ( 0.000000000000000000, 1.000000000000000000, 0.000000000000000000 ) ) ;
#21823 = DIRECTION ( 'NONE',  ( 0.000000000000000000, 0.000000000000000000, 1.000000000000000000 ) ) ;
#21824 = FACE_BOUND ( 'NONE', #19522, .T. ) ;
#21825 = FACE_OUTER_BOUND ( 'NONE', #16456, .T. ) ;
#21826 = EDGE_CURVE ( 'NONE', #26828, #26653, #82273, .T. ) ;
#21827 = CARTESIAN_POINT ( 'NONE',  ( 112.3492874949901932, -28.18945346073204306, 285.6356252759109680 ) ) ;
#21828 = CARTESIAN_POINT ( 'NONE',  ( 121.3178890780284434, -113.5468731908973439, -19.18411693322874356 ) ) ;
#21829 = ORIENTED_EDGE ( 'NONE', *, *, #88140, .T. ) ;
#21830 = CARTESIAN_POINT ( 'NONE',  ( 152.0371591254585155, -47.82818131005588214, 180.4678068554149775 ) ) ;
#21831 = VECTOR ( 'NONE', #14011, 1000.000000000000000 ) ;
#21832 = FACE_OUTER_BOUND ( 'NONE', #1163, .T. ) ;
#21833 = ORIENTED_EDGE ( 'NONE', *, *, #60116, .F. ) ;
#21834 = ORIENTED_EDGE ( 'NONE', *, *, #76339, .T. ) ;
#21835 = CARTESIAN_POINT ( 'NONE',  ( 183.5150000000000148, 14.63749999999999929, -19.05000000000000071 ) ) ;
#21836 = FACE_BOUND ( 'NONE', #67725, .T. ) ;
#21837 = DIRECTION ( 'NONE',  ( 1.017460296392624983E-15, 1.000000000000000000, 0.000000000000000000 ) ) ;
#21838 = DIRECTION ( 'NONE',  ( 1.000000000000000000, 0.000000000000000000, 0.000000000000000000 ) ) ;
#21839 = FACE_OUTER_BOUND ( 'NONE', #27528, .T. ) ;
#21840 = VECTOR ( 'NONE', #34962, 1000.000000000000000 ) ;
#21841 = CARTESIAN_POINT ( 'NONE',  ( 109.1470148533826432, -28.41539336262556503, 199.3038483995049717 ) ) ;
#21842 = LINE ( 'NONE', #15479, #73677 ) ;
#21843 = DIRECTION ( 'NONE',  ( 0.000000000000000000, 0.000000000000000000, -1.000000000000000000 ) ) ;
#21844 = CARTESIAN_POINT ( 'NONE',  ( 115.3018890743646665, -44.17195851134204077, 83.25372051400698581 ) ) ;
#21845 = ORIENTED_EDGE ( 'NONE', *, *, #53593, .F. ) ;
#21847 = ADVANCED_FACE ( 'NONE', ( #7300 ), #14110, .F. ) ;
#21846 = DIRECTION ( 'NONE',  ( 0.000000000000000000, 0.000000000000000000, 1.000000000000000000 ) ) ;
#21848 = ORIENTED_EDGE ( 'NONE', *, *, #26501, .T. ) ;
#21849 = EDGE_CURVE ( 'NONE', #11575, #2492, #83905, .T. ) ;
#21850 = DIRECTION ( 'NONE',  ( -0.000000000000000000, 1.000000000000000000, 0.000000000000000000 ) ) ;
#21851 = EDGE_LOOP ( 'NONE', ( #38747, #66681, #12395, #1596, #29492, #53495 ) ) ;
#21852 = CARTESIAN_POINT ( 'NONE',  ( 108.4173424463529756, -26.73501367913670279, 49.96897025569050754 ) ) ;
#21853 = ORIENTED_EDGE ( 'NONE', *, *, #53773, .F. ) ;
#21854 = CARTESIAN_POINT ( 'NONE',  ( -492.0614999999999668, 93.66249999999999432, 11.11250000000040217 ) ) ;
#21855 = CARTESIAN_POINT ( 'NONE',  ( 37.36643805256586859, -48.62818131006127231, 180.4678068554150911 ) ) ;
#21856 = CARTESIAN_POINT ( 'NONE',  ( 101.9943086291660137, -45.44649556581995142, 273.1560813037751245 ) ) ;
#21857 = VECTOR ( 'NONE', #663, 999.9999999999998863 ) ;
#21858 = CARTESIAN_POINT ( 'NONE',  ( 182.5667039024459939, -19.82844715994031048, -5.074374724088000832 ) ) ;
#21859 = ORIENTED_EDGE ( 'NONE', *, *, #73569, .F. ) ;
#21860 = CARTESIAN_POINT ( 'NONE',  ( 118.7574168473771152, -34.64232270468420438, 48.96705384733895983 ) ) ;
#21861 =( BOUNDED_CURVE ( )  B_SPLINE_CURVE ( 3, ( #8646, #49949, #77681, #42241 ),
 .UNSPECIFIED., .F., .T. ) 
 B_SPLINE_CURVE_WITH_KNOTS ( ( 4, 4 ),
 ( 3.141592653592887530, 4.712388980388064752 ),
 .UNSPECIFIED. ) 
 CURVE ( )  GEOMETRIC_REPRESENTATION_ITEM ( )  RATIONAL_B_SPLINE_CURVE ( ( 1.000000000000000000, 0.8047378541242988792, 0.8047378541242988792, 1.000000000000000000 ) ) 
 REPRESENTATION_ITEM ( '' )  );
#21863 = CARTESIAN_POINT ( 'NONE',  ( 194.5667039024482960, -47.82844715993405771, 300.4678068554149490 ) ) ;
#21862 = DIRECTION ( 'NONE',  ( 0.000000000000000000, 1.000000000000000000, 0.000000000000000000 ) ) ;
#21864 = DIRECTION ( 'NONE',  ( -0.000000000000000000, -0.000000000000000000, -1.000000000000000000 ) ) ;
#21865 = CARTESIAN_POINT ( 'NONE',  ( 100.8874678611112472, -44.70022135721517742, 142.0522919402655191 ) ) ;
#21866 = ORIENTED_EDGE ( 'NONE', *, *, #11891, .T. ) ;
#21867 = CARTESIAN_POINT ( 'NONE',  ( 80.06648329127402519, -46.72944715994105991, 1.625625275910943746 ) ) ;
#21868 = LINE ( 'NONE', #75137, #48301 ) ;
#21869 = CARTESIAN_POINT ( 'NONE',  ( 144.4532657509292335, -72.54478064608022692, 540.9756252759101471 ) ) ;
#21870 = CIRCLE ( 'NONE', #40709, 2.517499999999998739 ) ;
#21871 = CARTESIAN_POINT ( 'NONE',  ( 108.3220630915710530, -47.10059840840933987, 113.6727681330539639 ) ) ;
#21873 = CARTESIAN_POINT ( 'NONE',  ( 126.9629299006805638, -46.62589376934779750, 14.92562527591094046 ) ) ;
#21872 = DIRECTION ( 'NONE',  ( 0.9068632946707807507, -0.4214249218767881500, 9.028300618466658994E-16 ) ) ;
#21874 = DIRECTION ( 'NONE',  ( -0.000000000000000000, 1.000000000000000000, 0.000000000000000000 ) ) ;
#21875 = AXIS2_PLACEMENT_3D ( 'NONE', #68200, #62266, #5983 ) ;
#21876 = VERTEX_POINT ( 'NONE', #47706 ) ;
#21877 = LINE ( 'NONE', #22776, #78175 ) ;
#21878 = ADVANCED_FACE ( 'NONE', ( #13216 ), #82722, .F. ) ;
#21879 = CARTESIAN_POINT ( 'NONE',  ( 116.4171719250472137, -30.71472603919677624, 140.2813395616249750 ) ) ;
#21880 = AXIS2_PLACEMENT_3D ( 'NONE', #1717, #42563, #84401 ) ;
#21882 = ORIENTED_EDGE ( 'NONE', *, *, #2698, .T. ) ;
#21881 = DIRECTION ( 'NONE',  ( 1.000000000000000000, 0.000000000000000000, 0.000000000000000000 ) ) ;
#21883 = CARTESIAN_POINT ( 'NONE',  ( 99.34937008002601999, -28.84845824588786911, 266.7051490854347549 ) ) ;
#21884 = DIRECTION ( 'NONE',  ( 1.000000000000000000, 0.000000000000000000, 0.000000000000000000 ) ) ;
#21885 = DIRECTION ( 'NONE',  ( 0.9068632946707805287, -0.4214249218767882610, 1.035655806553318316E-15 ) ) ;
#21886 = CARTESIAN_POINT ( 'NONE',  ( -68.53801554307499089, 127.0000000000000000, 74.15067561874188584 ) ) ;
#21887 = LINE ( 'NONE', #75943, #79019 ) ;
#21888 = CARTESIAN_POINT ( 'NONE',  ( 67.65446888119937796, -138.2662121386932768, 245.5138901987639883 ) ) ;
#21889 = CARTESIAN_POINT ( 'NONE',  ( 172.5664832912740110, -18.82844715994099971, 201.0426252759120018 ) ) ;
#21890 = CARTESIAN_POINT ( 'NONE',  ( 101.5632356570520756, -44.81509498605974784, 197.1013395616259913 ) ) ;
#21891 = EDGE_LOOP ( 'NONE', ( #57241, #1644, #59323, #5436 ) ) ;
#21892 = EDGE_LOOP ( 'NONE', ( #42154, #34873, #25362, #20231 ) ) ;
#21893 = CARTESIAN_POINT ( 'NONE',  ( 99.50276801249795255, -32.11225214635365433, 167.3215833058969793 ) ) ;
#21894 = CARTESIAN_POINT ( 'NONE',  ( -3.175000000000120171, 111.1250000000000000, 33.98325472291465132 ) ) ;
#21895 = ADVANCED_FACE ( 'NONE', ( #19569 ), #21374, .F. ) ;
#21896 = CARTESIAN_POINT ( 'NONE',  ( 101.4562479827646371, -44.74122725731964323, 278.0899109901961879 ) ) ;
#21897 = DIRECTION ( 'NONE',  ( 0.000000000000000000, -1.000000000000000000, 0.000000000000000000 ) ) ;
#21898 = EDGE_CURVE ( 'NONE', #64904, #69092, #59221, .T. ) ;
#21899 = AXIS2_PLACEMENT_3D ( 'NONE', #83705, #34647, #14669 ) ;
#21900 = CARTESIAN_POINT ( 'NONE',  ( 123.6837132603319560, -54.60520651782485402, 218.8274735512161158 ) ) ;
#21901 = EDGE_CURVE ( 'NONE', #5232, #1162, #14569, .T. ) ;
#21902 = CARTESIAN_POINT ( 'NONE',  ( 7.661254700127833495, 82.54999999999999716, 320.6630000000000109 ) ) ;
#21903 = VECTOR ( 'NONE', #46518, 1000.000000000000000 ) ;
#21904 = DIRECTION ( 'NONE',  ( 1.000000000000000000, 0.000000000000000000, 0.000000000000000000 ) ) ;
#21905 = CARTESIAN_POINT ( 'NONE',  ( 63.06670390244699576, -67.87844715994098976, 190.2178068554179902 ) ) ;
#21906 = CARTESIAN_POINT ( 'NONE',  ( 115.4423046205436947, -29.55243945206539280, 229.4022919425779605 ) ) ;
#21907 = CARTESIAN_POINT ( 'NONE',  ( 9.497923889340652792, 90.87111597850432076, 117.9757597262406819 ) ) ;
#21908 = ORIENTED_EDGE ( 'NONE', *, *, #33286, .F. ) ;
#21910 = EDGE_LOOP ( 'NONE', ( #58824, #51697 ) ) ;
#21909 = VECTOR ( 'NONE', #54324, 1000.000000000000000 ) ;
#21911 = EDGE_CURVE ( 'NONE', #22294, #51499, #55857, .T. ) ;
#21912 = ADVANCED_FACE ( 'NONE', ( #88632 ), #40902, .T. ) ;
#21913 = CARTESIAN_POINT ( 'NONE',  ( 106.8177105000358154, -25.27021144450689505, 321.3088427749597713 ) ) ;
#21914 = CARTESIAN_POINT ( 'NONE',  ( -75.85717701425170389, 89.26692529358290074, -91.11128979799221383 ) ) ;
#21915 = CARTESIAN_POINT ( 'NONE',  ( 108.3341841271554244, -46.73478572737850101, 123.6756741429928184 ) ) ;
#21916 = DIRECTION ( 'NONE',  ( 1.000000000000000000, 0.000000000000000000, -7.043400939473319300E-33 ) ) ;
#21917 = AXIS2_PLACEMENT_3D ( 'NONE', #22396, #56445, #50078 ) ;
#21918 = EDGE_CURVE ( 'NONE', #52727, #63584, #51944, .T. ) ;
#21919 = CARTESIAN_POINT ( 'NONE',  ( 118.0115280580377402, -34.77548253539075063, 44.96705384733895272 ) ) ;
#21920 = CARTESIAN_POINT ( 'NONE',  ( 168.0371591254545649, -48.62818131005519007, 180.4678068554150059 ) ) ;
#21921 = VERTEX_POINT ( 'NONE', #54061 ) ;
#21922 = AXIS2_PLACEMENT_3D ( 'NONE', #25039, #80024, #81373 ) ;
#21923 = CARTESIAN_POINT ( 'NONE',  ( 111.0628700864597533, -47.08446675046669583, 13.85753003781498016 ) ) ;
#21924 = CARTESIAN_POINT ( 'NONE',  ( 46.83715912545424231, -47.82818131006082751, 300.4678068554150059 ) ) ;
#21925 = EDGE_CURVE ( 'NONE', #26765, #37091, #89807, .T. ) ;
#21926 = CARTESIAN_POINT ( 'NONE',  ( 110.8168587353559786, -26.33166992238134085, 249.7889586092445882 ) ) ;
#21927 = ORIENTED_EDGE ( 'NONE', *, *, #84015, .F. ) ;
#21928 = DIRECTION ( 'NONE',  ( 1.000000000000000078E-15, -1.000000000000000083E-30, -1.000000000000000000 ) ) ;
#21929 = CARTESIAN_POINT ( 'NONE',  ( 163.1639762274590169, -34.03355364505800651, -5.074374724088000832 ) ) ;
#21930 = CARTESIAN_POINT ( 'NONE',  ( 114.6207320473410931, -43.31440182122523197, 168.2560093401067149 ) ) ;
#21931 = EDGE_CURVE ( 'NONE', #37741, #6343, #76629, .T. ) ;
#21932 = CARTESIAN_POINT ( 'NONE',  ( 109.2937122495728772, -44.61120707852311540, 70.61380465530497474 ) ) ;
#21933 = CARTESIAN_POINT ( 'NONE',  ( 96.72156277063432128, -35.27346698316355145, 177.2156252759109805 ) ) ;
#21934 = AXIS2_PLACEMENT_3D ( 'NONE', #38400, #36644, #85258 ) ;
#21935 = DIRECTION ( 'NONE',  ( 1.017460296392624983E-15, 1.000000000000000000, 0.000000000000000000 ) ) ;
#21936 = VERTEX_POINT ( 'NONE', #78147 ) ;
#21937 = PLANE ( 'NONE',  #30575 ) ;
#21938 = ORIENTED_EDGE ( 'NONE', *, *, #20164, .T. ) ;
#21939 = ORIENTED_EDGE ( 'NONE', *, *, #42063, .F. ) ;
#21940 = DIRECTION ( 'NONE',  ( 0.000000000000000000, 0.000000000000000000, 1.000000000000000000 ) ) ;
#21941 = EDGE_LOOP ( 'NONE', ( #71486, #683, #35256, #15428, #55514, #29818, #31418 ) ) ;
#21942 = VERTEX_POINT ( 'NONE', #78596 ) ;
#21943 = CARTESIAN_POINT ( 'NONE',  ( 80.06648329127401098, -39.47944715994105991, 1.625625275910943746 ) ) ;
#21944 = LINE ( 'NONE', #53837, #46009 ) ;
#21945 = CARTESIAN_POINT ( 'NONE',  ( 103.9632409301644316, -45.23724106753869734, 96.70861030426696914 ) ) ;
#21946 = AXIS2_PLACEMENT_3D ( 'NONE', #35312, #84839, #63027 ) ;
#21947 = CARTESIAN_POINT ( 'NONE',  ( 104.5828969173064849, -26.58150870143000688, 285.2670538473396391 ) ) ;
#21948 = EDGE_CURVE ( 'NONE', #78870, #9320, #2725, .T. ) ;
#21949 = EDGE_CURVE ( 'NONE', #53017, #3248, #75193, .T. ) ;
#21950 = CARTESIAN_POINT ( 'NONE',  ( 88.90000000000000568, 66.67499999999999716, 219.0749999999999886 ) ) ;
#21951 = CARTESIAN_POINT ( 'NONE',  ( 127.5252020268926003, 20.32000000000000028, 177.0380000000000109 ) ) ;
#21952 = AXIS2_PLACEMENT_3D ( 'NONE', #29097, #57227, #85866 ) ;
#21953 = ORIENTED_EDGE ( 'NONE', *, *, #25905, .F. ) ;
#21954 = EDGE_CURVE ( 'NONE', #48511, #33376, #84058, .T. ) ;
#21955 = EDGE_LOOP ( 'NONE', ( #20027, #85567, #14759, #14645, #72315 ) ) ;
#21956 = PLANE ( 'NONE',  #29063 ) ;
#21957 = EDGE_CURVE ( 'NONE', #55604, #57432, #18584, .T. ) ;
#21958 = DIRECTION ( 'NONE',  ( 0.000000000000000000, 0.000000000000000000, -1.000000000000000000 ) ) ;
#21959 = CARTESIAN_POINT ( 'NONE',  ( 70.36520983569781151, -140.1685435066830223, 246.8677938034485635 ) ) ;
#21960 = CARTESIAN_POINT ( 'NONE',  ( 108.2420053567034017, -46.43931755893584779, 117.6727681330539639 ) ) ;
#21961 = CARTESIAN_POINT ( 'NONE',  ( 115.0563813407508889, -43.54951484902237979, 63.26419670448196797 ) ) ;
#21962 = DIRECTION ( 'NONE',  ( 0.000000000000000000, 0.000000000000000000, -1.000000000000000000 ) ) ;
#21963 = EDGE_LOOP ( 'NONE', ( #75267, #74519, #59464, #42601 ) ) ;
#21964 = CARTESIAN_POINT ( 'NONE',  ( 110.8168587353559786, -26.33166992238134085, 249.7889586092445882 ) ) ;
#21965 = CARTESIAN_POINT ( 'NONE',  ( 182.2300522401149863, -33.89581943344511217, -5.074374724088000832 ) ) ;
#21966 =( NAMED_UNIT ( * ) PLANE_ANGLE_UNIT ( ) SI_UNIT ( $, .RADIAN. ) );
#21967 = CARTESIAN_POINT ( 'NONE',  ( 25.56670390244797275, -67.87844715994100397, 137.2178068554150059 ) ) ;
#21968 = PLANE ( 'NONE',  #38685 ) ;
#21970 = FACE_OUTER_BOUND ( 'NONE', #66099, .T. ) ;
#21969 = DIRECTION ( 'NONE',  ( -0.7071067811865431318, 0.7071067811865517916, -7.071067811865425043E-16 ) ) ;
#21971 = CARTESIAN_POINT ( 'NONE',  ( 105.6456579547864436, -25.35845045263859987, 320.8626788258979445 ) ) ;
#21972 = CYLINDRICAL_SURFACE ( 'NONE', #19272, 0.2500000000000039968 ) ;
#21973 = DIRECTION ( 'NONE',  ( 0.7071067811865779928, -0.7071067811865171526, 7.071067811865786933E-16 ) ) ;
#21974 = VECTOR ( 'NONE', #41830, 1000.000000000000000 ) ;
#21975 = CARTESIAN_POINT ( 'NONE',  ( -12.70000000000000462, 82.96435431876527389, 129.9368274816651478 ) ) ;
#21976 = CARTESIAN_POINT ( 'NONE',  ( 0.000000000000000000, 100.5999999999999659, 88.90000000000000568 ) ) ;
#21977 = CARTESIAN_POINT ( 'NONE',  ( 20.03715912545639100, -24.42818131006202265, 180.4678068554150911 ) ) ;
#21979 = ORIENTED_EDGE ( 'NONE', *, *, #13176, .F. ) ;
#21978 = CARTESIAN_POINT ( 'NONE',  ( 104.4899544325742369, -26.97880758956900848, 260.2814586108214030 ) ) ;
#21980 = CARTESIAN_POINT ( 'NONE',  ( 31.56670390244699931, -19.82844715994111340, 342.9256252759109884 ) ) ;
#21981 = CARTESIAN_POINT ( 'NONE',  ( 114.4306803301698778, -27.41265490572180141, 274.5441967044824878 ) ) ;
#21982 = CARTESIAN_POINT ( 'NONE',  ( 114.0809025726587436, -44.48955379074138961, 129.1613395616249704 ) ) ;
#21983 = CARTESIAN_POINT ( 'NONE',  ( 118.0985323217624057, -37.71894194680212564, 29.74324432352998215 ) ) ;
#21984 = FACE_BOUND ( 'NONE', #80796, .T. ) ;
#21985 = CIRCLE ( 'NONE', #23479, 1.999999999999995781 ) ;
#21987 = CARTESIAN_POINT ( 'NONE',  ( 82.26522136040252065, -35.07517613921011446, 7.387586420632111128 ) ) ;
#21986 = DIRECTION ( 'NONE',  ( 1.000000000000000000, 1.000000000000000078E-15, 0.000000000000000000 ) ) ;
#21988 = CARTESIAN_POINT ( 'NONE',  ( 93.94797395270803975, -35.60435878782502783, 296.5517437918485939 ) ) ;
#21989 = VECTOR ( 'NONE', #18445, 1000.000000000000000 ) ;
#21990 = ORIENTED_EDGE ( 'NONE', *, *, #80777, .F. ) ;
#21991 = CARTESIAN_POINT ( 'NONE',  ( 107.0664832912739968, -36.72944715994100306, 287.6356252759109680 ) ) ;
#21992 = ORIENTED_EDGE ( 'NONE', *, *, #69839, .T. ) ;
#21993 = CARTESIAN_POINT ( 'NONE',  ( 108.5268020718178690, -45.14512305525489921, 167.1352769709339725 ) ) ;
#21995 = ORIENTED_EDGE ( 'NONE', *, *, #277, .F. ) ;
#21994 = CARTESIAN_POINT ( 'NONE',  ( 109.6395629035810231, -46.48095453850196179, 187.7817364959817326 ) ) ;
#21996 = DIRECTION ( 'NONE',  ( 1.000000000000000000, 0.000000000000000000, 0.000000000000000000 ) ) ;
#21997 = CARTESIAN_POINT ( 'NONE',  ( 117.2886123466743129, -34.79635738071010564, 154.9756252759109714 ) ) ;
#21998 = DIRECTION ( 'NONE',  ( -1.000000000000000078E-15, -1.000000000000000083E-30, 1.000000000000000000 ) ) ;
#21999 = DIRECTION ( 'NONE',  ( 1.157009245868378063E-15, -1.000000000000000000, 3.100000000000000044E-14 ) ) ;
#22000 = CARTESIAN_POINT ( 'NONE',  ( 116.3199495083284347, -32.94194616109231077, 85.13562527591095375 ) ) ;
#22001 = TOROIDAL_SURFACE ( 'NONE', #36518, 7.799999999999999822, 0.2999999999999999889 ) ;
#22002 = CARTESIAN_POINT ( 'NONE',  ( -90.32738470895290561, 74.16215221268205937, 76.79083731950235858 ) ) ;
#22003 = FACE_OUTER_BOUND ( 'NONE', #948, .T. ) ;
#22004 = CARTESIAN_POINT ( 'NONE',  ( 116.0091996907507905, -30.12340400999213941, 109.3327681330539605 ) ) ;
#22005 = ORIENTED_EDGE ( 'NONE', *, *, #8065, .F. ) ;
#22006 = EDGE_LOOP ( 'NONE', ( #63708, #40111 ) ) ;
#22008 = ORIENTED_EDGE ( 'NONE', *, *, #61530, .F. ) ;
#22007 = VECTOR ( 'NONE', #26535, 1000.000000000000000 ) ;
#22009 = CARTESIAN_POINT ( 'NONE',  ( 109.4844142153598057, -45.28606679814626546, 69.22729759161194352 ) ) ;
#22010 = PLANE ( 'NONE',  #12404 ) ;
#22012 = CYLINDRICAL_SURFACE ( 'NONE', #79600, 20.63750000000000284 ) ;
#22011 = CARTESIAN_POINT ( 'NONE',  ( 108.5755967597531679, -27.06580334247545494, 185.9527681330529845 ) ) ;
#22013 = DIRECTION ( 'NONE',  ( 1.639958061481212836E-42, -4.100000000000000342E-29, -1.000000000000000000 ) ) ;
#22014 = EDGE_CURVE ( 'NONE', #42594, #79965, #79031, .T. ) ;
#22015 = CARTESIAN_POINT ( 'NONE',  ( 127.0667052882550081, -78.66107132697013071, 55.21780685541800437 ) ) ;
#22016 = EDGE_CURVE ( 'NONE', #4456, #89731, #8648, .T. ) ;
#22017 = AXIS2_PLACEMENT_3D ( 'NONE', #12785, #62258, #75900 ) ;
#22018 = DIRECTION ( 'NONE',  ( 0.7071067811865969777, -0.7071067811864980568, 0.000000000000000000 ) ) ;
#22019 = EDGE_CURVE ( 'NONE', #77531, #74275, #37235, .T. ) ;
#22020 = DIRECTION ( 'NONE',  ( -0.7071067811865779928, 0.7071067811865171526, -6.612322855860441069E-17 ) ) ;
#22021 = LINE ( 'NONE', #65121, #34245 ) ;
#22022 = CARTESIAN_POINT ( 'NONE',  ( 103.2134869792595708, -46.43093390711695889, 117.2756252759109543 ) ) ;
#22023 = ORIENTED_EDGE ( 'NONE', *, *, #53206, .T. ) ;
#22024 = EDGE_LOOP ( 'NONE', ( #71932, #25948, #17901, #71874 ) ) ;
#22025 = AXIS2_PLACEMENT_3D ( 'NONE', #38805, #43830, #80168 ) ;
#22026 = ORIENTED_EDGE ( 'NONE', *, *, #49663, .T. ) ;
#22027 = EDGE_CURVE ( 'NONE', #2245, #16601, #78135, .T. ) ;
#22028 = ADVANCED_FACE ( 'NONE', ( #21832 ), #8192, .T. ) ;
#22029 = CARTESIAN_POINT ( 'NONE',  ( -99.33304294513271770, 89.94765885072627043, -84.72230615113613794 ) ) ;
#22030 = DIRECTION ( 'NONE',  ( -0.7071067811864671926, -0.7071067811866279529, -7.071067811864976379E-16 ) ) ;
#22031 = CARTESIAN_POINT ( 'NONE',  ( 51.34673845256550351, -29.62846900982264842, 313.9678068554150059 ) ) ;
#22032 = CARTESIAN_POINT ( 'NONE',  ( 98.55143180905920985, -33.04300857791147195, 208.8195189410199646 ) ) ;
#22033 = EDGE_CURVE ( 'NONE', #14083, #1794, #43274, .T. ) ;
#22034 = DIRECTION ( 'NONE',  ( 0.7071067811865597852, -0.7071067811865354713, 0.000000000000000000 ) ) ;
#22035 = EDGE_CURVE ( 'NONE', #8809, #84439, #80981, .T. ) ;
#22036 = FACE_OUTER_BOUND ( 'NONE', #15567, .T. ) ;
#22037 = ORIENTED_EDGE ( 'NONE', *, *, #83186, .F. ) ;
#22039 = ORIENTED_EDGE ( 'NONE', *, *, #47846, .T. ) ;
#22038 = ORIENTED_EDGE ( 'NONE', *, *, #33692, .T. ) ;
#22040 = VECTOR ( 'NONE', #29561, 1000.000000000000000 ) ;
#22041 = CARTESIAN_POINT ( 'NONE',  ( 106.5667039024470171, -94.77844715994206126, -19.78219314458232247 ) ) ;
#22042 = EDGE_LOOP ( 'NONE', ( #11469, #43970, #41218, #79058 ) ) ;
#22043 = VERTEX_POINT ( 'NONE', #2276 ) ;
#22044 = CARTESIAN_POINT ( 'NONE',  ( 31.89136050872298966, -31.76306994223740432, -5.074374724088000832 ) ) ;
#22045 = ADVANCED_FACE ( 'NONE', ( #84519 ), #15466, .T. ) ;
#22046 = CARTESIAN_POINT ( 'NONE',  ( 116.4296429186904049, -33.01435002197194279, 245.5587261630399780 ) ) ;
#22047 = LINE ( 'NONE', #49717, #50716 ) ;
#22048 = ORIENTED_EDGE ( 'NONE', *, *, #65025, .F. ) ;
#22049 = AXIS2_PLACEMENT_3D ( 'NONE', #49421, #83518, #14932 ) ;
#22050 = CARTESIAN_POINT ( 'NONE',  ( 183.5150000000000148, 53.21300000000000097, 41.63456447661469895 ) ) ;
#22051 = ADVANCED_FACE ( 'NONE', ( #51282 ), #57214, .T. ) ;
#22052 = CARTESIAN_POINT ( 'NONE',  ( -121.1982028425885858, 74.49303996718552412, 48.53946104397632411 ) ) ;
#22053 = ORIENTED_EDGE ( 'NONE', *, *, #6806, .T. ) ;
#22054 = VERTEX_POINT ( 'NONE', #86281 ) ;
#22055 = AXIS2_PLACEMENT_3D ( 'NONE', #57444, #78372, #29314 ) ;
#22056 = CARTESIAN_POINT ( 'NONE',  ( 110.8712199137570593, -45.97737147754565967, 112.8870656898620553 ) ) ;
#22057 = VERTEX_POINT ( 'NONE', #59443 ) ;
#22058 = VERTEX_POINT ( 'NONE', #80366 ) ;
#22059 = CARTESIAN_POINT ( 'NONE',  ( 99.09762411907954061, -31.97621503831505407, 278.7166617981628178 ) ) ;
#22060 = CARTESIAN_POINT ( 'NONE',  ( 95.99055855653007541, -36.58346519971924948, 156.3280062282919687 ) ) ;
#22061 = CARTESIAN_POINT ( 'NONE',  ( 114.0075736764523100, -28.98025818340840942, 114.4956252759109816 ) ) ;
#22062 = CARTESIAN_POINT ( 'NONE',  ( 116.5506768258616432, -39.71645928710276507, 249.5838068554167819 ) ) ;
#22063 = DIRECTION ( 'NONE',  ( 1.000000000000000000, 4.510281037539819615E-14, 0.000000000000000000 ) ) ;
#22064 = CARTESIAN_POINT ( 'NONE',  ( 106.3019393658184129, -47.12646404140136269, 218.5184824187679453 ) ) ;
#22065 = DIRECTION ( 'NONE',  ( -8.953411488912552682E-16, 1.000000000000000000, 0.000000000000000000 ) ) ;
#22066 = PLANE ( 'NONE',  #45120 ) ;
#22067 = ORIENTED_EDGE ( 'NONE', *, *, #43533, .F. ) ;
#22068 = CARTESIAN_POINT ( 'NONE',  ( 130.5559380315087878, 69.85063703626886422, 0.8489233174145797145 ) ) ;
#22069 = ORIENTED_EDGE ( 'NONE', *, *, #87865, .F. ) ;
#22070 = VECTOR ( 'NONE', #9710, 1000.000000000000000 ) ;
#22071 = EDGE_CURVE ( 'NONE', #65869, #7080, #9910, .T. ) ;
#22072 = ORIENTED_EDGE ( 'NONE', *, *, #66482, .T. ) ;
#22073 = DIRECTION ( 'NONE',  ( 0.000000000000000000, -1.000000000000000000, 0.000000000000000000 ) ) ;
#22074 = ADVANCED_FACE ( 'NONE', ( #18117 ), #25379, .T. ) ;
#22075 = AXIS2_PLACEMENT_3D ( 'NONE', #54437, #33577, #62173 ) ;
#22076 = CIRCLE ( 'NONE', #65556, 3.299999999999999822 ) ;
#22077 = EDGE_LOOP ( 'NONE', ( #35166, #53840, #81951, #38348 ) ) ;
#22078 = CARTESIAN_POINT ( 'NONE',  ( 114.7262375871959392, -43.80158930977980702, 123.2327681330539519 ) ) ;
#22079 = LINE ( 'NONE', #56099, #18124 ) ;
#22080 = CARTESIAN_POINT ( 'NONE',  ( -487.2989999999999782, 14.28750000000023945, 19.36139197104649767 ) ) ;
#22081 = DIRECTION ( 'NONE',  ( 1.000000000000000000, 4.163336342344333240E-14, 0.000000000000000000 ) ) ;
#22084 = CARTESIAN_POINT ( 'NONE',  ( 105.7790678824445223, -26.40611305247087870, 266.1756252759109884 ) ) ;
#22083 = CARTESIAN_POINT ( 'NONE',  ( 117.1011259092108787, -37.51040938078600107, 58.76384579545401721 ) ) ;
#22082 = CARTESIAN_POINT ( 'NONE',  ( 47.62500000000000000, 111.1250000000000000, 257.1750000000000114 ) ) ;
#22085 = DIRECTION ( 'NONE',  ( -0.8660254037844380415, -0.5000000000000012212, 1.550000000000001284E-14 ) ) ;
#22086 = CARTESIAN_POINT ( 'NONE',  ( 182.4202572930259976, -31.94127993907710206, -5.074374724088000832 ) ) ;
#22087 = DIRECTION ( 'NONE',  ( -0.8660253910675258515, -0.0001484127181930297611, 0.5000000000000041078 ) ) ;
#22088 = FACE_OUTER_BOUND ( 'NONE', #44136, .T. ) ;
#22089 = CARTESIAN_POINT ( 'NONE',  ( 115.8254323913364630, -31.73001882733125001, 255.2397919427014585 ) ) ;
#22090 = CIRCLE ( 'NONE', #72832, 4.750000000000004441 ) ;
#22091 = CARTESIAN_POINT ( 'NONE',  ( 146.4958942568945588, -137.3566279360900921, 246.9078157516118779 ) ) ;
#22093 = ORIENTED_EDGE ( 'NONE', *, *, #88459, .F. ) ;
#22092 = CARTESIAN_POINT ( 'NONE',  ( 115.0886446791137132, -30.00251675211520919, 269.3813395616250546 ) ) ;
#22094 = CARTESIAN_POINT ( 'NONE',  ( 44.45000000000000284, 50.79999999999999716, 206.3750000000000000 ) ) ;
#22095 = CARTESIAN_POINT ( 'NONE',  ( 98.07151883162052286, -42.11266039418816121, 161.7556252759109725 ) ) ;
#22096 = CARTESIAN_POINT ( 'NONE',  ( 100.4792253034169960, -27.85352395805916359, 31.59657765686396758 ) ) ;
#22097 = CARTESIAN_POINT ( 'NONE',  ( 98.51568282078342520, -45.00561318155631341, 187.9384824187679612 ) ) ;
#22098 = CARTESIAN_POINT ( 'NONE',  ( 0.000000000000000000, 1.270000000000000018, 0.000000000000000000 ) ) ;
#22099 = DIRECTION ( 'NONE',  ( 0.000000000000000000, -1.000000000000000000, 0.000000000000000000 ) ) ;
#22101 = DIRECTION ( 'NONE',  ( 1.000000000000000000, 4.299999999999999979E-14, 1.000000000000000078E-15 ) ) ;
#22100 = CARTESIAN_POINT ( 'NONE',  ( 141.8664832912739939, -71.52944715994085811, 361.9756252759100335 ) ) ;
#22102 = CARTESIAN_POINT ( 'NONE',  ( 199.3900000000000148, 52.73749999999999716, -34.92499999999999716 ) ) ;
#22103 = CARTESIAN_POINT ( 'NONE',  ( 98.58946256649487339, -99.96145986183429955, -19.78219314458215550 ) ) ;
#22104 = ORIENTED_EDGE ( 'NONE', *, *, #73838, .F. ) ;
#22105 = EDGE_CURVE ( 'NONE', #56233, #78479, #39005, .T. ) ;
#22106 = CARTESIAN_POINT ( 'NONE',  ( 163.1543517358616668, -31.62489322947754289, 237.4678068554150059 ) ) ;
#22107 = VERTEX_POINT ( 'NONE', #32185 ) ;
#22108 = ORIENTED_EDGE ( 'NONE', *, *, #57242, .F. ) ;
#22110 = ORIENTED_EDGE ( 'NONE', *, *, #84590, .T. ) ;
#22109 = CARTESIAN_POINT ( 'NONE',  ( 83.06670390244804025, -51.22944715994108122, 231.5838068554169524 ) ) ;
#22111 = CARTESIAN_POINT ( 'NONE',  ( 117.0329088946582630, -32.00354160957723337, 60.19086337114898555 ) ) ;
#22112 = DIRECTION ( 'NONE',  ( 1.000000000000000000, 1.000000000000000078E-15, 0.000000000000000000 ) ) ;
#22113 = LINE ( 'NONE', #85241, #51412 ) ;
#22114 = CARTESIAN_POINT ( 'NONE',  ( 101.9632951345543148, -45.91070444983295573, 183.1727681330539781 ) ) ;
#22115 = AXIS2_PLACEMENT_3D ( 'NONE', #82544, #13926, #61604 ) ;
#22116 = CARTESIAN_POINT ( 'NONE',  ( 100.7827017321902758, -30.20819270671951173, 265.0971817328389761 ) ) ;
#22117 = ORIENTED_EDGE ( 'NONE', *, *, #24591, .F. ) ;
#22118 = EDGE_CURVE ( 'NONE', #9193, #2431, #17242, .T. ) ;
#22119 = EDGE_LOOP ( 'NONE', ( #46810, #14355, #58523, #39866 ) ) ;
#22120 = ORIENTED_EDGE ( 'NONE', *, *, #185, .F. ) ;
#22121 = AXIS2_PLACEMENT_3D ( 'NONE', #19886, #784, #82585 ) ;
#22122 = ORIENTED_EDGE ( 'NONE', *, *, #49003, .F. ) ;
#22123 = CARTESIAN_POINT ( 'NONE',  ( 98.30753419365476020, -41.72887549635444060, 106.7397919430594300 ) ) ;
#22124 = CARTESIAN_POINT ( 'NONE',  ( 226.4410000000000025, 40.03750000000000142, -58.73749999999999716 ) ) ;
#22125 = CARTESIAN_POINT ( 'NONE',  ( 97.07205900541282517, -35.37856870842702506, 162.2189687603248558 ) ) ;
#22126 = CARTESIAN_POINT ( 'NONE',  ( 99.09570906993977246, -30.55043176099360025, 75.80229194336320120 ) ) ;
#22127 = DIRECTION ( 'NONE',  ( 4.299999999999999979E-14, -1.000000000000000000, 0.000000000000000000 ) ) ;
#22128 = EDGE_CURVE ( 'NONE', #27158, #10599, #30867, .T. ) ;
#22129 = CARTESIAN_POINT ( 'NONE',  ( 181.5667039024459939, -22.48495420874030515, -5.074374724088000832 ) ) ;
#22130 = EDGE_CURVE ( 'NONE', #49937, #29939, #38994, .T. ) ;
#22131 = DIRECTION ( 'NONE',  ( 0.7071067811862279395, -0.7071067811868672059, 7.071067811862286363E-16 ) ) ;
#22132 = EDGE_CURVE ( 'NONE', #24430, #76709, #58552, .T. ) ;
#22133 = CARTESIAN_POINT ( 'NONE',  ( 80.06648329127398256, -9.029447159941060619, 1.625625275910943746 ) ) ;
#22134 = CARTESIAN_POINT ( 'NONE',  ( 96.85498737197825392, -38.89503640450125488, 31.49276813305495892 ) ) ;
#22135 = FACE_OUTER_BOUND ( 'NONE', #87363, .T. ) ;
#22137 = ORIENTED_EDGE ( 'NONE', *, *, #19963, .T. ) ;
#22136 = AXIS2_PLACEMENT_3D ( 'NONE', #22140, #63450, #76180 ) ;
#22138 = EDGE_CURVE ( 'NONE', #64928, #41501, #34590, .T. ) ;
#22139 = DIRECTION ( 'NONE',  ( 0.000000000000000000, 0.000000000000000000, 1.000000000000000000 ) ) ;
#22140 = CARTESIAN_POINT ( 'NONE',  ( 134.0664832912740110, -8.729447159940999512, 308.6356252759119911 ) ) ;
#22141 = CARTESIAN_POINT ( 'NONE',  ( 108.0475348069766284, -44.83298120013808585, 115.4909475124489830 ) ) ;
#22142 = EDGE_CURVE ( 'NONE', #44500, #62791, #63652, .T. ) ;
#22143 = FACE_BOUND ( 'NONE', #23270, .T. ) ;
#22144 = ADVANCED_FACE ( 'NONE', ( #9981 ), #86730, .T. ) ;
#22145 = AXIS2_PLACEMENT_3D ( 'NONE', #39797, #47948, #75689 ) ;
#22146 = CARTESIAN_POINT ( 'NONE',  ( -98.60478223830740774, 120.6499999999999915, -1.074461880482445986E-12 ) ) ;
#22147 = ORIENTED_EDGE ( 'NONE', *, *, #62829, .F. ) ;
#22148 = ORIENTED_EDGE ( 'NONE', *, *, #86638, .T. ) ;
#22149 = CARTESIAN_POINT ( 'NONE',  ( 98.04152496004225270, -41.04187039268755655, 136.6813859289020741 ) ) ;
#22150 = ORIENTED_EDGE ( 'NONE', *, *, #22035, .T. ) ;
#22151 = ORIENTED_EDGE ( 'NONE', *, *, #50337, .F. ) ;
#22152 = CARTESIAN_POINT ( 'NONE',  ( 98.21222678671237816, -37.09057735734792516, 157.7901547344689845 ) ) ;
#22153 = CARTESIAN_POINT ( 'NONE',  ( -12.05172457139580011, 86.64129263485729382, 117.9422889837464510 ) ) ;
#22154 = CARTESIAN_POINT ( 'NONE',  ( 98.31807308660266642, -42.43931386104045345, 97.78705384733993355 ) ) ;
#22155 = FACE_OUTER_BOUND ( 'NONE', #64758, .T. ) ;
#22156 = ORIENTED_EDGE ( 'NONE', *, *, #86809, .F. ) ;
#22157 = ORIENTED_EDGE ( 'NONE', *, *, #21323, .T. ) ;
#22158 = ORIENTED_EDGE ( 'NONE', *, *, #34080, .T. ) ;
#22160 = DIRECTION ( 'NONE',  ( 0.000000000000000000, -1.000000000000000000, 0.000000000000000000 ) ) ;
#22159 = AXIS2_PLACEMENT_3D ( 'NONE', #59380, #25317, #4881 ) ;
#22161 = ORIENTED_EDGE ( 'NONE', *, *, #68606, .T. ) ;
#22162 = CARTESIAN_POINT ( 'NONE',  ( 97.60228370312334789, -39.19771807597653179, 276.5299109901972088 ) ) ;
#22163 = CARTESIAN_POINT ( 'NONE',  ( 118.9020112566783354, -37.70028621367283961, 184.7613395616249647 ) ) ;
#22164 = CARTESIAN_POINT ( 'NONE',  ( 160.2664750769284865, 20.32000000000000028, -148.0533267522753818 ) ) ;
#22165 = PLANE ( 'NONE',  #11222 ) ;
#22166 = CARTESIAN_POINT ( 'NONE',  ( 102.6976273654655643, -46.88262786655960923, 133.2651490854349561 ) ) ;
#22167 = DIRECTION ( 'NONE',  ( 0.9068632946707805287, -0.4214249218767882055, 8.839355291601567287E-16 ) ) ;
#22168 = EDGE_LOOP ( 'NONE', ( #62796, #75150, #74287, #87010 ) ) ;
#22169 = DIRECTION ( 'NONE',  ( 0.000000000000000000, 0.000000000000000000, -1.000000000000000000 ) ) ;
#22170 = VERTEX_POINT ( 'NONE', #18566 ) ;
#22171 = CARTESIAN_POINT ( 'NONE',  ( 116.8167403593138687, -34.15142894304322851, 135.0315941499441408 ) ) ;
#22172 = EDGE_LOOP ( 'NONE', ( #14769, #35913, #64254, #8402 ) ) ;
#22173 = EDGE_CURVE ( 'NONE', #46741, #71950, #10419, .T. ) ;
#22174 = ORIENTED_EDGE ( 'NONE', *, *, #34695, .F. ) ;
#22175 = CIRCLE ( 'NONE', #84560, 2.117000000000000881 ) ;
#22176 = CYLINDRICAL_SURFACE ( 'NONE', #88167, 34.13125000000000142 ) ;
#22177 = CARTESIAN_POINT ( 'NONE',  ( 11.65427314393061309, 87.39163397251130050, 117.9821062356120080 ) ) ;
#22178 = CARTESIAN_POINT ( 'NONE',  ( 97.10456541990245682, -39.80308206185652864, 21.56419670448195092 ) ) ;
#22179 = CARTESIAN_POINT ( 'NONE',  ( -33.98325472291465132, 111.1250000000000000, 3.174999999999764899 ) ) ;
#22180 = DIRECTION ( 'NONE',  ( 0.000000000000000000, 1.000000000000000000, 0.000000000000000000 ) ) ;
#22181 = CARTESIAN_POINT ( 'NONE',  ( 107.0664832912739257, -50.22944715994095333, 315.1356252759112522 ) ) ;
#22182 = CARTESIAN_POINT ( 'NONE',  ( 109.4837483930865574, -46.20680252518646114, 47.77562527591094721 ) ) ;
#22184 = CARTESIAN_POINT ( 'NONE',  ( 114.1602155298369325, -45.17592836263234091, 144.1203871806729637 ) ) ;
#22183 = DIRECTION ( 'NONE',  ( 0.002456323621556914284, -0.5003413983110611696, -0.8658247233767341067 ) ) ;
#22185 = CARTESIAN_POINT ( 'NONE',  ( 97.33784130821194935, -34.07106454015703179, 72.11479194342473420 ) ) ;
#22186 = DIRECTION ( 'NONE',  ( 0.000000000000000000, 0.000000000000000000, -1.000000000000000000 ) ) ;
#22187 = ORIENTED_EDGE ( 'NONE', *, *, #36671, .T. ) ;
#22188 = FACE_OUTER_BOUND ( 'NONE', #43252, .T. ) ;
#22189 = CARTESIAN_POINT ( 'NONE',  ( 98.58946256649485917, -108.5954344580498514, -19.78219314458187839 ) ) ;
#22190 = CARTESIAN_POINT ( 'NONE',  ( 151.0371591254573502, -24.42818131005593685, 237.4678068554150059 ) ) ;
#22191 = ORIENTED_EDGE ( 'NONE', *, *, #64421, .F. ) ;
#22192 = FACE_OUTER_BOUND ( 'NONE', #37721, .T. ) ;
#22194 = ORIENTED_EDGE ( 'NONE', *, *, #45770, .T. ) ;
#22193 = CARTESIAN_POINT ( 'NONE',  ( 117.1106518157658343, -39.68263944894788864, 183.5984824187679578 ) ) ;
#22195 = DIRECTION ( 'NONE',  ( 3.999999999999999995E-14, -1.000000000000000000, 4.100000000000000342E-29 ) ) ;
#22196 = CARTESIAN_POINT ( 'NONE',  ( 96.11533564597472434, -35.06885359281673686, 217.1946728949589840 ) ) ;
#22197 = CARTESIAN_POINT ( 'NONE',  ( 106.0723295733845362, -48.58789440604735432, 108.5099109901969712 ) ) ;
#22198 = LINE ( 'NONE', #14930, #59191 ) ;
#22199 = CARTESIAN_POINT ( 'NONE',  ( 103.1875000000000000, 127.0000000000000000, -5.041899999999640336 ) ) ;
#22200 = CARTESIAN_POINT ( 'NONE',  ( 108.3334481036005599, -46.73485935279997960, 77.67729194326504683 ) ) ;
#22201 = VERTEX_POINT ( 'NONE', #52604 ) ;
#22203 = EDGE_CURVE ( 'NONE', #65784, #73034, #11304, .T. ) ;
#22202 = CIRCLE ( 'NONE', #67162, 2.517499999999998739 ) ;
#22204 = VERTEX_POINT ( 'NONE', #46246 ) ;
#22205 = ORIENTED_EDGE ( 'NONE', *, *, #8773, .T. ) ;
#22206 = VERTEX_POINT ( 'NONE', #73983 ) ;
#22207 = CARTESIAN_POINT ( 'NONE',  ( 107.0667039024470313, -104.2784471599412086, 7.717806855417980394 ) ) ;
#22208 = CARTESIAN_POINT ( 'NONE',  ( 98.89890862997502552, -29.28198419350761483, 226.7261014663869503 ) ) ;
#22209 = CARTESIAN_POINT ( 'NONE',  ( 97.01732288581034425, -36.31871811287255980, 251.2938706393009340 ) ) ;
#22210 = CARTESIAN_POINT ( 'NONE',  ( 134.0664832912739826, -15.97944715994100306, 1.625625275910997480 ) ) ;
#22212 = CARTESIAN_POINT ( 'NONE',  ( 182.3467384525650061, -29.62846900982231446, 342.9256252759119548 ) ) ;
#22211 = FACE_BOUND ( 'NONE', #81715, .T. ) ;
#22213 = FACE_OUTER_BOUND ( 'NONE', #55576, .T. ) ;
#22214 = CARTESIAN_POINT ( 'NONE',  ( 117.5098600993040066, -37.01623072280121107, 43.80419670448293346 ) ) ;
#22215 = ORIENTED_EDGE ( 'NONE', *, *, #50194, .F. ) ;
#22216 = ORIENTED_EDGE ( 'NONE', *, *, #33440, .T. ) ;
#22217 = AXIS2_PLACEMENT_3D ( 'NONE', #3864, #72900, #5204 ) ;
#22218 = CARTESIAN_POINT ( 'NONE',  ( 115.0901107527865150, -30.61920090636028036, 15.34508885633713682 ) ) ;
#22219 = CARTESIAN_POINT ( 'NONE',  ( 117.6440909798951253, -33.30491947301820232, 280.0756252759109657 ) ) ;
#22220 = EDGE_CURVE ( 'NONE', #378, #7095, #57811, .T. ) ;
#22221 = DIRECTION ( 'NONE',  ( 0.8660254037844382635, 0.5000000000000008882, -1.550000000000000022E-14 ) ) ;
#22222 = AXIS2_PLACEMENT_3D ( 'NONE', #83773, #21998, #69239 ) ;
#22223 = CARTESIAN_POINT ( 'NONE',  ( 112.7054497023526238, -28.73785826246146158, 125.5870538473389502 ) ) ;
#22224 = EDGE_CURVE ( 'NONE', #57373, #8193, #52164, .T. ) ;
#22225 = FACE_BOUND ( 'NONE', #89735, .T. ) ;
#22226 = EDGE_CURVE ( 'NONE', #27286, #40899, #67159, .T. ) ;
#22227 = DIRECTION ( 'NONE',  ( 1.000000000000000000, -0.000000000000000000, 0.000000000000000000 ) ) ;
#22228 = ORIENTED_EDGE ( 'NONE', *, *, #68466, .T. ) ;
#22229 = DIRECTION ( 'NONE',  ( 0.000000000000000000, 1.000000000000000000, 0.000000000000000000 ) ) ;
#22230 = EDGE_CURVE ( 'NONE', #78219, #23819, #4942, .T. ) ;
#22231 = DIRECTION ( 'NONE',  ( -0.000000000000000000, -0.000000000000000000, -1.000000000000000000 ) ) ;
#22232 = ORIENTED_EDGE ( 'NONE', *, *, #55176, .F. ) ;
#22233 = VERTEX_POINT ( 'NONE', #10861 ) ;
#22234 = CARTESIAN_POINT ( 'NONE',  ( -74.62309654709146400, 85.43299024555680887, 92.12450916458723782 ) ) ;
#22235 = CARTESIAN_POINT ( 'NONE',  ( 100.5471494818408189, -29.96373860736636274, 262.1063452106591853 ) ) ;
#22236 = CIRCLE ( 'NONE', #6266, 188.9759999999999991 ) ;
#22237 = DIRECTION ( 'NONE',  ( 0.000000000000000000, 0.000000000000000000, -1.000000000000000000 ) ) ;
#22238 = CARTESIAN_POINT ( 'NONE',  ( 48.86082318535700608, -35.55794170701751256, 342.9256252759119548 ) ) ;
#22239 = FACE_OUTER_BOUND ( 'NONE', #70735, .T. ) ;
#22240 = ADVANCED_FACE ( 'NONE', ( #66254 ), #4048, .F. ) ;
#22241 = CARTESIAN_POINT ( 'NONE',  ( 87.72765544449647734, 71.14137858619483268, -79.74945239053471369 ) ) ;
#22242 = ORIENTED_EDGE ( 'NONE', *, *, #16473, .F. ) ;
#22243 = CYLINDRICAL_SURFACE ( 'NONE', #20419, 38.10000000000000142 ) ;
#22244 = CARTESIAN_POINT ( 'NONE',  ( 107.5667039024470171, -94.77844715994137914, 2.217806855417697953 ) ) ;
#22245 = EDGE_LOOP ( 'NONE', ( #53583, #57279 ) ) ;
#22246 = CARTESIAN_POINT ( 'NONE',  ( 97.62219055090962172, -32.23153194184447301, 75.97276813305397525 ) ) ;
#22247 = ORIENTED_EDGE ( 'NONE', *, *, #38084, .T. ) ;
#22248 = CARTESIAN_POINT ( 'NONE',  ( 99.46800687602927837, -39.83949638310546248, 11.05813411379097388 ) ) ;
#22249 = DIRECTION ( 'NONE',  ( 1.000000000000000000, 0.000000000000000000, 3.902639990948949304E-17 ) ) ;
#22250 = CARTESIAN_POINT ( 'NONE',  ( 109.2168187703261282, -26.58475186820026792, 184.9222919425779708 ) ) ;
#22251 = CARTESIAN_POINT ( 'NONE',  ( 23.44892695906009905, 79.39921112727093089, 299.3104155498348291 ) ) ;
#22252 = CARTESIAN_POINT ( 'NONE',  ( 181.8884939055946006, -32.11662333283960180, 313.9678068554149490 ) ) ;
#22253 = CARTESIAN_POINT ( 'NONE',  ( 52.99265158129170317, 95.25000000000000000, 346.9005000000000223 ) ) ;
#22254 = DIRECTION ( 'NONE',  ( -0.000000000000000000, -1.000000000000000000, 0.000000000000000000 ) ) ;
#22255 = CARTESIAN_POINT ( 'NONE',  ( 96.93665061341955891, -39.37131572480267749, 272.5299109901966972 ) ) ;
#22256 = CARTESIAN_POINT ( 'NONE',  ( 98.41008151203357102, -41.80409597589088833, 116.7490096102640251 ) ) ;
#22257 = ORIENTED_EDGE ( 'NONE', *, *, #86780, .T. ) ;
#22258 = VECTOR ( 'NONE', #55650, 1000.000000000000000 ) ;
#22259 = CARTESIAN_POINT ( 'NONE',  ( 107.0667039024470313, -104.2784471599420471, -19.18411693322902423 ) ) ;
#22260 = ORIENTED_EDGE ( 'NONE', *, *, #38145, .F. ) ;
#22261 = CARTESIAN_POINT ( 'NONE',  ( 118.9671133714783480, -36.92893286478360437, 149.8127681330539644 ) ) ;
#22262 = FACE_OUTER_BOUND ( 'NONE', #69448, .T. ) ;
#22263 = ORIENTED_EDGE ( 'NONE', *, *, #48538, .F. ) ;
#22264 = ORIENTED_EDGE ( 'NONE', *, *, #68550, .T. ) ;
#22265 = ORIENTED_EDGE ( 'NONE', *, *, #13098, .F. ) ;
#22266 = CARTESIAN_POINT ( 'NONE',  ( 116.3201495438094923, -32.94088975182634726, 124.1356252759109537 ) ) ;
#22267 = CARTESIAN_POINT ( 'NONE',  ( 194.0371591254575208, -24.42818131005417115, 180.4678068554150343 ) ) ;
#22268 = CYLINDRICAL_SURFACE ( 'NONE', #45699, 9.999999999999998224 ) ;
#22269 = LINE ( 'NONE', #57663, #36505 ) ;
#22270 = CARTESIAN_POINT ( 'NONE',  ( 140.0167039024470910, -144.7284471599409414, 55.21780685541800437 ) ) ;
#22271 = CARTESIAN_POINT ( 'NONE',  ( 114.0905851706116181, -46.27390148416495208, 29.08133956162595268 ) ) ;
#22272 = CARTESIAN_POINT ( 'NONE',  ( 172.5664832912729878, -27.57844715994070484, 138.9256252759119832 ) ) ;
#22273 = ORIENTED_EDGE ( 'NONE', *, *, #23217, .F. ) ;
#22274 = DIRECTION ( 'NONE',  ( -7.340987889507870014E-14, 0.000000000000000000, -1.000000000000000000 ) ) ;
#22275 = CARTESIAN_POINT ( 'NONE',  ( 112.0659081082637840, -45.48839843342108225, 42.98939337566707763 ) ) ;
#22276 = EDGE_CURVE ( 'NONE', #6343, #38814, #55740, .T. ) ;
#22277 = ORIENTED_EDGE ( 'NONE', *, *, #17456, .T. ) ;
#22278 = ORIENTED_EDGE ( 'NONE', *, *, #77080, .T. ) ;
#22279 = CARTESIAN_POINT ( 'NONE',  ( 82.74959284958350736, -19.33856210726131053, 3.004220725470469144 ) ) ;
#22280 = LINE ( 'NONE', #50409, #55601 ) ;
#22281 = PLANE ( 'NONE',  #35648 ) ;
#22282 = EDGE_CURVE ( 'NONE', #67095, #69124, #26278, .T. ) ;
#22283 = FACE_BOUND ( 'NONE', #34855, .T. ) ;
#22284 = LINE ( 'NONE', #36354, #6943 ) ;
#22285 = CARTESIAN_POINT ( 'NONE',  ( 102.4276729374712431, -43.93594010915269621, 221.5438483995059755 ) ) ;
#22286 = PLANE ( 'NONE',  #67845 ) ;
#22287 = CARTESIAN_POINT ( 'NONE',  ( -24.79284581386642827, 184.0000000000000000, 106.1020876358972771 ) ) ;
#22288 = CARTESIAN_POINT ( 'NONE',  ( 117.4149692539380681, -32.71426074976766074, 94.10895860924395606 ) ) ;
#22289 = EDGE_LOOP ( 'NONE', ( #74984, #15958, #65831, #60317 ) ) ;
#22290 = CARTESIAN_POINT ( 'NONE',  ( 131.4346950876525568, -19.52719034724729497, 6.916533740478841175 ) ) ;
#22291 = VERTEX_POINT ( 'NONE', #39897 ) ;
#22292 = AXIS2_PLACEMENT_3D ( 'NONE', #22326, #56372, #58176 ) ;
#22293 = CARTESIAN_POINT ( 'NONE',  ( 113.6135369627281335, -29.08718243961786598, 275.5131478814660682 ) ) ;
#22294 = VERTEX_POINT ( 'NONE', #5853 ) ;
#22295 = DIRECTION ( 'NONE',  ( 0.000000000000000000, -3.785359618865284342E-16, -1.000000000000000000 ) ) ;
#22296 = ORIENTED_EDGE ( 'NONE', *, *, #54344, .T. ) ;
#22297 = DIRECTION ( 'NONE',  ( 1.000000000000000000, 0.000000000000000000, 0.000000000000000000 ) ) ;
#22298 = CARTESIAN_POINT ( 'NONE',  ( 100.8879627497241387, -44.70063105137227666, 273.0519027137635248 ) ) ;
#22299 = VECTOR ( 'NONE', #20791, 1000.000000000000000 ) ;
#22300 = FACE_OUTER_BOUND ( 'NONE', #46687, .T. ) ;
#22301 = ORIENTED_EDGE ( 'NONE', *, *, #77802, .F. ) ;
#22302 = EDGE_CURVE ( 'NONE', #54218, #15323, #33975, .T. ) ;
#22303 = CARTESIAN_POINT ( 'NONE',  ( 102.5485826229696329, -27.30952478670668881, 95.43276813305395478 ) ) ;
#22304 = SURFACE_STYLE_FILL_AREA ( #56345 ) ;
#22306 = DIRECTION ( 'NONE',  ( -1.000000000000000078E-15, 1.000000000000000083E-30, 1.000000000000000000 ) ) ;
#22305 = LINE ( 'NONE', #34569, #52101 ) ;
#22307 = CARTESIAN_POINT ( 'NONE',  ( 3.175000000000355094, 124.5870000000000033, -33.98325472291460159 ) ) ;
#22308 = CARTESIAN_POINT ( 'NONE',  ( -10.69948253693739026, 75.88274056138229184, 117.8716134549241872 ) ) ;
#22309 = ORIENTED_EDGE ( 'NONE', *, *, #49782, .F. ) ;
#22310 = CARTESIAN_POINT ( 'NONE',  ( 127.4058501689331280, -122.7870702624433221, 250.2178068554179902 ) ) ;
#22311 = FACE_OUTER_BOUND ( 'NONE', #74906, .T. ) ;
#22312 = LINE ( 'NONE', #77728, #29883 ) ;
#22313 = CARTESIAN_POINT ( 'NONE',  ( 116.6182342972125809, -29.67350615900649657, 105.3327681330539463 ) ) ;
#22315 = DIRECTION ( 'NONE',  ( 0.000000000000000000, -1.000000000000000000, 0.000000000000000000 ) ) ;
#22314 = CARTESIAN_POINT ( 'NONE',  ( 29.56648329127298069, -71.37844715994266664, 342.9256252759109884 ) ) ;
#22316 = DIRECTION ( 'NONE',  ( -1.000000000000000000, 0.000000000000000000, 0.000000000000000000 ) ) ;
#22317 = VECTOR ( 'NONE', #36925, 1000.000000000000000 ) ;
#22318 = VERTEX_POINT ( 'NONE', #60791 ) ;
#22319 = VECTOR ( 'NONE', #11309, 1000.000000000000000 ) ;
#22320 = DIRECTION ( 'NONE',  ( -0.000000000000000000, 1.000000000000000000, -0.000000000000000000 ) ) ;
#22321 = CARTESIAN_POINT ( 'NONE',  ( 96.71010325458821910, -37.26253042779857338, 117.3794347997199594 ) ) ;
#22322 = EDGE_CURVE ( 'NONE', #82906, #69283, #34595, .T. ) ;
#22324 = ORIENTED_EDGE ( 'NONE', *, *, #68336, .F. ) ;
#22323 = DIRECTION ( 'NONE',  ( 1.000000000000000078E-15, -1.000000000000000000, 0.000000000000000000 ) ) ;
#22325 = CARTESIAN_POINT ( 'NONE',  ( 115.5963437193832277, -42.63132022635295471, 9.356577656862985037 ) ) ;
#22326 = CARTESIAN_POINT ( 'NONE',  ( 74.06670390244704549, -118.2784471599409812, 51.21780685541800437 ) ) ;
#22327 = DIRECTION ( 'NONE',  ( 1.000000000000000078E-15, 1.000000000000000083E-30, -1.000000000000000000 ) ) ;
#22328 = FACE_OUTER_BOUND ( 'NONE', #11995, .T. ) ;
#22329 = EDGE_CURVE ( 'NONE', #16664, #12989, #75332, .T. ) ;
#22330 = CARTESIAN_POINT ( 'NONE',  ( 245.4909999999999854, 65.43750000000000000, -67.11950000000000216 ) ) ;
#22331 = FACE_BOUND ( 'NONE', #36311, .T. ) ;
#22332 = CARTESIAN_POINT ( 'NONE',  ( 99.34779341711919187, -29.80408710710932496, 235.7565776568639819 ) ) ;
#22333 = ORIENTED_EDGE ( 'NONE', *, *, #65864, .F. ) ;
#22334 = ORIENTED_EDGE ( 'NONE', *, *, #31813, .F. ) ;
#22335 = CARTESIAN_POINT ( 'NONE',  ( 113.2524973562852608, -30.34232264463288686, 170.8958690201829711 ) ) ;
#22336 = B_SPLINE_CURVE_WITH_KNOTS ( 'NONE', 3,
 ( #15628, #15172, #63317, #21546, #69688, #8360, #49219, #76498, #64221, #70587, #62857, #36057, #50570, #14731, #77852, #55570, #63774, #83320, #70132, #29252, #78312, #43301, #1551, #56937, #71046, #633, #57385, #7459, #28804, #71492, #35600, #42405, #27895, #22000 ),
 .UNSPECIFIED., .F., .F.,
 ( 4, 2, 2, 2, 2, 2, 2, 2, 2, 1, 1, 1, 1, 2, 2, 2, 2, 2, 4 ),
 ( 0.5000923170378537286, 0.5625807774081261758, 0.6250692377783986231, 0.6875576981486710704, 0.7188019283338071830, 0.7500461585189430735, 0.8125346188892145216, 0.8437788490743498571, 0.8594009641669180244, 0.8672120217132019970, 0.8711175504863439834, 0.8730703148729151986, 0.8740466970662008617, 0.8745348881628436377, 0.8750230792594864138, 0.9062673094446147548, 0.9375115396297432069, 0.9687557698148714369, 1.000000000000000000 ),
 .UNSPECIFIED. ) ;
#22337 = AXIS2_PLACEMENT_3D ( 'NONE', #23589, #15873, #70382 ) ;
#22338 = LINE ( 'NONE', #535, #76270 ) ;
#22339 = CARTESIAN_POINT ( 'NONE',  ( 115.9938408324894539, -42.00591253359444011, 279.4137205140056608 ) ) ;
#22340 = VECTOR ( 'NONE', #9806, 1000.000000000000000 ) ;
#22341 = CARTESIAN_POINT ( 'NONE',  ( 23.71390425477495256, 83.78871496225653459, 298.2858669080578693 ) ) ;
#22342 = VECTOR ( 'NONE', #23961, 1000.000000000000000 ) ;
#22343 = B_SPLINE_CURVE_WITH_KNOTS ( 'NONE', 3,
 ( #78465, #37557, #43453, #65257, #37996, #86602, #72955, #85280, #72528, #65690, #43902, #23931, #31168, #79802, #50267, #3036, #29405, #51604, #30734, #71194, #23052, #50727, #58865, #64371, #79354, #36667, #24375, #58429, #17556, #84827, #57085, #45233, #2146, #22593, #36212, #1701, #29852, #78009, #15776, #16226, #57540, #37110, #64815, #2597, #30292, #57991, #85723, #23499, #51164 ),
 .UNSPECIFIED., .F., .F.,
 ( 4, 2, 1, 1, 1, 1, 2, 2, 2, 2, 2, 2, 2, 1, 1, 1, 1, 1, 1, 1, 2, 2, 2, 2, 2, 2, 2, 2, 2, 4 ),
 ( 0.5000151698130386180, 0.5005034362487721378, 0.5009917026845057686, 0.5019682355559731413, 0.5039213012989078866, 0.5078274327847773773, 0.5156396957565162475, 0.5312642216999940992, 0.5625132735869494693, 0.6250113773608605428, 0.6875094811347715051, 0.7500075849086826896, 0.7500686182131491853, 0.7501296515176159030, 0.7502517181265497825, 0.7504958513444184298, 0.7509841177801490630, 0.7519606506516048894, 0.7539137163944960029, 0.7578198478802943283, 0.7656321108518988616, 0.7812566367951041535, 0.8125056886815178459, 0.8437547405679315382, 0.8750037924543452306, 0.9062528443407589229, 0.9375018962271726153, 0.9687509481135863076, 0.9843754740567931538, 1.000000000000000000 ),
 .UNSPECIFIED. ) ;
#22344 = LINE ( 'NONE', #21900, #24355 ) ;
#22345 = EDGE_CURVE ( 'NONE', #34343, #82548, #47598, .T. ) ;
#22346 = FACE_OUTER_BOUND ( 'NONE', #84073, .T. ) ;
#22347 = VECTOR ( 'NONE', #76168, 1000.000000000000000 ) ;
#22348 = CARTESIAN_POINT ( 'NONE',  ( 107.0667039024470313, -104.2784471599418197, -11.78219314458200984 ) ) ;
#22349 = CARTESIAN_POINT ( 'NONE',  ( 97.53193330917046922, -39.74923349999438216, 37.57026538729112275 ) ) ;
#22350 = EDGE_CURVE ( 'NONE', #27695, #18119, #67996, .T. ) ;
#22351 = CARTESIAN_POINT ( 'NONE',  ( 118.0177608886754967, -35.41288285714057338, 238.9337205140059552 ) ) ;
#22352 = LINE ( 'NONE', #7814, #61949 ) ;
#22353 = ORIENTED_EDGE ( 'NONE', *, *, #6504, .T. ) ;
#22354 = ORIENTED_EDGE ( 'NONE', *, *, #64174, .T. ) ;
#22355 = CARTESIAN_POINT ( 'NONE',  ( 100.8874678657582677, -44.70022136077002983, 87.05229194071588950 ) ) ;
#22356 = CARTESIAN_POINT ( 'NONE',  ( -74.36911441044665594, 82.96450994655475597, -92.32962665258584423 ) ) ;
#22357 = DIRECTION ( 'NONE',  ( 0.000000000000000000, -0.9995520592605569021, -0.02992792722492374630 ) ) ;
#22358 = DIRECTION ( 'NONE',  ( 0.7071067811865496822, 7.071067811865498013E-16, -0.7071067811865453523 ) ) ;
#22359 = CARTESIAN_POINT ( 'NONE',  ( 115.1932381579439948, -43.17108053757041830, 44.30514908543392494 ) ) ;
#22360 = DIRECTION ( 'NONE',  ( 0.000000000000000000, 0.000000000000000000, 1.000000000000000000 ) ) ;
#22361 = ORIENTED_EDGE ( 'NONE', *, *, #55558, .T. ) ;
#22362 = CARTESIAN_POINT ( 'NONE',  ( 111.4336192290781753, -46.24370506310440732, 23.91848241876792969 ) ) ;
#22363 = CARTESIAN_POINT ( 'NONE',  ( 107.0667039024469886, -67.87844715994094713, 93.21780685541800437 ) ) ;
#22364 = CARTESIAN_POINT ( 'NONE',  ( 117.4915365000037042, -36.80222117025145678, 263.8213395616251660 ) ) ;
#22365 = ORIENTED_EDGE ( 'NONE', *, *, #7301, .F. ) ;
#22366 = CARTESIAN_POINT ( 'NONE',  ( 78.11989406980549688, -38.67261125150972134, 7.590611884311868174 ) ) ;
#22367 = CARTESIAN_POINT ( 'NONE',  ( -50.03799999999999670, 20.32000000000000028, 178.6098374884404905 ) ) ;
#22368 = CARTESIAN_POINT ( 'NONE',  ( 31.89136050872298966, -31.76306994223740432, -5.074374724088000832 ) ) ;
#22369 = CARTESIAN_POINT ( 'NONE',  ( 107.7548360709104855, -28.10233318731983232, 112.8433284648289430 ) ) ;
#22370 = CARTESIAN_POINT ( 'NONE',  ( 98.36161695517027681, -29.88032255785606139, 196.8080062282919869 ) ) ;
#22371 = CARTESIAN_POINT ( 'NONE',  ( 57.56670390244832447, -48.82844715994039575, 257.2178068554150627 ) ) ;
#22372 = EDGE_LOOP ( 'NONE', ( #32174, #2802, #30724, #72843 ) ) ;
#22373 = CARTESIAN_POINT ( 'NONE',  ( 172.5667039024482960, -42.82844715993499563, 180.4678068554150059 ) ) ;
#22374 = VERTEX_POINT ( 'NONE', #82164 ) ;
#22375 = ORIENTED_EDGE ( 'NONE', *, *, #30199, .T. ) ;
#22376 = VECTOR ( 'NONE', #48628, 1000.000000000000000 ) ;
#22377 = PLANE ( 'NONE',  #86551 ) ;
#22378 =( BOUNDED_CURVE ( )  B_SPLINE_CURVE ( 3, ( #37327, #65909, #78240, #3695 ),
 .UNSPECIFIED., .F., .F. ) 
 B_SPLINE_CURVE_WITH_KNOTS ( ( 4, 4 ),
 ( 4.712388980373003022, 6.283185307170268352 ),
 .UNSPECIFIED. ) 
 CURVE ( )  GEOMETRIC_REPRESENTATION_ITEM ( )  RATIONAL_B_SPLINE_CURVE ( ( 1.000000000000000000, 0.8047378541216103631, 0.8047378541216103631, 1.000000000000000000 ) ) 
 REPRESENTATION_ITEM ( '' )  );
#22379 = ORIENTED_EDGE ( 'NONE', *, *, #57788, .F. ) ;
#22380 = EDGE_LOOP ( 'NONE', ( #86932, #51662, #79682, #64089 ) ) ;
#22381 = CARTESIAN_POINT ( 'NONE',  ( 117.0612621577405008, -38.07784205248298548, 169.7193832652232004 ) ) ;
#22382 = AXIS2_PLACEMENT_3D ( 'NONE', #17798, #18242, #81396 ) ;
#22383 = ADVANCED_FACE ( 'NONE', ( #13112 ), #12207, .T. ) ;
#22384 = CARTESIAN_POINT ( 'NONE',  ( 113.5546853072178237, -29.03447022270776046, 40.51940965636622138 ) ) ;
#22385 = CARTESIAN_POINT ( 'NONE',  ( 103.7110576214454341, -44.58420688232069296, 91.67813411379100330 ) ) ;
#22386 = CARTESIAN_POINT ( 'NONE',  ( 106.1363778353814666, -47.76712558329867875, 262.4975300378158067 ) ) ;
#22387 = FACE_OUTER_BOUND ( 'NONE', #75838, .T. ) ;
#22388 = DIRECTION ( 'NONE',  ( 4.299999999999999979E-14, -1.000000000000000000, 4.400000000000000367E-29 ) ) ;
#22389 = ORIENTED_EDGE ( 'NONE', *, *, #26906, .F. ) ;
#22390 = ORIENTED_EDGE ( 'NONE', *, *, #61627, .T. ) ;
#22391 = CYLINDRICAL_SURFACE ( 'NONE', #23253, 0.9999999999999800160 ) ;
#22392 = CARTESIAN_POINT ( 'NONE',  ( 70.06670390244705970, -124.7784471599409812, 55.21780685541800437 ) ) ;
#22393 = CARTESIAN_POINT ( 'NONE',  ( 0.000000000000000000, 210.0000000000000000, 154.6557476874258441 ) ) ;
#22394 = CARTESIAN_POINT ( 'NONE',  ( 102.6513375509277495, -45.45698538002856282, 127.2041967044829960 ) ) ;
#22395 = CARTESIAN_POINT ( 'NONE',  ( 113.9459708190624241, -28.01821676562244789, 124.5565776568629559 ) ) ;
#22396 = CARTESIAN_POINT ( 'NONE',  ( 103.1875000000000000, 127.0000000000000000, 3.602774393244745134E-13 ) ) ;
#22397 = EDGE_LOOP ( 'NONE', ( #83148, #27537 ) ) ;
#22398 = EDGE_CURVE ( 'NONE', #61274, #50564, #68516, .T. ) ;
#22399 = PRODUCT_DEFINITION_CONTEXT ( 'detailed design', #89874, 'design' ) ;
#22400 = CARTESIAN_POINT ( 'NONE',  ( 99.39677155223240845, -28.76988628678374837, 265.6746728949588032 ) ) ;
#22401 = AXIS2_PLACEMENT_3D ( 'NONE', #85895, #44517, #31346 ) ;
#22402 = CARTESIAN_POINT ( 'NONE',  ( 106.5394234437989667, -24.24056378642895737, 322.0356252759110021 ) ) ;
#22403 =( LENGTH_UNIT ( ) NAMED_UNIT ( * ) SI_UNIT ( .MILLI., .METRE. ) );
#22405 = FACE_BOUND ( 'NONE', #22913, .T. ) ;
#22404 = VECTOR ( 'NONE', #40136, 1000.000000000000114 ) ;
#22406 = FACE_OUTER_BOUND ( 'NONE', #74525, .T. ) ;
#22408 = CARTESIAN_POINT ( 'NONE',  ( 49.21213752016101495, -29.73316016639650172, -5.074374724088000832 ) ) ;
#22407 = CARTESIAN_POINT ( 'NONE',  ( -446.0240000000000009, 3.174999999999999822, -1.387778780781445991E-14 ) ) ;
#22409 = CARTESIAN_POINT ( 'NONE',  ( 105.2934191044239043, -25.40803282519309647, 322.8191631070221774 ) ) ;
#22410 = DIRECTION ( 'NONE',  ( -1.000000000000000078E-15, 0.000000000000000000, -1.000000000000000000 ) ) ;
#22411 = DIRECTION ( 'NONE',  ( -0.8660254037844392627, 0.4999999999999990008, -1.549999999999999706E-14 ) ) ;
#22412 = CIRCLE ( 'NONE', #2121, 4.500000000000003553 ) ;
#22413 = AXIS2_PLACEMENT_3D ( 'NONE', #61508, #47874, #67889 ) ;
#22414 = FACE_OUTER_BOUND ( 'NONE', #18426, .T. ) ;
#22415 = FACE_BOUND ( 'NONE', #4798, .T. ) ;
#22416 = EDGE_CURVE ( 'NONE', #42450, #16685, #5626, .T. ) ;
#22417 = LINE ( 'NONE', #15149, #11506 ) ;
#22419 = ORIENTED_EDGE ( 'NONE', *, *, #1327, .T. ) ;
#22418 = DIRECTION ( 'NONE',  ( 0.000000000000000000, 0.000000000000000000, -1.000000000000000000 ) ) ;
#22420 = EDGE_CURVE ( 'NONE', #50747, #13441, #54850, .T. ) ;
#22421 = CARTESIAN_POINT ( 'NONE',  ( 41.56670390244689628, -36.32844715994109208, 180.4678068554150911 ) ) ;
#22422 = CARTESIAN_POINT ( 'NONE',  ( 117.5135424720979103, -36.80237478700602338, 263.8213395616250523 ) ) ;
#22423 = CARTESIAN_POINT ( 'NONE',  ( 113.7506423937859807, -44.72972868871420360, 189.1299109901969757 ) ) ;
#22424 = CARTESIAN_POINT ( 'NONE',  ( 99.04917799727566319, -44.37196124675453746, 32.92038718067297509 ) ) ;
#22426 = CARTESIAN_POINT ( 'NONE',  ( 194.0371591254574923, -24.42818131005417115, 193.9678068554150343 ) ) ;
#22425 = PLANE ( 'NONE',  #78357 ) ;
#22427 = DIRECTION ( 'NONE',  ( 0.2884130866282256789, -0.7071067811865450192, -0.6456143519637580486 ) ) ;
#22428 = EDGE_CURVE ( 'NONE', #61259, #17509, #27619, .T. ) ;
#22429 = ORIENTED_EDGE ( 'NONE', *, *, #23977, .F. ) ;
#22430 = PLANE ( 'NONE',  #9874 ) ;
#22431 = ORIENTED_EDGE ( 'NONE', *, *, #39714, .F. ) ;
#22432 = CARTESIAN_POINT ( 'NONE',  ( 97.92582740012257148, -33.45545302834237589, 175.4752769709339759 ) ) ;
#22434 = EDGE_LOOP ( 'NONE', ( #29998, #80337, #51838, #5313 ) ) ;
#22433 = CARTESIAN_POINT ( 'NONE',  ( 115.7803070267097354, -41.80703622889448923, 188.4066082405644522 ) ) ;
#22435 = DIRECTION ( 'NONE',  ( 0.000000000000000000, 0.000000000000000000, -1.000000000000000000 ) ) ;
#22436 = CARTESIAN_POINT ( 'NONE',  ( 116.8369567342159456, -40.30247308064090817, 214.5470538473389581 ) ) ;
#22437 = DIRECTION ( 'NONE',  ( 1.000000000000000000, 4.299999999999999979E-14, 1.000000000000000078E-15 ) ) ;
#22438 = CARTESIAN_POINT ( 'NONE',  ( 154.5667039024469886, -67.87844715994090450, 120.2178068554179902 ) ) ;
#22439 = ADVANCED_FACE ( 'NONE', ( #34877 ), #363, .F. ) ;
#22440 = DIRECTION ( 'NONE',  ( 3.100000000000000258E-29, -3.100000000000000044E-14, -1.000000000000000000 ) ) ;
#22441 = CARTESIAN_POINT ( 'NONE',  ( 31.56670390244700641, -22.48495420874110806, -5.074374724088000832 ) ) ;
#22442 = LINE ( 'NONE', #60053, #77638 ) ;
#22443 = CARTESIAN_POINT ( 'NONE',  ( 98.82386243697609984, -31.40279086140550291, 145.8699109901969848 ) ) ;
#22444 = ORIENTED_EDGE ( 'NONE', *, *, #59416, .F. ) ;
#22445 = ORIENTED_EDGE ( 'NONE', *, *, #89360, .F. ) ;
#22446 = AXIS2_PLACEMENT_3D ( 'NONE', #16831, #36384, #64088 ) ;
#22447 = CARTESIAN_POINT ( 'NONE',  ( 99.90998525089342763, -42.81722683197487811, 73.33110711542096283 ) ) ;
#22448 = CARTESIAN_POINT ( 'NONE',  ( 127.4058501689330996, -85.76982405743852667, 250.2178068554179902 ) ) ;
#22450 = CARTESIAN_POINT ( 'NONE',  ( 77.06670390244796920, -50.82844715994100682, 310.9178068554150514 ) ) ;
#22449 = CARTESIAN_POINT ( 'NONE',  ( 116.5663773505004315, -40.88766770462209621, 204.4861014663869696 ) ) ;
#22451 = AXIS2_PLACEMENT_3D ( 'NONE', #6750, #7650, #54869 ) ;
#22452 = DIRECTION ( 'NONE',  ( -1.000000000000000078E-15, 1.000000000000000000, 0.000000000000000000 ) ) ;
#22453 = CARTESIAN_POINT ( 'NONE',  ( 115.0439452383991892, -99.09543445804983719, -19.78219314458218392 ) ) ;
#22454 = CARTESIAN_POINT ( 'NONE',  ( 90.44969454456408187, -53.34645651782490461, 239.5838068554174356 ) ) ;
#22455 = EDGE_CURVE ( 'NONE', #36232, #66586, #64388, .T. ) ;
#22456 = LINE ( 'NONE', #7919, #10045 ) ;
#22457 = CARTESIAN_POINT ( 'NONE',  ( 67.07017578645290712, -67.88084389459083923, 245.6085276058775264 ) ) ;
#22458 = EDGE_CURVE ( 'NONE', #46976, #12137, #84844, .T. ) ;
#22459 = CARTESIAN_POINT ( 'NONE',  ( 114.7552509866192452, -44.63809267644818135, 118.2022919425779719 ) ) ;
#22460 = VERTEX_POINT ( 'NONE', #9418 ) ;
#22461 = ORIENTED_EDGE ( 'NONE', *, *, #83654, .T. ) ;
#22462 = ORIENTED_EDGE ( 'NONE', *, *, #2020, .T. ) ;
#22463 = EDGE_CURVE ( 'NONE', #16335, #85940, #28504, .T. ) ;
#22464 = CARTESIAN_POINT ( 'NONE',  ( 6.812220284937059779E-16, 60.82030000000000314, 271.1195999999999913 ) ) ;
#22465 = LINE ( 'NONE', #217, #62124 ) ;
#22466 = EDGE_CURVE ( 'NONE', #85489, #57830, #81046, .T. ) ;
#22467 = CARTESIAN_POINT ( 'NONE',  ( 108.3334480829778812, -46.73485935560395177, 78.67729194162538420 ) ) ;
#22468 = DIRECTION ( 'NONE',  ( -3.100000000000000258E-29, 3.100000000000000044E-14, 1.000000000000000000 ) ) ;
#22469 = CARTESIAN_POINT ( 'NONE',  ( 107.2048247310825388, -44.91868093929326022, 210.4080903695909512 ) ) ;
#22470 = VECTOR ( 'NONE', #73123, 1000.000000000000000 ) ;
#22471 = CYLINDRICAL_SURFACE ( 'NONE', #29110, 0.2500000000000046074 ) ;
#22472 = B_SPLINE_CURVE_WITH_KNOTS ( 'NONE', 3,
 ( #19828, #49308, #8446, #30228, #71575, #43388, #77939, #15261, #22982, #72013, #85655, #35687, #15711, #21637, #64307, #22525, #22089, #71129 ),
 .UNSPECIFIED., .F., .F.,
 ( 4, 2, 2, 2, 2, 2, 2, 2, 4 ),
 ( 0.4999999994038420992, 0.5624999994783618229, 0.6249999995528815466, 0.6874999996274013814, 0.7499999997019211051, 0.8124999997764408288, 0.8749999998509605525, 0.9374999999254802763, 1.000000000000000000 ),
 .UNSPECIFIED. ) ;
#22473 = CARTESIAN_POINT ( 'NONE',  ( 102.6975360555999259, -46.88284006984166297, 137.2651490854349561 ) ) ;
#22474 = CARTESIAN_POINT ( 'NONE',  ( 41.56648329127399677, -9.303447159940999356, 18.92562527591200094 ) ) ;
#22475 = ORIENTED_EDGE ( 'NONE', *, *, #6085, .T. ) ;
#22477 = VERTEX_POINT ( 'NONE', #78029 ) ;
#22476 = ORIENTED_EDGE ( 'NONE', *, *, #10807, .F. ) ;
#22478 = CONICAL_SURFACE ( 'NONE', #73217, 1.624999999999987566, 1.029744258676650093 ) ;
#22479 = AXIS2_PLACEMENT_3D ( 'NONE', #22784, #37745, #72712 ) ;
#22480 = FACE_OUTER_BOUND ( 'NONE', #45825, .T. ) ;
#22481 = ORIENTED_EDGE ( 'NONE', *, *, #66840, .T. ) ;
#22482 = ORIENTED_EDGE ( 'NONE', *, *, #6625, .F. ) ;
#22483 = CARTESIAN_POINT ( 'NONE',  ( -50.03799999999999670, 0.000000000000000000, 206.3750000000000000 ) ) ;
#22484 = CARTESIAN_POINT ( 'NONE',  ( 0.000000000000000000, 100.5999999999999659, 0.000000000000000000 ) ) ;
#22485 = CARTESIAN_POINT ( 'NONE',  ( 98.65401097786960349, -39.51487139837627893, 238.0130118773259653 ) ) ;
#22486 = CYLINDRICAL_SURFACE ( 'NONE', #8665, 3.000000000000002665 ) ;
#22487 = VERTEX_POINT ( 'NONE', #36688 ) ;
#22488 = CARTESIAN_POINT ( 'NONE',  ( 116.6298083638390324, -39.11748333416112899, 9.635625275910943088 ) ) ;
#22489 = PLANE ( 'NONE',  #83666 ) ;
#22490 = ORIENTED_EDGE ( 'NONE', *, *, #75488, .T. ) ;
#22491 = ORIENTED_EDGE ( 'NONE', *, *, #68381, .T. ) ;
#22492 = CARTESIAN_POINT ( 'NONE',  ( 110.8546043978908244, -45.98418316275319029, 112.8856366702089247 ) ) ;
#22493 = ORIENTED_EDGE ( 'NONE', *, *, #16299, .T. ) ;
#22494 = ORIENTED_EDGE ( 'NONE', *, *, #48420, .F. ) ;
#22495 = VECTOR ( 'NONE', #84308, 1000.000000000000000 ) ;
#22496 = CARTESIAN_POINT ( 'NONE',  ( 101.6725443455464131, -43.49748584897681525, 269.8471379886391901 ) ) ;
#22497 = CARTESIAN_POINT ( 'NONE',  ( 98.64801509901850807, -30.48302769619336416, 180.8184824187679567 ) ) ;
#22498 = CARTESIAN_POINT ( 'NONE',  ( 97.81366378802354689, -42.73395665195503312, 146.7965776568629508 ) ) ;
#22499 = DIRECTION ( 'NONE',  ( -1.000000000000000000, -3.999999999999999995E-14, -1.000000000000000078E-15 ) ) ;
#22500 = CARTESIAN_POINT ( 'NONE',  ( 99.75313521292756036, -29.29995004827394212, 221.6956252759109702 ) ) ;
#22501 = CARTESIAN_POINT ( 'NONE',  ( 179.4595971212720258, -26.00627455219131789, 117.4678068554150627 ) ) ;
#22502 = DIRECTION ( 'NONE',  ( -0.9825752044165969590, -0.1858654558159821002, 0.000000000000000000 ) ) ;
#22503 = EDGE_LOOP ( 'NONE', ( #39508, #19455, #49964, #5022, #36418 ) ) ;
#22504 = CARTESIAN_POINT ( 'NONE',  ( 19.56670390244739721, -25.42844715994192129, 249.9678068554150059 ) ) ;
#22505 = ORIENTED_EDGE ( 'NONE', *, *, #69003, .T. ) ;
#22506 = VERTEX_POINT ( 'NONE', #22614 ) ;
#22507 = AXIS2_PLACEMENT_3D ( 'NONE', #21830, #77235, #14567 ) ;
#22508 = CARTESIAN_POINT ( 'NONE',  ( 116.4168962126584717, -41.43863437684461104, 203.4556252759109611 ) ) ;
#22509 = ORIENTED_EDGE ( 'NONE', *, *, #47771, .T. ) ;
#22510 = EDGE_CURVE ( 'NONE', #76954, #16276, #49839, .T. ) ;
#22511 = CARTESIAN_POINT ( 'NONE',  ( 117.7037197400453437, -39.73414628438690244, 143.6194347997209775 ) ) ;
#22512 = DIRECTION ( 'NONE',  ( 1.000000000000000000, 1.000000000000000078E-15, 0.000000000000000000 ) ) ;
#22513 = CIRCLE ( 'NONE', #44202, 5.041900000000001825 ) ;
#22514 = CARTESIAN_POINT ( 'NONE',  ( 165.3359832912750278, -36.32844715993530826, 117.4678068554150485 ) ) ;
#22515 = CARTESIAN_POINT ( 'NONE',  ( 123.6837132603318992, -23.41243780205710578, 239.5838068554165545 ) ) ;
#22516 = EDGE_CURVE ( 'NONE', #55318, #2603, #20145, .T. ) ;
#22519 = CARTESIAN_POINT ( 'NONE',  ( 112.4780167374715631, -46.34085331822165443, 253.9965776568634510 ) ) ;
#22518 = CARTESIAN_POINT ( 'NONE',  ( 100.3900607503748574, -44.18760341221117471, 56.99518173324602799 ) ) ;
#22517 = DIRECTION ( 'NONE',  ( 0.000000000000000000, -1.000000000000000000, 0.000000000000000000 ) ) ;
#22520 = CARTESIAN_POINT ( 'NONE',  ( 1.102182119232618897E-15, 211.0000000000000000, 163.6557476874258441 ) ) ;
#22521 = DIRECTION ( 'NONE',  ( 0.000000000000000000, 0.000000000000000000, -1.000000000000000000 ) ) ;
#22522 = DIRECTION ( 'NONE',  ( 0.000000000000000000, 1.000000000000000000, 0.000000000000000000 ) ) ;
#22523 = ADVANCED_FACE ( 'NONE', ( #42131 ), #8989, .F. ) ;
#22524 = CARTESIAN_POINT ( 'NONE',  ( 151.5667039024485518, -48.82844715993590512, 180.4678068554149775 ) ) ;
#22525 = CARTESIAN_POINT ( 'NONE',  ( 115.0889047221861290, -30.61763667734028971, 255.3439586094922618 ) ) ;
#22526 = EDGE_CURVE ( 'NONE', #68501, #61899, #14455, .T. ) ;
#22527 = CYLINDRICAL_SURFACE ( 'NONE', #27450, 4.762500000000000178 ) ;
#22529 = ORIENTED_EDGE ( 'NONE', *, *, #67648, .F. ) ;
#22528 = DIRECTION ( 'NONE',  ( 0.000000000000000000, 0.000000000000000000, -1.000000000000000000 ) ) ;
#22530 = ADVANCED_FACE ( 'NONE', ( #29874 ), #65078, .T. ) ;
#22531 = LINE ( 'NONE', #83407, #39355 ) ;
#22532 = CARTESIAN_POINT ( 'NONE',  ( 95.54500964991285628, -39.60862429916534211, 166.5213395616259788 ) ) ;
#22533 = CARTESIAN_POINT ( 'NONE',  ( 117.3534687869931048, -38.62661931536851512, 84.68133956162593279 ) ) ;
#22534 = CARTESIAN_POINT ( 'NONE',  ( 113.7132347973738575, -45.61866494189415988, 184.0994347997199725 ) ) ;
#22535 = DIRECTION ( 'NONE',  ( 0.000000000000000000, 0.000000000000000000, -1.000000000000000000 ) ) ;
#22536 = DIRECTION ( 'NONE',  ( -0.000000000000000000, 0.000000000000000000, -1.000000000000000000 ) ) ;
#22538 = CARTESIAN_POINT ( 'NONE',  ( -3.175000000000109956, 8.255000000000000782, -31.75000000000000000 ) ) ;
#22537 = LINE ( 'NONE', #37048, #76780 ) ;
#22539 = DIRECTION ( 'NONE',  ( -1.000000000000000000, 1.774213772886706994E-13, 0.000000000000000000 ) ) ;
#22540 = CARTESIAN_POINT ( 'NONE',  ( 144.0646911277377740, -140.6784471599409017, 245.5179332673170052 ) ) ;
#22541 = ORIENTED_EDGE ( 'NONE', *, *, #68053, .T. ) ;
#22542 = EDGE_CURVE ( 'NONE', #48576, #50846, #7629, .T. ) ;
#22543 = CARTESIAN_POINT ( 'NONE',  ( -74.15067561874319324, 120.6499999999999915, 68.53801554307369770 ) ) ;
#22544 = AXIS2_PLACEMENT_3D ( 'NONE', #30694, #23892, #71049 ) ;
#22545 = VECTOR ( 'NONE', #39506, 1000.000000000000000 ) ;
#22546 = CIRCLE ( 'NONE', #13764, 8.999999999999994671 ) ;
#22547 = AXIS2_PLACEMENT_3D ( 'NONE', #58219, #85948, #60894 ) ;
#22548 = EDGE_CURVE ( 'NONE', #28811, #40401, #39889, .T. ) ;
#22549 = VERTEX_POINT ( 'NONE', #72097 ) ;
#22550 = VERTEX_POINT ( 'NONE', #58446 ) ;
#22551 = AXIS2_PLACEMENT_3D ( 'NONE', #13924, #41603, #291 ) ;
#22553 = VERTEX_POINT ( 'NONE', #45257 ) ;
#22552 = DIRECTION ( 'NONE',  ( 1.000000000000000078E-15, 0.000000000000000000, 1.000000000000000000 ) ) ;
#22554 = CARTESIAN_POINT ( 'NONE',  ( 95.37363933861288956, -34.96150835630653120, 67.20705384733894050 ) ) ;
#22555 = FACE_OUTER_BOUND ( 'NONE', #42315, .T. ) ;
#22556 = EDGE_CURVE ( 'NONE', #14017, #50559, #46141, .T. ) ;
#22557 = AXIS2_PLACEMENT_3D ( 'NONE', #83102, #83536, #20855 ) ;
#22558 = FACE_OUTER_BOUND ( 'NONE', #61135, .T. ) ;
#22559 = CARTESIAN_POINT ( 'NONE',  ( 101.7473938980672870, -45.74611303501656323, 158.1527681330539963 ) ) ;
#22561 = CARTESIAN_POINT ( 'NONE',  ( 98.74870792914448714, -34.66384430100242753, 275.5552769709340737 ) ) ;
#22560 = AXIS2_PLACEMENT_3D ( 'NONE', #64550, #30913, #37740 ) ;
#22562 = ORIENTED_EDGE ( 'NONE', *, *, #17207, .F. ) ;
#22563 = ORIENTED_EDGE ( 'NONE', *, *, #57579, .F. ) ;
#22564 = ORIENTED_EDGE ( 'NONE', *, *, #22428, .F. ) ;
#22565 = DIRECTION ( 'NONE',  ( 1.821299053822143307E-16, 0.000000000000000000, -1.000000000000000000 ) ) ;
#22566 = CARTESIAN_POINT ( 'NONE',  ( 120.0664832912739399, -36.72944715994095333, 293.6356252759106837 ) ) ;
#22567 = DIRECTION ( 'NONE',  ( 4.299999999999999979E-14, -1.000000000000000000, 4.400000000000000367E-29 ) ) ;
#22568 = DIRECTION ( 'NONE',  ( -3.100000000000000258E-29, 3.100000000000000044E-14, 1.000000000000000000 ) ) ;
#22569 = AXIS2_PLACEMENT_3D ( 'NONE', #6986, #69214, #41046 ) ;
#22570 = CARTESIAN_POINT ( 'NONE',  ( 95.16508291382824325, 94.58014758961630264, 89.37916159652695569 ) ) ;
#22571 = CARTESIAN_POINT ( 'NONE',  ( 2.684158038187649039E-15, 69.84999999999999432, -130.5560000000000116 ) ) ;
#22572 = PLANE ( 'NONE',  #55820 ) ;
#22573 = CARTESIAN_POINT ( 'NONE',  ( 156.5667039024480971, -42.82844715993568485, 293.2178068554149490 ) ) ;
#22574 = CARTESIAN_POINT ( 'NONE',  ( 118.0600790064084293, -37.62648441163795354, 38.77372051400595865 ) ) ;
#22575 = ORIENTED_EDGE ( 'NONE', *, *, #59881, .F. ) ;
#22576 = EDGE_CURVE ( 'NONE', #24886, #5965, #10612, .T. ) ;
#22577 = LINE ( 'NONE', #84366, #63701 ) ;
#22578 = ADVANCED_FACE ( 'NONE', ( #65278 ), #4837, .F. ) ;
#22579 = CARTESIAN_POINT ( 'NONE',  ( -54.73705905482161427, 54.20698630476788082, 70.79887152307878750 ) ) ;
#22580 = CARTESIAN_POINT ( 'NONE',  ( 98.90423600646026614, -36.64316113183544843, 109.1366617981629474 ) ) ;
#22581 = AXIS2_PLACEMENT_3D ( 'NONE', #75127, #20617, #82411 ) ;
#22582 = B_SPLINE_CURVE_WITH_KNOTS ( 'NONE', 3,
 ( #52924, #11648, #72965, #67048, #60212, #23509, #78914, #44360, #72089, #47927, #62019, #13881, #12091, #27065, #81154, #53386, #60666, #75667, #33869, #75215, #13437, #68847, #20257, #12996, #69299, #40227, #39775, #54284, #7070, #81605, #68402, #18900, #89753, #20700, #53835, #12540, #61125, #27503, #54735, #47482, #82048, #25712, #46584, #74762, #41564, #6618, #34767, #55180, #82940, #19801, #87947, #48368, #88854, #40682, #82498, #32971, #88405, #41123, #76102, #74322, #34314, #67488, #5275, #26167, #6181, #19355, #47027, #26608, #61565, #67945, #89301, #5733, #33424, #35659, #62915, #77455, #84740, #70189, #27950, #22062, #86396, #28396 ),
 .UNSPECIFIED., .F., .F.,
 ( 4, 2, 2, 2, 2, 2, 2, 2, 2, 2, 2, 2, 2, 2, 2, 2, 2, 2, 2, 2, 2, 2, 2, 2, 2, 2, 2, 2, 2, 2, 2, 2, 2, 2, 2, 2, 2, 2, 2, 2, 4 ),
 ( 6.083641046005872842E-05, 0.0002295799514885608656, 0.0003983234925170630095, 0.0007358105745741082802, 0.001410784738688156213, 0.002760733066916254246, 0.004110681395144351845, 0.005460629723372451179, 0.006810578051600549646, 0.008160526379828647245, 0.009510474708056746579, 0.01086042303628484418, 0.01356031969274100642, 0.01626021634919716866, 0.01693519051331119837, 0.01761016467742522809, 0.01896011300565331181, 0.01963508716976735541, 0.02031006133388139553, 0.02166000966210947579, 0.02300995799033755604, 0.02435990631856564323, 0.02570985464679372695, 0.02705980297502181414, 0.02840975130324989439, 0.02975969963147798159, 0.03043467379559202171, 0.03110964795970606531, 0.03245959628793418372, 0.03380954461616231255, 0.03515949294439044137, 0.03650944127261857020, 0.03785938960084669902, 0.03920933792907482784, 0.04055928625730294973, 0.04190923458553107855, 0.04258420874964514297, 0.04292169583170216129, 0.04309043937273064617, 0.04317481114324489555, 0.04325918291375914493 ),
 .UNSPECIFIED. ) ;
#22583 = LINE ( 'NONE', #1689, #68819 ) ;
#22584 = CARTESIAN_POINT ( 'NONE',  ( 83.06670390244801183, -42.97311385574013798, 231.5838068554169524 ) ) ;
#22585 = ORIENTED_EDGE ( 'NONE', *, *, #67509, .T. ) ;
#22586 = VERTEX_POINT ( 'NONE', #32082 ) ;
#22587 = CARTESIAN_POINT ( 'NONE',  ( 97.81469011401388514, -40.51612824417846070, 136.6360017533206417 ) ) ;
#22588 = VERTEX_POINT ( 'NONE', #39352 ) ;
#22589 = VERTEX_POINT ( 'NONE', #72975 ) ;
#22590 = CARTESIAN_POINT ( 'NONE',  ( 99.59846494627726088, -31.90336481815605296, 142.3015833058969974 ) ) ;
#22591 = DIRECTION ( 'NONE',  ( 1.000000000000000078E-15, -1.000000000000000083E-30, -1.000000000000000000 ) ) ;
#22592 = CARTESIAN_POINT ( 'NONE',  ( 98.13097783494514204, -43.27482323654912477, 102.8175300378159847 ) ) ;
#22593 = CARTESIAN_POINT ( 'NONE',  ( 111.4877917169584975, -45.70509539860793780, 17.94068519067145928 ) ) ;
#22594 = AXIS2_PLACEMENT_3D ( 'NONE', #74043, #19078, #79991 ) ;
#22595 = VERTEX_POINT ( 'NONE', #73420 ) ;
#22596 = AXIS2_PLACEMENT_3D ( 'NONE', #28803, #23350, #85127 ) ;
#22597 = VECTOR ( 'NONE', #72820, 1000.000000000000000 ) ;
#22598 = VECTOR ( 'NONE', #30856, 1000.000000000000114 ) ;
#22599 = ORIENTED_EDGE ( 'NONE', *, *, #44306, .T. ) ;
#22600 = ORIENTED_EDGE ( 'NONE', *, *, #49776, .F. ) ;
#22601 = TOROIDAL_SURFACE ( 'NONE', #61731, 13.09746158385919124, 3.000000000000000000 ) ;
#22602 = CARTESIAN_POINT ( 'NONE',  ( 117.0750736332619937, -31.98354782443029620, 64.19086337114899266 ) ) ;
#22603 = ORIENTED_EDGE ( 'NONE', *, *, #54882, .F. ) ;
#22604 = CARTESIAN_POINT ( 'NONE',  ( 115.7453557663426409, -41.23947501269460503, 288.4441967044829767 ) ) ;
#22605 = CARTESIAN_POINT ( 'NONE',  ( 101.9739164908862961, -45.89159533563675808, 183.1727681330539781 ) ) ;
#22606 = CARTESIAN_POINT ( 'NONE',  ( 165.6738106836042732, -28.98061976758451053, 313.9678068554149490 ) ) ;
#22607 = LINE ( 'NONE', #83943, #50317 ) ;
#22608 = CARTESIAN_POINT ( 'NONE',  ( 113.9169062821921727, -28.05502007051373070, 120.5565776568639507 ) ) ;
#22609 = DIRECTION ( 'NONE',  ( -0.000000000000000000, 1.000000000000000000, 0.000000000000000000 ) ) ;
#22610 = VERTEX_POINT ( 'NONE', #67057 ) ;
#22611 = AXIS2_PLACEMENT_3D ( 'NONE', #3829, #22959, #37907 ) ;
#22612 = CARTESIAN_POINT ( 'NONE',  ( -215.9000000000000057, 101.5999999999999943, -45.33899999999999864 ) ) ;
#22613 = EDGE_LOOP ( 'NONE', ( #48117, #53434, #46357, #89816 ) ) ;
#22614 = CARTESIAN_POINT ( 'NONE',  ( 56.06670390244699576, -67.87844715994098976, 155.2178068554179902 ) ) ;
#22615 = VERTEX_POINT ( 'NONE', #32520 ) ;
#22617 = VERTEX_POINT ( 'NONE', #66151 ) ;
#22616 = ADVANCED_FACE ( 'NONE', ( #3490 ), #52934, .T. ) ;
#22618 = DIRECTION ( 'NONE',  ( 1.000000000000000000, 2.999999999999999839E-15, 1.000000000000000078E-15 ) ) ;
#22619 = CARTESIAN_POINT ( 'NONE',  ( 9.487327754115383982, 90.88213376798057652, 118.1772177615633126 ) ) ;
#22620 = CARTESIAN_POINT ( 'NONE',  ( 101.3840881871039272, -27.98888560156178329, 25.53562527591096654 ) ) ;
#22621 = LINE ( 'NONE', #70769, #11239 ) ;
#22622 = CIRCLE ( 'NONE', #89347, 10.41399999999997839 ) ;
#22623 = ADVANCED_FACE ( 'NONE', ( #9870 ), #38895, .F. ) ;
#22624 = FACE_OUTER_BOUND ( 'NONE', #80029, .T. ) ;
#22625 = CARTESIAN_POINT ( 'NONE',  ( 3.175000000000355094, 24.56180297284579694, 33.98325472291460159 ) ) ;
#22626 = EDGE_CURVE ( 'NONE', #5764, #19968, #30758, .T. ) ;
#22627 = CARTESIAN_POINT ( 'NONE',  ( 97.00151786184777336, -41.45262973156714992, 61.67562527591097421 ) ) ;
#22629 = CARTESIAN_POINT ( 'NONE',  ( 117.6812658759004222, -39.72780374360937827, 139.6194347997199827 ) ) ;
#22628 = CARTESIAN_POINT ( 'NONE',  ( 149.4430470701762772, -12.91565541735124256, 394.9756252759100903 ) ) ;
#22630 = CARTESIAN_POINT ( 'NONE',  ( 38.10000000000000142, 82.54999999999999716, 302.8950000000000387 ) ) ;
#22631 = CARTESIAN_POINT ( 'NONE',  ( 188.5667039024479834, -65.37844715994100397, 137.2178068554150059 ) ) ;
#22632 = ORIENTED_EDGE ( 'NONE', *, *, #19246, .F. ) ;
#22633 = CARTESIAN_POINT ( 'NONE',  ( 107.0664832912739257, -49.72944715994096043, 315.6356252759111953 ) ) ;
#22634 = EDGE_CURVE ( 'NONE', #77176, #36098, #25269, .T. ) ;
#22635 = LINE ( 'NONE', #3399, #2951 ) ;
#22636 = CARTESIAN_POINT ( 'NONE',  ( 106.5667039024470455, -113.7784471599413791, 2.217806855418308132 ) ) ;
#22637 = ORIENTED_EDGE ( 'NONE', *, *, #9911, .T. ) ;
#22638 = EDGE_CURVE ( 'NONE', #86558, #75555, #52060, .T. ) ;
#22639 = FACE_OUTER_BOUND ( 'NONE', #39621, .T. ) ;
#22641 = EDGE_LOOP ( 'NONE', ( #28046, #22232, #27832, #63941 ) ) ;
#22640 = CARTESIAN_POINT ( 'NONE',  ( 107.9218747862861250, -47.19940893231376577, 177.6413395616249886 ) ) ;
#22643 = DIRECTION ( 'NONE',  ( 0.7071067811865160424, 0.7071067811865791031, 0.000000000000000000 ) ) ;
#22642 = PRODUCT_DEFINITION_CONTEXT ( 'detailed design', #32907, 'design' ) ;
#22644 = CARTESIAN_POINT ( 'NONE',  ( 100.6242249862060731, -26.75349815150567778, 216.5327681330539633 ) ) ;
#22645 = CARTESIAN_POINT ( 'NONE',  ( 98.29982688861167617, -42.45122269429050021, 97.78705384733993355 ) ) ;
#22646 = LINE ( 'NONE', #71684, #31642 ) ;
#22647 = LINE ( 'NONE', #23545, #73579 ) ;
#22648 = CYLINDRICAL_SURFACE ( 'NONE', #43799, 9.425000000000000711 ) ;
#22649 = EDGE_LOOP ( 'NONE', ( #66351, #38772, #74744, #62524 ) ) ;
#22650 = ADVANCED_FACE ( 'NONE', ( #17133, #80704 ), #78922, .F. ) ;
#22651 = CIRCLE ( 'NONE', #44331, 13.16666666666670160 ) ;
#22652 = ORIENTED_EDGE ( 'NONE', *, *, #34285, .F. ) ;
#22653 = EDGE_CURVE ( 'NONE', #87303, #24776, #18453, .T. ) ;
#22654 = ORIENTED_EDGE ( 'NONE', *, *, #57070, .F. ) ;
#22655 = EDGE_LOOP ( 'NONE', ( #84941, #77389, #46020, #34007, #85246, #66623 ) ) ;
#22656 = FACE_OUTER_BOUND ( 'NONE', #85121, .T. ) ;
#22657 = CARTESIAN_POINT ( 'NONE',  ( 115.4598468997141509, -29.53740796227222987, 225.4022919425769658 ) ) ;
#22658 = LINE ( 'NONE', #50331, #6947 ) ;
#22659 = DIRECTION ( 'NONE',  ( 0.9659258262890679791, 0.000000000000000000, -0.2588190451025220162 ) ) ;
#22660 = ADVANCED_FACE ( 'NONE', ( #38018 ), #87509, .T. ) ;
#22662 = CARTESIAN_POINT ( 'NONE',  ( 107.8173249548519692, -46.71069529603006032, 277.6356222035115024 ) ) ;
#22661 = CARTESIAN_POINT ( 'NONE',  ( 46.83715912545429205, -47.82818131006082751, 249.9678068554150343 ) ) ;
#22663 = VECTOR ( 'NONE', #31490, 1000.000000000000000 ) ;
#22664 = CARTESIAN_POINT ( 'NONE',  ( -103.1875000000000000, 120.6499999999999915, -7.937500000001089795 ) ) ;
#22665 = CARTESIAN_POINT ( 'NONE',  ( 99.12668881670464316, -43.51958910750428089, 31.88991099019594699 ) ) ;
#22666 = EDGE_LOOP ( 'NONE', ( #82162, #41997, #82084, #58423 ) ) ;
#22667 = VERTEX_POINT ( 'NONE', #86623 ) ;
#22668 = AXIS2_PLACEMENT_3D ( 'NONE', #63335, #1112, #7478 ) ;
#22669 = ORIENTED_EDGE ( 'NONE', *, *, #56134, .T. ) ;
#22670 = VECTOR ( 'NONE', #38628, 1000.000000000000000 ) ;
#22671 = CARTESIAN_POINT ( 'NONE',  ( 41.56648329127499153, -32.07844715994070839, 143.6756252759119832 ) ) ;
#22672 = VECTOR ( 'NONE', #8264, 1000.000000000000000 ) ;
#22673 = FACE_OUTER_BOUND ( 'NONE', #33573, .T. ) ;
#22674 = CARTESIAN_POINT ( 'NONE',  ( 106.8506556707825013, -46.50783423188139665, 268.5584824187674258 ) ) ;
#22675 = CARTESIAN_POINT ( 'NONE',  ( -103.1875000000000000, 117.4749999999999943, -1.080832317973422076E-12 ) ) ;
#22676 = CARTESIAN_POINT ( 'NONE',  ( 98.98846131648984681, -42.30253745798191289, 122.8070538473389490 ) ) ;
#22677 = DIRECTION ( 'NONE',  ( 0.000000000000000000, 1.000000000000000000, 0.000000000000000000 ) ) ;
#22678 = EDGE_LOOP ( 'NONE', ( #6471, #29423, #70987 ) ) ;
#22679 = CARTESIAN_POINT ( 'NONE',  ( 78.57724105935530190, 120.6499999999999915, -67.35192090801849929 ) ) ;
#22680 = CARTESIAN_POINT ( 'NONE',  ( 77.33253968407632328, -36.38436945697863933, 3.076560175368444838 ) ) ;
#22681 = ORIENTED_EDGE ( 'NONE', *, *, #65167, .F. ) ;
#22682 = ORIENTED_EDGE ( 'NONE', *, *, #11663, .F. ) ;
#22683 = EDGE_CURVE ( 'NONE', #44005, #75042, #79819, .T. ) ;
#22684 = AXIS2_PLACEMENT_3D ( 'NONE', #36110, #63825, #1601 ) ;
#22685 = CARTESIAN_POINT ( 'NONE',  ( -81.76533775135438020, 94.92435932957494060, 85.84941893669298452 ) ) ;
#22686 = CARTESIAN_POINT ( 'NONE',  ( 99.05427501747529107, -38.42862543901446060, 29.31094751244794949 ) ) ;
#22687 = DIRECTION ( 'NONE',  ( 1.000000000000000078E-15, 1.000000000000000083E-30, -1.000000000000000000 ) ) ;
#22688 = VECTOR ( 'NONE', #26548, 1000.000000000000000 ) ;
#22689 = FACE_OUTER_BOUND ( 'NONE', #5396, .T. ) ;
#22690 = CARTESIAN_POINT ( 'NONE',  ( 142.8821648370248170, -72.54478064608022692, 394.9756252759102040 ) ) ;
#22691 = ORIENTED_EDGE ( 'NONE', *, *, #7351, .T. ) ;
#22692 = CARTESIAN_POINT ( 'NONE',  ( 90.44969454456406766, -22.62993780205715311, 229.5838068554169809 ) ) ;
#22693 = FACE_OUTER_BOUND ( 'NONE', #25412, .T. ) ;
#22694 = ORIENTED_EDGE ( 'NONE', *, *, #41800, .T. ) ;
#22695 = CARTESIAN_POINT ( 'NONE',  ( 110.1579966911880888, -46.68583080861444756, 97.81562527591097478 ) ) ;
#22696 = VERTEX_POINT ( 'NONE', #45688 ) ;
#22697 = CARTESIAN_POINT ( 'NONE',  ( 109.8440526342893975, -45.34906309516006928, 57.25908649474392575 ) ) ;
#22698 = CARTESIAN_POINT ( 'NONE',  ( 48.79742451361993716, -36.32844715994080786, 117.4678068554150485 ) ) ;
#22699 = CARTESIAN_POINT ( 'NONE',  ( 112.1511370651177231, -26.84216853020813076, 169.6984824187689469 ) ) ;
#22700 = ADVANCED_FACE ( 'NONE', ( #89643 ), #87958, .F. ) ;
#22701 = DIRECTION ( 'NONE',  ( 0.7071067811865192621, 0.7071067811865758834, 7.071067811865185427E-16 ) ) ;
#22702 = DIRECTION ( 'NONE',  ( 0.000000000000000000, 0.000000000000000000, 1.000000000000000000 ) ) ;
#22703 = CYLINDRICAL_SURFACE ( 'NONE', #78236, 7.143750000000004263 ) ;
#22704 = LINE ( 'NONE', #8626, #33420 ) ;
#22705 = CARTESIAN_POINT ( 'NONE',  ( 117.5348948014565593, -36.80252384088669260, 259.8213395616249386 ) ) ;
#22706 = VERTEX_POINT ( 'NONE', #75998 ) ;
#22707 = EDGE_CURVE ( 'NONE', #32919, #33505, #35097, .T. ) ;
#22708 = CARTESIAN_POINT ( 'NONE',  ( 48.45959712128998120, -28.98061976758942748, 342.9256252759109884 ) ) ;
#22709 = ORIENTED_EDGE ( 'NONE', *, *, #62653, .F. ) ;
#22710 = CARTESIAN_POINT ( 'NONE',  ( 97.79748285543813324, -31.86337989110288405, 131.9413395616259947 ) ) ;
#22711 = LINE ( 'NONE', #72640, #35250 ) ;
#22712 = VERTEX_POINT ( 'NONE', #144 ) ;
#22713 = VERTEX_POINT ( 'NONE', #75565 ) ;
#22714 = ORIENTED_EDGE ( 'NONE', *, *, #74307, .T. ) ;
#22715 = CARTESIAN_POINT ( 'NONE',  ( 115.0372574689094023, -42.90846261676750828, 123.3022919376508071 ) ) ;
#22716 = CARTESIAN_POINT ( 'NONE',  ( 97.81413906161476746, -40.51632882248723888, 267.6361360915977343 ) ) ;
#22717 = DIRECTION ( 'NONE',  ( -1.000000000000000000, 0.000000000000000000, 0.000000000000000000 ) ) ;
#22718 = CARTESIAN_POINT ( 'NONE',  ( 100.4501120178094453, -50.96720088627028389, 0.4256252759109639960 ) ) ;
#22719 = LINE ( 'NONE', #77677, #9853 ) ;
#22720 = CARTESIAN_POINT ( 'NONE',  ( 97.35162482889903401, -32.85093483786611301, 37.02419670448292521 ) ) ;
#22721 = DIRECTION ( 'NONE',  ( 1.000000000000000000, 4.299999999999999979E-14, 1.000000000000000078E-15 ) ) ;
#22722 = ORIENTED_EDGE ( 'NONE', *, *, #29449, .F. ) ;
#22723 = CARTESIAN_POINT ( 'NONE',  ( 9.549149029459599092, 74.16675814752574070, 118.1711041523992662 ) ) ;
#22724 = VECTOR ( 'NONE', #62117, 1000.000000000000000 ) ;
#22725 = CARTESIAN_POINT ( 'NONE',  ( 105.7154676722796722, -46.72385723303512606, 42.46848526305529248 ) ) ;
#22726 = VERTEX_POINT ( 'NONE', #20598 ) ;
#22727 = ORIENTED_EDGE ( 'NONE', *, *, #72352, .F. ) ;
#22728 = VECTOR ( 'NONE', #85485, 1000.000000000000000 ) ;
#22729 = VECTOR ( 'NONE', #497, 1000.000000000000000 ) ;
#22730 = CARTESIAN_POINT ( 'NONE',  ( 82.80053463576300032, -19.07423037057760240, 3.076719480831280329 ) ) ;
#22731 = VECTOR ( 'NONE', #17428, 999.9999999999998863 ) ;
#22732 = CARTESIAN_POINT ( 'NONE',  ( 61.56670390244727287, -23.42844715994043980, 300.4678068554150627 ) ) ;
#22733 = DIRECTION ( 'NONE',  ( 0.000000000000000000, 0.000000000000000000, -1.000000000000000000 ) ) ;
#22734 = CONICAL_SURFACE ( 'NONE', #80688, 3.968750000000520473, 0.7853981633974667087 ) ;
#22735 = ADVANCED_FACE ( 'NONE', ( #62804 ), #82837, .T. ) ;
#22736 = CARTESIAN_POINT ( 'NONE',  ( 131.5667039024470455, -104.2784471599409244, 22.21780685541800082 ) ) ;
#22737 = CARTESIAN_POINT ( 'NONE',  ( 62.03715912545639100, -23.42818131006021787, 129.9678068554150911 ) ) ;
#22738 = EDGE_CURVE ( 'NONE', #76957, #51167, #41216, .T. ) ;
#22739 = CARTESIAN_POINT ( 'NONE',  ( 98.95796485450003388, -39.41423029504880304, 241.0038483995049603 ) ) ;
#22741 = CARTESIAN_POINT ( 'NONE',  ( 98.73996931189277859, -42.96625968561437503, 62.83848241876793850 ) ) ;
#22740 = CYLINDRICAL_SURFACE ( 'NONE', #31594, 5.041900000000001825 ) ;
#22742 = CARTESIAN_POINT ( 'NONE',  ( 150.5667039024473866, -25.42844715993594562, 249.9678068554149490 ) ) ;
#22743 = CARTESIAN_POINT ( 'NONE',  ( 95.43890296797121664, -34.19406290021405681, 106.1556252759109640 ) ) ;
#22744 = EDGE_LOOP ( 'NONE', ( #5590, #79885 ) ) ;
#22745 = LINE ( 'NONE', #50420, #24851 ) ;
#22746 = VERTEX_POINT ( 'NONE', #55521 ) ;
#22747 = EDGE_CURVE ( 'NONE', #81285, #89072, #56434, .T. ) ;
#22748 = FACE_BOUND ( 'NONE', #19124, .T. ) ;
#22749 = CYLINDRICAL_SURFACE ( 'NONE', #78988, 2.749999999999974687 ) ;
#22750 = VERTEX_POINT ( 'NONE', #583 ) ;
#22751 = CARTESIAN_POINT ( 'NONE',  ( 183.5150000000000148, 21.46300000000000097, 59.96543552338529537 ) ) ;
#22752 = ADVANCED_FACE ( 'NONE', ( #18909 ), #83717, .T. ) ;
#22753 = ORIENTED_EDGE ( 'NONE', *, *, #23933, .T. ) ;
#22754 = CARTESIAN_POINT ( 'NONE',  ( 84.06648329127399677, -18.72966777111522063, 17.92562527591199739 ) ) ;
#22755 = CARTESIAN_POINT ( 'NONE',  ( 98.30759644065037151, -41.72902612734809225, 272.7393669437288395 ) ) ;
#22756 = AXIS2_PLACEMENT_3D ( 'NONE', #20141, #26948, #41010 ) ;
#22757 = DIRECTION ( 'NONE',  ( -4.299999999999999979E-14, 1.000000000000000000, 0.000000000000000000 ) ) ;
#22758 = ORIENTED_EDGE ( 'NONE', *, *, #85346, .F. ) ;
#22759 = CIRCLE ( 'NONE', #66643, 1.499999999999987788 ) ;
#22760 = CARTESIAN_POINT ( 'NONE',  ( 97.24554646791794710, -31.60649478380229382, 90.93181575210196854 ) ) ;
#22761 = CARTESIAN_POINT ( 'NONE',  ( 0.000000000000000000, 0.000000000000000000, 0.000000000000000000 ) ) ;
#22762 = DIRECTION ( 'NONE',  ( -4.237773401492740281E-14, 1.000000000000000000, 0.000000000000000000 ) ) ;
#22763 = DIRECTION ( 'NONE',  ( 0.000000000000000000, 0.000000000000000000, 1.000000000000000000 ) ) ;
#22764 = CARTESIAN_POINT ( 'NONE',  ( 142.8698897858160706, -0.9167816978817300289, 396.9756252759102040 ) ) ;
#22765 = ORIENTED_EDGE ( 'NONE', *, *, #44642, .F. ) ;
#22766 = EDGE_CURVE ( 'NONE', #54446, #67055, #83273, .T. ) ;
#22767 = CARTESIAN_POINT ( 'NONE',  ( 114.0395979133839575, -29.51747486401405851, 120.4639116022243570 ) ) ;
#22768 = CARTESIAN_POINT ( 'NONE',  ( 97.06107108209303647, -37.99641183811671397, 156.4272919325953239 ) ) ;
#22769 = PLANE ( 'NONE',  #10991 ) ;
#22770 = CARTESIAN_POINT ( 'NONE',  ( 114.7874576214283167, -44.67122033332078246, 114.2022919425779719 ) ) ;
#22772 = LINE ( 'NONE', #70920, #44155 ) ;
#22771 = CARTESIAN_POINT ( 'NONE',  ( 177.3246001664172695, -48.34074026909179622, 300.4678068554149490 ) ) ;
#22773 = DIRECTION ( 'NONE',  ( -8.839355291601565315E-16, -1.000000000000000000, 0.000000000000000000 ) ) ;
#22774 = VECTOR ( 'NONE', #51419, 1000.000000000000000 ) ;
#22775 = EDGE_LOOP ( 'NONE', ( #40207, #17569, #24778, #2028 ) ) ;
#22776 = CARTESIAN_POINT ( 'NONE',  ( 76.06670390244796920, -26.72944715994109899, 239.5838068554169809 ) ) ;
#22777 = CARTESIAN_POINT ( 'NONE',  ( 114.4768422515204094, -30.34587328852060395, 180.3927681330529538 ) ) ;
#22779 = EDGE_LOOP ( 'NONE', ( #8433, #64175, #79498, #45475, #60713, #21536 ) ) ;
#22778 = CARTESIAN_POINT ( 'NONE',  ( 67.06670390244705970, -127.7048251178302678, 245.5588921750969860 ) ) ;
#22780 = CARTESIAN_POINT ( 'NONE',  ( 114.9268010244024225, -42.60560063232393446, 24.31562527591096767 ) ) ;
#22781 = CARTESIAN_POINT ( 'NONE',  ( 88.17226027475679473, -58.72944715994100306, 239.5838068554174924 ) ) ;
#22782 = CARTESIAN_POINT ( 'NONE',  ( 156.5667039024482676, -42.82844715993568485, 259.7178068554149490 ) ) ;
#22783 = CARTESIAN_POINT ( 'NONE',  ( 108.9744791726666051, -76.77844715994095282, 250.2178068554179902 ) ) ;
#22784 = CARTESIAN_POINT ( 'NONE',  ( 44.45000000000000284, 66.67499999999999716, 219.0749999999999886 ) ) ;
#22785 = DIRECTION ( 'NONE',  ( -1.000000000000000078E-15, 1.000000000000000083E-30, 1.000000000000000000 ) ) ;
#22786 = VECTOR ( 'NONE', #51239, 1000.000000000000000 ) ;
#22787 = CARTESIAN_POINT ( 'NONE',  ( 116.2522929705883712, -40.08866370952549829, 218.5470538473399529 ) ) ;
#22788 = VERTEX_POINT ( 'NONE', #7406 ) ;
#22789 = ORIENTED_EDGE ( 'NONE', *, *, #32084, .T. ) ;
#22790 = EDGE_CURVE ( 'NONE', #71894, #40087, #47825, .T. ) ;
#22791 = CARTESIAN_POINT ( 'NONE',  ( 112.6322303140947838, -44.29905650357037672, 179.5006309249449430 ) ) ;
#22792 = VECTOR ( 'NONE', #83745, 1000.000000000000000 ) ;
#22793 = FACE_OUTER_BOUND ( 'NONE', #41621, .T. ) ;
#22794 = PRESENTATION_LAYER_ASSIGNMENT (  '', '', ( #72065 ) ) ;
#22795 = CARTESIAN_POINT ( 'NONE',  ( 102.7262891916532084, -29.00345248032369483, 56.91586902018297423 ) ) ;
#22796 = VECTOR ( 'NONE', #33053, 1000.000000000000000 ) ;
#22797 = CARTESIAN_POINT ( 'NONE',  ( -93.48344774443276606, 95.14808745951972924, 91.13664476550712834 ) ) ;
#22798 = EDGE_CURVE ( 'NONE', #67480, #15446, #13775, .T. ) ;
#22799 = CARTESIAN_POINT ( 'NONE',  ( 104.4076873786489159, -46.45796789277314076, 267.3648837029242600 ) ) ;
#22800 = CARTESIAN_POINT ( 'NONE',  ( 85.35814995794051185, 12.92155284005802685, 335.5992267699911054 ) ) ;
#22801 = ORIENTED_EDGE ( 'NONE', *, *, #19498, .T. ) ;
#22802 = PLANE ( 'NONE',  #53 ) ;
#22803 = DIRECTION ( 'NONE',  ( 0.7071067811575898476, -0.7071067812155052978, 0.000000000000000000 ) ) ;
#22804 = CARTESIAN_POINT ( 'NONE',  ( 99.41296134609922319, -28.78668791560518514, 265.6746728949588032 ) ) ;
#22805 = CARTESIAN_POINT ( 'NONE',  ( 97.60818021318179660, -39.98327219696195556, 171.5903219849872698 ) ) ;
#22806 = EDGE_LOOP ( 'NONE', ( #88053, #78577 ) ) ;
#22807 = EDGE_LOOP ( 'NONE', ( #46592, #27072, #15871, #40206 ) ) ;
#22808 = DIRECTION ( 'NONE',  ( 0.000000000000000000, 1.000000000000000000, 0.000000000000000000 ) ) ;
#22809 = CARTESIAN_POINT ( 'NONE',  ( -85.84941893669265767, 94.92435932957486955, -81.76533775135462179 ) ) ;
#22810 = CARTESIAN_POINT ( 'NONE',  ( 97.86644135638643149, -40.64890597622355273, 122.6464849464893945 ) ) ;
#22811 = AXIS2_PLACEMENT_3D ( 'NONE', #76966, #35618, #7918 ) ;
#22812 = FACE_OUTER_BOUND ( 'NONE', #42758, .T. ) ;
#22813 = AXIS2_PLACEMENT_3D ( 'NONE', #41343, #54066, #48157 ) ;
#22814 = CARTESIAN_POINT ( 'NONE',  ( 112.4622727538958316, -27.87370092883246286, 45.62895860924398761 ) ) ;
#22815 = CARTESIAN_POINT ( 'NONE',  ( 12.52017789511383405, 80.90898357847464695, 117.6920314563592314 ) ) ;
#22816 = ORIENTED_EDGE ( 'NONE', *, *, #78270, .F. ) ;
#22817 = ADVANCED_FACE ( 'NONE', ( #13333 ), #21494, .T. ) ;
#22818 = CARTESIAN_POINT ( 'NONE',  ( 100.9155127638074703, -46.91653085812070856, 48.14419670448194211 ) ) ;
#22819 = CARTESIAN_POINT ( 'NONE',  ( 188.5667039024482960, -48.82844715993431350, 259.7178068554150059 ) ) ;
#22820 = CARTESIAN_POINT ( 'NONE',  ( 116.5366478410923463, -42.42989196264584706, 278.3832443235298797 ) ) ;
#22821 = ORIENTED_EDGE ( 'NONE', *, *, #87919, .F. ) ;
#22822 = CARTESIAN_POINT ( 'NONE',  ( 68.77377604071689632, -69.45229246467815187, 247.4784000562319761 ) ) ;
#22823 = CARTESIAN_POINT ( 'NONE',  ( 107.0667039024470313, -104.2784471599409528, 22.21780685541800082 ) ) ;
#22824 = LINE ( 'NONE', #85057, #88829 ) ;
#22825 = CARTESIAN_POINT ( 'NONE',  ( 98.00070950526129820, -34.75266269402447250, 103.9738046553059547 ) ) ;
#22826 = CARTESIAN_POINT ( 'NONE',  ( 101.4135918642175369, -46.25467808933209568, 203.1622919425779514 ) ) ;
#22827 = DIRECTION ( 'NONE',  ( 0.000000000000000000, 1.000000000000000000, 0.000000000000000000 ) ) ;
#22828 = ORIENTED_EDGE ( 'NONE', *, *, #17511, .F. ) ;
#22829 = CARTESIAN_POINT ( 'NONE',  ( 51.06648329127400388, 25.62155284005901379, 333.4006252759110112 ) ) ;
#22830 = ORIENTED_EDGE ( 'NONE', *, *, #29741, .T. ) ;
#22832 = EDGE_LOOP ( 'NONE', ( #29513, #23053, #87922, #5145 ) ) ;
#22831 = AXIS2_PLACEMENT_3D ( 'NONE', #79295, #17054, #73795 ) ;
#22833 = DIRECTION ( 'NONE',  ( -6.524622321627019585E-16, -3.741823817616790462E-31, -1.000000000000000000 ) ) ;
#22834 = EDGE_LOOP ( 'NONE', ( #70701, #38384, #38052, #11439 ) ) ;
#22835 = ORIENTED_EDGE ( 'NONE', *, *, #57005, .T. ) ;
#22836 = CARTESIAN_POINT ( 'NONE',  ( 3.968749999999229949, 127.0000000000000000, 100.8961411191535973 ) ) ;
#22837 = CARTESIAN_POINT ( 'NONE',  ( 107.7709757720581649, -26.73284657607137405, 41.02040754495594399 ) ) ;
#22838 = ADVANCED_FACE ( 'NONE', ( #7850 ), #25722, .F. ) ;
#22839 = CARTESIAN_POINT ( 'NONE',  ( 108.4402549024021312, -27.77817906387560143, 144.3657531614099412 ) ) ;
#22840 = CARTESIAN_POINT ( 'NONE',  ( 99.31672145811513985, -28.81511631862888123, 270.7051490854347549 ) ) ;
#22841 = EDGE_CURVE ( 'NONE', #88945, #74932, #42350, .T. ) ;
#22842 = LINE ( 'NONE', #85075, #19450 ) ;
#22843 = EDGE_CURVE ( 'NONE', #71309, #54367, #76444, .T. ) ;
#22844 = ORIENTED_EDGE ( 'NONE', *, *, #27141, .T. ) ;
#22845 = EDGE_CURVE ( 'NONE', #66449, #45792, #70080, .T. ) ;
#22846 = ORIENTED_EDGE ( 'NONE', *, *, #61192, .F. ) ;
#22847 = CARTESIAN_POINT ( 'NONE',  ( 13.86911000615387302, 224.4999999999999432, 102.9892450244911686 ) ) ;
#22848 = CIRCLE ( 'NONE', #15650, 1.000000000000000888 ) ;
#22849 = CARTESIAN_POINT ( 'NONE',  ( 1.475953350320055108E-14, 184.0000000000000000, 104.4754207677255806 ) ) ;
#22850 = CARTESIAN_POINT ( 'NONE',  ( 142.8832909413445122, -79.11588146349311046, 361.9756252759100335 ) ) ;
#22851 = CARTESIAN_POINT ( 'NONE',  ( 111.0995558192250456, -25.53287967237518430, 99.80133956162498521 ) ) ;
#22853 = DIRECTION ( 'NONE',  ( -0.000000000000000000, 1.000000000000000000, 0.000000000000000000 ) ) ;
#22852 = VECTOR ( 'NONE', #80964, 1000.000000000000000 ) ;
#22854 = ORIENTED_EDGE ( 'NONE', *, *, #78349, .T. ) ;
#22855 = CIRCLE ( 'NONE', #37302, 13.50000000000000533 ) ;
#22856 = CARTESIAN_POINT ( 'NONE',  ( 110.7331673686684610, -26.30186281216086996, 254.8194347997205682 ) ) ;
#22857 = DIRECTION ( 'NONE',  ( 0.000000000000000000, 1.000000000000000000, 0.000000000000000000 ) ) ;
#22858 = CIRCLE ( 'NONE', #19925, 8.999999999999994671 ) ;
#22859 = CARTESIAN_POINT ( 'NONE',  ( 45.77381068350376125, -48.62134037888161231, 180.4678068554150911 ) ) ;
#22860 = DIRECTION ( 'NONE',  ( 1.000000000000000078E-15, -1.000000000000000083E-30, -1.000000000000000000 ) ) ;
#22862 = DIRECTION ( 'NONE',  ( -0.000000000000000000, 1.000000000000000000, -0.000000000000000000 ) ) ;
#22861 = DIRECTION ( 'NONE',  ( 2.301579500234999682E-14, 0.000000000000000000, -1.000000000000000000 ) ) ;
#22863 = PLANE ( 'NONE',  #26408 ) ;
#22864 = CYLINDRICAL_SURFACE ( 'NONE', #55352, 2.500000000000002220 ) ;
#22865 = LINE ( 'NONE', #51864, #17952 ) ;
#22866 = EDGE_CURVE ( 'NONE', #68825, #23110, #70538, .T. ) ;
#22867 = CARTESIAN_POINT ( 'NONE',  ( 9.331435647859348646E-23, 95.25000000000000000, 130.5560000000000116 ) ) ;
#22868 = EDGE_CURVE ( 'NONE', #16110, #40366, #74564, .T. ) ;
#22869 = DIRECTION ( 'NONE',  ( 2.900000000000000265E-14, -2.000000000000000155E-15, 1.000000000000000000 ) ) ;
#22870 = CARTESIAN_POINT ( 'NONE',  ( 31.71315051186898870, -31.94127993907790852, -5.074374724088000832 ) ) ;
#22872 = VERTEX_POINT ( 'NONE', #1944 ) ;
#22871 = CARTESIAN_POINT ( 'NONE',  ( 144.5667039024470455, -118.2784471599408960, 51.21780685541800437 ) ) ;
#22873 = LINE ( 'NONE', #78290, #17713 ) ;
#22874 = CARTESIAN_POINT ( 'NONE',  ( 105.1555015486555078, -47.05240725173535310, 12.42991099019596923 ) ) ;
#22875 = CARTESIAN_POINT ( 'NONE',  ( 104.5626002042890974, -48.31241677248981858, 178.4070538473399665 ) ) ;
#22876 = CARTESIAN_POINT ( 'NONE',  ( 111.1374431767090414, -47.03053892029802796, 18.88800622829195319 ) ) ;
#22877 = VECTOR ( 'NONE', #80891, 1000.000000000000000 ) ;
#22878 = VECTOR ( 'NONE', #43024, 1000.000000000000000 ) ;
#22880 = CARTESIAN_POINT ( 'NONE',  ( 0.000000000000000000, 124.5870000000000033, 0.000000000000000000 ) ) ;
#22879 = LINE ( 'NONE', #76936, #33392 ) ;
#22881 = FACE_OUTER_BOUND ( 'NONE', #52691, .T. ) ;
#22882 = VECTOR ( 'NONE', #18063, 1000.000000000000000 ) ;
#22883 = VERTEX_POINT ( 'NONE', #64610 ) ;
#22884 = LINE ( 'NONE', #63762, #70832 ) ;
#22885 = ORIENTED_EDGE ( 'NONE', *, *, #44306, .F. ) ;
#22886 = CARTESIAN_POINT ( 'NONE',  ( 116.6363502066642468, -38.74961609181404043, 59.66133956162394725 ) ) ;
#22888 = ORIENTED_EDGE ( 'NONE', *, *, #85560, .T. ) ;
#22887 = DIRECTION ( 'NONE',  ( 1.000000000000000078E-15, 1.000000000000000083E-30, -1.000000000000000000 ) ) ;
#22889 = CARTESIAN_POINT ( 'NONE',  ( 101.9934276907083444, -45.44595233133192380, 48.15644075925013823 ) ) ;
#22890 = CARTESIAN_POINT ( 'NONE',  ( 108.1794352217186201, -47.07304438381563472, 198.6613395616249989 ) ) ;
#22891 = DIRECTION ( 'NONE',  ( 0.000000000000000000, 1.000000000000000000, 0.000000000000000000 ) ) ;
#22892 = CARTESIAN_POINT ( 'NONE',  ( 98.54783405468135982, -41.97727565318817966, 146.7658588207967796 ) ) ;
#22893 = DIRECTION ( 'NONE',  ( -0.000000000000000000, -0.000000000000000000, 1.000000000000000000 ) ) ;
#22894 = LINE ( 'NONE', #77396, #68829 ) ;
#22895 = FACE_OUTER_BOUND ( 'NONE', #58720, .T. ) ;
#22896 = CARTESIAN_POINT ( 'NONE',  ( 111.0136030271875285, -45.91768036457248314, 97.89935017080178170 ) ) ;
#22897 = CARTESIAN_POINT ( 'NONE',  ( 98.36735121233621726, -42.37464764417353535, 146.7965776568640024 ) ) ;
#22898 = ORIENTED_EDGE ( 'NONE', *, *, #4635, .T. ) ;
#22899 = VERTEX_POINT ( 'NONE', #29203 ) ;
#22900 = ADVANCED_FACE ( 'NONE', ( #50066 ), #36467, .T. ) ;
#22901 = VECTOR ( 'NONE', #75879, 1000.000000000000000 ) ;
#22902 = CARTESIAN_POINT ( 'NONE',  ( 115.8905597133153549, -37.54428082998141747, 75.18444044875394638 ) ) ;
#22903 = CARTESIAN_POINT ( 'NONE',  ( 128.5446125969797606, -87.02121134100629263, 250.2178068554179902 ) ) ;
#22905 = LINE ( 'NONE', #17414, #23073 ) ;
#22904 = CARTESIAN_POINT ( 'NONE',  ( 114.1395267584829014, -29.97404255306821241, 230.4327681330529742 ) ) ;
#22906 = CARTESIAN_POINT ( 'NONE',  ( 36.23715912545430484, -47.82818131006125384, 237.4678068554150059 ) ) ;
#22908 = ADVANCED_FACE ( 'NONE', ( #16915 ), #58665, .F. ) ;
#22907 = CARTESIAN_POINT ( 'NONE',  ( 3.968750000000000000, 127.0000000000000000, -105.4788588808464027 ) ) ;
#22909 = PLANE ( 'NONE',  #5426 ) ;
#22910 = CARTESIAN_POINT ( 'NONE',  ( 21.56670390244635271, -23.42844715994195326, 117.4678068554150343 ) ) ;
#22911 = CARTESIAN_POINT ( 'NONE',  ( 0.8226717696920563538, 69.95000000000000284, 118.5560000000000258 ) ) ;
#22912 = CARTESIAN_POINT ( 'NONE',  ( 114.4473569665854313, -28.53271593493105485, 159.5051490854349652 ) ) ;
#22913 = EDGE_LOOP ( 'NONE', ( #54430, #69988 ) ) ;
#22914 = ORIENTED_EDGE ( 'NONE', *, *, #27206, .T. ) ;
#22915 = ORIENTED_EDGE ( 'NONE', *, *, #89073, .F. ) ;
#22916 =( NAMED_UNIT ( * ) PLANE_ANGLE_UNIT ( ) SI_UNIT ( $, .RADIAN. ) );
#22917 = CARTESIAN_POINT ( 'NONE',  ( -103.1875000000000000, 127.0000000000000000, 7.143749999998919797 ) ) ;
#22918 = CARTESIAN_POINT ( 'NONE',  ( 97.78494223251618678, -40.45150674683588932, 131.6299638674549897 ) ) ;
#22919 = CARTESIAN_POINT ( 'NONE',  ( 131.3179999999999836, 34.75001145038165618, 43.29625283494679877 ) ) ;
#22920 = CARTESIAN_POINT ( 'NONE',  ( 111.7906875226637879, -43.98084836425640276, 220.8661856076869583 ) ) ;
#22921 = CIRCLE ( 'NONE', #34493, 11.45913725231036118 ) ;
#22923 = EDGE_CURVE ( 'NONE', #37352, #12546, #56885, .T. ) ;
#22922 = VECTOR ( 'NONE', #52, 1000.000000000000000 ) ;
#22924 = CARTESIAN_POINT ( 'NONE',  ( 107.0667039024470313, -104.2784471599413791, 2.217806855418003043 ) ) ;
#22925 = CARTESIAN_POINT ( 'NONE',  ( 95.67500926166044906, -33.46221576448694890, 141.1041967044829732 ) ) ;
#22926 = LINE ( 'NONE', #30172, #5404 ) ;
#22927 = VERTEX_POINT ( 'NONE', #72327 ) ;
#22929 = ORIENTED_EDGE ( 'NONE', *, *, #36908, .T. ) ;
#22928 = VERTEX_POINT ( 'NONE', #9644 ) ;
#22930 = B_SPLINE_CURVE_WITH_KNOTS ( 'NONE', 3,
 ( #68481, #62882, #56053, #50142, #28831, #77423, #42877, #70611, #56963, #84704, #22467, #36976, #24245, #31483, #9722, #86040, #58313, #23809 ),
 .UNSPECIFIED., .F., .F.,
 ( 4, 2, 2, 2, 2, 2, 2, 2, 4 ),
 ( 0.000000000000000000, 0.06250000004081082694, 0.1250000000816216539, 0.1875000001224324808, 0.2500000001632433078, 0.3125000002040541069, 0.3750000002448649616, 0.4375000002856758163, 0.5000000003264866155 ),
 .UNSPECIFIED. ) ;
#22931 = AXIS2_PLACEMENT_3D ( 'NONE', #77091, #84811, #48895 ) ;
#22932 = LINE ( 'NONE', #7498, #21563 ) ;
#22933 = ORIENTED_EDGE ( 'NONE', *, *, #30837, .T. ) ;
#22934 = ORIENTED_EDGE ( 'NONE', *, *, #31247, .T. ) ;
#22935 = DIRECTION ( 'NONE',  ( 0.000000000000000000, 0.4999999999999995004, 0.8660254037844390407 ) ) ;
#22936 = DIRECTION ( 'NONE',  ( -4.237773401492740281E-14, 1.000000000000000000, 0.000000000000000000 ) ) ;
#22937 = CARTESIAN_POINT ( 'NONE',  ( 100.4929819111635538, -30.01635508975405031, 267.1368214011352507 ) ) ;
#22938 = AXIS2_PLACEMENT_3D ( 'NONE', #37700, #51742, #38134 ) ;
#22939 = EDGE_CURVE ( 'NONE', #7001, #73034, #50522, .T. ) ;
#22940 = CARTESIAN_POINT ( 'NONE',  ( 109.6430113662638064, -46.48008694528652995, 272.7814585466231847 ) ) ;
#22941 = ORIENTED_EDGE ( 'NONE', *, *, #13205, .F. ) ;
#22942 = VECTOR ( 'NONE', #23146, 1000.000000000000000 ) ;
#22943 = VECTOR ( 'NONE', #62716, 1000.000000000000114 ) ;
#22944 = CARTESIAN_POINT ( 'NONE',  ( 111.4213356664735386, -44.07558929780552148, 9.635625275910941312 ) ) ;
#22945 = DIRECTION ( 'NONE',  ( 0.000000000000000000, 0.000000000000000000, -1.000000000000000000 ) ) ;
#22946 = EDGE_LOOP ( 'NONE', ( #45727, #89350 ) ) ;
#22947 = VERTEX_POINT ( 'NONE', #50970 ) ;
#22948 = AXIS2_PLACEMENT_3D ( 'NONE', #23469, #31142, #9823 ) ;
#22949 = CARTESIAN_POINT ( 'NONE',  ( 116.9125557316235557, -38.73407091525943002, 113.6668860931665108 ) ) ;
#22950 = EDGE_LOOP ( 'NONE', ( #2031, #85623, #66938, #80674 ) ) ;
#22951 = EDGE_LOOP ( 'NONE', ( #25198, #82846, #61046, #10950 ) ) ;
#22952 = ADVANCED_FACE ( 'NONE', ( #22387 ), #51401, .T. ) ;
#22953 = CIRCLE ( 'NONE', #44699, 2.117000000000000881 ) ;
#22954 = CARTESIAN_POINT ( 'NONE',  ( 114.3408732721816534, -41.20596775705023163, 17.80956268521999419 ) ) ;
#22955 = CARTESIAN_POINT ( 'NONE',  ( 114.2686970495659295, -44.29742072815643184, 158.1813395616249807 ) ) ;
#22956 = CARTESIAN_POINT ( 'NONE',  ( 117.5859182825552978, -33.41202194707543782, 129.0575300378159795 ) ) ;
#22957 = CARTESIAN_POINT ( 'NONE',  ( 194.5667039024479834, -48.82844715994099971, 300.9178068554150514 ) ) ;
#22958 = CARTESIAN_POINT ( 'NONE',  ( 97.47313694375068849, -40.89946378256092174, 227.6527681330539679 ) ) ;
#22959 = DIRECTION ( 'NONE',  ( 3.100000000000000258E-29, -3.100000000000000044E-14, -1.000000000000000000 ) ) ;
#22960 = EDGE_CURVE ( 'NONE', #67060, #22058, #30092, .T. ) ;
#22961 = CARTESIAN_POINT ( 'NONE',  ( 68.66208373768751017, -72.70246804406471597, 247.4783998280180128 ) ) ;
#22962 = EDGE_LOOP ( 'NONE', ( #38669, #57424, #84165, #11719, #82926, #33879 ) ) ;
#22963 = CARTESIAN_POINT ( 'NONE',  ( -130.4667021054748943, 70.80031572943160256, 4.873084223276297422 ) ) ;
#22964 = ORIENTED_EDGE ( 'NONE', *, *, #49533, .F. ) ;
#22965 = ORIENTED_EDGE ( 'NONE', *, *, #5335, .F. ) ;
#22966 = VECTOR ( 'NONE', #32462, 1000.000000000000000 ) ;
#22967 = CARTESIAN_POINT ( 'NONE',  ( 107.2439172579031919, -47.23279478401654075, 212.5899109901969837 ) ) ;
#22968 = ORIENTED_EDGE ( 'NONE', *, *, #59308, .F. ) ;
#22969 = CARTESIAN_POINT ( 'NONE',  ( 117.4874684240972300, -40.41484487456647656, 178.5680062282919778 ) ) ;
#22970 = LINE ( 'NONE', #35222, #42751 ) ;
#22971 = CARTESIAN_POINT ( 'NONE',  ( 134.4383386548979331, -33.97944715994099596, 8.225625275910996237 ) ) ;
#22972 = CARTESIAN_POINT ( 'NONE',  ( 32.25690895537066183, -33.54226604285041446, 313.9678068554150059 ) ) ;
#22975 = CARTESIAN_POINT ( 'NONE',  ( 101.3060704567421624, -26.40153104436181053, 251.4813395616249920 ) ) ;
#22974 = CARTESIAN_POINT ( 'NONE',  ( 107.0664832912739399, -36.72944715994095333, 290.1356252759106837 ) ) ;
#22973 = CARTESIAN_POINT ( 'NONE',  ( 0.000000000000000000, 11.98343896644750117, 0.000000000000000000 ) ) ;
#22976 = DIRECTION ( 'NONE',  ( 1.092739197465705130E-14, 0.000000000000000000, -1.000000000000000000 ) ) ;
#22977 = FACE_OUTER_BOUND ( 'NONE', #39309, .T. ) ;
#22978 = CARTESIAN_POINT ( 'NONE',  ( 97.06115611282757527, -37.99685616894899454, 272.4268914305668545 ) ) ;
#22979 = EDGE_CURVE ( 'NONE', #29605, #17228, #22842, .T. ) ;
#22980 = DIRECTION ( 'NONE',  ( -0.7071067811865170416, -0.7071067811865778818, -7.071067811865474347E-16 ) ) ;
#22981 = EDGE_CURVE ( 'NONE', #44492, #44045, #64173, .T. ) ;
#22982 = CARTESIAN_POINT ( 'NONE',  ( 102.0670549422599294, -27.97049806924179549, 256.4897919441917793 ) ) ;
#22983 = CARTESIAN_POINT ( 'NONE',  ( 107.0664832912739968, -36.72944715994100306, 287.6356252759109680 ) ) ;
#22985 = ORIENTED_EDGE ( 'NONE', *, *, #38503, .F. ) ;
#22984 = CARTESIAN_POINT ( 'NONE',  ( 98.59159163785028568, -35.76670619840676579, 195.5838068554172082 ) ) ;
#22986 = CARTESIAN_POINT ( 'NONE',  ( 74.19170390244700286, -80.65344715994098124, 55.21780685541800437 ) ) ;
#22987 = CARTESIAN_POINT ( 'NONE',  ( 97.74263787230347589, -41.52050856888216401, 196.7041967044819728 ) ) ;
#22988 = CARTESIAN_POINT ( 'NONE',  ( 106.6603377114791300, -26.31227224467070158, 81.10705384733896040 ) ) ;
#22989 = CARTESIAN_POINT ( 'NONE',  ( 117.1100247017212723, -39.68245506451066262, 179.5984824187679294 ) ) ;
#22990 = FACE_OUTER_BOUND ( 'NONE', #45919, .T. ) ;
#22991 = DIRECTION ( 'NONE',  ( 0.000000000000000000, 0.000000000000000000, 1.000000000000000000 ) ) ;
#22993 = CARTESIAN_POINT ( 'NONE',  ( 182.0374245136140132, -23.42844715993459559, 313.9678068554149490 ) ) ;
#22992 = DIRECTION ( 'NONE',  ( 1.000000000000000000, 4.163336342344333240E-14, 0.000000000000000000 ) ) ;
#22994 = DIRECTION ( 'NONE',  ( -1.000000000000000000, 0.000000000000000000, -2.108231265501709878E-16 ) ) ;
#22995 = CARTESIAN_POINT ( 'NONE',  ( 97.81670390244700286, -67.87844715994096134, 96.96780685541800437 ) ) ;
#22996 = EDGE_LOOP ( 'NONE', ( #48629, #80672, #68449, #19435, #80218, #10306 ) ) ;
#22997 = CARTESIAN_POINT ( 'NONE',  ( 52.06670390244700286, -77.67844715994100113, 222.2178068554179902 ) ) ;
#22998 = CIRCLE ( 'NONE', #88212, 4.749999999999976907 ) ;
#22999 = VECTOR ( 'NONE', #63062, 999.9999999999998863 ) ;
#23000 = EDGE_LOOP ( 'NONE', ( #53611, #75190 ) ) ;
#23001 = ORIENTED_EDGE ( 'NONE', *, *, #66951, .F. ) ;
#23002 = CARTESIAN_POINT ( 'NONE',  ( 113.3792027166817320, -43.22269317268541755, 117.6248007804579458 ) ) ;
#23003 = CIRCLE ( 'NONE', #41820, 30.99999999999998579 ) ;
#23005 = VERTEX_POINT ( 'NONE', #71443 ) ;
#23004 = LINE ( 'NONE', #72910, #80713 ) ;
#23006 = CARTESIAN_POINT ( 'NONE',  ( 112.7897778137181746, -47.07797880090539167, 98.97848241876793907 ) ) ;
#23007 = CARTESIAN_POINT ( 'NONE',  ( 180.3521107875639871, -35.65087443492551245, -5.074374724088000832 ) ) ;
#23008 = VECTOR ( 'NONE', #41081, 1000.000000000000000 ) ;
#23009 = DIRECTION ( 'NONE',  ( 4.299999999999999979E-14, -1.000000000000000000, 4.400000000000000367E-29 ) ) ;
#23010 = CYLINDRICAL_SURFACE ( 'NONE', #50557, 2.750000000000002665 ) ;
#23011 = VECTOR ( 'NONE', #58842, 1000.000000000000000 ) ;
#23012 = CIRCLE ( 'NONE', #78122, 7.937500000000000000 ) ;
#23013 = CARTESIAN_POINT ( 'NONE',  ( 100.8224265971272615, -29.20115443902020047, 40.62705384733994407 ) ) ;
#23014 = ORIENTED_EDGE ( 'NONE', *, *, #1441, .T. ) ;
#23015 = ORIENTED_EDGE ( 'NONE', *, *, #8266, .F. ) ;
#23016 = VERTEX_POINT ( 'NONE', #43251 ) ;
#23017 = DIRECTION ( 'NONE',  ( -1.500809167996645702E-15, 0.7071067811865391350, 0.7071067811865560104 ) ) ;
#23018 = DIRECTION ( 'NONE',  ( 0.000000000000000000, 0.000000000000000000, 1.000000000000000000 ) ) ;
#23019 = DIRECTION ( 'NONE',  ( -1.821231995776174246E-16, 0.000000000000000000, -1.000000000000000000 ) ) ;
#23020 = LINE ( 'NONE', #44769, #32429 ) ;
#23021 = CARTESIAN_POINT ( 'NONE',  ( 84.21071524772710859, 88.91113633199482535, 99.76704648670086328 ) ) ;
#23023 = EDGE_CURVE ( 'NONE', #46913, #58480, #35548, .T. ) ;
#23022 = DIRECTION ( 'NONE',  ( 0.000000000000000000, 0.000000000000000000, -1.000000000000000000 ) ) ;
#23024 = VECTOR ( 'NONE', #25838, 1000.000000000000000 ) ;
#23025 = LINE ( 'NONE', #9378, #73744 ) ;
#23026 = CARTESIAN_POINT ( 'NONE',  ( -7.158941453477376982, 93.04008847735218524, 130.3595723459966962 ) ) ;
#23027 = CARTESIAN_POINT ( 'NONE',  ( 115.9265467165008232, -42.18176083994495684, 18.38705384733896153 ) ) ;
#23028 = ORIENTED_EDGE ( 'NONE', *, *, #4088, .T. ) ;
#23029 = CARTESIAN_POINT ( 'NONE',  ( 97.31584336463156149, -39.30597463869850117, 271.5314584984529347 ) ) ;
#23030 = CIRCLE ( 'NONE', #36040, 25.39999999999999858 ) ;
#23031 = PLANE ( 'NONE',  #88839 ) ;
#23032 = CARTESIAN_POINT ( 'NONE',  ( 108.9785397593094132, -44.66504833944034658, 130.5823760838769658 ) ) ;
#23033 = VECTOR ( 'NONE', #66209, 1000.000000000000000 ) ;
#23034 = EDGE_CURVE ( 'NONE', #53581, #14208, #29635, .T. ) ;
#23035 = EDGE_CURVE ( 'NONE', #35978, #68568, #39737, .T. ) ;
#23036 = LINE ( 'NONE', #69157, #3522 ) ;
#23037 = CARTESIAN_POINT ( 'NONE',  ( -103.1875000000000000, 127.0000000000000000, -7.937500000001080913 ) ) ;
#23038 = VERTEX_POINT ( 'NONE', #60003 ) ;
#23039 = ORIENTED_EDGE ( 'NONE', *, *, #45907, .T. ) ;
#23040 = ADVANCED_FACE ( 'NONE', ( #80044 ), #88648, .F. ) ;
#23041 = CARTESIAN_POINT ( 'NONE',  ( 21.56670390244701707, -23.42844715994183957, 249.9678068554150059 ) ) ;
#23042 = ORIENTED_EDGE ( 'NONE', *, *, #40737, .T. ) ;
#23043 = EDGE_LOOP ( 'NONE', ( #11733, #62699, #66985, #38202 ) ) ;
#23044 = EDGE_CURVE ( 'NONE', #61646, #49324, #77501, .T. ) ;
#23045 = CARTESIAN_POINT ( 'NONE',  ( 102.7466871476783581, -44.50128676613118728, 183.6044404487539623 ) ) ;
#23046 = VECTOR ( 'NONE', #77033, 1000.000000000000000 ) ;
#23047 = EDGE_CURVE ( 'NONE', #8827, #20097, #87735, .T. ) ;
#23048 = CYLINDRICAL_SURFACE ( 'NONE', #61217, 1.000000000002049694 ) ;
#23049 = CARTESIAN_POINT ( 'NONE',  ( 108.0361718062294614, -25.69563957016125855, 105.9946728949589811 ) ) ;
#23050 = CARTESIAN_POINT ( 'NONE',  ( 108.4174893140138352, -26.73503593703446057, 119.9689586043175211 ) ) ;
#23051 = ADVANCED_FACE ( 'NONE', ( #45476 ), #80484, .T. ) ;
#23052 = CARTESIAN_POINT ( 'NONE',  ( 110.8537921787340252, -45.98451557629201147, 17.88556681916309898 ) ) ;
#23053 = ORIENTED_EDGE ( 'NONE', *, *, #4083, .F. ) ;
#23054 = EDGE_CURVE ( 'NONE', #15084, #38527, #44077, .T. ) ;
#23055 = CONICAL_SURFACE ( 'NONE', #11419, 10.00000000000000888, 0.7853981633974691512 ) ;
#23056 = ORIENTED_EDGE ( 'NONE', *, *, #37824, .F. ) ;
#23057 = ORIENTED_EDGE ( 'NONE', *, *, #13813, .T. ) ;
#23058 = ADVANCED_FACE ( 'NONE', ( #19147 ), #86850, .F. ) ;
#23059 = CARTESIAN_POINT ( 'NONE',  ( 114.8623915286450199, -39.24071799505598079, 156.3966617981629668 ) ) ;
#23060 = VECTOR ( 'NONE', #22701, 1000.000000000000000 ) ;
#23061 = CARTESIAN_POINT ( 'NONE',  ( 103.9507802182147600, -47.35902078718802954, 62.33753003781600199 ) ) ;
#23062 = ORIENTED_EDGE ( 'NONE', *, *, #57983, .F. ) ;
#23063 = CARTESIAN_POINT ( 'NONE',  ( 101.3960830062750063, -28.00733582429760204, 25.53562527591096654 ) ) ;
#23064 = CARTESIAN_POINT ( 'NONE',  ( 97.65507918845807467, -41.26406199109977280, 167.6841967044829573 ) ) ;
#23065 = EDGE_CURVE ( 'NONE', #16664, #86561, #53628, .T. ) ;
#23066 = B_SPLINE_CURVE_WITH_KNOTS ( 'NONE', 3,
 ( #39776, #60668, #40228, #32972, #6619, #5735, #89754, #13438, #26168, #55629, #34768, #75216, #53836, #34315, #55181, #33425, #89302, #88855, #62472, #82941, #68848, #81606, #12092, #83377, #48369, #76103, #74763, #13882, #12542, #26609, #67489 ),
 .UNSPECIFIED., .F., .F.,
 ( 4, 2, 2, 1, 2, 2, 2, 2, 2, 2, 2, 1, 1, 2, 2, 2, 4 ),
 ( 0.000000000000000000, 0.1249999999999597267, 0.1874999999999392708, 0.2187499999999290290, 0.2343749999999237554, 0.2499999999999185096, 0.3749999999999280575, 0.4374999999999334421, 0.4999999999999388267, 0.6249999999999505951, 0.6874999999999609201, 0.7187499999999670264, 0.7343749999999702460, 0.7421874999999727995, 0.7499999999999753530, 0.8749999999999876765, 1.000000000000000000 ),
 .UNSPECIFIED. ) ;
#23067 = CARTESIAN_POINT ( 'NONE',  ( 107.0667039024470313, -104.2784471599420755, -19.78219314458201694 ) ) ;
#23068 = CARTESIAN_POINT ( 'NONE',  ( -109.2774118001975836, 52.30007095126370587, 71.43750000000027001 ) ) ;
#23069 = CARTESIAN_POINT ( 'NONE',  ( 98.84006766826026080, -28.19945879207355688, 111.6870538473389587 ) ) ;
#23070 = EDGE_CURVE ( 'NONE', #83877, #32492, #46821, .T. ) ;
#23071 = DIRECTION ( 'NONE',  ( 0.000000000000000000, 0.000000000000000000, 1.000000000000000000 ) ) ;
#23072 = ORIENTED_EDGE ( 'NONE', *, *, #302, .T. ) ;
#23073 = VECTOR ( 'NONE', #45097, 999.9999999999998863 ) ;
#23074 = CARTESIAN_POINT ( 'NONE',  ( -41.60202597009397607, 76.06518036156089124, 50.85338361873603219 ) ) ;
#23075 = ORIENTED_EDGE ( 'NONE', *, *, #48631, .F. ) ;
#23076 = VECTOR ( 'NONE', #74793, 1000.000000000000000 ) ;
#23077 = CARTESIAN_POINT ( 'NONE',  ( 116.7954517155124563, -39.38667583240329151, 134.6155541235699786 ) ) ;
#23078 = DIRECTION ( 'NONE',  ( 0.000000000000000000, 0.000000000000000000, -1.000000000000000000 ) ) ;
#23079 = VERTEX_POINT ( 'NONE', #59557 ) ;
#23080 = DIRECTION ( 'NONE',  ( 0.000000000000000000, -1.000000000000000000, 0.000000000000000000 ) ) ;
#23081 = LINE ( 'NONE', #16250, #87033 ) ;
#23082 = CARTESIAN_POINT ( 'NONE',  ( 117.0539912639601852, -31.99354471700374702, 64.19086337114899266 ) ) ;
#23083 = CARTESIAN_POINT ( 'NONE',  ( 21.50062301572775780, 61.16842642911653627, 31.45420966082828329 ) ) ;
#23084 = DIRECTION ( 'NONE',  ( 0.000000000000000000, 0.000000000000000000, 1.000000000000000000 ) ) ;
#23085 = CARTESIAN_POINT ( 'NONE',  ( 71.25416588882602298, -72.55705569728901594, 540.9756252759101471 ) ) ;
#23086 = CARTESIAN_POINT ( 'NONE',  ( 111.6283393632454448, -28.07768985461828848, 59.68991099019693536 ) ) ;
#23088 = CARTESIAN_POINT ( 'NONE',  ( 101.7806060443209049, -45.68981339355057969, 158.1527681330539963 ) ) ;
#23087 = DIRECTION ( 'NONE',  ( 0.000000000000000000, 0.000000000000000000, -1.000000000000000000 ) ) ;
#23089 = FACE_BOUND ( 'NONE', #39946, .T. ) ;
#23090 = CARTESIAN_POINT ( 'NONE',  ( 51.24204729617298426, -31.76306994223730840, -5.074374724088000832 ) ) ;
#23091 = VERTEX_POINT ( 'NONE', #87294 ) ;
#23092 = AXIS2_PLACEMENT_3D ( 'NONE', #26285, #19024, #60342 ) ;
#23093 = CARTESIAN_POINT ( 'NONE',  ( 167.2371591254543262, -47.82818131005522844, 237.4678068554150059 ) ) ;
#23094 = EDGE_CURVE ( 'NONE', #67327, #2949, #2095, .T. ) ;
#23095 = CARTESIAN_POINT ( 'NONE',  ( 116.3176178399231873, -32.93748434060082531, 55.13562527591098217 ) ) ;
#23096 = ADVANCED_FACE ( 'NONE', ( #25058 ), #66837, .F. ) ;
#23097 = ORIENTED_EDGE ( 'NONE', *, *, #53013, .F. ) ;
#23098 = EDGE_CURVE ( 'NONE', #12422, #68005, #9496, .T. ) ;
#23099 = LINE ( 'NONE', #85324, #52000 ) ;
#23101 = VERTEX_POINT ( 'NONE', #35000 ) ;
#23100 = CARTESIAN_POINT ( 'NONE',  ( 109.6166107820099569, -26.53883167775938645, 199.8813395616249977 ) ) ;
#23102 = CARTESIAN_POINT ( 'NONE',  ( 179.4595971212720258, -26.00627455219131789, -5.074374724088000832 ) ) ;
#23103 = CARTESIAN_POINT ( 'NONE',  ( 116.6256809191353909, -40.94358996305180654, 249.4956252759109532 ) ) ;
#23104 = CARTESIAN_POINT ( 'NONE',  ( 101.4776230940428832, -27.87746311998561666, 106.5241967044819944 ) ) ;
#23105 = EDGE_CURVE ( 'NONE', #18949, #19900, #48169, .T. ) ;
#23106 = DIRECTION ( 'NONE',  ( 0.000000000000000000, -1.000000000000000000, 0.000000000000000000 ) ) ;
#23107 = CARTESIAN_POINT ( 'NONE',  ( 104.4880348644471724, -26.97933548612494903, 191.2814020040040930 ) ) ;
#23108 = CONICAL_SURFACE ( 'NONE', #21666, 82.41591158490093960, 0.7853981633974760346 ) ;
#23109 = CARTESIAN_POINT ( 'NONE',  ( 33.98325472291465132, 104.3431970271542042, -3.174999999999999822 ) ) ;
#23110 = VERTEX_POINT ( 'NONE', #69090 ) ;
#23111 = ORIENTED_EDGE ( 'NONE', *, *, #37857, .F. ) ;
#23112 = ORIENTED_EDGE ( 'NONE', *, *, #70006, .T. ) ;
#23113 = VERTEX_POINT ( 'NONE', #28642 ) ;
#23114 = DIRECTION ( 'NONE',  ( 0.000000000000000000, 0.000000000000000000, 1.000000000000000000 ) ) ;
#23115 = CARTESIAN_POINT ( 'NONE',  ( 96.91437895093065436, -34.20831442473366479, 272.1327681330538439 ) ) ;
#23116 = DIRECTION ( 'NONE',  ( 0.000000000000000000, 0.000000000000000000, -1.000000000000000000 ) ) ;
#23117 = CARTESIAN_POINT ( 'NONE',  ( 131.3165191078497855, -36.55813574389619447, 3.101427645695960411 ) ) ;
#23118 = CIRCLE ( 'NONE', #39028, 7.143750000000004263 ) ;
#23120 = CARTESIAN_POINT ( 'NONE',  ( 82.64146475440669803, 69.93366089391891194, 85.00925061401017047 ) ) ;
#23119 = DIRECTION ( 'NONE',  ( -0.7071067812160279908, 0.7071067811570671546, -2.899137802744091193E-29 ) ) ;
#23121 = DIRECTION ( 'NONE',  ( -0.000000000000000000, -1.000000000000000000, -0.000000000000000000 ) ) ;
#23122 = CARTESIAN_POINT ( 'NONE',  ( 113.9904334582008545, -30.89236017996071837, 223.7943245899819829 ) ) ;
#23123 = ORIENTED_EDGE ( 'NONE', *, *, #8384, .F. ) ;
#23124 = EDGE_LOOP ( 'NONE', ( #33266, #60870, #12317, #85954 ) ) ;
#23125 = CIRCLE ( 'NONE', #73851, 4.762500000000002842 ) ;
#23126 = EDGE_LOOP ( 'NONE', ( #72073, #33021 ) ) ;
#23127 = FACE_BOUND ( 'NONE', #39204, .T. ) ;
#23128 = CARTESIAN_POINT ( 'NONE',  ( 130.0664832912740110, -18.82844715994099971, 17.92562527591199739 ) ) ;
#23129 = CARTESIAN_POINT ( 'NONE',  ( 112.0124476237220676, -28.73397683645143275, 285.6356252759109680 ) ) ;
#23130 = LINE ( 'NONE', #63542, #15354 ) ;
#23131 = CIRCLE ( 'NONE', #73859, 81.91591158490091118 ) ;
#23132 = CARTESIAN_POINT ( 'NONE',  ( 116.9310496459149391, -33.53114825773884178, 130.0880062282909648 ) ) ;
#23133 =( GEOMETRIC_REPRESENTATION_CONTEXT ( 3 ) GLOBAL_UNCERTAINTY_ASSIGNED_CONTEXT ( ( #53528 ) ) GLOBAL_UNIT_ASSIGNED_CONTEXT ( ( #22403, #1958, #71007 ) ) REPRESENTATION_CONTEXT ( 'NONE', 'WORKASPACE' ) );
#23134 = CARTESIAN_POINT ( 'NONE',  ( 141.3509999999999991, 20.32000000000000028, 132.7150000000000034 ) ) ;
#23135 = EDGE_LOOP ( 'NONE', ( #25322, #61329 ) ) ;
#23136 = DIRECTION ( 'NONE',  ( -2.999999999999999839E-15, 1.000000000000000000, -2.999999999999999900E-30 ) ) ;
#23137 = DIRECTION ( 'NONE',  ( 1.000000000000000000, 0.000000000000000000, 0.000000000000000000 ) ) ;
#23138 = AXIS2_PLACEMENT_3D ( 'NONE', #167, #36032, #27868 ) ;
#23139 = ORIENTED_EDGE ( 'NONE', *, *, #69065, .F. ) ;
#23140 = DIRECTION ( 'NONE',  ( 0.000000000000000000, 1.000000000000000000, 0.000000000000000000 ) ) ;
#23141 = CARTESIAN_POINT ( 'NONE',  ( 116.0742395100671871, -34.51300936444170020, 11.83666179816295028 ) ) ;
#23142 = DIRECTION ( 'NONE',  ( 1.000000000000000000, 0.000000000000000000, 0.000000000000000000 ) ) ;
#23143 = EDGE_CURVE ( 'NONE', #66655, #6347, #61360, .T. ) ;
#23144 = EDGE_CURVE ( 'NONE', #88451, #79790, #75903, .T. ) ;
#23145 = CIRCLE ( 'NONE', #48656, 4.500000000000003553 ) ;
#23146 = DIRECTION ( 'NONE',  ( -0.8660254037844392627, 0.4999999999999990008, -1.549999999999999706E-14 ) ) ;
#23147 = VECTOR ( 'NONE', #18574, 1000.000000000000000 ) ;
#23148 = CARTESIAN_POINT ( 'NONE',  ( 117.0608701673778000, -38.08062519847543115, 194.7189615153010323 ) ) ;
#23149 = ORIENTED_EDGE ( 'NONE', *, *, #53149, .F. ) ;
#23150 = DIRECTION ( 'NONE',  ( 1.000000000000000000, 0.000000000000000000, 0.000000000000000000 ) ) ;
#23151 = EDGE_CURVE ( 'NONE', #54126, #56554, #20882, .T. ) ;
#23152 = DIRECTION ( 'NONE',  ( 0.000000000000000000, 1.000000000000000000, 0.000000000000000000 ) ) ;
#23153 = ORIENTED_EDGE ( 'NONE', *, *, #2221, .F. ) ;
#23154 = CARTESIAN_POINT ( 'NONE',  ( 107.2322097935746541, -25.67722466037449536, 80.07657765686299456 ) ) ;
#23155 = VERTEX_POINT ( 'NONE', #49064 ) ;
#23156 = CARTESIAN_POINT ( 'NONE',  ( 109.7746843348460857, -45.37110888865593239, 52.22861030426695095 ) ) ;
#23157 = EDGE_CURVE ( 'NONE', #57151, #48918, #32472, .T. ) ;
#23158 = CARTESIAN_POINT ( 'NONE',  ( 112.0396642006261629, -45.43305334282853636, 88.98868781504944536 ) ) ;
#23159 = CARTESIAN_POINT ( 'NONE',  ( 108.7386892141029477, -46.36620816325537930, 167.7127681330539701 ) ) ;
#23160 = DIRECTION ( 'NONE',  ( 0.7071067811865471286, 0.7071067811865479058, -2.102802400022911660E-16 ) ) ;
#23161 = EDGE_CURVE ( 'NONE', #70284, #24618, #27746, .T. ) ;
#23162 = DIRECTION ( 'NONE',  ( -0.000000000000000000, 1.000000000000000000, 0.000000000000000000 ) ) ;
#23163 = DIRECTION ( 'NONE',  ( 0.000000000000000000, 0.000000000000000000, -1.000000000000000000 ) ) ;
#23164 = AXIS2_PLACEMENT_3D ( 'NONE', #89826, #82569, #39848 ) ;
#23165 = CARTESIAN_POINT ( 'NONE',  ( 111.7933198282062364, -46.77516514641244783, 283.9146728949586418 ) ) ;
#23167 = ADVANCED_FACE ( 'NONE', ( #55429 ), #49518, .T. ) ;
#23166 = CARTESIAN_POINT ( 'NONE',  ( 183.5150000000000148, 52.73749999999999716, -26.11912895322935313 ) ) ;
#23168 = ORIENTED_EDGE ( 'NONE', *, *, #78750, .F. ) ;
#23169 = DIRECTION ( 'NONE',  ( 0.9834602067019604377, 0.1811243270069963496, 0.000000000000000000 ) ) ;
#23170 = EDGE_LOOP ( 'NONE', ( #12626, #71446, #68115, #67746, #19481 ) ) ;
#23171 = CARTESIAN_POINT ( 'NONE',  ( 112.1411864721344642, -47.49320580990715968, 133.9270538473399768 ) ) ;
#23172 = APPLICATION_CONTEXT ( 'automotive_design' ) ;
#23173 = FACE_OUTER_BOUND ( 'NONE', #43292, .T. ) ;
#23174 = VERTEX_POINT ( 'NONE', #40479 ) ;
#23175 = ORIENTED_EDGE ( 'NONE', *, *, #13406, .F. ) ;
#23176 = EDGE_CURVE ( 'NONE', #46082, #10162, #68196, .T. ) ;
#23177 = ORIENTED_EDGE ( 'NONE', *, *, #33739, .F. ) ;
#23179 = AXIS2_PLACEMENT_3D ( 'NONE', #83676, #20992, #48669 ) ;
#23178 = CYLINDRICAL_SURFACE ( 'NONE', #55041, 9.999999999999998224 ) ;
#23180 = FACE_OUTER_BOUND ( 'NONE', #74332, .T. ) ;
#23181 = CARTESIAN_POINT ( 'NONE',  ( 98.48461633480658861, -41.42146110206444121, 221.7241967044829494 ) ) ;
#23182 = DIRECTION ( 'NONE',  ( 0.000000000000000000, 0.000000000000000000, 1.000000000000000000 ) ) ;
#23183 = PLANE ( 'NONE',  #87265 ) ;
#23184 = CARTESIAN_POINT ( 'NONE',  ( 204.2160000000000082, 52.73749999999999716, -44.45000000000000284 ) ) ;
#23185 = CARTESIAN_POINT ( 'NONE',  ( 98.42378885047078541, -42.06819960529416136, 7.768006228291934434 ) ) ;
#23186 = EDGE_CURVE ( 'NONE', #15468, #71887, #83180, .T. ) ;
#23187 = CARTESIAN_POINT ( 'NONE',  ( 107.0667039024470313, -104.2784471599409528, 45.21780685541799727 ) ) ;
#23188 = ORIENTED_EDGE ( 'NONE', *, *, #44679, .F. ) ;
#23189 = CARTESIAN_POINT ( 'NONE',  ( 103.3374434664356869, -27.45071444193263588, 171.3805643286247573 ) ) ;
#23190 = CIRCLE ( 'NONE', #73920, 0.5000000000000004441 ) ;
#23191 = DIRECTION ( 'NONE',  ( 0.000000000000000000, 1.000000000000000000, 0.000000000000000000 ) ) ;
#23193 = ORIENTED_EDGE ( 'NONE', *, *, #36979, .F. ) ;
#23192 = EDGE_CURVE ( 'NONE', #42800, #89089, #57173, .T. ) ;
#23194 = VECTOR ( 'NONE', #28515, 1000.000000000000000 ) ;
#23195 = VECTOR ( 'NONE', #88727, 1000.000000000000000 ) ;
#23196 = DIRECTION ( 'NONE',  ( 1.000000000000000000, 0.000000000000000000, 0.000000000000000000 ) ) ;
#23197 = LINE ( 'NONE', #76787, #71610 ) ;
#23198 = CARTESIAN_POINT ( 'NONE',  ( 96.21411768969875311, -32.03111041547175120, 211.0013395616249738 ) ) ;
#23199 = FACE_BOUND ( 'NONE', #37981, .T. ) ;
#23200 = DIRECTION ( 'NONE',  ( -1.000000000000000000, -3.999999999999999995E-14, -1.000000000000000078E-15 ) ) ;
#23201 = CARTESIAN_POINT ( 'NONE',  ( 116.0662231142348162, -35.72080775710429634, 233.3257531614099776 ) ) ;
#23203 = CARTESIAN_POINT ( 'NONE',  ( 115.6551466294303054, -43.65033472170370032, 39.27467289495895386 ) ) ;
#23202 = CYLINDRICAL_SURFACE ( 'NONE', #5479, 0.2500000000000002220 ) ;
#23204 = CARTESIAN_POINT ( 'NONE',  ( 41.56648329127499153, -36.32844715994070839, 263.6756252759120116 ) ) ;
#23205 = CARTESIAN_POINT ( 'NONE',  ( 109.7815504499144339, -47.49240650911489325, 92.78514908543495210 ) ) ;
#23206 = ORIENTED_EDGE ( 'NONE', *, *, #71346, .F. ) ;
#23207 = CARTESIAN_POINT ( 'NONE',  ( 131.6545875264049528, -20.05177997654004685, 7.178113714829589043 ) ) ;
#23208 = VERTEX_POINT ( 'NONE', #49968 ) ;
#23209 = VECTOR ( 'NONE', #84276, 1000.000000000000000 ) ;
#23210 = DIRECTION ( 'NONE',  ( -1.000000000000000078E-15, 1.000000000000000083E-30, 1.000000000000000000 ) ) ;
#23211 = CARTESIAN_POINT ( 'NONE',  ( 103.2774390132985047, -27.47508908009983841, 276.3857178017252068 ) ) ;
#23212 = ORIENTED_EDGE ( 'NONE', *, *, #20870, .F. ) ;
#23213 = ADVANCED_FACE ( 'NONE', ( #77254 ), #43155, .F. ) ;
#23214 = PLANE ( 'NONE',  #28754 ) ;
#23215 = VERTEX_POINT ( 'NONE', #35905 ) ;
#23216 = LINE ( 'NONE', #57237, #75490 ) ;
#23217 = EDGE_CURVE ( 'NONE', #63602, #5603, #62578, .T. ) ;
#23218 = CYLINDRICAL_SURFACE ( 'NONE', #27307, 34.13125000000000142 ) ;
#23219 = DIRECTION ( 'NONE',  ( 1.000000000000000000, 4.163336342344333240E-14, 0.000000000000000000 ) ) ;
#23220 = ORIENTED_EDGE ( 'NONE', *, *, #77082, .T. ) ;
#23221 = CARTESIAN_POINT ( 'NONE',  ( 108.5410937779726623, -26.38672566707733225, 104.9641967044819779 ) ) ;
#23222 = AXIS2_PLACEMENT_3D ( 'NONE', #26001, #18733, #80987 ) ;
#23223 = LINE ( 'NONE', #10454, #69523 ) ;
#23224 = DIRECTION ( 'NONE',  ( 1.000000000000000000, 0.000000000000000000, 0.000000000000000000 ) ) ;
#23225 = CARTESIAN_POINT ( 'NONE',  ( -8.311122125636458691, 73.07069292649585179, 118.0642676351586573 ) ) ;
#23226 = EDGE_LOOP ( 'NONE', ( #78536, #3617, #35124, #43743 ) ) ;
#23227 = CIRCLE ( 'NONE', #13019, 1.000000000000000888 ) ;
#23228 = CARTESIAN_POINT ( 'NONE',  ( 1.387778780781445676E-14, 239.0000000000000000, 97.27542076772557778 ) ) ;
#23229 = CARTESIAN_POINT ( 'NONE',  ( 51.39690000000000225, 82.54999999999999716, 358.0130000000000337 ) ) ;
#23230 = CARTESIAN_POINT ( 'NONE',  ( 142.0664832912740394, -45.72944715994099596, 14.67562527591100441 ) ) ;
#23231 = EDGE_CURVE ( 'NONE', #26317, #11051, #16371, .T. ) ;
#23233 = CARTESIAN_POINT ( 'NONE',  ( 83.06670390244796920, -58.35344715994099829, 234.8338068554150198 ) ) ;
#23232 = DIRECTION ( 'NONE',  ( 0.000000000000000000, 0.000000000000000000, 1.000000000000000000 ) ) ;
#23234 = DIRECTION ( 'NONE',  ( 1.000000000000000078E-15, -1.000000000000000083E-30, -1.000000000000000000 ) ) ;
#23235 = VECTOR ( 'NONE', #40081, 1000.000000000000114 ) ;
#23236 = ADVANCED_FACE ( 'NONE', ( #58572 ), #22749, .F. ) ;
#23237 = ORIENTED_EDGE ( 'NONE', *, *, #81628, .T. ) ;
#23238 = CARTESIAN_POINT ( 'NONE',  ( -160.2664750769284865, 0.000000000000000000, 148.0533267522753818 ) ) ;
#23239 = CARTESIAN_POINT ( 'NONE',  ( 103.2204921605864314, -27.09891563476517717, 171.3908633711489813 ) ) ;
#23241 = ORIENTED_EDGE ( 'NONE', *, *, #39871, .T. ) ;
#23240 = DIRECTION ( 'NONE',  ( 0.000000000000000000, 1.000000000000000000, 0.000000000000000000 ) ) ;
#23242 = CIRCLE ( 'NONE', #56523, 2.749999999999974687 ) ;
#23243 = CARTESIAN_POINT ( 'NONE',  ( 116.7468388360763925, -38.12735696270775065, 24.71276813305395237 ) ) ;
#23244 = FACE_OUTER_BOUND ( 'NONE', #63403, .T. ) ;
#23245 = DIRECTION ( 'NONE',  ( -0.7071067811865249242, 0.7071067811865702213, -7.071067811865256424E-16 ) ) ;
#23246 = CARTESIAN_POINT ( 'NONE',  ( 115.7813681005709583, -41.80524612504061821, 13.40677487158930070 ) ) ;
#23247 = VECTOR ( 'NONE', #30239, 1000.000000000000000 ) ;
#23248 = LINE ( 'NONE', #84573, #12339 ) ;
#23249 = CARTESIAN_POINT ( 'NONE',  ( 101.2091419812964830, -45.28691980162484754, 242.1108633711499465 ) ) ;
#23250 = ORIENTED_EDGE ( 'NONE', *, *, #2758, .F. ) ;
#23251 = ORIENTED_EDGE ( 'NONE', *, *, #84781, .T. ) ;
#23252 = CARTESIAN_POINT ( 'NONE',  ( 107.5663136956459738, -46.11170142552477813, 194.0625356868489462 ) ) ;
#23253 = AXIS2_PLACEMENT_3D ( 'NONE', #9212, #8311, #2847 ) ;
#23254 = DIRECTION ( 'NONE',  ( 4.299999999999999979E-14, -1.000000000000000000, 4.400000000000000367E-29 ) ) ;
#23255 = CARTESIAN_POINT ( 'NONE',  ( 107.1760646772892756, -27.86850643495606406, 31.49872616304000417 ) ) ;
#23256 = CARTESIAN_POINT ( 'NONE',  ( 23.35554434807808022, 86.13711066444062681, 299.7470812929934709 ) ) ;
#23257 = EDGE_CURVE ( 'NONE', #57874, #69697, #41281, .T. ) ;
#23258 = EDGE_CURVE ( 'NONE', #52915, #83877, #1852, .T. ) ;
#23259 = DIRECTION ( 'NONE',  ( 1.000000000000000000, -9.073094938289460781E-13, 0.000000000000000000 ) ) ;
#23260 = AXIS2_PLACEMENT_3D ( 'NONE', #41440, #28264, #55959 ) ;
#23261 = DIRECTION ( 'NONE',  ( -0.000000000000000000, 1.000000000000000000, 0.000000000000000000 ) ) ;
#23262 = ORIENTED_EDGE ( 'NONE', *, *, #11256, .T. ) ;
#23263 = FACE_OUTER_BOUND ( 'NONE', #9995, .T. ) ;
#23264 = EDGE_CURVE ( 'NONE', #6675, #15555, #57233, .T. ) ;
#23265 = DIRECTION ( 'NONE',  ( -1.000000000000000000, -5.512527431108013646E-15, 0.000000000000000000 ) ) ;
#23266 = ORIENTED_EDGE ( 'NONE', *, *, #89696, .T. ) ;
#23267 = CARTESIAN_POINT ( 'NONE',  ( 100.2615012876617726, -45.41023301258256595, 277.0594347997204636 ) ) ;
#23268 = CARTESIAN_POINT ( 'NONE',  ( -254.0000000000000000, 3.174999999999999822, -41.27499999999999858 ) ) ;
#23269 = VERTEX_POINT ( 'NONE', #33114 ) ;
#23270 = EDGE_LOOP ( 'NONE', ( #16680, #88831 ) ) ;
#23271 = EDGE_CURVE ( 'NONE', #49742, #63793, #49978, .T. ) ;
#23272 = CARTESIAN_POINT ( 'NONE',  ( 116.3212776292269268, -32.94146857470660450, 84.13562527591095375 ) ) ;
#23273 = CARTESIAN_POINT ( 'NONE',  ( 41.56648329127399677, -18.82844715994099971, 321.0426252759119734 ) ) ;
#23274 = VECTOR ( 'NONE', #54419, 1000.000000000000000 ) ;
#23275 = CARTESIAN_POINT ( 'NONE',  ( 103.1875000000000000, 127.0000000000000000, 3.602774393244745134E-13 ) ) ;
#23276 = DIRECTION ( 'NONE',  ( -0.7071067811865483499, -0.7071067811865466846, -7.071067811865491110E-16 ) ) ;
#23277 = CARTESIAN_POINT ( 'NONE',  ( 101.7353989658871853, -28.52926574618699362, 21.53562527591096298 ) ) ;
#23278 = CARTESIAN_POINT ( 'NONE',  ( 12.60000000000000142, 82.54999999999999716, 117.6834004267381744 ) ) ;
#23279 = EDGE_CURVE ( 'NONE', #10350, #54390, #6480, .T. ) ;
#23280 = EDGE_LOOP ( 'NONE', ( #1782, #3226, #33373, #31312 ) ) ;
#23281 = CARTESIAN_POINT ( 'NONE',  ( 103.4621965996249600, -25.38836122657986394, 51.32133956162493149 ) ) ;
#23282 = DIRECTION ( 'NONE',  ( 2.108231265501709878E-16, 0.000000000000000000, -1.000000000000000000 ) ) ;
#23283 = CARTESIAN_POINT ( 'NONE',  ( 96.97860658150185031, -39.36037357437717787, 276.5299109901967540 ) ) ;
#23284 = ORIENTED_EDGE ( 'NONE', *, *, #80695, .F. ) ;
#23285 = EDGE_CURVE ( 'NONE', #56395, #28751, #57245, .T. ) ;
#23286 = LINE ( 'NONE', #78694, #81151 ) ;
#23287 = CARTESIAN_POINT ( 'NONE',  ( 109.6439838910708318, -46.47984676037744833, 18.78209685499881587 ) ) ;
#23288 = CARTESIAN_POINT ( 'NONE',  ( 46.03715912545348488, -48.62818131006090283, 129.9678068554150911 ) ) ;
#23289 = CARTESIAN_POINT ( 'NONE',  ( 104.8330862573783122, -27.72345643971313578, 88.08809036959192440 ) ) ;
#23290 = CARTESIAN_POINT ( 'NONE',  ( 104.4482647075962518, -26.61598136914473400, 196.2784824187679362 ) ) ;
#23291 = CYLINDRICAL_SURFACE ( 'NONE', #21757, 11.49999999999999645 ) ;
#23292 = VERTEX_POINT ( 'NONE', #39025 ) ;
#23293 = DIRECTION ( 'NONE',  ( 1.776356839400250465E-15, 0.000000000000000000, -1.000000000000000000 ) ) ;
#23294 = VECTOR ( 'NONE', #59514, 1000.000000000000000 ) ;
#23295 = ORIENTED_EDGE ( 'NONE', *, *, #67596, .F. ) ;
#23296 = ORIENTED_EDGE ( 'NONE', *, *, #64892, .T. ) ;
#23297 = FACE_BOUND ( 'NONE', #76435, .T. ) ;
#23298 = VERTEX_POINT ( 'NONE', #18587 ) ;
#23299 = VERTEX_POINT ( 'NONE', #17263 ) ;
#23300 = LINE ( 'NONE', #50965, #62820 ) ;
#23301 = CARTESIAN_POINT ( 'NONE',  ( 108.5087116869628545, -26.80026332916055765, 40.96182968949694470 ) ) ;
#23302 = CARTESIAN_POINT ( 'NONE',  ( 112.8135049847298461, -43.08742197748514968, 132.5838483995059676 ) ) ;
#23303 = CARTESIAN_POINT ( 'NONE',  ( 99.36516439250377175, -29.66998179773359823, 275.7356252759109907 ) ) ;
#23304 = VECTOR ( 'NONE', #42638, 1000.000000000000000 ) ;
#23305 = DIRECTION ( 'NONE',  ( 1.000000000000000078E-15, -1.000000000000000083E-30, -1.000000000000000000 ) ) ;
#23306 = EDGE_LOOP ( 'NONE', ( #52254, #28541 ) ) ;
#23307 = CARTESIAN_POINT ( 'NONE',  ( 103.2790308240917483, -27.47443741155154484, 136.3855809319543653 ) ) ;
#23308 = ORIENTED_EDGE ( 'NONE', *, *, #64663, .T. ) ;
#23309 = LINE ( 'NONE', #78717, #24709 ) ;
#23310 = CARTESIAN_POINT ( 'NONE',  ( 108.3323352706075582, -46.73498566967406731, 32.67742174073810446 ) ) ;
#23311 = ADVANCED_FACE ( 'NONE', ( #45383 ), #73103, .F. ) ;
#23312 = LINE ( 'NONE', #87301, #18549 ) ;
#23313 = CIRCLE ( 'NONE', #59507, 2.117000000000007987 ) ;
#23314 = LINE ( 'NONE', #77353, #16143 ) ;
#23315 = ORIENTED_EDGE ( 'NONE', *, *, #85399, .T. ) ;
#23316 = CARTESIAN_POINT ( 'NONE',  ( 99.33304576907053729, -28.83178728225833609, 270.7051490854348685 ) ) ;
#23317 = CARTESIAN_POINT ( 'NONE',  ( 100.5706289694924607, -28.47478668554837000, 11.60705384733995515 ) ) ;
#23318 = CARTESIAN_POINT ( 'NONE',  ( 99.04406185220089753, -42.84125763159654099, 117.8439586084165285 ) ) ;
#23319 = B_SPLINE_CURVE_WITH_KNOTS ( 'NONE', 3,
 ( #27167, #5387, #69407, #33086, #7182, #67608, #20366, #74876, #6723, #89863, #55295, #60784, #88518, #806, #15789, #70752, #8526, #2607 ),
 .UNSPECIFIED., .F., .F.,
 ( 4, 2, 2, 2, 2, 2, 2, 2, 4 ),
 ( 0.000000000000000000, 0.06249843091306516579, 0.1249968618261303316, 0.1874952927391954904, 0.2499937236522606632, 0.3124921545653258081, 0.3749905854783909809, 0.4374890163914561536, 0.4999874473045213263 ),
 .UNSPECIFIED. ) ;
#23321 = CARTESIAN_POINT ( 'NONE',  ( 68.80903792918766726, -139.1904132598590422, 246.4625416178163562 ) ) ;
#23320 = DIRECTION ( 'NONE',  ( -0.7071067811865463515, -0.7071067811865487940, 0.000000000000000000 ) ) ;
#23322 = DIRECTION ( 'NONE',  ( 0.000000000000000000, 0.000000000000000000, -1.000000000000000000 ) ) ;
#23323 = CARTESIAN_POINT ( 'NONE',  ( 107.0664832912739399, -36.72944715994095333, 293.1356252759106837 ) ) ;
#23324 = DIRECTION ( 'NONE',  ( -6.524622321627019585E-16, -4.013151879589939944E-16, -1.000000000000000000 ) ) ;
#23325 = AXIS2_PLACEMENT_3D ( 'NONE', #32182, #4498, #72649 ) ;
#23326 = DIRECTION ( 'NONE',  ( 0.000000000000000000, 0.000000000000000000, 1.000000000000000000 ) ) ;
#23327 = FACE_OUTER_BOUND ( 'NONE', #73708, .T. ) ;
#23328 = CARTESIAN_POINT ( 'NONE',  ( 143.0664832912740110, -8.729447159940999512, 17.92562527591199739 ) ) ;
#23329 = CARTESIAN_POINT ( 'NONE',  ( 136.8164806451553659, -36.72944715939129168, 6.749772901088312516 ) ) ;
#23330 = CARTESIAN_POINT ( 'NONE',  ( 100.2327115992702176, -45.44695862323239055, 277.0594347997204068 ) ) ;
#23331 = CARTESIAN_POINT ( 'NONE',  ( 116.7952044851831488, -40.57305441194377948, 189.5270538473389479 ) ) ;
#23332 = CARTESIAN_POINT ( 'NONE',  ( 100.4515265478786574, -44.84261285976553779, 8.032768133053981074 ) ) ;
#23333 = AXIS2_PLACEMENT_3D ( 'NONE', #34220, #4739, #20609 ) ;
#23335 = CARTESIAN_POINT ( 'NONE',  ( 19.56670390244734747, -25.42844715994192129, 300.4678068554150059 ) ) ;
#23334 = LINE ( 'NONE', #51000, #43556 ) ;
#23336 = CARTESIAN_POINT ( 'NONE',  ( 80.94673009889058335, -34.12360705087682788, 1.744847597651331572 ) ) ;
#23337 = EDGE_CURVE ( 'NONE', #85061, #31872, #44944, .T. ) ;
#23338 = EDGE_LOOP ( 'NONE', ( #89717, #14738 ) ) ;
#23339 = FACE_OUTER_BOUND ( 'NONE', #17451, .T. ) ;
#23340 = ORIENTED_EDGE ( 'NONE', *, *, #20417, .F. ) ;
#23341 = CIRCLE ( 'NONE', #34911, 17.00000000000000000 ) ;
#23342 = CARTESIAN_POINT ( 'NONE',  ( 97.35459460924926134, -38.14118110200429612, 62.44133956162495025 ) ) ;
#23344 = ORIENTED_EDGE ( 'NONE', *, *, #84795, .F. ) ;
#23343 = CARTESIAN_POINT ( 'NONE',  ( -48.02966122971776741, 91.07499999999996021, 74.26049396966043048 ) ) ;
#23345 = VECTOR ( 'NONE', #34689, 1000.000000000000114 ) ;
#23346 = CARTESIAN_POINT ( 'NONE',  ( 63.03715912545729338, -24.42818131006027826, 313.9678068554150059 ) ) ;
#23347 = CARTESIAN_POINT ( 'NONE',  ( 107.6532706963292441, -47.74396045468172645, 193.6308633711489620 ) ) ;
#23348 = LINE ( 'NONE', #29687, #20783 ) ;
#23349 = CARTESIAN_POINT ( 'NONE',  ( 107.0664832912749915, -36.72944715993903486, 25.56312527591096995 ) ) ;
#23350 = DIRECTION ( 'NONE',  ( -1.000000000000000078E-15, 0.000000000000000000, -1.000000000000000000 ) ) ;
#23351 = DIRECTION ( 'NONE',  ( -1.000000000000000078E-15, 1.000000000000000083E-30, 1.000000000000000000 ) ) ;
#23352 = PLANE ( 'NONE',  #60725 ) ;
#23353 = CARTESIAN_POINT ( 'NONE',  ( 111.0847094670297110, -45.88713190444605772, 97.90550790398889092 ) ) ;
#23354 = CARTESIAN_POINT ( 'NONE',  ( 98.98846131648976154, -42.30253745798197684, 126.8070538473399580 ) ) ;
#23355 = ORIENTED_EDGE ( 'NONE', *, *, #77383, .F. ) ;
#23356 = ORIENTED_EDGE ( 'NONE', *, *, #61112, .F. ) ;
#23357 = CARTESIAN_POINT ( 'NONE',  ( 115.6007127221643032, -39.11591036577164004, 95.04158330589696391 ) ) ;
#23358 = VECTOR ( 'NONE', #61437, 1000.000000000000000 ) ;
#23359 = DIRECTION ( 'NONE',  ( 0.7071067811865451302, 0.7071067811865500152, -0.000000000000000000 ) ) ;
#23361 = DIRECTION ( 'NONE',  ( 0.000000000000000000, -1.000000000000000000, 0.000000000000000000 ) ) ;
#23360 = CARTESIAN_POINT ( 'NONE',  ( 97.71246005893831921, -41.20616857227587815, 212.6937205140059461 ) ) ;
#23362 = CARTESIAN_POINT ( 'NONE',  ( -48.02966122971775320, 100.5999999999999659, -8.747637655308301746E-15 ) ) ;
#23363 = CARTESIAN_POINT ( 'NONE',  ( 21.03715912545739641, -47.82818131006197149, 180.4678068554150911 ) ) ;
#23364 = EDGE_CURVE ( 'NONE', #28401, #14757, #32529, .T. ) ;
#23365 = DIRECTION ( 'NONE',  ( 0.000000000000000000, 0.000000000000000000, -1.000000000000000000 ) ) ;
#23366 = CARTESIAN_POINT ( 'NONE',  ( -451.6120000000000232, 53.97500000000000142, -3.174999999999999822 ) ) ;
#23367 = EDGE_CURVE ( 'NONE', #12231, #12481, #12230, .T. ) ;
#23368 = CARTESIAN_POINT ( 'NONE',  ( -72.96458098368751166, 127.0000000000000000, 72.96458098368620426 ) ) ;
#23369 = CARTESIAN_POINT ( 'NONE',  ( 114.1602155298370036, -45.17592836263241196, 148.1203871806719405 ) ) ;
#23370 = EDGE_CURVE ( 'NONE', #23101, #45090, #87666, .T. ) ;
#23371 = ORIENTED_EDGE ( 'NONE', *, *, #75361, .F. ) ;
#23372 = ORIENTED_EDGE ( 'NONE', *, *, #83865, .F. ) ;
#23373 = VECTOR ( 'NONE', #31679, 1000.000000000000000 ) ;
#23374 = ADVANCED_FACE ( 'NONE', ( #74003 ), #31316, .F. ) ;
#23375 = CARTESIAN_POINT ( 'NONE',  ( 172.5664832912729878, -27.82844715994070484, 78.92562527591199739 ) ) ;
#23376 = CARTESIAN_POINT ( 'NONE',  ( 77.44501272126919389, -17.89730640218066426, 2.921034946746040806 ) ) ;
#23377 = LINE ( 'NONE', #17866, #53708 ) ;
#23378 = DIRECTION ( 'NONE',  ( 0.7071067708032332533, 0.0001211784769705727632, 0.7071067811865479058 ) ) ;
#23379 = CARTESIAN_POINT ( 'NONE',  ( 108.8441613132982155, -28.76266695291210951, 222.7195189410199703 ) ) ;
#23380 = VECTOR ( 'NONE', #16712, 1000.000000000000000 ) ;
#23381 = CARTESIAN_POINT ( 'NONE',  ( 142.0664832912739541, -9.729447159941033263, -4.970821333495754502 ) ) ;
#23382 = CARTESIAN_POINT ( 'NONE',  ( 98.43480628652092435, -29.82486610537253569, 195.7775300378159784 ) ) ;
#23383 = LINE ( 'NONE', #51051, #41684 ) ;
#23384 = VERTEX_POINT ( 'NONE', #4067 ) ;
#23386 = VERTEX_POINT ( 'NONE', #25401 ) ;
#23385 = ORIENTED_EDGE ( 'NONE', *, *, #50273, .T. ) ;
#23387 = EDGE_CURVE ( 'NONE', #20562, #67881, #87639, .T. ) ;
#23388 = AXIS2_PLACEMENT_3D ( 'NONE', #40687, #54288, #82052 ) ;
#23389 = DIRECTION ( 'NONE',  ( -0.7071067811865753283, 0.7071067811865197061, -7.071067811865760309E-16 ) ) ;
#23390 = ORIENTED_EDGE ( 'NONE', *, *, #45794, .F. ) ;
#23391 = CARTESIAN_POINT ( 'NONE',  ( 97.81469011401388514, -40.51612824417846070, 136.6360017533206417 ) ) ;
#23392 = CARTESIAN_POINT ( 'NONE',  ( 131.4524275574070771, -35.85322059724929034, 6.943211687812413935 ) ) ;
#23393 = AXIS2_PLACEMENT_3D ( 'NONE', #57572, #78498, #16258 ) ;
#23394 = CARTESIAN_POINT ( 'NONE',  ( 111.0382984267975246, -28.80776997321336097, 276.1387261630399621 ) ) ;
#23395 = DIRECTION ( 'NONE',  ( 1.000000000000000000, 0.000000000000000000, 1.047445008332813989E-14 ) ) ;
#23396 = EDGE_LOOP ( 'NONE', ( #80519, #77804, #83632, #89183 ) ) ;
#23397 = CARTESIAN_POINT ( 'NONE',  ( 115.0808484473774485, -41.07790926377064267, 9.635625275910941312 ) ) ;
#23398 = FACE_OUTER_BOUND ( 'NONE', #24932, .T. ) ;
#23399 = VERTEX_POINT ( 'NONE', #31768 ) ;
#23400 = ORIENTED_EDGE ( 'NONE', *, *, #89800, .F. ) ;
#23401 = CARTESIAN_POINT ( 'NONE',  ( -194.1576000000000022, 0.000000000000000000, -45.33899999999999864 ) ) ;
#23402 = VERTEX_POINT ( 'NONE', #59012 ) ;
#23403 = ORIENTED_EDGE ( 'NONE', *, *, #4920, .T. ) ;
#23404 = CARTESIAN_POINT ( 'NONE',  ( 111.2703484347609333, -28.70728902343469002, 14.10289601855296837 ) ) ;
#23405 = CARTESIAN_POINT ( 'NONE',  ( 114.9818473740405835, -29.91084206771912690, 184.3927681330539770 ) ) ;
#23406 = AXIS2_PLACEMENT_3D ( 'NONE', #48196, #22316, #70921 ) ;
#23407 = CARTESIAN_POINT ( 'NONE',  ( 114.4965984691701664, -29.44205611023136626, 149.4441967044819819 ) ) ;
#23408 = CARTESIAN_POINT ( 'NONE',  ( 64.67079002020508938, -0.9301828534102468682, 394.9756252759101471 ) ) ;
#23409 = CARTESIAN_POINT ( 'NONE',  ( 104.8412801004068058, -26.50840007386317509, 256.2470538473397141 ) ) ;
#23410 = CARTESIAN_POINT ( 'NONE',  ( 117.0718565137653968, -35.46215913205921311, 99.92773310503083906 ) ) ;
#23411 = CARTESIAN_POINT ( 'NONE',  ( 44.45000000000000284, 66.67499999999999716, 288.9250000000000114 ) ) ;
#23412 = CARTESIAN_POINT ( 'NONE',  ( -130.0575199856854169, 76.93632333215535368, -11.39952500586003836 ) ) ;
#23413 = VERTEX_POINT ( 'NONE', #39479 ) ;
#23414 = ORIENTED_EDGE ( 'NONE', *, *, #51318, .T. ) ;
#23415 = AXIS2_PLACEMENT_3D ( 'NONE', #61881, #42768, #55949 ) ;
#23416 = EDGE_CURVE ( 'NONE', #37218, #69459, #60080, .T. ) ;
#23417 = AXIS2_PLACEMENT_3D ( 'NONE', #45354, #17675, #73074 ) ;
#23418 = CARTESIAN_POINT ( 'NONE',  ( 107.5678864575881590, -47.81824684668375625, 192.6003871806729535 ) ) ;
#23419 = ORIENTED_EDGE ( 'NONE', *, *, #36368, .T. ) ;
#23420 = CARTESIAN_POINT ( 'NONE',  ( 114.2535261088984981, -44.28147934099003180, 158.1813395616249807 ) ) ;
#23421 = DIRECTION ( 'NONE',  ( 0.02150753337723812844, 0.0009076677972192511400, 0.9997682742251809973 ) ) ;
#23422 = EDGE_CURVE ( 'NONE', #12231, #2137, #86751, .T. ) ;
#23423 = CARTESIAN_POINT ( 'NONE',  ( 136.4578062354202359, -35.36823420008745700, 7.200493380652632780 ) ) ;
#23424 = CARTESIAN_POINT ( 'NONE',  ( 48.45959712128975383, -28.98061976758959801, 117.4678068554150485 ) ) ;
#23427 = CARTESIAN_POINT ( 'NONE',  ( 97.63514171170974976, -41.12017164899855715, 252.6727681330536655 ) ) ;
#23426 = CARTESIAN_POINT ( 'NONE',  ( 80.06648329127399677, 0.2215528400590013880, 308.6356252759119911 ) ) ;
#23425 = LINE ( 'NONE', #17477, #88270 ) ;
#23428 = PLANE ( 'NONE',  #55297 ) ;
#23429 = CARTESIAN_POINT ( 'NONE',  ( 144.4532657278588204, -72.54451140298851897, 540.9756252759101471 ) ) ;
#23430 = FACE_OUTER_BOUND ( 'NONE', #61624, .T. ) ;
#23431 = DIRECTION ( 'NONE',  ( -1.000000000000000000, -4.299999999999999979E-14, -1.000000000000000078E-15 ) ) ;
#23432 = CARTESIAN_POINT ( 'NONE',  ( 108.3334481168079435, -46.73485935100409705, 258.6772919443159253 ) ) ;
#23433 = CARTESIAN_POINT ( 'NONE',  ( 172.5664832912740110, -32.07844715994070839, 78.92562527591199739 ) ) ;
#23434 = AXIS2_PLACEMENT_3D ( 'NONE', #27907, #55137, #14749 ) ;
#23436 = VERTEX_POINT ( 'NONE', #60355 ) ;
#23435 = CARTESIAN_POINT ( 'NONE',  ( 112.8728595368667698, -42.45837713832621318, 195.5838068554166966 ) ) ;
#23437 = DIRECTION ( 'NONE',  ( 0.000000000000000000, 1.000000000000000000, 0.000000000000000000 ) ) ;
#23438 = CARTESIAN_POINT ( 'NONE',  ( 106.4823715260129688, -24.86804634255730662, 195.1156252759109861 ) ) ;
#23439 = CARTESIAN_POINT ( 'NONE',  ( 101.0662023700742935, -27.44663458233410935, 66.54514908543495721 ) ) ;
#23440 = CARTESIAN_POINT ( 'NONE',  ( 116.8358708857152095, -40.58912082693117185, 189.5270538473389479 ) ) ;
#23441 = CARTESIAN_POINT ( 'NONE',  ( -187.8075999999999794, 20.32000000000000028, -9.525000000000000355 ) ) ;
#23442 = LINE ( 'NONE', #35696, #27217 ) ;
#23444 = DIRECTION ( 'NONE',  ( -1.000000000000000078E-15, 1.000000000000000000, -3.100000000000000044E-14 ) ) ;
#23443 = CARTESIAN_POINT ( 'NONE',  ( 116.3212776292296127, -32.94146857471318413, 287.6356252759109680 ) ) ;
#23445 = CARTESIAN_POINT ( 'NONE',  ( 164.7830935719630361, -29.99615139349950965, -5.074374724088000832 ) ) ;
#23446 = DIRECTION ( 'NONE',  ( 0.000000000000000000, 0.000000000000000000, -1.000000000000000000 ) ) ;
#23447 = VERTEX_POINT ( 'NONE', #80838 ) ;
#23448 = AXIS2_PLACEMENT_3D ( 'NONE', #53311, #46953, #39702 ) ;
#23449 = LINE ( 'NONE', #37944, #45613 ) ;
#23450 = EDGE_CURVE ( 'NONE', #67268, #25932, #55954, .T. ) ;
#23451 = ORIENTED_EDGE ( 'NONE', *, *, #82732, .T. ) ;
#23452 = ORIENTED_EDGE ( 'NONE', *, *, #53586, .T. ) ;
#23453 = CARTESIAN_POINT ( 'NONE',  ( 103.9030524752275397, -44.69467205304180624, 116.6981341137909567 ) ) ;
#23455 = ORIENTED_EDGE ( 'NONE', *, *, #29044, .T. ) ;
#23454 = CARTESIAN_POINT ( 'NONE',  ( -3.291704278000410433, 94.82304653311918230, -130.5151038487541655 ) ) ;
#23456 = CARTESIAN_POINT ( 'NONE',  ( 115.1498815335950638, -43.27828968249928465, 84.28419670448195689 ) ) ;
#23457 = LINE ( 'NONE', #64330, #61359 ) ;
#23458 = AXIS2_PLACEMENT_3D ( 'NONE', #36139, #1177, #57015 ) ;
#23459 = LINE ( 'NONE', #17945, #47129 ) ;
#23460 = DIRECTION ( 'NONE',  ( 1.000000000000000078E-15, 1.000000000000000083E-30, -1.000000000000000000 ) ) ;
#23461 = CARTESIAN_POINT ( 'NONE',  ( 110.8778723976570433, -46.37372517399798255, 22.88800622829195675 ) ) ;
#23462 = ORIENTED_EDGE ( 'NONE', *, *, #62623, .T. ) ;
#23463 = ORIENTED_EDGE ( 'NONE', *, *, #4713, .F. ) ;
#23464 = VERTEX_POINT ( 'NONE', #19938 ) ;
#23465 = FACE_OUTER_BOUND ( 'NONE', #21115, .T. ) ;
#23466 = CARTESIAN_POINT ( 'NONE',  ( 193.0371591254583734, -47.82818131005421947, 313.9678068554149490 ) ) ;
#23467 = CARTESIAN_POINT ( 'NONE',  ( 109.7248659245813656, -27.00080518071327162, 115.8647919423142696 ) ) ;
#23468 = CARTESIAN_POINT ( 'NONE',  ( 71.25416588882602298, -72.55705569728901594, 540.9756252759101471 ) ) ;
#23469 = CARTESIAN_POINT ( 'NONE',  ( -29.99999999999998224, 172.0000000000000000, 113.8826257785461280 ) ) ;
#23470 = CARTESIAN_POINT ( 'NONE',  ( 97.07208927141411436, -35.37826970552124095, 52.21955069277615991 ) ) ;
#23471 = CARTESIAN_POINT ( 'NONE',  ( -46.60773131249376178, 91.07499999999996021, -44.42500552774628630 ) ) ;
#23472 = CIRCLE ( 'NONE', #19087, 11.45913725231036118 ) ;
#23473 = CARTESIAN_POINT ( 'NONE',  ( 80.04418453221538243, 94.12556101775334128, 87.45628510944696643 ) ) ;
#23474 = CARTESIAN_POINT ( 'NONE',  ( 112.9508454419806043, -28.15023113465287352, 44.59848241876795782 ) ) ;
#23475 = EDGE_CURVE ( 'NONE', #78082, #59268, #28076, .T. ) ;
#23476 = EDGE_LOOP ( 'NONE', ( #11486, #56170, #22375, #89635, #436, #39513, #34399, #24286, #72619, #41340, #34078, #68723, #23251, #28253, #13888 ) ) ;
#23477 = DIRECTION ( 'NONE',  ( 0.8660254037844387076, 0.4999999999999998890, 0.000000000000000000 ) ) ;
#23478 = B_SPLINE_CURVE_WITH_KNOTS ( 'NONE', 3,
 ( #45018, #65481, #10077, #79128, #1924, #37782, #8747, #10515, #31393, #23287, #44121, #3267, #70975, #30958, #72746, #43685, #9624, #65036, #64592, #38220, #3700, #59090, #78695, #58645, #2819, #2374, #24594 ),
 .UNSPECIFIED., .F., .F.,
 ( 4, 2, 2, 2, 2, 2, 2, 2, 2, 2, 1, 1, 1, 2, 4 ),
 ( 0.000000000000000000, 0.06250761762232094620, 0.1250152352446418924, 0.1875228528669628247, 0.2500304704892837848, 0.3125380881116047727, 0.3750457057339256495, 0.4375533233562466373, 0.4688071321674068814, 0.4844340365729870035, 0.4922474887757767870, 0.4961542148771715399, 0.4981075779278690274, 0.4990842594532179377, 0.5000609409785667925 ),
 .UNSPECIFIED. ) ;
#23479 = AXIS2_PLACEMENT_3D ( 'NONE', #69995, #85443, #15493 ) ;
#23480 = CYLINDRICAL_SURFACE ( 'NONE', #20620, 118.5560000000000116 ) ;
#23481 = CARTESIAN_POINT ( 'NONE',  ( 103.6457284375485131, -44.67924975648479347, 135.0833284648299752 ) ) ;
#23482 = B_SPLINE_CURVE_WITH_KNOTS ( 'NONE', 3,
 ( #19370, #74779, #34329, #39789, #40245, #33439, #61143, #54299, #82066, #62929, #36594, #16149, #69762, #63846, #35676, #70206, #42923, #1629 ),
 .UNSPECIFIED., .F., .F.,
 ( 4, 2, 2, 2, 2, 2, 2, 2, 4 ),
 ( 0.000000000000000000, 0.06249998643239338542, 0.1249999728647867708, 0.1874999592971801632, 0.2499999457295735417, 0.3124999321619669201, 0.3749999185943603264, 0.4374999050267536771, 0.4999998914591470833 ),
 .UNSPECIFIED. ) ;
#23483 = VECTOR ( 'NONE', #7071, 1000.000000000000000 ) ;
#23484 = CARTESIAN_POINT ( 'NONE',  ( 102.0647649218796289, -27.97183332977936132, 95.49000569952723083 ) ) ;
#23485 = DIRECTION ( 'NONE',  ( -3.999999999999999995E-14, 1.000000000000000000, -4.100000000000000342E-29 ) ) ;
#23486 = ORIENTED_EDGE ( 'NONE', *, *, #20308, .T. ) ;
#23487 = ORIENTED_EDGE ( 'NONE', *, *, #77936, .F. ) ;
#23488 = ADVANCED_FACE ( 'NONE', ( #48065 ), #51394, .T. ) ;
#23489 = CARTESIAN_POINT ( 'NONE',  ( 98.54782867203449825, -41.97726770183525957, 136.7656906696263093 ) ) ;
#23490 = ORIENTED_EDGE ( 'NONE', *, *, #33998, .F. ) ;
#23491 = ORIENTED_EDGE ( 'NONE', *, *, #25292, .T. ) ;
#23492 = ADVANCED_FACE ( 'NONE', ( #34896 ), #27193, .F. ) ;
#23493 = VECTOR ( 'NONE', #18749, 1000.000000000000000 ) ;
#23494 = CARTESIAN_POINT ( 'NONE',  ( 98.87114546532168902, -41.32433164768560374, 178.1768214011349585 ) ) ;
#23495 = FACE_OUTER_BOUND ( 'NONE', #45661, .T. ) ;
#23496 = CARTESIAN_POINT ( 'NONE',  ( 102.2923668651898339, -27.39740514546159389, 116.4527681330539650 ) ) ;
#23497 = CARTESIAN_POINT ( 'NONE',  ( 48.16670390244496502, -26.71338133339251542, 342.9256252759109884 ) ) ;
#23498 = AXIS2_PLACEMENT_3D ( 'NONE', #22421, #41933, #29232 ) ;
#23499 = CARTESIAN_POINT ( 'NONE',  ( 116.5679076829705707, -33.54432202151119924, 19.08379224916496497 ) ) ;
#23500 = ORIENTED_EDGE ( 'NONE', *, *, #8384, .T. ) ;
#23501 = AXIS2_PLACEMENT_3D ( 'NONE', #80502, #60021, #11454 ) ;
#23502 = ORIENTED_EDGE ( 'NONE', *, *, #49056, .T. ) ;
#23503 = ORIENTED_EDGE ( 'NONE', *, *, #26301, .F. ) ;
#23504 = CIRCLE ( 'NONE', #48095, 3.300000000000000711 ) ;
#23505 = CARTESIAN_POINT ( 'NONE',  ( 99.90434330870786539, -40.64524553156628173, 219.5423760838769738 ) ) ;
#23506 = CARTESIAN_POINT ( 'NONE',  ( 113.5198117145332475, -28.51355303769357619, 79.54705384733995288 ) ) ;
#23507 = ORIENTED_EDGE ( 'NONE', *, *, #57918, .T. ) ;
#23508 = CARTESIAN_POINT ( 'NONE',  ( 118.0600790064084293, -37.62648441163795354, 38.77372051400595865 ) ) ;
#23509 = CARTESIAN_POINT ( 'NONE',  ( 112.4324277152178837, -28.68226574489724001, 249.5838068554168956 ) ) ;
#23510 = CARTESIAN_POINT ( 'NONE',  ( 130.0664832912740110, -18.72922654876706972, 284.9256252759119548 ) ) ;
#23511 = CARTESIAN_POINT ( 'NONE',  ( 70.63919639214310564, 65.60000000000000853, 0.000000000000000000 ) ) ;
#23512 = CARTESIAN_POINT ( 'NONE',  ( 97.98655846647217516, -41.85169789442448263, 132.7356252759109623 ) ) ;
#23513 = CIRCLE ( 'NONE', #36607, 27.99999999999999645 ) ;
#23514 = CARTESIAN_POINT ( 'NONE',  ( 123.0079629938350223, -38.09664315643626509, 302.4856252759109907 ) ) ;
#23515 = ORIENTED_EDGE ( 'NONE', *, *, #1668, .T. ) ;
#23516 = CARTESIAN_POINT ( 'NONE',  ( 213.1962561210690126, 52.73749999999999716, -41.27499999999999858 ) ) ;
#23517 = VECTOR ( 'NONE', #9849, 1000.000000000000000 ) ;
#23518 = ORIENTED_EDGE ( 'NONE', *, *, #45338, .T. ) ;
#23519 = CARTESIAN_POINT ( 'NONE',  ( 193.0371591254583450, -47.82818131005411999, 249.9678068554149775 ) ) ;
#23520 = CARTESIAN_POINT ( 'NONE',  ( 0.000000000000000000, 49.07499999999999574, 0.000000000000000000 ) ) ;
#23521 = ORIENTED_EDGE ( 'NONE', *, *, #19541, .T. ) ;
#23522 = FACE_OUTER_BOUND ( 'NONE', #6594, .T. ) ;
#23523 = CARTESIAN_POINT ( 'NONE',  ( 103.1466689443337117, -27.50432134387084560, 131.3959253572286627 ) ) ;
#23524 = CARTESIAN_POINT ( 'NONE',  ( 96.92094985624760284, -32.34227964863599425, 61.01372051400599616 ) ) ;
#23525 = LINE ( 'NONE', #16693, #2577 ) ;
#23526 = EDGE_CURVE ( 'NONE', #65464, #83730, #55761, .T. ) ;
#23527 = DIRECTION ( 'NONE',  ( 0.000000000000000000, -1.000000000000000000, 0.000000000000000000 ) ) ;
#23528 = DIRECTION ( 'NONE',  ( 1.000000000000000000, 1.000000000000000078E-15, 0.000000000000000000 ) ) ;
#23529 = CARTESIAN_POINT ( 'NONE',  ( 116.1466984671188385, -33.09446055034462120, 54.12991099019798469 ) ) ;
#23531 = CARTESIAN_POINT ( 'NONE',  ( 108.5866130067098254, -47.05677245125736619, 138.6927681330539883 ) ) ;
#23530 = CARTESIAN_POINT ( 'NONE',  ( 72.31648329127402519, -45.62589376934781882, -5.074374724089063982 ) ) ;
#23532 = DIRECTION ( 'NONE',  ( 1.000000000000000000, 4.163336342344333240E-14, 0.000000000000000000 ) ) ;
#23533 = CARTESIAN_POINT ( 'NONE',  ( 165.9667039024473922, -26.71338133338714016, 313.9678068554149490 ) ) ;
#23534 = ORIENTED_EDGE ( 'NONE', *, *, #84995, .T. ) ;
#23535 = DIRECTION ( 'NONE',  ( 1.000000000000000000, 0.000000000000000000, 2.108231265501709878E-16 ) ) ;
#23536 = CARTESIAN_POINT ( 'NONE',  ( 70.63919639214310564, 49.07499999999999574, -53.97512327982435210 ) ) ;
#23537 = CARTESIAN_POINT ( 'NONE',  ( 144.0667052733537901, -71.37844715994090450, 55.21780685541800437 ) ) ;
#23538 = CARTESIAN_POINT ( 'NONE',  ( 59.56670390244700997, -79.67844715994098692, 85.21780685541799016 ) ) ;
#23540 = EDGE_LOOP ( 'NONE', ( #78974, #24488, #74105, #1724 ) ) ;
#23539 = CARTESIAN_POINT ( 'NONE',  ( 115.4232488078209258, -30.42301107085752321, 219.3413395616249773 ) ) ;
#23541 = CARTESIAN_POINT ( 'NONE',  ( 98.34968923854172829, -31.65687136160358506, 145.9064846611762505 ) ) ;
#23542 = CARTESIAN_POINT ( 'NONE',  ( 116.9053397700284478, -41.81689336946376301, 239.4346728949589647 ) ) ;
#23543 = CARTESIAN_POINT ( 'NONE',  ( 109.6947933286257353, -47.51320739032397000, 83.75467289495897205 ) ) ;
#23544 = CARTESIAN_POINT ( 'NONE',  ( 82.89895571708159139, 81.72130195885951309, 100.8594679592221155 ) ) ;
#23545 = CARTESIAN_POINT ( 'NONE',  ( -3.174999999999644995, 104.3431970271541616, -33.98325472291465132 ) ) ;
#23546 = CARTESIAN_POINT ( 'NONE',  ( 104.4076956878168261, -46.45797032905074531, 263.3648843889448585 ) ) ;
#23547 = ORIENTED_EDGE ( 'NONE', *, *, #69307, .T. ) ;
#23548 = ADVANCED_FACE ( 'NONE', ( #14012 ), #83077, .T. ) ;
#23549 = ORIENTED_EDGE ( 'NONE', *, *, #35839, .T. ) ;
#23550 = VERTEX_POINT ( 'NONE', #21277 ) ;
#23551 = ADVANCED_FACE ( 'NONE', ( #42150 ), #68981, .F. ) ;
#23552 = VERTEX_POINT ( 'NONE', #81736 ) ;
#23553 = DIRECTION ( 'NONE',  ( -0.000000000000000000, -0.000000000000000000, 1.000000000000000000 ) ) ;
#23554 = CARTESIAN_POINT ( 'NONE',  ( 118.1029919389229406, -36.12161712796727642, 269.8822919425776945 ) ) ;
#23555 = DIRECTION ( 'NONE',  ( 0.9963424814100678706, -0.08544974978095865037, 0.000000000000000000 ) ) ;
#23556 = CARTESIAN_POINT ( 'NONE',  ( 132.8830524875708363, -34.24700279812689274, 1.845048209623704416 ) ) ;
#23557 = ADVANCED_FACE ( 'NONE', ( #35338 ), #89432, .T. ) ;
#23558 = CIRCLE ( 'NONE', #74305, 160.4955849403809793 ) ;
#23559 = ADVANCED_FACE ( 'NONE', ( #61699 ), #381, .F. ) ;
#23561 = CARTESIAN_POINT ( 'NONE',  ( 85.85227416678092993, 70.17658267799284033, 81.76234319299453546 ) ) ;
#23560 = DIRECTION ( 'NONE',  ( 0.000000000000000000, 0.000000000000000000, -1.000000000000000000 ) ) ;
#23562 = CARTESIAN_POINT ( 'NONE',  ( -254.0000000000000000, 104.7749999999999915, -41.27499999999999858 ) ) ;
#23563 = CARTESIAN_POINT ( 'NONE',  ( 114.6950545185401609, -40.57145610743049247, 202.8781341137909635 ) ) ;
#23564 = EDGE_LOOP ( 'NONE', ( #3543, #62723, #66241, #71716, #11106, #57535 ) ) ;
#23565 = ADVANCED_FACE ( 'NONE', ( #20395 ), #62157, .F. ) ;
#23566 = ORIENTED_EDGE ( 'NONE', *, *, #64796, .F. ) ;
#23567 = ORIENTED_EDGE ( 'NONE', *, *, #15336, .F. ) ;
#23568 = VECTOR ( 'NONE', #61237, 999.9999999999998863 ) ;
#23569 = DIRECTION ( 'NONE',  ( 0.000000000000000000, 0.000000000000000000, 1.000000000000000000 ) ) ;
#23571 = EDGE_CURVE ( 'NONE', #33311, #56525, #64530, .T. ) ;
#23570 = CARTESIAN_POINT ( 'NONE',  ( 110.8541901428846899, -45.98435271355759824, 182.8856010440399018 ) ) ;
#23572 = CARTESIAN_POINT ( 'NONE',  ( 99.81116105471878086, -29.32005551970522461, 266.7051490854344706 ) ) ;
#23573 = CIRCLE ( 'NONE', #74318, 2.500000000000002220 ) ;
#23574 = CARTESIAN_POINT ( 'NONE',  ( 173.9900000000000091, 28.98850000000000193, -58.73749999999999716 ) ) ;
#23575 = CYLINDRICAL_SURFACE ( 'NONE', #39006, 12.70000000000000462 ) ;
#23576 = EDGE_CURVE ( 'NONE', #80585, #89702, #15184, .T. ) ;
#23577 = CARTESIAN_POINT ( 'NONE',  ( 0.000000000000000000, 127.0000000000000000, 85.23828826961327820 ) ) ;
#23578 = EDGE_LOOP ( 'NONE', ( #2379, #12616, #49463, #41291, #4782 ) ) ;
#23579 = FACE_OUTER_BOUND ( 'NONE', #81614, .T. ) ;
#23580 = ORIENTED_EDGE ( 'NONE', *, *, #1494, .F. ) ;
#23581 = DIRECTION ( 'NONE',  ( 0.000000000000000000, 0.000000000000000000, -1.000000000000000000 ) ) ;
#23582 = CARTESIAN_POINT ( 'NONE',  ( 110.3993955946342993, -29.27817736879564237, 22.55951894101998434 ) ) ;
#23583 = CARTESIAN_POINT ( 'NONE',  ( 136.7978637535031226, -18.40984252624964412, 6.777538624682987844 ) ) ;
#23584 = CARTESIAN_POINT ( 'NONE',  ( -54.12775174896490427, 53.97500000000000142, 69.87310403134814862 ) ) ;
#23585 = CARTESIAN_POINT ( 'NONE',  ( 92.32962665258614265, 81.72118090664558565, -74.36911441044638593 ) ) ;
#23586 = EDGE_LOOP ( 'NONE', ( #19447, #62535, #13875, #83312 ) ) ;
#23587 = FACE_OUTER_BOUND ( 'NONE', #83343, .T. ) ;
#23588 = EDGE_CURVE ( 'NONE', #71038, #43418, #56215, .T. ) ;
#23589 = CARTESIAN_POINT ( 'NONE',  ( 107.0664832912739968, -36.72944715994100306, -2.364374724089013391 ) ) ;
#23590 = VECTOR ( 'NONE', #34017, 1000.000000000000000 ) ;
#23591 = EDGE_LOOP ( 'NONE', ( #6103, #67600, #48759, #9391 ) ) ;
#23592 = CARTESIAN_POINT ( 'NONE',  ( 113.3425240358415778, -27.63052414531908596, 89.60800622829195561 ) ) ;
#23593 = VERTEX_POINT ( 'NONE', #50308 ) ;
#23594 = EDGE_CURVE ( 'NONE', #63455, #34012, #78050, .T. ) ;
#23595 = CARTESIAN_POINT ( 'NONE',  ( 99.48186602960301173, -30.66774701162068695, 45.21241982807700310 ) ) ;
#23596 = EDGE_CURVE ( 'NONE', #40553, #58657, #28994, .T. ) ;
#23597 = DIRECTION ( 'NONE',  ( 0.000000000000000000, -1.000000000000000000, 0.000000000000000000 ) ) ;
#23598 = CARTESIAN_POINT ( 'NONE',  ( 98.75489364002905290, -33.65605228111792968, 62.47586902018298360 ) ) ;
#23599 = CARTESIAN_POINT ( 'NONE',  ( 90.44969454456408187, -50.04645651782490745, 239.5838068554174356 ) ) ;
#23600 = DIRECTION ( 'NONE',  ( 1.000000000000000000, 8.163404592831600092E-16, 1.020425574103949962E-15 ) ) ;
#23601 = EDGE_CURVE ( 'NONE', #2953, #28826, #15816, .T. ) ;
#23602 = CARTESIAN_POINT ( 'NONE',  ( 68.91422814837490307, -69.55937875643057566, 247.4998451774034152 ) ) ;
#23603 = CARTESIAN_POINT ( 'NONE',  ( 118.7569292017688696, -34.64240976163905827, 44.96705384733895272 ) ) ;
#23604 = FACE_OUTER_BOUND ( 'NONE', #59527, .T. ) ;
#23605 = ORIENTED_EDGE ( 'NONE', *, *, #33901, .T. ) ;
#23606 = AXIS2_PLACEMENT_3D ( 'NONE', #22363, #50037, #77776 ) ;
#23607 = CARTESIAN_POINT ( 'NONE',  ( 128.0667039024480118, -50.82844715994100682, 250.9178068554150514 ) ) ;
#23608 = ORIENTED_EDGE ( 'NONE', *, *, #80409, .F. ) ;
#23609 = CARTESIAN_POINT ( 'NONE',  ( 113.8717716195138792, -28.72781827743602889, 135.5156252759109634 ) ) ;
#23610 = CARTESIAN_POINT ( 'NONE',  ( 199.3900000000000148, 52.73749999999999716, -44.45000000000000284 ) ) ;
#23611 = ORIENTED_EDGE ( 'NONE', *, *, #80991, .F. ) ;
#23612 = VERTEX_POINT ( 'NONE', #22636 ) ;
#23613 = B_SPLINE_CURVE_WITH_KNOTS ( 'NONE', 3,
 ( #46163, #73895, #11679, #39372, #60248, #65728, #10333, #87980, #67520, #25740, #58905, #53416, #81183, #18932, #74348, #12118, #39801, #5309, #32999, #81633, #3510, #44838, #31208, #86642, #52080, #24415, #79840, #17597 ),
 .UNSPECIFIED., .F., .F.,
 ( 4, 2, 2, 2, 2, 2, 2, 2, 2, 2, 1, 1, 1, 1, 2, 4 ),
 ( 0.000000000000000000, 0.06251128867752057949, 0.1250225773550411590, 0.1875338660325617246, 0.2500451547100823180, 0.3125564433876029113, 0.3750677320651234492, 0.4375790207426440426, 0.4688346650814042005, 0.4844624872507840574, 0.4922763983354739303, 0.4961833538778187003, 0.4981368316489910852, 0.4991135705345771667, 0.4996019399773705127, 0.5000903094201638588 ),
 .UNSPECIFIED. ) ;
#23614 = FACE_OUTER_BOUND ( 'NONE', #63731, .T. ) ;
#23615 = DIRECTION ( 'NONE',  ( 1.000000000000000000, 6.493183223601999383E-14, -1.022247060195607093E-42 ) ) ;
#23616 = CARTESIAN_POINT ( 'NONE',  ( 107.2322476904469966, -46.54200526979099095, 212.5899109901969837 ) ) ;
#23617 = CARTESIAN_POINT ( 'NONE',  ( -55.11501535285000131, 101.5999999999999943, 183.9403141659174992 ) ) ;
#23618 = LINE ( 'NONE', #63594, #53827 ) ;
#23619 = DIRECTION ( 'NONE',  ( 0.000000000000000000, 0.000000000000000000, -1.000000000000000000 ) ) ;
#23620 = CARTESIAN_POINT ( 'NONE',  ( 110.2841144599940577, -46.64559811412390644, 8.827053847339950465 ) ) ;
#23621 = AXIS2_PLACEMENT_3D ( 'NONE', #80117, #53699, #5595 ) ;
#23622 = CARTESIAN_POINT ( 'NONE',  ( 33.91903122894598965, -35.91149509761181235, -5.074374724088000832 ) ) ;
#23623 = ORIENTED_EDGE ( 'NONE', *, *, #16357, .F. ) ;
#23624 = FILL_AREA_STYLE ('',( #36791 ) ) ;
#23625 = DIRECTION ( 'NONE',  ( -1.000000000000000078E-15, 1.000000000000000083E-30, 1.000000000000000000 ) ) ;
#23626 = ORIENTED_EDGE ( 'NONE', *, *, #39219, .F. ) ;
#23627 = DIRECTION ( 'NONE',  ( 1.000000000000000000, 0.000000000000000000, 0.000000000000000000 ) ) ;
#23628 = CARTESIAN_POINT ( 'NONE',  ( 97.80791547859365664, -40.51903635482080546, 112.6360621818907077 ) ) ;
#23629 = CARTESIAN_POINT ( 'NONE',  ( 118.6297112294784029, -39.20734283244436114, 258.6584824187679033 ) ) ;
#23630 = CARTESIAN_POINT ( 'NONE',  ( 72.25757238336808541, -1.944390235229867425, 361.9756252759101471 ) ) ;
#23631 = DIRECTION ( 'NONE',  ( 1.000000000000000000, 4.237773401492740281E-14, 0.000000000000000000 ) ) ;
#23632 = LINE ( 'NONE', #77246, #47574 ) ;
#23633 = CARTESIAN_POINT ( 'NONE',  ( 98.11275290507195734, -35.37173493080541675, 220.6171817328389864 ) ) ;
#23635 = CARTESIAN_POINT ( 'NONE',  ( 106.6078071710152244, -25.70885557892973949, 36.09753003781596448 ) ) ;
#23634 = CYLINDRICAL_SURFACE ( 'NONE', #89645, 12.99999999999999822 ) ;
#23636 = LINE ( 'NONE', #9108, #49471 ) ;
#23637 = CARTESIAN_POINT ( 'NONE',  ( 117.7486274683349308, -39.74683136594191524, 143.6194347997209775 ) ) ;
#23638 = VERTEX_POINT ( 'NONE', #43938 ) ;
#23639 = DIRECTION ( 'NONE',  ( 1.054009200593500181E-15, 1.000000000000000000, 0.000000000000000000 ) ) ;
#23640 = EDGE_LOOP ( 'NONE', ( #25966, #72582, #26147, #988 ) ) ;
#23641 = LINE ( 'NONE', #64073, #31 ) ;
#23642 = CARTESIAN_POINT ( 'NONE',  ( 97.81281252356875200, -40.52015776331121089, 277.6356251289804504 ) ) ;
#23643 = ORIENTED_EDGE ( 'NONE', *, *, #31210, .T. ) ;
#23644 = DIRECTION ( 'NONE',  ( 0.000000000000000000, 1.000000000000000000, 0.000000000000000000 ) ) ;
#23645 = ORIENTED_EDGE ( 'NONE', *, *, #38302, .T. ) ;
#23646 = CARTESIAN_POINT ( 'NONE',  ( 251.6756888531239156, -13.32818131005263140, 117.4678068554150627 ) ) ;
#23647 = CARTESIAN_POINT ( 'NONE',  ( 107.0664832912739541, -36.72944715994095333, 309.2406250056037038 ) ) ;
#23648 = DIRECTION ( 'NONE',  ( 0.000000000000000000, 0.000000000000000000, 1.000000000000000000 ) ) ;
#23649 = ORIENTED_EDGE ( 'NONE', *, *, #13451, .F. ) ;
#23650 = CARTESIAN_POINT ( 'NONE',  ( 106.6594718829666704, -26.29006472227095870, 85.10705384733896040 ) ) ;
#23651 = EDGE_CURVE ( 'NONE', #75721, #68410, #81911, .T. ) ;
#23652 = CARTESIAN_POINT ( 'NONE',  ( 0.000000000000000000, 0.000000000000000000, 0.000000000000000000 ) ) ;
#23653 = DIRECTION ( 'NONE',  ( 0.000000000000000000, 0.000000000000000000, 1.000000000000000000 ) ) ;
#23654 = PLANE ( 'NONE',  #58258 ) ;
#23655 = EDGE_CURVE ( 'NONE', #65590, #17260, #646, .T. ) ;
#23656 = CARTESIAN_POINT ( 'NONE',  ( -11.30280630903569872, 76.96642768152659642, 117.8152258610045351 ) ) ;
#23657 = EDGE_LOOP ( 'NONE', ( #43430, #88808, #27637, #24276 ) ) ;
#23658 =( REPRESENTATION_RELATIONSHIP ('NONE','NONE', #82876, #14421 ) REPRESENTATION_RELATIONSHIP_WITH_TRANSFORMATION ( #27655 )SHAPE_REPRESENTATION_RELATIONSHIP( ) );
#23659 = EDGE_CURVE ( 'NONE', #79502, #74222, #63014, .T. ) ;
#23660 = VECTOR ( 'NONE', #39286, 1000.000000000000000 ) ;
#23661 = CARTESIAN_POINT ( 'NONE',  ( 172.5664832912729878, -27.57844715994070484, 18.92562527591200094 ) ) ;
#23662 = LINE ( 'NONE', #79970, #15012 ) ;
#23663 = CARTESIAN_POINT ( 'NONE',  ( 29.66666666666670338, 171.3333333333333428, 183.2159591118794708 ) ) ;
#23664 = ADVANCED_FACE ( 'NONE', ( #56680 ), #16707, .T. ) ;
#23665 = ADVANCED_FACE ( 'NONE', ( #64850 ), #83967, .T. ) ;
#23667 = CARTESIAN_POINT ( 'NONE',  ( 0.000000000000000000, 125.7300000000000040, 0.000000000000000000 ) ) ;
#23666 = PLANE ( 'NONE',  #2992 ) ;
#23668 = CARTESIAN_POINT ( 'NONE',  ( 88.17226027475707895, -14.72944715994102616, 249.5838068554175777 ) ) ;
#23669 = ADVANCED_FACE ( 'NONE', ( #51198 ), #84423, .F. ) ;
#23670 = VECTOR ( 'NONE', #14994, 1000.000000000000000 ) ;
#23671 = ORIENTED_EDGE ( 'NONE', *, *, #22798, .F. ) ;
#23673 = ADVANCED_FACE ( 'NONE', ( #77146, #29440 ), #832, .T. ) ;
#23672 = CARTESIAN_POINT ( 'NONE',  ( 182.0667039024480118, -32.29483332968430886, -5.074374724088000832 ) ) ;
#23674 = CARTESIAN_POINT ( 'NONE',  ( 102.3610132369663432, -45.97051510703448685, 168.2137205140059564 ) ) ;
#23676 = EDGE_LOOP ( 'NONE', ( #14838, #1695, #59674, #50258 ) ) ;
#23675 = CARTESIAN_POINT ( 'NONE',  ( 3.175000000000355094, 104.3431970271541616, -33.98325472291460159 ) ) ;
#23677 = CARTESIAN_POINT ( 'NONE',  ( 106.3024736416176950, -26.94527301088420046, 21.13848241876792144 ) ) ;
#23678 = DIRECTION ( 'NONE',  ( 2.900000000000000265E-14, -2.000000000000000155E-15, 1.000000000000000000 ) ) ;
#23679 = CARTESIAN_POINT ( 'NONE',  ( 1.387778780781445676E-14, 239.0000000000000000, 104.4754207677255806 ) ) ;
#23680 = DIRECTION ( 'NONE',  ( 0.000000000000000000, 1.000000000000000000, 0.000000000000000000 ) ) ;
#23681 = EDGE_CURVE ( 'NONE', #10148, #52594, #1288, .T. ) ;
#23682 = ORIENTED_EDGE ( 'NONE', *, *, #260, .F. ) ;
#23683 = CARTESIAN_POINT ( 'NONE',  ( 99.09606710607866376, -30.54995432804265576, 30.80247099595620952 ) ) ;
#23684 = CARTESIAN_POINT ( 'NONE',  ( 98.48461633480658861, -41.42146110206444121, 221.7241967044829494 ) ) ;
#23685 = ORIENTED_EDGE ( 'NONE', *, *, #18622, .F. ) ;
#23686 = ORIENTED_EDGE ( 'NONE', *, *, #26800, .T. ) ;
#23687 = CARTESIAN_POINT ( 'NONE',  ( 107.4908894006829172, -46.11541567637532069, 189.0320594963729661 ) ) ;
#23688 = AXIS2_PLACEMENT_3D ( 'NONE', #74000, #59904, #25399 ) ;
#23689 = DIRECTION ( 'NONE',  ( 0.000000000000000000, 0.000000000000000000, 1.000000000000000000 ) ) ;
#23690 = CARTESIAN_POINT ( 'NONE',  ( 106.1501016865858844, -27.91533782510476058, 46.59015473446797984 ) ) ;
#23691 = CARTESIAN_POINT ( 'NONE',  ( -99.18048580889399091, 90.29814575435203494, 84.90178614994292161 ) ) ;
#23692 = VECTOR ( 'NONE', #6073, 999.9999999999998863 ) ;
#23693 = VECTOR ( 'NONE', #25813, 1000.000000000000114 ) ;
#23694 = CARTESIAN_POINT ( 'NONE',  ( 0.000000000000000000, 65.60000000000000853, 118.5560000000000116 ) ) ;
#23695 = DIRECTION ( 'NONE',  ( 0.000000000000000000, 0.000000000000000000, 1.000000000000000000 ) ) ;
#23696 = EDGE_LOOP ( 'NONE', ( #58960, #75618, #52195 ) ) ;
#23697 = PLANE ( 'NONE',  #87070 ) ;
#23698 = DIRECTION ( 'NONE',  ( 2.999999999999999839E-15, -1.000000000000000000, 2.999999999999999900E-30 ) ) ;
#23699 = ORIENTED_EDGE ( 'NONE', *, *, #49367, .T. ) ;
#23700 = CARTESIAN_POINT ( 'NONE',  ( 118.0844448206164827, -36.21142561920247971, 268.8518157521015723 ) ) ;
#23701 = CARTESIAN_POINT ( 'NONE',  ( 121.2221484686747317, -94.95109689075218284, -11.78219314458228695 ) ) ;
#23702 = ORIENTED_EDGE ( 'NONE', *, *, #76061, .F. ) ;
#23703 = EDGE_CURVE ( 'NONE', #61554, #25758, #7914, .T. ) ;
#23704 = PRESENTATION_STYLE_ASSIGNMENT (( #80007 ) ) ;
#23705 = CARTESIAN_POINT ( 'NONE',  ( 80.06648329127399677, 0.2215528400590013880, 311.1531252759119752 ) ) ;
#23706 = LINE ( 'NONE', #31380, #82424 ) ;
#23708 = EDGE_CURVE ( 'NONE', #2107, #4290, #9006, .T. ) ;
#23707 = CARTESIAN_POINT ( 'NONE',  ( 172.5664832912740110, 0.2215528400590013880, 18.92562527591200094 ) ) ;
#23709 = CARTESIAN_POINT ( 'NONE',  ( 96.85055626654755656, -38.51091292166574220, 42.45181575209999636 ) ) ;
#23710 = DIRECTION ( 'NONE',  ( 0.000000000000000000, 0.5000000000000007772, -0.8660254037844381525 ) ) ;
#23711 = ORIENTED_EDGE ( 'NONE', *, *, #88059, .T. ) ;
#23712 = CARTESIAN_POINT ( 'NONE',  ( 95.20983985305964836, -35.71400682071400468, 32.25848241876794020 ) ) ;
#23713 = DIRECTION ( 'NONE',  ( 1.000000000000000000, 0.000000000000000000, 1.261617073437676668E-15 ) ) ;
#23714 = AXIS2_PLACEMENT_3D ( 'NONE', #40392, #54439, #5440 ) ;
#23715 = CARTESIAN_POINT ( 'NONE',  ( 104.5881283732255156, -26.60288457357396652, 285.2670538473396391 ) ) ;
#23716 = VERTEX_POINT ( 'NONE', #71235 ) ;
#23717 = AXIS2_PLACEMENT_3D ( 'NONE', #55912, #49104, #85 ) ;
#23718 = CARTESIAN_POINT ( 'NONE',  ( 82.81644824798257787, -18.55833207211307112, 3.101428811465905877 ) ) ;
#23719 = DIRECTION ( 'NONE',  ( -0.0001713722455994998422, 0.9999999853157766072, 0.000000000000000000 ) ) ;
#23720 = DIRECTION ( 'NONE',  ( 1.000000000000000000, 0.000000000000000000, 0.000000000000000000 ) ) ;
#23721 = CARTESIAN_POINT ( 'NONE',  ( 113.0492235774716363, -42.98306560958572931, 110.9899951314959594 ) ) ;
#23722 = CARTESIAN_POINT ( 'NONE',  ( 115.0562973506820157, -29.05819712879207017, 185.4232443235299570 ) ) ;
#23723 = FACE_OUTER_BOUND ( 'NONE', #3465, .T. ) ;
#23724 = DIRECTION ( 'NONE',  ( 0.7071067811571474238, 0.7071067812159476107, 0.000000000000000000 ) ) ;
#23725 = ORIENTED_EDGE ( 'NONE', *, *, #32024, .F. ) ;
#23726 = DIRECTION ( 'NONE',  ( 0.000000000000000000, 0.8660254037844387076, -0.4999999999999998890 ) ) ;
#23727 = VERTEX_POINT ( 'NONE', #64406 ) ;
#23728 = VERTEX_POINT ( 'NONE', #2186 ) ;
#23729 = AXIS2_PLACEMENT_3D ( 'NONE', #27010, #27449, #82889 ) ;
#23730 = CYLINDRICAL_SURFACE ( 'NONE', #56030, 2.030000000001872529 ) ;
#23731 = ORIENTED_EDGE ( 'NONE', *, *, #75735, .T. ) ;
#23732 = VERTEX_POINT ( 'NONE', #23095 ) ;
#23733 = CARTESIAN_POINT ( 'NONE',  ( -47.02966122971775320, 101.5999999999999943, -8.565507749926087908E-15 ) ) ;
#23734 = CARTESIAN_POINT ( 'NONE',  ( 115.8238408366701009, -31.72726729926949574, 24.24004256710726679 ) ) ;
#23735 = CARTESIAN_POINT ( 'NONE',  ( 112.1993679394656453, -43.55657132036190404, 142.5124198280769576 ) ) ;
#23736 = CARTESIAN_POINT ( 'NONE',  ( 116.6022279875747216, -42.36549642380604297, 283.4137205140060018 ) ) ;
#23737 = CARTESIAN_POINT ( 'NONE',  ( -5.635138049808393390, 71.13823012824934722, 130.4366002064613212 ) ) ;
#23738 = ORIENTED_EDGE ( 'NONE', *, *, #31742, .F. ) ;
#23739 = CARTESIAN_POINT ( 'NONE',  ( 108.5522760911612465, -26.80684647353728778, 135.9583350980946364 ) ) ;
#23740 = ORIENTED_EDGE ( 'NONE', *, *, #75622, .F. ) ;
#23741 = LINE ( 'NONE', #36010, #34826 ) ;
#23742 = CARTESIAN_POINT ( 'NONE',  ( -69.72411017813060141, 127.0000000000000000, 69.72411017812929401 ) ) ;
#23743 = DIRECTION ( 'NONE',  ( 0.000000000000000000, 1.000000000000000000, 0.000000000000000000 ) ) ;
#23744 = ADVANCED_FACE ( 'NONE', ( #57577 ), #50768, .T. ) ;
#23745 = CIRCLE ( 'NONE', #32395, 8.636000000000004562 ) ;
#23746 = CARTESIAN_POINT ( 'NONE',  ( 1.598849875094818280E-14, 61.59999999999999432, -130.5560000000000116 ) ) ;
#23747 = EDGE_LOOP ( 'NONE', ( #17654, #7284, #7816, #42509 ) ) ;
#23748 = CARTESIAN_POINT ( 'NONE',  ( 106.1383370350330324, -47.74387551462719159, 262.4975300378158636 ) ) ;
#23749 = CARTESIAN_POINT ( 'NONE',  ( 115.4796304032075653, -43.01888039838633659, 24.31562527591096767 ) ) ;
#23750 = AXIS2_PLACEMENT_3D ( 'NONE', #72656, #66260, #79034 ) ;
#23751 = DIRECTION ( 'NONE',  ( 0.000000000000000000, 0.000000000000000000, -1.000000000000000000 ) ) ;
#23752 = EDGE_CURVE ( 'NONE', #52709, #76080, #73893, .T. ) ;
#23754 = CARTESIAN_POINT ( 'NONE',  ( 68.77810336616866493, -139.2209757805153174, 246.3536556105786417 ) ) ;
#23753 = DIRECTION ( 'NONE',  ( 1.049727191138617833E-16, -0.5150380749100549327, 0.8571673007021118895 ) ) ;
#23755 = CARTESIAN_POINT ( 'NONE',  ( 51.06670390244899238, -32.29483332968430886, -5.074374724088000832 ) ) ;
#23756 = ADVANCED_FACE ( 'NONE', ( #80723 ), #53415, .T. ) ;
#23757 = CARTESIAN_POINT ( 'NONE',  ( 37.36643805256657913, -48.62818131006090994, 249.9678068554150343 ) ) ;
#23758 = CARTESIAN_POINT ( 'NONE',  ( 131.7293641403265099, -38.17925173418004192, 7.255518600575052268 ) ) ;
#23759 = EDGE_CURVE ( 'NONE', #72082, #10437, #44837, .T. ) ;
#23760 = CARTESIAN_POINT ( 'NONE',  ( 162.8913605087219878, -31.76306994223740432, -5.074374724088000832 ) ) ;
#23761 = FACE_OUTER_BOUND ( 'NONE', #80325, .T. ) ;
#23762 = DIRECTION ( 'NONE',  ( 0.000000000000000000, 0.000000000000000000, 1.000000000000000000 ) ) ;
#23763 = ADVANCED_FACE ( 'NONE', ( #65298 ), #23971, .T. ) ;
#23764 = LINE ( 'NONE', #51432, #84452 ) ;
#23765 = CARTESIAN_POINT ( 'NONE',  ( 118.6196304926710212, -33.88663714441439367, 14.01848241876796308 ) ) ;
#23766 = CARTESIAN_POINT ( 'NONE',  ( 98.09065366798802188, -42.10120877535955231, 157.7556252759109725 ) ) ;
#23767 = CARTESIAN_POINT ( 'NONE',  ( 110.3609615670502535, -25.32029891922833897, 60.85276813305395649 ) ) ;
#23769 = DIRECTION ( 'NONE',  ( 0.000000000000000000, 0.000000000000000000, -1.000000000000000000 ) ) ;
#23768 = DIRECTION ( 'NONE',  ( 0.000000000000000000, 0.000000000000000000, 1.000000000000000000 ) ) ;
#23770 = CARTESIAN_POINT ( 'NONE',  ( 82.58883806303516906, -35.63381004753058789, 2.797770231023114729 ) ) ;
#23771 = EDGE_CURVE ( 'NONE', #11533, #51807, #38022, .T. ) ;
#23772 = AXIS2_PLACEMENT_3D ( 'NONE', #63110, #82686, #7264 ) ;
#23773 = CIRCLE ( 'NONE', #17908, 0.4999999999999994449 ) ;
#23774 = VERTEX_POINT ( 'NONE', #17153 ) ;
#23775 = CARTESIAN_POINT ( 'NONE',  ( 100.9546728744814601, -28.70702568005829391, 186.5939586030299608 ) ) ;
#23776 = ORIENTED_EDGE ( 'NONE', *, *, #73173, .F. ) ;
#23777 = EDGE_CURVE ( 'NONE', #76504, #14135, #10816, .T. ) ;
#23778 = CARTESIAN_POINT ( 'NONE',  ( 98.84777479348176144, -29.24180311599948467, 76.73848241876795839 ) ) ;
#23780 = ORIENTED_EDGE ( 'NONE', *, *, #4141, .T. ) ;
#23779 = PLANE ( 'NONE',  #80578 ) ;
#23781 = AXIS2_PLACEMENT_3D ( 'NONE', #70711, #22568, #20760 ) ;
#23782 = CARTESIAN_POINT ( 'NONE',  ( 112.0653985349986357, -45.48868239570060723, 48.98974552996795495 ) ) ;
#23783 = CARTESIAN_POINT ( 'NONE',  ( 117.7539631054256972, -31.66723592997637482, 210.1784824187679703 ) ) ;
#23784 = LINE ( 'NONE', #51448, #77390 ) ;
#23785 = DIRECTION ( 'NONE',  ( 0.9068632946707805287, -0.4214249218767882610, 1.035655806553318316E-15 ) ) ;
#23786 = CARTESIAN_POINT ( 'NONE',  ( 132.2857443282840393, -124.7784471599409102, 222.2178068554179902 ) ) ;
#23787 = DIRECTION ( 'NONE',  ( 1.000000000000000078E-15, 1.000000000000000083E-30, -1.000000000000000000 ) ) ;
#23788 = ADVANCED_FACE ( 'NONE', ( #52957 ), #32101, .F. ) ;
#23789 = CARTESIAN_POINT ( 'NONE',  ( 145.7566936099118777, -137.2574666318677998, 247.4285154401919726 ) ) ;
#23790 = CARTESIAN_POINT ( 'NONE',  ( 110.8719906046491559, -45.97705236736918977, 97.88713169491219901 ) ) ;
#23791 = CARTESIAN_POINT ( 'NONE',  ( 102.9676436823273917, -46.25511244710201453, 137.2651490854349561 ) ) ;
#23792 = ORIENTED_EDGE ( 'NONE', *, *, #13347, .F. ) ;
#23793 = ORIENTED_EDGE ( 'NONE', *, *, #25207, .F. ) ;
#23794 = CARTESIAN_POINT ( 'NONE',  ( 116.2382276885637538, -38.76798346032508391, 100.0720594963729866 ) ) ;
#23795 = CARTESIAN_POINT ( 'NONE',  ( 128.0667039024481539, -16.72944715994115583, 239.5838068554164408 ) ) ;
#23797 = CARTESIAN_POINT ( 'NONE',  ( 41.56670390244777735, -36.32844715994104234, 300.4678068554150059 ) ) ;
#23796 = CARTESIAN_POINT ( 'NONE',  ( 107.2379402074490855, -25.61267671046461558, 226.0641967044819580 ) ) ;
#23798 = CARTESIAN_POINT ( 'NONE',  ( 113.8679580013058654, -39.89013407401493794, 9.125625275910969947 ) ) ;
#23799 = DIRECTION ( 'NONE',  ( 1.000000000000000000, 1.000000000000000078E-15, 0.000000000000000000 ) ) ;
#23800 = CARTESIAN_POINT ( 'NONE',  ( 118.4859477596447306, 70.52090377575430580, -4.094325160631359317 ) ) ;
#23801 = CARTESIAN_POINT ( 'NONE',  ( -487.2989999999999782, 93.66249999999999432, 82.23860802895320887 ) ) ;
#23802 = DIRECTION ( 'NONE',  ( -1.000000000000000000, 0.000000000000000000, 8.252657816380299978E-16 ) ) ;
#23803 = CARTESIAN_POINT ( 'NONE',  ( 11.79654850775738240, 78.10342437589451947, 117.9677577584307926 ) ) ;
#23804 = CARTESIAN_POINT ( 'NONE',  ( 97.69433714244404143, -41.24514667321086847, 171.6841967044819626 ) ) ;
#23805 = ORIENTED_EDGE ( 'NONE', *, *, #2347, .T. ) ;
#23806 = ORIENTED_EDGE ( 'NONE', *, *, #53457, .F. ) ;
#23807 = CARTESIAN_POINT ( 'NONE',  ( 72.06648329127403940, -56.72944715994105991, -4.824374724089063982 ) ) ;
#23808 = CARTESIAN_POINT ( 'NONE',  ( 146.9552639810710559, -67.98257152991943997, 246.1456466833680281 ) ) ;
#23809 = CARTESIAN_POINT ( 'NONE',  ( 97.81169182074827972, -40.51741433969252881, 77.63574375254798099 ) ) ;
#23811 = EDGE_CURVE ( 'NONE', #83896, #65511, #11213, .T. ) ;
#23810 = CARTESIAN_POINT ( 'NONE',  ( 98.54748562642340914, -41.97671081279658978, 102.7657787019688271 ) ) ;
#23812 = AXIS2_PLACEMENT_3D ( 'NONE', #60475, #32324, #88221 ) ;
#23813 = DIRECTION ( 'NONE',  ( -1.000000000000000078E-15, 1.000000000000000083E-30, 1.000000000000000000 ) ) ;
#23814 = VECTOR ( 'NONE', #61911, 1000.000000000000000 ) ;
#23815 = CARTESIAN_POINT ( 'NONE',  ( 97.76227787611212250, -41.51041654567812600, 196.7041967044819728 ) ) ;
#23816 = LINE ( 'NONE', #49705, #9751 ) ;
#23817 = ORIENTED_EDGE ( 'NONE', *, *, #32138, .T. ) ;
#23819 = VERTEX_POINT ( 'NONE', #32542 ) ;
#23818 = VERTEX_POINT ( 'NONE', #4855 ) ;
#23820 = CARTESIAN_POINT ( 'NONE',  ( -0.8399620612054651270, 69.85000000000003695, 118.5560000000000400 ) ) ;
#23821 = DIRECTION ( 'NONE',  ( 1.000000000000000000, 0.000000000000000000, 0.000000000000000000 ) ) ;
#23822 = DIRECTION ( 'NONE',  ( -1.000000000000000078E-15, 1.000000000000000083E-30, 1.000000000000000000 ) ) ;
#23823 = CARTESIAN_POINT ( 'NONE',  ( 113.8567361903355675, -31.03552547285496388, 265.8130118773257777 ) ) ;
#23824 = CARTESIAN_POINT ( 'NONE',  ( 45.77381068356938698, -48.62134037881676818, 249.9678068554150343 ) ) ;
#23825 = ORIENTED_EDGE ( 'NONE', *, *, #30218, .F. ) ;
#23826 = EDGE_CURVE ( 'NONE', #39335, #56383, #11678, .T. ) ;
#23827 = CARTESIAN_POINT ( 'NONE',  ( 115.8395158816858981, -40.05665934170760067, 9.635625275910941312 ) ) ;
#23828 = CARTESIAN_POINT ( 'NONE',  ( -127.0239848601436847, 55.39831567219715680, 30.16249999999990195 ) ) ;
#23829 = ORIENTED_EDGE ( 'NONE', *, *, #2529, .F. ) ;
#23830 = ORIENTED_EDGE ( 'NONE', *, *, #49672, .T. ) ;
#23831 = EDGE_CURVE ( 'NONE', #47474, #9456, #25290, .T. ) ;
#23832 = AXIS2_PLACEMENT_3D ( 'NONE', #55045, #54147, #48685 ) ;
#23833 = DIRECTION ( 'NONE',  ( 4.194175870806139918E-14, -1.000000000000000000, 0.000000000000000000 ) ) ;
#23834 = CIRCLE ( 'NONE', #60036, 1.000000000000000888 ) ;
#23835 = ORIENTED_EDGE ( 'NONE', *, *, #44132, .T. ) ;
#23836 = ORIENTED_EDGE ( 'NONE', *, *, #19913, .F. ) ;
#23837 = VECTOR ( 'NONE', #37141, 1000.000000000000000 ) ;
#23838 = CARTESIAN_POINT ( 'NONE',  ( 98.68252487213293023, -38.50746385042646125, 30.91527697093399141 ) ) ;
#23840 = CARTESIAN_POINT ( 'NONE',  ( 95.88624405714097065, -32.72491640434669335, 176.0527681330539735 ) ) ;
#23839 = CIRCLE ( 'NONE', #25240, 2.517500000000005844 ) ;
#23841 = CARTESIAN_POINT ( 'NONE',  ( 111.7842945758856672, -25.88553347519904335, 134.7499109901969518 ) ) ;
#23842 = B_SPLINE_CURVE_WITH_KNOTS ( 'NONE', 3,
 ( #21808, #49478, #79003, #15440, #14986, #64917, #57189, #2702, #36321, #64031, #8168, #23602, #1809, #29507 ),
 .UNSPECIFIED., .F., .F.,
 ( 4, 2, 2, 2, 2, 2, 4 ),
 ( 0.000000000000000000, 0.4999999999997828404, 0.7499999999996677102, 0.8749999999996868061, 0.9374999999997890576, 0.9687499999998945288, 1.000000000000000000 ),
 .UNSPECIFIED. ) ;
#23843 = CARTESIAN_POINT ( 'NONE',  ( 162.5667039024460223, -22.48495420874110806, -5.074374724088000832 ) ) ;
#23844 = CARTESIAN_POINT ( 'NONE',  ( 118.0816017896457453, -32.35888884030432422, 245.1270538473389706 ) ) ;
#23845 = DIRECTION ( 'NONE',  ( 1.639958061481212836E-42, -4.100000000000000342E-29, -1.000000000000000000 ) ) ;
#23846 = CARTESIAN_POINT ( 'NONE',  ( 80.75702474444096879, -128.2461948925749766, 249.3055308415380011 ) ) ;
#23847 = CARTESIAN_POINT ( 'NONE',  ( -130.2059614519578759, 74.16222525595216553, -9.571858562769296697 ) ) ;
#23848 = ORIENTED_EDGE ( 'NONE', *, *, #77057, .F. ) ;
#23849 = ORIENTED_EDGE ( 'NONE', *, *, #76693, .T. ) ;
#23850 = CARTESIAN_POINT ( 'NONE',  ( 109.3681991936945508, -25.87058038976459429, 184.9222919425779708 ) ) ;
#23851 = VERTEX_POINT ( 'NONE', #3958 ) ;
#23852 = CARTESIAN_POINT ( 'NONE',  ( 104.5625478726873894, -48.31265885861421339, 182.4070538473399665 ) ) ;
#23853 = CARTESIAN_POINT ( 'NONE',  ( 41.56648329127381203, -27.82844715994070484, 321.9256252759120116 ) ) ;
#23854 = LINE ( 'NONE', #25623, #17417 ) ;
#23855 = CARTESIAN_POINT ( 'NONE',  ( 143.4979113519680993, -139.5802913934610103, 247.3215535119185517 ) ) ;
#23858 = CARTESIAN_POINT ( 'NONE',  ( 98.36549455146196408, -40.29075363668730603, 7.635625275910939536 ) ) ;
#23857 = DIRECTION ( 'NONE',  ( -1.000000000000000000, 0.000000000000000000, 0.000000000000000000 ) ) ;
#23856 = LINE ( 'NONE', #59680, #56397 ) ;
#23859 = CYLINDRICAL_SURFACE ( 'NONE', #22025, 0.4999999999999989453 ) ;
#23860 = EDGE_CURVE ( 'NONE', #46362, #13204, #81182, .T. ) ;
#23861 = DIRECTION ( 'NONE',  ( 0.9242245927363031965, 0.3818493186865917766, 0.000000000000000000 ) ) ;
#23862 = FACE_OUTER_BOUND ( 'NONE', #41345, .T. ) ;
#23863 = EDGE_CURVE ( 'NONE', #44698, #75678, #12117, .T. ) ;
#23864 = CARTESIAN_POINT ( 'NONE',  ( 67.54744102787780946, -137.3996135046812412, 246.8082721997937767 ) ) ;
#23865 = FACE_OUTER_BOUND ( 'NONE', #46263, .T. ) ;
#23866 = CARTESIAN_POINT ( 'NONE',  ( 107.0664832912739968, 0.2215528400590083269, 336.6506252759110112 ) ) ;
#23868 = ORIENTED_EDGE ( 'NONE', *, *, #84286, .T. ) ;
#23867 = CARTESIAN_POINT ( 'NONE',  ( 100.8056940436082698, -41.93424458468394533, 195.5838068554169809 ) ) ;
#23869 = EDGE_CURVE ( 'NONE', #13668, #78028, #55790, .T. ) ;
#23870 = CARTESIAN_POINT ( 'NONE',  ( 135.7779513194053891, -20.88977919477191492, 7.751962620090911749 ) ) ;
#23871 = CARTESIAN_POINT ( 'NONE',  ( 108.6784406349466110, -26.40724015326817664, 189.9527681330539792 ) ) ;
#23872 = CARTESIAN_POINT ( 'NONE',  ( 115.2072660578295284, -44.20618685261739245, 74.22324432352993995 ) ) ;
#23873 = CARTESIAN_POINT ( 'NONE',  ( 106.5652502036378593, -47.22167190867460818, 243.5384824187679556 ) ) ;
#23874 = CARTESIAN_POINT ( 'NONE',  ( 188.5667039024479834, -62.87844715994099687, 175.9678068554150059 ) ) ;
#23875 = LINE ( 'NONE', #51545, #47493 ) ;
#23877 = CARTESIAN_POINT ( 'NONE',  ( 164.9190312289453004, -35.91149509760637670, 313.9678068554149490 ) ) ;
#23876 = DIRECTION ( 'NONE',  ( 1.000000000000000078E-15, -1.000000000000000000, 0.000000000000000000 ) ) ;
#23878 = CARTESIAN_POINT ( 'NONE',  ( 0.000000000000000000, 152.3879256507328250, -9.425000000000000711 ) ) ;
#23879 = CARTESIAN_POINT ( 'NONE',  ( 125.3463460965257070, 52.73749999999999716, -36.51249999999992468 ) ) ;
#23880 = ORIENTED_EDGE ( 'NONE', *, *, #89740, .T. ) ;
#23881 = VECTOR ( 'NONE', #27313, 1000.000000000000000 ) ;
#23882 = DIRECTION ( 'NONE',  ( -4.237773401492740281E-14, 1.000000000000000000, 0.000000000000000000 ) ) ;
#23883 = AXIS2_PLACEMENT_3D ( 'NONE', #23536, #71676, #43490 ) ;
#23884 = ORIENTED_EDGE ( 'NONE', *, *, #14229, .F. ) ;
#23885 = VERTEX_POINT ( 'NONE', #31207 ) ;
#23886 = EDGE_CURVE ( 'NONE', #49295, #85439, #58903, .T. ) ;
#23887 = CARTESIAN_POINT ( 'NONE',  ( 107.2856214976012552, -28.19082255356615008, 119.4781341137909578 ) ) ;
#23889 = ORIENTED_EDGE ( 'NONE', *, *, #14489, .T. ) ;
#23888 = DIRECTION ( 'NONE',  ( -1.150535366796005147E-15, 1.000000000000000000, -3.100000000000000044E-14 ) ) ;
#23890 = CARTESIAN_POINT ( 'NONE',  ( 96.05879824974444148, -41.05137697672054742, 92.62419670448296927 ) ) ;
#23891 = CARTESIAN_POINT ( 'NONE',  ( 122.2221484686747459, -104.2784471599418055, -11.78219314458200984 ) ) ;
#23892 = DIRECTION ( 'NONE',  ( 0.000000000000000000, 1.000000000000000000, 0.000000000000000000 ) ) ;
#23893 = DIRECTION ( 'NONE',  ( 0.000000000000000000, 1.000000000000000000, 1.914177628664063178E-15 ) ) ;
#23894 = CARTESIAN_POINT ( 'NONE',  ( 117.5198883494731632, -40.51604253578042858, 23.54991099019792955 ) ) ;
#23895 = VERTEX_POINT ( 'NONE', #17596 ) ;
#23896 = ORIENTED_EDGE ( 'NONE', *, *, #47538, .T. ) ;
#23897 = ORIENTED_EDGE ( 'NONE', *, *, #59388, .F. ) ;
#23898 = VECTOR ( 'NONE', #40731, 1000.000000000000000 ) ;
#23899 = AXIS2_PLACEMENT_3D ( 'NONE', #65088, #85997, #23769 ) ;
#23900 = DIRECTION ( 'NONE',  ( 1.000000000000000000, 4.299999999999999979E-14, 1.000000000000000078E-15 ) ) ;
#23901 = STYLED_ITEM ( 'NONE', ( #69914 ), #47652 ) ;
#23902 = DIRECTION ( 'NONE',  ( 0.000000000000000000, 0.000000000000000000, 1.000000000000000000 ) ) ;
#23903 = CARTESIAN_POINT ( 'NONE',  ( 105.4788588808464027, 127.0000000000000000, 3.968750000000405009 ) ) ;
#23904 = VECTOR ( 'NONE', #157, 1000.000000000000000 ) ;
#23905 = DIRECTION ( 'NONE',  ( -0.7071067811864671926, -0.7071067811866279529, -7.071067811864664779E-16 ) ) ;
#23906 = CARTESIAN_POINT ( 'NONE',  ( 194.0371591254573502, -24.89890238294407965, 249.9678068554149775 ) ) ;
#23907 = CARTESIAN_POINT ( 'NONE',  ( 0.000000000000000000, 65.60000000000000853, 0.000000000000000000 ) ) ;
#23909 = PLANE ( 'NONE',  #82271 ) ;
#23908 = VECTOR ( 'NONE', #22862, 1000.000000000000000 ) ;
#23910 = VECTOR ( 'NONE', #73589, 1000.000000000000114 ) ;
#23911 = CARTESIAN_POINT ( 'NONE',  ( -7.582671002870624122, 92.73938028448795023, 130.3355715079545689 ) ) ;
#23912 = CARTESIAN_POINT ( 'NONE',  ( 115.0059970501927182, -43.50650750775904640, 63.26419670448196797 ) ) ;
#23913 = ORIENTED_EDGE ( 'NONE', *, *, #2403, .T. ) ;
#23914 = DIRECTION ( 'NONE',  ( -0.7071067811865496822, 0.7071067811865453523, 0.000000000000000000 ) ) ;
#23915 = CARTESIAN_POINT ( 'NONE',  ( 127.0239848601435995, 53.97500000000000142, 30.16249999999999787 ) ) ;
#23916 = CARTESIAN_POINT ( 'NONE',  ( 163.5667039024460223, -18.82844715994111340, 330.9333219726761399 ) ) ;
#23917 = CARTESIAN_POINT ( 'NONE',  ( 108.2186271136511095, -28.64846388872622285, 102.7823760838769687 ) ) ;
#23918 = EDGE_CURVE ( 'NONE', #45771, #31400, #31170, .T. ) ;
#23919 = VECTOR ( 'NONE', #53296, 1000.000000000000000 ) ;
#23920 = CARTESIAN_POINT ( 'NONE',  ( 97.80514285669603680, -40.50139878960715834, 96.63424722611091511 ) ) ;
#23921 = DIRECTION ( 'NONE',  ( 0.000000000000000000, -1.000000000000000000, 0.000000000000000000 ) ) ;
#23922 = ORIENTED_EDGE ( 'NONE', *, *, #37978, .F. ) ;
#23923 = VERTEX_POINT ( 'NONE', #38467 ) ;
#23924 = CARTESIAN_POINT ( 'NONE',  ( 172.5667039024478413, -36.32844715993500273, 249.9678068554149775 ) ) ;
#23925 = ORIENTED_EDGE ( 'NONE', *, *, #36298, .T. ) ;
#23926 = ORIENTED_EDGE ( 'NONE', *, *, #89710, .F. ) ;
#23927 = CARTESIAN_POINT ( 'NONE',  ( 113.7913652599847438, -30.16800768036728542, 190.8853928297069444 ) ) ;
#23928 = PLANE ( 'NONE',  #88804 ) ;
#23929 = CARTESIAN_POINT ( 'NONE',  ( 104.9584626277977577, -25.04276672576827778, 121.2184824187679766 ) ) ;
#23930 = CARTESIAN_POINT ( 'NONE',  ( 20.03715912545745326, -46.82818131006192175, 180.4678068554150911 ) ) ;
#23931 = CARTESIAN_POINT ( 'NONE',  ( 99.08976676173786302, -42.79577391424577115, 16.84398999344881176 ) ) ;
#23932 = ORIENTED_EDGE ( 'NONE', *, *, #34011, .T. ) ;
#23933 = EDGE_CURVE ( 'NONE', #77606, #63506, #59358, .T. ) ;
#23934 = CIRCLE ( 'NONE', #57305, 173.3227045126509722 ) ;
#23935 = ORIENTED_EDGE ( 'NONE', *, *, #78216, .T. ) ;
#23936 = ORIENTED_EDGE ( 'NONE', *, *, #44010, .T. ) ;
#23937 = CARTESIAN_POINT ( 'NONE',  ( 113.3093514795881589, -30.73549005055465955, 187.2414237029249477 ) ) ;
#23938 = CARTESIAN_POINT ( 'NONE',  ( 97.26762016986505444, -33.10609988230974920, 66.04419670448297097 ) ) ;
#23939 = VERTEX_POINT ( 'NONE', #6644 ) ;
#23940 = CARTESIAN_POINT ( 'NONE',  ( 116.7068942081672276, -31.36975501082240569, 29.24229194257799236 ) ) ;
#23941 = DIRECTION ( 'NONE',  ( 0.000000000000000000, -1.000000000000000000, 0.000000000000000000 ) ) ;
#23942 = LINE ( 'NONE', #25259, #16211 ) ;
#23943 = CARTESIAN_POINT ( 'NONE',  ( 107.0079280548302592, -25.26905977990648466, 323.4874463521242092 ) ) ;
#23944 = CARTESIAN_POINT ( 'NONE',  ( 108.0069324954157537, -26.34569400419502827, 151.0041967044829505 ) ) ;
#23945 = FACE_OUTER_BOUND ( 'NONE', #43707, .T. ) ;
#23946 = ORIENTED_EDGE ( 'NONE', *, *, #44070, .T. ) ;
#23947 = CARTESIAN_POINT ( 'NONE',  ( 134.0664832912740110, -41.22944715994101017, 4.925625275910997303 ) ) ;
#23948 = ORIENTED_CLOSED_SHELL ( 'NONE', *, #35820, .F. );
#23949 = VERTEX_POINT ( 'NONE', #26193 ) ;
#23950 = CARTESIAN_POINT ( 'NONE',  ( 147.0667039024470455, -124.3811607159765060, 245.5761019086199894 ) ) ;
#23951 = ORIENTED_EDGE ( 'NONE', *, *, #41903, .F. ) ;
#23952 = ORIENTED_EDGE ( 'NONE', *, *, #18001, .F. ) ;
#23953 = VECTOR ( 'NONE', #69582, 1000.000000000000000 ) ;
#23954 = DIRECTION ( 'NONE',  ( 0.9068632946707805287, -0.4214249218767880389, 9.068632946707802473E-16 ) ) ;
#23955 = AXIS2_PLACEMENT_3D ( 'NONE', #6137, #32469, #39299 ) ;
#23956 = CARTESIAN_POINT ( 'NONE',  ( 51.23005224011598102, -33.89581943344511217, -5.074374724088000832 ) ) ;
#23957 = CARTESIAN_POINT ( 'NONE',  ( 107.8683683300076837, -26.33502505738635691, 70.01562527591099183 ) ) ;
#23958 = DIRECTION ( 'NONE',  ( -1.000000000000000000, -4.163336342344275811E-14, 0.000000000000000000 ) ) ;
#23959 = AXIS2_PLACEMENT_3D ( 'NONE', #76879, #62784, #6484 ) ;
#23960 = DIRECTION ( 'NONE',  ( -1.000000000000000078E-15, -9.367723249499513438E-31, 1.000000000000000000 ) ) ;
#23961 = DIRECTION ( 'NONE',  ( 0.000000000000000000, 1.000000000000000000, 0.000000000000000000 ) ) ;
#23962 = CARTESIAN_POINT ( 'NONE',  ( 104.2296407737279509, -46.70397019442136610, 67.36800622829292706 ) ) ;
#23964 = CARTESIAN_POINT ( 'NONE',  ( 117.4654710391979222, -40.40706546494229201, 174.5680062282919778 ) ) ;
#23963 = DIRECTION ( 'NONE',  ( 1.000000000000000000, 0.000000000000000000, -0.000000000000000000 ) ) ;
#23965 = DIRECTION ( 'NONE',  ( 0.000000000000000000, 0.000000000000000000, -1.000000000000000000 ) ) ;
#23966 = EDGE_CURVE ( 'NONE', #70579, #85819, #76587, .T. ) ;
#23967 = DIRECTION ( 'NONE',  ( 3.999999999999999995E-14, -1.000000000000000000, 4.100000000000000342E-29 ) ) ;
#23968 = ORIENTED_EDGE ( 'NONE', *, *, #37643, .F. ) ;
#23969 = DIRECTION ( 'NONE',  ( 1.000000000000000000, 0.000000000000000000, 1.261617073437676668E-15 ) ) ;
#23970 = VECTOR ( 'NONE', #52090, 1000.000000000000000 ) ;
#23971 = PLANE ( 'NONE',  #89160 ) ;
#23972 = EDGE_CURVE ( 'NONE', #59961, #67197, #26635, .T. ) ;
#23973 = DIRECTION ( 'NONE',  ( -3.100000000000000258E-29, 3.100000000000000044E-14, 1.000000000000000000 ) ) ;
#23974 = DIRECTION ( 'NONE',  ( 3.999999999999999995E-14, -1.000000000000000000, 4.100000000000000342E-29 ) ) ;
#23976 = ORIENTED_EDGE ( 'NONE', *, *, #3959, .F. ) ;
#23975 = CARTESIAN_POINT ( 'NONE',  ( 97.01576029581003979, -41.44069443601846814, 211.6632443235299945 ) ) ;
#23977 = EDGE_CURVE ( 'NONE', #49045, #83730, #53864, .T. ) ;
#23978 = DIRECTION ( 'NONE',  ( 0.000000000000000000, 0.000000000000000000, 1.000000000000000000 ) ) ;
#23979 = CARTESIAN_POINT ( 'NONE',  ( 103.0821958934680111, -47.91639064866039632, 248.3041967044829619 ) ) ;
#23980 = CARTESIAN_POINT ( 'NONE',  ( 107.2328990581281687, -25.63125793145087172, 76.07657765686298035 ) ) ;
#23981 = DIRECTION ( 'NONE',  ( -2.999999999999999839E-15, 1.000000000000000000, -2.999999999999999900E-30 ) ) ;
#23982 = CARTESIAN_POINT ( 'NONE',  ( 97.81021718220807770, -40.51802218317752846, 192.6354414398782353 ) ) ;
#23983 = CIRCLE ( 'NONE', #19616, 10.04999999999999361 ) ;
#23984 = CARTESIAN_POINT ( 'NONE',  ( 221.2791280605339921, 36.86249999999999716, -58.73749999999999716 ) ) ;
#23985 = DIRECTION ( 'NONE',  ( -2.108231265501709878E-16, 0.000000000000000000, 1.000000000000000000 ) ) ;
#23986 = VERTEX_POINT ( 'NONE', #13462 ) ;
#23987 = VECTOR ( 'NONE', #22418, 1000.000000000000000 ) ;
#23988 = ORIENTED_EDGE ( 'NONE', *, *, #64438, .F. ) ;
#23989 = EDGE_LOOP ( 'NONE', ( #87441, #80978, #8466, #35575 ) ) ;
#23990 = ADVANCED_FACE ( 'NONE', ( #41147 ), #82968, .F. ) ;
#23991 = ORIENTED_EDGE ( 'NONE', *, *, #81901, .T. ) ;
#23992 = DIRECTION ( 'NONE',  ( 0.000000000000000000, 0.000000000000000000, 1.000000000000000000 ) ) ;
#23993 = CARTESIAN_POINT ( 'NONE',  ( 95.23138046818854718, -37.33356364299761054, 267.3670538473395482 ) ) ;
#23994 = DIRECTION ( 'NONE',  ( 1.000000000000000000, 0.000000000000000000, 0.000000000000000000 ) ) ;
#23995 = ADVANCED_FACE ( 'NONE', ( #27090 ), #20724, .T. ) ;
#23996 = CARTESIAN_POINT ( 'NONE',  ( 131.4596324495014130, -35.85248396559212125, 2.902015641457837969 ) ) ;
#23998 = CARTESIAN_POINT ( 'NONE',  ( 77.45828646618581104, 73.28361289573329884, 89.75424775947740841 ) ) ;
#23997 = CARTESIAN_POINT ( 'NONE',  ( 55.11501535284990183, 0.000000000000000000, 183.9403141659174992 ) ) ;
#23999 = FACE_OUTER_BOUND ( 'NONE', #89762, .T. ) ;
#24000 = CARTESIAN_POINT ( 'NONE',  ( 109.5125757112413822, -28.00996883845181173, 219.2933722090289734 ) ) ;
#24001 = ORIENTED_EDGE ( 'NONE', *, *, #2414, .F. ) ;
#24002 = VERTEX_POINT ( 'NONE', #40257 ) ;
#24003 = AXIS2_PLACEMENT_3D ( 'NONE', #6398, #75454, #33660 ) ;
#24004 = ORIENTED_EDGE ( 'NONE', *, *, #18218, .F. ) ;
#24005 = PLANE ( 'NONE',  #60100 ) ;
#24006 = AXIS2_PLACEMENT_3D ( 'NONE', #86765, #39931, #5434 ) ;
#24007 = CARTESIAN_POINT ( 'NONE',  ( 97.81221995309677197, -40.51872308918434840, 181.6357364503598433 ) ) ;
#24008 = CARTESIAN_POINT ( 'NONE',  ( 97.40014589274353796, -35.23768424668793386, 262.2041967044816602 ) ) ;
#24009 = DIRECTION ( 'NONE',  ( -0.9068632946707805287, 0.4214249218767882610, -9.068632946707800501E-16 ) ) ;
#24010 = CARTESIAN_POINT ( 'NONE',  ( 115.8238554372424289, -31.72729253430197360, 174.2400402683865650 ) ) ;
#24011 = FACE_OUTER_BOUND ( 'NONE', #60229, .T. ) ;
#24012 = ORIENTED_EDGE ( 'NONE', *, *, #24168, .F. ) ;
#24013 = CARTESIAN_POINT ( 'NONE',  ( 107.9683749031584341, -26.74872499883632315, 56.00468566283465321 ) ) ;
#24014 = ORIENTED_EDGE ( 'NONE', *, *, #80736, .T. ) ;
#24015 = CARTESIAN_POINT ( 'NONE',  ( 0.000000000000000000, 127.0000000000000000, -110.3312500000000114 ) ) ;
#24016 = CARTESIAN_POINT ( 'NONE',  ( 113.6264423535256043, -41.63348889605062908, 26.13380465530496011 ) ) ;
#24017 = AXIS2_PLACEMENT_3D ( 'NONE', #19523, #40852, #21322 ) ;
#24018 = AXIS2_PLACEMENT_3D ( 'NONE', #72810, #30584, #58713 ) ;
#24019 = AXIS2_PLACEMENT_3D ( 'NONE', #89254, #67899, #55133 ) ;
#24020 = FACE_OUTER_BOUND ( 'NONE', #89646, .T. ) ;
#24021 = AXIS2_PLACEMENT_3D ( 'NONE', #3159, #72199, #9084 ) ;
#24022 = ADVANCED_FACE ( 'NONE', ( #61154, #27532 ), #34792, .T. ) ;
#24023 = CARTESIAN_POINT ( 'NONE',  ( 72.06648329127401098, -45.72944715994106701, 14.92562527591093691 ) ) ;
#24024 = CYLINDRICAL_SURFACE ( 'NONE', #35804, 7.499999999999996447 ) ;
#24025 = AXIS2_PLACEMENT_3D ( 'NONE', #6545, #34242, #19288 ) ;
#24026 = ORIENTED_EDGE ( 'NONE', *, *, #34586, .T. ) ;
#24027 = LINE ( 'NONE', #79446, #18977 ) ;
#24028 = DIRECTION ( 'NONE',  ( -3.100000000000000258E-29, 3.100000000000000044E-14, 1.000000000000000000 ) ) ;
#24029 = ORIENTED_EDGE ( 'NONE', *, *, #20585, .T. ) ;
#24030 = CARTESIAN_POINT ( 'NONE',  ( 96.71459513300293054, -38.23421233548538112, 66.44133956162495735 ) ) ;
#24031 = ORIENTED_EDGE ( 'NONE', *, *, #45758, .F. ) ;
#24032 = CARTESIAN_POINT ( 'NONE',  ( 114.0365971503568119, -41.66641429710976752, 52.75813411379098739 ) ) ;
#24033 = VECTOR ( 'NONE', #37173, 1000.000000000000000 ) ;
#24034 = CARTESIAN_POINT ( 'NONE',  ( 117.0564912681829952, -35.80799090043529276, 89.89887535740403735 ) ) ;
#24035 = CARTESIAN_POINT ( 'NONE',  ( 114.0372341014417543, -43.02906291645705039, 79.68539282970694160 ) ) ;
#24036 = DIRECTION ( 'NONE',  ( -2.981567257902526681E-15, 0.8571673007021100021, 0.5150380749100580413 ) ) ;
#24037 = DIRECTION ( 'NONE',  ( -1.000000000000000000, 0.000000000000000000, 0.000000000000000000 ) ) ;
#24038 = CARTESIAN_POINT ( 'NONE',  ( 131.8339555767850015, -67.87837171461835339, 246.1340590712410119 ) ) ;
#24039 = VECTOR ( 'NONE', #24554, 1000.000000000000000 ) ;
#24040 = CARTESIAN_POINT ( 'NONE',  ( 116.7472758669860013, -31.34730438484761805, 25.24229194257798881 ) ) ;
#24041 = DIRECTION ( 'NONE',  ( 0.9999999853157766072, 0.0001713722456143214551, 0.000000000000000000 ) ) ;
#24042 = ORIENTED_EDGE ( 'NONE', *, *, #51117, .T. ) ;
#24043 = FACE_OUTER_BOUND ( 'NONE', #60038, .T. ) ;
#24044 = EDGE_LOOP ( 'NONE', ( #83251, #50689, #70231, #65490 ) ) ;
#24045 = CARTESIAN_POINT ( 'NONE',  ( 97.96923373944615321, -30.37039525599472256, 156.8289586092439549 ) ) ;
#24046 = EDGE_CURVE ( 'NONE', #24962, #60191, #22513, .T. ) ;
#24047 = CARTESIAN_POINT ( 'NONE',  ( 78.80082187617171030, -21.17731672736319126, 1.873071027758830054 ) ) ;
#24048 = ORIENTED_EDGE ( 'NONE', *, *, #79771, .F. ) ;
#24049 = AXIS2_PLACEMENT_3D ( 'NONE', #5441, #87217, #39050 ) ;
#24050 = ORIENTED_EDGE ( 'NONE', *, *, #7042, .T. ) ;
#24051 = DIRECTION ( 'NONE',  ( 1.000000000000000000, 0.000000000000000000, 0.000000000000000000 ) ) ;
#24052 = CARTESIAN_POINT ( 'NONE',  ( 63.03715912545826683, -46.82818131006018092, 237.4678068554150059 ) ) ;
#24053 = CARTESIAN_POINT ( 'NONE',  ( 107.2379402074490429, -25.61267671046441308, 230.0641967044829812 ) ) ;
#24054 = CARTESIAN_POINT ( 'NONE',  ( 97.77504362009293004, -40.42681596862870208, 126.6273886944452016 ) ) ;
#24055 = CARTESIAN_POINT ( 'NONE',  ( 99.04406178308130393, -42.84125754196290359, 187.8439585994789809 ) ) ;
#24056 = CARTESIAN_POINT ( 'NONE',  ( 96.17756896972203151, -38.62826926382330583, 42.45181575210199298 ) ) ;
#24057 = CARTESIAN_POINT ( 'NONE',  ( 99.50455959988217103, -43.30559304351280048, 42.89599952138878081 ) ) ;
#24058 = ORIENTED_EDGE ( 'NONE', *, *, #52546, .T. ) ;
#24059 = CARTESIAN_POINT ( 'NONE',  ( 97.70650162570946407, -40.25115913408279766, 172.6128377269262728 ) ) ;
#24060 = EDGE_CURVE ( 'NONE', #33552, #46749, #55651, .T. ) ;
#24061 = DIRECTION ( 'NONE',  ( 1.000000000000000000, 0.000000000000000000, 0.000000000000000000 ) ) ;
#24062 = ORIENTED_EDGE ( 'NONE', *, *, #63006, .T. ) ;
#24063 = CIRCLE ( 'NONE', #74825, 1.000000000000000888 ) ;
#24064 = LINE ( 'NONE', #17246, #6839 ) ;
#24065 = CARTESIAN_POINT ( 'NONE',  ( 117.0724333545735902, -35.46694875580925554, 114.9279293202101968 ) ) ;
#24066 = CARTESIAN_POINT ( 'NONE',  ( 98.95962429139160577, -30.20966935044058488, 240.7870538473399620 ) ) ;
#24067 = DIRECTION ( 'NONE',  ( -0.000000000000000000, -1.000000000000000000, 0.000000000000000000 ) ) ;
#24068 = EDGE_CURVE ( 'NONE', #2616, #25068, #27975, .T. ) ;
#24069 = DIRECTION ( 'NONE',  ( 1.000000000000000000, 0.000000000000000000, 0.000000000000000000 ) ) ;
#24070 = DIRECTION ( 'NONE',  ( -0.9254794337955620787, -0.3787978585227822492, 0.000000000000000000 ) ) ;
#24071 = CARTESIAN_POINT ( 'NONE',  ( 102.6292086192877946, -44.02785282196147421, 246.5638483995049626 ) ) ;
#24073 = CARTESIAN_POINT ( 'NONE',  ( 117.2454586689011364, -38.87819698039182015, 59.66133956162595098 ) ) ;
#24072 = PLANE ( 'NONE',  #53356 ) ;
#24074 = CARTESIAN_POINT ( 'NONE',  ( 110.4401826102544533, 62.42991204253968363, 69.62641815663941713 ) ) ;
#24075 = CARTESIAN_POINT ( 'NONE',  ( 118.9539009387050186, -36.16544432761327954, 118.8641967044819836 ) ) ;
#24076 = ORIENTED_EDGE ( 'NONE', *, *, #3231, .F. ) ;
#24077 = CARTESIAN_POINT ( 'NONE',  ( 181.8764988495248929, -33.54226604284360036, 193.9678068554150059 ) ) ;
#24078 = ORIENTED_EDGE ( 'NONE', *, *, #59651, .F. ) ;
#24079 = CARTESIAN_POINT ( 'NONE',  ( 74.98969683741650272, 82.54999999999999716, 358.0130000000000337 ) ) ;
#24080 = DIRECTION ( 'NONE',  ( 0.000000000000000000, 0.000000000000000000, -1.000000000000000000 ) ) ;
#24081 = CARTESIAN_POINT ( 'NONE',  ( 103.4822561620420487, -27.39340619187812820, 276.3681719739503819 ) ) ;
#24083 = ORIENTED_EDGE ( 'NONE', *, *, #73804, .F. ) ;
#24082 = EDGE_CURVE ( 'NONE', #30852, #77060, #47509, .T. ) ;
#24084 = CARTESIAN_POINT ( 'NONE',  ( 97.33774635339761971, -34.07140301938782301, 51.11481945842477614 ) ) ;
#24085 = VERTEX_POINT ( 'NONE', #21178 ) ;
#24086 = PLANE ( 'NONE',  #42199 ) ;
#24087 = CARTESIAN_POINT ( 'NONE',  ( 116.3212776292295842, -32.94146857471309886, 45.13562527591097506 ) ) ;
#24089 = VECTOR ( 'NONE', #64677, 1000.000000000000000 ) ;
#24088 = DIRECTION ( 'NONE',  ( 0.000000000000000000, 1.000000000000000000, 0.000000000000000000 ) ) ;
#24090 = VERTEX_POINT ( 'NONE', #88433 ) ;
#24091 = CARTESIAN_POINT ( 'NONE',  ( 116.5534958752826213, -32.35418074550542400, 104.1699109901969535 ) ) ;
#24092 = VECTOR ( 'NONE', #77288, 1000.000000000000000 ) ;
#24093 = CARTESIAN_POINT ( 'NONE',  ( 2.170823869927923866, 1.527609608640607000E-59, 1.032816895392274876E-12 ) ) ;
#24094 = AXIS2_PLACEMENT_3D ( 'NONE', #75516, #32823, #68698 ) ;
#24095 = DIRECTION ( 'NONE',  ( 1.000000000000000078E-15, -1.000000000000000000, 0.000000000000000000 ) ) ;
#24096 = DIRECTION ( 'NONE',  ( 0.000000000000000000, 0.000000000000000000, 1.000000000000000000 ) ) ;
#24097 = DIRECTION ( 'NONE',  ( 0.000000000000000000, -1.000000000000000000, 0.000000000000000000 ) ) ;
#24098 = ORIENTED_EDGE ( 'NONE', *, *, #22302, .F. ) ;
#24099 = EDGE_CURVE ( 'NONE', #51053, #9116, #75246, .T. ) ;
#24100 = DIRECTION ( 'NONE',  ( 0.000000000000000000, 0.000000000000000000, 1.000000000000000000 ) ) ;
#24101 = EDGE_CURVE ( 'NONE', #63455, #35252, #68873, .T. ) ;
#24102 = FACE_OUTER_BOUND ( 'NONE', #38317, .T. ) ;
#24103 = EDGE_CURVE ( 'NONE', #72149, #51651, #19380, .T. ) ;
#24104 = LINE ( 'NONE', #85001, #16842 ) ;
#24105 = EDGE_CURVE ( 'NONE', #1814, #74222, #34339, .T. ) ;
#24106 = FACE_OUTER_BOUND ( 'NONE', #48290, .T. ) ;
#24107 = CARTESIAN_POINT ( 'NONE',  ( 182.4202572930400095, -33.70561438051981185, 117.4678068554150627 ) ) ;
#24108 = CIRCLE ( 'NONE', #64688, 25.39999999999999858 ) ;
#24109 = ORIENTED_EDGE ( 'NONE', *, *, #17984, .F. ) ;
#24110 = AXIS2_PLACEMENT_3D ( 'NONE', #43408, #64327, #42510 ) ;
#24111 = CARTESIAN_POINT ( 'NONE',  ( 101.9936211249197555, -45.44607164413606171, 33.15645862599451021 ) ) ;
#24112 = CARTESIAN_POINT ( 'NONE',  ( 116.4077482568849007, -39.73851878533132975, 154.5784824187679476 ) ) ;
#24114 = ORIENTED_EDGE ( 'NONE', *, *, #75119, .F. ) ;
#24113 = DIRECTION ( 'NONE',  ( 0.000000000000000000, 0.000000000000000000, -1.000000000000000000 ) ) ;
#24115 = CARTESIAN_POINT ( 'NONE',  ( 116.1702204287673794, -31.76348745224625958, 20.21181575210096071 ) ) ;
#24116 = DIRECTION ( 'NONE',  ( 1.000000000000000000, 6.145690160522439356E-16, 0.000000000000000000 ) ) ;
#24117 = CARTESIAN_POINT ( 'NONE',  ( -7.301849239715819957E-13, 120.6499999999999915, 98.60478223830740774 ) ) ;
#24118 = CARTESIAN_POINT ( 'NONE',  ( 172.5664832912729878, -18.82844715994071194, 318.9256252759120116 ) ) ;
#24119 = VERTEX_POINT ( 'NONE', #5308 ) ;
#24120 = CARTESIAN_POINT ( 'NONE',  ( 132.2857443282839824, -83.77844715994092439, 222.2178068554179902 ) ) ;
#24121 = ORIENTED_EDGE ( 'NONE', *, *, #51904, .F. ) ;
#24122 = ORIENTED_EDGE ( 'NONE', *, *, #82650, .F. ) ;
#24123 = CARTESIAN_POINT ( 'NONE',  ( 104.1527054293246550, -27.79712248444839773, 206.7711071154209606 ) ) ;
#24124 = CARTESIAN_POINT ( 'NONE',  ( 194.5667039024479834, -40.82844715993405771, 300.4678068554149490 ) ) ;
#24125 = CARTESIAN_POINT ( 'NONE',  ( 115.2933828064165311, -33.43605939358163681, 50.56158330589693861 ) ) ;
#24126 = CARTESIAN_POINT ( 'NONE',  ( 23.30833798207798324, 86.33530863199757732, 305.8016272809862812 ) ) ;
#24127 = EDGE_CURVE ( 'NONE', #49254, #23727, #60695, .T. ) ;
#24128 = CARTESIAN_POINT ( 'NONE',  ( 143.0667039024470171, -83.77844715994091018, 45.21780685541799727 ) ) ;
#24129 = FACE_OUTER_BOUND ( 'NONE', #19696, .T. ) ;
#24130 = ORIENTED_EDGE ( 'NONE', *, *, #86056, .T. ) ;
#24131 = FACE_OUTER_BOUND ( 'NONE', #84087, .T. ) ;
#24132 = CARTESIAN_POINT ( 'NONE',  ( 33.96670390244699433, -28.27351298637401200, -5.074374724088000832 ) ) ;
#24133 = ORIENTED_EDGE ( 'NONE', *, *, #19324, .T. ) ;
#24134 = CARTESIAN_POINT ( 'NONE',  ( 115.3062145713272599, -45.21207857638187022, 268.1899109901965517 ) ) ;
#24135 = CARTESIAN_POINT ( 'NONE',  ( 79.06648329127300201, -36.72944715994189835, 361.9756252759079871 ) ) ;
#24136 = ORIENTED_EDGE ( 'NONE', *, *, #64977, .F. ) ;
#24137 = PLANE ( 'NONE',  #88011 ) ;
#24138 = LINE ( 'NONE', #86812, #4101 ) ;
#24139 = DIRECTION ( 'NONE',  ( 0.000000000000000000, 0.000000000000000000, -1.000000000000000000 ) ) ;
#24140 = DIRECTION ( 'NONE',  ( 1.000000000000000078E-15, -1.000000000000000000, 0.000000000000000000 ) ) ;
#24141 = AXIS2_PLACEMENT_3D ( 'NONE', #36550, #77429, #64252 ) ;
#24142 = CARTESIAN_POINT ( 'NONE',  ( 106.8507155540331013, -47.82678659975260160, 223.5489586092439538 ) ) ;
#24144 = CARTESIAN_POINT ( 'NONE',  ( -487.2989999999999782, 18.41194598552320016, 97.63125000000000853 ) ) ;
#24143 = AXIS2_PLACEMENT_3D ( 'NONE', #72725, #79107, #43211 ) ;
#24145 = ORIENTED_EDGE ( 'NONE', *, *, #6288, .F. ) ;
#24146 = VECTOR ( 'NONE', #59121, 1000.000000000000000 ) ;
#24147 = CARTESIAN_POINT ( 'NONE',  ( 110.3857440325295443, -47.32095349711466525, 48.80610146638797175 ) ) ;
#24148 = ADVANCED_FACE ( 'NONE', ( #74790 ), #68431, .F. ) ;
#24149 = LINE ( 'NONE', #51375, #30846 ) ;
#24150 = AXIS2_PLACEMENT_3D ( 'NONE', #10490, #23695, #10929 ) ;
#24151 = CARTESIAN_POINT ( 'NONE',  ( 111.4804840314119758, -26.59568808167472653, 284.7375300378156453 ) ) ;
#24152 = EDGE_CURVE ( 'NONE', #1363, #1202, #14369, .T. ) ;
#24153 = EDGE_LOOP ( 'NONE', ( #43871, #58380, #9682, #27263 ) ) ;
#24154 = EDGE_CURVE ( 'NONE', #38408, #16560, #63083, .T. ) ;
#24155 = CARTESIAN_POINT ( 'NONE',  ( 107.0664832912739968, 25.62155284005901379, 339.0006252759110339 ) ) ;
#24156 = FACE_OUTER_BOUND ( 'NONE', #26292, .T. ) ;
#24157 = DIRECTION ( 'NONE',  ( 0.000000000000000000, -1.000000000000000000, 0.000000000000000000 ) ) ;
#24158 = CARTESIAN_POINT ( 'NONE',  ( 100.1260263088618103, -41.89964850235647020, 109.6661856076859607 ) ) ;
#24159 = CARTESIAN_POINT ( 'NONE',  ( 112.4656099449901916, -45.71435824391657832, 234.0070538473389377 ) ) ;
#24160 = EDGE_CURVE ( 'NONE', #51228, #51923, #23934, .T. ) ;
#24161 = LINE ( 'NONE', #51384, #69658 ) ;
#24162 = ORIENTED_EDGE ( 'NONE', *, *, #46876, .F. ) ;
#24163 = EDGE_CURVE ( 'NONE', #61077, #88430, #74695, .T. ) ;
#24164 = VECTOR ( 'NONE', #83709, 999.9999999999998863 ) ;
#24165 = CARTESIAN_POINT ( 'NONE',  ( 188.5667039024479834, -58.35344715994099829, 295.9678068554150059 ) ) ;
#24166 = ORIENTED_EDGE ( 'NONE', *, *, #4372, .T. ) ;
#24167 = ORIENTED_EDGE ( 'NONE', *, *, #21802, .T. ) ;
#24168 = EDGE_CURVE ( 'NONE', #58062, #7066, #80540, .T. ) ;
#24169 = DIRECTION ( 'NONE',  ( 0.7071067811865101582, 0.7071067811865849873, 0.000000000000000000 ) ) ;
#24170 = ORIENTED_EDGE ( 'NONE', *, *, #27227, .T. ) ;
#24171 = ORIENTED_EDGE ( 'NONE', *, *, #515, .F. ) ;
#24172 = CARTESIAN_POINT ( 'NONE',  ( 100.8880764000450370, -44.70071190640118886, 168.0529670008384926 ) ) ;
#24173 = ADVANCED_FACE ( 'NONE', ( #77039 ), #70670, .F. ) ;
#24174 = CARTESIAN_POINT ( 'NONE',  ( 103.2796802074614817, -27.47417168924152620, 41.38552508622479564 ) ) ;
#24175 = CARTESIAN_POINT ( 'NONE',  ( 106.2553484193443865, -46.40481216151710697, 111.9324198280769735 ) ) ;
#24176 = CARTESIAN_POINT ( 'NONE',  ( 115.9827728363227664, -42.21636132903250171, 18.38705384733896153 ) ) ;
#24177 = EDGE_CURVE ( 'NONE', #38814, #33479, #56575, .T. ) ;
#24178 = DIRECTION ( 'NONE',  ( 4.554376769437570034E-14, -1.000000000000000000, 0.000000000000000000 ) ) ;
#24180 = VERTEX_POINT ( 'NONE', #28425 ) ;
#24179 = ADVANCED_FACE ( 'NONE', ( #36605 ), #49754, .F. ) ;
#24181 = CYLINDRICAL_SURFACE ( 'NONE', #18565, 3.250000000000002665 ) ;
#24182 = VERTEX_POINT ( 'NONE', #35233 ) ;
#24183 = CARTESIAN_POINT ( 'NONE',  ( 7.661254700127822836, 98.64746158385918307, 317.6630000000000109 ) ) ;
#24184 = DIRECTION ( 'NONE',  ( 0.000000000000000000, 0.000000000000000000, -1.000000000000000000 ) ) ;
#24185 = CARTESIAN_POINT ( 'NONE',  ( 51.56670390244799762, -33.35206098992650681, -5.074374724088000832 ) ) ;
#24186 = CARTESIAN_POINT ( 'NONE',  ( 63.03715912545640521, -24.89890238295017255, 180.4678068554151196 ) ) ;
#24187 = ORIENTED_EDGE ( 'NONE', *, *, #49991, .F. ) ;
#24188 = CARTESIAN_POINT ( 'NONE',  ( 116.5821416419259435, -42.35362450032752690, 283.4137205140060587 ) ) ;
#24189 = CARTESIAN_POINT ( 'NONE',  ( 116.8105015878075079, -31.41422314659176607, 20.21181575210195902 ) ) ;
#24191 = CARTESIAN_POINT ( 'NONE',  ( 131.3179999999999836, 53.97500000000000142, 30.16249999999999787 ) ) ;
#24190 = CARTESIAN_POINT ( 'NONE',  ( 72.96458098368650269, 117.4749999999999943, 80.90208098368729850 ) ) ;
#24192 = DIRECTION ( 'NONE',  ( 0.000000000000000000, 0.000000000000000000, -1.000000000000000000 ) ) ;
#24193 = DIRECTION ( 'NONE',  ( 1.000000000000000078E-15, -1.000000000000000083E-30, -1.000000000000000000 ) ) ;
#24194 = DIRECTION ( 'NONE',  ( 0.000000000000000000, -1.000000000000000000, 0.000000000000000000 ) ) ;
#24195 = EDGE_CURVE ( 'NONE', #69092, #64904, #3632, .T. ) ;
#24196 = CARTESIAN_POINT ( 'NONE',  ( 91.91125933621943034, -104.2784471599418339, -11.78219314458200984 ) ) ;
#24197 = ADVANCED_FACE ( 'NONE', ( #7987 ), #70216, .T. ) ;
#24198 = CARTESIAN_POINT ( 'NONE',  ( 112.0663155181265580, -45.48817100771776722, 162.9896579463498369 ) ) ;
#24199 = EDGE_CURVE ( 'NONE', #29616, #45, #43836, .T. ) ;
#24200 = PLANE ( 'NONE',  #5165 ) ;
#24201 = CARTESIAN_POINT ( 'NONE',  ( 118.2557925370599179, -40.78261322564650015, 23.54991099019593292 ) ) ;
#24202 = CARTESIAN_POINT ( 'NONE',  ( 113.5650955083461326, -44.92635950737134465, 164.1099109901969655 ) ) ;
#24203 = CARTESIAN_POINT ( 'NONE',  ( 117.2880962612577349, -38.88719764259226253, 59.66133956162595098 ) ) ;
#24204 = EDGE_CURVE ( 'NONE', #32492, #60843, #50655, .T. ) ;
#24205 = CIRCLE ( 'NONE', #11083, 3.299999999999997158 ) ;
#24207 = CARTESIAN_POINT ( 'NONE',  ( 105.7154773334175815, -46.72385839260719109, 47.46895860948406920 ) ) ;
#24206 = FACE_OUTER_BOUND ( 'NONE', #74682, .T. ) ;
#24208 = CARTESIAN_POINT ( 'NONE',  ( 81.12494507884905204, -34.19118199975294203, 1.799893109327175500 ) ) ;
#24209 = AXIS2_PLACEMENT_3D ( 'NONE', #86480, #58311, #51474 ) ;
#24210 = VECTOR ( 'NONE', #43544, 1000.000000000000000 ) ;
#24211 = VERTEX_POINT ( 'NONE', #51098 ) ;
#24212 = FACE_OUTER_BOUND ( 'NONE', #67695, .T. ) ;
#24213 = ORIENTED_EDGE ( 'NONE', *, *, #32645, .F. ) ;
#24214 = CARTESIAN_POINT ( 'NONE',  ( 97.54819157151555942, -32.61351373332772852, 57.01372051400599616 ) ) ;
#24216 = ORIENTED_EDGE ( 'NONE', *, *, #36466, .F. ) ;
#24215 = CARTESIAN_POINT ( 'NONE',  ( 194.0371591254573218, -24.42818131005407878, 249.9678068554149775 ) ) ;
#24217 = DIRECTION ( 'NONE',  ( 0.7071067811865536790, -0.7071067811865414665, 0.000000000000000000 ) ) ;
#24218 = CARTESIAN_POINT ( 'NONE',  ( 103.6457867198658391, -26.24313906103854066, 206.3394347997209763 ) ) ;
#24219 = DIRECTION ( 'NONE',  ( 0.000000000000000000, 1.000000000000000000, 0.000000000000000000 ) ) ;
#24220 = CARTESIAN_POINT ( 'NONE',  ( 105.4788588808464027, 120.6499999999999915, 3.968750000000405009 ) ) ;
#24221 = FACE_BOUND ( 'NONE', #19902, .T. ) ;
#24222 = CARTESIAN_POINT ( 'NONE',  ( 121.2221484686747317, -94.95109689075241022, -19.26696060647628528 ) ) ;
#24223 = DIRECTION ( 'NONE',  ( -4.237773401492740281E-14, 1.000000000000000000, 0.000000000000000000 ) ) ;
#24224 = CYLINDRICAL_SURFACE ( 'NONE', #81995, 9.999999999999998224 ) ;
#24226 = CARTESIAN_POINT ( 'NONE',  ( 109.3575602964533431, -46.23809593081423941, 132.7641967044829698 ) ) ;
#24225 = VECTOR ( 'NONE', #72756, 1000.000000000000114 ) ;
#24227 = ORIENTED_EDGE ( 'NONE', *, *, #53761, .F. ) ;
#24228 = EDGE_LOOP ( 'NONE', ( #66641, #40463, #74879, #25918 ) ) ;
#24229 = CARTESIAN_POINT ( 'NONE',  ( 97.72568451978753501, -37.74236564027221874, 77.83205949637394383 ) ) ;
#24230 = CLOSED_SHELL ( 'NONE', ( #24261, #43904, #1388, #88028, #36060, #30256, #37908, #43206, #6325, #30529, #70524, #64945, #59102, #51035, #72629 ) ) ;
#24231 = CYLINDRICAL_SURFACE ( 'NONE', #70450, 2.749999999999974687 ) ;
#24233 = LINE ( 'NONE', #16087, #82528 ) ;
#24232 = CARTESIAN_POINT ( 'NONE',  ( 100.2051353121705546, -29.75912871662447756, 221.6956252759109702 ) ) ;
#24234 = LINE ( 'NONE', #51900, #66703 ) ;
#24235 = PLANE ( 'NONE',  #77169 ) ;
#24236 = CARTESIAN_POINT ( 'NONE',  ( 117.9723322394569891, 77.68452076096559722, 11.75283433610099593 ) ) ;
#24237 = DIRECTION ( 'NONE',  ( -0.7071067811865739960, 0.000000000000000000, -0.7071067811865210384 ) ) ;
#24238 = CARTESIAN_POINT ( 'NONE',  ( 184.5664832912740110, 25.62155284005901379, 323.8756252759109202 ) ) ;
#24239 = CARTESIAN_POINT ( 'NONE',  ( 173.9900000000000091, 101.5999999999999943, 131.6533725204182019 ) ) ;
#24240 = CARTESIAN_POINT ( 'NONE',  ( 113.3182355088851381, -45.04474967211709924, 143.0899109901969553 ) ) ;
#24241 = ORIENTED_EDGE ( 'NONE', *, *, #41359, .F. ) ;
#24242 = ORIENTED_EDGE ( 'NONE', *, *, #24177, .T. ) ;
#24243 = CARTESIAN_POINT ( 'NONE',  ( 74.81190481564590300, -74.97944988200733007, 248.4067532124560103 ) ) ;
#24244 = CARTESIAN_POINT ( 'NONE',  ( 145.9361736036992454, -68.96302025968714133, 247.2980205078839333 ) ) ;
#24245 = CARTESIAN_POINT ( 'NONE',  ( 104.4081006469831578, -46.45808913634610349, 78.36479194142131632 ) ) ;
#24246 = CARTESIAN_POINT ( 'NONE',  ( 115.7830029644259611, -41.80249729622526189, 104.4064416391778565 ) ) ;
#24247 = AXIS2_PLACEMENT_3D ( 'NONE', #68990, #26748, #41709 ) ;
#24248 = CARTESIAN_POINT ( 'NONE',  ( 142.0664832912740110, -9.729447159940995959, -4.824374724088994704 ) ) ;
#24249 = ADVANCED_FACE ( 'NONE', ( #718 ), #64306, .F. ) ;
#24250 = CARTESIAN_POINT ( 'NONE',  ( 112.4862084254573631, -26.19061110901967382, 169.6984824187679521 ) ) ;
#24251 = ADVANCED_FACE ( 'NONE', ( #22088 ), #71574, .T. ) ;
#24252 = CARTESIAN_POINT ( 'NONE',  ( 135.2499210002644361, -39.21189388395509923, 8.006199623927603426 ) ) ;
#24253 = ORIENTED_EDGE ( 'NONE', *, *, #55152, .F. ) ;
#24255 = VERTEX_POINT ( 'NONE', #28888 ) ;
#24254 = VERTEX_POINT ( 'NONE', #8904 ) ;
#24256 = EDGE_CURVE ( 'NONE', #4393, #78803, #77479, .T. ) ;
#24257 = CARTESIAN_POINT ( 'NONE',  ( 97.81801690659570170, -40.53285193764387628, 62.63741732645588911 ) ) ;
#24258 = FACE_OUTER_BOUND ( 'NONE', #51007, .T. ) ;
#24259 = DIRECTION ( 'NONE',  ( 0.000000000000000000, 1.000000000000000000, 0.000000000000000000 ) ) ;
#24260 = CARTESIAN_POINT ( 'NONE',  ( 103.0821812797523194, -45.97846664716049503, 283.6844404487542874 ) ) ;
#24261 = ADVANCED_FACE ( 'NONE', ( #57473 ), #85213, .T. ) ;
#24262 = CARTESIAN_POINT ( 'NONE',  ( 50.88849390559499142, -32.11662333284530746, 342.9256252759119548 ) ) ;
#24263 = ORIENTED_EDGE ( 'NONE', *, *, #13023, .T. ) ;
#24264 = AXIS2_PLACEMENT_3D ( 'NONE', #8455, #36153, #63869 ) ;
#24265 = VECTOR ( 'NONE', #22227, 1000.000000000000000 ) ;
#24266 = CARTESIAN_POINT ( 'NONE',  ( 108.9246099533292238, -44.86580503303185452, 9.635625275910941312 ) ) ;
#24267 = CARTESIAN_POINT ( 'NONE',  ( 82.81648064515530905, -18.72944715939135207, 6.749772901088279653 ) ) ;
#24268 = VERTEX_POINT ( 'NONE', #73329 ) ;
#24269 = ORIENTED_EDGE ( 'NONE', *, *, #44119, .F. ) ;
#24270 = EDGE_CURVE ( 'NONE', #35318, #18758, #48530, .T. ) ;
#24271 = AXIS2_PLACEMENT_3D ( 'NONE', #4639, #72349, #38259 ) ;
#24272 = CIRCLE ( 'NONE', #75035, 16.09746158385918946 ) ;
#24273 = CARTESIAN_POINT ( 'NONE',  ( 0.000000000000000000, 125.7300000000000040, 0.000000000000000000 ) ) ;
#24274 = CIRCLE ( 'NONE', #46018, 16.00000000000090239 ) ;
#24275 = ORIENTED_EDGE ( 'NONE', *, *, #30381, .T. ) ;
#24276 = ORIENTED_EDGE ( 'NONE', *, *, #43628, .T. ) ;
#24277 = CYLINDRICAL_SURFACE ( 'NONE', #19702, 12.59999999999999964 ) ;
#24278 = EDGE_CURVE ( 'NONE', #87961, #74649, #4303, .T. ) ;
#24279 = CARTESIAN_POINT ( 'NONE',  ( 110.3271547037548004, -45.17815799167961899, 17.28003887569495944 ) ) ;
#24280 = CARTESIAN_POINT ( 'NONE',  ( 114.9947137121727820, -28.99390558034420451, 194.4537205140059370 ) ) ;
#24281 = CARTESIAN_POINT ( 'NONE',  ( 102.0922439024870982, -27.59239485085791088, 145.4727681330539610 ) ) ;
#24282 = CARTESIAN_POINT ( 'NONE',  ( 0.000000000000000000, 65.60000000000000853, 0.000000000000000000 ) ) ;
#24283 = CARTESIAN_POINT ( 'NONE',  ( 115.6952998724001560, -42.57974731087075071, 269.3527681330536439 ) ) ;
#24284 = CARTESIAN_POINT ( 'NONE',  ( 98.30749083302823976, -41.72877197732193366, 97.74043806258440270 ) ) ;
#24285 = CARTESIAN_POINT ( 'NONE',  ( -130.5480269016124453, 69.93117631934792655, 1.660224752218731892 ) ) ;
#24286 = ORIENTED_EDGE ( 'NONE', *, *, #56022, .T. ) ;
#24287 = EDGE_CURVE ( 'NONE', #68689, #88451, #31993, .T. ) ;
#24288 = ORIENTED_EDGE ( 'NONE', *, *, #29123, .F. ) ;
#24289 = AXIS2_PLACEMENT_3D ( 'NONE', #50132, #30154, #28351 ) ;
#24290 = ADVANCED_FACE ( 'NONE', ( #44275 ), #37927, .T. ) ;
#24291 = AXIS2_PLACEMENT_3D ( 'NONE', #259, #21618, #35669 ) ;
#24292 = CARTESIAN_POINT ( 'NONE',  ( 98.63028220664102719, -30.46987006685205657, 180.8184824187679567 ) ) ;
#24293 = VERTEX_POINT ( 'NONE', #10656 ) ;
#24294 = CARTESIAN_POINT ( 'NONE',  ( 114.2400596693416475, -45.14401474321602592, 153.1508633711489722 ) ) ;
#24295 = CARTESIAN_POINT ( 'NONE',  ( 97.31587469920060585, -39.30605313440615589, 266.5315195702721667 ) ) ;
#24296 = CARTESIAN_POINT ( 'NONE',  ( 73.06648329127401098, -46.72944715994108122, 14.82207188531766029 ) ) ;
#24297 = LINE ( 'NONE', #79719, #52203 ) ;
#24298 = CARTESIAN_POINT ( 'NONE',  ( 123.0079629938350223, -38.09664315643626509, 293.9356252759109793 ) ) ;
#24301 = CARTESIAN_POINT ( 'NONE',  ( 110.0853110376240664, -46.03288293484944660, 8.827053847338950376 ) ) ;
#24300 = CARTESIAN_POINT ( 'NONE',  ( 37.03715912545349198, -48.62818131006128652, 117.4678068554150485 ) ) ;
#24299 = DIRECTION ( 'NONE',  ( -1.000000000000000078E-15, 1.000000000000000000, 0.000000000000000000 ) ) ;
#24302 = CARTESIAN_POINT ( 'NONE',  ( 59.56670390244699576, -67.87844715994098976, 190.2178068554179902 ) ) ;
#24303 = DIRECTION ( 'NONE',  ( 0.000000000000000000, 0.000000000000000000, 1.000000000000000000 ) ) ;
#24304 = CYLINDRICAL_SURFACE ( 'NONE', #62959, 4.875000000000017764 ) ;
#24305 = CARTESIAN_POINT ( 'NONE',  ( 68.18421604846717798, -137.1080028910827480, 247.3042482208074944 ) ) ;
#24306 = FACE_OUTER_BOUND ( 'NONE', #46014, .T. ) ;
#24307 = CARTESIAN_POINT ( 'NONE',  ( 126.9629299006806065, -46.62589376934779750, -5.074374724088961841 ) ) ;
#24309 = ORIENTED_EDGE ( 'NONE', *, *, #55474, .T. ) ;
#24308 = CARTESIAN_POINT ( 'NONE',  ( 104.9500019498489252, -44.48156792823318995, 195.5838068554170377 ) ) ;
#24310 = CARTESIAN_POINT ( 'NONE',  ( 149.4430470701762488, -12.91565541735124256, 378.4756252759100335 ) ) ;
#24311 = CARTESIAN_POINT ( 'NONE',  ( 117.5094658089964241, -40.42262428419060427, 178.5680062282919778 ) ) ;
#24312 = CARTESIAN_POINT ( 'NONE',  ( 98.09687384527185827, -31.41638835794072193, 81.90133956162493689 ) ) ;
#24313 = CARTESIAN_POINT ( 'NONE',  ( 117.3777842326014706, -34.92111847156615312, 239.9641967044819637 ) ) ;
#24314 = FACE_OUTER_BOUND ( 'NONE', #72331, .T. ) ;
#24315 = EDGE_CURVE ( 'NONE', #62435, #38828, #86405, .T. ) ;
#24316 = CARTESIAN_POINT ( 'NONE',  ( 81.84766347661003749, -124.7784471599409670, 45.21780685541799727 ) ) ;
#24318 = FACE_OUTER_BOUND ( 'NONE', #63090, .T. ) ;
#24317 = DIRECTION ( 'NONE',  ( 1.000000000000000000, 0.000000000000000000, 0.000000000000000000 ) ) ;
#24319 = DIRECTION ( 'NONE',  ( 0.000000000000000000, 1.000000000000000000, 0.000000000000000000 ) ) ;
#24320 = PLANE ( 'NONE',  #71689 ) ;
#24321 = DIRECTION ( 'NONE',  ( -1.000000000000000078E-15, 1.000000000000000000, 0.000000000000000000 ) ) ;
#24322 = ORIENTED_EDGE ( 'NONE', *, *, #2946, .F. ) ;
#24323 = ORIENTED_EDGE ( 'NONE', *, *, #53717, .F. ) ;
#24324 = CARTESIAN_POINT ( 'NONE',  ( 99.03715563995052662, -32.54106229299839725, 90.35432458998199934 ) ) ;
#24326 = EDGE_LOOP ( 'NONE', ( #82026, #34743, #10675, #86111 ) ) ;
#24325 = CARTESIAN_POINT ( 'NONE',  ( -12.27464498081148214, 85.83590841536251048, -129.9777558447946717 ) ) ;
#24327 = CARTESIAN_POINT ( 'NONE',  ( 97.24623519876082867, -31.70684325556598893, 91.96229194257693962 ) ) ;
#24328 = DIRECTION ( 'NONE',  ( 0.000000000000000000, -1.000000000000000000, 0.000000000000000000 ) ) ;
#24329 = CARTESIAN_POINT ( 'NONE',  ( 122.2221484686747317, -96.68314769832106492, -11.78219314458223188 ) ) ;
#24330 = ADVANCED_FACE ( 'NONE', ( #38810 ), #52406, .F. ) ;
#24331 = CARTESIAN_POINT ( 'NONE',  ( 182.0667039024480118, -32.29483332968430886, -5.074374724088000832 ) ) ;
#24332 = AXIS2_PLACEMENT_3D ( 'NONE', #36898, #1495, #64607 ) ;
#24333 = CARTESIAN_POINT ( 'NONE',  ( 109.4546162266718454, -25.87086512622375878, 29.90419670448296685 ) ) ;
#24334 = ORIENTED_EDGE ( 'NONE', *, *, #87426, .T. ) ;
#24335 = VERTEX_POINT ( 'NONE', #4748 ) ;
#24336 = ORIENTED_EDGE ( 'NONE', *, *, #6244, .T. ) ;
#24337 = EDGE_CURVE ( 'NONE', #68275, #74036, #77688, .T. ) ;
#24338 = AXIS2_PLACEMENT_3D ( 'NONE', #45731, #52099, #23994 ) ;
#24339 = AXIS2_PLACEMENT_3D ( 'NONE', #56933, #22435, #15624 ) ;
#24340 = CARTESIAN_POINT ( 'NONE',  ( 20.03715912545644073, -24.42818131006202265, 129.9678068554150627 ) ) ;
#24341 = DIRECTION ( 'NONE',  ( -4.237773401492740281E-14, 1.000000000000000000, 0.000000000000000000 ) ) ;
#24342 = LINE ( 'NONE', #43875, #84061 ) ;
#24343 = DIRECTION ( 'NONE',  ( 0.000000000000000000, 0.000000000000000000, 1.000000000000000000 ) ) ;
#24344 = DIRECTION ( 'NONE',  ( 0.000000000000000000, 0.000000000000000000, 1.000000000000000000 ) ) ;
#24345 = CARTESIAN_POINT ( 'NONE',  ( 2.883802008152356322, 70.17481864577712258, -130.5247784292598112 ) ) ;
#24346 = DIRECTION ( 'NONE',  ( 0.000000000000000000, -1.000000000000000000, 0.000000000000000000 ) ) ;
#24347 = AXIS2_PLACEMENT_3D ( 'NONE', #33939, #19876, #27136 ) ;
#24348 = CARTESIAN_POINT ( 'NONE',  ( -10.58606582829696308, 89.56609333295101294, 130.1261100651620950 ) ) ;
#24349 = CARTESIAN_POINT ( 'NONE',  ( 106.9276426037745011, -26.29176787048580266, 60.08705384733897858 ) ) ;
#24350 = ORIENTED_EDGE ( 'NONE', *, *, #24943, .F. ) ;
#24351 = ORIENTED_EDGE ( 'NONE', *, *, #30213, .T. ) ;
#24352 = CIRCLE ( 'NONE', #37443, 0.5000000000000016653 ) ;
#24353 = CARTESIAN_POINT ( 'NONE',  ( 10.33024153997673089, 89.94921403597288645, 130.1468737228267685 ) ) ;
#24354 = CARTESIAN_POINT ( 'NONE',  ( 126.7387501644084722, 47.09211651945648924, 31.33975947824927388 ) ) ;
#24355 = VECTOR ( 'NONE', #70492, 1000.000000000000000 ) ;
#24356 = CIRCLE ( 'NONE', #20007, 24.50000000000000711 ) ;
#24357 = CARTESIAN_POINT ( 'NONE',  ( 84.56587091301777548, -120.1789271773121186, 250.2178068554179902 ) ) ;
#24358 = CARTESIAN_POINT ( 'NONE',  ( 100.1874667927473439, -32.28399744105692548, 143.6880903695909524 ) ) ;
#24359 = AXIS2_PLACEMENT_3D ( 'NONE', #34142, #61840, #1439 ) ;
#24360 = EDGE_CURVE ( 'NONE', #63598, #44371, #46049, .T. ) ;
#24361 = ADVANCED_FACE ( 'NONE', ( #66967 ), #87866, .T. ) ;
#24362 = DIRECTION ( 'NONE',  ( -1.000000000000000000, -4.299999999999999979E-14, -1.000000000000000078E-15 ) ) ;
#24363 = ORIENTED_EDGE ( 'NONE', *, *, #22979, .T. ) ;
#24364 = ORIENTED_EDGE ( 'NONE', *, *, #20576, .F. ) ;
#24365 = PLANE ( 'NONE',  #7581 ) ;
#24366 = EDGE_CURVE ( 'NONE', #59170, #19054, #74678, .T. ) ;
#24367 = EDGE_LOOP ( 'NONE', ( #77806, #14373, #81585, #24930 ) ) ;
#24368 = VERTEX_POINT ( 'NONE', #54201 ) ;
#24369 = CARTESIAN_POINT ( 'NONE',  ( 115.7580415341064111, -34.85356206270782309, 180.4272975916109374 ) ) ;
#24370 = EDGE_CURVE ( 'NONE', #19996, #83706, #55097, .T. ) ;
#24371 = DIRECTION ( 'NONE',  ( -3.100000000000000258E-29, 3.100000000000000044E-14, 1.000000000000000000 ) ) ;
#24372 = AXIS2_PLACEMENT_3D ( 'NONE', #60526, #60990, #88274 ) ;
#24373 = CARTESIAN_POINT ( 'NONE',  ( 102.0670550486025121, -27.97049800993343993, 120.4897919345716133 ) ) ;
#24374 = AXIS2_PLACEMENT_3D ( 'NONE', #62840, #76935, #1075 ) ;
#24375 = CARTESIAN_POINT ( 'NONE',  ( 110.8567118704325623, -45.98332038337609617, 17.88581783518143453 ) ) ;
#24376 = VERTEX_POINT ( 'NONE', #26087 ) ;
#24377 = EDGE_CURVE ( 'NONE', #26375, #40569, #89666, .T. ) ;
#24378 = VERTEX_POINT ( 'NONE', #41480 ) ;
#24379 = VERTEX_POINT ( 'NONE', #33790 ) ;
#24380 = EDGE_CURVE ( 'NONE', #19753, #9456, #5194, .T. ) ;
#24381 = B_SPLINE_CURVE_WITH_KNOTS ( 'NONE', 3,
 ( #15923, #9550, #71339, #64515, #56784, #29999, #85869, #64958, #84533, #22290, #76794, #57689, #9111, #85432, #23207, #50874, #44044, #71779, #78612, #37255, #30442, #58137, #943, #59901, #31311, #52623, #11320, #4516, #65832, #66731, #52180, #87192, #38139, #10436, #16811, #3616, #87633, #39021 ),
 .UNSPECIFIED., .F., .F.,
 ( 4, 2, 2, 1, 2, 2, 2, 2, 1, 1, 2, 2, 2, 1, 2, 2, 1, 2, 1, 2, 2, 4 ),
 ( 0.000000000000000000, 0.04166793602358854348, 0.05208492002948607313, 0.05729341203243450142, 0.05989765803390947191, 0.06250190403538444239, 0.08333587204719075658, 0.1041698400589970708, 0.1145868240649016850, 0.1197953160678549983, 0.1223995620693313774, 0.1250038080708077703, 0.1666717440944421869, 0.1770887281003535874, 0.1822972201033092876, 0.1875057121062650156, 0.2083396801180918412, 0.2291736481299186945, 0.2395906321358344804, 0.2447991241387921235, 0.2500076161417498222, 0.3333434881890884882 ),
 .UNSPECIFIED. ) ;
#24382 = CARTESIAN_POINT ( 'NONE',  ( 111.0898924481313941, -43.83169361959101451, 210.8052332267339750 ) ) ;
#24383 = B_SPLINE_CURVE_WITH_KNOTS ( 'NONE', 3,
 ( #37579, #44820, #66152, #52500 ),
 .UNSPECIFIED., .F., .F.,
 ( 4, 4 ),
 ( -0.6035999334370359959, -0.5903216970416040876 ),
 .UNSPECIFIED. ) ;
#24384 = CARTESIAN_POINT ( 'NONE',  ( 107.3215719809018083, -25.65558735872630081, 75.04610146638695767 ) ) ;
#24385 = CARTESIAN_POINT ( 'NONE',  ( 111.3142535964730797, -27.23286288913589459, 24.74133956162494030 ) ) ;
#24386 =( NAMED_UNIT ( * ) SI_UNIT ( $, .STERADIAN. ) SOLID_ANGLE_UNIT ( ) );
#24387 = CARTESIAN_POINT ( 'NONE',  ( 177.1649999999999920, 14.63749999999999929, -19.05000000000000071 ) ) ;
#24388 = CARTESIAN_POINT ( 'NONE',  ( -179.8898777604659927, 101.5999999999999943, -123.4696824136383952 ) ) ;
#24389 = CARTESIAN_POINT ( 'NONE',  ( 96.65005459693196599, -37.15429219901626823, 157.3584824187679487 ) ) ;
#24390 = PLANE ( 'NONE',  #46547 ) ;
#24391 = ORIENTED_EDGE ( 'NONE', *, *, #47744, .T. ) ;
#24392 = FACE_BOUND ( 'NONE', #67493, .T. ) ;
#24393 = EDGE_LOOP ( 'NONE', ( #18438, #12321, #45767, #61571 ) ) ;
#24394 = ORIENTED_EDGE ( 'NONE', *, *, #40348, .F. ) ;
#24395 = DIRECTION ( 'NONE',  ( 0.000000000000000000, 1.000000000000000000, 0.000000000000000000 ) ) ;
#24396 = DIRECTION ( 'NONE',  ( 0.000000000000000000, 0.000000000000000000, -1.000000000000000000 ) ) ;
#24397 = VERTEX_POINT ( 'NONE', #47848 ) ;
#24398 = CIRCLE ( 'NONE', #73800, 5.599999999999994316 ) ;
#24399 = CARTESIAN_POINT ( 'NONE',  ( 143.5667039024469886, -67.87844715994090450, 222.2178068554179902 ) ) ;
#24400 = VECTOR ( 'NONE', #31324, 1000.000000000000000 ) ;
#24401 = ORIENTED_EDGE ( 'NONE', *, *, #46424, .F. ) ;
#24402 = CARTESIAN_POINT ( 'NONE',  ( 0.000000000000000000, 95.25000000000000000, 9.525000000000000355 ) ) ;
#24403 = CARTESIAN_POINT ( 'NONE',  ( 104.0426969376867987, -47.36127689622573200, 67.36800622829191809 ) ) ;
#24404 = CARTESIAN_POINT ( 'NONE',  ( 131.3179999999999836, 53.97500000000000142, 50.79999999999999716 ) ) ;
#24405 = CARTESIAN_POINT ( 'NONE',  ( 104.0667030381801936, -67.87844715994094713, 173.2178086137559774 ) ) ;
#24406 = CARTESIAN_POINT ( 'NONE',  ( 100.8874678934932518, -44.70022138198631012, 73.05229194346932786 ) ) ;
#24407 = CARTESIAN_POINT ( 'NONE',  ( 116.7343647603066614, -32.97833357388812914, 94.10895860924495082 ) ) ;
#24409 = CARTESIAN_POINT ( 'NONE',  ( 97.78191787992085438, -41.50032452247405246, 192.7041967044819728 ) ) ;
#24408 = CARTESIAN_POINT ( 'NONE',  ( -446.0240000000000009, 3.174999999999999822, -1.387778780781445991E-14 ) ) ;
#24410 = CARTESIAN_POINT ( 'NONE',  ( 113.2418788616994618, -28.75590518149876118, 59.55265118002041902 ) ) ;
#24411 = FACE_OUTER_BOUND ( 'NONE', #75554, .T. ) ;
#24412 = ORIENTED_EDGE ( 'NONE', *, *, #34723, .F. ) ;
#24413 = DIRECTION ( 'NONE',  ( 0.7071067811743789733, -0.7071067811987160612, 0.000000000000000000 ) ) ;
#24414 = DIRECTION ( 'NONE',  ( 0.000000000000000000, 0.000000000000000000, 1.000000000000000000 ) ) ;
#24415 = CARTESIAN_POINT ( 'NONE',  ( 97.80441965743102628, -40.49963042538360725, 136.6344769046315832 ) ) ;
#24416 = CIRCLE ( 'NONE', #75181, 11.45913725231036118 ) ;
#24417 = FACE_OUTER_BOUND ( 'NONE', #18408, .T. ) ;
#24419 = ORIENTED_EDGE ( 'NONE', *, *, #45751, .T. ) ;
#24418 = CARTESIAN_POINT ( 'NONE',  ( 114.8468557742592822, -29.67128889090990640, 209.4127681330539872 ) ) ;
#24420 = CARTESIAN_POINT ( 'NONE',  ( 97.75843951370882223, -40.38502501680090973, 146.6242685447254246 ) ) ;
#24421 = CARTESIAN_POINT ( 'NONE',  ( 100.8354465997397540, -45.15876371340904427, 253.0699109901969450 ) ) ;
#24422 = CARTESIAN_POINT ( 'NONE',  ( 117.2645927648968183, -42.86211997589052203, 124.3956252759109731 ) ) ;
#24423 = CIRCLE ( 'NONE', #86791, 11.45913725231036118 ) ;
#24424 = CARTESIAN_POINT ( 'NONE',  ( 105.8028360693176495, -26.72358448476759918, 251.1828494030555703 ) ) ;
#24425 = VECTOR ( 'NONE', #51308, 1000.000000000000114 ) ;
#24426 = EDGE_CURVE ( 'NONE', #24335, #30196, #53756, .T. ) ;
#24427 = CARTESIAN_POINT ( 'NONE',  ( 82.51464772713113405, -37.98222059078202761, 7.138441653511359952 ) ) ;
#24428 = DIRECTION ( 'NONE',  ( -0.000000000000000000, 1.000000000000000000, 0.000000000000000000 ) ) ;
#24429 = CARTESIAN_POINT ( 'NONE',  ( 188.5667039024481255, -42.82844715993431350, 257.2178068554150059 ) ) ;
#24430 = VERTEX_POINT ( 'NONE', #68767 ) ;
#24431 = VERTEX_POINT ( 'NONE', #40601 ) ;
#24432 = VERTEX_POINT ( 'NONE', #81963 ) ;
#24433 = VECTOR ( 'NONE', #23191, 1000.000000000000000 ) ;
#24434 = ORIENTED_EDGE ( 'NONE', *, *, #14623, .F. ) ;
#24435 = FACE_OUTER_BOUND ( 'NONE', #49727, .T. ) ;
#24436 = CARTESIAN_POINT ( 'NONE',  ( 116.1395517938576347, -31.55217135963209785, 285.2384824187680579 ) ) ;
#24437 = DIRECTION ( 'NONE',  ( 1.000000000000000000, 0.000000000000000000, 0.000000000000000000 ) ) ;
#24438 = CARTESIAN_POINT ( 'NONE',  ( 132.5731111080349649, -34.41810224487143444, 1.981704920702773043 ) ) ;
#24440 = CARTESIAN_POINT ( 'NONE',  ( 84.41866557162614981, 69.84937538953987257, 83.24493215373445310 ) ) ;
#24439 = CARTESIAN_POINT ( 'NONE',  ( 34.33598329127477911, -36.32844715994133367, 237.4678068554150059 ) ) ;
#24441 = AXIS2_PLACEMENT_3D ( 'NONE', #4584, #25023, #45883 ) ;
#24442 = CARTESIAN_POINT ( 'NONE',  ( 102.2605585157881194, -43.79055321879850027, 196.5238483995059937 ) ) ;
#24443 = ORIENTED_EDGE ( 'NONE', *, *, #3124, .F. ) ;
#24444 = AXIS2_PLACEMENT_3D ( 'NONE', #60160, #25209, #39291 ) ;
#24445 = ORIENTED_EDGE ( 'NONE', *, *, #24370, .F. ) ;
#24446 = ORIENTED_EDGE ( 'NONE', *, *, #52906, .T. ) ;
#24447 = EDGE_CURVE ( 'NONE', #50547, #77225, #75585, .T. ) ;
#24448 = CARTESIAN_POINT ( 'NONE',  ( 51.27381068362099370, -23.19206098993950604, -5.074374724088000832 ) ) ;
#24449 = DIRECTION ( 'NONE',  ( 0.000000000000000000, -1.000000000000000000, 0.000000000000000000 ) ) ;
#24450 = DIRECTION ( 'NONE',  ( 0.000000000000000000, 1.000000000000000000, 0.000000000000000000 ) ) ;
#24451 = CARTESIAN_POINT ( 'NONE',  ( 98.80858115845356338, -33.43260291865056644, 37.45586902018299469 ) ) ;
#24452 = CARTESIAN_POINT ( 'NONE',  ( 117.9171910823873048, 85.85031469618031963, 12.29178224785222895 ) ) ;
#24453 = FACE_OUTER_BOUND ( 'NONE', #49790, .T. ) ;
#24454 = DIRECTION ( 'NONE',  ( 1.000000000000000000, 0.000000000000000000, 0.000000000000000000 ) ) ;
#24455 = ORIENTED_EDGE ( 'NONE', *, *, #7060, .F. ) ;
#24456 = VECTOR ( 'NONE', #75685, 1000.000000000000000 ) ;
#24457 = CARTESIAN_POINT ( 'NONE',  ( 99.08946256649487339, -99.09543445804918349, 2.217806855417836509 ) ) ;
#24458 = VERTEX_POINT ( 'NONE', #48286 ) ;
#24459 = CARTESIAN_POINT ( 'NONE',  ( 162.7866693523300796, -36.02818131005322044, 117.4678068554150485 ) ) ;
#24460 = CARTESIAN_POINT ( 'NONE',  ( 112.5662596640460720, -44.20262526656594559, 30.89951894101994156 ) ) ;
#24461 = AXIS2_PLACEMENT_3D ( 'NONE', #51878, #17391, #59154 ) ;
#24462 = CONICAL_SURFACE ( 'NONE', #75232, 1.258750000000002922, 1.029744258676650093 ) ;
#24463 = CARTESIAN_POINT ( 'NONE',  ( -3.968749999999935163, 120.6499999999999915, -100.8961411191535973 ) ) ;
#24464 = LINE ( 'NONE', #52129, #73684 ) ;
#24465 = EDGE_CURVE ( 'NONE', #67541, #17862, #47181, .T. ) ;
#24466 = FACE_OUTER_BOUND ( 'NONE', #22996, .T. ) ;
#24467 = VERTEX_POINT ( 'NONE', #76020 ) ;
#24468 = DIRECTION ( 'NONE',  ( -1.000000000000000000, 0.000000000000000000, 0.000000000000000000 ) ) ;
#24469 = CIRCLE ( 'NONE', #81094, 3.000000864267343026 ) ;
#24470 = CARTESIAN_POINT ( 'NONE',  ( 120.9217020216711234, 59.09882332812808414, -49.22416681939083816 ) ) ;
#24471 = EDGE_CURVE ( 'NONE', #60222, #9337, #79122, .T. ) ;
#24472 = ORIENTED_EDGE ( 'NONE', *, *, #51404, .F. ) ;
#24473 = CARTESIAN_POINT ( 'NONE',  ( 98.14942788562998999, -43.26130833009477783, 106.8175300378159704 ) ) ;
#24474 = ORIENTED_EDGE ( 'NONE', *, *, #16573, .T. ) ;
#24475 = EDGE_CURVE ( 'NONE', #34264, #85910, #19274, .T. ) ;
#24476 = CARTESIAN_POINT ( 'NONE',  ( 115.5202298134134367, -37.95022619834508504, 28.13527697093398672 ) ) ;
#24477 = CIRCLE ( 'NONE', #47660, 17.00000000000000000 ) ;
#24478 = DIRECTION ( 'NONE',  ( -0.7071067811865501263, 0.7071067811865449082, -7.071067811865501957E-16 ) ) ;
#24479 = CARTESIAN_POINT ( 'NONE',  ( 99.97388925556708728, -42.04201607304819532, 63.27015473446895300 ) ) ;
#24480 = CARTESIAN_POINT ( 'NONE',  ( 115.7823355676851946, -41.80361319518412699, 14.40633917731446445 ) ) ;
#24481 = EDGE_CURVE ( 'NONE', #59994, #61557, #9473, .T. ) ;
#24482 = CARTESIAN_POINT ( 'NONE',  ( 46.83715912545345361, -47.82818131006086304, 117.4678068554150485 ) ) ;
#24483 = LINE ( 'NONE', #24922, #36819 ) ;
#24484 = CARTESIAN_POINT ( 'NONE',  ( 116.4941038412854510, -32.22865339830268283, 15.18133956162492915 ) ) ;
#24485 = DIRECTION ( 'NONE',  ( 1.000000000000000000, 0.000000000000000000, 0.000000000000000000 ) ) ;
#24486 = VERTEX_POINT ( 'NONE', #46948 ) ;
#24487 = CARTESIAN_POINT ( 'NONE',  ( 156.5667039024484666, -42.82844715993568485, 139.7178068554149775 ) ) ;
#24488 = ORIENTED_EDGE ( 'NONE', *, *, #31019, .T. ) ;
#24489 = CARTESIAN_POINT ( 'NONE',  ( 77.61460381940941033, -19.97617057400826468, 2.716753174556971295 ) ) ;
#24490 = ORIENTED_EDGE ( 'NONE', *, *, #15878, .F. ) ;
#24491 = ORIENTED_EDGE ( 'NONE', *, *, #57290, .F. ) ;
#24492 = EDGE_CURVE ( 'NONE', #35045, #66245, #74238, .T. ) ;
#24493 = DIRECTION ( 'NONE',  ( 0.000000000000000000, 0.000000000000000000, 1.000000000000000000 ) ) ;
#24494 = CARTESIAN_POINT ( 'NONE',  ( 109.9476544338203325, -26.76763818355050262, 214.8403871806739289 ) ) ;
#24495 = CARTESIAN_POINT ( 'NONE',  ( 168.3595971213392772, -48.62134037882587023, 180.4678068554150059 ) ) ;
#24496 = CARTESIAN_POINT ( 'NONE',  ( 112.0659115689755083, -45.48839629194433343, 188.9897919376950028 ) ) ;
#24497 = CARTESIAN_POINT ( 'NONE',  ( 103.9574082008755198, -47.33640867427461529, 58.33753003781600199 ) ) ;
#24498 = CARTESIAN_POINT ( 'NONE',  ( 98.38030477604230839, -41.69506886831626957, 42.73974658533858673 ) ) ;
#24499 = ORIENTED_EDGE ( 'NONE', *, *, #53074, .F. ) ;
#24500 = CARTESIAN_POINT ( 'NONE',  ( 115.1227284505533959, -30.77440371158323629, 170.3330730039945706 ) ) ;
#24501 = DIRECTION ( 'NONE',  ( 0.7071067811865460184, 0.000000000000000000, 0.7071067811865487940 ) ) ;
#24503 = ORIENTED_EDGE ( 'NONE', *, *, #85741, .F. ) ;
#24502 = CIRCLE ( 'NONE', #28849, 38.10000000000000142 ) ;
#24504 = LINE ( 'NONE', #32190, #15546 ) ;
#24505 = CARTESIAN_POINT ( 'NONE',  ( 27.27158787008327678, 184.0000000000000000, 85.23828826961327820 ) ) ;
#24506 = CARTESIAN_POINT ( 'NONE',  ( 118.0585799961421429, -32.36802338489820841, 249.1270538473389706 ) ) ;
#24507 = DIRECTION ( 'NONE',  ( -1.000000000000000000, -4.510281037539694659E-14, 0.000000000000000000 ) ) ;
#24508 = CARTESIAN_POINT ( 'NONE',  ( 0.000000000000000000, 1.270000000000000018, 0.000000000000000000 ) ) ;
#24509 = CARTESIAN_POINT ( 'NONE',  ( 78.98444042533921561, -39.25772566032940603, 1.807989669955163414 ) ) ;
#24510 = CARTESIAN_POINT ( 'NONE',  ( 114.8821461825539245, -40.17495804977037466, 252.9181341137911545 ) ) ;
#24512 = CARTESIAN_POINT ( 'NONE',  ( 115.1498815335950638, -43.27828968249928465, 84.28419670448195689 ) ) ;
#24511 = CARTESIAN_POINT ( 'NONE',  ( 1.387778780781445676E-14, 239.0000000000000000, 97.27542076772557778 ) ) ;
#24513 = CARTESIAN_POINT ( 'NONE',  ( 114.9214557239245096, 71.34069570408355787, 61.95106117944241930 ) ) ;
#24514 = CARTESIAN_POINT ( 'NONE',  ( 116.9458863120112539, -40.19413502446316500, 133.5584824187679658 ) ) ;
#24515 = ORIENTED_EDGE ( 'NONE', *, *, #62653, .T. ) ;
#24516 = CARTESIAN_POINT ( 'NONE',  ( 25.56670390244797275, -58.35344715994099829, 295.9678068554150059 ) ) ;
#24517 = ORIENTED_EDGE ( 'NONE', *, *, #24575, .F. ) ;
#24518 = DIRECTION ( 'NONE',  ( 0.000000000000000000, 0.000000000000000000, -1.000000000000000000 ) ) ;
#24519 = CARTESIAN_POINT ( 'NONE',  ( 194.5667039024480403, -40.82844715993405771, 249.9678068554149775 ) ) ;
#24520 = EDGE_LOOP ( 'NONE', ( #62448, #61644, #1293, #6392 ) ) ;
#24521 = AXIS2_PLACEMENT_3D ( 'NONE', #44161, #23320, #65516 ) ;
#24522 = LINE ( 'NONE', #19040, #8478 ) ;
#24524 = VERTEX_POINT ( 'NONE', #67403 ) ;
#24523 = CARTESIAN_POINT ( 'NONE',  ( 117.1490187775317793, -39.54886983357372543, 98.60991099019594230 ) ) ;
#24525 = DIRECTION ( 'NONE',  ( 0.000000000000000000, -1.000000000000000000, 0.000000000000000000 ) ) ;
#24526 = CARTESIAN_POINT ( 'NONE',  ( 44.45000000000000284, 111.1250000000000000, 219.0749999999999886 ) ) ;
#24527 = EDGE_CURVE ( 'NONE', #76266, #49377, #81071, .T. ) ;
#24529 = LINE ( 'NONE', #3198, #51062 ) ;
#24528 = AXIS2_PLACEMENT_3D ( 'NONE', #21312, #76724, #16739 ) ;
#24530 = ORIENTED_EDGE ( 'NONE', *, *, #64063, .F. ) ;
#24531 = VECTOR ( 'NONE', #32272, 1000.000000000000000 ) ;
#24532 = CARTESIAN_POINT ( 'NONE',  ( 109.2596401224901541, -46.98022400537049492, 107.7441967044829880 ) ) ;
#24533 = DIRECTION ( 'NONE',  ( -1.000000000000000000, 0.000000000000000000, -3.745918078535842888E-15 ) ) ;
#24535 = EDGE_CURVE ( 'NONE', #31678, #52430, #13355, .T. ) ;
#24534 = DIRECTION ( 'NONE',  ( 0.000000000000000000, 0.000000000000000000, -1.000000000000000000 ) ) ;
#24536 = CARTESIAN_POINT ( 'NONE',  ( 162.7131505118679797, -31.94127993907790852, -5.074374724088000832 ) ) ;
#24537 = CARTESIAN_POINT ( 'NONE',  ( 141.8664832912739939, -71.52944715994085811, 361.9756252759100335 ) ) ;
#24538 = ORIENTED_EDGE ( 'NONE', *, *, #53290, .F. ) ;
#24539 = AXIS2_PLACEMENT_3D ( 'NONE', #52700, #65480, #66357 ) ;
#24540 = EDGE_LOOP ( 'NONE', ( #32078, #55103, #31639, #24955 ) ) ;
#24541 = CARTESIAN_POINT ( 'NONE',  ( 107.0664832912739968, -0.2185775633790978945, 330.8831252759119934 ) ) ;
#24542 = LINE ( 'NONE', #87216, #32358 ) ;
#24543 = VECTOR ( 'NONE', #38858, 1000.000000000000000 ) ;
#24544 = DIRECTION ( 'NONE',  ( -0.7071067811864691910, -0.7071067811866257324, -7.071067811864685486E-16 ) ) ;
#24546 = FACE_BOUND ( 'NONE', #5819, .T. ) ;
#24545 = LINE ( 'NONE', #52208, #79901 ) ;
#24547 = CARTESIAN_POINT ( 'NONE',  ( -41.60202597009397607, 40.59999999999997300, 50.85338361873603219 ) ) ;
#24548 = EDGE_LOOP ( 'NONE', ( #64182, #5003 ) ) ;
#24549 = EDGE_CURVE ( 'NONE', #69843, #75721, #46503, .T. ) ;
#24550 = CARTESIAN_POINT ( 'NONE',  ( 104.4081008449446983, -46.45808918883411565, 33.36479195756466254 ) ) ;
#24551 = CARTESIAN_POINT ( 'NONE',  ( 96.81359797424460112, -35.17473563989039320, 217.1946728949579608 ) ) ;
#24552 = AXIS2_PLACEMENT_3D ( 'NONE', #69084, #82284, #14118 ) ;
#24553 = B_SPLINE_CURVE_WITH_KNOTS ( 'NONE', 3,
 ( #52705, #80465, #45904, #39110, #54505, #47702, #82268, #20920, #5958, #34538, #27728, #68623, #6387, #61338, #82718, #75442, #40897, #69066, #40456, #61781, #20479, #14104, #7296, #67719, #76324, #48149, #62241, #83163, #6835 ),
 .UNSPECIFIED., .F., .F.,
 ( 4, 2, 2, 2, 2, 2, 2, 2, 2, 2, 1, 1, 1, 1, 1, 2, 4 ),
 ( 0.000000000000000000, 0.06250186912378230542, 0.1250037382475646108, 0.1875056073713469162, 0.2500074764951292217, 0.3125093456189115271, 0.3750112147426938325, 0.4375130838664761379, 0.4687640184283670686, 0.4843894857093126172, 0.4922022193497853082, 0.4961085861700220145, 0.4980617695801402012, 0.4990383612851991835, 0.4995266571377283693, 0.4997708050639932953, 0.5000149529902581103 ),
 .UNSPECIFIED. ) ;
#24555 = EDGE_LOOP ( 'NONE', ( #1702, #70108 ) ) ;
#24554 = DIRECTION ( 'NONE',  ( 0.000000000000000000, -1.000000000000000000, 0.000000000000000000 ) ) ;
#24556 = CARTESIAN_POINT ( 'NONE',  ( 114.5308976578478166, -43.10096916487045604, 59.26419670448196086 ) ) ;
#24557 = CARTESIAN_POINT ( 'NONE',  ( -72.96458098368600531, 127.0000000000000000, -72.96458098368781009 ) ) ;
#24558 = CARTESIAN_POINT ( 'NONE',  ( 165.6738106836196494, -26.00627455219358453, 342.9256252759109884 ) ) ;
#24559 = EDGE_CURVE ( 'NONE', #17862, #65985, #47397, .T. ) ;
#24560 = VERTEX_POINT ( 'NONE', #40142 ) ;
#24561 = CARTESIAN_POINT ( 'NONE',  ( 97.06670390244703128, -104.2784471599412228, 7.717806855417980394 ) ) ;
#24562 = ORIENTED_EDGE ( 'NONE', *, *, #74411, .F. ) ;
#24563 = EDGE_LOOP ( 'NONE', ( #38432, #73467, #40851, #77224 ) ) ;
#24564 = CARTESIAN_POINT ( 'NONE',  ( 98.23266987703472353, -35.71659467859123538, 202.6672975916109465 ) ) ;
#24565 = CARTESIAN_POINT ( 'NONE',  ( 115.5439452383991892, -99.96145986183358900, 2.217806855417864043 ) ) ;
#24566 = CARTESIAN_POINT ( 'NONE',  ( -99.62873342662618370, 89.26666702275852572, 84.37439091330368512 ) ) ;
#24567 = CARTESIAN_POINT ( 'NONE',  ( 152.4409905591762708, -0.9151414768250908383, 394.9756252759102040 ) ) ;
#24568 = DIRECTION ( 'NONE',  ( 0.000000000000000000, 0.000000000000000000, -1.000000000000000000 ) ) ;
#24569 = ORIENTED_EDGE ( 'NONE', *, *, #57475, .T. ) ;
#24570 = CYLINDRICAL_SURFACE ( 'NONE', #46382, 2.999999999999988898 ) ;
#24571 = CARTESIAN_POINT ( 'NONE',  ( 71.24189083761808661, -0.9290567490904538817, 540.9756252759101471 ) ) ;
#24572 = ORIENTED_EDGE ( 'NONE', *, *, #74802, .T. ) ;
#24573 = CARTESIAN_POINT ( 'NONE',  ( 111.8540205700169139, -46.00543295620339990, 272.9556252759110180 ) ) ;
#24574 = DIRECTION ( 'NONE',  ( 0.000000000000000000, 0.000000000000000000, -1.000000000000000000 ) ) ;
#24576 = ORIENTED_EDGE ( 'NONE', *, *, #87650, .T. ) ;
#24575 = EDGE_CURVE ( 'NONE', #59746, #23716, #29839, .T. ) ;
#24577 = AXIS2_PLACEMENT_3D ( 'NONE', #34116, #63178, #56347 ) ;
#24578 = FACE_OUTER_BOUND ( 'NONE', #89172, .T. ) ;
#24579 = DIRECTION ( 'NONE',  ( 0.000000000000000000, -0.8660254037844394848, 0.4999999999999986122 ) ) ;
#24580 = FACE_OUTER_BOUND ( 'NONE', #12825, .T. ) ;
#24581 = DIRECTION ( 'NONE',  ( 0.000000000000000000, 0.000000000000000000, -1.000000000000000000 ) ) ;
#24582 = CARTESIAN_POINT ( 'NONE',  ( 110.5132149073354242, -26.84445748292755951, 205.8099109901969541 ) ) ;
#24584 = DIRECTION ( 'NONE',  ( 5.463695987328529395E-16, 0.000000000000000000, 1.000000000000000000 ) ) ;
#24583 = VECTOR ( 'NONE', #71448, 1000.000000000000000 ) ;
#24585 = CIRCLE ( 'NONE', #60885, 3.000000000000002665 ) ;
#24586 = EDGE_LOOP ( 'NONE', ( #79919, #6358, #33717, #49289 ) ) ;
#24587 = CARTESIAN_POINT ( 'NONE',  ( 96.14773132834588409, -38.72402830165600562, 47.48229194257797303 ) ) ;
#24588 = LINE ( 'NONE', #17772, #20740 ) ;
#24589 = EDGE_LOOP ( 'NONE', ( #89184, #26245, #24058, #1600 ) ) ;
#24590 = EDGE_LOOP ( 'NONE', ( #37389, #8938, #34486, #81597 ) ) ;
#24591 = EDGE_CURVE ( 'NONE', #42455, #17322, #80605, .T. ) ;
#24592 = AXIS2_PLACEMENT_3D ( 'NONE', #1222, #28926, #23018 ) ;
#24593 = CARTESIAN_POINT ( 'NONE',  ( 78.34779240610842521, -38.87777042261290461, 7.743969477056507955 ) ) ;
#24595 = EDGE_CURVE ( 'NONE', #5363, #4177, #84648, .T. ) ;
#24594 = CARTESIAN_POINT ( 'NONE',  ( 97.81483072311490901, -40.51614641965803543, 17.63529977666319937 ) ) ;
#24596 = CARTESIAN_POINT ( 'NONE',  ( 100.8868511195287567, -44.69971074744904627, 152.0528254920112943 ) ) ;
#24597 = CARTESIAN_POINT ( 'NONE',  ( 114.6841822258597148, -33.79680514827971649, 136.9366617981629588 ) ) ;
#24598 = CARTESIAN_POINT ( 'NONE',  ( 106.5662934289835988, -47.19983425457502335, 243.5384824187679556 ) ) ;
#24599 = PLANE ( 'NONE',  #16048 ) ;
#24600 = ORIENTED_EDGE ( 'NONE', *, *, #63577, .F. ) ;
#24601 = AXIS2_PLACEMENT_3D ( 'NONE', #85842, #3156, #17233 ) ;
#24602 = CARTESIAN_POINT ( 'NONE',  ( 135.3687878533317246, -39.15209318185264209, 1.893168666202053041 ) ) ;
#24603 = VERTEX_POINT ( 'NONE', #14703 ) ;
#24604 = ORIENTED_EDGE ( 'NONE', *, *, #2861, .T. ) ;
#24605 = CYLINDRICAL_SURFACE ( 'NONE', #80770, 9.525000000000000355 ) ;
#24606 = EDGE_LOOP ( 'NONE', ( #10294, #23711 ) ) ;
#24607 = ORIENTED_EDGE ( 'NONE', *, *, #8, .T. ) ;
#24608 = DIRECTION ( 'NONE',  ( 1.000000000000000000, 1.261617073437676668E-15, 1.261617073437676668E-15 ) ) ;
#24609 = FACE_OUTER_BOUND ( 'NONE', #55725, .T. ) ;
#24610 = CARTESIAN_POINT ( 'NONE',  ( 51.56670390244899238, -32.29483332968450782, -5.074374724088000832 ) ) ;
#24611 = VECTOR ( 'NONE', #83956, 1000.000000000000000 ) ;
#24612 = CARTESIAN_POINT ( 'NONE',  ( 116.7648798213666623, -36.26930322673007367, 118.2867055423629807 ) ) ;
#24613 = CARTESIAN_POINT ( 'NONE',  ( 118.1222316836501705, -37.72106760768119216, 33.74324432352998571 ) ) ;
#24614 = ORIENTED_EDGE ( 'NONE', *, *, #9677, .T. ) ;
#24615 = CARTESIAN_POINT ( 'NONE',  ( 164.9190312289449878, -35.91149509761181235, -5.074374724088000832 ) ) ;
#24616 = VERTEX_POINT ( 'NONE', #84203 ) ;
#24617 = DIRECTION ( 'NONE',  ( 3.114895971316861016E-16, -1.000000000000000000, 0.000000000000000000 ) ) ;
#24618 = VERTEX_POINT ( 'NONE', #83744 ) ;
#24619 = DIRECTION ( 'NONE',  ( 1.000000000000000000, 1.000000000000000078E-15, 0.000000000000000000 ) ) ;
#24620 = CARTESIAN_POINT ( 'NONE',  ( -0.8234102327917739439, 69.97007251634678937, 118.5538614604470098 ) ) ;
#24621 = LINE ( 'NONE', #30546, #28675 ) ;
#24622 = DIRECTION ( 'NONE',  ( 1.000000000000000000, 0.000000000000000000, 0.000000000000000000 ) ) ;
#24623 = ORIENTED_EDGE ( 'NONE', *, *, #44244, .F. ) ;
#24624 = CARTESIAN_POINT ( 'NONE',  ( 97.21658504226680009, -33.31410993950169086, 286.0613395616252888 ) ) ;
#24625 = CARTESIAN_POINT ( 'NONE',  ( 111.0628700864597533, -47.08446675046669583, 13.85753003781498016 ) ) ;
#24627 = LINE ( 'NONE', #24191, #57267 ) ;
#24626 = CARTESIAN_POINT ( 'NONE',  ( 138.0667039024480971, -58.72944715994091069, 199.5838068554170093 ) ) ;
#24628 = DIRECTION ( 'NONE',  ( 0.000000000000000000, 0.000000000000000000, -1.000000000000000000 ) ) ;
#24629 = DIRECTION ( 'NONE',  ( 0.9963424814100680926, -0.08544974978095730422, 0.000000000000000000 ) ) ;
#24630 = DIRECTION ( 'NONE',  ( 0.000000000000000000, 0.000000000000000000, -1.000000000000000000 ) ) ;
#24631 = VECTOR ( 'NONE', #67332, 1000.000000000000000 ) ;
#24632 = LINE ( 'NONE', #52299, #72132 ) ;
#24633 = CARTESIAN_POINT ( 'NONE',  ( 115.0376101259158901, -42.90801517561737910, 163.3021728873967788 ) ) ;
#24634 = DIRECTION ( 'NONE',  ( 0.000000000000000000, 0.000000000000000000, 1.000000000000000000 ) ) ;
#24635 = CIRCLE ( 'NONE', #42001, 4.762500000000000178 ) ;
#24636 = CARTESIAN_POINT ( 'NONE',  ( 96.64524470886469487, -32.90705862865544162, 21.03467289495897319 ) ) ;
#24637 = CARTESIAN_POINT ( 'NONE',  ( 114.8139851684208992, -29.70110827795256014, 205.4127681330539872 ) ) ;
#24638 = CARTESIAN_POINT ( 'NONE',  ( 96.69317630666223806, -38.23732580652426094, 62.44133956162495025 ) ) ;
#24640 = CARTESIAN_POINT ( 'NONE',  ( 128.0667039024480118, -58.72944715994110254, 310.9178068554150514 ) ) ;
#24639 = DIRECTION ( 'NONE',  ( -0.5000000000000003331, 0.8660254037844383745, 0.000000000000000000 ) ) ;
#24641 = DIRECTION ( 'NONE',  ( -0.7071067811869841124, 0.7071067811861110330, 0.000000000000000000 ) ) ;
#24642 = AXIS2_PLACEMENT_3D ( 'NONE', #88965, #88077, #41236 ) ;
#24643 = ADVANCED_FACE ( 'NONE', ( #16049 ), #45742, .T. ) ;
#24644 = EDGE_LOOP ( 'NONE', ( #14900, #5671, #63267, #88253, #77028, #54851 ) ) ;
#24645 = CARTESIAN_POINT ( 'NONE',  ( 102.0670550238970407, -27.97049802371184768, 186.4897919368071939 ) ) ;
#24646 = ORIENTED_EDGE ( 'NONE', *, *, #2061, .F. ) ;
#24647 = CARTESIAN_POINT ( 'NONE',  ( 106.8551140066829817, -47.84553036069057441, 73.56133956162396714 ) ) ;
#24649 = ADVANCED_FACE ( 'NONE', ( #22414 ), #28776, .F. ) ;
#24648 = CIRCLE ( 'NONE', #78369, 3.499999999999996003 ) ;
#24651 = ORIENTED_EDGE ( 'NONE', *, *, #10171, .T. ) ;
#24650 = FACE_OUTER_BOUND ( 'NONE', #20947, .T. ) ;
#24652 = LINE ( 'NONE', #23346, #50449 ) ;
#24653 = CARTESIAN_POINT ( 'NONE',  ( 113.7851844261089695, -26.99768152489570738, 235.5956252759109759 ) ) ;
#24654 = DIRECTION ( 'NONE',  ( 1.000000000000000000, 4.163336342344333240E-14, 0.000000000000000000 ) ) ;
#24655 = LINE ( 'NONE', #24220, #21132 ) ;
#24656 = CARTESIAN_POINT ( 'NONE',  ( 168.0371591254543375, -48.62818131005499822, 300.4678068554149490 ) ) ;
#24657 = CARTESIAN_POINT ( 'NONE',  ( 193.5667039024485803, -48.82844715993409324, 180.4678068554150343 ) ) ;
#24658 = ADVANCED_FACE ( 'NONE', ( #76470 ), #71015, .F. ) ;
#24659 = ADVANCED_FACE ( 'NONE', ( #55542 ), #62830, .F. ) ;
#24660 = DIRECTION ( 'NONE',  ( -0.9254794337955620787, -0.3787978585227822492, 0.000000000000000000 ) ) ;
#24661 = LINE ( 'NONE', #67324, #70372 ) ;
#24662 = VECTOR ( 'NONE', #4066, 1000.000000000000114 ) ;
#24663 = CARTESIAN_POINT ( 'NONE',  ( 116.6769215743980936, -34.91203320259893417, 158.9756252759109714 ) ) ;
#24664 = ORIENTED_EDGE ( 'NONE', *, *, #49782, .T. ) ;
#24665 = ORIENTED_EDGE ( 'NONE', *, *, #89661, .T. ) ;
#24666 = EDGE_CURVE ( 'NONE', #77124, #54148, #44266, .T. ) ;
#24667 = CARTESIAN_POINT ( 'NONE',  ( 99.30241108408027628, -32.39570601076609080, 107.3530118773259545 ) ) ;
#24668 = CYLINDRICAL_SURFACE ( 'NONE', #61724, 9.999999999999998224 ) ;
#24670 = DIRECTION ( 'NONE',  ( 0.000000000000000000, 0.000000000000000000, 1.000000000000000000 ) ) ;
#24669 = CARTESIAN_POINT ( 'NONE',  ( 109.9476544338203041, -26.76763818355061986, 210.8403871806729626 ) ) ;
#24671 = CARTESIAN_POINT ( 'NONE',  ( 0.000000000000000000, 92.07499999999998863, 0.000000000000000000 ) ) ;
#24672 = EDGE_CURVE ( 'NONE', #16560, #38408, #57371, .T. ) ;
#24673 = CARTESIAN_POINT ( 'NONE',  ( 115.5439452383991892, -99.96145986183358900, 2.217806855417864043 ) ) ;
#24674 = VECTOR ( 'NONE', #78388, 1000.000000000000000 ) ;
#24675 = CARTESIAN_POINT ( 'NONE',  ( 117.8738102209309062, 81.71068249639864689, -12.69999999999876827 ) ) ;
#24676 = CARTESIAN_POINT ( 'NONE',  ( -141.3509999999999991, 0.000000000000000000, 141.3509999999999991 ) ) ;
#24677 = CARTESIAN_POINT ( 'NONE',  ( 134.0664832912740110, -46.42944715994100591, -0.5743747240890021422 ) ) ;
#24678 = FACE_BOUND ( 'NONE', #17784, .T. ) ;
#24679 = CARTESIAN_POINT ( 'NONE',  ( 108.9412587213991088, -26.46057952311815953, 164.9327681330529742 ) ) ;
#24680 = ORIENTED_EDGE ( 'NONE', *, *, #73167, .T. ) ;
#24682 = ORIENTED_EDGE ( 'NONE', *, *, #15204, .F. ) ;
#24681 = ADVANCED_FACE ( 'NONE', ( #69659 ), #77824, .T. ) ;
#24683 = CARTESIAN_POINT ( 'NONE',  ( 85.12238035501010813, -78.13364596806115969, 249.3134381260879877 ) ) ;
#24684 = CARTESIAN_POINT ( 'NONE',  ( 145.9495235048387940, -68.95052383084446035, 247.2914646300089885 ) ) ;
#24685 = FACE_OUTER_BOUND ( 'NONE', #87198, .T. ) ;
#24686 = CARTESIAN_POINT ( 'NONE',  ( 62.03715912545838762, -47.82818131006021645, 249.9678068554150343 ) ) ;
#24687 = VECTOR ( 'NONE', #19993, 1000.000000000000000 ) ;
#24688 = CARTESIAN_POINT ( 'NONE',  ( 105.7154619534882016, -46.72385643955875878, 268.4689573849462363 ) ) ;
#24689 = CARTESIAN_POINT ( 'NONE',  ( 97.67451187568107684, -41.25469890874477841, 171.6841967044819626 ) ) ;
#24690 = DIRECTION ( 'NONE',  ( -1.000000000000000078E-15, 1.000000000000000083E-30, 1.000000000000000000 ) ) ;
#24691 = ORIENTED_EDGE ( 'NONE', *, *, #63650, .F. ) ;
#24693 = ORIENTED_EDGE ( 'NONE', *, *, #75266, .T. ) ;
#24692 = ORIENTED_EDGE ( 'NONE', *, *, #5701, .T. ) ;
#24694 = AXIS2_PLACEMENT_3D ( 'NONE', #10380, #3122, #78987 ) ;
#24695 = EDGE_CURVE ( 'NONE', #58480, #12034, #64518, .T. ) ;
#24696 = CARTESIAN_POINT ( 'NONE',  ( -7.400192735666117905, 72.22046014531929359, 118.3253218772466511 ) ) ;
#24698 = ADVANCED_FACE ( 'NONE', ( #38158 ), #2284, .F. ) ;
#24697 = DIRECTION ( 'NONE',  ( 0.000000000000000000, -1.000000000000000000, 0.000000000000000000 ) ) ;
#24699 = CARTESIAN_POINT ( 'NONE',  ( 109.6422123260156383, -46.48028807993739520, 163.7813936359489162 ) ) ;
#24700 = EDGE_CURVE ( 'NONE', #9455, #27014, #87653, .T. ) ;
#24701 = CARTESIAN_POINT ( 'NONE',  ( 98.11614316284976667, -39.58741349592436620, 277.9920594963732015 ) ) ;
#24702 = AXIS2_PLACEMENT_3D ( 'NONE', #44622, #65530, #80511 ) ;
#24703 = LINE ( 'NONE', #80130, #85565 ) ;
#24704 = ORIENTED_EDGE ( 'NONE', *, *, #86919, .F. ) ;
#24705 = EDGE_CURVE ( 'NONE', #21703, #13421, #67653, .T. ) ;
#24706 = CARTESIAN_POINT ( 'NONE',  ( 99.66264782090949836, -39.75983002812326106, 9.635625275910941312 ) ) ;
#24707 = DIRECTION ( 'NONE',  ( 1.000000000000000000, 0.000000000000000000, 0.000000000000000000 ) ) ;
#24708 = ORIENTED_EDGE ( 'NONE', *, *, #79981, .T. ) ;
#24710 = ORIENTED_EDGE ( 'NONE', *, *, #59303, .F. ) ;
#24709 = VECTOR ( 'NONE', #16470, 1000.000000000000000 ) ;
#24711 = CARTESIAN_POINT ( 'NONE',  ( 0.000000000000000000, 95.00619999999999266, -9.525000000000000355 ) ) ;
#24712 = VERTEX_POINT ( 'NONE', #32223 ) ;
#24713 = ORIENTED_EDGE ( 'NONE', *, *, #10978, .F. ) ;
#24714 = CARTESIAN_POINT ( 'NONE',  ( 112.1371669992097964, -28.01157492980850350, 155.6564172018965166 ) ) ;
#24715 = CARTESIAN_POINT ( 'NONE',  ( 113.9308110932664704, -41.86102644448636312, 27.73813411379200033 ) ) ;
#24716 = AXIS2_PLACEMENT_3D ( 'NONE', #22272, #15461, #43581 ) ;
#24717 = CARTESIAN_POINT ( 'NONE',  ( 101.3369781660191222, -46.20933176663394448, 202.1318157521019430 ) ) ;
#24718 = CARTESIAN_POINT ( 'NONE',  ( 108.6716496925947126, -26.45072611336619772, 189.9527681330539792 ) ) ;
#24719 = CARTESIAN_POINT ( 'NONE',  ( 107.0667039024470313, -104.2784471599412086, 7.717806855417980394 ) ) ;
#24720 = CARTESIAN_POINT ( 'NONE',  ( 106.5673366543293383, -47.17799660047543853, 243.5384824187679556 ) ) ;
#24721 = CARTESIAN_POINT ( 'NONE',  ( 97.81413651554109379, -40.51640884438177181, 97.63607350422876152 ) ) ;
#24722 = CARTESIAN_POINT ( 'NONE',  ( 182.2300522401177432, -33.89581943343662118, 237.4678068554150059 ) ) ;
#24723 = ORIENTED_EDGE ( 'NONE', *, *, #38969, .F. ) ;
#24724 = EDGE_LOOP ( 'NONE', ( #58101, #83524 ) ) ;
#24725 = STYLED_ITEM ( 'NONE', ( #81954 ), #88996 ) ;
#24726 = DIRECTION ( 'NONE',  ( -0.7071067811865453523, -0.7071067811865496822, -7.071067811865460542E-16 ) ) ;
#24727 = CARTESIAN_POINT ( 'NONE',  ( 104.1736071946568103, -26.63078081164005440, 225.2984824187679749 ) ) ;
#24728 = ORIENTED_EDGE ( 'NONE', *, *, #25147, .F. ) ;
#24729 = CARTESIAN_POINT ( 'NONE',  ( 99.10121394234140269, -45.50393173043428163, 156.9899109901969609 ) ) ;
#24730 = CARTESIAN_POINT ( 'NONE',  ( 165.9667039024459996, -26.71338133339301635, 342.9256252759109884 ) ) ;
#24731 = DIRECTION ( 'NONE',  ( 0.000000000000000000, -1.000000000000000000, 0.000000000000000000 ) ) ;
#24732 = CARTESIAN_POINT ( 'NONE',  ( 81.84766347661003749, -124.7784471599409670, 222.2178068554179902 ) ) ;
#24733 = CARTESIAN_POINT ( 'NONE',  ( 143.9462412624536398, -140.5180570844704278, 246.3267910350913610 ) ) ;
#24736 = CARTESIAN_POINT ( 'NONE',  ( 105.2810544170623359, -46.37316503544239765, 8.429910990195965681 ) ) ;
#24735 = CARTESIAN_POINT ( 'NONE',  ( 0.000000000000000000, 184.0000000000000000, 106.1020876358972629 ) ) ;
#24734 = DIRECTION ( 'NONE',  ( -1.000000000000000000, 0.000000000000000000, 2.544367396927093851E-16 ) ) ;
#24737 = DIRECTION ( 'NONE',  ( 0.000000000000000000, 1.000000000000000000, 0.000000000000000000 ) ) ;
#24738 = CYLINDRICAL_SURFACE ( 'NONE', #61275, 2.750000000000002665 ) ;
#24739 = VECTOR ( 'NONE', #63121, 1000.000000000000000 ) ;
#24740 = DIRECTION ( 'NONE',  ( 0.000000000000000000, -1.000000000000000000, 0.000000000000000000 ) ) ;
#24741 = CARTESIAN_POINT ( 'NONE',  ( 68.27270054217888173, -137.0689115924293446, 247.3475429858000894 ) ) ;
#24742 = LINE ( 'NONE', #37929, #3904 ) ;
#24743 = DIRECTION ( 'NONE',  ( 0.000000000000000000, 0.000000000000000000, -1.000000000000000000 ) ) ;
#24745 = ORIENTED_EDGE ( 'NONE', *, *, #12685, .T. ) ;
#24744 = CARTESIAN_POINT ( 'NONE',  ( 112.8613057705799605, -28.86133510866265084, 195.5838068554167819 ) ) ;
#24746 = CARTESIAN_POINT ( 'NONE',  ( 101.4133560641720067, -46.25507541695031222, 207.1622919425779514 ) ) ;
#24747 = CARTESIAN_POINT ( 'NONE',  ( 114.7713543040237454, -44.65465650488444993, 114.2022919425779719 ) ) ;
#24748 = CARTESIAN_POINT ( 'NONE',  ( 100.6107886340239901, -26.73269172650989489, 216.5327681330539633 ) ) ;
#24749 = CYLINDRICAL_SURFACE ( 'NONE', #60681, 0.9999999999999800160 ) ;
#24750 = DIRECTION ( 'NONE',  ( 2.999999999999999839E-15, -1.000000000000000000, 2.999999999999999900E-30 ) ) ;
#24751 = VECTOR ( 'NONE', #55600, 1000.000000000000000 ) ;
#24753 = CARTESIAN_POINT ( 'NONE',  ( 106.8019215826475943, -46.78094778693688482, 38.55552475618427621 ) ) ;
#24752 = CARTESIAN_POINT ( 'NONE',  ( 107.0667039024470313, -104.2784471599414502, 0.2178068554180012661 ) ) ;
#24754 = CARTESIAN_POINT ( 'NONE',  ( -41.60202597009397607, 40.59999999999997300, 47.03909206933071374 ) ) ;
#24755 = FACE_OUTER_BOUND ( 'NONE', #1833, .T. ) ;
#24756 = CARTESIAN_POINT ( 'NONE',  ( 115.0910585283885865, -30.62042626667451728, 64.34441744103244787 ) ) ;
#24758 = ORIENTED_EDGE ( 'NONE', *, *, #29409, .F. ) ;
#24757 = B_SPLINE_CURVE_WITH_KNOTS ( 'NONE', 3,
 ( #41599, #68440, #27543, #49316, #727, #7999, #35695, #69782, #63408, #33905, #1191, #56584, #62510, #40716, #83411, #69333, #41156, #34801 ),
 .UNSPECIFIED., .F., .F.,
 ( 4, 2, 2, 2, 2, 2, 2, 2, 4 ),
 ( 0.4999999957683650686, 0.5624999962973193934, 0.6249999968262738292, 0.6874999973552281540, 0.7499999978841824788, 0.8124999984131369146, 0.8749999989420912394, 0.9374999994710455642, 1.000000000000000000 ),
 .UNSPECIFIED. ) ;
#24759 = EDGE_CURVE ( 'NONE', #29576, #74086, #52991, .T. ) ;
#24760 = ORIENTED_EDGE ( 'NONE', *, *, #27758, .F. ) ;
#24761 = CARTESIAN_POINT ( 'NONE',  ( 100.5019087779429015, -42.19410572027086914, 116.3009912566479471 ) ) ;
#24762 = EDGE_CURVE ( 'NONE', #61450, #37451, #28320, .T. ) ;
#24764 = EDGE_LOOP ( 'NONE', ( #42119, #85746 ) ) ;
#24763 = CARTESIAN_POINT ( 'NONE',  ( 78.56670390244704549, -118.2784471599409812, 45.21780685541799727 ) ) ;
#24765 = CARTESIAN_POINT ( 'NONE',  ( 107.6020193903983966, -26.30459096080998904, 91.03562527591097364 ) ) ;
#24766 = CARTESIAN_POINT ( 'NONE',  ( 208.9149999999999920, 37.33800000000000097, 50.79999999999999716 ) ) ;
#24767 = AXIS2_PLACEMENT_3D ( 'NONE', #78879, #38847, #30706 ) ;
#24769 = CARTESIAN_POINT ( 'NONE',  ( 20.03715912545644073, -24.42818131006202265, 129.9678068554150627 ) ) ;
#24768 = VECTOR ( 'NONE', #87662, 1000.000000000000000 ) ;
#24770 = EDGE_CURVE ( 'NONE', #61077, #16601, #59918, .T. ) ;
#24771 = EDGE_CURVE ( 'NONE', #10976, #14667, #60204, .T. ) ;
#24772 = CARTESIAN_POINT ( 'NONE',  ( -479.3614999999999782, 14.28750000000023945, 19.36139197104649767 ) ) ;
#24773 = DIRECTION ( 'NONE',  ( 0.7071067811865525687, -0.7071067811865425767, 7.071067811865533512E-16 ) ) ;
#24774 = CARTESIAN_POINT ( 'NONE',  ( 106.3024736416914493, -26.94527301106431949, 25.13848241876892686 ) ) ;
#24775 = ORIENTED_EDGE ( 'NONE', *, *, #61975, .F. ) ;
#24776 = VERTEX_POINT ( 'NONE', #52200 ) ;
#24778 = ORIENTED_EDGE ( 'NONE', *, *, #88789, .T. ) ;
#24777 = CIRCLE ( 'NONE', #14671, 7.937500000000000000 ) ;
#24779 = ADVANCED_FACE ( 'NONE', ( #46737 ), #25416, .T. ) ;
#24780 = CARTESIAN_POINT ( 'NONE',  ( -47.18030668273772221, 353.0471713899363522, 75.34738655934134499 ) ) ;
#24782 = DIRECTION ( 'NONE',  ( 0.000000000000000000, 0.000000000000000000, 1.000000000000000000 ) ) ;
#24781 = CARTESIAN_POINT ( 'NONE',  ( 106.1376555893193370, -47.80867374849567852, 108.5099109901959622 ) ) ;
#24783 = DIRECTION ( 'NONE',  ( -1.000000000000000000, -4.299999999999999979E-14, -1.000000000000000078E-15 ) ) ;
#24784 = ADVANCED_FACE ( 'NONE', ( #73115 ), #67195, .F. ) ;
#24785 = CARTESIAN_POINT ( 'NONE',  ( 8.383129030752360933, 73.00074830044857777, -130.2869803084437592 ) ) ;
#24786 = VECTOR ( 'NONE', #19910, 1000.000000000000000 ) ;
#24787 = DIRECTION ( 'NONE',  ( 0.000000000000000000, 0.000000000000000000, -1.000000000000000000 ) ) ;
#24788 = CARTESIAN_POINT ( 'NONE',  ( -3.230781895526043890, 94.86034579432060809, 130.5182095844837704 ) ) ;
#24789 = LINE ( 'NONE', #57621, #67575 ) ;
#24790 = CARTESIAN_POINT ( 'NONE',  ( 115.7104945841387718, -43.58108136993647719, 48.30514908543492680 ) ) ;
#24791 = EDGE_LOOP ( 'NONE', ( #31592, #40648, #52683, #22682 ) ) ;
#24793 = ORIENTED_EDGE ( 'NONE', *, *, #16790, .F. ) ;
#24792 = EDGE_CURVE ( 'NONE', #33837, #28990, #79962, .T. ) ;
#24794 = CARTESIAN_POINT ( 'NONE',  ( 33.96670390244737803, -26.71338133339334320, 313.9678068554150059 ) ) ;
#24795 = CYLINDRICAL_SURFACE ( 'NONE', #35939, 9.999999999999998224 ) ;
#24796 = FACE_OUTER_BOUND ( 'NONE', #26942, .T. ) ;
#24797 = CARTESIAN_POINT ( 'NONE',  ( 108.7381085716129263, -28.73974155568626898, 137.7309475124479548 ) ) ;
#24798 = ADVANCED_FACE ( 'NONE', ( #32677 ), #33129, .T. ) ;
#24799 = AXIS2_PLACEMENT_3D ( 'NONE', #29627, #78701, #2381 ) ;
#24800 = CARTESIAN_POINT ( 'NONE',  ( 106.0667039024470171, -87.35579742913172652, -21.78219314458254630 ) ) ;
#24801 = ORIENTED_EDGE ( 'NONE', *, *, #49803, .T. ) ;
#24802 = ORIENTED_EDGE ( 'NONE', *, *, #64363, .F. ) ;
#24803 = CYLINDRICAL_SURFACE ( 'NONE', #49625, 2.030000000001311644 ) ;
#24804 = AXIS2_PLACEMENT_3D ( 'NONE', #76377, #29570, #84104 ) ;
#24805 = ORIENTED_EDGE ( 'NONE', *, *, #10224, .F. ) ;
#24806 = EDGE_LOOP ( 'NONE', ( #74988, #31364, #75986, #43870 ) ) ;
#24807 = DIRECTION ( 'NONE',  ( 3.902639990948949304E-17, 0.000000000000000000, -1.000000000000000000 ) ) ;
#24808 = VECTOR ( 'NONE', #39814, 1000.000000000000000 ) ;
#24809 = EDGE_CURVE ( 'NONE', #1463, #34216, #25869, .T. ) ;
#24810 = CARTESIAN_POINT ( 'NONE',  ( 103.4772640228778329, -44.83165572645120278, 173.6758690201829438 ) ) ;
#24811 = DIRECTION ( 'NONE',  ( 0.000000000000000000, 1.000000000000000000, 0.000000000000000000 ) ) ;
#24812 = EDGE_CURVE ( 'NONE', #45647, #56272, #19052, .T. ) ;
#24813 = AXIS2_PLACEMENT_3D ( 'NONE', #29171, #35070, #76873 ) ;
#24814 = DIRECTION ( 'NONE',  ( 3.999999999999999995E-14, -1.000000000000000000, 4.100000000000000342E-29 ) ) ;
#24815 = CARTESIAN_POINT ( 'NONE',  ( 107.0667039024470455, -135.2784471599409528, 25.71780685541800437 ) ) ;
#24816 = VERTEX_POINT ( 'NONE', #66296 ) ;
#24817 = ORIENTED_EDGE ( 'NONE', *, *, #20787, .T. ) ;
#24818 = CIRCLE ( 'NONE', #26241, 1.000000000000000888 ) ;
#24819 = EDGE_LOOP ( 'NONE', ( #7146, #84746, #78898, #76110 ) ) ;
#24820 = ORIENTED_EDGE ( 'NONE', *, *, #44744, .F. ) ;
#24821 = CARTESIAN_POINT ( 'NONE',  ( 111.7322531227442681, -44.01858407219413039, 215.8357094172109782 ) ) ;
#24822 = CARTESIAN_POINT ( 'NONE',  ( 96.00011186464382718, -37.20993085831212710, 116.3489586092439652 ) ) ;
#24823 = CARTESIAN_POINT ( 'NONE',  ( 96.68076663292303863, -33.01451620012163346, 26.06514908543494613 ) ) ;
#24824 = DIRECTION ( 'NONE',  ( 1.000000000000000000, 1.387778780781444413E-14, 0.000000000000000000 ) ) ;
#24825 = DIRECTION ( 'NONE',  ( -0.4214249218767883165, -0.9068632946707806397, -4.214249218767892389E-16 ) ) ;
#24826 = LINE ( 'NONE', #9863, #89562 ) ;
#24827 = CARTESIAN_POINT ( 'NONE',  ( 102.0510343613854189, -46.57928231165939081, 168.2137205140059564 ) ) ;
#24828 = DIRECTION ( 'NONE',  ( -0.000000000000000000, 1.000000000000000000, -0.000000000000000000 ) ) ;
#24829 = ORIENTED_EDGE ( 'NONE', *, *, #38708, .T. ) ;
#24830 = PLANE ( 'NONE',  #17717 ) ;
#24831 = EDGE_LOOP ( 'NONE', ( #29147, #16366, #43525, #56182 ) ) ;
#24832 = ORIENTED_EDGE ( 'NONE', *, *, #35769, .T. ) ;
#24833 = DIRECTION ( 'NONE',  ( 0.000000000000000000, 0.000000000000000000, 1.000000000000000000 ) ) ;
#24834 = CARTESIAN_POINT ( 'NONE',  ( 67.06670390244700286, -67.87844715994098976, 222.2178068554179902 ) ) ;
#24835 = ORIENTED_EDGE ( 'NONE', *, *, #1213, .T. ) ;
#24836 = VECTOR ( 'NONE', #12577, 1000.000000000000000 ) ;
#24837 = EDGE_CURVE ( 'NONE', #55506, #45213, #38595, .T. ) ;
#24838 = CARTESIAN_POINT ( 'NONE',  ( 120.3338511921238876, -37.86730215311064995, 299.5571190294419921 ) ) ;
#24839 = ORIENTED_EDGE ( 'NONE', *, *, #71341, .F. ) ;
#24840 = DIRECTION ( 'NONE',  ( 0.000000000000000000, 0.000000000000000000, 1.000000000000000000 ) ) ;
#24841 = CARTESIAN_POINT ( 'NONE',  ( 96.65640405957751113, -37.29272404675901242, 76.36991099019697060 ) ) ;
#24842 = DIRECTION ( 'NONE',  ( 0.000000000000000000, 0.000000000000000000, -1.000000000000000000 ) ) ;
#24843 = DIRECTION ( 'NONE',  ( 0.000000000000000000, 1.000000000000000000, 0.000000000000000000 ) ) ;
#24844 = DIRECTION ( 'NONE',  ( 0.000000000000000000, 0.000000000000000000, -1.000000000000000000 ) ) ;
#24845 = CARTESIAN_POINT ( 'NONE',  ( 96.75683229781650141, -37.84742820979680289, 81.40038718067398804 ) ) ;
#24847 = CARTESIAN_POINT ( 'NONE',  ( 102.0615167388205293, -46.55869598106821883, 168.2137205140059564 ) ) ;
#24846 = CARTESIAN_POINT ( 'NONE',  ( 154.4409905298078058, -0.9147987323338667709, 540.9756252759101471 ) ) ;
#24848 = CARTESIAN_POINT ( 'NONE',  ( 125.5177273812784762, -137.6784471599409301, 55.21780685541800437 ) ) ;
#24849 = DIRECTION ( 'NONE',  ( 0.000000000000000000, 0.000000000000000000, -1.000000000000000000 ) ) ;
#24850 = EDGE_LOOP ( 'NONE', ( #72084, #7236, #86933, #56789 ) ) ;
#24851 = VECTOR ( 'NONE', #78163, 1000.000000000000000 ) ;
#24852 = DIRECTION ( 'NONE',  ( 1.000000000000000078E-15, 1.000000000000000083E-30, -1.000000000000000000 ) ) ;
#24853 = CARTESIAN_POINT ( 'NONE',  ( 71.23990787207000608, 10.64204399490126463, 542.9756252759101471 ) ) ;
#24854 = DIRECTION ( 'NONE',  ( 0.000000000000000000, 1.000000000000000000, 0.000000000000000000 ) ) ;
#24855 = VECTOR ( 'NONE', #28071, 1000.000000000000000 ) ;
#24856 = DIRECTION ( 'NONE',  ( 0.000000000000000000, 0.000000000000000000, 1.000000000000000000 ) ) ;
#24858 = ORIENTED_EDGE ( 'NONE', *, *, #16145, .T. ) ;
#24857 = CARTESIAN_POINT ( 'NONE',  ( 96.09181007874647662, -35.06528625842698688, 221.1946728949589840 ) ) ;
#24859 = CARTESIAN_POINT ( 'NONE',  ( 100.9544530942022362, -28.70718995531744255, 145.5939800926359737 ) ) ;
#24860 = CARTESIAN_POINT ( 'NONE',  ( 96.99552470177088992, -33.95220897389439330, 247.1127681330539758 ) ) ;
#24861 = CARTESIAN_POINT ( 'NONE',  ( 99.02072372077822138, -43.42711337151016693, 112.8784824187679732 ) ) ;
#24862 = DIRECTION ( 'NONE',  ( 0.000000000000000000, 1.000000000000000000, 0.000000000000000000 ) ) ;
#24863 = CARTESIAN_POINT ( 'NONE',  ( 81.44716491654075696, -39.11090284777883852, 7.925007058955602091 ) ) ;
#24864 = ADVANCED_FACE ( 'NONE', ( #24974 ), #45835, .T. ) ;
#24865 = FACE_OUTER_BOUND ( 'NONE', #86060, .T. ) ;
#24866 = DIRECTION ( 'NONE',  ( -1.000000000000000000, 0.000000000000000000, 3.491483361109380094E-15 ) ) ;
#24867 = ORIENTED_EDGE ( 'NONE', *, *, #27713, .F. ) ;
#24868 = EDGE_CURVE ( 'NONE', #19039, #54183, #82042, .T. ) ;
#24869 = ORIENTED_EDGE ( 'NONE', *, *, #28654, .T. ) ;
#24870 = EDGE_CURVE ( 'NONE', #79942, #51804, #22651, .T. ) ;
#24871 = EDGE_LOOP ( 'NONE', ( #46399, #57555, #45225, #26750, #21084, #12425 ) ) ;
#24872 = CIRCLE ( 'NONE', #10408, 0.5000000000000004441 ) ;
#24873 = ADVANCED_FACE ( 'NONE', ( #50726 ), #42228, .F. ) ;
#24874 = ORIENTED_EDGE ( 'NONE', *, *, #52438, .F. ) ;
#24875 = CARTESIAN_POINT ( 'NONE',  ( 37.06648329127298780, 12.92155284005730387, 355.9756252759109998 ) ) ;
#24876 = CARTESIAN_POINT ( 'NONE',  ( 97.81168895331678925, -40.51742574516946860, 7.635625275910939536 ) ) ;
#24877 = CARTESIAN_POINT ( 'NONE',  ( 107.0667039024470313, -104.2784471599409528, 249.2178068554179902 ) ) ;
#24878 = CARTESIAN_POINT ( 'NONE',  ( 133.3151098752258292, -34.05633243510672514, 1.690787911851882264 ) ) ;
#24879 = EDGE_CURVE ( 'NONE', #69728, #2797, #82111, .T. ) ;
#24881 = CARTESIAN_POINT ( 'NONE',  ( 113.2461701916471810, -28.75918670901990382, 149.5525716684902022 ) ) ;
#24880 = DIRECTION ( 'NONE',  ( -4.299999999999999979E-14, 1.000000000000000000, -4.128053709984630540E-29 ) ) ;
#24882 = CIRCLE ( 'NONE', #72734, 3.500000000000003109 ) ;
#24883 = CARTESIAN_POINT ( 'NONE',  ( 115.8412394166662835, -32.57321297090945933, 213.6009912566489675 ) ) ;
#24884 = ORIENTED_EDGE ( 'NONE', *, *, #61975, .T. ) ;
#24885 = ORIENTED_EDGE ( 'NONE', *, *, #68671, .T. ) ;
#24886 = VERTEX_POINT ( 'NONE', #16661 ) ;
#24887 = EDGE_CURVE ( 'NONE', #893, #59432, #7726, .T. ) ;
#24888 = VECTOR ( 'NONE', #69406, 1000.000000000000000 ) ;
#24889 = CARTESIAN_POINT ( 'NONE',  ( 116.3167039024470029, -67.87844715994093292, 180.4678068554179902 ) ) ;
#24890 = CARTESIAN_POINT ( 'NONE',  ( 110.8544820967422311, -45.98423322291753124, 182.8856261428530843 ) ) ;
#24891 = CARTESIAN_POINT ( 'NONE',  ( 41.56648329127399677, -9.303447159940999356, 198.9256252759119832 ) ) ;
#24892 = CARTESIAN_POINT ( 'NONE',  ( 107.1760646772892756, -27.86850643495606406, 31.49872616304000417 ) ) ;
#24893 = EDGE_CURVE ( 'NONE', #1197, #86595, #76766, .T. ) ;
#24894 = CARTESIAN_POINT ( 'NONE',  ( 118.5108459337403701, 94.82191660594808980, -3.295896443148412569 ) ) ;
#24895 = DIRECTION ( 'NONE',  ( 0.7071067811575828532, -0.7071067812155121812, 0.000000000000000000 ) ) ;
#24896 = DIRECTION ( 'NONE',  ( 0.000000000000000000, 0.000000000000000000, 1.000000000000000000 ) ) ;
#24899 = VERTEX_POINT ( 'NONE', #63133 ) ;
#24898 = EDGE_CURVE ( 'NONE', #623, #68369, #49031, .T. ) ;
#24897 = VECTOR ( 'NONE', #51243, 1000.000000000000000 ) ;
#24900 = B_SPLINE_CURVE_WITH_KNOTS ( 'NONE', 3,
 ( #33735, #26916, #53245, #81013, #47789, #74177, #18759, #68706, #13738, #88272, #47342, #81902, #26472, #19653, #4691, #75070, #82353, #32372, #46443, #11957, #74617, #54591, #39641, #61425, #40088, #75524, #89152, #13298, #67343, #40987, #5131, #53696, #6472, #34165, #81463, #19213, #85037, #83686, #42318, #110, #21458, #70049, #6921, #55941, #77763, #29162, #36433, #64133 ),
 .UNSPECIFIED., .F., .F.,
 ( 4, 2, 2, 2, 2, 2, 2, 2, 2, 1, 2, 2, 2, 2, 2, 2, 2, 2, 2, 2, 2, 1, 2, 2, 4 ),
 ( 0.05959919981814693069, 0.06208168506169067097, 0.06332292768346255152, 0.06456417030523442513, 0.06704665554877820011, 0.06828789817055008760, 0.06952914079232196121, 0.07201162603586572231, 0.07325286865763758204, 0.07449411127940944177, 0.07573535390118130151, 0.07697659652295317512, 0.07945908176649690846, 0.08194156701004062793, 0.08318280963181251542, 0.08442405225358438903, 0.08690653749712810849, 0.08814778011889995435, 0.08938902274067181408, 0.09187150798421550579, 0.09311275060598732389, 0.09435399322775914199, 0.09559523584953097397, 0.09683647847130280595, 0.09931896371484646990 ),
 .UNSPECIFIED. ) ;
#24901 = CARTESIAN_POINT ( 'NONE',  ( 103.4307397011154279, -27.41362630817958035, 56.37257573100154673 ) ) ;
#24902 = ORIENTED_EDGE ( 'NONE', *, *, #17427, .T. ) ;
#24903 = DIRECTION ( 'NONE',  ( 0.000000000000000000, -1.000000000000000000, 0.000000000000000000 ) ) ;
#24904 = CARTESIAN_POINT ( 'NONE',  ( 100.5332814249895108, -41.62301430380158962, 64.65666179816298609 ) ) ;
#24905 = VECTOR ( 'NONE', #57363, 1000.000000000000000 ) ;
#24906 = CARTESIAN_POINT ( 'NONE',  ( 46.48091746482126041, -48.32844715994084339, 300.4678068554150059 ) ) ;
#24907 = PLANE ( 'NONE',  #43256 ) ;
#24908 = CONICAL_SURFACE ( 'NONE', #75691, 1.258750000000002922, 1.029744258676650093 ) ;
#24909 = CARTESIAN_POINT ( 'NONE',  ( 34.92499999999999716, 69.84999999999999432, 346.0750000000000455 ) ) ;
#24910 = ORIENTED_EDGE ( 'NONE', *, *, #55049, .F. ) ;
#24911 = FACE_OUTER_BOUND ( 'NONE', #75288, .T. ) ;
#24912 = CARTESIAN_POINT ( 'NONE',  ( 125.0187123012608481, 56.81681257766939552, -37.62034114384582750 ) ) ;
#24913 = ORIENTED_EDGE ( 'NONE', *, *, #51497, .T. ) ;
#24914 = CARTESIAN_POINT ( 'NONE',  ( 114.7715153371978687, -44.65482214316887877, 118.2022919425779719 ) ) ;
#24915 = ORIENTED_EDGE ( 'NONE', *, *, #45725, .T. ) ;
#24916 = CARTESIAN_POINT ( 'NONE',  ( 114.5755952152626946, -32.65889807719148052, 68.64384839950594142 ) ) ;
#24917 = CARTESIAN_POINT ( 'NONE',  ( 183.5150000000000148, 37.33800000000000097, 50.79999999999999716 ) ) ;
#24918 = CARTESIAN_POINT ( 'NONE',  ( 114.7653520042265143, -30.23343873216411026, 70.81586902018300123 ) ) ;
#24919 = CARTESIAN_POINT ( 'NONE',  ( 135.5598545223736551, -21.04079274303778391, 1.981704437708090127 ) ) ;
#24920 = FACE_OUTER_BOUND ( 'NONE', #59970, .T. ) ;
#24921 = EDGE_CURVE ( 'NONE', #83340, #63421, #84042, .T. ) ;
#24922 = CARTESIAN_POINT ( 'NONE',  ( 71.06648329127399677, -18.82844715994099971, -5.074374724088000832 ) ) ;
#24923 = CARTESIAN_POINT ( 'NONE',  ( 112.8297475082234484, -27.27058933724656953, 45.62895860924398761 ) ) ;
#24924 = CARTESIAN_POINT ( 'NONE',  ( 36.23715912545338114, -47.82818131006131779, 193.9678068554150911 ) ) ;
#24925 = EDGE_LOOP ( 'NONE', ( #51818, #76708, #50378, #4819 ) ) ;
#24926 = DIRECTION ( 'NONE',  ( -1.000000000000000000, 0.000000000000000000, 1.821231995776179916E-16 ) ) ;
#24927 = ORIENTED_EDGE ( 'NONE', *, *, #68387, .T. ) ;
#24928 = CARTESIAN_POINT ( 'NONE',  ( -118.5107509192928603, 70.27900073646857493, 3.299277431129246541 ) ) ;
#24929 = VERTEX_POINT ( 'NONE', #28612 ) ;
#24930 = ORIENTED_EDGE ( 'NONE', *, *, #88059, .F. ) ;
#24931 = VECTOR ( 'NONE', #32007, 1000.000000000000000 ) ;
#24932 = EDGE_LOOP ( 'NONE', ( #39770, #72412, #47932, #21587 ) ) ;
#24933 = CARTESIAN_POINT ( 'NONE',  ( 110.4719531740380347, -47.31314961125950447, 207.8241967044829721 ) ) ;
#24934 = CARTESIAN_POINT ( 'NONE',  ( 97.73888860506711751, -40.33520859504945832, 126.6195452632120038 ) ) ;
#24935 = CARTESIAN_POINT ( 'NONE',  ( 113.1782937269942124, -44.75186862722408421, 189.0939586048054935 ) ) ;
#24936 = CARTESIAN_POINT ( 'NONE',  ( 115.0226255289246922, -43.52070134976005988, 59.26419670448196086 ) ) ;
#24937 = CARTESIAN_POINT ( 'NONE',  ( 117.0608842944984644, -38.08055299089861023, 44.71895066874647995 ) ) ;
#24938 = ORIENTED_EDGE ( 'NONE', *, *, #51395, .T. ) ;
#24939 = CARTESIAN_POINT ( 'NONE',  ( 172.5664832912740110, -32.07844715994070839, 138.9256252759119832 ) ) ;
#24940 = EDGE_CURVE ( 'NONE', #49158, #6301, #14640, .T. ) ;
#24941 = DIRECTION ( 'NONE',  ( -1.000000000000000000, 0.000000000000000000, 0.000000000000000000 ) ) ;
#24942 = ORIENTED_EDGE ( 'NONE', *, *, #29560, .T. ) ;
#24943 = EDGE_CURVE ( 'NONE', #14978, #50013, #71915, .T. ) ;
#24944 = PLANE ( 'NONE',  #77922 ) ;
#24945 = DIRECTION ( 'NONE',  ( -0.7071067811734105257, 0.7071067811996846197, 0.000000000000000000 ) ) ;
#24946 = CARTESIAN_POINT ( 'NONE',  ( 115.7579298488887076, -31.01215564512770229, 254.2899109901966028 ) ) ;
#24947 = DIRECTION ( 'NONE',  ( 0.000000000000000000, -1.000000000000000000, 0.000000000000000000 ) ) ;
#24948 = CARTESIAN_POINT ( 'NONE',  ( 48.86082318535593316, -35.55794170701788204, 117.4678068554150485 ) ) ;
#24949 = DIRECTION ( 'NONE',  ( -4.299999999999999979E-14, 1.000000000000000000, -4.400000000000000367E-29 ) ) ;
#24950 = CARTESIAN_POINT ( 'NONE',  ( 98.83240126976802742, -34.45875894154226415, 250.5352769709339782 ) ) ;
#24952 = CARTESIAN_POINT ( 'NONE',  ( 98.11562048848820439, -31.42749274529986536, 81.90133956162493689 ) ) ;
#24951 = DIRECTION ( 'NONE',  ( 0.000000000000000000, 0.000000000000000000, 1.000000000000000000 ) ) ;
#24953 = CARTESIAN_POINT ( 'NONE',  ( 111.9933789837352833, 66.64000986900705925, 67.10026523892989303 ) ) ;
#24954 = CARTESIAN_POINT ( 'NONE',  ( 112.1415033342358640, -47.49387789398046067, 137.9270538473389820 ) ) ;
#24955 = ORIENTED_EDGE ( 'NONE', *, *, #12669, .T. ) ;
#24956 = CARTESIAN_POINT ( 'NONE',  ( 126.0667039024479266, -14.72944715994094977, 239.5838068554170377 ) ) ;
#24957 = ORIENTED_EDGE ( 'NONE', *, *, #66928, .T. ) ;
#24958 = DIRECTION ( 'NONE',  ( 4.299999999999999979E-14, -1.000000000000000000, 4.400000000000000367E-29 ) ) ;
#24959 = FACE_BOUND ( 'NONE', #58654, .T. ) ;
#24960 = PRODUCT_DEFINITION_SHAPE ( 'NONE', 'NONE',  #89943 ) ;
#24961 = CARTESIAN_POINT ( 'NONE',  ( 135.0140782791278582, -34.14703303315379657, 1.764000745016856886 ) ) ;
#24962 = VERTEX_POINT ( 'NONE', #37556 ) ;
#24963 = CARTESIAN_POINT ( 'NONE',  ( 37.56670390244749314, -48.82844715994126261, 129.9678068554150911 ) ) ;
#24965 = VERTEX_POINT ( 'NONE', #23497 ) ;
#24964 = CARTESIAN_POINT ( 'NONE',  ( 103.3467460430879612, -47.18776626161088927, 102.3165776568629752 ) ) ;
#24966 = DIRECTION ( 'NONE',  ( 1.000000000000000078E-15, 0.000000000000000000, -1.000000000000000000 ) ) ;
#24967 = CARTESIAN_POINT ( 'NONE',  ( -129.9368274816651478, 82.54999999999999716, 12.69999999999954809 ) ) ;
#24968 = AXIS2_PLACEMENT_3D ( 'NONE', #28095, #83528, #76257 ) ;
#24969 = CARTESIAN_POINT ( 'NONE',  ( 3.175000000000334666, 124.5870000000000033, -31.75000000000000000 ) ) ;
#24970 = EDGE_LOOP ( 'NONE', ( #62665, #54014, #41862, #10052, #26772, #84532, #5966, #42843, #4363, #88411 ) ) ;
#24971 = AXIS2_PLACEMENT_3D ( 'NONE', #23074, #16243, #79816 ) ;
#24972 = CARTESIAN_POINT ( 'NONE',  ( 104.9583746955643448, -25.04227923723010463, 125.2184824187689856 ) ) ;
#24973 = APPLICATION_PROTOCOL_DEFINITION ( 'draft international standard', 'automotive_design', 1998, #37076 ) ;
#24974 = FACE_OUTER_BOUND ( 'NONE', #13053, .T. ) ;
#24975 = DIRECTION ( 'NONE',  ( 0.7071067811575898476, -0.7071067812155052978, 0.000000000000000000 ) ) ;
#24976 = VERTEX_POINT ( 'NONE', #58428 ) ;
#24977 = EDGE_CURVE ( 'NONE', #14032, #79692, #55929, .T. ) ;
#24978 = VECTOR ( 'NONE', #17481, 1000.000000000000000 ) ;
#24979 = EDGE_CURVE ( 'NONE', #30195, #47060, #3034, .T. ) ;
#24980 = ORIENTED_EDGE ( 'NONE', *, *, #8625, .F. ) ;
#24981 = CARTESIAN_POINT ( 'NONE',  ( 100.7940789023227239, 84.21348395916258767, -82.97845804870311781 ) ) ;
#24982 = CARTESIAN_POINT ( 'NONE',  ( 170.2205283966864897, 101.5999999999999943, 79.24800000000000466 ) ) ;
#24983 = EDGE_CURVE ( 'NONE', #81368, #22460, #17114, .T. ) ;
#24984 = AXIS2_PLACEMENT_3D ( 'NONE', #27411, #15598, #7872 ) ;
#24985 = LINE ( 'NONE', #18611, #63196 ) ;
#24986 = ADVANCED_FACE ( 'NONE', ( #3919, #40670, #53376, #73399 ), #81141, .T. ) ;
#24988 = LINE ( 'NONE', #34018, #87748 ) ;
#24987 = CARTESIAN_POINT ( 'NONE',  ( 6.938893903907229955E-15, 60.82030000000000314, 216.0269999999999868 ) ) ;
#24989 = DIRECTION ( 'NONE',  ( 0.000000000000000000, 0.000000000000000000, -1.000000000000000000 ) ) ;
#24990 = VERTEX_POINT ( 'NONE', #12983 ) ;
#24991 = EDGE_CURVE ( 'NONE', #55038, #11706, #61113, .T. ) ;
#24992 = B_SPLINE_CURVE_WITH_KNOTS ( 'NONE', 3,
 ( #3891, #72497, #85695, #3005, #2571, #50697, #86576, #78438, #30271, #71170, #30707, #58403, #44772, #23470, #10696, #9376, #8945, #52012, #64786, #57959, #29828, #71613, #3449, #10264, #65231, #72050, #57059, #79772 ),
 .UNSPECIFIED., .F., .F.,
 ( 4, 2, 1, 1, 1, 1, 2, 2, 2, 2, 2, 2, 2, 2, 2, 4 ),
 ( 0.5000913810681943961, 0.5005795730788700215, 0.5010677650895456470, 0.5020441491108970089, 0.5039969171535993997, 0.5079024532390044033, 0.5157135254098140775, 0.5313356697514330929, 0.5625799584346710125, 0.6250685358011466297, 0.6875571131676221359, 0.7500456905340977531, 0.8125342679005732593, 0.8750228452670488766, 0.9375114226335243828, 1.000000000000000000 ),
 .UNSPECIFIED. ) ;
#24993 = CARTESIAN_POINT ( 'NONE',  ( 112.0659117286329547, -45.48839619832590131, 33.98979195227510530 ) ) ;
#24994 = CARTESIAN_POINT ( 'NONE',  ( 112.7271506738795779, -45.41826929060054852, 219.0480062282919960 ) ) ;
#24995 = EDGE_CURVE ( 'NONE', #31404, #56720, #80236, .T. ) ;
#24997 = EDGE_LOOP ( 'NONE', ( #53412, #49010, #9813, #66366 ) ) ;
#24996 = CARTESIAN_POINT ( 'NONE',  ( 98.60478223830740774, 127.0000000000000000, 3.859079674607175002E-13 ) ) ;
#24998 = CIRCLE ( 'NONE', #65649, 3.250000000000002665 ) ;
#24999 = CARTESIAN_POINT ( 'NONE',  ( 99.61812512063050917, -43.94476044465307751, 37.95086337114900488 ) ) ;
#25000 = FACE_OUTER_BOUND ( 'NONE', #63211, .T. ) ;
#25001 = CARTESIAN_POINT ( 'NONE',  ( 28.57499999999999929, 87.13271776169270311, 294.9574999999999818 ) ) ;
#25002 = DIRECTION ( 'NONE',  ( 1.000000000000000000, 0.000000000000000000, 0.000000000000000000 ) ) ;
#25003 = ORIENTED_EDGE ( 'NONE', *, *, #6931, .F. ) ;
#25004 = CARTESIAN_POINT ( 'NONE',  ( 115.0439452383992318, -109.4614598618342853, -19.78219314458184996 ) ) ;
#25005 = VERTEX_POINT ( 'NONE', #18889 ) ;
#25006 = VERTEX_POINT ( 'NONE', #88841 ) ;
#25007 = CARTESIAN_POINT ( 'NONE',  ( 108.9963713912396912, -28.08052754339530921, 221.3330118773259585 ) ) ;
#25008 = VECTOR ( 'NONE', #87040, 1000.000000000000000 ) ;
#25009 = CARTESIAN_POINT ( 'NONE',  ( 34.92499999999999716, 69.79919999999999902, 346.9005000000000223 ) ) ;
#25010 = CARTESIAN_POINT ( 'NONE',  ( -118.0447731586489652, 88.91144712388910420, -10.99980504627875533 ) ) ;
#25011 = DIRECTION ( 'NONE',  ( 1.000000000000000000, 0.000000000000000000, 0.000000000000000000 ) ) ;
#25012 = CARTESIAN_POINT ( 'NONE',  ( 81.20961857873525958, -39.23068377182526234, 1.829869271362388750 ) ) ;
#25013 = ORIENTED_EDGE ( 'NONE', *, *, #53114, .T. ) ;
#25014 = DIRECTION ( 'NONE',  ( 0.000000000000000000, 0.000000000000000000, 1.000000000000000000 ) ) ;
#25015 = CARTESIAN_POINT ( 'NONE',  ( 182.2420472961719895, -31.76306994223730840, 117.4678068554150627 ) ) ;
#25016 = ORIENTED_EDGE ( 'NONE', *, *, #60959, .F. ) ;
#25017 = CARTESIAN_POINT ( 'NONE',  ( 116.1584957626482435, -43.02035883463254606, 13.35657765686298859 ) ) ;
#25018 = CARTESIAN_POINT ( 'NONE',  ( 0.000000000000000000, 127.0000000000000000, 0.000000000000000000 ) ) ;
#25019 = ORIENTED_EDGE ( 'NONE', *, *, #46905, .T. ) ;
#25020 = CARTESIAN_POINT ( 'NONE',  ( 114.1044565855118265, -40.86425766668616433, 236.2223760838769806 ) ) ;
#25021 = AXIS2_PLACEMENT_3D ( 'NONE', #68375, #89269, #27035 ) ;
#25022 = CARTESIAN_POINT ( 'NONE',  ( 23.03807392221892769, 77.78746915432593312, 302.5815555703470068 ) ) ;
#25023 = DIRECTION ( 'NONE',  ( -1.000000000000000000, -4.299999999999999979E-14, -1.000000000000000078E-15 ) ) ;
#25024 = CARTESIAN_POINT ( 'NONE',  ( 0.000000000000000000, 152.3879256507328250, 0.000000000000000000 ) ) ;
#25025 = ADVANCED_FACE ( 'NONE', ( #17986 ), #80681, .F. ) ;
#25026 = CARTESIAN_POINT ( 'NONE',  ( 97.72358123494467463, -41.53030082902068898, 192.7041967044819728 ) ) ;
#25027 = CARTESIAN_POINT ( 'NONE',  ( -158.9822249764575020, 20.32000000000000028, 139.6999999999999886 ) ) ;
#25028 = ORIENTED_EDGE ( 'NONE', *, *, #70409, .T. ) ;
#25029 = VECTOR ( 'NONE', #66492, 1000.000000000000000 ) ;
#25030 = CARTESIAN_POINT ( 'NONE',  ( 100.2704505754038706, -46.49802187830721323, 83.09276813305294240 ) ) ;
#25031 = DIRECTION ( 'NONE',  ( 0.000000000000000000, 0.000000000000000000, 1.000000000000000000 ) ) ;
#25032 = EDGE_CURVE ( 'NONE', #3366, #66196, #28390, .T. ) ;
#25033 = ORIENTED_EDGE ( 'NONE', *, *, #80061, .T. ) ;
#25034 = EDGE_LOOP ( 'NONE', ( #26075, #72504 ) ) ;
#25035 = ORIENTED_EDGE ( 'NONE', *, *, #46560, .T. ) ;
#25036 = VECTOR ( 'NONE', #34674, 1000.000000000000000 ) ;
#25037 = CARTESIAN_POINT ( 'NONE',  ( 81.33214528238656271, -16.28157797492746184, 1.873071231918668200 ) ) ;
#25038 = CYLINDRICAL_SURFACE ( 'NONE', #44220, 0.5000000000000007772 ) ;
#25039 = CARTESIAN_POINT ( 'NONE',  ( 107.0664832912739968, -36.72944715994100306, 287.6356252759109680 ) ) ;
#25040 = CARTESIAN_POINT ( 'NONE',  ( 98.94907028073869526, -37.58812756235333552, 124.2280903695919818 ) ) ;
#25041 = CARTESIAN_POINT ( 'NONE',  ( 118.0739042565516712, -35.49579832924209910, 229.9032443235299468 ) ) ;
#25042 = CARTESIAN_POINT ( 'NONE',  ( 194.5664832912729878, -81.37844715994266664, 361.9756252759109998 ) ) ;
#25043 = VERTEX_POINT ( 'NONE', #11172 ) ;
#25044 = CARTESIAN_POINT ( 'NONE',  ( 135.1908702341735591, -39.23918067504811091, 1.822998012175016003 ) ) ;
#25045 = VERTEX_POINT ( 'NONE', #32063 ) ;
#25046 = VERTEX_POINT ( 'NONE', #74309 ) ;
#25047 = EDGE_CURVE ( 'NONE', #63589, #9020, #54493, .T. ) ;
#25048 = DIRECTION ( 'NONE',  ( 0.000000000000000000, 0.000000000000000000, -1.000000000000000000 ) ) ;
#25049 = ORIENTED_EDGE ( 'NONE', *, *, #21739, .T. ) ;
#25050 = ORIENTED_EDGE ( 'NONE', *, *, #51778, .F. ) ;
#25051 = FACE_OUTER_BOUND ( 'NONE', #31974, .T. ) ;
#25052 = CARTESIAN_POINT ( 'NONE',  ( 19.56670390244734747, -25.42844715994192129, 300.4678068554150059 ) ) ;
#25053 = CARTESIAN_POINT ( 'NONE',  ( 97.07201598029109846, -35.37898882807422751, 26.21900220677386528 ) ) ;
#25054 = CARTESIAN_POINT ( 'NONE',  ( 116.7762654731291860, -36.89220852042034693, 153.2352769709339668 ) ) ;
#25055 = CARTESIAN_POINT ( 'NONE',  ( 104.2289649446409783, -46.80690502001216657, 22.35848241876792031 ) ) ;
#25056 = VERTEX_POINT ( 'NONE', #66580 ) ;
#25057 = AXIS2_PLACEMENT_3D ( 'NONE', #78423, #37066, #81548 ) ;
#25058 = FACE_OUTER_BOUND ( 'NONE', #33938, .T. ) ;
#25059 = ORIENTED_EDGE ( 'NONE', *, *, #52790, .T. ) ;
#25060 = ORIENTED_CLOSED_SHELL ( 'NONE', *, #47417, .F. );
#25061 = DIRECTION ( 'NONE',  ( 0.000000000000000000, 1.000000000000000000, 0.000000000000000000 ) ) ;
#25062 = ORIENTED_EDGE ( 'NONE', *, *, #56339, .T. ) ;
#25063 = CARTESIAN_POINT ( 'NONE',  ( 97.04329235580377144, -37.22002798420894720, 167.3652492753220145 ) ) ;
#25064 = CARTESIAN_POINT ( 'NONE',  ( 109.6418137192420517, -46.48038841143647915, 32.78157913610764496 ) ) ;
#25065 = CARTESIAN_POINT ( 'NONE',  ( 5.210259806972410633E-15, 95.25000000000000000, -42.54500000000000171 ) ) ;
#25066 = AXIS2_PLACEMENT_3D ( 'NONE', #60427, #88174, #53144 ) ;
#25067 = FACE_BOUND ( 'NONE', #18428, .T. ) ;
#25068 = VERTEX_POINT ( 'NONE', #40213 ) ;
#25069 = CARTESIAN_POINT ( 'NONE',  ( 118.5953454549360231, -33.89261193510051839, 14.01848241876796308 ) ) ;
#25070 = CARTESIAN_POINT ( 'NONE',  ( 111.3409431244321439, -27.17319409035083666, 20.74133956162494030 ) ) ;
#25072 = DIRECTION ( 'NONE',  ( -0.1250000000000000278, -0.9921567416492215186, 3.035766082959410522E-14 ) ) ;
#25071 = DIRECTION ( 'NONE',  ( -3.100000000000000258E-29, 3.100000000000000044E-14, 1.000000000000000000 ) ) ;
#25073 = DIRECTION ( 'NONE',  ( -0.7071067811865774377, 0.7071067811865175967, -7.071067811865782003E-16 ) ) ;
#25074 = DIRECTION ( 'NONE',  ( 4.299999999999999979E-14, -1.000000000000000000, 0.000000000000000000 ) ) ;
#25075 = DIRECTION ( 'NONE',  ( -1.000000000000000000, -5.369304423922379141E-17, 0.000000000000000000 ) ) ;
#25076 = EDGE_CURVE ( 'NONE', #829, #20800, #47472, .T. ) ;
#25077 = CARTESIAN_POINT ( 'NONE',  ( 116.3212776292296127, -32.94146857471318413, 10.13562527591094309 ) ) ;
#25078 = CARTESIAN_POINT ( 'NONE',  ( 145.3505076167853076, -67.86861087870649101, 247.4717563792629846 ) ) ;
#25079 = CARTESIAN_POINT ( 'NONE',  ( 103.5840655562901134, -46.60261447156455716, 57.30705384733997221 ) ) ;
#25080 = CARTESIAN_POINT ( 'NONE',  ( 114.1247157756359769, -29.05716968555177004, 195.4841967044819739 ) ) ;
#25081 = CARTESIAN_POINT ( 'NONE',  ( 96.69309474412473548, -37.96640669985919914, 37.42133956162496844 ) ) ;
#25082 = ADVANCED_FACE ( 'NONE', ( #75201 ), #39766, .T. ) ;
#25084 = LINE ( 'NONE', #37835, #47203 ) ;
#25083 = DIRECTION ( 'NONE',  ( 1.000000000000000000, 0.000000000000000000, 0.000000000000000000 ) ) ;
#25085 = CARTESIAN_POINT ( 'NONE',  ( 81.08070086926755948, -34.17316201338597637, 1.785258157648824895 ) ) ;
#25086 = VECTOR ( 'NONE', #28991, 1000.000000000000000 ) ;
#25087 = AXIS2_PLACEMENT_3D ( 'NONE', #66828, #74098, #72759 ) ;
#25088 = ORIENTED_EDGE ( 'NONE', *, *, #86511, .F. ) ;
#25089 = DIRECTION ( 'NONE',  ( -4.237773401492740281E-14, 1.000000000000000000, 0.000000000000000000 ) ) ;
#25090 = ORIENTED_EDGE ( 'NONE', *, *, #16385, .T. ) ;
#25091 = AXIS2_PLACEMENT_3D ( 'NONE', #88506, #33521, #26259 ) ;
#25092 = CARTESIAN_POINT ( 'NONE',  ( 104.3903674582245742, -25.93822912171390982, 86.26991099019598153 ) ) ;
#25093 = EDGE_CURVE ( 'NONE', #27515, #36325, #5260, .T. ) ;
#25095 = ORIENTED_EDGE ( 'NONE', *, *, #27141, .F. ) ;
#25094 = CARTESIAN_POINT ( 'NONE',  ( 10.33715916136909563, 89.92838495571164970, 130.1461902906857802 ) ) ;
#25096 = CYLINDRICAL_SURFACE ( 'NONE', #63035, 9.999999999999998224 ) ;
#25097 = CARTESIAN_POINT ( 'NONE',  ( 101.4165038149807572, -45.50681337102567880, 218.1213395616249784 ) ) ;
#25098 = CARTESIAN_POINT ( 'NONE',  ( 105.8694971003958614, -26.37070548771162493, 321.6188579224977389 ) ) ;
#25099 = CYLINDRICAL_SURFACE ( 'NONE', #20273, 11.45913725231036118 ) ;
#25100 = EDGE_CURVE ( 'NONE', #60387, #47202, #4375, .T. ) ;
#25101 = PLANE ( 'NONE',  #793 ) ;
#25102 = FACE_OUTER_BOUND ( 'NONE', #34864, .T. ) ;
#25103 = CARTESIAN_POINT ( 'NONE',  ( 132.1570028294962924, -38.71057579844590180, 2.232988688758104967 ) ) ;
#25104 = CARTESIAN_POINT ( 'NONE',  ( -86.19129576945097426, 72.98383416765815923, 98.06260288352420673 ) ) ;
#25105 = CARTESIAN_POINT ( 'NONE',  ( 98.56701561008806323, -30.78824967682747271, 160.8289586092449497 ) ) ;
#25106 = ORIENTED_EDGE ( 'NONE', *, *, #27357, .F. ) ;
#25107 = ORIENTED_EDGE ( 'NONE', *, *, #29322, .T. ) ;
#25108 = CARTESIAN_POINT ( 'NONE',  ( 104.5515342781392008, -45.22670024980423165, 103.7787261630399911 ) ) ;
#25109 = DIRECTION ( 'NONE',  ( 4.237773401492740281E-14, -1.000000000000000000, 0.000000000000000000 ) ) ;
#25111 = DIRECTION ( 'NONE',  ( 0.9659258262890680902, 0.000000000000000000, 0.2588190451025215166 ) ) ;
#25110 = CARTESIAN_POINT ( 'NONE',  ( 97.40014589274353796, -35.23768424668793386, 262.2041967044816602 ) ) ;
#25112 = VECTOR ( 'NONE', #73120, 1000.000000000000000 ) ;
#25113 = CARTESIAN_POINT ( 'NONE',  ( 162.7866693523280048, -29.62846900982320264, 342.9256252759119548 ) ) ;
#25114 = LINE ( 'NONE', #48105, #30729 ) ;
#25115 = CARTESIAN_POINT ( 'NONE',  ( 118.3040894999503081, 72.45860812971085352, -7.755682336160053758 ) ) ;
#25116 = CARTESIAN_POINT ( 'NONE',  ( -9.573302534615132586, 74.16284337107215663, 118.1703442874588319 ) ) ;
#25117 = CIRCLE ( 'NONE', #68699, 17.00000000000000000 ) ;
#25118 = CARTESIAN_POINT ( 'NONE',  ( -487.2989999999999782, 14.28749999999982201, 90.48749999999999716 ) ) ;
#25119 = CARTESIAN_POINT ( 'NONE',  ( -544.5124999999999318, 53.97500000000000142, 50.79999999999999716 ) ) ;
#25120 = B_SPLINE_CURVE_WITH_KNOTS ( 'NONE', 3,
 ( #40358, #83066, #7195, #13554, #26725, #62594, #83496, #61686, #62145, #89421 ),
 .UNSPECIFIED., .F., .F.,
 ( 4, 3, 3, 4 ),
 ( 0.000000000000000000, 0.0009419788482794725975, 0.001910370295165490350, 0.002878829377803309320 ),
 .UNSPECIFIED. ) ;
#25121 = CARTESIAN_POINT ( 'NONE',  ( 96.76471471792625323, -35.27954033865438532, 181.2156252759109805 ) ) ;
#25122 = ORIENTED_EDGE ( 'NONE', *, *, #39119, .F. ) ;
#25123 = ORIENTED_EDGE ( 'NONE', *, *, #21826, .T. ) ;
#25124 = CARTESIAN_POINT ( 'NONE',  ( 125.9429424436864196, -84.18539835298642515, 250.2201230397200220 ) ) ;
#25125 = CARTESIAN_POINT ( 'NONE',  ( 102.0670550280536446, -27.97049802139369135, 151.4897919364310894 ) ) ;
#25126 = LINE ( 'NONE', #79675, #58082 ) ;
#25127 = DIRECTION ( 'NONE',  ( -1.000000000000000000, -8.163404592831600092E-16, -1.020425574103949962E-15 ) ) ;
#25128 = VECTOR ( 'NONE', #62416, 1000.000000000000000 ) ;
#25129 = ORIENTED_EDGE ( 'NONE', *, *, #88602, .F. ) ;
#25130 = CARTESIAN_POINT ( 'NONE',  ( -4.829308837915109898, 94.20942664101627884, 118.2592588614345885 ) ) ;
#25131 = EDGE_CURVE ( 'NONE', #14095, #69623, #68391, .T. ) ;
#25132 = CARTESIAN_POINT ( 'NONE',  ( 113.7507820938996872, -44.72989589602062210, 193.1299109901969757 ) ) ;
#25133 = FACE_OUTER_BOUND ( 'NONE', #38950, .T. ) ;
#25134 = VERTEX_POINT ( 'NONE', #52478 ) ;
#25135 = ORIENTED_EDGE ( 'NONE', *, *, #65535, .F. ) ;
#25136 = CARTESIAN_POINT ( 'NONE',  ( -11.75195648705195062, 77.68235131038592556, 117.9724202733717817 ) ) ;
#25137 = CARTESIAN_POINT ( 'NONE',  ( 194.0371591254575492, -24.42818131005407167, 129.9678068554150343 ) ) ;
#25138 = CARTESIAN_POINT ( 'NONE',  ( 107.0664832912739683, -18.82844715994099971, 199.5838068554169809 ) ) ;
#25139 = CARTESIAN_POINT ( 'NONE',  ( 115.6923476351215641, -37.43328618085965331, 36.59189989340094940 ) ) ;
#25140 = DIRECTION ( 'NONE',  ( 1.000000000000000078E-15, -1.000000000000000000, 0.000000000000000000 ) ) ;
#25141 = ORIENTED_EDGE ( 'NONE', *, *, #19256, .F. ) ;
#25142 = CARTESIAN_POINT ( 'NONE',  ( 180.2121375201600131, -29.73316016639650172, 117.4678068554150627 ) ) ;
#25143 = CARTESIAN_POINT ( 'NONE',  ( 82.19340217263071224, -16.98608769072388824, 7.448832051633130114 ) ) ;
#25144 = ORIENTED_EDGE ( 'NONE', *, *, #77180, .T. ) ;
#25145 = ORIENTED_EDGE ( 'NONE', *, *, #85183, .F. ) ;
#25146 = AXIS2_PLACEMENT_3D ( 'NONE', #75692, #13460, #7544 ) ;
#25147 = EDGE_CURVE ( 'NONE', #11800, #9965, #79190, .T. ) ;
#25148 = CARTESIAN_POINT ( 'NONE',  ( 41.56648329127399677, 0.2215528400590013880, 316.8086252759120498 ) ) ;
#25149 = VERTEX_POINT ( 'NONE', #25700 ) ;
#25150 = ORIENTED_EDGE ( 'NONE', *, *, #6536, .T. ) ;
#25151 = CARTESIAN_POINT ( 'NONE',  ( 100.9536334643962903, -28.70783906175504896, 156.5938426686704759 ) ) ;
#25152 = CARTESIAN_POINT ( 'NONE',  ( 106.6171843113225606, -27.68451483556421522, 44.55051506617196821 ) ) ;
#25153 = CARTESIAN_POINT ( 'NONE',  ( 97.38146765292194118, -40.64695096355149673, 206.6327681330539860 ) ) ;
#25154 = CARTESIAN_POINT ( 'NONE',  ( 114.4473569665854313, -28.53271593493105485, 159.5051490854349652 ) ) ;
#25156 = CARTESIAN_POINT ( 'NONE',  ( 99.39693184722126773, -28.77005263954443492, 261.6746728949588032 ) ) ;
#25155 = DIRECTION ( 'NONE',  ( 1.000000000000000078E-15, 1.000000000000000083E-30, -1.000000000000000000 ) ) ;
#25157 = DIRECTION ( 'NONE',  ( -0.04216478779797398074, 0.9991106698809455455, 0.000000000000000000 ) ) ;
#25158 = DIRECTION ( 'NONE',  ( 0.7071067812123270624, 0.7071067811607679721, 0.000000000000000000 ) ) ;
#25160 = ORIENTED_EDGE ( 'NONE', *, *, #65974, .T. ) ;
#25159 = EDGE_CURVE ( 'NONE', #14582, #67680, #74750, .T. ) ;
#25161 = EDGE_CURVE ( 'NONE', #69894, #26619, #60654, .T. ) ;
#25162 = ORIENTED_EDGE ( 'NONE', *, *, #67160, .F. ) ;
#25163 = DIRECTION ( 'NONE',  ( 1.000000000000000000, -5.337610695313248426E-16, 0.000000000000000000 ) ) ;
#25164 = CARTESIAN_POINT ( 'NONE',  ( 115.8924960319658055, -44.71257290243538307, 233.2413395616259493 ) ) ;
#25165 = ORIENTED_EDGE ( 'NONE', *, *, #39495, .T. ) ;
#25166 = CARTESIAN_POINT ( 'NONE',  ( 100.0080109101350985, -27.21007462382121744, 185.5841967044829630 ) ) ;
#25167 = DIRECTION ( 'NONE',  ( 1.000000000000000000, 1.132880637372608296E-15, 0.000000000000000000 ) ) ;
#25168 = CIRCLE ( 'NONE', #62907, 2.749999999999974687 ) ;
#25169 = CARTESIAN_POINT ( 'NONE',  ( -16.71522554099469815, 66.30250908626825890, 34.24257953154918965 ) ) ;
#25170 = ADVANCED_FACE ( 'NONE', ( #32502 ), #4817, .T. ) ;
#25171 = CARTESIAN_POINT ( 'NONE',  ( 162.5667039024470171, -33.35206098992711077, 342.9256252759109884 ) ) ;
#25172 = DIRECTION ( 'NONE',  ( 0.000000000000000000, 0.000000000000000000, 1.000000000000000000 ) ) ;
#25175 = CARTESIAN_POINT ( 'NONE',  ( 109.2074818670226222, -48.35976665079980563, 273.7213395616252569 ) ) ;
#25174 = DIRECTION ( 'NONE',  ( 5.512527431108029424E-15, -1.000000000000000000, 0.000000000000000000 ) ) ;
#25173 = CARTESIAN_POINT ( 'NONE',  ( 97.94068279941657806, -40.34109379996354505, 277.6356252759109111 ) ) ;
#25176 = FACE_OUTER_BOUND ( 'NONE', #64574, .T. ) ;
#25177 = DIRECTION ( 'NONE',  ( 1.000000000000000000, 0.000000000000000000, 9.462128050782575008E-16 ) ) ;
#25178 = LINE ( 'NONE', #52840, #28119 ) ;
#25179 = AXIS2_PLACEMENT_3D ( 'NONE', #43260, #84633, #7412 ) ;
#25180 = DIRECTION ( 'NONE',  ( -8.252657816380299978E-16, -2.773339119917620066E-31, -1.000000000000000000 ) ) ;
#25181 = DIRECTION ( 'NONE',  ( -3.201858731750027727E-15, 1.000000000000000000, -3.201858731750027724E-30 ) ) ;
#25182 = ADVANCED_FACE ( 'NONE', ( #45136 ), #24277, .T. ) ;
#25183 = CARTESIAN_POINT ( 'NONE',  ( 134.0664832912740110, -8.350947159940998787, 293.6356252759119911 ) ) ;
#25185 = VERTEX_POINT ( 'NONE', #40116 ) ;
#25184 = CARTESIAN_POINT ( 'NONE',  ( 107.0667039024470313, -104.2784471599418197, -11.78219314458200984 ) ) ;
#25186 = CARTESIAN_POINT ( 'NONE',  ( 136.5307003794597449, -19.95069274173234675, 7.120636252907847741 ) ) ;
#25187 = CARTESIAN_POINT ( 'NONE',  ( 104.1796880194223576, -26.65200820554803585, 225.2984824187679749 ) ) ;
#25188 = CARTESIAN_POINT ( 'NONE',  ( 98.85791787721181834, -43.21333385077131339, 87.85848241876792031 ) ) ;
#25189 = CARTESIAN_POINT ( 'NONE',  ( 106.8507155540331013, -47.82678659975260160, 223.5489586092439538 ) ) ;
#25190 = DIRECTION ( 'NONE',  ( -1.000000000000000078E-15, 1.000000000000000083E-30, 1.000000000000000000 ) ) ;
#25191 = DIRECTION ( 'NONE',  ( 0.000000000000000000, 0.000000000000000000, 1.000000000000000000 ) ) ;
#25193 = CARTESIAN_POINT ( 'NONE',  ( 116.3376065436754203, -32.98135602958129908, 40.13195101788765840 ) ) ;
#25192 = LINE ( 'NONE', #23443, #27561 ) ;
#25194 = CARTESIAN_POINT ( 'NONE',  ( 131.0667039024480118, -58.35344715994099829, 228.3338068554150198 ) ) ;
#25195 = AXIS2_PLACEMENT_3D ( 'NONE', #89620, #62785, #14203 ) ;
#25196 = CARTESIAN_POINT ( 'NONE',  ( 131.5325842222575545, -19.79809288067805539, 2.811527366592877275 ) ) ;
#25197 = EDGE_LOOP ( 'NONE', ( #41750, #81629, #47526, #14391 ) ) ;
#25198 = ORIENTED_EDGE ( 'NONE', *, *, #12792, .F. ) ;
#25199 = CARTESIAN_POINT ( 'NONE',  ( 107.8370078009992028, -28.22187835749811313, 154.4267055423619581 ) ) ;
#25200 = EDGE_CURVE ( 'NONE', #27479, #78184, #85026, .T. ) ;
#25202 = ORIENTED_EDGE ( 'NONE', *, *, #83386, .T. ) ;
#25201 = DIRECTION ( 'NONE',  ( -0.000000000000000000, -1.000000000000000000, 0.000000000000000000 ) ) ;
#25203 = CARTESIAN_POINT ( 'NONE',  ( 97.33783051261163166, -34.07110767403877816, 91.11349398838056857 ) ) ;
#25204 = CARTESIAN_POINT ( 'NONE',  ( 117.1049515565468226, -33.87427183379793405, 145.0470538473399529 ) ) ;
#25205 = PLANE ( 'NONE',  #65696 ) ;
#25206 = EDGE_CURVE ( 'NONE', #69283, #74946, #25564, .T. ) ;
#25207 = EDGE_CURVE ( 'NONE', #73831, #86897, #26972, .T. ) ;
#25208 = DIRECTION ( 'NONE',  ( -0.7071067811868619879, -0.7071067811862330466, -7.071067811868613027E-16 ) ) ;
#25209 = DIRECTION ( 'NONE',  ( -1.000000000000000000, 0.000000000000000000, 0.000000000000000000 ) ) ;
#25210 = LINE ( 'NONE', #81553, #48319 ) ;
#25211 = ADVANCED_FACE ( 'NONE', ( #39231 ), #86506, .T. ) ;
#25212 = CARTESIAN_POINT ( 'NONE',  ( 115.6651410650259066, -32.06827565682259262, 69.22133956162596746 ) ) ;
#25213 = ORIENTED_EDGE ( 'NONE', *, *, #76468, .F. ) ;
#25214 = EDGE_LOOP ( 'NONE', ( #52105, #27194 ) ) ;
#25215 = ORIENTED_EDGE ( 'NONE', *, *, #57036, .F. ) ;
#25216 = VECTOR ( 'NONE', #71014, 1000.000000000000000 ) ;
#25217 = LINE ( 'NONE', #17523, #15280 ) ;
#25219 = CARTESIAN_POINT ( 'NONE',  ( 97.81480632908598238, -40.51613010894325839, 171.6358981596145270 ) ) ;
#25218 = CARTESIAN_POINT ( 'NONE',  ( 98.56701561008813428, -30.78824967682752245, 156.8289586092439549 ) ) ;
#25220 = AXIS2_PLACEMENT_3D ( 'NONE', #49617, #34208, #6960 ) ;
#25221 = CARTESIAN_POINT ( 'NONE',  ( 53.35959712126198440, -48.62134037875358672, 129.9678068554150911 ) ) ;
#25222 = DIRECTION ( 'NONE',  ( 0.000000000000000000, 1.000000000000000000, 0.000000000000000000 ) ) ;
#25223 = FACE_OUTER_BOUND ( 'NONE', #61595, .T. ) ;
#25224 = CARTESIAN_POINT ( 'NONE',  ( 92.06080542007410372, 85.83559868056555331, 74.70172715947595066 ) ) ;
#25225 = DIRECTION ( 'NONE',  ( 0.000000000000000000, 0.000000000000000000, -1.000000000000000000 ) ) ;
#25226 = CARTESIAN_POINT ( 'NONE',  ( 101.7220374796296909, -27.76276858577399409, 85.50419670448295051 ) ) ;
#25227 = ORIENTED_EDGE ( 'NONE', *, *, #73583, .T. ) ;
#25228 = ORIENTED_EDGE ( 'NONE', *, *, #11710, .F. ) ;
#25229 = DIRECTION ( 'NONE',  ( 0.000000000000000000, 0.000000000000000000, -1.000000000000000000 ) ) ;
#25230 = CARTESIAN_POINT ( 'NONE',  ( 126.9292520036857894, 49.86282737081235439, 30.55937423833577071 ) ) ;
#25231 = CARTESIAN_POINT ( 'NONE',  ( 95.60734603896359829, -36.72944715994100306, 309.2406250056037038 ) ) ;
#25232 = CARTESIAN_POINT ( 'NONE',  ( 98.88612577743202792, -36.32393613343754879, 169.1052332267339580 ) ) ;
#25233 = AXIS2_PLACEMENT_3D ( 'NONE', #74954, #46773, #39531 ) ;
#25234 = CIRCLE ( 'NONE', #62981, 0.5000000000000004441 ) ;
#25235 = ADVANCED_FACE ( 'NONE', ( #18335 ), #74211, .T. ) ;
#25236 = CARTESIAN_POINT ( 'NONE',  ( 119.5435152932140426, -31.57448135767196362, 289.6356252759106837 ) ) ;
#25237 = ORIENTED_EDGE ( 'NONE', *, *, #38423, .F. ) ;
#25238 = VERTEX_POINT ( 'NONE', #45569 ) ;
#25239 = DIRECTION ( 'NONE',  ( 0.7071067811864671926, 0.7071067811866279529, 6.612322855854137577E-17 ) ) ;
#25240 = AXIS2_PLACEMENT_3D ( 'NONE', #23426, #10650, #64737 ) ;
#25241 = ORIENTED_EDGE ( 'NONE', *, *, #72157, .F. ) ;
#25242 = ORIENTED_EDGE ( 'NONE', *, *, #80592, .T. ) ;
#25243 = DIRECTION ( 'NONE',  ( 0.000000000000000000, 0.000000000000000000, -1.000000000000000000 ) ) ;
#25244 = CARTESIAN_POINT ( 'NONE',  ( 100.2828564484647274, -30.98100942051235052, 212.1987261630399360 ) ) ;
#25245 = DIRECTION ( 'NONE',  ( 4.194175870806139918E-14, -1.000000000000000000, 0.000000000000000000 ) ) ;
#25246 = DIRECTION ( 'NONE',  ( 1.000000000000000078E-15, -1.000000000000000000, 0.000000000000000000 ) ) ;
#25247 = CARTESIAN_POINT ( 'NONE',  ( -76.20505178924449297, 120.6499999999999915, 76.20505178924310030 ) ) ;
#25248 = VERTEX_POINT ( 'NONE', #11987 ) ;
#25249 = ORIENTED_EDGE ( 'NONE', *, *, #55807, .T. ) ;
#25250 = ADVANCED_FACE ( 'NONE', ( #11073 ), #4722, .F. ) ;
#25251 = ORIENTED_EDGE ( 'NONE', *, *, #4944, .T. ) ;
#25252 = ORIENTED_EDGE ( 'NONE', *, *, #6806, .F. ) ;
#25253 = ADVANCED_FACE ( 'NONE', ( #38778 ), #53277, .T. ) ;
#25254 = CARTESIAN_POINT ( 'NONE',  ( 104.5243549119882829, -45.65320838865366682, 215.1738046553059860 ) ) ;
#25255 = EDGE_CURVE ( 'NONE', #4284, #20155, #25601, .T. ) ;
#25256 = CARTESIAN_POINT ( 'NONE',  ( 117.3932167392688655, -32.72270067050601483, 94.10895860924395606 ) ) ;
#25257 = CARTESIAN_POINT ( 'NONE',  ( 104.0490797691969647, -47.33883444496888160, 67.36800622829191809 ) ) ;
#25258 = CARTESIAN_POINT ( 'NONE',  ( 116.8184952045819500, -34.15823809959283608, 254.0314695188159533 ) ) ;
#25259 = CARTESIAN_POINT ( 'NONE',  ( 97.81168895331838087, -40.51742574516882200, 287.6356252759109680 ) ) ;
#25260 = CARTESIAN_POINT ( 'NONE',  ( 134.0664832912740110, -46.42944715994100591, 4.925625275910997303 ) ) ;
#25261 = CARTESIAN_POINT ( 'NONE',  ( 117.4572939498068820, -40.49840382496243052, 169.5375300378159693 ) ) ;
#25262 = CARTESIAN_POINT ( 'NONE',  ( -479.3614999999999782, 3.174999999999999822, -1.387778780781445991E-14 ) ) ;
#25263 = ORIENTED_EDGE ( 'NONE', *, *, #37965, .T. ) ;
#25264 = DIRECTION ( 'NONE',  ( -0.5184798493102225070, -0.5184798493102369399, -0.6799685961266761502 ) ) ;
#25266 = VERTEX_POINT ( 'NONE', #11534 ) ;
#25265 = EDGE_CURVE ( 'NONE', #970, #77829, #31966, .T. ) ;
#25267 = EDGE_CURVE ( 'NONE', #63618, #78225, #88302, .T. ) ;
#25268 = ORIENTED_EDGE ( 'NONE', *, *, #56884, .F. ) ;
#25269 = LINE ( 'NONE', #18007, #11456 ) ;
#25270 = DIRECTION ( 'NONE',  ( 0.000000000000000000, 1.000000000000000000, 0.000000000000000000 ) ) ;
#25271 = ORIENTED_EDGE ( 'NONE', *, *, #8710, .T. ) ;
#25272 = ADVANCED_FACE ( 'NONE', ( #3382 ), #12067, .F. ) ;
#25273 = DIRECTION ( 'NONE',  ( 0.7071067811571474238, 0.7071067812159476107, 0.000000000000000000 ) ) ;
#25274 = ORIENTED_EDGE ( 'NONE', *, *, #89065, .T. ) ;
#25275 =( BOUNDED_CURVE ( )  B_SPLINE_CURVE ( 3, ( #88785, #20186, #75141, #81975 ),
 .UNSPECIFIED., .F., .T. ) 
 B_SPLINE_CURVE_WITH_KNOTS ( ( 4, 4 ),
 ( 2.074222157386416767E-12, 1.570796326797197162 ),
 .UNSPECIFIED. ) 
 CURVE ( )  GEOMETRIC_REPRESENTATION_ITEM ( )  RATIONAL_B_SPLINE_CURVE ( ( 1.000000000000000000, 0.8047378541243116468, 0.8047378541243116468, 1.000000000000000000 ) ) 
 REPRESENTATION_ITEM ( '' )  );
#25276 = DIRECTION ( 'NONE',  ( 0.000000000000000000, 0.000000000000000000, 1.000000000000000000 ) ) ;
#25277 = CARTESIAN_POINT ( 'NONE',  ( 102.9709959788349636, -46.31662683568885086, 92.25562527591097250 ) ) ;
#25278 = DIRECTION ( 'NONE',  ( -0.000000000000000000, 1.000000000000000000, 0.000000000000000000 ) ) ;
#25279 = AXIS2_PLACEMENT_3D ( 'NONE', #70781, #70325, #8553 ) ;
#25280 = EDGE_CURVE ( 'NONE', #77074, #76783, #67834, .T. ) ;
#25281 = LINE ( 'NONE', #24405, #75387 ) ;
#25282 = DIRECTION ( 'NONE',  ( 1.000000000000000078E-15, -1.000000000000000083E-30, -1.000000000000000000 ) ) ;
#25283 = CARTESIAN_POINT ( 'NONE',  ( 116.4859054502389881, -39.36344060769046393, 98.60991099019695127 ) ) ;
#25285 = CARTESIAN_POINT ( 'NONE',  ( 102.9757002774702102, -26.48594595611790581, 171.3908633711489813 ) ) ;
#25284 = CARTESIAN_POINT ( 'NONE',  ( 0.000000000000000000, 65.60000000000000853, 118.3560000000000088 ) ) ;
#25286 = CARTESIAN_POINT ( 'NONE',  ( 71.09939861440099662, 0.000000000000000000, 177.8662485265279827 ) ) ;
#25287 = DIRECTION ( 'NONE',  ( -0.0001211784769825758571, 0.7071067708032323651, 0.7071067811865486830 ) ) ;
#25288 = ORIENTED_EDGE ( 'NONE', *, *, #82913, .T. ) ;
#25289 = DIRECTION ( 'NONE',  ( 1.000000000000000000, -0.000000000000000000, 0.000000000000000000 ) ) ;
#25290 = LINE ( 'NONE', #24853, #70357 ) ;
#25291 = DIRECTION ( 'NONE',  ( 2.900000000000000265E-14, -2.000000000000000155E-15, 1.000000000000000000 ) ) ;
#25292 = EDGE_CURVE ( 'NONE', #35473, #43151, #47816, .T. ) ;
#25293 = CARTESIAN_POINT ( 'NONE',  ( -29.99999999999998224, 172.0000000000000000, 113.8826257785461280 ) ) ;
#25295 = ORIENTED_EDGE ( 'NONE', *, *, #4689, .T. ) ;
#25294 = CARTESIAN_POINT ( 'NONE',  ( 100.7967938542458199, -45.88935316334050185, 242.1108633711489517 ) ) ;
#25296 = CARTESIAN_POINT ( 'NONE',  ( 97.81168736999980240, -40.51740164104307240, 32.63591986563997693 ) ) ;
#25297 = CARTESIAN_POINT ( 'NONE',  ( 118.2085198165198676, -40.76548936363617059, 19.54991099019698453 ) ) ;
#25298 = CARTESIAN_POINT ( 'NONE',  ( 103.4533635841105479, -46.55483943026052174, 138.2956252759109645 ) ) ;
#25299 = FACE_OUTER_BOUND ( 'NONE', #39730, .T. ) ;
#25300 = CARTESIAN_POINT ( 'NONE',  ( 82.81058719979546368, -36.91414947189120710, 6.758631288822928518 ) ) ;
#25301 = DIRECTION ( 'NONE',  ( 0.4634479843259247112, 0.000000000000000000, 0.8861241255175470455 ) ) ;
#25302 = LINE ( 'NONE', #38051, #77016 ) ;
#25303 = ORIENTED_EDGE ( 'NONE', *, *, #78800, .T. ) ;
#25304 = AXIS2_PLACEMENT_3D ( 'NONE', #42101, #1239, #6696 ) ;
#25305 = VECTOR ( 'NONE', #32333, 1000.000000000000000 ) ;
#25306 = AXIS2_PLACEMENT_3D ( 'NONE', #16151, #85206, #9326 ) ;
#25307 = EDGE_LOOP ( 'NONE', ( #31365, #17122, #11546, #83026 ) ) ;
#25308 = ORIENTED_EDGE ( 'NONE', *, *, #23105, .F. ) ;
#25309 = AXIS2_PLACEMENT_3D ( 'NONE', #85208, #29333, #76580 ) ;
#25310 = CIRCLE ( 'NONE', #10977, 2.750000000000002665 ) ;
#25311 = EDGE_LOOP ( 'NONE', ( #20406, #8930, #19570, #16120 ) ) ;
#25312 = CARTESIAN_POINT ( 'NONE',  ( 138.8167039024479834, -50.82844715994100682, 58.80080685541479824 ) ) ;
#25313 = CARTESIAN_POINT ( 'NONE',  ( 115.5933672690473912, -28.53551910654245205, 35.43562527591098643 ) ) ;
#25314 = CARTESIAN_POINT ( 'NONE',  ( 61.56670390244730839, -23.42844715994043980, 249.9678068554150343 ) ) ;
#25315 = DIRECTION ( 'NONE',  ( 0.000000000000000000, 1.000000000000000000, 0.000000000000000000 ) ) ;
#25316 = EDGE_CURVE ( 'NONE', #86595, #18695, #62797, .T. ) ;
#25319 = ADVANCED_FACE ( 'NONE', ( #81933, #20144 ), #75098, .T. ) ;
#25318 = DIRECTION ( 'NONE',  ( 0.000000000000000000, 0.000000000000000000, 1.000000000000000000 ) ) ;
#25317 = DIRECTION ( 'NONE',  ( 1.000000000000000000, 0.000000000000000000, 0.000000000000000000 ) ) ;
#25320 = CARTESIAN_POINT ( 'NONE',  ( 98.21912858861395534, -34.79631884261151242, 255.5657531614102709 ) ) ;
#25321 = EDGE_LOOP ( 'NONE', ( #61169, #74273, #36051, #34605 ) ) ;
#25322 = ORIENTED_EDGE ( 'NONE', *, *, #7188, .T. ) ;
#25323 = VERTEX_POINT ( 'NONE', #88743 ) ;
#25324 = DIRECTION ( 'NONE',  ( -0.000000000000000000, 1.000000000000000000, 0.000000000000000000 ) ) ;
#25325 = CARTESIAN_POINT ( 'NONE',  ( 116.7485963143377461, -34.15446243945111604, 184.0333798272055503 ) ) ;
#25326 = DIRECTION ( 'NONE',  ( 0.000000000000000000, 0.000000000000000000, -1.000000000000000000 ) ) ;
#25327 = CARTESIAN_POINT ( 'NONE',  ( 114.9896934147946013, -32.69399539773264252, 40.63301187732598407 ) ) ;
#25328 = CARTESIAN_POINT ( 'NONE',  ( 118.1268318574024505, 90.28416741362497078, -10.08204661438621841 ) ) ;
#25329 = DIRECTION ( 'NONE',  ( 1.000000000000000078E-15, -1.000000000000000083E-30, -1.000000000000000000 ) ) ;
#25330 = CARTESIAN_POINT ( 'NONE',  ( 96.81359797424451585, -35.17473563989037899, 221.1946728949589840 ) ) ;
#25331 = LINE ( 'NONE', #73939, #55886 ) ;
#25332 = ORIENTED_EDGE ( 'NONE', *, *, #8194, .T. ) ;
#25333 = LINE ( 'NONE', #46206, #2768 ) ;
#25334 = FACE_OUTER_BOUND ( 'NONE', #85876, .T. ) ;
#25335 = CARTESIAN_POINT ( 'NONE',  ( 106.2223766104409037, -28.61050573088338922, 47.97666179816295795 ) ) ;
#25336 = STYLED_ITEM ( 'NONE', ( #67264 ), #79963 ) ;
#25337 = CARTESIAN_POINT ( 'NONE',  ( 135.2364670978548986, -16.23881677343959495, 8.012604157991546572 ) ) ;
#25338 = AXIS2_PLACEMENT_3D ( 'NONE', #8668, #36366, #37258 ) ;
#25339 = CARTESIAN_POINT ( 'NONE',  ( 148.0533267522752112, 101.5999999999999943, 160.2664750769284865 ) ) ;
#25340 = CARTESIAN_POINT ( 'NONE',  ( 98.30752845723139899, -41.72886325947258968, 192.7396747606553049 ) ) ;
#25341 = ORIENTED_EDGE ( 'NONE', *, *, #4248, .T. ) ;
#25342 = DIRECTION ( 'NONE',  ( -0.000000000000000000, -0.000000000000000000, 1.000000000000000000 ) ) ;
#25343 = CARTESIAN_POINT ( 'NONE',  ( 125.0952692105185804, 56.35416992947224912, -37.36429652679031221 ) ) ;
#25344 = ORIENTED_EDGE ( 'NONE', *, *, #81789, .T. ) ;
#25345 = CARTESIAN_POINT ( 'NONE',  ( 117.8566403422286299, -39.12769616061267186, 103.6403871806729455 ) ) ;
#25346 = ORIENTED_EDGE ( 'NONE', *, *, #55189, .T. ) ;
#25347 = CARTESIAN_POINT ( 'NONE',  ( 115.4237413257435918, -38.49363815508749553, 63.08384839950497991 ) ) ;
#25348 = CARTESIAN_POINT ( 'NONE',  ( 172.5664832912740110, -32.07844715994070839, 323.6756252759119548 ) ) ;
#25349 = CARTESIAN_POINT ( 'NONE',  ( 98.25403324269851169, -37.66165033158306130, 122.8415833058969469 ) ) ;
#25350 = CARTESIAN_POINT ( 'NONE',  ( 165.6738106836199904, -26.00627455219321860, 342.9256252759119548 ) ) ;
#25351 = FACE_OUTER_BOUND ( 'NONE', #80122, .T. ) ;
#25352 = ADVANCED_FACE ( 'NONE', ( #21485, #75992 ), #28275, .F. ) ;
#25353 = CARTESIAN_POINT ( 'NONE',  ( 99.11086226171772751, -44.43615201859483932, 37.95086337114900488 ) ) ;
#25354 = CARTESIAN_POINT ( 'NONE',  ( -487.2989999999999782, 14.28750000000036025, 2.863608028952925100 ) ) ;
#25355 = ORIENTED_EDGE ( 'NONE', *, *, #51396, .T. ) ;
#25356 = CARTESIAN_POINT ( 'NONE',  ( 98.30762054419153628, -41.72908882781142381, 256.7397536183686384 ) ) ;
#25357 = CIRCLE ( 'NONE', #36980, 6.571100913904396101 ) ;
#25358 = VERTEX_POINT ( 'NONE', #27389 ) ;
#25359 = CARTESIAN_POINT ( 'NONE',  ( -118.4859477596447306, 70.52090377575432001, 4.094325160632186211 ) ) ;
#25360 = CIRCLE ( 'NONE', #9485, 3.700000000000001954 ) ;
#25361 = AXIS2_PLACEMENT_3D ( 'NONE', #55250, #48428, #27123 ) ;
#25362 = ORIENTED_EDGE ( 'NONE', *, *, #27128, .T. ) ;
#25364 = EDGE_CURVE ( 'NONE', #25889, #47935, #16420, .T. ) ;
#25363 = ORIENTED_EDGE ( 'NONE', *, *, #26660, .F. ) ;
#25365 = EDGE_CURVE ( 'NONE', #24255, #2062, #43954, .T. ) ;
#25366 = AXIS2_PLACEMENT_3D ( 'NONE', #70555, #84644, #36485 ) ;
#25368 = EDGE_CURVE ( 'NONE', #13204, #64268, #70094, .T. ) ;
#25367 = VECTOR ( 'NONE', #44321, 1000.000000000000000 ) ;
#25369 = LINE ( 'NONE', #12646, #83285 ) ;
#25370 = EDGE_LOOP ( 'NONE', ( #1487, #3433 ) ) ;
#25371 = CARTESIAN_POINT ( 'NONE',  ( 115.4101910119110386, -30.57141770992054219, 259.3203871806734355 ) ) ;
#25372 = CARTESIAN_POINT ( 'NONE',  ( 51.56670390244699576, -22.48495420874030515, -5.074374724088000832 ) ) ;
#25373 = CARTESIAN_POINT ( 'NONE',  ( 122.2221484686745470, -111.9799080603168022, -11.78219314458175937 ) ) ;
#25374 = CARTESIAN_POINT ( 'NONE',  ( 103.5987781142019202, -46.56090220241721767, 53.30705384733997221 ) ) ;
#25375 = CARTESIAN_POINT ( 'NONE',  ( 101.9932059899096402, -45.44583378561615916, 43.15642108796611609 ) ) ;
#25376 = ORIENTED_EDGE ( 'NONE', *, *, #71843, .T. ) ;
#25377 = CARTESIAN_POINT ( 'NONE',  ( 108.4174567856275075, -26.73502315347771230, 114.9708767927032227 ) ) ;
#25378 = EDGE_CURVE ( 'NONE', #2431, #5415, #55515, .T. ) ;
#25379 = CYLINDRICAL_SURFACE ( 'NONE', #83964, 10.00000000000000355 ) ;
#25380 = VECTOR ( 'NONE', #54115, 1000.000000000000000 ) ;
#25381 = ORIENTED_EDGE ( 'NONE', *, *, #20989, .F. ) ;
#25382 = EDGE_CURVE ( 'NONE', #69025, #837, #61392, .T. ) ;
#25383 = DIRECTION ( 'NONE',  ( -1.000000000000000000, 0.000000000000000000, 0.000000000000000000 ) ) ;
#25384 = FACE_OUTER_BOUND ( 'NONE', #74312, .T. ) ;
#25385 = CARTESIAN_POINT ( 'NONE',  ( 106.5683798796750779, -47.15615894637593897, 247.5384824187679556 ) ) ;
#25386 = PLANE ( 'NONE',  #14167 ) ;
#25387 = AXIS2_PLACEMENT_3D ( 'NONE', #73771, #39250, #45587 ) ;
#25388 = DIRECTION ( 'NONE',  ( -1.000000000000000000, -4.238735976179846264E-15, 0.000000000000000000 ) ) ;
#25389 = CARTESIAN_POINT ( 'NONE',  ( 77.61460381940304387, -37.97617057399400409, 2.716753174564080275 ) ) ;
#25390 = EDGE_CURVE ( 'NONE', #89450, #44698, #57055, .T. ) ;
#25391 = CARTESIAN_POINT ( 'NONE',  ( 99.00226700525801959, -39.63126001020209799, 266.0238483995056527 ) ) ;
#25393 = CARTESIAN_POINT ( 'NONE',  ( 112.5028774994481466, -27.85959465031284310, 90.63848241876793566 ) ) ;
#25392 = CARTESIAN_POINT ( 'NONE',  ( 163.1639762274590169, -34.03355364505800651, -5.074374724088000832 ) ) ;
#25394 = CARTESIAN_POINT ( 'NONE',  ( 112.8147779832228963, 68.25761352872008558, 65.71143442840111959 ) ) ;
#25395 = CARTESIAN_POINT ( 'NONE',  ( 111.8142338872566626, -25.81671781287135303, 134.7499109901969518 ) ) ;
#25396 = VERTEX_POINT ( 'NONE', #34653 ) ;
#25397 = CARTESIAN_POINT ( 'NONE',  ( 107.0667039024470313, -104.2784471599418197, -11.78219314458200984 ) ) ;
#25398 = ORIENTED_EDGE ( 'NONE', *, *, #27135, .F. ) ;
#25399 = DIRECTION ( 'NONE',  ( 0.000000000000000000, 0.000000000000000000, -1.000000000000000000 ) ) ;
#25400 = CARTESIAN_POINT ( 'NONE',  ( 112.1393456299127251, -28.01282277393797315, 65.65645861032975006 ) ) ;
#25401 = CARTESIAN_POINT ( 'NONE',  ( 88.90000000000000568, 69.84999999999999432, 244.4749999999999943 ) ) ;
#25402 = VERTEX_POINT ( 'NONE', #82380 ) ;
#25403 = ADVANCED_FACE ( 'NONE', ( #62356 ), #61451, .T. ) ;
#25404 = CARTESIAN_POINT ( 'NONE',  ( 97.80798526467157217, -40.50836769862076636, 51.63484613625869457 ) ) ;
#25406 = ORIENTED_EDGE ( 'NONE', *, *, #82007, .F. ) ;
#25405 = CARTESIAN_POINT ( 'NONE',  ( 106.0722674988897296, -48.58863484196640314, 112.5099109901969712 ) ) ;
#25407 = CARTESIAN_POINT ( 'NONE',  ( 83.56670390244801183, -39.24694715994107952, 229.5838068554169524 ) ) ;
#25408 = DIRECTION ( 'NONE',  ( 1.000000000000000078E-15, -1.000000000000000083E-30, -1.000000000000000000 ) ) ;
#25409 = CYLINDRICAL_SURFACE ( 'NONE', #34356, 1.000000000000000888 ) ;
#25410 = AXIS2_PLACEMENT_3D ( 'NONE', #68634, #82729, #22733 ) ;
#25411 = FACE_OUTER_BOUND ( 'NONE', #72274, .T. ) ;
#25412 = EDGE_LOOP ( 'NONE', ( #18005, #2934, #5564, #65611 ) ) ;
#25413 = CARTESIAN_POINT ( 'NONE',  ( 117.6033054121008945, -33.31318886634804954, 134.0880062282919880 ) ) ;
#25414 = SHAPE_DEFINITION_REPRESENTATION ( #88094, #47290 ) ;
#25415 = AXIS2_PLACEMENT_3D ( 'NONE', #66061, #10222, #65627 ) ;
#25416 = PLANE ( 'NONE',  #21077 ) ;
#25417 = DIRECTION ( 'NONE',  ( -1.000000000000000000, -4.299999999999999979E-14, -1.000000000000000078E-15 ) ) ;
#25418 = EDGE_LOOP ( 'NONE', ( #21129, #2653, #65861, #215 ) ) ;
#25419 = ORIENTED_EDGE ( 'NONE', *, *, #81440, .F. ) ;
#25420 = CARTESIAN_POINT ( 'NONE',  ( 274.0659999999999741, 36.86249999999999716, -7.937500000000000000 ) ) ;
#25421 = CARTESIAN_POINT ( 'NONE',  ( 97.63151088911762088, 92.64985122628468162, -86.68005309089086552 ) ) ;
#25422 = FACE_OUTER_BOUND ( 'NONE', #45293, .T. ) ;
#25423 = CARTESIAN_POINT ( 'NONE',  ( 116.3279290549545806, -32.94269076977911226, 60.13562527591098927 ) ) ;
#25426 = EDGE_CURVE ( 'NONE', #38579, #88991, #13498, .T. ) ;
#25425 = CARTESIAN_POINT ( 'NONE',  ( -1.669011862100898913, 69.93236506402145380, -118.5470928879096562 ) ) ;
#25424 = CARTESIAN_POINT ( 'NONE',  ( 52.65249034007825912, -48.32844715994060181, 300.4678068554150059 ) ) ;
#25427 = CARTESIAN_POINT ( 'NONE',  ( 97.80797205823303386, -40.50833534217826326, 181.6348433549487424 ) ) ;
#25428 = AXIS2_PLACEMENT_3D ( 'NONE', #13274, #68686, #41843 ) ;
#25429 = ORIENTED_EDGE ( 'NONE', *, *, #71311, .T. ) ;
#25430 = CIRCLE ( 'NONE', #57319, 89.89999999999997726 ) ;
#25431 = CIRCLE ( 'NONE', #71876, 12.69999999999999929 ) ;
#25432 = CARTESIAN_POINT ( 'NONE',  ( 48.16670390244701139, -28.27351298637280408, -5.074374724088000832 ) ) ;
#25433 = CARTESIAN_POINT ( 'NONE',  ( 112.6540662323891837, -44.79745133516134104, 199.0584824187679374 ) ) ;
#25435 = VERTEX_POINT ( 'NONE', #35092 ) ;
#25434 = CARTESIAN_POINT ( 'NONE',  ( 73.06648329127396835, -8.729447159941065237, 14.92562527591093691 ) ) ;
#25436 = AXIS2_PLACEMENT_3D ( 'NONE', #61166, #27990, #55226 ) ;
#25437 = CARTESIAN_POINT ( 'NONE',  ( 96.86520444330115254, -38.59296402346411980, 47.48229194257691432 ) ) ;
#25438 = CARTESIAN_POINT ( 'NONE',  ( 116.9157166719834606, -38.71740874140498789, 53.66822714426762531 ) ) ;
#25439 = CARTESIAN_POINT ( 'NONE',  ( 97.46299999999996544, 82.54999999999999716, 1.020870737183004530E-12 ) ) ;
#25440 = VECTOR ( 'NONE', #76717, 1000.000000000000000 ) ;
#25441 = DIRECTION ( 'NONE',  ( 0.000000000000000000, -1.000000000000000000, 0.000000000000000000 ) ) ;
#25442 = ORIENTED_EDGE ( 'NONE', *, *, #41288, .T. ) ;
#25443 = EDGE_CURVE ( 'NONE', #56554, #54126, #10630, .T. ) ;
#25444 = CARTESIAN_POINT ( 'NONE',  ( 122.2189888861419433, -111.9861225405541347, -21.78219314458176825 ) ) ;
#25445 = VERTEX_POINT ( 'NONE', #41013 ) ;
#25446 = VERTEX_POINT ( 'NONE', #68734 ) ;
#25447 = AXIS2_PLACEMENT_3D ( 'NONE', #46303, #45853, #53560 ) ;
#25448 = CARTESIAN_POINT ( 'NONE',  ( 101.6176986403717279, -43.71793944654686470, 228.4815833058969758 ) ) ;
#25449 = EDGE_CURVE ( 'NONE', #45185, #12149, #6501, .T. ) ;
#25450 = CARTESIAN_POINT ( 'NONE',  ( 97.81847922488930180, -40.53401570104637841, 52.63663032143116993 ) ) ;
#25451 = CARTESIAN_POINT ( 'NONE',  ( -84.72230615113582530, 89.94765885072627043, 99.33304294513301613 ) ) ;
#25452 = AXIS2_PLACEMENT_3D ( 'NONE', #65082, #15605, #86434 ) ;
#25453 = CARTESIAN_POINT ( 'NONE',  ( 105.7154772353844265, -46.72385838015826920, 153.4689586016793612 ) ) ;
#25454 = CARTESIAN_POINT ( 'NONE',  ( 82.46407580264985882, -38.08864647353023258, 2.654395117673051363 ) ) ;
#25455 = EDGE_LOOP ( 'NONE', ( #16629, #13243, #19620, #39576 ) ) ;
#25456 = DIRECTION ( 'NONE',  ( 0.7071067811865506814, -0.7071067811865443531, 7.071067811865500971E-16 ) ) ;
#25457 = CARTESIAN_POINT ( 'NONE',  ( 70.63919639214310564, 91.07499999999996021, -53.97512327982435210 ) ) ;
#25458 = EDGE_LOOP ( 'NONE', ( #63808, #49487, #87362, #88859 ) ) ;
#25459 = CARTESIAN_POINT ( 'NONE',  ( 118.2087526870871415, -40.76557371769158777, 23.54991099019593292 ) ) ;
#25460 = ORIENTED_EDGE ( 'NONE', *, *, #52507, .F. ) ;
#25461 = VECTOR ( 'NONE', #46570, 1000.000000000000000 ) ;
#25462 = ORIENTED_EDGE ( 'NONE', *, *, #78641, .F. ) ;
#25463 = CARTESIAN_POINT ( 'NONE',  ( 105.9433607271350439, -44.81451498420922519, 255.2852332267341353 ) ) ;
#25464 = LINE ( 'NONE', #74061, #64799 ) ;
#25465 = CARTESIAN_POINT ( 'NONE',  ( 23.30868458379111985, 78.76602235523037621, 299.9862232315379629 ) ) ;
#25466 = CARTESIAN_POINT ( 'NONE',  ( 131.3179999999999836, 53.97500000000000142, 50.79999999999999716 ) ) ;
#25467 = DIRECTION ( 'NONE',  ( 9.351236661543306751E-17, -3.725950533538267725E-29, -1.000000000000000000 ) ) ;
#25469 = CARTESIAN_POINT ( 'NONE',  ( 108.1864281049355867, -47.13803512191609713, 198.6613395616249989 ) ) ;
#25468 = VECTOR ( 'NONE', #9100, 1000.000000000000000 ) ;
#25470 = DIRECTION ( 'NONE',  ( 0.7759704746411385523, -0.6307692307692301936, 0.000000000000000000 ) ) ;
#25471 = ORIENTED_EDGE ( 'NONE', *, *, #17389, .F. ) ;
#25472 = CARTESIAN_POINT ( 'NONE',  ( 101.6884573362309823, -27.70642928270265060, 81.50419670448295051 ) ) ;
#25473 = ORIENTED_EDGE ( 'NONE', *, *, #42132, .F. ) ;
#25475 = EDGE_CURVE ( 'NONE', #81368, #65933, #74440, .T. ) ;
#25474 = ORIENTED_EDGE ( 'NONE', *, *, #7573, .F. ) ;
#25477 = ORIENTED_EDGE ( 'NONE', *, *, #75735, .F. ) ;
#25476 = ADVANCED_FACE ( 'NONE', ( #29634 ), #85524, .F. ) ;
#25478 = ADVANCED_FACE ( 'NONE', ( #15574 ), #16019, .F. ) ;
#25479 = CARTESIAN_POINT ( 'NONE',  ( 99.09507348882181077, -30.55127953124965146, 160.8021594487345851 ) ) ;
#25480 = CARTESIAN_POINT ( 'NONE',  ( 184.5667039024483245, -48.82844715993448403, 300.4678068554149490 ) ) ;
#25481 = CARTESIAN_POINT ( 'NONE',  ( 0.000000000000000000, 60.82030000000000314, 258.9990212008905246 ) ) ;
#25482 = CARTESIAN_POINT ( 'NONE',  ( 112.6324121799619462, -43.35677846492738041, 145.9385665600669881 ) ) ;
#25483 = CARTESIAN_POINT ( 'NONE',  ( 96.11533564597472434, -35.06885359281673686, 217.1946728949589840 ) ) ;
#25484 = FACE_OUTER_BOUND ( 'NONE', #88293, .T. ) ;
#25485 = VERTEX_POINT ( 'NONE', #77794 ) ;
#25486 = CARTESIAN_POINT ( 'NONE',  ( 129.9449521816639788, 84.21449860606324478, -12.61764002986369171 ) ) ;
#25487 = EDGE_CURVE ( 'NONE', #84817, #80206, #23300, .T. ) ;
#25488 = CARTESIAN_POINT ( 'NONE',  ( 163.0822201311030142, 20.32000000000000028, 75.92468371870748456 ) ) ;
#25489 = ORIENTED_EDGE ( 'NONE', *, *, #40574, .T. ) ;
#25490 = ORIENTED_EDGE ( 'NONE', *, *, #55670, .T. ) ;
#25491 = AXIS2_PLACEMENT_3D ( 'NONE', #64114, #1884, #67221 ) ;
#25492 = VECTOR ( 'NONE', #9147, 1000.000000000000000 ) ;
#25493 = LINE ( 'NONE', #45911, #24225 ) ;
#25494 = VECTOR ( 'NONE', #69139, 1000.000000000000000 ) ;
#25495 = ORIENTED_EDGE ( 'NONE', *, *, #65670, .F. ) ;
#25496 = ORIENTED_EDGE ( 'NONE', *, *, #5174, .F. ) ;
#25497 = LINE ( 'NONE', #38233, #1894 ) ;
#25498 = DIRECTION ( 'NONE',  ( 0.8660254037844387076, -0.4999999999999998890, 0.000000000000000000 ) ) ;
#25499 = AXIS2_PLACEMENT_3D ( 'NONE', #54809, #75287, #13064 ) ;
#25500 = FACE_BOUND ( 'NONE', #26716, .T. ) ;
#25501 = ADVANCED_FACE ( 'NONE', ( #43246, #15114 ), #42790, .F. ) ;
#25502 = CARTESIAN_POINT ( 'NONE',  ( 108.5268020718178690, -45.14512305525489921, 167.1352769709339725 ) ) ;
#25503 = CARTESIAN_POINT ( 'NONE',  ( 118.1298445534695531, -37.63217702543061449, 38.77372051400595865 ) ) ;
#25504 = CARTESIAN_POINT ( 'NONE',  ( 68.36158985427030643, -82.61730200034398308, 247.4783998280180128 ) ) ;
#25505 = ORIENTED_EDGE ( 'NONE', *, *, #7917, .F. ) ;
#25506 = DIRECTION ( 'NONE',  ( 0.000000000000000000, 1.000000000000000000, 0.000000000000000000 ) ) ;
#25507 = ORIENTED_EDGE ( 'NONE', *, *, #15614, .T. ) ;
#25508 = PLANE ( 'NONE',  #1141 ) ;
#25509 = ORIENTED_EDGE ( 'NONE', *, *, #8692, .T. ) ;
#25510 = FACE_OUTER_BOUND ( 'NONE', #80749, .T. ) ;
#25511 = CYLINDRICAL_SURFACE ( 'NONE', #87939, 0.2499999999999941991 ) ;
#25512 = CARTESIAN_POINT ( 'NONE',  ( 116.5661000126995361, -33.54017338482336186, 134.0841521534302387 ) ) ;
#25513 = VECTOR ( 'NONE', #12440, 1000.000000000000000 ) ;
#25514 = DIRECTION ( 'NONE',  ( 1.000000000000000000, 0.000000000000000000, 6.982966722218760189E-15 ) ) ;
#25515 = EDGE_LOOP ( 'NONE', ( #89009, #79425, #55986, #51990 ) ) ;
#25516 = CARTESIAN_POINT ( 'NONE',  ( 116.7476796835742192, -31.34707987858772427, 29.24229194257799236 ) ) ;
#25517 = CARTESIAN_POINT ( 'NONE',  ( 97.24759266268939939, -33.09869426670887549, 62.04419670448196911 ) ) ;
#25518 = CIRCLE ( 'NONE', #24049, 3.000000000000002665 ) ;
#25520 = CARTESIAN_POINT ( 'NONE',  ( -72.96458098368751166, 101.5999999999999943, 72.96458098368620426 ) ) ;
#25519 = DIRECTION ( 'NONE',  ( 1.000000000000000000, 0.000000000000000000, 0.000000000000000000 ) ) ;
#25521 = CARTESIAN_POINT ( 'NONE',  ( 193.0374249753376432, -23.42844715993431848, 193.9678068554150343 ) ) ;
#25522 = LINE ( 'NONE', #45938, #70101 ) ;
#25523 = CARTESIAN_POINT ( 'NONE',  ( 50.96943157743499597, -34.03355364505720360, 237.4678068554150059 ) ) ;
#25524 = CARTESIAN_POINT ( 'NONE',  ( 106.8487982878802427, -25.26971417141049869, 322.7516258301318999 ) ) ;
#25525 = DIRECTION ( 'NONE',  ( 0.000000000000000000, 1.000000000000000000, 0.000000000000000000 ) ) ;
#25526 = ORIENTED_EDGE ( 'NONE', *, *, #9133, .F. ) ;
#25527 = CARTESIAN_POINT ( 'NONE',  ( 112.8421283165351809, -27.25026954951128388, 49.62895860924498947 ) ) ;
#25528 = CARTESIAN_POINT ( 'NONE',  ( 117.1921950572609603, -41.16159581679399793, 204.4861014663869696 ) ) ;
#25529 = CARTESIAN_POINT ( 'NONE',  ( 101.9498695335308014, -27.62134513440381411, 56.48419670448296159 ) ) ;
#25532 = EDGE_CURVE ( 'NONE', #35189, #37391, #85070, .T. ) ;
#25531 = CARTESIAN_POINT ( 'NONE',  ( 107.0664832912739968, -36.72944715994100306, -2.114374724089040924 ) ) ;
#25530 = CARTESIAN_POINT ( 'NONE',  ( 98.15104113905631777, -41.26173906225317722, 171.7005789228540777 ) ) ;
#25533 = CARTESIAN_POINT ( 'NONE',  ( 0.000000000000000000, 1.270000000000000018, -9.525000000000000355 ) ) ;
#25534 = CARTESIAN_POINT ( 'NONE',  ( 97.81170999498195329, -40.51745678363457159, 187.6351607544849287 ) ) ;
#25535 = ORIENTED_EDGE ( 'NONE', *, *, #77772, .T. ) ;
#25536 = CARTESIAN_POINT ( 'NONE',  ( 107.5699729851651938, -26.92841289699918050, 91.03562527591097364 ) ) ;
#25538 = VERTEX_POINT ( 'NONE', #78708 ) ;
#25537 = CARTESIAN_POINT ( 'NONE',  ( 9.368522474371046016, 91.14223545714233410, 130.2200199954151856 ) ) ;
#25539 = CARTESIAN_POINT ( 'NONE',  ( 97.49318720818088480, -40.89074837367928694, 227.6527681330539679 ) ) ;
#25540 = DIRECTION ( 'NONE',  ( 0.000000000000000000, 0.000000000000000000, 1.000000000000000000 ) ) ;
#25541 = CARTESIAN_POINT ( 'NONE',  ( 75.25757238336808541, -1.944390235229870978, 361.9756252759101471 ) ) ;
#25542 = LINE ( 'NONE', #11478, #60230 ) ;
#25543 = CARTESIAN_POINT ( 'NONE',  ( 102.0670549500623991, -27.97049806489031809, 46.48979194346625832 ) ) ;
#25544 = CARTESIAN_POINT ( 'NONE',  ( 133.0522658619989613, -39.28573230649611503, 1.785258109343265565 ) ) ;
#25545 = CARTESIAN_POINT ( 'NONE',  ( -185.9961463128564958, 101.5999999999999943, -3.174999999999349676 ) ) ;
#25546 = AXIS2_PLACEMENT_3D ( 'NONE', #9513, #38543, #36774 ) ;
#25547 = CARTESIAN_POINT ( 'NONE',  ( 101.2684584845351736, -45.32493232151070828, 152.0918157521019509 ) ) ;
#25548 = ORIENTED_EDGE ( 'NONE', *, *, #83576, .F. ) ;
#25549 = EDGE_LOOP ( 'NONE', ( #76585, #76503, #33187, #70342 ) ) ;
#25550 = AXIS2_PLACEMENT_3D ( 'NONE', #14300, #84247, #34728 ) ;
#25551 = CARTESIAN_POINT ( 'NONE',  ( 115.3364322588818851, -33.54570361940938739, 135.5501547344689754 ) ) ;
#25552 = EDGE_CURVE ( 'NONE', #8910, #61529, #35540, .T. ) ;
#25553 = CARTESIAN_POINT ( 'NONE',  ( 36.23715912545339535, -47.82818131006131779, 180.4678068554150911 ) ) ;
#25554 = AXIS2_PLACEMENT_3D ( 'NONE', #59185, #30609, #10600 ) ;
#25556 = DIRECTION ( 'NONE',  ( 0.7071067811865389130, -0.000000000000000000, 0.7071067811865561215 ) ) ;
#25555 = CARTESIAN_POINT ( 'NONE',  ( 116.8464009251321301, -35.91275531464980730, 249.8927681330532664 ) ) ;
#25557 = AXIS2_PLACEMENT_3D ( 'NONE', #5925, #46322, #81348 ) ;
#25558 = CARTESIAN_POINT ( 'NONE',  ( 19.56648329127400032, 0.2215528400590083269, 323.8756252759109202 ) ) ;
#25559 = CARTESIAN_POINT ( 'NONE',  ( 143.0667039024470455, -124.7784471599409102, 55.21780685541800437 ) ) ;
#25560 = CARTESIAN_POINT ( 'NONE',  ( 1.598849875094819542E-14, 101.5999999999999943, -130.5560000000000116 ) ) ;
#25561 = CARTESIAN_POINT ( 'NONE',  ( 180.3164832912740110, 12.92155284005802507, 336.5756252759111362 ) ) ;
#25562 = DIRECTION ( 'NONE',  ( 1.000000000000000000, 4.510281037539819615E-14, 0.000000000000000000 ) ) ;
#25563 = CARTESIAN_POINT ( 'NONE',  ( 144.5667039024470455, -123.2784471599409102, 55.21780685541800437 ) ) ;
#25564 = B_SPLINE_CURVE_WITH_KNOTS ( 'NONE', 3,
 ( #53727, #46918, #52813, #10629, #66033, #18791, #31513, #25151, #72862, #3823, #87839, #80586, #79702, #24714, #58768, #17455, #59220, #86950 ),
 .UNSPECIFIED., .F., .F.,
 ( 4, 2, 2, 2, 2, 2, 2, 2, 4 ),
 ( 0.5000310696403432731, 0.5625271859353003778, 0.6250233022302574826, 0.6875194185252144763, 0.7500155348201715810, 0.8125116511151286858, 0.8750077674100857905, 0.9375038837050428953, 1.000000000000000000 ),
 .UNSPECIFIED. ) ;
#25565 = B_SPLINE_SURFACE_WITH_KNOTS ( 'NONE', 3, 3, ( 
 ( #13262, #26439, #19181, #5560 ),
 ( #75037, #40950, #6441, #34135 ),
 ( #48646, #89569, #62291, #55456 ),
 ( #27328, #20531, #48199, #75932 ),
 ( #33252, #13704, #41391, #6885 ),
 ( #12824, #12363, #34587, #77 ),
 ( #27775, #83209, #76378, #14157 ) ),
 .UNSPECIFIED., .F., .F., .F.,
 ( 4, 1, 1, 1, 4 ),
 ( 4, 4 ),
 ( -0.0004313335404373049866, 0.2857142857142860315, 0.5714285714285709528, 0.8571428571428569843, 1.000431333540440004 ),
 ( 0.08686432420026919676, 1.000431333540440004 ),
 .UNSPECIFIED. ) ;
#25566 = CARTESIAN_POINT ( 'NONE',  ( 114.9485010938853975, -29.93956786141545834, 184.3927681330539770 ) ) ;
#25567 = CARTESIAN_POINT ( 'NONE',  ( 99.09567284741018511, -30.55045004867509562, 170.8014589425313829 ) ) ;
#25568 = ORIENTED_EDGE ( 'NONE', *, *, #22526, .F. ) ;
#25569 = ORIENTED_EDGE ( 'NONE', *, *, #24099, .F. ) ;
#25570 = LINE ( 'NONE', #82803, #89506 ) ;
#25571 = CARTESIAN_POINT ( 'NONE',  ( 82.50377070432760718, -20.00325133682503420, 7.150416387935383256 ) ) ;
#25572 = CARTESIAN_POINT ( 'NONE',  ( 97.06105352154311561, -37.99632076813814052, 186.4277894213790034 ) ) ;
#25573 = CARTESIAN_POINT ( 'NONE',  ( 160.5667039024426401, -48.82844715994099971, 300.4678068554149490 ) ) ;
#25574 = CIRCLE ( 'NONE', #63320, 7.873999999999991672 ) ;
#25575 = CARTESIAN_POINT ( 'NONE',  ( 105.7963341568336517, -26.72446301096675469, 95.17754999580937181 ) ) ;
#25576 = VERTEX_POINT ( 'NONE', #21943 ) ;
#25577 = CARTESIAN_POINT ( 'NONE',  ( -12.60000000000000142, 83.38334056604452371, 117.6834004267381601 ) ) ;
#25578 = CIRCLE ( 'NONE', #37199, 4.874999999999990230 ) ;
#25579 = CARTESIAN_POINT ( 'NONE',  ( 100.6562259211013384, -44.95110337444964443, 232.0499109901969632 ) ) ;
#25580 = CYLINDRICAL_SURFACE ( 'NONE', #82189, 7.937500000000000000 ) ;
#25581 = EDGE_LOOP ( 'NONE', ( #42632, #19291 ) ) ;
#25583 = EDGE_LOOP ( 'NONE', ( #22005, #81131, #64350, #3599 ) ) ;
#25582 = EDGE_CURVE ( 'NONE', #68811, #15841, #63713, .T. ) ;
#25584 = EDGE_CURVE ( 'NONE', #36668, #85068, #51393, .T. ) ;
#25585 = CARTESIAN_POINT ( 'NONE',  ( 103.5075036784956239, -46.12099098172097200, 63.28861473418663763 ) ) ;
#25586 = DIRECTION ( 'NONE',  ( 1.000000000000000000, 0.000000000000000000, 0.000000000000000000 ) ) ;
#25587 = EDGE_CURVE ( 'NONE', #42451, #31104, #56426, .T. ) ;
#25588 = CARTESIAN_POINT ( 'NONE',  ( 97.82528646310512954, -40.55050253551667083, 166.6384714708592867 ) ) ;
#25589 = CARTESIAN_POINT ( 'NONE',  ( 99.26659991834783625, -39.13601125124746716, 19.38237608387593980 ) ) ;
#25590 = CARTESIAN_POINT ( 'NONE',  ( 102.3833470591291785, -26.69184581432750747, 131.4118157521009778 ) ) ;
#25591 = FACE_OUTER_BOUND ( 'NONE', #37673, .T. ) ;
#25592 = ORIENTED_EDGE ( 'NONE', *, *, #88982, .F. ) ;
#25593 = EDGE_CURVE ( 'NONE', #44341, #72437, #43700, .T. ) ;
#25594 = DIRECTION ( 'NONE',  ( 1.000000000000000000, 0.000000000000000000, 2.108231265501709878E-16 ) ) ;
#25595 = CARTESIAN_POINT ( 'NONE',  ( 80.43833865491315294, -15.97944715994106524, 8.225625275910944723 ) ) ;
#25596 = EDGE_LOOP ( 'NONE', ( #66686, #73263, #31398, #55415 ) ) ;
#25597 = ORIENTED_EDGE ( 'NONE', *, *, #19629, .F. ) ;
#25598 = FACE_OUTER_BOUND ( 'NONE', #75762, .T. ) ;
#25599 = ORIENTED_EDGE ( 'NONE', *, *, #24771, .T. ) ;
#25600 = EDGE_LOOP ( 'NONE', ( #23490, #70330, #6515, #70436 ) ) ;
#25601 = LINE ( 'NONE', #31074, #63216 ) ;
#25602 = ADVANCED_FACE ( 'NONE', ( #77338, #8302 ), #8761, .T. ) ;
#25603 = CARTESIAN_POINT ( 'NONE',  ( 111.7785660440950011, -28.99582275371927764, 49.05146744712496343 ) ) ;
#25604 = CARTESIAN_POINT ( 'NONE',  ( 102.2269548454591046, -45.98824451103227062, 212.1927681330539599 ) ) ;
#25605 = CARTESIAN_POINT ( 'NONE',  ( 116.6407469026009238, -40.79910830432095281, 168.5070538473399608 ) ) ;
#25606 = EDGE_CURVE ( 'NONE', #34621, #87491, #41034, .T. ) ;
#25608 = CARTESIAN_POINT ( 'NONE',  ( 104.7405551043178633, -47.51155644559842273, 28.41943479971997988 ) ) ;
#25607 = CARTESIAN_POINT ( 'NONE',  ( 97.84500235132117041, -40.59787897505477616, 21.64223743672927469 ) ) ;
#25609 = LINE ( 'NONE', #75105, #3078 ) ;
#25610 = CARTESIAN_POINT ( 'NONE',  ( 223.2659999999999911, 52.73749999999999716, -33.78199999999999648 ) ) ;
#25611 = ORIENTED_EDGE ( 'NONE', *, *, #54699, .T. ) ;
#25612 = ORIENTED_EDGE ( 'NONE', *, *, #42431, .F. ) ;
#25613 = VECTOR ( 'NONE', #14438, 1000.000000000000114 ) ;
#25614 = AXIS2_PLACEMENT_3D ( 'NONE', #58197, #51362, #44547 ) ;
#25615 = DIRECTION ( 'NONE',  ( 0.000000000000000000, -1.000000000000000000, 0.000000000000000000 ) ) ;
#25617 = CARTESIAN_POINT ( 'NONE',  ( 113.2461215947159161, -45.18040784396236376, 228.0784824187679760 ) ) ;
#25616 = VECTOR ( 'NONE', #34677, 1000.000000000000114 ) ;
#25618 = VERTEX_POINT ( 'NONE', #70988 ) ;
#25619 = VECTOR ( 'NONE', #21341, 1000.000000000000000 ) ;
#25620 = CARTESIAN_POINT ( 'NONE',  ( 101.3490469528152715, -46.18936307759902604, 202.1318157521019430 ) ) ;
#25621 = CARTESIAN_POINT ( 'NONE',  ( 131.3164832912740110, -36.72944715994100306, -5.074374724089004474 ) ) ;
#25622 = TOROIDAL_SURFACE ( 'NONE', #25686, 6.647542495715439870, 3.174999999999999822 ) ;
#25623 = CARTESIAN_POINT ( 'NONE',  ( 141.0664832912740394, -46.72944715994099596, 14.92562527591100618 ) ) ;
#25624 = DIRECTION ( 'NONE',  ( 0.000000000000000000, 1.000000000000000000, 0.000000000000000000 ) ) ;
#25626 = CARTESIAN_POINT ( 'NONE',  ( 31.75000000000000000, 66.67499999999999716, 346.0750000000000455 ) ) ;
#25625 = CARTESIAN_POINT ( 'NONE',  ( 115.1362341769185917, -35.67412036042625800, 277.6356252759107974 ) ) ;
#25627 = DIRECTION ( 'NONE',  ( 1.000000000000000078E-15, -1.000000000000000083E-30, -1.000000000000000000 ) ) ;
#25628 = LINE ( 'NONE', #18362, #4746 ) ;
#25629 = CARTESIAN_POINT ( 'NONE',  ( 72.96458098368650269, 117.4749999999999943, 72.96458098368729850 ) ) ;
#25630 = CARTESIAN_POINT ( 'NONE',  ( 199.3900000000000148, 52.73749999999999716, -44.45000000000000284 ) ) ;
#25631 = CARTESIAN_POINT ( 'NONE',  ( 31.75000000000000000, 66.67499999999999716, 342.8999999999999773 ) ) ;
#25632 = FACE_OUTER_BOUND ( 'NONE', #22655, .T. ) ;
#25634 = EDGE_LOOP ( 'NONE', ( #77671, #46340, #86048, #3528 ) ) ;
#25633 = CARTESIAN_POINT ( 'NONE',  ( 101.1312616121724659, -28.98109996770097396, 195.5838068554168103 ) ) ;
#25635 = CARTESIAN_POINT ( 'NONE',  ( 71.24102794365336422, 4.106145706013555774, 542.9756252759101471 ) ) ;
#25636 = CARTESIAN_POINT ( 'NONE',  ( 110.1440020323170330, -26.08875547494869451, 214.8403871806729342 ) ) ;
#25637 = CARTESIAN_POINT ( 'NONE',  ( 114.7074080197622976, -44.71632701241580321, 109.1718157521009687 ) ) ;
#25638 = CARTESIAN_POINT ( 'NONE',  ( 115.2859307195537326, -30.18890446381676540, 240.3613395616249875 ) ) ;
#25639 = CARTESIAN_POINT ( 'NONE',  ( 162.5667039024481255, -33.35206098992175328, 313.9678068554149490 ) ) ;
#25640 = CARTESIAN_POINT ( 'NONE',  ( -7.301849239715819957E-13, 120.6499999999999915, 98.60478223830740774 ) ) ;
#25641 = AXIS2_PLACEMENT_3D ( 'NONE', #1489, #22833, #44584 ) ;
#25644 = ADVANCED_FACE ( 'NONE', ( #85962 ), #2834, .F. ) ;
#25643 = LINE ( 'NONE', #54661, #83475 ) ;
#25642 = PLANE ( 'NONE',  #66714 ) ;
#25645 = DIRECTION ( 'NONE',  ( -0.9963424814100680926, 0.08544974978095698503, 0.000000000000000000 ) ) ;
#25646 = CARTESIAN_POINT ( 'NONE',  ( 35.44148329127400388, 12.92155284005802685, 335.5992267699910485 ) ) ;
#25647 = CLOSED_SHELL ( 'NONE', ( #83457, #68665, #52093, #44530, #85605, #32245, #409, #8619, #29620, #87279, #59302, #8398, #79614, #42162, #56510, #40564, #46499, #31121, #7553, #79243, #54276, #77534, #31515, #46271, #39161, #50183, #44450, #22530, #54886, #42390, #43831, #87678, #11552, #86133, #44573, #21412, #85155, #72637, #86398, #82595, #11999, #48899, #52028, #73148, #65476, #50903, #57362, #48513, #88574, #47849, #28943, #53858, #79866, #19277, #45406, #36879, #78568, #42945, #3923, #4360, #32638, #68874, #52692, #63643, #31358, #17659, #2965, #59538, #39004, #49875, #11724, #26532, #6246, #88875, #38482, #24681, #22240, #7306, #23096, #9917, #58601, #55693, #54884, #45083, #4340, #81295, #11703, #38694, #21632, #78645, #28205, #19672, #40446, #66732, #59836, #8612, #81274, #73070, #14657, #89109, #5514, #32548, #53118, #86962, #32116, #64263, #5176, #76863, #40236, #49656, #8043, #4875, #78684, #81803, #80012, #57175, #63102, #73430, #69270, #41572, #20313, #30515, #76573, #12587, #61572, #44339, #67976, #36266, #21205, #49141, #12514, #75431, #75652, #75731, #57409, #56845, #8905, #16968, #19428, #14402, #73575, #16061 ) ) ;
#25648 = EDGE_CURVE ( 'NONE', #71480, #15206, #86160, .T. ) ;
#25649 = EDGE_LOOP ( 'NONE', ( #69163, #15952, #58158, #38879, #8570 ) ) ;
#25650 = ORIENTED_EDGE ( 'NONE', *, *, #47951, .T. ) ;
#25651 = CARTESIAN_POINT ( 'NONE',  ( 115.4001863486352022, -38.60401951598402803, 148.0724198280769883 ) ) ;
#25653 = ORIENTED_EDGE ( 'NONE', *, *, #82058, .F. ) ;
#25652 = CARTESIAN_POINT ( 'NONE',  ( -215.9000000000000057, 3.174999999999999822, -41.27499999999999858 ) ) ;
#25654 = CARTESIAN_POINT ( 'NONE',  ( 168.0371591254543091, -48.62818131005519717, 313.9678068554149490 ) ) ;
#25655 = CARTESIAN_POINT ( 'NONE',  ( 117.1882713363356174, -39.28166824301211335, 119.6299109901969615 ) ) ;
#25656 = FACE_OUTER_BOUND ( 'NONE', #20828, .T. ) ;
#25657 = CARTESIAN_POINT ( 'NONE',  ( -47.08008653354679041, 92.40823363359756115, 74.62285435386985455 ) ) ;
#25658 = CARTESIAN_POINT ( 'NONE',  ( 161.4809174648185888, -48.32844715993547169, 129.9678068554149775 ) ) ;
#25659 = CARTESIAN_POINT ( 'NONE',  ( 116.7951252719045101, -39.38782978815772395, 109.6147919427310171 ) ) ;
#25660 = CARTESIAN_POINT ( 'NONE',  ( 113.1080853710608238, -29.03773216254911915, 79.54705384733995288 ) ) ;
#25661 = VERTEX_POINT ( 'NONE', #4613 ) ;
#25662 = ORIENTED_EDGE ( 'NONE', *, *, #85909, .T. ) ;
#25664 = ORIENTED_EDGE ( 'NONE', *, *, #41255, .F. ) ;
#25663 = VECTOR ( 'NONE', #63973, 1000.000000000000000 ) ;
#25665 = EDGE_CURVE ( 'NONE', #55229, #37453, #87725, .T. ) ;
#25666 = CARTESIAN_POINT ( 'NONE',  ( 25.56670390244797275, -62.87844715994099687, 293.2178068554150627 ) ) ;
#25668 = DIRECTION ( 'NONE',  ( 0.000000000000000000, 0.000000000000000000, -1.000000000000000000 ) ) ;
#25667 = CARTESIAN_POINT ( 'NONE',  ( 114.0056865186721922, -29.02320718445401226, 155.5051490854339704 ) ) ;
#25669 = LINE ( 'NONE', #46090, #56653 ) ;
#25670 = DIRECTION ( 'NONE',  ( 1.000000000000000000, 4.299999999999999979E-14, 1.000000000000000078E-15 ) ) ;
#25671 = DIRECTION ( 'NONE',  ( -1.000000000000000000, 0.000000000000000000, 0.000000000000000000 ) ) ;
#25672 = DIRECTION ( 'NONE',  ( 0.000000000000000000, 0.000000000000000000, -1.000000000000000000 ) ) ;
#25673 = CARTESIAN_POINT ( 'NONE',  ( -72.96458098368600531, 127.0000000000000000, -65.02708098368781009 ) ) ;
#25674 = CARTESIAN_POINT ( 'NONE',  ( 117.3173117416417739, -32.65705981835808558, 99.13943479972098771 ) ) ;
#25675 = VERTEX_POINT ( 'NONE', #53620 ) ;
#25676 = ORIENTED_EDGE ( 'NONE', *, *, #78415, .T. ) ;
#25677 = EDGE_CURVE ( 'NONE', #27344, #47300, #59891, .T. ) ;
#25678 = CARTESIAN_POINT ( 'NONE',  ( 270.8910000000000196, 65.43750000000000000, -67.11950000000000216 ) ) ;
#25679 = AXIS2_PLACEMENT_3D ( 'NONE', #80292, #45718, #18038 ) ;
#25680 = CARTESIAN_POINT ( 'NONE',  ( 172.5664832912740110, -9.303447159940999356, 18.92562527591200094 ) ) ;
#25681 = VECTOR ( 'NONE', #22677, 1000.000000000000000 ) ;
#25682 = CARTESIAN_POINT ( 'NONE',  ( -487.2989999999999782, 6.038608028953049711, 90.48749999999999716 ) ) ;
#25683 = CARTESIAN_POINT ( 'NONE',  ( 97.86260780209082100, -37.94289672904660193, 149.2480903695909547 ) ) ;
#25684 = CIRCLE ( 'NONE', #21352, 0.5000000000000004441 ) ;
#25685 = VECTOR ( 'NONE', #20198, 1000.000000000000000 ) ;
#25686 = AXIS2_PLACEMENT_3D ( 'NONE', #31157, #84374, #43892 ) ;
#25687 = CYLINDRICAL_SURFACE ( 'NONE', #35870, 0.9999999999992039701 ) ;
#25688 = EDGE_LOOP ( 'NONE', ( #54259, #45049 ) ) ;
#25689 = VERTEX_POINT ( 'NONE', #17789 ) ;
#25690 = DIRECTION ( 'NONE',  ( -6.524622321627019585E-16, -3.741823817616790462E-31, -1.000000000000000000 ) ) ;
#25691 = ORIENTED_EDGE ( 'NONE', *, *, #20271, .T. ) ;
#25692 = PRODUCT_DEFINITION_SHAPE ( 'NONE', 'NONE',  #89944 ) ;
#25693 = ORIENTED_EDGE ( 'NONE', *, *, #11484, .T. ) ;
#25694 = CARTESIAN_POINT ( 'NONE',  ( 173.9900000000000091, 37.33800000000000097, 50.79999999999999716 ) ) ;
#25695 = EDGE_CURVE ( 'NONE', #45930, #6765, #80475, .T. ) ;
#25696 = CARTESIAN_POINT ( 'NONE',  ( 99.68253537205306714, -30.91964177047806217, 197.2396785439919711 ) ) ;
#25697 = PLANE ( 'NONE',  #63205 ) ;
#25698 = VECTOR ( 'NONE', #37534, 1000.000000000000000 ) ;
#25699 = CIRCLE ( 'NONE', #3918, 4.500000000000003553 ) ;
#25700 = CARTESIAN_POINT ( 'NONE',  ( 191.6377717143134873, -48.82844715994099971, 13.84673904354932006 ) ) ;
#25701 = B_SPLINE_CURVE_WITH_KNOTS ( 'NONE', 3,
 ( #11105, #18367, #5653, #81526, #32892, #61045, #68322, #38813, #26984, #46507, #46951, #54650, #52846, #74243, #11574, #81966, #39265, #80618, #73332, #88775, #4751, #12018, #75131, #53309, #87424 ),
 .UNSPECIFIED., .F., .F.,
 ( 4, 2, 2, 1, 2, 2, 2, 2, 2, 2, 2, 2, 4 ),
 ( 0.03973448063954118648, 0.04221847903031242938, 0.04346047822569805430, 0.04470247742108367228, 0.04594447661646929720, 0.04718647581185492212, 0.04967047420262618584, 0.05091247339801183852, 0.05215447259339749120, 0.05463847098416878961, 0.05588047017955442841, 0.05712246937494005333, 0.05960646776571127542 ),
 .UNSPECIFIED. ) ;
#25702 = CARTESIAN_POINT ( 'NONE',  ( 116.3212776292296127, -32.94146857471318413, 287.6356252759109680 ) ) ;
#25703 = ORIENTED_EDGE ( 'NONE', *, *, #17959, .T. ) ;
#25704 = VERTEX_POINT ( 'NONE', #65496 ) ;
#25705 = CIRCLE ( 'NONE', #79426, 7.500000000000007105 ) ;
#25706 = ORIENTED_EDGE ( 'NONE', *, *, #74207, .T. ) ;
#25707 = EDGE_LOOP ( 'NONE', ( #84139, #50917, #70251, #49414, #9606, #5915 ) ) ;
#25708 = ADVANCED_FACE ( 'NONE', ( #38671 ), #30972, .T. ) ;
#25709 = CARTESIAN_POINT ( 'NONE',  ( 115.2284764178246661, -36.04786338006340429, 251.7109475124485414 ) ) ;
#25710 = CARTESIAN_POINT ( 'NONE',  ( 97.24554646791794710, -31.60649478380229382, 90.93181575210196854 ) ) ;
#25711 = CARTESIAN_POINT ( 'NONE',  ( 107.3204973292724276, -25.70223992296332582, 75.04610146638695767 ) ) ;
#25712 = CARTESIAN_POINT ( 'NONE',  ( 100.2186905329472353, -40.88491400341852966, 249.5838068554171230 ) ) ;
#25713 = EDGE_CURVE ( 'NONE', #21182, #12019, #64274, .T. ) ;
#25714 = CARTESIAN_POINT ( 'NONE',  ( 184.5664832912740110, 25.62155284005901379, 328.6381252759109088 ) ) ;
#25715 = CARTESIAN_POINT ( 'NONE',  ( 106.5667039024470171, -94.77844715994206126, -19.78219314458232247 ) ) ;
#25716 = CARTESIAN_POINT ( 'NONE',  ( 110.6962928707952756, -48.01036458606073865, 203.8241967044819489 ) ) ;
#25717 = FACE_OUTER_BOUND ( 'NONE', #34500, .T. ) ;
#25718 = ORIENTED_EDGE ( 'NONE', *, *, #37362, .T. ) ;
#25719 = CARTESIAN_POINT ( 'NONE',  ( -67.92268098368600704, 117.4749999999999943, -72.96458098368781009 ) ) ;
#25720 = ORIENTED_EDGE ( 'NONE', *, *, #30410, .F. ) ;
#25721 = VERTEX_POINT ( 'NONE', #5057 ) ;
#25722 = PLANE ( 'NONE',  #75993 ) ;
#25723 = CARTESIAN_POINT ( 'NONE',  ( 0.000000000000000000, 152.3879256507328250, -9.425000000000000711 ) ) ;
#25724 = ORIENTED_EDGE ( 'NONE', *, *, #10017, .F. ) ;
#25725 = AXIS2_PLACEMENT_3D ( 'NONE', #87877, #58807, #80624 ) ;
#25726 = LINE ( 'NONE', #62033, #59148 ) ;
#25727 = CARTESIAN_POINT ( 'NONE',  ( 97.06114394585299010, -37.99679135525541795, 92.42732210906062562 ) ) ;
#25728 = CARTESIAN_POINT ( 'NONE',  ( 112.8018845221357367, -47.09986945403115044, 102.9784824187679817 ) ) ;
#25729 = CYLINDRICAL_SURFACE ( 'NONE', #40210, 0.5000000000000073275 ) ;
#25730 = DIRECTION ( 'NONE',  ( -1.000000000000000000, 0.000000000000000000, 0.000000000000000000 ) ) ;
#25731 = LINE ( 'NONE', #18464, #22342 ) ;
#25734 = CARTESIAN_POINT ( 'NONE',  ( 96.76471471792635271, -35.27954033865441374, 177.2156252759109805 ) ) ;
#25733 = CARTESIAN_POINT ( 'NONE',  ( 97.81269203708822602, -40.51987569166981018, 56.63541895716551267 ) ) ;
#25732 = LINE ( 'NONE', #82959, #8511 ) ;
#25735 = CARTESIAN_POINT ( 'NONE',  ( 41.56648329127499153, -36.32844715994070839, 138.9256252759119832 ) ) ;
#25736 = LINE ( 'NONE', #18925, #83023 ) ;
#25737 = ORIENTED_EDGE ( 'NONE', *, *, #65804, .T. ) ;
#25738 = CARTESIAN_POINT ( 'NONE',  ( 7.661254700127844153, 69.45253841614081125, 320.6630000000000109 ) ) ;
#25739 = DIRECTION ( 'NONE',  ( 0.000000000000000000, 1.000000000000000000, 0.000000000000000000 ) ) ;
#25740 = CARTESIAN_POINT ( 'NONE',  ( 102.0677916066047857, -27.97004931035759867, 135.4896765091952489 ) ) ;
#25741 = CARTESIAN_POINT ( 'NONE',  ( 0.000000000000000000, 82.54999999999999716, 206.3750000000000000 ) ) ;
#25743 = ORIENTED_EDGE ( 'NONE', *, *, #406, .F. ) ;
#25742 = CARTESIAN_POINT ( 'NONE',  ( 96.76538361991065074, -40.86468949728195099, 251.6422919425776001 ) ) ;
#25744 = DIRECTION ( 'NONE',  ( 0.000000000000000000, 0.000000000000000000, -1.000000000000000000 ) ) ;
#25745 = CARTESIAN_POINT ( 'NONE',  ( 115.6732227570775819, -30.74586734987101622, 275.3099109901965562 ) ) ;
#25746 = CARTESIAN_POINT ( 'NONE',  ( 117.0748215982922176, -30.29170057715430531, 140.2813395616249750 ) ) ;
#25747 = PLANE ( 'NONE',  #83880 ) ;
#25748 = CARTESIAN_POINT ( 'NONE',  ( 5.244075232672828157, 94.12423341047686165, -130.4512049017868094 ) ) ;
#25749 = CARTESIAN_POINT ( 'NONE',  ( 99.77245543246479542, 76.20343663217362007, -84.20430400022915762 ) ) ;
#25750 = DIRECTION ( 'NONE',  ( 3.100000000000000258E-29, -3.100000000000000044E-14, -1.000000000000000000 ) ) ;
#25751 = CARTESIAN_POINT ( 'NONE',  ( 6.174546696621020337E-16, 117.4749999999999943, -108.2293999999999983 ) ) ;
#25752 = ORIENTED_EDGE ( 'NONE', *, *, #47737, .T. ) ;
#25753 = AXIS2_PLACEMENT_3D ( 'NONE', #17725, #87215, #38163 ) ;
#25754 = AXIS2_PLACEMENT_3D ( 'NONE', #11594, #18387, #12485 ) ;
#25755 = ADVANCED_FACE ( 'NONE', ( #58659 ), #31405, .F. ) ;
#25756 = ORIENTED_EDGE ( 'NONE', *, *, #4192, .F. ) ;
#25757 = ORIENTED_EDGE ( 'NONE', *, *, #6429, .T. ) ;
#25758 = VERTEX_POINT ( 'NONE', #45914 ) ;
#25759 = CARTESIAN_POINT ( 'NONE',  ( 112.0659116130450030, -45.48839626610337916, 72.98979194171874951 ) ) ;
#25760 = CARTESIAN_POINT ( 'NONE',  ( 114.8031991714176741, -43.68443766454699073, 34.24419670448197905 ) ) ;
#25761 = CARTESIAN_POINT ( 'NONE',  ( 68.53801554307389665, 120.6499999999999915, 74.15067561874289481 ) ) ;
#25762 = CARTESIAN_POINT ( 'NONE',  ( 118.2946795739112957, -118.1912118068161703, -9.274842254010202680 ) ) ;
#25763 = CIRCLE ( 'NONE', #21436, 3.000000000000002665 ) ;
#25764 = VECTOR ( 'NONE', #52234, 1000.000000000000114 ) ;
#25766 = DIRECTION ( 'NONE',  ( 0.000000000000000000, 0.000000000000000000, 1.000000000000000000 ) ) ;
#25765 = LINE ( 'NONE', #67101, #84552 ) ;
#25767 = VECTOR ( 'NONE', #87072, 1000.000000000000000 ) ;
#25768 = CARTESIAN_POINT ( 'NONE',  ( 111.4808447759429413, -44.07556959346039349, 237.4295626852199632 ) ) ;
#25769 = ORIENTED_EDGE ( 'NONE', *, *, #34238, .F. ) ;
#25770 = EDGE_LOOP ( 'NONE', ( #11404, #48331 ) ) ;
#25771 = ORIENTED_EDGE ( 'NONE', *, *, #77057, .T. ) ;
#25772 = VECTOR ( 'NONE', #69127, 1000.000000000000000 ) ;
#25773 = EDGE_CURVE ( 'NONE', #5538, #28440, #25497, .T. ) ;
#25774 = DIRECTION ( 'NONE',  ( 0.000000000000000000, -1.000000000000000000, 0.000000000000000000 ) ) ;
#25775 = CARTESIAN_POINT ( 'NONE',  ( 117.0518796628545601, -35.94349769466420241, 183.8890245146588995 ) ) ;
#25776 = CARTESIAN_POINT ( 'NONE',  ( 97.81168895331838087, -40.51742574516882200, 287.6356252759109680 ) ) ;
#25777 = DIRECTION ( 'NONE',  ( 0.000000000000000000, 0.000000000000000000, -1.000000000000000000 ) ) ;
#25778 = EDGE_CURVE ( 'NONE', #57892, #11788, #35271, .T. ) ;
#25779 = CARTESIAN_POINT ( 'NONE',  ( 115.2782656938782821, -32.16401669718150202, 25.67396425827794815 ) ) ;
#25780 = CARTESIAN_POINT ( 'NONE',  ( 130.0664832912740110, -14.47844715994100007, 284.9256252759119548 ) ) ;
#25781 = EDGE_CURVE ( 'NONE', #62123, #22667, #59011, .T. ) ;
#25782 = CARTESIAN_POINT ( 'NONE',  ( 116.7892270726677140, -35.66563809581925426, 278.9127681330543851 ) ) ;
#25783 = LINE ( 'NONE', #53909, #39949 ) ;
#25784 = ADVANCED_FACE ( 'NONE', ( #25051 ), #20759, .T. ) ;
#25785 = ORIENTED_EDGE ( 'NONE', *, *, #58502, .F. ) ;
#25786 = ADVANCED_FACE ( 'NONE', ( #25954 ), #28011, .T. ) ;
#25787 = CARTESIAN_POINT ( 'NONE',  ( -29.99999999999998224, 171.0000000000000000, 114.8826257785461280 ) ) ;
#25788 = AXIS2_PLACEMENT_3D ( 'NONE', #49819, #21240, #35294 ) ;
#25789 = DIRECTION ( 'NONE',  ( 0.7071067811865453523, 0.7071067811865496822, 0.000000000000000000 ) ) ;
#25790 = CARTESIAN_POINT ( 'NONE',  ( 109.7208934110032743, -44.96686374295461519, 55.65475703625794068 ) ) ;
#25791 = VECTOR ( 'NONE', #26099, 1000.000000000000000 ) ;
#25792 = EDGE_CURVE ( 'NONE', #86125, #73517, #52272, .T. ) ;
#25793 = EDGE_CURVE ( 'NONE', #82312, #75243, #75893, .T. ) ;
#25794 = CARTESIAN_POINT ( 'NONE',  ( 134.4383386549280317, -15.97944715994100839, 8.225625275911001566 ) ) ;
#25795 = ADVANCED_FACE ( 'NONE', ( #27736 ), #74995, .T. ) ;
#25796 = DIRECTION ( 'NONE',  ( 0.000000000000000000, 0.000000000000000000, -1.000000000000000000 ) ) ;
#25797 = CARTESIAN_POINT ( 'NONE',  ( -4.084829003145262760, 94.58238198110524309, 118.4862812673465982 ) ) ;
#25798 = ORIENTED_EDGE ( 'NONE', *, *, #9209, .F. ) ;
#25799 = CARTESIAN_POINT ( 'NONE',  ( 83.56670390244801183, -39.24694715994102268, 219.5838068554169809 ) ) ;
#25800 = CARTESIAN_POINT ( 'NONE',  ( 50.79999999999999716, 73.02500000000000568, 257.1750000000000114 ) ) ;
#25801 = EDGE_CURVE ( 'NONE', #60102, #9112, #7724, .T. ) ;
#25802 = ORIENTED_EDGE ( 'NONE', *, *, #27128, .F. ) ;
#25803 = CARTESIAN_POINT ( 'NONE',  ( 117.3640430381357334, -38.35649778030718693, 113.7013395616249767 ) ) ;
#25804 = VERTEX_POINT ( 'NONE', #7304 ) ;
#25805 = CARTESIAN_POINT ( 'NONE',  ( 112.2681825743621431, -29.31628353742046755, 84.00003887569602057 ) ) ;
#25806 = EDGE_CURVE ( 'NONE', #62879, #34580, #20929, .T. ) ;
#25807 = CARTESIAN_POINT ( 'NONE',  ( 194.5664832912739826, 15.62155284005900491, 328.6381252759109088 ) ) ;
#25808 = CARTESIAN_POINT ( 'NONE',  ( 99.48689454471329441, -42.28159629070200509, 103.2492023535159831 ) ) ;
#25809 = DIRECTION ( 'NONE',  ( 4.299999999999999979E-14, -1.000000000000000000, 0.000000000000000000 ) ) ;
#25810 = VECTOR ( 'NONE', #39467, 1000.000000000000000 ) ;
#25811 = FACE_OUTER_BOUND ( 'NONE', #74228, .T. ) ;
#25812 = CARTESIAN_POINT ( 'NONE',  ( 108.9892323659770170, -46.99785963944585632, 78.72419670448194040 ) ) ;
#25813 = DIRECTION ( 'NONE',  ( -0.7071067811865779928, 0.7071067811865171526, -7.071067811865475333E-16 ) ) ;
#25814 = VERTEX_POINT ( 'NONE', #6846 ) ;
#25815 = LINE ( 'NONE', #11283, #67702 ) ;
#25816 = AXIS2_PLACEMENT_3D ( 'NONE', #52754, #39167, #67311 ) ;
#25817 = ORIENTED_EDGE ( 'NONE', *, *, #25449, .T. ) ;
#25818 = AXIS2_PLACEMENT_3D ( 'NONE', #65509, #17806, #52287 ) ;
#25819 = CARTESIAN_POINT ( 'NONE',  ( -118.4860207371918221, 70.52018178143200089, -4.092354625462838236 ) ) ;
#25820 = ORIENTED_EDGE ( 'NONE', *, *, #82033, .T. ) ;
#25821 = ORIENTED_EDGE ( 'NONE', *, *, #60881, .F. ) ;
#25822 = ADVANCED_FACE ( 'NONE', ( #68187 ), #40910, .T. ) ;
#25823 = AXIS2_PLACEMENT_3D ( 'NONE', #52686, #61319, #74514 ) ;
#25824 = CYLINDRICAL_SURFACE ( 'NONE', #44093, 4.762500000000002842 ) ;
#25825 = ORIENTED_EDGE ( 'NONE', *, *, #29698, .T. ) ;
#25826 = CARTESIAN_POINT ( 'NONE',  ( 116.3159835831962852, -41.41832011455028351, 248.4651490854349731 ) ) ;
#25827 = EDGE_CURVE ( 'NONE', #16260, #3733, #59952, .T. ) ;
#25828 = CARTESIAN_POINT ( 'NONE',  ( 97.44427603289686601, -39.46115625027057661, 126.5460739273663364 ) ) ;
#25829 = CARTESIAN_POINT ( 'NONE',  ( 100.8874677950680478, -44.70022130669426730, 188.0522919337000758 ) ) ;
#25830 = CARTESIAN_POINT ( 'NONE',  ( 96.71481148478426348, -38.23418088628295664, 62.44133956162495025 ) ) ;
#25832 = ADVANCED_FACE ( 'NONE', ( #55419 ), #7786, .T. ) ;
#25831 = DIRECTION ( 'NONE',  ( 0.000000000000000000, 1.000000000000000000, 0.000000000000000000 ) ) ;
#25833 = ORIENTED_EDGE ( 'NONE', *, *, #45548, .F. ) ;
#25834 = CARTESIAN_POINT ( 'NONE',  ( 165.3359832912748004, -36.32844715993531537, 300.4678068554149490 ) ) ;
#25835 = AXIS2_PLACEMENT_3D ( 'NONE', #18984, #46212, #74396 ) ;
#25836 = ADVANCED_FACE ( 'NONE', ( #19137 ), #41346, .F. ) ;
#25837 = AXIS2_PLACEMENT_3D ( 'NONE', #67283, #74111, #11892 ) ;
#25838 = DIRECTION ( 'NONE',  ( 0.000000000000000000, 0.000000000000000000, 1.000000000000000000 ) ) ;
#25839 = ORIENTED_EDGE ( 'NONE', *, *, #51796, .F. ) ;
#25840 = DIRECTION ( 'NONE',  ( -1.000000000000000000, -1.181088324069315053E-15, 0.000000000000000000 ) ) ;
#25841 = CARTESIAN_POINT ( 'NONE',  ( 72.26648329127297643, -1.929447159941394263, 352.4506252759079530 ) ) ;
#25842 = CARTESIAN_POINT ( 'NONE',  ( 117.4970320020027259, -36.54623693216564106, 288.8413395616252615 ) ) ;
#25843 = CARTESIAN_POINT ( 'NONE',  ( 51.06670390244799762, -33.35206098992630075, -5.074374724088000832 ) ) ;
#25844 = DIRECTION ( 'NONE',  ( -0.8660254037844392627, 0.4999999999999990008, -1.549999999999999706E-14 ) ) ;
#25845 = CARTESIAN_POINT ( 'NONE',  ( 121.3178890780284291, -95.01002112898673602, -19.18411693322930134 ) ) ;
#25846 = CARTESIAN_POINT ( 'NONE',  ( 111.4459538621439805, -44.65616828817710626, 252.3886103042673028 ) ) ;
#25848 = CARTESIAN_POINT ( 'NONE',  ( 100.3128846869253294, -46.43702735306945328, 83.09276813305294240 ) ) ;
#25847 = CARTESIAN_POINT ( 'NONE',  ( 107.0667039024470313, -119.4690460831833150, -11.78219314458153733 ) ) ;
#25849 = CARTESIAN_POINT ( 'NONE',  ( 69.72411017813010403, 120.6499999999999915, -69.72411017812979139 ) ) ;
#25850 = CARTESIAN_POINT ( 'NONE',  ( 117.8461808354131080, -34.08161713018977679, 164.0061014663869798 ) ) ;
#25851 = VERTEX_POINT ( 'NONE', #41792 ) ;
#25852 = LINE ( 'NONE', #26733, #3207 ) ;
#25853 = ORIENTED_EDGE ( 'NONE', *, *, #44785, .T. ) ;
#25854 = AXIS2_PLACEMENT_3D ( 'NONE', #16795, #927, #65815 ) ;
#25855 = CARTESIAN_POINT ( 'NONE',  ( -458.3598257906459708, 60.32499999999999574, 3.174999999999999822 ) ) ;
#25856 = FACE_OUTER_BOUND ( 'NONE', #33775, .T. ) ;
#25857 = CARTESIAN_POINT ( 'NONE',  ( 134.7196861477233654, -34.05633243510673935, 1.689562801603117892 ) ) ;
#25858 = ORIENTED_EDGE ( 'NONE', *, *, #22790, .F. ) ;
#25859 = LINE ( 'NONE', #10444, #36012 ) ;
#25861 = EDGE_LOOP ( 'NONE', ( #45234, #47434, #70563, #71310 ) ) ;
#25860 = CARTESIAN_POINT ( 'NONE',  ( 117.0653594338693892, -39.95035295773606521, 158.5784824187679476 ) ) ;
#25862 = DIRECTION ( 'NONE',  ( 0.000000000000000000, 1.000000000000000000, 0.000000000000000000 ) ) ;
#25863 = CARTESIAN_POINT ( 'NONE',  ( -130.3837601098274490, 93.33885111288434189, 6.713053715883731343 ) ) ;
#25864 = DIRECTION ( 'NONE',  ( 1.000000000000000000, 0.000000000000000000, -7.043400939473319300E-33 ) ) ;
#25865 = CIRCLE ( 'NONE', #18596, 3.499999999999996003 ) ;
#25866 = CARTESIAN_POINT ( 'NONE',  ( 32.09598329127702243, -23.42844715994121785, 313.9678068554150059 ) ) ;
#25867 = ORIENTED_EDGE ( 'NONE', *, *, #48383, .T. ) ;
#25868 = PRODUCT_CONTEXT ( 'NONE', #37076, 'mechanical' ) ;
#25869 = LINE ( 'NONE', #3635, #86376 ) ;
#25870 = CARTESIAN_POINT ( 'NONE',  ( 0.000000000000000000, 12.27000000000000313, 0.000000000000000000 ) ) ;
#25871 = EDGE_LOOP ( 'NONE', ( #84897, #56928, #6234, #2203 ) ) ;
#25872 = ORIENTED_EDGE ( 'NONE', *, *, #6962, .F. ) ;
#25873 = DIRECTION ( 'NONE',  ( -3.360405532702990443E-14, 1.000000000000000000, 0.000000000000000000 ) ) ;
#25874 = CARTESIAN_POINT ( 'NONE',  ( 95.16331303980187784, 94.60320878023495084, -89.38347482486616968 ) ) ;
#25875 = DIRECTION ( 'NONE',  ( -1.000000000000000078E-15, 1.000000000000000083E-30, 1.000000000000000000 ) ) ;
#25876 = LINE ( 'NONE', #3643, #16909 ) ;
#25877 = AXIS2_PLACEMENT_3D ( 'NONE', #22973, #36597, #42478 ) ;
#25879 = LINE ( 'NONE', #35814, #81996 ) ;
#25878 = CARTESIAN_POINT ( 'NONE',  ( 112.1390831963027637, -28.01267242204366781, 104.6564824957334423 ) ) ;
#25880 = CARTESIAN_POINT ( 'NONE',  ( 111.2668257968264527, -46.89591768004029149, 292.6356252759106837 ) ) ;
#25881 = AXIS2_PLACEMENT_3D ( 'NONE', #71032, #1082, #28794 ) ;
#25882 = ORIENTED_EDGE ( 'NONE', *, *, #47966, .T. ) ;
#25883 = VECTOR ( 'NONE', #47520, 1000.000000000000000 ) ;
#25884 = EDGE_CURVE ( 'NONE', #66001, #26221, #6397, .T. ) ;
#25885 = CARTESIAN_POINT ( 'NONE',  ( 123.6837132603319418, -50.82895651782485658, 229.5838068554170093 ) ) ;
#25886 = EDGE_CURVE ( 'NONE', #82398, #43244, #54069, .T. ) ;
#25887 = CARTESIAN_POINT ( 'NONE',  ( 99.57924082623978279, -30.38476633542330774, 211.7670538473389570 ) ) ;
#25889 = VERTEX_POINT ( 'NONE', #62702 ) ;
#25888 = CARTESIAN_POINT ( 'NONE',  ( 106.5646857698207981, -25.28130207810567498, 321.1698005525342978 ) ) ;
#25891 = EDGE_CURVE ( 'NONE', #59432, #628, #58540, .T. ) ;
#25890 = AXIS2_PLACEMENT_3D ( 'NONE', #14320, #672, #2030 ) ;
#25892 = CARTESIAN_POINT ( 'NONE',  ( 115.5638989210037124, -29.55965564860111527, 70.38419670448092802 ) ) ;
#25893 = DIRECTION ( 'NONE',  ( 9.351236661543306751E-17, -3.725950533538267725E-29, -1.000000000000000000 ) ) ;
#25894 = LINE ( 'NONE', #78440, #25367 ) ;
#25895 = CIRCLE ( 'NONE', #76672, 11.49999999999999645 ) ;
#25896 = DIRECTION ( 'NONE',  ( -5.551115123125777653E-14, -1.000000000000000000, 0.000000000000000000 ) ) ;
#25897 = EDGE_CURVE ( 'NONE', #35135, #34504, #14115, .T. ) ;
#25898 = ORIENTED_EDGE ( 'NONE', *, *, #55622, .T. ) ;
#25899 = DIRECTION ( 'NONE',  ( -0.000000000000000000, -1.000000000000000000, -0.000000000000000000 ) ) ;
#25900 = EDGE_CURVE ( 'NONE', #64418, #3248, #34547, .T. ) ;
#25901 = AXIS2_PLACEMENT_3D ( 'NONE', #33560, #83509, #67637 ) ;
#25902 = ORIENTED_EDGE ( 'NONE', *, *, #29712, .F. ) ;
#25903 = EDGE_LOOP ( 'NONE', ( #12480, #84561 ) ) ;
#25904 = CARTESIAN_POINT ( 'NONE',  ( 101.6974430329241272, -44.43982537643711339, 233.5120594963729559 ) ) ;
#25905 = EDGE_CURVE ( 'NONE', #27387, #4960, #32400, .T. ) ;
#25906 = FACE_OUTER_BOUND ( 'NONE', #14547, .T. ) ;
#25907 = CARTESIAN_POINT ( 'NONE',  ( -118.0074504647927398, 88.17653575778737718, -11.39323553397000666 ) ) ;
#25908 = EDGE_CURVE ( 'NONE', #35863, #88126, #62252, .T. ) ;
#25909 = DIRECTION ( 'NONE',  ( 1.000000000000000078E-15, 0.000000000000000000, 1.000000000000000000 ) ) ;
#25910 = VECTOR ( 'NONE', #53047, 1000.000000000000000 ) ;
#25911 = FACE_OUTER_BOUND ( 'NONE', #66121, .T. ) ;
#25912 = ORIENTED_EDGE ( 'NONE', *, *, #61778, .F. ) ;
#25913 = LINE ( 'NONE', #87690, #66762 ) ;
#25914 = PLANE ( 'NONE',  #25233 ) ;
#25915 = ORIENTED_EDGE ( 'NONE', *, *, #71963, .T. ) ;
#25916 = CARTESIAN_POINT ( 'NONE',  ( 96.58568816239599641, -40.17018292043295702, 286.5908633711491120 ) ) ;
#25917 = ORIENTED_EDGE ( 'NONE', *, *, #20404, .T. ) ;
#25918 = ORIENTED_EDGE ( 'NONE', *, *, #32811, .F. ) ;
#25919 = CARTESIAN_POINT ( 'NONE',  ( 105.3241794147103008, -28.72650611001668608, 258.0652332267344491 ) ) ;
#25920 = EDGE_CURVE ( 'NONE', #21569, #48100, #481, .T. ) ;
#25921 = CARTESIAN_POINT ( 'NONE',  ( 113.6473777113568531, -44.00994186338857617, 133.1613395616259936 ) ) ;
#25922 = DIRECTION ( 'NONE',  ( 0.000000000000000000, 0.000000000000000000, 1.000000000000000000 ) ) ;
#25923 = CARTESIAN_POINT ( 'NONE',  ( 92.91125933621934507, -113.6057974291317691, -21.78219314458173983 ) ) ;
#25924 = CYLINDRICAL_SURFACE ( 'NONE', #44743, 2.030000000001869864 ) ;
#25926 = EDGE_CURVE ( 'NONE', #78352, #16601, #88640, .T. ) ;
#25925 = CIRCLE ( 'NONE', #73766, 2.500000000000002220 ) ;
#25927 = CARTESIAN_POINT ( 'NONE',  ( 95.35923950155199691, -38.86288465644625489, 197.4699109901969791 ) ) ;
#25928 = DIRECTION ( 'NONE',  ( 0.000000000000000000, 0.000000000000000000, -1.000000000000000000 ) ) ;
#25929 = ORIENTED_EDGE ( 'NONE', *, *, #83933, .F. ) ;
#25930 = CARTESIAN_POINT ( 'NONE',  ( 118.8919219083537797, -35.39899076563189340, 79.91562527591095488 ) ) ;
#25931 = CARTESIAN_POINT ( 'NONE',  ( 128.5967921371759815, -18.82844715994100682, 342.9256252759109884 ) ) ;
#25932 = VERTEX_POINT ( 'NONE', #19576 ) ;
#25933 = EDGE_LOOP ( 'NONE', ( #82683, #68929, #82920, #36848 ) ) ;
#25934 = EDGE_LOOP ( 'NONE', ( #47419, #24680, #15054, #36044 ) ) ;
#25935 = CARTESIAN_POINT ( 'NONE',  ( 77.31648329127401098, -36.72944715994107412, 3.101481641215480867 ) ) ;
#25936 = DIRECTION ( 'NONE',  ( 1.000000000000000078E-15, -1.000000000000000083E-30, -1.000000000000000000 ) ) ;
#25937 = CARTESIAN_POINT ( 'NONE',  ( 41.56648329127399677, -9.303447159940999356, 258.9256252759120116 ) ) ;
#25938 = CARTESIAN_POINT ( 'NONE',  ( 114.9723337227840005, -34.69788249897437993, 121.8452332267339671 ) ) ;
#25939 = CARTESIAN_POINT ( 'NONE',  ( 100.8102337077607871, -45.86971777371983450, 238.1108633711489517 ) ) ;
#25941 = EDGE_CURVE ( 'NONE', #14995, #30543, #15472, .T. ) ;
#25940 = DIRECTION ( 'NONE',  ( 0.000000000000000000, 0.000000000000000000, -1.000000000000000000 ) ) ;
#25942 = ORIENTED_EDGE ( 'NONE', *, *, #36522, .T. ) ;
#25943 = CARTESIAN_POINT ( 'NONE',  ( 130.4355093393840832, 93.94653598907720493, -5.619751006018297801 ) ) ;
#25944 = CIRCLE ( 'NONE', #75289, 16.00000000000000000 ) ;
#25945 = EDGE_CURVE ( 'NONE', #1529, #58575, #8200, .T. ) ;
#25946 = CYLINDRICAL_SURFACE ( 'NONE', #6982, 2.116999999999980009 ) ;
#25947 = ORIENTED_EDGE ( 'NONE', *, *, #40374, .T. ) ;
#25948 = ORIENTED_EDGE ( 'NONE', *, *, #62994, .T. ) ;
#25949 = AXIS2_PLACEMENT_3D ( 'NONE', #40052, #75491, #53661 ) ;
#25950 = AXIS2_PLACEMENT_3D ( 'NONE', #17326, #37320, #43220 ) ;
#25951 = CARTESIAN_POINT ( 'NONE',  ( -254.0000000000000000, 3.174999999999999822, -41.27499999999999858 ) ) ;
#25952 = ORIENTED_EDGE ( 'NONE', *, *, #46278, .F. ) ;
#25953 = ORIENTED_EDGE ( 'NONE', *, *, #53674, .T. ) ;
#25954 = FACE_OUTER_BOUND ( 'NONE', #61290, .T. ) ;
#25955 = DIRECTION ( 'NONE',  ( 0.000000000000000000, 0.000000000000000000, -1.000000000000000000 ) ) ;
#25956 = FACE_OUTER_BOUND ( 'NONE', #57361, .T. ) ;
#25957 = CARTESIAN_POINT ( 'NONE',  ( 107.7643578131546178, -45.27140672887451700, 177.0638483995059858 ) ) ;
#25958 = CARTESIAN_POINT ( 'NONE',  ( 99.03195499373370581, -44.38837911315224716, 36.92038718067297509 ) ) ;
#25959 = CARTESIAN_POINT ( 'NONE',  ( 68.54895288615315962, -132.5647336068149684, 247.4783998280180128 ) ) ;
#25960 = EDGE_LOOP ( 'NONE', ( #58948, #24745, #34211, #85868 ) ) ;
#25961 = AXIS2_PLACEMENT_3D ( 'NONE', #20127, #122, #53259 ) ;
#25962 = DIRECTION ( 'NONE',  ( -1.000000000000000078E-15, 0.000000000000000000, -1.000000000000000000 ) ) ;
#25963 = ORIENTED_EDGE ( 'NONE', *, *, #40976, .F. ) ;
#25964 = VECTOR ( 'NONE', #24670, 1000.000000000000000 ) ;
#25965 = CARTESIAN_POINT ( 'NONE',  ( 142.8821648370248170, -72.54478064608022692, 394.9756252759102040 ) ) ;
#25966 = ORIENTED_EDGE ( 'NONE', *, *, #28378, .T. ) ;
#25967 = CARTESIAN_POINT ( 'NONE',  ( 103.1366983212326573, -27.50878891356330769, 166.3966305085834847 ) ) ;
#25968 = CARTESIAN_POINT ( 'NONE',  ( -10.70251298044785493, 75.88783213464688515, 118.0721548101077474 ) ) ;
#25969 = CARTESIAN_POINT ( 'NONE',  ( 99.50471754548186709, -43.30576767929590432, 131.8960681784909070 ) ) ;
#25970 = EDGE_CURVE ( 'NONE', #49424, #71630, #44012, .T. ) ;
#25971 = CARTESIAN_POINT ( 'NONE',  ( 51.56670390244683944, -33.35206098992668444, 117.4678068554150485 ) ) ;
#25972 = ORIENTED_EDGE ( 'NONE', *, *, #19121, .F. ) ;
#25973 = CARTESIAN_POINT ( 'NONE',  ( 100.5838780899822922, -28.49162262467549667, 15.60705384733995871 ) ) ;
#25974 = CARTESIAN_POINT ( 'NONE',  ( 101.0411209824609813, -27.40783209567417700, 66.54514908543495721 ) ) ;
#25976 = DIRECTION ( 'NONE',  ( -1.000000000000000000, 0.000000000000000000, 0.000000000000000000 ) ) ;
#25975 = DIRECTION ( 'NONE',  ( 0.000000000000000000, 1.000000000000000000, 0.000000000000000000 ) ) ;
#25977 = DIRECTION ( 'NONE',  ( 0.000000000000000000, 0.000000000000000000, -1.000000000000000000 ) ) ;
#25978 = CARTESIAN_POINT ( 'NONE',  ( 132.7628207310659150, -39.15113447712369776, 7.957506268078478939 ) ) ;
#25979 = AXIS2_PLACEMENT_3D ( 'NONE', #40803, #19926, #7638 ) ;
#25980 = CARTESIAN_POINT ( 'NONE',  ( 102.3363410760962608, -27.82220188792448567, 121.4623623916829587 ) ) ;
#25981 = CARTESIAN_POINT ( 'NONE',  ( 146.6607710079033779, -137.6835511433035037, 246.9874215757600098 ) ) ;
#25982 = ORIENTED_EDGE ( 'NONE', *, *, #24337, .T. ) ;
#25983 = CARTESIAN_POINT ( 'NONE',  ( 115.7653496281367325, -43.62456195820889349, 48.30514908543492680 ) ) ;
#25984 = CARTESIAN_POINT ( 'NONE',  ( 112.2050260072902290, -45.80016191694880234, 208.9870538473389558 ) ) ;
#25985 = CARTESIAN_POINT ( 'NONE',  ( 101.7448744985357223, -27.01524695604527082, 96.46324432352997746 ) ) ;
#25987 = FACE_OUTER_BOUND ( 'NONE', #82737, .T. ) ;
#25986 = CARTESIAN_POINT ( 'NONE',  ( 115.0386160834107017, -42.90673886385352631, 173.2986915154965004 ) ) ;
#25988 = CARTESIAN_POINT ( 'NONE',  ( 191.6377717143134873, -67.87844715994100397, 307.9888746672805269 ) ) ;
#25990 = EDGE_CURVE ( 'NONE', #2492, #14095, #2729, .T. ) ;
#25989 = CIRCLE ( 'NONE', #43417, 3.250000000000002665 ) ;
#25991 = EDGE_CURVE ( 'NONE', #65338, #72917, #23197, .T. ) ;
#25992 = DIRECTION ( 'NONE',  ( -1.000000000000000000, 0.000000000000000000, 0.000000000000000000 ) ) ;
#25993 = ORIENTED_EDGE ( 'NONE', *, *, #25884, .F. ) ;
#25994 = ADVANCED_FACE ( 'NONE', ( #29987 ), #16354, .F. ) ;
#25995 = CARTESIAN_POINT ( 'NONE',  ( 112.9285164932675514, -28.85859325239454165, 100.5670538473389684 ) ) ;
#25997 = EDGE_LOOP ( 'NONE', ( #42336, #14586, #72056, #19319 ) ) ;
#25996 = LINE ( 'NONE', #19184, #63122 ) ;
#25998 = EDGE_CURVE ( 'NONE', #84598, #35448, #70427, .T. ) ;
#25999 = CARTESIAN_POINT ( 'NONE',  ( 116.9047011640239759, -41.71676023082950735, 244.4651490854349731 ) ) ;
#26000 = CARTESIAN_POINT ( 'NONE',  ( 115.7827659893201968, -41.80290719135400934, 254.4082417524339235 ) ) ;
#26001 = CARTESIAN_POINT ( 'NONE',  ( 90.44969454456408187, -53.34645651782490461, 239.5838068554174356 ) ) ;
#26002 = DIRECTION ( 'NONE',  ( 0.000000000000000000, 1.000000000000000000, 0.000000000000000000 ) ) ;
#26003 = CARTESIAN_POINT ( 'NONE',  ( 97.33784131839850318, -34.07106450384809193, 82.11479194044655117 ) ) ;
#26004 = AXIS2_PLACEMENT_3D ( 'NONE', #22100, #48861, #8001 ) ;
#26005 = CARTESIAN_POINT ( 'NONE',  ( 131.3165190107490048, -36.90078909148135011, 3.101427792080953871 ) ) ;
#26006 = ADVANCED_FACE ( 'NONE', ( #83613 ), #14573, .F. ) ;
#26007 = CYLINDRICAL_SURFACE ( 'NONE', #19594, 130.5560000000000116 ) ;
#26008 = CARTESIAN_POINT ( 'NONE',  ( 97.38117110781242047, -35.36630255995240191, 181.2156252759109805 ) ) ;
#26009 = EDGE_LOOP ( 'NONE', ( #42873, #64008, #23111, #70368 ) ) ;
#26010 = ORIENTED_EDGE ( 'NONE', *, *, #13286, .F. ) ;
#26011 = CIRCLE ( 'NONE', #4223, 12.99999999999999822 ) ;
#26012 = CARTESIAN_POINT ( 'NONE',  ( 108.6971488411468414, -45.98241724535997577, 119.1349166392299566 ) ) ;
#26013 = TOROIDAL_SURFACE ( 'NONE', #88396, 15.69999999999999929, 0.2999999999999999889 ) ;
#26014 = ADVANCED_FACE ( 'NONE', ( #7744 ), #85420, .T. ) ;
#26015 = CARTESIAN_POINT ( 'NONE',  ( 33.92127028473601769, -29.73316016639540749, 313.9678068554150059 ) ) ;
#26017 = LINE ( 'NONE', #20102, #46222 ) ;
#26016 = CARTESIAN_POINT ( 'NONE',  ( 98.19951187208815213, -40.85743130997446571, 252.6727681330533812 ) ) ;
#26018 = CARTESIAN_POINT ( 'NONE',  ( -254.0000000000000000, 104.7749999999999915, -41.27499999999999858 ) ) ;
#26019 = ADVANCED_FACE ( 'NONE', ( #49054 ), #15913, .T. ) ;
#26020 = FACE_OUTER_BOUND ( 'NONE', #86363, .T. ) ;
#26021 = VECTOR ( 'NONE', #27270, 1000.000000000000000 ) ;
#26022 = DIRECTION ( 'NONE',  ( -1.000000000000000000, 0.000000000000000000, 0.000000000000000000 ) ) ;
#26023 = CARTESIAN_POINT ( 'NONE',  ( 144.5667039024470171, -90.27844715994091018, 45.21780685541799727 ) ) ;
#26024 = DIRECTION ( 'NONE',  ( -1.000000000000000000, 0.000000000000000000, -0.000000000000000000 ) ) ;
#26026 = CARTESIAN_POINT ( 'NONE',  ( 116.3308458273176456, -44.07926308385601999, 198.2927681330539542 ) ) ;
#26025 = STYLED_ITEM ( 'NONE', ( #5992 ), #44568 ) ;
#26027 = CARTESIAN_POINT ( 'NONE',  ( 116.3212776292296127, -32.94146857471318413, 287.6356252759109680 ) ) ;
#26028 = EDGE_LOOP ( 'NONE', ( #12817, #52497, #9302, #52263 ) ) ;
#26029 = ORIENTED_EDGE ( 'NONE', *, *, #88719, .F. ) ;
#26030 = DIRECTION ( 'NONE',  ( 0.000000000000000000, -1.000000000000000000, 0.000000000000000000 ) ) ;
#26031 = CARTESIAN_POINT ( 'NONE',  ( 78.82300719539804845, -16.27587548316634525, 1.868342134758776307 ) ) ;
#26032 = AXIS2_PLACEMENT_3D ( 'NONE', #1641, #28427, #29342 ) ;
#26033 = PLANE ( 'NONE',  #51891 ) ;
#26034 = LINE ( 'NONE', #60527, #62751 ) ;
#26035 = CARTESIAN_POINT ( 'NONE',  ( 67.06681736700808472, -67.87844715931913697, 245.5130139978070076 ) ) ;
#26036 = ORIENTED_EDGE ( 'NONE', *, *, #9182, .F. ) ;
#26037 = CARTESIAN_POINT ( 'NONE',  ( 113.1764815558486390, -44.75322278302650147, 63.09378032628466570 ) ) ;
#26038 = CARTESIAN_POINT ( 'NONE',  ( 107.2492389712779612, -24.88009754917498739, 230.0641967044819580 ) ) ;
#26039 = DIRECTION ( 'NONE',  ( -0.9254794337955620787, -0.3787978585227822492, 0.000000000000000000 ) ) ;
#26040 = ORIENTED_EDGE ( 'NONE', *, *, #20432, .F. ) ;
#26041 = VECTOR ( 'NONE', #65718, 1000.000000000000000 ) ;
#26042 = CARTESIAN_POINT ( 'NONE',  ( -5.590575964937773534, 93.87199967727632099, 118.4265748443029338 ) ) ;
#26043 = CARTESIAN_POINT ( 'NONE',  ( 184.5667039024480118, -67.87844715994100397, 300.9178068554150514 ) ) ;
#26044 = CARTESIAN_POINT ( 'NONE',  ( 113.1774532810855760, -44.75249673545214080, 164.0938759193286955 ) ) ;
#26045 = CARTESIAN_POINT ( 'NONE',  ( 98.96120113019971143, -37.69594967233602034, 39.23951894101995919 ) ) ;
#26046 = CARTESIAN_POINT ( 'NONE',  ( 103.4608836344597194, -46.53438966646587005, 138.2956252759109645 ) ) ;
#26047 = DIRECTION ( 'NONE',  ( 1.000000000000000078E-15, -1.000000000000000000, 0.000000000000000000 ) ) ;
#26048 = VERTEX_POINT ( 'NONE', #1387 ) ;
#26049 = ADVANCED_FACE ( 'NONE', ( #69977 ), #77428, .T. ) ;
#26050 = FACE_OUTER_BOUND ( 'NONE', #48493, .T. ) ;
#26051 = AXIS2_PLACEMENT_3D ( 'NONE', #85031, #86361, #50477 ) ;
#26052 = LINE ( 'NONE', #46911, #44475 ) ;
#26053 = ORIENTED_EDGE ( 'NONE', *, *, #68578, .T. ) ;
#26054 = ORIENTED_EDGE ( 'NONE', *, *, #4031, .F. ) ;
#26055 = APPLICATION_CONTEXT ( 'automotive_design' ) ;
#26056 = DIRECTION ( 'NONE',  ( -0.000000000000000000, 1.000000000000000000, -0.000000000000000000 ) ) ;
#26057 = ORIENTED_EDGE ( 'NONE', *, *, #39314, .F. ) ;
#26058 = ORIENTED_EDGE ( 'NONE', *, *, #44285, .F. ) ;
#26059 = DIRECTION ( 'NONE',  ( -0.000000000000000000, -0.000000000000000000, 1.000000000000000000 ) ) ;
#26060 = CARTESIAN_POINT ( 'NONE',  ( 100.2301541646454552, -41.85006585248910937, 66.26099125664796929 ) ) ;
#26061 = CARTESIAN_POINT ( 'NONE',  ( 99.27200920372420967, -29.77297264586844960, 190.7470538473399415 ) ) ;
#26062 = CIRCLE ( 'NONE', #8704, 3.499999999999996003 ) ;
#26063 = CARTESIAN_POINT ( 'NONE',  ( 101.7806060443208480, -45.68981339355064364, 162.1527681330539679 ) ) ;
#26065 = CARTESIAN_POINT ( 'NONE',  ( 104.5881800117806932, -26.60309611811081254, 281.2670538473395823 ) ) ;
#26064 = CARTESIAN_POINT ( 'NONE',  ( 110.1478212817822424, -46.33253055760241068, 22.82345756811338333 ) ) ;
#26066 = DIRECTION ( 'NONE',  ( 1.000000000000000078E-15, -1.000000000000000000, 0.000000000000000000 ) ) ;
#26067 = DIRECTION ( 'NONE',  ( 0.7071067811873671394, 0.7071067811857280061, -2.899137802861369224E-29 ) ) ;
#26068 = ORIENTED_EDGE ( 'NONE', *, *, #66512, .T. ) ;
#26069 = CIRCLE ( 'NONE', #37686, 2.999999999999947153 ) ;
#26070 = ORIENTED_EDGE ( 'NONE', *, *, #22203, .T. ) ;
#26071 = AXIS2_PLACEMENT_3D ( 'NONE', #4705, #80570, #12411 ) ;
#26072 = EDGE_CURVE ( 'NONE', #28588, #45463, #51269, .T. ) ;
#26073 = DIRECTION ( 'NONE',  ( 0.000000000000000000, -1.000000000000000000, 0.000000000000000000 ) ) ;
#26074 = CARTESIAN_POINT ( 'NONE',  ( 118.0975507117283883, -35.49314816969329200, 233.9032443235299752 ) ) ;
#26075 = ORIENTED_EDGE ( 'NONE', *, *, #61535, .F. ) ;
#26076 = CARTESIAN_POINT ( 'NONE',  ( 114.9651742339629976, -29.92520496456729262, 184.3927681330539770 ) ) ;
#26077 = DIRECTION ( 'NONE',  ( 0.000000000000000000, 0.000000000000000000, 1.000000000000000000 ) ) ;
#26078 = CARTESIAN_POINT ( 'NONE',  ( -21.00265438680891705, 62.01110210563430769, 31.78899330339352858 ) ) ;
#26079 = DIRECTION ( 'NONE',  ( 0.000000000000000000, 0.000000000000000000, 1.000000000000000000 ) ) ;
#26080 = CARTESIAN_POINT ( 'NONE',  ( 116.8785659245552466, -39.03624075203685351, 29.64421603613703482 ) ) ;
#26082 = FACE_OUTER_BOUND ( 'NONE', #14431, .T. ) ;
#26081 = CARTESIAN_POINT ( 'NONE',  ( 98.33459205555250549, -35.67394987134639450, 277.6356252759110816 ) ) ;
#26083 = DIRECTION ( 'NONE',  ( 1.000000000000000000, 0.000000000000000000, -4.277118011829300531E-15 ) ) ;
#26084 = DIRECTION ( 'NONE',  ( -0.9254794337955621897, -0.3787978585227819717, 0.000000000000000000 ) ) ;
#26085 = CARTESIAN_POINT ( 'NONE',  ( 160.2664750769289697, 101.5999999999999943, 148.0533267522752112 ) ) ;
#26086 = VECTOR ( 'NONE', #36561, 1000.000000000000000 ) ;
#26087 = CARTESIAN_POINT ( 'NONE',  ( 80.06648329127399677, -9.029447159941060619, 1.625625275910943746 ) ) ;
#26088 = AXIS2_PLACEMENT_3D ( 'NONE', #26314, #87652, #12698 ) ;
#26089 = CARTESIAN_POINT ( 'NONE',  ( 183.5150000000000148, 37.33800000000000097, 60.32499999999999574 ) ) ;
#26090 = PLANE ( 'NONE',  #7169 ) ;
#26092 = ORIENTED_EDGE ( 'NONE', *, *, #53450, .T. ) ;
#26091 = DIRECTION ( 'NONE',  ( 0.000000000000000000, 0.000000000000000000, 1.000000000000000000 ) ) ;
#26093 = DIRECTION ( 'NONE',  ( 0.000000000000000000, 0.000000000000000000, -1.000000000000000000 ) ) ;
#26094 = CARTESIAN_POINT ( 'NONE',  ( 103.6313148537710305, -26.19877486694289459, 210.3394347997209763 ) ) ;
#26095 = CARTESIAN_POINT ( 'NONE',  ( 117.8564148307409596, -39.12764603782969886, 99.64038718067195077 ) ) ;
#26096 = CARTESIAN_POINT ( 'NONE',  ( 100.2187443247741783, -45.46477599873944797, 273.0594347997206910 ) ) ;
#26097 = CARTESIAN_POINT ( 'NONE',  ( 83.56670390244801183, -36.72944715994108122, 219.5838068554169809 ) ) ;
#26098 = AXIS2_PLACEMENT_3D ( 'NONE', #6173, #33861, #83827 ) ;
#26099 = DIRECTION ( 'NONE',  ( 0.000000000000000000, 0.000000000000000000, 1.000000000000000000 ) ) ;
#26101 = DIRECTION ( 'NONE',  ( 0.000000000000000000, 1.000000000000000000, 0.000000000000000000 ) ) ;
#26100 = DIRECTION ( 'NONE',  ( 0.000000000000000000, 0.000000000000000000, 1.000000000000000000 ) ) ;
#26102 = FACE_OUTER_BOUND ( 'NONE', #44851, .T. ) ;
#26103 = CARTESIAN_POINT ( 'NONE',  ( 133.3217830637437658, -21.37853523628597330, 1.709393643970599674 ) ) ;
#26104 = ORIENTED_EDGE ( 'NONE', *, *, #29872, .T. ) ;
#26105 = VERTEX_POINT ( 'NONE', #63152 ) ;
#26106 = EDGE_CURVE ( 'NONE', #59488, #48723, #56775, .T. ) ;
#26107 = CONICAL_SURFACE ( 'NONE', #18843, 7.000000000000006217, 0.7853981633974699283 ) ;
#26108 = CARTESIAN_POINT ( 'NONE',  ( 115.7032693465968975, -34.00573701374007385, 128.4800388756959819 ) ) ;
#26110 = ORIENTED_EDGE ( 'NONE', *, *, #72891, .F. ) ;
#26109 = CARTESIAN_POINT ( 'NONE',  ( 22.68560957326527472, 49.60990628430907634, 30.61209429277630534 ) ) ;
#26111 = LINE ( 'NONE', #54223, #88076 ) ;
#26112 = EDGE_CURVE ( 'NONE', #77555, #43158, #22280, .T. ) ;
#26113 = CARTESIAN_POINT ( 'NONE',  ( 102.7067583520261138, -46.86140753836539119, 133.2651490854349561 ) ) ;
#26114 = CYLINDRICAL_SURFACE ( 'NONE', #86032, 2.030000000001807248 ) ;
#26115 = ADVANCED_FACE ( 'NONE', ( #21836, #36797 ), #35893, .F. ) ;
#26116 = CARTESIAN_POINT ( 'NONE',  ( -47.09267117624717969, 92.49156081278650277, 74.71343019242331707 ) ) ;
#26117 = LINE ( 'NONE', #74269, #14268 ) ;
#26118 = EDGE_CURVE ( 'NONE', #66670, #84435, #49507, .T. ) ;
#26119 = DIRECTION ( 'NONE',  ( 0.000000000000000000, 0.000000000000000000, -1.000000000000000000 ) ) ;
#26120 = CARTESIAN_POINT ( 'NONE',  ( 106.0550521757682816, -27.00111521709620277, 50.15848241876896907 ) ) ;
#26121 = ORIENTED_EDGE ( 'NONE', *, *, #66281, .F. ) ;
#26122 = AXIS2_PLACEMENT_3D ( 'NONE', #16425, #72284, #10492 ) ;
#26123 = ORIENTED_EDGE ( 'NONE', *, *, #82096, .F. ) ;
#26124 = EDGE_LOOP ( 'NONE', ( #57038, #21411, #58241, #49966, #45037, #31511 ) ) ;
#26125 = LINE ( 'NONE', #39734, #63176 ) ;
#26127 = CARTESIAN_POINT ( 'NONE',  ( 107.0667039024470313, -104.2784471599420755, -19.78219314458201694 ) ) ;
#26126 = CARTESIAN_POINT ( 'NONE',  ( 104.0088209277215867, -27.43890701233904394, 161.3299109901969643 ) ) ;
#26128 = DIRECTION ( 'NONE',  ( 0.000000000000000000, 0.000000000000000000, -1.000000000000000000 ) ) ;
#26129 = CARTESIAN_POINT ( 'NONE',  ( -75.03318300175403976, 88.97500000000002274, 34.21687604822299988 ) ) ;
#26130 = B_SPLINE_CURVE_WITH_KNOTS ( 'NONE', 3,
 ( #34774, #6187, #62477, #61570, #89306, #27070, #54740, #82503, #41128, #27957, #21156, #65163, #51079, #2507, #2948, #10202, #70653, #78378, #22963, #86074, #43815, #71555, #24285, #8885, #85637, #8427, #17024, #37909, #71110, #2059, #77918, #86516, #57449, #29319, #16140, #31083, #23847, #79262, #65609, #85191, #23412, #44707, #9317, #3390, #37018, #30649, #36584, #58345 ),
 .UNSPECIFIED., .F., .F.,
 ( 4, 2, 2, 2, 2, 2, 2, 2, 2, 1, 2, 2, 2, 2, 2, 2, 2, 2, 2, 2, 2, 1, 2, 2, 4 ),
 ( 0.05959919981814688211, 0.06208168506169060852, 0.06332292768346245437, 0.06456417030523430023, 0.06704665554877801970, 0.06828789817054987943, 0.06952914079232173916, 0.07201162603586545863, 0.07325286865763731836, 0.07449411127940917809, 0.07573535390118102395, 0.07697659652295288368, 0.07945908176649660315, 0.08194156701004032262, 0.08318280963181218235, 0.08442405225358404208, 0.08690653749712776155, 0.08814778011889962128, 0.08938902274067148102, 0.09187150798421522824, 0.09311275060598708797, 0.09435399322775894770, 0.09559523584953080744, 0.09683647847130266717, 0.09931896371484638664 ),
 .UNSPECIFIED. ) ;
#26131 = EDGE_CURVE ( 'NONE', #8047, #44005, #49298, .T. ) ;
#26132 = DIRECTION ( 'NONE',  ( 0.000000000000000000, 0.000000000000000000, 1.000000000000000000 ) ) ;
#26133 = VECTOR ( 'NONE', #64453, 1000.000000000000000 ) ;
#26134 = DIRECTION ( 'NONE',  ( -0.7071067811865175967, -0.7071067811865774377, -7.071067811865168663E-16 ) ) ;
#26135 = CARTESIAN_POINT ( 'NONE',  ( 72.06648329127396835, -8.979447159941065237, 14.67562527591093513 ) ) ;
#26136 = CARTESIAN_POINT ( 'NONE',  ( 117.3497117099304745, -32.73958051198272301, 94.10895860924395606 ) ) ;
#26137 = EDGE_LOOP ( 'NONE', ( #46916, #65584, #59502, #13760 ) ) ;
#26138 = ORIENTED_EDGE ( 'NONE', *, *, #18842, .T. ) ;
#26139 = AXIS2_PLACEMENT_3D ( 'NONE', #68224, #13258, #88677 ) ;
#26140 = DIRECTION ( 'NONE',  ( 0.000000000000000000, 0.000000000000000000, -1.000000000000000000 ) ) ;
#26141 = FACE_OUTER_BOUND ( 'NONE', #46777, .T. ) ;
#26142 = LINE ( 'NONE', #87917, #33647 ) ;
#26143 = CARTESIAN_POINT ( 'NONE',  ( 107.5257129551532813, -44.87112140103544533, 150.4395189410199407 ) ) ;
#26144 = CARTESIAN_POINT ( 'NONE',  ( 0.000000000000000000, 125.7300000000000040, 0.000000000000000000 ) ) ;
#26145 = EDGE_LOOP ( 'NONE', ( #20742, #9470, #19398, #69954 ) ) ;
#26146 = ORIENTED_EDGE ( 'NONE', *, *, #46420, .T. ) ;
#26147 = ORIENTED_EDGE ( 'NONE', *, *, #53074, .T. ) ;
#26148 = VERTEX_POINT ( 'NONE', #17247 ) ;
#26149 = PRODUCT_DEFINITION_FORMATION_WITH_SPECIFIED_SOURCE ( 'ANY', '', #75331, .NOT_KNOWN. ) ;
#26150 = CARTESIAN_POINT ( 'NONE',  ( 77.59226090855182179, -19.93375462387231067, 7.110117206099022980 ) ) ;
#26151 = CARTESIAN_POINT ( 'NONE',  ( 115.8610455727973090, -35.41879699190349129, 215.3758690201829609 ) ) ;
#26152 = DIRECTION ( 'NONE',  ( 1.000000000000000000, 0.000000000000000000, 0.000000000000000000 ) ) ;
#26153 = AXIS2_PLACEMENT_3D ( 'NONE', #39477, #33113, #61258 ) ;
#26154 = EDGE_CURVE ( 'NONE', #48853, #47787, #44481, .T. ) ;
#26155 = CARTESIAN_POINT ( 'NONE',  ( 72.96458098368701428, 127.0000000000000000, -72.96458098368670164 ) ) ;
#26156 = DIRECTION ( 'NONE',  ( 0.000000000000000000, 0.000000000000000000, 1.000000000000000000 ) ) ;
#26157 = ORIENTED_EDGE ( 'NONE', *, *, #45360, .F. ) ;
#26158 = VERTEX_POINT ( 'NONE', #51735 ) ;
#26159 = DIRECTION ( 'NONE',  ( 0.000000000000000000, 0.000000000000000000, 1.000000000000000000 ) ) ;
#26160 = ORIENTED_EDGE ( 'NONE', *, *, #3030, .T. ) ;
#26161 = ORIENTED_EDGE ( 'NONE', *, *, #53648, .T. ) ;
#26162 = ADVANCED_FACE ( 'NONE', ( #86285 ), #44928, .F. ) ;
#26163 = CIRCLE ( 'NONE', #87124, 7.199999999999998401 ) ;
#26164 = CARTESIAN_POINT ( 'NONE',  ( 111.7906875226637879, -43.98084836425640276, 220.8661856076869583 ) ) ;
#26165 = CARTESIAN_POINT ( 'NONE',  ( 98.07775226919108036, -31.40506188283435307, 85.90133956162493689 ) ) ;
#26166 = CARTESIAN_POINT ( 'NONE',  ( 117.2454586689012359, -38.87819698039184146, 63.66133956162494911 ) ) ;
#26167 = CARTESIAN_POINT ( 'NONE',  ( 111.9916049118937877, -43.86739420629758257, 249.5838068554168672 ) ) ;
#26168 = CARTESIAN_POINT ( 'NONE',  ( 133.0080215814353721, -16.19118199975284611, 8.051357469095140829 ) ) ;
#26169 = PLANE ( 'NONE',  #19982 ) ;
#26170 = CARTESIAN_POINT ( 'NONE',  ( 117.4263761885577537, -30.97555849962366281, 175.2299109901969700 ) ) ;
#26171 = CARTESIAN_POINT ( 'NONE',  ( 48.16670390244701139, -26.71338133339251542, -5.074374724088000832 ) ) ;
#26172 = VERTEX_POINT ( 'NONE', #59887 ) ;
#26173 = DIRECTION ( 'NONE',  ( -1.000000000000000000, -4.299999999999999979E-14, -1.000000000000000078E-15 ) ) ;
#26174 = ORIENTED_EDGE ( 'NONE', *, *, #7930, .T. ) ;
#26175 = ORIENTED_EDGE ( 'NONE', *, *, #4165, .F. ) ;
#26176 = LINE ( 'NONE', #13006, #54664 ) ;
#26178 = VERTEX_POINT ( 'NONE', #73086 ) ;
#26177 = AXIS2_PLACEMENT_3D ( 'NONE', #77648, #29948, #36758 ) ;
#26179 = LINE ( 'NONE', #47494, #67848 ) ;
#26180 = EDGE_CURVE ( 'NONE', #58422, #27248, #35326, .T. ) ;
#26181 = DIRECTION ( 'NONE',  ( -1.000000000000000078E-15, 1.000000000000000000, 0.000000000000000000 ) ) ;
#26182 = CARTESIAN_POINT ( 'NONE',  ( 103.2788000081581288, -47.11369209158109328, 97.28610146638693834 ) ) ;
#26183 = CARTESIAN_POINT ( 'NONE',  ( -12.06903998855693061, 78.50064190147526233, 129.9973879043436398 ) ) ;
#26184 = CARTESIAN_POINT ( 'NONE',  ( 107.0664832912739968, 0.2215528400590083269, 330.1506252759110680 ) ) ;
#26185 = PLANE ( 'NONE',  #48430 ) ;
#26188 = CARTESIAN_POINT ( 'NONE',  ( 97.93839266929580845, -41.72010113774604889, 217.7241967044829494 ) ) ;
#26187 = DIRECTION ( 'NONE',  ( 0.000000000000000000, 0.000000000000000000, 1.000000000000000000 ) ) ;
#26186 = DIRECTION ( 'NONE',  ( 0.8660254037844392627, -0.4999999999999990008, 1.549999999999999706E-14 ) ) ;
#26189 = LINE ( 'NONE', #46609, #68433 ) ;
#26190 = CARTESIAN_POINT ( 'NONE',  ( 179.4595971212720258, -26.00627455219132500, 342.9256252759109884 ) ) ;
#26191 = VERTEX_POINT ( 'NONE', #45806 ) ;
#26192 = CARTESIAN_POINT ( 'NONE',  ( 146.0667039024470171, -86.77844715994089597, 45.21780685541799727 ) ) ;
#26193 = CARTESIAN_POINT ( 'NONE',  ( 0.000000000000000000, 125.7300000000000040, -9.425000000000000711 ) ) ;
#26194 = CARTESIAN_POINT ( 'NONE',  ( -105.4788588808462038, 127.0000000000000000, -3.968750000001139977 ) ) ;
#26195 = CIRCLE ( 'NONE', #45041, 5.562600000000000655 ) ;
#26196 = FACE_BOUND ( 'NONE', #76152, .T. ) ;
#26198 = ORIENTED_EDGE ( 'NONE', *, *, #22322, .F. ) ;
#26197 = CARTESIAN_POINT ( 'NONE',  ( 106.5652189068774902, -47.22232703829767786, 247.5384824187679556 ) ) ;
#26199 = CARTESIAN_POINT ( 'NONE',  ( 104.5038485128689416, -27.03369106489477502, 195.2819955450332827 ) ) ;
#26200 = CARTESIAN_POINT ( 'NONE',  ( 105.3204089162997263, -26.45171782723944176, 11.20991099019697046 ) ) ;
#26201 = CARTESIAN_POINT ( 'NONE',  ( 98.80568095843470644, -28.16380313737984764, 111.6870538473389587 ) ) ;
#26202 = FACE_OUTER_BOUND ( 'NONE', #25307, .T. ) ;
#26203 = CARTESIAN_POINT ( 'NONE',  ( 0.8301116440132043639, 95.22976338641700522, -130.5540265925894801 ) ) ;
#26205 = CYLINDRICAL_SURFACE ( 'NONE', #87821, 2.500000000000002220 ) ;
#26204 = LINE ( 'NONE', #20735, #85550 ) ;
#26206 = CARTESIAN_POINT ( 'NONE',  ( 98.34985895919700738, -31.65658473072328860, 190.9064586020228660 ) ) ;
#26207 = ORIENTED_EDGE ( 'NONE', *, *, #35823, .T. ) ;
#26208 = VERTEX_POINT ( 'NONE', #9985 ) ;
#26209 = ORIENTED_EDGE ( 'NONE', *, *, #8956, .T. ) ;
#26210 = ORIENTED_EDGE ( 'NONE', *, *, #39242, .T. ) ;
#26211 = DIRECTION ( 'NONE',  ( 0.7071067811865473507, 0.7071067811865476838, 0.000000000000000000 ) ) ;
#26212 = CARTESIAN_POINT ( 'NONE',  ( 105.4244226815142298, -47.00233879195495490, 33.44991099019695469 ) ) ;
#26213 = LINE ( 'NONE', #60719, #84661 ) ;
#26214 = EDGE_CURVE ( 'NONE', #21569, #20525, #3604, .T. ) ;
#26215 = CARTESIAN_POINT ( 'NONE',  ( 145.4416927396864878, -139.3034583227001804, 245.6607614918409865 ) ) ;
#26217 = DIRECTION ( 'NONE',  ( 0.000000000000000000, 0.000000000000000000, -1.000000000000000000 ) ) ;
#26216 = LINE ( 'NONE', #19404, #38091 ) ;
#26218 = CARTESIAN_POINT ( 'NONE',  ( 109.4611421171680945, -28.53056059958231216, 259.2724198280769770 ) ) ;
#26219 = ORIENTED_EDGE ( 'NONE', *, *, #9520, .F. ) ;
#26220 = ORIENTED_EDGE ( 'NONE', *, *, #5272, .F. ) ;
#26221 = VERTEX_POINT ( 'NONE', #67164 ) ;
#26222 = PLANE ( 'NONE',  #66009 ) ;
#26223 = CARTESIAN_POINT ( 'NONE',  ( 98.04154813939969415, -41.04191879011435162, 101.6816083635749379 ) ) ;
#26224 = DIRECTION ( 'NONE',  ( 8.659560562355121445E-17, -0.7071067811865315855, 0.7071067811865634489 ) ) ;
#26225 = CARTESIAN_POINT ( 'NONE',  ( -27.27158787008326968, 184.0000000000000000, 80.02307622376218887 ) ) ;
#26226 = CARTESIAN_POINT ( 'NONE',  ( 115.8371248229627639, -37.99598801341877419, 25.14444044875396855 ) ) ;
#26227 = AXIS2_PLACEMENT_3D ( 'NONE', #34192, #20586, #61895 ) ;
#26228 = CARTESIAN_POINT ( 'NONE',  ( 118.5385583271987855, 95.08639429146512612, 2.073938160689064336 ) ) ;
#26229 = ADVANCED_FACE ( 'NONE', ( #25384 ), #31298, .F. ) ;
#26230 = VECTOR ( 'NONE', #81976, 1000.000000000000000 ) ;
#26231 = CARTESIAN_POINT ( 'NONE',  ( 97.31589510082254435, -39.30610152985839534, 176.5314694035164678 ) ) ;
#26232 = EDGE_CURVE ( 'NONE', #22899, #39347, #53052, .T. ) ;
#26233 = CARTESIAN_POINT ( 'NONE',  ( 96.91794407517402021, -34.59732685048006573, 261.1737205140070159 ) ) ;
#26234 = VECTOR ( 'NONE', #80295, 1000.000000000000000 ) ;
#26235 = DIRECTION ( 'NONE',  ( -4.299999999999999979E-14, 1.000000000000000000, -4.128053709984630540E-29 ) ) ;
#26236 = VERTEX_POINT ( 'NONE', #58994 ) ;
#26237 = CARTESIAN_POINT ( 'NONE',  ( 165.3359832912740046, -36.32844715994100682, 117.4678068554150485 ) ) ;
#26238 = CIRCLE ( 'NONE', #13217, 1.000000000000000888 ) ;
#26239 = DIRECTION ( 'NONE',  ( 0.000000000000000000, 0.000000000000000000, 1.000000000000000000 ) ) ;
#26240 = CARTESIAN_POINT ( 'NONE',  ( 98.66659878002396056, -40.67125783036974696, 59.49380465530595785 ) ) ;
#26241 = AXIS2_PLACEMENT_3D ( 'NONE', #47698, #6383, #68619 ) ;
#26242 = PLANE ( 'NONE',  #55139 ) ;
#26243 = CARTESIAN_POINT ( 'NONE',  ( 172.5664832912729878, -18.82844715994071194, 198.9256252759119832 ) ) ;
#26244 = CARTESIAN_POINT ( 'NONE',  ( -8.382543579435365544, 92.09976689429159080, 118.2597275672832069 ) ) ;
#26245 = ORIENTED_EDGE ( 'NONE', *, *, #39421, .T. ) ;
#26246 = DIRECTION ( 'NONE',  ( 0.000000000000000000, 0.000000000000000000, 1.000000000000000000 ) ) ;
#26247 = CARTESIAN_POINT ( 'NONE',  ( 121.5330498715421896, 59.98657059693208282, -47.69329234032820608 ) ) ;
#26248 = ORIENTED_EDGE ( 'NONE', *, *, #77603, .T. ) ;
#26249 = CARTESIAN_POINT ( 'NONE',  ( 97.93239114460148187, -31.63098981178377755, 110.9213395616259703 ) ) ;
#26250 = ORIENTED_EDGE ( 'NONE', *, *, #52522, .F. ) ;
#26251 = CARTESIAN_POINT ( 'NONE',  ( 115.1845888671227556, -34.07379402343466523, 88.50099125664800681 ) ) ;
#26252 = AXIS2_PLACEMENT_3D ( 'NONE', #18051, #73915, #58485 ) ;
#26253 = DIRECTION ( 'NONE',  ( -0.7071067811578587436, 0.7071067812152364018, 0.000000000000000000 ) ) ;
#26254 = CARTESIAN_POINT ( 'NONE',  ( 116.2382276885637538, -38.76798346032508391, 100.0720594963729866 ) ) ;
#26255 = DIRECTION ( 'NONE',  ( 0.000000000000000000, 1.000000000000000000, 0.000000000000000000 ) ) ;
#26256 = DIRECTION ( 'NONE',  ( 0.000000000000000000, 0.000000000000000000, -1.000000000000000000 ) ) ;
#26257 = CARTESIAN_POINT ( 'NONE',  ( 117.2880962612577349, -38.88719764259226253, 59.66133956162595098 ) ) ;
#26258 = VECTOR ( 'NONE', #42595, 1000.000000000000114 ) ;
#26259 = DIRECTION ( 'NONE',  ( -0.1250000000000000278, -0.9921567416492215186, 3.035766082959410522E-14 ) ) ;
#26260 = CARTESIAN_POINT ( 'NONE',  ( 116.8172185371468146, -34.15328862580971503, 259.0314398403625091 ) ) ;
#26261 = ORIENTED_EDGE ( 'NONE', *, *, #48067, .T. ) ;
#26262 = FACE_OUTER_BOUND ( 'NONE', #85504, .T. ) ;
#26263 = ORIENTED_EDGE ( 'NONE', *, *, #44664, .F. ) ;
#26264 = VERTEX_POINT ( 'NONE', #24505 ) ;
#26265 = EDGE_CURVE ( 'NONE', #65449, #55364, #42575, .T. ) ;
#26266 = VECTOR ( 'NONE', #23071, 1000.000000000000000 ) ;
#26267 = LINE ( 'NONE', #46237, #70254 ) ;
#26268 = VERTEX_POINT ( 'NONE', #46251 ) ;
#26269 = CARTESIAN_POINT ( 'NONE',  ( 101.1405520526759574, -45.23956608920065037, 237.0803871806729717 ) ) ;
#26270 = CARTESIAN_POINT ( 'NONE',  ( 117.2592865896494345, -39.02220311275136311, 144.6499109901969859 ) ) ;
#26271 = CARTESIAN_POINT ( 'NONE',  ( 6.364907348149458244, 71.52879593750107290, -118.3870396030140029 ) ) ;
#26272 = DIRECTION ( 'NONE',  ( 0.000000000000000000, 1.000000000000000000, 0.000000000000000000 ) ) ;
#26273 = CARTESIAN_POINT ( 'NONE',  ( 98.85791787721181834, -43.21333385077131339, 87.85848241876792031 ) ) ;
#26274 = AXIS2_PLACEMENT_3D ( 'NONE', #35783, #50763, #55754 ) ;
#26275 = CARTESIAN_POINT ( 'NONE',  ( 163.5667039024460223, -22.48495420874110806, -5.074374724088000832 ) ) ;
#26276 = ORIENTED_EDGE ( 'NONE', *, *, #86903, .F. ) ;
#26277 = CARTESIAN_POINT ( 'NONE',  ( 180.3503142329326465, -29.99615139350787629, 342.9256252759109884 ) ) ;
#26278 = LINE ( 'NONE', #20812, #47672 ) ;
#26279 = ORIENTED_EDGE ( 'NONE', *, *, #39630, .F. ) ;
#26280 = LINE ( 'NONE', #88527, #2581 ) ;
#26281 = EDGE_CURVE ( 'NONE', #7509, #57079, #72214, .T. ) ;
#26282 = DIRECTION ( 'NONE',  ( 0.000000000000000000, -1.000000000000000000, 0.000000000000000000 ) ) ;
#26283 = CARTESIAN_POINT ( 'NONE',  ( 110.9847977634196496, -46.36662828626499078, 282.8841967044824628 ) ) ;
#26284 = LINE ( 'NONE', #74889, #83747 ) ;
#26285 = CARTESIAN_POINT ( 'NONE',  ( 30.48091746481835429, -49.32844715994148288, 249.9678068554150059 ) ) ;
#26286 = LINE ( 'NONE', #84413, #60037 ) ;
#26287 = CARTESIAN_POINT ( 'NONE',  ( 114.1362055435773613, -41.52268812998874381, 272.7752769709339304 ) ) ;
#26289 = CARTESIAN_POINT ( 'NONE',  ( 97.24623519876082867, -31.70684325556598893, 91.96229194257693962 ) ) ;
#26288 = CARTESIAN_POINT ( 'NONE',  ( 97.72316397745180439, -40.29463414041478586, 101.6170128052498995 ) ) ;
#26290 = CYLINDRICAL_SURFACE ( 'NONE', #58179, 3.000000000000002665 ) ;
#26291 = CARTESIAN_POINT ( 'NONE',  ( 95.86269369446621624, -32.71648115089089259, 176.0527681330539735 ) ) ;
#26292 = EDGE_LOOP ( 'NONE', ( #32056, #55291, #5115, #55409 ) ) ;
#26293 = DIRECTION ( 'NONE',  ( -1.000000000000000000, -1.000000000000000078E-15, 0.000000000000000000 ) ) ;
#26294 = ORIENTED_EDGE ( 'NONE', *, *, #89339, .T. ) ;
#26295 = ADVANCED_FACE ( 'NONE', ( #85859 ), #58125, .F. ) ;
#26296 = CARTESIAN_POINT ( 'NONE',  ( 32.15435173583699680, -31.62489322948790971, 237.4678068554150059 ) ) ;
#26297 = CIRCLE ( 'NONE', #66875, 2.116999999999980009 ) ;
#26298 = CARTESIAN_POINT ( 'NONE',  ( 115.8254323908916206, -31.73001882624620862, 65.23979194279471017 ) ) ;
#26299 = CARTESIAN_POINT ( 'NONE',  ( 107.0667039024470313, -104.2784471599420755, -19.78219314458201694 ) ) ;
#26300 = ORIENTED_EDGE ( 'NONE', *, *, #65601, .F. ) ;
#26301 = EDGE_CURVE ( 'NONE', #65247, #78334, #58557, .T. ) ;
#26302 = EDGE_CURVE ( 'NONE', #83222, #84863, #80372, .T. ) ;
#26303 = DIRECTION ( 'NONE',  ( -0.7071067811861110330, -0.7071067811869841124, 0.000000000000000000 ) ) ;
#26305 = ORIENTED_EDGE ( 'NONE', *, *, #29682, .T. ) ;
#26304 = CARTESIAN_POINT ( 'NONE',  ( 114.2703446987665643, -45.17953892438131192, 153.1508633711489722 ) ) ;
#26306 = DIRECTION ( 'NONE',  ( 0.000000000000000000, 0.000000000000000000, -1.000000000000000000 ) ) ;
#26307 = DIRECTION ( 'NONE',  ( -1.000000000000000078E-15, 1.000000000000000083E-30, 1.000000000000000000 ) ) ;
#26308 = AXIS2_PLACEMENT_3D ( 'NONE', #12800, #88657, #7323 ) ;
#26309 = DIRECTION ( 'NONE',  ( -7.136255983449500255E-16, 0.000000000000000000, -1.000000000000000000 ) ) ;
#26310 = EDGE_CURVE ( 'NONE', #51954, #84121, #53958, .T. ) ;
#26311 = PLANE ( 'NONE',  #56827 ) ;
#26312 = ORIENTED_EDGE ( 'NONE', *, *, #19175, .T. ) ;
#26313 = VECTOR ( 'NONE', #2606, 1000.000000000000000 ) ;
#26314 = CARTESIAN_POINT ( 'NONE',  ( 0.000000000000000000, 3.010054685665091170E-14, -295.6978641014162008 ) ) ;
#26315 = EDGE_CURVE ( 'NONE', #37237, #41991, #74437, .T. ) ;
#26316 = PLANE ( 'NONE',  #2092 ) ;
#26317 = VERTEX_POINT ( 'NONE', #40800 ) ;
#26318 = ORIENTED_EDGE ( 'NONE', *, *, #18781, .T. ) ;
#26319 = DIRECTION ( 'NONE',  ( 0.9068632946707807507, -0.4214249218767881500, 1.031805784967618114E-15 ) ) ;
#26320 = CARTESIAN_POINT ( 'NONE',  ( 83.41565754067528360, 86.63355734047006251, -100.4326241145867300 ) ) ;
#26321 = LINE ( 'NONE', #46744, #26598 ) ;
#26322 = ADVANCED_FACE ( 'NONE', ( #60795 ), #46708, .F. ) ;
#26323 = CARTESIAN_POINT ( 'NONE',  ( 116.3262419368496978, -32.93860311337579105, 160.1356252759109680 ) ) ;
#26324 = CIRCLE ( 'NONE', #64003, 12.69999999999998863 ) ;
#26326 = DIRECTION ( 'NONE',  ( 1.000000000000000000, -1.332267629550186637E-12, 0.000000000000000000 ) ) ;
#26325 = DIRECTION ( 'NONE',  ( 0.000000000000000000, 0.000000000000000000, 1.000000000000000000 ) ) ;
#26327 = CARTESIAN_POINT ( 'NONE',  ( 109.7247516442869539, -27.00077167917759979, 179.8648013270537263 ) ) ;
#26328 = AXIS2_PLACEMENT_3D ( 'NONE', #64747, #38816, #87427 ) ;
#26329 = VERTEX_POINT ( 'NONE', #4947 ) ;
#26330 = DIRECTION ( 'NONE',  ( -1.000000000000000000, -4.299999999999999979E-14, -1.000000000000000078E-15 ) ) ;
#26331 = CARTESIAN_POINT ( 'NONE',  ( 109.8674951572811267, -26.74480306206640989, 215.8708633711489711 ) ) ;
#26332 = CIRCLE ( 'NONE', #35018, 13.16666666666670160 ) ;
#26334 = ORIENTED_EDGE ( 'NONE', *, *, #15336, .T. ) ;
#26333 = FACE_OUTER_BOUND ( 'NONE', #86659, .T. ) ;
#26335 = ADVANCED_FACE ( 'NONE', ( #89418 ), #6289, .F. ) ;
#26336 = CARTESIAN_POINT ( 'NONE',  ( 100.4186822966650539, -43.90371905523895890, 42.98133956162492098 ) ) ;
#26338 = EDGE_CURVE ( 'NONE', #22610, #46354, #74887, .T. ) ;
#26337 = CARTESIAN_POINT ( 'NONE',  ( 110.8601161811647273, -45.98192586914924362, 52.88611059975448825 ) ) ;
#26339 = DIRECTION ( 'NONE',  ( -0.7071067811865516806, 0.7071067811865434649, -7.071067811865511818E-16 ) ) ;
#26340 = VECTOR ( 'NONE', #70667, 1000.000000000000000 ) ;
#26341 = EDGE_CURVE ( 'NONE', #77150, #75223, #55306, .T. ) ;
#26342 = FACE_OUTER_BOUND ( 'NONE', #23696, .T. ) ;
#26343 = VERTEX_POINT ( 'NONE', #82617 ) ;
#26344 = FACE_OUTER_BOUND ( 'NONE', #29105, .T. ) ;
#26345 = EDGE_CURVE ( 'NONE', #14963, #24180, #2023, .T. ) ;
#26346 = VERTEX_POINT ( 'NONE', #83063 ) ;
#26347 = ORIENTED_EDGE ( 'NONE', *, *, #49988, .T. ) ;
#26348 = CARTESIAN_POINT ( 'NONE',  ( 101.7595872045747285, -44.48272901101389465, 238.5425356868499591 ) ) ;
#26349 = CARTESIAN_POINT ( 'NONE',  ( 100.8876536524146843, -44.70040499368899134, 53.05193493111340786 ) ) ;
#26350 = CARTESIAN_POINT ( 'NONE',  ( 177.0664832912740110, 12.92155284005802685, 336.5756252759111362 ) ) ;
#26351 = CARTESIAN_POINT ( 'NONE',  ( 116.8171228687850203, -34.15291832615506706, 155.0314586087714588 ) ) ;
#26352 = CARTESIAN_POINT ( 'NONE',  ( -47.02966122971776741, 101.5999999999999943, 76.61736725193563302 ) ) ;
#26354 = ORIENTED_EDGE ( 'NONE', *, *, #84214, .F. ) ;
#26353 = VECTOR ( 'NONE', #79063, 1000.000000000000000 ) ;
#26355 = DIRECTION ( 'NONE',  ( -1.000000000000000000, 0.000000000000000000, 0.000000000000000000 ) ) ;
#26356 = FACE_OUTER_BOUND ( 'NONE', #61549, .T. ) ;
#26357 = ORIENTED_EDGE ( 'NONE', *, *, #54204, .T. ) ;
#26358 = CARTESIAN_POINT ( 'NONE',  ( 116.5620552962771654, -42.34175257684902505, 283.4137205140060587 ) ) ;
#26359 = ORIENTED_EDGE ( 'NONE', *, *, #11856, .F. ) ;
#26360 = EDGE_LOOP ( 'NONE', ( #20309, #37997 ) ) ;
#26361 = CARTESIAN_POINT ( 'NONE',  ( 99.66640463149437323, -40.17452507577532117, 254.4909475124484857 ) ) ;
#26362 = DIRECTION ( 'NONE',  ( 0.000000000000000000, 0.000000000000000000, -1.000000000000000000 ) ) ;
#26363 = CARTESIAN_POINT ( 'NONE',  ( 118.1851208724672233, -36.91582462397655462, 153.8127681330539644 ) ) ;
#26364 = CARTESIAN_POINT ( 'NONE',  ( 23.44962858617382295, 79.40261884150201865, 306.4827471306458051 ) ) ;
#26365 = CARTESIAN_POINT ( 'NONE',  ( 0.000000000000000000, 95.00619999999999266, 0.000000000000000000 ) ) ;
#26366 = LINE ( 'NONE', #54035, #24531 ) ;
#26367 = DIRECTION ( 'NONE',  ( -1.000000000000000000, -8.163404592832032979E-16, 0.000000000000000000 ) ) ;
#26368 = CARTESIAN_POINT ( 'NONE',  ( 105.1027920011780452, -26.44660240447466037, 231.2270538473399597 ) ) ;
#26369 = CARTESIAN_POINT ( 'NONE',  ( -75.61066417432020614, 101.5999999999999943, 189.7379999999999995 ) ) ;
#26370 = VERTEX_POINT ( 'NONE', #20378 ) ;
#26371 = VECTOR ( 'NONE', #69748, 1000.000000000000000 ) ;
#26372 = CARTESIAN_POINT ( 'NONE',  ( 107.2328990581281687, -25.63125793145087172, 76.07657765686298035 ) ) ;
#26373 = CYLINDRICAL_SURFACE ( 'NONE', #45342, 5.599999999999994316 ) ;
#26374 = ORIENTED_EDGE ( 'NONE', *, *, #78663, .T. ) ;
#26375 = VERTEX_POINT ( 'NONE', #75337 ) ;
#26376 = EDGE_LOOP ( 'NONE', ( #12700, #65458, #62976, #54628, #56325 ) ) ;
#26377 = FACE_BOUND ( 'NONE', #6457, .T. ) ;
#26378 = DIRECTION ( 'NONE',  ( 5.512527431108029424E-15, -1.000000000000000000, 0.000000000000000000 ) ) ;
#26379 = DIRECTION ( 'NONE',  ( -1.000000000000000000, -4.299999999999999979E-14, -9.351236661543306751E-17 ) ) ;
#26380 = CARTESIAN_POINT ( 'NONE',  ( 143.0667039024470455, -124.7784471599409102, 45.21780685541799727 ) ) ;
#26381 = CARTESIAN_POINT ( 'NONE',  ( 112.6831787765100898, -43.31780159632685212, 150.9690427505439914 ) ) ;
#26382 = CARTESIAN_POINT ( 'NONE',  ( 100.1631548973110739, -45.39139052332982516, 268.0289586092443415 ) ) ;
#26383 = AXIS2_PLACEMENT_3D ( 'NONE', #86472, #2899, #84692 ) ;
#26384 = CARTESIAN_POINT ( 'NONE',  ( 41.56670390244804025, -42.82844715994103524, 300.4678068554150059 ) ) ;
#26385 = ORIENTED_EDGE ( 'NONE', *, *, #51285, .T. ) ;
#26386 = CARTESIAN_POINT ( 'NONE',  ( 130.1098569802757652, 89.26666702275853993, 10.78644903371371733 ) ) ;
#26387 = DIRECTION ( 'NONE',  ( 1.000000000000000000, 0.000000000000000000, 0.000000000000000000 ) ) ;
#26388 = EDGE_LOOP ( 'NONE', ( #33416, #84896 ) ) ;
#26390 = VERTEX_POINT ( 'NONE', #27178 ) ;
#26389 = CIRCLE ( 'NONE', #20568, 2.517500000000005844 ) ;
#26391 = CIRCLE ( 'NONE', #35134, 14.49999999999997158 ) ;
#26392 = FACE_BOUND ( 'NONE', #69630, .T. ) ;
#26393 = ADVANCED_FACE ( 'NONE', ( #67617 ), #5401, .F. ) ;
#26394 = VERTEX_POINT ( 'NONE', #6734 ) ;
#26395 = EDGE_LOOP ( 'NONE', ( #153, #76034, #4927, #20796 ) ) ;
#26396 = CARTESIAN_POINT ( 'NONE',  ( 162.8913605087228404, -31.76306994223244118, 117.4678068554150485 ) ) ;
#26397 = CARTESIAN_POINT ( 'NONE',  ( -12.03356702080700202, 78.46872568947895843, -130.0002966128845969 ) ) ;
#26398 = EDGE_CURVE ( 'NONE', #60336, #67129, #40355, .T. ) ;
#26399 = DIRECTION ( 'NONE',  ( -2.900000000000000265E-14, 2.000000000000000155E-15, -1.000000000000000000 ) ) ;
#26400 = CARTESIAN_POINT ( 'NONE',  ( 107.5667039024470171, -94.77844715994206126, -19.78219314458232247 ) ) ;
#26401 = CARTESIAN_POINT ( 'NONE',  ( 115.4001863486352022, -38.60401951598402803, 148.0724198280769883 ) ) ;
#26402 = AXIS2_PLACEMENT_3D ( 'NONE', #34443, #62152, #35784 ) ;
#26403 = CARTESIAN_POINT ( 'NONE',  ( 100.9151287000745896, -46.91716693487881429, 52.14419670448194921 ) ) ;
#26404 = DIRECTION ( 'NONE',  ( -0.000000000000000000, -0.000000000000000000, 1.000000000000000000 ) ) ;
#26405 = EDGE_LOOP ( 'NONE', ( #74014, #35538, #68185, #41196 ) ) ;
#26406 = ADVANCED_FACE ( 'NONE', ( #61682 ), #68070, .T. ) ;
#26407 = DIRECTION ( 'NONE',  ( 0.000000000000000000, 0.000000000000000000, 1.000000000000000000 ) ) ;
#26408 = AXIS2_PLACEMENT_3D ( 'NONE', #50539, #78281, #9225 ) ;
#26409 = ORIENTED_EDGE ( 'NONE', *, *, #64862, .T. ) ;
#26410 = ADVANCED_FACE ( 'NONE', ( #33542 ), #34432, .T. ) ;
#26411 = ADVANCED_FACE ( 'NONE', ( #68966 ), #62142, .F. ) ;
#26412 = PLANE ( 'NONE',  #69413 ) ;
#26413 = VECTOR ( 'NONE', #45665, 1000.000000000000000 ) ;
#26414 = EDGE_LOOP ( 'NONE', ( #37221, #35047, #42547, #49840 ) ) ;
#26415 = LINE ( 'NONE', #14587, #87101 ) ;
#26416 = DIRECTION ( 'NONE',  ( -0.000000000000000000, 1.000000000000000000, 0.000000000000000000 ) ) ;
#26417 = CARTESIAN_POINT ( 'NONE',  ( 110.9845004553952208, -45.93008197751423438, 132.8968334499706145 ) ) ;
#26418 = EDGE_CURVE ( 'NONE', #17652, #31120, #48481, .T. ) ;
#26419 = FACE_OUTER_BOUND ( 'NONE', #44552, .T. ) ;
#26420 = VERTEX_POINT ( 'NONE', #81275 ) ;
#26421 = CARTESIAN_POINT ( 'NONE',  ( 96.63682800883232460, -32.99879952304045361, 26.06514908543494613 ) ) ;
#26422 = CARTESIAN_POINT ( 'NONE',  ( 97.58291127976856671, -32.21282489450084086, 71.97276813305397525 ) ) ;
#26423 = EDGE_CURVE ( 'NONE', #52268, #78030, #85622, .T. ) ;
#26425 = CARTESIAN_POINT ( 'NONE',  ( 208.9149999999999920, 37.33800000000000097, 50.79999999999999716 ) ) ;
#26424 = CARTESIAN_POINT ( 'NONE',  ( 34.92499999999999716, 66.67499999999999716, 295.2750000000000341 ) ) ;
#26426 = CARTESIAN_POINT ( 'NONE',  ( 63.03715912545644784, -24.42818131006017168, 117.4678068554150485 ) ) ;
#26427 = DIRECTION ( 'NONE',  ( 0.000000000000000000, 0.000000000000000000, 1.000000000000000000 ) ) ;
#26428 = CARTESIAN_POINT ( 'NONE',  ( 188.5667039024479834, -62.87844715994099687, 173.2178068554149775 ) ) ;
#26429 = EDGE_CURVE ( 'NONE', #21656, #88388, #36265, .T. ) ;
#26430 = CARTESIAN_POINT ( 'NONE',  ( 88.90000000000000568, 66.67499999999999716, 219.0749999999999886 ) ) ;
#26431 = DIRECTION ( 'NONE',  ( 3.114895971316861016E-16, -1.000000000000000000, 0.000000000000000000 ) ) ;
#26432 = ORIENTED_EDGE ( 'NONE', *, *, #48011, .F. ) ;
#26433 = CARTESIAN_POINT ( 'NONE',  ( 97.73303842741869119, -31.98671872394393034, 50.95276813305294183 ) ) ;
#26434 = CARTESIAN_POINT ( 'NONE',  ( 116.9955931624231624, -33.48136526131695234, 85.07848241876791917 ) ) ;
#26435 = VECTOR ( 'NONE', #19841, 1000.000000000000000 ) ;
#26437 = DIRECTION ( 'NONE',  ( -6.524622321627019585E-16, -3.741823817616790462E-31, -1.000000000000000000 ) ) ;
#26436 = CARTESIAN_POINT ( 'NONE',  ( 101.9941904926150613, -45.44642369002148286, 172.1539441930640635 ) ) ;
#26438 = CARTESIAN_POINT ( 'NONE',  ( 31.71315051186932621, -31.94127993907824958, 342.9256252759109884 ) ) ;
#26439 = CARTESIAN_POINT ( 'NONE',  ( 139.3670900352978208, -74.85671702932823734, 248.3919668373590071 ) ) ;
#26440 = ORIENTED_EDGE ( 'NONE', *, *, #39337, .F. ) ;
#26441 = CARTESIAN_POINT ( 'NONE',  ( 103.5913876162975953, -46.49993820617270757, 98.31657765686297523 ) ) ;
#26443 = EDGE_LOOP ( 'NONE', ( #24031, #34413, #10209, #45027 ) ) ;
#26442 = CARTESIAN_POINT ( 'NONE',  ( 12.69999999999999751, 83.33714971666560700, 129.9368274816649773 ) ) ;
#26444 = CARTESIAN_POINT ( 'NONE',  ( 115.8368392028493190, -44.66223131803943858, 229.2413395616249545 ) ) ;
#26445 = CARTESIAN_POINT ( 'NONE',  ( 116.3136297247243078, -32.94478793390952376, 255.1356252759109395 ) ) ;
#26446 = CARTESIAN_POINT ( 'NONE',  ( 29.56670390244797630, -48.82844715994099971, 310.9178068554150514 ) ) ;
#26447 = DIRECTION ( 'NONE',  ( -6.831565154159360295E-14, 1.000000000000000000, 0.000000000000000000 ) ) ;
#26448 = CARTESIAN_POINT ( 'NONE',  ( 115.8254323924586231, -31.73001883007492552, 80.23979194246547308 ) ) ;
#26449 = VECTOR ( 'NONE', #35282, 1000.000000000000000 ) ;
#26450 = EDGE_CURVE ( 'NONE', #8036, #28811, #35323, .T. ) ;
#26451 = CARTESIAN_POINT ( 'NONE',  ( 131.5867845949876198, -37.92005462650919156, 2.747931806398446586 ) ) ;
#26452 = CARTESIAN_POINT ( 'NONE',  ( 25.56670390244744695, -48.82844715994178841, 173.2178068554150627 ) ) ;
#26453 = EDGE_CURVE ( 'NONE', #87386, #25446, #42136, .T. ) ;
#26454 = CARTESIAN_POINT ( 'NONE',  ( 102.9544237342423969, -27.85507949283293527, 180.4213395616259845 ) ) ;
#26455 = ORIENTED_EDGE ( 'NONE', *, *, #7102, .F. ) ;
#26456 = ORIENTED_EDGE ( 'NONE', *, *, #76350, .T. ) ;
#26457 = CARTESIAN_POINT ( 'NONE',  ( 116.0270257299131487, -33.90363670229466919, 125.4892023535159638 ) ) ;
#26458 = VECTOR ( 'NONE', #13887, 1000.000000000000000 ) ;
#26459 = DIRECTION ( 'NONE',  ( 0.000000000000000000, 3.785359618865284342E-16, -1.000000000000000000 ) ) ;
#26461 = DIRECTION ( 'NONE',  ( 0.000000000000000000, 0.000000000000000000, 1.000000000000000000 ) ) ;
#26460 = CARTESIAN_POINT ( 'NONE',  ( 100.6033219294153724, -44.83909144599376617, 268.0289586092438867 ) ) ;
#26462 = DIRECTION ( 'NONE',  ( 0.000000000000000000, 0.000000000000000000, 1.000000000000000000 ) ) ;
#26463 = AXIS2_PLACEMENT_3D ( 'NONE', #6640, #76124, #39367 ) ;
#26464 = FACE_OUTER_BOUND ( 'NONE', #10738, .T. ) ;
#26465 = CARTESIAN_POINT ( 'NONE',  ( -107.7702177616926065, 120.6499999999999915, -1.170464777364108012E-12 ) ) ;
#26466 = CARTESIAN_POINT ( 'NONE',  ( 164.9667039024459996, -26.71338133339301635, -5.074374724088000832 ) ) ;
#26467 = PLANE ( 'NONE',  #16881 ) ;
#26468 = CARTESIAN_POINT ( 'NONE',  ( 117.4654710391980217, -40.40706546494233464, 178.5680062282919778 ) ) ;
#26469 = CARTESIAN_POINT ( 'NONE',  ( 115.0900420730608147, -30.61910110487549019, 169.3437578978403337 ) ) ;
#26470 = ORIENTED_EDGE ( 'NONE', *, *, #39941, .T. ) ;
#26471 = EDGE_LOOP ( 'NONE', ( #33693, #5255, #15069, #22026 ) ) ;
#26472 = CARTESIAN_POINT ( 'NONE',  ( -98.64078293412680409, 73.86195533656251655, -85.52748787272817310 ) ) ;
#26473 = CARTESIAN_POINT ( 'NONE',  ( 77.59184326793636899, -17.51852171451485063, 2.740177351661285954 ) ) ;
#26474 = DIRECTION ( 'NONE',  ( 4.299999999999999979E-14, -1.000000000000000000, 4.400000000000000367E-29 ) ) ;
#26475 = DIRECTION ( 'NONE',  ( 0.02150753337723862457, 0.0009076677972192722819, 0.9997682742251809973 ) ) ;
#26476 = DIRECTION ( 'NONE',  ( 0.000000000000000000, 1.000000000000000000, 0.000000000000000000 ) ) ;
#26477 = VERTEX_POINT ( 'NONE', #8538 ) ;
#26478 = CARTESIAN_POINT ( 'NONE',  ( -8.325041732967005004, 92.04361142620588510, 118.0642879194596446 ) ) ;
#26479 = CARTESIAN_POINT ( 'NONE',  ( 115.3881169701508327, -30.44952332473371115, 219.3413395616249773 ) ) ;
#26480 = ORIENTED_EDGE ( 'NONE', *, *, #62533, .T. ) ;
#26481 = CIRCLE ( 'NONE', #43863, 16.00000000000000000 ) ;
#26482 = DIRECTION ( 'NONE',  ( -0.7071067811865512365, 0.000000000000000000, 0.7071067811865436870 ) ) ;
#26483 = DIRECTION ( 'NONE',  ( 1.000000000000000078E-15, 0.000000000000000000, -1.000000000000000000 ) ) ;
#26484 = CARTESIAN_POINT ( 'NONE',  ( 98.30750600249929505, -41.72880667514048980, 162.7397860246828714 ) ) ;
#26485 = CARTESIAN_POINT ( 'NONE',  ( 101.5184502652259084, -42.71685524349225460, 44.79951894101996857 ) ) ;
#26486 = CARTESIAN_POINT ( 'NONE',  ( 117.7011894673193382, -39.82593390098057284, 134.5889586092439743 ) ) ;
#26487 = CARTESIAN_POINT ( 'NONE',  ( 172.5664832912740110, -32.07844715994070839, 14.17562527591199917 ) ) ;
#26488 = EDGE_LOOP ( 'NONE', ( #54926, #44763, #31465, #37856 ) ) ;
#26489 = DIRECTION ( 'NONE',  ( 1.000000000000000078E-15, 1.000000000000000083E-30, -1.000000000000000000 ) ) ;
#26490 = EDGE_CURVE ( 'NONE', #6493, #45463, #15803, .T. ) ;
#26491 = CARTESIAN_POINT ( 'NONE',  ( 100.7388752691453391, -44.57574992080446918, 67.03815598159052058 ) ) ;
#26492 = VERTEX_POINT ( 'NONE', #2171 ) ;
#26493 = VERTEX_POINT ( 'NONE', #1726 ) ;
#26494 = AXIS2_PLACEMENT_3D ( 'NONE', #45893, #32734, #82257 ) ;
#26495 = B_SPLINE_CURVE_WITH_KNOTS ( 'NONE', 3,
 ( #4104, #31804, #64999, #50459, #43645, #30035, #58178, #71383, #9148, #50912, #57728, #85469, #23246, #9588, #85908, #39517, #60847, #33600 ),
 .UNSPECIFIED., .F., .F.,
 ( 4, 2, 2, 2, 2, 2, 2, 2, 4 ),
 ( 0.000000000000000000, 0.1250000000000000000, 0.2500000000000000000, 0.3750000000000000000, 0.5000000000000000000, 0.6250000000000000000, 0.7500000000000000000, 0.8750000000000000000, 1.000000000000000000 ),
 .UNSPECIFIED. ) ;
#26496 = CARTESIAN_POINT ( 'NONE',  ( 160.7738106836348777, -48.62134037874901082, 249.9678068554149490 ) ) ;
#26497 = EDGE_LOOP ( 'NONE', ( #13466, #58443, #44263, #64325 ) ) ;
#26498 = EDGE_LOOP ( 'NONE', ( #75004, #49737, #63763, #70702, #67026, #33976 ) ) ;
#26499 = DIRECTION ( 'NONE',  ( 1.000000000000000000, 4.163336342344333240E-14, 0.000000000000000000 ) ) ;
#26500 = EDGE_CURVE ( 'NONE', #20871, #44627, #78488, .T. ) ;
#26501 = EDGE_CURVE ( 'NONE', #68029, #16276, #78035, .T. ) ;
#26502 = CARTESIAN_POINT ( 'NONE',  ( 104.9561144943094035, -45.03597746244296474, 46.80099125664899162 ) ) ;
#26503 = CARTESIAN_POINT ( 'NONE',  ( 96.78703652860848194, -40.85599721901744630, 251.6422919425777138 ) ) ;
#26504 = EDGE_CURVE ( 'NONE', #34907, #71626, #15972, .T. ) ;
#26505 = CARTESIAN_POINT ( 'NONE',  ( 108.8451227504523331, -46.97957433935484772, 167.7127681330539701 ) ) ;
#26507 = CARTESIAN_POINT ( 'NONE',  ( 111.4063510358307241, -46.18429848020799255, 23.91848241876792969 ) ) ;
#26506 = DIRECTION ( 'NONE',  ( 0.000000000000000000, 0.000000000000000000, 1.000000000000000000 ) ) ;
#26508 = CARTESIAN_POINT ( 'NONE',  ( 32.06670390244800473, -33.35206098992711077, -5.074374724088000832 ) ) ;
#26509 = CARTESIAN_POINT ( 'NONE',  ( 71.06648329127399677, -18.82844715994099971, 17.92562527591199739 ) ) ;
#26510 = EDGE_CURVE ( 'NONE', #70068, #1129, #72003, .T. ) ;
#26511 = EDGE_LOOP ( 'NONE', ( #23880, #84669 ) ) ;
#26512 = EDGE_CURVE ( 'NONE', #42491, #66495, #14909, .T. ) ;
#26513 = CIRCLE ( 'NONE', #84578, 4.750000000000004441 ) ;
#26514 = CARTESIAN_POINT ( 'NONE',  ( 78.56670390244704549, -118.2784471599409812, 51.21780685541800437 ) ) ;
#26515 = CARTESIAN_POINT ( 'NONE',  ( 100.7967938542458199, -45.88935316334050185, 242.1108633711489517 ) ) ;
#26516 = ORIENTED_EDGE ( 'NONE', *, *, #10468, .F. ) ;
#26517 = CARTESIAN_POINT ( 'NONE',  ( 110.6963687344609184, -48.01060035924083280, 207.8241967044819489 ) ) ;
#26518 = DIRECTION ( 'NONE',  ( 0.000000000000000000, 0.000000000000000000, -1.000000000000000000 ) ) ;
#26519 = SURFACE_SIDE_STYLE ('',( #55086 ) ) ;
#26520 = LINE ( 'NONE', #27856, #47867 ) ;
#26521 = CARTESIAN_POINT ( 'NONE',  ( 117.0885360161528439, -37.77856303987432796, 29.74381011534493524 ) ) ;
#26523 = DIRECTION ( 'NONE',  ( -4.237773401492740281E-14, 1.000000000000000000, 0.000000000000000000 ) ) ;
#26522 = CARTESIAN_POINT ( 'NONE',  ( 99.08811452206278148, -33.58219759109908864, 277.6356252759111385 ) ) ;
#26524 = DIRECTION ( 'NONE',  ( -3.100000000000000258E-29, 3.100000000000000044E-14, 1.000000000000000000 ) ) ;
#26526 = EDGE_CURVE ( 'NONE', #36938, #13582, #23081, .T. ) ;
#26525 = DIRECTION ( 'NONE',  ( 1.000000000000000000, 4.299999999999999979E-14, 1.000000000000000078E-15 ) ) ;
#26527 = CIRCLE ( 'NONE', #6242, 32.50000000000001421 ) ;
#26528 = DIRECTION ( 'NONE',  ( 0.000000000000000000, 1.000000000000000000, 0.000000000000000000 ) ) ;
#26529 = DIRECTION ( 'NONE',  ( 0.7071067811571474238, 0.7071067812159476107, 0.000000000000000000 ) ) ;
#26530 = CARTESIAN_POINT ( 'NONE',  ( 99.09330906164119313, -30.55363432604262286, 40.80189661388796196 ) ) ;
#26531 = CARTESIAN_POINT ( 'NONE',  ( 113.2454987006837968, -28.75867294695902743, 75.55229194230558676 ) ) ;
#26532 = ADVANCED_FACE ( 'NONE', ( #63488 ), #7192, .F. ) ;
#26534 = ORIENTED_EDGE ( 'NONE', *, *, #13297, .F. ) ;
#26533 = CARTESIAN_POINT ( 'NONE',  ( 100.8523774812658900, -29.53301242784285563, 195.5838068554162135 ) ) ;
#26535 = DIRECTION ( 'NONE',  ( -0.000000000000000000, 1.000000000000000000, -0.000000000000000000 ) ) ;
#26536 = CARTESIAN_POINT ( 'NONE',  ( 98.82177599387378564, -29.33213395062421469, 235.7565776568629872 ) ) ;
#26537 = CARTESIAN_POINT ( 'NONE',  ( 111.0825168487035626, -25.58018305758348632, 95.80133956162495679 ) ) ;
#26538 = CARTESIAN_POINT ( 'NONE',  ( 99.50795136241276850, -29.43516104912357179, 246.7156252759109520 ) ) ;
#26539 = CARTESIAN_POINT ( 'NONE',  ( 106.5667039024470171, -94.77844715994206126, -19.78219314458232247 ) ) ;
#26540 = DIRECTION ( 'NONE',  ( 1.000000000000000000, 4.299999999999999979E-14, 1.000000000000000078E-15 ) ) ;
#26542 = CARTESIAN_POINT ( 'NONE',  ( 107.0667039024470313, -104.2784471599413791, 2.217806855418003043 ) ) ;
#26541 = DIRECTION ( 'NONE',  ( 0.000000000000000000, 0.4999999999999995004, -0.8660254037844390407 ) ) ;
#26543 = FACE_OUTER_BOUND ( 'NONE', #32893, .T. ) ;
#26544 = CARTESIAN_POINT ( 'NONE',  ( 131.7155263566516226, -20.16021090639161528, 2.608895778942307508 ) ) ;
#26545 = ORIENTED_EDGE ( 'NONE', *, *, #77466, .F. ) ;
#26546 = ORIENTED_EDGE ( 'NONE', *, *, #35732, .T. ) ;
#26547 = CARTESIAN_POINT ( 'NONE',  ( 115.2323353771322445, -31.47685829367418009, 143.7038483995059721 ) ) ;
#26549 = ORIENTED_EDGE ( 'NONE', *, *, #86670, .T. ) ;
#26548 = DIRECTION ( 'NONE',  ( 1.000000000000000000, -7.570719237730591757E-15, 0.000000000000000000 ) ) ;
#26550 = VECTOR ( 'NONE', #86452, 1000.000000000000114 ) ;
#26551 = LINE ( 'NONE', #25654, #27177 ) ;
#26552 = CARTESIAN_POINT ( 'NONE',  ( 99.70004787478436015, -45.98060041612298221, 118.0413395616259606 ) ) ;
#26553 = DIRECTION ( 'NONE',  ( 0.000000000000000000, 0.000000000000000000, -1.000000000000000000 ) ) ;
#26554 = CARTESIAN_POINT ( 'NONE',  ( 165.2748236753140247, -30.08671355700301575, -5.074374724088000832 ) ) ;
#26555 = CARTESIAN_POINT ( 'NONE',  ( 151.0667039024469886, -67.87844715994090450, 155.2178068554179902 ) ) ;
#26556 = DIRECTION ( 'NONE',  ( -3.100000000000000258E-29, 3.100000000000000044E-14, 1.000000000000000000 ) ) ;
#26557 = EDGE_CURVE ( 'NONE', #40401, #86883, #58939, .T. ) ;
#26558 = CARTESIAN_POINT ( 'NONE',  ( 97.58158007118568378, -32.53714515026960896, 55.98324432352996638 ) ) ;
#26559 = ORIENTED_EDGE ( 'NONE', *, *, #77893, .T. ) ;
#26560 = EDGE_LOOP ( 'NONE', ( #9479, #34759, #68245, #79405 ) ) ;
#26561 = ORIENTED_EDGE ( 'NONE', *, *, #6017, .F. ) ;
#26562 = VECTOR ( 'NONE', #24773, 999.9999999999998863 ) ;
#26563 = DIRECTION ( 'NONE',  ( -0.000000000000000000, -1.000000000000000000, -0.000000000000000000 ) ) ;
#26565 = DIRECTION ( 'NONE',  ( 0.7071067811865473507, 0.000000000000000000, -0.7071067811865476838 ) ) ;
#26564 = CARTESIAN_POINT ( 'NONE',  ( 97.98063455390173715, -41.72806076336409120, 172.7146728949579710 ) ) ;
#26566 = DIRECTION ( 'NONE',  ( 0.000000000000000000, 0.000000000000000000, 1.000000000000000000 ) ) ;
#26567 = CARTESIAN_POINT ( 'NONE',  ( 172.5664832912729878, -27.82844715994070484, 194.1756252759119832 ) ) ;
#26568 = LINE ( 'NONE', #47887, #43064 ) ;
#26569 = LINE ( 'NONE', #54694, #12967 ) ;
#26570 = DIRECTION ( 'NONE',  ( -0.7118375500353263385, -0.7021341844407537058, 0.01717234402817945094 ) ) ;
#26571 = CARTESIAN_POINT ( 'NONE',  ( 108.9812119692459049, -46.95502683147942236, 82.72419670448194040 ) ) ;
#26572 = VERTEX_POINT ( 'NONE', #16691 ) ;
#26573 = VERTEX_POINT ( 'NONE', #2620 ) ;
#26574 = VERTEX_POINT ( 'NONE', #24402 ) ;
#26575 = EDGE_CURVE ( 'NONE', #14882, #24211, #46407, .T. ) ;
#26576 = DIRECTION ( 'NONE',  ( 0.000000000000000000, 0.000000000000000000, 1.000000000000000000 ) ) ;
#26577 = CARTESIAN_POINT ( 'NONE',  ( 38.10000000000000142, 69.84999999999999432, 346.9005000000000223 ) ) ;
#26578 = CARTESIAN_POINT ( 'NONE',  ( -103.1875000000000000, 127.0000000000000000, -1.080832317973422076E-12 ) ) ;
#26579 = CARTESIAN_POINT ( 'NONE',  ( 104.4487311862825578, -28.48030787377049577, 203.1271379886389639 ) ) ;
#26581 = ADVANCED_FACE ( 'NONE', ( #66611 ), #65715, .T. ) ;
#26580 = AXIS2_PLACEMENT_3D ( 'NONE', #44495, #4065, #72227 ) ;
#26582 = AXIS2_PLACEMENT_3D ( 'NONE', #82728, #37, #83171 ) ;
#26583 = CARTESIAN_POINT ( 'NONE',  ( 49.65699999999999648, 82.54999999999999716, 358.0130000000000337 ) ) ;
#26584 = ORIENTED_EDGE ( 'NONE', *, *, #89380, .T. ) ;
#26586 = ORIENTED_EDGE ( 'NONE', *, *, #19670, .T. ) ;
#26585 = ORIENTED_EDGE ( 'NONE', *, *, #2430, .T. ) ;
#26587 = CARTESIAN_POINT ( 'NONE',  ( 80.06648329127399677, -8.729447159940999512, 308.6356252759119911 ) ) ;
#26588 = CARTESIAN_POINT ( 'NONE',  ( 144.1851062731161619, -138.0565978134347063, 247.6574394623689841 ) ) ;
#26589 = VERTEX_POINT ( 'NONE', #38901 ) ;
#26590 = ORIENTED_EDGE ( 'NONE', *, *, #43224, .T. ) ;
#26591 = CARTESIAN_POINT ( 'NONE',  ( 108.0667039024470455, -121.2010968907525239, -21.78219314458149114 ) ) ;
#26592 = CARTESIAN_POINT ( 'NONE',  ( 98.85146132857330770, -40.05235142642286661, 203.0644404487539703 ) ) ;
#26593 = DIRECTION ( 'NONE',  ( 1.000000000000000078E-15, -1.000000000000000083E-30, -1.000000000000000000 ) ) ;
#26594 = CARTESIAN_POINT ( 'NONE',  ( -109.2774118001975836, 54.68092463569039552, 71.43750000000027001 ) ) ;
#26595 = ORIENTED_EDGE ( 'NONE', *, *, #51403, .T. ) ;
#26596 = ORIENTED_EDGE ( 'NONE', *, *, #28995, .F. ) ;
#26597 = LINE ( 'NONE', #37675, #27513 ) ;
#26598 = VECTOR ( 'NONE', #81316, 1000.000000000000000 ) ;
#26599 = ORIENTED_EDGE ( 'NONE', *, *, #81399, .T. ) ;
#26600 = ORIENTED_EDGE ( 'NONE', *, *, #89227, .F. ) ;
#26601 = ADVANCED_FACE ( 'NONE', ( #9877 ), #45696, .T. ) ;
#26602 = ADVANCED_FACE ( 'NONE', ( #66157 ), #78927, .F. ) ;
#26603 = CARTESIAN_POINT ( 'NONE',  ( 104.9194883499490061, -28.34545421100826346, 243.1061856076869958 ) ) ;
#26605 = CARTESIAN_POINT ( 'NONE',  ( 96.67713595657845360, -37.82845849995531040, 126.4099109901969626 ) ) ;
#26604 = AXIS2_PLACEMENT_3D ( 'NONE', #45963, #60497, #66877 ) ;
#26606 = EDGE_CURVE ( 'NONE', #42662, #84235, #30323, .T. ) ;
#26607 = CARTESIAN_POINT ( 'NONE',  ( 97.64212626138829876, -32.24102647341085515, 75.97276813305397525 ) ) ;
#26608 = CARTESIAN_POINT ( 'NONE',  ( 114.1404429899671555, -42.27958953989512025, 249.5838068554168672 ) ) ;
#26609 = CARTESIAN_POINT ( 'NONE',  ( 131.3165190107488627, -18.55810522839977139, 6.749822759740949252 ) ) ;
#26610 = CARTESIAN_POINT ( 'NONE',  ( 105.8259002483207922, -25.33766151058717142, 321.6188579224977389 ) ) ;
#26611 = CARTESIAN_POINT ( 'NONE',  ( 96.19138854833354912, -32.02127024200479610, 207.0013395616249738 ) ) ;
#26612 = PLANE ( 'NONE',  #23388 ) ;
#26613 = ORIENTED_EDGE ( 'NONE', *, *, #65535, .T. ) ;
#26614 = CARTESIAN_POINT ( 'NONE',  ( 168.0371591254543944, -48.62818131005519717, 249.9678068554149775 ) ) ;
#26615 = ORIENTED_EDGE ( 'NONE', *, *, #86119, .T. ) ;
#26616 = EDGE_CURVE ( 'NONE', #73652, #27672, #17140, .T. ) ;
#26617 = VERTEX_POINT ( 'NONE', #44373 ) ;
#26618 = CARTESIAN_POINT ( 'NONE',  ( 71.24189083761808661, -0.9290567490904538817, 540.9756252759101471 ) ) ;
#26619 = VERTEX_POINT ( 'NONE', #23956 ) ;
#26620 = AXIS2_PLACEMENT_3D ( 'NONE', #33954, #89849, #5829 ) ;
#26621 = CARTESIAN_POINT ( 'NONE',  ( 53.06670390244699576, -67.87844715994100397, 55.21780685541800437 ) ) ;
#26622 = CARTESIAN_POINT ( 'NONE',  ( 193.0371591254586576, -47.82818131005411999, 129.9678068554150343 ) ) ;
#26623 = CARTESIAN_POINT ( 'NONE',  ( 117.8755673099929453, -39.04089478637848032, 108.6708633711489824 ) ) ;
#26624 = CARTESIAN_POINT ( 'NONE',  ( -12.31154164839621146, 79.32405795620842071, 129.9746777458391591 ) ) ;
#26625 = CARTESIAN_POINT ( 'NONE',  ( 136.7925547069167749, -36.36732994130177588, 6.785344856283919590 ) ) ;
#26626 = CARTESIAN_POINT ( 'NONE',  ( 150.5667039024476139, -25.42844715993593852, 129.9678068554149775 ) ) ;
#26629 = CARTESIAN_POINT ( 'NONE',  ( 100.6697571656888499, -44.93374849542860971, 228.0499109901969348 ) ) ;
#26628 = DIRECTION ( 'NONE',  ( 1.000000000000000000, 0.000000000000000000, 0.000000000000000000 ) ) ;
#26627 = CARTESIAN_POINT ( 'NONE',  ( 116.8171228667634125, -34.15291832121570792, 145.0314586091961928 ) ) ;
#26630 = CARTESIAN_POINT ( 'NONE',  ( 239.7378999999999962, 52.73749999999999716, 10.66800000000000104 ) ) ;
#26632 = ADVANCED_FACE ( 'NONE', ( #65284 ), #51633, .T. ) ;
#26631 = DIRECTION ( 'NONE',  ( 2.056463827196271584E-15, -0.8571673007021100021, 0.5150380749100580413 ) ) ;
#26633 = ORIENTED_EDGE ( 'NONE', *, *, #40750, .T. ) ;
#26634 = DIRECTION ( 'NONE',  ( 0.000000000000000000, 0.000000000000000000, 1.000000000000000000 ) ) ;
#26635 = LINE ( 'NONE', #19827, #47112 ) ;
#26636 = CYLINDRICAL_SURFACE ( 'NONE', #37179, 10.00000000000000355 ) ;
#26637 = DIRECTION ( 'NONE',  ( -1.000000000000000000, -3.999999999999999995E-14, -1.000000000000000078E-15 ) ) ;
#26639 = VERTEX_POINT ( 'NONE', #86628 ) ;
#26638 = CARTESIAN_POINT ( 'NONE',  ( 116.6462162596975389, -40.95264290462791479, 253.4956252759109532 ) ) ;
#26640 = CARTESIAN_POINT ( 'NONE',  ( 110.4848523211437339, -27.30132240271888122, 194.7993133264554046 ) ) ;
#26641 = CARTESIAN_POINT ( 'NONE',  ( 96.34427168469159142, -39.41376207380771746, 12.53372051400597442 ) ) ;
#26642 = CARTESIAN_POINT ( 'NONE',  ( 108.6553284749260229, -25.75107874774626993, 145.9737205140069420 ) ) ;
#26643 = CARTESIAN_POINT ( 'NONE',  ( 69.63919639214307722, 92.07499999999998863, 53.63573739454427880 ) ) ;
#26644 = CARTESIAN_POINT ( 'NONE',  ( 108.4175022753835691, -26.73504371419085501, 100.9690269479842613 ) ) ;
#26646 = DIRECTION ( 'NONE',  ( 0.000000000000000000, 0.000000000000000000, -1.000000000000000000 ) ) ;
#26645 = CARTESIAN_POINT ( 'NONE',  ( 77.06670390244701707, -90.27844715994098124, 51.21780685541800437 ) ) ;
#26647 = CARTESIAN_POINT ( 'NONE',  ( 0.000000000000000000, 1.270000000000000018, -9.425000000000000711 ) ) ;
#26648 = LINE ( 'NONE', #68445, #65592 ) ;
#26649 = VERTEX_POINT ( 'NONE', #44824 ) ;
#26650 = VECTOR ( 'NONE', #67972, 1000.000000000000000 ) ;
#26651 = AXIS2_PLACEMENT_3D ( 'NONE', #46811, #61348, #89077 ) ;
#26652 = ORIENTED_EDGE ( 'NONE', *, *, #85815, .T. ) ;
#26653 = VERTEX_POINT ( 'NONE', #72550 ) ;
#26654 = ORIENTED_EDGE ( 'NONE', *, *, #38191, .T. ) ;
#26655 = CARTESIAN_POINT ( 'NONE',  ( 172.5664832912740110, -9.303447159940999356, 261.0426252759119734 ) ) ;
#26656 = CARTESIAN_POINT ( 'NONE',  ( 99.14404768239424470, -44.40400490628089614, 37.95086337114900488 ) ) ;
#26657 = CARTESIAN_POINT ( 'NONE',  ( 77.10147176826316695, -139.5747906685508894, 247.4459311921649771 ) ) ;
#26658 = CARTESIAN_POINT ( 'NONE',  ( 162.5667039024460223, -19.82844715994111340, -5.074374724088000832 ) ) ;
#26659 = CARTESIAN_POINT ( 'NONE',  ( 131.0667039024480118, -67.87844715994100397, 207.5838068554149913 ) ) ;
#26660 = EDGE_CURVE ( 'NONE', #32398, #85160, #81825, .T. ) ;
#26661 = CARTESIAN_POINT ( 'NONE',  ( 111.5095219758393483, -44.62071306430618023, 257.4190864947434534 ) ) ;
#26662 = ORIENTED_EDGE ( 'NONE', *, *, #87246, .F. ) ;
#26663 = ORIENTED_EDGE ( 'NONE', *, *, #65372, .T. ) ;
#26664 = ORIENTED_EDGE ( 'NONE', *, *, #82457, .F. ) ;
#26665 = CIRCLE ( 'NONE', #78889, 118.5560000000000116 ) ;
#26666 = CARTESIAN_POINT ( 'NONE',  ( 128.2586590417343189, -60.54728653293321372, 361.9756252759100903 ) ) ;
#26667 = VECTOR ( 'NONE', #41613, 1000.000000000000000 ) ;
#26668 = CARTESIAN_POINT ( 'NONE',  ( 99.08985340457110169, -42.79589214074761117, 101.8442426276604493 ) ) ;
#26669 = EDGE_CURVE ( 'NONE', #14785, #56383, #83916, .T. ) ;
#26670 = CARTESIAN_POINT ( 'NONE',  ( 107.0664832912750057, -36.72944715993903486, 9.125625275910969947 ) ) ;
#26671 = CARTESIAN_POINT ( 'NONE',  ( 107.0664832912739399, -36.72944715994095333, 312.6356252759112522 ) ) ;
#26672 = CARTESIAN_POINT ( 'NONE',  ( 1.451892247740217613E-14, 95.25000000000000000, -118.5560000000000116 ) ) ;
#26673 = VECTOR ( 'NONE', #72924, 1000.000000000000000 ) ;
#26674 = DIRECTION ( 'NONE',  ( 1.000000000000000000, 0.000000000000000000, 0.000000000000000000 ) ) ;
#26675 = CARTESIAN_POINT ( 'NONE',  ( 104.9788083641148688, -27.14010996210884485, 260.2470538473402826 ) ) ;
#26676 = DIRECTION ( 'NONE',  ( -0.000000000000000000, -1.000000000000000000, -0.000000000000000000 ) ) ;
#26677 = ORIENTED_EDGE ( 'NONE', *, *, #87182, .F. ) ;
#26678 = CARTESIAN_POINT ( 'NONE',  ( 97.81168895331838087, -40.51742574516882200, 287.6356252759109680 ) ) ;
#26679 = CYLINDRICAL_SURFACE ( 'NONE', #10498, 3.000000000000002665 ) ;
#26680 = CARTESIAN_POINT ( 'NONE',  ( 114.2426363300227763, -32.83938885940727204, 67.03951894101994924 ) ) ;
#26681 = EDGE_CURVE ( 'NONE', #74344, #19571, #18915, .T. ) ;
#26682 = CARTESIAN_POINT ( 'NONE',  ( 97.79834864326036836, -40.48469191151001922, 131.6328120007984808 ) ) ;
#26683 = CARTESIAN_POINT ( 'NONE',  ( 57.14999999999999858, 95.25000000000000000, 280.2255000000000109 ) ) ;
#26684 = CARTESIAN_POINT ( 'NONE',  ( 97.81021718220807770, -40.51802218317752846, 192.6354414398782353 ) ) ;
#26685 = ORIENTED_EDGE ( 'NONE', *, *, #33713, .T. ) ;
#26686 = CARTESIAN_POINT ( 'NONE',  ( 78.15700282949505606, -34.74831852143766042, 7.618261863062902428 ) ) ;
#26687 = VERTEX_POINT ( 'NONE', #46601 ) ;
#26688 = CARTESIAN_POINT ( 'NONE',  ( 117.1261863205049423, -33.86823216992616636, 149.0470538473389581 ) ) ;
#26689 = VERTEX_POINT ( 'NONE', #60682 ) ;
#26690 = DIRECTION ( 'NONE',  ( 0.000000000000000000, 1.000000000000000000, 0.000000000000000000 ) ) ;
#26691 = CARTESIAN_POINT ( 'NONE',  ( 115.6883067454668463, -38.90345035940969609, 120.0615833058969457 ) ) ;
#26692 = LINE ( 'NONE', #81247, #56056 ) ;
#26693 = CYLINDRICAL_SURFACE ( 'NONE', #73039, 3.174999999999983391 ) ;
#26694 = CARTESIAN_POINT ( 'NONE',  ( 97.26802889450139844, -33.10625101732204456, 62.04419670448196911 ) ) ;
#26695 = CARTESIAN_POINT ( 'NONE',  ( 31.71315051185399270, -33.70561438052121161, 117.4678068554150485 ) ) ;
#26696 = CARTESIAN_POINT ( 'NONE',  ( 163.0664832912739826, 0.2215528400590083269, 333.4006252759110112 ) ) ;
#26697 = VERTEX_POINT ( 'NONE', #26622 ) ;
#26698 = DIRECTION ( 'NONE',  ( -0.000000000000000000, -0.000000000000000000, -1.000000000000000000 ) ) ;
#26699 = AXIS2_PLACEMENT_3D ( 'NONE', #41020, #68742, #78265 ) ;
#26700 = EDGE_LOOP ( 'NONE', ( #80219, #15632, #62351, #71980 ) ) ;
#26701 = ORIENTED_EDGE ( 'NONE', *, *, #77192, .T. ) ;
#26702 = EDGE_CURVE ( 'NONE', #87213, #63160, #5855, .T. ) ;
#26703 = DIRECTION ( 'NONE',  ( 0.000000000000000000, -1.000000000000000000, 0.000000000000000000 ) ) ;
#26704 = ORIENTED_EDGE ( 'NONE', *, *, #32436, .T. ) ;
#26705 = CARTESIAN_POINT ( 'NONE',  ( 107.4826147187165333, -46.50135945624624156, 237.6099109901969655 ) ) ;
#26706 = CARTESIAN_POINT ( 'NONE',  ( 114.5431187036783740, -28.56067750227894564, 150.4746728949579619 ) ) ;
#26707 = CARTESIAN_POINT ( 'NONE',  ( 10.09446275336743781, 74.79825716961998694, -118.1263904669630733 ) ) ;
#26708 = LINE ( 'NONE', #54842, #43108 ) ;
#26709 = EDGE_CURVE ( 'NONE', #25248, #74974, #79787, .T. ) ;
#26710 = CARTESIAN_POINT ( 'NONE',  ( 107.6031410145815528, -26.28275719304336633, 91.03562527591097364 ) ) ;
#26711 = CARTESIAN_POINT ( 'NONE',  ( 100.9563739204374855, -28.70569515775407510, 96.59303380014206653 ) ) ;
#26712 = ORIENTED_EDGE ( 'NONE', *, *, #82036, .T. ) ;
#26713 = DIRECTION ( 'NONE',  ( 0.7071067811868687603, 0.7071067811862262742, 7.071067811868681067E-16 ) ) ;
#26714 = EDGE_CURVE ( 'NONE', #55378, #13441, #71096, .T. ) ;
#26715 = CARTESIAN_POINT ( 'NONE',  ( 41.56648329127398966, -18.82844715994071194, 318.9256252759120116 ) ) ;
#26716 = EDGE_LOOP ( 'NONE', ( #29750, #69022 ) ) ;
#26717 = AXIS2_PLACEMENT_3D ( 'NONE', #30721, #71181, #39645 ) ;
#26718 = CARTESIAN_POINT ( 'NONE',  ( 34.92499999999999716, 73.38456447661469895, 302.8950000000000387 ) ) ;
#26719 = AXIS2_PLACEMENT_3D ( 'NONE', #70228, #43400, #78410 ) ;
#26720 = VECTOR ( 'NONE', #88672, 1000.000000000000000 ) ;
#26721 = DIRECTION ( 'NONE',  ( 0.000000000000000000, -0.000000000000000000, -1.000000000000000000 ) ) ;
#26722 = CARTESIAN_POINT ( 'NONE',  ( 100.0388059118472341, -29.01104360887432776, 285.6641967044823787 ) ) ;
#26723 = CARTESIAN_POINT ( 'NONE',  ( 34.27482367531500529, -30.08671355700301575, 342.9256252759119548 ) ) ;
#26724 = AXIS2_PLACEMENT_3D ( 'NONE', #43029, #57111, #30328 ) ;
#26725 = CARTESIAN_POINT ( 'NONE',  ( 69.30528942165814499, 92.51192757647309861, 54.77470860734664626 ) ) ;
#26726 = LINE ( 'NONE', #54409, #35991 ) ;
#26727 = CARTESIAN_POINT ( 'NONE',  ( 100.9534786964907482, -28.35269599622599301, 30.56610146638794134 ) ) ;
#26729 = CARTESIAN_POINT ( 'NONE',  ( 109.2504006710444173, -46.93703897017532967, 103.7441967044829880 ) ) ;
#26728 = DIRECTION ( 'NONE',  ( 0.000000000000000000, 0.000000000000000000, 1.000000000000000000 ) ) ;
#26730 = DIRECTION ( 'NONE',  ( 0.000000000000000000, 0.000000000000000000, -1.000000000000000000 ) ) ;
#26731 = CARTESIAN_POINT ( 'NONE',  ( 98.82181093208917844, -30.27703119756231942, 155.7984824187679465 ) ) ;
#26732 = VERTEX_POINT ( 'NONE', #54297 ) ;
#26734 = EDGE_CURVE ( 'NONE', #30196, #38484, #47042, .T. ) ;
#26733 = CARTESIAN_POINT ( 'NONE',  ( -446.0240000000000009, 104.7749999999999915, -1.387778780781445991E-14 ) ) ;
#26735 = ORIENTED_EDGE ( 'NONE', *, *, #71354, .T. ) ;
#26736 = DIRECTION ( 'NONE',  ( -3.100000000000000258E-29, 3.100000000000000044E-14, 1.000000000000000000 ) ) ;
#26737 = VECTOR ( 'NONE', #78830, 1000.000000000000000 ) ;
#26738 = AXIS2_PLACEMENT_3D ( 'NONE', #54121, #11928, #12834 ) ;
#26739 = PLANE ( 'NONE',  #60968 ) ;
#26740 = EDGE_CURVE ( 'NONE', #3336, #48583, #17450, .T. ) ;
#26741 = CARTESIAN_POINT ( 'NONE',  ( 136.4599941731065655, -35.37149686612711719, 2.653088969733340630 ) ) ;
#26742 = VERTEX_POINT ( 'NONE', #18459 ) ;
#26743 = CARTESIAN_POINT ( 'NONE',  ( 97.31571814629074879, -39.30557183317851155, 62.53186119129362908 ) ) ;
#26745 = ORIENTED_EDGE ( 'NONE', *, *, #56837, .T. ) ;
#26744 = CARTESIAN_POINT ( 'NONE',  ( 96.56283406263658264, -36.88802528585984675, 136.3384824187679385 ) ) ;
#26746 = CARTESIAN_POINT ( 'NONE',  ( 41.56648329127499153, -32.07844715994070839, 323.6756252759119548 ) ) ;
#26747 = CARTESIAN_POINT ( 'NONE',  ( -129.9681618895518795, 85.43248893795410481, 12.37548408773453623 ) ) ;
#26748 = DIRECTION ( 'NONE',  ( 0.000000000000000000, 1.000000000000000000, 0.000000000000000000 ) ) ;
#26749 = CARTESIAN_POINT ( 'NONE',  ( 107.0667039024470313, -104.2784471599412086, 7.717806855417980394 ) ) ;
#26750 = ORIENTED_EDGE ( 'NONE', *, *, #5196, .T. ) ;
#26751 = APPLICATION_PROTOCOL_DEFINITION ( 'draft international standard', 'automotive_design', 1998, #21423 ) ;
#26752 = ORIENTED_EDGE ( 'NONE', *, *, #33842, .T. ) ;
#26753 = ORIENTED_EDGE ( 'NONE', *, *, #12569, .T. ) ;
#26754 = EDGE_LOOP ( 'NONE', ( #28495, #84375, #31267, #86075 ) ) ;
#26755 = PLANE ( 'NONE',  #64137 ) ;
#26756 = CARTESIAN_POINT ( 'NONE',  ( 99.18048580889457355, 90.29814575435202073, -84.90178614994225370 ) ) ;
#26757 = CARTESIAN_POINT ( 'NONE',  ( 115.7831076504716634, -41.80230954540643040, 158.4064586060680995 ) ) ;
#26758 = DIRECTION ( 'NONE',  ( -0.9254794337955620787, -0.3787978585227822492, 0.000000000000000000 ) ) ;
#26760 = CARTESIAN_POINT ( 'NONE',  ( -12.27510648567648133, 79.26588701359587219, -117.9188774285743762 ) ) ;
#26759 = CARTESIAN_POINT ( 'NONE',  ( 80.06648329127402519, -46.72944715994105991, 8.225625275910942946 ) ) ;
#26761 = CARTESIAN_POINT ( 'NONE',  ( 97.81061268084424398, -40.51479618546458994, 181.6353987547717566 ) ) ;
#26762 = EDGE_CURVE ( 'NONE', #20160, #59338, #14685, .T. ) ;
#26763 = ORIENTED_EDGE ( 'NONE', *, *, #7536, .F. ) ;
#26764 = AXIS2_PLACEMENT_3D ( 'NONE', #24537, #52201, #45397 ) ;
#26765 = VERTEX_POINT ( 'NONE', #42353 ) ;
#26766 = DIRECTION ( 'NONE',  ( 4.299999999999999979E-14, -1.000000000000000000, 4.400000000000000367E-29 ) ) ;
#26767 = VECTOR ( 'NONE', #73440, 1000.000000000000000 ) ;
#26768 = DIRECTION ( 'NONE',  ( -4.237773401492740281E-14, 1.000000000000000000, 0.000000000000000000 ) ) ;
#26769 = EDGE_CURVE ( 'NONE', #7132, #78594, #82701, .T. ) ;
#26770 = CARTESIAN_POINT ( 'NONE',  ( 114.9950743857440756, -30.04541929558971702, 220.3718157521009573 ) ) ;
#26772 = ORIENTED_EDGE ( 'NONE', *, *, #85286, .F. ) ;
#26771 = FACE_OUTER_BOUND ( 'NONE', #86126, .T. ) ;
#26773 = CARTESIAN_POINT ( 'NONE',  ( 104.2906771502716055, -46.10805769451163627, 103.3470538473389411 ) ) ;
#26774 = CARTESIAN_POINT ( 'NONE',  ( 111.4697974980132642, -45.71384261549509631, 52.93909454086460187 ) ) ;
#26775 = CYLINDRICAL_SURFACE ( 'NONE', #60177, 12.70000000000000107 ) ;
#26776 = CARTESIAN_POINT ( 'NONE',  ( -487.2989999999999782, 100.8062500000000057, 94.61194598552329182 ) ) ;
#26777 = VERTEX_POINT ( 'NONE', #28752 ) ;
#26778 = LINE ( 'NONE', #27684, #26921 ) ;
#26779 = ORIENTED_EDGE ( 'NONE', *, *, #18893, .F. ) ;
#26780 = ORIENTED_EDGE ( 'NONE', *, *, #52510, .F. ) ;
#26781 = CARTESIAN_POINT ( 'NONE',  ( 97.77711562652216060, -35.32084007268648662, 217.6263452106589682 ) ) ;
#26782 = CIRCLE ( 'NONE', #61606, 31.75000000000000000 ) ;
#26783 = CARTESIAN_POINT ( 'NONE',  ( 98.04129441745654105, -41.04138963897023018, 52.68073796447941248 ) ) ;
#26784 = ADVANCED_FACE ( 'NONE', ( #46149 ), #43255, .T. ) ;
#26785 = CIRCLE ( 'NONE', #2110, 2.750000000000002665 ) ;
#26786 = CIRCLE ( 'NONE', #61608, 8.636000000000004562 ) ;
#26787 = CARTESIAN_POINT ( 'NONE',  ( -118.5560163110023808, 95.25015226514366873, -0.4098827902168798998 ) ) ;
#26788 = CIRCLE ( 'NONE', #13703, 0.5000000000000004441 ) ;
#26789 = DIRECTION ( 'NONE',  ( 0.000000000000000000, 0.000000000000000000, -1.000000000000000000 ) ) ;
#26790 = CARTESIAN_POINT ( 'NONE',  ( 82.81651833456541567, -36.90056224776740379, 3.101534470965026546 ) ) ;
#26791 = AXIS2_PLACEMENT_3D ( 'NONE', #5190, #67858, #61034 ) ;
#26792 = ORIENTED_EDGE ( 'NONE', *, *, #61627, .F. ) ;
#26793 = LINE ( 'NONE', #28583, #29039 ) ;
#26794 = VECTOR ( 'NONE', #83662, 1000.000000000000000 ) ;
#26795 = CARTESIAN_POINT ( 'NONE',  ( 97.81168895331838087, -40.51742574516882200, 287.6356252759109680 ) ) ;
#26796 = EDGE_LOOP ( 'NONE', ( #87390, #80934, #1812, #55235, #14835 ) ) ;
#26797 = CARTESIAN_POINT ( 'NONE',  ( 101.9604343285081569, -27.64015156285208974, 60.48419670448296159 ) ) ;
#26798 = ORIENTED_EDGE ( 'NONE', *, *, #64525, .F. ) ;
#26799 = CARTESIAN_POINT ( 'NONE',  ( 113.8860208566381544, -32.24350986527421981, 252.1080903695913662 ) ) ;
#26800 = EDGE_CURVE ( 'NONE', #75315, #17260, #71447, .T. ) ;
#26801 = DIRECTION ( 'NONE',  ( 0.000000000000000000, 1.000000000000000000, 6.056575390184510167E-15 ) ) ;
#26802 = CARTESIAN_POINT ( 'NONE',  ( 116.5042510202519708, -34.04512512578503447, 149.0470538473399529 ) ) ;
#26803 = CARTESIAN_POINT ( 'NONE',  ( 97.81670390244700286, -68.87844715994096134, 222.2178068554179902 ) ) ;
#26804 = FACE_OUTER_BOUND ( 'NONE', #59467, .T. ) ;
#26805 = CARTESIAN_POINT ( 'NONE',  ( 46.83715912545337545, -47.82818131006086304, 193.9678068554150911 ) ) ;
#26806 = DIRECTION ( 'NONE',  ( 0.000000000000000000, 0.000000000000000000, -1.000000000000000000 ) ) ;
#26807 = CARTESIAN_POINT ( 'NONE',  ( 98.86476787746175887, -29.25085353348518424, 226.7261014663869503 ) ) ;
#26808 = CARTESIAN_POINT ( 'NONE',  ( 193.0371591254572934, -23.42818131005412496, 249.9678068554149775 ) ) ;
#26809 = ORIENTED_EDGE ( 'NONE', *, *, #22981, .T. ) ;
#26810 = CARTESIAN_POINT ( 'NONE',  ( 97.58291127976856671, -32.21282489450084086, 71.97276813305397525 ) ) ;
#26811 = DIRECTION ( 'NONE',  ( -4.237773401492740281E-14, 1.000000000000000000, 0.000000000000000000 ) ) ;
#26812 = EDGE_CURVE ( 'NONE', #58138, #77202, #65064, .T. ) ;
#26813 = ORIENTED_EDGE ( 'NONE', *, *, #11337, .F. ) ;
#26814 = AXIS2_PLACEMENT_3D ( 'NONE', #89655, #19701, #81512 ) ;
#26815 = ORIENTED_EDGE ( 'NONE', *, *, #77509, .T. ) ;
#26816 = ORIENTED_EDGE ( 'NONE', *, *, #37400, .F. ) ;
#26817 = DIRECTION ( 'NONE',  ( 0.7071067811575828532, -0.7071067812155121812, 0.000000000000000000 ) ) ;
#26818 = CARTESIAN_POINT ( 'NONE',  ( 151.0667039024469886, -79.67844715994088745, 85.21780685541799016 ) ) ;
#26819 = DIRECTION ( 'NONE',  ( 0.000000000000000000, 0.000000000000000000, -1.000000000000000000 ) ) ;
#26820 = DIRECTION ( 'NONE',  ( 0.000000000000000000, 0.000000000000000000, -1.000000000000000000 ) ) ;
#26821 = ADVANCED_FACE ( 'NONE', ( #44147 ), #84183, .F. ) ;
#26822 = CARTESIAN_POINT ( 'NONE',  ( 98.33113000137380766, -33.60062404821446336, 173.8709475124489359 ) ) ;
#26823 = CARTESIAN_POINT ( 'NONE',  ( 101.0741685120301412, -45.28686133165523131, 278.0899109901965858 ) ) ;
#26824 = DIRECTION ( 'NONE',  ( 0.000000000000000000, -1.000000000000000000, 0.000000000000000000 ) ) ;
#26825 = ORIENTED_EDGE ( 'NONE', *, *, #11656, .T. ) ;
#26826 = CARTESIAN_POINT ( 'NONE',  ( 130.5461193570662601, 95.14808745951974345, 1.659440300508242760 ) ) ;
#26827 = DIRECTION ( 'NONE',  ( -0.000000000000000000, 1.000000000000000000, 0.000000000000000000 ) ) ;
#26828 = VERTEX_POINT ( 'NONE', #58244 ) ;
#26829 = ORIENTED_EDGE ( 'NONE', *, *, #25781, .F. ) ;
#26830 = AXIS2_PLACEMENT_3D ( 'NONE', #84518, #35429, #36343 ) ;
#26831 = DIRECTION ( 'NONE',  ( 0.000000000000000000, 0.000000000000000000, 1.000000000000000000 ) ) ;
#26832 = ORIENTED_EDGE ( 'NONE', *, *, #19541, .F. ) ;
#26833 = ORIENTED_EDGE ( 'NONE', *, *, #52348, .F. ) ;
#26834 = DIRECTION ( 'NONE',  ( 0.000000000000000000, -1.000000000000000000, 0.000000000000000000 ) ) ;
#26835 = VECTOR ( 'NONE', #67519, 999.9999999999998863 ) ;
#26836 = CARTESIAN_POINT ( 'NONE',  ( -1.668880554893940493, 69.93234144696143062, -130.5479136978233896 ) ) ;
#26837 = CARTESIAN_POINT ( 'NONE',  ( -492.0614999999999668, 93.66249999999999432, 95.25000000000000000 ) ) ;
#26838 = DIRECTION ( 'NONE',  ( 0.000000000000000000, 0.000000000000000000, -1.000000000000000000 ) ) ;
#26839 = CARTESIAN_POINT ( 'NONE',  ( 104.3962608544918993, -28.61612207615715775, 164.7524198280769667 ) ) ;
#26840 = CARTESIAN_POINT ( 'NONE',  ( 101.1165878437261227, -28.07204926635110098, 50.55562527591095545 ) ) ;
#26841 = EDGE_CURVE ( 'NONE', #43365, #2670, #2933, .T. ) ;
#26842 = VERTEX_POINT ( 'NONE', #1948 ) ;
#26843 = EDGE_CURVE ( 'NONE', #18276, #29468, #29209, .T. ) ;
#26844 = CARTESIAN_POINT ( 'NONE',  ( 184.5667039024483813, -48.82844715993448403, 249.9678068554149775 ) ) ;
#26845 = ORIENTED_EDGE ( 'NONE', *, *, #72456, .T. ) ;
#26846 = ADVANCED_FACE ( 'NONE', ( #29643 ), #22391, .F. ) ;
#26847 = DIRECTION ( 'NONE',  ( 0.7071067811865500152, -0.7071067811865451302, 1.287852911526284856E-16 ) ) ;
#26848 = VERTEX_POINT ( 'NONE', #22847 ) ;
#26849 = CARTESIAN_POINT ( 'NONE',  ( 173.9900000000000091, 21.46300000000000097, 59.96543552338529537 ) ) ;
#26850 = EDGE_CURVE ( 'NONE', #23101, #30005, #9648, .T. ) ;
#26851 = CARTESIAN_POINT ( 'NONE',  ( -6.662630065772598975, 71.84777277514653804, 118.3691311527337859 ) ) ;
#26852 = CARTESIAN_POINT ( 'NONE',  ( 110.8867401108072812, -45.97098272926901785, 132.8884009179573695 ) ) ;
#26854 = VECTOR ( 'NONE', #80200, 1000.000000000000000 ) ;
#26853 = DIRECTION ( 'NONE',  ( -0.000000000000000000, 1.000000000000000000, 0.000000000000000000 ) ) ;
#26855 = VERTEX_POINT ( 'NONE', #8770 ) ;
#26856 = CARTESIAN_POINT ( 'NONE',  ( 116.7655018478977951, -32.84674153052576884, 54.12991099019698282 ) ) ;
#26857 = CIRCLE ( 'NONE', #32620, 8.999999999999994671 ) ;
#26858 = CARTESIAN_POINT ( 'NONE',  ( 109.9229042994399492, -46.83780379245977343, 68.79562527591099297 ) ) ;
#26859 = VECTOR ( 'NONE', #81216, 1000.000000000000000 ) ;
#26860 = SURFACE_STYLE_FILL_AREA ( #32319 ) ;
#26861 = VECTOR ( 'NONE', #76423, 1000.000000000000000 ) ;
#26863 = CARTESIAN_POINT ( 'NONE',  ( 142.8698897858160706, -0.9167816978817300289, 394.9756252759102040 ) ) ;
#26862 = DIRECTION ( 'NONE',  ( 0.000000000000000000, 0.000000000000000000, 1.000000000000000000 ) ) ;
#26864 = FACE_OUTER_BOUND ( 'NONE', #66548, .T. ) ;
#26865 = CARTESIAN_POINT ( 'NONE',  ( -2.859109359865526390, 70.27181035201802217, 118.3221464644018255 ) ) ;
#26866 = ORIENTED_EDGE ( 'NONE', *, *, #20264, .F. ) ;
#26867 = VECTOR ( 'NONE', #74804, 1000.000000000000000 ) ;
#26868 = CARTESIAN_POINT ( 'NONE',  ( 107.0664832912739541, -36.72944715994095333, 309.2406250056037038 ) ) ;
#26869 = VECTOR ( 'NONE', #44705, 1000.000000000000000 ) ;
#26870 = CARTESIAN_POINT ( 'NONE',  ( -487.2989999999999782, 89.53805401447691281, 18.25625000000039933 ) ) ;
#26871 = LINE ( 'NONE', #13254, #41183 ) ;
#26872 = ORIENTED_EDGE ( 'NONE', *, *, #55739, .T. ) ;
#26873 = CARTESIAN_POINT ( 'NONE',  ( 117.3602503114455402, -32.64000144215158628, 95.13943479972097350 ) ) ;
#26875 = DIRECTION ( 'NONE',  ( -7.723290606088049820E-15, 0.000000000000000000, -1.000000000000000000 ) ) ;
#26874 = CARTESIAN_POINT ( 'NONE',  ( 97.92339844016763095, -40.78107841467939920, 171.6585333637830502 ) ) ;
#26876 = CARTESIAN_POINT ( 'NONE',  ( 28.57499999999999929, 91.71543552338529537, 302.8950000000000387 ) ) ;
#26877 = AXIS2_PLACEMENT_3D ( 'NONE', #627, #15165, #14725 ) ;
#26878 =( BOUNDED_CURVE ( )  B_SPLINE_CURVE ( 2, ( #66579, #17985, #4373 ),
 .UNSPECIFIED., .F., .F. ) 
 B_SPLINE_CURVE_WITH_KNOTS ( ( 3, 3 ),
 ( 0.01169420784674130021, 0.5170228498526558969 ),
 .UNSPECIFIED. ) 
 CURVE ( )  GEOMETRIC_REPRESENTATION_ITEM ( )  RATIONAL_B_SPLINE_CURVE ( ( 1.000420656333759872, 1.009299002520659849, 1.000000000000000000 ) ) 
 REPRESENTATION_ITEM ( '' )  );
#26879 = AXIS2_PLACEMENT_3D ( 'NONE', #16039, #41918, #28296 ) ;
#26880 = DIRECTION ( 'NONE',  ( 1.000000000000000000, 4.163336342344333240E-14, 0.000000000000000000 ) ) ;
#26881 = EDGE_LOOP ( 'NONE', ( #35819, #34796 ) ) ;
#26882 = EDGE_CURVE ( 'NONE', #36478, #33876, #16920, .T. ) ;
#26883 = CARTESIAN_POINT ( 'NONE',  ( 99.34849973496659459, -28.72665311504493246, 111.6870538473389587 ) ) ;
#26885 = ORIENTED_EDGE ( 'NONE', *, *, #24377, .F. ) ;
#26884 = CARTESIAN_POINT ( 'NONE',  ( 10.45076961392105908, 89.76615655770415003, 130.1370655302031025 ) ) ;
#26886 = CARTESIAN_POINT ( 'NONE',  ( 117.4695305279093986, -36.80206755349690440, 259.8213395616249386 ) ) ;
#26887 = CARTESIAN_POINT ( 'NONE',  ( 142.8698897858160706, -0.9167816978817300289, 542.9756252759101471 ) ) ;
#26888 = CARTESIAN_POINT ( 'NONE',  ( 111.2428885491283239, -45.81710051344609980, 147.9192755852553205 ) ) ;
#26889 = CARTESIAN_POINT ( 'NONE',  ( 0.000000000000000000, 127.0000000000000000, -103.1875000000000000 ) ) ;
#26890 = CARTESIAN_POINT ( 'NONE',  ( 116.3212776292293995, -32.94146857471265122, 80.13562527591095375 ) ) ;
#26891 = CARTESIAN_POINT ( 'NONE',  ( 114.2313622454167046, -107.8376143137176655, -19.78219314458190681 ) ) ;
#26892 = CARTESIAN_POINT ( 'NONE',  ( -100.0252357601321762, 76.93632333215533947, 83.90387289223399137 ) ) ;
#26893 = CARTESIAN_POINT ( 'NONE',  ( 117.1144258088630750, -31.97015794161411861, 214.1784824187679419 ) ) ;
#26894 = ORIENTED_EDGE ( 'NONE', *, *, #5793, .F. ) ;
#26895 = ORIENTED_EDGE ( 'NONE', *, *, #16649, .T. ) ;
#26896 = AXIS2_PLACEMENT_3D ( 'NONE', #62471, #42019, #69747 ) ;
#26897 = CARTESIAN_POINT ( 'NONE',  ( 103.0256836488564716, -28.24720316769774797, 136.8739642582779652 ) ) ;
#26898 = LINE ( 'NONE', #18745, #32692 ) ;
#26899 = EDGE_CURVE ( 'NONE', #34034, #752, #72580, .T. ) ;
#26901 = PLANE ( 'NONE',  #68037 ) ;
#26900 = CARTESIAN_POINT ( 'NONE',  ( 116.8470136369841725, -36.79772195930840439, 259.8213395616247681 ) ) ;
#26902 = AXIS2_PLACEMENT_3D ( 'NONE', #65850, #66750, #53084 ) ;
#26903 = CARTESIAN_POINT ( 'NONE',  ( 0.000000000000000000, 101.5999999999999943, 88.90000000000000568 ) ) ;
#26904 = EDGE_CURVE ( 'NONE', #52724, #28401, #23741, .T. ) ;
#26905 = DIRECTION ( 'NONE',  ( -1.000000000000000000, -1.000000000000000078E-15, 0.000000000000000000 ) ) ;
#26906 = EDGE_CURVE ( 'NONE', #86805, #81323, #88526, .T. ) ;
#26907 = DIRECTION ( 'NONE',  ( 1.000000000000000078E-15, -1.000000000000000083E-30, -1.000000000000000000 ) ) ;
#26908 = DIRECTION ( 'NONE',  ( 0.000000000000000000, 0.000000000000000000, -1.000000000000000000 ) ) ;
#26909 = CARTESIAN_POINT ( 'NONE',  ( 31.71315051186735801, -31.94127993907786589, 193.9678068554150911 ) ) ;
#26910 = CARTESIAN_POINT ( 'NONE',  ( 104.4591861284129948, -26.65816784528755790, 200.2784824187679362 ) ) ;
#26911 = DIRECTION ( 'NONE',  ( 0.9254794337955621897, 0.3787978585227821382, 0.000000000000000000 ) ) ;
#26912 = ORIENTED_EDGE ( 'NONE', *, *, #53723, .F. ) ;
#26913 = ORIENTED_EDGE ( 'NONE', *, *, #348, .F. ) ;
#26914 = EDGE_CURVE ( 'NONE', #87649, #31858, #60950, .T. ) ;
#26915 = EDGE_CURVE ( 'NONE', #39062, #62015, #72332, .T. ) ;
#26916 = CARTESIAN_POINT ( 'NONE',  ( -100.8594679592207086, 81.71102547120852932, -82.89895571708335353 ) ) ;
#26917 = CARTESIAN_POINT ( 'NONE',  ( 81.91398979885782694, -20.77444411302980853, 7.664507283826766049 ) ) ;
#26918 = CARTESIAN_POINT ( 'NONE',  ( 117.0715937733379093, -35.45994745709830198, 124.9267458150729482 ) ) ;
#26919 = CARTESIAN_POINT ( 'NONE',  ( -47.11752803141010304, 65.68786680169236547, 108.7909173056707317 ) ) ;
#26920 = ADVANCED_FACE ( 'NONE', ( #78268 ), #37809, .T. ) ;
#26922 = DIRECTION ( 'NONE',  ( -3.100000000000000258E-29, 3.100000000000000044E-14, 1.000000000000000000 ) ) ;
#26921 = VECTOR ( 'NONE', #54463, 1000.000000000000000 ) ;
#26923 = ADVANCED_FACE ( 'NONE', ( #2397 ), #21956, .T. ) ;
#26924 = ORIENTED_EDGE ( 'NONE', *, *, #62520, .T. ) ;
#26925 = AXIS2_PLACEMENT_3D ( 'NONE', #71491, #64654, #8359 ) ;
#26926 = CARTESIAN_POINT ( 'NONE',  ( -12.51814195203456137, 84.20263175503735908, 117.6922463100763423 ) ) ;
#26927 = AXIS2_PLACEMENT_3D ( 'NONE', #57394, #85137, #57847 ) ;
#26928 = AXIS2_PLACEMENT_3D ( 'NONE', #29523, #36337, #16341 ) ;
#26929 = EDGE_CURVE ( 'NONE', #36112, #26158, #23309, .T. ) ;
#26930 = CARTESIAN_POINT ( 'NONE',  ( 106.8516092256838306, -47.78082339050276772, 227.5489586092439538 ) ) ;
#26931 = VERTEX_POINT ( 'NONE', #45925 ) ;
#26932 = VECTOR ( 'NONE', #50669, 1000.000000000000000 ) ;
#26933 = FACE_OUTER_BOUND ( 'NONE', #17118, .T. ) ;
#26934 = ADVANCED_FACE ( 'NONE', ( #11894 ), #46826, .F. ) ;
#26935 = CARTESIAN_POINT ( 'NONE',  ( 21.03689327557615130, -23.42844715994197813, 180.4678068554150911 ) ) ;
#26936 = CARTESIAN_POINT ( 'NONE',  ( 156.5667039024485518, -48.82844715993568485, 173.2178068554149775 ) ) ;
#26937 = EDGE_CURVE ( 'NONE', #80043, #5970, #66780, .T. ) ;
#26938 = CARTESIAN_POINT ( 'NONE',  ( 101.1433531317129280, -42.34605246296819558, 79.74809036959096886 ) ) ;
#26940 = AXIS2_PLACEMENT_3D ( 'NONE', #31910, #9692, #3330 ) ;
#26939 = CARTESIAN_POINT ( 'NONE',  ( 117.5090302172161500, -40.42247023647522752, 174.5680062282919778 ) ) ;
#26941 = LINE ( 'NONE', #19676, #37758 ) ;
#26942 = EDGE_LOOP ( 'NONE', ( #32719, #11617, #60551 ) ) ;
#26943 = CIRCLE ( 'NONE', #6656, 10.04999999999999361 ) ;
#26944 = CARTESIAN_POINT ( 'NONE',  ( 30.00000000000001776, 127.0000000000000000, 113.8826257785461280 ) ) ;
#26945 = CARTESIAN_POINT ( 'NONE',  ( 112.9065472848678127, -44.95407874994433683, 68.06887155916673748 ) ) ;
#26946 = EDGE_LOOP ( 'NONE', ( #18649, #24569, #8024, #53072 ) ) ;
#26947 = VERTEX_POINT ( 'NONE', #74113 ) ;
#26948 = DIRECTION ( 'NONE',  ( -0.000000000000000000, 1.000000000000000000, 0.000000000000000000 ) ) ;
#26949 = ORIENTED_EDGE ( 'NONE', *, *, #56646, .T. ) ;
#26950 = ORIENTED_EDGE ( 'NONE', *, *, #71550, .F. ) ;
#26951 = DIRECTION ( 'NONE',  ( 0.000000000000000000, 0.000000000000000000, 1.000000000000000000 ) ) ;
#26952 = AXIS2_PLACEMENT_3D ( 'NONE', #60939, #25525, #24634 ) ;
#26953 = CARTESIAN_POINT ( 'NONE',  ( 109.7600704110825802, -27.40125247274746556, 64.27527697093398729 ) ) ;
#26954 = CARTESIAN_POINT ( 'NONE',  ( 98.82177599387378564, -29.33213395062421469, 235.7565776568629872 ) ) ;
#26955 = EDGE_CURVE ( 'NONE', #8825, #43693, #59564, .T. ) ;
#26956 = CARTESIAN_POINT ( 'NONE',  ( 113.0874441278155871, -45.97130050132146550, 223.0480062282919675 ) ) ;
#26959 = ADVANCED_FACE ( 'NONE', ( #25510 ), #51850, .F. ) ;
#26958 = CARTESIAN_POINT ( 'NONE',  ( 116.7496603916996207, -31.44741115753631178, 20.21181575210195902 ) ) ;
#26957 = CARTESIAN_POINT ( 'NONE',  ( 71.06648329127310149, -18.82844715994099971, 81.92562527591198318 ) ) ;
#26960 = CARTESIAN_POINT ( 'NONE',  ( 25.56670390244797275, -65.37844715994100397, 132.3428068554150343 ) ) ;
#26961 = CARTESIAN_POINT ( 'NONE',  ( 117.0724591054688517, -35.46716173184821486, 94.92691977030953865 ) ) ;
#26962 = ADVANCED_FACE ( 'NONE', ( #32772 ), #52728, .F. ) ;
#26963 = VERTEX_POINT ( 'NONE', #81405 ) ;
#26964 = ORIENTED_EDGE ( 'NONE', *, *, #83725, .T. ) ;
#26965 = EDGE_CURVE ( 'NONE', #64372, #62172, #23313, .T. ) ;
#26966 = CARTESIAN_POINT ( 'NONE',  ( 99.11394507416765975, -43.38496525699394368, 71.86895860924497015 ) ) ;
#26967 = CARTESIAN_POINT ( 'NONE',  ( 100.2700262342886219, -46.49863182355969116, 87.09276813305393716 ) ) ;
#26968 = CARTESIAN_POINT ( 'NONE',  ( 96.93601811142059432, -39.37148068186442629, 276.5299109901966403 ) ) ;
#26969 = ORIENTED_EDGE ( 'NONE', *, *, #70421, .T. ) ;
#26970 = CARTESIAN_POINT ( 'NONE',  ( 109.3585227812971539, -25.91623105973918939, 184.9222919425779708 ) ) ;
#26971 = CARTESIAN_POINT ( 'NONE',  ( 109.7248658851862047, -27.00080516916434092, 34.86479194556028460 ) ) ;
#26972 = CIRCLE ( 'NONE', #66118, 2.117000000000000881 ) ;
#26973 = CYLINDRICAL_SURFACE ( 'NONE', #23333, 2.750000000000002665 ) ;
#26974 = CARTESIAN_POINT ( 'NONE',  ( 20.03715912545732891, -24.95799193693189721, 300.4678068554150059 ) ) ;
#26975 = DIRECTION ( 'NONE',  ( 1.000000000000000000, 4.272717921125146745E-14, 0.000000000000000000 ) ) ;
#26977 = CARTESIAN_POINT ( 'NONE',  ( 107.0664832912739399, -36.72944715994095333, 315.1356252759112522 ) ) ;
#26976 = CARTESIAN_POINT ( 'NONE',  ( 109.6970437850230979, -45.56375468492142744, 277.6356252759109680 ) ) ;
#26978 = CARTESIAN_POINT ( 'NONE',  ( 75.61066417432020614, 0.000000000000000000, 177.0380000000000109 ) ) ;
#26979 = CARTESIAN_POINT ( 'NONE',  ( 0.000000000000000000, 92.07499999999998863, 87.89999999999994884 ) ) ;
#26980 = DIRECTION ( 'NONE',  ( -1.000000000000000078E-15, 1.000000000000000083E-30, 1.000000000000000000 ) ) ;
#26981 = DIRECTION ( 'NONE',  ( 0.000000000000000000, 0.000000000000000000, -1.000000000000000000 ) ) ;
#26982 = CARTESIAN_POINT ( 'NONE',  ( 100.9507452397097467, -28.71010058181673230, 40.59361269664083949 ) ) ;
#26983 = CARTESIAN_POINT ( 'NONE',  ( 115.0889047249108614, -30.61763668143413497, 75.34395860910829867 ) ) ;
#26985 = EDGE_LOOP ( 'NONE', ( #18079, #38546 ) ) ;
#26984 = CARTESIAN_POINT ( 'NONE',  ( -6.350224805574129938, 93.55624312175208956, -118.3863781049609685 ) ) ;
#26986 = CARTESIAN_POINT ( 'NONE',  ( 32.25690895537100289, -33.54226604285010893, -5.074374724088000832 ) ) ;
#26987 = CARTESIAN_POINT ( 'NONE',  ( 107.2496247454619152, -24.85508506706595000, 230.0641967044819580 ) ) ;
#26988 = CARTESIAN_POINT ( 'NONE',  ( 97.83606632657298974, -31.88363555591887533, 131.9413395616259947 ) ) ;
#26989 = CARTESIAN_POINT ( 'NONE',  ( 110.9086127847465377, -26.95314644129561543, 265.7784824187680783 ) ) ;
#26990 = CARTESIAN_POINT ( 'NONE',  ( 25.56670390244797275, -58.35344715994099829, 257.2178068554150059 ) ) ;
#26991 = AXIS2_PLACEMENT_3D ( 'NONE', #58973, #66238, #51265 ) ;
#26992 = CARTESIAN_POINT ( 'NONE',  ( 194.5667039024483529, -47.82844715993405771, 249.9678068554149775 ) ) ;
#26994 = FACE_OUTER_BOUND ( 'NONE', #30845, .T. ) ;
#26993 = DIRECTION ( 'NONE',  ( 1.000000000000000000, 0.000000000000000000, 0.000000000000000000 ) ) ;
#26995 = DIRECTION ( 'NONE',  ( 0.7071067811989671936, 0.7071067811741279519, 6.612322855971028274E-17 ) ) ;
#26996 = DIRECTION ( 'NONE',  ( -3.062684205862500216E-15, 0.000000000000000000, 1.000000000000000000 ) ) ;
#26997 = VECTOR ( 'NONE', #40082, 1000.000000000000000 ) ;
#26998 = AXIS2_PLACEMENT_3D ( 'NONE', #10542, #24184, #58245 ) ;
#26999 = VECTOR ( 'NONE', #66898, 1000.000000000000000 ) ;
#27000 = ORIENTED_EDGE ( 'NONE', *, *, #55187, .F. ) ;
#27001 = VERTEX_POINT ( 'NONE', #5069 ) ;
#27002 = CARTESIAN_POINT ( 'NONE',  ( 103.2375202873391800, -28.52263824056898756, 134.8343245899819465 ) ) ;
#27004 = ORIENTED_EDGE ( 'NONE', *, *, #41697, .T. ) ;
#27003 = DIRECTION ( 'NONE',  ( 0.000000000000000000, 0.000000000000000000, -1.000000000000000000 ) ) ;
#27005 = CARTESIAN_POINT ( 'NONE',  ( 150.5667039024485234, -47.82844715993594065, 180.4678068554149775 ) ) ;
#27006 = CARTESIAN_POINT ( 'NONE',  ( 109.5033840998383994, -46.84330794493973826, 128.7641967044819751 ) ) ;
#27007 = CARTESIAN_POINT ( 'NONE',  ( 100.8868115320050549, -44.69967795324804882, 148.0528215568805308 ) ) ;
#27008 = CARTESIAN_POINT ( 'NONE',  ( 1.387778780781445676E-14, 184.0000000000000000, 90.07542076772557493 ) ) ;
#27009 = DIRECTION ( 'NONE',  ( 1.000000000000000000, 3.999999999999999995E-14, 1.000000000000000078E-15 ) ) ;
#27010 = CARTESIAN_POINT ( 'NONE',  ( 83.06670390244796920, -61.87844715994100397, 231.5838068554150198 ) ) ;
#27012 = CARTESIAN_POINT ( 'NONE',  ( 112.3909220325769667, -27.83061929752856400, 54.65943479972096242 ) ) ;
#27011 = VECTOR ( 'NONE', #76628, 1000.000000000000000 ) ;
#27013 = ORIENTED_EDGE ( 'NONE', *, *, #64063, .T. ) ;
#27014 = VERTEX_POINT ( 'NONE', #24183 ) ;
#27015 = ORIENTED_EDGE ( 'NONE', *, *, #47530, .F. ) ;
#27016 = LINE ( 'NONE', #82450, #54449 ) ;
#27018 = DIRECTION ( 'NONE',  ( 0.1250000000000000278, 0.9921567416492215186, -3.035766082959410522E-14 ) ) ;
#27017 = CARTESIAN_POINT ( 'NONE',  ( 116.6093774848465472, -38.87601340171671893, 144.6499109901959628 ) ) ;
#27019 = CIRCLE ( 'NONE', #5296, 2.116999999999980009 ) ;
#27020 = LINE ( 'NONE', #74280, #61000 ) ;
#27021 = EDGE_CURVE ( 'NONE', #76097, #26390, #66386, .T. ) ;
#27022 = FACE_OUTER_BOUND ( 'NONE', #21892, .T. ) ;
#27023 = EDGE_CURVE ( 'NONE', #1162, #51892, #53178, .T. ) ;
#27024 = CARTESIAN_POINT ( 'NONE',  ( 122.2221484686747459, -111.8737466215628729, -21.78219314458179667 ) ) ;
#27025 = EDGE_CURVE ( 'NONE', #15206, #51994, #55705, .T. ) ;
#27026 = LINE ( 'NONE', #67010, #30348 ) ;
#27027 = DIRECTION ( 'NONE',  ( 6.524622321627019585E-16, 3.741823817616790462E-31, 1.000000000000000000 ) ) ;
#27028 = CARTESIAN_POINT ( 'NONE',  ( 113.4926247784321021, -28.54816540729036589, 79.54705384733995288 ) ) ;
#27029 = ORIENTED_EDGE ( 'NONE', *, *, #55501, .T. ) ;
#27030 = VERTEX_POINT ( 'NONE', #41807 ) ;
#27031 = ORIENTED_EDGE ( 'NONE', *, *, #82115, .T. ) ;
#27032 = EDGE_CURVE ( 'NONE', #30851, #37640, #7319, .T. ) ;
#27033 = DIRECTION ( 'NONE',  ( -1.000000000000000000, -4.299999999999999979E-14, -1.000000000000000078E-15 ) ) ;
#27034 = DIRECTION ( 'NONE',  ( 0.000000000000000000, 0.000000000000000000, -1.000000000000000000 ) ) ;
#27035 = DIRECTION ( 'NONE',  ( 1.000000000000000000, 0.000000000000000000, 0.000000000000000000 ) ) ;
#27036 = CARTESIAN_POINT ( 'NONE',  ( 110.4730825863185260, -45.36026475776040456, 170.6938046553059678 ) ) ;
#27037 = EDGE_CURVE ( 'NONE', #16242, #23402, #13237, .T. ) ;
#27038 = CARTESIAN_POINT ( 'NONE',  ( 37.35959712141614375, -48.62134037890901084, 300.4678068554150059 ) ) ;
#27039 = ORIENTED_EDGE ( 'NONE', *, *, #40460, .F. ) ;
#27041 = ORIENTED_EDGE ( 'NONE', *, *, #69440, .T. ) ;
#27040 = EDGE_LOOP ( 'NONE', ( #76642, #81011 ) ) ;
#27042 = CARTESIAN_POINT ( 'NONE',  ( 131.0667039024480118, -64.87844715994098976, 213.1838068554149856 ) ) ;
#27043 = CARTESIAN_POINT ( 'NONE',  ( 136.6734006051289612, -19.60624470235256567, 2.902100967938342269 ) ) ;
#27044 = ORIENTED_EDGE ( 'NONE', *, *, #15866, .T. ) ;
#27045 = EDGE_LOOP ( 'NONE', ( #55891, #24515, #43715, #8853 ) ) ;
#27046 = DIRECTION ( 'NONE',  ( -0.7071067812163264188, 0.7071067811567686157, -7.071067812162960697E-16 ) ) ;
#27047 = B_SPLINE_CURVE_WITH_KNOTS ( 'NONE', 3,
 ( #32983, #60680, #82061, #67959, #81617, #5746, #56095, #84304, #37806, #76572, #21619, #65505, #30542, #21161, #77026, #14353, #58242, #86411, #48380, #23307, #10100, #37353, #69758, #9646, #58667, #3288, #83844, #7528, #13892, #56561, #28408, #85970, #27961, #55639, #2844, #62926, #78715, #34779, #48832, #23739, #14804, #51405, #49294, #50974, #65062, #79158, #704, #16918, #72330 ),
 .UNSPECIFIED., .F., .F.,
 ( 4, 2, 1, 1, 1, 1, 2, 2, 2, 2, 2, 2, 2, 1, 1, 1, 1, 1, 1, 1, 2, 2, 2, 2, 2, 2, 2, 2, 2, 4 ),
 ( 0.5000151141236341967, 0.5005033806137728636, 0.5009916471039114194, 0.5019681800841889752, 0.5039212460447435316, 0.5078273779658523113, 0.5156396418080697597, 0.5312641694925048785, 0.5625132248613745611, 0.6250113355991141484, 0.6875094463368538467, 0.7500075570745934339, 0.7500685903858610448, 0.7501296236971285447, 0.7502516903196607689, 0.7504958235647252174, 0.7509840900548254705, 0.7519606230349995535, 0.7539136889953474974, 0.7578198209160560417, 0.7656320847574735744, 0.7812566124403086398, 0.8125056678059787707, 0.8437547231716489016, 0.8750037785373191435, 0.9062528339029893854, 0.9375018892686595162, 0.9687509446343296471, 0.9843754723171647125, 1.000000000000000000 ),
 .UNSPECIFIED. ) ;
#27048 = EDGE_CURVE ( 'NONE', #37074, #28060, #69720, .T. ) ;
#27049 = CARTESIAN_POINT ( 'NONE',  ( 99.81674604704261355, -31.63341061165540680, 202.2701547344679796 ) ) ;
#27050 = CIRCLE ( 'NONE', #73465, 3.999999999999998224 ) ;
#27051 = CARTESIAN_POINT ( 'NONE',  ( 142.8821648370248170, -72.54478064608022692, 542.9756252759101471 ) ) ;
#27052 = EDGE_CURVE ( 'NONE', #68551, #50389, #50, .T. ) ;
#27053 = CARTESIAN_POINT ( 'NONE',  ( -114.6380061954168923, 70.99355617351733372, 62.47401523881796948 ) ) ;
#27054 = VECTOR ( 'NONE', #28242, 1000.000000000000000 ) ;
#27055 = ORIENTED_EDGE ( 'NONE', *, *, #46600, .F. ) ;
#27056 = ORIENTED_EDGE ( 'NONE', *, *, #65981, .F. ) ;
#27057 = VECTOR ( 'NONE', #16922, 1000.000000000000000 ) ;
#27058 = AXIS2_PLACEMENT_3D ( 'NONE', #61095, #26140, #12512 ) ;
#27059 = DIRECTION ( 'NONE',  ( 0.000000000000000000, 0.000000000000000000, 1.000000000000000000 ) ) ;
#27060 = EDGE_LOOP ( 'NONE', ( #83538, #87104, #7967, #75191 ) ) ;
#27061 = ORIENTED_EDGE ( 'NONE', *, *, #81598, .T. ) ;
#27062 = CARTESIAN_POINT ( 'NONE',  ( 104.9869425053901892, -28.32846893322983917, 238.0757094172099642 ) ) ;
#27063 = CARTESIAN_POINT ( 'NONE',  ( 100.8733315758915552, -45.91070206092880568, 152.0918157521009562 ) ) ;
#27064 = CARTESIAN_POINT ( 'NONE',  ( 98.22092589535427010, -43.31882777834842813, 111.8480062282919647 ) ) ;
#27065 = CARTESIAN_POINT ( 'NONE',  ( 108.4649749756400183, -27.96694839443428293, 249.5838068554169524 ) ) ;
#27066 = CARTESIAN_POINT ( 'NONE',  ( 147.0667039024469886, -67.87844715994090450, 247.2178068554179902 ) ) ;
#27067 = CARTESIAN_POINT ( 'NONE',  ( 103.7231914492017637, -26.19396519929847145, 201.3089586092439731 ) ) ;
#27068 = CARTESIAN_POINT ( 'NONE',  ( 98.20858259865026696, -41.48711566647967430, 276.7185663392993433 ) ) ;
#27069 = VERTEX_POINT ( 'NONE', #33226 ) ;
#27070 = CARTESIAN_POINT ( 'NONE',  ( -130.0003553321326990, 78.46683822717000112, 12.03293382262464206 ) ) ;
#27071 = ORIENTED_EDGE ( 'NONE', *, *, #19328, .T. ) ;
#27072 = ORIENTED_EDGE ( 'NONE', *, *, #17586, .F. ) ;
#27073 = DIRECTION ( 'NONE',  ( 1.000000000000000078E-15, -1.000000000000000000, 0.000000000000000000 ) ) ;
#27074 = EDGE_CURVE ( 'NONE', #40366, #34574, #54976, .T. ) ;
#27075 = VECTOR ( 'NONE', #57320, 1000.000000000000000 ) ;
#27076 = ORIENTED_EDGE ( 'NONE', *, *, #55792, .T. ) ;
#27077 = DIRECTION ( 'NONE',  ( 0.000000000000000000, 0.000000000000000000, -1.000000000000000000 ) ) ;
#27078 = AXIS2_PLACEMENT_3D ( 'NONE', #26618, #54743, #52935 ) ;
#27079 = CARTESIAN_POINT ( 'NONE',  ( 114.0222564360173720, -28.96386602133403798, 114.4956252759109816 ) ) ;
#27080 = CARTESIAN_POINT ( 'NONE',  ( -7.291605166176498010, 72.14803965971481148, 130.3524295837840725 ) ) ;
#27081 = CARTESIAN_POINT ( 'NONE',  ( 105.4788588808464027, 127.0000000000000000, 3.968750000000405009 ) ) ;
#27082 = DIRECTION ( 'NONE',  ( 0.000000000000000000, 0.000000000000000000, -1.000000000000000000 ) ) ;
#27085 = CARTESIAN_POINT ( 'NONE',  ( 117.2062538965839309, -41.07097622818925942, 209.5165776568640013 ) ) ;
#27084 = CARTESIAN_POINT ( 'NONE',  ( 28.57499999999999929, 82.54999999999999716, 302.8950000000000387 ) ) ;
#27083 = CARTESIAN_POINT ( 'NONE',  ( 33.98325472291465132, 8.255000000000000782, 3.174999999999999822 ) ) ;
#27086 = DIRECTION ( 'NONE',  ( 0.000000000000000000, 0.000000000000000000, 1.000000000000000000 ) ) ;
#27087 = CYLINDRICAL_SURFACE ( 'NONE', #11945, 3.500000000000003109 ) ;
#27088 = ORIENTED_EDGE ( 'NONE', *, *, #73838, .T. ) ;
#27089 = DIRECTION ( 'NONE',  ( 0.7071067811861589947, -0.7071067811869361508, 0.000000000000000000 ) ) ;
#27090 = FACE_OUTER_BOUND ( 'NONE', #69040, .T. ) ;
#27091 = CARTESIAN_POINT ( 'NONE',  ( 151.0371591254575776, -24.42818131005592264, 117.4678068554150485 ) ) ;
#27092 = DIRECTION ( 'NONE',  ( 4.299999999999999979E-14, -1.000000000000000000, 4.400000000000000367E-29 ) ) ;
#27093 = EDGE_CURVE ( 'NONE', #18383, #23728, #82294, .T. ) ;
#27095 = ORIENTED_EDGE ( 'NONE', *, *, #35099, .F. ) ;
#27094 = CARTESIAN_POINT ( 'NONE',  ( 97.51966259852430596, -43.83486848311488160, 261.8356252759109566 ) ) ;
#27096 = DIRECTION ( 'NONE',  ( 0.000000000000000000, 0.000000000000000000, 1.000000000000000000 ) ) ;
#27097 = CARTESIAN_POINT ( 'NONE',  ( 102.2921677216391174, -27.39701587636625391, 120.4527681330539792 ) ) ;
#27098 = CARTESIAN_POINT ( 'NONE',  ( 95.20664489286731680, -37.33482625718801273, 267.3670538473395482 ) ) ;
#27099 = CARTESIAN_POINT ( 'NONE',  ( 100.8606736390591720, -45.92946726319084405, 148.0918157521009562 ) ) ;
#27100 = FACE_OUTER_BOUND ( 'NONE', #37064, .T. ) ;
#27101 = LINE ( 'NONE', #81640, #89547 ) ;
#27103 = FACE_OUTER_BOUND ( 'NONE', #36524, .T. ) ;
#27102 = FACE_OUTER_BOUND ( 'NONE', #63378, .T. ) ;
#27104 = CARTESIAN_POINT ( 'NONE',  ( 97.07207207411279626, -35.37844109237227741, 191.2189586007484934 ) ) ;
#27105 = DIRECTION ( 'NONE',  ( -0.7071067811864693020, -0.7071067811866258435, 2.899137802865049595E-29 ) ) ;
#27106 = ORIENTED_EDGE ( 'NONE', *, *, #2860, .T. ) ;
#27107 = AXIS2_PLACEMENT_3D ( 'NONE', #88989, #14484, #54428 ) ;
#27108 = EDGE_CURVE ( 'NONE', #59214, #17803, #30547, .T. ) ;
#27109 = ORIENTED_EDGE ( 'NONE', *, *, #45076, .T. ) ;
#27110 = ORIENTED_EDGE ( 'NONE', *, *, #26904, .F. ) ;
#27111 = ORIENTED_EDGE ( 'NONE', *, *, #50507, .T. ) ;
#27112 = LINE ( 'NONE', #47979, #39489 ) ;
#27113 = CARTESIAN_POINT ( 'NONE',  ( 112.1067112481348431, -26.91823048478340397, 15.71086337114896381 ) ) ;
#27114 = CARTESIAN_POINT ( 'NONE',  ( 107.9747653995834753, -121.2541776101292186, -11.78219314458148226 ) ) ;
#27115 = CARTESIAN_POINT ( 'NONE',  ( 145.3811004230890376, -139.2461875257762358, 246.2327794654912907 ) ) ;
#27116 = DIRECTION ( 'NONE',  ( 0.000000000000000000, -1.000000000000000000, 0.000000000000000000 ) ) ;
#27117 = AXIS2_PLACEMENT_3D ( 'NONE', #37895, #43351, #22945 ) ;
#27118 = CARTESIAN_POINT ( 'NONE',  ( 101.8914336387190502, -44.16123909860101548, 236.5028960185529456 ) ) ;
#27119 = ORIENTED_EDGE ( 'NONE', *, *, #9983, .F. ) ;
#27120 = ORIENTED_EDGE ( 'NONE', *, *, #85298, .F. ) ;
#27121 = ORIENTED_EDGE ( 'NONE', *, *, #70304, .T. ) ;
#27122 = CIRCLE ( 'NONE', #57592, 0.4999999999999933387 ) ;
#27123 = DIRECTION ( 'NONE',  ( -3.201858731750027727E-15, 1.000000000000000000, -3.201858731750027724E-30 ) ) ;
#27124 = CARTESIAN_POINT ( 'NONE',  ( 113.1784658275440449, -44.75174020452156753, 103.0937353791139799 ) ) ;
#27125 = LINE ( 'NONE', #79536, #51302 ) ;
#27126 = CARTESIAN_POINT ( 'NONE',  ( 97.81168895331838087, -40.51742574516882200, 287.6356252759109680 ) ) ;
#27127 = EDGE_CURVE ( 'NONE', #11211, #76903, #47281, .T. ) ;
#27128 = EDGE_CURVE ( 'NONE', #54496, #2932, #55876, .T. ) ;
#27129 = CARTESIAN_POINT ( 'NONE',  ( 134.0664832912740110, -8.350947159940998787, 4.925625275911999168 ) ) ;
#27130 = EDGE_CURVE ( 'NONE', #2756, #28030, #26415, .T. ) ;
#27131 = CARTESIAN_POINT ( 'NONE',  ( 194.0371591254573218, -24.42818131005417825, 237.4678068554150059 ) ) ;
#27132 = CARTESIAN_POINT ( 'NONE',  ( 114.8131502045276449, -44.70447909941025699, 268.1899109901970633 ) ) ;
#27133 = CARTESIAN_POINT ( 'NONE',  ( 20.03715912545737510, -24.95799193693189721, 249.9678068554150059 ) ) ;
#27134 = ORIENTED_EDGE ( 'NONE', *, *, #29119, .F. ) ;
#27135 = EDGE_CURVE ( 'NONE', #62140, #41893, #47732, .T. ) ;
#27136 = DIRECTION ( 'NONE',  ( 1.000000000000000000, 0.000000000000000000, 0.000000000000000000 ) ) ;
#27137 = AXIS2_PLACEMENT_3D ( 'NONE', #209, #27909, #41523 ) ;
#27138 = AXIS2_PLACEMENT_3D ( 'NONE', #52711, #74095, #80472 ) ;
#27139 = CARTESIAN_POINT ( 'NONE',  ( 0.000000000000000000, 223.9999999999999716, 154.6557476874258441 ) ) ;
#27140 = CARTESIAN_POINT ( 'NONE',  ( 111.5571307036148312, -44.84917726517733882, 100.7966617981629582 ) ) ;
#27142 = CLOSED_SHELL ( 'NONE', ( #14754, #8238, #4157, #63115, #76156, #76689 ) ) ;
#27141 = EDGE_CURVE ( 'NONE', #25851, #20875, #71163, .T. ) ;
#27143 = CYLINDRICAL_SURFACE ( 'NONE', #89118, 6.571100913904396990 ) ;
#27144 = EDGE_CURVE ( 'NONE', #45997, #45134, #61010, .T. ) ;
#27145 = CARTESIAN_POINT ( 'NONE',  ( 97.07207205845678288, -35.37844120283712357, 46.21895860954398927 ) ) ;
#27146 = VERTEX_POINT ( 'NONE', #48613 ) ;
#27147 = CARTESIAN_POINT ( 'NONE',  ( 77.53592152231070145, -35.65293368212927305, 7.043713522541964700 ) ) ;
#27148 = EDGE_LOOP ( 'NONE', ( #19623, #52228, #64569, #11878 ) ) ;
#27149 = CARTESIAN_POINT ( 'NONE',  ( 102.3126588425671315, -26.75045724741508124, 140.4422919425769578 ) ) ;
#27150 = VERTEX_POINT ( 'NONE', #40484 ) ;
#27151 = DIRECTION ( 'NONE',  ( -3.100000000000000258E-29, 3.100000000000000044E-14, 1.000000000000000000 ) ) ;
#27152 = CARTESIAN_POINT ( 'NONE',  ( 115.7982244386701609, -33.26055366603426933, 95.57110711542094350 ) ) ;
#27153 = CARTESIAN_POINT ( 'NONE',  ( -12.59756045763256793, 84.21337188079044722, 117.8848095194958034 ) ) ;
#27154 = DIRECTION ( 'NONE',  ( 0.000000000000000000, -1.000000000000000000, 0.000000000000000000 ) ) ;
#27155 = CARTESIAN_POINT ( 'NONE',  ( 117.1124756048696440, -32.06433792440376607, 55.16038718067301261 ) ) ;
#27156 = VECTOR ( 'NONE', #42947, 1000.000000000000000 ) ;
#27157 = CARTESIAN_POINT ( 'NONE',  ( 0.000000000000000000, 239.0000000000000000, 149.8557476874258896 ) ) ;
#27158 = VERTEX_POINT ( 'NONE', #21397 ) ;
#27159 = CARTESIAN_POINT ( 'NONE',  ( 173.9900000000000091, 20.32000000000000028, 71.37400000000000944 ) ) ;
#27160 = ORIENTED_EDGE ( 'NONE', *, *, #8281, .F. ) ;
#27161 = ORIENTED_EDGE ( 'NONE', *, *, #45886, .T. ) ;
#27162 = DIRECTION ( 'NONE',  ( 1.000000000000000000, 0.000000000000000000, 0.000000000000000000 ) ) ;
#27163 = VERTEX_POINT ( 'NONE', #27301 ) ;
#27164 = CARTESIAN_POINT ( 'NONE',  ( 116.0161715043950466, -40.67488961668907166, 253.4956252759109532 ) ) ;
#27165 = CARTESIAN_POINT ( 'NONE',  ( 107.6542194910912684, -47.14941140656445384, 148.6213395616249784 ) ) ;
#27166 = CARTESIAN_POINT ( 'NONE',  ( 11.75195648705195062, 77.68235131038592556, -117.9724202733717817 ) ) ;
#27167 = CARTESIAN_POINT ( 'NONE',  ( 116.3192736897089645, -32.94707975126958388, 130.1356252759109680 ) ) ;
#27168 = CARTESIAN_POINT ( 'NONE',  ( 97.62238793418175931, -32.23162594710754547, 71.97276813305397525 ) ) ;
#27169 = CARTESIAN_POINT ( 'NONE',  ( 107.0664832912739968, 25.62155284005901379, 333.4006252759110112 ) ) ;
#27170 = ORIENTED_EDGE ( 'NONE', *, *, #74601, .F. ) ;
#27171 = CARTESIAN_POINT ( 'NONE',  ( 194.0371591254582881, -46.82818131005407736, 249.9678068554149775 ) ) ;
#27172 = DIRECTION ( 'NONE',  ( 0.9068632946707807507, -0.4214249218767880945, 8.673617379884035472E-16 ) ) ;
#27173 = EDGE_CURVE ( 'NONE', #59761, #30868, #13675, .T. ) ;
#27174 = ORIENTED_EDGE ( 'NONE', *, *, #66045, .F. ) ;
#27175 = AXIS2_PLACEMENT_3D ( 'NONE', #19607, #54098, #27316 ) ;
#27176 = CARTESIAN_POINT ( 'NONE',  ( 115.0439452383991892, -99.09543445804983719, -19.78219314458218392 ) ) ;
#27177 = VECTOR ( 'NONE', #81985, 1000.000000000000114 ) ;
#27178 = CARTESIAN_POINT ( 'NONE',  ( 130.5667039024481255, -40.02944715994102154, 249.5838068554162987 ) ) ;
#27179 = CARTESIAN_POINT ( 'NONE',  ( 105.7790678824445081, -26.40611305247077567, 270.1756252759109884 ) ) ;
#27180 = DIRECTION ( 'NONE',  ( -0.7071067811865506814, 0.7071067811865443531, -7.071067811865500971E-16 ) ) ;
#27181 = AXIS2_PLACEMENT_3D ( 'NONE', #2918, #29730, #50603 ) ;
#27182 = FACE_OUTER_BOUND ( 'NONE', #54685, .T. ) ;
#27183 = CARTESIAN_POINT ( 'NONE',  ( 0.000000000000000000, 95.25000000000000000, 0.000000000000000000 ) ) ;
#27184 = CARTESIAN_POINT ( 'NONE',  ( 100.9974734301594310, -29.01720366022859565, 15.60705384733995871 ) ) ;
#27186 = CARTESIAN_POINT ( 'NONE',  ( 96.66103594285313250, -37.56076609107801545, 97.38991099019594344 ) ) ;
#27185 = DIRECTION ( 'NONE',  ( -1.047445008332813989E-14, 0.000000000000000000, -1.000000000000000000 ) ) ;
#27187 = CARTESIAN_POINT ( 'NONE',  ( 122.8585116216235065, -38.08382569396911776, 302.6356252759109680 ) ) ;
#27188 = CARTESIAN_POINT ( 'NONE',  ( 100.8602861511969024, -45.93004170815812159, 152.0918157521009562 ) ) ;
#27189 = FACE_OUTER_BOUND ( 'NONE', #69874, .T. ) ;
#27190 = VERTEX_POINT ( 'NONE', #34559 ) ;
#27191 = PLANE ( 'NONE',  #74435 ) ;
#27192 = DIRECTION ( 'NONE',  ( -0.000000000000000000, 1.000000000000000000, 0.000000000000000000 ) ) ;
#27193 = PLANE ( 'NONE',  #31118 ) ;
#27194 = ORIENTED_EDGE ( 'NONE', *, *, #55904, .F. ) ;
#27195 = DIRECTION ( 'NONE',  ( -0.000000000000000000, 1.000000000000000000, -0.000000000000000000 ) ) ;
#27197 = ORIENTED_EDGE ( 'NONE', *, *, #64870, .F. ) ;
#27196 = CARTESIAN_POINT ( 'NONE',  ( 109.2104764766756517, -26.48201038666214657, 139.9127681330539872 ) ) ;
#27198 = DIRECTION ( 'NONE',  ( -4.237773401492740281E-14, 1.000000000000000000, 0.000000000000000000 ) ) ;
#27199 = AXIS2_PLACEMENT_3D ( 'NONE', #70950, #43659, #84130 ) ;
#27200 = CARTESIAN_POINT ( 'NONE',  ( 90.25011051337631329, 70.17666187254640420, 94.33955404248759180 ) ) ;
#27201 = CIRCLE ( 'NONE', #60505, 15.69999999999999574 ) ;
#27202 = CARTESIAN_POINT ( 'NONE',  ( -24.79284581386642827, 184.0000000000000000, 106.1020876358972771 ) ) ;
#27203 = DIRECTION ( 'NONE',  ( 3.062684205862500216E-15, 0.000000000000000000, -1.000000000000000000 ) ) ;
#27204 = ORIENTED_EDGE ( 'NONE', *, *, #43370, .T. ) ;
#27205 = VECTOR ( 'NONE', #74613, 1000.000000000000000 ) ;
#27206 = EDGE_CURVE ( 'NONE', #6607, #593, #27622, .T. ) ;
#27207 = ORIENTED_EDGE ( 'NONE', *, *, #46702, .F. ) ;
#27208 = ORIENTED_EDGE ( 'NONE', *, *, #16740, .T. ) ;
#27209 = ORIENTED_EDGE ( 'NONE', *, *, #66414, .F. ) ;
#27210 = LINE ( 'NONE', #19502, #51027 ) ;
#27211 = CARTESIAN_POINT ( 'NONE',  ( 99.28081699872726062, -30.36252297428069724, 250.7808459398054310 ) ) ;
#27212 = FACE_OUTER_BOUND ( 'NONE', #44581, .T. ) ;
#27214 = LINE ( 'NONE', #41276, #51480 ) ;
#27213 = CARTESIAN_POINT ( 'NONE',  ( 21.03715912545746036, -47.82818131006197149, 117.4678068554150485 ) ) ;
#27215 = LINE ( 'NONE', #76264, #50069 ) ;
#27216 = ORIENTED_EDGE ( 'NONE', *, *, #78333, .F. ) ;
#27217 = VECTOR ( 'NONE', #72022, 1000.000000000000000 ) ;
#27218 = ORIENTED_EDGE ( 'NONE', *, *, #29582, .T. ) ;
#27219 = DIRECTION ( 'NONE',  ( 0.000000000000000000, 0.000000000000000000, 1.000000000000000000 ) ) ;
#27220 = CARTESIAN_POINT ( 'NONE',  ( 71.06670390244705970, -124.7784471599409812, 55.21780685541800437 ) ) ;
#27221 = CARTESIAN_POINT ( 'NONE',  ( 113.3831382903590566, -27.58002901871528323, 235.5956252759109759 ) ) ;
#27222 = EDGE_CURVE ( 'NONE', #53871, #29598, #78431, .T. ) ;
#27223 = DIRECTION ( 'NONE',  ( 0.000000000000000000, 0.000000000000000000, -1.000000000000000000 ) ) ;
#27224 = CARTESIAN_POINT ( 'NONE',  ( 103.5913876162975953, -46.49993820617270757, 98.31657765686297523 ) ) ;
#27225 = ADVANCED_FACE ( 'NONE', ( #49070 ), #42263, .F. ) ;
#27226 = DIRECTION ( 'NONE',  ( 1.000000000000000000, 0.000000000000000000, 0.000000000000000000 ) ) ;
#27227 = EDGE_CURVE ( 'NONE', #84439, #51309, #23216, .T. ) ;
#27228 = CARTESIAN_POINT ( 'NONE',  ( 114.7529613671623139, -30.30768866273729500, 20.38027562559657113 ) ) ;
#27229 = ORIENTED_EDGE ( 'NONE', *, *, #87034, .F. ) ;
#27230 = DIRECTION ( 'NONE',  ( 0.000000000000000000, -1.000000000000000000, 0.000000000000000000 ) ) ;
#27231 = EDGE_CURVE ( 'NONE', #58613, #41326, #39225, .T. ) ;
#27232 = AXIS2_PLACEMENT_3D ( 'NONE', #31861, #80938, #5521 ) ;
#27233 = EDGE_LOOP ( 'NONE', ( #35938, #54002, #11056, #33174 ) ) ;
#27234 = ORIENTED_EDGE ( 'NONE', *, *, #46201, .F. ) ;
#27235 = CARTESIAN_POINT ( 'NONE',  ( 131.3164832912740110, -36.72944715994100306, 3.101481641215535046 ) ) ;
#27236 = CARTESIAN_POINT ( 'NONE',  ( 114.3671945862968045, -31.65384462053443571, 275.7415833058969952 ) ) ;
#27237 = CIRCLE ( 'NONE', #30167, 5.035202529042104302 ) ;
#27238 = CYLINDRICAL_SURFACE ( 'NONE', #70575, 2.999999999999975131 ) ;
#27239 = VECTOR ( 'NONE', #48309, 1000.000000000000000 ) ;
#27240 = DIRECTION ( 'NONE',  ( -1.000000000000000000, 0.000000000000000000, -2.108231265501709878E-16 ) ) ;
#27241 = DIRECTION ( 'NONE',  ( 0.000000000000000000, 0.000000000000000000, 1.000000000000000000 ) ) ;
#27242 = EDGE_CURVE ( 'NONE', #65418, #16063, #50428, .T. ) ;
#27243 = CARTESIAN_POINT ( 'NONE',  ( 86.67600044576353469, 70.52018178143200089, -80.88853703239280435 ) ) ;
#27244 = ORIENTED_EDGE ( 'NONE', *, *, #64099, .T. ) ;
#27245 = DIRECTION ( 'NONE',  ( 0.000000000000000000, -1.000000000000000000, 0.000000000000000000 ) ) ;
#27246 = CONICAL_SURFACE ( 'NONE', #85376, 1.571100913904388552, 1.047197551196592302 ) ;
#27247 = CARTESIAN_POINT ( 'NONE',  ( 113.1764918811396399, -44.75321505856369697, 184.0943504403222164 ) ) ;
#27248 = VERTEX_POINT ( 'NONE', #63621 ) ;
#27249 = CARTESIAN_POINT ( 'NONE',  ( 117.0539912639601852, -31.99354471700374702, 64.19086337114899266 ) ) ;
#27250 = ORIENTED_EDGE ( 'NONE', *, *, #15570, .F. ) ;
#27251 = CARTESIAN_POINT ( 'NONE',  ( 113.9883325317156135, -31.53436023685440048, 262.1690427505439516 ) ) ;
#27252 = VECTOR ( 'NONE', #61619, 1000.000000000000000 ) ;
#27253 = DIRECTION ( 'NONE',  ( 3.360405532702990443E-14, -1.000000000000000000, 0.000000000000000000 ) ) ;
#27254 = CARTESIAN_POINT ( 'NONE',  ( 97.31342953368660176, -35.99458159538090030, 146.2670538473399517 ) ) ;
#27255 = CARTESIAN_POINT ( 'NONE',  ( 106.0667039024470455, -121.2010968907522113, -11.78219314458148226 ) ) ;
#27256 = DIRECTION ( 'NONE',  ( 0.8660254037844381525, 0.000000000000000000, 0.5000000000000007772 ) ) ;
#27257 = TOROIDAL_SURFACE ( 'NONE', #63575, 6.647542495715439870, 3.174999999999999822 ) ;
#27258 = CARTESIAN_POINT ( 'NONE',  ( 181.8764988495247223, -33.54226604284360747, 237.4678068554150059 ) ) ;
#27259 = VECTOR ( 'NONE', #74774, 999.9999999999998863 ) ;
#27260 = DIRECTION ( 'NONE',  ( -3.100000000000000258E-29, 3.100000000000000044E-14, 1.000000000000000000 ) ) ;
#27261 = CARTESIAN_POINT ( 'NONE',  ( 110.0014563237810137, -26.68062070874399438, 255.8499109901966051 ) ) ;
#27262 = CYLINDRICAL_SURFACE ( 'NONE', #3583, 12.69999999999998863 ) ;
#27263 = ORIENTED_EDGE ( 'NONE', *, *, #17191, .F. ) ;
#27264 = EDGE_LOOP ( 'NONE', ( #88375, #69526, #50354, #3199 ) ) ;
#27265 = CARTESIAN_POINT ( 'NONE',  ( 113.8847749867171046, -44.67324210339663182, 104.1413395616249744 ) ) ;
#27266 = CARTESIAN_POINT ( 'NONE',  ( 121.2221484686747459, -113.6057974291317549, -21.78219314458173983 ) ) ;
#27267 = VERTEX_POINT ( 'NONE', #57698 ) ;
#27268 = ORIENTED_EDGE ( 'NONE', *, *, #238, .T. ) ;
#27269 = ORIENTED_EDGE ( 'NONE', *, *, #43674, .T. ) ;
#27270 = DIRECTION ( 'NONE',  ( 0.000000000000000000, -1.000000000000000000, 0.000000000000000000 ) ) ;
#27271 = CARTESIAN_POINT ( 'NONE',  ( 107.0664832912739541, -23.56278049327425350, 357.5272416190308604 ) ) ;
#27272 = CARTESIAN_POINT ( 'NONE',  ( 128.8897065959775432, -58.55267046464430791, -5.074374724089007138 ) ) ;
#27273 = DIRECTION ( 'NONE',  ( 0.000000000000000000, 0.000000000000000000, -1.000000000000000000 ) ) ;
#27274 = CARTESIAN_POINT ( 'NONE',  ( 99.93348902297414327, -31.82829241803101894, 163.6776141791149826 ) ) ;
#27275 = CARTESIAN_POINT ( 'NONE',  ( 100.2329966457367334, -45.44659500335379221, 273.0594347997205773 ) ) ;
#27276 = FACE_OUTER_BOUND ( 'NONE', #19683, .T. ) ;
#27277 = ORIENTED_EDGE ( 'NONE', *, *, #76061, .T. ) ;
#27278 = CARTESIAN_POINT ( 'NONE',  ( 130.5480414536683895, 95.16896684734908263, -1.658263961149670118 ) ) ;
#27279 = VECTOR ( 'NONE', #38750, 1000.000000000000000 ) ;
#27280 = DIRECTION ( 'NONE',  ( -0.7071067811865462405, 0.000000000000000000, 0.7071067811865486830 ) ) ;
#27281 = EDGE_CURVE ( 'NONE', #21126, #25185, #84982, .T. ) ;
#27282 = ORIENTED_EDGE ( 'NONE', *, *, #10741, .T. ) ;
#27284 = VERTEX_POINT ( 'NONE', #44501 ) ;
#27283 = AXIS2_PLACEMENT_3D ( 'NONE', #57209, #77230, #15459 ) ;
#27285 = LINE ( 'NONE', #34990, #83691 ) ;
#27286 = VERTEX_POINT ( 'NONE', #35451 ) ;
#27287 = ORIENTED_EDGE ( 'NONE', *, *, #29285, .F. ) ;
#27288 = DIRECTION ( 'NONE',  ( 0.7071067812152160847, -0.7071067811578790607, 0.000000000000000000 ) ) ;
#27289 = CARTESIAN_POINT ( 'NONE',  ( 97.33781463699185110, -34.07115960914099162, 16.11479949169054393 ) ) ;
#27290 = EDGE_CURVE ( 'NONE', #18666, #65691, #63167, .T. ) ;
#27291 = CARTESIAN_POINT ( 'NONE',  ( 83.73314995794039817, 12.92155284005802685, 349.2756252759109543 ) ) ;
#27292 = DIRECTION ( 'NONE',  ( 0.7071067811571474238, 0.7071067812159476107, 0.000000000000000000 ) ) ;
#27293 = CARTESIAN_POINT ( 'NONE',  ( 100.0898434420045788, -43.48201142159524579, 191.3609912566489584 ) ) ;
#27294 = CARTESIAN_POINT ( 'NONE',  ( 112.7839950898761288, -27.91685089337277503, 69.61848241876793963 ) ) ;
#27295 = CARTESIAN_POINT ( 'NONE',  ( 7.661254700127844153, 66.45253841614081125, 275.4630000000000223 ) ) ;
#27296 = ORIENTED_EDGE ( 'NONE', *, *, #16301, .F. ) ;
#27297 = CARTESIAN_POINT ( 'NONE',  ( 51.23005224011698289, -33.89581943344334292, 313.9678068554150059 ) ) ;
#27298 = VERTEX_POINT ( 'NONE', #30006 ) ;
#27299 = CARTESIAN_POINT ( 'NONE',  ( 109.7235518845674136, -27.00045683442361266, 260.8648104962068146 ) ) ;
#27300 = ORIENTED_EDGE ( 'NONE', *, *, #7824, .T. ) ;
#27301 = CARTESIAN_POINT ( 'NONE',  ( 135.9998166246059839, 12.92155284005730387, 361.9756252759109998 ) ) ;
#27302 = CARTESIAN_POINT ( 'NONE',  ( -4.059050453778890066, 70.59316187249579855, 118.4889539811882457 ) ) ;
#27303 = CARTESIAN_POINT ( 'NONE',  ( 105.7145417833327343, -46.72371677956441260, 132.4689531747473268 ) ) ;
#27305 = DIRECTION ( 'NONE',  ( 0.000000000000000000, -1.000000000000000000, 0.000000000000000000 ) ) ;
#27304 = AXIS2_PLACEMENT_3D ( 'NONE', #67098, #39392, #12142 ) ;
#27306 = ORIENTED_EDGE ( 'NONE', *, *, #71944, .T. ) ;
#27308 = EDGE_CURVE ( 'NONE', #28373, #69770, #33466, .T. ) ;
#27307 = AXIS2_PLACEMENT_3D ( 'NONE', #51758, #38585, #9120 ) ;
#27309 = CARTESIAN_POINT ( 'NONE',  ( 110.3610989901968651, -25.31982300743893077, 64.85276813305395649 ) ) ;
#27311 = CARTESIAN_POINT ( 'NONE',  ( 142.0664832912740394, -45.72944715994099596, 14.67562527591100441 ) ) ;
#27310 = FACE_OUTER_BOUND ( 'NONE', #39446, .T. ) ;
#27312 = DIRECTION ( 'NONE',  ( -0.7071067811865474617, -0.000000000000000000, 0.7071067811865474617 ) ) ;
#27313 = DIRECTION ( 'NONE',  ( -0.9999999853157766072, -0.0001713722456127291416, 9.999999853157765648E-16 ) ) ;
#27314 = EDGE_LOOP ( 'NONE', ( #58735, #77257 ) ) ;
#27315 = AXIS2_PLACEMENT_3D ( 'NONE', #64578, #17324, #85935 ) ;
#27316 = DIRECTION ( 'NONE',  ( 0.000000000000000000, 0.000000000000000000, 1.000000000000000000 ) ) ;
#27317 = CIRCLE ( 'NONE', #31661, 10.00000000000000888 ) ;
#27318 = CARTESIAN_POINT ( 'NONE',  ( 160.0667039024470171, -79.67844715994088745, 55.21780685541800437 ) ) ;
#27319 = CARTESIAN_POINT ( 'NONE',  ( 11.89159109876203146, 78.07192968827520474, 117.9582163940502966 ) ) ;
#27320 = ADVANCED_FACE ( 'NONE', ( #85877 ), #85440, .T. ) ;
#27321 = ORIENTED_EDGE ( 'NONE', *, *, #48420, .T. ) ;
#27322 = CARTESIAN_POINT ( 'NONE',  ( 97.60264960697516301, -32.22222542080420027, 71.97276813305397525 ) ) ;
#27323 = CIRCLE ( 'NONE', #89724, 3.000000000000002665 ) ;
#27324 = CIRCLE ( 'NONE', #70854, 16.00000000000000000 ) ;
#27326 = CARTESIAN_POINT ( 'NONE',  ( 41.56648329127381203, -27.82844715994070484, 141.9256252759119832 ) ) ;
#27325 = CARTESIAN_POINT ( 'NONE',  ( 89.17003477451882532, -56.47944715994104570, 14.92562527591095289 ) ) ;
#27327 = CARTESIAN_POINT ( 'NONE',  ( 107.0667039024470313, -104.2784471599413934, 2.217806855418003043 ) ) ;
#27328 = CARTESIAN_POINT ( 'NONE',  ( 146.0392919387902282, -109.2859103858200029, 247.4783998280190076 ) ) ;
#27329 = ORIENTED_EDGE ( 'NONE', *, *, #5664, .T. ) ;
#27330 = CARTESIAN_POINT ( 'NONE',  ( 105.4244293397739085, -47.72525222749315787, 143.4584824187679715 ) ) ;
#27331 = AXIS2_PLACEMENT_3D ( 'NONE', #48152, #475, #89525 ) ;
#27333 = ORIENTED_EDGE ( 'NONE', *, *, #56541, .F. ) ;
#27332 = CYLINDRICAL_SURFACE ( 'NONE', #74736, 2.517500000000005844 ) ;
#27334 = CARTESIAN_POINT ( 'NONE',  ( 100.2624651760415873, -28.85963121439202794, 256.6441967044821695 ) ) ;
#27335 = CARTESIAN_POINT ( 'NONE',  ( 223.2659999999999911, 52.73749999999999716, -44.45000000000000284 ) ) ;
#27336 = CARTESIAN_POINT ( 'NONE',  ( -487.2989999999999782, 97.78694598552370110, 18.25625000000050235 ) ) ;
#27337 = CARTESIAN_POINT ( 'NONE',  ( 165.2725846195380086, -35.55794170701810941, -5.074374724088000832 ) ) ;
#27338 = ADVANCED_FACE ( 'NONE', ( #29108 ), #35909, .F. ) ;
#27339 = PLANE ( 'NONE',  #77527 ) ;
#27340 = DIRECTION ( 'NONE',  ( 1.000000000000000000, 0.000000000000000000, 0.000000000000000000 ) ) ;
#27341 = CARTESIAN_POINT ( 'NONE',  ( 131.3164832912739826, -18.72944715994100662, -5.074374724089004474 ) ) ;
#27342 = CARTESIAN_POINT ( 'NONE',  ( 114.4888877093246293, -29.48743791597849651, 194.4537205140069318 ) ) ;
#27343 = AXIS2_PLACEMENT_3D ( 'NONE', #25466, #11847, #39541 ) ;
#27344 = VERTEX_POINT ( 'NONE', #44053 ) ;
#27345 = ORIENTED_EDGE ( 'NONE', *, *, #62623, .F. ) ;
#27346 = VECTOR ( 'NONE', #82888, 1000.000000000000000 ) ;
#27347 = CARTESIAN_POINT ( 'NONE',  ( 103.4772640228778329, -44.83165572645120278, 173.6758690201829438 ) ) ;
#27348 = FACE_OUTER_BOUND ( 'NONE', #34104, .T. ) ;
#27350 = DIRECTION ( 'NONE',  ( -1.000000000000000000, 0.000000000000000000, 0.000000000000000000 ) ) ;
#27349 = CARTESIAN_POINT ( 'NONE',  ( 102.6690082227317475, -46.93785447722112281, 283.2527681330534506 ) ) ;
#27351 = PLANE ( 'NONE',  #10177 ) ;
#27352 = FACE_OUTER_BOUND ( 'NONE', #71068, .T. ) ;
#27353 = EDGE_CURVE ( 'NONE', #46749, #87063, #85687, .T. ) ;
#27354 = DIRECTION ( 'NONE',  ( 0.000000000000000000, 0.000000000000000000, -1.000000000000000000 ) ) ;
#27355 = CARTESIAN_POINT ( 'NONE',  ( 97.81168895331838087, -40.51742574516882200, 11.63562527591094309 ) ) ;
#27356 = PLANE ( 'NONE',  #3834 ) ;
#27357 = EDGE_CURVE ( 'NONE', #7162, #77531, #15029, .T. ) ;
#27358 = CARTESIAN_POINT ( 'NONE',  ( 100.6697571656888073, -44.93374849542868787, 232.0499109901969632 ) ) ;
#27359 = CARTESIAN_POINT ( 'NONE',  ( 116.3170820643562564, -32.94538914428453324, 169.1356252759109680 ) ) ;
#27360 = EDGE_LOOP ( 'NONE', ( #24913, #35818, #52664, #71095 ) ) ;
#27361 = EDGE_LOOP ( 'NONE', ( #27550, #47759, #43996, #84252 ) ) ;
#27362 = VECTOR ( 'NONE', #22517, 1000.000000000000000 ) ;
#27363 = DIRECTION ( 'NONE',  ( 0.000000000000000000, 0.000000000000000000, 1.000000000000000000 ) ) ;
#27364 = CARTESIAN_POINT ( 'NONE',  ( 82.49755700851123663, -20.01506174167580099, 7.157201688891981384 ) ) ;
#27365 = CARTESIAN_POINT ( 'NONE',  ( 102.0674957170151060, -27.97023961310380713, 185.4902194784735912 ) ) ;
#27366 = DIRECTION ( 'NONE',  ( -0.7071067811865634489, 0.7071067811865315855, -7.071067811865641980E-16 ) ) ;
#27368 = LINE ( 'NONE', #81468, #78954 ) ;
#27367 = AXIS2_PLACEMENT_3D ( 'NONE', #76827, #43635, #56365 ) ;
#27369 = ORIENTED_EDGE ( 'NONE', *, *, #32998, .T. ) ;
#27370 = CARTESIAN_POINT ( 'NONE',  ( 116.8105015878075079, -31.41422314659176607, 20.21181575210195902 ) ) ;
#27371 = CARTESIAN_POINT ( 'NONE',  ( 115.5175571194294122, -29.60495148624196204, 224.3718157521009573 ) ) ;
#27372 = VERTEX_POINT ( 'NONE', #49972 ) ;
#27373 = CIRCLE ( 'NONE', #20126, 2.500000000000002220 ) ;
#27374 = CARTESIAN_POINT ( 'NONE',  ( 172.5664832912729878, -27.57844715994070484, 135.9256252759119832 ) ) ;
#27375 = CARTESIAN_POINT ( 'NONE',  ( 123.0664832912757163, -36.72944715993921960, -4.074374724089013355 ) ) ;
#27376 = CARTESIAN_POINT ( 'NONE',  ( 208.9149999999999920, 30.98800000000000310, 44.45000000000000284 ) ) ;
#27377 = CARTESIAN_POINT ( 'NONE',  ( 104.3513172347134770, -44.42734293102004273, 55.12523322673396109 ) ) ;
#27379 = CARTESIAN_POINT ( 'NONE',  ( 98.14969091592392658, -31.28627964566590336, 166.8899109901969950 ) ) ;
#27378 = AXIS2_PLACEMENT_3D ( 'NONE', #71940, #31471, #51463 ) ;
#27380 = DIRECTION ( 'NONE',  ( 0.000000000000000000, 0.000000000000000000, -1.000000000000000000 ) ) ;
#27381 = ORIENTED_EDGE ( 'NONE', *, *, #42995, .F. ) ;
#27382 = VECTOR ( 'NONE', #77041, 1000.000000000000000 ) ;
#27383 = CYLINDRICAL_SURFACE ( 'NONE', #77007, 0.5000000000000079936 ) ;
#27384 = VERTEX_POINT ( 'NONE', #70443 ) ;
#27385 = ORIENTED_EDGE ( 'NONE', *, *, #32422, .T. ) ;
#27386 = LINE ( 'NONE', #33759, #58949 ) ;
#27387 = VERTEX_POINT ( 'NONE', #1407 ) ;
#27388 = ORIENTED_EDGE ( 'NONE', *, *, #62886, .T. ) ;
#27389 = CARTESIAN_POINT ( 'NONE',  ( 97.81170255947417047, -40.51743869465033754, 117.6354096206635518 ) ) ;
#27390 = AXIS2_PLACEMENT_3D ( 'NONE', #32636, #53503, #24941 ) ;
#27391 = CARTESIAN_POINT ( 'NONE',  ( 108.8595479556035599, -45.11020018309576329, 107.1667055423619672 ) ) ;
#27392 = CARTESIAN_POINT ( 'NONE',  ( 114.6215443236117153, -29.51367161159714314, 234.4327681330539690 ) ) ;
#27393 = CARTESIAN_POINT ( 'NONE',  ( 117.1710321396411416, -41.15233254730030410, 208.4861014663869696 ) ) ;
#27395 = CARTESIAN_POINT ( 'NONE',  ( 118.5467753794658705, -33.90456151647279626, 10.01848241876795953 ) ) ;
#27394 = FACE_OUTER_BOUND ( 'NONE', #45409, .T. ) ;
#27396 = CARTESIAN_POINT ( 'NONE',  ( 24.79284581386643183, 184.0000000000000000, 0.000000000000000000 ) ) ;
#27397 = FACE_OUTER_BOUND ( 'NONE', #57611, .T. ) ;
#27398 = ORIENTED_EDGE ( 'NONE', *, *, #5142, .T. ) ;
#27399 = AXIS2_PLACEMENT_3D ( 'NONE', #74154, #39178, #11930 ) ;
#27400 = CARTESIAN_POINT ( 'NONE',  ( 107.2219638487720488, -26.36052190073617041, 80.07657765686398932 ) ) ;
#27401 = CARTESIAN_POINT ( 'NONE',  ( 110.3680388590993573, -25.29578946207851331, 64.85276813305395649 ) ) ;
#27402 = CARTESIAN_POINT ( 'NONE',  ( 111.7588773036880383, -27.37059502548119028, 279.7070538473396937 ) ) ;
#27403 = EDGE_LOOP ( 'NONE', ( #82702, #40510, #51761, #15678, #43959, #32129, #81770, #40014, #10512, #17426, #39566, #61094, #34525, #50934, #84237, #10483, #4886, #252, #2599, #73911, #22110, #42043, #37175, #86568, #67554, #7508, #46013, #77450, #30908, #4002, #47988, #56757, #71653, #32506, #10894, #56193, #36093, #41089, #77018, #59457, #25019, #68448, #42425, #23817, #82213, #1169, #66013, #46168, #58860, #16215, #70151, #31691, #81898, #17785, #36624, #63880, #55113, #61236, #66956, #1272, #42520, #60606, #43263, #14888, #68323, #44399, #61765, #58579, #17264, #58046, #83181, #14643, #52624, #50963, #52241, #57888, #22117, #52096, #48424, #9048, #70285, #45507, #28643, #43745, #19556, #76690, #75472, #16441, #31236, #55772, #69626, #32120 ) ) ;
#27404 = EDGE_CURVE ( 'NONE', #86337, #11051, #53721, .T. ) ;
#27405 = CARTESIAN_POINT ( 'NONE',  ( 113.0255487838780937, -46.03904575001691768, 218.0175300378159591 ) ) ;
#27406 = CARTESIAN_POINT ( 'NONE',  ( 163.0664832912739826, 12.92155284005902516, 333.4006252759110112 ) ) ;
#27407 = CARTESIAN_POINT ( 'NONE',  ( 53.35959712126142307, -48.62134037875158299, 180.4678068554151196 ) ) ;
#27408 = DIRECTION ( 'NONE',  ( 0.000000000000000000, 1.000000000000000000, 0.000000000000000000 ) ) ;
#27410 = DIRECTION ( 'NONE',  ( 1.000000000000000000, 8.673617379883546378E-16, 9.757819552368989676E-16 ) ) ;
#27409 = CARTESIAN_POINT ( 'NONE',  ( 114.1839641476628913, -41.30284314992755412, 277.6356252759110248 ) ) ;
#27411 = CARTESIAN_POINT ( 'NONE',  ( 188.5667039024479834, -67.87844715994100397, 137.2178068554150059 ) ) ;
#27412 = DIRECTION ( 'NONE',  ( 0.000000000000000000, 1.000000000000000000, 0.000000000000000000 ) ) ;
#27413 = LINE ( 'NONE', #69657, #38310 ) ;
#27415 = ADVANCED_FACE ( 'NONE', ( #15932 ), #2752, .F. ) ;
#27414 = B_SPLINE_CURVE_WITH_KNOTS ( 'NONE', 3,
 ( #41747, #27692, #75404, #34944, #42201, #20440, #6796, #69030, #55370, #70376, #6352, #76741, #56730, #13175, #8148, #63100, #14522, #48550 ),
 .UNSPECIFIED., .F., .F.,
 ( 4, 2, 2, 2, 2, 2, 2, 2, 4 ),
 ( 0.000000000000000000, 0.06249937177560595247, 0.1249987435512119049, 0.1874981153268178713, 0.2499974871024238099, 0.3124968588780297485, 0.3749962306536357426, 0.4374956024292416812, 0.4999949742048476198 ),
 .UNSPECIFIED. ) ;
#27416 = CARTESIAN_POINT ( 'NONE',  ( 71.24025061656124080, 8.642044024269713631, 394.9756252759102040 ) ) ;
#27417 = CARTESIAN_POINT ( 'NONE',  ( 97.33724564666434276, -34.07349040010189611, 41.11432248975863502 ) ) ;
#27418 = EDGE_CURVE ( 'NONE', #20886, #1757, #65363, .T. ) ;
#27419 = CARTESIAN_POINT ( 'NONE',  ( 147.0667039024470171, -79.67844715994090166, 222.2178068554179902 ) ) ;
#27421 = EDGE_LOOP ( 'NONE', ( #62160, #42508, #58511, #66658, #13249 ) ) ;
#27420 = CARTESIAN_POINT ( 'NONE',  ( 172.5664832912740110, 0.2215528400590013880, 316.8086252759120498 ) ) ;
#27422 = TOROIDAL_SURFACE ( 'NONE', #46270, 15.84999999999999964, 0.1499999999999999944 ) ;
#27423 = EDGE_CURVE ( 'NONE', #2591, #23447, #84260, .T. ) ;
#27424 = FACE_OUTER_BOUND ( 'NONE', #68414, .T. ) ;
#27425 = CARTESIAN_POINT ( 'NONE',  ( 112.5009111935468411, -46.38151608383146396, 257.9965776568635647 ) ) ;
#27426 = CARTESIAN_POINT ( 'NONE',  ( 95.31164914186729220, -38.27921806354234491, 147.4299109901969871 ) ) ;
#27427 = CARTESIAN_POINT ( 'NONE',  ( 106.1344768297789329, -47.78968505587090476, 258.4975300378158636 ) ) ;
#27428 = FACE_OUTER_BOUND ( 'NONE', #53680, .T. ) ;
#27430 = CARTESIAN_POINT ( 'NONE',  ( 172.5664832912729878, -27.82844715994070484, 318.9256252759120116 ) ) ;
#27429 = DIRECTION ( 'NONE',  ( 0.9963424814100680926, -0.08544974978095730422, 0.000000000000000000 ) ) ;
#27431 = DIRECTION ( 'NONE',  ( -0.7071067811865171526, -0.7071067811865779928, -6.612322855854603498E-17 ) ) ;
#27432 = EDGE_CURVE ( 'NONE', #60265, #70284, #79054, .T. ) ;
#27433 = LINE ( 'NONE', #55112, #51459 ) ;
#27434 = AXIS2_PLACEMENT_3D ( 'NONE', #29474, #35372, #63084 ) ;
#27435 = EDGE_CURVE ( 'NONE', #18059, #51056, #47898, .T. ) ;
#27436 = EDGE_LOOP ( 'NONE', ( #77779, #22205, #73954, #63135 ) ) ;
#27437 = DIRECTION ( 'NONE',  ( -0.7071067811865764385, 0.7071067811865187069, -7.071067811865771156E-16 ) ) ;
#27438 = EDGE_LOOP ( 'NONE', ( #76215, #72071 ) ) ;
#27439 = CARTESIAN_POINT ( 'NONE',  ( 108.1312808730283166, -45.72271566404705112, 162.1048007804579640 ) ) ;
#27440 = AXIS2_PLACEMENT_3D ( 'NONE', #75977, #48245, #26482 ) ;
#27442 = VERTEX_POINT ( 'NONE', #3194 ) ;
#27441 = CARTESIAN_POINT ( 'NONE',  ( 147.0667039024469886, -67.87844715994090450, 222.2178068554179902 ) ) ;
#27443 = CARTESIAN_POINT ( 'NONE',  ( 48.79742451362098166, -36.32844715994040996, 342.9256252759119548 ) ) ;
#27444 = CARTESIAN_POINT ( 'NONE',  ( 109.3536845750984128, -25.93905639472658819, 180.9222919425779708 ) ) ;
#27445 = PRESENTATION_LAYER_ASSIGNMENT (  '', '', ( #31789 ) ) ;
#27446 = EDGE_CURVE ( 'NONE', #54334, #87716, #87645, .T. ) ;
#27447 = DIRECTION ( 'NONE',  ( 0.000000000000000000, 0.000000000000000000, 1.000000000000000000 ) ) ;
#27448 = DIRECTION ( 'NONE',  ( 1.000000000000000000, 0.000000000000000000, 2.108231265501709878E-16 ) ) ;
#27449 = DIRECTION ( 'NONE',  ( 0.000000000000000000, 1.000000000000000000, 0.000000000000000000 ) ) ;
#27450 = AXIS2_PLACEMENT_3D ( 'NONE', #38812, #80175, #59251 ) ;
#27451 = CARTESIAN_POINT ( 'NONE',  ( 113.0229309284916752, -28.24065945027244595, 84.57753003781698453 ) ) ;
#27452 = ORIENTED_EDGE ( 'NONE', *, *, #68600, .F. ) ;
#27453 = ORIENTED_EDGE ( 'NONE', *, *, #30296, .T. ) ;
#27454 = VERTEX_POINT ( 'NONE', #11333 ) ;
#27455 = DIRECTION ( 'NONE',  ( 0.000000000000000000, 1.000000000000000000, 0.000000000000000000 ) ) ;
#27457 = CARTESIAN_POINT ( 'NONE',  ( 172.5664832912728457, -18.82844715994071194, 261.9256252759119548 ) ) ;
#27456 = CARTESIAN_POINT ( 'NONE',  ( 102.2986265273211615, -45.30740241592380357, 183.1727681330529833 ) ) ;
#27458 = CARTESIAN_POINT ( 'NONE',  ( 112.1400925610924730, -28.01325243291391232, 54.65557868090081683 ) ) ;
#27459 = CARTESIAN_POINT ( 'NONE',  ( 71.06670390244705970, -118.2784471599409812, 222.2178068554179902 ) ) ;
#27460 = AXIS2_PLACEMENT_3D ( 'NONE', #26508, #66946, #81052 ) ;
#27461 = AXIS2_PLACEMENT_3D ( 'NONE', #79489, #17251, #78155 ) ;
#27462 = DIRECTION ( 'NONE',  ( 0.000000000000000000, -1.000000000000000000, 0.000000000000000000 ) ) ;
#27463 = EDGE_CURVE ( 'NONE', #7579, #30851, #32214, .T. ) ;
#27464 = LINE ( 'NONE', #48784, #33250 ) ;
#27465 = DIRECTION ( 'NONE',  ( 0.000000000000000000, 0.000000000000000000, 1.000000000000000000 ) ) ;
#27466 = EDGE_CURVE ( 'NONE', #59958, #44336, #65414, .T. ) ;
#27467 = CARTESIAN_POINT ( 'NONE',  ( 102.6254653968535990, -46.82603978519644272, 132.2346728949579528 ) ) ;
#27468 = ORIENTED_EDGE ( 'NONE', *, *, #42615, .F. ) ;
#27469 = ORIENTED_EDGE ( 'NONE', *, *, #42507, .F. ) ;
#27470 = VERTEX_POINT ( 'NONE', #37717 ) ;
#27471 = EDGE_CURVE ( 'NONE', #75399, #72082, #19044, .T. ) ;
#27472 = CARTESIAN_POINT ( 'NONE',  ( 88.06670390244791236, -14.72944715994105991, 239.5838068554169809 ) ) ;
#27473 = CARTESIAN_POINT ( 'NONE',  ( -82.89895571708225930, 82.96445444011520465, -100.8594679592215329 ) ) ;
#27474 = EDGE_CURVE ( 'NONE', #52538, #21031, #86308, .T. ) ;
#27475 = DIRECTION ( 'NONE',  ( -0.000000000000000000, 1.000000000000000000, -0.000000000000000000 ) ) ;
#27476 = CARTESIAN_POINT ( 'NONE',  ( 102.5899018517108772, -44.13627803831183627, 199.9499951314959674 ) ) ;
#27477 = AXIS2_PLACEMENT_3D ( 'NONE', #5348, #88476, #46200 ) ;
#27478 = LINE ( 'NONE', #33399, #30106 ) ;
#27479 = VERTEX_POINT ( 'NONE', #10885 ) ;
#27481 = EDGE_LOOP ( 'NONE', ( #35706, #29732, #39933, #28410 ) ) ;
#27480 = EDGE_LOOP ( 'NONE', ( #22191, #39475, #52552, #7704 ) ) ;
#27482 = VECTOR ( 'NONE', #82898, 1000.000000000000000 ) ;
#27483 = DIRECTION ( 'NONE',  ( -0.000000000000000000, -0.000000000000000000, -1.000000000000000000 ) ) ;
#27484 = EDGE_LOOP ( 'NONE', ( #45146, #58612, #52030, #32948 ) ) ;
#27485 = ORIENTED_EDGE ( 'NONE', *, *, #88683, .T. ) ;
#27486 = DIRECTION ( 'NONE',  ( 2.761895400282000234E-15, 0.000000000000000000, 1.000000000000000000 ) ) ;
#27487 = CARTESIAN_POINT ( 'NONE',  ( 100.0731593717985106, -30.45489967868845227, 232.1882499725639661 ) ) ;
#27488 = AXIS2_PLACEMENT_3D ( 'NONE', #40493, #25071, #33682 ) ;
#27489 = ORIENTED_EDGE ( 'NONE', *, *, #70185, .F. ) ;
#27490 = DIRECTION ( 'NONE',  ( 1.000000000000000078E-15, 1.000000000000000083E-30, -1.000000000000000000 ) ) ;
#27491 = CARTESIAN_POINT ( 'NONE',  ( -119.8041702335904546, 74.58518942925769579, 51.88336617615348700 ) ) ;
#27492 = VECTOR ( 'NONE', #15585, 1000.000000000000000 ) ;
#27493 = ORIENTED_EDGE ( 'NONE', *, *, #2020, .F. ) ;
#27495 = VERTEX_POINT ( 'NONE', #59468 ) ;
#27494 = AXIS2_PLACEMENT_3D ( 'NONE', #82483, #11632, #81136 ) ;
#27496 = DIRECTION ( 'NONE',  ( 0.000000000000000000, 1.000000000000000000, 0.000000000000000000 ) ) ;
#27497 = EDGE_LOOP ( 'NONE', ( #77513, #69428, #21992, #36876, #77609, #58430 ) ) ;
#27498 = ORIENTED_EDGE ( 'NONE', *, *, #19651, .T. ) ;
#27499 = CARTESIAN_POINT ( 'NONE',  ( 111.2851091291901042, -43.74983776777182953, 235.8252332267339852 ) ) ;
#27500 = VECTOR ( 'NONE', #3157, 999.9999999999998863 ) ;
#27501 = CARTESIAN_POINT ( 'NONE',  ( 98.43795593625375773, -42.68233540891471023, 126.8070538473389490 ) ) ;
#27502 = CARTESIAN_POINT ( 'NONE',  ( 104.1140010245780445, -46.70499295924816607, 107.3470538473389411 ) ) ;
#27503 = CARTESIAN_POINT ( 'NONE',  ( 99.21395805206054774, -38.40459780144472290, 249.5838068554171514 ) ) ;
#27504 = CYLINDRICAL_SURFACE ( 'NONE', #1754, 4.874999999999990230 ) ;
#27505 =( GEOMETRIC_REPRESENTATION_CONTEXT ( 3 ) GLOBAL_UNCERTAINTY_ASSIGNED_CONTEXT ( ( #594 ) ) GLOBAL_UNIT_ASSIGNED_CONTEXT ( ( #15036, #84545, #31332 ) ) REPRESENTATION_CONTEXT ( 'NONE', 'WORKASPACE' ) );
#27506 = CARTESIAN_POINT ( 'NONE',  ( 96.04670619665022002, -35.87009084903410638, 187.2765776568629406 ) ) ;
#27507 = CARTESIAN_POINT ( 'NONE',  ( 164.9190312289449878, -35.91149509761181235, 193.9678068554150059 ) ) ;
#27508 = DIRECTION ( 'NONE',  ( 0.000000000000000000, 0.000000000000000000, 1.000000000000000000 ) ) ;
#27509 = EDGE_LOOP ( 'NONE', ( #57301, #82291, #55633, #47866 ) ) ;
#27510 = CARTESIAN_POINT ( 'NONE',  ( 130.1093520674643287, 75.84295037288963215, 10.79257909650501013 ) ) ;
#27511 = EDGE_LOOP ( 'NONE', ( #46612, #6746, #1662, #84747 ) ) ;
#27512 = ORIENTED_EDGE ( 'NONE', *, *, #84562, .F. ) ;
#27513 = VECTOR ( 'NONE', #86271, 1000.000000000000000 ) ;
#27514 = DIRECTION ( 'NONE',  ( 1.000000000000000000, 0.000000000000000000, -3.491483361109380094E-15 ) ) ;
#27515 = VERTEX_POINT ( 'NONE', #59911 ) ;
#27516 = LINE ( 'NONE', #53399, #63512 ) ;
#27517 = VECTOR ( 'NONE', #46859, 1000.000000000000114 ) ;
#27518 = CARTESIAN_POINT ( 'NONE',  ( 113.3314600845033482, -45.06233935626208620, 143.0899109901969553 ) ) ;
#27519 = CARTESIAN_POINT ( 'NONE',  ( -6.892982596720425015, 71.88311738247121241, 130.3739197406787582 ) ) ;
#27520 = DIRECTION ( 'NONE',  ( -0.4999999999999931166, -0.8660254037844425934, 2.684678751731770391E-14 ) ) ;
#27521 = CARTESIAN_POINT ( 'NONE',  ( 99.06670390244704549, -104.2784471599421181, -19.78219314458201694 ) ) ;
#27522 = ADVANCED_FACE ( 'NONE', ( #66285 ), #24086, .F. ) ;
#27525 = CARTESIAN_POINT ( 'NONE',  ( 110.4916936757735186, -26.90617889774112825, 205.8099109901969541 ) ) ;
#27524 = DIRECTION ( 'NONE',  ( -1.000000000000000000, -1.541976423090496028E-15, 0.000000000000000000 ) ) ;
#27523 = PLANE ( 'NONE',  #56534 ) ;
#27526 = CARTESIAN_POINT ( 'NONE',  ( 20.03715912545737510, -24.95799193693189721, 249.9678068554150059 ) ) ;
#27527 = DIRECTION ( 'NONE',  ( 0.000000000000000000, 0.000000000000000000, -1.000000000000000000 ) ) ;
#27528 = EDGE_LOOP ( 'NONE', ( #22681, #32052, #80260, #87141 ) ) ;
#27529 = VECTOR ( 'NONE', #5750, 1000.000000000000000 ) ;
#27530 = CARTESIAN_POINT ( 'NONE',  ( 162.8913605087219878, -31.76306994223740432, 117.4678068554150627 ) ) ;
#27531 = EDGE_CURVE ( 'NONE', #29629, #40068, #72233, .T. ) ;
#27532 = FACE_BOUND ( 'NONE', #17722, .T. ) ;
#27533 = DIRECTION ( 'NONE',  ( 1.000000000000000078E-15, 1.000000000000000083E-30, -1.000000000000000000 ) ) ;
#27534 = ADVANCED_FACE ( 'NONE', ( #39032 ), #72681, .T. ) ;
#27535 = DIRECTION ( 'NONE',  ( 0.000000000000000000, 0.000000000000000000, 1.000000000000000000 ) ) ;
#27537 = ORIENTED_EDGE ( 'NONE', *, *, #74129, .F. ) ;
#27536 = CARTESIAN_POINT ( 'NONE',  ( 105.1007409166104054, -25.80476224416663200, 275.2061014663870537 ) ) ;
#27538 = EDGE_CURVE ( 'NONE', #59703, #18271, #66743, .T. ) ;
#27539 = CARTESIAN_POINT ( 'NONE',  ( 101.1158614047228070, -28.69863163947533735, 195.5838086201111992 ) ) ;
#27540 = CARTESIAN_POINT ( 'NONE',  ( 99.03713458771083822, -43.41345219906346387, 116.8784824187679732 ) ) ;
#27541 = CARTESIAN_POINT ( 'NONE',  ( 96.95674990518240577, -32.26097187787489418, 51.98324432352996638 ) ) ;
#27542 = CARTESIAN_POINT ( 'NONE',  ( 97.34161151642148013, -42.07962167312376067, 172.7146728949589942 ) ) ;
#27543 = CARTESIAN_POINT ( 'NONE',  ( 97.06107112666785497, -37.99641220746794090, 32.42729196197263519 ) ) ;
#27544 = DIRECTION ( 'NONE',  ( 1.000000000000000078E-15, -1.000000000000000083E-30, -1.000000000000000000 ) ) ;
#27545 = AXIS2_PLACEMENT_3D ( 'NONE', #45534, #54136, #39634 ) ;
#27547 = CARTESIAN_POINT ( 'NONE',  ( -69.72411017812909506, 120.6499999999999915, -69.72411017813089984 ) ) ;
#27546 = DIRECTION ( 'NONE',  ( -1.000000000000000000, -6.493183223601999383E-14, -1.000000000000000078E-15 ) ) ;
#27548 = CARTESIAN_POINT ( 'NONE',  ( 116.3135867418571650, -32.94878190598771539, 189.1356252759109680 ) ) ;
#27549 = DIRECTION ( 'NONE',  ( 0.000000000000000000, 0.000000000000000000, 1.000000000000000000 ) ) ;
#27550 = ORIENTED_EDGE ( 'NONE', *, *, #40858, .F. ) ;
#27551 = EDGE_CURVE ( 'NONE', #66630, #34986, #59018, .T. ) ;
#27552 = EDGE_CURVE ( 'NONE', #60401, #44708, #3625, .T. ) ;
#27553 = ORIENTED_EDGE ( 'NONE', *, *, #3237, .F. ) ;
#27554 = ORIENTED_EDGE ( 'NONE', *, *, #25032, .F. ) ;
#27555 = VECTOR ( 'NONE', #84690, 1000.000000000000000 ) ;
#27556 = ORIENTED_EDGE ( 'NONE', *, *, #23918, .T. ) ;
#27557 = CARTESIAN_POINT ( 'NONE',  ( 134.5667039024480118, -50.82844715994100682, 280.9178068554149945 ) ) ;
#27558 = CARTESIAN_POINT ( 'NONE',  ( 116.6546583390152279, -32.60254457569000408, 75.14991099019697174 ) ) ;
#27559 = CARTESIAN_POINT ( 'NONE',  ( 92.81551872686561921, -95.01002112898652285, -11.78219314458228695 ) ) ;
#27560 = EDGE_CURVE ( 'NONE', #23949, #35428, #77056, .T. ) ;
#27562 = FACE_OUTER_BOUND ( 'NONE', #82490, .T. ) ;
#27561 = VECTOR ( 'NONE', #79741, 1000.000000000000000 ) ;
#27563 = CARTESIAN_POINT ( 'NONE',  ( 116.8358708857152095, -40.58912082693117185, 189.5270538473389479 ) ) ;
#27564 = CARTESIAN_POINT ( 'NONE',  ( -89.60916260784479448, 239.0000000000000000, 134.1927865330827103 ) ) ;
#27565 = CARTESIAN_POINT ( 'NONE',  ( 98.95807093800334542, -41.73853705562144967, 11.76800622829293808 ) ) ;
#27566 = VERTEX_POINT ( 'NONE', #39485 ) ;
#27567 = EDGE_CURVE ( 'NONE', #38934, #57278, #86756, .T. ) ;
#27568 = ORIENTED_EDGE ( 'NONE', *, *, #72395, .T. ) ;
#27570 = EDGE_LOOP ( 'NONE', ( #68234, #41846, #25490, #89053, #84469 ) ) ;
#27569 = VECTOR ( 'NONE', #70767, 1000.000000000000000 ) ;
#27571 = CARTESIAN_POINT ( 'NONE',  ( 70.56670390244700286, -67.87844715994098976, 222.2178068554179902 ) ) ;
#27572 = CARTESIAN_POINT ( 'NONE',  ( 116.3262419368496978, -32.93860311337579105, 160.1356252759109680 ) ) ;
#27573 = CARTESIAN_POINT ( 'NONE',  ( 109.7260717835659563, -27.00112607981847290, 19.86400788967373998 ) ) ;
#27574 = DIRECTION ( 'NONE',  ( 0.000000000000000000, 1.000000000000000000, 0.000000000000000000 ) ) ;
#27575 = DIRECTION ( 'NONE',  ( 0.000000000000000000, 0.000000000000000000, 1.000000000000000000 ) ) ;
#27576 = DIRECTION ( 'NONE',  ( 0.000000000000000000, 0.000000000000000000, -1.000000000000000000 ) ) ;
#27577 = VECTOR ( 'NONE', #8293, 1000.000000000000000 ) ;
#27578 = CARTESIAN_POINT ( 'NONE',  ( -77.39114642429849766, 120.6499999999999915, -71.77848634863219957 ) ) ;
#27579 = CARTESIAN_POINT ( 'NONE',  ( 115.6529839569025455, -41.48189714014875307, 263.4241967044829948 ) ) ;
#27580 = CARTESIAN_POINT ( 'NONE',  ( 193.0374249753376432, -23.42844715993431848, 193.9678068554150343 ) ) ;
#27581 = ORIENTED_EDGE ( 'NONE', *, *, #88734, .T. ) ;
#27582 = ADVANCED_FACE ( 'NONE', ( #45389 ), #18143, .F. ) ;
#27583 = DIRECTION ( 'NONE',  ( 0.5773502691896260641, -0.5773502691896252870, 0.5773502691896260641 ) ) ;
#27584 = AXIS2_PLACEMENT_3D ( 'NONE', #50307, #8552, #56679 ) ;
#27585 = EDGE_CURVE ( 'NONE', #7937, #10881, #75551, .T. ) ;
#27586 = DIRECTION ( 'NONE',  ( 1.387778780781444492E-15, 0.000000000000000000, -1.000000000000000000 ) ) ;
#27587 = CARTESIAN_POINT ( 'NONE',  ( 98.46239236780679960, -37.66247686286469332, 79.21856656006798403 ) ) ;
#27588 = DIRECTION ( 'NONE',  ( 0.000000000000000000, 0.000000000000000000, 1.000000000000000000 ) ) ;
#27589 = CIRCLE ( 'NONE', #78395, 7.143750000000001599 ) ;
#27590 = DIRECTION ( 'NONE',  ( 0.000000000000000000, 1.000000000000000000, 0.000000000000000000 ) ) ;
#27591 = EDGE_LOOP ( 'NONE', ( #54698, #59494, #49061, #89436 ) ) ;
#27592 = CARTESIAN_POINT ( 'NONE',  ( 77.55659459556528645, -35.60518703965896492, 7.068229416970963186 ) ) ;
#27593 = VERTEX_POINT ( 'NONE', #73556 ) ;
#27594 = CARTESIAN_POINT ( 'NONE',  ( 118.9178230750475649, -36.92810663041961305, 153.8127681330539644 ) ) ;
#27595 = ORIENTED_EDGE ( 'NONE', *, *, #57971, .T. ) ;
#27596 = CARTESIAN_POINT ( 'NONE',  ( 99.04406189553675688, -42.84125768779406229, 67.84395861402028061 ) ) ;
#27597 = CARTESIAN_POINT ( 'NONE',  ( 99.34829255622855726, -41.08350393070648465, 133.1672975916119697 ) ) ;
#27598 = CARTESIAN_POINT ( 'NONE',  ( 194.0371591254573502, -24.89890238294407965, 249.9678068554149775 ) ) ;
#27599 = CARTESIAN_POINT ( 'NONE',  ( 97.06670390244703128, -109.9573555057414609, 7.717806855418146483 ) ) ;
#27600 = CARTESIAN_POINT ( 'NONE',  ( 107.3215613407866584, -25.65604926530302166, 71.04610146638795243 ) ) ;
#27601 = EDGE_CURVE ( 'NONE', #30540, #87253, #67186, .T. ) ;
#27602 = CARTESIAN_POINT ( 'NONE',  ( 117.0718954858506038, -35.46248235908498714, 84.92729194235329260 ) ) ;
#27603 = ORIENTED_EDGE ( 'NONE', *, *, #80368, .F. ) ;
#27604 = CARTESIAN_POINT ( 'NONE',  ( -117.9190617242382046, 79.25941250729457010, -12.27333445685015967 ) ) ;
#27605 = ORIENTED_EDGE ( 'NONE', *, *, #48735, .F. ) ;
#27606 = ORIENTED_EDGE ( 'NONE', *, *, #73041, .T. ) ;
#27607 = VECTOR ( 'NONE', #27240, 1000.000000000000000 ) ;
#27608 = LINE ( 'NONE', #48920, #58618 ) ;
#27609 = ORIENTED_EDGE ( 'NONE', *, *, #44468, .T. ) ;
#27610 = CARTESIAN_POINT ( 'NONE',  ( 116.8729656461675148, -36.55725972750698105, 288.8413395616257731 ) ) ;
#27611 = CARTESIAN_POINT ( 'NONE',  ( 101.9613826146451885, -46.55915482862852173, 163.1832443235299763 ) ) ;
#27612 = CARTESIAN_POINT ( 'NONE',  ( 5.635505087355097587, 71.13841253056517644, -118.4244851085658468 ) ) ;
#27613 = CARTESIAN_POINT ( 'NONE',  ( 97.31584371250237098, -39.30597598563051065, 142.5314586081371147 ) ) ;
#27614 = CARTESIAN_POINT ( 'NONE',  ( 97.22566771925157525, -31.69632393854739760, 91.96229194257693962 ) ) ;
#27615 = FACE_OUTER_BOUND ( 'NONE', #62197, .T. ) ;
#27616 = ORIENTED_EDGE ( 'NONE', *, *, #27538, .F. ) ;
#27617 = CARTESIAN_POINT ( 'NONE',  ( 51.39690000000000225, 82.54999999999999716, 335.3740053999999304 ) ) ;
#27618 = CIRCLE ( 'NONE', #82762, 4.762500000000002842 ) ;
#27619 = LINE ( 'NONE', #55302, #14318 ) ;
#27621 = ORIENTED_EDGE ( 'NONE', *, *, #84101, .T. ) ;
#27620 = EDGE_CURVE ( 'NONE', #25005, #40315, #81300, .T. ) ;
#27622 = CIRCLE ( 'NONE', #21875, 16.00000000000090239 ) ;
#27623 = DIRECTION ( 'NONE',  ( 0.000000000000000000, -1.000000000000000000, 0.000000000000000000 ) ) ;
#27624 = DIRECTION ( 'NONE',  ( -6.524622321627019585E-16, -4.013151879589939944E-16, -1.000000000000000000 ) ) ;
#27625 = CARTESIAN_POINT ( 'NONE',  ( 115.3062145713272599, -45.21207857638187022, 268.1899109901965517 ) ) ;
#27626 = DIRECTION ( 'NONE',  ( 1.000000000000000078E-15, -1.000000000000000083E-30, -1.000000000000000000 ) ) ;
#27627 = ADVANCED_FACE ( 'NONE', ( #20401 ), #33564, .F. ) ;
#27628 = CARTESIAN_POINT ( 'NONE',  ( 141.0664832912740110, -8.729447159940896483, 14.82207188531772957 ) ) ;
#27629 = LINE ( 'NONE', #53963, #67892 ) ;
#27630 = EDGE_CURVE ( 'NONE', #5834, #55364, #82641, .T. ) ;
#27631 = CARTESIAN_POINT ( 'NONE',  ( 110.9231077663976066, -44.92578233336853799, 287.3371817328388147 ) ) ;
#27633 = CARTESIAN_POINT ( 'NONE',  ( 103.3702027031294648, -47.12181610991854086, 98.31657765686297523 ) ) ;
#27632 = CARTESIAN_POINT ( 'NONE',  ( 116.1804594027163517, -40.96476762480074996, 6.826283056785800163 ) ) ;
#27634 = CARTESIAN_POINT ( 'NONE',  ( -31.75000000000000000, 8.255000000000000782, -3.174999999999779998 ) ) ;
#27635 = CARTESIAN_POINT ( 'NONE',  ( 107.6554820827327461, -47.17179587048914158, 152.6213395616249500 ) ) ;
#27636 = CARTESIAN_POINT ( 'NONE',  ( -479.3614999999999782, 10.16305401447644030, 97.63125000000000853 ) ) ;
#27637 = ORIENTED_EDGE ( 'NONE', *, *, #45866, .F. ) ;
#27638 = CIRCLE ( 'NONE', #18952, 2.517500000000005844 ) ;
#27639 = DIRECTION ( 'NONE',  ( 0.000000000000000000, -1.000000000000000000, 0.000000000000000000 ) ) ;
#27640 = EDGE_CURVE ( 'NONE', #80786, #23384, #67641, .T. ) ;
#27641 = FACE_BOUND ( 'NONE', #89433, .T. ) ;
#27642 = CARTESIAN_POINT ( 'NONE',  ( -487.2989999999999782, 18.41194598552324990, 83.34375000000000000 ) ) ;
#27643 = ORIENTED_EDGE ( 'NONE', *, *, #46375, .F. ) ;
#27644 = FACE_OUTER_BOUND ( 'NONE', #2843, .T. ) ;
#27646 = VERTEX_POINT ( 'NONE', #47174 ) ;
#27645 = CARTESIAN_POINT ( 'NONE',  ( 117.7486274683349308, -39.74683136594191524, 143.6194347997209775 ) ) ;
#27647 = DIRECTION ( 'NONE',  ( -1.000000000000000000, -8.163404592832032979E-16, 0.000000000000000000 ) ) ;
#27648 = CARTESIAN_POINT ( 'NONE',  ( 101.4135918642175369, -46.25467808933209568, 203.1622919425779514 ) ) ;
#27649 =( GEOMETRIC_REPRESENTATION_CONTEXT ( 3 ) GLOBAL_UNCERTAINTY_ASSIGNED_CONTEXT ( ( #72339 ) ) GLOBAL_UNIT_ASSIGNED_CONTEXT ( ( #81063, #6523, #47386 ) ) REPRESENTATION_CONTEXT ( 'NONE', 'WORKASPACE' ) );
#27650 = CARTESIAN_POINT ( 'NONE',  ( 98.64078293412623566, 73.86195533656253076, 85.52748787272882680 ) ) ;
#27651 = LINE ( 'NONE', #89441, #64835 ) ;
#27652 = PLANE ( 'NONE',  #77155 ) ;
#27653 = ORIENTED_EDGE ( 'NONE', *, *, #57080, .T. ) ;
#27654 = ADVANCED_FACE ( 'NONE', ( #19491 ), #13570, .T. ) ;
#27655 = ITEM_DEFINED_TRANSFORMATION ( 'NONE', 'NONE', #76857,  #50656 ) ;
#27656 = EDGE_LOOP ( 'NONE', ( #80474, #16810, #11390, #34051, #38172, #19813 ) ) ;
#27657 = EDGE_CURVE ( 'NONE', #82307, #37791, #7213, .T. ) ;
#27659 = ORIENTED_EDGE ( 'NONE', *, *, #244, .T. ) ;
#27658 = VECTOR ( 'NONE', #75656, 1000.000000000000000 ) ;
#27660 = VECTOR ( 'NONE', #66980, 1000.000000000000000 ) ;
#27661 = ORIENTED_EDGE ( 'NONE', *, *, #969, .T. ) ;
#27662 = DIRECTION ( 'NONE',  ( 1.639958061481212836E-42, -4.100000000000000342E-29, -1.000000000000000000 ) ) ;
#27663 = CARTESIAN_POINT ( 'NONE',  ( 101.4253818664906959, -46.23481170842615740, 203.1622919425779514 ) ) ;
#27664 = CARTESIAN_POINT ( 'NONE',  ( 77.31648329127402519, -36.72944715994107412, -5.074374724089059541 ) ) ;
#27665 = CARTESIAN_POINT ( 'NONE',  ( 135.0140782791311551, -16.14703303315377880, 1.764000745017878069 ) ) ;
#27666 = B_SPLINE_CURVE_WITH_KNOTS ( 'NONE', 3,
 ( #39657, #11061, #4257, #60541, #25588, #80572, #31952, #66926, #4707, #32386, #60088, #87824, #53261, #81030, #46459, #11973, #32846, #13752, #15101, #75979, #41882, #42776, #84157, #34639, #47803, #20580, #48247, #34183, #55055, #20129, #62344, #83700, #40999, #69618, #82815, #69167, #63249, #35077, #41437, #21930, #61888, #75539, #70519, #6937, #13312, #42331, #124, #68719, #27823, #55502 ),
 .UNSPECIFIED., .F., .F.,
 ( 4, 2, 1, 1, 1, 1, 1, 2, 2, 2, 2, 2, 2, 2, 1, 1, 1, 1, 1, 1, 1, 2, 2, 2, 2, 2, 2, 2, 2, 2, 4 ),
 ( 0.5000148065476123227, 0.5002589399428646333, 0.5005030733381169439, 0.5009913401286217871, 0.5019678737096311405, 0.5039209408716495142, 0.5078270751956860396, 0.5156393438437590904, 0.5312638811399049699, 0.5625129557321965068, 0.6250111049167789146, 0.6875092541013613223, 0.7500074032859437301, 0.7500684366347565302, 0.7501294699835694413, 0.7502515366812014808, 0.7504956700764423561, 0.7509839368669025683, 0.7519604704478229928, 0.7539135376096571806, 0.7578196719333130105, 0.7656319405806258915, 0.7812564778752518757, 0.8125055524645015126, 0.8437546270537512605, 0.8750037016430010084, 0.9062527762322506453, 0.9375018508215002822, 0.9687509254107500301, 0.9843754627053750150, 1.000000000000000000 ),
 .UNSPECIFIED. ) ;
#27667 = EDGE_CURVE ( 'NONE', #22899, #50035, #24777, .T. ) ;
#27669 = CARTESIAN_POINT ( 'NONE',  ( 20.56670390244833158, -48.82844715994187368, 249.9678068554150059 ) ) ;
#27668 = CARTESIAN_POINT ( 'NONE',  ( -100.8961411191535973, 127.0000000000000000, -3.968750000001104894 ) ) ;
#27670 = DIRECTION ( 'NONE',  ( -1.224646799147355426E-16, 0.000000000000000000, -1.000000000000000000 ) ) ;
#27671 = CIRCLE ( 'NONE', #78462, 3.499999999999996003 ) ;
#27672 = VERTEX_POINT ( 'NONE', #68093 ) ;
#27673 = VERTEX_POINT ( 'NONE', #5425 ) ;
#27674 = FACE_OUTER_BOUND ( 'NONE', #2187, .T. ) ;
#27675 = DIRECTION ( 'NONE',  ( 0.7071067811865516806, -0.7071067811865434649, 7.071067811865511818E-16 ) ) ;
#27676 = CARTESIAN_POINT ( 'NONE',  ( 97.40895461294502411, -34.98419235835276453, 237.1841967044819626 ) ) ;
#27677 = DIRECTION ( 'NONE',  ( 1.000000000000000000, 0.000000000000000000, 0.000000000000000000 ) ) ;
#27678 = CARTESIAN_POINT ( 'NONE',  ( 102.0841886111852688, -27.63463957783716651, 96.46324432352997746 ) ) ;
#27679 = FACE_OUTER_BOUND ( 'NONE', #42620, .T. ) ;
#27680 = VECTOR ( 'NONE', #63786, 1000.000000000000000 ) ;
#27681 = CARTESIAN_POINT ( 'NONE',  ( 115.1188116510141128, -30.76893447370202139, 20.33360764784250208 ) ) ;
#27683 = EDGE_LOOP ( 'NONE', ( #30737, #29118, #75522, #32618, #76434, #15389, #64611, #88332, #85353, #38240, #82362, #48608, #11370, #70577, #82651, #63418, #38392, #80158, #30370, #41551, #31009, #84221, #59569, #84338, #67190, #6136, #65853, #11174, #74473, #89284, #30884, #69449, #9945, #53652, #64707, #61325, #29034, #1146, #77022, #46230, #13388, #82990, #39671, #69180, #69937, #42062, #66931, #16182 ) ) ;
#27682 = AXIS2_PLACEMENT_3D ( 'NONE', #71255, #1306, #36271 ) ;
#27684 = CARTESIAN_POINT ( 'NONE',  ( 45.56670390244828184, -48.82844715994087892, 300.4678068554150059 ) ) ;
#27685 = VERTEX_POINT ( 'NONE', #5878 ) ;
#27686 = ORIENTED_EDGE ( 'NONE', *, *, #35254, .T. ) ;
#27687 = EDGE_CURVE ( 'NONE', #18505, #42340, #61266, .T. ) ;
#27688 = DIRECTION ( 'NONE',  ( -1.000000000000000000, 0.000000000000000000, 0.000000000000000000 ) ) ;
#27689 = CARTESIAN_POINT ( 'NONE',  ( 107.8719782714504873, -26.68843711164719323, 261.4444404487539941 ) ) ;
#27690 = AXIS2_PLACEMENT_3D ( 'NONE', #838, #28527, #35793 ) ;
#27691 = CARTESIAN_POINT ( 'NONE',  ( 172.5664832912729878, -27.82844715994070484, 138.9256252759119832 ) ) ;
#27692 = CARTESIAN_POINT ( 'NONE',  ( 115.8251266376895074, -31.72949007719681092, 139.2398401005303299 ) ) ;
#27693 = DIRECTION ( 'NONE',  ( -1.000000000000000000, -8.163404592832032979E-16, 0.000000000000000000 ) ) ;
#27694 = LINE ( 'NONE', #8153, #45894 ) ;
#27695 = VERTEX_POINT ( 'NONE', #34901 ) ;
#27696 = CARTESIAN_POINT ( 'NONE',  ( -57.91199999999999903, 101.5999999999999943, 191.3008000794699797 ) ) ;
#27697 = CARTESIAN_POINT ( 'NONE',  ( 97.81170003938157720, -40.51743348276853851, 42.63567940883270069 ) ) ;
#27698 = VERTEX_POINT ( 'NONE', #62613 ) ;
#27699 = CARTESIAN_POINT ( 'NONE',  ( 97.80902780829600829, -29.33079837672297074, 45.78991099019697231 ) ) ;
#27700 = ORIENTED_EDGE ( 'NONE', *, *, #45860, .F. ) ;
#27702 = VECTOR ( 'NONE', #56323, 1000.000000000000000 ) ;
#27701 = CARTESIAN_POINT ( 'NONE',  ( 114.4813385407417741, -41.19272473522806166, 276.2014237029247852 ) ) ;
#27703 = CARTESIAN_POINT ( 'NONE',  ( 117.0611684525443650, -38.07849049335855085, 128.7190349916091066 ) ) ;
#27704 = CARTESIAN_POINT ( 'NONE',  ( 116.9310496459150244, -33.53114825773879915, 134.0880062282919880 ) ) ;
#27705 = EDGE_CURVE ( 'NONE', #21321, #24090, #88987, .T. ) ;
#27706 = DIRECTION ( 'NONE',  ( 0.000000000000000000, 0.000000000000000000, 1.000000000000000000 ) ) ;
#27707 = DIRECTION ( 'NONE',  ( 0.000000000000000000, -1.000000000000000000, 0.000000000000000000 ) ) ;
#27708 = PLANE ( 'NONE',  #5723 ) ;
#27709 = CARTESIAN_POINT ( 'NONE',  ( 7.373078322898753534, 72.20904964896763545, 130.3475976157996570 ) ) ;
#27710 = CARTESIAN_POINT ( 'NONE',  ( 96.20418022731425367, -34.44737123974878301, 257.1737205140064475 ) ) ;
#27711 = PLANE ( 'NONE',  #89179 ) ;
#27712 = EDGE_LOOP ( 'NONE', ( #62158, #46031, #26219, #69321 ) ) ;
#27713 = EDGE_CURVE ( 'NONE', #8740, #50121, #48071, .T. ) ;
#27714 = CARTESIAN_POINT ( 'NONE',  ( 70.06670417066790435, -71.37844715994097555, 222.2178068554179902 ) ) ;
#27715 = ORIENTED_EDGE ( 'NONE', *, *, #39623, .T. ) ;
#27716 = CARTESIAN_POINT ( 'NONE',  ( 109.2641226286370824, -47.00117516105910198, 103.7441967044829880 ) ) ;
#27717 = CARTESIAN_POINT ( 'NONE',  ( 122.8247853069674136, 44.79825420117990120, -44.26074039117278147 ) ) ;
#27718 = VERTEX_POINT ( 'NONE', #54425 ) ;
#27719 = EDGE_LOOP ( 'NONE', ( #49376, #77465, #88450, #30685 ) ) ;
#27720 = ORIENTED_EDGE ( 'NONE', *, *, #76037, .F. ) ;
#27721 = AXIS2_PLACEMENT_3D ( 'NONE', #24547, #10029, #86775 ) ;
#27722 = CARTESIAN_POINT ( 'NONE',  ( 172.5664832912729878, -27.82844715994070484, 18.92562527591200094 ) ) ;
#27723 = CARTESIAN_POINT ( 'NONE',  ( 106.5667039024470171, -96.29408744860641889, -19.78219314458226563 ) ) ;
#27724 = LINE ( 'NONE', #61776, #10291 ) ;
#27725 = DIRECTION ( 'NONE',  ( -1.000000000000000078E-15, 1.000000000000000083E-30, 1.000000000000000000 ) ) ;
#27726 = CARTESIAN_POINT ( 'NONE',  ( 114.8576755932693487, -34.29489411463138282, 171.8852332267339591 ) ) ;
#27727 = CARTESIAN_POINT ( 'NONE',  ( 96.51501197915654018, -40.09867661842082498, 277.5603871806729899 ) ) ;
#27728 = CARTESIAN_POINT ( 'NONE',  ( 108.3317990709242480, -46.73504955168621677, 58.67715742008988400 ) ) ;
#27729 = ORIENTED_EDGE ( 'NONE', *, *, #58094, .F. ) ;
#27730 = CARTESIAN_POINT ( 'NONE',  ( 80.54920390244802775, -43.72944715994108833, 231.5838068554169524 ) ) ;
#27731 = PLANE ( 'NONE',  #73696 ) ;
#27732 = ORIENTED_EDGE ( 'NONE', *, *, #61778, .T. ) ;
#27733 = ORIENTED_EDGE ( 'NONE', *, *, #60852, .F. ) ;
#27734 = AXIS2_PLACEMENT_3D ( 'NONE', #5043, #32741, #86826 ) ;
#27735 = CARTESIAN_POINT ( 'NONE',  ( 36.23715912545344509, -47.82818131006131779, 129.9678068554150911 ) ) ;
#27736 = FACE_OUTER_BOUND ( 'NONE', #2199, .T. ) ;
#27737 = CARTESIAN_POINT ( 'NONE',  ( 109.7248310533103819, -27.00079495799194973, 14.86479478277475863 ) ) ;
#27738 = DIRECTION ( 'NONE',  ( 1.000000000000000078E-15, -1.000000000000000083E-30, -1.000000000000000000 ) ) ;
#27739 = DIRECTION ( 'NONE',  ( 0.000000000000000000, 0.000000000000000000, 1.000000000000000000 ) ) ;
#27740 = EDGE_CURVE ( 'NONE', #32183, #638, #56727, .T. ) ;
#27741 = CARTESIAN_POINT ( 'NONE',  ( 115.0373743241724327, -39.87857374794037923, 192.9495626852199450 ) ) ;
#27742 = CARTESIAN_POINT ( 'NONE',  ( 107.3221093067165128, -25.63226107660779007, 75.04610146638695767 ) ) ;
#27743 = DIRECTION ( 'NONE',  ( 0.000000000000000000, 0.000000000000000000, -1.000000000000000000 ) ) ;
#27744 = VERTEX_POINT ( 'NONE', #47626 ) ;
#27745 = EDGE_CURVE ( 'NONE', #69050, #45263, #40820, .T. ) ;
#27746 = LINE ( 'NONE', #76799, #51333 ) ;
#27747 = ORIENTED_EDGE ( 'NONE', *, *, #20963, .T. ) ;
#27748 = VECTOR ( 'NONE', #37964, 1000.000000000000000 ) ;
#27749 = CARTESIAN_POINT ( 'NONE',  ( 219.9639999999999986, 40.03750000000000142, -7.937500000000000000 ) ) ;
#27750 = ADVANCED_FACE ( 'NONE', ( #68542 ), #6311, .F. ) ;
#27751 = ORIENTED_EDGE ( 'NONE', *, *, #28319, .F. ) ;
#27752 = CARTESIAN_POINT ( 'NONE',  ( 182.3467384525650061, -29.62846900982231446, -5.074374724088000832 ) ) ;
#27753 = LINE ( 'NONE', #84084, #48754 ) ;
#27754 = CARTESIAN_POINT ( 'NONE',  ( 116.3185006702053244, -32.93849971620830530, 275.1356252759109680 ) ) ;
#27755 = AXIS2_PLACEMENT_3D ( 'NONE', #41152, #54764, #82534 ) ;
#27756 = LINE ( 'NONE', #75471, #61111 ) ;
#27757 = ORIENTED_EDGE ( 'NONE', *, *, #76446, .T. ) ;
#27758 = EDGE_CURVE ( 'NONE', #26346, #31292, #14018, .T. ) ;
#27759 = CARTESIAN_POINT ( 'NONE',  ( 117.1128946550982732, -32.06414332788899912, 59.16038718067295576 ) ) ;
#27761 = FACE_OUTER_BOUND ( 'NONE', #69057, .T. ) ;
#27760 = DIRECTION ( 'NONE',  ( -0.000000000000000000, -1.000000000000000000, -0.000000000000000000 ) ) ;
#27762 = CARTESIAN_POINT ( 'NONE',  ( 128.0667039024480118, -48.82844715994099971, 198.9178068554149945 ) ) ;
#27763 = CARTESIAN_POINT ( 'NONE',  ( 57.56670390244829605, -48.82844715994039575, 293.2178068554150627 ) ) ;
#27764 = ORIENTED_EDGE ( 'NONE', *, *, #28406, .T. ) ;
#27765 = EDGE_CURVE ( 'NONE', #4142, #11193, #59567, .T. ) ;
#27766 = AXIS2_PLACEMENT_3D ( 'NONE', #80384, #65404, #86745 ) ;
#27767 = FACE_OUTER_BOUND ( 'NONE', #88464, .T. ) ;
#27768 = CARTESIAN_POINT ( 'NONE',  ( 184.5667039024486087, -48.82844715993447693, 129.9678068554150059 ) ) ;
#27769 = DIRECTION ( 'NONE',  ( 0.000000000000000000, 0.000000000000000000, 1.000000000000000000 ) ) ;
#27770 = ORIENTED_EDGE ( 'NONE', *, *, #88763, .T. ) ;
#27771 = CARTESIAN_POINT ( 'NONE',  ( 117.6173583669683040, -42.17933576662011319, 89.44705384733997278 ) ) ;
#27773 = CARTESIAN_POINT ( 'NONE',  ( 107.7702177616926065, 127.0000000000000000, 4.179089330879380409E-13 ) ) ;
#27772 = DIRECTION ( 'NONE',  ( 0.000000000000000000, 0.000000000000000000, 1.000000000000000000 ) ) ;
#27774 = FACE_OUTER_BOUND ( 'NONE', #86592, .T. ) ;
#27775 = CARTESIAN_POINT ( 'NONE',  ( 145.3578527754884533, -139.1541231917475727, 247.4783998280190076 ) ) ;
#27776 = ORIENTED_EDGE ( 'NONE', *, *, #36572, .T. ) ;
#27777 = CARTESIAN_POINT ( 'NONE',  ( 112.9441315310008918, -44.54716313336194844, 139.0899109901959605 ) ) ;
#27779 = EDGE_LOOP ( 'NONE', ( #56418, #78714, #75814, #55871 ) ) ;
#27778 = LINE ( 'NONE', #7345, #82019 ) ;
#27780 = CIRCLE ( 'NONE', #64043, 3.000000000000002665 ) ;
#27781 = CARTESIAN_POINT ( 'NONE',  ( 99.39760893136107711, -29.69972230079153519, 271.7356252759109907 ) ) ;
#27782 = PLANE ( 'NONE',  #16442 ) ;
#27783 = CARTESIAN_POINT ( 'NONE',  ( 61.56670390244634916, -23.42844715994043270, 180.4678068554151196 ) ) ;
#27784 = LINE ( 'NONE', #77743, #25492 ) ;
#27785 = DIRECTION ( 'NONE',  ( -4.825893423866870279E-33, 0.000000000000000000, 1.000000000000000000 ) ) ;
#27786 = DIRECTION ( 'NONE',  ( 0.000000000000000000, -1.000000000000000000, 0.000000000000000000 ) ) ;
#27787 = CARTESIAN_POINT ( 'NONE',  ( -100.5868491334642272, 79.25971567868505474, 83.22961976134736517 ) ) ;
#27788 = CARTESIAN_POINT ( 'NONE',  ( 112.7790632652332050, -27.19118669266615740, 204.6470538473399756 ) ) ;
#27789 = EDGE_LOOP ( 'NONE', ( #2513, #32382, #26104, #69073 ) ) ;
#27790 = CIRCLE ( 'NONE', #80011, 1.000000000000000888 ) ;
#27791 = VERTEX_POINT ( 'NONE', #89896 ) ;
#27792 = ADVANCED_FACE ( 'NONE', ( #20836 ), #41704, .T. ) ;
#27793 = CARTESIAN_POINT ( 'NONE',  ( 111.9232213988593827, -44.14162454355680865, 174.4701547344689629 ) ) ;
#27794 = AXIS2_PLACEMENT_3D ( 'NONE', #19907, #28052, #47142 ) ;
#27795 = FACE_BOUND ( 'NONE', #20547, .T. ) ;
#27796 = CARTESIAN_POINT ( 'NONE',  ( 102.2363890476183599, -29.29987999758196793, 21.96729759161197748 ) ) ;
#27797 = CARTESIAN_POINT ( 'NONE',  ( 23.75871628398702384, 82.54999999999999716, 298.1325000000000500 ) ) ;
#27798 = ADVANCED_FACE ( 'NONE', ( #36712 ), #30343, .T. ) ;
#27799 = CARTESIAN_POINT ( 'NONE',  ( 98.30751288258193199, -41.72882199423717253, 266.7398595753476798 ) ) ;
#27800 = CARTESIAN_POINT ( 'NONE',  ( 131.0667039024480118, -61.87844715994100397, 207.5838068554149913 ) ) ;
#27801 = CARTESIAN_POINT ( 'NONE',  ( 50.03799999999999670, 101.5999999999999943, 206.3750000000000000 ) ) ;
#27802 = FACE_OUTER_BOUND ( 'NONE', #58553, .T. ) ;
#27803 = CARTESIAN_POINT ( 'NONE',  ( 106.9407056411434951, -47.75886249174727283, 232.5794347997199907 ) ) ;
#27804 = LINE ( 'NONE', #34618, #50344 ) ;
#27805 = ORIENTED_EDGE ( 'NONE', *, *, #78527, .F. ) ;
#27806 = VERTEX_POINT ( 'NONE', #84873 ) ;
#27807 = VECTOR ( 'NONE', #11263, 999.9999999999998863 ) ;
#27808 = CARTESIAN_POINT ( 'NONE',  ( 116.0667040365575104, -83.77844715994093860, 222.2178068554179902 ) ) ;
#27809 = CARTESIAN_POINT ( 'NONE',  ( -91.90730674524679955, 86.63388195152285221, -74.89049941105116659 ) ) ;
#27810 = CARTESIAN_POINT ( 'NONE',  ( 97.81442241246865876, -40.52410417640054874, 122.6357492958329374 ) ) ;
#27811 = DIRECTION ( 'NONE',  ( 0.000000000000000000, 0.000000000000000000, -1.000000000000000000 ) ) ;
#27812 = VECTOR ( 'NONE', #57816, 1000.000000000000114 ) ;
#27813 = DIRECTION ( 'NONE',  ( 0.000000000000000000, 0.000000000000000000, 1.000000000000000000 ) ) ;
#27814 = ORIENTED_EDGE ( 'NONE', *, *, #16336, .T. ) ;
#27816 = EDGE_CURVE ( 'NONE', #51066, #44952, #63945, .T. ) ;
#27815 = AXIS2_PLACEMENT_3D ( 'NONE', #45492, #44164, #57354 ) ;
#27817 = CARTESIAN_POINT ( 'NONE',  ( 98.38769172161842391, -42.09058819985752109, 7.768006228291934434 ) ) ;
#27818 = CARTESIAN_POINT ( 'NONE',  ( 96.76314818047262634, -35.13937921927007579, 266.2041967044821149 ) ) ;
#27819 = ORIENTED_EDGE ( 'NONE', *, *, #71848, .T. ) ;
#27820 = AXIS2_PLACEMENT_3D ( 'NONE', #49855, #14468, #84418 ) ;
#27821 = CARTESIAN_POINT ( 'NONE',  ( 77.33333279747652966, -37.08363404521340101, 6.775960187534254331 ) ) ;
#27822 = CARTESIAN_POINT ( 'NONE',  ( -446.0240000000000009, 53.97500000000000142, 50.79999999999999716 ) ) ;
#27823 = CARTESIAN_POINT ( 'NONE',  ( 116.5674885483476402, -33.54335893859623496, 169.0838757843391136 ) ) ;
#27824 = VECTOR ( 'NONE', #77820, 1000.000000000000000 ) ;
#27825 = CARTESIAN_POINT ( 'NONE',  ( 115.0531750927473951, -38.41541278395968817, 61.47951894101993986 ) ) ;
#27827 = B_SPLINE_CURVE_WITH_KNOTS ( 'NONE', 3,
 ( #68050, #67147, #19005, #45345, #4928, #53940, #86714, #66240, #46233, #73066, #4032, #87601, #5376, #52593, #31732, #59430, #60318, #73969, #46688, #25359, #24928, #80349, #18100, #53031, #45787, #33076, #88056, #11287, #25819, #73515, #38991, #66699, #48461, #7173, #75313, #69397, #19899, #82150, #35299, #89399, #13094, #14440, #42117, #27604, #6711, #13979, #62121, #62570 ),
 .UNSPECIFIED., .F., .F.,
 ( 4, 2, 2, 2, 2, 2, 2, 2, 2, 1, 2, 2, 2, 2, 2, 2, 2, 2, 2, 2, 2, 1, 2, 2, 4 ),
 ( 0.05960646776571126848, 0.06208927922045070352, 0.06333068494782041757, 0.06457209067519013856, 0.06705490212992959442, 0.06829630785729932929, 0.06953771358466906416, 0.07202052503940857553, 0.07326193076677831040, 0.07450333649414805914, 0.07574474222151779401, 0.07698614794888752888, 0.07946895940362701249, 0.08195177085836649611, 0.08319317658573623098, 0.08443458231310596585, 0.08691739376784544946, 0.08815879949521518433, 0.08940020522258490532, 0.09188301667732433342, 0.09312442240469404053, 0.09436582813206376152, 0.09560723385943348251, 0.09684863958680320351, 0.09933145104154258997 ),
 .UNSPECIFIED. ) ;
#27826 = CARTESIAN_POINT ( 'NONE',  ( 117.8230732226064532, -34.08729308082334342, 160.0061014663869798 ) ) ;
#27828 = CARTESIAN_POINT ( 'NONE',  ( 41.56648329127399677, 0.2215528400590013880, 18.92562527591200094 ) ) ;
#27829 = EDGE_LOOP ( 'NONE', ( #79370, #51516, #55460, #32755 ) ) ;
#27830 = DIRECTION ( 'NONE',  ( -0.7759704746411383303, 0.6307692307692303046, 0.000000000000000000 ) ) ;
#27831 = VERTEX_POINT ( 'NONE', #57126 ) ;
#27832 = ORIENTED_EDGE ( 'NONE', *, *, #57793, .T. ) ;
#27833 = CARTESIAN_POINT ( 'NONE',  ( 1.654053778667920804, 95.16954379564978694, 118.5472977239360972 ) ) ;
#27834 = EDGE_LOOP ( 'NONE', ( #32768, #3287, #42788, #14069 ) ) ;
#27835 = ORIENTED_EDGE ( 'NONE', *, *, #51290, .F. ) ;
#27836 = CARTESIAN_POINT ( 'NONE',  ( -185.9961463128564958, 101.5999999999999943, -9.525000000000000355 ) ) ;
#27837 = ADVANCED_FACE ( 'NONE', ( #69883 ), #76699, .F. ) ;
#27838 = CARTESIAN_POINT ( 'NONE',  ( 115.5093363421805606, -33.45364150533647063, 93.53146744712398686 ) ) ;
#27839 = CARTESIAN_POINT ( 'NONE',  ( 100.8099727397313217, -45.87009904342127697, 242.1108633711489517 ) ) ;
#27840 = CARTESIAN_POINT ( 'NONE',  ( 116.3579325164319869, -41.40893824611053020, 203.4556252759109611 ) ) ;
#27841 = CARTESIAN_POINT ( 'NONE',  ( 109.6376038899290393, -46.81002275840752702, 43.77562527591094721 ) ) ;
#27842 = CARTESIAN_POINT ( 'NONE',  ( 20.03715912545824906, -46.82818131006190043, 249.9678068554150059 ) ) ;
#27843 = EDGE_CURVE ( 'NONE', #63081, #58666, #2192, .T. ) ;
#27844 = CARTESIAN_POINT ( 'NONE',  ( 115.0351357599961375, -42.91115358527014934, 94.30202127052717742 ) ) ;
#27845 = EDGE_CURVE ( 'NONE', #70274, #11434, #29898, .T. ) ;
#27846 = ORIENTED_EDGE ( 'NONE', *, *, #8590, .T. ) ;
#27847 = AXIS2_PLACEMENT_3D ( 'NONE', #74911, #13573, #41264 ) ;
#27848 = DIRECTION ( 'NONE',  ( 0.000000000000000000, -0.000000000000000000, -1.000000000000000000 ) ) ;
#27849 = VECTOR ( 'NONE', #32074, 1000.000000000000000 ) ;
#27850 = CARTESIAN_POINT ( 'NONE',  ( 101.8448680821487073, -28.45912855063583891, 110.5241967044829892 ) ) ;
#27851 = CARTESIAN_POINT ( 'NONE',  ( 118.0484485056734769, -38.34478726580598362, 73.72229194257801055 ) ) ;
#27852 = CARTESIAN_POINT ( 'NONE',  ( 115.9443088281525149, -30.06633247050010382, 264.3508633711492735 ) ) ;
#27853 = ORIENTED_EDGE ( 'NONE', *, *, #34415, .F. ) ;
#27854 = CARTESIAN_POINT ( 'NONE',  ( 117.4744730450754560, -36.12879772292662039, 228.8727681330539667 ) ) ;
#27855 = FACE_OUTER_BOUND ( 'NONE', #79483, .T. ) ;
#27856 = CARTESIAN_POINT ( 'NONE',  ( -13.86911000615384104, 223.9999999999999716, 102.9892450244911828 ) ) ;
#27857 = DIRECTION ( 'NONE',  ( 0.000000000000000000, 0.000000000000000000, -1.000000000000000000 ) ) ;
#27859 = DIRECTION ( 'NONE',  ( -1.000000000000000078E-15, 1.000000000000000083E-30, 1.000000000000000000 ) ) ;
#27858 = DIRECTION ( 'NONE',  ( 0.000000000000000000, 1.000000000000000000, 0.000000000000000000 ) ) ;
#27860 = CARTESIAN_POINT ( 'NONE',  ( 106.5510518188671227, -25.28190781890620542, 320.5359728645732389 ) ) ;
#27861 = DIRECTION ( 'NONE',  ( 0.000000000000000000, 0.000000000000000000, 1.000000000000000000 ) ) ;
#27862 = B_SPLINE_CURVE_WITH_KNOTS ( 'NONE', 3,
 ( #84773, #35247, #2542, #63874, #77953, #14833, #62956, #84332, #43401, #83415, #28438, #15274, #57032, #77494, #50218, #42951, #8920, #42501 ),
 .UNSPECIFIED., .F., .F.,
 ( 4, 2, 2, 2, 2, 2, 2, 2, 4 ),
 ( 0.000000000000000000, 0.06249999995315230761, 0.1249999999063046152, 0.1874999998594569228, 0.2499999998126092304, 0.3124999997657615380, 0.3749999997189138456, 0.4374999996720661533, 0.4999999996252184609 ),
 .UNSPECIFIED. ) ;
#27863 = DIRECTION ( 'NONE',  ( 1.000000000000000078E-15, 1.000000000000000083E-30, -1.000000000000000000 ) ) ;
#27864 = ADVANCED_FACE ( 'NONE', ( #9013 ), #57584, .F. ) ;
#27865 = CARTESIAN_POINT ( 'NONE',  ( 90.44969454456403923, -20.11243780205715481, 239.5838068554169809 ) ) ;
#27866 = ADVANCED_FACE ( 'NONE', ( #78509 ), #52288, .F. ) ;
#27867 = CARTESIAN_POINT ( 'NONE',  ( 20.03715912545820288, -46.82818131006180096, 300.4678068554150059 ) ) ;
#27868 = DIRECTION ( 'NONE',  ( 0.000000000000000000, 0.000000000000000000, 1.000000000000000000 ) ) ;
#27869 = CIRCLE ( 'NONE', #85932, 0.5000000000000004441 ) ;
#27871 = ORIENTED_EDGE ( 'NONE', *, *, #30435, .F. ) ;
#27870 = LINE ( 'NONE', #77370, #68969 ) ;
#27872 = FACE_BOUND ( 'NONE', #59784, .T. ) ;
#27873 = CARTESIAN_POINT ( 'NONE',  ( 109.9663390834669912, -48.24573355310754152, 242.7727681330539724 ) ) ;
#27874 = CARTESIAN_POINT ( 'NONE',  ( 102.0818258798731506, -27.57325825325154867, 141.4727681330539895 ) ) ;
#27875 = CARTESIAN_POINT ( 'NONE',  ( 118.7023651333632159, -39.22291191012653400, 254.6584824187681022 ) ) ;
#27876 = LINE ( 'NONE', #20627, #40240 ) ;
#27878 = CARTESIAN_POINT ( 'NONE',  ( 82.80005790026068269, -36.42904715602206522, 6.774297104452852381 ) ) ;
#27877 = PLANE ( 'NONE',  #49332 ) ;
#27879 = DIRECTION ( 'NONE',  ( -1.000000000000000000, -1.541976423090496028E-15, 0.000000000000000000 ) ) ;
#27880 = VECTOR ( 'NONE', #49881, 1000.000000000000000 ) ;
#27881 = DIRECTION ( 'NONE',  ( -0.9834602067153815907, -0.1811243269341220596, 0.000000000000000000 ) ) ;
#27882 = AXIS2_PLACEMENT_3D ( 'NONE', #47488, #53841, #82054 ) ;
#27883 = VERTEX_POINT ( 'NONE', #64856 ) ;
#27884 = CYLINDRICAL_SURFACE ( 'NONE', #27304, 9.999999999999998224 ) ;
#27885 = VERTEX_POINT ( 'NONE', #8558 ) ;
#27886 = AXIS2_PLACEMENT_3D ( 'NONE', #75242, #88429, #5756 ) ;
#27887 = CARTESIAN_POINT ( 'NONE',  ( 100.6939357996894557, -31.04202505589751837, 190.1695626852199439 ) ) ;
#27889 = EDGE_LOOP ( 'NONE', ( #26600, #53703, #23792, #41445 ) ) ;
#27888 = DIRECTION ( 'NONE',  ( -2.999999999999999839E-15, 1.000000000000000000, -2.999999999999999900E-30 ) ) ;
#27890 = CARTESIAN_POINT ( 'NONE',  ( 164.9190312289449878, -35.91149509761181235, -5.074374724088000832 ) ) ;
#27891 = CARTESIAN_POINT ( 'NONE',  ( 98.18688568738953393, -31.30898482519909365, 166.8899109901969950 ) ) ;
#27892 = DIRECTION ( 'NONE',  ( -0.0001713722455994998422, 0.9999999853157766072, 0.000000000000000000 ) ) ;
#27893 = DIRECTION ( 'NONE',  ( -4.237773401492740281E-14, 1.000000000000000000, 0.000000000000000000 ) ) ;
#27894 = AXIS2_PLACEMENT_3D ( 'NONE', #69554, #28657, #68657 ) ;
#27895 = CARTESIAN_POINT ( 'NONE',  ( 116.0343967343886504, -32.24059753838103859, 85.19573006588439057 ) ) ;
#27896 = CARTESIAN_POINT ( 'NONE',  ( -81.46681417397449820, 70.27900073646854651, 86.13269706310923368 ) ) ;
#27897 = DIRECTION ( 'NONE',  ( 0.7071067811865758834, -0.7071067811865192621, 7.071067811865765240E-16 ) ) ;
#27898 = CARTESIAN_POINT ( 'NONE',  ( 108.4470127171752125, -27.04659769318750762, 104.9641967044829869 ) ) ;
#27899 = VERTEX_POINT ( 'NONE', #16268 ) ;
#27900 = ORIENTED_EDGE ( 'NONE', *, *, #47771, .F. ) ;
#27901 = ORIENTED_EDGE ( 'NONE', *, *, #46886, .T. ) ;
#27902 = CARTESIAN_POINT ( 'NONE',  ( 106.9482176359816634, -27.83854490981203256, 56.51872616303998598 ) ) ;
#27903 = PLANE ( 'NONE',  #41370 ) ;
#27905 = CARTESIAN_POINT ( 'NONE',  ( 131.3179999999999836, 53.97500000000000142, 50.79999999999999716 ) ) ;
#27904 = CARTESIAN_POINT ( 'NONE',  ( 97.99937763885738207, -40.39701179870334613, 202.6327681330529629 ) ) ;
#27906 = CARTESIAN_POINT ( 'NONE',  ( 70.63919639214310564, 65.60000000000000853, 0.000000000000000000 ) ) ;
#27908 = EDGE_CURVE ( 'NONE', #28327, #8825, #1294, .T. ) ;
#27907 = CARTESIAN_POINT ( 'NONE',  ( 41.56648329127398966, -27.82844715994070484, 78.92562527591199739 ) ) ;
#27909 = DIRECTION ( 'NONE',  ( 0.000000000000000000, 0.000000000000000000, -1.000000000000000000 ) ) ;
#27910 = CIRCLE ( 'NONE', #68574, 0.5000000000000073275 ) ;
#27911 = DIRECTION ( 'NONE',  ( 1.000000000000000078E-15, -1.000000000000000083E-30, -1.000000000000000000 ) ) ;
#27912 = CARTESIAN_POINT ( 'NONE',  ( 68.47164110671278081, -69.21472957910711443, 247.4213243805862987 ) ) ;
#27913 = CARTESIAN_POINT ( 'NONE',  ( 99.70004787478420383, -45.98060041612311721, 122.0413395616249659 ) ) ;
#27914 = EDGE_LOOP ( 'NONE', ( #73979, #34940, #6964, #76147, #68824, #64288, #71338, #84818, #10416, #68186, #42179, #53112, #86580, #10718, #71184, #29498 ) ) ;
#27915 = VERTEX_POINT ( 'NONE', #9445 ) ;
#27916 = VERTEX_POINT ( 'NONE', #2643 ) ;
#27917 = LINE ( 'NONE', #16100, #38652 ) ;
#27918 = FACE_OUTER_BOUND ( 'NONE', #40727, .T. ) ;
#27919 = CARTESIAN_POINT ( 'NONE',  ( 70.63919639214310564, 49.07499999999999574, -53.97512327982435210 ) ) ;
#27920 = CARTESIAN_POINT ( 'NONE',  ( 115.1682430951150735, -35.73384980259207566, 191.7423760838769908 ) ) ;
#27921 = AXIS2_PLACEMENT_3D ( 'NONE', #10280, #86594, #3911 ) ;
#27922 = EDGE_CURVE ( 'NONE', #1768, #79680, #29000, .T. ) ;
#27923 = CARTESIAN_POINT ( 'NONE',  ( 179.1667039024460166, -28.27351298637280408, -5.074374724088000832 ) ) ;
#27924 = CARTESIAN_POINT ( 'NONE',  ( 48.45959712127301344, -26.00627455219131789, 313.9678068554150059 ) ) ;
#27925 = ORIENTED_EDGE ( 'NONE', *, *, #58031, .T. ) ;
#27927 = ORIENTED_EDGE ( 'NONE', *, *, #89170, .T. ) ;
#27926 = ORIENTED_EDGE ( 'NONE', *, *, #79574, .F. ) ;
#27928 = DIRECTION ( 'NONE',  ( 0.000000000000000000, 0.000000000000000000, 1.000000000000000000 ) ) ;
#27929 = VERTEX_POINT ( 'NONE', #37155 ) ;
#27930 = VERTEX_POINT ( 'NONE', #84428 ) ;
#27931 = LINE ( 'NONE', #76538, #75365 ) ;
#27932 = EDGE_CURVE ( 'NONE', #6555, #71592, #36258, .T. ) ;
#27933 = AXIS2_PLACEMENT_3D ( 'NONE', #69718, #34736, #62443 ) ;
#27934 = CARTESIAN_POINT ( 'NONE',  ( 104.7356562592608498, -27.62759180600148667, 241.7196785439919609 ) ) ;
#27935 = ADVANCED_FACE ( 'NONE', ( #58038 ), #8106, .F. ) ;
#27936 = ORIENTED_EDGE ( 'NONE', *, *, #71159, .F. ) ;
#27937 = LINE ( 'NONE', #42004, #18896 ) ;
#27938 = CARTESIAN_POINT ( 'NONE',  ( -114.7114918133012793, 71.08538102460907737, 62.33898210981162435 ) ) ;
#27939 = VERTEX_POINT ( 'NONE', #48958 ) ;
#27940 = ORIENTED_EDGE ( 'NONE', *, *, #78168, .T. ) ;
#27941 = CONICAL_SURFACE ( 'NONE', #12000, 1.258750000000002922, 1.029744258676650093 ) ;
#27942 = LINE ( 'NONE', #75207, #69606 ) ;
#27943 = ORIENTED_EDGE ( 'NONE', *, *, #48563, .F. ) ;
#27944 = EDGE_LOOP ( 'NONE', ( #30026, #48253, #22654, #55762, #18926, #49708, #81144, #31688, #50839, #78482, #15298, #639, #58394, #88238, #68552, #68838 ) ) ;
#27945 = ADVANCED_FACE ( 'NONE', ( #56222 ), #78058, .F. ) ;
#27946 = VECTOR ( 'NONE', #31098, 1000.000000000000000 ) ;
#27947 = CARTESIAN_POINT ( 'NONE',  ( 105.9433607271350439, -44.81451498420922519, 255.2852332267341353 ) ) ;
#27948 = CARTESIAN_POINT ( 'NONE',  ( 108.7467888895124162, -25.78085441620226348, 144.9432443235299672 ) ) ;
#27949 = CARTESIAN_POINT ( 'NONE',  ( 110.1514708964275968, -46.66481413883396812, 97.81562527591097478 ) ) ;
#27950 = CARTESIAN_POINT ( 'NONE',  ( 116.4947067722135188, -39.72538118426291476, 249.5838068554167819 ) ) ;
#27951 = DIRECTION ( 'NONE',  ( 2.900000000000000265E-14, -2.000000000000000155E-15, 1.000000000000000000 ) ) ;
#27952 = CARTESIAN_POINT ( 'NONE',  ( 113.7992560408602145, -26.97729936261201900, 235.5956252759109759 ) ) ;
#27953 = CARTESIAN_POINT ( 'NONE',  ( 160.5667039024429243, -48.82844715994099971, 129.9678068554149775 ) ) ;
#27954 = ADVANCED_FACE ( 'NONE', ( #43046 ), #63969, .T. ) ;
#27955 = LINE ( 'NONE', #70651, #208 ) ;
#27956 = EDGE_LOOP ( 'NONE', ( #83127, #57518, #17546, #41129 ) ) ;
#27957 = CARTESIAN_POINT ( 'NONE',  ( -130.1467648208192713, 75.15271101351808625, 10.33160863867537316 ) ) ;
#27958 = ORIENTED_EDGE ( 'NONE', *, *, #17456, .F. ) ;
#27959 = EDGE_LOOP ( 'NONE', ( #23355, #68983, #35646, #66886 ) ) ;
#27960 = DIRECTION ( 'NONE',  ( 1.000000000000000000, 0.000000000000000000, 0.000000000000000000 ) ) ;
#27961 = CARTESIAN_POINT ( 'NONE',  ( 103.6874411509537595, -27.31610070321936234, 136.3507228384528105 ) ) ;
#27962 = CARTESIAN_POINT ( 'NONE',  ( 97.57106248370669732, -31.07117258718254149, 130.9108633711489915 ) ) ;
#27963 = CARTESIAN_POINT ( 'NONE',  ( -11.70177394069033383, 77.61446958840116395, 130.0305271391580675 ) ) ;
#27964 = FACE_OUTER_BOUND ( 'NONE', #41622, .T. ) ;
#27965 = DIRECTION ( 'NONE',  ( 0.000000000000000000, 0.000000000000000000, 1.000000000000000000 ) ) ;
#27968 = CARTESIAN_POINT ( 'NONE',  ( 103.6457867198658391, -26.24313906103854066, 206.3394347997209763 ) ) ;
#27967 = DIRECTION ( 'NONE',  ( -1.000000000000000000, 0.000000000000000000, 0.000000000000000000 ) ) ;
#27966 = CARTESIAN_POINT ( 'NONE',  ( 162.9033555647783658, -33.89581943343814174, 313.9678068554149490 ) ) ;
#27969 = DIRECTION ( 'NONE',  ( -0.04216478779797398074, 0.9991106698809455455, 0.000000000000000000 ) ) ;
#27970 = LINE ( 'NONE', #55648, #43833 ) ;
#27971 = ORIENTED_EDGE ( 'NONE', *, *, #59207, .T. ) ;
#27972 = DIRECTION ( 'NONE',  ( 0.000000000000000000, 1.000000000000000000, 0.000000000000000000 ) ) ;
#27973 = EDGE_CURVE ( 'NONE', #18422, #18383, #15821, .T. ) ;
#27974 = VECTOR ( 'NONE', #1549, 1000.000000000000000 ) ;
#27975 = LINE ( 'NONE', #83402, #29772 ) ;
#27976 = ADVANCED_FACE ( 'NONE', ( #30779 ), #65305, .T. ) ;
#27977 = DIRECTION ( 'NONE',  ( 0.000000000000000000, 1.000000000000000000, 0.000000000000000000 ) ) ;
#27978 = EDGE_CURVE ( 'NONE', #31607, #68056, #31665, .T. ) ;
#27979 = DIRECTION ( 'NONE',  ( 0.000000000000000000, 0.000000000000000000, 1.000000000000000000 ) ) ;
#27981 = VERTEX_POINT ( 'NONE', #25296 ) ;
#27980 = CARTESIAN_POINT ( 'NONE',  ( 105.7708979221677197, -26.34060099707374292, 270.1756252759109884 ) ) ;
#27982 = DIRECTION ( 'NONE',  ( 0.000000000000000000, -1.000000000000000000, 0.000000000000000000 ) ) ;
#27983 = CARTESIAN_POINT ( 'NONE',  ( 114.2552021840540846, -45.16177683379865471, 153.1508633711489722 ) ) ;
#27984 = CARTESIAN_POINT ( 'NONE',  ( 107.1953983157108041, -26.30515493630308654, 31.06705384733893283 ) ) ;
#27985 = CARTESIAN_POINT ( 'NONE',  ( 114.3743266858445935, -29.18402207539437399, 170.4641967044829585 ) ) ;
#27986 = EDGE_CURVE ( 'NONE', #59735, #65816, #19865, .T. ) ;
#27987 = CYLINDRICAL_SURFACE ( 'NONE', #18413, 9.999999999999998224 ) ;
#27988 = DIRECTION ( 'NONE',  ( -0.000000000000000000, 1.000000000000000000, 0.000000000000000000 ) ) ;
#27990 = DIRECTION ( 'NONE',  ( 0.000000000000000000, 1.000000000000000000, 0.000000000000000000 ) ) ;
#27989 = CARTESIAN_POINT ( 'NONE',  ( 50.96943157743499597, -34.03355364505720360, 313.9678068554150059 ) ) ;
#27991 = DIRECTION ( 'NONE',  ( 0.3387333329185071573, -0.3387333329185072683, 0.8777923776952267776 ) ) ;
#27992 = CARTESIAN_POINT ( 'NONE',  ( 53.97500000000000142, 69.84999999999999432, 283.4005000000000223 ) ) ;
#27993 = ORIENTED_EDGE ( 'NONE', *, *, #48300, .T. ) ;
#27994 = CIRCLE ( 'NONE', #78786, 2.750000000000002665 ) ;
#27995 = CARTESIAN_POINT ( 'NONE',  ( 21.03715912545824551, -47.82818131006186491, 300.4678068554150059 ) ) ;
#27996 = EDGE_LOOP ( 'NONE', ( #5231, #23731, #24434, #70641 ) ) ;
#27997 = ORIENTED_EDGE ( 'NONE', *, *, #3964, .T. ) ;
#27998 = ORIENTED_EDGE ( 'NONE', *, *, #64168, .T. ) ;
#27999 = CARTESIAN_POINT ( 'NONE',  ( 107.8666756518570793, -26.35696637107995954, 66.01562527591097762 ) ) ;
#28000 = PLANE ( 'NONE',  #65819 ) ;
#28001 = CARTESIAN_POINT ( 'NONE',  ( 145.1692508678690103, -139.0365492197044546, 246.8416124795636222 ) ) ;
#28002 = CARTESIAN_POINT ( 'NONE',  ( 109.8676264040644526, -26.64249633179236909, 170.8613395616249591 ) ) ;
#28003 = CARTESIAN_POINT ( 'NONE',  ( 101.4793796374089965, -43.85664460571122447, 276.4819436376007502 ) ) ;
#28004 = ORIENTED_EDGE ( 'NONE', *, *, #81789, .F. ) ;
#28005 = ORIENTED_EDGE ( 'NONE', *, *, #31210, .F. ) ;
#28006 = VERTEX_POINT ( 'NONE', #87093 ) ;
#28007 = CIRCLE ( 'NONE', #7718, 38.10000000000000142 ) ;
#28008 = CARTESIAN_POINT ( 'NONE',  ( 80.06648329127398256, -8.729447159941058132, 4.925625275910944012 ) ) ;
#28009 = LINE ( 'NONE', #62979, #18819 ) ;
#28011 = TOROIDAL_SURFACE ( 'NONE', #78810, 13.50000000000000000, 0.5000000000000000000 ) ;
#28010 = FACE_OUTER_BOUND ( 'NONE', #53846, .T. ) ;
#28012 = DIRECTION ( 'NONE',  ( 0.000000000000000000, -1.000000000000000000, 0.000000000000000000 ) ) ;
#28013 = CARTESIAN_POINT ( 'NONE',  ( 98.64044413062926253, 91.23859726994550101, 85.52787878288761192 ) ) ;
#28014 = CARTESIAN_POINT ( 'NONE',  ( 183.5150000000000148, 37.33800000000000097, 69.13087104677069306 ) ) ;
#28015 = VECTOR ( 'NONE', #16327, 1000.000000000000000 ) ;
#28016 = CARTESIAN_POINT ( 'NONE',  ( 41.56648329127398966, -27.82844715994070484, 18.92562527591200094 ) ) ;
#28017 = CARTESIAN_POINT ( 'NONE',  ( 163.0664832912739826, 19.62155284005901024, 333.4006252759110112 ) ) ;
#28018 = CARTESIAN_POINT ( 'NONE',  ( 100.5643946202652330, -27.81952766013690237, 30.56610146638794134 ) ) ;
#28019 = CARTESIAN_POINT ( 'NONE',  ( -105.4788588808464027, 120.6499999999999915, 3.968749999998844924 ) ) ;
#28020 = ORIENTED_EDGE ( 'NONE', *, *, #74936, .T. ) ;
#28021 = DIRECTION ( 'NONE',  ( 0.000000000000000000, -1.000000000000000000, 0.000000000000000000 ) ) ;
#28022 = DIRECTION ( 'NONE',  ( -1.000000000000000000, 6.036837696399408848E-13, 0.000000000000000000 ) ) ;
#28023 = CARTESIAN_POINT ( 'NONE',  ( 115.1349747707284479, -33.59889284931170295, 91.92713798863898944 ) ) ;
#28024 = EDGE_CURVE ( 'NONE', #69770, #28373, #74117, .T. ) ;
#28025 = AXIS2_PLACEMENT_3D ( 'NONE', #77726, #43622, #8688 ) ;
#28026 = EDGE_CURVE ( 'NONE', #88995, #70782, #58469, .T. ) ;
#28027 = FACE_OUTER_BOUND ( 'NONE', #71865, .T. ) ;
#28028 = FACE_OUTER_BOUND ( 'NONE', #54785, .T. ) ;
#28029 = ORIENTED_EDGE ( 'NONE', *, *, #68926, .F. ) ;
#28030 = VERTEX_POINT ( 'NONE', #59363 ) ;
#28031 = ADVANCED_FACE ( 'NONE', ( #10339 ), #67083, .F. ) ;
#28032 = FACE_OUTER_BOUND ( 'NONE', #63560, .T. ) ;
#28033 = VERTEX_POINT ( 'NONE', #86646 ) ;
#28034 = VERTEX_POINT ( 'NONE', #52085 ) ;
#28035 = EDGE_CURVE ( 'NONE', #84376, #68878, #52526, .T. ) ;
#28036 = CARTESIAN_POINT ( 'NONE',  ( 103.8797721312301405, -101.8611209747514010, -19.78219314458209865 ) ) ;
#28037 = CARTESIAN_POINT ( 'NONE',  ( 98.17580767689473475, -36.86367352702462341, 132.7701547344679511 ) ) ;
#28038 = EDGE_CURVE ( 'NONE', #78082, #78823, #48025, .T. ) ;
#28039 = CARTESIAN_POINT ( 'NONE',  ( 75.31670390244798341, -57.40094715994099772, 63.03480685541479289 ) ) ;
#28040 = CARTESIAN_POINT ( 'NONE',  ( 113.3555096308132022, -27.61169779702804306, 85.60800622829195561 ) ) ;
#28041 = EDGE_CURVE ( 'NONE', #30366, #970, #87536, .T. ) ;
#28042 = LINE ( 'NONE', #35752, #19855 ) ;
#28043 = ORIENTED_EDGE ( 'NONE', *, *, #86522, .T. ) ;
#28044 = CARTESIAN_POINT ( 'NONE',  ( 77.39114642429960611, 120.6499999999999915, -71.77848634863110533 ) ) ;
#28045 = VERTEX_POINT ( 'NONE', #4860 ) ;
#28046 = ORIENTED_EDGE ( 'NONE', *, *, #81708, .F. ) ;
#28047 = ADVANCED_FACE ( 'NONE', ( #34344 ), #82085, .F. ) ;
#28048 = PLANE ( 'NONE',  #32560 ) ;
#28049 = VERTEX_POINT ( 'NONE', #60254 ) ;
#28050 = CARTESIAN_POINT ( 'NONE',  ( 105.9660763718858618, -46.48152545022894344, 282.4870538473400643 ) ) ;
#28051 = CARTESIAN_POINT ( 'NONE',  ( 102.3833470591291785, -26.69184581432750747, 131.4118157521009778 ) ) ;
#28052 = DIRECTION ( 'NONE',  ( -2.900000000000000265E-14, 2.000000000000000155E-15, -1.000000000000000000 ) ) ;
#28053 = CARTESIAN_POINT ( 'NONE',  ( 100.9546728181673245, -28.70702572214929305, 141.5939586085704036 ) ) ;
#28054 = CARTESIAN_POINT ( 'NONE',  ( 96.79170515468972269, -38.49336940632627346, 87.46133956162493917 ) ) ;
#28055 = EDGE_CURVE ( 'NONE', #72426, #83684, #89785, .T. ) ;
#28056 = DIRECTION ( 'NONE',  ( 0.000000000000000000, 0.5000000000000087708, -0.8660254037844336006 ) ) ;
#28057 = VERTEX_POINT ( 'NONE', #33902 ) ;
#28058 = DIRECTION ( 'NONE',  ( 0.000000000000000000, 1.000000000000000000, 0.000000000000000000 ) ) ;
#28059 = CARTESIAN_POINT ( 'NONE',  ( 163.0664832912739826, -8.350947159940998787, 333.4006252759120343 ) ) ;
#28060 = VERTEX_POINT ( 'NONE', #47962 ) ;
#28061 = CONICAL_SURFACE ( 'NONE', #78873, 3.299999999999999822, 0.7853981633974602694 ) ;
#28062 = DIRECTION ( 'NONE',  ( 0.000000000000000000, 0.000000000000000000, 1.000000000000000000 ) ) ;
#28063 = CARTESIAN_POINT ( 'NONE',  ( 97.81461822720238786, -40.51595288653417981, 132.6359866545674890 ) ) ;
#28064 = CARTESIAN_POINT ( 'NONE',  ( 97.80902780829600829, -29.33079837672297074, 45.78991099019697231 ) ) ;
#28065 = CARTESIAN_POINT ( 'NONE',  ( 156.5667039024485803, -48.82844715993568485, 134.7178068554149775 ) ) ;
#28066 = VECTOR ( 'NONE', #36350, 1000.000000000000000 ) ;
#28067 = CARTESIAN_POINT ( 'NONE',  ( -158.9822249764575020, 20.32000000000000028, 139.6999999999999886 ) ) ;
#28068 = CARTESIAN_POINT ( 'NONE',  ( 110.8778723976570433, -46.37372517399798255, 22.88800622829195675 ) ) ;
#28070 = CARTESIAN_POINT ( 'NONE',  ( 96.66376384204026806, -36.61947630124858932, 107.3184824187679567 ) ) ;
#28069 = CARTESIAN_POINT ( 'NONE',  ( 115.5439452383992176, -108.5954344580491551, 2.217806855418142042 ) ) ;
#28071 = DIRECTION ( 'NONE',  ( 0.000000000000000000, 1.000000000000000000, 0.000000000000000000 ) ) ;
#28072 = CARTESIAN_POINT ( 'NONE',  ( -487.2989999999999782, 18.41194598552320016, 97.63125000000000853 ) ) ;
#28073 = EDGE_LOOP ( 'NONE', ( #895, #80470, #39549, #33285 ) ) ;
#28074 = DIRECTION ( 'NONE',  ( 0.000000000000000000, 1.000000000000000000, 0.000000000000000000 ) ) ;
#28075 = CARTESIAN_POINT ( 'NONE',  ( 172.5664832912740110, -18.82844715994099971, 316.8086252759120498 ) ) ;
#28076 = LINE ( 'NONE', #76238, #80476 ) ;
#28077 = ORIENTED_EDGE ( 'NONE', *, *, #28549, .F. ) ;
#28078 = EDGE_CURVE ( 'NONE', #18676, #69089, #59890, .T. ) ;
#28079 = DIRECTION ( 'NONE',  ( 2.775557561562888827E-14, -1.000000000000000000, 0.000000000000000000 ) ) ;
#28081 = VERTEX_POINT ( 'NONE', #67983 ) ;
#28080 = CARTESIAN_POINT ( 'NONE',  ( 112.5090891374639313, -26.14611880238131647, 169.6984824187679521 ) ) ;
#28082 = DIRECTION ( 'NONE',  ( 0.000000000000000000, 1.000000000000000000, 0.000000000000000000 ) ) ;
#28083 = CARTESIAN_POINT ( 'NONE',  ( 110.0582552220427175, -26.06480902925029497, 215.8708633711489711 ) ) ;
#28084 = EDGE_CURVE ( 'NONE', #667, #79585, #5314, .T. ) ;
#28085 = CARTESIAN_POINT ( 'NONE',  ( 86.19613171056606404, 73.00415124681447310, 98.05713019660873897 ) ) ;
#28086 = DIRECTION ( 'NONE',  ( -1.000000000000000000, -1.541976423090496028E-15, 0.000000000000000000 ) ) ;
#28087 = DIRECTION ( 'NONE',  ( -1.000000000000000000, 0.000000000000000000, 0.000000000000000000 ) ) ;
#28088 = ORIENTED_EDGE ( 'NONE', *, *, #61770, .T. ) ;
#28089 = ITEM_DEFINED_TRANSFORMATION ( 'NONE', 'NONE', #53671,  #50656 ) ;
#28090 = CIRCLE ( 'NONE', #45447, 12.69999999999998863 ) ;
#28091 = ORIENTED_EDGE ( 'NONE', *, *, #46792, .F. ) ;
#28092 = ORIENTED_EDGE ( 'NONE', *, *, #54370, .F. ) ;
#28093 = VECTOR ( 'NONE', #81218, 1000.000000000000000 ) ;
#28094 = ORIENTED_EDGE ( 'NONE', *, *, #41731, .F. ) ;
#28095 = CARTESIAN_POINT ( 'NONE',  ( 41.56670390244777735, -36.32844715994104234, 300.4678068554150059 ) ) ;
#28096 = CARTESIAN_POINT ( 'NONE',  ( 116.9253062793529665, -41.72720563489927770, 244.4651490854349731 ) ) ;
#28097 = CARTESIAN_POINT ( 'NONE',  ( 84.06648329127399677, -14.47844715994100007, 17.92562527591199739 ) ) ;
#28098 = CARTESIAN_POINT ( 'NONE',  ( 135.7756147485513907, -16.57277681852953677, 2.101554741600898613 ) ) ;
#28100 = FACE_OUTER_BOUND ( 'NONE', #47164, .T. ) ;
#28099 = CARTESIAN_POINT ( 'NONE',  ( 32.06670390244800473, -33.35206098992711077, -5.074374724088000832 ) ) ;
#28101 = CYLINDRICAL_SURFACE ( 'NONE', #22557, 9.999999999999998224 ) ;
#28102 = CARTESIAN_POINT ( 'NONE',  ( 107.1956731390977779, -26.28293224109629733, 35.06705384733893283 ) ) ;
#28103 = VERTEX_POINT ( 'NONE', #6212 ) ;
#28104 = AXIS2_PLACEMENT_3D ( 'NONE', #12412, #87379, #47354 ) ;
#28105 = ORIENTED_EDGE ( 'NONE', *, *, #43504, .F. ) ;
#28106 = CARTESIAN_POINT ( 'NONE',  ( 89.06648138392532132, -56.72944715994137255, 14.82207188531717001 ) ) ;
#28107 = CARTESIAN_POINT ( 'NONE',  ( 97.75826863619981566, -40.38458993153165011, 17.62397050589623859 ) ) ;
#28108 = CARTESIAN_POINT ( 'NONE',  ( 106.9482321581270270, -47.09886382165559127, 228.5794347997199907 ) ) ;
#28109 = DIRECTION ( 'NONE',  ( 1.000000000000000000, 0.000000000000000000, 0.000000000000000000 ) ) ;
#28110 = CARTESIAN_POINT ( 'NONE',  ( 116.7176835877704093, -38.50936494796416554, 84.68133956162493803 ) ) ;
#28111 = DIRECTION ( 'NONE',  ( 0.000000000000000000, 0.000000000000000000, -1.000000000000000000 ) ) ;
#28112 = CARTESIAN_POINT ( 'NONE',  ( 97.60785906575104320, -39.98233608924685001, 22.59004718401966372 ) ) ;
#28113 = EDGE_LOOP ( 'NONE', ( #74327, #50156, #86931, #37945 ) ) ;
#28114 = DIRECTION ( 'NONE',  ( 0.000000000000000000, 0.000000000000000000, -1.000000000000000000 ) ) ;
#28115 = ORIENTED_EDGE ( 'NONE', *, *, #43112, .F. ) ;
#28116 = ORIENTED_EDGE ( 'NONE', *, *, #3352, .F. ) ;
#28117 = CARTESIAN_POINT ( 'NONE',  ( -91.11128979799197225, 89.26692529358290074, 75.85717701425203074 ) ) ;
#28118 = CARTESIAN_POINT ( 'NONE',  ( 111.0382984267975246, -28.80776997321336097, 276.1387261630399621 ) ) ;
#28119 = VECTOR ( 'NONE', #80614, 1000.000000000000000 ) ;
#28120 = CARTESIAN_POINT ( 'NONE',  ( 112.0659115712803668, -45.48839629059288825, 192.9897919379049256 ) ) ;
#28121 = CARTESIAN_POINT ( 'NONE',  ( -118.2599598282757114, 92.11680164986013608, 8.393562877891261209 ) ) ;
#28122 = VECTOR ( 'NONE', #33668, 1000.000000000000000 ) ;
#28123 = ADVANCED_FACE ( 'NONE', ( #68437 ), #7105, .F. ) ;
#28124 = ADVANCED_FACE ( 'NONE', ( #81188 ), #55219, .F. ) ;
#28125 = CARTESIAN_POINT ( 'NONE',  ( 92.91125933621933086, -94.95109689075242443, -19.26696060647628528 ) ) ;
#28126 = FACE_OUTER_BOUND ( 'NONE', #29309, .T. ) ;
#28127 = ORIENTED_EDGE ( 'NONE', *, *, #68982, .F. ) ;
#28128 = CARTESIAN_POINT ( 'NONE',  ( -41.60202597009397607, 65.59999999999998010, 50.85338361873603219 ) ) ;
#28129 = EDGE_CURVE ( 'NONE', #67885, #14739, #46598, .T. ) ;
#28130 = CARTESIAN_POINT ( 'NONE',  ( 116.7943018416943062, -39.39076309558235067, 184.6151407780641307 ) ) ;
#28131 = EDGE_LOOP ( 'NONE', ( #46066, #81540, #32497, #46002, #64286, #9997 ) ) ;
#28132 = CARTESIAN_POINT ( 'NONE',  ( 110.4566641872556403, -47.25017721759432732, 57.83657765686300678 ) ) ;
#28133 = ORIENTED_EDGE ( 'NONE', *, *, #33974, .T. ) ;
#28134 = CARTESIAN_POINT ( 'NONE',  ( 114.5169583807067966, -41.13300932163210177, 281.2318998934008505 ) ) ;
#28135 = EDGE_CURVE ( 'NONE', #31769, #64268, #82976, .T. ) ;
#28136 = DIRECTION ( 'NONE',  ( 0.000000000000000000, 0.000000000000000000, -1.000000000000000000 ) ) ;
#28137 = CARTESIAN_POINT ( 'NONE',  ( 99.07755742602699911, -44.46178485432853478, 191.9384824187689560 ) ) ;
#28138 = DIRECTION ( 'NONE',  ( 0.000000000000000000, 1.000000000000000000, 0.000000000000000000 ) ) ;
#28139 = LINE ( 'NONE', #34959, #4131 ) ;
#28140 = CARTESIAN_POINT ( 'NONE',  ( 46.83715912545424231, -47.82818131006082751, 300.4678068554150059 ) ) ;
#28141 = DIRECTION ( 'NONE',  ( 3.999999999999999995E-14, -1.000000000000000000, 4.100000000000000342E-29 ) ) ;
#28142 = CARTESIAN_POINT ( 'NONE',  ( 112.5120184049100089, -46.40124356417671692, 253.9965776568635647 ) ) ;
#28143 = CARTESIAN_POINT ( 'NONE',  ( 109.7881854341049177, -46.37695241868441087, 117.7973390980168205 ) ) ;
#28144 = EDGE_CURVE ( 'NONE', #11510, #80206, #48399, .T. ) ;
#28145 = ORIENTED_EDGE ( 'NONE', *, *, #5223, .F. ) ;
#28146 = DIRECTION ( 'NONE',  ( -4.237773401492740281E-14, 1.000000000000000000, 0.000000000000000000 ) ) ;
#28147 = VECTOR ( 'NONE', #41427, 1000.000000000000000 ) ;
#28148 = ORIENTED_EDGE ( 'NONE', *, *, #59929, .T. ) ;
#28149 = CARTESIAN_POINT ( 'NONE',  ( 113.1020477030913582, -28.17579636167772605, 125.5870538473399591 ) ) ;
#28150 = CARTESIAN_POINT ( 'NONE',  ( 124.0809317655093764, 45.78809315698909899, -40.60603252858108903 ) ) ;
#28151 = AXIS2_PLACEMENT_3D ( 'NONE', #16611, #3870, #73343 ) ;
#28152 = VECTOR ( 'NONE', #87520, 1000.000000000000000 ) ;
#28153 = ORIENTED_EDGE ( 'NONE', *, *, #46579, .F. ) ;
#28154 = ORIENTED_EDGE ( 'NONE', *, *, #4996, .F. ) ;
#28155 = ORIENTED_EDGE ( 'NONE', *, *, #35643, .T. ) ;
#28156 = EDGE_CURVE ( 'NONE', #57167, #13204, #13916, .T. ) ;
#28157 = CONICAL_SURFACE ( 'NONE', #16571, 16.33514202138210791, 0.7853981633974517207 ) ;
#28158 = DIRECTION ( 'NONE',  ( 1.639958061481212836E-42, -4.100000000000000342E-29, -1.000000000000000000 ) ) ;
#28159 = CARTESIAN_POINT ( 'NONE',  ( 163.0667039024470171, -33.35206098992711077, -5.074374724088000832 ) ) ;
#28160 = LINE ( 'NONE', #42234, #32622 ) ;
#28161 = CARTESIAN_POINT ( 'NONE',  ( 47.62500000000000000, 111.1250000000000000, 219.0749999999999886 ) ) ;
#28162 = CARTESIAN_POINT ( 'NONE',  ( 50.56670390244699576, -18.82844715994031048, -5.074374724088000832 ) ) ;
#28163 = CARTESIAN_POINT ( 'NONE',  ( 99.97311099609123630, -31.77112186149751949, 158.6471379886389741 ) ) ;
#28164 = CARTESIAN_POINT ( 'NONE',  ( 96.54178838847580835, -40.18459672615917100, 282.5908633711491120 ) ) ;
#28165 = EDGE_CURVE ( 'NONE', #39822, #62232, #75620, .T. ) ;
#28166 = CARTESIAN_POINT ( 'NONE',  ( 19.56670390244829605, -47.82844715994191631, 249.9678068554150059 ) ) ;
#28167 = ORIENTED_EDGE ( 'NONE', *, *, #14107, .T. ) ;
#28168 = CARTESIAN_POINT ( 'NONE',  ( 7.751770026801673374, 72.45555771672430012, 118.3043497398993082 ) ) ;
#28169 = DIRECTION ( 'NONE',  ( 0.000000000000000000, 0.000000000000000000, -1.000000000000000000 ) ) ;
#28170 = ORIENTED_EDGE ( 'NONE', *, *, #22329, .F. ) ;
#28171 = ORIENTED_EDGE ( 'NONE', *, *, #26512, .T. ) ;
#28172 = DIRECTION ( 'NONE',  ( 0.000000000000000000, 0.8660254037844387076, 0.4999999999999998890 ) ) ;
#28173 = CARTESIAN_POINT ( 'NONE',  ( 0.000000000000000000, 127.0000000000000000, 101.0189074266571794 ) ) ;
#28174 = CARTESIAN_POINT ( 'NONE',  ( -7.759765182912740755, 72.46180059790658845, -130.3270382739332831 ) ) ;
#28175 = CARTESIAN_POINT ( 'NONE',  ( 3.110602869834275287E-15, 2.031999999999865025, -25.39999999999999858 ) ) ;
#28176 = CARTESIAN_POINT ( 'NONE',  ( 49.35211078757041747, -35.65087443489839814, 193.9678068554150911 ) ) ;
#28177 = CARTESIAN_POINT ( 'NONE',  ( 98.60840819187967554, -35.53902818534925245, 180.6381341137909544 ) ) ;
#28178 = CARTESIAN_POINT ( 'NONE',  ( 98.61163144626758026, -43.92169047526947168, 76.89943479971999807 ) ) ;
#28179 = ORIENTED_EDGE ( 'NONE', *, *, #7035, .T. ) ;
#28180 = DIRECTION ( 'NONE',  ( -1.000000000000000000, 0.000000000000000000, 1.821231995776179916E-16 ) ) ;
#28181 = ORIENTED_EDGE ( 'NONE', *, *, #20376, .T. ) ;
#28182 = CARTESIAN_POINT ( 'NONE',  ( -74.36911441044668436, 82.54999999999999716, -92.32962665258587265 ) ) ;
#28183 = ORIENTED_EDGE ( 'NONE', *, *, #59116, .F. ) ;
#28184 = CARTESIAN_POINT ( 'NONE',  ( 0.000000000000000000, 124.5870000000000033, 0.000000000000000000 ) ) ;
#28185 = ORIENTED_EDGE ( 'NONE', *, *, #38923, .F. ) ;
#28186 = CARTESIAN_POINT ( 'NONE',  ( 52.38749999999999574, 94.53880000000000905, 229.3937500000000114 ) ) ;
#28187 = CARTESIAN_POINT ( 'NONE',  ( 105.4788588808462038, 120.6499999999999915, -3.968749999999580336 ) ) ;
#28188 = ADVANCED_FACE ( 'NONE', ( #33456 ), #61160, .T. ) ;
#28189 = DIRECTION ( 'NONE',  ( 0.7071067811865514585, -0.7071067811865435759, 7.071067811865522665E-16 ) ) ;
#28190 = AXIS2_PLACEMENT_3D ( 'NONE', #27763, #55443, #89555 ) ;
#28191 = LINE ( 'NONE', #55879, #48074 ) ;
#28192 = EDGE_LOOP ( 'NONE', ( #44740, #387 ) ) ;
#28193 = CARTESIAN_POINT ( 'NONE',  ( 104.0363141061766186, -47.38371934748259662, 67.36800622829191809 ) ) ;
#28194 =( BOUNDED_CURVE ( )  B_SPLINE_CURVE ( 3, ( #53564, #81333, #28464, #77526 ),
 .UNSPECIFIED., .F., .T. ) 
 B_SPLINE_CURVE_WITH_KNOTS ( ( 4, 4 ),
 ( 0.2392026736790540120, 0.2483601390811745191 ),
 .UNSPECIFIED. ) 
 CURVE ( )  GEOMETRIC_REPRESENTATION_ITEM ( )  RATIONAL_B_SPLINE_CURVE ( ( 1.000000000000000000, 0.9999930117478262881, 0.9999930117478262881, 1.000000000000000000 ) ) 
 REPRESENTATION_ITEM ( '' )  );
#28195 = VECTOR ( 'NONE', #63501, 1000.000000000000000 ) ;
#28197 = CARTESIAN_POINT ( 'NONE',  ( 90.24991642302090611, 70.17656663518266669, -94.33976020835932275 ) ) ;
#28196 = DIRECTION ( 'NONE',  ( -1.000000000000000000, -1.000000000000000078E-15, 0.000000000000000000 ) ) ;
#28198 = DIRECTION ( 'NONE',  ( -4.299999999999999979E-14, 1.000000000000000000, -4.100000000000000342E-29 ) ) ;
#28199 = CARTESIAN_POINT ( 'NONE',  ( 132.6481957738584754, -16.37139167074703039, 1.944749297856041670 ) ) ;
#28200 = ORIENTED_EDGE ( 'NONE', *, *, #40796, .T. ) ;
#28201 = CARTESIAN_POINT ( 'NONE',  ( 106.3701732919943055, -26.72731777573979883, 121.1301100331873926 ) ) ;
#28202 = CARTESIAN_POINT ( 'NONE',  ( 83.06670390244796920, -64.87844715994098976, 237.1838068554150141 ) ) ;
#28203 = FACE_OUTER_BOUND ( 'NONE', #54331, .T. ) ;
#28204 = ORIENTED_EDGE ( 'NONE', *, *, #3639, .F. ) ;
#28205 = ADVANCED_FACE ( 'NONE', ( #284 ), #35691, .T. ) ;
#28206 = CARTESIAN_POINT ( 'NONE',  ( 104.9584626277977577, -25.04276672576827778, 121.2184824187679766 ) ) ;
#28208 = DIRECTION ( 'NONE',  ( -1.000000000000000078E-15, 1.000000000000000083E-30, 1.000000000000000000 ) ) ;
#28207 = CARTESIAN_POINT ( 'NONE',  ( 123.4696824136382105, 20.32000000000000028, -179.8898777604649979 ) ) ;
#28209 = LINE ( 'NONE', #49096, #36426 ) ;
#28210 = ADVANCED_FACE ( 'NONE', ( #29345 ), #1645, .F. ) ;
#28211 = CIRCLE ( 'NONE', #73205, 9.571100913904325935 ) ;
#28212 = AXIS2_PLACEMENT_3D ( 'NONE', #966, #21420, #35029 ) ;
#28213 = VECTOR ( 'NONE', #4445, 1000.000000000000000 ) ;
#28214 = VECTOR ( 'NONE', #74232, 1000.000000000000000 ) ;
#28215 = CARTESIAN_POINT ( 'NONE',  ( 59.56670390244699576, -67.87844715994098976, 120.2178068554179902 ) ) ;
#28216 = CARTESIAN_POINT ( 'NONE',  ( 111.8077268321493278, -46.78591733285061594, 133.9270538473389536 ) ) ;
#28218 = ORIENTED_EDGE ( 'NONE', *, *, #37722, .T. ) ;
#28217 = CARTESIAN_POINT ( 'NONE',  ( -3.968749999999935163, 120.6499999999999915, -100.8961411191535973 ) ) ;
#28219 = VECTOR ( 'NONE', #19269, 999.9999999999998863 ) ;
#28220 = VECTOR ( 'NONE', #29581, 1000.000000000000000 ) ;
#28221 = CARTESIAN_POINT ( 'NONE',  ( 111.7292870705843342, -27.42961193919087748, 275.7070538473395800 ) ) ;
#28222 = CARTESIAN_POINT ( 'NONE',  ( 25.56670390244797275, -62.87844715994099687, 173.2178068554149775 ) ) ;
#28223 = DIRECTION ( 'NONE',  ( -0.7071067811865671127, -0.7071067811865279218, -7.071067811865664660E-16 ) ) ;
#28224 = FACE_BOUND ( 'NONE', #49213, .T. ) ;
#28225 = DIRECTION ( 'NONE',  ( 0.000000000000000000, 0.000000000000000000, -1.000000000000000000 ) ) ;
#28226 = PLANE ( 'NONE',  #31748 ) ;
#28227 = CARTESIAN_POINT ( 'NONE',  ( -87.71474477836267170, 71.54617234588346264, 96.70122665881213209 ) ) ;
#28228 = CARTESIAN_POINT ( 'NONE',  ( 97.48942487598446860, -34.74365074496812156, 216.1641967044829755 ) ) ;
#28229 = ORIENTED_EDGE ( 'NONE', *, *, #804, .T. ) ;
#28230 = ORIENTED_EDGE ( 'NONE', *, *, #19432, .F. ) ;
#28231 = CARTESIAN_POINT ( 'NONE',  ( 99.92577194148378794, -31.43111053364522434, 177.2501547344679693 ) ) ;
#28232 = DIRECTION ( 'NONE',  ( 0.000000000000000000, 0.000000000000000000, 1.000000000000000000 ) ) ;
#28233 = CARTESIAN_POINT ( 'NONE',  ( 114.7948027157550399, -42.07682430429896669, 9.788249972563944468 ) ) ;
#28234 = CARTESIAN_POINT ( 'NONE',  ( 134.0664832912739826, -18.72944715994100306, 14.92562527591099908 ) ) ;
#28235 = AXIS2_PLACEMENT_3D ( 'NONE', #67391, #75117, #62374 ) ;
#28236 = EDGE_CURVE ( 'NONE', #59735, #64543, #7554, .T. ) ;
#28237 = ADVANCED_FACE ( 'NONE', ( #42493 ), #77486, .F. ) ;
#28238 = LINE ( 'NONE', #998, #12747 ) ;
#28239 = PLANE ( 'NONE',  #32819 ) ;
#28240 = CARTESIAN_POINT ( 'NONE',  ( 0.000000000000000000, 211.0000000000000000, 164.6557476874258441 ) ) ;
#28241 = ADVANCED_FACE ( 'NONE', ( #21183 ), #1186, .F. ) ;
#28242 = DIRECTION ( 'NONE',  ( 0.7071067810573865575, 0.7071067813157084769, 7.071067810574170182E-16 ) ) ;
#28243 = CARTESIAN_POINT ( 'NONE',  ( 110.0457755916377778, -26.10929462018208369, 219.8708633711489711 ) ) ;
#28244 = CARTESIAN_POINT ( 'NONE',  ( 1.650257911361945773, 95.04836909505033304, 118.3452167253284131 ) ) ;
#28245 = EDGE_LOOP ( 'NONE', ( #65445, #3877, #50025, #74584, #7129, #80021, #60266 ) ) ;
#28246 = VERTEX_POINT ( 'NONE', #14825 ) ;
#28247 = EDGE_CURVE ( 'NONE', #12987, #74492, #14374, .T. ) ;
#28248 = CARTESIAN_POINT ( 'NONE',  ( 57.14999999999999858, 69.84999999999999432, 326.2630000000000337 ) ) ;
#28249 = CARTESIAN_POINT ( 'NONE',  ( -91.26325766987453392, 88.91291927174614784, -75.67533895324370974 ) ) ;
#28250 = CARTESIAN_POINT ( 'NONE',  ( 99.08956020682818178, -42.79551379493017293, 122.8430804584095455 ) ) ;
#28251 = CARTESIAN_POINT ( 'NONE',  ( 92.32962665258456525, 82.54999999999999716, 74.36911441044829019 ) ) ;
#28252 = EDGE_CURVE ( 'NONE', #48540, #44152, #22531, .T. ) ;
#28253 = ORIENTED_EDGE ( 'NONE', *, *, #19558, .T. ) ;
#28254 = FACE_OUTER_BOUND ( 'NONE', #41812, .T. ) ;
#28255 = VECTOR ( 'NONE', #48393, 999.9999999999998863 ) ;
#28256 = CARTESIAN_POINT ( 'NONE',  ( 116.6059430675273063, -40.93488859202243901, 253.4956252759109532 ) ) ;
#28257 = ORIENTED_EDGE ( 'NONE', *, *, #73569, .T. ) ;
#28258 = EDGE_CURVE ( 'NONE', #74870, #86147, #14740, .T. ) ;
#28259 = CARTESIAN_POINT ( 'NONE',  ( 77.76764265987422675, -38.23887630718186159, 7.293197373623000246 ) ) ;
#28260 = DIRECTION ( 'NONE',  ( -0.9254794337955620787, -0.3787978585227822492, 0.000000000000000000 ) ) ;
#28261 = DIRECTION ( 'NONE',  ( 0.000000000000000000, 1.000000000000000000, 5.300584669389750404E-15 ) ) ;
#28262 = CARTESIAN_POINT ( 'NONE',  ( 108.5688297718456852, -44.75270591617022831, 80.54237608387698799 ) ) ;
#28263 = CARTESIAN_POINT ( 'NONE',  ( 95.99102054923815786, -36.58347128883620059, 152.3280062282919971 ) ) ;
#28264 = DIRECTION ( 'NONE',  ( 0.000000000000000000, 1.000000000000000000, 0.000000000000000000 ) ) ;
#28265 = ORIENTED_EDGE ( 'NONE', *, *, #74403, .T. ) ;
#28266 = DIRECTION ( 'NONE',  ( 0.000000000000000000, 0.000000000000000000, -1.000000000000000000 ) ) ;
#28267 = ORIENTED_EDGE ( 'NONE', *, *, #33572, .T. ) ;
#28268 = VERTEX_POINT ( 'NONE', #42941 ) ;
#28269 = VECTOR ( 'NONE', #79756, 1000.000000000000000 ) ;
#28270 = VECTOR ( 'NONE', #85457, 1000.000000000000000 ) ;
#28271 = CARTESIAN_POINT ( 'NONE',  ( 172.5667039024478413, -36.32844715993500273, 249.9678068554149775 ) ) ;
#28272 = AXIS2_PLACEMENT_3D ( 'NONE', #42523, #62536, #56610 ) ;
#28273 = VERTEX_POINT ( 'NONE', #63404 ) ;
#28274 = VERTEX_POINT ( 'NONE', #35239 ) ;
#28275 = PLANE ( 'NONE',  #84641 ) ;
#28276 = AXIS2_PLACEMENT_3D ( 'NONE', #22823, #36883, #79576 ) ;
#28277 = CARTESIAN_POINT ( 'NONE',  ( 106.5510518188671227, -25.28190781890620542, 320.5359728645732389 ) ) ;
#28278 = CARTESIAN_POINT ( 'NONE',  ( 98.07131787375925569, -37.77809840677601017, 85.85337220902894728 ) ) ;
#28280 = CARTESIAN_POINT ( 'NONE',  ( 115.4777400244682042, -29.52207584268309759, 229.4022919425779605 ) ) ;
#28279 = AXIS2_PLACEMENT_3D ( 'NONE', #9903, #47523, #68443 ) ;
#28281 = CONICAL_SURFACE ( 'NONE', #79086, 5.562599999999973122, 1.029744258676653645 ) ;
#28282 = CARTESIAN_POINT ( 'NONE',  ( 117.3921119255897452, -35.46056622170122097, 193.9241967044829664 ) ) ;
#28283 = DIRECTION ( 'NONE',  ( -0.7071067811865165975, -0.7071067811865784369, -7.071067811865158803E-16 ) ) ;
#28284 = DIRECTION ( 'NONE',  ( 1.000000000000000000, 0.000000000000000000, 0.000000000000000000 ) ) ;
#28285 = ORIENTED_EDGE ( 'NONE', *, *, #33703, .F. ) ;
#28286 = CARTESIAN_POINT ( 'NONE',  ( 108.4144577094060082, -26.73465142943761919, 90.96919997473116837 ) ) ;
#28287 = CARTESIAN_POINT ( 'NONE',  ( 130.0664832912740110, -18.82844715994099971, 284.9256252759119548 ) ) ;
#28288 = EDGE_CURVE ( 'NONE', #69150, #60648, #42051, .T. ) ;
#28289 = CARTESIAN_POINT ( 'NONE',  ( 97.81443832832722762, -40.51607714565724905, 56.63519146330476417 ) ) ;
#28290 = AXIS2_PLACEMENT_3D ( 'NONE', #33364, #39282, #67427 ) ;
#28291 = CARTESIAN_POINT ( 'NONE',  ( 109.1197153606379970, -46.32621810461561296, 107.7441967044829880 ) ) ;
#28292 = CARTESIAN_POINT ( 'NONE',  ( 104.0299312746664526, -47.40616179873944702, 67.36800622829191809 ) ) ;
#28293 = CARTESIAN_POINT ( 'NONE',  ( 115.8130859178907599, -30.97587361506452197, 254.2899109901966028 ) ) ;
#28294 = ORIENTED_EDGE ( 'NONE', *, *, #80079, .T. ) ;
#28295 = CARTESIAN_POINT ( 'NONE',  ( 115.3881169701508327, -30.44952332473371115, 219.3413395616249773 ) ) ;
#28296 = DIRECTION ( 'NONE',  ( 0.000000000000000000, 0.000000000000000000, -1.000000000000000000 ) ) ;
#28297 = CARTESIAN_POINT ( 'NONE',  ( 11.58771219026867527, 77.33901287876103936, 130.0408192685323741 ) ) ;
#28298 = FACE_OUTER_BOUND ( 'NONE', #80131, .T. ) ;
#28300 = CYLINDRICAL_SURFACE ( 'NONE', #25366, 3.000000000000002665 ) ;
#28299 = CARTESIAN_POINT ( 'NONE',  ( 108.4861102935399089, -46.16112076858227908, 277.6356252759110816 ) ) ;
#28301 = DIRECTION ( 'NONE',  ( -1.000000000000000000, 0.000000000000000000, 0.000000000000000000 ) ) ;
#28302 = FACE_OUTER_BOUND ( 'NONE', #37342, .T. ) ;
#28303 = CARTESIAN_POINT ( 'NONE',  ( 151.5667039024536678, -48.82844715994099971, 180.4678068554149775 ) ) ;
#28304 = CARTESIAN_POINT ( 'NONE',  ( -5.624702496966066612, 93.94413577832827400, 130.4352985349312632 ) ) ;
#28305 = CARTESIAN_POINT ( 'NONE',  ( 90.44969454456408187, -23.41243780205710578, 239.5838068554175209 ) ) ;
#28306 = CARTESIAN_POINT ( 'NONE',  ( -50.35902679310718355, 54.97499999999996589, 27.95514712793348977 ) ) ;
#28308 = ORIENTED_EDGE ( 'NONE', *, *, #38503, .T. ) ;
#28307 = CARTESIAN_POINT ( 'NONE',  ( 107.9678037105606450, -121.2545485715091047, -11.78219314458148226 ) ) ;
#28309 = CARTESIAN_POINT ( 'NONE',  ( 105.1589286322275143, -131.7784471599410097, 250.2178068554179902 ) ) ;
#28310 = CARTESIAN_POINT ( 'NONE',  ( 105.7736212422599777, -26.36243834887274673, 270.1756252759109884 ) ) ;
#28311 = CARTESIAN_POINT ( 'NONE',  ( 117.3100215237039805, -34.79230872694400034, 154.9756252759109714 ) ) ;
#28312 = CARTESIAN_POINT ( 'NONE',  ( 96.63726304471626349, -32.99895513370901057, 22.06514908543494258 ) ) ;
#28313 = CARTESIAN_POINT ( 'NONE',  ( 78.56670390244701707, -90.27844715994098124, 45.21780685541799727 ) ) ;
#28315 = CARTESIAN_POINT ( 'NONE',  ( 80.80620050779884878, -34.05355276379768981, 8.162233076795734732 ) ) ;
#28314 = CARTESIAN_POINT ( 'NONE',  ( 20.03715912545645139, -24.42818131006202265, 117.4678068554150485 ) ) ;
#28316 = CARTESIAN_POINT ( 'NONE',  ( 100.8873625800001719, -44.70014081962553831, 138.0522817664394495 ) ) ;
#28317 = CIRCLE ( 'NONE', #39926, 17.00000000000000000 ) ;
#28318 = CARTESIAN_POINT ( 'NONE',  ( 7.620115932400938793E-15, 60.82030000000000314, 221.5895999999999901 ) ) ;
#28319 = EDGE_CURVE ( 'NONE', #56872, #76329, #84765, .T. ) ;
#28320 = CIRCLE ( 'NONE', #37096, 2.517500000000005844 ) ;
#28321 = ORIENTED_EDGE ( 'NONE', *, *, #52507, .T. ) ;
#28322 = CARTESIAN_POINT ( 'NONE',  ( 22.62762465138250789, 172.0000000000000000, 0.000000000000000000 ) ) ;
#28323 = ORIENTED_EDGE ( 'NONE', *, *, #5909, .F. ) ;
#28324 = ADVANCED_BREP_SHAPE_REPRESENTATION ( '', ( #80543, #50656 ), #23133 ) ;
#28325 = CARTESIAN_POINT ( 'NONE',  ( 108.9443472801882393, -27.87019791606706320, 184.3448007804579447 ) ) ;
#28327 = VERTEX_POINT ( 'NONE', #62947 ) ;
#28326 = CARTESIAN_POINT ( 'NONE',  ( 23.27731929905162289, 53.53152164542878211, 30.16249999999999787 ) ) ;
#28328 = DIRECTION ( 'NONE',  ( 4.299999999999999979E-14, -1.000000000000000000, 4.400000000000000367E-29 ) ) ;
#28329 = CARTESIAN_POINT ( 'NONE',  ( 109.8501361970267425, -26.70547878262040342, 170.8613395616249591 ) ) ;
#28330 = DIRECTION ( 'NONE',  ( 0.000000000000000000, 0.000000000000000000, 1.000000000000000000 ) ) ;
#28331 = DIRECTION ( 'NONE',  ( 0.000000000000000000, 1.000000000000000000, 0.000000000000000000 ) ) ;
#28332 = DIRECTION ( 'NONE',  ( -1.000000000000000000, 0.000000000000000000, 0.000000000000000000 ) ) ;
#28333 = CARTESIAN_POINT ( 'NONE',  ( -88.21655330423224939, 71.53193882405246029, 79.20758933349385700 ) ) ;
#28334 = DIRECTION ( 'NONE',  ( 0.000000000000000000, 0.000000000000000000, 1.000000000000000000 ) ) ;
#28335 = CARTESIAN_POINT ( 'NONE',  ( 114.1038288540493539, -43.56973530630605751, 98.21276813305496489 ) ) ;
#28336 = VERTEX_POINT ( 'NONE', #77045 ) ;
#28337 = ORIENTED_EDGE ( 'NONE', *, *, #62192, .T. ) ;
#28338 = EDGE_LOOP ( 'NONE', ( #87921, #8518, #40513, #13096 ) ) ;
#28339 = CIRCLE ( 'NONE', #60296, 6.349999999999994316 ) ;
#28340 = CARTESIAN_POINT ( 'NONE',  ( 98.26727195740441800, -38.00851302551287603, 62.87301187732596475 ) ) ;
#28341 = CIRCLE ( 'NONE', #6630, 1.523999999999053889 ) ;
#28342 = CARTESIAN_POINT ( 'NONE',  ( 134.4101120871804653, -107.6623471058698414, 250.2178068554180470 ) ) ;
#28343 = VECTOR ( 'NONE', #74603, 1000.000000000000000 ) ;
#28345 = CARTESIAN_POINT ( 'NONE',  ( 98.30753425284424907, -41.72887559872005170, 36.73979195237785689 ) ) ;
#28344 = CARTESIAN_POINT ( 'NONE',  ( 106.5196382177907140, -25.62481104856566105, 191.1156252759109861 ) ) ;
#28346 = CIRCLE ( 'NONE', #51555, 2.116999999999993776 ) ;
#28347 = CARTESIAN_POINT ( 'NONE',  ( 134.0664832912740110, -36.72944715994100306, -5.074374724089001809 ) ) ;
#28348 = DIRECTION ( 'NONE',  ( -3.100000000000000258E-29, 3.100000000000000044E-14, 1.000000000000000000 ) ) ;
#28349 = ADVANCED_FACE ( 'NONE', ( #77944 ), #36455, .T. ) ;
#28351 = DIRECTION ( 'NONE',  ( 8.755702086949183871E-16, 1.000000000000000000, 0.000000000000000000 ) ) ;
#28350 = AXIS2_PLACEMENT_3D ( 'NONE', #19724, #41493, #48297 ) ;
#28352 = CARTESIAN_POINT ( 'NONE',  ( 119.2563820928105400, -114.7407331754008055, -21.02845593540893532 ) ) ;
#28353 = ADVANCED_FACE ( 'NONE', ( #57480 ), #7994, .F. ) ;
#28354 = CARTESIAN_POINT ( 'NONE',  ( 67.06888395500608624, -67.87985678217047791, 245.5863101313805146 ) ) ;
#28355 = CARTESIAN_POINT ( 'NONE',  ( 109.1969564574039282, -26.54663071456422330, 139.9127681330539872 ) ) ;
#28356 = ORIENTED_EDGE ( 'NONE', *, *, #31247, .F. ) ;
#28357 = EDGE_CURVE ( 'NONE', #79893, #57125, #85219, .T. ) ;
#28358 = EDGE_LOOP ( 'NONE', ( #1254, #45418 ) ) ;
#28359 = ORIENTED_EDGE ( 'NONE', *, *, #1720, .T. ) ;
#28360 = TOROIDAL_SURFACE ( 'NONE', #811, 29.50000000000000000, 1.500000000000000000 ) ;
#28361 = EDGE_CURVE ( 'NONE', #4530, #67525, #43694, .T. ) ;
#28362 = CARTESIAN_POINT ( 'NONE',  ( 148.0533267522749838, 20.32000000000000028, -160.2664750769289697 ) ) ;
#28363 = CARTESIAN_POINT ( 'NONE',  ( -100.8594679592206518, 83.38918798244688446, -82.89895571708331090 ) ) ;
#28364 = CARTESIAN_POINT ( 'NONE',  ( 144.0667039024470455, -124.7784471599409102, 55.21780685541800437 ) ) ;
#28365 = FACE_OUTER_BOUND ( 'NONE', #7225, .T. ) ;
#28367 = CARTESIAN_POINT ( 'NONE',  ( 103.0873890296785333, -43.88832256772609952, 184.9909475124489688 ) ) ;
#28366 = VECTOR ( 'NONE', #66767, 1000.000000000000000 ) ;
#28368 = FACE_OUTER_BOUND ( 'NONE', #81054, .T. ) ;
#28369 = VECTOR ( 'NONE', #61825, 1000.000000000000000 ) ;
#28370 = DIRECTION ( 'NONE',  ( -4.299999999999999979E-14, 1.000000000000000000, -4.400000000000000367E-29 ) ) ;
#28371 = VERTEX_POINT ( 'NONE', #57024 ) ;
#28373 = VERTEX_POINT ( 'NONE', #8912 ) ;
#28372 = VERTEX_POINT ( 'NONE', #63865 ) ;
#28374 = ADVANCED_FACE ( 'NONE', ( #62506 ), #65632, .F. ) ;
#28375 = CARTESIAN_POINT ( 'NONE',  ( 105.4788588808464027, 120.6499999999999915, 3.968750000000405009 ) ) ;
#28376 = ORIENTED_EDGE ( 'NONE', *, *, #65446, .T. ) ;
#28377 = ORIENTED_EDGE ( 'NONE', *, *, #29802, .F. ) ;
#28378 = EDGE_CURVE ( 'NONE', #38559, #51120, #30233, .T. ) ;
#28379 = CARTESIAN_POINT ( 'NONE',  ( 134.0664832912740110, 0.2215528400590013880, 308.6356252759119911 ) ) ;
#28380 = AXIS2_PLACEMENT_3D ( 'NONE', #44638, #86013, #65545 ) ;
#28381 = CARTESIAN_POINT ( 'NONE',  ( 105.8471956337337190, -45.50678253122700312, 253.8987261630398677 ) ) ;
#28382 = CARTESIAN_POINT ( 'NONE',  ( 132.2857443282840393, -124.7784471599409102, 45.21780685541799727 ) ) ;
#28383 = EDGE_LOOP ( 'NONE', ( #66184, #65984, #75413, #5175 ) ) ;
#28384 = CARTESIAN_POINT ( 'NONE',  ( 182.4202572930265660, -31.94127993907054730, 313.9678068554149490 ) ) ;
#28385 = AXIS2_PLACEMENT_3D ( 'NONE', #8201, #29536, #77689 ) ;
#28386 = CARTESIAN_POINT ( 'NONE',  ( -121.5196524476492215, 74.38311268679323973, 47.72707487632980161 ) ) ;
#28387 = ORIENTED_EDGE ( 'NONE', *, *, #58077, .F. ) ;
#28388 = ORIENTED_EDGE ( 'NONE', *, *, #66454, .T. ) ;
#28389 = CARTESIAN_POINT ( 'NONE',  ( 107.0664832912749915, -36.72944715993903486, 25.56312527591096995 ) ) ;
#28390 = CIRCLE ( 'NONE', #42902, 7.937500000000000000 ) ;
#28391 = VERTEX_POINT ( 'NONE', #2971 ) ;
#28392 = VERTEX_POINT ( 'NONE', #86985 ) ;
#28393 = CARTESIAN_POINT ( 'NONE',  ( 101.7278717236064836, -30.55458258274888905, 258.4623760838770750 ) ) ;
#28394 = CARTESIAN_POINT ( 'NONE',  ( 112.1308356434906273, -47.47125106351535351, 137.9270538473389820 ) ) ;
#28395 = CARTESIAN_POINT ( 'NONE',  ( 117.5733473178508319, -42.15660255127708211, 93.44705384733897802 ) ) ;
#28396 = CARTESIAN_POINT ( 'NONE',  ( 116.6018603435394141, -39.73108032723776972, 249.5838075904518121 ) ) ;
#28397 = FACE_OUTER_BOUND ( 'NONE', #87573, .T. ) ;
#28398 = CARTESIAN_POINT ( 'NONE',  ( 103.3035667682879932, -27.00715593367326406, 211.3699109901969848 ) ) ;
#28399 = DIRECTION ( 'NONE',  ( 0.000000000000000000, 0.000000000000000000, -1.000000000000000000 ) ) ;
#28400 = CYLINDRICAL_SURFACE ( 'NONE', #13250, 0.5000000000000197620 ) ;
#28401 = VERTEX_POINT ( 'NONE', #78844 ) ;
#28402 = CARTESIAN_POINT ( 'NONE',  ( 130.0261948852675005, 77.68489675156568808, 11.75299070208665597 ) ) ;
#28403 = VERTEX_POINT ( 'NONE', #57926 ) ;
#28404 = ORIENTED_EDGE ( 'NONE', *, *, #41084, .F. ) ;
#28405 = LINE ( 'NONE', #42918, #77923 ) ;
#28406 = EDGE_CURVE ( 'NONE', #30159, #50189, #65194, .T. ) ;
#28407 = CIRCLE ( 'NONE', #5262, 4.750000000000000888 ) ;
#28408 = CARTESIAN_POINT ( 'NONE',  ( 103.3880255802097849, -27.43047095121296408, 136.3762285854526795 ) ) ;
#28409 = CIRCLE ( 'NONE', #8129, 7.937500000000000000 ) ;
#28410 = ORIENTED_EDGE ( 'NONE', *, *, #84667, .F. ) ;
#28411 = AXIS2_PLACEMENT_3D ( 'NONE', #17310, #71393, #57281 ) ;
#28412 = CARTESIAN_POINT ( 'NONE',  ( 98.28068559441094010, -31.05177188324158166, 145.8699109901969848 ) ) ;
#28413 = CARTESIAN_POINT ( 'NONE',  ( 107.2792697713003776, -24.20934055526686279, 321.5865679059475610 ) ) ;
#28414 = CIRCLE ( 'NONE', #79214, 12.99999999999999822 ) ;
#28415 = EDGE_CURVE ( 'NONE', #75208, #73048, #13095, .T. ) ;
#28416 = DIRECTION ( 'NONE',  ( -0.9254794337955620787, -0.3787978585227822492, 0.000000000000000000 ) ) ;
#28417 = DIRECTION ( 'NONE',  ( 1.000000000000000000, 4.299999999999999979E-14, 1.000000000000000078E-15 ) ) ;
#28420 = CARTESIAN_POINT ( 'NONE',  ( 96.79426660377265534, -34.87310936442968057, 237.1841967044819626 ) ) ;
#28419 = CARTESIAN_POINT ( 'NONE',  ( 110.1997925270103309, -46.26506069963132006, 57.82863803721590301 ) ) ;
#28418 = DIRECTION ( 'NONE',  ( -3.100000000000000258E-29, 3.100000000000000044E-14, 1.000000000000000000 ) ) ;
#28421 = DIRECTION ( 'NONE',  ( 0.000000000000000000, 0.000000000000000000, -1.000000000000000000 ) ) ;
#28422 = DIRECTION ( 'NONE',  ( 1.000000000000000000, 0.000000000000000000, 0.000000000000000000 ) ) ;
#28423 = ORIENTED_EDGE ( 'NONE', *, *, #29604, .T. ) ;
#28424 = DIRECTION ( 'NONE',  ( 1.000000000000000000, 1.000000000000000078E-15, 0.000000000000000000 ) ) ;
#28425 = CARTESIAN_POINT ( 'NONE',  ( 0.000000000000000000, 95.25000000000000000, 38.10000000000000142 ) ) ;
#28426 = DIRECTION ( 'NONE',  ( 1.000000000000000000, 4.163336342344333240E-14, 0.000000000000000000 ) ) ;
#28427 = DIRECTION ( 'NONE',  ( -1.000000000000000000, -1.000000000000000078E-15, -1.000000000000000078E-15 ) ) ;
#28429 = ORIENTED_EDGE ( 'NONE', *, *, #9742, .F. ) ;
#28428 = CARTESIAN_POINT ( 'NONE',  ( 102.3593652026347343, -47.65646955129418672, 287.2527681330535643 ) ) ;
#28430 = DIRECTION ( 'NONE',  ( 0.000000000000000000, -1.000000000000000000, 0.000000000000000000 ) ) ;
#28431 = CARTESIAN_POINT ( 'NONE',  ( 108.5930441862165026, -47.10046404026961397, 142.6927681330539883 ) ) ;
#28432 = CARTESIAN_POINT ( 'NONE',  ( 99.12745497205600032, -44.42007846243786418, 37.95086337114900488 ) ) ;
#28433 = CARTESIAN_POINT ( 'NONE',  ( 118.9671133714783480, -36.92893286478360437, 149.8127681330539644 ) ) ;
#28434 = DIRECTION ( 'NONE',  ( -1.000000000000000000, -1.734723475976808672E-15, 0.000000000000000000 ) ) ;
#28435 = CARTESIAN_POINT ( 'NONE',  ( 80.06648329127402519, -36.72944715994107412, -5.074374724089057764 ) ) ;
#28436 = CIRCLE ( 'NONE', #69098, 13.63963572536219715 ) ;
#28437 = CARTESIAN_POINT ( 'NONE',  ( 48.16670390244661348, -28.27351298637380950, 117.4678068554150485 ) ) ;
#28438 = CARTESIAN_POINT ( 'NONE',  ( 100.9546728224220260, -28.70702571896925903, 70.59395860815119761 ) ) ;
#28439 = LINE ( 'NONE', #43402, #13210 ) ;
#28440 = VERTEX_POINT ( 'NONE', #4310 ) ;
#28441 = CARTESIAN_POINT ( 'NONE',  ( 107.0664832912739968, -18.82844715994099971, 168.9256252759119832 ) ) ;
#28442 = ADVANCED_FACE ( 'NONE', ( #18369 ), #3860, .F. ) ;
#28443 = VECTOR ( 'NONE', #12248, 1000.000000000000000 ) ;
#28444 = ORIENTED_EDGE ( 'NONE', *, *, #43160, .T. ) ;
#28445 = ORIENTED_EDGE ( 'NONE', *, *, #31813, .T. ) ;
#28447 = ORIENTED_EDGE ( 'NONE', *, *, #74106, .F. ) ;
#28446 = FACE_OUTER_BOUND ( 'NONE', #8616, .T. ) ;
#28448 = CARTESIAN_POINT ( 'NONE',  ( 116.7246412902988908, -32.86309880586080823, 50.12991099019698282 ) ) ;
#28449 = CARTESIAN_POINT ( 'NONE',  ( 177.3246001664175537, -48.34074026909178912, 129.9678068554150059 ) ) ;
#28450 = CARTESIAN_POINT ( 'NONE',  ( 73.06670390244801183, -50.82844715994100682, 250.9178068554160461 ) ) ;
#28451 = EDGE_CURVE ( 'NONE', #61548, #11120, #52414, .T. ) ;
#28452 = CARTESIAN_POINT ( 'NONE',  ( 95.86339321018937198, -32.71673170297378164, 172.0527681330539735 ) ) ;
#28453 = CARTESIAN_POINT ( 'NONE',  ( 115.5572469886287479, -35.80043457063792545, 278.3352769709341032 ) ) ;
#28454 = ORIENTED_EDGE ( 'NONE', *, *, #31010, .F. ) ;
#28455 = EDGE_LOOP ( 'NONE', ( #1903, #29819 ) ) ;
#28456 = ORIENTED_EDGE ( 'NONE', *, *, #71101, .T. ) ;
#28457 = VERTEX_POINT ( 'NONE', #30672 ) ;
#28458 = DIRECTION ( 'NONE',  ( -1.000200923085726652E-15, -1.000000000000000000, 0.000000000000000000 ) ) ;
#28459 = CYLINDRICAL_SURFACE ( 'NONE', #37637, 0.5000000000000079936 ) ;
#28460 = CARTESIAN_POINT ( 'NONE',  ( 97.33780276779580731, -34.07122131011711730, 162.1148046345169860 ) ) ;
#28461 = CARTESIAN_POINT ( 'NONE',  ( 105.7995184814174934, -26.72403496660779254, 75.17729194306866702 ) ) ;
#28462 = CARTESIAN_POINT ( 'NONE',  ( 90.83954799657384171, 95.08644067748865325, 93.77212533081443269 ) ) ;
#28463 = CARTESIAN_POINT ( 'NONE',  ( 181.9790560690580037, -31.62489322948711035, -5.074374724088000832 ) ) ;
#28464 = CARTESIAN_POINT ( 'NONE',  ( 147.0666650806933262, -67.87844715994090450, 245.5060119364703439 ) ) ;
#28465 = DIRECTION ( 'NONE',  ( 0.000000000000000000, 0.000000000000000000, 1.000000000000000000 ) ) ;
#28466 = CARTESIAN_POINT ( 'NONE',  ( 111.3142535964730797, -27.23286288913589459, 24.74133956162494030 ) ) ;
#28467 = ADVANCED_FACE ( 'NONE', ( #16602 ), #51540, .F. ) ;
#28468 = CARTESIAN_POINT ( 'NONE',  ( 167.6524903400753033, -48.32844715993521589, 300.4678068554149490 ) ) ;
#28469 = ORIENTED_EDGE ( 'NONE', *, *, #89603, .F. ) ;
#28470 = DIRECTION ( 'NONE',  ( -0.7071067811865475727, 0.000000000000000000, -0.7071067811865475727 ) ) ;
#28471 = AXIS2_PLACEMENT_3D ( 'NONE', #5374, #4484, #33072 ) ;
#28472 = CARTESIAN_POINT ( 'NONE',  ( 165.6738106836030227, -28.98061976758901892, -5.074374724088000832 ) ) ;
#28473 = CARTESIAN_POINT ( 'NONE',  ( 103.5365535965830475, -29.36946602085958702, 93.25094751244894553 ) ) ;
#28474 = VECTOR ( 'NONE', #34616, 1000.000000000000000 ) ;
#28475 = AXIS2_PLACEMENT_3D ( 'NONE', #45481, #52729, #50977 ) ;
#28476 = AXIS2_PLACEMENT_3D ( 'NONE', #15424, #32044, #25229 ) ;
#28477 = DIRECTION ( 'NONE',  ( 0.000000000000000000, 1.000000000000000000, 0.000000000000000000 ) ) ;
#28478 = CARTESIAN_POINT ( 'NONE',  ( 109.7248659201067795, -27.00080517940160973, 44.86479194268253679 ) ) ;
#28479 = ORIENTED_EDGE ( 'NONE', *, *, #35304, .T. ) ;
#28480 = ORIENTED_EDGE ( 'NONE', *, *, #77940, .T. ) ;
#28481 = EDGE_CURVE ( 'NONE', #69245, #32266, #20511, .T. ) ;
#28482 = DIRECTION ( 'NONE',  ( 0.000000000000000000, 0.000000000000000000, -1.000000000000000000 ) ) ;
#28483 = ORIENTED_EDGE ( 'NONE', *, *, #69511, .F. ) ;
#28484 = EDGE_LOOP ( 'NONE', ( #21799, #12269, #84271, #20784 ) ) ;
#28485 = EDGE_CURVE ( 'NONE', #73586, #35967, #60859, .T. ) ;
#28486 = CARTESIAN_POINT ( 'NONE',  ( 115.3364322588818851, -33.54570361940938739, 135.5501547344689754 ) ) ;
#28487 = CARTESIAN_POINT ( 'NONE',  ( -10.09762896578686409, 90.29673011329586529, 118.1261022283270421 ) ) ;
#28488 = AXIS2_PLACEMENT_3D ( 'NONE', #11070, #3820, #81042 ) ;
#28489 = CARTESIAN_POINT ( 'NONE',  ( 116.9423613927432939, -33.21572726007214271, 110.0984824187679578 ) ) ;
#28490 = CARTESIAN_POINT ( 'NONE',  ( -546.0365000000000464, 53.97500000000000142, 88.90000000000000568 ) ) ;
#28491 = ORIENTED_EDGE ( 'NONE', *, *, #89810, .T. ) ;
#28492 = ORIENTED_EDGE ( 'NONE', *, *, #43040, .T. ) ;
#28493 = ORIENTED_EDGE ( 'NONE', *, *, #66302, .T. ) ;
#28494 = DIRECTION ( 'NONE',  ( 0.4214249218767882055, 0.9068632946707806397, 4.214249218767890910E-16 ) ) ;
#28495 = ORIENTED_EDGE ( 'NONE', *, *, #39851, .F. ) ;
#28496 = CARTESIAN_POINT ( 'NONE',  ( 101.6204011159889831, -47.22657592904994317, 17.19562527591095247 ) ) ;
#28497 = CARTESIAN_POINT ( 'NONE',  ( 95.38360599640527937, -38.85844429501600672, 197.4699109901969791 ) ) ;
#28498 = DIRECTION ( 'NONE',  ( -1.000000000000000000, 0.000000000000000000, 0.000000000000000000 ) ) ;
#28499 = LINE ( 'NONE', #56190, #37296 ) ;
#28500 = CARTESIAN_POINT ( 'NONE',  ( 102.3127581962668273, -26.75066580571964536, 136.4422919425779526 ) ) ;
#28501 = DIRECTION ( 'NONE',  ( 1.000000000000000000, 0.000000000000000000, 0.000000000000000000 ) ) ;
#28502 = VERTEX_POINT ( 'NONE', #25635 ) ;
#28503 = LINE ( 'NONE', #48045, #19199 ) ;
#28504 = LINE ( 'NONE', #1722, #7049 ) ;
#28505 = VECTOR ( 'NONE', #11738, 1000.000000000000114 ) ;
#28506 = ORIENTED_EDGE ( 'NONE', *, *, #72598, .T. ) ;
#28507 = CARTESIAN_POINT ( 'NONE',  ( 0.000000000000000000, 8.255000000000000782, 0.000000000000000000 ) ) ;
#28508 = CARTESIAN_POINT ( 'NONE',  ( 0.000000000000000000, 95.14999999999999147, 118.5560000000000116 ) ) ;
#28509 = CARTESIAN_POINT ( 'NONE',  ( 116.1584957626482435, -43.02035883463254606, 13.35657765686298859 ) ) ;
#28510 = CARTESIAN_POINT ( 'NONE',  ( 22.56045403639487290, 58.71535241393495141, 30.70317686336609597 ) ) ;
#28511 = EDGE_CURVE ( 'NONE', #75837, #42151, #37943, .T. ) ;
#28512 = CARTESIAN_POINT ( 'NONE',  ( 141.0664832912740394, -46.72944715994099596, -5.074374724088994704 ) ) ;
#28513 = FACE_OUTER_BOUND ( 'NONE', #80288, .T. ) ;
#28514 = CARTESIAN_POINT ( 'NONE',  ( 97.72045520820927322, -39.61305636501506910, 21.56419670448295278 ) ) ;
#28516 = CARTESIAN_POINT ( 'NONE',  ( 96.03721982003250446, -36.58408020053186505, 152.3280062282919971 ) ) ;
#28515 = DIRECTION ( 'NONE',  ( -4.237773401492740281E-14, 1.000000000000000000, 0.000000000000000000 ) ) ;
#28517 = FACE_BOUND ( 'NONE', #71398, .T. ) ;
#28518 = FACE_OUTER_BOUND ( 'NONE', #46807, .T. ) ;
#28519 = ORIENTED_EDGE ( 'NONE', *, *, #81384, .T. ) ;
#28520 = FACE_OUTER_BOUND ( 'NONE', #34825, .T. ) ;
#28521 = FACE_BOUND ( 'NONE', #8549, .T. ) ;
#28522 = CARTESIAN_POINT ( 'NONE',  ( 199.3900000000000148, 52.73749999999999716, -44.45000000000000284 ) ) ;
#28523 = ORIENTED_EDGE ( 'NONE', *, *, #26681, .F. ) ;
#28524 = DIRECTION ( 'NONE',  ( 0.000000000000000000, 0.000000000000000000, 1.000000000000000000 ) ) ;
#28526 = ORIENTED_EDGE ( 'NONE', *, *, #25945, .T. ) ;
#28525 = CARTESIAN_POINT ( 'NONE',  ( 96.57452018799374116, -36.20934681947932177, 171.2870538473399620 ) ) ;
#28527 = DIRECTION ( 'NONE',  ( 1.000000000000000078E-15, -1.000000000000000083E-30, -1.000000000000000000 ) ) ;
#28528 = CARTESIAN_POINT ( 'NONE',  ( 110.2625522973084600, -26.74624433126517076, 230.8299109901969643 ) ) ;
#28529 = CARTESIAN_POINT ( 'NONE',  ( 103.5842829832543686, -46.60199803408937669, 53.30705384733997221 ) ) ;
#28530 = VECTOR ( 'NONE', #11980, 1000.000000000000000 ) ;
#28531 = CARTESIAN_POINT ( 'NONE',  ( 0.000000000000000000, 101.5999999999999943, 0.000000000000000000 ) ) ;
#28532 = CARTESIAN_POINT ( 'NONE',  ( -179.8898777604655095, 20.32000000000000028, 114.2999999999999972 ) ) ;
#28533 = CARTESIAN_POINT ( 'NONE',  ( 72.26648329127297643, -71.52944715994141234, 352.4506252759078961 ) ) ;
#28534 = ORIENTED_EDGE ( 'NONE', *, *, #3902, .F. ) ;
#28535 = CIRCLE ( 'NONE', #38709, 2.750000000000002665 ) ;
#28537 = ADVANCED_FACE ( 'NONE', ( #12020 ), #33796, .F. ) ;
#28536 = CIRCLE ( 'NONE', #67709, 179.8898777604655095 ) ;
#28538 = ITEM_DEFINED_TRANSFORMATION ( 'NONE', 'NONE', #15927,  #50656 ) ;
#28539 = AXIS2_PLACEMENT_3D ( 'NONE', #76185, #8045, #48444 ) ;
#28540 = ADVANCED_FACE ( 'NONE', ( #60591 ), #81528, .F. ) ;
#28541 = ORIENTED_EDGE ( 'NONE', *, *, #2352, .T. ) ;
#28542 = ORIENTED_EDGE ( 'NONE', *, *, #31624, .F. ) ;
#28543 = EDGE_CURVE ( 'NONE', #82635, #37523, #74683, .T. ) ;
#28544 = ORIENTED_EDGE ( 'NONE', *, *, #26214, .T. ) ;
#28545 = DIRECTION ( 'NONE',  ( 0.000000000000000000, -1.000000000000000000, 0.000000000000000000 ) ) ;
#28546 = CARTESIAN_POINT ( 'NONE',  ( 112.4543492094282726, -45.69561878580546477, 234.0070538473389377 ) ) ;
#28547 = CARTESIAN_POINT ( 'NONE',  ( 97.40471326410413155, -39.52310482453168561, 251.5503829890487566 ) ) ;
#28548 = CARTESIAN_POINT ( 'NONE',  ( 135.9759635523877819, -16.74831825236557137, 2.232988539014289397 ) ) ;
#28549 = EDGE_CURVE ( 'NONE', #55608, #14919, #85812, .T. ) ;
#28550 = ADVANCED_FACE ( 'NONE', ( #34234 ), #5200, .F. ) ;
#28552 = LINE ( 'NONE', #75819, #60168 ) ;
#28551 = LINE ( 'NONE', #15396, #4703 ) ;
#28553 = CARTESIAN_POINT ( 'NONE',  ( 121.3178890780284291, -95.01002112898679286, -21.78219314458229405 ) ) ;
#28554 = CIRCLE ( 'NONE', #51759, 1.000000000000000888 ) ;
#28555 = CARTESIAN_POINT ( 'NONE',  ( 105.9861246248700439, -26.33814362677674836, 50.15848241876796720 ) ) ;
#28556 = ORIENTED_EDGE ( 'NONE', *, *, #21492, .T. ) ;
#28557 = EDGE_CURVE ( 'NONE', #78790, #38527, #46509, .T. ) ;
#28558 = ADVANCED_FACE ( 'NONE', ( #87872 ), #5656, .T. ) ;
#28559 = ORIENTED_EDGE ( 'NONE', *, *, #57812, .F. ) ;
#28560 = AXIS2_PLACEMENT_3D ( 'NONE', #88863, #19811, #4838 ) ;
#28561 = LINE ( 'NONE', #56248, #41235 ) ;
#28563 = EDGE_CURVE ( 'NONE', #60315, #7937, #11576, .T. ) ;
#28562 = CARTESIAN_POINT ( 'NONE',  ( 97.60782674972406880, -39.98224406465867986, 17.58997982183609210 ) ) ;
#28564 = CARTESIAN_POINT ( 'NONE',  ( 112.1213531720969883, -45.14146623880446185, 234.0070538473389377 ) ) ;
#28565 = CARTESIAN_POINT ( 'NONE',  ( 63.06670390244732971, -24.92844715994017690, 300.4678068554150627 ) ) ;
#28566 = CARTESIAN_POINT ( 'NONE',  ( 106.8551140066829817, -47.84553036069057441, 73.56133956162396714 ) ) ;
#28567 = CARTESIAN_POINT ( 'NONE',  ( 196.2150000000000034, 43.68799999999999528, 44.45000000000000284 ) ) ;
#28568 = EDGE_CURVE ( 'NONE', #18287, #63937, #19716, .T. ) ;
#28569 = CARTESIAN_POINT ( 'NONE',  ( 103.3069155499675986, -27.46306005310784926, 21.38318458331234240 ) ) ;
#28570 = EDGE_LOOP ( 'NONE', ( #62211, #39441, #64662, #74872 ) ) ;
#28571 = DIRECTION ( 'NONE',  ( -0.000000000000000000, 1.000000000000000000, -0.000000000000000000 ) ) ;
#28572 = EDGE_LOOP ( 'NONE', ( #59532, #45621 ) ) ;
#28573 = ORIENTED_EDGE ( 'NONE', *, *, #30339, .F. ) ;
#28574 = VECTOR ( 'NONE', #59422, 1000.000000000000000 ) ;
#28575 = DIRECTION ( 'NONE',  ( 1.000000000000000000, 0.000000000000000000, 1.047445008332813989E-14 ) ) ;
#28576 = CARTESIAN_POINT ( 'NONE',  ( 98.30854254679421445, -35.37787306724802505, 262.6358690201826676 ) ) ;
#28577 = VECTOR ( 'NONE', #48506, 1000.000000000000000 ) ;
#28578 = DIRECTION ( 'NONE',  ( 0.000000000000000000, 0.000000000000000000, 1.000000000000000000 ) ) ;
#28579 = CARTESIAN_POINT ( 'NONE',  ( -117.8738102209308352, 83.38952084682854604, 12.69999999999959428 ) ) ;
#28580 = CARTESIAN_POINT ( 'NONE',  ( 141.0664832912739826, -8.729447159940995959, 14.92562527591100618 ) ) ;
#28581 = CYLINDRICAL_SURFACE ( 'NONE', #16888, 12.70000000000000107 ) ;
#28582 = VERTEX_POINT ( 'NONE', #68324 ) ;
#28583 = CARTESIAN_POINT ( 'NONE',  ( 12.69999999999999929, 82.54999999999999716, -179.8908777604655143 ) ) ;
#28584 = ADVANCED_FACE ( 'NONE', ( #32437 ), #6104, .T. ) ;
#28585 = CARTESIAN_POINT ( 'NONE',  ( 186.6899999999999977, 52.73749999999999716, -34.92499999999999716 ) ) ;
#28586 = ORIENTED_EDGE ( 'NONE', *, *, #12157, .T. ) ;
#28587 = CARTESIAN_POINT ( 'NONE',  ( 116.7450715690984140, -32.85492016819326722, 54.12991099019698282 ) ) ;
#28588 = VERTEX_POINT ( 'NONE', #20179 ) ;
#28589 = EDGE_CURVE ( 'NONE', #23091, #27806, #47854, .T. ) ;
#28590 = CARTESIAN_POINT ( 'NONE',  ( 101.7664832247249365, -29.99442739451795958, 15.02956268521998773 ) ) ;
#28591 = EDGE_CURVE ( 'NONE', #22872, #85451, #61938, .T. ) ;
#28592 = CARTESIAN_POINT ( 'NONE',  ( 41.56648329127499153, -32.07844715994070839, 318.9256252759120116 ) ) ;
#28593 = CARTESIAN_POINT ( 'NONE',  ( 96.73459541816642115, -35.84013382243347223, 186.2461014663879837 ) ) ;
#28594 = DIRECTION ( 'NONE',  ( -3.999999999999999995E-14, 1.000000000000000000, -4.100000000000000342E-29 ) ) ;
#28595 = VECTOR ( 'NONE', #65636, 1000.000000000000000 ) ;
#28596 = DIRECTION ( 'NONE',  ( -0.7071067811868619879, -0.7071067811862330466, -7.071067811868613027E-16 ) ) ;
#28598 = ADVANCED_FACE ( 'NONE', ( #27424 ), #82866, .T. ) ;
#28597 = LINE ( 'NONE', #13632, #14420 ) ;
#28599 = VECTOR ( 'NONE', #64002, 1000.000000000000114 ) ;
#28600 = CARTESIAN_POINT ( 'NONE',  ( 45.76696975232771081, -48.62818131006071098, 180.4678068554150911 ) ) ;
#28601 = CARTESIAN_POINT ( 'NONE',  ( 97.17561725847181719, -33.29990440931864271, 282.0613395616252888 ) ) ;
#28602 = CARTESIAN_POINT ( 'NONE',  ( 84.41404664249431278, 95.23005795263748041, -83.24642779537427373 ) ) ;
#28603 = ORIENTED_EDGE ( 'NONE', *, *, #134, .F. ) ;
#28604 = CARTESIAN_POINT ( 'NONE',  ( 136.4975570085112793, -38.01506174167548835, 7.157201688892038227 ) ) ;
#28605 = CIRCLE ( 'NONE', #53207, 2.750000000000002665 ) ;
#28606 = ORIENTED_EDGE ( 'NONE', *, *, #53149, .T. ) ;
#28607 = CARTESIAN_POINT ( 'NONE',  ( 117.3817195963474518, -32.63147225404833307, 95.13943479972097350 ) ) ;
#28608 = CIRCLE ( 'NONE', #89566, 10.41399999999997839 ) ;
#28609 = CARTESIAN_POINT ( 'NONE',  ( 124.4929055791733248, 46.65249925418791577, -39.32612047173540049 ) ) ;
#28610 = VECTOR ( 'NONE', #16107, 1000.000000000000000 ) ;
#28611 = EDGE_LOOP ( 'NONE', ( #62909, #69008, #9365, #72642, #21291, #48648 ) ) ;
#28612 = CARTESIAN_POINT ( 'NONE',  ( 130.5667039024480118, -34.21194715994104740, 219.5838068554170093 ) ) ;
#28613 = ORIENTED_EDGE ( 'NONE', *, *, #3076, .F. ) ;
#28614 = VERTEX_POINT ( 'NONE', #21980 ) ;
#28615 = CARTESIAN_POINT ( 'NONE',  ( 97.81170242524891023, -40.51743837274789684, 121.6354095930283137 ) ) ;
#28616 = DIRECTION ( 'NONE',  ( 0.000000000000000000, 0.000000000000000000, 1.000000000000000000 ) ) ;
#28617 = DIRECTION ( 'NONE',  ( 0.000000000000000000, 0.000000000000000000, 1.000000000000000000 ) ) ;
#28618 = CARTESIAN_POINT ( 'NONE',  ( -123.4696824136392053, 0.000000000000000000, -179.8898777604655095 ) ) ;
#28619 = CARTESIAN_POINT ( 'NONE',  ( 172.5664832912740110, -18.82844715994099971, 18.92562527591200094 ) ) ;
#28620 = CARTESIAN_POINT ( 'NONE',  ( 99.06589935993768847, -44.35602157064030848, 32.92038718067297509 ) ) ;
#28621 = CARTESIAN_POINT ( 'NONE',  ( 88.17226027475679473, -14.72944715994100484, 239.5838068554175777 ) ) ;
#28622 = VERTEX_POINT ( 'NONE', #56918 ) ;
#28623 = VECTOR ( 'NONE', #42574, 1000.000000000000000 ) ;
#28624 = CARTESIAN_POINT ( 'NONE',  ( 5.616470115748687597, 71.15184505290909556, 118.4234566822760542 ) ) ;
#28625 = AXIS2_PLACEMENT_3D ( 'NONE', #21562, #63332, #2005 ) ;
#28626 = AXIS2_PLACEMENT_3D ( 'NONE', #55743, #83489, #21262 ) ;
#28627 = CARTESIAN_POINT ( 'NONE',  ( 141.3509999999999991, 20.32000000000000028, 141.3509999999999991 ) ) ;
#28628 = ORIENTED_EDGE ( 'NONE', *, *, #72825, .T. ) ;
#28629 = EDGE_LOOP ( 'NONE', ( #41179, #40955 ) ) ;
#28630 = CIRCLE ( 'NONE', #24291, 15.00000000000000000 ) ;
#28631 = FACE_OUTER_BOUND ( 'NONE', #9301, .T. ) ;
#28632 = DIRECTION ( 'NONE',  ( 0.000000000000000000, 1.000000000000000000, 0.000000000000000000 ) ) ;
#28633 = CARTESIAN_POINT ( 'NONE',  ( -4.100932966941606139, 70.52316614063619227, -130.4921811224707824 ) ) ;
#28634 = LINE ( 'NONE', #20040, #89857 ) ;
#28635 = DIRECTION ( 'NONE',  ( 0.000000000000000000, 0.000000000000000000, 1.000000000000000000 ) ) ;
#28636 = CARTESIAN_POINT ( 'NONE',  ( 99.14828105993673546, -39.93229045078558670, 206.0552769709339884 ) ) ;
#28637 = CARTESIAN_POINT ( 'NONE',  ( 123.2646066340916349, 73.09139164160541213, 43.02039627876905570 ) ) ;
#28638 = CARTESIAN_POINT ( 'NONE',  ( 117.1490187775317793, -39.54886983357372543, 98.60991099019594230 ) ) ;
#28639 = ORIENTED_EDGE ( 'NONE', *, *, #22302, .T. ) ;
#28640 = DIRECTION ( 'NONE',  ( 0.000000000000000000, 1.000000000000000000, 0.000000000000000000 ) ) ;
#28641 = VERTEX_POINT ( 'NONE', #76930 ) ;
#28642 = CARTESIAN_POINT ( 'NONE',  ( -31.75000000000000000, 17.78000000000000114, 3.175000000000219647 ) ) ;
#28643 = ORIENTED_EDGE ( 'NONE', *, *, #44249, .F. ) ;
#28644 = CARTESIAN_POINT ( 'NONE',  ( 113.2454418602651600, -28.75862586841305557, 49.55229777713112327 ) ) ;
#28645 = ORIENTED_EDGE ( 'NONE', *, *, #33602, .F. ) ;
#28646 = DIRECTION ( 'NONE',  ( 3.100000000000000258E-29, -3.100000000000000044E-14, -1.000000000000000000 ) ) ;
#28647 = LINE ( 'NONE', #51, #22729 ) ;
#28648 = CARTESIAN_POINT ( 'NONE',  ( 109.6447271640448378, -46.47965470880307493, 273.7811528438442679 ) ) ;
#28649 = VECTOR ( 'NONE', #13086, 1000.000000000000000 ) ;
#28650 = VECTOR ( 'NONE', #32442, 1000.000000000000000 ) ;
#28651 = CARTESIAN_POINT ( 'NONE',  ( -147.4575741623270062, 20.32000000000000028, 135.2444258376732193 ) ) ;
#28652 = ORIENTED_EDGE ( 'NONE', *, *, #2529, .T. ) ;
#28653 = CARTESIAN_POINT ( 'NONE',  ( 98.57199122844706096, -43.83852907894476658, 71.86895860924397539 ) ) ;
#28654 = EDGE_CURVE ( 'NONE', #54956, #67371, #16225, .T. ) ;
#28656 = CARTESIAN_POINT ( 'NONE',  ( 94.61736061587667734, 70.27756284692564748, -89.95878776288191148 ) ) ;
#28655 = DIRECTION ( 'NONE',  ( -0.9963424814100688698, 0.08544974978094983797, 0.000000000000000000 ) ) ;
#28657 = DIRECTION ( 'NONE',  ( 0.000000000000000000, 1.000000000000000000, 0.000000000000000000 ) ) ;
#28658 = ADVANCED_FACE ( 'NONE', ( #76025, #27872 ), #36035, .T. ) ;
#28659 = CARTESIAN_POINT ( 'NONE',  ( 131.4596324495014699, -17.85248396559163808, 2.902015641457815764 ) ) ;
#28660 = VERTEX_POINT ( 'NONE', #13803 ) ;
#28661 = EDGE_CURVE ( 'NONE', #48200, #88900, #3197, .T. ) ;
#28662 = CARTESIAN_POINT ( 'NONE',  ( 151.0667039024469886, -67.87844715994090450, 120.2178068554179902 ) ) ;
#28663 = CARTESIAN_POINT ( 'NONE',  ( 182.5667039024480118, -32.29483332968450782, -5.074374724088000832 ) ) ;
#28664 = PLANE ( 'NONE',  #69031 ) ;
#28665 = ADVANCED_FACE ( 'NONE', ( #36496 ), #62391, .T. ) ;
#28667 = ADVANCED_FACE ( 'NONE', ( #55547 ), #28782, .T. ) ;
#28666 = CARTESIAN_POINT ( 'NONE',  ( 107.3345073157536689, -26.28600797661530208, 116.0556252759109555 ) ) ;
#28668 = AXIS2_PLACEMENT_3D ( 'NONE', #32513, #46134, #79812 ) ;
#28670 = FACE_OUTER_BOUND ( 'NONE', #39399, .T. ) ;
#28669 = CARTESIAN_POINT ( 'NONE',  ( 107.0664832912750057, -36.72944715993903486, 6.826283056785790393 ) ) ;
#28671 = DIRECTION ( 'NONE',  ( -1.000000000000000000, -1.181088324069315053E-15, 0.000000000000000000 ) ) ;
#28672 = EDGE_CURVE ( 'NONE', #65123, #54206, #71021, .T. ) ;
#28673 = AXIS2_PLACEMENT_3D ( 'NONE', #7228, #15834, #76712 ) ;
#28674 = ORIENTED_EDGE ( 'NONE', *, *, #57102, .T. ) ;
#28675 = VECTOR ( 'NONE', #2399, 999.9999999999998863 ) ;
#28677 = ADVANCED_FACE ( 'NONE', ( #7436 ), #76476, .T. ) ;
#28676 = LINE ( 'NONE', #972, #41870 ) ;
#28678 = CARTESIAN_POINT ( 'NONE',  ( 111.5019814087853405, -26.53443175268790100, 130.7499109901969518 ) ) ;
#28680 = VERTEX_POINT ( 'NONE', #1070 ) ;
#28679 = CARTESIAN_POINT ( 'NONE',  ( 52.06670390244699576, -67.87844715994100397, 222.2178068554179902 ) ) ;
#28681 = VECTOR ( 'NONE', #60184, 1000.000000000000000 ) ;
#28682 = CARTESIAN_POINT ( 'NONE',  ( 101.3060704567421624, -26.40153104436181053, 251.4813395616249920 ) ) ;
#28683 = DIRECTION ( 'NONE',  ( 0.000000000000000000, 0.000000000000000000, 1.000000000000000000 ) ) ;
#28684 = DIRECTION ( 'NONE',  ( 5.782411586589351722E-16, 0.000000000000000000, 1.000000000000000000 ) ) ;
#28685 = DIRECTION ( 'NONE',  ( -1.784063995862374817E-16, 0.000000000000000000, -1.000000000000000000 ) ) ;
#28686 = CARTESIAN_POINT ( 'NONE',  ( -17.54031676229692849, 65.59999999999998010, 43.71138335376673467 ) ) ;
#28687 = EDGE_CURVE ( 'NONE', #74740, #61361, #35932, .T. ) ;
#28688 = VECTOR ( 'NONE', #82385, 1000.000000000000000 ) ;
#28689 = DIRECTION ( 'NONE',  ( 0.000000000000000000, -1.000000000000000000, 0.000000000000000000 ) ) ;
#28690 = CARTESIAN_POINT ( 'NONE',  ( -86.67141577317396184, 72.45841406287408404, 97.63922045723946042 ) ) ;
#28691 = VECTOR ( 'NONE', #62316, 1000.000000000000000 ) ;
#28693 = CARTESIAN_POINT ( 'NONE',  ( 103.8504807240352790, -26.87063827031080621, 210.3394347997209763 ) ) ;
#28692 = CIRCLE ( 'NONE', #41764, 15.84999999999999964 ) ;
#28694 = ORIENTED_EDGE ( 'NONE', *, *, #43289, .F. ) ;
#28695 = ORIENTED_EDGE ( 'NONE', *, *, #84432, .F. ) ;
#28696 = ADVANCED_FACE ( 'NONE', ( #42382 ), #64200, .T. ) ;
#28697 = CARTESIAN_POINT ( 'NONE',  ( 115.2219208674478352, -40.19601845633869175, 164.9387261630399450 ) ) ;
#28698 = AXIS2_PLACEMENT_3D ( 'NONE', #38504, #11712, #66205 ) ;
#28699 = DIRECTION ( 'NONE',  ( 2.999999999999999839E-15, -1.000000000000000000, 2.999999999999999900E-30 ) ) ;
#28700 = CARTESIAN_POINT ( 'NONE',  ( 109.8015415646094226, -45.15840846867854452, 9.258726163039964874 ) ) ;
#28701 = DIRECTION ( 'NONE',  ( -0.000000000000000000, -0.000000000000000000, 1.000000000000000000 ) ) ;
#28702 = CARTESIAN_POINT ( 'NONE',  ( 127.0664832912740394, -46.72944715994101017, -4.824374724089008915 ) ) ;
#28703 = CARTESIAN_POINT ( 'NONE',  ( 107.3366192906461549, -25.27349273040127997, 322.1637998480665033 ) ) ;
#28704 = LINE ( 'NONE', #56391, #88443 ) ;
#28705 = DIRECTION ( 'NONE',  ( 0.4999999999999986122, 0.000000000000000000, 0.8660254037844394848 ) ) ;
#28706 = CARTESIAN_POINT ( 'NONE',  ( 117.7539631054257967, -31.66723592997632863, 214.1784824187679419 ) ) ;
#28707 = CARTESIAN_POINT ( 'NONE',  ( 6.662635722923305082, 93.25222367490323450, 118.1688145635824441 ) ) ;
#28708 = ORIENTED_EDGE ( 'NONE', *, *, #65373, .T. ) ;
#28709 = ORIENTED_EDGE ( 'NONE', *, *, #74921, .T. ) ;
#28710 = EDGE_CURVE ( 'NONE', #50783, #33306, #77373, .T. ) ;
#28711 = CARTESIAN_POINT ( 'NONE',  ( 106.5646857698207981, -25.28130207810567498, 321.1698005525342978 ) ) ;
#28712 = CARTESIAN_POINT ( 'NONE',  ( 82.81519967300323515, -18.82419990105044860, 6.751707299519896566 ) ) ;
#28713 = LINE ( 'NONE', #55489, #17112 ) ;
#28715 = EDGE_CURVE ( 'NONE', #34986, #49377, #85103, .T. ) ;
#28714 = CARTESIAN_POINT ( 'NONE',  ( 131.0667039024480118, -42.97311385573999587, 231.5838068554170093 ) ) ;
#28716 = VECTOR ( 'NONE', #22357, 999.9999999999998863 ) ;
#28717 = VECTOR ( 'NONE', #82715, 1000.000000000000000 ) ;
#28718 = CARTESIAN_POINT ( 'NONE',  ( 97.33063402535807995, -33.15845140301009053, 17.03467289495797132 ) ) ;
#28719 = PLANE ( 'NONE',  #51352 ) ;
#28720 = VERTEX_POINT ( 'NONE', #9232 ) ;
#28721 = CARTESIAN_POINT ( 'NONE',  ( 97.06313332029375829, -39.81586545721199144, 17.56419670448195092 ) ) ;
#28722 = DIRECTION ( 'NONE',  ( -1.047445008332813989E-14, 0.000000000000000000, -1.000000000000000000 ) ) ;
#28723 = CARTESIAN_POINT ( 'NONE',  ( 103.9392425780951754, -26.78422740453794404, 250.3184824187678714 ) ) ;
#28724 = VERTEX_POINT ( 'NONE', #11347 ) ;
#28725 = CARTESIAN_POINT ( 'NONE',  ( 77.86687873443747776, -38.38871026384816076, 7.389079501587738186 ) ) ;
#28726 = FACE_OUTER_BOUND ( 'NONE', #4112, .T. ) ;
#28727 = DIRECTION ( 'NONE',  ( 0.000000000000000000, 1.000000000000000000, 0.000000000000000000 ) ) ;
#28728 = CARTESIAN_POINT ( 'NONE',  ( 113.7275377883433549, -41.44750597731145092, 51.15380465530594734 ) ) ;
#28729 = CARTESIAN_POINT ( 'NONE',  ( 116.6808514842340259, -40.81615526105927927, 164.5070538473399608 ) ) ;
#28730 = DIRECTION ( 'NONE',  ( -1.000000000000000000, 0.000000000000000000, 0.000000000000000000 ) ) ;
#28731 = ORIENTED_EDGE ( 'NONE', *, *, #75745, .T. ) ;
#28732 = AXIS2_PLACEMENT_3D ( 'NONE', #34437, #48941, #14463 ) ;
#28733 = PLANE ( 'NONE',  #87185 ) ;
#28734 = ORIENTED_EDGE ( 'NONE', *, *, #51509, .T. ) ;
#28735 = VERTEX_POINT ( 'NONE', #59925 ) ;
#28736 = EDGE_CURVE ( 'NONE', #64255, #52806, #22873, .T. ) ;
#28737 = CIRCLE ( 'NONE', #75165, 2.117000000000000881 ) ;
#28738 = VECTOR ( 'NONE', #23106, 1000.000000000000000 ) ;
#28739 = DIRECTION ( 'NONE',  ( 1.000000000000000000, 4.299999999999999979E-14, 1.000000000000000078E-15 ) ) ;
#28740 = SHAPE_REPRESENTATION ( 'Hydraulic Index Locking Pin', ( #50656 ), #14432 ) ;
#28741 = VERTEX_POINT ( 'NONE', #39501 ) ;
#28742 = ORIENTED_EDGE ( 'NONE', *, *, #38715, .F. ) ;
#28743 = CARTESIAN_POINT ( 'NONE',  ( 0.000000000000000000, 61.59999999999999432, 118.5560000000000116 ) ) ;
#28744 = CARTESIAN_POINT ( 'NONE',  ( 116.3167039024470029, -67.87844715994093292, 222.2178068554179902 ) ) ;
#28745 = CARTESIAN_POINT ( 'NONE',  ( 98.02882863141191194, -40.27788709084830998, 96.04670554236294322 ) ) ;
#28746 = CARTESIAN_POINT ( 'NONE',  ( 116.5566381636777322, -42.44192488244189576, 278.3832443235297660 ) ) ;
#28747 = CIRCLE ( 'NONE', #59200, 1.000000000000000888 ) ;
#28748 = DIRECTION ( 'NONE',  ( 0.000000000000000000, 0.000000000000000000, -1.000000000000000000 ) ) ;
#28749 = CARTESIAN_POINT ( 'NONE',  ( 84.06648329127399677, -18.72966777111504300, 199.5838068554169524 ) ) ;
#28750 = AXIS2_PLACEMENT_3D ( 'NONE', #78875, #71608, #24782 ) ;
#28751 = VERTEX_POINT ( 'NONE', #65083 ) ;
#28752 = CARTESIAN_POINT ( 'NONE',  ( -479.3614999999999782, 21.43125000000029701, 15.23694598552314972 ) ) ;
#28753 = AXIS2_PLACEMENT_3D ( 'NONE', #26243, #12624, #25796 ) ;
#28754 = AXIS2_PLACEMENT_3D ( 'NONE', #9117, #50426, #50880 ) ;
#28755 = DIRECTION ( 'NONE',  ( 1.000000000000000000, 1.000000000000000078E-15, 0.000000000000000000 ) ) ;
#28756 = DIRECTION ( 'NONE',  ( 0.000000000000000000, -1.000000000000000000, 0.000000000000000000 ) ) ;
#28757 = EDGE_CURVE ( 'NONE', #77829, #71894, #37378, .T. ) ;
#28758 = CARTESIAN_POINT ( 'NONE',  ( 116.5394839232220505, -34.29517225379350975, 124.0270538473399426 ) ) ;
#28759 = CARTESIAN_POINT ( 'NONE',  ( 115.2011789175540741, -43.31984874952732412, 88.28419670448195689 ) ) ;
#28760 = CARTESIAN_POINT ( 'NONE',  ( 95.18116725028646385, -37.33612674980418689, 271.3670538473392639 ) ) ;
#28761 = VERTEX_POINT ( 'NONE', #50995 ) ;
#28762 = UNCERTAINTY_MEASURE_WITH_UNIT (LENGTH_MEASURE( 1.000000000000000082E-05 ), #3736, 'distance_accuracy_value', 'NONE');
#28763 = CARTESIAN_POINT ( 'NONE',  ( 111.6085881668573450, -46.11327973307566452, 247.9356252759109509 ) ) ;
#28764 = FACE_OUTER_BOUND ( 'NONE', #7604, .T. ) ;
#28765 =( NAMED_UNIT ( * ) PLANE_ANGLE_UNIT ( ) SI_UNIT ( $, .RADIAN. ) );
#28766 = PRESENTATION_STYLE_ASSIGNMENT (( #15138 ) ) ;
#28767 = CARTESIAN_POINT ( 'NONE',  ( 98.17570384001206207, -41.31031557640367424, 27.70558999709250614 ) ) ;
#28768 = EDGE_CURVE ( 'NONE', #57023, #32260, #71471, .T. ) ;
#28770 = CARTESIAN_POINT ( 'NONE',  ( 68.73724395117878316, -139.2608654268313728, 246.1571707801609250 ) ) ;
#28769 = CARTESIAN_POINT ( 'NONE',  ( -135.2444258376730204, 20.32000000000000028, 147.4575741623271767 ) ) ;
#28771 = DIRECTION ( 'NONE',  ( 1.000000000000000000, 3.999999999999999995E-14, 1.000000000000000078E-15 ) ) ;
#28772 = EDGE_CURVE ( 'NONE', #59006, #60222, #26389, .T. ) ;
#28773 = FACE_OUTER_BOUND ( 'NONE', #8886, .T. ) ;
#28774 = FACE_BOUND ( 'NONE', #59939, .T. ) ;
#28775 = EDGE_CURVE ( 'NONE', #394, #58704, #79180, .T. ) ;
#28776 = PLANE ( 'NONE',  #12384 ) ;
#28777 = PLANE ( 'NONE',  #70636 ) ;
#28778 = DIRECTION ( 'NONE',  ( 0.000000000000000000, 0.000000000000000000, 1.000000000000000000 ) ) ;
#28780 = VERTEX_POINT ( 'NONE', #2866 ) ;
#28779 = LINE ( 'NONE', #50093, #48645 ) ;
#28781 = EDGE_CURVE ( 'NONE', #26329, #44492, #33653, .T. ) ;
#28782 = PLANE ( 'NONE',  #69910 ) ;
#28783 = CARTESIAN_POINT ( 'NONE',  ( 95.20615018136085439, -37.33485150947186781, 271.3670538473392639 ) ) ;
#28784 = CARTESIAN_POINT ( 'NONE',  ( 117.7034974245586483, -39.73408348695345182, 139.6194347997199827 ) ) ;
#28785 = CARTESIAN_POINT ( 'NONE',  ( 106.2504415414193488, -26.27893178022805998, 21.13848241876792144 ) ) ;
#28786 = DIRECTION ( 'NONE',  ( 0.000000000000000000, 0.000000000000000000, 1.000000000000000000 ) ) ;
#28787 = AXIS2_PLACEMENT_3D ( 'NONE', #35857, #36319, #49018 ) ;
#28789 = CARTESIAN_POINT ( 'NONE',  ( 82.41409441627625654, -35.29397280665990166, 7.245803660790303802 ) ) ;
#28788 = DIRECTION ( 'NONE',  ( -0.000000000000000000, -0.000000000000000000, 1.000000000000000000 ) ) ;
#28790 = CARTESIAN_POINT ( 'NONE',  ( 34.92499999999999716, 87.13271776169258942, 310.8325000000000387 ) ) ;
#28791 = AXIS2_PLACEMENT_3D ( 'NONE', #87895, #80644, #81989 ) ;
#28792 = EDGE_CURVE ( 'NONE', #10845, #25134, #36931, .T. ) ;
#28793 = ORIENTED_EDGE ( 'NONE', *, *, #76452, .T. ) ;
#28794 = DIRECTION ( 'NONE',  ( 0.000000000000000000, 0.000000000000000000, 1.000000000000000000 ) ) ;
#28795 = EDGE_LOOP ( 'NONE', ( #32115, #14674, #89902, #60095 ) ) ;
#28796 = EDGE_CURVE ( 'NONE', #80581, #45331, #4982, .T. ) ;
#28797 = CARTESIAN_POINT ( 'NONE',  ( 98.60840819187967554, -35.53902818534925245, 180.6381341137909544 ) ) ;
#28799 = VERTEX_POINT ( 'NONE', #4539 ) ;
#28798 = CARTESIAN_POINT ( 'NONE',  ( 70.98999999999998067, 52.73749999999999716, -36.61250000000002558 ) ) ;
#28800 = CARTESIAN_POINT ( 'NONE',  ( 208.9149999999999920, 30.98800000000000310, 57.14999999999999858 ) ) ;
#28801 = CARTESIAN_POINT ( 'NONE',  ( 96.64068249873270133, -36.21262657180042766, 167.2870538473399620 ) ) ;
#28802 = CARTESIAN_POINT ( 'NONE',  ( 116.8183451804401045, -34.15765563543617134, 150.0318682641123758 ) ) ;
#28803 = CARTESIAN_POINT ( 'NONE',  ( 107.0620278373210255, -36.73691869758540207, 361.9756252759100903 ) ) ;
#28804 = CARTESIAN_POINT ( 'NONE',  ( 113.4728681846144127, -29.02320129775888446, 85.52423081353769874 ) ) ;
#28805 = VECTOR ( 'NONE', #10325, 1000.000000000000000 ) ;
#28806 = CARTESIAN_POINT ( 'NONE',  ( -92.32962665258560264, 82.54999999999999716, 74.36911441044701121 ) ) ;
#28807 = CARTESIAN_POINT ( 'NONE',  ( 223.2659999999999911, 52.73749999999999716, -44.45000000000000284 ) ) ;
#28808 = CARTESIAN_POINT ( 'NONE',  ( 98.87588542518393808, -42.07524381596793006, 101.7870538473399620 ) ) ;
#28809 = VERTEX_POINT ( 'NONE', #30563 ) ;
#28810 = ORIENTED_EDGE ( 'NONE', *, *, #42086, .F. ) ;
#28811 = VERTEX_POINT ( 'NONE', #50548 ) ;
#28812 = VECTOR ( 'NONE', #74484, 1000.000000000000000 ) ;
#28813 = CARTESIAN_POINT ( 'NONE',  ( 116.3507336416864746, -38.17139756410392692, 65.12348806780198629 ) ) ;
#28814 = AXIS2_PLACEMENT_3D ( 'NONE', #71409, #9173, #36436 ) ;
#28815 = CARTESIAN_POINT ( 'NONE',  ( 129.5675368918763581, -120.1789271773120333, 250.2178068554180470 ) ) ;
#28817 = CARTESIAN_POINT ( 'NONE',  ( 116.3121618740066623, -32.93870344941997530, 39.13562527591096796 ) ) ;
#28816 = CARTESIAN_POINT ( 'NONE',  ( 96.73459541816653484, -35.84013382243349355, 182.2461014663859658 ) ) ;
#28818 = CYLINDRICAL_SURFACE ( 'NONE', #5906, 2.116999999999980009 ) ;
#28819 = DIRECTION ( 'NONE',  ( -1.000000000000000000, -1.541976423090496028E-15, 0.000000000000000000 ) ) ;
#28820 = LINE ( 'NONE', #43772, #75052 ) ;
#28821 = VECTOR ( 'NONE', #63352, 1000.000000000000000 ) ;
#28822 = LINE ( 'NONE', #6577, #31810 ) ;
#28823 = CARTESIAN_POINT ( 'NONE',  ( 67.49017891634400712, -68.28604453786587669, 246.7253416711091631 ) ) ;
#28824 = CARTESIAN_POINT ( 'NONE',  ( 98.85726102317293851, -28.21728661942034577, 115.6870538473389587 ) ) ;
#28825 = ORIENTED_EDGE ( 'NONE', *, *, #65411, .F. ) ;
#28826 = VERTEX_POINT ( 'NONE', #74474 ) ;
#28827 = ORIENTED_EDGE ( 'NONE', *, *, #23703, .T. ) ;
#28828 = VECTOR ( 'NONE', #2453, 1000.000000000000000 ) ;
#28829 = CARTESIAN_POINT ( 'NONE',  ( 36.23715912545344509, -47.82818131006131779, 129.9678068554150911 ) ) ;
#28830 = VECTOR ( 'NONE', #77482, 1000.000000000000000 ) ;
#28831 = CARTESIAN_POINT ( 'NONE',  ( 116.7951252704057907, -39.38782979425321429, 79.61479194223753098 ) ) ;
#28833 = EDGE_CURVE ( 'NONE', #21942, #29924, #1769, .T. ) ;
#28832 = FACE_OUTER_BOUND ( 'NONE', #87241, .T. ) ;
#28834 = CARTESIAN_POINT ( 'NONE',  ( 115.0224139972512063, -40.13592505470528238, 211.3347570362579404 ) ) ;
#28835 = CARTESIAN_POINT ( 'NONE',  ( 160.7738106836362419, -48.62134037874780290, 180.4678068554150059 ) ) ;
#28836 = DIRECTION ( 'NONE',  ( -0.9999999853157766072, -0.0001713722456127291416, 9.999999853157765648E-16 ) ) ;
#28837 = EDGE_LOOP ( 'NONE', ( #60886, #41265 ) ) ;
#28839 = VERTEX_POINT ( 'NONE', #32228 ) ;
#28838 = ORIENTED_EDGE ( 'NONE', *, *, #23047, .T. ) ;
#28840 = AXIS2_PLACEMENT_3D ( 'NONE', #35317, #37130, #2614 ) ;
#28841 = CYLINDRICAL_SURFACE ( 'NONE', #1256, 38.10000000000000142 ) ;
#28842 = VERTEX_POINT ( 'NONE', #58262 ) ;
#28843 = ORIENTED_EDGE ( 'NONE', *, *, #50519, .T. ) ;
#28844 = PLANE ( 'NONE',  #7220 ) ;
#28845 = CARTESIAN_POINT ( 'NONE',  ( 98.98570259493575918, -42.74373749968300729, 258.2672975916112819 ) ) ;
#28846 = LINE ( 'NONE', #43347, #23209 ) ;
#28847 = VERTEX_POINT ( 'NONE', #23329 ) ;
#28848 = CARTESIAN_POINT ( 'NONE',  ( 41.56648329127399677, -18.82844715994099971, 198.9256252759119832 ) ) ;
#28849 = AXIS2_PLACEMENT_3D ( 'NONE', #49558, #20093, #89582 ) ;
#28850 = CARTESIAN_POINT ( 'NONE',  ( -113.0224119320542400, 68.60953631961947963, 65.35142026045585339 ) ) ;
#28851 = EDGE_LOOP ( 'NONE', ( #74316, #48845 ) ) ;
#28852 = VERTEX_POINT ( 'NONE', #60377 ) ;
#28853 = ADVANCED_FACE ( 'NONE', ( #16493 ), #80857, .F. ) ;
#28854 = CARTESIAN_POINT ( 'NONE',  ( 91.27445496092437338, -35.37506862591278889, 302.4856252759109907 ) ) ;
#28855 = ORIENTED_EDGE ( 'NONE', *, *, #84995, .F. ) ;
#28856 = EDGE_LOOP ( 'NONE', ( #4811, #28526, #53955, #13814 ) ) ;
#28857 = CARTESIAN_POINT ( 'NONE',  ( 106.4091095994060652, -45.35897697767001091, 265.3461856076867207 ) ) ;
#28858 = CARTESIAN_POINT ( 'NONE',  ( 101.7582431991767464, -45.72772181880441167, 162.1527681330539679 ) ) ;
#28859 = CARTESIAN_POINT ( 'NONE',  ( 96.05093434719793777, -37.29646042206077539, 121.3794347997209684 ) ) ;
#28860 = CARTESIAN_POINT ( 'NONE',  ( 41.56670390244777735, -36.32844715994104234, 300.4678068554150059 ) ) ;
#28861 = SURFACE_STYLE_USAGE ( .BOTH. , #7962 ) ;
#28862 = CARTESIAN_POINT ( 'NONE',  ( 118.7901020289055225, -38.45900758189035429, 219.7099109901969882 ) ) ;
#28863 = CARTESIAN_POINT ( 'NONE',  ( 161.0667039024469886, -67.87844715994089029, 222.2178068554179902 ) ) ;
#28864 = PLANE ( 'NONE',  #46613 ) ;
#28865 = ORIENTED_EDGE ( 'NONE', *, *, #9184, .T. ) ;
#28866 = CARTESIAN_POINT ( 'NONE',  ( 130.4924667154230065, 70.52006616879376111, 4.092011266638223788 ) ) ;
#28867 = ORIENTED_EDGE ( 'NONE', *, *, #16766, .F. ) ;
#28868 = VECTOR ( 'NONE', #80056, 1000.000000000000000 ) ;
#28869 = ORIENTED_EDGE ( 'NONE', *, *, #42187, .F. ) ;
#28870 = CARTESIAN_POINT ( 'NONE',  ( -465.6921742093550165, 47.62500000000000000, -3.174999999999999822 ) ) ;
#28871 = VECTOR ( 'NONE', #34025, 1000.000000000000000 ) ;
#28872 = CARTESIAN_POINT ( 'NONE',  ( 25.56670390244719115, -42.82844715994178131, 173.2178068554150627 ) ) ;
#28873 = AXIS2_PLACEMENT_3D ( 'NONE', #28140, #68605, #14540 ) ;
#28874 = ORIENTED_EDGE ( 'NONE', *, *, #70130, .T. ) ;
#28875 = CARTESIAN_POINT ( 'NONE',  ( 103.2053365856880873, -46.45145584090948176, 117.2756252759109543 ) ) ;
#28876 = FACE_OUTER_BOUND ( 'NONE', #59902, .T. ) ;
#28877 = CARTESIAN_POINT ( 'NONE',  ( 134.0664832912739826, -33.97944715994100306, 8.225625275910998013 ) ) ;
#28878 = FACE_OUTER_BOUND ( 'NONE', #15744, .T. ) ;
#28881 = CARTESIAN_POINT ( 'NONE',  ( 110.8089421659425540, -26.35361831834165969, 245.7889586092439629 ) ) ;
#28880 = FACE_BOUND ( 'NONE', #59588, .T. ) ;
#28879 = CARTESIAN_POINT ( 'NONE',  ( -215.9000000000000057, 101.5999999999999943, 146.9389999999999930 ) ) ;
#28882 = DIRECTION ( 'NONE',  ( 1.000000000000000000, 0.000000000000000000, 1.047444401652940007E-14 ) ) ;
#28883 = EDGE_CURVE ( 'NONE', #72034, #68380, #23764, .T. ) ;
#28884 = DIRECTION ( 'NONE',  ( -0.000000000000000000, -1.000000000000000000, -0.000000000000000000 ) ) ;
#28885 = CARTESIAN_POINT ( 'NONE',  ( 171.4664832912730219, 12.92155284005730387, 355.9756252759109998 ) ) ;
#28886 = CIRCLE ( 'NONE', #25961, 89.89999999999997726 ) ;
#28887 = ADVANCED_FACE ( 'NONE', ( #18608 ), #88116, .T. ) ;
#28888 = CARTESIAN_POINT ( 'NONE',  ( 1.088711004441995877E-14, 101.5999999999999943, -88.90000000000000568 ) ) ;
#28889 = ADVANCED_FACE ( 'NONE', ( #66755 ), #46290, .T. ) ;
#28890 = DIRECTION ( 'NONE',  ( 0.000000000000000000, 0.000000000000000000, -1.000000000000000000 ) ) ;
#28891 = VECTOR ( 'NONE', #65672, 1000.000000000000000 ) ;
#28892 = CARTESIAN_POINT ( 'NONE',  ( 84.06648329127399677, -14.47844715994100007, 284.9256252759119548 ) ) ;
#28894 = VERTEX_POINT ( 'NONE', #67658 ) ;
#28893 = CARTESIAN_POINT ( 'NONE',  ( 112.8431189249872091, -28.80713414957965313, 195.5838068554226084 ) ) ;
#28895 = EDGE_CURVE ( 'NONE', #20709, #60678, #32150, .T. ) ;
#28896 = DIRECTION ( 'NONE',  ( 1.000000000000000078E-15, 0.000000000000000000, -1.000000000000000000 ) ) ;
#28897 = CARTESIAN_POINT ( 'NONE',  ( 100.8733315758915552, -45.91070206092880568, 152.0918157521009562 ) ) ;
#28898 = CARTESIAN_POINT ( 'NONE',  ( 118.0831039394318083, -37.62836316206458065, 34.77372051400695341 ) ) ;
#28899 = CARTESIAN_POINT ( 'NONE',  ( 117.2699639542694001, -41.09825485984158178, 209.5165776568640013 ) ) ;
#28900 = CARTESIAN_POINT ( 'NONE',  ( 125.5177273812784762, -137.6784471599409301, 55.21780685541800437 ) ) ;
#28901 = AXIS2_PLACEMENT_3D ( 'NONE', #56458, #76927, #14705 ) ;
#28902 = CARTESIAN_POINT ( 'NONE',  ( -24.20305689751608824, 53.97499999999997300, 74.96110745944689313 ) ) ;
#28904 = CARTESIAN_POINT ( 'NONE',  ( 242.3160000000000025, 65.43750000000000000, -63.94449999999999790 ) ) ;
#28903 = CARTESIAN_POINT ( 'NONE',  ( 37.35959712144415334, -48.62134037893600436, 249.9678068554150343 ) ) ;
#28905 = CARTESIAN_POINT ( 'NONE',  ( 69.95929469538076262, -138.0461895383713795, 247.6591799766680140 ) ) ;
#28906 = FACE_OUTER_BOUND ( 'NONE', #66031, .T. ) ;
#28907 = ORIENTED_EDGE ( 'NONE', *, *, #25908, .F. ) ;
#28908 = DIRECTION ( 'NONE',  ( 0.000000000000000000, 0.000000000000000000, 1.000000000000000000 ) ) ;
#28909 = ORIENTED_EDGE ( 'NONE', *, *, #85470, .T. ) ;
#28910 = EDGE_LOOP ( 'NONE', ( #67263, #84122, #28218, #35834 ) ) ;
#28911 = EDGE_CURVE ( 'NONE', #9022, #36325, #48082, .T. ) ;
#28912 = AXIS2_PLACEMENT_3D ( 'NONE', #11769, #52613, #79934 ) ;
#28914 = VERTEX_POINT ( 'NONE', #68107 ) ;
#28913 = DIRECTION ( 'NONE',  ( 0.000000000000000000, 1.000000000000000000, 0.000000000000000000 ) ) ;
#28915 = CARTESIAN_POINT ( 'NONE',  ( 109.9050689397999605, -46.77468768478695438, 68.79562527591099297 ) ) ;
#28916 = FACE_OUTER_BOUND ( 'NONE', #10478, .T. ) ;
#28917 = CARTESIAN_POINT ( 'NONE',  ( -71.77848634863029531, 120.6499999999999915, -77.39114642430038771 ) ) ;
#28918 = CARTESIAN_POINT ( 'NONE',  ( 117.5308098062252498, -40.43017262224169883, 174.5680062282919778 ) ) ;
#28919 = CARTESIAN_POINT ( 'NONE',  ( 101.2965385564679792, -30.39239502954603367, 285.0867055423626084 ) ) ;
#28920 = ORIENTED_EDGE ( 'NONE', *, *, #21249, .T. ) ;
#28921 = AXIS2_PLACEMENT_3D ( 'NONE', #210, #27911, #14752 ) ;
#28922 = EDGE_LOOP ( 'NONE', ( #18905, #88214, #42442, #14996 ) ) ;
#28923 = ORIENTED_EDGE ( 'NONE', *, *, #58349, .F. ) ;
#28924 = ORIENTED_EDGE ( 'NONE', *, *, #72373, .F. ) ;
#28925 = CARTESIAN_POINT ( 'NONE',  ( 107.0667039024470313, -104.2784471599413934, 2.217806855418003043 ) ) ;
#28926 = DIRECTION ( 'NONE',  ( 0.000000000000000000, -1.000000000000000000, 0.000000000000000000 ) ) ;
#28927 = CARTESIAN_POINT ( 'NONE',  ( 109.7243363830542364, -27.00066479321645829, 160.8648351248226334 ) ) ;
#28928 = CARTESIAN_POINT ( 'NONE',  ( 108.4174892472081808, -26.73503592690951436, 74.96895860963714142 ) ) ;
#28929 = CARTESIAN_POINT ( 'NONE',  ( 188.5667039024486087, -48.82844715993430640, 139.7178068554150059 ) ) ;
#28930 = DIRECTION ( 'NONE',  ( 0.7071067811865460184, 0.000000000000000000, 0.7071067811865489050 ) ) ;
#28931 = CARTESIAN_POINT ( 'NONE',  ( -7.205548786489490269E-13, 127.0000000000000000, 103.1875000000000000 ) ) ;
#28932 = DIRECTION ( 'NONE',  ( 0.000000000000000000, 0.000000000000000000, 1.000000000000000000 ) ) ;
#28933 = CARTESIAN_POINT ( 'NONE',  ( 112.1705331031350994, -27.62378402076933526, 34.66991099019695355 ) ) ;
#28934 = CARTESIAN_POINT ( 'NONE',  ( -12.53570085554762237, 80.47189671605593730, 117.8914246743695458 ) ) ;
#28935 = ORIENTED_EDGE ( 'NONE', *, *, #62484, .F. ) ;
#28936 = CIRCLE ( 'NONE', #33262, 2.750000000000002665 ) ;
#28937 = CARTESIAN_POINT ( 'NONE',  ( 97.06107093643949213, -37.99641063121843843, 271.4272918366033309 ) ) ;
#28939 = EDGE_CURVE ( 'NONE', #55858, #35298, #27210, .T. ) ;
#28938 = FACE_OUTER_BOUND ( 'NONE', #8082, .T. ) ;
#28940 = CARTESIAN_POINT ( 'NONE',  ( 106.2913146648166531, -45.97580021205838818, 110.3280903695919903 ) ) ;
#28941 = VECTOR ( 'NONE', #57336, 1000.000000000000114 ) ;
#28942 = CIRCLE ( 'NONE', #37690, 4.874999999999990230 ) ;
#28943 = ADVANCED_FACE ( 'NONE', ( #47638 ), #48515, .T. ) ;
#28944 = DIRECTION ( 'NONE',  ( -3.100000000000000258E-29, 3.100000000000000044E-14, 1.000000000000000000 ) ) ;
#28945 = DIRECTION ( 'NONE',  ( 0.000000000000000000, 0.000000000000000000, -1.000000000000000000 ) ) ;
#28946 = EDGE_LOOP ( 'NONE', ( #17016, #83368, #18633, #18767 ) ) ;
#28947 = ORIENTED_EDGE ( 'NONE', *, *, #1142, .F. ) ;
#28948 = VECTOR ( 'NONE', #23615, 1000.000000000000000 ) ;
#28949 = CARTESIAN_POINT ( 'NONE',  ( 20.56670390244833158, -48.82844715994187368, 249.9678068554150059 ) ) ;
#28950 = VERTEX_POINT ( 'NONE', #55778 ) ;
#28951 = ORIENTED_EDGE ( 'NONE', *, *, #13070, .F. ) ;
#28952 = MECHANICAL_DESIGN_GEOMETRIC_PRESENTATION_REPRESENTATION (  '', ( #36206 ), #79729 ) ;
#28953 = CARTESIAN_POINT ( 'NONE',  ( 98.22997538087754776, -36.06364078424440578, 142.6987261630399644 ) ) ;
#28954 = CARTESIAN_POINT ( 'NONE',  ( -12.29197255332129401, 85.84955738763289901, 117.9171711396470386 ) ) ;
#28955 = AXIS2_PLACEMENT_3D ( 'NONE', #66244, #79472, #47020 ) ;
#28956 = CARTESIAN_POINT ( 'NONE',  ( 117.1274056176845733, -39.54282605291903252, 94.60991099019693706 ) ) ;
#28957 = DIRECTION ( 'NONE',  ( -0.000000000000000000, -0.000000000000000000, -1.000000000000000000 ) ) ;
#28958 = VERTEX_POINT ( 'NONE', #68556 ) ;
#28959 = EDGE_CURVE ( 'NONE', #13820, #36065, #80096, .T. ) ;
#28960 = ORIENTED_EDGE ( 'NONE', *, *, #57215, .F. ) ;
#28961 = EDGE_LOOP ( 'NONE', ( #4933, #84913, #88861, #82785 ) ) ;
#28962 = VECTOR ( 'NONE', #10322, 1000.000000000000000 ) ;
#28963 = DIRECTION ( 'NONE',  ( 0.000000000000000000, 0.000000000000000000, 1.000000000000000000 ) ) ;
#28964 = ORIENTED_EDGE ( 'NONE', *, *, #57579, .T. ) ;
#28965 = CARTESIAN_POINT ( 'NONE',  ( 112.1867106929447999, -26.95862322015887358, 14.68038718067299442 ) ) ;
#28966 = CARTESIAN_POINT ( 'NONE',  ( 113.6994007951720107, -45.60016365472323230, 184.0994347997199725 ) ) ;
#28967 = CARTESIAN_POINT ( 'NONE',  ( 12.70000000000000107, 82.54999999999999716, -117.8738102209307641 ) ) ;
#28968 = CARTESIAN_POINT ( 'NONE',  ( 163.0664832912739826, 22.62155284005901024, 327.8006252759110453 ) ) ;
#28969 = CARTESIAN_POINT ( 'NONE',  ( 102.3931144830280715, -26.71278082505766704, 131.4118157521009778 ) ) ;
#28970 = DIRECTION ( 'NONE',  ( -0.02150753337724187197, -0.0009076677972194977960, -0.9997682742251811083 ) ) ;
#28971 = ORIENTED_EDGE ( 'NONE', *, *, #31173, .T. ) ;
#28972 = CARTESIAN_POINT ( 'NONE',  ( 97.07195551945122247, -35.37924153545726114, 116.2203645627087099 ) ) ;
#28973 = ORIENTED_EDGE ( 'NONE', *, *, #63061, .T. ) ;
#28974 = CARTESIAN_POINT ( 'NONE',  ( 99.50479149024018000, -43.30586258244627373, 132.8967665784813903 ) ) ;
#28975 = VERTEX_POINT ( 'NONE', #89000 ) ;
#28977 = ORIENTED_EDGE ( 'NONE', *, *, #83033, .F. ) ;
#28976 = VECTOR ( 'NONE', #38298, 1000.000000000000000 ) ;
#28978 = DIRECTION ( 'NONE',  ( 1.000000000000000000, 0.000000000000000000, 0.000000000000000000 ) ) ;
#28979 = DIRECTION ( 'NONE',  ( 0.000000000000000000, -1.000000000000000000, 0.000000000000000000 ) ) ;
#28980 = CARTESIAN_POINT ( 'NONE',  ( 110.5552498863747246, -46.59121243395724576, 37.84705384733994293 ) ) ;
#28981 = CARTESIAN_POINT ( 'NONE',  ( 23.23280569011280505, 55.35248209492627325, 30.19701270168030405 ) ) ;
#28982 = CARTESIAN_POINT ( 'NONE',  ( 108.0015156553065054, -87.31935934938634603, -19.21044887263853695 ) ) ;
#28983 = CARTESIAN_POINT ( 'NONE',  ( 104.4081006704565908, -46.45808914256989652, 73.36479194333554688 ) ) ;
#28984 = CARTESIAN_POINT ( 'NONE',  ( 110.1509004715571791, -26.04776408289588474, 64.85276813305395649 ) ) ;
#28986 = CARTESIAN_POINT ( 'NONE',  ( 114.2249171546290967, -45.12625265263328345, 149.1508633711489722 ) ) ;
#28985 = DIRECTION ( 'NONE',  ( -0.9254794337955620787, -0.3787978585227822492, 0.000000000000000000 ) ) ;
#28987 = CARTESIAN_POINT ( 'NONE',  ( 108.4174892476684704, -26.73503592697917597, 70.96895860960096059 ) ) ;
#28988 = ADVANCED_FACE ( 'NONE', ( #19959 ), #26755, .F. ) ;
#28989 = CARTESIAN_POINT ( 'NONE',  ( 130.1657039024480582, -18.82844715994099971, 168.9256252759120116 ) ) ;
#28990 = VERTEX_POINT ( 'NONE', #62626 ) ;
#28991 = DIRECTION ( 'NONE',  ( 0.000000000000000000, 0.000000000000000000, -1.000000000000000000 ) ) ;
#28992 = VECTOR ( 'NONE', #78771, 1000.000000000000114 ) ;
#28993 = CARTESIAN_POINT ( 'NONE',  ( 99.99294959284291906, -33.44233276930008714, 9.125625275910962841 ) ) ;
#28994 = LINE ( 'NONE', #72115, #68861 ) ;
#28996 = ORIENTED_EDGE ( 'NONE', *, *, #50798, .F. ) ;
#28995 = EDGE_CURVE ( 'NONE', #85897, #26492, #40904, .T. ) ;
#28997 = CARTESIAN_POINT ( 'NONE',  ( 25.56670390244744695, -48.82844715994178841, 173.2178068554150627 ) ) ;
#28999 = ORIENTED_EDGE ( 'NONE', *, *, #2750, .T. ) ;
#28998 = CARTESIAN_POINT ( 'NONE',  ( 96.60586043895887087, -37.15609470439714102, 161.3584824187679487 ) ) ;
#29000 = LINE ( 'NONE', #49415, #58167 ) ;
#29001 = CARTESIAN_POINT ( 'NONE',  ( 105.1068790668079203, -26.46800427226792962, 231.2270538473399597 ) ) ;
#29002 = CARTESIAN_POINT ( 'NONE',  ( 116.5728860035299164, -32.34523831224304047, 100.1699109901969535 ) ) ;
#29003 = CARTESIAN_POINT ( 'NONE',  ( 143.2522959336310748, -139.0102598546870922, 247.5112310255240118 ) ) ;
#29004 = CARTESIAN_POINT ( 'NONE',  ( 46.32460016641637424, -48.34074026909789268, 180.4678068554150911 ) ) ;
#29006 = CARTESIAN_POINT ( 'NONE',  ( 72.26648329127297643, -71.52944715994142655, 342.9256252759110453 ) ) ;
#29005 = VECTOR ( 'NONE', #86634, 1000.000000000000000 ) ;
#29007 = EDGE_LOOP ( 'NONE', ( #44279, #85190, #26866, #18879 ) ) ;
#29008 = AXIS2_PLACEMENT_3D ( 'NONE', #39358, #49171, #7854 ) ;
#29009 = ORIENTED_EDGE ( 'NONE', *, *, #71557, .F. ) ;
#29010 = VERTEX_POINT ( 'NONE', #75371 ) ;
#29011 = ADVANCED_FACE ( 'NONE', ( #82202 ), #88561, .T. ) ;
#29012 = CIRCLE ( 'NONE', #13061, 2.117000000000000881 ) ;
#29013 = ORIENTED_EDGE ( 'NONE', *, *, #37803, .T. ) ;
#29014 = LINE ( 'NONE', #14942, #71410 ) ;
#29015 = CARTESIAN_POINT ( 'NONE',  ( 103.9393079366161032, -26.78443525705497663, 246.3184824187679567 ) ) ;
#29016 = FACE_OUTER_BOUND ( 'NONE', #17575, .T. ) ;
#29017 = EDGE_CURVE ( 'NONE', #14032, #31593, #53993, .T. ) ;
#29018 = DIRECTION ( 'NONE',  ( 0.000000000000000000, 0.000000000000000000, 1.000000000000000000 ) ) ;
#29019 = AXIS2_PLACEMENT_3D ( 'NONE', #74755, #3592, #40219 ) ;
#29021 = DIRECTION ( 'NONE',  ( 0.7071067811865171526, 0.7071067811865779928, 7.071067811865162747E-16 ) ) ;
#29020 = CARTESIAN_POINT ( 'NONE',  ( 176.7738106835046779, -48.62134037887552296, 300.4678068554149490 ) ) ;
#29022 = DIRECTION ( 'NONE',  ( 0.000000000000000000, 0.000000000000000000, 1.000000000000000000 ) ) ;
#29023 = CARTESIAN_POINT ( 'NONE',  ( 96.63682800883232460, -32.99879952304045361, 26.06514908543494613 ) ) ;
#29024 = ORIENTED_EDGE ( 'NONE', *, *, #68447, .T. ) ;
#29025 = EDGE_LOOP ( 'NONE', ( #17107, #16671, #79533, #15247, #8632, #36162, #61950, #87600, #60836, #10087, #77111, #49341, #29456, #60644, #47829, #2011, #62405, #42914, #12058, #53098, #2010, #35767 ) ) ;
#29026 = CARTESIAN_POINT ( 'NONE',  ( 95.56670390244703128, -104.2784471599411660, 17.71780685541799016 ) ) ;
#29027 = CARTESIAN_POINT ( 'NONE',  ( 108.4189123056540609, -26.73521668993834055, 15.97197629934867358 ) ) ;
#29028 = CARTESIAN_POINT ( 'NONE',  ( 100.4593337790148837, -29.47290724209160828, 281.6641967044818671 ) ) ;
#29029 =( GEOMETRIC_REPRESENTATION_CONTEXT ( 3 ) GLOBAL_UNCERTAINTY_ASSIGNED_CONTEXT ( ( #44153 ) ) GLOBAL_UNIT_ASSIGNED_CONTEXT ( ( #50535, #14695, #63281 ) ) REPRESENTATION_CONTEXT ( 'NONE', 'WORKASPACE' ) );
#29030 = CARTESIAN_POINT ( 'NONE',  ( 25.56670390244748603, -48.82844715994178841, 134.7178068554150627 ) ) ;
#29031 = CARTESIAN_POINT ( 'NONE',  ( 98.32242264099485851, -42.30440888850449710, 137.7661014663869992 ) ) ;
#29032 = DIRECTION ( 'NONE',  ( 0.000000000000000000, -1.000000000000000000, 0.000000000000000000 ) ) ;
#29033 = CARTESIAN_POINT ( 'NONE',  ( 107.0664832912750057, -36.72944715993903486, 9.425625275910970657 ) ) ;
#29034 = ORIENTED_EDGE ( 'NONE', *, *, #74084, .F. ) ;
#29035 = CARTESIAN_POINT ( 'NONE',  ( 116.8172847295623598, -34.15354512507032325, 180.0314075673595937 ) ) ;
#29036 = CARTESIAN_POINT ( 'NONE',  ( 97.70650630222581867, -40.25117133593911234, 57.61283866776680185 ) ) ;
#29037 = ORIENTED_EDGE ( 'NONE', *, *, #6855, .F. ) ;
#29038 = ORIENTED_EDGE ( 'NONE', *, *, #66840, .F. ) ;
#29039 = VECTOR ( 'NONE', #35392, 1000.000000000000000 ) ;
#29040 = CARTESIAN_POINT ( 'NONE',  ( -78.17042387453707875, 92.64232203292145584, 89.13693605261745745 ) ) ;
#29041 = CARTESIAN_POINT ( 'NONE',  ( 109.5509076938284068, -28.22321920626787062, 256.2815833058970725 ) ) ;
#29042 = DIRECTION ( 'NONE',  ( 0.000000000000000000, 0.000000000000000000, 1.000000000000000000 ) ) ;
#29043 = CARTESIAN_POINT ( 'NONE',  ( 51.34673845256487823, -36.02818131005847135, 193.9678068554150911 ) ) ;
#29044 = EDGE_CURVE ( 'NONE', #76131, #9747, #74924, .T. ) ;
#29045 = CARTESIAN_POINT ( 'NONE',  ( 97.06107109413245837, -37.99641193787602589, 86.42729194052971309 ) ) ;
#29046 = CARTESIAN_POINT ( 'NONE',  ( 84.43201024598467086, 69.85063172184842983, -83.23139715273229911 ) ) ;
#29047 = EDGE_LOOP ( 'NONE', ( #8839, #71526, #83882, #68263 ) ) ;
#29048 = AXIS2_PLACEMENT_3D ( 'NONE', #49117, #28701, #50018 ) ;
#29049 = LINE ( 'NONE', #37204, #58149 ) ;
#29050 = DIRECTION ( 'NONE',  ( -0.7071067811865436870, 0.000000000000000000, -0.7071067811865514585 ) ) ;
#29051 = ORIENTED_EDGE ( 'NONE', *, *, #41289, .F. ) ;
#29052 = CARTESIAN_POINT ( 'NONE',  ( 101.7107321646854246, -27.74380102040660390, 85.50419670448295051 ) ) ;
#29053 = ORIENTED_EDGE ( 'NONE', *, *, #44822, .F. ) ;
#29054 = CARTESIAN_POINT ( 'NONE',  ( 98.56159230830689921, -41.41319107723295900, 26.14956268521895311 ) ) ;
#29055 = CARTESIAN_POINT ( 'NONE',  ( 116.3254862984629909, -32.93730789470958342, 129.1356252759109680 ) ) ;
#29056 = CARTESIAN_POINT ( 'NONE',  ( 113.8941270090217444, -29.67983328691845557, 174.4641967044829585 ) ) ;
#29057 = CARTESIAN_POINT ( 'NONE',  ( 34.67381068360400320, -28.98061976758901181, 342.9256252759109884 ) ) ;
#29058 = CARTESIAN_POINT ( 'NONE',  ( 0.000000000000000000, 93.07500000000001705, 88.90000000000000568 ) ) ;
#29059 = PLANE ( 'NONE',  #21686 ) ;
#29060 = LINE ( 'NONE', #35860, #100 ) ;
#29061 = CARTESIAN_POINT ( 'NONE',  ( 116.1773114014176969, -43.03338396708490166, 9.356577656862985037 ) ) ;
#29062 = CARTESIAN_POINT ( 'NONE',  ( 80.31773373136907423, 94.30044247306076954, -87.20679752240577898 ) ) ;
#29063 = AXIS2_PLACEMENT_3D ( 'NONE', #15125, #16029, #57795 ) ;
#29064 = EDGE_LOOP ( 'NONE', ( #69247, #25703, #77549, #13127 ) ) ;
#29065 = CARTESIAN_POINT ( 'NONE',  ( 188.5667039024479834, -67.87844715994100397, 293.2178068554150627 ) ) ;
#29066 = VERTEX_POINT ( 'NONE', #40829 ) ;
#29067 = CARTESIAN_POINT ( 'NONE',  ( 117.2057360052074415, -34.12396560160815540, 120.0270538473389479 ) ) ;
#29068 = ADVANCED_FACE ( 'NONE', ( #6322 ), #89910, .F. ) ;
#29069 = CARTESIAN_POINT ( 'NONE',  ( 124.7270369540910622, 47.39308626936165325, -38.57547257139917463 ) ) ;
#29070 = ORIENTED_EDGE ( 'NONE', *, *, #17511, .T. ) ;
#29071 = EDGE_LOOP ( 'NONE', ( #83372, #6642 ) ) ;
#29072 = ORIENTED_EDGE ( 'NONE', *, *, #23601, .T. ) ;
#29073 = AXIS2_PLACEMENT_3D ( 'NONE', #48043, #74878, #34423 ) ;
#29074 = CARTESIAN_POINT ( 'NONE',  ( 29.56648329127400388, 15.62155284005900491, 328.6381252759109088 ) ) ;
#29075 = CARTESIAN_POINT ( 'NONE',  ( -254.0000000000000000, 53.97500000000000142, 50.79999999999999716 ) ) ;
#29076 = CARTESIAN_POINT ( 'NONE',  ( 147.0667039024470739, -137.6784471599409017, 55.21780685541800437 ) ) ;
#29077 = DIRECTION ( 'NONE',  ( 0.000000000000000000, 0.000000000000000000, -1.000000000000000000 ) ) ;
#29078 = PLANE ( 'NONE',  #14193 ) ;
#29079 = CARTESIAN_POINT ( 'NONE',  ( 97.07537224739735393, -33.75284044148263973, 27.09562527591097236 ) ) ;
#29080 = ADVANCED_FACE ( 'NONE', ( #76710 ), #75815, .F. ) ;
#29081 = FACE_BOUND ( 'NONE', #48757, .T. ) ;
#29082 = EDGE_LOOP ( 'NONE', ( #5040, #34309, #60953, #62619, #55673 ) ) ;
#29083 = PLANE ( 'NONE',  #68857 ) ;
#29084 = EDGE_CURVE ( 'NONE', #30532, #52826, #81537, .T. ) ;
#29085 = AXIS2_PLACEMENT_3D ( 'NONE', #56214, #83966, #41251 ) ;
#29086 = CARTESIAN_POINT ( 'NONE',  ( 194.5667039024485234, -47.82844715993405060, 180.4678068554150343 ) ) ;
#29087 = ORIENTED_EDGE ( 'NONE', *, *, #17423, .F. ) ;
#29088 = ORIENTED_EDGE ( 'NONE', *, *, #61140, .F. ) ;
#29089 = CARTESIAN_POINT ( 'NONE',  ( 168.0371591254543944, -48.62818131005519007, 237.4678068554150059 ) ) ;
#29090 = CARTESIAN_POINT ( 'NONE',  ( 107.0667039024470313, -104.2784471599420471, -19.18411693322902423 ) ) ;
#29091 = ADVANCED_FACE ( 'NONE', ( #7669 ), #81752, .T. ) ;
#29092 = CARTESIAN_POINT ( 'NONE',  ( 183.5150000000000148, 37.33800000000000097, 32.46912895322940074 ) ) ;
#29093 = CARTESIAN_POINT ( 'NONE',  ( 160.2664750769289697, 20.32000000000000028, 148.0533267522752112 ) ) ;
#29094 = AXIS2_PLACEMENT_3D ( 'NONE', #448, #28141, #47237 ) ;
#29095 = CARTESIAN_POINT ( 'NONE',  ( 106.5889295881363950, -27.03189230550456656, 194.5381341137909601 ) ) ;
#29096 = CARTESIAN_POINT ( 'NONE',  ( 0.000000000000000000, 127.0000000000000000, -103.1875000000000000 ) ) ;
#29097 = CARTESIAN_POINT ( 'NONE',  ( 163.0664832912739826, -0.2185775633789972805, 333.4006252759120343 ) ) ;
#29098 = CARTESIAN_POINT ( 'NONE',  ( 103.8276485124378183, -46.72253193893131140, 82.32705384733995402 ) ) ;
#29099 = ORIENTED_EDGE ( 'NONE', *, *, #53251, .T. ) ;
#29100 = CARTESIAN_POINT ( 'NONE',  ( 172.5664832912728457, -18.82844715994071194, 141.9256252759118979 ) ) ;
#29101 = ORIENTED_EDGE ( 'NONE', *, *, #22173, .F. ) ;
#29102 = VECTOR ( 'NONE', #24319, 1000.000000000000000 ) ;
#29103 = CARTESIAN_POINT ( 'NONE',  ( 106.0291822676640408, -26.77097407813891650, 276.1590324519580122 ) ) ;
#29105 = EDGE_LOOP ( 'NONE', ( #81992, #84810, #66999, #65600, #7063, #55947, #8461, #80638, #46218, #76295 ) ) ;
#29104 = EDGE_CURVE ( 'NONE', #73470, #34867, #7527, .T. ) ;
#29106 = CARTESIAN_POINT ( 'NONE',  ( 167.2371591254545820, -47.82818131005522133, 117.4678068554150485 ) ) ;
#29107 = ORIENTED_EDGE ( 'NONE', *, *, #46285, .T. ) ;
#29108 = FACE_OUTER_BOUND ( 'NONE', #2278, .T. ) ;
#29109 = CARTESIAN_POINT ( 'NONE',  ( -31.75000000000000000, 24.56180297284579694, -3.174999999999779998 ) ) ;
#29110 = AXIS2_PLACEMENT_3D ( 'NONE', #2022, #29282, #22034 ) ;
#29111 = CARTESIAN_POINT ( 'NONE',  ( 154.5667039024470171, -79.67844715994088745, 155.2178068554179902 ) ) ;
#29112 = ORIENTED_EDGE ( 'NONE', *, *, #7776, .T. ) ;
#29113 = CARTESIAN_POINT ( 'NONE',  ( 98.84041870859987000, -43.22715631800404879, 91.85848241876892928 ) ) ;
#29115 = CARTESIAN_POINT ( 'NONE',  ( 83.22858459372966422, 79.26455342200334542, -100.5877059554736093 ) ) ;
#29114 = DIRECTION ( 'NONE',  ( 0.000000000000000000, 0.000000000000000000, -1.000000000000000000 ) ) ;
#29116 = CARTESIAN_POINT ( 'NONE',  ( 100.8961411191535973, 120.6499999999999915, -3.968749999999580336 ) ) ;
#29117 = CARTESIAN_POINT ( 'NONE',  ( -7.336232340149017261, 72.29773750292761747, 118.1289122150180475 ) ) ;
#29118 = ORIENTED_EDGE ( 'NONE', *, *, #4599, .T. ) ;
#29119 = EDGE_CURVE ( 'NONE', #15522, #20262, #83096, .T. ) ;
#29120 = CARTESIAN_POINT ( 'NONE',  ( 57.14999999999999858, 60.86974387893089755, 297.6879999999999882 ) ) ;
#29121 = EDGE_CURVE ( 'NONE', #18060, #63362, #77610, .T. ) ;
#29122 = CARTESIAN_POINT ( 'NONE',  ( 105.7995185446386444, -26.72403495942892349, 155.1772919380402129 ) ) ;
#29123 = EDGE_CURVE ( 'NONE', #64715, #17090, #29460, .T. ) ;
#29124 = DIRECTION ( 'NONE',  ( 0.000000000000000000, 0.000000000000000000, -1.000000000000000000 ) ) ;
#29125 = CIRCLE ( 'NONE', #68282, 10.00000000000002487 ) ;
#29126 = CARTESIAN_POINT ( 'NONE',  ( 114.0366484478682310, -28.94779845652852757, 110.4956252759109816 ) ) ;
#29127 = ADVANCED_FACE ( 'NONE', ( #22656 ), #64874, .F. ) ;
#29129 = CYLINDRICAL_SURFACE ( 'NONE', #28212, 0.5000000000000031086 ) ;
#29128 = DIRECTION ( 'NONE',  ( 0.000000000000000000, 1.000000000000000000, 0.000000000000000000 ) ) ;
#29130 = DIRECTION ( 'NONE',  ( -0.6893610196960178182, -0.7071067811865296981, -0.1574210421884305322 ) ) ;
#29131 = AXIS2_PLACEMENT_3D ( 'NONE', #32310, #67285, #24619 ) ;
#29132 = EDGE_LOOP ( 'NONE', ( #69508, #13170 ) ) ;
#29133 = LINE ( 'NONE', #49547, #57844 ) ;
#29134 = CARTESIAN_POINT ( 'NONE',  ( 96.37928053093618530, -33.66421044892481262, 137.1041967044819501 ) ) ;
#29135 = AXIS2_PLACEMENT_3D ( 'NONE', #60671, #4832, #33873 ) ;
#29137 = ORIENTED_EDGE ( 'NONE', *, *, #49043, .F. ) ;
#29136 = FACE_OUTER_BOUND ( 'NONE', #13219, .T. ) ;
#29138 = CARTESIAN_POINT ( 'NONE',  ( 110.0853110376240664, -46.03288293484944660, 8.827053847338950376 ) ) ;
#29139 = DIRECTION ( 'NONE',  ( -0.7071067811856560636, -0.7071067811874389708, 0.000000000000000000 ) ) ;
#29140 = DIRECTION ( 'NONE',  ( 1.000000000000000000, 0.000000000000000000, 0.000000000000000000 ) ) ;
#29141 = LINE ( 'NONE', #1882, #85047 ) ;
#29142 = DIRECTION ( 'NONE',  ( 0.2884130866282236250, -0.7071067811865507924, -0.6456143519637524975 ) ) ;
#29143 = CARTESIAN_POINT ( 'NONE',  ( 63.03715912545639100, -24.42818131006017168, 180.4678068554151196 ) ) ;
#29144 = CARTESIAN_POINT ( 'NONE',  ( 123.6837132603318423, -20.11243780205705534, 239.5838068554170377 ) ) ;
#29145 = CARTESIAN_POINT ( 'NONE',  ( 107.4826147187165333, -46.50135945624624156, 237.6099109901969655 ) ) ;
#29146 = EDGE_LOOP ( 'NONE', ( #57435, #2382 ) ) ;
#29147 = ORIENTED_EDGE ( 'NONE', *, *, #3689, .F. ) ;
#29148 = CARTESIAN_POINT ( 'NONE',  ( 98.18569924386140713, -36.28921507361370402, 167.7187261630399462 ) ) ;
#29149 = CARTESIAN_POINT ( 'NONE',  ( 131.3167039024479834, -50.82844715994100682, 198.9178068554149945 ) ) ;
#29150 = CARTESIAN_POINT ( 'NONE',  ( 101.4552306925257454, -43.61128330217721327, 8.464440448754938728 ) ) ;
#29151 = CARTESIAN_POINT ( 'NONE',  ( 147.0667039024470739, -137.6784471599409017, 245.4361138694860074 ) ) ;
#29152 = DIRECTION ( 'NONE',  ( 1.000000000000000000, 1.261617073437676668E-15, 9.462128050782575008E-16 ) ) ;
#29153 = DIRECTION ( 'NONE',  ( 0.000000000000000000, -1.000000000000000000, 0.000000000000000000 ) ) ;
#29154 = VECTOR ( 'NONE', #41388, 1000.000000000000000 ) ;
#29155 = LINE ( 'NONE', #41857, #17364 ) ;
#29156 = CARTESIAN_POINT ( 'NONE',  ( 97.79822847042071032, -40.48439528968561518, 37.63249612555365786 ) ) ;
#29157 = CARTESIAN_POINT ( 'NONE',  ( 113.0129699484216133, -46.01939436189644539, 218.0175300378159591 ) ) ;
#29158 = CARTESIAN_POINT ( 'NONE',  ( 97.81480632908598238, -40.51613010894325839, 171.6358981596145270 ) ) ;
#29159 = VERTEX_POINT ( 'NONE', #850 ) ;
#29161 = EDGE_LOOP ( 'NONE', ( #60070, #33429 ) ) ;
#29160 = VECTOR ( 'NONE', #78412, 1000.000000000000000 ) ;
#29162 = CARTESIAN_POINT ( 'NONE',  ( -82.96136257730057650, 80.89704698943971550, -100.8082743238004610 ) ) ;
#29163 = CARTESIAN_POINT ( 'NONE',  ( -88.20392011030175183, 93.55466788070658879, -79.21949419058860542 ) ) ;
#29164 = CARTESIAN_POINT ( 'NONE',  ( 112.0669571316796151, -45.48782181672719815, 123.9881978270240950 ) ) ;
#29165 = LINE ( 'NONE', #64580, #33208 ) ;
#29166 = AXIS2_PLACEMENT_3D ( 'NONE', #7825, #14196, #13746 ) ;
#29167 = CARTESIAN_POINT ( 'NONE',  ( 96.86520444330115254, -38.59296402346411980, 47.48229194257691432 ) ) ;
#29168 = DIRECTION ( 'NONE',  ( -0.4999999999999985567, -0.8660254037844395958, 2.602085213965200860E-14 ) ) ;
#29169 = VERTEX_POINT ( 'NONE', #43060 ) ;
#29170 = CIRCLE ( 'NONE', #84305, 2.500000000000002220 ) ;
#29171 = CARTESIAN_POINT ( 'NONE',  ( 50.79999999999999716, 73.02500000000000568, 257.1750000000000114 ) ) ;
#29172 = EDGE_CURVE ( 'NONE', #76706, #65464, #88787, .T. ) ;
#29173 = CYLINDRICAL_SURFACE ( 'NONE', #23606, 3.000000864267367895 ) ;
#29174 = CARTESIAN_POINT ( 'NONE',  ( 111.1275225509982505, -27.12762490620188771, 244.7584824187679544 ) ) ;
#29175 = EDGE_CURVE ( 'NONE', #60931, #28457, #49429, .T. ) ;
#29176 = ORIENTED_EDGE ( 'NONE', *, *, #12782, .F. ) ;
#29177 = EDGE_CURVE ( 'NONE', #5363, #23986, #50786, .T. ) ;
#29178 = LINE ( 'NONE', #43684, #88350 ) ;
#29179 = CARTESIAN_POINT ( 'NONE',  ( 0.000000000000000000, 65.60000000000000853, 118.5560000000000116 ) ) ;
#29180 = DIRECTION ( 'NONE',  ( -3.100000000000000258E-29, 3.100000000000000044E-14, 1.000000000000000000 ) ) ;
#29181 = CARTESIAN_POINT ( 'NONE',  ( 109.1158479366964684, -45.13783758831200998, 85.57285227435401964 ) ) ;
#29182 = CARTESIAN_POINT ( 'NONE',  ( 103.7162039098101332, -26.17194585468624624, 201.3089586092439731 ) ) ;
#29183 = EDGE_CURVE ( 'NONE', #9320, #83315, #29014, .T. ) ;
#29184 = AXIS2_PLACEMENT_3D ( 'NONE', #60628, #67006, #80657 ) ;
#29185 = DIRECTION ( 'NONE',  ( -1.000000000000000000, -1.206764157201257538E-15, 0.000000000000000000 ) ) ;
#29186 = VERTEX_POINT ( 'NONE', #51218 ) ;
#29187 = EDGE_CURVE ( 'NONE', #87997, #46741, #9458, .T. ) ;
#29188 = CARTESIAN_POINT ( 'NONE',  ( 138.0667039024479550, -26.72944715994091069, 239.5838068554170377 ) ) ;
#29190 = VERTEX_POINT ( 'NONE', #78522 ) ;
#29189 = EDGE_CURVE ( 'NONE', #48853, #56759, #20632, .T. ) ;
#29192 = VERTEX_POINT ( 'NONE', #56698 ) ;
#29191 = AXIS2_PLACEMENT_3D ( 'NONE', #21746, #56685, #63507 ) ;
#29193 = EDGE_CURVE ( 'NONE', #34651, #58881, #2205, .T. ) ;
#29194 = FACE_OUTER_BOUND ( 'NONE', #46671, .T. ) ;
#29195 = ORIENTED_EDGE ( 'NONE', *, *, #41285, .F. ) ;
#29196 = ORIENTED_EDGE ( 'NONE', *, *, #18301, .T. ) ;
#29197 = DIRECTION ( 'NONE',  ( -1.000000000000000000, 0.000000000000000000, 0.000000000000000000 ) ) ;
#29198 = ADVANCED_FACE ( 'NONE', ( #63071 ), #70799, .T. ) ;
#29199 = CARTESIAN_POINT ( 'NONE',  ( 98.34984597051438016, -31.65660619317119640, 41.90638639042374791 ) ) ;
#29200 = CARTESIAN_POINT ( 'NONE',  ( 113.7853715510712789, -42.80144937323932908, 82.67622935188595079 ) ) ;
#29201 = AXIS2_PLACEMENT_3D ( 'NONE', #67279, #32763, #30648 ) ;
#29202 = CARTESIAN_POINT ( 'NONE',  ( 117.4518178387850895, -35.59314106485747686, 278.9127681330539872 ) ) ;
#29203 = CARTESIAN_POINT ( 'NONE',  ( 0.000000000000000000, 117.4749999999999943, -95.25000000000000000 ) ) ;
#29204 = DIRECTION ( 'NONE',  ( 0.8660254037844382635, 0.5000000000000008882, -1.550000000000000022E-14 ) ) ;
#29205 = CIRCLE ( 'NONE', #79988, 0.5000000000000004441 ) ;
#29207 = EDGE_LOOP ( 'NONE', ( #37131, #16904 ) ) ;
#29206 = EDGE_CURVE ( 'NONE', #68878, #13709, #20430, .T. ) ;
#29208 = EDGE_LOOP ( 'NONE', ( #30376, #39389 ) ) ;
#29209 = LINE ( 'NONE', #71888, #11624 ) ;
#29210 = LINE ( 'NONE', #16030, #27492 ) ;
#29211 = LINE ( 'NONE', #49624, #75960 ) ;
#29212 = CARTESIAN_POINT ( 'NONE',  ( 116.7274023843879718, -38.25590632018516857, 113.7013395616259857 ) ) ;
#29213 = CARTESIAN_POINT ( 'NONE',  ( 117.2063690954211808, -34.12380291655402687, 124.0270538473399426 ) ) ;
#29214 = CARTESIAN_POINT ( 'NONE',  ( 117.5632142390390555, -36.54506796471968499, 288.8413395616251478 ) ) ;
#29215 = ORIENTED_EDGE ( 'NONE', *, *, #66563, .T. ) ;
#29216 = CARTESIAN_POINT ( 'NONE',  ( 96.68196755257399388, -35.80810936406337674, 231.2556252759109725 ) ) ;
#29217 = DIRECTION ( 'NONE',  ( 2.999999999999999839E-15, -1.000000000000000000, 2.999999999999999900E-30 ) ) ;
#29218 = CARTESIAN_POINT ( 'NONE',  ( 12.10537486922539863, 78.70349232879850376, 129.9937543560634481 ) ) ;
#29219 = DIRECTION ( 'NONE',  ( 1.000000000000000000, 4.163336342344333240E-14, 0.000000000000000000 ) ) ;
#29221 = CARTESIAN_POINT ( 'NONE',  ( 68.69165074297623619, -139.3035918984462000, 245.6745758308635175 ) ) ;
#29220 = CARTESIAN_POINT ( 'NONE',  ( 183.5150000000000148, 52.73749999999999716, -26.11912895322935313 ) ) ;
#29222 = CARTESIAN_POINT ( 'NONE',  ( 105.1030388873302854, -25.43975401280837900, 322.2645585102944779 ) ) ;
#29223 = DIRECTION ( 'NONE',  ( 0.5000000000000015543, 0.8660254037844377084, -2.602085213965216006E-14 ) ) ;
#29224 = CARTESIAN_POINT ( 'NONE',  ( 111.4303245704231244, -106.2204344580498372, -19.78219314458196010 ) ) ;
#29225 = AXIS2_PLACEMENT_3D ( 'NONE', #5322, #5773, #62514 ) ;
#29226 = CARTESIAN_POINT ( 'NONE',  ( -12.67977336836081825, 83.37982733273464930, 129.9388093972407034 ) ) ;
#29227 = CARTESIAN_POINT ( 'NONE',  ( 116.3212776292296127, -32.94146857471318413, 287.6356252759109680 ) ) ;
#29228 = DIRECTION ( 'NONE',  ( 0.000000000000000000, 0.000000000000000000, -1.000000000000000000 ) ) ;
#29229 = EDGE_CURVE ( 'NONE', #81211, #78112, #1758, .T. ) ;
#29231 = VERTEX_POINT ( 'NONE', #84887 ) ;
#29230 = CARTESIAN_POINT ( 'NONE',  ( 100.9546727909157511, -28.70702574251799533, 260.5939586112514803 ) ) ;
#29232 = DIRECTION ( 'NONE',  ( 1.000000000000000000, 4.299999999999999979E-14, 1.000000000000000078E-15 ) ) ;
#29233 = CARTESIAN_POINT ( 'NONE',  ( 101.6391055438642894, -45.65636906804281381, 247.1413395616249602 ) ) ;
#29234 = CARTESIAN_POINT ( 'NONE',  ( 98.26135236841564335, -42.31085888804770434, 182.7756252759109543 ) ) ;
#29235 = CARTESIAN_POINT ( 'NONE',  ( 95.23451729606020422, -35.71612027476381002, 32.25848241876794020 ) ) ;
#29236 = ADVANCED_FACE ( 'NONE', ( #85342 ), #78072, .F. ) ;
#29237 = VECTOR ( 'NONE', #87205, 1000.000000000000000 ) ;
#29239 = CARTESIAN_POINT ( 'NONE',  ( 99.04406186115555499, -42.84125764320888408, 46.84395860957398128 ) ) ;
#29238 = CARTESIAN_POINT ( 'NONE',  ( 72.26648329127297643, -71.52944715994141234, 361.9756252759109998 ) ) ;
#29240 = DIRECTION ( 'NONE',  ( -3.100000000000000258E-29, 3.100000000000000044E-14, 1.000000000000000000 ) ) ;
#29241 = AXIS2_PLACEMENT_3D ( 'NONE', #36223, #1261, #28498 ) ;
#29242 = ORIENTED_EDGE ( 'NONE', *, *, #76047, .F. ) ;
#29243 = DIRECTION ( 'NONE',  ( -4.237773401492740281E-14, 1.000000000000000000, 0.000000000000000000 ) ) ;
#29244 = ORIENTED_EDGE ( 'NONE', *, *, #12391, .F. ) ;
#29245 = CARTESIAN_POINT ( 'NONE',  ( 107.7643578131546178, -45.27140672887451700, 177.0638483995059858 ) ) ;
#29247 = ORIENTED_EDGE ( 'NONE', *, *, #4068, .F. ) ;
#29246 = CARTESIAN_POINT ( 'NONE',  ( 99.04370088267752692, -42.84071521736686350, 186.8444288791077668 ) ) ;
#29248 = DIRECTION ( 'NONE',  ( -0.9963424814100680926, 0.08544974978095698503, 0.000000000000000000 ) ) ;
#29249 = CARTESIAN_POINT ( 'NONE',  ( 97.44537786355549258, -42.12371753947135744, 177.7451490854349743 ) ) ;
#29250 = CARTESIAN_POINT ( 'NONE',  ( 118.5256205435843526, -36.72944715994100306, 277.6356252759110248 ) ) ;
#29251 = CARTESIAN_POINT ( 'NONE',  ( -546.0365000000000464, 53.97500000000000142, 50.79999999999999716 ) ) ;
#29252 = CARTESIAN_POINT ( 'NONE',  ( 110.6700764351487578, -27.40068518752502413, 85.78334170510873946 ) ) ;
#29253 = AXIS2_PLACEMENT_3D ( 'NONE', #49454, #14967, #48544 ) ;
#29254 = FACE_OUTER_BOUND ( 'NONE', #36445, .T. ) ;
#29255 = DIRECTION ( 'NONE',  ( 0.000000000000000000, 0.000000000000000000, -1.000000000000000000 ) ) ;
#29256 = CARTESIAN_POINT ( 'NONE',  ( 112.4472966703649348, -46.45872411559678028, 102.9784824187679817 ) ) ;
#29257 = ORIENTED_EDGE ( 'NONE', *, *, #62192, .F. ) ;
#29258 = ORIENTED_EDGE ( 'NONE', *, *, #40528, .T. ) ;
#29259 = VECTOR ( 'NONE', #50661, 999.9999999999998863 ) ;
#29260 = CARTESIAN_POINT ( 'NONE',  ( 101.8597501770084364, -45.35270844728685802, 48.57586902018196184 ) ) ;
#29261 = CARTESIAN_POINT ( 'NONE',  ( 132.1035770464691836, -92.77767617834375358, 250.2178068554180470 ) ) ;
#29263 = CARTESIAN_POINT ( 'NONE',  ( 115.7831076883988146, -41.80230947738378688, 38.40645861222698443 ) ) ;
#29262 = CARTESIAN_POINT ( 'NONE',  ( 97.28849942844340148, -36.49606577720026479, 192.3070538473389490 ) ) ;
#29264 = CARTESIAN_POINT ( 'NONE',  ( 142.0664832912740110, -8.729447159940995959, -4.824374724088994704 ) ) ;
#29265 = CARTESIAN_POINT ( 'NONE',  ( 177.1649999999999920, 14.63749999999999929, -9.525000000000000355 ) ) ;
#29266 = AXIS2_PLACEMENT_3D ( 'NONE', #38032, #23967, #86191 ) ;
#29267 = CARTESIAN_POINT ( 'NONE',  ( 107.0664832912739968, -36.72944715994100306, 287.6356252759109680 ) ) ;
#29268 = DIRECTION ( 'NONE',  ( 0.000000000000000000, 0.000000000000000000, 1.000000000000000000 ) ) ;
#29269 = CARTESIAN_POINT ( 'NONE',  ( 67.12633028470673935, -67.93405945762680176, 245.9787629646199036 ) ) ;
#29270 = CARTESIAN_POINT ( 'NONE',  ( 114.7100688122353063, -43.78666090992615523, 123.2327681330539519 ) ) ;
#29271 = ORIENTED_EDGE ( 'NONE', *, *, #52324, .F. ) ;
#29272 = ORIENTED_EDGE ( 'NONE', *, *, #25093, .F. ) ;
#29273 = AXIS2_PLACEMENT_3D ( 'NONE', #45162, #24737, #44272 ) ;
#29274 = ORIENTED_EDGE ( 'NONE', *, *, #34961, .T. ) ;
#29275 =( NAMED_UNIT ( * ) SI_UNIT ( $, .STERADIAN. ) SOLID_ANGLE_UNIT ( ) );
#29276 = CARTESIAN_POINT ( 'NONE',  ( -99.17062120112652224, 90.28418055714726620, -84.91247172076052152 ) ) ;
#29277 = DIRECTION ( 'NONE',  ( 1.000000000000000000, 4.237773401492740281E-14, 0.000000000000000000 ) ) ;
#29278 = B_SPLINE_CURVE_WITH_KNOTS ( 'NONE', 3,
 ( #75031, #32332, #87766, #18720, #89115, #81860, #33247, #26874, #61829, #25530, #19177, #46846, #54550, #5556, #53203, #26436, #67306, #89563, #60484, #80972, #82766, #88233, #25986, #46403, #45947, #47303, #73686, #12821, #43178 ),
 .UNSPECIFIED., .F., .F.,
 ( 4, 2, 1, 1, 1, 1, 1, 2, 2, 2, 2, 2, 2, 2, 2, 2, 4 ),
 ( 0.5000605868651970543, 0.5003046979067664601, 0.5005488089483359770, 0.5010370310314751219, 0.5020134751977542997, 0.5039663635303122113, 0.5078721401954277015, 0.5156836935256587928, 0.5313068001861211975, 0.5625530135070464510, 0.6250454401488969580, 0.6875378667907473540, 0.7500302934325979720, 0.8125227200744484790, 0.8750151467162989860, 0.9375075733581494930, 1.000000000000000000 ),
 .UNSPECIFIED. ) ;
#29279 = CARTESIAN_POINT ( 'NONE',  ( 0.000000000000000000, 2.269999999999994245, 0.000000000000000000 ) ) ;
#29280 = CARTESIAN_POINT ( 'NONE',  ( 104.3825147926133354, -28.50161402210781603, 208.1576141791150008 ) ) ;
#29281 = EDGE_CURVE ( 'NONE', #15679, #55444, #71695, .T. ) ;
#29282 = DIRECTION ( 'NONE',  ( -0.7071067811865483499, -0.7071067811865466846, -7.071067811865491110E-16 ) ) ;
#29283 = EDGE_CURVE ( 'NONE', #53694, #22477, #75544, .T. ) ;
#29284 = CARTESIAN_POINT ( 'NONE',  ( 111.7942743463426609, -25.86259492108981206, 134.7499109901969518 ) ) ;
#29285 = EDGE_CURVE ( 'NONE', #66793, #64886, #14665, .T. ) ;
#29286 = CARTESIAN_POINT ( 'NONE',  ( 179.7974245136200011, -36.32844715994040996, 117.4678068554150627 ) ) ;
#29287 = VERTEX_POINT ( 'NONE', #25312 ) ;
#29289 = ORIENTED_EDGE ( 'NONE', *, *, #73052, .F. ) ;
#29288 = ORIENTED_EDGE ( 'NONE', *, *, #59088, .T. ) ;
#29290 = CIRCLE ( 'NONE', #87313, 2.750000000000002665 ) ;
#29291 = ADVANCED_FACE ( 'NONE', ( #79862 ), #52979, .T. ) ;
#29292 = PLANE ( 'NONE',  #82524 ) ;
#29293 = ORIENTED_EDGE ( 'NONE', *, *, #86196, .F. ) ;
#29294 = EDGE_LOOP ( 'NONE', ( #10527, #58476, #64711, #26735 ) ) ;
#29295 = DIRECTION ( 'NONE',  ( -0.7071067812159692600, -0.7071067811571258854, 2.899137802744100722E-29 ) ) ;
#29296 = CARTESIAN_POINT ( 'NONE',  ( 219.9639999999999986, 40.03750000000000142, -7.937500000000000000 ) ) ;
#29297 = CARTESIAN_POINT ( 'NONE',  ( 115.4467593082293178, -40.97768201889641659, 244.8968214011349573 ) ) ;
#29298 = EDGE_CURVE ( 'NONE', #63362, #24618, #4434, .T. ) ;
#29299 = LINE ( 'NONE', #71534, #26086 ) ;
#29300 = VERTEX_POINT ( 'NONE', #46635 ) ;
#29301 = CIRCLE ( 'NONE', #67018, 9.499999999999980460 ) ;
#29302 = CARTESIAN_POINT ( 'NONE',  ( 116.3379421530591884, -39.39079624489408360, 9.635625275910941312 ) ) ;
#29303 = DIRECTION ( 'NONE',  ( 1.387778780781444492E-15, 0.000000000000000000, -1.000000000000000000 ) ) ;
#29304 = ORIENTED_EDGE ( 'NONE', *, *, #22420, .T. ) ;
#29305 = ORIENTED_EDGE ( 'NONE', *, *, #37185, .F. ) ;
#29306 = EDGE_CURVE ( 'NONE', #28582, #34717, #39289, .T. ) ;
#29307 = CARTESIAN_POINT ( 'NONE',  ( 111.0058300909787761, -45.92119593049321935, 112.8986727163515269 ) ) ;
#29308 = VERTEX_POINT ( 'NONE', #87551 ) ;
#29309 = EDGE_LOOP ( 'NONE', ( #55909, #88139, #61273 ) ) ;
#29310 = EDGE_CURVE ( 'NONE', #68446, #83210, #80302, .T. ) ;
#29311 = CARTESIAN_POINT ( 'NONE',  ( 113.9883325317156135, -31.53436023685440048, 262.1690427505439516 ) ) ;
#29312 = CARTESIAN_POINT ( 'NONE',  ( 108.8526476014722277, -47.02293932800507292, 167.7127681330539701 ) ) ;
#29313 = CARTESIAN_POINT ( 'NONE',  ( 109.5033840998384136, -46.84330794493983774, 132.7641967044819751 ) ) ;
#29314 = DIRECTION ( 'NONE',  ( -0.9254794337955620787, -0.3787978585227823602, 0.000000000000000000 ) ) ;
#29315 = CARTESIAN_POINT ( 'NONE',  ( 104.4105741502040701, -26.00004237129247642, 236.2575300378159682 ) ) ;
#29316 = CARTESIAN_POINT ( 'NONE',  ( 30.48091746481746611, -48.32844715994156815, 129.9678068554150627 ) ) ;
#29317 = CARTESIAN_POINT ( 'NONE',  ( 0.000000000000000000, 239.0000000000000000, 154.6557476874258441 ) ) ;
#29318 = ORIENTED_EDGE ( 'NONE', *, *, #18001, .T. ) ;
#29319 = CARTESIAN_POINT ( 'NONE',  ( -130.3267157422428966, 72.47310549519059464, -7.740869983443031010 ) ) ;
#29320 = ORIENTED_EDGE ( 'NONE', *, *, #14255, .T. ) ;
#29322 = EDGE_CURVE ( 'NONE', #10974, #18138, #127, .T. ) ;
#29321 = AXIS2_PLACEMENT_3D ( 'NONE', #26578, #40195, #18416 ) ;
#29323 = ORIENTED_EDGE ( 'NONE', *, *, #75319, .F. ) ;
#29324 = VECTOR ( 'NONE', #23553, 1000.000000000000000 ) ;
#29325 = AXIS2_PLACEMENT_3D ( 'NONE', #89413, #59880, #6283 ) ;
#29326 = CARTESIAN_POINT ( 'NONE',  ( 98.34291691341793751, -29.86560907334282788, 200.8080062282919869 ) ) ;
#29327 = EDGE_LOOP ( 'NONE', ( #27940, #4915, #74957, #62745 ) ) ;
#29328 = CARTESIAN_POINT ( 'NONE',  ( 108.5898285964631640, -47.07861824576353627, 142.6927681330539883 ) ) ;
#29329 = CARTESIAN_POINT ( 'NONE',  ( 41.56648329127399677, -18.82844715994099971, 76.80862527591200717 ) ) ;
#29330 = LINE ( 'NONE', #15252, #53623 ) ;
#29331 = CARTESIAN_POINT ( 'NONE',  ( 0.000000000000000000, 20.32000000000000028, 0.000000000000000000 ) ) ;
#29334 = CARTESIAN_POINT ( 'NONE',  ( 106.5683798796750779, -47.15615894637585370, 243.5384824187679556 ) ) ;
#29333 = DIRECTION ( 'NONE',  ( 0.000000000000000000, 0.000000000000000000, 1.000000000000000000 ) ) ;
#29332 = FACE_OUTER_BOUND ( 'NONE', #54436, .T. ) ;
#29335 = CARTESIAN_POINT ( 'NONE',  ( 115.0439452383991892, -99.09543445804915507, 2.217806855417836509 ) ) ;
#29336 = CARTESIAN_POINT ( 'NONE',  ( 219.9639999999999986, 40.03750000000000142, -7.937500000000000000 ) ) ;
#29337 = CIRCLE ( 'NONE', #22145, 2.517499999999998739 ) ;
#29338 = CARTESIAN_POINT ( 'NONE',  ( 107.3241674272228892, -25.27320757387406402, 321.5865679059475610 ) ) ;
#29339 = DIRECTION ( 'NONE',  ( -0.7071067811567173234, 0.7071067812163779331, 0.000000000000000000 ) ) ;
#29340 = CARTESIAN_POINT ( 'NONE',  ( 115.7831076753790143, -41.80230950073445939, 259.4064586101131908 ) ) ;
#29341 = AXIS2_PLACEMENT_3D ( 'NONE', #13792, #28301, #77363 ) ;
#29342 = DIRECTION ( 'NONE',  ( 0.000000000000000000, 0.000000000000000000, -1.000000000000000000 ) ) ;
#29344 = ORIENTED_EDGE ( 'NONE', *, *, #82344, .F. ) ;
#29343 = CARTESIAN_POINT ( 'NONE',  ( 114.4461924768642405, -27.39302975889309266, 274.5441967044824878 ) ) ;
#29345 = FACE_OUTER_BOUND ( 'NONE', #24925, .T. ) ;
#29346 = CARTESIAN_POINT ( 'NONE',  ( 101.7582431991767464, -45.72772181880441167, 162.1527681330539679 ) ) ;
#29347 = CARTESIAN_POINT ( 'NONE',  ( 116.9748844278823015, -33.48813965163778050, 85.07848241876791917 ) ) ;
#29348 = CARTESIAN_POINT ( 'NONE',  ( 113.7785824165150643, -44.76317014998476651, 189.1299109901969757 ) ) ;
#29349 = CARTESIAN_POINT ( 'NONE',  ( 223.2659999999999911, 52.73749999999999716, -56.89600000000000080 ) ) ;
#29350 = ADVANCED_FACE ( 'NONE', ( #74367, #37618 ), #52097, .F. ) ;
#29351 = DIRECTION ( 'NONE',  ( 1.639958061481212836E-42, -4.100000000000000342E-29, -1.000000000000000000 ) ) ;
#29353 = DIRECTION ( 'NONE',  ( 0.000000000000000000, 0.000000000000000000, -1.000000000000000000 ) ) ;
#29352 = CARTESIAN_POINT ( 'NONE',  ( 33.78309357196401663, -29.99615139349950965, -5.074374724088000832 ) ) ;
#29354 = DIRECTION ( 'NONE',  ( 1.000000000000000000, 0.000000000000000000, 0.000000000000000000 ) ) ;
#29355 = CARTESIAN_POINT ( 'NONE',  ( 71.25580610988301089, -82.12815647064932989, 394.9756252759102040 ) ) ;
#29356 = ORIENTED_EDGE ( 'NONE', *, *, #13403, .T. ) ;
#29357 = FACE_OUTER_BOUND ( 'NONE', #62259, .T. ) ;
#29358 = ORIENTED_EDGE ( 'NONE', *, *, #48571, .F. ) ;
#29359 = ORIENTED_EDGE ( 'NONE', *, *, #2442, .T. ) ;
#29361 = ORIENTED_EDGE ( 'NONE', *, *, #50805, .F. ) ;
#29360 = CARTESIAN_POINT ( 'NONE',  ( 172.5664832912740110, -32.07844715994070839, 78.92562527591199739 ) ) ;
#29362 = CIRCLE ( 'NONE', #81631, 0.5000000000000004441 ) ;
#29363 = CARTESIAN_POINT ( 'NONE',  ( 96.67837842349544530, -37.29153504031420141, 72.36991099019596163 ) ) ;
#29364 = DIRECTION ( 'NONE',  ( 0.000000000000000000, 0.000000000000000000, -1.000000000000000000 ) ) ;
#29365 = B_SPLINE_CURVE_WITH_KNOTS ( 'NONE', 3,
 ( #82589, #20347, #48018, #13525, #34403, #46528 ),
 .UNSPECIFIED., .F., .F.,
 ( 4, 2, 4 ),
 ( 1.047024443964650053E-05, 0.008642110246132650442, 0.01810021157327289937 ),
 .UNSPECIFIED. ) ;
#29366 = DIRECTION ( 'NONE',  ( 1.000000000000000000, 0.000000000000000000, 0.000000000000000000 ) ) ;
#29367 = EDGE_CURVE ( 'NONE', #79206, #2874, #83018, .T. ) ;
#29368 = CARTESIAN_POINT ( 'NONE',  ( 98.22454660805831850, -42.33418938753942484, 182.7756252759109543 ) ) ;
#29369 = VECTOR ( 'NONE', #63875, 1000.000000000000000 ) ;
#29370 = CARTESIAN_POINT ( 'NONE',  ( 98.72788526414296939, -31.75567473670096774, 280.3209912566482558 ) ) ;
#29371 = ORIENTED_EDGE ( 'NONE', *, *, #39402, .F. ) ;
#29372 = ORIENTED_EDGE ( 'NONE', *, *, #61802, .T. ) ;
#29373 = ORIENTED_EDGE ( 'NONE', *, *, #79349, .F. ) ;
#29374 = VECTOR ( 'NONE', #17547, 1000.000000000000000 ) ;
#29375 = EDGE_CURVE ( 'NONE', #44052, #74767, #74110, .T. ) ;
#29376 = DIRECTION ( 'NONE',  ( -1.000000000000000000, -2.756263715554006823E-15, 0.000000000000000000 ) ) ;
#29377 = CARTESIAN_POINT ( 'NONE',  ( 179.1667039024439703, -26.71338133339251542, 342.9256252759109884 ) ) ;
#29378 = CARTESIAN_POINT ( 'NONE',  ( 113.2449868381543894, -28.75828141597592591, 160.5523427473990239 ) ) ;
#29379 = CARTESIAN_POINT ( 'NONE',  ( -487.2989999999999782, 86.51875000000001137, 86.36305401447658880 ) ) ;
#29380 = CARTESIAN_POINT ( 'NONE',  ( 88.25669247804529505, 93.94566094357735153, 96.20686424029969430 ) ) ;
#29381 = DIRECTION ( 'NONE',  ( -5.773159642023980606E-15, -5.773159642023980170E-30, -1.000000000000000000 ) ) ;
#29382 = DIRECTION ( 'NONE',  ( 0.000000000000000000, 0.000000000000000000, -1.000000000000000000 ) ) ;
#29383 = CARTESIAN_POINT ( 'NONE',  ( 72.06648329127402519, -45.72944715994106701, -4.824374724089063982 ) ) ;
#29384 = CARTESIAN_POINT ( 'NONE',  ( 97.09625384711483775, -33.75906160244644383, 31.09562527591097592 ) ) ;
#29385 = ORIENTED_EDGE ( 'NONE', *, *, #60273, .F. ) ;
#29386 = CYLINDRICAL_SURFACE ( 'NONE', #33020, 10.00000000000000888 ) ;
#29387 = CARTESIAN_POINT ( 'NONE',  ( -54.20184508647076171, 54.02065945192997987, 70.80016487573695372 ) ) ;
#29388 = CARTESIAN_POINT ( 'NONE',  ( 99.83919217201646745, -32.93524248800951426, 133.7595189410199623 ) ) ;
#29389 = VECTOR ( 'NONE', #4280, 1000.000000000000000 ) ;
#29390 = EDGE_CURVE ( 'NONE', #36063, #20396, #63940, .T. ) ;
#29391 = CARTESIAN_POINT ( 'NONE',  ( 97.33746229064173860, -34.07254350826487155, 96.11491520920078813 ) ) ;
#29392 = ADVANCED_FACE ( 'NONE', ( #24435 ), #87999, .F. ) ;
#29393 = AXIS2_PLACEMENT_3D ( 'NONE', #69208, #6980, #15143 ) ;
#29394 = DIRECTION ( 'NONE',  ( -1.000000000000000000, -5.512527431108013646E-15, 0.000000000000000000 ) ) ;
#29395 = VERTEX_POINT ( 'NONE', #51664 ) ;
#29396 = ORIENTED_EDGE ( 'NONE', *, *, #78215, .T. ) ;
#29397 = CARTESIAN_POINT ( 'NONE',  ( 27.27158787008325902, 127.0000000000000000, -5.920431057502157584E-15 ) ) ;
#29398 = EDGE_CURVE ( 'NONE', #55059, #65439, #11735, .T. ) ;
#29399 = EDGE_LOOP ( 'NONE', ( #20891, #23725, #25825, #27925, #71084 ) ) ;
#29400 = ORIENTED_EDGE ( 'NONE', *, *, #51140, .F. ) ;
#29401 = CARTESIAN_POINT ( 'NONE',  ( 116.0874278420761527, -39.35605806303598797, 135.0206309249449532 ) ) ;
#29402 = EDGE_CURVE ( 'NONE', #67223, #49327, #4404, .T. ) ;
#29403 = DIRECTION ( 'NONE',  ( 1.639958061481212836E-42, -4.100000000000000342E-29, -1.000000000000000000 ) ) ;
#29404 = CARTESIAN_POINT ( 'NONE',  ( 102.9625221110550513, -46.33646342331733337, 88.25562527591095829 ) ) ;
#29405 = CARTESIAN_POINT ( 'NONE',  ( 105.7149664547234806, -46.72378104326954684, 17.46898624714683024 ) ) ;
#29406 = ORIENTED_EDGE ( 'NONE', *, *, #26450, .F. ) ;
#29407 = EDGE_LOOP ( 'NONE', ( #64057, #60635, #73709, #69561, #66421, #39769 ) ) ;
#29408 = ORIENTED_EDGE ( 'NONE', *, *, #52115, .T. ) ;
#29409 = EDGE_CURVE ( 'NONE', #36232, #12855, #53435, .T. ) ;
#29411 = CARTESIAN_POINT ( 'NONE',  ( 96.05424466460999611, -37.92361698284899774, 81.40038718067299328 ) ) ;
#29410 = CIRCLE ( 'NONE', #45399, 2.749999999999974687 ) ;
#29412 = ORIENTED_EDGE ( 'NONE', *, *, #37503, .T. ) ;
#29413 = CARTESIAN_POINT ( 'NONE',  ( 114.5610390845466355, -30.44493693613343765, 269.3813395616256798 ) ) ;
#29414 = CARTESIAN_POINT ( 'NONE',  ( 116.3696522983621549, -44.11004992080503229, 194.2927681330539542 ) ) ;
#29415 = CARTESIAN_POINT ( 'NONE',  ( 21.56670390244604718, -23.42844715994195326, 180.4678068554150911 ) ) ;
#29416 = DIRECTION ( 'NONE',  ( 1.000000000000000000, 0.000000000000000000, 1.248844797103662002E-15 ) ) ;
#29417 = CARTESIAN_POINT ( 'NONE',  ( 113.9864041344766861, -28.11035927269328738, 115.5261014663869474 ) ) ;
#29418 = FACE_OUTER_BOUND ( 'NONE', #39414, .T. ) ;
#29419 = VERTEX_POINT ( 'NONE', #55236 ) ;
#29420 = CARTESIAN_POINT ( 'NONE',  ( 66.20668838251407351, -0.9299196430550271675, 542.9756252759101471 ) ) ;
#29421 = VERTEX_POINT ( 'NONE', #20745 ) ;
#29422 = DIRECTION ( 'NONE',  ( -1.000000000000000000, -3.555032108465730541E-16, 0.000000000000000000 ) ) ;
#29423 = ORIENTED_EDGE ( 'NONE', *, *, #28035, .T. ) ;
#29424 = VERTEX_POINT ( 'NONE', #41611 ) ;
#29425 = AXIS2_PLACEMENT_3D ( 'NONE', #16333, #37672, #71308 ) ;
#29426 = DIRECTION ( 'NONE',  ( -0.7071067811865614505, -0.7071067811865336949, 0.000000000000000000 ) ) ;
#29427 = CARTESIAN_POINT ( 'NONE',  ( 0.000000000000000000, 20.32000000000000028, 0.000000000000000000 ) ) ;
#29428 = CARTESIAN_POINT ( 'NONE',  ( 112.1813298990327183, -27.60452245592377807, 34.66991099019695355 ) ) ;
#29429 = DIRECTION ( 'NONE',  ( -0.7071067811855830110, -0.7071067811875120235, 0.000000000000000000 ) ) ;
#29430 = DIRECTION ( 'NONE',  ( 1.000000000000000000, 4.299999999999999979E-14, 1.000000000000000078E-15 ) ) ;
#29431 = CARTESIAN_POINT ( 'NONE',  ( 101.9936209501908309, -45.44607154402763172, 73.15645861009139139 ) ) ;
#29432 = CARTESIAN_POINT ( 'NONE',  ( 106.5519926023875712, -26.37212682281782250, 45.12800622829394115 ) ) ;
#29434 = CARTESIAN_POINT ( 'NONE',  ( 114.4473569665853603, -28.53271593493113301, 155.5051490854349652 ) ) ;
#29433 = DIRECTION ( 'NONE',  ( 0.000000000000000000, 0.000000000000000000, -1.000000000000000000 ) ) ;
#29435 = CARTESIAN_POINT ( 'NONE',  ( 115.0889047233127513, -30.61763667903340291, 70.34395860933346967 ) ) ;
#29436 = CARTESIAN_POINT ( 'NONE',  ( 107.0664832912730020, -36.72944715994189835, 361.9756252759079871 ) ) ;
#29437 = EDGE_LOOP ( 'NONE', ( #75649, #42301, #41755, #33537 ) ) ;
#29438 = CARTESIAN_POINT ( 'NONE',  ( 72.26949937496598864, -71.54137415153812185, 361.9756252759101471 ) ) ;
#29439 = DIRECTION ( 'NONE',  ( -3.100000000000000258E-29, 3.100000000000000044E-14, 1.000000000000000000 ) ) ;
#29440 = FACE_BOUND ( 'NONE', #43952, .T. ) ;
#29441 = ORIENTED_EDGE ( 'NONE', *, *, #64830, .F. ) ;
#29442 = CARTESIAN_POINT ( 'NONE',  ( 193.0374249753376432, -23.42844715993431848, 180.4678068554150343 ) ) ;
#29444 = VERTEX_POINT ( 'NONE', #33022 ) ;
#29443 = CARTESIAN_POINT ( 'NONE',  ( 114.9985205141181837, -29.89647917087096118, 184.3927681330539770 ) ) ;
#29445 = CARTESIAN_POINT ( 'NONE',  ( 51.56670390244699576, -19.82844715994031048, -5.074374724088000832 ) ) ;
#29446 = CARTESIAN_POINT ( 'NONE',  ( 103.8129894719335624, -48.15035030529833904, 213.3556252759109668 ) ) ;
#29447 = CARTESIAN_POINT ( 'NONE',  ( 117.3964687521579293, -38.63454956243933225, 84.68133956162593279 ) ) ;
#29448 = LINE ( 'NONE', #86203, #28738 ) ;
#29449 = EDGE_CURVE ( 'NONE', #68825, #60182, #81650, .T. ) ;
#29450 = CARTESIAN_POINT ( 'NONE',  ( 97.33765849503933509, -34.07180872970644003, 192.1146941698899582 ) ) ;
#29451 = CARTESIAN_POINT ( 'NONE',  ( 134.0664832912740110, 0.2215528400590013880, 306.1181252759120071 ) ) ;
#29452 = ORIENTED_EDGE ( 'NONE', *, *, #3086, .F. ) ;
#29453 = VECTOR ( 'NONE', #29204, 999.9999999999998863 ) ;
#29454 = AXIS2_PLACEMENT_3D ( 'NONE', #33762, #7400, #83712 ) ;
#29455 = EDGE_CURVE ( 'NONE', #30532, #70798, #88454, .T. ) ;
#29456 = ORIENTED_EDGE ( 'NONE', *, *, #82399, .F. ) ;
#29457 = EDGE_LOOP ( 'NONE', ( #74072, #3272, #17410, #8671, #51182 ) ) ;
#29458 = AXIS2_PLACEMENT_3D ( 'NONE', #41477, #55994, #43272 ) ;
#29459 = ORIENTED_EDGE ( 'NONE', *, *, #17987, .F. ) ;
#29460 = LINE ( 'NONE', #9026, #37994 ) ;
#29461 = CARTESIAN_POINT ( 'NONE',  ( 111.1274376763295635, -27.12782558180003889, 240.7584824187679544 ) ) ;
#29462 = CARTESIAN_POINT ( 'NONE',  ( 172.5664832912740110, 0.2215528400590013880, 136.8086252759119645 ) ) ;
#29463 = CARTESIAN_POINT ( 'NONE',  ( 136.5763721200466989, -17.60518726038198167, 2.783021291310912027 ) ) ;
#29465 = CARTESIAN_POINT ( 'NONE',  ( 156.5667039024483529, -48.82844715993569196, 290.7178068554149490 ) ) ;
#29464 = DIRECTION ( 'NONE',  ( 1.000000000000000078E-15, -1.000000000000000083E-30, -1.000000000000000000 ) ) ;
#29466 = DIRECTION ( 'NONE',  ( 0.9068632946707805287, -0.4214249218767882610, 8.630465054610985966E-16 ) ) ;
#29467 = CARTESIAN_POINT ( 'NONE',  ( 115.4624701790509391, -43.00605189524043936, 28.31562527591097123 ) ) ;
#29468 = VERTEX_POINT ( 'NONE', #61615 ) ;
#29469 = VERTEX_POINT ( 'NONE', #82101 ) ;
#29470 = VERTEX_POINT ( 'NONE', #68900 ) ;
#29471 = EDGE_CURVE ( 'NONE', #27150, #14550, #59561, .T. ) ;
#29472 = CARTESIAN_POINT ( 'NONE',  ( 51.03742451361310373, -23.42844715994068849, 193.9678068554150911 ) ) ;
#29473 = VECTOR ( 'NONE', #76818, 1000.000000000000000 ) ;
#29474 = CARTESIAN_POINT ( 'NONE',  ( 226.4410000000000025, 65.43750000000000000, 10.66800000000000104 ) ) ;
#29475 = CARTESIAN_POINT ( 'NONE',  ( 105.8561066403589308, -27.02385992090132305, 266.1756252759109884 ) ) ;
#29476 = DIRECTION ( 'NONE',  ( 4.299999999999999979E-14, -1.000000000000000000, 4.400000000000000367E-29 ) ) ;
#29477 = AXIS2_PLACEMENT_3D ( 'NONE', #14729, #190, #76044 ) ;
#29478 = CARTESIAN_POINT ( 'NONE',  ( 116.2961327041337825, -39.96626766897446714, 129.5584824187679658 ) ) ;
#29479 = CARTESIAN_POINT ( 'NONE',  ( 117.0720918726942301, -35.46411075774014421, 28.92716242642622504 ) ) ;
#29480 = VERTEX_POINT ( 'NONE', #19849 ) ;
#29481 = DIRECTION ( 'NONE',  ( -0.7071067811865473507, -0.7071067811865477948, 0.000000000000000000 ) ) ;
#29482 = CARTESIAN_POINT ( 'NONE',  ( 77.44501272126922231, -35.89730640218657243, 2.921034946746044803 ) ) ;
#29483 = ORIENTED_EDGE ( 'NONE', *, *, #50914, .F. ) ;
#29484 = ORIENTED_EDGE ( 'NONE', *, *, #46767, .T. ) ;
#29485 = CARTESIAN_POINT ( 'NONE',  ( -80.88915705228852460, 94.58006533271586136, 86.67541640318147245 ) ) ;
#29486 = CARTESIAN_POINT ( 'NONE',  ( 109.5858817268311611, -44.49374890974875285, 10.64523322673399619 ) ) ;
#29487 = VECTOR ( 'NONE', #27897, 1000.000000000000000 ) ;
#29488 = CARTESIAN_POINT ( 'NONE',  ( 51.06648329127400388, 19.62155284005901024, 339.0006252759110339 ) ) ;
#29489 = CARTESIAN_POINT ( 'NONE',  ( 115.0889047252626511, -30.61763668196338628, 84.34395860905816278 ) ) ;
#29490 = EDGE_CURVE ( 'NONE', #70034, #17117, #27112, .T. ) ;
#29491 = DIRECTION ( 'NONE',  ( 0.000000000000000000, 0.000000000000000000, -1.000000000000000000 ) ) ;
#29492 = ORIENTED_EDGE ( 'NONE', *, *, #26398, .F. ) ;
#29493 = DIRECTION ( 'NONE',  ( -1.000000000000000078E-15, 1.000000000000000083E-30, 1.000000000000000000 ) ) ;
#29494 = DIRECTION ( 'NONE',  ( 0.000000000000000000, 0.000000000000000000, -1.000000000000000000 ) ) ;
#29495 = EDGE_CURVE ( 'NONE', #28780, #18226, #12592, .T. ) ;
#29496 = ORIENTED_EDGE ( 'NONE', *, *, #67266, .T. ) ;
#29497 = CARTESIAN_POINT ( 'NONE',  ( 103.2788000081581288, -47.11369209158109328, 97.28610146638693834 ) ) ;
#29498 = ORIENTED_EDGE ( 'NONE', *, *, #79126, .T. ) ;
#29499 = EDGE_CURVE ( 'NONE', #2385, #57151, #85744, .T. ) ;
#29500 = CARTESIAN_POINT ( 'NONE',  ( 102.3843679657495329, -43.41581164733459985, 279.9080903695913776 ) ) ;
#29501 = CARTESIAN_POINT ( 'NONE',  ( 92.81932083335593120, -113.5527167097541934, -11.78219314458173272 ) ) ;
#29502 = CARTESIAN_POINT ( 'NONE',  ( 113.2095242374420252, -45.08419629851117350, 183.0689586092449588 ) ) ;
#29503 = CARTESIAN_POINT ( 'NONE',  ( -23.27731929905162289, 53.08310398829927834, 30.16249999999998721 ) ) ;
#29504 = EDGE_CURVE ( 'NONE', #71916, #17169, #3055, .T. ) ;
#29505 = DIRECTION ( 'NONE',  ( 0.000000000000000000, 0.000000000000000000, -1.000000000000000000 ) ) ;
#29506 = DIRECTION ( 'NONE',  ( 0.000000000000000000, 0.000000000000000000, 1.000000000000000000 ) ) ;
#29507 = CARTESIAN_POINT ( 'NONE',  ( 68.91678303834669350, -69.56165394957326953, 247.5002289977139753 ) ) ;
#29508 = CARTESIAN_POINT ( 'NONE',  ( 99.36487284946518628, -28.73678208742278173, 261.6746728949589169 ) ) ;
#29509 = CARTESIAN_POINT ( 'NONE',  ( 111.8140854152826336, -45.56118024207201955, 117.9710264827728707 ) ) ;
#29510 = ORIENTED_EDGE ( 'NONE', *, *, #32592, .F. ) ;
#29511 = AXIS2_PLACEMENT_3D ( 'NONE', #73891, #88878, #5759 ) ;
#29512 = DIRECTION ( 'NONE',  ( 0.000000000000000000, 1.000000000000000000, 0.000000000000000000 ) ) ;
#29513 = ORIENTED_EDGE ( 'NONE', *, *, #89818, .F. ) ;
#29514 = CARTESIAN_POINT ( 'NONE',  ( 116.8361817273313790, -32.96833395228159702, 135.1184824187679396 ) ) ;
#29515 = DIRECTION ( 'NONE',  ( 1.000000000000000078E-15, -1.000000000000000083E-30, -1.000000000000000000 ) ) ;
#29516 = VECTOR ( 'NONE', #71435, 999.9999999999998863 ) ;
#29517 = ORIENTED_EDGE ( 'NONE', *, *, #62372, .F. ) ;
#29518 = ORIENTED_EDGE ( 'NONE', *, *, #86112, .T. ) ;
#29519 = ORIENTED_EDGE ( 'NONE', *, *, #72322, .F. ) ;
#29520 = EDGE_CURVE ( 'NONE', #4943, #44354, #58598, .T. ) ;
#29521 = CARTESIAN_POINT ( 'NONE',  ( 116.7951252620880922, -39.38782982808247368, 123.6147919394983887 ) ) ;
#29522 = PLANE ( 'NONE',  #50654 ) ;
#29524 = ADVANCED_FACE ( 'NONE', ( #20310 ), #41169, .T. ) ;
#29523 = CARTESIAN_POINT ( 'NONE',  ( 83.06670390244796920, -58.72944715994098885, 231.5838068554150198 ) ) ;
#29525 = CARTESIAN_POINT ( 'NONE',  ( 143.1700167138480708, -139.0938916433959207, 247.5000110694289788 ) ) ;
#29526 = DIRECTION ( 'NONE',  ( 0.000000000000000000, 0.000000000000000000, 1.000000000000000000 ) ) ;
#29527 = CARTESIAN_POINT ( 'NONE',  ( 97.48672026426986292, -32.61689163886055809, 12.00419670448293985 ) ) ;
#29528 = CARTESIAN_POINT ( 'NONE',  ( 34.92499999999999716, 82.54999999999999716, 315.3410000000000082 ) ) ;
#29529 = EDGE_LOOP ( 'NONE', ( #42284, #55389 ) ) ;
#29530 = CARTESIAN_POINT ( 'NONE',  ( 6.123233995736773185E-16, 215.0000000000000000, 149.6557476874258441 ) ) ;
#29531 = EDGE_LOOP ( 'NONE', ( #87144, #3105, #32702, #36704 ) ) ;
#29532 = ORIENTED_EDGE ( 'NONE', *, *, #36985, .F. ) ;
#29533 = DIRECTION ( 'NONE',  ( -0.7071067811571960515, 0.7071067812158990940, 0.000000000000000000 ) ) ;
#29534 = VECTOR ( 'NONE', #55675, 1000.000000000000000 ) ;
#29535 = DIRECTION ( 'NONE',  ( 0.000000000000000000, -1.000000000000000000, 0.000000000000000000 ) ) ;
#29536 = DIRECTION ( 'NONE',  ( 0.000000000000000000, 1.000000000000000000, 0.000000000000000000 ) ) ;
#29537 = CARTESIAN_POINT ( 'NONE',  ( 107.0664832912739968, -18.82844715994099971, 168.9256252759119832 ) ) ;
#29538 = CARTESIAN_POINT ( 'NONE',  ( 63.03715912545730760, -24.42818131006017879, 300.4678068554150627 ) ) ;
#29539 = CARTESIAN_POINT ( 'NONE',  ( 111.4808447759429413, -44.07556959346039349, 237.4295626852199632 ) ) ;
#29541 = CARTESIAN_POINT ( 'NONE',  ( 115.7104945841387007, -43.58108136993639903, 44.30514908543492680 ) ) ;
#29540 = CARTESIAN_POINT ( 'NONE',  ( 131.0667039024480118, -61.87844715994100397, 231.5838068554150198 ) ) ;
#29542 = CARTESIAN_POINT ( 'NONE',  ( 123.0975592459876822, 73.27678779245984231, 43.49559623943592612 ) ) ;
#29543 = CARTESIAN_POINT ( 'NONE',  ( 97.50197496249766971, -32.47188371672483242, 100.9927681330539713 ) ) ;
#29544 = ORIENTED_EDGE ( 'NONE', *, *, #89065, .F. ) ;
#29545 = DIRECTION ( 'NONE',  ( -0.1811243269278930978, 0.9834602067165288952, 0.000000000000000000 ) ) ;
#29546 = VERTEX_POINT ( 'NONE', #89805 ) ;
#29547 = CARTESIAN_POINT ( 'NONE',  ( 98.34985888866438586, -31.65658484983705634, 66.90645861293477026 ) ) ;
#29548 = CARTESIAN_POINT ( 'NONE',  ( 141.0667039024479834, -58.72944715994110254, 198.9178068554149945 ) ) ;
#29549 = VERTEX_POINT ( 'NONE', #13045 ) ;
#29550 = CARTESIAN_POINT ( 'NONE',  ( 107.0664832912739968, -8.729447159940999512, 284.9256252759119548 ) ) ;
#29551 = ORIENTED_EDGE ( 'NONE', *, *, #65386, .F. ) ;
#29552 = CARTESIAN_POINT ( 'NONE',  ( 172.5667039024480118, -36.32844715993499563, 180.4678068554150059 ) ) ;
#29553 = CARTESIAN_POINT ( 'NONE',  ( 99.04424376774331051, -42.84153041693851804, 272.8435455337404960 ) ) ;
#29554 = ADVANCED_FACE ( 'NONE', ( #5781 ), #33472, .F. ) ;
#29555 = AXIS2_PLACEMENT_3D ( 'NONE', #6485, #21016, #33748 ) ;
#29556 = CARTESIAN_POINT ( 'NONE',  ( 107.0664832912739968, -8.350947159940998787, 335.9181252759120184 ) ) ;
#29557 = VERTEX_POINT ( 'NONE', #75268 ) ;
#29558 = CARTESIAN_POINT ( 'NONE',  ( 96.05424466460999611, -37.92361698284899774, 81.40038718067299328 ) ) ;
#29559 = PRESENTATION_STYLE_ASSIGNMENT (( #16828 ) ) ;
#29560 = EDGE_CURVE ( 'NONE', #24085, #85724, #87150, .T. ) ;
#29561 = DIRECTION ( 'NONE',  ( 0.000000000000000000, 1.000000000000000000, 0.000000000000000000 ) ) ;
#29562 = DIRECTION ( 'NONE',  ( -0.7071067811865517916, 0.000000000000000000, -0.7071067811865431318 ) ) ;
#29563 = ORIENTED_EDGE ( 'NONE', *, *, #80592, .F. ) ;
#29564 = DIRECTION ( 'NONE',  ( -1.000000000000000000, -4.299999999999999979E-14, -9.351236661543306751E-17 ) ) ;
#29565 = DIRECTION ( 'NONE',  ( 0.7071067811865475727, -0.7071067811865475727, 0.000000000000000000 ) ) ;
#29566 = DIRECTION ( 'NONE',  ( 4.194175870806139918E-14, -1.000000000000000000, 0.000000000000000000 ) ) ;
#29567 = CARTESIAN_POINT ( 'NONE',  ( 98.82287431334749783, -28.18163096472671469, 111.6870538473389587 ) ) ;
#29569 = DIRECTION ( 'NONE',  ( 4.194175870806139918E-14, -1.000000000000000000, 0.000000000000000000 ) ) ;
#29568 = CARTESIAN_POINT ( 'NONE',  ( 90.44969454456416713, -53.34645651782494724, 218.0711402470150801 ) ) ;
#29570 = DIRECTION ( 'NONE',  ( -1.000000000000000078E-15, 0.000000000000000000, 1.000000000000000000 ) ) ;
#29571 = VECTOR ( 'NONE', #80503, 1000.000000000000000 ) ;
#29572 = ORIENTED_EDGE ( 'NONE', *, *, #42504, .F. ) ;
#29573 = DIRECTION ( 'NONE',  ( 0.7071067811865449082, 0.7071067811865501263, 7.071067811865448709E-16 ) ) ;
#29574 = CARTESIAN_POINT ( 'NONE',  ( 116.2045471004837083, -43.06251688283437318, 159.3441967044819592 ) ) ;
#29576 = VERTEX_POINT ( 'NONE', #84359 ) ;
#29575 = DIRECTION ( 'NONE',  ( 0.000000000000000000, 0.000000000000000000, 1.000000000000000000 ) ) ;
#29577 = CARTESIAN_POINT ( 'NONE',  ( 101.9462946551393543, -46.59843102978671681, 13.19562527591094891 ) ) ;
#29578 = FACE_BOUND ( 'NONE', #26985, .T. ) ;
#29579 = CARTESIAN_POINT ( 'NONE',  ( 241.3336515812914911, 40.03750000000000142, -2.032000000000000028 ) ) ;
#29580 = CARTESIAN_POINT ( 'NONE',  ( 124.6905118036815310, -83.08196156581362857, 250.2178068554180470 ) ) ;
#29581 = DIRECTION ( 'NONE',  ( 0.000000000000000000, 0.000000000000000000, 1.000000000000000000 ) ) ;
#29582 = EDGE_CURVE ( 'NONE', #42178, #4517, #76171, .T. ) ;
#29583 = CARTESIAN_POINT ( 'NONE',  ( 67.65734841870819594, 95.25000000000000000, 346.9005000000000223 ) ) ;
#29584 = CARTESIAN_POINT ( 'NONE',  ( 117.3624379696767335, -35.49166588079122420, 238.9337205140069500 ) ) ;
#29585 = ORIENTED_EDGE ( 'NONE', *, *, #43798, .T. ) ;
#29586 = VERTEX_POINT ( 'NONE', #48433 ) ;
#29587 = CARTESIAN_POINT ( 'NONE',  ( 116.1701677112242237, -32.41741342456931818, 210.6101547344689777 ) ) ;
#29588 = AXIS2_PLACEMENT_3D ( 'NONE', #1796, #43097, #43993 ) ;
#29589 = CARTESIAN_POINT ( 'NONE',  ( 72.25757238336808541, -1.944390235229867425, 361.9756252759101471 ) ) ;
#29590 = CARTESIAN_POINT ( 'NONE',  ( 115.5880482615279163, -32.77224410791782816, 55.59205949637296840 ) ) ;
#29591 = CONICAL_SURFACE ( 'NONE', #62978, 1.625000000000001332, 1.029744258676650093 ) ;
#29592 = CARTESIAN_POINT ( 'NONE',  ( 23.07567186625316680, 87.18950910861248360, 301.8082642732044292 ) ) ;
#29593 = ADVANCED_FACE ( 'NONE', ( #34834 ), #15307, .F. ) ;
#29594 = CIRCLE ( 'NONE', #32490, 3.250000000000002665 ) ;
#29595 = CARTESIAN_POINT ( 'NONE',  ( 107.0664832912739541, -36.72944715994095333, 305.0306255462182321 ) ) ;
#29596 = CARTESIAN_POINT ( 'NONE',  ( 192.5667039024475002, -23.42844715993433624, 129.9678068554150343 ) ) ;
#29597 = VECTOR ( 'NONE', #50242, 1000.000000000000000 ) ;
#29598 = VERTEX_POINT ( 'NONE', #28463 ) ;
#29599 = DIRECTION ( 'NONE',  ( 0.000000000000000000, -1.000000000000000000, 0.000000000000000000 ) ) ;
#29600 = CYLINDRICAL_SURFACE ( 'NONE', #64797, 0.5000000000000031086 ) ;
#29601 = CARTESIAN_POINT ( 'NONE',  ( 104.3301552612371381, -26.04411461992200927, 245.2880062282919482 ) ) ;
#29602 = DIRECTION ( 'NONE',  ( -0.000000000000000000, 1.000000000000000000, 0.000000000000000000 ) ) ;
#29603 = ORIENTED_EDGE ( 'NONE', *, *, #64146, .F. ) ;
#29605 = VERTEX_POINT ( 'NONE', #13947 ) ;
#29604 = EDGE_CURVE ( 'NONE', #46083, #58766, #317, .T. ) ;
#29606 = CARTESIAN_POINT ( 'NONE',  ( 108.3334480785710383, -46.73485935620319509, 87.67729194127437609 ) ) ;
#29607 = CARTESIAN_POINT ( 'NONE',  ( -84.99816483510880971, 95.16897323824362331, -82.65294504194714875 ) ) ;
#29608 = CARTESIAN_POINT ( 'NONE',  ( 100.8873238325640784, -44.70013431002061566, 123.0511152429078123 ) ) ;
#29609 = CARTESIAN_POINT ( 'NONE',  ( 145.2166182285888851, -69.56242951228074389, 247.5001056298889921 ) ) ;
#29610 = CARTESIAN_POINT ( 'NONE',  ( 100.9534786964906345, -28.35269599622561643, 26.56610146638693948 ) ) ;
#29611 = LINE ( 'NONE', #15996, #87680 ) ;
#29612 = EDGE_LOOP ( 'NONE', ( #36216, #7512, #83812, #335 ) ) ;
#29613 = CARTESIAN_POINT ( 'NONE',  ( 106.9267702420067678, -26.22618599733332090, 56.08705384733997334 ) ) ;
#29614 = CARTESIAN_POINT ( 'NONE',  ( 53.97500000000000142, 69.84999999999999432, 283.4005000000000223 ) ) ;
#29615 = CARTESIAN_POINT ( 'NONE',  ( 105.1595199372206793, -47.03071207059073799, 12.42991099019596923 ) ) ;
#29616 = VERTEX_POINT ( 'NONE', #56153 ) ;
#29617 = EDGE_CURVE ( 'NONE', #30791, #57079, #71212, .T. ) ;
#29618 = DIRECTION ( 'NONE',  ( 0.7071067810573865575, 0.7071067813157084769, 7.071067810573858582E-16 ) ) ;
#29620 = ADVANCED_FACE ( 'NONE', ( #41188 ), #42085, .F. ) ;
#29619 = PLANE ( 'NONE',  #738 ) ;
#29621 = CARTESIAN_POINT ( 'NONE',  ( 48.45959712127301344, -26.00627455219131789, -5.074374724088000832 ) ) ;
#29622 = EDGE_CURVE ( 'NONE', #40569, #53148, #42529, .T. ) ;
#29623 = CARTESIAN_POINT ( 'NONE',  ( 101.7674321979440606, -44.34626990135510738, 84.91094751244793315 ) ) ;
#29624 = CARTESIAN_POINT ( 'NONE',  ( 97.38187162881654046, -40.64678755884852279, 202.6327681330539860 ) ) ;
#29625 = CARTESIAN_POINT ( 'NONE',  ( 179.1667039024474377, -28.27351298636771659, 313.9678068554149490 ) ) ;
#29626 = EDGE_LOOP ( 'NONE', ( #66803, #12552, #66185, #15590 ) ) ;
#29627 = CARTESIAN_POINT ( 'NONE',  ( 51.06670390244799762, -33.35206098992630075, -5.074374724088000832 ) ) ;
#29628 = ORIENTED_EDGE ( 'NONE', *, *, #43515, .F. ) ;
#29629 = VERTEX_POINT ( 'NONE', #41631 ) ;
#29630 = AXIS2_PLACEMENT_3D ( 'NONE', #22764, #30014, #78183 ) ;
#29631 = FACE_OUTER_BOUND ( 'NONE', #12234, .T. ) ;
#29632 = ORIENTED_EDGE ( 'NONE', *, *, #79860, .F. ) ;
#29633 = ORIENTED_EDGE ( 'NONE', *, *, #55194, .T. ) ;
#29634 = FACE_OUTER_BOUND ( 'NONE', #41993, .T. ) ;
#29635 = CIRCLE ( 'NONE', #61520, 20.00000000000000355 ) ;
#29636 = CARTESIAN_POINT ( 'NONE',  ( 97.79819947057245599, -40.48432372764506226, 42.63278048571394407 ) ) ;
#29637 = CARTESIAN_POINT ( 'NONE',  ( 115.7815527111783069, -39.19119195442627301, 143.0419436376009799 ) ) ;
#29638 = CARTESIAN_POINT ( 'NONE',  ( 96.74139913992713957, -35.13602278645100796, 266.2041967044820581 ) ) ;
#29639 = B_SPLINE_CURVE_WITH_KNOTS ( 'NONE', 3,
 ( #53152, #12308, #60896, #24596, #32284, #31394, #38221, #45901, #88181, #4146, #40001, #59091, #74081, #59982, #67259, #73632, #38659, #65914 ),
 .UNSPECIFIED., .F., .F.,
 ( 4, 2, 2, 2, 2, 2, 2, 2, 4 ),
 ( 0.5000457028255199665, 0.5625399899723300123, 0.6250342771191399471, 0.6875285642659499930, 0.7500228514127600388, 0.8125171385595699736, 0.8750114257063800194, 0.9375057128531900652, 1.000000000000000000 ),
 .UNSPECIFIED. ) ;
#29640 = CARTESIAN_POINT ( 'NONE',  ( -11.00676631360785862, 76.20068480870281746, 130.0913480697105342 ) ) ;
#29641 = EDGE_LOOP ( 'NONE', ( #68639, #48409 ) ) ;
#29642 = EDGE_LOOP ( 'NONE', ( #59907, #2497, #16997, #24530 ) ) ;
#29643 = FACE_OUTER_BOUND ( 'NONE', #85193, .T. ) ;
#29644 = CARTESIAN_POINT ( 'NONE',  ( 172.5664832912729878, -27.57844715994070484, 18.92562527591200094 ) ) ;
#29645 = CARTESIAN_POINT ( 'NONE',  ( 70.27560645192561140, -140.3532164138353551, 246.6574697873465993 ) ) ;
#29646 = CARTESIAN_POINT ( 'NONE',  ( 116.5734795788845020, -32.34496456428597355, 104.1699109901969535 ) ) ;
#29647 = FACE_OUTER_BOUND ( 'NONE', #69260, .T. ) ;
#29648 = ORIENTED_EDGE ( 'NONE', *, *, #44685, .F. ) ;
#29649 = UNCERTAINTY_MEASURE_WITH_UNIT (LENGTH_MEASURE( 1.000000000000000082E-05 ), #8131, 'distance_accuracy_value', 'NONE');
#29650 = CARTESIAN_POINT ( 'NONE',  ( 105.6320445689042486, -47.05559920284586184, 257.4670538473393435 ) ) ;
#29651 = AXIS2_PLACEMENT_3D ( 'NONE', #55452, #20961, #76376 ) ;
#29652 = DIRECTION ( 'NONE',  ( 1.000000000000000000, 4.299999999999999979E-14, 1.000000000000000078E-15 ) ) ;
#29653 = VECTOR ( 'NONE', #37181, 1000.000000000000000 ) ;
#29654 = CARTESIAN_POINT ( 'NONE',  ( 0.000000000000000000, 0.000000000000000000, 0.000000000000000000 ) ) ;
#29656 = CARTESIAN_POINT ( 'NONE',  ( 11.73526988453661346, 77.69473719258546396, 130.0275070810828311 ) ) ;
#29655 = AXIS2_PLACEMENT_3D ( 'NONE', #62488, #48838, #27965 ) ;
#29657 = CARTESIAN_POINT ( 'NONE',  ( 172.5664832912728457, -18.82844715994071194, 201.9256252759118979 ) ) ;
#29659 = CARTESIAN_POINT ( 'NONE',  ( 46.03715912545427358, -48.62818131006086020, 300.4678068554150059 ) ) ;
#29658 = CARTESIAN_POINT ( 'NONE',  ( 50.03799999999999670, 0.000000000000000000, 206.3750000000000000 ) ) ;
#29660 = CARTESIAN_POINT ( 'NONE',  ( 255.9983484187079910, 40.03750000000000142, 10.66800000000000104 ) ) ;
#29661 = DIRECTION ( 'NONE',  ( 0.000000000000000000, 0.000000000000000000, 1.000000000000000000 ) ) ;
#29662 = CYLINDRICAL_SURFACE ( 'NONE', #55667, 2.750000000000002665 ) ;
#29663 = VECTOR ( 'NONE', #51092, 1000.000000000000000 ) ;
#29664 = DIRECTION ( 'NONE',  ( 0.4078776986755216494, 0.000000000000000000, -0.9130365726098601531 ) ) ;
#29665 = CARTESIAN_POINT ( 'NONE',  ( 107.0667039024467329, -19.36444715994092292, 196.2188068554170002 ) ) ;
#29666 = DIRECTION ( 'NONE',  ( 1.000000000000000000, 6.508581945447490214E-14, 1.000000000000000078E-15 ) ) ;
#29668 = VERTEX_POINT ( 'NONE', #68915 ) ;
#29667 = DIRECTION ( 'NONE',  ( 0.000000000000000000, 0.000000000000000000, -1.000000000000000000 ) ) ;
#29669 = DIRECTION ( 'NONE',  ( 1.000000000000000000, 0.000000000000000000, 0.000000000000000000 ) ) ;
#29670 = CARTESIAN_POINT ( 'NONE',  ( 111.7490138926534797, -27.39026733005105640, 279.7070538473396937 ) ) ;
#29671 = CARTESIAN_POINT ( 'NONE',  ( 108.3661019610163123, -47.70601195518164417, 158.6822919425779617 ) ) ;
#29672 = CARTESIAN_POINT ( 'NONE',  ( 112.3603056216204550, -28.17164194844215430, 285.6356252759109680 ) ) ;
#29674 = DIRECTION ( 'NONE',  ( -1.000000000000000000, 0.000000000000000000, 0.000000000000000000 ) ) ;
#29673 = DIRECTION ( 'NONE',  ( 3.100000000000000258E-29, -3.100000000000000044E-14, -1.000000000000000000 ) ) ;
#29675 = CARTESIAN_POINT ( 'NONE',  ( 116.8171253540862722, -34.15292439824600024, 140.0314580866620418 ) ) ;
#29676 = EDGE_CURVE ( 'NONE', #11556, #79496, #55216, .T. ) ;
#29677 = ORIENTED_EDGE ( 'NONE', *, *, #10608, .T. ) ;
#29678 = EDGE_CURVE ( 'NONE', #39780, #5447, #66841, .T. ) ;
#29679 = CYLINDRICAL_SURFACE ( 'NONE', #81017, 9.999999999999998224 ) ;
#29680 = ORIENTED_EDGE ( 'NONE', *, *, #3979, .F. ) ;
#29681 = CARTESIAN_POINT ( 'NONE',  ( 96.76615086495803553, -37.93025403122315709, 82.43086337114895912 ) ) ;
#29682 = EDGE_CURVE ( 'NONE', #5757, #24119, #37873, .T. ) ;
#29684 = ORIENTED_EDGE ( 'NONE', *, *, #27932, .T. ) ;
#29683 = CARTESIAN_POINT ( 'NONE',  ( 4.811414547114572393, 94.30331772199949114, 130.4673117074386823 ) ) ;
#29685 = LINE ( 'NONE', #10136, #21424 ) ;
#29686 = CARTESIAN_POINT ( 'NONE',  ( 117.3910620576582318, -35.19077923515893502, 214.9441967044829767 ) ) ;
#29687 = CARTESIAN_POINT ( 'NONE',  ( 182.6664832912729821, 12.92155284005730387, 358.9756252759109998 ) ) ;
#29688 = CARTESIAN_POINT ( 'NONE',  ( 110.8542634740689294, -45.98432270134635047, 147.8856073499956096 ) ) ;
#29689 = CARTESIAN_POINT ( 'NONE',  ( 97.31582641009998724, -39.30593163064425966, 151.5319995835646694 ) ) ;
#29690 = LINE ( 'NONE', #85128, #10782 ) ;
#29691 = EDGE_CURVE ( 'NONE', #3973, #68199, #10309, .T. ) ;
#29692 = EDGE_CURVE ( 'NONE', #45031, #12282, #14862, .T. ) ;
#29693 = FACE_BOUND ( 'NONE', #86224, .T. ) ;
#29694 = CARTESIAN_POINT ( 'NONE',  ( 98.38046330306050891, -41.69534231700428251, 96.73979469042932067 ) ) ;
#29695 = CARTESIAN_POINT ( 'NONE',  ( 116.5944731948638804, -42.45914096480947819, 128.3956252759109873 ) ) ;
#29696 = ORIENTED_EDGE ( 'NONE', *, *, #3850, .T. ) ;
#29697 = VERTEX_POINT ( 'NONE', #56615 ) ;
#29698 = EDGE_CURVE ( 'NONE', #36849, #53830, #49797, .T. ) ;
#29699 =( GEOMETRIC_REPRESENTATION_CONTEXT ( 3 ) GLOBAL_UNCERTAINTY_ASSIGNED_CONTEXT ( ( #81741 ) ) GLOBAL_UNIT_ASSIGNED_CONTEXT ( ( #80927, #68179, #74087 ) ) REPRESENTATION_CONTEXT ( 'NONE', 'WORKASPACE' ) );
#29700 = CARTESIAN_POINT ( 'NONE',  ( 107.2828545668587878, -27.33638008851531609, 71.47777378208797927 ) ) ;
#29701 = ADVANCED_FACE ( 'NONE', ( #69815 ), #77525, .T. ) ;
#29702 = CARTESIAN_POINT ( 'NONE',  ( 83.56670390244799762, -36.72944715994108122, 229.5838068554169524 ) ) ;
#29704 = CARTESIAN_POINT ( 'NONE',  ( 108.3334481699632192, -46.73485934377682582, 37.67729194854296537 ) ) ;
#29703 = CARTESIAN_POINT ( 'NONE',  ( 115.3120223323505940, -44.18753462406601074, 229.2413395616249545 ) ) ;
#29705 = AXIS2_PLACEMENT_3D ( 'NONE', #37598, #16262, #30337 ) ;
#29706 = CARTESIAN_POINT ( 'NONE',  ( 104.4905885192464865, -26.97863551867121146, 55.28004222319953698 ) ) ;
#29707 = EDGE_CURVE ( 'NONE', #23818, #77101, #35002, .T. ) ;
#29708 = CARTESIAN_POINT ( 'NONE',  ( 134.0664832912740110, -46.72944715994100306, 4.925625275910997303 ) ) ;
#29709 = CARTESIAN_POINT ( 'NONE',  ( 168.0371591254545365, -48.62818131005519007, 193.9678068554149775 ) ) ;
#29710 = LINE ( 'NONE', #22910, #69566 ) ;
#29711 = DIRECTION ( 'NONE',  ( 8.659560562355118980E-17, -0.7071067811865321406, 0.7071067811865628938 ) ) ;
#29712 = EDGE_CURVE ( 'NONE', #7158, #52534, #13234, .T. ) ;
#29713 = CARTESIAN_POINT ( 'NONE',  ( 108.6454077996538530, -25.81962716842089378, 149.9737205140059473 ) ) ;
#29714 = VERTEX_POINT ( 'NONE', #83007 ) ;
#29715 = ORIENTED_EDGE ( 'NONE', *, *, #3042, .T. ) ;
#29717 = EDGE_LOOP ( 'NONE', ( #75609, #80454, #28229, #42783 ) ) ;
#29716 = ADVANCED_FACE ( 'NONE', ( #20762 ), #763, .F. ) ;
#29718 = FACE_BOUND ( 'NONE', #42206, .T. ) ;
#29719 = CARTESIAN_POINT ( 'NONE',  ( 145.6103092929421337, -69.25820179750351713, 247.4237039382404930 ) ) ;
#29720 = CARTESIAN_POINT ( 'NONE',  ( 104.4885766460745486, -26.97918181991462916, 130.2815734883101868 ) ) ;
#29721 = CARTESIAN_POINT ( 'NONE',  ( 105.7149892088140319, -46.72379639561137310, 103.4689199191626869 ) ) ;
#29722 = CARTESIAN_POINT ( 'NONE',  ( 109.9085748933103162, -45.56225229135190347, 205.6423760838769681 ) ) ;
#29723 = B_SPLINE_CURVE_WITH_KNOTS ( 'NONE', 3,
 ( #32013, #79307, #31123, #71595, #23454, #17065, #78862, #45620, #72033, #9803, #9356, #73354, #37513, #65212, #37063, #51993, #86560, #64767, #2988, #72478, #24325, #38832, #37948, #79752, #2552 ),
 .UNSPECIFIED., .F., .F.,
 ( 4, 2, 2, 1, 2, 2, 2, 2, 2, 2, 2, 2, 4 ),
 ( 0.03972946622853321813, 0.04221318292723494348, 0.04345504127658580962, 0.04469689962593667576, 0.04593875797528754190, 0.04718061632463840110, 0.04966433302334011257, 0.05090619137269095096, 0.05214804972204178934, 0.05463176642074347306, 0.05587362477009431838, 0.05711548311944515677, 0.05959919981814688211 ),
 .UNSPECIFIED. ) ;
#29724 = CIRCLE ( 'NONE', #9421, 12.99999999999999822 ) ;
#29725 = VECTOR ( 'NONE', #60834, 999.9999999999998863 ) ;
#29726 = PLANE ( 'NONE',  #34924 ) ;
#29727 = AXIS2_PLACEMENT_3D ( 'NONE', #25666, #12949, #53342 ) ;
#29728 = AXIS2_PLACEMENT_3D ( 'NONE', #52258, #12762, #26378 ) ;
#29729 = CARTESIAN_POINT ( 'NONE',  ( 117.5811103608870383, -33.32038496654947579, 134.0880062282919880 ) ) ;
#29730 = DIRECTION ( 'NONE',  ( 1.000000000000000000, 0.000000000000000000, 0.000000000000000000 ) ) ;
#29731 = ORIENTED_EDGE ( 'NONE', *, *, #37538, .F. ) ;
#29733 = VERTEX_POINT ( 'NONE', #9825 ) ;
#29732 = ORIENTED_EDGE ( 'NONE', *, *, #46010, .T. ) ;
#29734 = AXIS2_PLACEMENT_3D ( 'NONE', #25520, #46390, #32321 ) ;
#29735 = EDGE_CURVE ( 'NONE', #59978, #27885, #45107, .T. ) ;
#29736 = CIRCLE ( 'NONE', #71754, 7.199999999999998401 ) ;
#29737 = LINE ( 'NONE', #70166, #28821 ) ;
#29738 = ORIENTED_EDGE ( 'NONE', *, *, #42937, .T. ) ;
#29739 = ORIENTED_EDGE ( 'NONE', *, *, #53872, .F. ) ;
#29741 = EDGE_CURVE ( 'NONE', #73485, #84299, #58841, .T. ) ;
#29740 = LINE ( 'NONE', #57879, #69588 ) ;
#29742 = CARTESIAN_POINT ( 'NONE',  ( 131.5325842222575261, -35.66080143920349599, 7.039723185229046720 ) ) ;
#29743 = EDGE_CURVE ( 'NONE', #18491, #85626, #84804, .T. ) ;
#29744 = CARTESIAN_POINT ( 'NONE',  ( 102.0014872285204035, -30.29305903553749602, 13.42523322673394581 ) ) ;
#29745 = FACE_BOUND ( 'NONE', #66684, .T. ) ;
#29746 = ORIENTED_EDGE ( 'NONE', *, *, #56713, .T. ) ;
#29747 = EDGE_CURVE ( 'NONE', #35180, #58643, #24992, .T. ) ;
#29748 = CARTESIAN_POINT ( 'NONE',  ( 113.0350491764517216, -43.12594021296303737, 9.635625275910943088 ) ) ;
#29749 = CARTESIAN_POINT ( 'NONE',  ( -126.8151218862759180, 59.90404055707092823, 31.02911582310609973 ) ) ;
#29750 = ORIENTED_EDGE ( 'NONE', *, *, #84160, .T. ) ;
#29751 = ORIENTED_EDGE ( 'NONE', *, *, #77000, .F. ) ;
#29752 = CARTESIAN_POINT ( 'NONE',  ( 110.8557683604797290, -45.98370673585618817, 112.8857367299098229 ) ) ;
#29753 = ORIENTED_EDGE ( 'NONE', *, *, #26915, .T. ) ;
#29754 = ORIENTED_EDGE ( 'NONE', *, *, #31874, .F. ) ;
#29755 = AXIS2_PLACEMENT_3D ( 'NONE', #55988, #71006, #21053 ) ;
#29756 = CARTESIAN_POINT ( 'NONE',  ( 101.6136182267745056, -30.15507309768812050, 40.04956268521897300 ) ) ;
#29757 = CARTESIAN_POINT ( 'NONE',  ( 103.8004457107024194, -26.80577029241926112, 165.3299109901969643 ) ) ;
#29758 = CARTESIAN_POINT ( 'NONE',  ( 108.2741602056595411, -26.36093993100598354, 129.9841967044819739 ) ) ;
#29759 = DIRECTION ( 'NONE',  ( -1.000000000000000000, -4.299999999999999979E-14, -1.000000000000000078E-15 ) ) ;
#29760 = CARTESIAN_POINT ( 'NONE',  ( 96.68218458626328982, -35.80812861978466799, 227.2556252759109725 ) ) ;
#29761 = CARTESIAN_POINT ( 'NONE',  ( 113.1784580317933120, -44.75174589757562416, 99.09546334846962168 ) ) ;
#29762 = CARTESIAN_POINT ( 'NONE',  ( 100.9537377020563582, -28.70775746239330317, 126.5940524488469379 ) ) ;
#29763 = ORIENTED_EDGE ( 'NONE', *, *, #39298, .F. ) ;
#29764 = CARTESIAN_POINT ( 'NONE',  ( 31.75000000000000000, 124.5870000000000033, -3.174999999999999822 ) ) ;
#29765 = ORIENTED_EDGE ( 'NONE', *, *, #11536, .F. ) ;
#29766 = ORIENTED_EDGE ( 'NONE', *, *, #28589, .F. ) ;
#29767 = VECTOR ( 'NONE', #56548, 1000.000000000000000 ) ;
#29768 = CARTESIAN_POINT ( 'NONE',  ( 102.6649408499558689, -27.23033719207987602, 180.4213395616249898 ) ) ;
#29769 = ORIENTED_EDGE ( 'NONE', *, *, #12511, .F. ) ;
#29770 = CARTESIAN_POINT ( 'NONE',  ( 103.0496837167155491, -26.43166057102584077, 170.3603871806729444 ) ) ;
#29771 = DIRECTION ( 'NONE',  ( 1.000000000000000000, 4.299999999999999979E-14, 1.000000000000000078E-15 ) ) ;
#29772 = VECTOR ( 'NONE', #81632, 1000.000000000000114 ) ;
#29773 = CARTESIAN_POINT ( 'NONE',  ( 136.1807380203761682, -34.97076862298531097, 7.459445689450600270 ) ) ;
#29774 = PLANE ( 'NONE',  #49999 ) ;
#29777 = CARTESIAN_POINT ( 'NONE',  ( 112.4005920293389948, -46.38403708128146974, 248.9661014663869878 ) ) ;
#29776 = CARTESIAN_POINT ( 'NONE',  ( 97.90460831411941456, -40.73749365022396063, 56.65424410226409435 ) ) ;
#29775 = DIRECTION ( 'NONE',  ( 0.000000000000000000, 0.000000000000000000, 1.000000000000000000 ) ) ;
#29778 = DIRECTION ( 'NONE',  ( -1.000000000000000000, -2.999999999999999839E-15, -1.000000000000000078E-15 ) ) ;
#29779 = DIRECTION ( 'NONE',  ( 1.000000000000000000, -0.000000000000000000, 0.000000000000000000 ) ) ;
#29780 = DIRECTION ( 'NONE',  ( -1.000000000000000000, 0.000000000000000000, 0.000000000000000000 ) ) ;
#29781 = DIRECTION ( 'NONE',  ( -1.000000000000000000, 0.000000000000000000, 0.000000000000000000 ) ) ;
#29782 = CARTESIAN_POINT ( 'NONE',  ( 3.968750000000000000, 120.6499999999999915, -105.4788588808464027 ) ) ;
#29783 = FACE_OUTER_BOUND ( 'NONE', #3258, .T. ) ;
#29785 = ORIENTED_EDGE ( 'NONE', *, *, #45748, .T. ) ;
#29784 = CARTESIAN_POINT ( 'NONE',  ( 99.99848706593783731, -40.87057048248247071, 195.5838068554172651 ) ) ;
#29786 = DIRECTION ( 'NONE',  ( 0.000000000000000000, 0.000000000000000000, -1.000000000000000000 ) ) ;
#29787 = CARTESIAN_POINT ( 'NONE',  ( 99.40582560697848180, -27.65448416857716651, 150.6356252759109680 ) ) ;
#29788 = CARTESIAN_POINT ( 'NONE',  ( 97.62238793418175931, -32.23162594710754547, 71.97276813305397525 ) ) ;
#29789 = CARTESIAN_POINT ( 'NONE',  ( 109.6164515631795524, -26.53946793531281756, 195.8813395616249977 ) ) ;
#29790 = DIRECTION ( 'NONE',  ( -0.7071067812158990940, -0.7071067811571960515, 0.000000000000000000 ) ) ;
#29791 = LINE ( 'NONE', #77950, #2545 ) ;
#29793 = CARTESIAN_POINT ( 'NONE',  ( 7.661254700127833495, 82.54999999999999716, 317.6630000000000109 ) ) ;
#29792 = CARTESIAN_POINT ( 'NONE',  ( -147.4575741623271767, 101.5999999999999943, -135.2444258376735888 ) ) ;
#29794 = DIRECTION ( 'NONE',  ( 0.000000000000000000, 0.000000000000000000, 1.000000000000000000 ) ) ;
#29795 = CARTESIAN_POINT ( 'NONE',  ( -74.15067561874319324, 120.6499999999999915, 68.53801554307369770 ) ) ;
#29796 = ORIENTED_EDGE ( 'NONE', *, *, #30022, .T. ) ;
#29797 = CARTESIAN_POINT ( 'NONE',  ( -72.96458098368751166, 127.0000000000000000, 65.82083098368619289 ) ) ;
#29798 = VECTOR ( 'NONE', #44305, 1000.000000000000000 ) ;
#29799 = AXIS2_PLACEMENT_3D ( 'NONE', #75500, #55013, #68238 ) ;
#29800 = CIRCLE ( 'NONE', #76201, 2.517500000000000071 ) ;
#29801 = VECTOR ( 'NONE', #63593, 1000.000000000000000 ) ;
#29802 = EDGE_CURVE ( 'NONE', #8874, #5965, #57514, .T. ) ;
#29803 = EDGE_LOOP ( 'NONE', ( #10540, #30921, #68167, #65329, #15218 ) ) ;
#29804 = ADVANCED_FACE ( 'NONE', ( #44320 ), #86132, .T. ) ;
#29805 = EDGE_LOOP ( 'NONE', ( #84764, #42024, #17612, #34619 ) ) ;
#29806 = VECTOR ( 'NONE', #68656, 999.9999999999998863 ) ;
#29807 = EDGE_CURVE ( 'NONE', #87649, #56977, #65664, .T. ) ;
#29809 = VERTEX_POINT ( 'NONE', #64346 ) ;
#29808 = DIRECTION ( 'NONE',  ( -2.999999999999999839E-15, 1.000000000000000000, -2.999999999999999900E-30 ) ) ;
#29810 = CARTESIAN_POINT ( 'NONE',  ( 107.9437834512411314, -25.73425880284256095, 111.0251490854349754 ) ) ;
#29811 = DIRECTION ( 'NONE',  ( -2.999999999999999839E-15, 1.000000000000000000, -2.999999999999999900E-30 ) ) ;
#29812 = AXIS2_PLACEMENT_3D ( 'NONE', #42463, #23845, #79708 ) ;
#29813 = DIRECTION ( 'NONE',  ( 0.000000000000000000, 1.000000000000000000, 0.000000000000000000 ) ) ;
#29814 = EDGE_CURVE ( 'NONE', #53126, #33347, #2119, .T. ) ;
#29815 = DIRECTION ( 'NONE',  ( 0.000000000000000000, -1.000000000000000000, 0.000000000000000000 ) ) ;
#29816 = CARTESIAN_POINT ( 'NONE',  ( 97.69287098190314111, -33.93680905855605801, 31.09562527591097592 ) ) ;
#29817 = ORIENTED_EDGE ( 'NONE', *, *, #15423, .T. ) ;
#29818 = ORIENTED_EDGE ( 'NONE', *, *, #39206, .T. ) ;
#29819 = ORIENTED_EDGE ( 'NONE', *, *, #85526, .T. ) ;
#29820 = EDGE_CURVE ( 'NONE', #59781, #35831, #44431, .T. ) ;
#29821 = DIRECTION ( 'NONE',  ( 0.000000000000000000, 0.000000000000000000, 1.000000000000000000 ) ) ;
#29822 = DIRECTION ( 'NONE',  ( 0.7071067811578790607, 0.7071067812152160847, 0.000000000000000000 ) ) ;
#29823 = CARTESIAN_POINT ( 'NONE',  ( 107.0664832912739968, -36.72944715994100306, 287.6356252759109680 ) ) ;
#29824 = CARTESIAN_POINT ( 'NONE',  ( 97.81169962758427516, -40.51743340529665005, 76.63548575323150658 ) ) ;
#29825 = AXIS2_PLACEMENT_3D ( 'NONE', #22402, #14242, #63279 ) ;
#29826 = CARTESIAN_POINT ( 'NONE',  ( 91.73195104381078124, 95.23006786499112764, 92.89936586972081045 ) ) ;
#29827 = EDGE_CURVE ( 'NONE', #27673, #74190, #78546, .T. ) ;
#29828 = CARTESIAN_POINT ( 'NONE',  ( 105.8001462888458519, -26.72394952473684882, 51.17876692797100446 ) ) ;
#29829 = DIRECTION ( 'NONE',  ( -1.000000000000000078E-15, 1.000000000000000083E-30, 1.000000000000000000 ) ) ;
#29830 = CARTESIAN_POINT ( 'NONE',  ( -5.303323664314122610, 94.09012423098154443, 130.4482521264637285 ) ) ;
#29831 = CARTESIAN_POINT ( 'NONE',  ( 104.6539710028518897, -47.49251396406771164, 27.38895860924395009 ) ) ;
#29833 = VERTEX_POINT ( 'NONE', #4345 ) ;
#29832 = ADVANCED_FACE ( 'NONE', ( #12953 ), #52450, .F. ) ;
#29834 = CARTESIAN_POINT ( 'NONE',  ( 107.0664832912739541, -22.72944715994095688, 315.1356252759112522 ) ) ;
#29835 = CARTESIAN_POINT ( 'NONE',  ( 79.56670390244703128, -105.9704134719596738, 250.2178068554180470 ) ) ;
#29836 = CARTESIAN_POINT ( 'NONE',  ( 108.6369934722860506, -45.24028864696019525, 125.5518998934009574 ) ) ;
#29837 = ADVANCED_FACE ( 'NONE', ( #33381 ), #18402, .F. ) ;
#29838 = VECTOR ( 'NONE', #15914, 1000.000000000000227 ) ;
#29839 = CIRCLE ( 'NONE', #83452, 7.500000000000007105 ) ;
#29840 = CARTESIAN_POINT ( 'NONE',  ( 97.75849014177104834, -40.38515380072060168, 96.62427964741705466 ) ) ;
#29841 = CARTESIAN_POINT ( 'NONE',  ( 48.16670390244701139, -26.71338133339251542, 342.9256252759119548 ) ) ;
#29842 = ORIENTED_EDGE ( 'NONE', *, *, #10196, .F. ) ;
#29843 = EDGE_LOOP ( 'NONE', ( #39143, #30620, #86115, #1402 ) ) ;
#29844 = CARTESIAN_POINT ( 'NONE',  ( 226.4410000000000025, 40.03750000000000142, -2.032000000000000028 ) ) ;
#29845 = ORIENTED_EDGE ( 'NONE', *, *, #80138, .T. ) ;
#29846 = VERTEX_POINT ( 'NONE', #73824 ) ;
#29847 = EDGE_CURVE ( 'NONE', #13859, #80299, #62561, .T. ) ;
#29848 = CARTESIAN_POINT ( 'NONE',  ( 115.9244277637092040, -39.86207309682762912, 174.9996785439919904 ) ) ;
#29849 = CARTESIAN_POINT ( 'NONE',  ( 57.91199999999999903, 20.32000000000000028, 178.6098374884404905 ) ) ;
#29850 = EDGE_CURVE ( 'NONE', #1345, #87676, #53843, .T. ) ;
#29851 = CARTESIAN_POINT ( 'NONE',  ( 95.46382812221506242, -34.19949780945433560, 102.1556252759109640 ) ) ;
#29852 = CARTESIAN_POINT ( 'NONE',  ( 113.2363792478179789, -44.61460182729985036, 18.10486178924557521 ) ) ;
#29853 = CONICAL_SURFACE ( 'NONE', #31254, 190.5000000000000000, 0.7853981633974300713 ) ;
#29854 = EDGE_LOOP ( 'NONE', ( #35908, #7582, #60853, #17200 ) ) ;
#29855 = VECTOR ( 'NONE', #39064, 1000.000000000000000 ) ;
#29856 = VECTOR ( 'NONE', #81885, 1000.000000000000000 ) ;
#29857 = AXIS2_PLACEMENT_3D ( 'NONE', #13951, #41635, #62545 ) ;
#29858 = VERTEX_POINT ( 'NONE', #11143 ) ;
#29859 = VERTEX_POINT ( 'NONE', #59730 ) ;
#29860 = CARTESIAN_POINT ( 'NONE',  ( 103.0873890296785333, -43.88832256772609952, 184.9909475124489688 ) ) ;
#29861 = CARTESIAN_POINT ( 'NONE',  ( 110.3789737648050107, -47.29935009229100729, 52.80610146638697699 ) ) ;
#29862 = EDGE_LOOP ( 'NONE', ( #1755, #71593 ) ) ;
#29863 = CARTESIAN_POINT ( 'NONE',  ( 109.6066175024219973, -25.17973177368032012, 29.90419670448196854 ) ) ;
#29864 = CARTESIAN_POINT ( 'NONE',  ( 114.9815172128508465, -29.91112648151817410, 180.3927681330539770 ) ) ;
#29865 = CYLINDRICAL_SURFACE ( 'NONE', #29241, 16.09746158385918946 ) ;
#29866 = CARTESIAN_POINT ( 'NONE',  ( -110.7653435595065901, 44.45000000000000284, 69.10794311903988785 ) ) ;
#29867 = CARTESIAN_POINT ( 'NONE',  ( 113.0769238478409449, -28.21140209294909695, 125.5870538473399591 ) ) ;
#29868 = DIRECTION ( 'NONE',  ( 1.000000000000000000, 0.000000000000000000, 0.000000000000000000 ) ) ;
#29869 = ORIENTED_EDGE ( 'NONE', *, *, #51162, .F. ) ;
#29870 = VECTOR ( 'NONE', #17404, 1000.000000000000000 ) ;
#29871 = FACE_OUTER_BOUND ( 'NONE', #48349, .T. ) ;
#29872 = EDGE_CURVE ( 'NONE', #77063, #34249, #52882, .T. ) ;
#29873 = ORIENTED_EDGE ( 'NONE', *, *, #27048, .F. ) ;
#29874 = FACE_OUTER_BOUND ( 'NONE', #88311, .T. ) ;
#29875 = ORIENTED_EDGE ( 'NONE', *, *, #51693, .F. ) ;
#29876 = AXIS2_PLACEMENT_3D ( 'NONE', #50452, #78199, #51336 ) ;
#29877 = ORIENTED_EDGE ( 'NONE', *, *, #64054, .T. ) ;
#29878 = EDGE_CURVE ( 'NONE', #81504, #60315, #71277, .T. ) ;
#29879 = DIRECTION ( 'NONE',  ( 0.000000000000000000, 0.000000000000000000, 1.000000000000000000 ) ) ;
#29880 = CARTESIAN_POINT ( 'NONE',  ( 6.309809686823171226, 93.48723291110538014, 118.3899544324468849 ) ) ;
#29881 = CARTESIAN_POINT ( 'NONE',  ( 98.64717563880898865, -43.89145428829765194, 76.89943479971999807 ) ) ;
#29882 = CARTESIAN_POINT ( 'NONE',  ( 48.86082318535700608, -35.55794170701751256, -5.074374724088000832 ) ) ;
#29883 = VECTOR ( 'NONE', #70916, 1000.000000000000000 ) ;
#29884 = PLANE ( 'NONE',  #59407 ) ;
#29885 = DIRECTION ( 'NONE',  ( 0.000000000000000000, -1.000000000000000000, 0.000000000000000000 ) ) ;
#29886 = CARTESIAN_POINT ( 'NONE',  ( 116.4365193811697310, -32.28633913640743458, 64.19086337114998742 ) ) ;
#29888 = CARTESIAN_POINT ( 'NONE',  ( 118.8928063919343145, -36.92768728534039013, 149.8127681330539644 ) ) ;
#29887 = LINE ( 'NONE', #63495, #53595 ) ;
#29889 = DIRECTION ( 'NONE',  ( 0.000000000000000000, 0.000000000000000000, -1.000000000000000000 ) ) ;
#29890 = LINE ( 'NONE', #78044, #33664 ) ;
#29891 = VERTEX_POINT ( 'NONE', #32474 ) ;
#29892 = DIRECTION ( 'NONE',  ( 0.000000000000000000, 0.000000000000000000, -1.000000000000000000 ) ) ;
#29893 = DIRECTION ( 'NONE',  ( -1.000000000000000000, 0.000000000000000000, 0.000000000000000000 ) ) ;
#29894 = ORIENTED_EDGE ( 'NONE', *, *, #54065, .F. ) ;
#29895 = CARTESIAN_POINT ( 'NONE',  ( 74.06670390244701707, -90.27844715994098124, 222.2178068554179902 ) ) ;
#29897 = EDGE_LOOP ( 'NONE', ( #3106, #25952, #19715, #31012 ) ) ;
#29896 = CARTESIAN_POINT ( 'NONE',  ( 111.4357194830650002, -47.79916136671457849, 172.8756252759109771 ) ) ;
#29898 = LINE ( 'NONE', #77596, #26258 ) ;
#29899 = CARTESIAN_POINT ( 'NONE',  ( 108.0160737019250377, -24.89219542061752577, 261.0127681330534415 ) ) ;
#29900 = CARTESIAN_POINT ( 'NONE',  ( 95.98963492482539550, -41.07853246264400582, 92.62419670448296927 ) ) ;
#29901 = CARTESIAN_POINT ( 'NONE',  ( 128.5492039024480562, -51.22944715994093912, 207.5838068554170377 ) ) ;
#29902 = CARTESIAN_POINT ( 'NONE',  ( 97.07201034874346135, -35.37904553719489797, 192.2188556906257304 ) ) ;
#29903 = DIRECTION ( 'NONE',  ( 6.524622321627019585E-16, 3.741823817616790462E-31, 1.000000000000000000 ) ) ;
#29904 = ORIENTED_EDGE ( 'NONE', *, *, #73779, .F. ) ;
#29905 = ADVANCED_FACE ( 'NONE', ( #11610 ), #60174, .T. ) ;
#29906 = VERTEX_POINT ( 'NONE', #26567 ) ;
#29907 = EDGE_CURVE ( 'NONE', #76165, #58962, #81116, .T. ) ;
#29908 = ORIENTED_EDGE ( 'NONE', *, *, #64493, .T. ) ;
#29909 = EDGE_CURVE ( 'NONE', #47878, #74702, #43856, .T. ) ;
#29910 = ORIENTED_EDGE ( 'NONE', *, *, #52240, .F. ) ;
#29911 = DIRECTION ( 'NONE',  ( 4.299999999999999979E-14, -1.000000000000000000, 4.400000000000000367E-29 ) ) ;
#29912 = CARTESIAN_POINT ( 'NONE',  ( 95.29510253380274776, -38.09663793710245017, 232.4184824187679794 ) ) ;
#29913 = DIRECTION ( 'NONE',  ( -4.237773401492740281E-14, 1.000000000000000000, 0.000000000000000000 ) ) ;
#29914 = CARTESIAN_POINT ( 'NONE',  ( 132.8230071953894083, -34.27587548316717658, 1.868342134762299045 ) ) ;
#29915 = EDGE_CURVE ( 'NONE', #89702, #80585, #79973, .T. ) ;
#29917 = CARTESIAN_POINT ( 'NONE',  ( 86.67734222162479796, 70.52090377575433422, 80.88709205069480390 ) ) ;
#29916 = DIRECTION ( 'NONE',  ( -6.831565154159360295E-14, 1.000000000000000000, 0.000000000000000000 ) ) ;
#29918 = AXIS2_PLACEMENT_3D ( 'NONE', #66919, #65580, #32381 ) ;
#29919 = DIRECTION ( 'NONE',  ( -1.000000000000000000, 7.980413499659419871E-32, 0.000000000000000000 ) ) ;
#29920 = CARTESIAN_POINT ( 'NONE',  ( 99.96564438395634511, -44.39263518965486099, 46.98133956162592284 ) ) ;
#29921 = ORIENTED_EDGE ( 'NONE', *, *, #15796, .T. ) ;
#29922 = ORIENTED_EDGE ( 'NONE', *, *, #4195, .T. ) ;
#29923 = AXIS2_PLACEMENT_3D ( 'NONE', #25119, #81457, #4685 ) ;
#29924 = VERTEX_POINT ( 'NONE', #27459 ) ;
#29925 = EDGE_CURVE ( 'NONE', #30966, #29159, #43689, .T. ) ;
#29926 = VECTOR ( 'NONE', #3728, 1000.000000000000000 ) ;
#29927 = VECTOR ( 'NONE', #47219, 1000.000000000000000 ) ;
#29928 = CARTESIAN_POINT ( 'NONE',  ( 140.0667039024470455, -118.2784471599408960, 51.21780685541800437 ) ) ;
#29929 = CIRCLE ( 'NONE', #13961, 17.33514202138210081 ) ;
#29930 = FACE_OUTER_BOUND ( 'NONE', #76889, .T. ) ;
#29931 = CARTESIAN_POINT ( 'NONE',  ( 110.6561457788924230, -27.59554888373227755, 265.7784824187677941 ) ) ;
#29932 = EDGE_CURVE ( 'NONE', #26236, #43244, #41083, .T. ) ;
#29933 = DIRECTION ( 'NONE',  ( 1.000000000000000000, 0.000000000000000000, 0.000000000000000000 ) ) ;
#29934 = CARTESIAN_POINT ( 'NONE',  ( 116.0091996907507195, -30.12340400999218559, 105.3327681330529515 ) ) ;
#29935 = CARTESIAN_POINT ( 'NONE',  ( 107.0664832912739968, -36.72944715994100306, 287.6356252759109680 ) ) ;
#29936 = ORIENTED_EDGE ( 'NONE', *, *, #10860, .F. ) ;
#29937 = FACE_OUTER_BOUND ( 'NONE', #66337, .T. ) ;
#29938 = CARTESIAN_POINT ( 'NONE',  ( 74.06670390244701707, -90.27844715994098124, 222.2178068554179902 ) ) ;
#29939 = VERTEX_POINT ( 'NONE', #34272 ) ;
#29940 = CIRCLE ( 'NONE', #67593, 11.57110091390439699 ) ;
#29941 = CARTESIAN_POINT ( 'NONE',  ( -76.39920031718024518, 90.28416741362498499, 90.65736737572441939 ) ) ;
#29942 = CARTESIAN_POINT ( 'NONE',  ( 99.56565989216673529, -33.50937434423423156, 13.82237608387698558 ) ) ;
#29943 = FACE_OUTER_BOUND ( 'NONE', #72908, .T. ) ;
#29944 = AXIS2_PLACEMENT_3D ( 'NONE', #40832, #22552, #8013 ) ;
#29945 = DIRECTION ( 'NONE',  ( 0.000000000000000000, 0.000000000000000000, -1.000000000000000000 ) ) ;
#29946 = CARTESIAN_POINT ( 'NONE',  ( 116.8171726708769285, -34.15311105152028404, 195.0314804765609722 ) ) ;
#29947 = ORIENTED_EDGE ( 'NONE', *, *, #52171, .T. ) ;
#29948 = DIRECTION ( 'NONE',  ( -0.000000000000000000, 1.000000000000000000, 0.000000000000000000 ) ) ;
#29949 = FACE_OUTER_BOUND ( 'NONE', #63664, .T. ) ;
#29950 = ORIENTED_EDGE ( 'NONE', *, *, #84604, .T. ) ;
#29951 = CARTESIAN_POINT ( 'NONE',  ( 102.9709959788349636, -46.31662683568885086, 92.25562527591097250 ) ) ;
#29952 = ORIENTED_EDGE ( 'NONE', *, *, #52908, .T. ) ;
#29953 = CARTESIAN_POINT ( 'NONE',  ( 109.9248237270229680, -44.80917438794489271, 37.26956268521996662 ) ) ;
#29954 = CARTESIAN_POINT ( 'NONE',  ( 115.0390926746001981, -42.79681148600482032, 89.30794038968477366 ) ) ;
#29955 = CARTESIAN_POINT ( 'NONE',  ( 112.4269750522866502, -44.91043508143939533, 178.0384824187689503 ) ) ;
#29956 = DIRECTION ( 'NONE',  ( 0.000000000000000000, 0.000000000000000000, -1.000000000000000000 ) ) ;
#29957 = CARTESIAN_POINT ( 'NONE',  ( 140.0667039024470455, -118.2784471599408960, 222.2178068554179902 ) ) ;
#29958 = CARTESIAN_POINT ( 'NONE',  ( 69.72411017812960665, 127.0000000000000000, 69.72411017813040246 ) ) ;
#29959 = CARTESIAN_POINT ( 'NONE',  ( 115.6911734784272170, -30.73338764459478867, 275.3099109901965562 ) ) ;
#29960 = ORIENTED_EDGE ( 'NONE', *, *, #14103, .T. ) ;
#29961 = CARTESIAN_POINT ( 'NONE',  ( 48.85858412958099706, -30.08671355700241179, -5.074374724088000832 ) ) ;
#29962 = VERTEX_POINT ( 'NONE', #89711 ) ;
#29963 = CARTESIAN_POINT ( 'NONE',  ( 100.8606736390591720, -45.92946726319084405, 148.0918157521009562 ) ) ;
#29964 = DIRECTION ( 'NONE',  ( 0.000000000000000000, -0.8660254037844387076, 0.4999999999999998890 ) ) ;
#29965 = EDGE_LOOP ( 'NONE', ( #50367, #1905 ) ) ;
#29966 = ORIENTED_EDGE ( 'NONE', *, *, #43724, .T. ) ;
#29967 = EDGE_LOOP ( 'NONE', ( #15581, #39132, #62171, #83310 ) ) ;
#29968 = LINE ( 'NONE', #7730, #8673 ) ;
#29969 = LINE ( 'NONE', #72197, #39102 ) ;
#29970 = CARTESIAN_POINT ( 'NONE',  ( 114.3351522754913674, -30.13549343754558407, 209.4127681330539872 ) ) ;
#29971 = CARTESIAN_POINT ( 'NONE',  ( 67.65734841870819594, 69.84999999999999432, 346.9005000000000223 ) ) ;
#29972 = CARTESIAN_POINT ( 'NONE',  ( 144.0315611170736645, -140.7135899453143111, 245.8512780488640033 ) ) ;
#29973 = DIRECTION ( 'NONE',  ( 0.000000000000000000, 0.000000000000000000, -1.000000000000000000 ) ) ;
#29974 = CARTESIAN_POINT ( 'NONE',  ( 111.3231501057927346, -27.21297328954094041, 20.74133956162494030 ) ) ;
#29975 = LINE ( 'NONE', #76777, #68232 ) ;
#29976 = ORIENTED_EDGE ( 'NONE', *, *, #32785, .F. ) ;
#29977 = CARTESIAN_POINT ( 'NONE',  ( 103.2784589858348596, -27.47467144708731368, 171.3856301094683374 ) ) ;
#29978 = VECTOR ( 'NONE', #49375, 1000.000000000000000 ) ;
#29979 = DIRECTION ( 'NONE',  ( 0.000000000000000000, 0.000000000000000000, 1.000000000000000000 ) ) ;
#29980 = EDGE_LOOP ( 'NONE', ( #54068, #54386, #20590, #14941 ) ) ;
#29981 = EDGE_LOOP ( 'NONE', ( #8603, #78001, #83104, #21845, #88843 ) ) ;
#29982 = AXIS2_PLACEMENT_3D ( 'NONE', #41417, #69147, #83680 ) ;
#29983 = EDGE_CURVE ( 'NONE', #40161, #34521, #13394, .T. ) ;
#29984 = VECTOR ( 'NONE', #30545, 1000.000000000000000 ) ;
#29985 = CARTESIAN_POINT ( 'NONE',  ( 168.0371591254546217, -48.62818131005519007, 129.9678068554150059 ) ) ;
#29986 = AXIS2_PLACEMENT_3D ( 'NONE', #7037, #216, #88379 ) ;
#29987 = FACE_OUTER_BOUND ( 'NONE', #18605, .T. ) ;
#29988 = CARTESIAN_POINT ( 'NONE',  ( 110.4916936757735471, -26.90617889774101812, 209.8099109901969541 ) ) ;
#29989 = DIRECTION ( 'NONE',  ( -1.986798540846734824E-16, 0.000000000000000000, 1.000000000000000000 ) ) ;
#29990 = CIRCLE ( 'NONE', #80756, 2.500000000000002220 ) ;
#29991 = CARTESIAN_POINT ( 'NONE',  ( 75.31670390244798341, -57.40094715994099772, 35.51780685541480409 ) ) ;
#29992 = DIRECTION ( 'NONE',  ( -4.237773401492740281E-14, 1.000000000000000000, 0.000000000000000000 ) ) ;
#29993 = CARTESIAN_POINT ( 'NONE',  ( 115.0883484252707376, -39.66301350383546520, 217.9695626852199837 ) ) ;
#29995 = CARTESIAN_POINT ( 'NONE',  ( 100.4929927897290582, -27.87207479535962662, 31.59657765686396758 ) ) ;
#29994 = DIRECTION ( 'NONE',  ( 5.512527431108029424E-15, -1.000000000000000000, 0.000000000000000000 ) ) ;
#29996 = DIRECTION ( 'NONE',  ( 0.000000000000000000, -1.000000000000000000, 0.000000000000000000 ) ) ;
#29997 = CARTESIAN_POINT ( 'NONE',  ( 100.2700262342886219, -46.49863182355969116, 87.09276813305393716 ) ) ;
#29998 = ORIENTED_EDGE ( 'NONE', *, *, #22105, .F. ) ;
#29999 = CARTESIAN_POINT ( 'NONE',  ( 131.4052890608957682, -19.42303004212037010, 6.877070700250059510 ) ) ;
#30000 = ORIENTED_EDGE ( 'NONE', *, *, #78325, .F. ) ;
#30001 = CARTESIAN_POINT ( 'NONE',  ( 177.1649999999999920, 14.63749999999999929, -47.62500000000000000 ) ) ;
#30002 = CARTESIAN_POINT ( 'NONE',  ( 103.2798918628733134, -27.47408509851724290, 276.3855069386696073 ) ) ;
#30003 = ORIENTED_EDGE ( 'NONE', *, *, #81384, .F. ) ;
#30004 = LINE ( 'NONE', #1405, #24425 ) ;
#30005 = VERTEX_POINT ( 'NONE', #7473 ) ;
#30006 = CARTESIAN_POINT ( 'NONE',  ( 63.03715912545639100, -24.42818131006026761, 180.4678068554151196 ) ) ;
#30007 = FACE_OUTER_BOUND ( 'NONE', #31506, .T. ) ;
#30008 = DIRECTION ( 'NONE',  ( 1.000000000000000000, 0.000000000000000000, 0.000000000000000000 ) ) ;
#30009 = EDGE_LOOP ( 'NONE', ( #44242, #18210, #74258, #12917 ) ) ;
#30010 = VECTOR ( 'NONE', #27073, 1000.000000000000000 ) ;
#30011 = CARTESIAN_POINT ( 'NONE',  ( 103.3545649297684577, -47.16578287771347533, 102.3165776568629752 ) ) ;
#30012 = CARTESIAN_POINT ( 'NONE',  ( -215.9000000000000057, 0.000000000000000000, -45.33899999999999864 ) ) ;
#30013 = DIRECTION ( 'NONE',  ( -0.7071067811571960515, 0.7071067812158990940, 0.000000000000000000 ) ) ;
#30014 = DIRECTION ( 'NONE',  ( -0.000000000000000000, -0.000000000000000000, 1.000000000000000000 ) ) ;
#30015 = ORIENTED_EDGE ( 'NONE', *, *, #73789, .F. ) ;
#30016 = EDGE_CURVE ( 'NONE', #52044, #43910, #58224, .T. ) ;
#30017 = ADVANCED_FACE ( 'NONE', ( #69253 ), #68806, .T. ) ;
#30018 = LINE ( 'NONE', #70914, #34429 ) ;
#30019 = CARTESIAN_POINT ( 'NONE',  ( -215.9000000000000057, 0.000000000000000000, 146.9389999999999930 ) ) ;
#30020 = EDGE_CURVE ( 'NONE', #22233, #58142, #40931, .T. ) ;
#30021 = CARTESIAN_POINT ( 'NONE',  ( 41.56648329127398966, -18.82844715994071194, 18.92562527591200094 ) ) ;
#30022 = EDGE_CURVE ( 'NONE', #26639, #8253, #39350, .T. ) ;
#30024 = CARTESIAN_POINT ( 'NONE',  ( 107.0664832912739968, -36.72944715994100306, 287.6356252759109680 ) ) ;
#30023 = FACE_OUTER_BOUND ( 'NONE', #62339, .T. ) ;
#30025 = CARTESIAN_POINT ( 'NONE',  ( -72.96458098368600531, 127.0000000000000000, -80.90208098368781009 ) ) ;
#30026 = ORIENTED_EDGE ( 'NONE', *, *, #969, .F. ) ;
#30027 = PLANE ( 'NONE',  #36066 ) ;
#30028 = CARTESIAN_POINT ( 'NONE',  ( 118.1473594538625349, -37.63838399483782382, 184.7613395616249647 ) ) ;
#30029 = EDGE_CURVE ( 'NONE', #54555, #30833, #26324, .T. ) ;
#30031 = EDGE_LOOP ( 'NONE', ( #25612, #58624, #32394, #78148 ) ) ;
#30030 = DIRECTION ( 'NONE',  ( 0.000000000000000000, 1.000000000000000000, 0.000000000000000000 ) ) ;
#30032 = CARTESIAN_POINT ( 'NONE',  ( 97.72045521349410535, -39.61305637792672485, 17.56419670448195092 ) ) ;
#30033 = CARTESIAN_POINT ( 'NONE',  ( -3.968750000000754508, 120.6499999999999915, 100.8961411191535973 ) ) ;
#30034 = CARTESIAN_POINT ( 'NONE',  ( 110.8549148032106615, -45.98405610977419400, 52.88566334576604788 ) ) ;
#30035 = CARTESIAN_POINT ( 'NONE',  ( 104.4067564067896399, -46.45769496072055915, 12.36492216824909463 ) ) ;
#30036 = CARTESIAN_POINT ( 'NONE',  ( 1.387778780781445676E-14, 238.8000000000000114, 97.27542076772557778 ) ) ;
#30037 = AXIS2_PLACEMENT_3D ( 'NONE', #23441, #77490, #30676 ) ;
#30038 = VECTOR ( 'NONE', #69853, 1000.000000000000000 ) ;
#30039 = CARTESIAN_POINT ( 'NONE',  ( 117.4008144674645280, -32.62901037329574905, 249.1270538473399654 ) ) ;
#30040 = EDGE_LOOP ( 'NONE', ( #10806, #26053, #43601, #79388 ) ) ;
#30041 = ORIENTED_EDGE ( 'NONE', *, *, #19874, .F. ) ;
#30042 = CARTESIAN_POINT ( 'NONE',  ( 109.0147404159584568, -27.53810233378435157, 181.3539642582779550 ) ) ;
#30043 = AXIS2_PLACEMENT_3D ( 'NONE', #29782, #63400, #1181 ) ;
#30044 = DIRECTION ( 'NONE',  ( -0.000000000000000000, -0.000000000000000000, 1.000000000000000000 ) ) ;
#30045 = VECTOR ( 'NONE', #27253, 1000.000000000000000 ) ;
#30046 = CARTESIAN_POINT ( 'NONE',  ( 97.81060075337646254, -38.34349919808700236, 42.88348806780201272 ) ) ;
#30047 = AXIS2_PLACEMENT_3D ( 'NONE', #69380, #6697, #56628 ) ;
#30048 = CARTESIAN_POINT ( 'NONE',  ( 23.75644972749645589, 82.86210472292506779, 307.6498562130229857 ) ) ;
#30049 = CARTESIAN_POINT ( 'NONE',  ( 84.06648329127399677, -18.82844715994099971, 17.92562527591199739 ) ) ;
#30050 = DIRECTION ( 'NONE',  ( 0.000000000000000000, -1.000000000000000000, 0.000000000000000000 ) ) ;
#30051 = ORIENTED_EDGE ( 'NONE', *, *, #38318, .F. ) ;
#30052 = CARTESIAN_POINT ( 'NONE',  ( 167.2371591254543262, -47.82818131005522844, 249.9678068554149775 ) ) ;
#30053 = DIRECTION ( 'NONE',  ( 0.000000000000000000, 1.000000000000000000, 0.000000000000000000 ) ) ;
#30054 = CARTESIAN_POINT ( 'NONE',  ( 112.6519946835718855, -45.50616226388166297, 263.0270538473394595 ) ) ;
#30055 = CARTESIAN_POINT ( 'NONE',  ( 12.49830496249506240, 84.20078624585569571, 117.6942513177057776 ) ) ;
#30056 = EDGE_LOOP ( 'NONE', ( #72946, #11934 ) ) ;
#30057 = ORIENTED_EDGE ( 'NONE', *, *, #17243, .F. ) ;
#30058 = FACE_OUTER_BOUND ( 'NONE', #23657, .T. ) ;
#30059 = CARTESIAN_POINT ( 'NONE',  ( 107.0667039024470313, -104.2784471599409528, 55.21780685541800437 ) ) ;
#30060 = DIRECTION ( 'NONE',  ( 0.000000000000000000, 0.000000000000000000, 1.000000000000000000 ) ) ;
#30061 = AXIS2_PLACEMENT_3D ( 'NONE', #52884, #25671, #18404 ) ;
#30062 = CARTESIAN_POINT ( 'NONE',  ( 123.0664832912757163, -36.72944715993921960, -4.074374724089013355 ) ) ;
#30063 = VECTOR ( 'NONE', #3172, 1000.000000000000000 ) ;
#30064 = ADVANCED_FACE ( 'NONE', ( #27022 ), #62427, .F. ) ;
#30065 = CARTESIAN_POINT ( 'NONE',  ( 117.3951115944450123, -37.65585020919950665, 29.74324432352998215 ) ) ;
#30066 = CARTESIAN_POINT ( 'NONE',  ( -7.661254700127833495, 82.54999999999999716, 275.4630000000000223 ) ) ;
#30067 = EDGE_LOOP ( 'NONE', ( #33419, #72852, #80735, #50681 ) ) ;
#30068 = CARTESIAN_POINT ( 'NONE',  ( 112.7653987728015323, -27.20474975302890996, 50.65943479972101215 ) ) ;
#30069 = LINE ( 'NONE', #64586, #46830 ) ;
#30070 = EDGE_CURVE ( 'NONE', #82153, #76973, #30669, .T. ) ;
#30071 = CARTESIAN_POINT ( 'NONE',  ( 100.1774089044720881, -45.37350532423673144, 272.0289586092443415 ) ) ;
#30072 = EDGE_LOOP ( 'NONE', ( #89429, #37900, #80135, #2989 ) ) ;
#30073 = CARTESIAN_POINT ( 'NONE',  ( 82.59704509974100972, -17.65293374834238094, 2.807537076564926348 ) ) ;
#30074 = DIRECTION ( 'NONE',  ( -1.000000000000000000, 0.000000000000000000, 0.000000000000000000 ) ) ;
#30075 = DIRECTION ( 'NONE',  ( -0.7071067811868619879, -0.7071067811862330466, -7.071067811868925614E-16 ) ) ;
#30076 = CARTESIAN_POINT ( 'NONE',  ( 111.9804352529405804, -29.60526291441071578, 87.42618560768700320 ) ) ;
#30077 = CARTESIAN_POINT ( 'NONE',  ( 96.83718905160354495, -34.60841009949970726, 212.1641967044819808 ) ) ;
#30078 = CARTESIAN_POINT ( 'NONE',  ( 57.14999999999999858, 95.25000000000000000, 300.8629999999999995 ) ) ;
#30079 = ORIENTED_EDGE ( 'NONE', *, *, #34196, .F. ) ;
#30080 = DIRECTION ( 'NONE',  ( 0.000000000000000000, 0.000000000000000000, -1.000000000000000000 ) ) ;
#30081 = ORIENTED_EDGE ( 'NONE', *, *, #74802, .F. ) ;
#30083 = ORIENTED_EDGE ( 'NONE', *, *, #75777, .F. ) ;
#30082 = AXIS2_PLACEMENT_3D ( 'NONE', #43848, #51108, #22099 ) ;
#30084 = EDGE_CURVE ( 'NONE', #10149, #50389, #75614, .T. ) ;
#30085 = LINE ( 'NONE', #4160, #89458 ) ;
#30086 = VERTEX_POINT ( 'NONE', #54692 ) ;
#30087 = ORIENTED_EDGE ( 'NONE', *, *, #32838, .F. ) ;
#30088 = CARTESIAN_POINT ( 'NONE',  ( 116.3153332067577850, -32.94059133099460723, 170.1356252759109680 ) ) ;
#30089 = CARTESIAN_POINT ( 'NONE',  ( 97.06382365635857923, -37.34195890833274234, 42.37516235093055883 ) ) ;
#30090 = CARTESIAN_POINT ( 'NONE',  ( 115.5032561769494066, -38.06248691838574416, 113.1238483995059596 ) ) ;
#30091 = CARTESIAN_POINT ( 'NONE',  ( 104.8365363718904888, -26.48661066032647327, 260.2470538473397710 ) ) ;
#30092 = LINE ( 'NONE', #15579, #65863 ) ;
#30093 = ORIENTED_EDGE ( 'NONE', *, *, #45260, .F. ) ;
#30094 = EDGE_CURVE ( 'NONE', #30425, #46304, #82454, .T. ) ;
#30095 = VERTEX_POINT ( 'NONE', #62871 ) ;
#30096 = CARTESIAN_POINT ( 'NONE',  ( 41.56648329127399677, -18.82844715994099971, 78.92562527591199739 ) ) ;
#30097 = AXIS2_PLACEMENT_3D ( 'NONE', #39127, #65930, #66830 ) ;
#30098 = CARTESIAN_POINT ( 'NONE',  ( 104.4073484937606935, -46.45786862655047145, 32.36494955462968903 ) ) ;
#30099 = CARTESIAN_POINT ( 'NONE',  ( 46.48091746482051434, -49.32844715994088602, 129.9678068554150911 ) ) ;
#30101 = CARTESIAN_POINT ( 'NONE',  ( 41.56648329127398966, -27.82844715994070484, 15.92562527591200094 ) ) ;
#30100 = AXIS2_PLACEMENT_3D ( 'NONE', #77271, #7777, #77725 ) ;
#30102 = ORIENTED_EDGE ( 'NONE', *, *, #88734, .F. ) ;
#30103 = CIRCLE ( 'NONE', #1054, 34.13125000000000142 ) ;
#30104 = CARTESIAN_POINT ( 'NONE',  ( 97.55979742750555772, -43.80499729575070234, 261.8356252759109566 ) ) ;
#30105 = CARTESIAN_POINT ( 'NONE',  ( 114.8518103909616315, -43.72813715869710904, 34.24419670448197905 ) ) ;
#30106 = VECTOR ( 'NONE', #41537, 1000.000000000000000 ) ;
#30107 = CARTESIAN_POINT ( 'NONE',  ( 104.4081006533185274, -46.45808913802587625, 118.3647919419379662 ) ) ;
#30109 = CARTESIAN_POINT ( 'NONE',  ( 181.5667039024459939, -18.82844715994099971, 342.9256252759109884 ) ) ;
#30108 = LINE ( 'NONE', #78727, #5655 ) ;
#30110 = DIRECTION ( 'NONE',  ( 4.194175870806139918E-14, -1.000000000000000000, 0.000000000000000000 ) ) ;
#30111 = DIRECTION ( 'NONE',  ( 0.000000000000000000, 0.000000000000000000, -1.000000000000000000 ) ) ;
#30112 = CARTESIAN_POINT ( 'NONE',  ( 77.39114642429899504, 120.6499999999999915, 71.77848634863160271 ) ) ;
#30113 = CARTESIAN_POINT ( 'NONE',  ( 168.5667039024485803, -48.82844715993516616, 180.4678068554150059 ) ) ;
#30114 = ADVANCED_FACE ( 'NONE', ( #20215 ), #7916, .F. ) ;
#30115 = CARTESIAN_POINT ( 'NONE',  ( 98.30754688952644926, -41.72890701560834970, 161.7395981821620978 ) ) ;
#30116 = CIRCLE ( 'NONE', #80902, 0.5000000000000004441 ) ;
#30117 = DIRECTION ( 'NONE',  ( -0.9254794337955620787, -0.3787978585227822492, 0.000000000000000000 ) ) ;
#30118 = CARTESIAN_POINT ( 'NONE',  ( 81.80795390244803400, -42.97311385574014508, 207.5838068554169809 ) ) ;
#30119 = CARTESIAN_POINT ( 'NONE',  ( 118.3649377238561300, -33.07154184081399961, 284.0756252759109657 ) ) ;
#30120 = CARTESIAN_POINT ( 'NONE',  ( 98.16828830165673025, -31.29763223543249850, 166.8899109901969950 ) ) ;
#30121 = CARTESIAN_POINT ( 'NONE',  ( 97.46669833601751520, -32.60829619471579122, 12.00419670448293985 ) ) ;
#30122 = VECTOR ( 'NONE', #53120, 1000.000000000000000 ) ;
#30123 = CIRCLE ( 'NONE', #18503, 34.13125000000000142 ) ;
#30125 = CARTESIAN_POINT ( 'NONE',  ( 115.0372575073645578, -42.90846256548200444, 48.30229194269750792 ) ) ;
#30124 = CARTESIAN_POINT ( 'NONE',  ( -109.2774118001976120, 53.97500000000000142, 71.43750000000000000 ) ) ;
#30126 = CARTESIAN_POINT ( 'NONE',  ( 82.45999417309988644, -35.37149686611228816, 2.653088969726210777 ) ) ;
#30127 = AXIS2_PLACEMENT_3D ( 'NONE', #42292, #7349, #63203 ) ;
#30128 = ORIENTED_EDGE ( 'NONE', *, *, #12101, .T. ) ;
#30129 = FACE_OUTER_BOUND ( 'NONE', #18519, .T. ) ;
#30130 = ORIENTED_EDGE ( 'NONE', *, *, #51238, .F. ) ;
#30131 = CARTESIAN_POINT ( 'NONE',  ( 112.3909220325769382, -27.83061929752864572, 50.65943479972001739 ) ) ;
#30132 = EDGE_CURVE ( 'NONE', #58881, #78082, #87218, .T. ) ;
#30134 = EDGE_LOOP ( 'NONE', ( #56142, #68771, #35181, #50845, #60922, #4651, #48775, #15969 ) ) ;
#30133 = DIRECTION ( 'NONE',  ( 0.9068632946707805287, -0.4214249218767882610, 9.061988307341536250E-16 ) ) ;
#30135 = DIRECTION ( 'NONE',  ( 1.000000000000000000, 4.194175870806139918E-14, 0.000000000000000000 ) ) ;
#30136 = CARTESIAN_POINT ( 'NONE',  ( 101.9951592035502586, -45.85337710724431304, 183.1727681330539781 ) ) ;
#30137 = PLANE ( 'NONE',  #36673 ) ;
#30138 = CARTESIAN_POINT ( 'NONE',  ( 97.81362463995230883, -40.52215243649990128, 146.6360314391660893 ) ) ;
#30139 = EDGE_CURVE ( 'NONE', #59400, #71967, #84244, .T. ) ;
#30140 = DIRECTION ( 'NONE',  ( 0.000000000000000000, 0.000000000000000000, -1.000000000000000000 ) ) ;
#30141 = CARTESIAN_POINT ( 'NONE',  ( 107.9678037105606307, -121.2545485715093463, -19.18411693322849487 ) ) ;
#30142 = CARTESIAN_POINT ( 'NONE',  ( -75.61066417432020614, 101.5999999999999943, 177.0380000000000109 ) ) ;
#30143 = CARTESIAN_POINT ( 'NONE',  ( 110.8532826261943569, -45.98472416447314259, 97.88552295559415484 ) ) ;
#30144 = CARTESIAN_POINT ( 'NONE',  ( 108.8662857618680562, -46.94215964495590043, 122.7032443235309671 ) ) ;
#30145 = VERTEX_POINT ( 'NONE', #15186 ) ;
#30146 = ORIENTED_EDGE ( 'NONE', *, *, #13627, .T. ) ;
#30147 = VECTOR ( 'NONE', #70416, 1000.000000000000000 ) ;
#30148 = CARTESIAN_POINT ( 'NONE',  ( 106.2249424221556922, -46.76750045321607985, 108.9415833058969554 ) ) ;
#30149 = CARTESIAN_POINT ( 'NONE',  ( 76.06670390244796920, -26.72944715994109899, 239.5838068554169809 ) ) ;
#30151 = PLANE ( 'NONE',  #89781 ) ;
#30150 = CARTESIAN_POINT ( 'NONE',  ( 98.06605190618653012, -40.64173669134672906, 227.6527681330529731 ) ) ;
#30152 = FACE_OUTER_BOUND ( 'NONE', #2247, .T. ) ;
#30153 = DIRECTION ( 'NONE',  ( -0.04216478779797398074, 0.9991106698809455455, 0.000000000000000000 ) ) ;
#30154 = DIRECTION ( 'NONE',  ( 0.000000000000000000, 0.000000000000000000, -1.000000000000000000 ) ) ;
#30155 = CARTESIAN_POINT ( 'NONE',  ( 73.06670390244801183, -48.82844715994099971, 250.9178068554160461 ) ) ;
#30156 = CARTESIAN_POINT ( 'NONE',  ( 0.000000000000000000, 127.0000000000000000, -190.5000000000000000 ) ) ;
#30157 = CARTESIAN_POINT ( 'NONE',  ( 108.3633857348901586, -47.68307073960303910, 162.6822919425769669 ) ) ;
#30158 = VERTEX_POINT ( 'NONE', #42864 ) ;
#30159 = VERTEX_POINT ( 'NONE', #6141 ) ;
#30160 = ORIENTED_EDGE ( 'NONE', *, *, #38299, .F. ) ;
#30161 = CARTESIAN_POINT ( 'NONE',  ( 120.9654100508053176, -79.85256584427183668, 250.2201230397200220 ) ) ;
#30162 = CARTESIAN_POINT ( 'NONE',  ( 146.8142838399337791, -68.11919575773853808, 246.4623081562874347 ) ) ;
#30163 = VECTOR ( 'NONE', #21384, 1000.000000000000000 ) ;
#30164 = LINE ( 'NONE', #51046, #27279 ) ;
#30165 = CARTESIAN_POINT ( 'NONE',  ( 98.04124286399094501, -41.04127998252142362, 102.6811413373515762 ) ) ;
#30166 = CARTESIAN_POINT ( 'NONE',  ( 114.9947780803761503, -40.19975936245594283, 206.3042808457819604 ) ) ;
#30167 = AXIS2_PLACEMENT_3D ( 'NONE', #1760, #57143, #84889 ) ;
#30168 = CIRCLE ( 'NONE', #60552, 5.600000000000000533 ) ;
#30169 = CARTESIAN_POINT ( 'NONE',  ( 68.53801554307389665, 120.6499999999999915, 74.15067561874289481 ) ) ;
#30170 = ADVANCED_FACE ( 'NONE', ( #47885 ), #75627, .F. ) ;
#30171 = CARTESIAN_POINT ( 'NONE',  ( 98.55109871784688380, -44.97133477160940629, 191.9384824187679612 ) ) ;
#30172 = CARTESIAN_POINT ( 'NONE',  ( 70.63919639214310564, 49.07499999999999574, -33.74458626278666884 ) ) ;
#30173 = EDGE_LOOP ( 'NONE', ( #45106, #57723, #70424, #43023, #89412, #2830, #57872, #86262, #44013, #72971, #55765, #8730, #84306, #69304, #11747, #82140 ) ) ;
#30175 = ORIENTED_EDGE ( 'NONE', *, *, #24672, .T. ) ;
#30174 = ORIENTED_EDGE ( 'NONE', *, *, #71171, .T. ) ;
#30176 = AXIS2_PLACEMENT_3D ( 'NONE', #42096, #7596, #49805 ) ;
#30177 = CARTESIAN_POINT ( 'NONE',  ( 28.57499999999999929, 87.13271776169270311, 294.9574999999999818 ) ) ;
#30178 = ORIENTED_EDGE ( 'NONE', *, *, #67509, .F. ) ;
#30179 = ORIENTED_EDGE ( 'NONE', *, *, #47951, .F. ) ;
#30180 = PLANE ( 'NONE',  #88466 ) ;
#30181 = CARTESIAN_POINT ( 'NONE',  ( 0.000000000000000000, 44.45000000000000284, 0.000000000000000000 ) ) ;
#30182 = CARTESIAN_POINT ( 'NONE',  ( 108.8902037297786762, -46.63625027785658972, 274.1530118773256390 ) ) ;
#30183 = AXIS2_PLACEMENT_3D ( 'NONE', #58562, #80379, #60346 ) ;
#30184 = FACE_OUTER_BOUND ( 'NONE', #52753, .T. ) ;
#30185 = ORIENTED_EDGE ( 'NONE', *, *, #63218, .T. ) ;
#30186 = CIRCLE ( 'NONE', #80971, 2.116999999999980009 ) ;
#30187 = CIRCLE ( 'NONE', #4047, 2.500000000000002220 ) ;
#30188 = CARTESIAN_POINT ( 'NONE',  ( 115.8167425921599971, -40.08859881155650129, 9.635625275910941312 ) ) ;
#30189 = CARTESIAN_POINT ( 'NONE',  ( -72.96458098368600531, 127.0000000000000000, -65.82083098368781293 ) ) ;
#30190 = ORIENTED_EDGE ( 'NONE', *, *, #44023, .T. ) ;
#30191 = ORIENTED_EDGE ( 'NONE', *, *, #16223, .F. ) ;
#30192 = VECTOR ( 'NONE', #22127, 1000.000000000000000 ) ;
#30193 = EDGE_CURVE ( 'NONE', #11178, #56606, #86028, .T. ) ;
#30194 = CARTESIAN_POINT ( 'NONE',  ( 110.8546553593343589, -45.98416230330774823, 112.8856410521173501 ) ) ;
#30195 = VERTEX_POINT ( 'NONE', #23363 ) ;
#30196 = VERTEX_POINT ( 'NONE', #22907 ) ;
#30197 = AXIS2_PLACEMENT_3D ( 'NONE', #35888, #70879, #57672 ) ;
#30198 = CARTESIAN_POINT ( 'NONE',  ( 111.2046685188893775, -28.67413054290084062, 19.13337220902994318 ) ) ;
#30199 = EDGE_CURVE ( 'NONE', #14989, #82724, #44204, .T. ) ;
#30200 = CARTESIAN_POINT ( 'NONE',  ( 117.8235219141173218, -34.08718286818967158, 164.0061014663869798 ) ) ;
#30201 = CARTESIAN_POINT ( 'NONE',  ( 103.4759237351580623, -46.49349013887667326, 142.2956252759109645 ) ) ;
#30202 = CARTESIAN_POINT ( 'NONE',  ( 188.5667039024479834, -62.87844715994099687, 137.2178068554150059 ) ) ;
#30203 = CARTESIAN_POINT ( 'NONE',  ( 97.01652928432748979, -33.95800134492240119, 247.1127681330539758 ) ) ;
#30204 = CYLINDRICAL_SURFACE ( 'NONE', #22611, 11.49999999999999645 ) ;
#30205 = DIRECTION ( 'NONE',  ( 0.7071067811868677611, 0.7071067811862271624, 7.071067811868671206E-16 ) ) ;
#30206 = DIRECTION ( 'NONE',  ( 0.000000000000000000, 1.000000000000000000, 0.000000000000000000 ) ) ;
#30208 = ORIENTED_EDGE ( 'NONE', *, *, #54049, .F. ) ;
#30207 = ADVANCED_FACE ( 'NONE', ( #10155 ), #79216, .F. ) ;
#30209 = EDGE_CURVE ( 'NONE', #44005, #6482, #46521, .T. ) ;
#30210 = EDGE_LOOP ( 'NONE', ( #7302, #11227, #5005, #86755 ) ) ;
#30211 = VECTOR ( 'NONE', #81015, 1000.000000000000000 ) ;
#30212 = AXIS2_PLACEMENT_3D ( 'NONE', #33820, #40630, #32020 ) ;
#30213 = EDGE_CURVE ( 'NONE', #3990, #16856, #78772, .T. ) ;
#30214 = CARTESIAN_POINT ( 'NONE',  ( 113.7790015168560558, -44.76367177190390834, 193.1299109901969757 ) ) ;
#30215 = ORIENTED_EDGE ( 'NONE', *, *, #41968, .F. ) ;
#30216 = CARTESIAN_POINT ( 'NONE',  ( 100.8863770005861795, -45.89136241369948976, 152.0918157521009562 ) ) ;
#30217 = CARTESIAN_POINT ( 'NONE',  ( 136.8164832912739826, -18.72944715994099951, -5.074374724088999145 ) ) ;
#30218 = EDGE_CURVE ( 'NONE', #24379, #49324, #16972, .T. ) ;
#30219 = DIRECTION ( 'NONE',  ( 0.000000000000000000, 1.000000000000000000, 0.000000000000000000 ) ) ;
#30220 = DIRECTION ( 'NONE',  ( 1.000000000000000078E-15, -1.000000000000000083E-30, -1.000000000000000000 ) ) ;
#30223 = CARTESIAN_POINT ( 'NONE',  ( 103.0988156209413518, -47.86972635628415418, 248.3041967044829619 ) ) ;
#30222 = CARTESIAN_POINT ( 'NONE',  ( 70.63919639214310564, 65.60000000000000853, 95.21359708083839735 ) ) ;
#30221 = CARTESIAN_POINT ( 'NONE',  ( -28.99999999999997513, 127.0000000000000000, 183.8826257785461280 ) ) ;
#30224 = CARTESIAN_POINT ( 'NONE',  ( 176.7738106835694225, -48.62134037881071436, 249.9678068554149775 ) ) ;
#30225 = DIRECTION ( 'NONE',  ( 0.000000000000000000, -1.000000000000000000, 0.000000000000000000 ) ) ;
#30226 = CARTESIAN_POINT ( 'NONE',  ( 108.4139696804897852, -26.73458958342939340, 270.9688129685129638 ) ) ;
#30227 = DIRECTION ( 'NONE',  ( -1.346944695195362088E-15, 1.000000000000000000, -3.469446951953620425E-31 ) ) ;
#30228 = CARTESIAN_POINT ( 'NONE',  ( 97.07207205457036991, -35.37844123025803356, 257.2189586117278850 ) ) ;
#30229 = EDGE_CURVE ( 'NONE', #7741, #30095, #17416, .T. ) ;
#30230 = CYLINDRICAL_SURFACE ( 'NONE', #66604, 9.999999999999998224 ) ;
#30232 = ORIENTED_EDGE ( 'NONE', *, *, #13633, .T. ) ;
#30231 = CARTESIAN_POINT ( 'NONE',  ( 111.7894810538943347, -43.25978944192451792, 195.5838068554170377 ) ) ;
#30233 = LINE ( 'NONE', #24310, #64012 ) ;
#30234 = CARTESIAN_POINT ( 'NONE',  ( 107.9200767535970584, -47.17740107552570805, 177.6413395616249886 ) ) ;
#30235 = CARTESIAN_POINT ( 'NONE',  ( 97.28846512631339749, -33.11380776793520653, 62.04419670448196911 ) ) ;
#30236 = CARTESIAN_POINT ( 'NONE',  ( 97.72358123494467463, -41.53030082902068898, 192.7041967044819728 ) ) ;
#30237 = CARTESIAN_POINT ( 'NONE',  ( -67.35192090801770348, 120.6499999999999915, -78.57724105935601244 ) ) ;
#30238 = CARTESIAN_POINT ( 'NONE',  ( 167.6524903400753601, -49.32844715993521589, 300.4678068554149490 ) ) ;
#30240 = FACE_OUTER_BOUND ( 'NONE', #50476, .T. ) ;
#30239 = DIRECTION ( 'NONE',  ( 0.000000000000000000, 0.000000000000000000, -1.000000000000000000 ) ) ;
#30241 = LINE ( 'NONE', #23878, #52452 ) ;
#30242 = DIRECTION ( 'NONE',  ( 0.000000000000000000, 1.000000000000000000, 0.000000000000000000 ) ) ;
#30243 = EDGE_LOOP ( 'NONE', ( #51300, #30263 ) ) ;
#30244 = CARTESIAN_POINT ( 'NONE',  ( 105.8015779202953013, -26.72375086159097890, 65.17860495093832185 ) ) ;
#30245 = CIRCLE ( 'NONE', #44671, 2.116999999999993776 ) ;
#30246 = AXIS2_PLACEMENT_3D ( 'NONE', #23647, #59019, #85878 ) ;
#30247 = ORIENTED_EDGE ( 'NONE', *, *, #74004, .T. ) ;
#30248 = VERTEX_POINT ( 'NONE', #31037 ) ;
#30249 = CARTESIAN_POINT ( 'NONE',  ( 99.26324148224303201, -33.25589724784042289, 100.4152769709339736 ) ) ;
#30250 = EDGE_CURVE ( 'NONE', #87811, #78226, #1696, .T. ) ;
#30251 = VECTOR ( 'NONE', #78781, 1000.000000000000000 ) ;
#30253 = ORIENTED_EDGE ( 'NONE', *, *, #44334, .F. ) ;
#30252 = CARTESIAN_POINT ( 'NONE',  ( 147.0667039024470739, -140.6784471599409017, 247.2178068554179902 ) ) ;
#30254 = CARTESIAN_POINT ( 'NONE',  ( 97.28692064948108964, -31.62807703868918807, 86.93181575210095957 ) ) ;
#30255 = CARTESIAN_POINT ( 'NONE',  ( -71.77848634863029531, 120.6499999999999915, -77.39114642430038771 ) ) ;
#30256 = ADVANCED_FACE ( 'NONE', ( #57851 ), #58728, .T. ) ;
#30257 = ADVANCED_FACE ( 'NONE', ( #30599, #51901 ), #24235, .F. ) ;
#30258 = DIRECTION ( 'NONE',  ( -0.9068632946707755327, 0.4214249218767993077, 0.000000000000000000 ) ) ;
#30259 = DIRECTION ( 'NONE',  ( 1.000000000000000000, -3.885780586188044357E-13, 0.000000000000000000 ) ) ;
#30260 = EDGE_CURVE ( 'NONE', #34521, #51959, #75675, .T. ) ;
#30261 = CIRCLE ( 'NONE', #15741, 3.600000000000000089 ) ;
#30262 = CARTESIAN_POINT ( 'NONE',  ( 115.1412022171004850, -43.23618977845876543, 43.27467289495995573 ) ) ;
#30263 = ORIENTED_EDGE ( 'NONE', *, *, #63536, .T. ) ;
#30264 = VERTEX_POINT ( 'NONE', #1564 ) ;
#30265 = ORIENTED_EDGE ( 'NONE', *, *, #29691, .T. ) ;
#30266 = LINE ( 'NONE', #72492, #21029 ) ;
#30267 = DIRECTION ( 'NONE',  ( 0.000000000000000000, 1.000000000000000000, 0.000000000000000000 ) ) ;
#30268 = CARTESIAN_POINT ( 'NONE',  ( 102.0670549655111330, -27.97049805627439412, 116.4897919420885017 ) ) ;
#30269 = CARTESIAN_POINT ( 'NONE',  ( -50.03799999999999670, 20.32000000000000028, 178.6098374884404905 ) ) ;
#30270 = FACE_OUTER_BOUND ( 'NONE', #21403, .T. ) ;
#30271 = CARTESIAN_POINT ( 'NONE',  ( 97.53180040003341844, -39.74881746577888464, 52.57028483553885678 ) ) ;
#30272 = VECTOR ( 'NONE', #30318, 1000.000000000000000 ) ;
#30273 = DIRECTION ( 'NONE',  ( 1.000000000000000000, 0.000000000000000000, 0.000000000000000000 ) ) ;
#30274 = CARTESIAN_POINT ( 'NONE',  ( -10.56235306858779133, 89.60171684026197170, 130.1280363297576059 ) ) ;
#30275 = CARTESIAN_POINT ( 'NONE',  ( 100.9539191370901960, -46.85292318231938680, 52.14419670448194921 ) ) ;
#30276 = ORIENTED_EDGE ( 'NONE', *, *, #38118, .F. ) ;
#30277 = CARTESIAN_POINT ( 'NONE',  ( 112.1393459024198478, -28.01282294203041801, 269.6564585851592142 ) ) ;
#30278 = CARTESIAN_POINT ( 'NONE',  ( 88.90000000000000568, 66.67499999999999716, 342.8999999999999773 ) ) ;
#30279 = CARTESIAN_POINT ( 'NONE',  ( 100.7929862627584754, -41.95179922106267156, 114.6966617981629639 ) ) ;
#30280 = CARTESIAN_POINT ( 'NONE',  ( 107.0664832912739257, -52.42944715994095617, 311.6356252759109680 ) ) ;
#30281 = DIRECTION ( 'NONE',  ( 0.000000000000000000, 0.000000000000000000, -1.000000000000000000 ) ) ;
#30282 = ORIENTED_EDGE ( 'NONE', *, *, #67433, .T. ) ;
#30283 = VERTEX_POINT ( 'NONE', #29265 ) ;
#30284 = CARTESIAN_POINT ( 'NONE',  ( 97.86670452396658959, -40.64952357659477400, 136.6473464318451647 ) ) ;
#30285 = ORIENTED_EDGE ( 'NONE', *, *, #40061, .F. ) ;
#30286 = VERTEX_POINT ( 'NONE', #22453 ) ;
#30287 = CARTESIAN_POINT ( 'NONE',  ( 108.5815432132388878, -45.46059095889125246, 164.1444404487539828 ) ) ;
#30288 = VECTOR ( 'NONE', #15596, 1000.000000000000000 ) ;
#30289 = LINE ( 'NONE', #78461, #3212 ) ;
#30290 = CARTESIAN_POINT ( 'NONE',  ( 98.43831584450654759, -42.68208710540699258, 122.8070538473389490 ) ) ;
#30291 = CARTESIAN_POINT ( 'NONE',  ( 109.7248659736901999, -27.00080519511008248, 119.8647919382667055 ) ) ;
#30292 = CARTESIAN_POINT ( 'NONE',  ( 117.0509866428105710, -35.93349926821310447, 18.88982133577855649 ) ) ;
#30293 = CIRCLE ( 'NONE', #25949, 5.599999999999994316 ) ;
#30294 = ORIENTED_EDGE ( 'NONE', *, *, #85795, .T. ) ;
#30295 = CIRCLE ( 'NONE', #2757, 2.117000000000000881 ) ;
#30296 = EDGE_CURVE ( 'NONE', #50718, #55800, #25114, .T. ) ;
#30297 = ORIENTED_EDGE ( 'NONE', *, *, #76346, .F. ) ;
#30298 = EDGE_LOOP ( 'NONE', ( #37450, #32656, #64873, #79556 ) ) ;
#30299 = EDGE_CURVE ( 'NONE', #49377, #53126, #75839, .T. ) ;
#30300 = CARTESIAN_POINT ( 'NONE',  ( 100.3081386793954408, -31.32336695771306623, 193.5957094172099744 ) ) ;
#30302 = EDGE_CURVE ( 'NONE', #60027, #41538, #87353, .T. ) ;
#30301 = VECTOR ( 'NONE', #50833, 1000.000000000000000 ) ;
#30303 = CARTESIAN_POINT ( 'NONE',  ( 96.89953391513134306, -32.33301889150666142, 61.01372051400599616 ) ) ;
#30304 = ORIENTED_EDGE ( 'NONE', *, *, #50234, .T. ) ;
#30305 = CARTESIAN_POINT ( 'NONE',  ( 117.4658636684177679, -37.01502254527063940, 43.80419670448293346 ) ) ;
#30306 = CARTESIAN_POINT ( 'NONE',  ( 117.0378900095125942, -33.61363155034663208, 170.0670538473399631 ) ) ;
#30307 = LINE ( 'NONE', #21712, #4590 ) ;
#30308 = CARTESIAN_POINT ( 'NONE',  ( 82.54999999999999716, 95.25000000000000000, 358.0130000000000337 ) ) ;
#30309 = CARTESIAN_POINT ( 'NONE',  ( 103.1746689306972939, -27.05803214298817849, 126.3813395616259783 ) ) ;
#30310 = DIRECTION ( 'NONE',  ( 0.000000000000000000, 0.000000000000000000, -1.000000000000000000 ) ) ;
#30311 = EDGE_LOOP ( 'NONE', ( #38766, #18780, #37354, #26385 ) ) ;
#30312 = VECTOR ( 'NONE', #17639, 1000.000000000000000 ) ;
#30313 = DIRECTION ( 'NONE',  ( 0.0001713722456127401463, -0.9999999853157766072, -1.713722456137401502E-19 ) ) ;
#30314 = EDGE_CURVE ( 'NONE', #55131, #2012, #17854, .T. ) ;
#30315 = ADVANCED_FACE ( 'NONE', ( #11038 ), #53233, .T. ) ;
#30316 = EDGE_LOOP ( 'NONE', ( #58151, #906, #27204, #71785 ) ) ;
#30317 = AXIS2_PLACEMENT_3D ( 'NONE', #65302, #18031, #86643 ) ;
#30318 = DIRECTION ( 'NONE',  ( 0.000000000000000000, 0.000000000000000000, 1.000000000000000000 ) ) ;
#30319 = ORIENTED_EDGE ( 'NONE', *, *, #65275, .F. ) ;
#30320 = VERTEX_POINT ( 'NONE', #82677 ) ;
#30321 = ADVANCED_FACE ( 'NONE', ( #52338 ), #81003, .F. ) ;
#30322 = FACE_OUTER_BOUND ( 'NONE', #47545, .T. ) ;
#30323 = LINE ( 'NONE', #3944, #69644 ) ;
#30324 = CARTESIAN_POINT ( 'NONE',  ( 96.33825113647944249, -41.76388066030261115, 61.67562527591097421 ) ) ;
#30325 = CARTESIAN_POINT ( 'NONE',  ( 4.804656715581928417, 70.00525152650509142, 37.80205776086838654 ) ) ;
#30326 = EDGE_CURVE ( 'NONE', #76187, #36750, #11867, .T. ) ;
#30327 = LINE ( 'NONE', #42577, #34725 ) ;
#30328 = DIRECTION ( 'NONE',  ( 0.000000000000000000, 0.000000000000000000, 1.000000000000000000 ) ) ;
#30329 = CARTESIAN_POINT ( 'NONE',  ( 100.8863495415024119, -28.40209871822978371, 35.59657765686397113 ) ) ;
#30331 = CARTESIAN_POINT ( 'NONE',  ( 108.6454077996538246, -25.81962716842098970, 145.9737205140069420 ) ) ;
#30330 = CARTESIAN_POINT ( 'NONE',  ( 0.000000000000000000, 127.0000000000000000, -110.3312500000000114 ) ) ;
#30332 = FACE_OUTER_BOUND ( 'NONE', #54845, .T. ) ;
#30333 = CARTESIAN_POINT ( 'NONE',  ( -50.03799999999999670, 20.32000000000000028, 206.3750000000000000 ) ) ;
#30334 = ORIENTED_EDGE ( 'NONE', *, *, #28781, .F. ) ;
#30335 = CIRCLE ( 'NONE', #49163, 6.350000000000659561 ) ;
#30336 = CARTESIAN_POINT ( 'NONE',  ( 31.75000000000000000, 124.5870000000000033, 3.174999999999999822 ) ) ;
#30337 = DIRECTION ( 'NONE',  ( 1.000000000000000000, 0.000000000000000000, 0.000000000000000000 ) ) ;
#30338 = PLANE ( 'NONE',  #80686 ) ;
#30339 = EDGE_CURVE ( 'NONE', #66654, #76607, #55366, .T. ) ;
#30340 = DIRECTION ( 'NONE',  ( -1.000000000000000000, 0.000000000000000000, 0.000000000000000000 ) ) ;
#30342 = ORIENTED_EDGE ( 'NONE', *, *, #31926, .T. ) ;
#30341 = CARTESIAN_POINT ( 'NONE',  ( 110.0646822317013118, -26.04189894992025955, 219.8708633711489711 ) ) ;
#30343 = PLANE ( 'NONE',  #72703 ) ;
#30344 = CARTESIAN_POINT ( 'NONE',  ( 115.7943364950945977, -30.98820711043258669, 250.2899109901966028 ) ) ;
#30345 = CARTESIAN_POINT ( 'NONE',  ( 102.5393486652204160, -27.29027178147674348, 91.43276813305395478 ) ) ;
#30346 = CARTESIAN_POINT ( 'NONE',  ( 83.22961976134631357, 79.25971567868505474, 100.5868491334651225 ) ) ;
#30347 = CARTESIAN_POINT ( 'NONE',  ( 113.2430583326422493, -28.75680677547383723, 190.5522713588539148 ) ) ;
#30349 = ADVANCED_FACE ( 'NONE', ( #74166 ), #65993, .F. ) ;
#30348 = VECTOR ( 'NONE', #46989, 1000.000000000000000 ) ;
#30350 = LINE ( 'NONE', #23109, #33630 ) ;
#30351 = VERTEX_POINT ( 'NONE', #66442 ) ;
#30352 = EDGE_LOOP ( 'NONE', ( #21350, #53792, #28973, #28454 ) ) ;
#30353 = ORIENTED_EDGE ( 'NONE', *, *, #36171, .F. ) ;
#30354 = VERTEX_POINT ( 'NONE', #45531 ) ;
#30355 = DIRECTION ( 'NONE',  ( -2.170915417798913418E-16, 0.000000000000000000, -1.000000000000000000 ) ) ;
#30356 = CARTESIAN_POINT ( 'NONE',  ( 118.1075207852818068, -36.21034067742461815, 264.8518157521014587 ) ) ;
#30357 = CARTESIAN_POINT ( 'NONE',  ( 107.0667039024470313, -104.2784471599420897, -20.48315503890502143 ) ) ;
#30358 = DIRECTION ( 'NONE',  ( 0.4999999999999915623, -0.8660254037844433705, 0.000000000000000000 ) ) ;
#30359 = EDGE_CURVE ( 'NONE', #7162, #67833, #4229, .T. ) ;
#30360 = AXIS2_PLACEMENT_3D ( 'NONE', #43614, #37724, #51765 ) ;
#30363 = EDGE_CURVE ( 'NONE', #88034, #34414, #10591, .T. ) ;
#30362 = CARTESIAN_POINT ( 'NONE',  ( 87.20837788851326877, 70.80054595721396993, 80.31601367611443720 ) ) ;
#30361 = CARTESIAN_POINT ( 'NONE',  ( 1.387778780781445676E-14, 239.0000000000000000, 97.27542076772557778 ) ) ;
#30364 = FACE_OUTER_BOUND ( 'NONE', #74019, .T. ) ;
#30365 = CARTESIAN_POINT ( 'NONE',  ( 107.5482541545970605, -45.77270802984816811, 197.0533722090289643 ) ) ;
#30366 = VERTEX_POINT ( 'NONE', #31473 ) ;
#30367 = VERTEX_POINT ( 'NONE', #31922 ) ;
#30368 = VECTOR ( 'NONE', #20758, 1000.000000000000000 ) ;
#30370 = ORIENTED_EDGE ( 'NONE', *, *, #32590, .F. ) ;
#30369 = CIRCLE ( 'NONE', #49206, 3.000000000000002665 ) ;
#30371 = CARTESIAN_POINT ( 'NONE',  ( 110.8561819789184284, -45.98353734325511510, 182.8857722960176204 ) ) ;
#30372 = CARTESIAN_POINT ( 'NONE',  ( 106.2788006184939888, -47.06957971430141185, 263.5280062282914741 ) ) ;
#30373 = CARTESIAN_POINT ( 'NONE',  ( 147.0667039024470171, -104.2784471599409102, 234.7178068554179902 ) ) ;
#30374 =( GEOMETRIC_REPRESENTATION_CONTEXT ( 3 ) GLOBAL_UNCERTAINTY_ASSIGNED_CONTEXT ( ( #37815 ) ) GLOBAL_UNIT_ASSIGNED_CONTEXT ( ( #41919, #57347, #14694 ) ) REPRESENTATION_CONTEXT ( 'NONE', 'WORKASPACE' ) );
#30375 = CARTESIAN_POINT ( 'NONE',  ( 109.6422150510572635, -46.48028739024776002, 27.78139385761759428 ) ) ;
#30376 = ORIENTED_EDGE ( 'NONE', *, *, #1151, .T. ) ;
#30377 = CARTESIAN_POINT ( 'NONE',  ( 77.52387074035010528, -35.68172011937328136, 2.822018711113899236 ) ) ;
#30378 = VERTEX_POINT ( 'NONE', #27235 ) ;
#30379 = CARTESIAN_POINT ( 'NONE',  ( 168.0371591254543944, -48.62818131005519007, 237.4678068554150059 ) ) ;
#30380 = CARTESIAN_POINT ( 'NONE',  ( 98.69396380956492010, -33.82637249272325164, 282.4930118773256709 ) ) ;
#30381 = EDGE_CURVE ( 'NONE', #5511, #1241, #20436, .T. ) ;
#30382 = DIRECTION ( 'NONE',  ( 1.000000000000000078E-15, -1.000000000000000083E-30, -1.000000000000000000 ) ) ;
#30383 = DIRECTION ( 'NONE',  ( -4.299999999999999979E-14, 1.000000000000000000, -4.400000000000000367E-29 ) ) ;
#30384 = AXIS2_PLACEMENT_3D ( 'NONE', #75788, #88969, #64841 ) ;
#30385 = FACE_OUTER_BOUND ( 'NONE', #17307, .T. ) ;
#30386 = ORIENTED_EDGE ( 'NONE', *, *, #19350, .F. ) ;
#30387 = DIRECTION ( 'NONE',  ( 1.000000000000000078E-15, -1.000000000000000083E-30, -1.000000000000000000 ) ) ;
#30388 = CARTESIAN_POINT ( 'NONE',  ( 51.06648329127400388, -18.82844715994099971, 333.4006252759120343 ) ) ;
#30389 = ORIENTED_EDGE ( 'NONE', *, *, #17702, .T. ) ;
#30390 = CARTESIAN_POINT ( 'NONE',  ( 107.3210346550871179, -25.67891364084480799, 75.04610146638695767 ) ) ;
#30391 = EDGE_LOOP ( 'NONE', ( #86802, #13236, #10624, #50881, #19517, #27197, #58468, #56942, #74406, #58859, #61343, #52768, #51702, #34279, #75484, #60220, #27345, #39456, #46114, #68164, #7842, #39424, #18555, #15892, #3454, #30500, #22069, #6445, #3714, #15569, #28029, #50427, #69176, #59504, #16414, #16177, #37101, #50635, #36506, #62082, #16350, #82916, #71512, #2395, #74730, #43568, #39715, #24213, #57478 ) ) ;
#30392 = CARTESIAN_POINT ( 'NONE',  ( 98.68252487213293023, -38.50746385042646125, 30.91527697093399141 ) ) ;
#30393 = CARTESIAN_POINT ( 'NONE',  ( 107.5667039024470171, -94.77844715994137914, 2.217806855417697953 ) ) ;
#30394 = CARTESIAN_POINT ( 'NONE',  ( 115.8258230018156354, -33.33084548093709287, 90.54063092494496345 ) ) ;
#30395 = LINE ( 'NONE', #2252, #50586 ) ;
#30396 = CARTESIAN_POINT ( 'NONE',  ( 172.5664832912729878, -18.82844715994071194, 15.92562527591207022 ) ) ;
#30397 = CARTESIAN_POINT ( 'NONE',  ( 117.0667039024470313, -98.59953881414062948, 19.21780685541782319 ) ) ;
#30399 = EDGE_CURVE ( 'NONE', #43566, #4960, #59618, .T. ) ;
#30398 = VECTOR ( 'NONE', #4684, 1000.000000000000000 ) ;
#30400 = CARTESIAN_POINT ( 'NONE',  ( 106.2234015700748699, -47.79681864418333959, 263.5280062282922131 ) ) ;
#30401 = CYLINDRICAL_SURFACE ( 'NONE', #1895, 12.70000000000000107 ) ;
#30402 = ORIENTED_EDGE ( 'NONE', *, *, #38046, .F. ) ;
#30403 = FACE_OUTER_BOUND ( 'NONE', #30591, .T. ) ;
#30404 = ORIENTED_EDGE ( 'NONE', *, *, #70513, .F. ) ;
#30405 = CARTESIAN_POINT ( 'NONE',  ( 117.6248412043677121, -33.30620651169719082, 130.0880062282919880 ) ) ;
#30406 = CARTESIAN_POINT ( 'NONE',  ( 79.11888855177762991, -21.31186128672829128, 1.764000668898225044 ) ) ;
#30407 = ORIENTED_EDGE ( 'NONE', *, *, #45198, .T. ) ;
#30409 = EDGE_CURVE ( 'NONE', #33706, #65644, #58284, .T. ) ;
#30408 = ORIENTED_EDGE ( 'NONE', *, *, #52309, .F. ) ;
#30410 = EDGE_CURVE ( 'NONE', #17392, #59373, #11494, .T. ) ;
#30412 = VECTOR ( 'NONE', #62762, 1000.000000000000000 ) ;
#30411 = DIRECTION ( 'NONE',  ( 1.000000000000000078E-15, -1.000000000000000083E-30, -1.000000000000000000 ) ) ;
#30413 = EDGE_CURVE ( 'NONE', #11261, #88962, #52410, .T. ) ;
#30414 = DIRECTION ( 'NONE',  ( 1.071939472051879986E-15, 0.000000000000000000, 1.000000000000000000 ) ) ;
#30415 = CARTESIAN_POINT ( 'NONE',  ( 116.5663773505005310, -40.88766770462213884, 208.4861014663879644 ) ) ;
#30416 = CARTESIAN_POINT ( 'NONE',  ( 172.5664832912740110, -36.32844715994070839, 138.9256252759119832 ) ) ;
#30417 = DIRECTION ( 'NONE',  ( 0.000000000000000000, -1.000000000000000000, 0.000000000000000000 ) ) ;
#30418 = DIRECTION ( 'NONE',  ( 0.000000000000000000, -1.000000000000000000, 0.000000000000000000 ) ) ;
#30419 = CARTESIAN_POINT ( 'NONE',  ( 96.65901483881968659, -33.00673566691533978, 22.06514908543494258 ) ) ;
#30420 = DIRECTION ( 'NONE',  ( 1.000000000000000000, 0.000000000000000000, 0.000000000000000000 ) ) ;
#30421 = ORIENTED_EDGE ( 'NONE', *, *, #54154, .T. ) ;
#30422 = CARTESIAN_POINT ( 'NONE',  ( 115.7815775597082109, -31.78852007784938039, 170.2368360151835702 ) ) ;
#30423 = AXIS2_PLACEMENT_3D ( 'NONE', #59262, #16608, #58376 ) ;
#30424 = CARTESIAN_POINT ( 'NONE',  ( 163.0667039024469034, -32.29483332967940612, 117.4678068554150485 ) ) ;
#30425 = VERTEX_POINT ( 'NONE', #87794 ) ;
#30426 = VECTOR ( 'NONE', #75791, 1000.000000000000000 ) ;
#30427 = AXIS2_PLACEMENT_3D ( 'NONE', #10179, #36995, #64701 ) ;
#30428 = EDGE_CURVE ( 'NONE', #44647, #59006, #68411, .T. ) ;
#30429 = CARTESIAN_POINT ( 'NONE',  ( 81.20961857873741963, -21.23068377182416455, 1.829869271363169458 ) ) ;
#30430 = CARTESIAN_POINT ( 'NONE',  ( 180.1667039024460166, -26.71338133339240528, -5.074374724088000832 ) ) ;
#30431 = CARTESIAN_POINT ( 'NONE',  ( 99.76842024043810397, -29.31547782932919688, 225.6956252759109702 ) ) ;
#30432 = CARTESIAN_POINT ( 'NONE',  ( -215.9000000000000057, 3.174999999999999822, -41.27499999999999858 ) ) ;
#30433 = FACE_BOUND ( 'NONE', #20400, .T. ) ;
#30434 = CARTESIAN_POINT ( 'NONE',  ( 63.06670390244641311, -24.92844715994017335, 180.4678068554151196 ) ) ;
#30435 = EDGE_CURVE ( 'NONE', #34288, #48773, #7254, .T. ) ;
#30436 = CARTESIAN_POINT ( 'NONE',  ( 104.8198721574821803, -27.95645401395800533, 244.7105150661719790 ) ) ;
#30438 = CARTESIAN_POINT ( 'NONE',  ( 103.4847015977353379, -25.45917443855082496, 51.32133956162493149 ) ) ;
#30437 = DIRECTION ( 'NONE',  ( 0.000000000000000000, -1.000000000000000000, 0.000000000000000000 ) ) ;
#30439 = CARTESIAN_POINT ( 'NONE',  ( 0.000000000000000000, 101.5999999999999943, 0.000000000000000000 ) ) ;
#30440 = CARTESIAN_POINT ( 'NONE',  ( 108.2818241440822788, -26.29514120620494921, 129.9841967044819739 ) ) ;
#30441 = ORIENTED_EDGE ( 'NONE', *, *, #41022, .T. ) ;
#30442 = CARTESIAN_POINT ( 'NONE',  ( 131.8668787344577424, -20.38871026387126051, 7.389079501607389133 ) ) ;
#30443 = ORIENTED_EDGE ( 'NONE', *, *, #33326, .F. ) ;
#30444 = AXIS2_PLACEMENT_3D ( 'NONE', #58756, #79691, #88292 ) ;
#30445 = CARTESIAN_POINT ( 'NONE',  ( 107.0664832912739968, -36.72944715994100306, -1.864374724089012947 ) ) ;
#30446 = CARTESIAN_POINT ( 'NONE',  ( 103.7389900727278729, -27.29752428252023577, 276.3463639899791815 ) ) ;
#30447 = VERTEX_POINT ( 'NONE', #49905 ) ;
#30448 = ADVANCED_FACE ( 'NONE', ( #9052 ), #63094, .F. ) ;
#30449 = CARTESIAN_POINT ( 'NONE',  ( 62.03715912545833078, -47.82818131006021645, 313.9678068554150059 ) ) ;
#30450 = ORIENTED_EDGE ( 'NONE', *, *, #29747, .T. ) ;
#30451 = CARTESIAN_POINT ( 'NONE',  ( 130.5667039024479834, -36.72944715994093912, 239.5838068554170377 ) ) ;
#30452 = AXIS2_PLACEMENT_3D ( 'NONE', #88847, #10847, #24493 ) ;
#30453 = FACE_OUTER_BOUND ( 'NONE', #69610, .T. ) ;
#30454 = CARTESIAN_POINT ( 'NONE',  ( 116.3259296754763028, -32.93870509136930025, 260.1356252759109680 ) ) ;
#30455 = ORIENTED_EDGE ( 'NONE', *, *, #769, .F. ) ;
#30456 = CARTESIAN_POINT ( 'NONE',  ( 116.6952228212742995, -32.58508497927773817, 79.14991099019697174 ) ) ;
#30457 = LINE ( 'NONE', #58155, #56462 ) ;
#30458 = FACE_OUTER_BOUND ( 'NONE', #21155, .T. ) ;
#30459 = CARTESIAN_POINT ( 'NONE',  ( 108.3334480745109545, -46.73485935675521574, 142.6772919409591509 ) ) ;
#30460 = VERTEX_POINT ( 'NONE', #15421 ) ;
#30461 = AXIS2_PLACEMENT_3D ( 'NONE', #71119, #2068, #85205 ) ;
#30462 = DIRECTION ( 'NONE',  ( 8.673617379884035472E-16, 1.000000000000000000, 0.000000000000000000 ) ) ;
#30463 = DIRECTION ( 'NONE',  ( 0.000000000000000000, 0.000000000000000000, -1.000000000000000000 ) ) ;
#30464 = FACE_OUTER_BOUND ( 'NONE', #39997, .T. ) ;
#30467 = EDGE_CURVE ( 'NONE', #57201, #70164, #1018, .T. ) ;
#30466 = CARTESIAN_POINT ( 'NONE',  ( 67.06670390244707392, -137.6784471599409869, 245.4361138696909848 ) ) ;
#30465 = CARTESIAN_POINT ( 'NONE',  ( 184.5667039024480118, -67.87844715994100397, 300.9178068554150514 ) ) ;
#30468 = CARTESIAN_POINT ( 'NONE',  ( 25.56670390244797275, -62.87844715994099687, 254.4678068554150343 ) ) ;
#30469 = AXIS2_PLACEMENT_3D ( 'NONE', #47226, #53579, #53123 ) ;
#30470 = ORIENTED_EDGE ( 'NONE', *, *, #75755, .T. ) ;
#30471 = PLANE ( 'NONE',  #88276 ) ;
#30472 = CARTESIAN_POINT ( 'NONE',  ( 113.8941270090216733, -29.67983328691853018, 170.4641967044819637 ) ) ;
#30474 = EDGE_LOOP ( 'NONE', ( #35998, #77619, #38485, #84830 ) ) ;
#30473 = LINE ( 'NONE', #72708, #66025 ) ;
#30475 = AXIS2_PLACEMENT_3D ( 'NONE', #8606, #23142, #72167 ) ;
#30476 = CARTESIAN_POINT ( 'NONE',  ( 105.4283309587863613, -27.08694620864308789, 11.20991099019597037 ) ) ;
#30477 = LINE ( 'NONE', #57270, #35290 ) ;
#30478 = DIRECTION ( 'NONE',  ( 0.000000000000000000, 0.000000000000000000, 1.000000000000000000 ) ) ;
#30479 = CARTESIAN_POINT ( 'NONE',  ( 167.2371591254542693, -47.82818131005522844, 300.4678068554149490 ) ) ;
#30480 = AXIS2_PLACEMENT_3D ( 'NONE', #49992, #63190, #7781 ) ;
#30481 = ORIENTED_EDGE ( 'NONE', *, *, #69276, .T. ) ;
#30482 = ADVANCED_FACE ( 'NONE', ( #20876 ), #7694, .F. ) ;
#30483 = DIRECTION ( 'NONE',  ( 0.000000000000000000, 0.000000000000000000, 1.000000000000000000 ) ) ;
#30484 = CARTESIAN_POINT ( 'NONE',  ( 114.8736367985563334, -30.83777597042981711, 219.3413395616259720 ) ) ;
#30485 = ORIENTED_EDGE ( 'NONE', *, *, #27404, .T. ) ;
#30486 = ORIENTED_EDGE ( 'NONE', *, *, #55213, .F. ) ;
#30487 = CARTESIAN_POINT ( 'NONE',  ( 115.3361691346596558, -39.99662111280561305, 189.9587261630399553 ) ) ;
#30488 = AXIS2_PLACEMENT_3D ( 'NONE', #14232, #35101, #76904 ) ;
#30489 = EDGE_CURVE ( 'NONE', #28975, #22460, #10442, .T. ) ;
#30490 = CARTESIAN_POINT ( 'NONE',  ( 182.3467384525650061, -29.62846900982231446, -5.074374724088000832 ) ) ;
#30491 = CARTESIAN_POINT ( 'NONE',  ( 106.6003420031022415, -27.34545878416701115, 41.55967854399195005 ) ) ;
#30492 = CARTESIAN_POINT ( 'NONE',  ( -100.8594679592212486, 82.96445444011520465, 82.89895571708262878 ) ) ;
#30493 = DIRECTION ( 'NONE',  ( 0.000000000000000000, 0.000000000000000000, -1.000000000000000000 ) ) ;
#30494 = CARTESIAN_POINT ( 'NONE',  ( 88.17226027475679473, -58.72944715994100306, 239.5838068554174924 ) ) ;
#30495 = ORIENTED_EDGE ( 'NONE', *, *, #89050, .F. ) ;
#30496 = CARTESIAN_POINT ( 'NONE',  ( 62.03715912545828814, -47.82818131006021645, 249.9678068554150343 ) ) ;
#30497 = CARTESIAN_POINT ( 'NONE',  ( 48.86082318535700608, -35.55794170701751256, -5.074374724088000832 ) ) ;
#30498 = CARTESIAN_POINT ( 'NONE',  ( 96.29057984255072711, -34.37493501460198075, 256.1432443235300980 ) ) ;
#30499 = PLANE ( 'NONE',  #18439 ) ;
#30500 = ORIENTED_EDGE ( 'NONE', *, *, #43224, .F. ) ;
#30501 = SURFACE_STYLE_FILL_AREA ( #3685 ) ;
#30502 = DIRECTION ( 'NONE',  ( 1.000000000000000078E-15, -1.000000000000000000, 0.000000000000000000 ) ) ;
#30503 = CIRCLE ( 'NONE', #79867, 5.599999999999994316 ) ;
#30504 = CYLINDRICAL_SURFACE ( 'NONE', #31613, 2.030000000001807248 ) ;
#30505 = CARTESIAN_POINT ( 'NONE',  ( 134.0664832912739826, -8.729447159941003065, 4.925625275910997303 ) ) ;
#30506 = CARTESIAN_POINT ( 'NONE',  ( 115.0831197249979851, -29.02584261466837390, 35.43562527591098643 ) ) ;
#30507 = CARTESIAN_POINT ( 'NONE',  ( 1.652234655685276277, 70.03180882406793728, 118.3472113678285638 ) ) ;
#30508 = ORIENTED_EDGE ( 'NONE', *, *, #50935, .F. ) ;
#30509 = CARTESIAN_POINT ( 'NONE',  ( 101.9391980234526187, -27.60234874203171884, 56.48419670448296159 ) ) ;
#30510 = LINE ( 'NONE', #16438, #35174 ) ;
#30511 = CARTESIAN_POINT ( 'NONE',  ( 114.4151681834755294, -27.43228005255051016, 274.5441967044824878 ) ) ;
#30513 = ORIENTED_EDGE ( 'NONE', *, *, #26841, .T. ) ;
#30512 = EDGE_CURVE ( 'NONE', #64107, #13859, #45756, .T. ) ;
#30514 = AXIS2_PLACEMENT_3D ( 'NONE', #69736, #54724, #70632 ) ;
#30515 = ADVANCED_FACE ( 'NONE', ( #58950 ), #86238, .T. ) ;
#30516 = CARTESIAN_POINT ( 'NONE',  ( 41.56648329127398966, -18.82844715994071194, 138.9256252759119832 ) ) ;
#30517 = CARTESIAN_POINT ( 'NONE',  ( 53.56670390244743629, -48.82844715994058049, 180.4678068554151196 ) ) ;
#30518 = CYLINDRICAL_SURFACE ( 'NONE', #74094, 9.999999999999998224 ) ;
#30519 = CARTESIAN_POINT ( 'NONE',  ( 112.9396172237807860, -42.43812354398048114, 96.03094751244795191 ) ) ;
#30520 = CARTESIAN_POINT ( 'NONE',  ( 116.8155376854491720, -40.58108761943747567, 189.5270538473389479 ) ) ;
#30521 = CYLINDRICAL_SURFACE ( 'NONE', #67310, 3.000000864267343026 ) ;
#30522 = DIRECTION ( 'NONE',  ( 0.000000000000000000, 0.000000000000000000, 1.000000000000000000 ) ) ;
#30523 = VERTEX_POINT ( 'NONE', #65342 ) ;
#30524 = EDGE_CURVE ( 'NONE', #74810, #40280, #87135, .T. ) ;
#30525 = DIRECTION ( 'NONE',  ( -9.868649107779159826E-16, 0.000000000000000000, 1.000000000000000000 ) ) ;
#30526 = AXIS2_PLACEMENT_3D ( 'NONE', #43095, #70839, #78105 ) ;
#30527 = EDGE_LOOP ( 'NONE', ( #44788, #6841, #35268, #35772, #47034, #8429, #89484, #15633, #82719, #23344, #13321, #19750 ) ) ;
#30528 = ORIENTED_EDGE ( 'NONE', *, *, #75951, .T. ) ;
#30529 = ADVANCED_FACE ( 'NONE', ( #52126 ), #32148, .F. ) ;
#30530 = FACE_OUTER_BOUND ( 'NONE', #55712, .T. ) ;
#30531 = EDGE_LOOP ( 'NONE', ( #56476, #4043, #86079, #46963 ) ) ;
#30532 = VERTEX_POINT ( 'NONE', #86687 ) ;
#30533 = DIRECTION ( 'NONE',  ( 3.100000000000000258E-29, -3.100000000000000044E-14, -1.000000000000000000 ) ) ;
#30534 = CARTESIAN_POINT ( 'NONE',  ( 103.2798274406795116, -27.47411150201141439, 41.38551241025358962 ) ) ;
#30535 = EDGE_CURVE ( 'NONE', #8142, #32905, #18071, .T. ) ;
#30536 = CARTESIAN_POINT ( 'NONE',  ( 98.02237212078092909, -37.19498283172546849, 120.8019436376009708 ) ) ;
#30537 = CARTESIAN_POINT ( 'NONE',  ( 117.5135424720979103, -36.80237478700602338, 263.8213395616250523 ) ) ;
#30538 = AXIS2_PLACEMENT_3D ( 'NONE', #35171, #49700, #29277 ) ;
#30539 = CARTESIAN_POINT ( 'NONE',  ( 107.0664832912739399, -36.72944715994095333, 247.7440089327910755 ) ) ;
#30540 = VERTEX_POINT ( 'NONE', #38963 ) ;
#30541 = AXIS2_PLACEMENT_3D ( 'NONE', #21419, #70013, #1426 ) ;
#30542 = CARTESIAN_POINT ( 'NONE',  ( 97.06383274664968042, -37.34207438287794645, 137.3751712589593126 ) ) ;
#30543 = VERTEX_POINT ( 'NONE', #16308 ) ;
#30544 = CARTESIAN_POINT ( 'NONE',  ( 173.9900000000000091, 14.32000000000000028, -71.37400000000000944 ) ) ;
#30545 = DIRECTION ( 'NONE',  ( -0.7071067811875165754, -0.7071067811855784591, -7.071067811875470201E-16 ) ) ;
#30546 = CARTESIAN_POINT ( 'NONE',  ( 102.7778427608900955, -89.25462229453661678, -11.78219314458248057 ) ) ;
#30547 = CIRCLE ( 'NONE', #52231, 3.999999999999992895 ) ;
#30548 = DIRECTION ( 'NONE',  ( -2.999999999999999839E-15, 1.000000000000000000, -2.999999999999999900E-30 ) ) ;
#30549 = VERTEX_POINT ( 'NONE', #38513 ) ;
#30550 = UNCERTAINTY_MEASURE_WITH_UNIT (LENGTH_MEASURE( 1.000000000000000082E-05 ), #31626, 'distance_accuracy_value', 'NONE');
#30551 = CARTESIAN_POINT ( 'NONE',  ( 117.4908834113230682, -35.85893649831510999, 253.8927681330538348 ) ) ;
#30552 = CARTESIAN_POINT ( 'NONE',  ( 115.6469432611725665, -28.48403513818922761, 35.43562527591098643 ) ) ;
#30553 = SHAPE_REPRESENTATION_RELATIONSHIP ( 'NONE' , 'NONE' ,  #47290, #60825 ) ;
#30554 = FACE_OUTER_BOUND ( 'NONE', #32265, .T. ) ;
#30556 = FACE_OUTER_BOUND ( 'NONE', #71589, .T. ) ;
#30555 = DIRECTION ( 'NONE',  ( 5.512527431108029424E-15, -1.000000000000000000, 0.000000000000000000 ) ) ;
#30557 = CARTESIAN_POINT ( 'NONE',  ( 152.0368932755770288, -23.42844715993588522, 313.9678068554149490 ) ) ;
#30558 = LINE ( 'NONE', #79173, #9105 ) ;
#30559 = CARTESIAN_POINT ( 'NONE',  ( 131.7606268095730684, -38.22815166920154439, 7.286367513305490817 ) ) ;
#30560 = AXIS2_PLACEMENT_3D ( 'NONE', #10519, #16899, #44578 ) ;
#30561 = CARTESIAN_POINT ( 'NONE',  ( 112.1393456294539419, -28.01282277365494977, 10.65645861034278852 ) ) ;
#30562 = CARTESIAN_POINT ( 'NONE',  ( 105.7157591367752758, -46.72390112185112088, 162.4687997112716289 ) ) ;
#30563 = CARTESIAN_POINT ( 'NONE',  ( 116.3212776292293995, -32.94146857471267253, 120.1356252759109537 ) ) ;
#30564 = CARTESIAN_POINT ( 'NONE',  ( 96.86726761138238828, -30.64586122335317953, 280.8984824187682534 ) ) ;
#30565 = CARTESIAN_POINT ( 'NONE',  ( 112.4860951546057919, -26.19083136796355404, 165.6984824187679521 ) ) ;
#30566 = CARTESIAN_POINT ( 'NONE',  ( 99.27755186283980038, -43.74455535675208040, 52.90991099019698396 ) ) ;
#30569 = EDGE_CURVE ( 'NONE', #13373, #51663, #79888, .T. ) ;
#30568 = DIRECTION ( 'NONE',  ( -4.237773401492740281E-14, 1.000000000000000000, 0.000000000000000000 ) ) ;
#30567 = PLANE ( 'NONE',  #72567 ) ;
#30570 = CARTESIAN_POINT ( 'NONE',  ( 82.81644824798257787, -36.55833207211471603, 3.101428811465905433 ) ) ;
#30571 = ADVANCED_FACE ( 'NONE', ( #78984 ), #17642, .F. ) ;
#30572 = ORIENTED_EDGE ( 'NONE', *, *, #42633, .T. ) ;
#30573 = DIRECTION ( 'NONE',  ( -0.2588190451025281225, 0.000000000000000000, 0.9659258262890663138 ) ) ;
#30574 = VERTEX_POINT ( 'NONE', #50815 ) ;
#30575 = AXIS2_PLACEMENT_3D ( 'NONE', #36890, #30525, #65044 ) ;
#30576 = CARTESIAN_POINT ( 'NONE',  ( 114.5308976578478166, -43.10096916487045604, 59.26419670448196086 ) ) ;
#30578 = ORIENTED_EDGE ( 'NONE', *, *, #20866, .T. ) ;
#30577 = FACE_OUTER_BOUND ( 'NONE', #66701, .T. ) ;
#30579 = VECTOR ( 'NONE', #46961, 1000.000000000000000 ) ;
#30580 = CARTESIAN_POINT ( 'NONE',  ( 97.81169418859235520, -40.51741816698509524, 47.63568902202231925 ) ) ;
#30581 = CARTESIAN_POINT ( 'NONE',  ( 97.07914014679033698, -41.41098531455288168, 207.6632443235299661 ) ) ;
#30582 = DIRECTION ( 'NONE',  ( 0.000000000000000000, 0.000000000000000000, -1.000000000000000000 ) ) ;
#30583 = LINE ( 'NONE', #78758, #37090 ) ;
#30584 = DIRECTION ( 'NONE',  ( 0.000000000000000000, -1.000000000000000000, 0.000000000000000000 ) ) ;
#30585 = CARTESIAN_POINT ( 'NONE',  ( 97.07207205650352932, -35.37844121661813546, 47.21895861061143052 ) ) ;
#30586 = PLANE ( 'NONE',  #89743 ) ;
#30587 = CARTESIAN_POINT ( 'NONE',  ( 97.81201254632964037, -40.51821635194160365, 96.63569287326528467 ) ) ;
#30588 = CARTESIAN_POINT ( 'NONE',  ( 116.2961327041338535, -39.96626766897450977, 133.5584824187689605 ) ) ;
#30589 = ORIENTED_EDGE ( 'NONE', *, *, #81091, .T. ) ;
#30590 = CIRCLE ( 'NONE', #48002, 1.000000000000000888 ) ;
#30591 = EDGE_LOOP ( 'NONE', ( #85701, #14656, #56131, #69960 ) ) ;
#30592 = CARTESIAN_POINT ( 'NONE',  ( 103.9179606659962616, -45.58175368509670733, 98.74824997256392578 ) ) ;
#30593 = CIRCLE ( 'NONE', #3039, 218.1859999999999786 ) ;
#30594 = EDGE_CURVE ( 'NONE', #85915, #23208, #73037, .T. ) ;
#30595 = FACE_OUTER_BOUND ( 'NONE', #7651, .T. ) ;
#30597 = FACE_OUTER_BOUND ( 'NONE', #49878, .T. ) ;
#30596 = CARTESIAN_POINT ( 'NONE',  ( 117.1144258088630039, -31.97015794161414703, 210.1784824187679703 ) ) ;
#30598 = FACE_OUTER_BOUND ( 'NONE', #31869, .T. ) ;
#30599 = FACE_BOUND ( 'NONE', #85532, .T. ) ;
#30600 = CARTESIAN_POINT ( 'NONE',  ( 118.2598914205052552, 72.98405218941671535, -8.394510633989694881 ) ) ;
#30601 = CARTESIAN_POINT ( 'NONE',  ( 145.2166182285888851, -69.56242951228074389, 247.5001056298889921 ) ) ;
#30602 = DIRECTION ( 'NONE',  ( 0.000000000000000000, 0.000000000000000000, 1.000000000000000000 ) ) ;
#30603 = PLANE ( 'NONE',  #6691 ) ;
#30604 = CARTESIAN_POINT ( 'NONE',  ( 103.0581626738561880, -26.45339789934162411, 170.3603871806729444 ) ) ;
#30605 = ORIENTED_EDGE ( 'NONE', *, *, #10224, .T. ) ;
#30606 = VECTOR ( 'NONE', #647, 1000.000000000000000 ) ;
#30607 = ORIENTED_EDGE ( 'NONE', *, *, #86456, .F. ) ;
#30608 = AXIS2_PLACEMENT_3D ( 'NONE', #79412, #87107, #23992 ) ;
#30609 = DIRECTION ( 'NONE',  ( 0.000000000000000000, -1.000000000000000000, 0.000000000000000000 ) ) ;
#30610 = CARTESIAN_POINT ( 'NONE',  ( 146.6569661690436703, -68.27214332003397601, 246.7106591300727416 ) ) ;
#30611 = DIRECTION ( 'NONE',  ( 0.000000000000000000, -1.000000000000000000, 0.000000000000000000 ) ) ;
#30612 = DIRECTION ( 'NONE',  ( -4.237773401492740281E-14, 1.000000000000000000, 0.000000000000000000 ) ) ;
#30613 = CARTESIAN_POINT ( 'NONE',  ( 109.4041143893713297, -28.39659615353044231, 217.6890427505439902 ) ) ;
#30614 = AXIS2_PLACEMENT_3D ( 'NONE', #86200, #66176, #31214 ) ;
#30615 = CARTESIAN_POINT ( 'NONE',  ( 41.56648329127398966, -27.57844715994070484, 15.92562527591200094 ) ) ;
#30616 = CARTESIAN_POINT ( 'NONE',  ( 109.8560245667294311, -26.68427469084152293, 174.8613395616249591 ) ) ;
#30617 = CYLINDRICAL_SURFACE ( 'NONE', #48885, 2.117000000000000881 ) ;
#30618 = EDGE_LOOP ( 'NONE', ( #85726, #46992 ) ) ;
#30621 = ORIENTED_EDGE ( 'NONE', *, *, #34710, .T. ) ;
#30620 = ORIENTED_EDGE ( 'NONE', *, *, #25206, .T. ) ;
#30619 = EDGE_CURVE ( 'NONE', #87954, #43612, #79438, .T. ) ;
#30622 = VECTOR ( 'NONE', #70296, 1000.000000000000000 ) ;
#30623 = CARTESIAN_POINT ( 'NONE',  ( -2.884119045937113768, 70.17489121805367347, 118.5216098345816960 ) ) ;
#30624 = PLANE ( 'NONE',  #15911 ) ;
#30625 = EDGE_CURVE ( 'NONE', #74189, #89290, #14801, .T. ) ;
#30626 = DIRECTION ( 'NONE',  ( 0.000000000000000000, 0.000000000000000000, -1.000000000000000000 ) ) ;
#30627 = VECTOR ( 'NONE', #53515, 1000.000000000000000 ) ;
#30628 = CARTESIAN_POINT ( 'NONE',  ( 99.56565989216673529, -33.50937434423423156, 13.82237608387698558 ) ) ;
#30629 = LINE ( 'NONE', #58327, #78304 ) ;
#30630 = VERTEX_POINT ( 'NONE', #4003 ) ;
#30631 = EDGE_CURVE ( 'NONE', #43486, #52485, #3119, .T. ) ;
#30632 = CARTESIAN_POINT ( 'NONE',  ( 115.2616190319047433, -40.84650019411598976, 9.635625275910943088 ) ) ;
#30633 = CYLINDRICAL_SURFACE ( 'NONE', #31441, 3.250000000000002665 ) ;
#30634 = ORIENTED_EDGE ( 'NONE', *, *, #82134, .F. ) ;
#30635 = VERTEX_POINT ( 'NONE', #31704 ) ;
#30636 = CARTESIAN_POINT ( 'NONE',  ( 115.9332344144704194, -41.42518548927348121, 113.4390407645330185 ) ) ;
#30637 = EDGE_LOOP ( 'NONE', ( #53789, #21667, #12885, #3541, #37514 ) ) ;
#30638 = ORIENTED_EDGE ( 'NONE', *, *, #70515, .F. ) ;
#30639 = ADVANCED_FACE ( 'NONE', ( #17201 ), #22001, .T. ) ;
#30640 = CARTESIAN_POINT ( 'NONE',  ( 98.28161005395152472, -38.92874716189901818, 15.95622935188595370 ) ) ;
#30641 = CARTESIAN_POINT ( 'NONE',  ( 96.62784866533952766, -37.15519789137512419, 161.3584824187679487 ) ) ;
#30642 = AXIS2_PLACEMENT_3D ( 'NONE', #79075, #3215, #78193 ) ;
#30643 = CARTESIAN_POINT ( 'NONE',  ( 95.80265872640100611, -40.33145541733363615, 131.5727681330539554 ) ) ;
#30644 = EDGE_CURVE ( 'NONE', #2462, #67095, #72614, .T. ) ;
#30645 = LINE ( 'NONE', #38782, #4649 ) ;
#30646 = CARTESIAN_POINT ( 'NONE',  ( 116.2186307022408727, -41.79497087860992366, 259.4241967044825969 ) ) ;
#30647 = LINE ( 'NONE', #58343, #9379 ) ;
#30648 = DIRECTION ( 'NONE',  ( 0.000000000000000000, 0.000000000000000000, 1.000000000000000000 ) ) ;
#30649 = CARTESIAN_POINT ( 'NONE',  ( -129.9447564289581578, 80.89704698943971550, -12.61967231918767496 ) ) ;
#30650 = ORIENTED_EDGE ( 'NONE', *, *, #33959, .T. ) ;
#30651 = ORIENTED_EDGE ( 'NONE', *, *, #22798, .T. ) ;
#30652 = CIRCLE ( 'NONE', #21917, 7.937500000000000000 ) ;
#30653 = AXIS2_PLACEMENT_3D ( 'NONE', #23067, #70293, #63474 ) ;
#30654 = CARTESIAN_POINT ( 'NONE',  ( 106.9746081534954669, -47.19836424831742505, 187.5699109901969734 ) ) ;
#30655 = ORIENTED_EDGE ( 'NONE', *, *, #71368, .T. ) ;
#30656 = CARTESIAN_POINT ( 'NONE',  ( 108.2778356434855027, -47.71639565607667066, 157.6518157521019532 ) ) ;
#30657 = CARTESIAN_POINT ( 'NONE',  ( 72.96458098368701428, 127.0000000000000000, -72.96458098368670164 ) ) ;
#30658 = DIRECTION ( 'NONE',  ( 3.100000000000000258E-29, -3.100000000000000044E-14, -1.000000000000000000 ) ) ;
#30659 = DIRECTION ( 'NONE',  ( 0.000000000000000000, 0.000000000000000000, -1.000000000000000000 ) ) ;
#30662 = CARTESIAN_POINT ( 'NONE',  ( 106.8369185487093063, -47.13021470646864941, 268.5584824187679374 ) ) ;
#30661 = CARTESIAN_POINT ( 'NONE',  ( 107.0664832912739968, -36.72944715994100306, 287.6356252759109680 ) ) ;
#30660 = CARTESIAN_POINT ( 'NONE',  ( 41.56670390244804025, -42.82844715994103524, 300.4678068554150059 ) ) ;
#30663 = CARTESIAN_POINT ( 'NONE',  ( 85.58420390244799592, -43.72944715994107412, 231.5838068554169524 ) ) ;
#30664 = CARTESIAN_POINT ( 'NONE',  ( 196.2150000000000034, 30.98800000000000310, 44.45000000000000284 ) ) ;
#30665 = CARTESIAN_POINT ( 'NONE',  ( -3.175000000000109956, 104.3431970271541900, 31.75000000000000000 ) ) ;
#30666 = CARTESIAN_POINT ( 'NONE',  ( 67.23038816984393407, -137.5598464125348244, 246.3084021292352759 ) ) ;
#30667 = CARTESIAN_POINT ( 'NONE',  ( 97.81171235735017433, -40.51746255502365557, 257.6350867217079212 ) ) ;
#30668 = FACE_OUTER_BOUND ( 'NONE', #46190, .T. ) ;
#30669 = CIRCLE ( 'NONE', #10373, 2.750000000000002665 ) ;
#30671 = ORIENTED_EDGE ( 'NONE', *, *, #1637, .F. ) ;
#30670 = CARTESIAN_POINT ( 'NONE',  ( 114.3253520721945620, -31.31565170232914497, 195.5838068554167819 ) ) ;
#30672 = CARTESIAN_POINT ( 'NONE',  ( 12.70000000000000107, 82.54999999999999716, 117.8738102209307641 ) ) ;
#30673 = CARTESIAN_POINT ( 'NONE',  ( 118.9025049541195358, -37.70032671045152028, 188.7613395616259595 ) ) ;
#30674 = CARTESIAN_POINT ( 'NONE',  ( 106.9273518165185948, -26.26990724610170247, 56.08705384733997334 ) ) ;
#30675 = CARTESIAN_POINT ( 'NONE',  ( 96.73312529990856490, -40.78150971882554643, 242.6118157521009664 ) ) ;
#30676 = DIRECTION ( 'NONE',  ( 1.000000000000000000, 0.000000000000000000, 0.000000000000000000 ) ) ;
#30677 = DIRECTION ( 'NONE',  ( 0.7071067811864886199, 0.7071067811866064146, 7.071067811864879743E-16 ) ) ;
#30679 = CARTESIAN_POINT ( 'NONE',  ( 116.9190213240937197, -38.53463890124888280, 39.68201433323524441 ) ) ;
#30678 = DIRECTION ( 'NONE',  ( 0.000000000000000000, 0.000000000000000000, -1.000000000000000000 ) ) ;
#30680 = CARTESIAN_POINT ( 'NONE',  ( 167.2371591254542693, -47.82818131005522844, 300.4678068554149490 ) ) ;
#30681 = LINE ( 'NONE', #4320, #74581 ) ;
#30682 = ORIENTED_EDGE ( 'NONE', *, *, #56157, .F. ) ;
#30683 = DIRECTION ( 'NONE',  ( -1.000000000000000000, -3.999999999999999995E-14, 4.193851878741028267E-47 ) ) ;
#30684 = EDGE_CURVE ( 'NONE', #65669, #83014, #38080, .T. ) ;
#30685 = ORIENTED_EDGE ( 'NONE', *, *, #13705, .T. ) ;
#30686 = ORIENTED_EDGE ( 'NONE', *, *, #19629, .T. ) ;
#30687 = AXIS2_PLACEMENT_3D ( 'NONE', #29317, #41568, #27508 ) ;
#30688 = CARTESIAN_POINT ( 'NONE',  ( 100.0140161817732860, -31.91085406740108610, 120.2724198280769912 ) ) ;
#30690 = ORIENTED_EDGE ( 'NONE', *, *, #11856, .T. ) ;
#30689 = CARTESIAN_POINT ( 'NONE',  ( 160.7738106836351051, -48.62134037874900372, 129.9678068554149775 ) ) ;
#30691 = CARTESIAN_POINT ( 'NONE',  ( 108.0321269276242049, -25.74166508409292220, 105.9946728949589811 ) ) ;
#30692 = CARTESIAN_POINT ( 'NONE',  ( 147.0667039024470171, -79.67844715994090166, 55.21780685541800437 ) ) ;
#30693 = AXIS2_PLACEMENT_3D ( 'NONE', #6639, #67513, #34335 ) ;
#30694 = CARTESIAN_POINT ( 'NONE',  ( 0.000000000000000000, 92.07499999999998863, 0.000000000000000000 ) ) ;
#30695 = CARTESIAN_POINT ( 'NONE',  ( 80.06648329127402519, -36.72944715994107412, -5.074374724089057764 ) ) ;
#30696 = CARTESIAN_POINT ( 'NONE',  ( 103.0217603569634690, -26.37318327779222216, 20.37276813305394185 ) ) ;
#30697 = ORIENTED_EDGE ( 'NONE', *, *, #52266, .T. ) ;
#30698 = ORIENTED_EDGE ( 'NONE', *, *, #89616, .T. ) ;
#30699 = ORIENTED_EDGE ( 'NONE', *, *, #34177, .T. ) ;
#30700 = APPLICATION_CONTEXT ( 'automotive_design' ) ;
#30701 = ADVANCED_FACE ( 'NONE', ( #66673 ), #4459, .F. ) ;
#30702 = LINE ( 'NONE', #44314, #70375 ) ;
#30703 = DIRECTION ( 'NONE',  ( 1.000000000000000078E-15, 1.000000000000000083E-30, -1.000000000000000000 ) ) ;
#30704 = CARTESIAN_POINT ( 'NONE',  ( 162.5667039024470171, -33.35206098992711077, -5.074374724088000832 ) ) ;
#30705 = DIRECTION ( 'NONE',  ( 1.907762142705490052E-15, 7.167082501179359715E-16, -1.000000000000000000 ) ) ;
#30706 = DIRECTION ( 'NONE',  ( 0.000000000000000000, 0.000000000000000000, -1.000000000000000000 ) ) ;
#30707 = CARTESIAN_POINT ( 'NONE',  ( 97.31300249461010310, -38.96030167564788371, 52.50535227464659727 ) ) ;
#30708 = CARTESIAN_POINT ( 'NONE',  ( 177.4809174648213741, -49.32844715993478957, 300.4678068554149490 ) ) ;
#30709 = CIRCLE ( 'NONE', #40864, 2.500000000000002220 ) ;
#30710 = CARTESIAN_POINT ( 'NONE',  ( -7.066900032206758553, 93.10220157233833049, 130.3645965947815455 ) ) ;
#30711 = CARTESIAN_POINT ( 'NONE',  ( 117.4658636684177679, -37.01502254527063940, 43.80419670448293346 ) ) ;
#30712 = ORIENTED_EDGE ( 'NONE', *, *, #20318, .F. ) ;
#30713 = ADVANCED_FACE ( 'NONE', ( #39854 ), #40755, .F. ) ;
#30714 = CARTESIAN_POINT ( 'NONE',  ( 12.70000000000000107, 83.38939070830900846, 129.9368274816650626 ) ) ;
#30715 = CARTESIAN_POINT ( 'NONE',  ( 126.5426538762358604, 45.18699313767324099, 32.12251388581796618 ) ) ;
#30716 = VECTOR ( 'NONE', #27305, 1000.000000000000000 ) ;
#30717 = CARTESIAN_POINT ( 'NONE',  ( 86.72755763596096301, -122.7870702624433648, 250.2178068554179902 ) ) ;
#30718 = CARTESIAN_POINT ( 'NONE',  ( 115.1291642039608547, -38.00337907228554712, 111.5195189410199674 ) ) ;
#30719 = VECTOR ( 'NONE', #59225, 1000.000000000000000 ) ;
#30720 = EDGE_CURVE ( 'NONE', #3831, #31184, #48085, .T. ) ;
#30721 = CARTESIAN_POINT ( 'NONE',  ( -31.75000000000000000, 24.56180297284579694, -3.174999999999779998 ) ) ;
#30722 = DIRECTION ( 'NONE',  ( 0.000000000000000000, 0.000000000000000000, 1.000000000000000000 ) ) ;
#30723 = ORIENTED_EDGE ( 'NONE', *, *, #80061, .F. ) ;
#30724 = ORIENTED_EDGE ( 'NONE', *, *, #8757, .T. ) ;
#30725 = DIRECTION ( 'NONE',  ( 0.000000000000000000, 0.000000000000000000, 1.000000000000000000 ) ) ;
#30726 = ORIENTED_EDGE ( 'NONE', *, *, #24940, .F. ) ;
#30727 = ORIENTED_EDGE ( 'NONE', *, *, #50358, .F. ) ;
#30728 = ADVANCED_FACE ( 'NONE', ( #25334 ), #6689, .T. ) ;
#30729 = VECTOR ( 'NONE', #54914, 1000.000000000000227 ) ;
#30730 = CARTESIAN_POINT ( 'NONE',  ( 115.3457950989190408, -42.46736495413998824, 159.7758690201829666 ) ) ;
#30731 = DIRECTION ( 'NONE',  ( 0.000000000000000000, -0.8660254037844392627, 0.4999999999999990008 ) ) ;
#30732 = CARTESIAN_POINT ( 'NONE',  ( 117.7257289732168744, -39.74036323029751117, 139.6194347997199827 ) ) ;
#30733 = CARTESIAN_POINT ( 'NONE',  ( 97.33784135113081959, -34.07106438717736552, 121.1147919308765353 ) ) ;
#30734 = CARTESIAN_POINT ( 'NONE',  ( 109.6423256655219660, -46.48025961810147066, 17.78142711047368962 ) ) ;
#30735 = ORIENTED_EDGE ( 'NONE', *, *, #1891, .T. ) ;
#30736 = VECTOR ( 'NONE', #72635, 1000.000000000000000 ) ;
#30737 = ORIENTED_EDGE ( 'NONE', *, *, #63632, .F. ) ;
#30738 = VERTEX_POINT ( 'NONE', #5812 ) ;
#30739 = CIRCLE ( 'NONE', #16231, 17.00000000000000000 ) ;
#30740 = EDGE_CURVE ( 'NONE', #944, #41003, #54813, .T. ) ;
#30741 = CARTESIAN_POINT ( 'NONE',  ( 115.5869623526398016, -35.21209367091628906, 196.7728522743529425 ) ) ;
#30742 = CARTESIAN_POINT ( 'NONE',  ( 103.5913855974186362, -46.58186107657011377, 57.30705384733997221 ) ) ;
#30743 = ORIENTED_EDGE ( 'NONE', *, *, #25207, .T. ) ;
#30744 = CARTESIAN_POINT ( 'NONE',  ( 96.73636544059188225, -37.96124694896867169, 41.42133956162496844 ) ) ;
#30745 = CARTESIAN_POINT ( 'NONE',  ( 113.1756163759788620, -44.75386896731635744, 253.0940677049611338 ) ) ;
#30746 = EDGE_CURVE ( 'NONE', #40826, #68446, #81674, .T. ) ;
#30747 = PLANE ( 'NONE',  #84370 ) ;
#30748 = CARTESIAN_POINT ( 'NONE',  ( -82.89895571708295563, 82.54999999999999716, 100.8594679592209644 ) ) ;
#30749 = CARTESIAN_POINT ( 'NONE',  ( 96.67093460706618657, -35.94617138369610387, 142.2670538473399517 ) ) ;
#30750 = AXIS2_PLACEMENT_3D ( 'NONE', #64190, #1061, #15142 ) ;
#30752 = EDGE_CURVE ( 'NONE', #63918, #58668, #33940, .T. ) ;
#30751 = CARTESIAN_POINT ( 'NONE',  ( 64.67079002020506096, -0.9301828534102468682, 361.9756252759101471 ) ) ;
#30753 = EDGE_LOOP ( 'NONE', ( #63916, #49194, #54267, #52783 ) ) ;
#30754 = DIRECTION ( 'NONE',  ( -0.8571673007021118895, 1.049727191138617833E-16, 0.5150380749100549327 ) ) ;
#30755 = AXIS2_PLACEMENT_3D ( 'NONE', #84823, #57537, #70738 ) ;
#30756 = ADVANCED_FACE ( 'NONE', ( #88025 ), #19424, .T. ) ;
#30757 = EDGE_LOOP ( 'NONE', ( #86248, #51833, #54820, #25228 ) ) ;
#30758 = LINE ( 'NONE', #51181, #89802 ) ;
#30759 = FACE_OUTER_BOUND ( 'NONE', #64764, .T. ) ;
#30760 = EDGE_LOOP ( 'NONE', ( #75804, #67720, #55607, #51349 ) ) ;
#30761 = FACE_OUTER_BOUND ( 'NONE', #18730, .T. ) ;
#30762 = CARTESIAN_POINT ( 'NONE',  ( 97.03967865257850178, -35.94463544949734057, 132.2646067221455155 ) ) ;
#30763 = CARTESIAN_POINT ( 'NONE',  ( 117.4547340842499210, -37.95832963484174627, 53.73276813305394484 ) ) ;
#30764 = CARTESIAN_POINT ( 'NONE',  ( -487.2989999999999782, 93.66249999999999432, 85.72499999999999432 ) ) ;
#30765 = CARTESIAN_POINT ( 'NONE',  ( 41.56648329127398966, -27.82844715994070484, 14.17562527591199917 ) ) ;
#30766 = FACE_OUTER_BOUND ( 'NONE', #47799, .T. ) ;
#30767 = CARTESIAN_POINT ( 'NONE',  ( 115.6651410650259066, -32.06827565682259262, 69.22133956162596746 ) ) ;
#30769 = CARTESIAN_POINT ( 'NONE',  ( 109.6005296801413067, -26.60309369064642127, 195.8813395616249977 ) ) ;
#30768 = DIRECTION ( 'NONE',  ( 1.000000000000000078E-15, -1.000000000000000000, 0.000000000000000000 ) ) ;
#30770 = DIRECTION ( 'NONE',  ( 1.000000000000000078E-15, -1.000000000000000083E-30, -1.000000000000000000 ) ) ;
#30771 = DIRECTION ( 'NONE',  ( 0.000000000000000000, -1.000000000000000000, 0.000000000000000000 ) ) ;
#30772 = EDGE_LOOP ( 'NONE', ( #28444, #27469, #55156, #37104 ) ) ;
#30773 = CARTESIAN_POINT ( 'NONE',  ( 63.03715912545730760, -24.42818131006027826, 300.4678068554150627 ) ) ;
#30774 = DIRECTION ( 'NONE',  ( 1.000000000000000000, 0.000000000000000000, -0.000000000000000000 ) ) ;
#30775 = CARTESIAN_POINT ( 'NONE',  ( 87.06648329127403940, -54.72944906728955061, -5.074374724089050659 ) ) ;
#30776 = CARTESIAN_POINT ( 'NONE',  ( 182.0374245136172249, -23.42844715993459559, 300.4678068554149490 ) ) ;
#30778 = ORIENTED_EDGE ( 'NONE', *, *, #75743, .T. ) ;
#30777 = CARTESIAN_POINT ( 'NONE',  ( 96.60014388984734524, -36.47963607454698831, 196.3070538473399438 ) ) ;
#30779 = FACE_OUTER_BOUND ( 'NONE', #61541, .T. ) ;
#30780 = CARTESIAN_POINT ( 'NONE',  ( 100.1243021666677606, -44.53607127582347402, 262.9984824187678782 ) ) ;
#30781 = CARTESIAN_POINT ( 'NONE',  ( 97.89440201276070752, -31.60978508062128967, 106.9213395616259703 ) ) ;
#30782 = CARTESIAN_POINT ( 'NONE',  ( 100.9565521831709987, -28.70555570752797792, 251.5995088816804355 ) ) ;
#30783 = VECTOR ( 'NONE', #59913, 1000.000000000000000 ) ;
#30784 = CARTESIAN_POINT ( 'NONE',  ( -15.88716625750469902, 91.07499999999996021, -53.54073290201169044 ) ) ;
#30785 = CARTESIAN_POINT ( 'NONE',  ( 91.91125933621933086, -96.68314769832139177, -21.78219314458224076 ) ) ;
#30786 = CARTESIAN_POINT ( 'NONE',  ( 98.30751334827748167, -41.72882313198851278, 262.7398596741535357 ) ) ;
#30787 = ORIENTED_EDGE ( 'NONE', *, *, #45147, .F. ) ;
#30788 = TOROIDAL_SURFACE ( 'NONE', #43872, 9.000000000000007105, 1.000000000000000000 ) ;
#30789 = EDGE_CURVE ( 'NONE', #61847, #80812, #89374, .T. ) ;
#30790 = ORIENTED_EDGE ( 'NONE', *, *, #65300, .F. ) ;
#30791 = VERTEX_POINT ( 'NONE', #74842 ) ;
#30792 = EDGE_LOOP ( 'NONE', ( #43524, #11743 ) ) ;
#30793 = CARTESIAN_POINT ( 'NONE',  ( 138.8167039024479834, -67.87844715994100397, 86.31780685541500020 ) ) ;
#30794 = CARTESIAN_POINT ( 'NONE',  ( 110.8926193997603065, -26.99384161864454157, 265.7784824187680783 ) ) ;
#30795 = DIRECTION ( 'NONE',  ( 1.000000000000000000, 4.163336342344333240E-14, 0.000000000000000000 ) ) ;
#30796 = LINE ( 'NONE', #79415, #89052 ) ;
#30797 = VECTOR ( 'NONE', #77989, 1000.000000000000000 ) ;
#30799 = CARTESIAN_POINT ( 'NONE',  ( 76.38829385798568694, 74.80137413886473041, 90.66736180499722764 ) ) ;
#30798 = CARTESIAN_POINT ( 'NONE',  ( 172.5664832912740110, -36.32844715994070839, 203.6756252759119832 ) ) ;
#30800 = CARTESIAN_POINT ( 'NONE',  ( 146.0667039024470455, -121.7784471599409102, 55.21780685541800437 ) ) ;
#30801 = CARTESIAN_POINT ( 'NONE',  ( 109.5825779133427460, -28.02991049533996204, 214.2628960185529365 ) ) ;
#30802 = ORIENTED_EDGE ( 'NONE', *, *, #82576, .F. ) ;
#30803 = VERTEX_POINT ( 'NONE', #47561 ) ;
#30804 = ORIENTED_EDGE ( 'NONE', *, *, #77481, .T. ) ;
#30805 = CIRCLE ( 'NONE', #9039, 1.524000000000001132 ) ;
#30806 = ADVANCED_FACE ( 'NONE', ( #39416 ), #61200, .F. ) ;
#30807 = DIRECTION ( 'NONE',  ( 1.000000000000000000, 3.930900487435134677E-14, 0.000000000000000000 ) ) ;
#30808 = CARTESIAN_POINT ( 'NONE',  ( 0.000000000000000000, 91.07499999999996021, 38.10000000000000142 ) ) ;
#30809 = ADVANCED_FACE ( 'NONE', ( #19879 ), #46662, .F. ) ;
#30810 = CARTESIAN_POINT ( 'NONE',  ( 97.60228370342871074, -39.19771807616534431, 272.5299109901961856 ) ) ;
#30811 = CIRCLE ( 'NONE', #9043, 2.999999999999933387 ) ;
#30812 = LINE ( 'NONE', #2673, #73422 ) ;
#30813 = ADVANCED_FACE ( 'NONE', ( #87577 ), #26679, .F. ) ;
#30814 = LINE ( 'NONE', #59839, #88313 ) ;
#30815 = CARTESIAN_POINT ( 'NONE',  ( -48.02966122971777452, 100.5999999999999659, 106.4272185163641780 ) ) ;
#30816 = EDGE_CURVE ( 'NONE', #51305, #5456, #73943, .T. ) ;
#30817 = ORIENTED_EDGE ( 'NONE', *, *, #1404, .T. ) ;
#30818 = ADVANCED_FACE ( 'NONE', ( #12170 ), #13068, .F. ) ;
#30819 = CARTESIAN_POINT ( 'NONE',  ( 100.9530876688875480, -28.70826590416694302, 56.59407357525381599 ) ) ;
#30820 = ORIENTED_EDGE ( 'NONE', *, *, #80306, .F. ) ;
#30821 = DIRECTION ( 'NONE',  ( 0.9659258262890704216, 0.000000000000000000, -0.2588190451025129124 ) ) ;
#30822 = CARTESIAN_POINT ( 'NONE',  ( 111.0211786934911231, -29.03130846684521060, 17.52904275054395455 ) ) ;
#30823 = ADVANCED_FACE ( 'NONE', ( #67573 ), #82125, .F. ) ;
#30824 = DIRECTION ( 'NONE',  ( 0.000000000000000000, 0.000000000000000000, 1.000000000000000000 ) ) ;
#30825 = EDGE_CURVE ( 'NONE', #36562, #41877, #53913, .T. ) ;
#30826 = CARTESIAN_POINT ( 'NONE',  ( 49.16670390244752298, -28.27351298637373489, 237.4678068554150059 ) ) ;
#30827 = CARTESIAN_POINT ( 'NONE',  ( -6.802569982901797644E-16, 69.84999999999999432, -118.5560000000000116 ) ) ;
#30828 = ORIENTED_EDGE ( 'NONE', *, *, #69213, .F. ) ;
#30829 = CARTESIAN_POINT ( 'NONE',  ( 172.5664832912740110, -36.32844715994070839, 314.1756252759120116 ) ) ;
#30830 = CARTESIAN_POINT ( 'NONE',  ( 25.56670390244797275, -65.37844715994100397, 137.2178068554150059 ) ) ;
#30831 = VECTOR ( 'NONE', #76262, 1000.000000000000000 ) ;
#30832 = EDGE_CURVE ( 'NONE', #24378, #22610, #75736, .T. ) ;
#30833 = VERTEX_POINT ( 'NONE', #13955 ) ;
#30834 = CARTESIAN_POINT ( 'NONE',  ( 108.9852622695951112, -46.97665739950247143, 82.72419670448194040 ) ) ;
#30835 = EDGE_LOOP ( 'NONE', ( #42380, #9168, #38271, #77503 ) ) ;
#30836 = CARTESIAN_POINT ( 'NONE',  ( 105.1568233002730182, -45.58189704936153674, 31.84194363760095570 ) ) ;
#30837 = EDGE_CURVE ( 'NONE', #37713, #34867, #48441, .T. ) ;
#30838 = CARTESIAN_POINT ( 'NONE',  ( 0.000000000000000000, 17.78000000000000114, 0.000000000000000000 ) ) ;
#30839 = CARTESIAN_POINT ( 'NONE',  ( 97.94737569220006890, -41.00876738043628222, 58.10729759161198160 ) ) ;
#30840 = CARTESIAN_POINT ( 'NONE',  ( 29.56670390244797630, -67.87844715994100397, 310.9178068554150514 ) ) ;
#30841 = CARTESIAN_POINT ( 'NONE',  ( -7.196800215918080040E-13, 127.0000000000000000, 110.3312500000000114 ) ) ;
#30842 = CARTESIAN_POINT ( 'NONE',  ( 143.2570480158645978, -67.87844715994090450, 245.5376130668579719 ) ) ;
#30843 = CARTESIAN_POINT ( 'NONE',  ( 100.3971814656068915, -28.68844771884695888, 36.62705384733894221 ) ) ;
#30844 = FACE_OUTER_BOUND ( 'NONE', #73830, .T. ) ;
#30845 = EDGE_LOOP ( 'NONE', ( #63794, #41112, #79944, #89730 ) ) ;
#30846 = VECTOR ( 'NONE', #51820, 999.9999999999998863 ) ;
#30847 = DIRECTION ( 'NONE',  ( 1.000000000000000000, 0.000000000000000000, -7.043400939473319300E-33 ) ) ;
#30848 = VERTEX_POINT ( 'NONE', #1685 ) ;
#30849 = CARTESIAN_POINT ( 'NONE',  ( 95.26251351713513316, -38.28569616102737427, 147.4299109901969871 ) ) ;
#30850 = CARTESIAN_POINT ( 'NONE',  ( 124.9714502624620707, 48.43269546781706936, -37.77605326482454018 ) ) ;
#30851 = VERTEX_POINT ( 'NONE', #28472 ) ;
#30852 = VERTEX_POINT ( 'NONE', #8038 ) ;
#30853 = DIRECTION ( 'NONE',  ( -1.000000000000000078E-15, 0.000000000000000000, -1.000000000000000000 ) ) ;
#30854 = CARTESIAN_POINT ( 'NONE',  ( 71.06648329127399677, -18.82844715994099971, 226.9256252759120116 ) ) ;
#30855 = CARTESIAN_POINT ( 'NONE',  ( 115.9419818307744663, -40.91744192719425399, 228.4756252759109714 ) ) ;
#30856 = DIRECTION ( 'NONE',  ( -0.2588190451025206285, 0.000000000000000000, 0.9659258262890683122 ) ) ;
#30857 = EDGE_CURVE ( 'NONE', #77207, #74702, #57304, .T. ) ;
#30858 = CARTESIAN_POINT ( 'NONE',  ( 144.5707550238523709, -140.1743960385356047, 245.5280425831230104 ) ) ;
#30859 = CARTESIAN_POINT ( 'NONE',  ( 167.6524903400755875, -49.32844715993520879, 180.4678068554150059 ) ) ;
#30860 = CARTESIAN_POINT ( 'NONE',  ( 118.0020517745808633, -38.33796275862062686, 69.72229194257801055 ) ) ;
#30861 = AXIS2_PLACEMENT_3D ( 'NONE', #76524, #83800, #83347 ) ;
#30863 = EDGE_CURVE ( 'NONE', #60356, #36108, #87341, .T. ) ;
#30862 = CARTESIAN_POINT ( 'NONE',  ( 163.2569089553709034, -33.54226604284439617, 193.9678068554149775 ) ) ;
#30864 = VERTEX_POINT ( 'NONE', #77535 ) ;
#30865 = CARTESIAN_POINT ( 'NONE',  ( 103.2894945095962242, -27.47016022250103973, 171.3846815306852704 ) ) ;
#30866 = ADVANCED_FACE ( 'NONE', ( #28938 ), #77093, .F. ) ;
#30867 = LINE ( 'NONE', #87175, #46179 ) ;
#30868 = VERTEX_POINT ( 'NONE', #55702 ) ;
#30869 = VECTOR ( 'NONE', #76900, 1000.000000000000000 ) ;
#30870 = FACE_OUTER_BOUND ( 'NONE', #66168, .T. ) ;
#30871 = DIRECTION ( 'NONE',  ( 1.000000000000000078E-15, -1.000000000000000000, 0.000000000000000000 ) ) ;
#30872 = CARTESIAN_POINT ( 'NONE',  ( 117.4525030917818782, -36.13006561810994555, 228.8727681330539667 ) ) ;
#30873 = PRESENTATION_STYLE_ASSIGNMENT (( #84966 ) ) ;
#30874 = CARTESIAN_POINT ( 'NONE',  ( 27.27158787008325902, 184.0000000000000000, -5.920431057502157584E-15 ) ) ;
#30875 = CYLINDRICAL_SURFACE ( 'NONE', #86772, 2.517500000000005844 ) ;
#30876 = CARTESIAN_POINT ( 'NONE',  ( 98.63267121701338169, -35.20533560836722131, 240.6067055423629597 ) ) ;
#30879 = CARTESIAN_POINT ( 'NONE',  ( 118.0525141433397636, -37.71481444994962118, 29.74324432352998215 ) ) ;
#30878 = DIRECTION ( 'NONE',  ( -0.7071067811864671926, -0.7071067811866279529, -6.612322855854137577E-17 ) ) ;
#30877 = CONICAL_SURFACE ( 'NONE', #68553, 161.5439999999999827, 0.08726646259971625186 ) ;
#30880 = CARTESIAN_POINT ( 'NONE',  ( 110.8238305604934624, 63.68415021057004566, 69.01438277976548363 ) ) ;
#30881 = CARTESIAN_POINT ( 'NONE',  ( 108.3247603638532865, -47.12287801086134920, 117.6727681330539639 ) ) ;
#30882 = ORIENTED_EDGE ( 'NONE', *, *, #21789, .T. ) ;
#30883 = DIRECTION ( 'NONE',  ( 1.000000000000000000, 4.237773401492740281E-14, 0.000000000000000000 ) ) ;
#30884 = ORIENTED_EDGE ( 'NONE', *, *, #49803, .F. ) ;
#30885 = FACE_OUTER_BOUND ( 'NONE', #78430, .T. ) ;
#30886 = CARTESIAN_POINT ( 'NONE',  ( 108.4174892303373241, -26.73503592435250198, 65.96895861098096248 ) ) ;
#30887 = CARTESIAN_POINT ( 'NONE',  ( 102.7778427608900955, -89.25462229453692942, -21.78219314458248945 ) ) ;
#30888 = ORIENTED_EDGE ( 'NONE', *, *, #50705, .F. ) ;
#30889 = FACE_OUTER_BOUND ( 'NONE', #40373, .T. ) ;
#30890 = ORIENTED_EDGE ( 'NONE', *, *, #13091, .T. ) ;
#30891 = DIRECTION ( 'NONE',  ( 0.000000000000000000, 0.000000000000000000, 1.000000000000000000 ) ) ;
#30892 = DIRECTION ( 'NONE',  ( -4.237773401492740281E-14, 1.000000000000000000, 0.000000000000000000 ) ) ;
#30893 = DIRECTION ( 'NONE',  ( 0.000000000000000000, -1.000000000000000000, 0.000000000000000000 ) ) ;
#30894 = VERTEX_POINT ( 'NONE', #42098 ) ;
#30895 = CARTESIAN_POINT ( 'NONE',  ( 117.1278252906914048, -39.54294340788323581, 98.60991099019594230 ) ) ;
#30896 = DIRECTION ( 'NONE',  ( 0.000000000000000000, 0.000000000000000000, 1.000000000000000000 ) ) ;
#30897 = DIRECTION ( 'NONE',  ( 0.000000000000000000, 0.000000000000000000, 1.000000000000000000 ) ) ;
#30898 = CARTESIAN_POINT ( 'NONE',  ( 41.56648329127398966, -27.82844715994070484, 138.9256252759119832 ) ) ;
#30899 = CARTESIAN_POINT ( 'NONE',  ( 109.6430121121371570, -46.48008674026510079, 142.7814586077414276 ) ) ;
#30900 = ORIENTED_EDGE ( 'NONE', *, *, #9625, .T. ) ;
#30901 = AXIS2_PLACEMENT_3D ( 'NONE', #87448, #52867, #60156 ) ;
#30902 = DIRECTION ( 'NONE',  ( -4.237773401492740281E-14, 1.000000000000000000, 0.000000000000000000 ) ) ;
#30903 = CARTESIAN_POINT ( 'NONE',  ( 71.77848634863140376, 127.0000000000000000, -77.39114642429929347 ) ) ;
#30905 = CARTESIAN_POINT ( 'NONE',  ( 91.91125933621954402, -111.9799080603168449, -11.78219314458175937 ) ) ;
#30904 = DIRECTION ( 'NONE',  ( -0.7071067811865671127, -0.7071067811865279218, -7.071067811865664660E-16 ) ) ;
#30906 = DIRECTION ( 'NONE',  ( 0.000000000000000000, 0.000000000000000000, 1.000000000000000000 ) ) ;
#30907 = VECTOR ( 'NONE', #6132, 1000.000000000000000 ) ;
#30908 = ORIENTED_EDGE ( 'NONE', *, *, #50819, .F. ) ;
#30909 = ADVANCED_FACE ( 'NONE', ( #55264, #14872 ), #69375, .F. ) ;
#30910 = CARTESIAN_POINT ( 'NONE',  ( 115.0372575601887917, -42.90846249503305643, 34.30229194963032313 ) ) ;
#30911 = EDGE_CURVE ( 'NONE', #14111, #38840, #42378, .T. ) ;
#30912 = CARTESIAN_POINT ( 'NONE',  ( 108.2857792741417597, -47.02760743735399984, 158.6822919425769669 ) ) ;
#30914 = EDGE_LOOP ( 'NONE', ( #50730, #44456, #77968, #70221 ) ) ;
#30913 = DIRECTION ( 'NONE',  ( -4.237773401492740281E-14, 1.000000000000000000, 0.000000000000000000 ) ) ;
#30915 = ADVANCED_FACE ( 'NONE', ( #15314 ), #83013, .T. ) ;
#30916 = CARTESIAN_POINT ( 'NONE',  ( 100.2135729606528685, -43.75450166055420453, 17.96133956162493206 ) ) ;
#30917 = LINE ( 'NONE', #67562, #41191 ) ;
#30918 = CARTESIAN_POINT ( 'NONE',  ( -487.2989999999999782, 18.41194598552324990, 83.34375000000000000 ) ) ;
#30919 = LINE ( 'NONE', #64556, #48558 ) ;
#30920 = EDGE_CURVE ( 'NONE', #71852, #8565, #21226, .T. ) ;
#30921 = ORIENTED_EDGE ( 'NONE', *, *, #37751, .T. ) ;
#30922 = DIRECTION ( 'NONE',  ( -3.100000000000000258E-29, 3.100000000000000044E-14, 1.000000000000000000 ) ) ;
#30923 = ORIENTED_EDGE ( 'NONE', *, *, #9055, .F. ) ;
#30924 = ORIENTED_EDGE ( 'NONE', *, *, #41066, .T. ) ;
#30925 = CARTESIAN_POINT ( 'NONE',  ( 102.2066036383193222, -44.77047292137198298, 198.5634880678019272 ) ) ;
#30926 = EDGE_CURVE ( 'NONE', #68369, #88451, #76636, .T. ) ;
#30927 = VECTOR ( 'NONE', #44385, 1000.000000000000000 ) ;
#30928 = FACE_OUTER_BOUND ( 'NONE', #29854, .T. ) ;
#30929 = CARTESIAN_POINT ( 'NONE',  ( 100.3180865808431719, -43.26669944020724756, 38.38253568684996253 ) ) ;
#30930 = CARTESIAN_POINT ( 'NONE',  ( -91.72735010416610635, 95.24968527363476767, 92.90667244829751326 ) ) ;
#30931 = AXIS2_PLACEMENT_3D ( 'NONE', #57782, #70532, #57324 ) ;
#30932 = EDGE_CURVE ( 'NONE', #58319, #77842, #42980, .T. ) ;
#30933 = VECTOR ( 'NONE', #45340, 1000.000000000000000 ) ;
#30934 = CARTESIAN_POINT ( 'NONE',  ( 104.4899544582702049, -26.97880758309926819, 80.28145860873343054 ) ) ;
#30935 = DIRECTION ( 'NONE',  ( 1.000000000000000000, 4.299999999999999979E-14, 1.000000000000000078E-15 ) ) ;
#30936 = ORIENTED_EDGE ( 'NONE', *, *, #76983, .F. ) ;
#30937 = FACE_OUTER_BOUND ( 'NONE', #45831, .T. ) ;
#30938 = DIRECTION ( 'NONE',  ( 1.000000000000000078E-15, -1.000000000000000083E-30, -1.000000000000000000 ) ) ;
#30939 = VERTEX_POINT ( 'NONE', #36195 ) ;
#30940 = CARTESIAN_POINT ( 'NONE',  ( 103.0988156209413233, -47.86972635628425365, 252.3041967044823366 ) ) ;
#30941 = CARTESIAN_POINT ( 'NONE',  ( 12.43699659993004403, 84.61172699943961106, 117.7007664268632112 ) ) ;
#30942 = ORIENTED_EDGE ( 'NONE', *, *, #73254, .T. ) ;
#30943 = EDGE_CURVE ( 'NONE', #6162, #73924, #64132, .T. ) ;
#30944 = DIRECTION ( 'NONE',  ( 4.299999999999999979E-14, -1.000000000000000000, 0.000000000000000000 ) ) ;
#30945 = CARTESIAN_POINT ( 'NONE',  ( -100.8961411191535973, 127.0000000000000000, 3.968749999998880451 ) ) ;
#30946 = CARTESIAN_POINT ( 'NONE',  ( 107.0664832912739968, -18.82844715994099971, 168.9256252759119832 ) ) ;
#30947 = FACE_OUTER_BOUND ( 'NONE', #12378, .T. ) ;
#30948 = CARTESIAN_POINT ( 'NONE',  ( 113.0503328260151079, -46.07776482166018184, 214.0175300378159591 ) ) ;
#30949 = CARTESIAN_POINT ( 'NONE',  ( 0.8330848375387808202, 69.94999999999998863, 118.3559999999999803 ) ) ;
#30950 = ORIENTED_EDGE ( 'NONE', *, *, #79250, .T. ) ;
#30951 = CARTESIAN_POINT ( 'NONE',  ( 115.9284861604400731, -31.15648700444841879, 30.27276813305396175 ) ) ;
#30952 = DIRECTION ( 'NONE',  ( 1.000000000000000000, 0.000000000000000000, 0.000000000000000000 ) ) ;
#30953 = CIRCLE ( 'NONE', #72957, 4.875000000000017764 ) ;
#30954 = CARTESIAN_POINT ( 'NONE',  ( 110.9930863310008959, -46.38701419431276207, 282.8841967044824628 ) ) ;
#30955 = ORIENTED_EDGE ( 'NONE', *, *, #72717, .F. ) ;
#30956 = VECTOR ( 'NONE', #14163, 1000.000000000000000 ) ;
#30957 = CARTESIAN_POINT ( 'NONE',  ( 78.24498361944210956, -38.78962918509265023, 7.677444906553891890 ) ) ;
#30958 = CARTESIAN_POINT ( 'NONE',  ( 101.9938210835711203, -45.44620686955099131, 18.15674971878247490 ) ) ;
#30959 = FACE_OUTER_BOUND ( 'NONE', #54343, .T. ) ;
#30960 = CARTESIAN_POINT ( 'NONE',  ( 115.1349747707284479, -33.59889284931170295, 91.92713798863898944 ) ) ;
#30961 = CARTESIAN_POINT ( 'NONE',  ( 107.6557286256638264, -47.79009794008123890, 193.6308633711489620 ) ) ;
#30962 = DIRECTION ( 'NONE',  ( 1.000000000000000000, 0.000000000000000000, 0.000000000000000000 ) ) ;
#30963 = EDGE_LOOP ( 'NONE', ( #75949, #45413, #78162, #11293 ) ) ;
#30964 = EDGE_CURVE ( 'NONE', #70690, #19753, #72872, .T. ) ;
#30965 = CARTESIAN_POINT ( 'NONE',  ( -41.60202597009397607, 65.59999999999998010, 50.85338361873603219 ) ) ;
#30966 = VERTEX_POINT ( 'NONE', #43885 ) ;
#30967 = EDGE_LOOP ( 'NONE', ( #9058, #23414, #8870, #83259 ) ) ;
#30968 = AXIS2_PLACEMENT_3D ( 'NONE', #80342, #65360, #44452 ) ;
#30969 = DIRECTION ( 'NONE',  ( 1.042073847087816516E-15, 1.000000000000000000, 0.000000000000000000 ) ) ;
#30970 = VERTEX_POINT ( 'NONE', #71619 ) ;
#30971 = ORIENTED_EDGE ( 'NONE', *, *, #73537, .T. ) ;
#30972 = PLANE ( 'NONE',  #87478 ) ;
#30973 = CYLINDRICAL_SURFACE ( 'NONE', #32670, 4.762500000000002842 ) ;
#30974 = CARTESIAN_POINT ( 'NONE',  ( 103.2961519303028552, -27.46744216278922579, 41.38410912957840537 ) ) ;
#30975 = CARTESIAN_POINT ( 'NONE',  ( 103.1631342820178929, -29.09950819311272951, 119.8752769709339816 ) ) ;
#30976 = CARTESIAN_POINT ( 'NONE',  ( 107.6091449839925929, -48.61785814739364042, 42.61276813305398292 ) ) ;
#30977 = CARTESIAN_POINT ( 'NONE',  ( -11.75210537873753402, 77.68270844259760111, 130.0262747911924635 ) ) ;
#30978 = ORIENTED_EDGE ( 'NONE', *, *, #3130, .T. ) ;
#30979 = EDGE_CURVE ( 'NONE', #47447, #74740, #83391, .T. ) ;
#30980 = DIRECTION ( 'NONE',  ( 1.000000000000000000, -5.337610695313248426E-16, 0.000000000000000000 ) ) ;
#30981 = ORIENTED_EDGE ( 'NONE', *, *, #14644, .T. ) ;
#30982 = DIRECTION ( 'NONE',  ( 2.108231265501709878E-16, 0.000000000000000000, -1.000000000000000000 ) ) ;
#30983 = CARTESIAN_POINT ( 'NONE',  ( 105.7145878461457187, -46.72372356240133939, 32.46910694999912295 ) ) ;
#30984 = PLANE ( 'NONE',  #67830 ) ;
#30986 = EDGE_CURVE ( 'NONE', #13566, #64803, #87031, .T. ) ;
#30985 = CIRCLE ( 'NONE', #65796, 2.750000000000002665 ) ;
#30987 = CARTESIAN_POINT ( 'NONE',  ( 172.5664832912728457, -27.82844715994070484, 201.9256252759119832 ) ) ;
#30988 = ORIENTED_EDGE ( 'NONE', *, *, #39118, .F. ) ;
#30989 = CARTESIAN_POINT ( 'NONE',  ( 101.0865414634836696, -45.26919196907830667, 282.0899109901967563 ) ) ;
#30990 = CARTESIAN_POINT ( 'NONE',  ( 104.6388127410885005, -47.56014030727299513, 23.38895860924494841 ) ) ;
#30991 = VECTOR ( 'NONE', #80821, 1000.000000000000000 ) ;
#30992 = LINE ( 'NONE', #50985, #53183 ) ;
#30994 = FACE_OUTER_BOUND ( 'NONE', #86789, .T. ) ;
#30993 = DIRECTION ( 'NONE',  ( 0.7071067811865483499, 0.7071067811865466846, 7.071067811865491110E-16 ) ) ;
#30995 = CARTESIAN_POINT ( 'NONE',  ( -546.0365000000000464, 53.97500000000000142, 50.79999999999999716 ) ) ;
#30996 = DIRECTION ( 'NONE',  ( 0.000000000000000000, 0.000000000000000000, -1.000000000000000000 ) ) ;
#30997 = CARTESIAN_POINT ( 'NONE',  ( 131.4241199117880114, -37.49143581486269738, 6.902478035881958185 ) ) ;
#30998 = CARTESIAN_POINT ( 'NONE',  ( 156.5667039024485803, -48.82844715993568485, 137.2178068554149775 ) ) ;
#30999 = DIRECTION ( 'NONE',  ( 0.000000000000000000, 1.000000000000000000, 0.000000000000000000 ) ) ;
#31000 = FACE_OUTER_BOUND ( 'NONE', #29843, .T. ) ;
#31001 = CARTESIAN_POINT ( 'NONE',  ( 105.3130012014428445, -26.40811315510063295, 15.20991099019697401 ) ) ;
#31002 = CARTESIAN_POINT ( 'NONE',  ( 101.9845378472182773, -45.87248622144053911, 183.1727681330539781 ) ) ;
#31003 = CARTESIAN_POINT ( 'NONE',  ( 118.7569292017688696, -34.64240976163905827, 44.96705384733895272 ) ) ;
#31005 = CARTESIAN_POINT ( 'NONE',  ( 108.3334480975946974, -46.73485935361659926, 47.67729194278742000 ) ) ;
#31004 = FACE_BOUND ( 'NONE', #67677, .T. ) ;
#31006 = CARTESIAN_POINT ( 'NONE',  ( 80.25489464535191075, -33.97944715994105991, 1.625625275910944634 ) ) ;
#31007 = AXIS2_PLACEMENT_3D ( 'NONE', #34503, #62213, #83130 ) ;
#31008 = CIRCLE ( 'NONE', #33862, 3.250000000000002665 ) ;
#31009 = ORIENTED_EDGE ( 'NONE', *, *, #38150, .F. ) ;
#31010 = EDGE_CURVE ( 'NONE', #89279, #81541, #9836, .T. ) ;
#31011 = CARTESIAN_POINT ( 'NONE',  ( 113.2454987153061694, -28.75867295907008270, 185.5522919408021494 ) ) ;
#31012 = ORIENTED_EDGE ( 'NONE', *, *, #82221, .T. ) ;
#31013 = EDGE_CURVE ( 'NONE', #28274, #89072, #2582, .T. ) ;
#31014 = CARTESIAN_POINT ( 'NONE',  ( 106.6854394624702849, -26.95610377642496758, 81.10705384733896040 ) ) ;
#31016 = ORIENTED_EDGE ( 'NONE', *, *, #5959, .T. ) ;
#31015 = FACE_OUTER_BOUND ( 'NONE', #58086, .T. ) ;
#31017 = VECTOR ( 'NONE', #32582, 1000.000000000000000 ) ;
#31018 = DIRECTION ( 'NONE',  ( 0.000000000000000000, 0.000000000000000000, -1.000000000000000000 ) ) ;
#31019 = EDGE_CURVE ( 'NONE', #5511, #24458, #9031, .T. ) ;
#31020 = CARTESIAN_POINT ( 'NONE',  ( 113.1426608820137716, -26.58408993604434301, 200.6470538473399756 ) ) ;
#31021 = CARTESIAN_POINT ( 'NONE',  ( 0.000000000000000000, 239.0000000000000000, 154.6557476874258441 ) ) ;
#31022 = CARTESIAN_POINT ( 'NONE',  ( 110.8542472415531250, -45.98432934487685486, 147.8856059545649941 ) ) ;
#31023 = CARTESIAN_POINT ( 'NONE',  ( 107.0667039024470313, -104.2784471599409102, 17.71780685541799016 ) ) ;
#31024 = CARTESIAN_POINT ( 'NONE',  ( 144.5667039024470455, -118.2784471599408960, 45.21780685541799727 ) ) ;
#31025 = CARTESIAN_POINT ( 'NONE',  ( 145.8907002709979963, -138.8544507913900077, 245.5998607319569942 ) ) ;
#31026 = EDGE_CURVE ( 'NONE', #17885, #15997, #23558, .T. ) ;
#31027 = CARTESIAN_POINT ( 'NONE',  ( 117.0956141847452869, -37.54243412410453118, 98.76173397921864705 ) ) ;
#31028 = CARTESIAN_POINT ( 'NONE',  ( 98.40655050692420502, -32.18313002855524729, 135.9413395616259947 ) ) ;
#31029 = ORIENTED_EDGE ( 'NONE', *, *, #64625, .F. ) ;
#31030 = ORIENTED_EDGE ( 'NONE', *, *, #49250, .T. ) ;
#31031 = CARTESIAN_POINT ( 'NONE',  ( 106.7212481586559392, -27.87455634666363835, 81.53872616303998200 ) ) ;
#31032 = ADVANCED_FACE ( 'NONE', ( #3459, #85705 ), #23031, .F. ) ;
#31033 = FACE_OUTER_BOUND ( 'NONE', #13276, .T. ) ;
#31035 = CARTESIAN_POINT ( 'NONE',  ( 172.5664832912729878, -27.57844715994070484, 75.92562527591199739 ) ) ;
#31034 = CARTESIAN_POINT ( 'NONE',  ( 109.7813264909552231, -47.51098736074720108, 238.7727681330529776 ) ) ;
#31036 = DIRECTION ( 'NONE',  ( 1.000000000000000000, 0.000000000000000000, 0.000000000000000000 ) ) ;
#31037 = CARTESIAN_POINT ( 'NONE',  ( 49.21213752015889042, -29.73316016639542880, 117.4678068554150485 ) ) ;
#31038 = ADVANCED_FACE ( 'NONE', ( #24796 ), #23480, .F. ) ;
#31039 = CARTESIAN_POINT ( 'NONE',  ( 21.03715912545739641, -47.82818131006197149, 180.4678068554150911 ) ) ;
#31040 = CARTESIAN_POINT ( 'NONE',  ( 80.06648329127399677, 0.2215528400590013880, 7.443125275912000127 ) ) ;
#31041 = FACE_OUTER_BOUND ( 'NONE', #46523, .T. ) ;
#31042 = LINE ( 'NONE', #59181, #85044 ) ;
#31043 = CARTESIAN_POINT ( 'NONE',  ( 113.5515132932711566, -44.90922781482916548, 168.1099109901969939 ) ) ;
#31044 = ORIENTED_EDGE ( 'NONE', *, *, #61673, .T. ) ;
#31045 = EDGE_LOOP ( 'NONE', ( #45838, #47815, #58833, #50448 ) ) ;
#31046 = CARTESIAN_POINT ( 'NONE',  ( 76.05567402747949757, -69.25962940816080504, 247.5000682988239760 ) ) ;
#31047 = CARTESIAN_POINT ( 'NONE',  ( 98.34985896447652465, -31.65658472180727401, 151.9064586012064808 ) ) ;
#31048 = CARTESIAN_POINT ( 'NONE',  ( 194.5667039024482108, -40.82844715993405060, 180.4678068554150343 ) ) ;
#31049 = CARTESIAN_POINT ( 'NONE',  ( 97.92310363649473004, -40.78041284545158618, 102.6583543547307329 ) ) ;
#31050 = CARTESIAN_POINT ( 'NONE',  ( 101.9936049672545550, -45.44606238681409138, 268.1564571553904557 ) ) ;
#31051 = VECTOR ( 'NONE', #36005, 1000.000000000000000 ) ;
#31052 = CARTESIAN_POINT ( 'NONE',  ( 117.2917222856570447, -34.52255020207628888, 183.9956252759109532 ) ) ;
#31053 = CARTESIAN_POINT ( 'NONE',  ( 63.56670390244796920, -40.82844715994016127, 300.4678068554150627 ) ) ;
#31054 = ORIENTED_EDGE ( 'NONE', *, *, #46931, .T. ) ;
#31056 = VERTEX_POINT ( 'NONE', #51148 ) ;
#31055 = ORIENTED_EDGE ( 'NONE', *, *, #32562, .F. ) ;
#31057 = CARTESIAN_POINT ( 'NONE',  ( 114.1612546374381907, -43.81239283379284899, 64.20290172889339431 ) ) ;
#31058 = CARTESIAN_POINT ( 'NONE',  ( 51.56670390244760682, -32.29483332968564469, 313.9678068554150059 ) ) ;
#31059 = LINE ( 'NONE', #85165, #10672 ) ;
#31060 = CARTESIAN_POINT ( 'NONE',  ( 101.1777422249941338, -43.35145646725580804, 263.4301547344683740 ) ) ;
#31061 = CARTESIAN_POINT ( 'NONE',  ( 115.0988951105837259, -108.3384846469520113, 2.217806855418142042 ) ) ;
#31062 = ORIENTED_EDGE ( 'NONE', *, *, #58382, .T. ) ;
#31063 = ADVANCED_FACE ( 'NONE', ( #66116 ), #8952, .T. ) ;
#31064 = CARTESIAN_POINT ( 'NONE',  ( 116.2888956068410522, -39.44798389054702170, 9.635625275910941312 ) ) ;
#31065 = CARTESIAN_POINT ( 'NONE',  ( -126.8390414488319635, 59.56676029426186858, 30.93113591434403276 ) ) ;
#31066 = ORIENTED_EDGE ( 'NONE', *, *, #14200, .F. ) ;
#31067 = ORIENTED_EDGE ( 'NONE', *, *, #88184, .T. ) ;
#31068 = CIRCLE ( 'NONE', #23832, 15.99999999999999822 ) ;
#31069 = CIRCLE ( 'NONE', #24025, 3.250000000000002665 ) ;
#31070 = CARTESIAN_POINT ( 'NONE',  ( 113.6434775417805554, -44.29062971714213148, 113.1460879784515896 ) ) ;
#31071 = AXIS2_PLACEMENT_3D ( 'NONE', #2824, #18554, #47585 ) ;
#31072 = ORIENTED_EDGE ( 'NONE', *, *, #74640, .F. ) ;
#31073 = ORIENTED_EDGE ( 'NONE', *, *, #5444, .F. ) ;
#31074 = CARTESIAN_POINT ( 'NONE',  ( 97.81670390244700286, -67.87844715994096134, 55.21780685541800437 ) ) ;
#31075 = CIRCLE ( 'NONE', #73089, 2.517500000000000071 ) ;
#31076 = CARTESIAN_POINT ( 'NONE',  ( 106.6898958108015307, -27.68119582636871456, 39.52003887569599527 ) ) ;
#31078 = CARTESIAN_POINT ( 'NONE',  ( 112.2159804458396479, -45.81949903116512246, 212.9870538473389558 ) ) ;
#31077 = VECTOR ( 'NONE', #67967, 1000.000000000000000 ) ;
#31079 = CARTESIAN_POINT ( 'NONE',  ( 107.6517678568360594, -47.10594642807022581, 152.6213395616249500 ) ) ;
#31080 = DIRECTION ( 'NONE',  ( -0.7759704746411383303, 0.6307692307692303046, 0.000000000000000000 ) ) ;
#31081 = CARTESIAN_POINT ( 'NONE',  ( 95.23138046818854718, -37.33356364299761054, 267.3670538473395482 ) ) ;
#31082 = CARTESIAN_POINT ( 'NONE',  ( 158.0667039024469886, -67.87844715994090450, 190.2178068554179902 ) ) ;
#31083 = CARTESIAN_POINT ( 'NONE',  ( -130.2664984484596005, 73.28356282573680858, -8.694507028640293456 ) ) ;
#31084 = VERTEX_POINT ( 'NONE', #72511 ) ;
#31085 = EDGE_LOOP ( 'NONE', ( #63550, #87615, #83282, #28153, #71511 ) ) ;
#31086 = EDGE_CURVE ( 'NONE', #21942, #41501, #78447, .T. ) ;
#31087 = CARTESIAN_POINT ( 'NONE',  ( 97.36106687025375095, -40.65520290104787904, 206.6327681330539860 ) ) ;
#31088 = ORIENTED_EDGE ( 'NONE', *, *, #10674, .F. ) ;
#31089 = CARTESIAN_POINT ( 'NONE',  ( 113.5652313304969567, -44.92653082429684730, 168.1099109901969939 ) ) ;
#31090 = CARTESIAN_POINT ( 'NONE',  ( 112.1380301846104146, -28.01206920713002191, 264.6564718616416485 ) ) ;
#31091 = FACE_BOUND ( 'NONE', #66150, .T. ) ;
#31092 = CARTESIAN_POINT ( 'NONE',  ( 83.56670559755357885, -33.43837296219067667, 249.5838068554176630 ) ) ;
#31093 = CARTESIAN_POINT ( 'NONE',  ( 143.8252070173663810, -140.2851082128090070, 246.7259429745822388 ) ) ;
#31096 = CARTESIAN_POINT ( 'NONE',  ( 96.93559702949583823, -34.21358363697174099, 272.1327681330538439 ) ) ;
#31095 = CYLINDRICAL_SURFACE ( 'NONE', #65890, 4.500000000000003553 ) ;
#31094 = FACE_OUTER_BOUND ( 'NONE', #45078, .T. ) ;
#31097 = DIRECTION ( 'NONE',  ( 0.000000000000000000, -1.000000000000000000, 0.000000000000000000 ) ) ;
#31098 = DIRECTION ( 'NONE',  ( -0.0001713722456133526934, 0.9999999853157766072, 0.000000000000000000 ) ) ;
#31099 = DIRECTION ( 'NONE',  ( 1.000000000000000078E-15, 0.000000000000000000, 1.000000000000000000 ) ) ;
#31100 = CARTESIAN_POINT ( 'NONE',  ( 67.71624685027074975, -137.3191804951919437, 246.9862057923735392 ) ) ;
#31101 = PLANE ( 'NONE',  #43054 ) ;
#31102 = FACE_OUTER_BOUND ( 'NONE', #82043, .T. ) ;
#31104 = VERTEX_POINT ( 'NONE', #44328 ) ;
#31103 = CARTESIAN_POINT ( 'NONE',  ( 111.2166545661128652, -43.61238145012286083, 195.5838068554168672 ) ) ;
#31105 = CARTESIAN_POINT ( 'NONE',  ( 84.06648329127399677, -18.82844715994099971, 17.92562527591199739 ) ) ;
#31106 = CARTESIAN_POINT ( 'NONE',  ( 117.4484615961127218, -30.96329225543088270, 179.2299109901959753 ) ) ;
#31107 = CARTESIAN_POINT ( 'NONE',  ( 109.9110140596799425, -46.79572638734455126, 68.79562527591099297 ) ) ;
#31108 = CARTESIAN_POINT ( 'NONE',  ( 116.9665165100108908, -41.74809644303882550, 244.4651490854349731 ) ) ;
#31109 = DIRECTION ( 'NONE',  ( 0.000000000000000000, 1.000000000000000000, 0.000000000000000000 ) ) ;
#31110 = CARTESIAN_POINT ( 'NONE',  ( 41.56670390244695312, -36.32844715994109208, 129.9678068554150911 ) ) ;
#31112 = LINE ( 'NONE', #38823, #35617 ) ;
#31111 = CARTESIAN_POINT ( 'NONE',  ( 67.06670390244701707, -83.77844715994098124, 45.21780685541799727 ) ) ;
#31113 = LINE ( 'NONE', #86554, #27660 ) ;
#31114 = DIRECTION ( 'NONE',  ( -0.000000000000000000, 1.000000000000000000, 0.000000000000000000 ) ) ;
#31115 = AXIS2_PLACEMENT_3D ( 'NONE', #49535, #16388, #64974 ) ;
#31116 = PLANE ( 'NONE',  #703 ) ;
#31117 =( BOUNDED_CURVE ( )  B_SPLINE_CURVE ( 3, ( #37732, #51771, #9575, #23230 ),
 .UNSPECIFIED., .F., .T. ) 
 B_SPLINE_CURVE_WITH_KNOTS ( ( 4, 4 ),
 ( 1.570796326780094843, 3.141592653577910621 ),
 .UNSPECIFIED. ) 
 CURVE ( )  GEOMETRIC_REPRESENTATION_ITEM ( )  RATIONAL_B_SPLINE_CURVE ( ( 1.000000000000000000, 0.8047378541236769323, 0.8047378541236769323, 1.000000000000000000 ) ) 
 REPRESENTATION_ITEM ( '' )  );
#31118 = AXIS2_PLACEMENT_3D ( 'NONE', #74902, #40815, #14473 ) ;
#31119 = EDGE_LOOP ( 'NONE', ( #38496, #25442, #48878, #68007 ) ) ;
#31120 = VERTEX_POINT ( 'NONE', #23916 ) ;
#31121 = ADVANCED_FACE ( 'NONE', ( #72061 ), #51588, .T. ) ;
#31122 = CARTESIAN_POINT ( 'NONE',  ( 103.7110576214454341, -44.58420688232069296, 91.67813411379100330 ) ) ;
#31124 = ORIENTED_EDGE ( 'NONE', *, *, #30489, .T. ) ;
#31123 = CARTESIAN_POINT ( 'NONE',  ( -1.653891986036712280, 95.16955141394549855, -130.5480982590283645 ) ) ;
#31125 = ADVANCED_FACE ( 'NONE', ( #31154 ), #46558, .T. ) ;
#31126 = CARTESIAN_POINT ( 'NONE',  ( 104.2200364793041700, -25.25138339198311144, 86.26991099019699050 ) ) ;
#31127 = DIRECTION ( 'NONE',  ( -0.7071067811865470176, 2.110218113313392652E-14, 0.7071067811865480168 ) ) ;
#31128 = EDGE_CURVE ( 'NONE', #62792, #26105, #4801, .T. ) ;
#31129 = CARTESIAN_POINT ( 'NONE',  ( 248.6659999999999968, 52.73749999999999716, -2.903194600000015502 ) ) ;
#31130 = CARTESIAN_POINT ( 'NONE',  ( 41.56648329127499153, -32.07844715994070839, 134.1756252759119832 ) ) ;
#31131 = ADVANCED_FACE ( 'NONE', ( #11622 ), #54704, .F. ) ;
#31132 = CARTESIAN_POINT ( 'NONE',  ( 101.7353989658528661, -28.52926574610319932, 25.53562527591096654 ) ) ;
#31133 = ORIENTED_EDGE ( 'NONE', *, *, #76473, .T. ) ;
#31134 = ORIENTED_EDGE ( 'NONE', *, *, #66383, .F. ) ;
#31135 = ORIENTED_EDGE ( 'NONE', *, *, #60949, .T. ) ;
#31136 = CYLINDRICAL_SURFACE ( 'NONE', #87750, 2.500000000000002220 ) ;
#31137 = CIRCLE ( 'NONE', #81930, 16.00000000000090239 ) ;
#31138 = CARTESIAN_POINT ( 'NONE',  ( 107.0664832912748068, -36.72944715993923381, -4.074374724089028454 ) ) ;
#31139 = CARTESIAN_POINT ( 'NONE',  ( 98.34985891665434110, -31.65658480256832519, 116.9064586086046376 ) ) ;
#31140 = CIRCLE ( 'NONE', #45570, 218.1859999999999786 ) ;
#31141 = CARTESIAN_POINT ( 'NONE',  ( 91.91125933621933086, -100.4807974291317691, -21.78219314458213063 ) ) ;
#31142 = DIRECTION ( 'NONE',  ( 0.000000000000000000, 0.000000000000000000, 1.000000000000000000 ) ) ;
#31143 = CARTESIAN_POINT ( 'NONE',  ( 0.8398470015645936870, 69.84999999999999432, -130.5559999999999832 ) ) ;
#31144 = EDGE_CURVE ( 'NONE', #42921, #34489, #27869, .T. ) ;
#31146 = CARTESIAN_POINT ( 'NONE',  ( 41.56648329127398966, -27.82844715994070484, 315.9256252759120116 ) ) ;
#31145 = VECTOR ( 'NONE', #73777, 1000.000000000000000 ) ;
#31147 = AXIS2_PLACEMENT_3D ( 'NONE', #83217, #41400, #69129 ) ;
#31148 = CARTESIAN_POINT ( 'NONE',  ( -0.7868074802740107065, 95.24999999999995737, 130.5560000000000400 ) ) ;
#31149 = CARTESIAN_POINT ( 'NONE',  ( 101.1541078795467996, -28.12664281037970682, 50.55562527591095545 ) ) ;
#31150 = ORIENTED_EDGE ( 'NONE', *, *, #12848, .T. ) ;
#31151 = EDGE_LOOP ( 'NONE', ( #78104, #24665, #29684, #11069, #64776 ) ) ;
#31152 = PLANE ( 'NONE',  #67650 ) ;
#31153 = PLANE ( 'NONE',  #1131 ) ;
#31154 = FACE_OUTER_BOUND ( 'NONE', #63891, .T. ) ;
#31155 = CARTESIAN_POINT ( 'NONE',  ( 111.9717725103620722, -43.25385221418022752, 140.9080903695919460 ) ) ;
#31156 = AXIS2_PLACEMENT_3D ( 'NONE', #88759, #74230, #82401 ) ;
#31157 = CARTESIAN_POINT ( 'NONE',  ( 213.7409999999999854, 52.73749999999999716, -44.45000000000000284 ) ) ;
#31158 = VERTEX_POINT ( 'NONE', #81127 ) ;
#31159 = EDGE_LOOP ( 'NONE', ( #56171, #24391, #64437, #31608 ) ) ;
#31160 = DIRECTION ( 'NONE',  ( -1.000000000000000000, -1.561055996379579722E-16, 0.000000000000000000 ) ) ;
#31161 = VERTEX_POINT ( 'NONE', #33396 ) ;
#31162 = ORIENTED_EDGE ( 'NONE', *, *, #45145, .T. ) ;
#31163 = LINE ( 'NONE', #46568, #20190 ) ;
#31164 = CARTESIAN_POINT ( 'NONE',  ( 117.1060311394199402, -37.55296641157723769, 185.1930118773259437 ) ) ;
#31165 = CARTESIAN_POINT ( 'NONE',  ( 135.9998166246059839, 12.92155284005730387, 355.9756252759109998 ) ) ;
#31166 = EDGE_CURVE ( 'NONE', #13980, #62710, #68474, .T. ) ;
#31167 = CARTESIAN_POINT ( 'NONE',  ( 107.0664832912739399, -36.72944715994095333, 311.6356252759109680 ) ) ;
#31168 = CARTESIAN_POINT ( 'NONE',  ( 99.50480724682302025, -43.30587341447913019, 16.89607863635162488 ) ) ;
#31169 = ORIENTED_EDGE ( 'NONE', *, *, #38012, .T. ) ;
#31170 = CIRCLE ( 'NONE', #71794, 3.250000000000002665 ) ;
#31171 = ORIENTED_EDGE ( 'NONE', *, *, #5909, .T. ) ;
#31172 = ORIENTED_EDGE ( 'NONE', *, *, #25584, .T. ) ;
#31173 = EDGE_CURVE ( 'NONE', #7552, #59397, #32937, .T. ) ;
#31174 = CARTESIAN_POINT ( 'NONE',  ( 102.6495774910181780, -44.17201850306531696, 204.9804713219729706 ) ) ;
#31175 = CARTESIAN_POINT ( 'NONE',  ( 96.90545716317438973, -39.15842060370329847, 56.51276813305394597 ) ) ;
#31176 = CARTESIAN_POINT ( 'NONE',  ( 115.6551466294303623, -43.65033472170377138, 43.27467289495795200 ) ) ;
#31177 = DIRECTION ( 'NONE',  ( 9.351236661543306751E-17, -3.725950533538267725E-29, -1.000000000000000000 ) ) ;
#31178 = FACE_BOUND ( 'NONE', #80996, .T. ) ;
#31179 = DIRECTION ( 'NONE',  ( 0.000000000000000000, -1.000000000000000000, 0.000000000000000000 ) ) ;
#31180 = CARTESIAN_POINT ( 'NONE',  ( 114.1750726078950890, -45.19361863149571690, 144.1203871806729637 ) ) ;
#31181 = DIRECTION ( 'NONE',  ( 1.000000000000000078E-15, 0.000000000000000000, 1.000000000000000000 ) ) ;
#31182 = VERTEX_POINT ( 'NONE', #61097 ) ;
#31183 = DIRECTION ( 'NONE',  ( 0.000000000000000000, 0.000000000000000000, 1.000000000000000000 ) ) ;
#31184 = VERTEX_POINT ( 'NONE', #74735 ) ;
#31185 = DIRECTION ( 'NONE',  ( 0.7071067811862258301, -0.7071067811868692043, 7.071067811862265655E-16 ) ) ;
#31186 = CARTESIAN_POINT ( 'NONE',  ( -487.2989999999999782, 21.43125000000029701, 15.23694598552314972 ) ) ;
#31187 = EDGE_LOOP ( 'NONE', ( #15008, #46776, #74650, #4362 ) ) ;
#31188 = CIRCLE ( 'NONE', #80556, 1.000000000000000888 ) ;
#31189 = DIRECTION ( 'NONE',  ( 0.000000000000000000, -1.000000000000000000, 0.000000000000000000 ) ) ;
#31190 = EDGE_CURVE ( 'NONE', #3872, #37614, #26142, .T. ) ;
#31191 = AXIS2_PLACEMENT_3D ( 'NONE', #66305, #43630, #31793 ) ;
#31192 = VECTOR ( 'NONE', #3886, 1000.000000000000000 ) ;
#31193 = DIRECTION ( 'NONE',  ( 0.000000000000000000, 0.000000000000000000, 1.000000000000000000 ) ) ;
#31194 = CARTESIAN_POINT ( 'NONE',  ( 109.6430426817424433, -46.83134659365198615, 47.77562527591094721 ) ) ;
#31195 = DIRECTION ( 'NONE',  ( -1.000000000000000000, 0.000000000000000000, 0.000000000000000000 ) ) ;
#31196 = AXIS2_PLACEMENT_3D ( 'NONE', #43232, #17338, #65913 ) ;
#31197 = CARTESIAN_POINT ( 'NONE',  ( 25.56670390244797275, -48.82844715994099971, 173.2178068554149775 ) ) ;
#31198 = DIRECTION ( 'NONE',  ( 1.365069428641121829E-15, 0.000000000000000000, 1.000000000000000000 ) ) ;
#31199 = CARTESIAN_POINT ( 'NONE',  ( 104.9021620152489191, -46.26774620671726268, 72.39848241876894974 ) ) ;
#31201 = CARTESIAN_POINT ( 'NONE',  ( 117.3921119255896599, -35.46056622170122807, 189.9241967044829664 ) ) ;
#31200 = DIRECTION ( 'NONE',  ( 3.100000000000000258E-29, -3.100000000000000044E-14, -1.000000000000000000 ) ) ;
#31202 = CARTESIAN_POINT ( 'NONE',  ( 48.86082318535585500, -35.55794170701788204, 193.9678068554150911 ) ) ;
#31203 = DIRECTION ( 'NONE',  ( 2.170915417798913171E-16, 0.000000000000000000, 1.000000000000000000 ) ) ;
#31204 = ORIENTED_EDGE ( 'NONE', *, *, #86122, .F. ) ;
#31205 = PLANE ( 'NONE',  #77351 ) ;
#31206 = AXIS2_PLACEMENT_3D ( 'NONE', #31220, #25301, #11225 ) ;
#31207 = CARTESIAN_POINT ( 'NONE',  ( 146.0667039024470455, -121.7784471599409102, 45.21780685541799727 ) ) ;
#31208 = CARTESIAN_POINT ( 'NONE',  ( 97.75871328428027596, -40.38572213467175231, 136.6247029066429377 ) ) ;
#31209 = VECTOR ( 'NONE', #16287, 1000.000000000000000 ) ;
#31210 = EDGE_CURVE ( 'NONE', #45792, #83969, #52893, .T. ) ;
#31211 = CARTESIAN_POINT ( 'NONE',  ( 172.5664832912740110, -18.82844715994099971, 198.9256252759119832 ) ) ;
#31213 = EDGE_LOOP ( 'NONE', ( #86268, #68583, #44777, #75892 ) ) ;
#31212 = CARTESIAN_POINT ( 'NONE',  ( 96.07878916947804271, -35.15354693665655361, 226.2251490854349640 ) ) ;
#31214 = DIRECTION ( 'NONE',  ( 0.000000000000000000, 0.000000000000000000, -1.000000000000000000 ) ) ;
#31215 = CARTESIAN_POINT ( 'NONE',  ( 111.1359251431956210, -27.10775802199072970, 240.7584824187679544 ) ) ;
#31216 = CARTESIAN_POINT ( 'NONE',  ( 111.8139374584311554, -25.81739915606283375, 130.7499109901969518 ) ) ;
#31217 = CARTESIAN_POINT ( 'NONE',  ( 131.3179999999999836, 53.97500000000000142, 71.43750000000000000 ) ) ;
#31218 = CARTESIAN_POINT ( 'NONE',  ( 82.81519967300334883, -36.82419990104791196, 6.751707299519725147 ) ) ;
#31219 = CIRCLE ( 'NONE', #48573, 3.250000000000002665 ) ;
#31220 = CARTESIAN_POINT ( 'NONE',  ( -54.12775174896490427, 55.97500000000000142, 69.87310403134814862 ) ) ;
#31221 = DIRECTION ( 'NONE',  ( 3.999999999999999995E-14, -1.000000000000000000, 4.100000000000000342E-29 ) ) ;
#31222 = ORIENTED_EDGE ( 'NONE', *, *, #76871, .T. ) ;
#31223 = VECTOR ( 'NONE', #36021, 1000.000000000000000 ) ;
#31224 = ORIENTED_EDGE ( 'NONE', *, *, #9184, .F. ) ;
#31225 = EDGE_LOOP ( 'NONE', ( #57342, #3206, #59125, #88114 ) ) ;
#31226 = ORIENTED_EDGE ( 'NONE', *, *, #83344, .T. ) ;
#31227 = CARTESIAN_POINT ( 'NONE',  ( 99.04406184532244595, -42.84125762267669302, 71.84395860752657370 ) ) ;
#31228 = CARTESIAN_POINT ( 'NONE',  ( 99.33320739591177073, -28.83195234130426243, 266.7051490854347549 ) ) ;
#31229 = CARTESIAN_POINT ( 'NONE',  ( 188.5667039024479834, -48.82844715994099971, 259.9678068554150059 ) ) ;
#31230 = CARTESIAN_POINT ( 'NONE',  ( 131.3834856945509841, -36.12003772029553517, 3.004064388422954313 ) ) ;
#31231 = ADVANCED_FACE ( 'NONE', ( #61533 ), #12965, .F. ) ;
#31233 = CARTESIAN_POINT ( 'NONE',  ( 76.79083731950140645, 74.16215221268211621, 90.32738470895372984 ) ) ;
#31232 = CARTESIAN_POINT ( 'NONE',  ( 97.81169150544869240, -40.51741169384158781, 71.63577594787710723 ) ) ;
#31234 = CARTESIAN_POINT ( 'NONE',  ( 102.3821975904229333, -44.47993990548584975, 201.5543245899819738 ) ) ;
#31235 = ORIENTED_EDGE ( 'NONE', *, *, #33941, .F. ) ;
#31236 = ORIENTED_EDGE ( 'NONE', *, *, #60728, .F. ) ;
#31237 = AXIS2_PLACEMENT_3D ( 'NONE', #65268, #80252, #86612 ) ;
#31238 = VERTEX_POINT ( 'NONE', #25231 ) ;
#31239 = CARTESIAN_POINT ( 'NONE',  ( 31.78666935232950408, -29.62846900982343001, 313.9678068554150059 ) ) ;
#31240 = VECTOR ( 'NONE', #19711, 1000.000000000000000 ) ;
#31241 = CARTESIAN_POINT ( 'NONE',  ( 57.56670390244732260, -42.82844715994040996, 175.7178068554150911 ) ) ;
#31242 = DIRECTION ( 'NONE',  ( 0.7071067811866377228, -0.7071067811864573116, 0.000000000000000000 ) ) ;
#31243 = CARTESIAN_POINT ( 'NONE',  ( 114.3297541623348224, -29.74979092151301074, 35.86729759161094933 ) ) ;
#31244 = CARTESIAN_POINT ( 'NONE',  ( 118.5560163110023524, 95.25015226514366873, 0.4098827902177066274 ) ) ;
#31245 = ADVANCED_FACE ( 'NONE', ( #87475 ), #4356, .T. ) ;
#31246 = CARTESIAN_POINT ( 'NONE',  ( 116.3212776292296127, -32.94146857471318413, 249.5838068554167535 ) ) ;
#31247 = EDGE_CURVE ( 'NONE', #41448, #35668, #51081, .T. ) ;
#31248 = DIRECTION ( 'NONE',  ( 0.9999999853157766072, 0.0001713722456143218888, 0.000000000000000000 ) ) ;
#31249 = ORIENTED_EDGE ( 'NONE', *, *, #20438, .F. ) ;
#31250 = CARTESIAN_POINT ( 'NONE',  ( 97.12559044764091709, -37.99707808599399783, 57.42728215261879399 ) ) ;
#31251 = ORIENTED_EDGE ( 'NONE', *, *, #30863, .T. ) ;
#31252 = DIRECTION ( 'NONE',  ( 0.000000000000000000, -1.000000000000000000, 0.000000000000000000 ) ) ;
#31253 = CARTESIAN_POINT ( 'NONE',  ( 116.6500553765360451, -33.62673909641207359, 280.5072975916113478 ) ) ;
#31254 = AXIS2_PLACEMENT_3D ( 'NONE', #59050, #87675, #66321 ) ;
#31255 = AXIS2_PLACEMENT_3D ( 'NONE', #19627, #19190, #88246 ) ;
#31256 = AXIS2_PLACEMENT_3D ( 'NONE', #88810, #26563, #20656 ) ;
#31257 = CARTESIAN_POINT ( 'NONE',  ( 136.7925547069177128, -18.36732994130890262, 6.785344856282517156 ) ) ;
#31258 = AXIS2_PLACEMENT_3D ( 'NONE', #4455, #46658, #52998 ) ;
#31259 = DIRECTION ( 'NONE',  ( 0.000000000000000000, 1.000000000000000000, 0.000000000000000000 ) ) ;
#31260 = DIRECTION ( 'NONE',  ( 0.7071067811868696484, 0.7071067811862253860, 7.071067811869001541E-16 ) ) ;
#31261 = AXIS2_PLACEMENT_3D ( 'NONE', #44288, #37499, #86104 ) ;
#31262 = VERTEX_POINT ( 'NONE', #67917 ) ;
#31263 = DIRECTION ( 'NONE',  ( 0.000000000000000000, 0.000000000000000000, 1.000000000000000000 ) ) ;
#31264 = CARTESIAN_POINT ( 'NONE',  ( 122.3615910276390650, 60.60584201542124561, -45.52561893181081132 ) ) ;
#31265 = VERTEX_POINT ( 'NONE', #46105 ) ;
#31266 = CARTESIAN_POINT ( 'NONE',  ( 99.05404782812107101, -43.39937282746017644, 116.8784824187679732 ) ) ;
#31267 = ORIENTED_EDGE ( 'NONE', *, *, #54579, .T. ) ;
#31268 = CARTESIAN_POINT ( 'NONE',  ( 98.58513254605244924, -37.74079342042374918, 40.84384839950494239 ) ) ;
#31269 = VECTOR ( 'NONE', #22440, 1000.000000000000000 ) ;
#31270 = CARTESIAN_POINT ( 'NONE',  ( 31.75000000000000000, 104.3431970271542042, -3.174999999999999822 ) ) ;
#31271 = CARTESIAN_POINT ( 'NONE',  ( 109.4844142153598057, -45.28606679814626546, 69.22729759161194352 ) ) ;
#31272 = CARTESIAN_POINT ( 'NONE',  ( 112.0649019730212643, -45.48895927759898683, 13.98970061351897343 ) ) ;
#31273 = DIRECTION ( 'NONE',  ( 1.000000000000000000, 0.000000000000000000, 9.868649107779159826E-16 ) ) ;
#31274 = CARTESIAN_POINT ( 'NONE',  ( 112.7841083645756015, -67.87923500319460857, 246.2950307662580087 ) ) ;
#31275 = AXIS2_PLACEMENT_3D ( 'NONE', #42625, #13161, #14051 ) ;
#31276 = CARTESIAN_POINT ( 'NONE',  ( 114.8356066511136504, -43.71357066064707197, 34.24419670448197905 ) ) ;
#31277 = CARTESIAN_POINT ( 'NONE',  ( 0.000000000000000000, 127.0000000000000000, -188.9759999999999991 ) ) ;
#31278 = VERTEX_POINT ( 'NONE', #54250 ) ;
#31279 = DIRECTION ( 'NONE',  ( -0.7071067811864671926, -0.7071067811866279529, 2.899137802865059124E-29 ) ) ;
#31280 = ORIENTED_EDGE ( 'NONE', *, *, #44463, .T. ) ;
#31281 = DIRECTION ( 'NONE',  ( 0.7071067811868710917, -0.7071067811862240537, 0.000000000000000000 ) ) ;
#31282 = EDGE_LOOP ( 'NONE', ( #30528, #33211, #81327, #38182 ) ) ;
#31283 = VECTOR ( 'NONE', #63187, 1000.000000000000000 ) ;
#31284 = ORIENTED_EDGE ( 'NONE', *, *, #55580, .T. ) ;
#31285 = EDGE_CURVE ( 'NONE', #77101, #24431, #7593, .T. ) ;
#31286 = CYLINDRICAL_SURFACE ( 'NONE', #17407, 3.299999999999997158 ) ;
#31287 = CARTESIAN_POINT ( 'NONE',  ( 117.3720538532507618, -35.57445771113444977, 233.9032443235299752 ) ) ;
#31288 = DIRECTION ( 'NONE',  ( 1.000000000000000000, 0.000000000000000000, 0.000000000000000000 ) ) ;
#31289 = CARTESIAN_POINT ( 'NONE',  ( 89.92341143738899234, -67.87844715994096134, 245.7176246693439907 ) ) ;
#31290 = CARTESIAN_POINT ( 'NONE',  ( 107.6068523407233926, -48.56763185392661342, 38.61276813305397582 ) ) ;
#31291 = CARTESIAN_POINT ( 'NONE',  ( 97.81825285133052716, -40.53342921643464081, 42.63700214333596250 ) ) ;
#31292 = VERTEX_POINT ( 'NONE', #5704 ) ;
#31293 = CARTESIAN_POINT ( 'NONE',  ( 97.80396622205201140, -40.49851628999532949, 172.6339998519910637 ) ) ;
#31294 = CARTESIAN_POINT ( 'NONE',  ( 0.000000000000000000, 44.45000000000000284, 0.000000000000000000 ) ) ;
#31295 = ORIENTED_EDGE ( 'NONE', *, *, #32765, .F. ) ;
#31296 = DIRECTION ( 'NONE',  ( 0.000000000000000000, -1.000000000000000000, 0.000000000000000000 ) ) ;
#31297 = EDGE_CURVE ( 'NONE', #71309, #8142, #88381, .T. ) ;
#31298 = CYLINDRICAL_SURFACE ( 'NONE', #81779, 1.000000000002049694 ) ;
#31300 = AXIS2_PLACEMENT_3D ( 'NONE', #39329, #87048, #67477 ) ;
#31299 = CARTESIAN_POINT ( 'NONE',  ( 111.1189502094635202, -27.14789314160929479, 244.7584824187679544 ) ) ;
#31301 = DIRECTION ( 'NONE',  ( 0.7967329428042202455, -0.6043315462976655006, 1.875669758399919831E-14 ) ) ;
#31302 = ADVANCED_FACE ( 'NONE', ( #33841 ), #40654, .F. ) ;
#31303 = DIRECTION ( 'NONE',  ( 0.000000000000000000, 0.000000000000000000, 1.000000000000000000 ) ) ;
#31304 = CARTESIAN_POINT ( 'NONE',  ( 98.30761769748181678, -41.72907704524488537, 91.73956018709316140 ) ) ;
#31305 = CARTESIAN_POINT ( 'NONE',  ( 114.8253727231603136, -41.39981172478538696, 277.8057531614101663 ) ) ;
#31307 = CARTESIAN_POINT ( 'NONE',  ( 117.5733473178507467, -42.15660255127702527, 89.44705384733997278 ) ) ;
#31306 = FACE_OUTER_BOUND ( 'NONE', #37325, .T. ) ;
#31308 = CARTESIAN_POINT ( 'NONE',  ( 109.7396867053641643, 59.36954314920819797, 70.72544642611300958 ) ) ;
#31309 = CARTESIAN_POINT ( 'NONE',  ( 99.65330034922125435, -46.03930839343899351, 122.0413395616249659 ) ) ;
#31310 = VERTEX_POINT ( 'NONE', #20226 ) ;
#31311 = CARTESIAN_POINT ( 'NONE',  ( 132.2129280580766135, -20.76093376057972861, 7.655955902696334192 ) ) ;
#31312 = ORIENTED_EDGE ( 'NONE', *, *, #24127, .T. ) ;
#31313 = EDGE_CURVE ( 'NONE', #74351, #54782, #73384, .T. ) ;
#31314 = FACE_BOUND ( 'NONE', #9394, .T. ) ;
#31315 = LINE ( 'NONE', #9552, #53677 ) ;
#31316 = CYLINDRICAL_SURFACE ( 'NONE', #61580, 3.000000000000002665 ) ;
#31317 = ORIENTED_EDGE ( 'NONE', *, *, #61869, .T. ) ;
#31318 = EDGE_CURVE ( 'NONE', #11860, #3381, #1121, .T. ) ;
#31319 = ADVANCED_FACE ( 'NONE', ( #28832 ), #63344, .F. ) ;
#31320 = LINE ( 'NONE', #72678, #34582 ) ;
#31322 = ORIENTED_EDGE ( 'NONE', *, *, #51347, .T. ) ;
#31321 = CARTESIAN_POINT ( 'NONE',  ( 107.9493508131109962, -25.66448314884807047, 115.0251490854349612 ) ) ;
#31323 = DIRECTION ( 'NONE',  ( 0.7071067812158990940, 0.7071067811571960515, 0.000000000000000000 ) ) ;
#31324 = DIRECTION ( 'NONE',  ( -1.000000000000000000, 0.000000000000000000, 0.000000000000000000 ) ) ;
#31325 = EDGE_CURVE ( 'NONE', #45648, #20355, #70612, .T. ) ;
#31327 = AXIS2_PLACEMENT_3D ( 'NONE', #48785, #76515, #27465 ) ;
#31326 = CARTESIAN_POINT ( 'NONE',  ( 0.000000000000000000, 82.54999999999999716, 206.3750000000000000 ) ) ;
#31328 = ORIENTED_EDGE ( 'NONE', *, *, #61982, .F. ) ;
#31329 = CARTESIAN_POINT ( 'NONE',  ( 116.6186327310674500, -29.67321183330947321, 109.3327681330539605 ) ) ;
#31330 = AXIS2_PLACEMENT_3D ( 'NONE', #35828, #8138, #6785 ) ;
#31331 = AXIS2_PLACEMENT_3D ( 'NONE', #97, #55024, #69589 ) ;
#31332 =( NAMED_UNIT ( * ) SI_UNIT ( $, .STERADIAN. ) SOLID_ANGLE_UNIT ( ) );
#31333 = CIRCLE ( 'NONE', #82132, 13.49999999999999822 ) ;
#31334 = ADVANCED_FACE ( 'NONE', ( #28365 ), #61986, .T. ) ;
#31335 = DIRECTION ( 'NONE',  ( 0.000000000000000000, 1.000000000000000000, 0.000000000000000000 ) ) ;
#31336 = CARTESIAN_POINT ( 'NONE',  ( 137.8897065959775716, -5.906223855237799469, 14.67562527591100263 ) ) ;
#31337 = DIRECTION ( 'NONE',  ( 0.000000000000000000, 0.000000000000000000, 1.000000000000000000 ) ) ;
#31338 = CYLINDRICAL_SURFACE ( 'NONE', #77547, 11.17600000000001970 ) ;
#31339 = ORIENTED_EDGE ( 'NONE', *, *, #43528, .T. ) ;
#31340 = ORIENTED_EDGE ( 'NONE', *, *, #64375, .F. ) ;
#31341 = FACE_OUTER_BOUND ( 'NONE', #88202, .T. ) ;
#31342 = CARTESIAN_POINT ( 'NONE',  ( -179.8898777604655095, 101.5999999999999943, -12.69999999999999929 ) ) ;
#31343 = EDGE_CURVE ( 'NONE', #43788, #8973, #17761, .T. ) ;
#31344 = CARTESIAN_POINT ( 'NONE',  ( 40.31648329127400388, 12.92155284005802507, 349.2756252759108406 ) ) ;
#31346 = DIRECTION ( 'NONE',  ( 0.000000000000000000, 0.000000000000000000, -1.000000000000000000 ) ) ;
#31345 = DIRECTION ( 'NONE',  ( 0.000000000000000000, -1.000000000000000000, 0.000000000000000000 ) ) ;
#31347 = CARTESIAN_POINT ( 'NONE',  ( -71.77848634863029531, 120.6499999999999915, -77.39114642430038771 ) ) ;
#31348 = CIRCLE ( 'NONE', #13974, 34.13125000000000142 ) ;
#31349 = ORIENTED_EDGE ( 'NONE', *, *, #45748, .F. ) ;
#31350 = CIRCLE ( 'NONE', #82152, 7.199999999999998401 ) ;
#31351 = DIRECTION ( 'NONE',  ( 0.000000000000000000, 1.000000000000000000, 0.000000000000000000 ) ) ;
#31352 = CARTESIAN_POINT ( 'NONE',  ( 96.59955023297828802, -32.98040794253982000, 172.0527681330529788 ) ) ;
#31354 = ORIENTED_EDGE ( 'NONE', *, *, #78415, .F. ) ;
#31353 = CARTESIAN_POINT ( 'NONE',  ( 67.06670390244701707, -81.17316614790567542, 245.5580738794290028 ) ) ;
#31355 = EDGE_CURVE ( 'NONE', #87708, #16685, #11996, .T. ) ;
#31356 = CARTESIAN_POINT ( 'NONE',  ( 97.95204982468537480, -33.09064556074058316, 37.02419670448192335 ) ) ;
#31358 = ADVANCED_FACE ( 'NONE', ( #75640 ), #56514, .F. ) ;
#31357 = CARTESIAN_POINT ( 'NONE',  ( 97.81362140459485488, -40.52214454336083094, 51.63603076018934956 ) ) ;
#31359 = DIRECTION ( 'NONE',  ( 1.000000000000000000, 4.237773401492740281E-14, 0.000000000000000000 ) ) ;
#31360 = EDGE_CURVE ( 'NONE', #68501, #28780, #67100, .T. ) ;
#31361 = ORIENTED_EDGE ( 'NONE', *, *, #23271, .T. ) ;
#31362 = LINE ( 'NONE', #53568, #38515 ) ;
#31363 = EDGE_CURVE ( 'NONE', #54435, #11233, #55596, .T. ) ;
#31364 = ORIENTED_EDGE ( 'NONE', *, *, #51285, .F. ) ;
#31365 = ORIENTED_EDGE ( 'NONE', *, *, #46869, .T. ) ;
#31366 = CARTESIAN_POINT ( 'NONE',  ( 116.3165111044169038, -35.08217335353153743, 195.3863452106589875 ) ) ;
#31367 = CARTESIAN_POINT ( 'NONE',  ( 182.3467384525650061, -36.02818131005800950, -5.074374724088000832 ) ) ;
#31368 = CARTESIAN_POINT ( 'NONE',  ( 23.04771283656240399, 87.28173361942839392, 302.2699916481048490 ) ) ;
#31369 = CARTESIAN_POINT ( 'NONE',  ( 151.0371591254575208, -24.42818131005592264, 180.4678068554149775 ) ) ;
#31370 = DIRECTION ( 'NONE',  ( 0.000000000000000000, 0.000000000000000000, -1.000000000000000000 ) ) ;
#31371 = ORIENTED_EDGE ( 'NONE', *, *, #37585, .F. ) ;
#31372 = DIRECTION ( 'NONE',  ( -1.000000000000000000, 0.000000000000000000, 0.000000000000000000 ) ) ;
#31373 = CARTESIAN_POINT ( 'NONE',  ( 151.0371591254575208, -24.42818131005592264, 193.9678068554149775 ) ) ;
#31374 = ORIENTED_EDGE ( 'NONE', *, *, #89162, .F. ) ;
#31375 = CARTESIAN_POINT ( 'NONE',  ( 111.5990003564989905, -46.09347164638234062, 247.9356252759109509 ) ) ;
#31376 = FACE_OUTER_BOUND ( 'NONE', #67543, .T. ) ;
#31377 = VERTEX_POINT ( 'NONE', #27919 ) ;
#31378 = CARTESIAN_POINT ( 'NONE',  ( 117.0608945233188507, -38.08045312314173003, 83.71895860905850384 ) ) ;
#31379 = CARTESIAN_POINT ( 'NONE',  ( 0.000000000000000000, 95.14999999999999147, 118.5560000000000116 ) ) ;
#31380 = CARTESIAN_POINT ( 'NONE',  ( 72.96458098368650269, 127.0000000000000000, 65.02708098368729850 ) ) ;
#31381 = DIRECTION ( 'NONE',  ( 1.000000000000000000, 0.000000000000000000, 0.000000000000000000 ) ) ;
#31382 = VECTOR ( 'NONE', #44907, 1000.000000000000000 ) ;
#31383 = CARTESIAN_POINT ( 'NONE',  ( 114.1542194384027908, -29.02509929289194801, 195.4841967044819739 ) ) ;
#31384 = CARTESIAN_POINT ( 'NONE',  ( -187.8075999999999794, 20.32000000000000028, -3.174999999999999822 ) ) ;
#31385 = VERTEX_POINT ( 'NONE', #55149 ) ;
#31386 = AXIS2_PLACEMENT_3D ( 'NONE', #67977, #6208, #28426 ) ;
#31387 = CARTESIAN_POINT ( 'NONE',  ( 107.1959371850970086, -26.26158102413311468, 31.06705384733893283 ) ) ;
#31388 = VECTOR ( 'NONE', #12061, 1000.000000000000000 ) ;
#31389 = DIRECTION ( 'NONE',  ( -0.000000000000000000, -1.000000000000000000, -0.000000000000000000 ) ) ;
#31390 = CARTESIAN_POINT ( 'NONE',  ( 111.8641478345923019, -46.02505481121716002, 272.9556252759110180 ) ) ;
#31391 = EDGE_LOOP ( 'NONE', ( #19958, #37256, #20098, #47489 ) ) ;
#31392 = CARTESIAN_POINT ( 'NONE',  ( 81.48703104220281546, -16.36767655967523893, 1.942446731261492143 ) ) ;
#31393 = CARTESIAN_POINT ( 'NONE',  ( 112.0670051061717771, -45.48779079837375861, 18.99044305992054760 ) ) ;
#31394 = CARTESIAN_POINT ( 'NONE',  ( 104.4067584314151134, -46.45769567148069967, 152.3653096109091791 ) ) ;
#31395 = CARTESIAN_POINT ( 'NONE',  ( 99.83919217201646745, -32.93524248800951426, 133.7595189410199623 ) ) ;
#31396 = CARTESIAN_POINT ( 'NONE',  ( 112.4229354917722787, -46.42447813297522430, 248.9661014663869878 ) ) ;
#31397 = CARTESIAN_POINT ( 'NONE',  ( 80.06648329127399677, 0.2215528400590013880, 296.1531252759119752 ) ) ;
#31398 = ORIENTED_EDGE ( 'NONE', *, *, #37695, .T. ) ;
#31399 = CARTESIAN_POINT ( 'NONE',  ( 135.4847699230674323, -39.08750326150417465, 1.944748881531143336 ) ) ;
#31400 = VERTEX_POINT ( 'NONE', #84257 ) ;
#31401 = ORIENTED_EDGE ( 'NONE', *, *, #13757, .T. ) ;
#31402 = DIRECTION ( 'NONE',  ( 5.512527431108029424E-15, -1.000000000000000000, 0.000000000000000000 ) ) ;
#31403 = ORIENTED_EDGE ( 'NONE', *, *, #53197, .F. ) ;
#31404 = VERTEX_POINT ( 'NONE', #20671 ) ;
#31405 = CYLINDRICAL_SURFACE ( 'NONE', #67167, 0.9999999999999731326 ) ;
#31406 = DIRECTION ( 'NONE',  ( 1.000000000000000078E-15, -1.000000000000000000, 0.000000000000000000 ) ) ;
#31407 = EDGE_CURVE ( 'NONE', #28006, #27158, #75801, .T. ) ;
#31408 = LINE ( 'NONE', #24610, #18480 ) ;
#31409 = CARTESIAN_POINT ( 'NONE',  ( 111.2069583914694419, -45.51165039160690640, 137.3495626852199507 ) ) ;
#31410 = CARTESIAN_POINT ( 'NONE',  ( 104.7257947241298979, -47.57997989614905521, 32.41943479972098174 ) ) ;
#31411 = ORIENTED_EDGE ( 'NONE', *, *, #51314, .T. ) ;
#31412 = EDGE_CURVE ( 'NONE', #53911, #85068, #68816, .T. ) ;
#31413 = CARTESIAN_POINT ( 'NONE',  ( 176.7738106836355314, -48.62134037874481152, 180.4678068554150059 ) ) ;
#31414 = EDGE_LOOP ( 'NONE', ( #50059, #23645, #11840, #81256 ) ) ;
#31415 = ADVANCED_FACE ( 'NONE', ( #218 ), #48338, .F. ) ;
#31416 = ADVANCED_FACE ( 'NONE', ( #69263 ), #43882, .T. ) ;
#31417 = CARTESIAN_POINT ( 'NONE',  ( 90.44969454456408187, -50.04645651782490745, 239.5838068554174356 ) ) ;
#31418 = ORIENTED_EDGE ( 'NONE', *, *, #34820, .T. ) ;
#31419 = DIRECTION ( 'NONE',  ( 1.000000000000000000, 0.000000000000000000, 0.000000000000000000 ) ) ;
#31420 = CARTESIAN_POINT ( 'NONE',  ( 74.98969683741650272, 82.54999999999999716, 346.9005000000000223 ) ) ;
#31421 = LINE ( 'NONE', #25065, #53341 ) ;
#31422 = VECTOR ( 'NONE', #4021, 1000.000000000000227 ) ;
#31423 = EDGE_CURVE ( 'NONE', #11403, #19525, #7040, .T. ) ;
#31424 = DIRECTION ( 'NONE',  ( 0.2588190451025215166, 0.000000000000000000, -0.9659258262890680902 ) ) ;
#31425 = ORIENTED_EDGE ( 'NONE', *, *, #83708, .T. ) ;
#31426 = CARTESIAN_POINT ( 'NONE',  ( 105.3166869522846838, -26.42980843014500181, 15.20991099019697401 ) ) ;
#31427 = CARTESIAN_POINT ( 'NONE',  ( 102.7372881883638058, -25.64480981559214712, 16.37276813305293999 ) ) ;
#31428 = EDGE_CURVE ( 'NONE', #18839, #8744, #14308, .T. ) ;
#31430 = DIRECTION ( 'NONE',  ( 0.000000000000000000, 1.000000000000000000, 1.914177628664063178E-15 ) ) ;
#31429 = CARTESIAN_POINT ( 'NONE',  ( 183.5150000000000148, 53.21300000000000097, 59.96543552338529537 ) ) ;
#31431 = DIRECTION ( 'NONE',  ( 0.000000000000000000, 0.000000000000000000, -1.000000000000000000 ) ) ;
#31432 = LINE ( 'NONE', #59132, #19329 ) ;
#31433 = FACE_OUTER_BOUND ( 'NONE', #46690, .T. ) ;
#31434 = CARTESIAN_POINT ( 'NONE',  ( 51.34673845256598668, -36.02818131005800950, -5.074374724088000832 ) ) ;
#31435 = DIRECTION ( 'NONE',  ( -0.000000000000000000, -1.000000000000000000, -0.000000000000000000 ) ) ;
#31436 = EDGE_CURVE ( 'NONE', #5064, #65413, #35172, .T. ) ;
#31437 = DIRECTION ( 'NONE',  ( 0.000000000000000000, 0.000000000000000000, 1.000000000000000000 ) ) ;
#31438 = CARTESIAN_POINT ( 'NONE',  ( 96.95731234646120811, -39.36592712812080208, 276.5299109901967540 ) ) ;
#31439 = CARTESIAN_POINT ( 'NONE',  ( 96.13817600250692408, -35.07231702426307152, 217.1946728949589840 ) ) ;
#31440 = CARTESIAN_POINT ( 'NONE',  ( 105.9861696881796860, -26.33857706295247070, 46.15848241876796720 ) ) ;
#31441 = AXIS2_PLACEMENT_3D ( 'NONE', #50163, #51065, #9745 ) ;
#31443 = DIRECTION ( 'NONE',  ( -1.000000000000000078E-15, 1.000000000000000083E-30, 1.000000000000000000 ) ) ;
#31442 = DIRECTION ( 'NONE',  ( 0.000000000000000000, 1.000000000000000000, 0.000000000000000000 ) ) ;
#31444 = FACE_OUTER_BOUND ( 'NONE', #44311, .T. ) ;
#31445 = EDGE_CURVE ( 'NONE', #61667, #53177, #18213, .T. ) ;
#31446 = CIRCLE ( 'NONE', #82254, 4.500000000000003553 ) ;
#31447 = CIRCLE ( 'NONE', #43056, 3.300000000000000711 ) ;
#31448 = ORIENTED_EDGE ( 'NONE', *, *, #46902, .F. ) ;
#31449 = FACE_OUTER_BOUND ( 'NONE', #11006, .T. ) ;
#31450 = ORIENTED_EDGE ( 'NONE', *, *, #10017, .T. ) ;
#31451 = CARTESIAN_POINT ( 'NONE',  ( 110.2470682213182300, -46.59973918892927003, 53.83657765686300678 ) ) ;
#31453 = VERTEX_POINT ( 'NONE', #59189 ) ;
#31452 = CARTESIAN_POINT ( 'NONE',  ( -47.02966122971774610, 92.07499999999998863, 74.26049396966043048 ) ) ;
#31454 = DIRECTION ( 'NONE',  ( 1.000000000000000000, 0.000000000000000000, 0.000000000000000000 ) ) ;
#31455 = CARTESIAN_POINT ( 'NONE',  ( 109.6005296801413067, -26.60309369064642127, 195.8813395616249977 ) ) ;
#31456 = CARTESIAN_POINT ( 'NONE',  ( 99.08905494682572623, -42.79484345344285146, 252.8444919503191102 ) ) ;
#31457 = FACE_OUTER_BOUND ( 'NONE', #48596, .T. ) ;
#31458 = LINE ( 'NONE', #78759, #84988 ) ;
#31459 = EDGE_CURVE ( 'NONE', #72895, #36690, #71957, .T. ) ;
#31460 = CARTESIAN_POINT ( 'NONE',  ( 131.5565945955644622, -37.85370728022187592, 2.783021134851944911 ) ) ;
#31461 = FACE_BOUND ( 'NONE', #4623, .T. ) ;
#31462 = CIRCLE ( 'NONE', #32957, 2.124999999999998224 ) ;
#31463 = EDGE_CURVE ( 'NONE', #16883, #26687, #8846, .T. ) ;
#31464 = CARTESIAN_POINT ( 'NONE',  ( 102.3899016914588458, -28.13915478247111679, 145.4727681330539610 ) ) ;
#31465 = ORIENTED_EDGE ( 'NONE', *, *, #6394, .F. ) ;
#31466 = VERTEX_POINT ( 'NONE', #57866 ) ;
#31467 = CARTESIAN_POINT ( 'NONE',  ( 108.9267623252842441, -45.42435897675616019, 104.1758690201829722 ) ) ;
#31468 = CLOSED_SHELL ( 'NONE', ( #89553, #33121, #71545, #20756 ) ) ;
#31469 = LINE ( 'NONE', #59613, #87815 ) ;
#31471 = DIRECTION ( 'NONE',  ( 1.000000000000000078E-15, 0.000000000000000000, -1.000000000000000000 ) ) ;
#31470 = CARTESIAN_POINT ( 'NONE',  ( 112.6571330189592430, -45.46348522128858605, 214.0175300378159591 ) ) ;
#31472 = FACE_OUTER_BOUND ( 'NONE', #27497, .T. ) ;
#31473 = CARTESIAN_POINT ( 'NONE',  ( -487.2989999999999782, 22.53639197104660141, 90.48749999999999716 ) ) ;
#31474 = CARTESIAN_POINT ( 'NONE',  ( 117.8738102209305936, 81.72118090664554302, 12.70000000000123030 ) ) ;
#31475 = CARTESIAN_POINT ( 'NONE',  ( -12.69999999999999574, 82.13551494250060614, 117.8738102209306930 ) ) ;
#31476 = CARTESIAN_POINT ( 'NONE',  ( 181.5667039024459939, -18.82844715994099971, -5.074374724088000832 ) ) ;
#31477 = LINE ( 'NONE', #24239, #45830 ) ;
#31478 = CARTESIAN_POINT ( 'NONE',  ( 117.4355769707883468, -40.49052663852281597, 173.5375300378159693 ) ) ;
#31479 = VERTEX_POINT ( 'NONE', #22919 ) ;
#31480 = ORIENTED_EDGE ( 'NONE', *, *, #26490, .T. ) ;
#31481 = CARTESIAN_POINT ( 'NONE',  ( 141.6666952063141878, -69.41153784729984011, 247.5000682988239760 ) ) ;
#31482 = CARTESIAN_POINT ( 'NONE',  ( 77.38348569455060044, -18.12003772028603876, 3.004064388423441478 ) ) ;
#31483 = CARTESIAN_POINT ( 'NONE',  ( 101.9936209266849119, -45.44607153056026760, 78.15645860795193300 ) ) ;
#31484 = CARTESIAN_POINT ( 'NONE',  ( 184.5667039024483245, -48.82844715993448403, 300.4678068554149490 ) ) ;
#31485 = VECTOR ( 'NONE', #5828, 1000.000000000000000 ) ;
#31486 = VECTOR ( 'NONE', #39488, 1000.000000000000000 ) ;
#31487 = EDGE_CURVE ( 'NONE', #78352, #45673, #42444, .T. ) ;
#31488 = CARTESIAN_POINT ( 'NONE',  ( 113.1782861458026730, -44.75187455886691623, 269.0939578440578543 ) ) ;
#31489 = CARTESIAN_POINT ( 'NONE',  ( 96.04647588134957914, -35.87007288833441976, 191.2765776568629690 ) ) ;
#31490 = DIRECTION ( 'NONE',  ( 0.000000000000000000, 1.000000000000000000, 0.000000000000000000 ) ) ;
#31491 = ORIENTED_EDGE ( 'NONE', *, *, #81916, .F. ) ;
#31493 = ORIENTED_EDGE ( 'NONE', *, *, #86270, .F. ) ;
#31492 = ORIENTED_EDGE ( 'NONE', *, *, #19410, .T. ) ;
#31494 = CARTESIAN_POINT ( 'NONE',  ( 97.82290962912863108, -40.54474197294914717, 62.63844076402585870 ) ) ;
#31495 = CARTESIAN_POINT ( 'NONE',  ( 165.6738106836030227, -28.98061976758901892, -5.074374724088000832 ) ) ;
#31496 = DIRECTION ( 'NONE',  ( 0.000000000000000000, 0.000000000000000000, 1.000000000000000000 ) ) ;
#31497 = CARTESIAN_POINT ( 'NONE',  ( 98.43690990026183840, -34.58641363334965035, 272.5644404487542829 ) ) ;
#31498 = DIRECTION ( 'NONE',  ( 0.000000000000000000, 0.000000000000000000, -1.000000000000000000 ) ) ;
#31499 = ORIENTED_EDGE ( 'NONE', *, *, #30193, .F. ) ;
#31500 = VECTOR ( 'NONE', #5660, 1000.000000000000000 ) ;
#31501 = CIRCLE ( 'NONE', #82314, 7.999999999999992895 ) ;
#31502 = CARTESIAN_POINT ( 'NONE',  ( 165.9667039024452038, -28.27351298637401200, 342.9256252759109884 ) ) ;
#31503 = ADVANCED_FACE ( 'NONE', ( #65130 ), #51477, .F. ) ;
#31504 = DIRECTION ( 'NONE',  ( 3.100000000000000258E-29, -3.100000000000000044E-14, -1.000000000000000000 ) ) ;
#31505 = EDGE_LOOP ( 'NONE', ( #81294, #43020, #34556 ) ) ;
#31506 = EDGE_LOOP ( 'NONE', ( #75178, #21655, #64804, #64897 ) ) ;
#31507 = VECTOR ( 'NONE', #56805, 1000.000000000000000 ) ;
#31508 = AXIS2_PLACEMENT_3D ( 'NONE', #12632, #33063, #60764 ) ;
#31509 = DIRECTION ( 'NONE',  ( -0.000000000000000000, 1.000000000000000000, 0.000000000000000000 ) ) ;
#31510 = AXIS2_PLACEMENT_3D ( 'NONE', #37434, #71524, #84264 ) ;
#31511 = ORIENTED_EDGE ( 'NONE', *, *, #70196, .F. ) ;
#31512 = EDGE_LOOP ( 'NONE', ( #8014, #19842, #40828, #38227, #81162, #82040 ) ) ;
#31513 = CARTESIAN_POINT ( 'NONE',  ( 99.09507348882337396, -30.55127953124758378, 156.8021594390647238 ) ) ;
#31514 = EDGE_CURVE ( 'NONE', #9965, #39484, #32268, .T. ) ;
#31515 = ADVANCED_FACE ( 'NONE', ( #44670, #17431 ), #38309, .F. ) ;
#31516 = CARTESIAN_POINT ( 'NONE',  ( 111.1942201901869680, -30.05669425270436790, 287.4538046553057029 ) ) ;
#31517 = CARTESIAN_POINT ( 'NONE',  ( 118.9025049541195358, -37.70032671045152028, 188.7613395616259595 ) ) ;
#31518 = EDGE_CURVE ( 'NONE', #15446, #52251, #3797, .T. ) ;
#31519 = CARTESIAN_POINT ( 'NONE',  ( 97.44537786355540732, -42.12371753947140007, 181.7451490854349743 ) ) ;
#31520 = CYLINDRICAL_SURFACE ( 'NONE', #69891, 2.517500000000005844 ) ;
#31521 = CARTESIAN_POINT ( 'NONE',  ( 118.1075207852818068, -36.21034067742461815, 264.8518157521014587 ) ) ;
#31522 = LINE ( 'NONE', #37016, #61734 ) ;
#31523 = DIRECTION ( 'NONE',  ( 0.000000000000000000, 0.000000000000000000, -1.000000000000000000 ) ) ;
#31524 = ORIENTED_EDGE ( 'NONE', *, *, #87252, .T. ) ;
#31525 = AXIS2_PLACEMENT_3D ( 'NONE', #7194, #34884, #42138 ) ;
#31526 = ADVANCED_FACE ( 'NONE', ( #77877 ), #64687, .F. ) ;
#31527 = EDGE_LOOP ( 'NONE', ( #20752, #21781 ) ) ;
#31528 = VECTOR ( 'NONE', #8263, 1000.000000000000000 ) ;
#31529 = CIRCLE ( 'NONE', #21373, 7.999999999999992895 ) ;
#31531 = EDGE_CURVE ( 'NONE', #55564, #65795, #16539, .T. ) ;
#31530 = VECTOR ( 'NONE', #74173, 1000.000000000000000 ) ;
#31532 = CARTESIAN_POINT ( 'NONE',  ( 130.3998166246070127, 12.92155284005802685, 336.5756252759110225 ) ) ;
#31533 = CARTESIAN_POINT ( 'NONE',  ( 95.24515967180828113, -38.10243856675759133, 236.4184824187679510 ) ) ;
#31534 = EDGE_LOOP ( 'NONE', ( #53944, #62478, #82674, #78997 ) ) ;
#31535 = CARTESIAN_POINT ( 'NONE',  ( 117.1261863205049423, -33.86823216992616636, 149.0470538473389581 ) ) ;
#31536 = DIRECTION ( 'NONE',  ( -0.7071067811865849873, 0.7071067811865101582, 0.000000000000000000 ) ) ;
#31537 = CARTESIAN_POINT ( 'NONE',  ( -13.28435107523728220, 68.09058761799009574, 35.73330652649276828 ) ) ;
#31538 = DIRECTION ( 'NONE',  ( 0.000000000000000000, -1.000000000000000000, 0.000000000000000000 ) ) ;
#31539 = DIRECTION ( 'NONE',  ( 0.000000000000000000, 0.000000000000000000, -1.000000000000000000 ) ) ;
#31542 = CARTESIAN_POINT ( 'NONE',  ( 116.5166575185068467, -42.41785904284974862, 274.3832443235299365 ) ) ;
#31541 = CARTESIAN_POINT ( 'NONE',  ( -13.40680633928205090, 223.9999999999999716, 102.7987842159323293 ) ) ;
#31540 = LINE ( 'NONE', #59243, #18674 ) ;
#31543 = FACE_OUTER_BOUND ( 'NONE', #37021, .T. ) ;
#31545 = EDGE_CURVE ( 'NONE', #82808, #45317, #39538, .T. ) ;
#31544 = DIRECTION ( 'NONE',  ( 0.000000000000000000, -1.000000000000000000, 0.000000000000000000 ) ) ;
#31546 = DIRECTION ( 'NONE',  ( 0.7071067811865157093, 0.7071067811865794361, 7.071067811865148942E-16 ) ) ;
#31547 = DIRECTION ( 'NONE',  ( 0.000000000000000000, 1.000000000000000000, 0.000000000000000000 ) ) ;
#31548 = CARTESIAN_POINT ( 'NONE',  ( 123.6837132603318707, -18.85368780205705619, 218.8274735512161158 ) ) ;
#31549 = CARTESIAN_POINT ( 'NONE',  ( -47.02966122971774610, 92.07499999999998863, 74.26049396966043048 ) ) ;
#31551 = ORIENTED_EDGE ( 'NONE', *, *, #65643, .F. ) ;
#31550 = CARTESIAN_POINT ( 'NONE',  ( 98.79997750155241931, -33.98483017033598941, 195.5838068554174356 ) ) ;
#31552 = DIRECTION ( 'NONE',  ( 2.900000000000000265E-14, -2.000000000000000155E-15, 1.000000000000000000 ) ) ;
#31553 = CARTESIAN_POINT ( 'NONE',  ( 98.41658590534017037, -29.81029140585139814, 195.7775300378159784 ) ) ;
#31554 = CARTESIAN_POINT ( 'NONE',  ( 99.05421528594702352, -43.39923342774125814, 112.8784824187679732 ) ) ;
#31555 = CARTESIAN_POINT ( 'NONE',  ( 99.05265045910354615, -29.93853425193624318, 211.7670538473399517 ) ) ;
#31556 = DIRECTION ( 'NONE',  ( 5.512527431108029424E-15, -1.000000000000000000, 0.000000000000000000 ) ) ;
#31557 = DIRECTION ( 'NONE',  ( 1.000000000000000078E-15, -1.000000000000000083E-30, -1.000000000000000000 ) ) ;
#31559 = CARTESIAN_POINT ( 'NONE',  ( 107.8235642108959382, -46.74791189189382834, 38.63593913708626815 ) ) ;
#31558 = DIRECTION ( 'NONE',  ( -1.000000000000000078E-15, 1.000000000000000083E-30, 1.000000000000000000 ) ) ;
#31560 = DIRECTION ( 'NONE',  ( 0.000000000000000000, 0.000000000000000000, 1.000000000000000000 ) ) ;
#31561 = CARTESIAN_POINT ( 'NONE',  ( -2.684158038187649039E-15, 69.84999999999999432, 130.5560000000000116 ) ) ;
#31562 = CIRCLE ( 'NONE', #4006, 0.5000000000000004441 ) ;
#31563 = CARTESIAN_POINT ( 'NONE',  ( 98.35024246080324417, -31.65587940141233148, 65.90773501403860735 ) ) ;
#31564 = ORIENTED_EDGE ( 'NONE', *, *, #77303, .F. ) ;
#31565 = ORIENTED_EDGE ( 'NONE', *, *, #74108, .T. ) ;
#31566 = CARTESIAN_POINT ( 'NONE',  ( 115.9223471279375843, -38.62321220144315248, 108.0933722090289564 ) ) ;
#31568 = VERTEX_POINT ( 'NONE', #32834 ) ;
#31567 = DIRECTION ( 'NONE',  ( -1.000000000000000000, 0.000000000000000000, -1.047445008332813989E-14 ) ) ;
#31569 = CARTESIAN_POINT ( 'NONE',  ( 98.16825066461163374, -43.24752039522706326, 102.8175300378159847 ) ) ;
#31570 = LINE ( 'NONE', #88800, #74402 ) ;
#31571 = CARTESIAN_POINT ( 'NONE',  ( 77.33253953643593093, -18.38432368373347359, 6.774690158159028641 ) ) ;
#31572 = CARTESIAN_POINT ( 'NONE',  ( 97.31584370704455011, -39.30597596449835862, 177.5314586064030209 ) ) ;
#31573 = AXIS2_PLACEMENT_3D ( 'NONE', #86169, #87060, #58878 ) ;
#31574 = EDGE_CURVE ( 'NONE', #6845, #88991, #26034, .T. ) ;
#31575 = CARTESIAN_POINT ( 'NONE',  ( 97.46604185887800043, -38.76544784714115366, 31.49276813305495892 ) ) ;
#31576 = ORIENTED_EDGE ( 'NONE', *, *, #60162, .T. ) ;
#31577 = ORIENTED_EDGE ( 'NONE', *, *, #18536, .F. ) ;
#31578 = VERTEX_POINT ( 'NONE', #81466 ) ;
#31579 = VECTOR ( 'NONE', #37168, 1000.000000000000000 ) ;
#31580 = VECTOR ( 'NONE', #89691, 1000.000000000000000 ) ;
#31581 = LINE ( 'NONE', #24780, #16690 ) ;
#31583 = CARTESIAN_POINT ( 'NONE',  ( 164.7830935719574939, -29.99615139351707782, 237.4678068554150059 ) ) ;
#31582 = CARTESIAN_POINT ( 'NONE',  ( 111.5019814087853405, -26.53443175268790100, 130.7499109901969518 ) ) ;
#31584 = DIRECTION ( 'NONE',  ( 2.900000000000000265E-14, -2.000000000000000155E-15, 1.000000000000000000 ) ) ;
#31585 = CARTESIAN_POINT ( 'NONE',  ( 12.37530111100094743, 79.66613297688917328, -129.9681797613511947 ) ) ;
#31586 = B_SPLINE_CURVE_WITH_KNOTS ( 'NONE', 3,
 ( #6474, #33737, #60074, #13300, #46889, #61873, #4693, #40989, #89607, #27365, #82355, #33290, #54144, #75072, #32374, #25572, #68708, #47791 ),
 .UNSPECIFIED., .F., .F.,
 ( 4, 2, 2, 2, 2, 2, 2, 2, 4 ),
 ( 0.000000000000000000, 0.06250874477208767654, 0.1250174895441753531, 0.1875262343162630296, 0.2500349790883507062, 0.3125437238604384382, 0.3750524686325260593, 0.4375612134046134027, 0.5000699581767007462 ),
 .UNSPECIFIED. ) ;
#31587 = LINE ( 'NONE', #38849, #25698 ) ;
#31588 = VECTOR ( 'NONE', #7149, 1000.000000000000000 ) ;
#31589 = CARTESIAN_POINT ( 'NONE',  ( -4.941314120920629271, 94.24933258371393663, 130.4624588263053226 ) ) ;
#31590 = DIRECTION ( 'NONE',  ( -4.237773401492740281E-14, 1.000000000000000000, 0.000000000000000000 ) ) ;
#31591 = CARTESIAN_POINT ( 'NONE',  ( 116.2124334422530865, -31.77159869865914388, 69.22133956162495849 ) ) ;
#31592 = ORIENTED_EDGE ( 'NONE', *, *, #61363, .F. ) ;
#31593 = VERTEX_POINT ( 'NONE', #67346 ) ;
#31594 = AXIS2_PLACEMENT_3D ( 'NONE', #29096, #9106, #50415 ) ;
#31595 = CARTESIAN_POINT ( 'NONE',  ( 9.270409258063832425, 91.24028187096000408, 130.2267823906806541 ) ) ;
#31596 = DIRECTION ( 'NONE',  ( 0.000000000000000000, -1.000000000000000000, 0.000000000000000000 ) ) ;
#31597 = AXIS2_PLACEMENT_3D ( 'NONE', #59062, #23259, #66332 ) ;
#31598 = AXIS2_PLACEMENT_3D ( 'NONE', #66384, #86854, #24617 ) ;
#31599 = CARTESIAN_POINT ( 'NONE',  ( 80.34435516212749917, -97.56809487397644887, 250.2178068554179902 ) ) ;
#31600 = CARTESIAN_POINT ( 'NONE',  ( 112.9083776113003665, -30.34675141079074834, 152.2928522743529527 ) ) ;
#31601 = VECTOR ( 'NONE', #43191, 1000.000000000000000 ) ;
#31602 = EDGE_CURVE ( 'NONE', #15550, #55635, #81905, .T. ) ;
#31603 = DIRECTION ( 'NONE',  ( 0.000000000000000000, 0.000000000000000000, 1.000000000000000000 ) ) ;
#31604 = ORIENTED_EDGE ( 'NONE', *, *, #83743, .T. ) ;
#31605 = ORIENTED_EDGE ( 'NONE', *, *, #37990, .F. ) ;
#31606 = CARTESIAN_POINT ( 'NONE',  ( 93.91125933621933086, -96.68314769832137756, -21.78219314458224076 ) ) ;
#31607 = VERTEX_POINT ( 'NONE', #88275 ) ;
#31608 = ORIENTED_EDGE ( 'NONE', *, *, #33842, .F. ) ;
#31609 = CARTESIAN_POINT ( 'NONE',  ( 34.67381068360400320, -28.98061976758901892, -5.074374724088000832 ) ) ;
#31610 = PRODUCT_RELATED_PRODUCT_CATEGORY ( 'part', '', ( #38722 ) ) ;
#31611 = CARTESIAN_POINT ( 'NONE',  ( 106.5710281304903901, -26.66837221057895846, 191.5472975916109704 ) ) ;
#31612 = FACE_OUTER_BOUND ( 'NONE', #33158, .T. ) ;
#31613 = AXIS2_PLACEMENT_3D ( 'NONE', #50485, #30060, #16432 ) ;
#31614 = CARTESIAN_POINT ( 'NONE',  ( 115.0889047326819536, -30.61763669310897029, 119.3439586080126276 ) ) ;
#31615 = VECTOR ( 'NONE', #20184, 1000.000000000000000 ) ;
#31616 = DIRECTION ( 'NONE',  ( 0.000000000000000000, 1.000000000000000000, 0.000000000000000000 ) ) ;
#31617 = ORIENTED_EDGE ( 'NONE', *, *, #80865, .F. ) ;
#31618 = ORIENTED_EDGE ( 'NONE', *, *, #73381, .F. ) ;
#31619 = EDGE_LOOP ( 'NONE', ( #67982, #61575, #72802, #31931 ) ) ;
#31620 = ORIENTED_EDGE ( 'NONE', *, *, #4489, .T. ) ;
#31621 = ADVANCED_FACE ( 'NONE', ( #33291 ), #11960, .F. ) ;
#31622 = CARTESIAN_POINT ( 'NONE',  ( 105.0207293620135118, -28.82725652202227096, 198.0966617981629554 ) ) ;
#31623 = CARTESIAN_POINT ( 'NONE',  ( 97.91311022844104173, -31.62022761154550210, 110.9213395616259703 ) ) ;
#31624 = EDGE_CURVE ( 'NONE', #25804, #3896, #35186, .T. ) ;
#31625 = CARTESIAN_POINT ( 'NONE',  ( 112.8057071037347754, -27.31004523576145360, 49.62895860924498947 ) ) ;
#31626 =( LENGTH_UNIT ( ) NAMED_UNIT ( * ) SI_UNIT ( .MILLI., .METRE. ) );
#31627 = CARTESIAN_POINT ( 'NONE',  ( 90.06670390244701707, -101.5893827172046002, -9.937637710810113489 ) ) ;
#31628 = DIRECTION ( 'NONE',  ( 0.000000000000000000, 0.000000000000000000, 1.000000000000000000 ) ) ;
#31629 = EDGE_CURVE ( 'NONE', #54188, #77895, #87808, .T. ) ;
#31630 = CARTESIAN_POINT ( 'NONE',  ( 117.3100215237039805, -34.79230872694400034, 154.9756252759109714 ) ) ;
#31631 = CARTESIAN_POINT ( 'NONE',  ( -487.2989999999999782, 93.66249999999999432, 11.11250000000040217 ) ) ;
#31632 = VERTEX_POINT ( 'NONE', #52788 ) ;
#31633 = DIRECTION ( 'NONE',  ( 1.000000000000000000, 0.000000000000000000, 0.000000000000000000 ) ) ;
#31634 = VERTEX_POINT ( 'NONE', #24686 ) ;
#31635 = EDGE_CURVE ( 'NONE', #24467, #54402, #85990, .T. ) ;
#31636 = ORIENTED_EDGE ( 'NONE', *, *, #50908, .F. ) ;
#31637 = CARTESIAN_POINT ( 'NONE',  ( 41.56648329127399677, -9.303447159940999356, 138.9256252759119832 ) ) ;
#31638 = ORIENTED_EDGE ( 'NONE', *, *, #8057, .F. ) ;
#31639 = ORIENTED_EDGE ( 'NONE', *, *, #61882, .F. ) ;
#31640 = CYLINDRICAL_SURFACE ( 'NONE', #6899, 0.5000000000000129896 ) ;
#31641 = EDGE_CURVE ( 'NONE', #60807, #11982, #52545, .T. ) ;
#31642 = VECTOR ( 'NONE', #10342, 999.9999999999998863 ) ;
#31643 = ORIENTED_EDGE ( 'NONE', *, *, #57990, .T. ) ;
#31644 =( BOUNDED_CURVE ( )  B_SPLINE_CURVE ( 2, ( #55294, #48038, #13987 ),
 .UNSPECIFIED., .F., .T. ) 
 B_SPLINE_CURVE_WITH_KNOTS ( ( 3, 3 ),
 ( 0.000000000000000000, 0.5053286420056770645 ),
 .UNSPECIFIED. ) 
 CURVE ( )  GEOMETRIC_REPRESENTATION_ITEM ( )  RATIONAL_B_SPLINE_CURVE ( ( 1.000000000000000000, 1.009299002520649857, 1.000420656333769864 ) ) 
 REPRESENTATION_ITEM ( '' )  );
#31645 = CARTESIAN_POINT ( 'NONE',  ( 113.9010889189769955, -29.38240039765346978, 130.4802758126486140 ) ) ;
#31646 = CARTESIAN_POINT ( 'NONE',  ( 114.3532617768494504, -44.18530993788802874, 73.19276813305397411 ) ) ;
#31647 = DIRECTION ( 'NONE',  ( 1.000000000000000078E-15, -1.000000000000000000, 0.000000000000000000 ) ) ;
#31648 = CARTESIAN_POINT ( 'NONE',  ( 25.56670390244797275, -62.87844715994099687, 175.9678068554150059 ) ) ;
#31649 = CARTESIAN_POINT ( 'NONE',  ( 52.99265158129180264, 69.84999999999999432, 346.9005000000000223 ) ) ;
#31650 = CARTESIAN_POINT ( 'NONE',  ( 101.3216544293209864, -28.81361639883581205, 75.57562527591093726 ) ) ;
#31652 = CARTESIAN_POINT ( 'NONE',  ( 114.3286968523003253, -29.23113535793739359, 170.4641967044829585 ) ) ;
#31651 = DIRECTION ( 'NONE',  ( 1.639958061481212836E-42, -4.100000000000000342E-29, -1.000000000000000000 ) ) ;
#31653 = DIRECTION ( 'NONE',  ( 4.299999999999999979E-14, -1.000000000000000000, 4.400000000000000367E-29 ) ) ;
#31655 = ADVANCED_FACE ( 'NONE', ( #66453 ), #73727, .F. ) ;
#31654 = DIRECTION ( 'NONE',  ( -0.7071067811865165975, -0.7071067811865784369, -7.071067811865470403E-16 ) ) ;
#31656 = ORIENTED_EDGE ( 'NONE', *, *, #33079, .F. ) ;
#31657 = CARTESIAN_POINT ( 'NONE',  ( 147.0667039024469886, -67.87844715994090450, 222.2178068554179902 ) ) ;
#31658 = AXIS2_PLACEMENT_3D ( 'NONE', #66003, #58312, #86039 ) ;
#31659 = DIRECTION ( 'NONE',  ( 4.299999999999999979E-14, -1.000000000000000000, 0.000000000000000000 ) ) ;
#31660 = CARTESIAN_POINT ( 'NONE',  ( 0.000000000000000000, 44.45000000000000284, 130.5560000000000116 ) ) ;
#31661 = AXIS2_PLACEMENT_3D ( 'NONE', #87628, #87014, #72493 ) ;
#31662 = CARTESIAN_POINT ( 'NONE',  ( 107.0664832912739968, -14.47844715994100007, 151.4256252759119832 ) ) ;
#31664 = EDGE_LOOP ( 'NONE', ( #15041, #71355, #74745, #19465, #66147 ) ) ;
#31663 = CARTESIAN_POINT ( 'NONE',  ( 118.8398422492546018, -38.46634565031615693, 223.7099109901969598 ) ) ;
#31665 = LINE ( 'NONE', #18477, #62517 ) ;
#31666 = CARTESIAN_POINT ( 'NONE',  ( 99.38090234834324121, -28.75341736348360655, 261.6746728949589169 ) ) ;
#31667 = CARTESIAN_POINT ( 'NONE',  ( 99.65376319600918009, -46.03872712633670972, 118.0413395616259606 ) ) ;
#31668 = CIRCLE ( 'NONE', #21500, 15.69999999999999929 ) ;
#31669 = CARTESIAN_POINT ( 'NONE',  ( 41.56648329127399677, 0.2215528400590013880, 136.8086252759119645 ) ) ;
#31670 = VECTOR ( 'NONE', #12232, 1000.000000000000000 ) ;
#31671 = CYLINDRICAL_SURFACE ( 'NONE', #43162, 10.00000000000000888 ) ;
#31672 = PLANE ( 'NONE',  #28279 ) ;
#31673 = CARTESIAN_POINT ( 'NONE',  ( 115.0366562237703647, -42.90922531116172678, 264.3024214611318143 ) ) ;
#31674 = ORIENTED_EDGE ( 'NONE', *, *, #4765, .T. ) ;
#31675 = ORIENTED_EDGE ( 'NONE', *, *, #44259, .T. ) ;
#31676 = ORIENTED_EDGE ( 'NONE', *, *, #29189, .T. ) ;
#31677 = AXIS2_PLACEMENT_3D ( 'NONE', #45462, #86832, #80929 ) ;
#31678 = VERTEX_POINT ( 'NONE', #25573 ) ;
#31679 = DIRECTION ( 'NONE',  ( -1.000000000000000000, -4.299999999999999979E-14, -1.000000000000000078E-15 ) ) ;
#31680 = CARTESIAN_POINT ( 'NONE',  ( 112.3382693683599314, -28.20726497302192826, 285.6356252759109680 ) ) ;
#31681 = CARTESIAN_POINT ( 'NONE',  ( 0.000000000000000000, 92.07499999999998863, 0.000000000000000000 ) ) ;
#31682 = CARTESIAN_POINT ( 'NONE',  ( 131.5238707403503042, -35.68172011937276267, 2.822018711113692735 ) ) ;
#31684 = CARTESIAN_POINT ( 'NONE',  ( -41.60202597009397607, 40.59999999999997300, 50.85338361873603219 ) ) ;
#31683 = CARTESIAN_POINT ( 'NONE',  ( 122.2221484686747459, -111.8737466215628018, -19.26696060647578435 ) ) ;
#31685 = CIRCLE ( 'NONE', #28787, 2.517500000000005844 ) ;
#31686 = EDGE_CURVE ( 'NONE', #11064, #55190, #60075, .T. ) ;
#31687 = CARTESIAN_POINT ( 'NONE',  ( 98.11275290507195734, -35.37173493080541675, 220.6171817328389864 ) ) ;
#31688 = ORIENTED_EDGE ( 'NONE', *, *, #461, .F. ) ;
#31689 = AXIS2_PLACEMENT_3D ( 'NONE', #38116, #18111, #32180 ) ;
#31690 = ORIENTED_EDGE ( 'NONE', *, *, #45450, .T. ) ;
#31691 = ORIENTED_EDGE ( 'NONE', *, *, #25801, .T. ) ;
#31692 = DIRECTION ( 'NONE',  ( 0.000000000000000000, -1.000000000000000000, 0.000000000000000000 ) ) ;
#31693 = CARTESIAN_POINT ( 'NONE',  ( 99.08980160023928363, -42.79582177768785556, 181.8439945534138076 ) ) ;
#31694 = EDGE_CURVE ( 'NONE', #1382, #14442, #40547, .T. ) ;
#31695 = CARTESIAN_POINT ( 'NONE',  ( -240.5296158183964792, 14.28749999999982201, 85.72499999999999432 ) ) ;
#31696 = CARTESIAN_POINT ( 'NONE',  ( 101.4671292710339117, -29.18466352532158226, 32.02824997256392692 ) ) ;
#31697 = CARTESIAN_POINT ( 'NONE',  ( 117.8738102209308920, 82.54999999999999716, -12.69999999999876827 ) ) ;
#31698 = DIRECTION ( 'NONE',  ( 0.000000000000000000, 0.000000000000000000, -1.000000000000000000 ) ) ;
#31699 = FACE_BOUND ( 'NONE', #50873, .T. ) ;
#31700 = EDGE_LOOP ( 'NONE', ( #89056, #45200, #10619, #74754 ) ) ;
#31701 = VECTOR ( 'NONE', #26186, 1000.000000000000000 ) ;
#31702 = CARTESIAN_POINT ( 'NONE',  ( 103.2764230263689598, -27.47550512461969774, 56.38580517588684415 ) ) ;
#31703 = ORIENTED_EDGE ( 'NONE', *, *, #22526, .T. ) ;
#31704 = CARTESIAN_POINT ( 'NONE',  ( 116.3136297247243078, -32.94478793390952376, 255.1356252759109395 ) ) ;
#31705 = CARTESIAN_POINT ( 'NONE',  ( 109.6406350139562136, -27.81487066565610888, 62.67094751244894724 ) ) ;
#31706 = AXIS2_PLACEMENT_3D ( 'NONE', #7787, #22320, #71374 ) ;
#31707 = AXIS2_PLACEMENT_3D ( 'NONE', #53134, #25467, #10502 ) ;
#31708 = EDGE_CURVE ( 'NONE', #58445, #79084, #37560, .T. ) ;
#31709 = CARTESIAN_POINT ( 'NONE',  ( 107.0664832912739968, -18.82844715994099971, 168.9256252759119832 ) ) ;
#31710 = DIRECTION ( 'NONE',  ( -0.4999999999999998890, -0.8660254037844387076, 0.000000000000000000 ) ) ;
#31711 = CARTESIAN_POINT ( 'NONE',  ( -12.70000000000000462, 83.37936054969095778, 117.8738102209308067 ) ) ;
#31712 = EDGE_LOOP ( 'NONE', ( #81430, #31284, #69996, #77432 ) ) ;
#31713 = DIRECTION ( 'NONE',  ( 0.000000000000000000, 0.000000000000000000, 1.000000000000000000 ) ) ;
#31714 = AXIS2_PLACEMENT_3D ( 'NONE', #71299, #17220, #57641 ) ;
#31715 = FACE_OUTER_BOUND ( 'NONE', #24871, .T. ) ;
#31716 = EDGE_LOOP ( 'NONE', ( #35848, #7398, #71254, #65710, #53882, #53140, #67302, #73023, #20970, #24133, #49223, #72130, #25202, #63245, #52698, #36891, #60555, #28519, #35595, #86497 ) ) ;
#31717 = CARTESIAN_POINT ( 'NONE',  ( 95.48778530930356112, -34.20472165425801592, 106.1556252759109640 ) ) ;
#31718 = EDGE_LOOP ( 'NONE', ( #50907, #74424, #75937, #19983 ) ) ;
#31719 = CARTESIAN_POINT ( 'NONE',  ( 99.71754419879584930, -32.37637629707774778, 85.32384839950596245 ) ) ;
#31720 = AXIS2_PLACEMENT_3D ( 'NONE', #34154, #48219, #23137 ) ;
#31721 = CARTESIAN_POINT ( 'NONE',  ( -148.0533267522759786, 0.000000000000000000, -160.2664750769289697 ) ) ;
#31722 = CARTESIAN_POINT ( 'NONE',  ( 100.6361971157895283, -42.82696290926312344, 78.36158330589692866 ) ) ;
#31723 = CARTESIAN_POINT ( 'NONE',  ( 135.7780479399592366, -20.88970947302825110, 2.099345637358482453 ) ) ;
#31724 = DIRECTION ( 'NONE',  ( 0.000000000000000000, 0.000000000000000000, 1.000000000000000000 ) ) ;
#31725 = AXIS2_PLACEMENT_3D ( 'NONE', #23538, #84425, #76696 ) ;
#31726 = DIRECTION ( 'NONE',  ( 1.000000000000000000, 0.000000000000000000, 0.000000000000000000 ) ) ;
#31727 = CARTESIAN_POINT ( 'NONE',  ( 118.1061288724552725, -37.63024191249119355, 34.77372051400695341 ) ) ;
#31728 = DIRECTION ( 'NONE',  ( -1.000000000000000000, 0.000000000000000000, 0.000000000000000000 ) ) ;
#31729 = EDGE_LOOP ( 'NONE', ( #74955, #67282 ) ) ;
#31730 = CARTESIAN_POINT ( 'NONE',  ( -487.2989999999999782, 85.41360802895360393, 11.11250000000036131 ) ) ;
#31731 = ORIENTED_EDGE ( 'NONE', *, *, #77509, .F. ) ;
#31732 = CARTESIAN_POINT ( 'NONE',  ( -118.3040894999502655, 72.45860812971085352, 7.755682336160878876 ) ) ;
#31733 = ORIENTED_EDGE ( 'NONE', *, *, #31128, .T. ) ;
#31734 = ORIENTED_EDGE ( 'NONE', *, *, #32927, .F. ) ;
#31735 = EDGE_CURVE ( 'NONE', #83342, #72907, #74180, .T. ) ;
#31736 = AXIS2_PLACEMENT_3D ( 'NONE', #26715, #54400, #89869 ) ;
#31737 = FACE_OUTER_BOUND ( 'NONE', #70983, .T. ) ;
#31738 = ORIENTED_EDGE ( 'NONE', *, *, #15350, .T. ) ;
#31739 = CARTESIAN_POINT ( 'NONE',  ( 99.40370404213540212, -29.74227323812493751, 230.7261014663879735 ) ) ;
#31740 = CARTESIAN_POINT ( 'NONE',  ( 97.27692878956830214, -38.81776010764613005, 126.4931294640330179 ) ) ;
#31741 = CARTESIAN_POINT ( 'NONE',  ( 116.3231543710223121, -32.93883412237410369, 190.1356252759109680 ) ) ;
#31742 = EDGE_CURVE ( 'NONE', #60190, #77633, #9636, .T. ) ;
#31743 = CARTESIAN_POINT ( 'NONE',  ( 96.19318211390864803, -38.71572558720041712, 47.48229194257797303 ) ) ;
#31744 = CARTESIAN_POINT ( 'NONE',  ( 97.81533971292206786, -40.52633391481636949, 42.63639178031785093 ) ) ;
#31745 = ORIENTED_EDGE ( 'NONE', *, *, #48131, .T. ) ;
#31746 = CARTESIAN_POINT ( 'NONE',  ( 97.12556571727343169, -37.99690723059678277, 172.4272692053028493 ) ) ;
#31747 = DIRECTION ( 'NONE',  ( 0.000000000000000000, 0.000000000000000000, 1.000000000000000000 ) ) ;
#31749 = ORIENTED_EDGE ( 'NONE', *, *, #68202, .T. ) ;
#31748 = AXIS2_PLACEMENT_3D ( 'NONE', #62304, #54566, #84117 ) ;
#31750 = CARTESIAN_POINT ( 'NONE',  ( 99.48898161933318818, -91.15344715994181968, -11.78219314458242550 ) ) ;
#31751 = CARTESIAN_POINT ( 'NONE',  ( 115.0352363965828886, -42.91102566678780050, 114.3029152670657709 ) ) ;
#31752 = CARTESIAN_POINT ( 'NONE',  ( 101.6619702986602505, -45.61876124157287649, 247.1413395616249602 ) ) ;
#31753 = CARTESIAN_POINT ( 'NONE',  ( 191.6377717143134589, -67.87844715994100397, 307.9888746672805269 ) ) ;
#31754 = DIRECTION ( 'NONE',  ( 0.000000000000000000, -0.000000000000000000, -1.000000000000000000 ) ) ;
#31755 = CARTESIAN_POINT ( 'NONE',  ( 78.15700282949474342, -38.71057579844610075, 2.232988688759218743 ) ) ;
#31756 = CARTESIAN_POINT ( 'NONE',  ( 110.0705912124663968, -28.18614534367760172, 254.2419436376007695 ) ) ;
#31758 = CARTESIAN_POINT ( 'NONE',  ( 103.8480726019013645, -46.65951555449685628, 78.32705384733995402 ) ) ;
#31757 = CARTESIAN_POINT ( 'NONE',  ( 142.0664832912740394, -45.72944715994099596, -4.824374724088994704 ) ) ;
#31759 = CARTESIAN_POINT ( 'NONE',  ( 110.3862196296579299, 62.23620089231086894, 69.71192191839192276 ) ) ;
#31760 = CARTESIAN_POINT ( 'NONE',  ( 97.79690410337100559, -31.86307605613059835, 135.9413395616259947 ) ) ;
#31761 = VERTEX_POINT ( 'NONE', #45542 ) ;
#31763 = EDGE_CURVE ( 'NONE', #86337, #57531, #32375, .T. ) ;
#31762 = CARTESIAN_POINT ( 'NONE',  ( 151.0371591254573218, -24.95799193692592866, 300.4678068554149490 ) ) ;
#31764 = EDGE_LOOP ( 'NONE', ( #54887, #59871, #80485, #15572 ) ) ;
#31765 = FACE_OUTER_BOUND ( 'NONE', #25197, .T. ) ;
#31766 = LINE ( 'NONE', #59462, #76934 ) ;
#31767 = ADVANCED_FACE ( 'NONE', ( #59631 ), #46210, .F. ) ;
#31768 = CARTESIAN_POINT ( 'NONE',  ( 3.110602869834275287E-15, 8.255000000000000782, -25.39999999999999858 ) ) ;
#31769 = VERTEX_POINT ( 'NONE', #13301 ) ;
#31770 = VECTOR ( 'NONE', #22861, 1000.000000000000000 ) ;
#31771 = DIRECTION ( 'NONE',  ( 0.000000000000000000, 0.000000000000000000, -1.000000000000000000 ) ) ;
#31773 = ORIENTED_EDGE ( 'NONE', *, *, #69735, .T. ) ;
#31772 = CARTESIAN_POINT ( 'NONE',  ( 95.97680135624298714, -37.21094296235740018, 116.3489586092439652 ) ) ;
#31774 = CARTESIAN_POINT ( 'NONE',  ( 144.0667052733537901, -71.37844715994090450, 55.21780685541800437 ) ) ;
#31775 = CARTESIAN_POINT ( 'NONE',  ( 80.06648329127399677, 0.2215528400590013880, 2.408125275911999097 ) ) ;
#31777 = CYLINDRICAL_SURFACE ( 'NONE', #7576, 42.54500000000000171 ) ;
#31776 = AXIS2_PLACEMENT_3D ( 'NONE', #79429, #44419, #87119 ) ;
#31778 = ORIENTED_EDGE ( 'NONE', *, *, #53700, .F. ) ;
#31779 = AXIS2_PLACEMENT_3D ( 'NONE', #88838, #60195, #12076 ) ;
#31780 = CARTESIAN_POINT ( 'NONE',  ( 114.0011561472229289, -28.09198494482817310, 119.5261014663869474 ) ) ;
#31781 =( NAMED_UNIT ( * ) SI_UNIT ( $, .STERADIAN. ) SOLID_ANGLE_UNIT ( ) );
#31782 = DIRECTION ( 'NONE',  ( 0.000000000000000000, 1.000000000000000000, 0.000000000000000000 ) ) ;
#31783 = LINE ( 'NONE', #53540, #640 ) ;
#31784 = ORIENTED_EDGE ( 'NONE', *, *, #3455, .T. ) ;
#31785 = AXIS2_PLACEMENT_3D ( 'NONE', #69059, #21822, #63138 ) ;
#31786 = ORIENTED_EDGE ( 'NONE', *, *, #81713, .T. ) ;
#31787 = DIRECTION ( 'NONE',  ( 1.000000000000000078E-15, -1.000000000000000083E-30, -1.000000000000000000 ) ) ;
#31788 = CARTESIAN_POINT ( 'NONE',  ( 172.5664832912729878, -27.57844715994070484, 21.92562527591199739 ) ) ;
#31789 = STYLED_ITEM ( 'NONE', ( #16040 ), #60825 ) ;
#31790 = FACE_OUTER_BOUND ( 'NONE', #72584, .T. ) ;
#31791 = AXIS2_PLACEMENT_3D ( 'NONE', #44614, #64630, #85548 ) ;
#31793 = DIRECTION ( 'NONE',  ( 1.000000000000000000, 0.000000000000000000, 0.000000000000000000 ) ) ;
#31792 = LINE ( 'NONE', #79073, #52282 ) ;
#31794 = FACE_BOUND ( 'NONE', #25214, .T. ) ;
#31795 = ORIENTED_EDGE ( 'NONE', *, *, #3565, .F. ) ;
#31796 = CYLINDRICAL_SURFACE ( 'NONE', #15777, 2.117000000000007987 ) ;
#31797 = EDGE_CURVE ( 'NONE', #21236, #1301, #59490, .T. ) ;
#31798 = CARTESIAN_POINT ( 'NONE',  ( 101.0349934672011614, -27.38958028709088310, 216.5327681330529686 ) ) ;
#31799 = AXIS2_PLACEMENT_3D ( 'NONE', #24948, #4055, #18125 ) ;
#31801 = ORIENTED_EDGE ( 'NONE', *, *, #147, .T. ) ;
#31800 = CARTESIAN_POINT ( 'NONE',  ( 34.67381068360361951, -28.98061976759042224, 117.4678068554150485 ) ) ;
#31802 = CARTESIAN_POINT ( 'NONE',  ( 99.23822674327652749, -42.59304969680523101, 62.83848241876793850 ) ) ;
#31803 = DIRECTION ( 'NONE',  ( 0.000000000000000000, 1.000000000000000000, 0.000000000000000000 ) ) ;
#31804 = CARTESIAN_POINT ( 'NONE',  ( 98.30745885735822753, -41.72869143677799997, 11.73981054624496245 ) ) ;
#31805 = LINE ( 'NONE', #68125, #75030 ) ;
#31806 = ORIENTED_EDGE ( 'NONE', *, *, #63985, .F. ) ;
#31807 = DIRECTION ( 'NONE',  ( -4.440892098500939734E-16, 3.100000000000000044E-14, 1.000000000000000000 ) ) ;
#31808 = ORIENTED_EDGE ( 'NONE', *, *, #40382, .F. ) ;
#31809 = VERTEX_POINT ( 'NONE', #83245 ) ;
#31810 = VECTOR ( 'NONE', #7028, 1000.000000000000000 ) ;
#31811 = CARTESIAN_POINT ( 'NONE',  ( 98.31652346514815122, -35.14820314722400241, 237.6158690201829415 ) ) ;
#31812 = CARTESIAN_POINT ( 'NONE',  ( 193.0371591254582881, -47.82818131005411999, 300.4678068554149490 ) ) ;
#31813 = EDGE_CURVE ( 'NONE', #43969, #25661, #35510, .T. ) ;
#31814 = CARTESIAN_POINT ( 'NONE',  ( -82.89895571708295563, 82.54999999999999716, 100.8594679592209644 ) ) ;
#31815 = FACE_BOUND ( 'NONE', #7356, .T. ) ;
#31816 = CARTESIAN_POINT ( 'NONE',  ( 82.27374021058591325, -38.37320971852818019, 2.471387388685636566 ) ) ;
#31817 = VERTEX_POINT ( 'NONE', #6475 ) ;
#31818 = CARTESIAN_POINT ( 'NONE',  ( 76.06670390244796920, -14.72944715994109899, 199.5838068554169524 ) ) ;
#31819 = CARTESIAN_POINT ( 'NONE',  ( 0.000000000000000000, 124.5870000000000033, 0.000000000000000000 ) ) ;
#31820 = ORIENTED_EDGE ( 'NONE', *, *, #49475, .T. ) ;
#31821 = CARTESIAN_POINT ( 'NONE',  ( 117.4080659314679025, -35.59792815749687378, 278.9127681330539872 ) ) ;
#31822 = CARTESIAN_POINT ( 'NONE',  ( 12.70000000000000284, 83.38917085147761554, 117.8738102209307925 ) ) ;
#31823 = ORIENTED_EDGE ( 'NONE', *, *, #83989, .F. ) ;
#31824 = EDGE_CURVE ( 'NONE', #41012, #55523, #82806, .T. ) ;
#31825 = AXIS2_PLACEMENT_3D ( 'NONE', #61601, #6657, #41602 ) ;
#31826 = EDGE_CURVE ( 'NONE', #638, #36009, #49583, .T. ) ;
#31827 = FACE_BOUND ( 'NONE', #16247, .T. ) ;
#31828 = CARTESIAN_POINT ( 'NONE',  ( 71.25614885437424562, -84.12815644128085069, 396.9756252759102040 ) ) ;
#31829 = DIRECTION ( 'NONE',  ( -0.000000000000000000, 1.000000000000000000, 0.000000000000000000 ) ) ;
#31830 = DIRECTION ( 'NONE',  ( -8.252657816380299978E-16, 0.000000000000000000, -1.000000000000000000 ) ) ;
#31831 = CARTESIAN_POINT ( 'NONE',  ( 113.0470503471827044, -45.36488765107162635, 199.0584824187679374 ) ) ;
#31833 = CARTESIAN_POINT ( 'NONE',  ( 5.590585941178334295, 71.22800506564998102, 118.2263554555544118 ) ) ;
#31832 = AXIS2_PLACEMENT_3D ( 'NONE', #83723, #47610, #54860 ) ;
#31834 = AXIS2_PLACEMENT_3D ( 'NONE', #85164, #17441, #45122 ) ;
#31835 = ORIENTED_EDGE ( 'NONE', *, *, #38184, .F. ) ;
#31836 = CARTESIAN_POINT ( 'NONE',  ( 115.2412948192700952, -44.23743989039658686, 74.22324432352993995 ) ) ;
#31837 = CARTESIAN_POINT ( 'NONE',  ( 71.06670390244705970, -124.7784471599409812, 55.21780685541800437 ) ) ;
#31838 = ADVANCED_FACE ( 'NONE', ( #1010 ), #75971, .F. ) ;
#31839 = ORIENTED_EDGE ( 'NONE', *, *, #41349, .T. ) ;
#31840 = ORIENTED_EDGE ( 'NONE', *, *, #76869, .T. ) ;
#31841 = EDGE_LOOP ( 'NONE', ( #73803, #37420, #18216, #77059 ) ) ;
#31842 = VECTOR ( 'NONE', #2267, 1000.000000000000000 ) ;
#31843 = CARTESIAN_POINT ( 'NONE',  ( 80.06648281188265059, -39.47944715903999224, 8.225259175037734849 ) ) ;
#31844 = DIRECTION ( 'NONE',  ( -1.000000000000000078E-15, -1.000000000000000083E-30, 1.000000000000000000 ) ) ;
#31845 = PLANE ( 'NONE',  #85725 ) ;
#31846 = EDGE_CURVE ( 'NONE', #11788, #57892, #78178, .T. ) ;
#31847 = CARTESIAN_POINT ( 'NONE',  ( 98.42339386660059120, -37.17434067858062008, 119.1976141791149786 ) ) ;
#31848 = CARTESIAN_POINT ( 'NONE',  ( 105.1068790668079203, -26.46800427226792962, 231.2270538473399597 ) ) ;
#31849 = DIRECTION ( 'NONE',  ( 0.000000000000000000, 0.000000000000000000, 1.000000000000000000 ) ) ;
#31850 = ORIENTED_EDGE ( 'NONE', *, *, #64143, .T. ) ;
#31851 = AXIS2_PLACEMENT_3D ( 'NONE', #64488, #50390, #56760 ) ;
#31852 = CARTESIAN_POINT ( 'NONE',  ( 135.2096185787368086, -39.23068377182440969, 1.829869271362987604 ) ) ;
#31853 = ORIENTED_EDGE ( 'NONE', *, *, #8436, .F. ) ;
#31854 = ORIENTED_EDGE ( 'NONE', *, *, #80762, .T. ) ;
#31855 = CARTESIAN_POINT ( 'NONE',  ( 87.06648329127402519, -54.72944906728955061, 14.67562527591094934 ) ) ;
#31856 = VECTOR ( 'NONE', #82387, 1000.000000000000000 ) ;
#31857 = ORIENTED_EDGE ( 'NONE', *, *, #82115, .F. ) ;
#31858 = VERTEX_POINT ( 'NONE', #551 ) ;
#31859 = CARTESIAN_POINT ( 'NONE',  ( 116.7179538190731733, -33.91062837146667164, 10.05229194257760916 ) ) ;
#31860 = LINE ( 'NONE', #87727, #42836 ) ;
#31861 = CARTESIAN_POINT ( 'NONE',  ( -44.45000000000000284, 114.2999999999999972, 257.1750000000000114 ) ) ;
#31862 = AXIS2_PLACEMENT_3D ( 'NONE', #28512, #41685, #82171 ) ;
#31863 = CARTESIAN_POINT ( 'NONE',  ( 108.3628298334300268, -27.77214277553820665, 149.3962293518869444 ) ) ;
#31864 = CARTESIAN_POINT ( 'NONE',  ( 101.5858402103170590, -47.29319095008832363, 17.19562527591095247 ) ) ;
#31865 = ADVANCED_FACE ( 'NONE', ( #40990 ), #24462, .F. ) ;
#31866 = ORIENTED_EDGE ( 'NONE', *, *, #983, .F. ) ;
#31867 = EDGE_CURVE ( 'NONE', #87914, #42451, #21006, .T. ) ;
#31868 = CARTESIAN_POINT ( 'NONE',  ( -89.13771950014300671, 72.45860812971082510, -78.16952835488712026 ) ) ;
#31869 = EDGE_LOOP ( 'NONE', ( #35179, #87068, #66120, #72176 ) ) ;
#31870 = ADVANCED_FACE ( 'NONE', ( #41425 ), #23055, .T. ) ;
#31871 = FACE_OUTER_BOUND ( 'NONE', #67388, .T. ) ;
#31872 = VERTEX_POINT ( 'NONE', #7820 ) ;
#31873 = CARTESIAN_POINT ( 'NONE',  ( 31.75000000000000000, 8.255000000000000782, -3.174999999999999822 ) ) ;
#31874 = EDGE_CURVE ( 'NONE', #62791, #44500, #88345, .T. ) ;
#31875 = CARTESIAN_POINT ( 'NONE',  ( 100.8871230453359686, -44.69993579328431821, 32.05247736852121676 ) ) ;
#31876 = DIRECTION ( 'NONE',  ( 0.000000000000000000, 1.000000000000000000, 0.000000000000000000 ) ) ;
#31877 = VECTOR ( 'NONE', #65120, 1000.000000000000000 ) ;
#31878 = DIRECTION ( 'NONE',  ( 0.000000000000000000, 0.000000000000000000, 1.000000000000000000 ) ) ;
#31879 = ORIENTED_EDGE ( 'NONE', *, *, #32960, .T. ) ;
#31880 = CARTESIAN_POINT ( 'NONE',  ( 111.0547186471684995, -47.06334559972322751, 17.85753003781598380 ) ) ;
#31881 = CARTESIAN_POINT ( 'NONE',  ( 112.2026027939200361, -27.56657145192123082, 30.66991099019694644 ) ) ;
#31883 = CARTESIAN_POINT ( 'NONE',  ( 131.0667039024480118, -61.87844715994100397, 234.8338068554150198 ) ) ;
#31882 = FACE_OUTER_BOUND ( 'NONE', #10299, .T. ) ;
#31884 = LINE ( 'NONE', #82305, #83032 ) ;
#31885 = FACE_OUTER_BOUND ( 'NONE', #21722, .T. ) ;
#31886 = DIRECTION ( 'NONE',  ( 0.7071067811989671936, 0.7071067811741279519, -2.899137802813809155E-29 ) ) ;
#31887 = AXIS2_PLACEMENT_3D ( 'NONE', #23362, #11037, #38738 ) ;
#31888 = CARTESIAN_POINT ( 'NONE',  ( 12.70000000000000107, 82.54999999999999716, 92.46299999999996544 ) ) ;
#31889 = CARTESIAN_POINT ( 'NONE',  ( 182.5667039024476708, -32.29483332967956954, 237.4678068554150059 ) ) ;
#31890 = AXIS2_PLACEMENT_3D ( 'NONE', #19723, #20185, #27429 ) ;
#31891 = CARTESIAN_POINT ( 'NONE',  ( 104.4797840155964082, -46.91084102236943920, 47.37848241876796607 ) ) ;
#31892 = CARTESIAN_POINT ( 'NONE',  ( 97.05822270422260090, -41.42079030513556859, 207.6632443235299661 ) ) ;
#31893 = CARTESIAN_POINT ( 'NONE',  ( 97.78987344453990715, -29.31549002224505429, 41.78991099019596334 ) ) ;
#31895 = DIRECTION ( 'NONE',  ( -0.7071067811864666375, -0.7071067811866283970, -7.071067811864659848E-16 ) ) ;
#31894 = CARTESIAN_POINT ( 'NONE',  ( 107.0664832912750057, -36.72944715993903486, 0.7256252759109708128 ) ) ;
#31896 = DIRECTION ( 'NONE',  ( 0.000000000000000000, 0.000000000000000000, 1.000000000000000000 ) ) ;
#31897 = VECTOR ( 'NONE', #586, 1000.000000000000114 ) ;
#31898 = ORIENTED_EDGE ( 'NONE', *, *, #55622, .F. ) ;
#31899 = PLANE ( 'NONE',  #25816 ) ;
#31900 = VERTEX_POINT ( 'NONE', #69155 ) ;
#31901 = CARTESIAN_POINT ( 'NONE',  ( 109.9668656698224538, -46.07028316908876775, 93.81562527591097478 ) ) ;
#31902 = CIRCLE ( 'NONE', #23260, 2.517500000000005844 ) ;
#31904 = ORIENTED_EDGE ( 'NONE', *, *, #56218, .F. ) ;
#31903 = DIRECTION ( 'NONE',  ( 0.000000000000000000, 0.5000000000000087708, -0.8660254037844336006 ) ) ;
#31905 = LINE ( 'NONE', #54450, #83351 ) ;
#31906 = CARTESIAN_POINT ( 'NONE',  ( 96.83034234600431489, -40.83861266248838007, 247.6422919425769749 ) ) ;
#31907 = DIRECTION ( 'NONE',  ( 0.000000000000000000, -1.000000000000000000, 0.000000000000000000 ) ) ;
#31908 = DIRECTION ( 'NONE',  ( 1.000000000000000078E-15, 0.000000000000000000, 1.000000000000000000 ) ) ;
#31909 = LINE ( 'NONE', #16513, #13832 ) ;
#31910 = CARTESIAN_POINT ( 'NONE',  ( 48.16670390244701139, -28.27351298637280408, -5.074374724088000832 ) ) ;
#31911 = FACE_OUTER_BOUND ( 'NONE', #22962, .T. ) ;
#31912 = CARTESIAN_POINT ( 'NONE',  ( -83.22858459372896789, 79.26455342200334542, 100.5877059554742061 ) ) ;
#31913 = CARTESIAN_POINT ( 'NONE',  ( 104.7173522264389334, -47.59653351925024367, 182.4070538473399665 ) ) ;
#31914 = ORIENTED_EDGE ( 'NONE', *, *, #33050, .T. ) ;
#31915 = ORIENTED_EDGE ( 'NONE', *, *, #79178, .F. ) ;
#31916 = CARTESIAN_POINT ( 'NONE',  ( 98.97073112826979013, -33.12568863208839076, 97.42444044875497866 ) ) ;
#31917 = DIRECTION ( 'NONE',  ( 0.000000000000000000, 0.000000000000000000, 1.000000000000000000 ) ) ;
#31918 = EDGE_CURVE ( 'NONE', #42810, #78790, #38967, .T. ) ;
#31920 = CARTESIAN_POINT ( 'NONE',  ( 172.5664832912740110, -36.32844715994070839, 198.9256252759119832 ) ) ;
#31919 = CARTESIAN_POINT ( 'NONE',  ( 97.41213207386813622, -40.51524797426102253, 242.6118157521009664 ) ) ;
#31921 = CARTESIAN_POINT ( 'NONE',  ( 107.0664832912750057, -36.72944715993903486, 3.024967495036150922 ) ) ;
#31922 = CARTESIAN_POINT ( 'NONE',  ( 182.4202572930269923, -31.94127993907680718, 193.9678068554150059 ) ) ;
#31923 = EDGE_CURVE ( 'NONE', #43506, #76954, #76414, .T. ) ;
#31924 = PRESENTATION_LAYER_ASSIGNMENT (  '', '', ( #72532 ) ) ;
#31925 = CARTESIAN_POINT ( 'NONE',  ( 118.0439878494275945, 76.20320268897036442, 11.00820894928519245 ) ) ;
#31926 = EDGE_CURVE ( 'NONE', #57874, #62557, #13741, .T. ) ;
#31927 = CARTESIAN_POINT ( 'NONE',  ( 51.06648329127400388, 19.62155284005901024, 330.1506252759110680 ) ) ;
#31928 = CARTESIAN_POINT ( 'NONE',  ( 172.5664832912740110, -32.07844715994070839, 18.92562527591200094 ) ) ;
#31929 = CARTESIAN_POINT ( 'NONE',  ( 123.6837132603319418, -53.34645651782485487, 239.5838068554170377 ) ) ;
#31930 = CARTESIAN_POINT ( 'NONE',  ( 117.1759530674219860, -34.27439392744687296, 209.0156252759109634 ) ) ;
#31931 = ORIENTED_EDGE ( 'NONE', *, *, #76554, .F. ) ;
#31932 = VERTEX_POINT ( 'NONE', #34626 ) ;
#31933 = EDGE_CURVE ( 'NONE', #1202, #1599, #77315, .T. ) ;
#31934 = ADVANCED_FACE ( 'NONE', ( #82356 ), #79588, .F. ) ;
#31935 = CARTESIAN_POINT ( 'NONE',  ( 63.03715912545643363, -24.42818131006026761, 129.9678068554150911 ) ) ;
#31936 = CARTESIAN_POINT ( 'NONE',  ( 146.0886660495907279, -68.82006323756704091, 247.2209606857130950 ) ) ;
#31937 = CARTESIAN_POINT ( 'NONE',  ( 0.000000000000000000, 238.5000000000000000, 154.6557476874258441 ) ) ;
#31938 = DIRECTION ( 'NONE',  ( 0.000000000000000000, 0.000000000000000000, 1.000000000000000000 ) ) ;
#31939 = CONICAL_SURFACE ( 'NONE', #82748, 16.33514202138212923, 0.7853981633974482790 ) ;
#31940 = ADVANCED_FACE ( 'NONE', ( #83689 ), #7377, .F. ) ;
#31941 = VERTEX_POINT ( 'NONE', #16433 ) ;
#31942 = DIRECTION ( 'NONE',  ( -0.7071067811865433539, -0.7071067811865516806, -7.071067811865440820E-16 ) ) ;
#31943 = EDGE_CURVE ( 'NONE', #70423, #55559, #81088, .T. ) ;
#31944 = CARTESIAN_POINT ( 'NONE',  ( 102.8439234467419965, -46.26134197790700853, 177.2441967044819648 ) ) ;
#31945 = FACE_OUTER_BOUND ( 'NONE', #36454, .T. ) ;
#31946 = ORIENTED_EDGE ( 'NONE', *, *, #11171, .F. ) ;
#31948 = ORIENTED_EDGE ( 'NONE', *, *, #54791, .T. ) ;
#31947 = ORIENTED_EDGE ( 'NONE', *, *, #18224, .T. ) ;
#31949 = VECTOR ( 'NONE', #60298, 999.9999999999998863 ) ;
#31950 = CARTESIAN_POINT ( 'NONE',  ( 97.83437608159194099, -40.57245513861558095, 62.64082807836916800 ) ) ;
#31951 = PLANE ( 'NONE',  #8652 ) ;
#31952 = CARTESIAN_POINT ( 'NONE',  ( 97.86671988816787859, -40.64955957847482182, 166.6470179981232036 ) ) ;
#31953 = EDGE_CURVE ( 'NONE', #31900, #19378, #29165, .T. ) ;
#31954 = CARTESIAN_POINT ( 'NONE',  ( 102.4274780401303531, -29.97946060242000144, 48.37380465530593909 ) ) ;
#31955 = CIRCLE ( 'NONE', #85681, 1.000000000000000888 ) ;
#31956 = CARTESIAN_POINT ( 'NONE',  ( 164.9667039024477333, -28.27351298636832055, 117.4678068554150485 ) ) ;
#31957 = ORIENTED_EDGE ( 'NONE', *, *, #29017, .T. ) ;
#31958 = CARTESIAN_POINT ( 'NONE',  ( 163.0664832912739826, 25.62155284005901379, 327.8006252759110453 ) ) ;
#31959 = CARTESIAN_POINT ( 'NONE',  ( 82.79255470691722962, -18.36732994130672836, 6.785344856283117565 ) ) ;
#31960 = ORIENTED_EDGE ( 'NONE', *, *, #75155, .F. ) ;
#31962 = ORIENTED_EDGE ( 'NONE', *, *, #20808, .T. ) ;
#31961 = AXIS2_PLACEMENT_3D ( 'NONE', #27752, #33673, #55434 ) ;
#31963 = DIRECTION ( 'NONE',  ( -1.047445008332813989E-14, 0.000000000000000000, -1.000000000000000000 ) ) ;
#31964 = ORIENTED_EDGE ( 'NONE', *, *, #62386, .T. ) ;
#31965 = VERTEX_POINT ( 'NONE', #79564 ) ;
#31966 = LINE ( 'NONE', #59659, #70278 ) ;
#31967 = CARTESIAN_POINT ( 'NONE',  ( 99.32879058785749748, -33.04431300321336806, 75.39527697093394920 ) ) ;
#31968 = CARTESIAN_POINT ( 'NONE',  ( 117.9717084303226500, -34.78741065070708061, 198.9546728949589749 ) ) ;
#31969 = CARTESIAN_POINT ( 'NONE',  ( 117.0473132972741865, -39.66401662079137225, 183.5984824187679578 ) ) ;
#31971 = CARTESIAN_POINT ( 'NONE',  ( 114.4150145978633049, -27.43247436093422920, 270.5441967044823741 ) ) ;
#31970 = LINE ( 'NONE', #46025, #44687 ) ;
#31972 = DIRECTION ( 'NONE',  ( 0.000000000000000000, 0.000000000000000000, -1.000000000000000000 ) ) ;
#31973 = DIRECTION ( 'NONE',  ( 0.000000000000000000, 1.000000000000000000, 0.000000000000000000 ) ) ;
#31974 = EDGE_LOOP ( 'NONE', ( #86393, #57121, #73854, #42192 ) ) ;
#31975 = EDGE_CURVE ( 'NONE', #50744, #31593, #40400, .T. ) ;
#31976 = VERTEX_POINT ( 'NONE', #2360 ) ;
#31977 = EDGE_CURVE ( 'NONE', #33306, #40190, #85040, .T. ) ;
#31978 = CARTESIAN_POINT ( 'NONE',  ( 175.4414832912740110, 12.92155284005802685, 335.5992267699913327 ) ) ;
#31979 = CARTESIAN_POINT ( 'NONE',  ( 117.8217860357262481, -31.63511105064214490, 214.1784824187679419 ) ) ;
#31980 = ORIENTED_EDGE ( 'NONE', *, *, #74084, .T. ) ;
#31981 = CARTESIAN_POINT ( 'NONE',  ( 96.19116125691978425, -32.02117184027007113, 211.0013395616249738 ) ) ;
#31982 = LINE ( 'NONE', #60122, #44248 ) ;
#31983 = CARTESIAN_POINT ( 'NONE',  ( -16.16525963187149983, 66.64697067941781938, 34.50616615423284372 ) ) ;
#31984 = CARTESIAN_POINT ( 'NONE',  ( 41.56670390244777735, -36.32844715994104234, 300.4678068554150059 ) ) ;
#31985 = DIRECTION ( 'NONE',  ( -0.7071067811875165754, -0.7071067811855784591, -7.071067811875158601E-16 ) ) ;
#31988 = CARTESIAN_POINT ( 'NONE',  ( 111.8540205700168713, -46.00543295620330753, 268.9556252759110180 ) ) ;
#31987 = FACE_OUTER_BOUND ( 'NONE', #84219, .T. ) ;
#31986 = CARTESIAN_POINT ( 'NONE',  ( 97.89674744388518945, -40.44469223237895505, 277.6356252759110248 ) ) ;
#31989 = DIRECTION ( 'NONE',  ( 0.000000000000000000, 1.000000000000000000, 0.000000000000000000 ) ) ;
#31990 = CARTESIAN_POINT ( 'NONE',  ( 141.8897065959774011, -45.55267046464435055, 14.92562527591100618 ) ) ;
#31991 = CIRCLE ( 'NONE', #10220, 2.749999999999974687 ) ;
#31992 = DIRECTION ( 'NONE',  ( 0.000000000000000000, -1.000000000000000000, 0.000000000000000000 ) ) ;
#31993 = LINE ( 'NONE', #32430, #52916 ) ;
#31994 = CARTESIAN_POINT ( 'NONE',  ( 107.0667039024470313, -104.2784471599408676, 19.21780685541799016 ) ) ;
#31995 = FACE_OUTER_BOUND ( 'NONE', #3640, .T. ) ;
#31997 = EDGE_LOOP ( 'NONE', ( #27606, #11530, #34127, #54942 ) ) ;
#31996 = CARTESIAN_POINT ( 'NONE',  ( 162.9033555647770015, -33.89581943344391135, 117.4678068554150485 ) ) ;
#31998 = CARTESIAN_POINT ( 'NONE',  ( 136.5037707043289288, -20.00325133682047252, 7.150416387933974605 ) ) ;
#31999 = CARTESIAN_POINT ( 'NONE',  ( 99.27200920372420967, -29.77297264586844960, 190.7470538473399415 ) ) ;
#32000 = CARTESIAN_POINT ( 'NONE',  ( 107.3339483091110225, -26.30778942656879948, 116.0556252759109555 ) ) ;
#32001 = CARTESIAN_POINT ( 'NONE',  ( 116.8983464293968524, -40.32492306460803633, 214.5470538473389581 ) ) ;
#32002 = DIRECTION ( 'NONE',  ( 0.000000000000000000, 0.000000000000000000, -1.000000000000000000 ) ) ;
#32003 = DIRECTION ( 'NONE',  ( 1.000000000000000000, 0.000000000000000000, 0.000000000000000000 ) ) ;
#32004 = CIRCLE ( 'NONE', #59545, 12.44600000000001216 ) ;
#32006 = FACE_OUTER_BOUND ( 'NONE', #77663, .T. ) ;
#32005 = LINE ( 'NONE', #58809, #52163 ) ;
#32007 = DIRECTION ( 'NONE',  ( -0.7071067811865774377, 0.7071067811865175967, -7.071067811865782003E-16 ) ) ;
#32008 = LINE ( 'NONE', #60941, #6375 ) ;
#32009 = CARTESIAN_POINT ( 'NONE',  ( 131.3325395364357462, -19.07457063614894821, 3.076560393663102300 ) ) ;
#32010 = VERTEX_POINT ( 'NONE', #78683 ) ;
#32011 = ORIENTED_EDGE ( 'NONE', *, *, #65276, .F. ) ;
#32012 = CARTESIAN_POINT ( 'NONE',  ( 99.80400324059088746, -42.13953531443270606, 111.2705150661719671 ) ) ;
#32014 = ORIENTED_EDGE ( 'NONE', *, *, #46396, .F. ) ;
#32013 = CARTESIAN_POINT ( 'NONE',  ( 1.598849865763559337E-14, 95.25000000000000000, -130.5560000000000116 ) ) ;
#32015 = CARTESIAN_POINT ( 'NONE',  ( 114.1602155298369325, -45.17592836263234091, 144.1203871806729637 ) ) ;
#32016 = CARTESIAN_POINT ( 'NONE',  ( 142.8830277309892836, -77.57998310118428265, 542.9756252759101471 ) ) ;
#32018 = CARTESIAN_POINT ( 'NONE',  ( 165.9667039024459996, -28.27351298637401200, -5.074374724088000832 ) ) ;
#32017 = AXIS2_PLACEMENT_3D ( 'NONE', #39053, #89917, #83534 ) ;
#32019 = AXIS2_PLACEMENT_3D ( 'NONE', #47535, #82551, #26211 ) ;
#32020 = DIRECTION ( 'NONE',  ( 1.000000000000000000, -3.885780586187990841E-13, 0.000000000000000000 ) ) ;
#32021 = CARTESIAN_POINT ( 'NONE',  ( 45.76696975232822950, -48.62818131005971622, 129.9678068554150911 ) ) ;
#32022 = CARTESIAN_POINT ( 'NONE',  ( 110.1509004715571791, -26.04776408289588474, 64.85276813305395649 ) ) ;
#32023 = ORIENTED_EDGE ( 'NONE', *, *, #54081, .F. ) ;
#32024 = EDGE_CURVE ( 'NONE', #36849, #17132, #64136, .T. ) ;
#32025 = ORIENTED_EDGE ( 'NONE', *, *, #7060, .T. ) ;
#32026 = ORIENTED_EDGE ( 'NONE', *, *, #69975, .T. ) ;
#32027 = CARTESIAN_POINT ( 'NONE',  ( 34.92499999999999716, 66.67499999999999716, 346.0750000000000455 ) ) ;
#32029 = DIRECTION ( 'NONE',  ( 0.000000000000000000, 0.000000000000000000, -1.000000000000000000 ) ) ;
#32028 = CARTESIAN_POINT ( 'NONE',  ( 113.4245949246307532, -29.25360672088989489, 135.5156252759109634 ) ) ;
#32030 = PLANE ( 'NONE',  #22948 ) ;
#32031 = EDGE_CURVE ( 'NONE', #38678, #28371, #63685, .T. ) ;
#32032 = DIRECTION ( 'NONE',  ( 0.7071067811861728725, -0.7071067811869222730, 0.000000000000000000 ) ) ;
#32033 = EDGE_CURVE ( 'NONE', #41944, #7841, #30295, .T. ) ;
#32034 = CIRCLE ( 'NONE', #58172, 4.762500000000001066 ) ;
#32035 = LINE ( 'NONE', #59291, #11372 ) ;
#32036 = ADVANCED_FACE ( 'NONE', ( #57756, #9610, #50939, #44109, #71847, #50030 ), #58635, .F. ) ;
#32037 = CARTESIAN_POINT ( 'NONE',  ( 22.62762465138245460, 171.9999999999999716, 96.88262577854611379 ) ) ;
#32038 = DIRECTION ( 'NONE',  ( 1.000000000000000000, 0.000000000000000000, 0.000000000000000000 ) ) ;
#32039 = CARTESIAN_POINT ( 'NONE',  ( 115.5559444348971851, -42.74257571503951425, 53.33562527591095659 ) ) ;
#32040 = ORIENTED_EDGE ( 'NONE', *, *, #16357, .T. ) ;
#32041 = VECTOR ( 'NONE', #76687, 1000.000000000000000 ) ;
#32042 = ORIENTED_EDGE ( 'NONE', *, *, #12263, .T. ) ;
#32043 = EDGE_CURVE ( 'NONE', #61450, #20221, #1911, .T. ) ;
#32044 = DIRECTION ( 'NONE',  ( 0.000000000000000000, -1.000000000000000000, 0.000000000000000000 ) ) ;
#32045 = CARTESIAN_POINT ( 'NONE',  ( 127.0122246826498866, 52.32189085609214629, 30.21215538458211824 ) ) ;
#32046 = CARTESIAN_POINT ( 'NONE',  ( 0.000000000000000000, 239.0000000000000000, 154.6557476874258441 ) ) ;
#32047 = CARTESIAN_POINT ( 'NONE',  ( 108.4620505914581798, -44.77196653648033475, 165.5309475124489609 ) ) ;
#32048 = EDGE_CURVE ( 'NONE', #64360, #34428, #32191, .T. ) ;
#32049 = EDGE_CURVE ( 'NONE', #78413, #7174, #76722, .T. ) ;
#32050 = VECTOR ( 'NONE', #20136, 1000.000000000000000 ) ;
#32051 = DIRECTION ( 'NONE',  ( 0.000000000000000000, -1.000000000000000000, 0.000000000000000000 ) ) ;
#32052 = ORIENTED_EDGE ( 'NONE', *, *, #67572, .F. ) ;
#32053 = ORIENTED_EDGE ( 'NONE', *, *, #19436, .T. ) ;
#32054 = LINE ( 'NONE', #3467, #36638 ) ;
#32055 = VECTOR ( 'NONE', #47305, 1000.000000000000114 ) ;
#32056 = ORIENTED_EDGE ( 'NONE', *, *, #34586, .F. ) ;
#32057 = ORIENTED_EDGE ( 'NONE', *, *, #15240, .T. ) ;
#32058 = DIRECTION ( 'NONE',  ( 0.000000000000000000, 0.000000000000000000, -1.000000000000000000 ) ) ;
#32059 = EDGE_CURVE ( 'NONE', #85061, #86269, #51815, .T. ) ;
#32060 = CARTESIAN_POINT ( 'NONE',  ( 116.3165111044169038, -35.08217335353153743, 195.3863452106589875 ) ) ;
#32061 = DIRECTION ( 'NONE',  ( -0.9242245927363031965, -0.3818493186865919986, 0.000000000000000000 ) ) ;
#32062 = CIRCLE ( 'NONE', #7441, 2.550000000000006040 ) ;
#32063 = CARTESIAN_POINT ( 'NONE',  ( 144.8545562996767444, -1.932463243632626781, 361.9756252759100335 ) ) ;
#32064 = CARTESIAN_POINT ( 'NONE',  ( -109.7630092984566801, 59.52527381720275201, 70.68955123198077217 ) ) ;
#32065 = ORIENTED_EDGE ( 'NONE', *, *, #16990, .F. ) ;
#32066 = ORIENTED_EDGE ( 'NONE', *, *, #12787, .T. ) ;
#32067 = CIRCLE ( 'NONE', #78537, 2.500000000000002220 ) ;
#32068 = ORIENTED_EDGE ( 'NONE', *, *, #49469, .F. ) ;
#32069 = ORIENTED_EDGE ( 'NONE', *, *, #29827, .T. ) ;
#32070 = CARTESIAN_POINT ( 'NONE',  ( 114.6839398542181101, -39.73893943580953447, 191.3452332267339671 ) ) ;
#32071 = CARTESIAN_POINT ( 'NONE',  ( 98.31770816264274515, -42.43955203770550355, 101.7870538473399620 ) ) ;
#32072 = CARTESIAN_POINT ( 'NONE',  ( 113.4020503763144632, -27.70036014686454351, 84.57753003781698453 ) ) ;
#32073 = CARTESIAN_POINT ( 'NONE',  ( 34.27482367531369789, -30.08671355700341010, 117.4678068554150485 ) ) ;
#32074 = DIRECTION ( 'NONE',  ( -0.4999999999999932832, 0.8660254037844424824, 0.000000000000000000 ) ) ;
#32075 = DIRECTION ( 'NONE',  ( 0.000000000000000000, 0.000000000000000000, 1.000000000000000000 ) ) ;
#32076 = CARTESIAN_POINT ( 'NONE',  ( 98.00710227423795118, -30.39686567179408172, 156.8289586092439549 ) ) ;
#32077 = PLANE ( 'NONE',  #1588 ) ;
#32078 = ORIENTED_EDGE ( 'NONE', *, *, #34820, .F. ) ;
#32079 = CARTESIAN_POINT ( 'NONE',  ( 19.56670390244796920, -67.87844715994100397, 10.91780685541479734 ) ) ;
#32080 = ORIENTED_EDGE ( 'NONE', *, *, #32732, .F. ) ;
#32081 = ORIENTED_EDGE ( 'NONE', *, *, #48243, .T. ) ;
#32082 = CARTESIAN_POINT ( 'NONE',  ( 167.2371591254544967, -47.82818131005522133, 193.9678068554149775 ) ) ;
#32083 = DIRECTION ( 'NONE',  ( -0.000000000000000000, -1.000000000000000000, -0.000000000000000000 ) ) ;
#32084 = EDGE_CURVE ( 'NONE', #3056, #6765, #83997, .T. ) ;
#32085 = ORIENTED_EDGE ( 'NONE', *, *, #44960, .F. ) ;
#32086 = AXIS2_PLACEMENT_3D ( 'NONE', #74796, #39805, #60701 ) ;
#32087 = DIRECTION ( 'NONE',  ( 1.000000000000000078E-15, 1.000000000000000083E-30, -1.000000000000000000 ) ) ;
#32088 = ORIENTED_EDGE ( 'NONE', *, *, #15204, .T. ) ;
#32089 = CARTESIAN_POINT ( 'NONE',  ( 105.1805947621287345, -26.88300331097110885, 131.2268115755357201 ) ) ;
#32090 = CARTESIAN_POINT ( 'NONE',  ( 108.9852622695951112, -46.97665739950247143, 82.72419670448194040 ) ) ;
#32091 = FACE_OUTER_BOUND ( 'NONE', #82726, .T. ) ;
#32092 = DIRECTION ( 'NONE',  ( 0.8571673007021115565, -0.5150380749100554878, 7.521945815882500121E-16 ) ) ;
#32093 = DIRECTION ( 'NONE',  ( -0.9254794337955620787, -0.3787978585227822492, 0.000000000000000000 ) ) ;
#32094 = CARTESIAN_POINT ( 'NONE',  ( 98.84777479348167617, -29.24180311599940651, 80.73848241876795839 ) ) ;
#32095 = CARTESIAN_POINT ( 'NONE',  ( 108.6716496925947126, -26.45072611336629720, 185.9527681330539792 ) ) ;
#32096 = LINE ( 'NONE', #16700, #40791 ) ;
#32097 = PLANE ( 'NONE',  #49661 ) ;
#32098 = ORIENTED_EDGE ( 'NONE', *, *, #10919, .T. ) ;
#32099 = VECTOR ( 'NONE', #37705, 1000.000000000000000 ) ;
#32100 = DIRECTION ( 'NONE',  ( 0.000000000000000000, 0.000000000000000000, 1.000000000000000000 ) ) ;
#32101 = CYLINDRICAL_SURFACE ( 'NONE', #18151, 7.937500000000000000 ) ;
#32102 = DIRECTION ( 'NONE',  ( -0.5000000000000061062, 0.000000000000000000, 0.8660254037844351549 ) ) ;
#32103 = CIRCLE ( 'NONE', #66927, 3.499999999999996003 ) ;
#32104 = FACE_OUTER_BOUND ( 'NONE', #557, .T. ) ;
#32105 = ADVANCED_FACE ( 'NONE', ( #22812 ), #45005, .T. ) ;
#32107 = ORIENTED_EDGE ( 'NONE', *, *, #80428, .F. ) ;
#32106 = CARTESIAN_POINT ( 'NONE',  ( 96.47340144944560336, -31.30584922022854144, 245.9499109901969689 ) ) ;
#32108 = CARTESIAN_POINT ( 'NONE',  ( 112.1392620572132870, -28.01277122371624273, 144.6564663131155726 ) ) ;
#32109 = CARTESIAN_POINT ( 'NONE',  ( 100.0093689611455687, -28.97871315454919028, 281.6641967044822650 ) ) ;
#32110 = CARTESIAN_POINT ( 'NONE',  ( 95.62763156918455820, -33.44862719079586810, 137.1041967044819501 ) ) ;
#32111 = DIRECTION ( 'NONE',  ( 0.000000000000000000, -1.000000000000000000, 0.000000000000000000 ) ) ;
#32112 = CARTESIAN_POINT ( 'NONE',  ( 10.78734560828563183, 89.26522093196125240, -130.1097824653510031 ) ) ;
#32113 = CARTESIAN_POINT ( 'NONE',  ( 91.91441891875204817, -111.9861225405540637, -19.18411693322877198 ) ) ;
#32114 = CARTESIAN_POINT ( 'NONE',  ( 116.3251085584666527, -32.94148239642360210, 265.1356252759109680 ) ) ;
#32115 = ORIENTED_EDGE ( 'NONE', *, *, #14953, .F. ) ;
#32116 = ADVANCED_FACE ( 'NONE', ( #30947 ), #86370, .F. ) ;
#32117 = ORIENTED_EDGE ( 'NONE', *, *, #66609, .T. ) ;
#32118 = ORIENTED_EDGE ( 'NONE', *, *, #57691, .T. ) ;
#32119 = CIRCLE ( 'NONE', #61173, 7.837499999999996803 ) ;
#32120 = ORIENTED_EDGE ( 'NONE', *, *, #40278, .T. ) ;
#32121 = DIRECTION ( 'NONE',  ( 1.000000000000000000, 0.000000000000000000, 0.000000000000000000 ) ) ;
#32122 = CARTESIAN_POINT ( 'NONE',  ( 99.77739493559407435, -44.20163642594127396, 17.96133956162493206 ) ) ;
#32123 = CARTESIAN_POINT ( 'NONE',  ( 117.0667039024470455, -109.9573555057411056, 17.71780685541815714 ) ) ;
#32124 = CARTESIAN_POINT ( 'NONE',  ( 112.3521622943470675, -140.6784471636648561, 245.8674567499459727 ) ) ;
#32125 = B_SPLINE_CURVE_WITH_KNOTS ( 'NONE', 3,
 ( #71618, #42536, #35733, #21682, #30277, #1234, #85703, #64351, #9383, #2578, #64792, #78445, #77986, #57520, #56162, #28937, #23029, #63448 ),
 .UNSPECIFIED., .F., .F.,
 ( 4, 2, 2, 2, 2, 2, 2, 2, 4 ),
 ( 0.000000000000000000, 0.06249999710979182305, 0.1249999942195836461, 0.1874999913293754761, 0.2499999884391672922, 0.3124999855489591361, 0.3749999826587509522, 0.4374999797685427683, 0.4999999768783345844 ),
 .UNSPECIFIED. ) ;
#32127 = CARTESIAN_POINT ( 'NONE',  ( 69.56265278104177696, -140.1743960385357752, 245.5280425831230104 ) ) ;
#32126 = LINE ( 'NONE', #46186, #58388 ) ;
#32128 = CARTESIAN_POINT ( 'NONE',  ( 99.57203460073428403, -40.82693060065560076, 221.1467055423629517 ) ) ;
#32129 = ORIENTED_EDGE ( 'NONE', *, *, #45866, .T. ) ;
#32130 = ORIENTED_EDGE ( 'NONE', *, *, #44649, .T. ) ;
#32131 = ORIENTED_EDGE ( 'NONE', *, *, #55792, .F. ) ;
#32132 = CIRCLE ( 'NONE', #82932, 4.874999999999990230 ) ;
#32133 = PLANE ( 'NONE',  #15202 ) ;
#32134 = CARTESIAN_POINT ( 'NONE',  ( 172.5664832912729878, -27.82844715994070484, 18.92562527591200094 ) ) ;
#32135 = CARTESIAN_POINT ( 'NONE',  ( 172.5664832912740110, 0.2215528400590013880, 258.9256252759120116 ) ) ;
#32136 = ADVANCED_FACE ( 'NONE', ( #74065 ), #25924, .F. ) ;
#32137 = CARTESIAN_POINT ( 'NONE',  ( 105.0852382675896024, -45.91373775275845759, 28.85110711542093753 ) ) ;
#32138 = EDGE_CURVE ( 'NONE', #81368, #84820, #54898, .T. ) ;
#32139 = CARTESIAN_POINT ( 'NONE',  ( 183.5150000000000148, 36.86249999999999716, -35.28456447661465489 ) ) ;
#32140 = EDGE_CURVE ( 'NONE', #39757, #10951, #70906, .T. ) ;
#32141 = LINE ( 'NONE', #58944, #76704 ) ;
#32142 = CARTESIAN_POINT ( 'NONE',  ( 116.8310051202518309, -36.16593252570070405, 228.8727681330539667 ) ) ;
#32143 = DIRECTION ( 'NONE',  ( 4.299999999999999979E-14, -1.000000000000000000, 4.400000000000000367E-29 ) ) ;
#32145 = ORIENTED_EDGE ( 'NONE', *, *, #30911, .T. ) ;
#32144 = VECTOR ( 'NONE', #11722, 1000.000000000000000 ) ;
#32146 = ADVANCED_FACE ( 'NONE', ( #45441 ), #80448, .F. ) ;
#32147 = CARTESIAN_POINT ( 'NONE',  ( 106.0828347753605811, -26.76541559764442724, 56.15474603281727184 ) ) ;
#32148 = PLANE ( 'NONE',  #53910 ) ;
#32149 = CARTESIAN_POINT ( 'NONE',  ( 99.12283442819817481, -33.29442637601800214, 58.83189989340093007 ) ) ;
#32150 = CIRCLE ( 'NONE', #82952, 2.999999999999999112 ) ;
#32151 = CARTESIAN_POINT ( 'NONE',  ( -68.91674821478409285, 82.54999999999999716, -68.91674821478481761 ) ) ;
#32152 = CARTESIAN_POINT ( 'NONE',  ( -13.86911000615384104, 224.4999999999999432, 102.9892450244911828 ) ) ;
#32153 = ADVANCED_FACE ( 'NONE', ( #59966 ), #86814, .T. ) ;
#32154 = VECTOR ( 'NONE', #30883, 1000.000000000000000 ) ;
#32155 = CARTESIAN_POINT ( 'NONE',  ( -10.79024059098301080, 89.26081878472081144, 118.0641780253921098 ) ) ;
#32156 = ORIENTED_EDGE ( 'NONE', *, *, #70009, .T. ) ;
#32157 = CARTESIAN_POINT ( 'NONE',  ( 114.0075790447407087, -33.88846322102013175, 9.635625275910941312 ) ) ;
#32158 = LINE ( 'NONE', #10386, #54187 ) ;
#32159 = ORIENTED_EDGE ( 'NONE', *, *, #66374, .T. ) ;
#32160 = CARTESIAN_POINT ( 'NONE',  ( 109.2550203967672928, -46.95863148777297624, 107.7441967044829880 ) ) ;
#32161 = ORIENTED_EDGE ( 'NONE', *, *, #19060, .F. ) ;
#32163 = AXIS2_PLACEMENT_3D ( 'NONE', #7424, #70556, #48282 ) ;
#32162 = CARTESIAN_POINT ( 'NONE',  ( 113.5850730991778619, -42.29362625859309333, 62.68670554236294379 ) ) ;
#32164 = DIRECTION ( 'NONE',  ( -1.000000000000000078E-15, 1.000000000000000083E-30, 1.000000000000000000 ) ) ;
#32165 = CARTESIAN_POINT ( 'NONE',  ( 111.9059958850653800, -29.27014106345288624, 66.05015473446795227 ) ) ;
#32166 = CARTESIAN_POINT ( 'NONE',  ( -479.3614999999999782, 7.143750000000280487, 15.23694598552305024 ) ) ;
#32167 = CARTESIAN_POINT ( 'NONE',  ( 182.0667039024480118, -32.29483332968430886, -5.074374724088000832 ) ) ;
#32168 = CARTESIAN_POINT ( 'NONE',  ( 115.6290845971308414, -28.50119646097363812, 35.43562527591098643 ) ) ;
#32169 = DIRECTION ( 'NONE',  ( 1.907762142705490052E-15, 7.167082501179359715E-16, -1.000000000000000000 ) ) ;
#32170 = ORIENTED_EDGE ( 'NONE', *, *, #78573, .T. ) ;
#32171 = CARTESIAN_POINT ( 'NONE',  ( 101.9935452999619798, -45.44602508736877411, 257.1563564671954509 ) ) ;
#32172 = VERTEX_POINT ( 'NONE', #32727 ) ;
#32173 = CARTESIAN_POINT ( 'NONE',  ( 3.174999999999889688, 111.1250000000000000, 31.75000000000000000 ) ) ;
#32174 = ORIENTED_EDGE ( 'NONE', *, *, #80976, .F. ) ;
#32175 = ORIENTED_EDGE ( 'NONE', *, *, #55931, .F. ) ;
#32176 = FACE_OUTER_BOUND ( 'NONE', #31391, .T. ) ;
#32177 = EDGE_LOOP ( 'NONE', ( #25963, #47139, #23830, #18437 ) ) ;
#32178 = CARTESIAN_POINT ( 'NONE',  ( 115.4995704134666994, -41.68388727776413560, 238.4041967044829562 ) ) ;
#32179 = DIRECTION ( 'NONE',  ( -1.000000000000000000, 0.000000000000000000, 0.000000000000000000 ) ) ;
#32180 = DIRECTION ( 'NONE',  ( -0.1811243269279065315, 0.9834602067165264527, 0.000000000000000000 ) ) ;
#32181 = CARTESIAN_POINT ( 'NONE',  ( 95.34914990350537778, -34.95780559393485731, 67.20705384733894050 ) ) ;
#32182 = CARTESIAN_POINT ( 'NONE',  ( 107.0667039024470313, -104.2784471599420755, -19.78219314458201694 ) ) ;
#32183 = VERTEX_POINT ( 'NONE', #4130 ) ;
#32184 = FACE_OUTER_BOUND ( 'NONE', #69158, .T. ) ;
#32185 = CARTESIAN_POINT ( 'NONE',  ( 239.7378999999999962, 52.73749999999999716, -10.97647784993501396 ) ) ;
#32186 = VECTOR ( 'NONE', #17714, 1000.000000000000000 ) ;
#32187 = ADVANCED_FACE ( 'NONE', ( #59076 ), #87700, .F. ) ;
#32188 = ORIENTED_EDGE ( 'NONE', *, *, #22220, .T. ) ;
#32189 = AXIS2_PLACEMENT_3D ( 'NONE', #17896, #58773, #45577 ) ;
#32190 = CARTESIAN_POINT ( 'NONE',  ( 107.0667039024479834, -54.72944715994100306, 239.5838068554169809 ) ) ;
#32191 = B_SPLINE_CURVE_WITH_KNOTS ( 'NONE', 3,
 ( #72294, #65468, #43673, #51370, #10063, #77766, #29609 ),
 .UNSPECIFIED., .F., .F.,
 ( 4, 1, 1, 1, 4 ),
 ( 0.000000000000000000, 0.2752441480442837096, 0.5749187429555715489, 0.8745933378668595548, 1.000000000000000000 ),
 .UNSPECIFIED. ) ;
#32192 = CARTESIAN_POINT ( 'NONE',  ( 112.0635997081393640, -45.48968496527341188, 113.9904082404935366 ) ) ;
#32193 = CARTESIAN_POINT ( 'NONE',  ( 98.05565822401619869, -44.38798742045811707, 226.8870538473399563 ) ) ;
#32194 = CARTESIAN_POINT ( 'NONE',  ( -13.40680633928205090, 223.9999999999999716, 102.7987842159323293 ) ) ;
#32195 = EDGE_CURVE ( 'NONE', #43151, #39354, #74516, .T. ) ;
#32196 = CARTESIAN_POINT ( 'NONE',  ( 97.81168895331838087, -40.51742574516882200, 287.6356252759109680 ) ) ;
#32197 = CARTESIAN_POINT ( 'NONE',  ( 194.0667039024475571, -24.92844715993407334, 129.9678068554150343 ) ) ;
#32198 = CARTESIAN_POINT ( 'NONE',  ( 98.66229053285113082, -40.10320091580625501, 251.0648007804577730 ) ) ;
#32200 = CARTESIAN_POINT ( 'NONE',  ( 100.9560042165379770, -28.30978499293933126, 71.57562527591099411 ) ) ;
#32199 = DIRECTION ( 'NONE',  ( 1.000000000000000078E-15, -1.000000000000000083E-30, -1.000000000000000000 ) ) ;
#32201 = CARTESIAN_POINT ( 'NONE',  ( 120.2829076421031544, 74.61365623713926709, 50.76363797295935854 ) ) ;
#32202 = CARTESIAN_POINT ( 'NONE',  ( 95.97680135624298714, -37.21094296235740018, 116.3489586092439652 ) ) ;
#32203 = ORIENTED_EDGE ( 'NONE', *, *, #50181, .T. ) ;
#32204 = DIRECTION ( 'NONE',  ( -0.4999999999999998890, 0.8660254037844387076, 0.000000000000000000 ) ) ;
#32205 = ORIENTED_EDGE ( 'NONE', *, *, #13198, .T. ) ;
#32206 = CARTESIAN_POINT ( 'NONE',  ( 90.06648329127389729, -36.72944715993924802, 14.92562527591095289 ) ) ;
#32207 = DIRECTION ( 'NONE',  ( 1.000000000000000000, -1.000000000000000078E-15, 0.000000000000000000 ) ) ;
#32208 = CARTESIAN_POINT ( 'NONE',  ( 41.56648329127398966, -27.57844715994070484, 198.9256252759119832 ) ) ;
#32209 = ORIENTED_EDGE ( 'NONE', *, *, #40970, .T. ) ;
#32210 = VECTOR ( 'NONE', #16647, 1000.000000000000000 ) ;
#32211 = DIRECTION ( 'NONE',  ( -0.9659258262890690894, 0.000000000000000000, -0.2588190451025180749 ) ) ;
#32213 = ORIENTED_EDGE ( 'NONE', *, *, #59812, .F. ) ;
#32212 = CARTESIAN_POINT ( 'NONE',  ( 108.5441999379606983, -26.36493947475176114, 104.9641967044819779 ) ) ;
#32214 = LINE ( 'NONE', #58576, #82769 ) ;
#32215 = CARTESIAN_POINT ( 'NONE',  ( -130.1467854596290010, 89.94765885072629885, 10.33135106516698265 ) ) ;
#32216 = AXIS2_PLACEMENT_3D ( 'NONE', #30793, #11234, #46181 ) ;
#32217 = CARTESIAN_POINT ( 'NONE',  ( 31.78666935232898894, -29.62846900982320264, -5.074374724088000832 ) ) ;
#32218 = ORIENTED_EDGE ( 'NONE', *, *, #37098, .T. ) ;
#32220 = EDGE_CURVE ( 'NONE', #39347, #12421, #41943, .T. ) ;
#32219 = CIRCLE ( 'NONE', #16293, 190.5000000000000000 ) ;
#32221 = CARTESIAN_POINT ( 'NONE',  ( 113.9315101381565682, -28.03652776953382286, 124.5565776568629559 ) ) ;
#32222 = APPLICATION_PROTOCOL_DEFINITION ( 'draft international standard', 'automotive_design', 1998, #39967 ) ;
#32223 = CARTESIAN_POINT ( 'NONE',  ( 95.60734603896362671, -36.72944715994100306, 277.6356252759110248 ) ) ;
#32224 = DIRECTION ( 'NONE',  ( 9.912705577010326536E-16, 1.000000000000000000, 0.000000000000000000 ) ) ;
#32225 = VERTEX_POINT ( 'NONE', #60879 ) ;
#32226 = VECTOR ( 'NONE', #31654, 1000.000000000000000 ) ;
#32227 = ORIENTED_EDGE ( 'NONE', *, *, #43724, .F. ) ;
#32228 = CARTESIAN_POINT ( 'NONE',  ( 51.03742451361238608, -23.42844715994066362, 237.4678068554150059 ) ) ;
#32229 = DIRECTION ( 'NONE',  ( 0.000000000000000000, 0.000000000000000000, 1.000000000000000000 ) ) ;
#32230 = DIRECTION ( 'NONE',  ( 0.7071067811743789733, -0.7071067811987160612, 0.000000000000000000 ) ) ;
#32231 = VECTOR ( 'NONE', #62728, 1000.000000000000000 ) ;
#32232 = CARTESIAN_POINT ( 'NONE',  ( 138.0667039024480403, -58.72944715994091069, 239.5838068554170377 ) ) ;
#32234 = FACE_OUTER_BOUND ( 'NONE', #38497, .T. ) ;
#32233 = DIRECTION ( 'NONE',  ( -0.7071067811864671926, -0.7071067811866279529, -7.071067811864664779E-16 ) ) ;
#32235 = PLANE ( 'NONE',  #9502 ) ;
#32236 = VERTEX_POINT ( 'NONE', #87260 ) ;
#32237 = CARTESIAN_POINT ( 'NONE',  ( 117.0608945280935274, -38.08045307652025713, 34.71895861277068462 ) ) ;
#32238 = CARTESIAN_POINT ( 'NONE',  ( 97.48942487598456808, -34.74365074496814998, 212.1641967044819808 ) ) ;
#32239 = ADVANCED_FACE ( 'NONE', ( #67701 ), #5485, .T. ) ;
#32241 = ORIENTED_EDGE ( 'NONE', *, *, #36045, .T. ) ;
#32240 = CARTESIAN_POINT ( 'NONE',  ( 63.56670390244824631, -47.82844715994016127, 300.4678068554150627 ) ) ;
#32242 = CARTESIAN_POINT ( 'NONE',  ( 112.4079628628857250, -28.49644221148697198, 65.61848241876694487 ) ) ;
#32243 = EDGE_CURVE ( 'NONE', #52020, #61274, #26366, .T. ) ;
#32244 = FACE_OUTER_BOUND ( 'NONE', #84267, .T. ) ;
#32245 = ADVANCED_FACE ( 'NONE', ( #81794 ), #19547, .T. ) ;
#32246 = CARTESIAN_POINT ( 'NONE',  ( 99.90204555947735798, -100.7192800061664713, -19.78219314458212708 ) ) ;
#32247 = LINE ( 'NONE', #87673, #59052 ) ;
#32248 = ORIENTED_EDGE ( 'NONE', *, *, #35430, .T. ) ;
#32249 = CARTESIAN_POINT ( 'NONE',  ( 83.06670390244796920, -58.72944715994098885, 231.5838068554150198 ) ) ;
#32250 = EDGE_CURVE ( 'NONE', #56062, #39918, #52688, .T. ) ;
#32251 = ORIENTED_EDGE ( 'NONE', *, *, #813, .F. ) ;
#32252 = EDGE_LOOP ( 'NONE', ( #22354, #10779, #78069, #31638, #44895 ) ) ;
#32253 = CARTESIAN_POINT ( 'NONE',  ( 115.8610455727973090, -35.41879699190349129, 215.3758690201829609 ) ) ;
#32254 = VECTOR ( 'NONE', #3024, 1000.000000000000000 ) ;
#32255 = LINE ( 'NONE', #31812, #22670 ) ;
#32256 = CYLINDRICAL_SURFACE ( 'NONE', #16023, 11.45913725231036118 ) ;
#32257 = FACE_OUTER_BOUND ( 'NONE', #60411, .T. ) ;
#32258 = EDGE_CURVE ( 'NONE', #50690, #9081, #88166, .T. ) ;
#32259 = CARTESIAN_POINT ( 'NONE',  ( 82.63685198412170507, -37.70758306363496359, 2.855952960430489185 ) ) ;
#32260 = VERTEX_POINT ( 'NONE', #3688 ) ;
#32261 = CARTESIAN_POINT ( 'NONE',  ( 173.9900000000000091, 20.32000000000000028, -71.37400000000000944 ) ) ;
#32262 = CARTESIAN_POINT ( 'NONE',  ( 97.33721762003443700, -34.07359039618388863, 37.11469305630519244 ) ) ;
#32263 = EDGE_LOOP ( 'NONE', ( #57800, #68104 ) ) ;
#32264 = CARTESIAN_POINT ( 'NONE',  ( 109.6119907475197550, -25.15530020966791369, 29.90419670448196854 ) ) ;
#32265 = EDGE_LOOP ( 'NONE', ( #12530, #41007, #63958, #89075 ) ) ;
#32266 = VERTEX_POINT ( 'NONE', #80010 ) ;
#32267 = CARTESIAN_POINT ( 'NONE',  ( 101.0114332956932088, -30.54581597779692359, 268.5233284648295466 ) ) ;
#32268 = CIRCLE ( 'NONE', #80152, 7.999999999999992895 ) ;
#32269 = LINE ( 'NONE', #12292, #18419 ) ;
#32270 = DIRECTION ( 'NONE',  ( 0.000000000000000000, 0.000000000000000000, -1.000000000000000000 ) ) ;
#32271 = DIRECTION ( 'NONE',  ( 0.000000000000000000, -1.000000000000000000, 0.000000000000000000 ) ) ;
#32272 = DIRECTION ( 'NONE',  ( -1.004914528670390057E-14, 0.000000000000000000, 1.000000000000000000 ) ) ;
#32273 = CARTESIAN_POINT ( 'NONE',  ( 113.1808386317757282, -26.52034477659904610, 200.6470538473399756 ) ) ;
#32274 = CARTESIAN_POINT ( 'NONE',  ( 1.232595164407830946E-29, 69.95000000000000284, 118.3560000000000088 ) ) ;
#32275 = EDGE_LOOP ( 'NONE', ( #52109, #41105 ) ) ;
#32276 = CARTESIAN_POINT ( 'NONE',  ( 98.26973918885833825, -28.71518450514261289, 76.73848241876795839 ) ) ;
#32277 = DIRECTION ( 'NONE',  ( 0.000000000000000000, -1.000000000000000000, 0.000000000000000000 ) ) ;
#32278 = ORIENTED_EDGE ( 'NONE', *, *, #39113, .T. ) ;
#32279 = ORIENTED_EDGE ( 'NONE', *, *, #84548, .F. ) ;
#32280 = ORIENTED_EDGE ( 'NONE', *, *, #13705, .F. ) ;
#32281 = VECTOR ( 'NONE', #604, 1000.000000000000114 ) ;
#32282 = CYLINDRICAL_SURFACE ( 'NONE', #36142, 2.749999999999974687 ) ;
#32283 = DIRECTION ( 'NONE',  ( 1.000000000000000000, 8.163404592831600092E-16, 1.020425574103949962E-15 ) ) ;
#32284 = CARTESIAN_POINT ( 'NONE',  ( 101.9927640441988501, -45.44554309988366469, 152.1569868649772843 ) ) ;
#32285 = CARTESIAN_POINT ( 'NONE',  ( 100.3248355287147291, -41.38056247698398238, 124.6252332267339682 ) ) ;
#32286 = CARTESIAN_POINT ( 'NONE',  ( 106.3003414554210764, -47.14819399153626023, 218.5184824187679453 ) ) ;
#32287 = CARTESIAN_POINT ( 'NONE',  ( -29.99999999999998224, 127.0000000000000000, 113.8826257785461280 ) ) ;
#32288 = EDGE_LOOP ( 'NONE', ( #71499, #45854 ) ) ;
#32289 = CARTESIAN_POINT ( 'NONE',  ( 130.5247076678899703, 94.92443974548208985, -2.887521757539373457 ) ) ;
#32290 = CARTESIAN_POINT ( 'NONE',  ( 136.6880318146010325, -37.56139158948385415, 2.921136715971366371 ) ) ;
#32291 = EDGE_CURVE ( 'NONE', #62792, #33465, #39037, .T. ) ;
#32292 = ORIENTED_EDGE ( 'NONE', *, *, #60623, .F. ) ;
#32293 = ORIENTED_EDGE ( 'NONE', *, *, #2526, .T. ) ;
#32294 = DIRECTION ( 'NONE',  ( -0.000000000000000000, -0.000000000000000000, -1.000000000000000000 ) ) ;
#32295 = ORIENTED_EDGE ( 'NONE', *, *, #55906, .T. ) ;
#32296 = ORIENTED_EDGE ( 'NONE', *, *, #65804, .F. ) ;
#32297 = CARTESIAN_POINT ( 'NONE',  ( 98.30773656818189465, -41.72926007762017520, 167.7402057210307191 ) ) ;
#32298 = LINE ( 'NONE', #33213, #68925 ) ;
#32299 = EDGE_CURVE ( 'NONE', #40647, #5575, #82580, .T. ) ;
#32300 = CARTESIAN_POINT ( 'NONE',  ( 51.42025729302798709, -31.94127993907680718, 237.4678068554150059 ) ) ;
#32301 = CARTESIAN_POINT ( 'NONE',  ( 98.54925023078828872, -36.08769725913535353, 145.6895626852199541 ) ) ;
#32302 = CARTESIAN_POINT ( 'NONE',  ( 100.4512773062034370, -27.81586575833916442, 35.59657765686397113 ) ) ;
#32303 = CARTESIAN_POINT ( 'NONE',  ( 75.29769027782792534, -100.6205720721962820, 249.3055308415380011 ) ) ;
#32304 = ORIENTED_EDGE ( 'NONE', *, *, #7998, .F. ) ;
#32305 = CIRCLE ( 'NONE', #33814, 7.199999999999998401 ) ;
#32306 = CARTESIAN_POINT ( 'NONE',  ( -88.44575049335551853, 71.76236341257998674, -78.94931995840768479 ) ) ;
#32307 = EDGE_LOOP ( 'NONE', ( #50959, #16275, #7384 ) ) ;
#32308 = DIRECTION ( 'NONE',  ( -0.7071067811865774377, 0.7071067811865175967, -7.071067811865470403E-16 ) ) ;
#32309 = VERTEX_POINT ( 'NONE', #39542 ) ;
#32310 = CARTESIAN_POINT ( 'NONE',  ( 107.0667039024470313, -104.2784471599420755, -19.78219314458201694 ) ) ;
#32311 = CARTESIAN_POINT ( 'NONE',  ( 93.16752758198826712, -128.7026216972209625, 250.2203867545810283 ) ) ;
#32312 = LINE ( 'NONE', #53181, #9818 ) ;
#32313 = VECTOR ( 'NONE', #26811, 1000.000000000000000 ) ;
#32314 = DIRECTION ( 'NONE',  ( -1.000000000000000000, 0.000000000000000000, -0.000000000000000000 ) ) ;
#32315 = ORIENTED_EDGE ( 'NONE', *, *, #79629, .T. ) ;
#32316 = EDGE_CURVE ( 'NONE', #78335, #70136, #76306, .T. ) ;
#32317 = CARTESIAN_POINT ( 'NONE',  ( 112.2083724274664291, -26.91728527761779333, 14.68038718067299442 ) ) ;
#32318 = CARTESIAN_POINT ( 'NONE',  ( 103.9444121564427235, -47.38074615057520589, 58.33753003781600199 ) ) ;
#32319 = FILL_AREA_STYLE ('',( #74122 ) ) ;
#32321 = DIRECTION ( 'NONE',  ( 0.000000000000000000, 0.000000000000000000, 1.000000000000000000 ) ) ;
#32320 = DIRECTION ( 'NONE',  ( 1.000000000000000000, 3.651563665954199690E-16, 0.000000000000000000 ) ) ;
#32322 = DIRECTION ( 'NONE',  ( 4.299999999999999979E-14, -1.000000000000000000, 4.128053709984630540E-29 ) ) ;
#32323 = DIRECTION ( 'NONE',  ( 9.912705577010326536E-16, 1.000000000000000000, 0.000000000000000000 ) ) ;
#32324 = DIRECTION ( 'NONE',  ( -4.237773401492740281E-14, 1.000000000000000000, 0.000000000000000000 ) ) ;
#32325 = DIRECTION ( 'NONE',  ( 1.000000000000000078E-15, -1.000000000000000083E-30, -1.000000000000000000 ) ) ;
#32326 = CARTESIAN_POINT ( 'NONE',  ( 54.06670390244700997, -79.67844715994098692, 55.21780685541800437 ) ) ;
#32327 = EDGE_CURVE ( 'NONE', #66477, #71033, #12930, .T. ) ;
#32328 = ORIENTED_EDGE ( 'NONE', *, *, #76370, .T. ) ;
#32329 = CARTESIAN_POINT ( 'NONE',  ( 96.13137017992535505, -38.63632546489608188, 46.45181575210094138 ) ) ;
#32330 = CARTESIAN_POINT ( 'NONE',  ( 99.75313521292756036, -29.29995004827394212, 221.6956252759109702 ) ) ;
#32331 = CARTESIAN_POINT ( 'NONE',  ( 112.9754938005188478, -28.11429459860147873, 40.59848241876795782 ) ) ;
#32333 = DIRECTION ( 'NONE',  ( 0.000000000000000000, 0.000000000000000000, 1.000000000000000000 ) ) ;
#32332 = CARTESIAN_POINT ( 'NONE',  ( 97.81304204170952232, -40.52073163124537558, 171.6361819576471532 ) ) ;
#32334 = CARTESIAN_POINT ( 'NONE',  ( 6.812220284937080487E-16, 50.79999999999999716, 271.1195999999999913 ) ) ;
#32335 = AXIS2_PLACEMENT_3D ( 'NONE', #12227, #19034, #4518 ) ;
#32336 = VECTOR ( 'NONE', #4163, 1000.000000000000000 ) ;
#32337 = EDGE_LOOP ( 'NONE', ( #29763, #32175, #67927, #35456 ) ) ;
#32338 = DIRECTION ( 'NONE',  ( 1.000000000000000000, 0.000000000000000000, 0.000000000000000000 ) ) ;
#32339 = VERTEX_POINT ( 'NONE', #55384 ) ;
#32340 = CARTESIAN_POINT ( 'NONE',  ( 97.28369645613172167, -37.51102008256656717, 97.38991099019594344 ) ) ;
#32342 = ORIENTED_EDGE ( 'NONE', *, *, #81101, .T. ) ;
#32341 = CARTESIAN_POINT ( 'NONE',  ( 11.72308525109137634, 87.43461473045920229, 130.0286063932555294 ) ) ;
#32343 = CARTESIAN_POINT ( 'NONE',  ( 113.0874441278155160, -45.97130050132138024, 219.0480062282919960 ) ) ;
#32344 = DIRECTION ( 'NONE',  ( 0.000000000000000000, 0.000000000000000000, 1.000000000000000000 ) ) ;
#32345 = CYLINDRICAL_SURFACE ( 'NONE', #71056, 17.33514202138210081 ) ;
#32346 = DIRECTION ( 'NONE',  ( 0.000000000000000000, 0.000000000000000000, 1.000000000000000000 ) ) ;
#32347 = EDGE_CURVE ( 'NONE', #56526, #85724, #40436, .T. ) ;
#32348 = CARTESIAN_POINT ( 'NONE',  ( 105.7995184788125016, -26.72403496690349911, 46.17729194326120989 ) ) ;
#32349 = DIRECTION ( 'NONE',  ( 0.000000000000000000, 0.000000000000000000, -1.000000000000000000 ) ) ;
#32350 = FACE_OUTER_BOUND ( 'NONE', #65754, .T. ) ;
#32351 = CARTESIAN_POINT ( 'NONE',  ( 113.2095242374420252, -45.08419629851117350, 183.0689586092449588 ) ) ;
#32352 = ORIENTED_EDGE ( 'NONE', *, *, #27560, .F. ) ;
#32353 = ORIENTED_EDGE ( 'NONE', *, *, #40976, .T. ) ;
#32354 = CARTESIAN_POINT ( 'NONE',  ( 99.22037001696983793, -32.61037140242165577, 132.3730118773259790 ) ) ;
#32355 = FACE_OUTER_BOUND ( 'NONE', #21237, .T. ) ;
#32357 = DIRECTION ( 'NONE',  ( 1.000000000000000000, 0.000000000000000000, 0.000000000000000000 ) ) ;
#32356 = CARTESIAN_POINT ( 'NONE',  ( 106.2788006184939888, -47.06957971430141185, 263.5280062282914741 ) ) ;
#32358 = VECTOR ( 'NONE', #9574, 1000.000000000000000 ) ;
#32359 = DIRECTION ( 'NONE',  ( 0.7071067812164788524, -0.7071067811566160710, 0.000000000000000000 ) ) ;
#32360 = DIRECTION ( 'NONE',  ( 0.000000000000000000, 1.000000000000000000, 0.000000000000000000 ) ) ;
#32361 = CARTESIAN_POINT ( 'NONE',  ( 117.8738102209306362, 82.54999999999999716, 12.70000000000123386 ) ) ;
#32362 = EDGE_CURVE ( 'NONE', #42340, #68948, #33270, .T. ) ;
#32363 = DIRECTION ( 'NONE',  ( -0.9254794337955620787, -0.3787978585227822492, 0.000000000000000000 ) ) ;
#32364 = VECTOR ( 'NONE', #88244, 1000.000000000000000 ) ;
#32365 = DIRECTION ( 'NONE',  ( 0.000000000000000000, 0.000000000000000000, 1.000000000000000000 ) ) ;
#32366 = CARTESIAN_POINT ( 'NONE',  ( 25.56670390244797275, -62.87844715994099687, 170.4678068554149775 ) ) ;
#32367 = ADVANCED_FACE ( 'NONE', ( #69498 ), #41763, .F. ) ;
#32368 = CARTESIAN_POINT ( 'NONE',  ( 95.93334478249045105, -32.74178691125829488, 176.0527681330539735 ) ) ;
#32369 = CARTESIAN_POINT ( 'NONE',  ( 107.0664832912739968, -36.72944715994100306, 9.635625275910941312 ) ) ;
#32370 = VERTEX_POINT ( 'NONE', #26805 ) ;
#32371 = VERTEX_POINT ( 'NONE', #49020 ) ;
#32372 = CARTESIAN_POINT ( 'NONE',  ( -96.20681132576102357, 71.15434825076368952, -88.25674559704586386 ) ) ;
#32373 = CARTESIAN_POINT ( 'NONE',  ( 79.68958420874194815, -15.97944715994105813, 1.625625275910942413 ) ) ;
#32374 = CARTESIAN_POINT ( 'NONE',  ( 97.07209078958956638, -35.37825800277666133, 186.2194405451776902 ) ) ;
#32375 = LINE ( 'NONE', #11050, #20120 ) ;
#32376 = CONICAL_SURFACE ( 'NONE', #46893, 1.258749999999999369, 1.029744258676650093 ) ;
#32377 = CARTESIAN_POINT ( 'NONE',  ( 109.7212179059393407, -26.99983407561881066, 94.86509365950415429 ) ) ;
#32378 = ORIENTED_EDGE ( 'NONE', *, *, #67452, .F. ) ;
#32379 = CARTESIAN_POINT ( 'NONE',  ( 107.0667039024470313, -104.2784471599420755, -19.78219314458201694 ) ) ;
#32380 = CARTESIAN_POINT ( 'NONE',  ( 103.7231215738078163, -26.19374500585225363, 205.3089586092439731 ) ) ;
#32381 = DIRECTION ( 'NONE',  ( 0.000000000000000000, 0.000000000000000000, -1.000000000000000000 ) ) ;
#32382 = ORIENTED_EDGE ( 'NONE', *, *, #55324, .F. ) ;
#32383 = ORIENTED_EDGE ( 'NONE', *, *, #37865, .F. ) ;
#32384 = CARTESIAN_POINT ( 'NONE',  ( -1.665763066381118485, 69.93250922127340630, 118.5470808886261125 ) ) ;
#32385 = DIRECTION ( 'NONE',  ( 1.000000000000000000, 4.299999999999999979E-14, 1.000000000000000078E-15 ) ) ;
#32386 = CARTESIAN_POINT ( 'NONE',  ( 98.15098341961036965, -41.26162459717305353, 166.7007383883326952 ) ) ;
#32387 = CARTESIAN_POINT ( 'NONE',  ( 112.5662596640460720, -44.20262526656594559, 30.89951894101994156 ) ) ;
#32388 = CARTESIAN_POINT ( 'NONE',  ( 116.9247085916874909, -40.18670803819183845, 129.5584824187679658 ) ) ;
#32389 = DIRECTION ( 'NONE',  ( 0.000000000000000000, -1.000000000000000000, 0.000000000000000000 ) ) ;
#32390 = ORIENTED_EDGE ( 'NONE', *, *, #30740, .F. ) ;
#32391 = DIRECTION ( 'NONE',  ( -4.237773401492740281E-14, 1.000000000000000000, 0.000000000000000000 ) ) ;
#32392 = CARTESIAN_POINT ( 'NONE',  ( 82.51738923907551282, -17.48112160756095790, 7.135585143040647615 ) ) ;
#32393 = ORIENTED_EDGE ( 'NONE', *, *, #55195, .F. ) ;
#32394 = ORIENTED_EDGE ( 'NONE', *, *, #43139, .T. ) ;
#32395 = AXIS2_PLACEMENT_3D ( 'NONE', #20722, #62938, #42483 ) ;
#32396 = CARTESIAN_POINT ( 'NONE',  ( 99.53451269431033666, -99.35238426914629883, 2.217806855417836509 ) ) ;
#32397 = EDGE_LOOP ( 'NONE', ( #53487, #42468, #77205, #47879, #82275 ) ) ;
#32398 = VERTEX_POINT ( 'NONE', #47685 ) ;
#32399 = DIRECTION ( 'NONE',  ( 1.000000000000000000, 0.000000000000000000, -2.544367396927093358E-16 ) ) ;
#32400 = CIRCLE ( 'NONE', #12136, 2.500000000000002220 ) ;
#32401 = ADVANCED_FACE ( 'NONE', ( #48570 ), #34515, .T. ) ;
#32402 = CARTESIAN_POINT ( 'NONE',  ( 106.8818968526635160, -46.43699862984655624, 76.98384839950495007 ) ) ;
#32403 = CARTESIAN_POINT ( 'NONE',  ( 103.2955449146038376, -26.98642977692344758, 215.3699109901969848 ) ) ;
#32404 = CARTESIAN_POINT ( 'NONE',  ( 97.40233316251681117, -42.04621543282991780, 176.7146728949589658 ) ) ;
#32406 = CARTESIAN_POINT ( 'NONE',  ( 97.09625384711495144, -33.75906160244647936, 27.09562527591097236 ) ) ;
#32405 = CARTESIAN_POINT ( 'NONE',  ( 98.17490182338630689, -41.30874685505506960, 21.70468755961504925 ) ) ;
#32407 = DIRECTION ( 'NONE',  ( -1.000000000000000078E-15, 1.000000000000000000, 0.000000000000000000 ) ) ;
#32408 = DIRECTION ( 'NONE',  ( -0.9242245927363026414, -0.3818493186865932754, 0.000000000000000000 ) ) ;
#32409 = ORIENTED_EDGE ( 'NONE', *, *, #79264, .F. ) ;
#32410 = VERTEX_POINT ( 'NONE', #20006 ) ;
#32411 = FACE_OUTER_BOUND ( 'NONE', #76929, .T. ) ;
#32413 = AXIS2_PLACEMENT_3D ( 'NONE', #58085, #78561, #78108 ) ;
#32412 = CARTESIAN_POINT ( 'NONE',  ( 116.5668037432639608, -41.21227053747742985, 228.4756252759109714 ) ) ;
#32414 = VERTEX_POINT ( 'NONE', #7713 ) ;
#32415 = EDGE_CURVE ( 'NONE', #58184, #30833, #20456, .T. ) ;
#32416 = CARTESIAN_POINT ( 'NONE',  ( 117.4139541310910175, -35.45788210829842058, 193.9241967044829664 ) ) ;
#32417 = DIRECTION ( 'NONE',  ( 0.000000000000000000, 0.000000000000000000, 1.000000000000000000 ) ) ;
#32418 = AXIS2_PLACEMENT_3D ( 'NONE', #52100, #9916, #43963 ) ;
#32419 = LINE ( 'NONE', #47838, #92 ) ;
#32420 = PLANE ( 'NONE',  #14509 ) ;
#32421 = LINE ( 'NONE', #38800, #38398 ) ;
#32422 = EDGE_CURVE ( 'NONE', #50547, #79315, #30369, .T. ) ;
#32424 = FACE_OUTER_BOUND ( 'NONE', #10936, .T. ) ;
#32423 = CARTESIAN_POINT ( 'NONE',  ( 113.4284485525086836, -31.82768681777509201, 277.6356252759110248 ) ) ;
#32425 = CARTESIAN_POINT ( 'NONE',  ( 168.5667039024485803, -48.82844715993516616, 180.4678068554150059 ) ) ;
#32426 = CARTESIAN_POINT ( 'NONE',  ( 28.57499999999999929, 73.38456447661469895, 302.8950000000000387 ) ) ;
#32427 = LINE ( 'NONE', #47395, #9280 ) ;
#32428 = EDGE_CURVE ( 'NONE', #31120, #33618, #68024, .T. ) ;
#32429 = VECTOR ( 'NONE', #79769, 1000.000000000000000 ) ;
#32430 = CARTESIAN_POINT ( 'NONE',  ( 73.06670390244801183, -58.72944715994110254, 310.9178068554150514 ) ) ;
#32431 = LINE ( 'NONE', #31548, #992 ) ;
#32432 = ADVANCED_FACE ( 'NONE', ( #54932 ), #12748, .T. ) ;
#32433 = CARTESIAN_POINT ( 'NONE',  ( 116.3212776292294279, -32.94146857471271517, 75.13562527591093954 ) ) ;
#32435 = ORIENTED_EDGE ( 'NONE', *, *, #16381, .T. ) ;
#32434 = PLANE ( 'NONE',  #18187 ) ;
#32436 = EDGE_CURVE ( 'NONE', #31292, #38678, #74625, .T. ) ;
#32437 = FACE_OUTER_BOUND ( 'NONE', #40705, .T. ) ;
#32438 = CARTESIAN_POINT ( 'NONE',  ( 103.8128537583787363, -48.15082670742215498, 217.3556252759109668 ) ) ;
#32439 = CARTESIAN_POINT ( 'NONE',  ( 103.3624612311685809, -47.14358183654965018, 98.31657765686297523 ) ) ;
#32440 = CARTESIAN_POINT ( 'NONE',  ( 106.2987435450237541, -47.16992394167115776, 218.5184824187679453 ) ) ;
#32441 = DIRECTION ( 'NONE',  ( 0.000000000000000000, 0.000000000000000000, 1.000000000000000000 ) ) ;
#32442 = DIRECTION ( 'NONE',  ( 0.000000000000000000, 0.000000000000000000, 1.000000000000000000 ) ) ;
#32444 = CARTESIAN_POINT ( 'NONE',  ( 100.6688401597533868, -44.50955353575831452, 38.02898386382569385 ) ) ;
#32443 = DIRECTION ( 'NONE',  ( -4.237773401492740281E-14, 1.000000000000000000, 0.000000000000000000 ) ) ;
#32445 = DIRECTION ( 'NONE',  ( -3.100000000000000258E-29, 3.100000000000000044E-14, 1.000000000000000000 ) ) ;
#32446 = EDGE_CURVE ( 'NONE', #22553, #77150, #47710, .T. ) ;
#32447 = AXIS2_PLACEMENT_3D ( 'NONE', #59645, #18324, #38763 ) ;
#32448 = DIRECTION ( 'NONE',  ( 1.000000000000000078E-15, -1.000000000000000000, 0.000000000000000000 ) ) ;
#32449 = EDGE_CURVE ( 'NONE', #29859, #46563, #28597, .T. ) ;
#32450 = EDGE_CURVE ( 'NONE', #42888, #88057, #75860, .T. ) ;
#32451 = VERTEX_POINT ( 'NONE', #69046 ) ;
#32452 = ORIENTED_EDGE ( 'NONE', *, *, #66428, .F. ) ;
#32453 = CARTESIAN_POINT ( 'NONE',  ( 103.8778598771455677, -28.80550795996352420, 129.8038483995049432 ) ) ;
#32455 = ORIENTED_EDGE ( 'NONE', *, *, #37422, .T. ) ;
#32454 = DIRECTION ( 'NONE',  ( 0.000000000000000000, 0.000000000000000000, -1.000000000000000000 ) ) ;
#32456 = CARTESIAN_POINT ( 'NONE',  ( 97.81375517989221180, -40.51659548082960072, 91.63516306087667829 ) ) ;
#32457 = CARTESIAN_POINT ( 'NONE',  ( 108.5866130067098254, -47.05677245125736619, 138.6927681330539883 ) ) ;
#32458 = ADVANCED_FACE ( 'NONE', ( #6812 ), #56286, .T. ) ;
#32459 = FACE_OUTER_BOUND ( 'NONE', #77269, .T. ) ;
#32460 = ADVANCED_FACE ( 'NONE', ( #84030 ), #27708, .F. ) ;
#32461 = CARTESIAN_POINT ( 'NONE',  ( 77.31648329127399677, -18.72944715994106346, 6.749768910606400496 ) ) ;
#32462 = DIRECTION ( 'NONE',  ( 0.000000000000000000, -1.000000000000000000, -8.792068030499130893E-15 ) ) ;
#32463 = CARTESIAN_POINT ( 'NONE',  ( -7.196800215918080040E-13, 117.4749999999999943, 110.3312500000000114 ) ) ;
#32464 = CARTESIAN_POINT ( 'NONE',  ( 110.1676348244934616, -46.62498374987622896, 52.80610146638697699 ) ) ;
#32465 = ORIENTED_EDGE ( 'NONE', *, *, #14214, .T. ) ;
#32466 = ORIENTED_EDGE ( 'NONE', *, *, #14633, .F. ) ;
#32467 = VERTEX_POINT ( 'NONE', #38424 ) ;
#32468 = AXIS2_PLACEMENT_3D ( 'NONE', #26085, #52404, #24740 ) ;
#32469 = DIRECTION ( 'NONE',  ( 1.000000000000000000, 1.087812297297669405E-15, -2.722181216227750097E-30 ) ) ;
#32471 = FACE_OUTER_BOUND ( 'NONE', #59827, .T. ) ;
#32470 = CARTESIAN_POINT ( 'NONE',  ( 111.1483613326457629, -47.07112276671751516, 168.8756252759109486 ) ) ;
#32472 = CIRCLE ( 'NONE', #576, 10.00000000000000711 ) ;
#32473 = CARTESIAN_POINT ( 'NONE',  ( -187.8075999999999794, 101.5999999999999943, -9.525000000000000355 ) ) ;
#32474 = CARTESIAN_POINT ( 'NONE',  ( 176.5667039024412759, -48.82844715994099971, 180.4678068554150343 ) ) ;
#32475 = DIRECTION ( 'NONE',  ( -1.000000000000000000, 8.775353200852647323E-16, 0.000000000000000000 ) ) ;
#32476 = ADVANCED_FACE ( 'NONE', ( #78121 ), #26013, .T. ) ;
#32477 = CARTESIAN_POINT ( 'NONE',  ( 80.89343850130745750, 94.60304557064716846, 86.67392531623393381 ) ) ;
#32478 = CARTESIAN_POINT ( 'NONE',  ( 105.7152543472329427, -46.72382459542755839, 178.4689408536116275 ) ) ;
#32479 = CARTESIAN_POINT ( 'NONE',  ( 115.1902516771093445, -44.19056033372790893, 78.22324432352995416 ) ) ;
#32480 = ORIENTED_EDGE ( 'NONE', *, *, #36048, .F. ) ;
#32481 = EDGE_LOOP ( 'NONE', ( #4487, #52811, #13706, #85275 ) ) ;
#32482 = ADVANCED_FACE ( 'NONE', ( #45662, #1356 ), #56748, .F. ) ;
#32483 = DIRECTION ( 'NONE',  ( 1.000000000000000078E-15, -1.000000000000000083E-30, -1.000000000000000000 ) ) ;
#32484 = CARTESIAN_POINT ( 'NONE',  ( 74.98969683741650272, 82.54999999999999716, 346.9005000000000223 ) ) ;
#32485 = ADVANCED_FACE ( 'NONE', ( #84935 ), #15439, .T. ) ;
#32486 = DIRECTION ( 'NONE',  ( -1.000000000000000000, 1.122464679914735423E-15, 0.000000000000000000 ) ) ;
#32487 = CARTESIAN_POINT ( 'NONE',  ( 112.8963470814680932, -31.01156847455079912, 147.2623760838769726 ) ) ;
#32488 = VECTOR ( 'NONE', #71412, 1000.000000000000000 ) ;
#32489 = VECTOR ( 'NONE', #26431, 1000.000000000000000 ) ;
#32490 = AXIS2_PLACEMENT_3D ( 'NONE', #38905, #80715, #58894 ) ;
#32491 = CARTESIAN_POINT ( 'NONE',  ( 177.0664832912730162, 12.92155284005730387, 355.9756252759109998 ) ) ;
#32492 = VERTEX_POINT ( 'NONE', #3914 ) ;
#32493 = EDGE_LOOP ( 'NONE', ( #70239, #60907, #62862, #79249 ) ) ;
#32494 = CARTESIAN_POINT ( 'NONE',  ( 162.7866693523280048, -29.62846900982320264, -5.074374724088000832 ) ) ;
#32495 = AXIS2_PLACEMENT_3D ( 'NONE', #30661, #51529, #79279 ) ;
#32496 = EDGE_LOOP ( 'NONE', ( #57761, #65260 ) ) ;
#32497 = ORIENTED_EDGE ( 'NONE', *, *, #16921, .T. ) ;
#32498 = CARTESIAN_POINT ( 'NONE',  ( 100.8594679592218171, 82.54999999999999716, -82.89895571708191824 ) ) ;
#32499 = B_SPLINE_CURVE_WITH_KNOTS ( 'NONE', 3,
 ( #81402, #19151, #19587, #69990, #20506, #34557, #76801, #494, #54083, #48172, #20048, #54528, #27299, #75905, #82292, #89542, #35449, #83182 ),
 .UNSPECIFIED., .F., .F.,
 ( 4, 2, 2, 2, 2, 2, 2, 2, 4 ),
 ( 0.5000035245575573661, 0.5625030839878626399, 0.6250026434181680246, 0.6875022028484734093, 0.7500017622787786831, 0.8125013217090839568, 0.8750008811393893415, 0.9375004405696947263, 1.000000000000000000 ),
 .UNSPECIFIED. ) ;
#32500 = CARTESIAN_POINT ( 'NONE',  ( 109.6042693146342515, -27.68311267370638618, 216.3025356868499500 ) ) ;
#32501 = CARTESIAN_POINT ( 'NONE',  ( 104.0667030381796963, -67.87844715994094713, 93.21780742166239975 ) ) ;
#32502 = FACE_OUTER_BOUND ( 'NONE', #10402, .T. ) ;
#32503 = DIRECTION ( 'NONE',  ( 0.7071067811864697461, 0.7071067811866252883, 7.071067811864691403E-16 ) ) ;
#32504 = ORIENTED_EDGE ( 'NONE', *, *, #29827, .F. ) ;
#32505 = ORIENTED_EDGE ( 'NONE', *, *, #39832, .F. ) ;
#32506 = ORIENTED_EDGE ( 'NONE', *, *, #39402, .T. ) ;
#32507 = ORIENTED_EDGE ( 'NONE', *, *, #70071, .T. ) ;
#32508 = CARTESIAN_POINT ( 'NONE',  ( 104.8109701446277171, -28.85573464981227687, 223.1166617981629656 ) ) ;
#32509 = CARTESIAN_POINT ( 'NONE',  ( 117.6177984774595870, -42.17956309877360610, 93.44705384733897802 ) ) ;
#32510 = CARTESIAN_POINT ( 'NONE',  ( 115.0059970501927182, -43.50650750775904640, 63.26419670448196797 ) ) ;
#32511 = CARTESIAN_POINT ( 'NONE',  ( 115.7810385730902709, -41.80580201647777017, 253.4065349762460357 ) ) ;
#32512 = FACE_OUTER_BOUND ( 'NONE', #84730, .T. ) ;
#32513 = CARTESIAN_POINT ( 'NONE',  ( 172.5664832912740110, -32.07844715994070839, 258.9256252759120116 ) ) ;
#32514 = CARTESIAN_POINT ( 'NONE',  ( 114.3439067968150624, -29.21543093042305728, 170.4641967044829585 ) ) ;
#32515 = DIRECTION ( 'NONE',  ( 0.000000000000000000, 0.000000000000000000, -1.000000000000000000 ) ) ;
#32516 = ORIENTED_EDGE ( 'NONE', *, *, #71708, .F. ) ;
#32517 = CARTESIAN_POINT ( 'NONE',  ( 51.23005224011598102, -33.89581943344511217, -5.074374724088000832 ) ) ;
#32518 = EDGE_LOOP ( 'NONE', ( #754, #78348, #87901, #66418, #52281, #12082 ) ) ;
#32519 = ORIENTED_EDGE ( 'NONE', *, *, #13198, .F. ) ;
#32520 = CARTESIAN_POINT ( 'NONE',  ( 49.35031423293579422, -29.99615139352249926, 193.9678068554150911 ) ) ;
#32521 = DIRECTION ( 'NONE',  ( -0.7071067811865470176, -0.7071067811865480168, 0.000000000000000000 ) ) ;
#32522 = ORIENTED_EDGE ( 'NONE', *, *, #88901, .T. ) ;
#32523 = CIRCLE ( 'NONE', #44133, 3.499999999999996003 ) ;
#32524 = DIRECTION ( 'NONE',  ( 1.000000000000000000, 1.000000000000000078E-15, 1.000000000000000078E-15 ) ) ;
#32525 = EDGE_LOOP ( 'NONE', ( #48662, #24801, #32690, #51406 ) ) ;
#32526 = CARTESIAN_POINT ( 'NONE',  ( 117.0608945229253095, -38.08045312698342144, 178.7189586088083217 ) ) ;
#32527 = CARTESIAN_POINT ( 'NONE',  ( 118.8429430416104680, -35.40450127974935413, 83.91562527591095488 ) ) ;
#32528 = CARTESIAN_POINT ( 'NONE',  ( -4.046498181513055847, 70.50995738321196882, 130.4933223593253047 ) ) ;
#32529 = CIRCLE ( 'NONE', #18075, 2.750000000000002665 ) ;
#32530 = ADVANCED_FACE ( 'NONE', ( #70392 ), #52474, .T. ) ;
#32531 = CARTESIAN_POINT ( 'NONE',  ( 118.7735074478422348, -37.73348171986721411, 298.1356252759109680 ) ) ;
#32532 = CARTESIAN_POINT ( 'NONE',  ( 180.1667039024476651, -28.27351298636767041, 193.9678068554150059 ) ) ;
#32533 = ADVANCED_FACE ( 'NONE', ( #79795 ), #29059, .T. ) ;
#32536 = CARTESIAN_POINT ( 'NONE',  ( 98.68348088377354088, -30.50934295487602199, 176.8184824187679567 ) ) ;
#32535 = CARTESIAN_POINT ( 'NONE',  ( 97.81196631179071233, -40.51810333633504513, 56.63526628290931342 ) ) ;
#32534 = CARTESIAN_POINT ( 'NONE',  ( 25.56670390244797275, -48.82844715994099971, 257.2178068554150059 ) ) ;
#32537 = DIRECTION ( 'NONE',  ( 0.000000000000000000, 0.000000000000000000, 1.000000000000000000 ) ) ;
#32538 = LINE ( 'NONE', #60243, #85946 ) ;
#32539 = VERTEX_POINT ( 'NONE', #49923 ) ;
#32540 = CYLINDRICAL_SURFACE ( 'NONE', #13548, 2.500000000000002220 ) ;
#32541 = EDGE_CURVE ( 'NONE', #48061, #47812, #59311, .T. ) ;
#32542 = CARTESIAN_POINT ( 'NONE',  ( 182.5667039024469886, -33.35206098992650681, 342.9256252759109884 ) ) ;
#32543 = LINE ( 'NONE', #52521, #89445 ) ;
#32544 = ADVANCED_FACE ( 'NONE', ( #87044 ), #22703, .T. ) ;
#32545 = DIRECTION ( 'NONE',  ( 1.054009200593500181E-15, 1.000000000000000000, 0.000000000000000000 ) ) ;
#32547 = ORIENTED_EDGE ( 'NONE', *, *, #51810, .T. ) ;
#32546 = CARTESIAN_POINT ( 'NONE',  ( 100.6291634319263864, -44.98581313249158598, 232.0499109901969632 ) ) ;
#32548 = ADVANCED_FACE ( 'NONE', ( #57188 ), #35858, .T. ) ;
#32549 = CARTESIAN_POINT ( 'NONE',  ( 104.4897453729551984, -26.97886022956733143, 145.2814755117790355 ) ) ;
#32550 = CARTESIAN_POINT ( 'NONE',  ( 116.1583077856502086, -43.02023234939740348, 9.356577656862985037 ) ) ;
#32551 = CARTESIAN_POINT ( 'NONE',  ( 96.65590158217011663, -37.83070472558634378, 122.4099109901969626 ) ) ;
#32552 = DIRECTION ( 'NONE',  ( 0.000000000000000000, 0.000000000000000000, -1.000000000000000000 ) ) ;
#32553 = CARTESIAN_POINT ( 'NONE',  ( 8.387211759491236762, 92.12327290876406494, -130.2876699444761073 ) ) ;
#32554 = LINE ( 'NONE', #60260, #39883 ) ;
#32555 = CARTESIAN_POINT ( 'NONE',  ( 140.0667039024470171, -90.27844715994091018, 222.2178068554179902 ) ) ;
#32556 = ORIENTED_EDGE ( 'NONE', *, *, #81762, .T. ) ;
#32557 = ADVANCED_FACE ( 'NONE', ( #43107, #63576, #80233, #17981 ), #73395, .T. ) ;
#32558 = AXIS2_PLACEMENT_3D ( 'NONE', #42071, #71599, #2557 ) ;
#32559 = AXIS2_PLACEMENT_3D ( 'NONE', #11465, #89116, #20528 ) ;
#32560 = AXIS2_PLACEMENT_3D ( 'NONE', #83476, #55727, #14445 ) ;
#32561 = AXIS2_PLACEMENT_3D ( 'NONE', #78389, #30220, #28417 ) ;
#32562 = EDGE_CURVE ( 'NONE', #42067, #50592, #84062, .T. ) ;
#32563 = EDGE_LOOP ( 'NONE', ( #72670, #88090, #41557 ) ) ;
#32564 = ORIENTED_EDGE ( 'NONE', *, *, #9236, .T. ) ;
#32565 = AXIS2_PLACEMENT_3D ( 'NONE', #20060, #60019, #32782 ) ;
#32566 = CIRCLE ( 'NONE', #35482, 0.5000000000000004441 ) ;
#32567 = ORIENTED_EDGE ( 'NONE', *, *, #6491, .T. ) ;
#32568 = CARTESIAN_POINT ( 'NONE',  ( 104.4081006448918174, -46.45808913579163857, 72.36479194125030290 ) ) ;
#32569 = CARTESIAN_POINT ( 'NONE',  ( 109.6376038899290393, -46.81002275840752702, 43.77562527591094721 ) ) ;
#32570 = CARTESIAN_POINT ( 'NONE',  ( 25.56670390244797275, -62.87844715994099687, 257.2178068554150059 ) ) ;
#32571 = CARTESIAN_POINT ( 'NONE',  ( 116.3167039024470029, -68.87844715994093292, 222.2178068554179902 ) ) ;
#32572 = EDGE_CURVE ( 'NONE', #16242, #7908, #44871, .T. ) ;
#32574 = CARTESIAN_POINT ( 'NONE',  ( 68.55293230179317732, -139.1646755592869908, 245.6810956053649875 ) ) ;
#32573 = CARTESIAN_POINT ( 'NONE',  ( 127.0667052882549797, -71.37844715994091871, 55.21780685541800437 ) ) ;
#32575 = CARTESIAN_POINT ( 'NONE',  ( 100.3258375188005402, -30.68160747159130963, 235.1790864947439559 ) ) ;
#32576 = VERTEX_POINT ( 'NONE', #64030 ) ;
#32577 = EDGE_CURVE ( 'NONE', #35335, #30635, #36769, .T. ) ;
#32578 = ORIENTED_EDGE ( 'NONE', *, *, #58909, .T. ) ;
#32579 = VERTEX_POINT ( 'NONE', #3472 ) ;
#32580 = PLANE ( 'NONE',  #58679 ) ;
#32581 = CARTESIAN_POINT ( 'NONE',  ( 113.2149055592938964, -44.63128427178952506, 183.1027008292588505 ) ) ;
#32582 = DIRECTION ( 'NONE',  ( 0.000000000000000000, -1.000000000000000000, 0.000000000000000000 ) ) ;
#32583 = CYLINDRICAL_SURFACE ( 'NONE', #2584, 5.599999999999994316 ) ;
#32584 = CARTESIAN_POINT ( 'NONE',  ( 110.7632188227358512, -44.78316835090528514, 24.35015473446894418 ) ) ;
#32585 = DIRECTION ( 'NONE',  ( 0.000000000000000000, 3.785359618865284342E-16, -1.000000000000000000 ) ) ;
#32586 = DIRECTION ( 'NONE',  ( -0.000000000000000000, 1.000000000000000000, 0.000000000000000000 ) ) ;
#32587 = CARTESIAN_POINT ( 'NONE',  ( 114.5610390845466355, -30.44493693613343765, 269.3813395616256798 ) ) ;
#32588 = CARTESIAN_POINT ( 'NONE',  ( 63.06670390244645574, -24.92844715994017335, 129.9678068554150911 ) ) ;
#32589 = ORIENTED_EDGE ( 'NONE', *, *, #2662, .T. ) ;
#32590 = EDGE_CURVE ( 'NONE', #30367, #82586, #31163, .T. ) ;
#32591 = CARTESIAN_POINT ( 'NONE',  ( 103.7678503744106138, -27.28725441292130682, 56.34392717193131972 ) ) ;
#32592 = EDGE_CURVE ( 'NONE', #39230, #87811, #74746, .T. ) ;
#32593 = DIRECTION ( 'NONE',  ( 0.000000000000000000, 1.000000000000000000, 0.000000000000000000 ) ) ;
#32594 = CARTESIAN_POINT ( 'NONE',  ( 99.15069935661746570, -33.23069170325895527, 53.80142370292495713 ) ) ;
#32595 = VECTOR ( 'NONE', #55556, 1000.000000000000000 ) ;
#32596 = CARTESIAN_POINT ( 'NONE',  ( 135.3633572498686988, -16.30134337669370836, 7.962481652676212107 ) ) ;
#32597 = VECTOR ( 'NONE', #10332, 1000.000000000000000 ) ;
#32598 = DIRECTION ( 'NONE',  ( 1.067522139062650671E-15, 1.000000000000000000, 0.000000000000000000 ) ) ;
#32599 = CARTESIAN_POINT ( 'NONE',  ( -3.968750000000754508, 127.0000000000000000, 100.8961411191535973 ) ) ;
#32600 = VERTEX_POINT ( 'NONE', #12978 ) ;
#32601 = LINE ( 'NONE', #73495, #66822 ) ;
#32602 = DIRECTION ( 'NONE',  ( -0.7071067811864671926, -0.7071067811866279529, -7.071067811864664779E-16 ) ) ;
#32603 = ORIENTED_EDGE ( 'NONE', *, *, #84015, .T. ) ;
#32604 = CARTESIAN_POINT ( 'NONE',  ( 112.8018845221357367, -47.09986945403115044, 102.9784824187679817 ) ) ;
#32605 = EDGE_LOOP ( 'NONE', ( #22541, #25489 ) ) ;
#32606 = CARTESIAN_POINT ( 'NONE',  ( 104.4240671743138478, -44.88234475468695450, 81.74956268521998481 ) ) ;
#32607 = DIRECTION ( 'NONE',  ( -0.7071067811856560636, -0.7071067811874389708, 0.000000000000000000 ) ) ;
#32608 = CARTESIAN_POINT ( 'NONE',  ( 103.0662520580798116, -44.63681263099613972, 123.6358690201829802 ) ) ;
#32609 = EDGE_CURVE ( 'NONE', #46763, #6826, #44802, .T. ) ;
#32610 = DIRECTION ( 'NONE',  ( 1.000000000000000000, 0.000000000000000000, 0.000000000000000000 ) ) ;
#32611 = CARTESIAN_POINT ( 'NONE',  ( 147.0700838452252981, -67.87844715994090450, 246.0535151165250056 ) ) ;
#32612 = CARTESIAN_POINT ( 'NONE',  ( 106.5169537372109545, -25.66675205370546919, 41.12800622829193742 ) ) ;
#32613 = FACE_OUTER_BOUND ( 'NONE', #34757, .T. ) ;
#32614 = VERTEX_POINT ( 'NONE', #32498 ) ;
#32615 = EDGE_CURVE ( 'NONE', #46455, #42342, #4812, .T. ) ;
#32616 = LINE ( 'NONE', #33957, #37234 ) ;
#32617 = VECTOR ( 'NONE', #25208, 1000.000000000000114 ) ;
#32618 = ORIENTED_EDGE ( 'NONE', *, *, #15375, .F. ) ;
#32619 = PLANE ( 'NONE',  #83188 ) ;
#32620 = AXIS2_PLACEMENT_3D ( 'NONE', #42174, #14041, #63076 ) ;
#32621 = CIRCLE ( 'NONE', #86331, 27.49999999999999645 ) ;
#32622 = VECTOR ( 'NONE', #8183, 1000.000000000000000 ) ;
#32623 = ORIENTED_EDGE ( 'NONE', *, *, #10140, .T. ) ;
#32624 = VERTEX_POINT ( 'NONE', #40666 ) ;
#32625 = AXIS2_PLACEMENT_3D ( 'NONE', #2088, #56121, #42059 ) ;
#32626 = VECTOR ( 'NONE', #78881, 1000.000000000000000 ) ;
#32627 = DIRECTION ( 'NONE',  ( 1.000000000000000000, 0.000000000000000000, 0.000000000000000000 ) ) ;
#32628 = ORIENTED_EDGE ( 'NONE', *, *, #25047, .F. ) ;
#32629 = CARTESIAN_POINT ( 'NONE',  ( 116.2779988688840547, -41.49250982992363390, 243.4346728949589647 ) ) ;
#32630 = LINE ( 'NONE', #45795, #46576 ) ;
#32631 = LINE ( 'NONE', #88064, #49050 ) ;
#32632 = CARTESIAN_POINT ( 'NONE',  ( 116.7448692891101985, -32.85500114480387168, 50.12991099019698282 ) ) ;
#32633 = DIRECTION ( 'NONE',  ( 0.000000000000000000, 0.000000000000000000, -1.000000000000000000 ) ) ;
#32634 = VERTEX_POINT ( 'NONE', #54717 ) ;
#32635 = CARTESIAN_POINT ( 'NONE',  ( 115.0891255709548773, -30.61791286384668354, 114.3446839461548024 ) ) ;
#32636 = CARTESIAN_POINT ( 'NONE',  ( 74.06670390244704549, -118.2784471599409812, 51.21780685541800437 ) ) ;
#32637 = VECTOR ( 'NONE', #1086, 1000.000000000000000 ) ;
#32639 = ORIENTED_EDGE ( 'NONE', *, *, #10510, .T. ) ;
#32638 = ADVANCED_FACE ( 'NONE', ( #13422 ), #53819, .F. ) ;
#32640 = LINE ( 'NONE', #11307, #88024 ) ;
#32641 = DIRECTION ( 'NONE',  ( 1.000000000000000000, 3.999999999999999995E-14, 1.000000000000000078E-15 ) ) ;
#32642 = CARTESIAN_POINT ( 'NONE',  ( 96.55902551080266960, -40.08462249002853639, 281.5603871806728762 ) ) ;
#32643 = CARTESIAN_POINT ( 'NONE',  ( 172.5664832912740110, 0.2215528400590013880, 18.92562527591200094 ) ) ;
#32644 = AXIS2_PLACEMENT_3D ( 'NONE', #44715, #65616, #17035 ) ;
#32645 = EDGE_CURVE ( 'NONE', #32309, #75634, #11489, .T. ) ;
#32646 = CARTESIAN_POINT ( 'NONE',  ( 46.83715912545339677, -47.82818131006086304, 180.4678068554150911 ) ) ;
#32647 = CARTESIAN_POINT ( 'NONE',  ( 19.56648329127400032, -18.82844715994099971, -5.074374724088000832 ) ) ;
#32648 = EDGE_CURVE ( 'NONE', #72716, #69535, #24585, .T. ) ;
#32649 = CARTESIAN_POINT ( 'NONE',  ( 105.4627246288800109, -27.81649992262058646, 274.6286103042674540 ) ) ;
#32651 = CARTESIAN_POINT ( 'NONE',  ( 113.4461594614341209, -46.68675298423766407, 64.02991099019695298 ) ) ;
#32650 = CARTESIAN_POINT ( 'NONE',  ( -186.2398777604655038, 0.000000000000000000, -6.349999999999999645 ) ) ;
#32652 = CARTESIAN_POINT ( 'NONE',  ( 113.1214584048637732, 68.77817172032477799, 65.17982383002866698 ) ) ;
#32653 = CARTESIAN_POINT ( 'NONE',  ( 114.5437501075917481, -29.39581020157643110, 149.4441967044819819 ) ) ;
#32654 = VERTEX_POINT ( 'NONE', #47013 ) ;
#32655 = CARTESIAN_POINT ( 'NONE',  ( 108.0667039024470455, -121.2010968907522113, -11.78219314458148226 ) ) ;
#32656 = ORIENTED_EDGE ( 'NONE', *, *, #7946, .F. ) ;
#32657 = LINE ( 'NONE', #68083, #39602 ) ;
#32658 = EDGE_CURVE ( 'NONE', #61103, #74274, #73845, .T. ) ;
#32659 = FACE_OUTER_BOUND ( 'NONE', #56422, .T. ) ;
#32660 = CARTESIAN_POINT ( 'NONE',  ( 107.0664832912750057, -36.72944715993903486, 6.826283056785790393 ) ) ;
#32661 = ORIENTED_EDGE ( 'NONE', *, *, #16473, .T. ) ;
#32662 = CARTESIAN_POINT ( 'NONE',  ( 0.000000000000000000, 127.0000000000000000, 90.32146847885337593 ) ) ;
#32663 = EDGE_CURVE ( 'NONE', #35560, #2509, #61109, .T. ) ;
#32665 = EDGE_LOOP ( 'NONE', ( #31690, #70338 ) ) ;
#32664 = CARTESIAN_POINT ( 'NONE',  ( 112.1415033342358640, -47.49387789398046067, 137.9270538473389820 ) ) ;
#32667 = DIRECTION ( 'NONE',  ( 3.491483361109380094E-15, 0.000000000000000000, 1.000000000000000000 ) ) ;
#32666 = UNCERTAINTY_MEASURE_WITH_UNIT (LENGTH_MEASURE( 1.000000000000000082E-05 ), #45438, 'distance_accuracy_value', 'NONE');
#32668 = CARTESIAN_POINT ( 'NONE',  ( -130.4667782423797746, 94.30053025434479252, 4.871090630222163043 ) ) ;
#32669 = CARTESIAN_POINT ( 'NONE',  ( 41.56648329127399677, 0.2215528400590013880, 201.0426252759120018 ) ) ;
#32670 = AXIS2_PLACEMENT_3D ( 'NONE', #21150, #48822, #77012 ) ;
#32671 = DIRECTION ( 'NONE',  ( 0.000000000000000000, 0.000000000000000000, -1.000000000000000000 ) ) ;
#32672 = ORIENTED_EDGE ( 'NONE', *, *, #70287, .F. ) ;
#32673 = EDGE_CURVE ( 'NONE', #11503, #31292, #42009, .T. ) ;
#32674 = CARTESIAN_POINT ( 'NONE',  ( 102.3831517106511484, -26.69142711411281255, 135.4118157521009493 ) ) ;
#32675 = PRODUCT_CONTEXT ( 'NONE', #9218, 'mechanical' ) ;
#32676 = AXIS2_PLACEMENT_3D ( 'NONE', #80615, #18364, #72890 ) ;
#32677 = FACE_OUTER_BOUND ( 'NONE', #89291, .T. ) ;
#32678 = CYLINDRICAL_SURFACE ( 'NONE', #38376, 0.9999999999992039701 ) ;
#32679 = ORIENTED_EDGE ( 'NONE', *, *, #27667, .T. ) ;
#32680 = ADVANCED_FACE ( 'NONE', ( #87927 ), #52905, .F. ) ;
#32681 = ORIENTED_EDGE ( 'NONE', *, *, #66602, .F. ) ;
#32682 = DIRECTION ( 'NONE',  ( 0.000000000000000000, 0.000000000000000000, -1.000000000000000000 ) ) ;
#32683 = CARTESIAN_POINT ( 'NONE',  ( 101.6985779264912821, -28.22415967511243906, 250.5243335900576653 ) ) ;
#32684 = DIRECTION ( 'NONE',  ( 0.000000000000000000, 0.000000000000000000, 1.000000000000000000 ) ) ;
#32685 = CARTESIAN_POINT ( 'NONE',  ( 110.7536356736639078, -102.7271463785358492, -19.78219314458207378 ) ) ;
#32687 = CARTESIAN_POINT ( 'NONE',  ( 165.3359832912740046, -36.32844715994100682, 193.9678068554150059 ) ) ;
#32686 = CARTESIAN_POINT ( 'NONE',  ( 97.07206558903125426, -35.37850437031580242, 106.2189636383757687 ) ) ;
#32688 = CARTESIAN_POINT ( 'NONE',  ( -33.98325472291465132, 124.5870000000000033, 3.174999999999764899 ) ) ;
#32689 = AXIS2_PLACEMENT_3D ( 'NONE', #59276, #4331, #66092 ) ;
#32690 = ORIENTED_EDGE ( 'NONE', *, *, #32615, .T. ) ;
#32691 = CIRCLE ( 'NONE', #39947, 11.49999999999999645 ) ;
#32692 = VECTOR ( 'NONE', #61852, 1000.000000000000000 ) ;
#32693 = VECTOR ( 'NONE', #43577, 1000.000000000000000 ) ;
#32694 = CARTESIAN_POINT ( 'NONE',  ( 172.5664832912728457, -27.82844715994070484, 81.92562527591199739 ) ) ;
#32695 = CARTESIAN_POINT ( 'NONE',  ( 96.86352172870826394, -32.31225822881506815, 207.0013395616249738 ) ) ;
#32697 = VERTEX_POINT ( 'NONE', #6600 ) ;
#32696 = FACE_OUTER_BOUND ( 'NONE', #41358, .T. ) ;
#32698 = VECTOR ( 'NONE', #54215, 1000.000000000000000 ) ;
#32699 = CARTESIAN_POINT ( 'NONE',  ( 107.8187922529720026, -26.97765417004757538, 66.01562527591097762 ) ) ;
#32700 = CARTESIAN_POINT ( 'NONE',  ( 61.56670390244727287, -23.42844715994043980, 300.4678068554150627 ) ) ;
#32701 = CARTESIAN_POINT ( 'NONE',  ( 188.5667039024479834, -62.87844715994099687, 257.2178068554150059 ) ) ;
#32702 = ORIENTED_EDGE ( 'NONE', *, *, #25884, .T. ) ;
#32703 = DIRECTION ( 'NONE',  ( -0.000000000000000000, -0.000000000000000000, 1.000000000000000000 ) ) ;
#32704 = ORIENTED_EDGE ( 'NONE', *, *, #36375, .T. ) ;
#32705 = ORIENTED_EDGE ( 'NONE', *, *, #42984, .F. ) ;
#32706 = EDGE_CURVE ( 'NONE', #79978, #4573, #76845, .T. ) ;
#32707 = AXIS2_PLACEMENT_3D ( 'NONE', #48534, #7243, #8135 ) ;
#32708 = CARTESIAN_POINT ( 'NONE',  ( 115.9133815579708937, -36.21888896485111076, 225.3044404487539794 ) ) ;
#32709 = DIRECTION ( 'NONE',  ( 1.000000000000000000, 0.000000000000000000, 0.000000000000000000 ) ) ;
#32710 = CARTESIAN_POINT ( 'NONE',  ( -84.19383299529339126, 88.91243380484083048, 99.78216974382904425 ) ) ;
#32711 = B_SPLINE_CURVE_WITH_KNOTS ( 'NONE', 3,
 ( #62806, #69188, #26961, #82388, #145, #54181, #27844, #7851, #19695, #35551, #6961, #34209, #55522, #42351, #49168, #62363, #75999, #20152 ),
 .UNSPECIFIED., .F., .F.,
 ( 4, 2, 2, 2, 2, 2, 2, 2, 4 ),
 ( 0.000000000000000000, 0.06249945059766286864, 0.1249989011953257373, 0.1874983517929885990, 0.2499978023906514746, 0.3124972529883143224, 0.3749967035859771980, 0.4374961541836400736, 0.4999956047813029492 ),
 .UNSPECIFIED. ) ;
#32712 = DIRECTION ( 'NONE',  ( 1.639958061481212836E-42, -4.100000000000000342E-29, -1.000000000000000000 ) ) ;
#32713 = CARTESIAN_POINT ( 'NONE',  ( 82.80053463576300032, -37.07423037057513682, 3.076719480831281217 ) ) ;
#32714 = ORIENTED_EDGE ( 'NONE', *, *, #27640, .F. ) ;
#32715 = DIRECTION ( 'NONE',  ( 2.900000000000000265E-14, -2.000000000000000155E-15, 1.000000000000000000 ) ) ;
#32716 = CARTESIAN_POINT ( 'NONE',  ( 116.3137647483393806, -32.94861263809731611, 185.1356252759109680 ) ) ;
#32717 = ORIENTED_EDGE ( 'NONE', *, *, #10741, .F. ) ;
#32718 = CARTESIAN_POINT ( 'NONE',  ( 104.2408938701987040, -46.76453939261368475, 22.35848241876792031 ) ) ;
#32719 = ORIENTED_EDGE ( 'NONE', *, *, #33393, .F. ) ;
#32720 = AXIS2_PLACEMENT_3D ( 'NONE', #87931, #45230, #32061 ) ;
#32721 = ORIENTED_EDGE ( 'NONE', *, *, #25593, .F. ) ;
#32722 = CARTESIAN_POINT ( 'NONE',  ( 101.0613286755868359, -30.49734935201787422, 263.4928522743534813 ) ) ;
#32723 = CARTESIAN_POINT ( 'NONE',  ( -89.60916260784479448, 224.4999999999999432, 134.1927865330827103 ) ) ;
#32724 = CARTESIAN_POINT ( 'NONE',  ( 116.6769215743980936, -34.91203320259893417, 158.9756252759109714 ) ) ;
#32725 = CARTESIAN_POINT ( 'NONE',  ( 23.22105850524281934, 78.42056979272489059, 305.2876152861762193 ) ) ;
#32726 = DIRECTION ( 'NONE',  ( 0.000000000000000000, 0.000000000000000000, 1.000000000000000000 ) ) ;
#32727 = CARTESIAN_POINT ( 'NONE',  ( 92.82872956494375671, -30.11307588647346023, 0.4256252759109567241 ) ) ;
#32729 = CARTESIAN_POINT ( 'NONE',  ( 99.05265045910354615, -29.93853425193624318, 211.7670538473399517 ) ) ;
#32728 = AXIS2_PLACEMENT_3D ( 'NONE', #88530, #4506, #45368 ) ;
#32730 = DIRECTION ( 'NONE',  ( 0.2884130866282246797, -0.7071067811865454633, -0.6456143519637579375 ) ) ;
#32731 = ORIENTED_EDGE ( 'NONE', *, *, #56380, .F. ) ;
#32732 = EDGE_CURVE ( 'NONE', #87803, #53062, #11549, .T. ) ;
#32733 = CARTESIAN_POINT ( 'NONE',  ( 107.3220933465437810, -25.63295393647281628, 71.04610146638795243 ) ) ;
#32734 = DIRECTION ( 'NONE',  ( 1.000000000000000078E-15, -1.000000000000000000, 0.000000000000000000 ) ) ;
#32735 = VECTOR ( 'NONE', #87489, 1000.000000000000000 ) ;
#32736 = ORIENTED_EDGE ( 'NONE', *, *, #19493, .T. ) ;
#32737 = ORIENTED_EDGE ( 'NONE', *, *, #60747, .F. ) ;
#32738 = ORIENTED_EDGE ( 'NONE', *, *, #29741, .F. ) ;
#32739 = DIRECTION ( 'NONE',  ( 0.000000000000000000, 0.000000000000000000, 1.000000000000000000 ) ) ;
#32740 = DIRECTION ( 'NONE',  ( -1.000000000000000000, 0.000000000000000000, -7.867884063170659983E-16 ) ) ;
#32741 = DIRECTION ( 'NONE',  ( 3.100000000000000258E-29, -3.100000000000000044E-14, -1.000000000000000000 ) ) ;
#32742 = CARTESIAN_POINT ( 'NONE',  ( 97.86260780209082100, -37.94289672904660193, 149.2480903695909547 ) ) ;
#32743 = CARTESIAN_POINT ( 'NONE',  ( 110.8246185410185944, -26.31015614812341141, 245.7889586092439629 ) ) ;
#32744 = PRODUCT_DEFINITION ( 'UNKNOWN', '', #78373, #85085 ) ;
#32745 = DIRECTION ( 'NONE',  ( 0.000000000000000000, -1.000000000000000000, 0.000000000000000000 ) ) ;
#32746 = ORIENTED_EDGE ( 'NONE', *, *, #61227, .T. ) ;
#32747 = FILL_AREA_STYLE ('',( #39112 ) ) ;
#32748 = FACE_OUTER_BOUND ( 'NONE', #82031, .T. ) ;
#32749 = VERTEX_POINT ( 'NONE', #49713 ) ;
#32750 = VERTEX_POINT ( 'NONE', #70169 ) ;
#32751 = AXIS2_PLACEMENT_3D ( 'NONE', #42293, #83661, #64112 ) ;
#32752 = LINE ( 'NONE', #45029, #57538 ) ;
#32753 = CIRCLE ( 'NONE', #40013, 3.300000000000000711 ) ;
#32754 = ORIENTED_EDGE ( 'NONE', *, *, #35969, .T. ) ;
#32755 = ORIENTED_EDGE ( 'NONE', *, *, #9007, .F. ) ;
#32756 = DIRECTION ( 'NONE',  ( 0.000000000000000000, 0.000000000000000000, -1.000000000000000000 ) ) ;
#32757 = DIRECTION ( 'NONE',  ( 1.000000000000000000, 1.000000000000000078E-15, 0.000000000000000000 ) ) ;
#32758 = CIRCLE ( 'NONE', #83545, 130.5560000000000116 ) ;
#32759 = LINE ( 'NONE', #60454, #48931 ) ;
#32760 = EDGE_CURVE ( 'NONE', #57180, #67629, #34748, .T. ) ;
#32761 = CARTESIAN_POINT ( 'NONE',  ( 103.7755263489600281, -28.29248842296361133, 169.7828960185539415 ) ) ;
#32762 = CARTESIAN_POINT ( 'NONE',  ( 111.4338919110110311, -46.24429912893436523, 27.91848241876792969 ) ) ;
#32763 = DIRECTION ( 'NONE',  ( 0.000000000000000000, 1.000000000000000000, 0.000000000000000000 ) ) ;
#32764 = ORIENTED_EDGE ( 'NONE', *, *, #24759, .T. ) ;
#32765 = EDGE_CURVE ( 'NONE', #32906, #2876, #55161, .T. ) ;
#32766 = DIRECTION ( 'NONE',  ( -1.000000000000000000, -0.000000000000000000, -0.000000000000000000 ) ) ;
#32767 = ADVANCED_FACE ( 'NONE', ( #82922 ), #28844, .T. ) ;
#32768 = ORIENTED_EDGE ( 'NONE', *, *, #21898, .F. ) ;
#32769 = CARTESIAN_POINT ( 'NONE',  ( 97.81169138727440782, -40.51741131469341184, 51.63568823874075520 ) ) ;
#32770 = EDGE_CURVE ( 'NONE', #36953, #62140, #15214, .T. ) ;
#32771 = ORIENTED_EDGE ( 'NONE', *, *, #78051, .F. ) ;
#32772 = FACE_OUTER_BOUND ( 'NONE', #31712, .T. ) ;
#32773 = FACE_OUTER_BOUND ( 'NONE', #74059, .T. ) ;
#32774 = CARTESIAN_POINT ( 'NONE',  ( 110.8532532929841636, -45.98473607795947515, 132.8855204752115924 ) ) ;
#32775 = AXIS2_PLACEMENT_3D ( 'NONE', #72156, #49896, #36289 ) ;
#32776 = DIRECTION ( 'NONE',  ( -2.999999999999999839E-15, 1.000000000000000000, -2.999999999999999900E-30 ) ) ;
#32777 = ORIENTED_EDGE ( 'NONE', *, *, #49709, .T. ) ;
#32778 = CARTESIAN_POINT ( 'NONE',  ( 105.4174756516424054, -47.04580008967651850, 37.44991099019695469 ) ) ;
#32779 = CARTESIAN_POINT ( 'NONE',  ( 96.88468944541251915, -39.16338508605922186, 52.51276813305394597 ) ) ;
#32780 = CIRCLE ( 'NONE', #26952, 17.33514202138209370 ) ;
#32782 = DIRECTION ( 'NONE',  ( -3.100000000000000258E-29, 3.100000000000000044E-14, 1.000000000000000000 ) ) ;
#32781 = DIRECTION ( 'NONE',  ( 0.9068632946707807507, -0.4214249218767880945, 8.673617379884035472E-16 ) ) ;
#32783 = CARTESIAN_POINT ( 'NONE',  ( 41.56648329127399677, -9.303447159940999356, 16.80862527591200006 ) ) ;
#32784 = CYLINDRICAL_SURFACE ( 'NONE', #23812, 4.749999999999976907 ) ;
#32785 = EDGE_CURVE ( 'NONE', #11728, #64364, #76994, .T. ) ;
#32786 = CARTESIAN_POINT ( 'NONE',  ( 51.06670390244683944, -33.35206098992668444, 117.4678068554150485 ) ) ;
#32787 = DIRECTION ( 'NONE',  ( 1.000000000000000078E-15, 1.000000000000000083E-30, -1.000000000000000000 ) ) ;
#32788 = ORIENTED_EDGE ( 'NONE', *, *, #51307, .T. ) ;
#32789 = CARTESIAN_POINT ( 'NONE',  ( 105.4140021367065003, -47.06753073853725056, 37.44991099019695469 ) ) ;
#32790 = CARTESIAN_POINT ( 'NONE',  ( 98.37977233551227130, -29.89460749427659181, 196.8080062282919869 ) ) ;
#32791 = CARTESIAN_POINT ( 'NONE',  ( 111.0909104302412373, -25.55688089738240976, 95.80133956162495679 ) ) ;
#32793 = LINE ( 'NONE', #4647, #45564 ) ;
#32792 = CARTESIAN_POINT ( 'NONE',  ( 194.0371591254574923, -24.42818131005417115, 193.9678068554150343 ) ) ;
#32794 = LINE ( 'NONE', #25988, #11781 ) ;
#32795 = VECTOR ( 'NONE', #2253, 1000.000000000000000 ) ;
#32796 = CARTESIAN_POINT ( 'NONE',  ( 105.7995185434065775, -26.72403495956872277, 186.1772919381388647 ) ) ;
#32797 = ORIENTED_EDGE ( 'NONE', *, *, #78936, .F. ) ;
#32798 = CARTESIAN_POINT ( 'NONE',  ( 104.2906771502716055, -46.10805769451163627, 103.3470538473389411 ) ) ;
#32800 = ORIENTED_EDGE ( 'NONE', *, *, #70300, .F. ) ;
#32799 = CARTESIAN_POINT ( 'NONE',  ( 11.71935769674032279, 87.44354605777512290, 130.0289424465127581 ) ) ;
#32801 = CARTESIAN_POINT ( 'NONE',  ( 107.2488531970940073, -24.90511003128411360, 226.0641967044829812 ) ) ;
#32802 = CARTESIAN_POINT ( 'NONE',  ( 186.6899999999999977, 46.38749999999999574, -50.79999999999999716 ) ) ;
#32803 = CARTESIAN_POINT ( 'NONE',  ( 112.4064011319317729, -45.19864057730971751, 148.0241013645836290 ) ) ;
#32804 = CARTESIAN_POINT ( 'NONE',  ( 97.81169817874256012, -40.51742791483425776, 82.63555527327814332 ) ) ;
#32805 = CARTESIAN_POINT ( 'NONE',  ( 165.3359832912749710, -36.32844715993532247, 193.9678068554149775 ) ) ;
#32806 = CARTESIAN_POINT ( 'NONE',  ( 133.1188885517794347, -39.31186128672820956, 1.764000668897718560 ) ) ;
#32807 = DIRECTION ( 'NONE',  ( 1.387778780781444492E-15, 0.000000000000000000, -1.000000000000000000 ) ) ;
#32808 = CARTESIAN_POINT ( 'NONE',  ( 102.3610132369663148, -45.97051510703457922, 172.2137205140069511 ) ) ;
#32809 = ORIENTED_EDGE ( 'NONE', *, *, #80138, .F. ) ;
#32810 = EDGE_LOOP ( 'NONE', ( #62464, #77386, #63761, #62153 ) ) ;
#32811 = EDGE_CURVE ( 'NONE', #81580, #46354, #72514, .T. ) ;
#32812 = CIRCLE ( 'NONE', #64727, 121.3994834560769647 ) ;
#32813 = CARTESIAN_POINT ( 'NONE',  ( 103.0939887460847189, -28.21499987170311385, 131.8434880678019567 ) ) ;
#32814 = VECTOR ( 'NONE', #72566, 1000.000000000000000 ) ;
#32815 = CARTESIAN_POINT ( 'NONE',  ( 21.03715912545829170, -47.82818131006186491, 249.9678068554150059 ) ) ;
#32816 = AXIS2_PLACEMENT_3D ( 'NONE', #25678, #44326, #51585 ) ;
#32818 = FACE_OUTER_BOUND ( 'NONE', #54354, .T. ) ;
#32817 = CARTESIAN_POINT ( 'NONE',  ( 113.9608400058609874, -28.00707201209563024, 270.5441967044819194 ) ) ;
#32819 = AXIS2_PLACEMENT_3D ( 'NONE', #49119, #540, #55933 ) ;
#32820 = DIRECTION ( 'NONE',  ( -0.9988791501868375944, -0.04215501712985142424, 0.02152667770008048417 ) ) ;
#32821 = EDGE_CURVE ( 'NONE', #43994, #48000, #1592, .T. ) ;
#32822 = PLANE ( 'NONE',  #20005 ) ;
#32823 = DIRECTION ( 'NONE',  ( -0.7071067811861110330, -0.7071067811869841124, 0.000000000000000000 ) ) ;
#32824 = LINE ( 'NONE', #68258, #59424 ) ;
#32825 = LINE ( 'NONE', #81008, #8127 ) ;
#32826 = B_SPLINE_SURFACE_WITH_KNOTS ( 'NONE', 3, 3, ( 
 ( #35042, #40520, #984, #55918 ),
 ( #76838, #61404, #69581, #6896 ),
 ( #35488, #41402, #83218, #7353 ),
 ( #75502, #62752, #70030, #63207 ),
 ( #55467, #20542, #21888, #82781 ) ),
 .UNSPECIFIED., .F., .F., .F.,
 ( 4, 1, 4 ),
 ( 4, 4 ),
 ( 0.000000000000000000, 0.5714285714285709528, 1.000000000000000000 ),
 ( -1.896658054595430056E-14, 0.2508910862621460125 ),
 .UNSPECIFIED. ) ;
#32827 = CARTESIAN_POINT ( 'NONE',  ( 101.3611157396114066, -46.16939438856412181, 202.1318157521019430 ) ) ;
#32828 = CARTESIAN_POINT ( 'NONE',  ( 123.6837132603318992, -20.11243780205710507, 239.5838068554165545 ) ) ;
#32829 = ORIENTED_EDGE ( 'NONE', *, *, #60839, .T. ) ;
#32830 = ORIENTED_EDGE ( 'NONE', *, *, #36741, .T. ) ;
#32831 = CARTESIAN_POINT ( 'NONE',  ( -187.8075999999999794, 101.5999999999999943, -6.349999999999999645 ) ) ;
#32832 = CARTESIAN_POINT ( 'NONE',  ( 81.19091742810981316, -21.23916151080281622, 8.028235474618183432 ) ) ;
#32833 = DIRECTION ( 'NONE',  ( 0.000000000000000000, 1.000000000000000000, 0.000000000000000000 ) ) ;
#32834 = CARTESIAN_POINT ( 'NONE',  ( 106.1656040943334318, -87.30234574837452044, -11.78219314458253741 ) ) ;
#32835 = VECTOR ( 'NONE', #61900, 1000.000000000000114 ) ;
#32836 = CARTESIAN_POINT ( 'NONE',  ( 107.0664832912739968, -36.72944715994100306, 9.635625275910941312 ) ) ;
#32837 = ORIENTED_EDGE ( 'NONE', *, *, #55698, .F. ) ;
#32838 = EDGE_CURVE ( 'NONE', #64390, #52978, #27931, .T. ) ;
#32839 = DIRECTION ( 'NONE',  ( 2.973811673103097665E-16, 0.000000000000000000, 1.000000000000000000 ) ) ;
#32840 = VECTOR ( 'NONE', #88351, 1000.000000000000000 ) ;
#32841 = CARTESIAN_POINT ( 'NONE',  ( 106.3019233867144351, -47.12668134090281313, 222.5184824187679453 ) ) ;
#32842 = CARTESIAN_POINT ( 'NONE',  ( 135.2096432771673733, -39.23067567606470618, 8.021372095560604265 ) ) ;
#32843 = EDGE_LOOP ( 'NONE', ( #86767, #45171 ) ) ;
#32844 = CARTESIAN_POINT ( 'NONE',  ( -10.70530292206537482, 89.20793846563920226, 118.0719063050892998 ) ) ;
#32845 = DIRECTION ( 'NONE',  ( 0.7071067811865473507, 0.7071067811865476838, 0.000000000000000000 ) ) ;
#32846 = CARTESIAN_POINT ( 'NONE',  ( 104.4076216956003407, -46.45794926476974496, 167.3648273245584051 ) ) ;
#32847 = CARTESIAN_POINT ( 'NONE',  ( 100.8629568432159260, -42.03472619363567730, 29.70809036959193250 ) ) ;
#32848 = CARTESIAN_POINT ( 'NONE',  ( 114.0008668920709738, -28.09234522576677762, 115.5261014663869474 ) ) ;
#32849 = CARTESIAN_POINT ( 'NONE',  ( 71.06670390244701707, -83.77844715994098124, 55.21780685541800437 ) ) ;
#32850 = EDGE_LOOP ( 'NONE', ( #88577, #71216, #2349, #33540 ) ) ;
#32851 = CIRCLE ( 'NONE', #87991, 17.00000000000090239 ) ;
#32852 = PLANE ( 'NONE',  #20470 ) ;
#32853 = CARTESIAN_POINT ( 'NONE',  ( 82.78382032693684778, -18.30343833343667015, 6.798133076500889160 ) ) ;
#32854 = ORIENTED_EDGE ( 'NONE', *, *, #39075, .T. ) ;
#32855 = VERTEX_POINT ( 'NONE', #41544 ) ;
#32856 = LINE ( 'NONE', #26496, #24164 ) ;
#32857 = ORIENTED_EDGE ( 'NONE', *, *, #61807, .F. ) ;
#32858 = VERTEX_POINT ( 'NONE', #8860 ) ;
#32859 = CARTESIAN_POINT ( 'NONE',  ( 125.9611475301391721, -14.72944715994100484, 239.5838068554164977 ) ) ;
#32860 = CARTESIAN_POINT ( 'NONE',  ( 102.2122376447956213, -29.66627497393060509, 49.97813411379098625 ) ) ;
#32861 = CARTESIAN_POINT ( 'NONE',  ( 109.6112504147204163, -26.56025234872169349, 199.8813395616249977 ) ) ;
#32862 = CARTESIAN_POINT ( 'NONE',  ( 103.0581626738561880, -26.45339789934162411, 170.3603871806729444 ) ) ;
#32864 = CARTESIAN_POINT ( 'NONE',  ( 96.71096103112840581, -32.93116260832598385, 17.03467289495896964 ) ) ;
#32863 = DIRECTION ( 'NONE',  ( -4.237773401492740281E-14, 1.000000000000000000, 0.000000000000000000 ) ) ;
#32865 = CARTESIAN_POINT ( 'NONE',  ( 183.5150000000000148, 14.63749999999999929, -52.38749999999999574 ) ) ;
#32866 = EDGE_CURVE ( 'NONE', #4156, #15222, #53597, .T. ) ;
#32867 = CARTESIAN_POINT ( 'NONE',  ( 119.5435152932140426, -31.57448135767196362, 293.1356252759106837 ) ) ;
#32868 = VERTEX_POINT ( 'NONE', #56527 ) ;
#32869 = ORIENTED_EDGE ( 'NONE', *, *, #84715, .F. ) ;
#32870 = VECTOR ( 'NONE', #53268, 1000.000000000000000 ) ;
#32871 = LINE ( 'NONE', #4288, #2380 ) ;
#32873 = CARTESIAN_POINT ( 'NONE',  ( 96.63812674735558517, -35.80421970836195555, 231.2556252759109725 ) ) ;
#32872 = VECTOR ( 'NONE', #57020, 1000.000000000000000 ) ;
#32874 = ORIENTED_EDGE ( 'NONE', *, *, #86587, .F. ) ;
#32875 =( GEOMETRIC_REPRESENTATION_CONTEXT ( 3 ) GLOBAL_UNCERTAINTY_ASSIGNED_CONTEXT ( ( #32666 ) ) GLOBAL_UNIT_ASSIGNED_CONTEXT ( ( #45438, #87257, #19543 ) ) REPRESENTATION_CONTEXT ( 'NONE', 'WORKASPACE' ) );
#32876 = CARTESIAN_POINT ( 'NONE',  ( 117.2277029493381377, -41.08016003417893103, 213.5165776568629781 ) ) ;
#32877 = CARTESIAN_POINT ( 'NONE',  ( 97.33784128341626740, -34.07106462853889894, 36.11479195067344250 ) ) ;
#32878 = CARTESIAN_POINT ( 'NONE',  ( -23.18606991449689403, 55.71041480586442418, 30.23275321802606186 ) ) ;
#32879 = AXIS2_PLACEMENT_3D ( 'NONE', #88930, #82135, #11268 ) ;
#32880 = CARTESIAN_POINT ( 'NONE',  ( 100.8870258581724357, -44.69987146937267397, 23.05224687894370206 ) ) ;
#32881 = DIRECTION ( 'NONE',  ( 1.000000000000000000, 0.000000000000000000, 0.000000000000000000 ) ) ;
#32883 = DIRECTION ( 'NONE',  ( -4.237773401492740281E-14, 1.000000000000000000, 0.000000000000000000 ) ) ;
#32882 = CARTESIAN_POINT ( 'NONE',  ( 103.1392712078617961, -29.55585189219027953, 277.6356252759111953 ) ) ;
#32884 = DIRECTION ( 'NONE',  ( 0.000000000000000000, 0.000000000000000000, -1.000000000000000000 ) ) ;
#32885 = PLANE ( 'NONE',  #51152 ) ;
#32886 = LINE ( 'NONE', #60585, #61447 ) ;
#32887 = EDGE_CURVE ( 'NONE', #64424, #66028, #46339, .T. ) ;
#32888 = CARTESIAN_POINT ( 'NONE',  ( 115.5439452383991892, -99.96145986183427112, -19.78219314458215550 ) ) ;
#32889 = EDGE_CURVE ( 'NONE', #89539, #20262, #675, .T. ) ;
#32890 = DIRECTION ( 'NONE',  ( 0.000000000000000000, 0.000000000000000000, 1.000000000000000000 ) ) ;
#32891 = CARTESIAN_POINT ( 'NONE',  ( 103.3797721312301547, -105.8297479413482876, -19.78219314458196010 ) ) ;
#32893 = EDGE_LOOP ( 'NONE', ( #9783, #67208, #54434, #79804 ) ) ;
#32892 = CARTESIAN_POINT ( 'NONE',  ( -3.292096649336115011, 94.82294024675948663, -118.5109520256350208 ) ) ;
#32894 = DIRECTION ( 'NONE',  ( 1.000000000000000000, 1.000000000000000078E-15, 0.000000000000000000 ) ) ;
#32895 = CARTESIAN_POINT ( 'NONE',  ( 117.4964429983690337, -36.12752982774328103, 228.8727681330539667 ) ) ;
#32896 = CARTESIAN_POINT ( 'NONE',  ( 117.2094703596446550, -39.28701360234872197, 119.6299109901969615 ) ) ;
#32897 = CARTESIAN_POINT ( 'NONE',  ( 99.34942397265413661, -29.65555323683921074, 271.7356252759109907 ) ) ;
#32898 = LINE ( 'NONE', #81532, #31500 ) ;
#32899 = DIRECTION ( 'NONE',  ( 0.9659258262890688673, 0.000000000000000000, -0.2588190451025189631 ) ) ;
#32900 = AXIS2_PLACEMENT_3D ( 'NONE', #79930, #38560, #38126 ) ;
#32902 = CARTESIAN_POINT ( 'NONE',  ( 71.25416588882602298, -72.55705569728901594, 542.9756252759101471 ) ) ;
#32901 = DIRECTION ( 'NONE',  ( -3.999999999999999995E-14, 1.000000000000000000, -4.100000000000000342E-29 ) ) ;
#32903 = DIRECTION ( 'NONE',  ( -1.000000000000000000, 0.000000000000000000, 0.000000000000000000 ) ) ;
#32904 = CARTESIAN_POINT ( 'NONE',  ( 133.8780722764207098, -21.47944715994101017, 1.625625275910997036 ) ) ;
#32905 = VERTEX_POINT ( 'NONE', #62896 ) ;
#32906 = VERTEX_POINT ( 'NONE', #83814 ) ;
#32907 = APPLICATION_CONTEXT ( 'automotive_design' ) ;
#32908 = CARTESIAN_POINT ( 'NONE',  ( 115.3871705984363984, -41.73312485046139386, 127.8181341137909470 ) ) ;
#32910 = ORIENTED_EDGE ( 'NONE', *, *, #15660, .T. ) ;
#32909 = CARTESIAN_POINT ( 'NONE',  ( 116.3212776292296127, -32.94146857471318413, 287.6356252759109680 ) ) ;
#32911 = CARTESIAN_POINT ( 'NONE',  ( -47.02966122971773899, 65.60000000000000853, 66.31971987082251019 ) ) ;
#32912 = CARTESIAN_POINT ( 'NONE',  ( 102.6254653968536417, -46.82603978519634325, 128.2346728949589760 ) ) ;
#32913 = FACE_OUTER_BOUND ( 'NONE', #38760, .T. ) ;
#32914 = DIRECTION ( 'NONE',  ( -0.7071067811865171526, -0.7071067811865779928, -7.071067811865164719E-16 ) ) ;
#32915 = CARTESIAN_POINT ( 'NONE',  ( -76.20754074253656540, 75.15251084995277608, 90.81844170390348836 ) ) ;
#32916 = CARTESIAN_POINT ( 'NONE',  ( 107.9678037105606023, -87.30234574837452044, -11.78219314458253741 ) ) ;
#32917 = CARTESIAN_POINT ( 'NONE',  ( 97.55373691267104164, -39.00345059616621768, 56.51276813305494784 ) ) ;
#32918 = ORIENTED_EDGE ( 'NONE', *, *, #77339, .T. ) ;
#32919 = VERTEX_POINT ( 'NONE', #21588 ) ;
#32921 = ORIENTED_EDGE ( 'NONE', *, *, #59603, .F. ) ;
#32920 = VECTOR ( 'NONE', #9018, 1000.000000000000114 ) ;
#32922 = CARTESIAN_POINT ( 'NONE',  ( 89.24325807922211595, -56.55267046464445002, 14.92562527591095289 ) ) ;
#32924 = DIRECTION ( 'NONE',  ( 0.5773502691896201799, 0.5773502691896286176, 0.5773502691896283956 ) ) ;
#32923 = CARTESIAN_POINT ( 'NONE',  ( 116.4077482568849007, -39.73851878533132975, 154.5784824187679476 ) ) ;
#32925 = FACE_OUTER_BOUND ( 'NONE', #29208, .T. ) ;
#32927 = EDGE_CURVE ( 'NONE', #41091, #21703, #84273, .T. ) ;
#32926 = DIRECTION ( 'NONE',  ( 1.000000000000000000, 1.000000000000000078E-15, 0.000000000000000000 ) ) ;
#32928 = DIRECTION ( 'NONE',  ( 0.000000000000000000, 0.000000000000000000, 1.000000000000000000 ) ) ;
#32929 = LINE ( 'NONE', #13398, #65147 ) ;
#32930 = CARTESIAN_POINT ( 'NONE',  ( 117.0608155050156256, -38.08101054489313242, 179.7189142246099891 ) ) ;
#32931 = CARTESIAN_POINT ( 'NONE',  ( 96.67837842349533162, -37.29153504031420141, 76.36991099019697060 ) ) ;
#32932 = ORIENTED_EDGE ( 'NONE', *, *, #3191, .T. ) ;
#32933 = ORIENTED_EDGE ( 'NONE', *, *, #68368, .T. ) ;
#32934 = DIRECTION ( 'NONE',  ( 0.000000000000000000, 0.000000000000000000, -1.000000000000000000 ) ) ;
#32935 = VECTOR ( 'NONE', #72021, 1000.000000000000000 ) ;
#32936 = DIRECTION ( 'NONE',  ( -1.000000000000000000, 0.000000000000000000, 0.000000000000000000 ) ) ;
#32937 = LINE ( 'NONE', #60185, #55407 ) ;
#32938 = CARTESIAN_POINT ( 'NONE',  ( 108.0149359080884324, -45.33189881898218232, 155.4699951314959776 ) ) ;
#32939 = VECTOR ( 'NONE', #57250, 1000.000000000000000 ) ;
#32941 = EDGE_CURVE ( 'NONE', #76097, #27698, #17330, .T. ) ;
#32940 = CIRCLE ( 'NONE', #25754, 2.550000000000006040 ) ;
#32942 = CIRCLE ( 'NONE', #67770, 2.517500000000005844 ) ;
#32943 = LINE ( 'NONE', #19330, #61992 ) ;
#32944 = EDGE_LOOP ( 'NONE', ( #36637, #72476 ) ) ;
#32945 = ORIENTED_EDGE ( 'NONE', *, *, #41855, .F. ) ;
#32946 = EDGE_CURVE ( 'NONE', #14773, #32309, #37887, .T. ) ;
#32947 = DIRECTION ( 'NONE',  ( 1.000000000000000000, 4.163336342344333240E-14, 0.000000000000000000 ) ) ;
#32948 = ORIENTED_EDGE ( 'NONE', *, *, #77471, .F. ) ;
#32949 = PRODUCT_DEFINITION_SHAPE ( 'NONE', 'NONE',  #89942 ) ;
#32950 = VERTEX_POINT ( 'NONE', #86936 ) ;
#32951 = CARTESIAN_POINT ( 'NONE',  ( 77.43081253121032148, -19.51428458727107440, 6.911392308671570284 ) ) ;
#32952 = EDGE_CURVE ( 'NONE', #15112, #7607, #5791, .T. ) ;
#32953 = CARTESIAN_POINT ( 'NONE',  ( 115.7036244402283529, -40.42759782077664710, 209.9482499725639855 ) ) ;
#32954 = VECTOR ( 'NONE', #9427, 1000.000000000000000 ) ;
#32955 = EDGE_CURVE ( 'NONE', #78242, #59655, #51927, .T. ) ;
#32956 = CARTESIAN_POINT ( 'NONE',  ( 177.0371591254545365, -48.62818131005479927, 193.9678068554150059 ) ) ;
#32957 = AXIS2_PLACEMENT_3D ( 'NONE', #10697, #32475, #24346 ) ;
#32958 = AXIS2_PLACEMENT_3D ( 'NONE', #38899, #3494, #18457 ) ;
#32959 = DIRECTION ( 'NONE',  ( 1.000000000000000000, 3.999999999999999995E-14, 1.000000000000000078E-15 ) ) ;
#32960 = EDGE_CURVE ( 'NONE', #72800, #87961, #65586, .T. ) ;
#32961 = CARTESIAN_POINT ( 'NONE',  ( -110.2127075062171997, 61.58157470217958007, 69.98598948281733101 ) ) ;
#32962 = VERTEX_POINT ( 'NONE', #44233 ) ;
#32963 = ORIENTED_EDGE ( 'NONE', *, *, #59277, .F. ) ;
#32964 = AXIS2_PLACEMENT_3D ( 'NONE', #89149, #75521, #88267 ) ;
#32965 = EDGE_LOOP ( 'NONE', ( #57150, #50687, #29406, #73940 ) ) ;
#32966 = EDGE_LOOP ( 'NONE', ( #56645, #73388, #49545, #13028 ) ) ;
#32967 = EDGE_CURVE ( 'NONE', #56235, #71705, #29740, .T. ) ;
#32968 = CARTESIAN_POINT ( 'NONE',  ( 113.9479352111735295, -42.95371825284467349, 231.0595189410199453 ) ) ;
#32969 = CARTESIAN_POINT ( 'NONE',  ( 113.3280054804099137, -28.32220607287434078, 104.5670538473399347 ) ) ;
#32970 = CARTESIAN_POINT ( 'NONE',  ( 115.1498815335951491, -43.27828968249936992, 88.28419670448195689 ) ) ;
#32971 = CARTESIAN_POINT ( 'NONE',  ( 106.8071438116306382, -44.97946765276041958, 249.5838068554170093 ) ) ;
#32972 = CARTESIAN_POINT ( 'NONE',  ( 133.4132809338111940, -16.05633243510671804, 8.161687850939825850 ) ) ;
#32973 = CARTESIAN_POINT ( 'NONE',  ( 107.6934652253138722, -25.28725624216507484, 321.0207719853553385 ) ) ;
#32974 = CARTESIAN_POINT ( 'NONE',  ( 97.76247233159546113, -41.51031662465626937, 192.7041967044819728 ) ) ;
#32975 = EDGE_CURVE ( 'NONE', #6171, #61270, #56536, .T. ) ;
#32976 = CARTESIAN_POINT ( 'NONE',  ( 59.68306514483415270, -72.55903866283681225, 396.9756252759102040 ) ) ;
#32977 = ORIENTED_EDGE ( 'NONE', *, *, #43324, .T. ) ;
#32978 = LINE ( 'NONE', #32079, #45235 ) ;
#32979 = EDGE_LOOP ( 'NONE', ( #87957, #2386, #31134, #20284 ) ) ;
#32980 = VERTEX_POINT ( 'NONE', #78354 ) ;
#32981 = CARTESIAN_POINT ( 'NONE',  ( 161.4809174648183330, -48.32844715993547879, 300.4678068554149490 ) ) ;
#32982 = VERTEX_POINT ( 'NONE', #23391 ) ;
#32983 = CARTESIAN_POINT ( 'NONE',  ( 97.81170238817014706, -40.51743819009087844, 137.6355114220584994 ) ) ;
#32984 = CARTESIAN_POINT ( 'NONE',  ( 115.0863374808427011, -30.61430893546196330, 90.34429048859003331 ) ) ;
#32985 = CARTESIAN_POINT ( 'NONE',  ( 109.2550203967672928, -46.95863148777297624, 107.7441967044829880 ) ) ;
#32986 = CARTESIAN_POINT ( 'NONE',  ( -11.71543264365797477, 77.64706452475591902, 130.0292962180824929 ) ) ;
#32987 = DIRECTION ( 'NONE',  ( 0.000000000000000000, 0.000000000000000000, 1.000000000000000000 ) ) ;
#32988 = DIRECTION ( 'NONE',  ( 0.000000000000000000, 0.000000000000000000, 1.000000000000000000 ) ) ;
#32991 = CARTESIAN_POINT ( 'NONE',  ( 110.6887065042382545, -47.98678726807230532, 203.8241967044819489 ) ) ;
#32990 = DIRECTION ( 'NONE',  ( -0.9254794337955620787, -0.3787978585227822492, 0.000000000000000000 ) ) ;
#32989 = CARTESIAN_POINT ( 'NONE',  ( 116.3135867418571650, -32.94878190598771539, 189.1356252759109680 ) ) ;
#32992 = CARTESIAN_POINT ( 'NONE',  ( 46.48091746482041486, -48.32844715994088602, 180.4678068554150911 ) ) ;
#32993 = LINE ( 'NONE', #54307, #4681 ) ;
#32994 = EDGE_LOOP ( 'NONE', ( #37750, #66824, #61543, #24136 ) ) ;
#32995 = CARTESIAN_POINT ( 'NONE',  ( 182.5667039024476708, -33.35206098992057377, 313.9678068554149490 ) ) ;
#32996 = EDGE_CURVE ( 'NONE', #41877, #32414, #52108, .T. ) ;
#32997 = DIRECTION ( 'NONE',  ( 0.7071067811865474617, -0.000000000000000000, 0.7071067811865474617 ) ) ;
#32998 = EDGE_CURVE ( 'NONE', #53561, #56608, #78795, .T. ) ;
#32999 = CARTESIAN_POINT ( 'NONE',  ( 97.39155240945729020, -39.27951294533326632, 136.5318526297954520 ) ) ;
#33000 = EDGE_CURVE ( 'NONE', #40888, #70942, #16999, .T. ) ;
#33001 = FACE_OUTER_BOUND ( 'NONE', #39349, .T. ) ;
#33003 = EDGE_LOOP ( 'NONE', ( #72303, #18661, #4641, #55285 ) ) ;
#33002 = CARTESIAN_POINT ( 'NONE',  ( 110.7486471836621860, -26.25784018214204707, 254.8194347997204545 ) ) ;
#33004 = CARTESIAN_POINT ( 'NONE',  ( 114.2795876152497243, -29.76195770723571954, 194.4373016625220032 ) ) ;
#33005 = CARTESIAN_POINT ( 'NONE',  ( 100.1631548973110739, -45.39139052332982516, 268.0289586092443415 ) ) ;
#33006 = CARTESIAN_POINT ( 'NONE',  ( 117.6520138419322734, -33.39117794972031561, 125.0575300378149706 ) ) ;
#33007 = ADVANCED_FACE ( 'NONE', ( #11060 ), #30180, .T. ) ;
#33008 = AXIS2_PLACEMENT_3D ( 'NONE', #20932, #13227, #48604 ) ;
#33009 = LINE ( 'NONE', #18941, #14291 ) ;
#33010 = CARTESIAN_POINT ( 'NONE',  ( 11.57415360872102994, 87.79424630570801469, -130.0420457590603860 ) ) ;
#33012 = DIRECTION ( 'NONE',  ( 3.386875084296745512E-15, 0.000000000000000000, -1.000000000000000000 ) ) ;
#33011 = CARTESIAN_POINT ( 'NONE',  ( 134.0664832912739826, -9.029447159941003775, 1.625625275910997480 ) ) ;
#33013 = CARTESIAN_POINT ( 'NONE',  ( 105.7995185409999692, -26.72403495984207922, 190.1772919383297449 ) ) ;
#33014 = DIRECTION ( 'NONE',  ( -0.000000000000000000, -0.000000000000000000, 1.000000000000000000 ) ) ;
#33015 = EDGE_LOOP ( 'NONE', ( #38486, #28493, #34999, #76310 ) ) ;
#33016 = AXIS2_PLACEMENT_3D ( 'NONE', #40391, #12704, #88117 ) ;
#33017 = VECTOR ( 'NONE', #21085, 1000.000000000000000 ) ;
#33018 = EDGE_LOOP ( 'NONE', ( #3092, #35890 ) ) ;
#33019 = ORIENTED_EDGE ( 'NONE', *, *, #68253, .F. ) ;
#33020 = AXIS2_PLACEMENT_3D ( 'NONE', #62991, #772, #28470 ) ;
#33021 = ORIENTED_EDGE ( 'NONE', *, *, #22868, .T. ) ;
#33022 = CARTESIAN_POINT ( 'NONE',  ( 0.000000000000000000, 101.5999999999999943, -98.14560000000000173 ) ) ;
#33023 = CARTESIAN_POINT ( 'NONE',  ( 111.0379167980822928, -47.01981040405694756, 13.85753003781498016 ) ) ;
#33024 = LINE ( 'NONE', #47083, #67252 ) ;
#33025 = AXIS2_PLACEMENT_3D ( 'NONE', #41238, #35325, #20380 ) ;
#33026 = CARTESIAN_POINT ( 'NONE',  ( 145.2153822645345826, -139.0823765015731794, 246.7463595109249184 ) ) ;
#33027 = VECTOR ( 'NONE', #86030, 1000.000000000000000 ) ;
#33029 = CARTESIAN_POINT ( 'NONE',  ( 137.8167039024479834, -50.82844715994100682, 250.9178068554160461 ) ) ;
#33028 = LINE ( 'NONE', #66192, #67076 ) ;
#33030 = VECTOR ( 'NONE', #83388, 1000.000000000000000 ) ;
#33031 = CARTESIAN_POINT ( 'NONE',  ( 114.8821461825539245, -40.17495804977037466, 252.9181341137911545 ) ) ;
#33032 = EDGE_LOOP ( 'NONE', ( #61980, #51360, #56878, #77562 ) ) ;
#33033 = ORIENTED_EDGE ( 'NONE', *, *, #52911, .F. ) ;
#33034 = ORIENTED_EDGE ( 'NONE', *, *, #24695, .F. ) ;
#33035 = AXIS2_PLACEMENT_3D ( 'NONE', #6892, #8246, #49554 ) ;
#33036 = LINE ( 'NONE', #60729, #2170 ) ;
#33037 = DIRECTION ( 'NONE',  ( -0.7071067811866279529, 0.7071067811864671926, -7.071067811866286874E-16 ) ) ;
#33038 = DIRECTION ( 'NONE',  ( -0.9825752044165969590, -0.1858654558159821002, 0.000000000000000000 ) ) ;
#33039 = CARTESIAN_POINT ( 'NONE',  ( -47.02966122971776031, 65.60000000000000853, 108.8289304395572401 ) ) ;
#33040 = CARTESIAN_POINT ( 'NONE',  ( 115.0635112019030686, -32.91162553226137533, 15.61301187732594364 ) ) ;
#33041 = DIRECTION ( 'NONE',  ( 1.000000000000000000, 0.000000000000000000, 0.000000000000000000 ) ) ;
#33042 = DIRECTION ( 'NONE',  ( 1.067522139062650671E-15, 1.000000000000000000, 0.000000000000000000 ) ) ;
#33043 = CARTESIAN_POINT ( 'NONE',  ( 97.18779033502694631, -39.88384928074078317, 281.5603871806734446 ) ) ;
#33044 = LINE ( 'NONE', #59396, #38519 ) ;
#33045 = ORIENTED_EDGE ( 'NONE', *, *, #15375, .T. ) ;
#33046 = FACE_OUTER_BOUND ( 'NONE', #11332, .T. ) ;
#33047 = CARTESIAN_POINT ( 'NONE',  ( 204.2160000000000082, 52.73749999999999716, -44.45000000000000284 ) ) ;
#33048 = CARTESIAN_POINT ( 'NONE',  ( 109.6546009468767693, -44.98793201169110034, 50.62428084578196774 ) ) ;
#33049 = VECTOR ( 'NONE', #7734, 1000.000000000000000 ) ;
#33050 = EDGE_CURVE ( 'NONE', #48266, #82635, #44682, .T. ) ;
#33051 = DIRECTION ( 'NONE',  ( -0.7071067811865437980, 0.000000000000000000, -0.7071067811865512365 ) ) ;
#33052 = DIRECTION ( 'NONE',  ( 0.000000000000000000, 0.000000000000000000, -1.000000000000000000 ) ) ;
#33053 = DIRECTION ( 'NONE',  ( 0.000000000000000000, 0.000000000000000000, 1.000000000000000000 ) ) ;
#33054 = ORIENTED_EDGE ( 'NONE', *, *, #70835, .T. ) ;
#33055 = DIRECTION ( 'NONE',  ( -4.237773401492740281E-14, 1.000000000000000000, 0.000000000000000000 ) ) ;
#33056 = ADVANCED_FACE ( 'NONE', ( #24258 ), #64260, .T. ) ;
#33057 = CARTESIAN_POINT ( 'NONE',  ( 124.8316159268321712, 57.68278277478432159, -38.23569996530863335 ) ) ;
#33058 = ORIENTED_EDGE ( 'NONE', *, *, #50811, .F. ) ;
#33059 = CARTESIAN_POINT ( 'NONE',  ( 109.5085389712880612, -46.86470218963918200, 132.7641967044819751 ) ) ;
#33060 = ORIENTED_EDGE ( 'NONE', *, *, #7369, .F. ) ;
#33061 = CARTESIAN_POINT ( 'NONE',  ( 105.1764056618614944, -45.05913732685939976, 71.82099125664798578 ) ) ;
#33062 = ADVANCED_FACE ( 'NONE', ( #50612, #16115 ), #30624, .T. ) ;
#33063 = DIRECTION ( 'NONE',  ( 0.7071067811868710917, -0.7071067811862240537, 0.000000000000000000 ) ) ;
#33064 = CARTESIAN_POINT ( 'NONE',  ( 99.30241108408027628, -32.39570601076609080, 107.3530118773259545 ) ) ;
#33065 = ADVANCED_FACE ( 'NONE', ( #72415 ), #71531, .F. ) ;
#33066 = CARTESIAN_POINT ( 'NONE',  ( 177.0664832912730162, 12.92155284005730387, 355.9756252759109998 ) ) ;
#33067 = VECTOR ( 'NONE', #40913, 1000.000000000000000 ) ;
#33068 = CARTESIAN_POINT ( 'NONE',  ( 1.154229608196380665E-15, 152.3879256507328250, 9.425000000000000711 ) ) ;
#33069 = CARTESIAN_POINT ( 'NONE',  ( 114.3683386633632324, -44.20073667237542026, 69.19276813305397411 ) ) ;
#33071 = ADVANCED_FACE ( 'NONE', ( #38320 ), #66018, .T. ) ;
#33070 = CARTESIAN_POINT ( 'NONE',  ( 117.0667039024470313, -104.2784471599408960, 17.71780685541799016 ) ) ;
#33072 = DIRECTION ( 'NONE',  ( 0.000000000000000000, 0.000000000000000000, 1.000000000000000000 ) ) ;
#33073 = VECTOR ( 'NONE', #36507, 1000.000000000000000 ) ;
#33074 = ORIENTED_EDGE ( 'NONE', *, *, #13978, .T. ) ;
#33075 = VECTOR ( 'NONE', #34456, 1000.000000000000000 ) ;
#33076 = CARTESIAN_POINT ( 'NONE',  ( -118.5469577077833065, 69.93366089391888352, -1.674277437722204720 ) ) ;
#33077 = ORIENTED_EDGE ( 'NONE', *, *, #83155, .F. ) ;
#33078 = ORIENTED_EDGE ( 'NONE', *, *, #44757, .T. ) ;
#33079 = EDGE_CURVE ( 'NONE', #31182, #23292, #5607, .T. ) ;
#33080 = VECTOR ( 'NONE', #13299, 1000.000000000000000 ) ;
#33081 = DIRECTION ( 'NONE',  ( -0.9999999999998281375, 0.000000000000000000, 5.861124988064729938E-07 ) ) ;
#33082 = EDGE_LOOP ( 'NONE', ( #71146, #80394, #86699, #15282, #80602, #13639, #48047, #25771, #40688, #11045, #37509, #72174 ) ) ;
#33083 = CARTESIAN_POINT ( 'NONE',  ( 112.1541913332956710, -45.76570811864968391, 257.9965776568639626 ) ) ;
#33084 = CARTESIAN_POINT ( 'NONE',  ( 97.72691728231733066, -42.68408598780226271, 137.7661014663869992 ) ) ;
#33085 = CARTESIAN_POINT ( 'NONE',  ( 19.56648329127303043, -81.37844715994266664, 342.9256252759109884 ) ) ;
#33086 = CARTESIAN_POINT ( 'NONE',  ( 117.0603735531381346, -38.08412411259971009, 129.7186663005400078 ) ) ;
#33087 = CARTESIAN_POINT ( 'NONE',  ( 111.0825168487035626, -25.58018305758348632, 95.80133956162495679 ) ) ;
#33088 = ADVANCED_FACE ( 'NONE', ( #46458 ), #61436, .F. ) ;
#33089 = CARTESIAN_POINT ( 'NONE',  ( 192.5667039024472444, -23.42844715993414084, 300.4678068554149490 ) ) ;
#33090 = ORIENTED_EDGE ( 'NONE', *, *, #85425, .T. ) ;
#33091 = CIRCLE ( 'NONE', #72268, 15.69999999999999574 ) ;
#33092 = CARTESIAN_POINT ( 'NONE',  ( 156.5667039024485803, -48.82844715993568485, 139.7178068554149775 ) ) ;
#33093 = AXIS2_PLACEMENT_3D ( 'NONE', #15868, #2238, #29945 ) ;
#33094 = AXIS2_PLACEMENT_3D ( 'NONE', #52630, #80392, #11330 ) ;
#33095 = DIRECTION ( 'NONE',  ( -0.7071067811865279218, 0.7071067811865670016, -6.612322855859973915E-17 ) ) ;
#33096 = ORIENTED_EDGE ( 'NONE', *, *, #46486, .T. ) ;
#33097 = DIRECTION ( 'NONE',  ( 5.512527431108029424E-15, -1.000000000000000000, 0.000000000000000000 ) ) ;
#33098 = DIRECTION ( 'NONE',  ( 0.000000000000000000, 1.000000000000000000, 0.000000000000000000 ) ) ;
#33099 = CARTESIAN_POINT ( 'NONE',  ( 116.1995025514324169, -41.78438384397603045, 263.4241967044824833 ) ) ;
#33100 = CARTESIAN_POINT ( 'NONE',  ( 107.0664832912739399, -36.72944715994096754, 300.2406250056037038 ) ) ;
#33101 = CARTESIAN_POINT ( 'NONE',  ( 182.5667039024480118, -32.29483332968450782, 342.9256252759119548 ) ) ;
#33102 = CARTESIAN_POINT ( 'NONE',  ( 79.41328093381464726, -39.40256188477533073, 1.689562700881423130 ) ) ;
#33103 = CARTESIAN_POINT ( 'NONE',  ( 111.6523633261645188, -43.93540552976629243, 262.4495626852196892 ) ) ;
#33105 = CARTESIAN_POINT ( 'NONE',  ( 107.2318599658364207, -25.70055450771780059, 76.07657765686298035 ) ) ;
#33104 = DIRECTION ( 'NONE',  ( 2.900000000000000265E-14, -2.000000000000000155E-15, 1.000000000000000000 ) ) ;
#33106 = LINE ( 'NONE', #62600, #146 ) ;
#33107 = CARTESIAN_POINT ( 'NONE',  ( 118.9678564412739092, -36.92894532057803758, 153.8127681330539644 ) ) ;
#33108 = ORIENTED_EDGE ( 'NONE', *, *, #11254, .T. ) ;
#33109 = DIRECTION ( 'NONE',  ( -0.7071067812163274180, 0.7071067811567677275, -6.612322856138636565E-17 ) ) ;
#33110 = ORIENTED_EDGE ( 'NONE', *, *, #61350, .F. ) ;
#33111 = VECTOR ( 'NONE', #81270, 1000.000000000000000 ) ;
#33112 = FACE_OUTER_BOUND ( 'NONE', #43153, .T. ) ;
#33113 = DIRECTION ( 'NONE',  ( 0.000000000000000000, -1.000000000000000000, 0.000000000000000000 ) ) ;
#33114 = CARTESIAN_POINT ( 'NONE',  ( 131.3179999999999836, 53.97500000000000142, 30.16249999999999787 ) ) ;
#33115 = ORIENTED_EDGE ( 'NONE', *, *, #88125, .T. ) ;
#33116 = EDGE_CURVE ( 'NONE', #48698, #77063, #28942, .T. ) ;
#33117 = CARTESIAN_POINT ( 'NONE',  ( 112.1419149229391650, -28.01429753427307290, 60.65653136556989722 ) ) ;
#33119 = ORIENTED_EDGE ( 'NONE', *, *, #84511, .T. ) ;
#33118 = CARTESIAN_POINT ( 'NONE',  ( 97.75494523667518365, -42.77206137223026161, 146.7965776568629508 ) ) ;
#33120 = DIRECTION ( 'NONE',  ( 0.000000000000000000, -1.000000000000000000, 0.000000000000000000 ) ) ;
#33121 = ADVANCED_FACE ( 'NONE', ( #75082 ), #87823, .T. ) ;
#33122 = CARTESIAN_POINT ( 'NONE',  ( -130.5540562089606738, 95.23006786499111342, -0.8254869398575555017 ) ) ;
#33123 = VECTOR ( 'NONE', #68153, 1000.000000000000114 ) ;
#33124 = CARTESIAN_POINT ( 'NONE',  ( 97.81170255947417047, -40.51743869465033754, 117.6354096206635518 ) ) ;
#33125 = CIRCLE ( 'NONE', #34544, 8.999999999999994671 ) ;
#33126 = CARTESIAN_POINT ( 'NONE',  ( 100.8874678944084593, -44.70022138268650735, 77.05229194355962363 ) ) ;
#33127 = EDGE_LOOP ( 'NONE', ( #87776, #40819, #54455, #73643 ) ) ;
#33128 =( NAMED_UNIT ( * ) PLANE_ANGLE_UNIT ( ) SI_UNIT ( $, .RADIAN. ) );
#33129 = PLANE ( 'NONE',  #35586 ) ;
#33130 = PLANE ( 'NONE',  #63080 ) ;
#33131 = VERTEX_POINT ( 'NONE', #60539 ) ;
#33132 = ORIENTED_EDGE ( 'NONE', *, *, #27978, .T. ) ;
#33133 = DIRECTION ( 'NONE',  ( 1.000000000000000000, 0.000000000000000000, 0.000000000000000000 ) ) ;
#33134 = CARTESIAN_POINT ( 'NONE',  ( 95.94886839522645516, 94.12569442554141119, -88.53717826876584240 ) ) ;
#33135 = CARTESIAN_POINT ( 'NONE',  ( 49.35211078756547209, -35.65087443492560482, 342.9256252759109884 ) ) ;
#33136 = DIRECTION ( 'NONE',  ( -1.000000000000000000, -2.999999999999999839E-15, -1.000000000000000078E-15 ) ) ;
#33137 = AXIS2_PLACEMENT_3D ( 'NONE', #30660, #37920, #57912 ) ;
#33139 = CARTESIAN_POINT ( 'NONE',  ( -6.720192613126054759, 71.76561204655834558, -118.3658933525135524 ) ) ;
#33138 = CARTESIAN_POINT ( 'NONE',  ( 31.56670390244800828, -32.29483332968611364, -5.074374724088000832 ) ) ;
#33140 = CARTESIAN_POINT ( 'NONE',  ( 31.56670390244679325, -32.29483332968652576, 117.4678068554150485 ) ) ;
#33141 = AXIS2_PLACEMENT_3D ( 'NONE', #10031, #37738, #65436 ) ;
#33143 = ORIENTED_EDGE ( 'NONE', *, *, #31708, .F. ) ;
#33142 = AXIS2_PLACEMENT_3D ( 'NONE', #3254, #50486, #78232 ) ;
#33144 = LINE ( 'NONE', #20862, #53532 ) ;
#33145 = CARTESIAN_POINT ( 'NONE',  ( 97.99937763885738207, -40.39701179870334613, 202.6327681330529629 ) ) ;
#33147 = ORIENTED_EDGE ( 'NONE', *, *, #53773, .T. ) ;
#33146 = FACE_BOUND ( 'NONE', #47919, .T. ) ;
#33148 = AXIS2_PLACEMENT_3D ( 'NONE', #51055, #77887, #78351 ) ;
#33149 = CARTESIAN_POINT ( 'NONE',  ( 116.1466984671187248, -33.09446055034466383, 50.12991099019598096 ) ) ;
#33150 = CARTESIAN_POINT ( 'NONE',  ( 107.0664832912739399, -36.72944715994095333, 311.3356252759109566 ) ) ;
#33151 = CYLINDRICAL_SURFACE ( 'NONE', #80505, 0.2500000000000002220 ) ;
#33152 = AXIS2_PLACEMENT_3D ( 'NONE', #88367, #89708, #27018 ) ;
#33153 = CARTESIAN_POINT ( 'NONE',  ( 194.0371591254575208, -24.89890238294407254, 180.4678068554150343 ) ) ;
#33154 = ORIENTED_EDGE ( 'NONE', *, *, #14429, .F. ) ;
#33155 = DIRECTION ( 'NONE',  ( -3.100000000000000258E-29, 3.100000000000000044E-14, 1.000000000000000000 ) ) ;
#33156 = AXIS2_PLACEMENT_3D ( 'NONE', #49068, #14585, #42261 ) ;
#33157 = ORIENTED_EDGE ( 'NONE', *, *, #3738, .T. ) ;
#33158 = EDGE_LOOP ( 'NONE', ( #13523, #61738, #82822, #72805 ) ) ;
#33159 = EDGE_CURVE ( 'NONE', #53213, #75348, #36198, .T. ) ;
#33160 = CARTESIAN_POINT ( 'NONE',  ( 98.65401097786960349, -39.51487139837627893, 238.0130118773259653 ) ) ;
#33161 = CARTESIAN_POINT ( 'NONE',  ( -3.174999999999644995, 8.255000000000000782, 33.98325472291465132 ) ) ;
#33162 = DIRECTION ( 'NONE',  ( 1.000000000000000000, 0.000000000000000000, 0.000000000000000000 ) ) ;
#33163 = EDGE_CURVE ( 'NONE', #19112, #66320, #18323, .T. ) ;
#33164 = EDGE_CURVE ( 'NONE', #61703, #26268, #86964, .T. ) ;
#33165 = CARTESIAN_POINT ( 'NONE',  ( 97.81169409577289287, -40.51741657705139232, 81.63570706759205109 ) ) ;
#33166 = VECTOR ( 'NONE', #10312, 1000.000000000000000 ) ;
#33167 = CARTESIAN_POINT ( 'NONE',  ( 97.81452210549078075, -40.51628237377364883, 52.63520911028864901 ) ) ;
#33168 = ORIENTED_EDGE ( 'NONE', *, *, #84781, .F. ) ;
#33169 = CARTESIAN_POINT ( 'NONE',  ( 179.4595971212720258, -26.00627455219131789, -5.074374724088000832 ) ) ;
#33170 = EDGE_CURVE ( 'NONE', #69198, #77789, #81029, .T. ) ;
#33171 = DIRECTION ( 'NONE',  ( 0.000000000000000000, 0.000000000000000000, -1.000000000000000000 ) ) ;
#33172 = ORIENTED_EDGE ( 'NONE', *, *, #33571, .T. ) ;
#33173 = CARTESIAN_POINT ( 'NONE',  ( 112.1975415602056216, -26.93795424888832812, 14.68038718067299442 ) ) ;
#33174 = ORIENTED_EDGE ( 'NONE', *, *, #80979, .F. ) ;
#33175 = ORIENTED_EDGE ( 'NONE', *, *, #39821, .F. ) ;
#33176 = CARTESIAN_POINT ( 'NONE',  ( 113.4754094548699186, -31.62960856676687982, 242.1795189410199782 ) ) ;
#33177 = ADVANCED_FACE ( 'NONE', ( #68278 ), #31951, .T. ) ;
#33178 = CARTESIAN_POINT ( 'NONE',  ( 98.51953950620406886, -30.85675296092858844, 165.8594347997209582 ) ) ;
#33179 = CARTESIAN_POINT ( 'NONE',  ( 23.68742839265041766, 81.00938505711215498, 307.4121377794205614 ) ) ;
#33180 = DIRECTION ( 'NONE',  ( -1.000000000000000000, 0.000000000000000000, 0.000000000000000000 ) ) ;
#33181 = DIRECTION ( 'NONE',  ( 0.000000000000000000, 0.000000000000000000, -1.000000000000000000 ) ) ;
#33182 = CARTESIAN_POINT ( 'NONE',  ( 8.588557746091451506, 73.17833598766388548, 130.2737784290322338 ) ) ;
#33183 = AXIS2_PLACEMENT_3D ( 'NONE', #16077, #78762, #37402 ) ;
#33184 = CARTESIAN_POINT ( 'NONE',  ( 99.50795136241276850, -29.43516104912357179, 246.7156252759109520 ) ) ;
#33185 = FACE_OUTER_BOUND ( 'NONE', #17010, .T. ) ;
#33186 = EDGE_CURVE ( 'NONE', #81111, #73627, #6059, .T. ) ;
#33187 = ORIENTED_EDGE ( 'NONE', *, *, #77502, .T. ) ;
#33188 = CARTESIAN_POINT ( 'NONE',  ( 112.5370353716610055, -27.80386372334747236, 90.63848241876793566 ) ) ;
#33189 = CARTESIAN_POINT ( 'NONE',  ( -544.5124999999999318, 53.97500000000000142, 88.90000000000000568 ) ) ;
#33190 = ORIENTED_EDGE ( 'NONE', *, *, #1720, .F. ) ;
#33191 = ORIENTED_EDGE ( 'NONE', *, *, #18536, .T. ) ;
#33192 = ORIENTED_EDGE ( 'NONE', *, *, #22466, .T. ) ;
#33193 = ADVANCED_FACE ( 'NONE', ( #89166 ), #40101, .T. ) ;
#33194 = DIRECTION ( 'NONE',  ( 4.194175870806139918E-14, -1.000000000000000000, 0.000000000000000000 ) ) ;
#33195 = FACE_OUTER_BOUND ( 'NONE', #14195, .T. ) ;
#33196 = CARTESIAN_POINT ( 'NONE',  ( 34.96670390244699433, -26.71338133339301635, 237.4678068554150059 ) ) ;
#33197 = CARTESIAN_POINT ( 'NONE',  ( 108.2592170473780300, -44.83253820548913637, 140.5109475124479559 ) ) ;
#33198 = CARTESIAN_POINT ( 'NONE',  ( 109.3416101119966442, -26.53331765884353644, 220.9013395616249795 ) ) ;
#33199 = EDGE_CURVE ( 'NONE', #35463, #77666, #33301, .T. ) ;
#33200 = DIRECTION ( 'NONE',  ( 1.000000000000000000, 3.999999999999999995E-14, 1.000000000000000078E-15 ) ) ;
#33201 = ORIENTED_EDGE ( 'NONE', *, *, #24700, .F. ) ;
#33202 = CARTESIAN_POINT ( 'NONE',  ( 130.0906791124284894, 88.91243380484084469, -11.02261862230788303 ) ) ;
#33203 = AXIS2_PLACEMENT_3D ( 'NONE', #38355, #66055, #3846 ) ;
#33204 = CARTESIAN_POINT ( 'NONE',  ( 136.6235172543038061, -37.74149216370406634, 2.839569540204782250 ) ) ;
#33205 = ORIENTED_EDGE ( 'NONE', *, *, #58850, .T. ) ;
#33206 = ORIENTED_EDGE ( 'NONE', *, *, #21518, .T. ) ;
#33207 = VECTOR ( 'NONE', #77077, 1000.000000000000000 ) ;
#33208 = VECTOR ( 'NONE', #23276, 1000.000000000000000 ) ;
#33209 = DIRECTION ( 'NONE',  ( -3.360405532702990443E-14, 1.000000000000000000, 0.000000000000000000 ) ) ;
#33210 = VERTEX_POINT ( 'NONE', #87378 ) ;
#33211 = ORIENTED_EDGE ( 'NONE', *, *, #11762, .F. ) ;
#33212 = DIRECTION ( 'NONE',  ( -4.299999999999999979E-14, 1.000000000000000000, 0.000000000000000000 ) ) ;
#33213 = CARTESIAN_POINT ( 'NONE',  ( 183.6524903400785433, -48.32844715993451956, 180.4678068554150343 ) ) ;
#33214 = PLANE ( 'NONE',  #84436 ) ;
#33215 = DIRECTION ( 'NONE',  ( 0.000000000000000000, 0.000000000000000000, 1.000000000000000000 ) ) ;
#33216 = CARTESIAN_POINT ( 'NONE',  ( 97.43556672503765981, -37.99919831760565359, 150.8524198280769895 ) ) ;
#33217 = CARTESIAN_POINT ( 'NONE',  ( 116.4271464750313498, -31.96187137292554681, 44.20133956162491984 ) ) ;
#33218 = PLANE ( 'NONE',  #52362 ) ;
#33219 = VERTEX_POINT ( 'NONE', #26935 ) ;
#33220 = VECTOR ( 'NONE', #29618, 1000.000000000000000 ) ;
#33221 = CARTESIAN_POINT ( 'NONE',  ( -92.12448541806607238, 79.66685870724428753, -74.62312585591620007 ) ) ;
#33222 = ORIENTED_EDGE ( 'NONE', *, *, #873, .T. ) ;
#33223 = AXIS2_PLACEMENT_3D ( 'NONE', #11492, #39187, #26461 ) ;
#33224 = LINE ( 'NONE', #87297, #15675 ) ;
#33225 = VERTEX_POINT ( 'NONE', #5148 ) ;
#33226 = CARTESIAN_POINT ( 'NONE',  ( 41.56648329127499153, -36.32844715994070839, 314.1756252759120116 ) ) ;
#33227 = CIRCLE ( 'NONE', #41888, 81.91591158490091118 ) ;
#33228 = CARTESIAN_POINT ( 'NONE',  ( -7.685739755354498826, 72.53188479423953083, 118.3085854593769568 ) ) ;
#33229 = EDGE_CURVE ( 'NONE', #7923, #71348, #54602, .T. ) ;
#33230 = CARTESIAN_POINT ( 'NONE',  ( 115.1270644249241997, -42.70333644879877255, 133.3187822923470378 ) ) ;
#33231 = CARTESIAN_POINT ( 'NONE',  ( 177.4809174648216299, -49.32844715993478246, 129.9678068554150059 ) ) ;
#33232 = ORIENTED_EDGE ( 'NONE', *, *, #54665, .T. ) ;
#33233 = CARTESIAN_POINT ( 'NONE',  ( 112.3383795496262820, -28.20708685789894687, 289.6356252759109680 ) ) ;
#33234 = CARTESIAN_POINT ( 'NONE',  ( 100.9155127638074703, -46.91653085812070856, 48.14419670448194211 ) ) ;
#33236 = DIRECTION ( 'NONE',  ( 0.000000000000000000, 1.000000000000000000, 0.000000000000000000 ) ) ;
#33235 = CARTESIAN_POINT ( 'NONE',  ( 97.81168839172025287, -40.51739946886939947, 131.6358419732753475 ) ) ;
#33237 = CARTESIAN_POINT ( 'NONE',  ( 116.3212776292299253, -32.94146857471393730, 145.1356252759109680 ) ) ;
#33238 = CARTESIAN_POINT ( 'NONE',  ( 107.0664832912730020, -27.87844715994269862, 361.9756252759109998 ) ) ;
#33239 = VECTOR ( 'NONE', #77691, 1000.000000000000000 ) ;
#33240 = B_SPLINE_CURVE_WITH_KNOTS ( 'NONE', 3,
 ( #43466, #36683, #57552, #85294, #48471, #76214, #41671, #62583, #7184, #34872, #358, #83483, #48927, #76670, #38013, #37572, #72541, #79369 ),
 .UNSPECIFIED., .F., .F.,
 ( 4, 2, 2, 2, 2, 2, 2, 2, 4 ),
 ( 0.5000000006881730741, 0.5625000006021514398, 0.6250000005161298056, 0.6875000004301081713, 0.7500000003440865370, 0.8125000002580649028, 0.8750000001720432685, 0.9375000000860216343, 1.000000000000000000 ),
 .UNSPECIFIED. ) ;
#33241 = CARTESIAN_POINT ( 'NONE',  ( 70.63919639214310564, 91.07499999999996021, 0.000000000000000000 ) ) ;
#33242 = CARTESIAN_POINT ( 'NONE',  ( 136.5167039024470341, -103.2284471599409272, 55.21780685541800437 ) ) ;
#33243 = ORIENTED_EDGE ( 'NONE', *, *, #244, .F. ) ;
#33244 = EDGE_CURVE ( 'NONE', #37103, #33131, #46004, .T. ) ;
#33245 = CARTESIAN_POINT ( 'NONE',  ( 97.76994516709639527, -29.29956314839395048, 45.78991099019697231 ) ) ;
#33246 = CARTESIAN_POINT ( 'NONE',  ( 96.05470400087912708, -37.92356717231275098, 77.40038718067299328 ) ) ;
#33248 = CARTESIAN_POINT ( 'NONE',  ( 2.323620343766204915E-14, 101.5999999999999943, -188.9759999999999991 ) ) ;
#33247 = CARTESIAN_POINT ( 'NONE',  ( 97.86672871672134022, -40.64958041416993240, 171.6472150801397163 ) ) ;
#33249 = CYLINDRICAL_SURFACE ( 'NONE', #50927, 0.5000000000000004441 ) ;
#33250 = VECTOR ( 'NONE', #22020, 1000.000000000000114 ) ;
#33251 = EDGE_CURVE ( 'NONE', #10387, #26370, #38762, .T. ) ;
#33252 = CARTESIAN_POINT ( 'NONE',  ( 145.7718159158550293, -125.9396293856170956, 247.4783998280190076 ) ) ;
#33253 = ORIENTED_EDGE ( 'NONE', *, *, #64704, .F. ) ;
#33254 = CARTESIAN_POINT ( 'NONE',  ( 116.3624975636023322, -33.68846805112529808, 85.07848241876692441 ) ) ;
#33256 = EDGE_LOOP ( 'NONE', ( #30421, #8095 ) ) ;
#33255 = LINE ( 'NONE', #88685, #25380 ) ;
#33257 = CARTESIAN_POINT ( 'NONE',  ( 98.05565822401628395, -44.38798742045805312, 222.8870538473399563 ) ) ;
#33258 = CARTESIAN_POINT ( 'NONE',  ( 104.4070333491352471, -46.45780296964726119, 253.3665111305816140 ) ) ;
#33259 = CYLINDRICAL_SURFACE ( 'NONE', #23222, 3.299999999999997158 ) ;
#33260 = DIRECTION ( 'NONE',  ( 0.7071067811865524577, 0.000000000000000000, -0.7071067811865425767 ) ) ;
#33261 = CARTESIAN_POINT ( 'NONE',  ( 104.4899544425265532, -26.97880758706315873, 46.28145860999622130 ) ) ;
#33262 = AXIS2_PLACEMENT_3D ( 'NONE', #77718, #14137, #35012 ) ;
#33263 = CARTESIAN_POINT ( 'NONE',  ( 73.06670390244801183, -48.82844715994099971, 250.9178068554160461 ) ) ;
#33264 = CARTESIAN_POINT ( 'NONE',  ( 41.56648329127399677, 0.2215528400590013880, 18.92562527591200094 ) ) ;
#33265 = CARTESIAN_POINT ( 'NONE',  ( 118.1851208724672233, -36.91582462397655462, 153.8127681330539644 ) ) ;
#33266 = ORIENTED_EDGE ( 'NONE', *, *, #59967, .T. ) ;
#33267 = EDGE_LOOP ( 'NONE', ( #37896, #15743, #32130, #31786, #9963 ) ) ;
#33268 = AXIS2_PLACEMENT_3D ( 'NONE', #62598, #33104, #88534 ) ;
#33269 = CARTESIAN_POINT ( 'NONE',  ( 107.8137748826309377, -27.36365403737595159, 111.4568214011349738 ) ) ;
#33270 = CIRCLE ( 'NONE', #50641, 0.5000000000000004441 ) ;
#33271 = DIRECTION ( 'NONE',  ( -0.9999999853157766072, -0.0001713722456126752025, 0.000000000000000000 ) ) ;
#33273 = FACE_OUTER_BOUND ( 'NONE', #25596, .T. ) ;
#33272 = CARTESIAN_POINT ( 'NONE',  ( 106.1957191385480854, -47.06291487533366080, 258.4975300378154088 ) ) ;
#33274 = LINE ( 'NONE', #88259, #88452 ) ;
#33275 = ADVANCED_FACE ( 'NONE', ( #53710 ), #66465, .T. ) ;
#33276 = EDGE_CURVE ( 'NONE', #1529, #68029, #82001, .T. ) ;
#33277 = DIRECTION ( 'NONE',  ( -1.000000000000000000, 0.000000000000000000, 9.299908063537909262E-17 ) ) ;
#33278 = CIRCLE ( 'NONE', #20253, 0.5000000000000129896 ) ;
#33279 = CYLINDRICAL_SURFACE ( 'NONE', #73962, 2.750000000000002665 ) ;
#33280 = ADVANCED_FACE ( 'NONE', ( #560, #68718 ), #42330, .T. ) ;
#33281 = DIRECTION ( 'NONE',  ( 0.000000000000000000, -1.000000000000000000, 0.000000000000000000 ) ) ;
#33282 = CARTESIAN_POINT ( 'NONE',  ( 113.0097079652340568, -45.31096836313454190, 203.0584824187679374 ) ) ;
#33283 = DIRECTION ( 'NONE',  ( 0.000000000000000000, 1.000000000000000000, 0.000000000000000000 ) ) ;
#33284 = ORIENTED_EDGE ( 'NONE', *, *, #78133, .F. ) ;
#33285 = ORIENTED_EDGE ( 'NONE', *, *, #51013, .F. ) ;
#33286 = EDGE_CURVE ( 'NONE', #53618, #33391, #49143, .T. ) ;
#33287 = DIRECTION ( 'NONE',  ( -3.418174336900117128E-15, -1.000000000000000000, 0.000000000000000000 ) ) ;
#33288 = DIRECTION ( 'NONE',  ( 0.000000000000000000, 0.000000000000000000, 1.000000000000000000 ) ) ;
#33289 = AXIS2_PLACEMENT_3D ( 'NONE', #25183, #66516, #58798 ) ;
#33290 = CARTESIAN_POINT ( 'NONE',  ( 99.09593196240410862, -30.55013448537800258, 185.8027427927754047 ) ) ;
#33291 = FACE_OUTER_BOUND ( 'NONE', #51178, .T. ) ;
#33292 = DIRECTION ( 'NONE',  ( 0.000000000000000000, 0.000000000000000000, 1.000000000000000000 ) ) ;
#33293 = ORIENTED_EDGE ( 'NONE', *, *, #53022, .T. ) ;
#33294 = CYLINDRICAL_SURFACE ( 'NONE', #20484, 9.999999999999998224 ) ;
#33295 = CARTESIAN_POINT ( 'NONE',  ( 103.3034881226635946, -27.00695273605797908, 215.3699109901969848 ) ) ;
#33296 = CARTESIAN_POINT ( 'NONE',  ( 51.03742451361726751, -23.42844715994066362, 300.4678068554150059 ) ) ;
#33297 = ORIENTED_EDGE ( 'NONE', *, *, #48557, .T. ) ;
#33298 = ADVANCED_FACE ( 'NONE', ( #28726 ), #89618, .T. ) ;
#33299 = AXIS2_PLACEMENT_3D ( 'NONE', #58019, #51189, #64397 ) ;
#33300 = CARTESIAN_POINT ( 'NONE',  ( 126.8164832912740394, -54.62589567669621005, -5.074374724089010691 ) ) ;
#33301 = LINE ( 'NONE', #60998, #50710 ) ;
#33302 = LINE ( 'NONE', #75083, #68711 ) ;
#33303 = CARTESIAN_POINT ( 'NONE',  ( 101.9087497524793804, -29.77971984236790703, 33.41475703625796001 ) ) ;
#33304 = CARTESIAN_POINT ( 'NONE',  ( 114.7420861883949215, -43.81622209775510157, 119.2327681330539804 ) ) ;
#33305 = CYLINDRICAL_SURFACE ( 'NONE', #62382, 3.500000000000003109 ) ;
#33306 = VERTEX_POINT ( 'NONE', #27375 ) ;
#33307 = FACE_OUTER_BOUND ( 'NONE', #6593, .T. ) ;
#33308 = VECTOR ( 'NONE', #65459, 1000.000000000000000 ) ;
#33309 = CARTESIAN_POINT ( 'NONE',  ( 82.26522136039946531, -17.07517613920460420, 7.387586420634624673 ) ) ;
#33310 = ORIENTED_EDGE ( 'NONE', *, *, #80984, .T. ) ;
#33311 = VERTEX_POINT ( 'NONE', #35985 ) ;
#33312 = LINE ( 'NONE', #83264, #952 ) ;
#33313 = EDGE_LOOP ( 'NONE', ( #20686, #9061 ) ) ;
#33314 = ORIENTED_EDGE ( 'NONE', *, *, #77635, .T. ) ;
#33315 = DIRECTION ( 'NONE',  ( -1.000000000000000000, -8.163404592831600092E-16, -1.020425574103949962E-15 ) ) ;
#33316 = CARTESIAN_POINT ( 'NONE',  ( 107.2750367832685043, -27.67576416532946126, 74.46861030426799744 ) ) ;
#33317 = CARTESIAN_POINT ( 'NONE',  ( 103.9326413674837539, -26.76323430032771000, 250.3184824187677577 ) ) ;
#33318 = AXIS2_PLACEMENT_3D ( 'NONE', #24671, #79215, #52337 ) ;
#33319 = CARTESIAN_POINT ( 'NONE',  ( 98.27975524859421341, -42.29919363830190804, 186.7756252759109543 ) ) ;
#33321 = CARTESIAN_POINT ( 'NONE',  ( 104.2468583329775811, -46.74335657891433726, 18.35848241876792031 ) ) ;
#33320 = CARTESIAN_POINT ( 'NONE',  ( 180.2121375201600131, -29.73316016639650172, -5.074374724088000832 ) ) ;
#33322 = FACE_OUTER_BOUND ( 'NONE', #16263, .T. ) ;
#33323 = DIRECTION ( 'NONE',  ( -8.568612280633850929E-05, 0.4999999926578935772, -0.8660254037844357100 ) ) ;
#33324 = AXIS2_PLACEMENT_3D ( 'NONE', #66527, #72902, #30678 ) ;
#33325 = EDGE_LOOP ( 'NONE', ( #42955, #19224, #39099, #3991 ) ) ;
#33326 = EDGE_CURVE ( 'NONE', #84820, #28975, #41436, .T. ) ;
#33327 = VECTOR ( 'NONE', #79832, 1000.000000000000000 ) ;
#33328 = AXIS2_PLACEMENT_3D ( 'NONE', #28379, #42890, #70624 ) ;
#33329 = CARTESIAN_POINT ( 'NONE',  ( 0.000000000000000000, 8.255000000000000782, 0.000000000000000000 ) ) ;
#33330 = CARTESIAN_POINT ( 'NONE',  ( 110.2694181837619141, -26.72479813065621812, 234.8299109901969643 ) ) ;
#33331 = ORIENTED_EDGE ( 'NONE', *, *, #27531, .F. ) ;
#33332 = CARTESIAN_POINT ( 'NONE',  ( 115.0397999656063917, -29.07403674218411638, 189.4232443235299570 ) ) ;
#33333 = FACE_OUTER_BOUND ( 'NONE', #50523, .T. ) ;
#33334 = EDGE_CURVE ( 'NONE', #10966, #46111, #49596, .T. ) ;
#33335 = CARTESIAN_POINT ( 'NONE',  ( 108.3326240688572994, -46.73495791008426892, 23.67722514622035490 ) ) ;
#33336 = DIRECTION ( 'NONE',  ( -0.7071067811865779928, 0.7071067811865171526, -7.071067811865786933E-16 ) ) ;
#33338 = CYLINDRICAL_SURFACE ( 'NONE', #42733, 0.4999999999999932832 ) ;
#33337 = CARTESIAN_POINT ( 'NONE',  ( 114.8103026587852042, -34.36884736280054398, 277.6356252759111953 ) ) ;
#33339 = CARTESIAN_POINT ( 'NONE',  ( 98.04139480429049058, -41.04159787523226299, 172.6811693813438637 ) ) ;
#33340 = CARTESIAN_POINT ( 'NONE',  ( 148.0533267522752112, 0.000000000000000000, 160.2664750769284865 ) ) ;
#33341 = CARTESIAN_POINT ( 'NONE',  ( 134.0664832912740110, -46.72944715994100306, 10.72562527591099801 ) ) ;
#33342 = CIRCLE ( 'NONE', #53665, 6.557978799109520196 ) ;
#33343 = DIRECTION ( 'NONE',  ( 1.000000000000000078E-15, 1.000000000000000083E-30, -1.000000000000000000 ) ) ;
#33344 = CARTESIAN_POINT ( 'NONE',  ( 41.56648329127499153, -32.07844715994070839, 198.9256252759119832 ) ) ;
#33345 = PLANE ( 'NONE',  #69544 ) ;
#33347 = VERTEX_POINT ( 'NONE', #34182 ) ;
#33346 = CARTESIAN_POINT ( 'NONE',  ( 101.1158614047228070, -28.69863163947533735, 195.5838086201111992 ) ) ;
#33348 = CARTESIAN_POINT ( 'NONE',  ( 136.7703230406665398, -19.23127003359448395, 6.817519769821157816 ) ) ;
#33349 = CARTESIAN_POINT ( 'NONE',  ( 117.2491520020922451, -41.08934384016853869, 213.5165776568629781 ) ) ;
#33350 = CARTESIAN_POINT ( 'NONE',  ( 117.1064219673475719, -39.53695830471063744, 94.60991099019693706 ) ) ;
#33351 = CARTESIAN_POINT ( 'NONE',  ( 117.4730440113279855, -35.59081861377887179, 274.9127681330539872 ) ) ;
#33352 = CARTESIAN_POINT ( 'NONE',  ( 107.0664832912739399, -48.18858441225130917, 309.2406250056037038 ) ) ;
#33353 = AXIS2_PLACEMENT_3D ( 'NONE', #44464, #26159, #53829 ) ;
#33354 = FACE_OUTER_BOUND ( 'NONE', #12484, .T. ) ;
#33356 = DIRECTION ( 'NONE',  ( -4.237773401492740281E-14, 1.000000000000000000, 0.000000000000000000 ) ) ;
#33355 = DIRECTION ( 'NONE',  ( 0.000000000000000000, 0.000000000000000000, 1.000000000000000000 ) ) ;
#33357 = CARTESIAN_POINT ( 'NONE',  ( 48.45959712127249475, -26.00627455219082407, 117.4678068554150485 ) ) ;
#33358 = CARTESIAN_POINT ( 'NONE',  ( 29.56670390244828184, -48.82844715994152551, 300.4678068554150059 ) ) ;
#33359 = EDGE_CURVE ( 'NONE', #72100, #74526, #45638, .T. ) ;
#33360 = ORIENTED_EDGE ( 'NONE', *, *, #31360, .F. ) ;
#33361 = ORIENTED_EDGE ( 'NONE', *, *, #77085, .T. ) ;
#33362 = VECTOR ( 'NONE', #6634, 1000.000000000000000 ) ;
#33363 = CARTESIAN_POINT ( 'NONE',  ( 98.01111206384085506, -36.61009632703314765, 155.7505150661719995 ) ) ;
#33365 = ORIENTED_EDGE ( 'NONE', *, *, #82116, .F. ) ;
#33364 = CARTESIAN_POINT ( 'NONE',  ( 0.000000000000000000, 152.3879256507328250, 0.000000000000000000 ) ) ;
#33366 = CARTESIAN_POINT ( 'NONE',  ( 188.5667039024479834, -48.82844715994099971, 254.4678068554150343 ) ) ;
#33367 = CARTESIAN_POINT ( 'NONE',  ( 102.0922439024871551, -27.59239485085799970, 141.4727681330539895 ) ) ;
#33368 = DIRECTION ( 'NONE',  ( 0.000000000000000000, 0.000000000000000000, 1.000000000000000000 ) ) ;
#33369 = DIRECTION ( 'NONE',  ( -1.000000000000000000, -4.299999999999999979E-14, -1.000000000000000078E-15 ) ) ;
#33370 = DIRECTION ( 'NONE',  ( -1.000000000000000000, 0.000000000000000000, 0.000000000000000000 ) ) ;
#33371 = FACE_OUTER_BOUND ( 'NONE', #33313, .T. ) ;
#33372 = CARTESIAN_POINT ( 'NONE',  ( 110.2470682213182869, -46.59973918892936240, 57.83657765686300678 ) ) ;
#33373 = ORIENTED_EDGE ( 'NONE', *, *, #51902, .T. ) ;
#33374 = VECTOR ( 'NONE', #79106, 1000.000000000000000 ) ;
#33375 = ORIENTED_EDGE ( 'NONE', *, *, #52235, .T. ) ;
#33376 = VERTEX_POINT ( 'NONE', #34637 ) ;
#33377 = FACE_OUTER_BOUND ( 'NONE', #51754, .T. ) ;
#33379 = CARTESIAN_POINT ( 'NONE',  ( -33.98325472291465132, 124.5870000000000033, 3.174999999999764899 ) ) ;
#33378 = CARTESIAN_POINT ( 'NONE',  ( 98.71823956546970180, -31.63334453281608916, 166.8899109901959719 ) ) ;
#33380 = DIRECTION ( 'NONE',  ( 0.000000000000000000, 0.000000000000000000, 1.000000000000000000 ) ) ;
#33381 = FACE_OUTER_BOUND ( 'NONE', #83588, .T. ) ;
#33382 = ADVANCED_FACE ( 'NONE', ( #61887 ), #55054, .F. ) ;
#33383 = DIRECTION ( 'NONE',  ( -1.000000000000000000, -8.843517682682131024E-16, -1.000000000000000078E-15 ) ) ;
#33384 = CIRCLE ( 'NONE', #30475, 9.524999999999998579 ) ;
#33385 = CARTESIAN_POINT ( 'NONE',  ( 86.67541640318067664, 94.58006533271583294, 80.88915705228943409 ) ) ;
#33386 = CARTESIAN_POINT ( 'NONE',  ( 109.6427116155909545, -46.48016239540778827, 178.7814341963612605 ) ) ;
#33387 = CARTESIAN_POINT ( 'NONE',  ( 98.87507392487043489, -43.19978241230797522, 91.85848241876892928 ) ) ;
#33388 = EDGE_LOOP ( 'NONE', ( #10245, #80473, #16317, #18217, #58243 ) ) ;
#33389 = EDGE_CURVE ( 'NONE', #79084, #2549, #15100, .T. ) ;
#33390 = EDGE_LOOP ( 'NONE', ( #85836, #82180, #21244, #25535, #11532, #48333 ) ) ;
#33391 = VERTEX_POINT ( 'NONE', #48693 ) ;
#33392 = VECTOR ( 'NONE', #14714, 1000.000000000000114 ) ;
#33393 = EDGE_CURVE ( 'NONE', #44353, #70068, #83699, .T. ) ;
#33394 = CYLINDRICAL_SURFACE ( 'NONE', #27058, 9.999999999999998224 ) ;
#33395 = CARTESIAN_POINT ( 'NONE',  ( -88.25669247804601980, 93.94566094357733732, -96.20686424029906902 ) ) ;
#33396 = CARTESIAN_POINT ( 'NONE',  ( 53.56670390244786262, -48.82844715994099971, 180.4678068554151196 ) ) ;
#33397 = CARTESIAN_POINT ( 'NONE',  ( 109.2506105747909828, -28.86437792779224409, 172.6795189410199498 ) ) ;
#33398 = VECTOR ( 'NONE', #10102, 1000.000000000000000 ) ;
#33399 = CARTESIAN_POINT ( 'NONE',  ( 144.0667052733537901, -75.82844715994092155, 222.2178068554179902 ) ) ;
#33400 = ORIENTED_EDGE ( 'NONE', *, *, #40284, .F. ) ;
#33402 = VERTEX_POINT ( 'NONE', #13311 ) ;
#33401 = ORIENTED_EDGE ( 'NONE', *, *, #14209, .F. ) ;
#33403 = EDGE_CURVE ( 'NONE', #32600, #4876, #70517, .T. ) ;
#33404 = VECTOR ( 'NONE', #37231, 1000.000000000000000 ) ;
#33405 = LINE ( 'NONE', #68382, #68519 ) ;
#33406 = FACE_OUTER_BOUND ( 'NONE', #82802, .T. ) ;
#33407 = VERTEX_POINT ( 'NONE', #123 ) ;
#33408 = ORIENTED_EDGE ( 'NONE', *, *, #9191, .T. ) ;
#33409 = EDGE_CURVE ( 'NONE', #79637, #68056, #6502, .T. ) ;
#33410 = CARTESIAN_POINT ( 'NONE',  ( 41.56648329127398966, -27.82844715994070484, 258.9256252759120116 ) ) ;
#33411 = CARTESIAN_POINT ( 'NONE',  ( 112.1951879357659152, -44.60173489647391420, 219.4796785439919802 ) ) ;
#33412 = CIRCLE ( 'NONE', #55108, 7.937500000000000000 ) ;
#33413 = CARTESIAN_POINT ( 'NONE',  ( 107.0667039024470313, -104.2784471599420755, -19.78219314458201694 ) ) ;
#33414 = FACE_OUTER_BOUND ( 'NONE', #23226, .T. ) ;
#33415 = ORIENTED_EDGE ( 'NONE', *, *, #32362, .T. ) ;
#33416 = ORIENTED_EDGE ( 'NONE', *, *, #20863, .T. ) ;
#33417 = CARTESIAN_POINT ( 'NONE',  ( 141.8664832912739939, -71.52944715994085811, 361.9756252759100335 ) ) ;
#33418 = ORIENTED_EDGE ( 'NONE', *, *, #13588, .F. ) ;
#33419 = ORIENTED_EDGE ( 'NONE', *, *, #8566, .F. ) ;
#33420 = VECTOR ( 'NONE', #64473, 1000.000000000000114 ) ;
#33421 = CARTESIAN_POINT ( 'NONE',  ( 110.2461554203946292, -29.21150786992351911, 242.5766617981629452 ) ) ;
#33422 = CARTESIAN_POINT ( 'NONE',  ( 98.13060510664840308, -43.27509626496242134, 106.8175300378159704 ) ) ;
#33423 = CARTESIAN_POINT ( 'NONE',  ( 117.9019101119220068, -41.46671778014666643, 58.49848241876792798 ) ) ;
#33424 = CARTESIAN_POINT ( 'NONE',  ( 115.9130035588905798, -40.24476411946300658, 249.5838068554177482 ) ) ;
#33425 = CARTESIAN_POINT ( 'NONE',  ( 132.1570028294955819, -16.74831852143706712, 7.618261863063341188 ) ) ;
#33426 = CARTESIAN_POINT ( 'NONE',  ( 107.4813127257300636, -25.27694550238891580, 320.8178638332907440 ) ) ;
#33427 = CARTESIAN_POINT ( 'NONE',  ( 97.05822270422260090, -41.42079030513556859, 207.6632443235299661 ) ) ;
#33428 = DIRECTION ( 'NONE',  ( 0.000000000000000000, 0.000000000000000000, -1.000000000000000000 ) ) ;
#33429 = ORIENTED_EDGE ( 'NONE', *, *, #29471, .F. ) ;
#33430 = CARTESIAN_POINT ( 'NONE',  ( 19.56648329127400032, -18.82844715994099971, -5.074374724088000832 ) ) ;
#33431 = ORIENTED_EDGE ( 'NONE', *, *, #24447, .F. ) ;
#33432 = VERTEX_POINT ( 'NONE', #20578 ) ;
#33433 = DIRECTION ( 'NONE',  ( -1.000000000000000000, -4.299999999999999979E-14, -1.000000000000000078E-15 ) ) ;
#33435 = ORIENTED_EDGE ( 'NONE', *, *, #45791, .F. ) ;
#33434 = VECTOR ( 'NONE', #11729, 1000.000000000000000 ) ;
#33436 = CARTESIAN_POINT ( 'NONE',  ( -487.2989999999999782, 101.9113919710471947, 11.11250000000054072 ) ) ;
#33437 = CARTESIAN_POINT ( 'NONE',  ( 112.1361961822399707, -28.01101909465306150, 90.65674523166063636 ) ) ;
#33438 = CARTESIAN_POINT ( 'NONE',  ( 113.3148160382734773, -28.33991531616941728, 104.5670538473399347 ) ) ;
#33439 = CARTESIAN_POINT ( 'NONE',  ( 109.7287940957687908, -27.00184760396491868, 254.8647456037904533 ) ) ;
#33440 = EDGE_CURVE ( 'NONE', #38972, #5327, #55500, .T. ) ;
#33441 = CARTESIAN_POINT ( 'NONE',  ( 88.24325903289653183, -55.55267141831875222, -4.824374724089048883 ) ) ;
#33442 = LINE ( 'NONE', #13012, #52752 ) ;
#33445 = CARTESIAN_POINT ( 'NONE',  ( 97.07914014679033698, -41.41098531455288168, 207.6632443235299661 ) ) ;
#33444 = CARTESIAN_POINT ( 'NONE',  ( -41.60202597009397607, 65.59999999999998010, 50.85338361873603219 ) ) ;
#33443 = DIRECTION ( 'NONE',  ( 0.000000000000000000, 0.000000000000000000, 1.000000000000000000 ) ) ;
#33446 = CARTESIAN_POINT ( 'NONE',  ( 177.0371591254543375, -48.62818131005480637, 300.4678068554149490 ) ) ;
#33447 = CARTESIAN_POINT ( 'NONE',  ( 165.9667039024476765, -26.71338133338628040, 117.4678068554150485 ) ) ;
#33448 = ORIENTED_EDGE ( 'NONE', *, *, #54174, .F. ) ;
#33449 = CARTESIAN_POINT ( 'NONE',  ( 163.0959832912772356, -23.42844715993520310, 193.9678068554149775 ) ) ;
#33450 = CARTESIAN_POINT ( 'NONE',  ( 29.00000000000001421, 127.0000000000000000, 113.8826257785461280 ) ) ;
#33451 = FACE_OUTER_BOUND ( 'NONE', #6698, .T. ) ;
#33452 = AXIS2_PLACEMENT_3D ( 'NONE', #68112, #74478, #32233 ) ;
#33453 = CARTESIAN_POINT ( 'NONE',  ( 37.36643805256671413, -48.62818131006120836, 300.4678068554150059 ) ) ;
#33455 = ORIENTED_EDGE ( 'NONE', *, *, #14319, .T. ) ;
#33454 = CARTESIAN_POINT ( 'NONE',  ( 99.50747941120199869, -29.43470559729854230, 250.7156252759109520 ) ) ;
#33456 = FACE_OUTER_BOUND ( 'NONE', #35313, .T. ) ;
#33457 = CARTESIAN_POINT ( 'NONE',  ( 96.68927247633037325, -32.92320750051204215, 17.03467289495896964 ) ) ;
#33458 = CARTESIAN_POINT ( 'NONE',  ( 102.8960693947464051, -27.08911147246314499, 151.4013395616249511 ) ) ;
#33459 = PLANE ( 'NONE',  #40329 ) ;
#33460 = CARTESIAN_POINT ( 'NONE',  ( 102.0672082652289419, -27.97040743572448562, 101.4897538293649006 ) ) ;
#33462 = DIRECTION ( 'NONE',  ( -1.000000000000000000, 0.000000000000000000, 0.000000000000000000 ) ) ;
#33461 = DIRECTION ( 'NONE',  ( 0.000000000000000000, 0.000000000000000000, 1.000000000000000000 ) ) ;
#33463 = CARTESIAN_POINT ( 'NONE',  ( 100.9546728717598540, -28.70702568209258843, 190.5939586032972670 ) ) ;
#33464 = LINE ( 'NONE', #5774, #75587 ) ;
#33465 = VERTEX_POINT ( 'NONE', #56412 ) ;
#33466 = CIRCLE ( 'NONE', #20375, 7.143750000000004263 ) ;
#33467 = EDGE_CURVE ( 'NONE', #82508, #65069, #67447, .T. ) ;
#33468 = VERTEX_POINT ( 'NONE', #1479 ) ;
#33469 = ORIENTED_EDGE ( 'NONE', *, *, #56729, .T. ) ;
#33470 = AXIS2_PLACEMENT_3D ( 'NONE', #77123, #71208, #14899 ) ;
#33471 = ORIENTED_EDGE ( 'NONE', *, *, #3195, .T. ) ;
#33472 = PLANE ( 'NONE',  #53785 ) ;
#33473 = CARTESIAN_POINT ( 'NONE',  ( 104.7405551043178633, -47.51155644559842273, 28.41943479971997988 ) ) ;
#33474 = DIRECTION ( 'NONE',  ( 0.000000000000000000, 0.000000000000000000, -1.000000000000000000 ) ) ;
#33475 = CARTESIAN_POINT ( 'NONE',  ( 145.4156254839468829, -139.2796780384615261, 246.0351580304962056 ) ) ;
#33476 = EDGE_CURVE ( 'NONE', #55433, #38579, #8289, .T. ) ;
#33477 = CARTESIAN_POINT ( 'NONE',  ( 122.2211117073404409, -111.9484015127202667, -19.21046202161275218 ) ) ;
#33478 = CARTESIAN_POINT ( 'NONE',  ( 114.2672205647202048, -43.24251175450689288, 232.6638483995059801 ) ) ;
#33479 = VERTEX_POINT ( 'NONE', #48246 ) ;
#33480 = ORIENTED_EDGE ( 'NONE', *, *, #26740, .F. ) ;
#33481 = VERTEX_POINT ( 'NONE', #69617 ) ;
#33482 = LINE ( 'NONE', #82110, #48549 ) ;
#33484 = ADVANCED_FACE ( 'NONE', ( #7386, #35076, #86380, #50500 ), #16893, .F. ) ;
#33483 = FACE_BOUND ( 'NONE', #55145, .T. ) ;
#33485 = CARTESIAN_POINT ( 'NONE',  ( 63.06670390244645574, -24.92844715994017335, 129.9678068554150911 ) ) ;
#33486 = CARTESIAN_POINT ( 'NONE',  ( 179.1667039024460166, -28.27351298637280408, -5.074374724088000832 ) ) ;
#33487 = CARTESIAN_POINT ( 'NONE',  ( 111.8905564713631549, -28.66688903671830246, 51.09110711541997318 ) ) ;
#33488 = AXIS2_PLACEMENT_3D ( 'NONE', #85063, #37339, #56873 ) ;
#33489 = DIRECTION ( 'NONE',  ( 0.000000000000000000, 0.000000000000000000, -1.000000000000000000 ) ) ;
#33490 = AXIS2_PLACEMENT_3D ( 'NONE', #12028, #89679, #67878 ) ;
#33491 = CARTESIAN_POINT ( 'NONE',  ( 31.75000000000000000, 66.67499999999999716, 346.0750000000000455 ) ) ;
#33492 = CARTESIAN_POINT ( 'NONE',  ( 116.0161715043950466, -40.67488961668907166, 253.4956252759109532 ) ) ;
#33494 = EDGE_CURVE ( 'NONE', #30523, #62685, #36447, .T. ) ;
#33493 = VECTOR ( 'NONE', #15724, 1000.000000000000000 ) ;
#33495 = CYLINDRICAL_SURFACE ( 'NONE', #55950, 2.500000000000002220 ) ;
#33496 = ORIENTED_EDGE ( 'NONE', *, *, #87626, .F. ) ;
#33497 = CARTESIAN_POINT ( 'NONE',  ( 162.7131505118539962, -33.70561438052111214, -5.074374724088000832 ) ) ;
#33498 = AXIS2_PLACEMENT_3D ( 'NONE', #11898, #18700, #74559 ) ;
#33499 = DIRECTION ( 'NONE',  ( 0.000000000000000000, 0.000000000000000000, 1.000000000000000000 ) ) ;
#33500 = CARTESIAN_POINT ( 'NONE',  ( 99.41042786952979782, -33.89845062227509231, 63.86237608387695985 ) ) ;
#33501 = AXIS2_PLACEMENT_3D ( 'NONE', #79129, #44122, #2821 ) ;
#33502 = CARTESIAN_POINT ( 'NONE',  ( -72.96458098368751166, 117.4749999999999943, 72.96458098368620426 ) ) ;
#33503 = FACE_OUTER_BOUND ( 'NONE', #89032, .T. ) ;
#33504 = DIRECTION ( 'NONE',  ( -0.9999999853157766072, -0.0001713722456134502174, 0.000000000000000000 ) ) ;
#33505 = VERTEX_POINT ( 'NONE', #78246 ) ;
#33506 = ADVANCED_FACE ( 'NONE', ( #51379 ), #29619, .T. ) ;
#33507 = FACE_BOUND ( 'NONE', #86158, .T. ) ;
#33508 = EDGE_LOOP ( 'NONE', ( #51210, #11731, #84301, #3883, #59650, #67365 ) ) ;
#33509 = CARTESIAN_POINT ( 'NONE',  ( 99.42196222650996162, -27.67359991961172128, 150.6356252759109680 ) ) ;
#33510 = ORIENTED_EDGE ( 'NONE', *, *, #82758, .F. ) ;
#33511 = EDGE_CURVE ( 'NONE', #76783, #67053, #86825, .T. ) ;
#33512 = CARTESIAN_POINT ( 'NONE',  ( 104.7294611837924094, -27.30559681290521112, 89.69241982807696445 ) ) ;
#33513 = ADVANCED_FACE ( 'NONE', ( #24156 ), #8010, .T. ) ;
#33514 = LINE ( 'NONE', #61215, #15591 ) ;
#33515 = CARTESIAN_POINT ( 'NONE',  ( 100.0737993132363783, -29.47871783549896918, 112.1187261630399661 ) ) ;
#33516 = CYLINDRICAL_SURFACE ( 'NONE', #1098, 2.500000000000002220 ) ;
#33517 = EDGE_CURVE ( 'NONE', #73231, #37163, #23478, .T. ) ;
#33518 = CARTESIAN_POINT ( 'NONE',  ( 63.06670390244732971, -24.92844715994017690, 300.4678068554150627 ) ) ;
#33519 = CARTESIAN_POINT ( 'NONE',  ( 110.4636787236150184, -47.27194539037950705, 53.83657765686300678 ) ) ;
#33520 = VECTOR ( 'NONE', #26306, 1000.000000000000000 ) ;
#33521 = DIRECTION ( 'NONE',  ( -3.100000000000000258E-29, 3.100000000000000044E-14, 1.000000000000000000 ) ) ;
#33522 = CARTESIAN_POINT ( 'NONE',  ( 182.2738106836200132, -23.19206098993950604, 342.9256252759119548 ) ) ;
#33523 = VERTEX_POINT ( 'NONE', #77781 ) ;
#33524 = CARTESIAN_POINT ( 'NONE',  ( 74.06670390244704549, -118.2784471599409812, 230.7030882296565721 ) ) ;
#33525 = ORIENTED_EDGE ( 'NONE', *, *, #4141, .F. ) ;
#33526 = EDGE_LOOP ( 'NONE', ( #68614, #24269, #29070, #8535 ) ) ;
#33527 = VECTOR ( 'NONE', #47275, 999.9999999999998863 ) ;
#33528 = DIRECTION ( 'NONE',  ( 0.000000000000000000, 0.000000000000000000, -1.000000000000000000 ) ) ;
#33529 = EDGE_LOOP ( 'NONE', ( #5129, #31835 ) ) ;
#33530 = CARTESIAN_POINT ( 'NONE',  ( 106.1957191385480570, -47.06291487533376028, 262.4975300378164320 ) ) ;
#33531 = CARTESIAN_POINT ( 'NONE',  ( 105.7176149122623485, -24.93101994221251516, 156.1670538473399574 ) ) ;
#33532 = CARTESIAN_POINT ( 'NONE',  ( -100.8594679592212344, 82.54999999999999716, 82.89895571708261457 ) ) ;
#33533 = DIRECTION ( 'NONE',  ( 0.000000000000000000, 0.000000000000000000, 1.000000000000000000 ) ) ;
#33534 = CARTESIAN_POINT ( 'NONE',  ( 117.3534687869931048, -38.62661931536851512, 84.68133956162593279 ) ) ;
#33535 = CIRCLE ( 'NONE', #64025, 12.44600000000001216 ) ;
#33536 = PLANE ( 'NONE',  #10330 ) ;
#33537 = ORIENTED_EDGE ( 'NONE', *, *, #58715, .T. ) ;
#33538 = DIRECTION ( 'NONE',  ( -1.000000000000000000, -6.814610998690690172E-14, -1.000000000000000078E-15 ) ) ;
#33539 = CARTESIAN_POINT ( 'NONE',  ( 117.0718120722267628, -35.46179131731675227, 159.9271957950691956 ) ) ;
#33540 = ORIENTED_EDGE ( 'NONE', *, *, #72266, .F. ) ;
#33541 = DIRECTION ( 'NONE',  ( 0.000000000000000000, 0.000000000000000000, 1.000000000000000000 ) ) ;
#33542 = FACE_OUTER_BOUND ( 'NONE', #53977, .T. ) ;
#33543 = CARTESIAN_POINT ( 'NONE',  ( 105.1131368864170241, -25.87365329830167937, 275.2061014663871674 ) ) ;
#33544 = LINE ( 'NONE', #28065, #88160 ) ;
#33545 = DIRECTION ( 'NONE',  ( -1.000000000000000000, -8.540177112501204385E-16, 0.000000000000000000 ) ) ;
#33546 = CARTESIAN_POINT ( 'NONE',  ( 116.3137647483393806, -32.94861263809731611, 185.1356252759109680 ) ) ;
#33547 = CARTESIAN_POINT ( 'NONE',  ( 105.0359719168109933, -28.43277227512634298, 284.6895626852196415 ) ) ;
#33549 = CARTESIAN_POINT ( 'NONE',  ( 102.6254653968536417, -46.82603978519634325, 128.2346728949589760 ) ) ;
#33548 = PLANE ( 'NONE',  #34756 ) ;
#33550 = PLANE ( 'NONE',  #19014 ) ;
#33551 = CARTESIAN_POINT ( 'NONE',  ( 108.2829496674670224, -47.76277978039057359, 157.6518157521019532 ) ) ;
#33552 = VERTEX_POINT ( 'NONE', #71421 ) ;
#33553 = DIRECTION ( 'NONE',  ( 0.000000000000000000, -0.8660254037844387076, 0.4999999999999998890 ) ) ;
#33554 = ORIENTED_EDGE ( 'NONE', *, *, #50908, .T. ) ;
#33555 = DIRECTION ( 'NONE',  ( 0.7071067811865536790, 0.000000000000000000, -0.7071067811865414665 ) ) ;
#33556 = VECTOR ( 'NONE', #36397, 1000.000000000000000 ) ;
#33557 = CARTESIAN_POINT ( 'NONE',  ( 188.5667039024479834, -62.87844715994099687, 293.2178068554150627 ) ) ;
#33558 = CARTESIAN_POINT ( 'NONE',  ( 136.7325000480765311, -36.03188439719874481, 2.979900720422823390 ) ) ;
#33559 = ORIENTED_EDGE ( 'NONE', *, *, #6422, .T. ) ;
#33560 = CARTESIAN_POINT ( 'NONE',  ( -103.1875000000000000, 127.0000000000000000, -1.080832317973422076E-12 ) ) ;
#33562 = ORIENTED_EDGE ( 'NONE', *, *, #53543, .T. ) ;
#33561 = CARTESIAN_POINT ( 'NONE',  ( 99.06758658495417080, -45.54097539030503583, 156.9899109901969609 ) ) ;
#33564 = PLANE ( 'NONE',  #8849 ) ;
#33563 = UNCERTAINTY_MEASURE_WITH_UNIT (LENGTH_MEASURE( 1.000000000000000082E-05 ), #70451, 'distance_accuracy_value', 'NONE');
#33565 = CARTESIAN_POINT ( 'NONE',  ( -129.9777364973647025, 85.83513192049078100, 12.27484926615008476 ) ) ;
#33566 = VECTOR ( 'NONE', #1858, 1000.000000000000000 ) ;
#33567 = FACE_OUTER_BOUND ( 'NONE', #68813, .T. ) ;
#33568 = DIRECTION ( 'NONE',  ( 1.000000000000000000, 4.299999999999999979E-14, 1.000000000000000078E-15 ) ) ;
#33569 = ORIENTED_EDGE ( 'NONE', *, *, #38191, .F. ) ;
#33570 = AXIS2_PLACEMENT_3D ( 'NONE', #46586, #24825, #52490 ) ;
#33571 = EDGE_CURVE ( 'NONE', #82307, #71390, #15558, .T. ) ;
#33572 = EDGE_CURVE ( 'NONE', #37178, #30283, #85056, .T. ) ;
#33573 = EDGE_LOOP ( 'NONE', ( #78362, #40765, #6787, #64322 ) ) ;
#33574 = ORIENTED_EDGE ( 'NONE', *, *, #16186, .T. ) ;
#33575 = EDGE_CURVE ( 'NONE', #31161, #20465, #57768, .T. ) ;
#33576 = ORIENTED_EDGE ( 'NONE', *, *, #54791, .F. ) ;
#33577 = DIRECTION ( 'NONE',  ( -2.900000000000000265E-14, 2.000000000000000155E-15, -1.000000000000000000 ) ) ;
#33578 = CARTESIAN_POINT ( 'NONE',  ( 105.7386178790360418, -26.75993881439924138, 250.1823171237273584 ) ) ;
#33579 = PLANE ( 'NONE',  #43973 ) ;
#33580 = CYLINDRICAL_SURFACE ( 'NONE', #29944, 3.000000000000002665 ) ;
#33581 = ADVANCED_FACE ( 'NONE', ( #50950 ), #71859, .T. ) ;
#33582 = VECTOR ( 'NONE', #30821, 1000.000000000000114 ) ;
#33583 = ADVANCED_FACE ( 'NONE', ( #59537 ), #74530, .F. ) ;
#33585 = DIRECTION ( 'NONE',  ( 0.000000000000000000, 1.000000000000000000, 0.000000000000000000 ) ) ;
#33584 = CARTESIAN_POINT ( 'NONE',  ( 108.4172366116780637, -26.73500384902263960, 104.9689787242619019 ) ) ;
#33586 = CARTESIAN_POINT ( 'NONE',  ( 105.7993493439852699, -26.72405417386548265, 180.1773053279698331 ) ) ;
#33587 = AXIS2_PLACEMENT_3D ( 'NONE', #69778, #71579, #15715 ) ;
#33588 = EDGE_CURVE ( 'NONE', #50227, #57751, #53099, .T. ) ;
#33589 = ORIENTED_EDGE ( 'NONE', *, *, #78526, .T. ) ;
#33590 = DIRECTION ( 'NONE',  ( -0.000000000000000000, 1.000000000000000000, 0.000000000000000000 ) ) ;
#33592 = ADVANCED_FACE ( 'NONE', ( #67715 ), #73631, .T. ) ;
#33591 = DIRECTION ( 'NONE',  ( 0.000000000000000000, 0.000000000000000000, 1.000000000000000000 ) ) ;
#33593 = CARTESIAN_POINT ( 'NONE',  ( 106.5196382177907140, -25.62481104856566105, 191.1156252759109861 ) ) ;
#33594 = AXIS2_PLACEMENT_3D ( 'NONE', #88646, #54077, #40022 ) ;
#33596 = ORIENTED_EDGE ( 'NONE', *, *, #35121, .T. ) ;
#33595 = CARTESIAN_POINT ( 'NONE',  ( -479.3614999999999782, 3.174999999999999822, -1.387778780781445991E-14 ) ) ;
#33597 = CARTESIAN_POINT ( 'NONE',  ( 102.0112516875887678, -27.67497761899955933, 101.4937205140059575 ) ) ;
#33598 = EDGE_CURVE ( 'NONE', #18234, #76080, #88623, .T. ) ;
#33599 = CARTESIAN_POINT ( 'NONE',  ( 32.06670390244668312, -32.29483332968541731, 237.4678068554150059 ) ) ;
#33600 = CARTESIAN_POINT ( 'NONE',  ( 116.3265979651016409, -32.94445627519164077, 14.13562527591094664 ) ) ;
#33601 = CONICAL_SURFACE ( 'NONE', #45194, 6.857999999999975671, 0.02993239667170383839 ) ;
#33602 = EDGE_CURVE ( 'NONE', #89451, #4210, #76146, .T. ) ;
#33603 = DIRECTION ( 'NONE',  ( 0.000000000000000000, 0.000000000000000000, 1.000000000000000000 ) ) ;
#33604 = ORIENTED_EDGE ( 'NONE', *, *, #15284, .T. ) ;
#33605 = CARTESIAN_POINT ( 'NONE',  ( 226.4410000000000025, 65.43750000000000000, 10.66800000000000104 ) ) ;
#33606 = ORIENTED_EDGE ( 'NONE', *, *, #45028, .F. ) ;
#33607 = ORIENTED_EDGE ( 'NONE', *, *, #39096, .T. ) ;
#33608 = CARTESIAN_POINT ( 'NONE',  ( 107.2218274976867463, -26.65737820016106951, 226.4958690201829654 ) ) ;
#33609 = CARTESIAN_POINT ( 'NONE',  ( 99.50484159579329457, -43.30592805723910033, 52.89564321832823879 ) ) ;
#33610 = CARTESIAN_POINT ( 'NONE',  ( -117.8738102209307215, 82.96450994655481281, -12.70000000000041496 ) ) ;
#33611 = CARTESIAN_POINT ( 'NONE',  ( 117.0718954875924851, -35.46248236815851840, 154.9272919416320065 ) ) ;
#33612 = DIRECTION ( 'NONE',  ( -0.000000000000000000, -1.000000000000000000, -0.000000000000000000 ) ) ;
#33614 = EDGE_LOOP ( 'NONE', ( #61170, #70355, #6116, #56579, #51631 ) ) ;
#33613 = VECTOR ( 'NONE', #23224, 1000.000000000000000 ) ;
#33615 = FACE_OUTER_BOUND ( 'NONE', #71763, .T. ) ;
#33616 = EDGE_CURVE ( 'NONE', #65725, #28720, #66813, .T. ) ;
#33617 = DIRECTION ( 'NONE',  ( 0.000000000000000000, -1.000000000000000000, 0.000000000000000000 ) ) ;
#33618 = VERTEX_POINT ( 'NONE', #19560 ) ;
#33619 = CARTESIAN_POINT ( 'NONE',  ( 100.5975332644244844, -28.50897509465477597, 15.60705384733995871 ) ) ;
#33620 = ORIENTED_EDGE ( 'NONE', *, *, #42716, .F. ) ;
#33621 = ADVANCED_FACE ( 'NONE', ( #33195 ), #5501, .F. ) ;
#33622 = CARTESIAN_POINT ( 'NONE',  ( 102.8259602516037177, -43.70423678882019658, 244.9595189410199794 ) ) ;
#33623 = EDGE_CURVE ( 'NONE', #13040, #28371, #53151, .T. ) ;
#33624 = DIRECTION ( 'NONE',  ( -0.000000000000000000, -0.000000000000000000, 1.000000000000000000 ) ) ;
#33625 = CARTESIAN_POINT ( 'NONE',  ( 117.0460787713799817, -39.54838250520750620, 143.6194347997209775 ) ) ;
#33626 = DIRECTION ( 'NONE',  ( 0.000000000000000000, 0.000000000000000000, 1.000000000000000000 ) ) ;
#33627 = CYLINDRICAL_SURFACE ( 'NONE', #63600, 9.999999999999998224 ) ;
#33629 = EDGE_CURVE ( 'NONE', #51052, #8294, #34041, .T. ) ;
#33628 = CARTESIAN_POINT ( 'NONE',  ( 34.67381068360400320, -28.98061976758901892, -5.074374724088000832 ) ) ;
#33630 = VECTOR ( 'NONE', #50779, 1000.000000000000000 ) ;
#33631 = DIRECTION ( 'NONE',  ( 0.000000000000000000, 0.000000000000000000, 1.000000000000000000 ) ) ;
#33632 = CARTESIAN_POINT ( 'NONE',  ( 100.7237713325202861, -45.83809708005067307, 233.0803871806729717 ) ) ;
#33633 = DIRECTION ( 'NONE',  ( 0.000000000000000000, -1.000000000000000000, 0.000000000000000000 ) ) ;
#33634 = VERTEX_POINT ( 'NONE', #40451 ) ;
#33635 = AXIS2_PLACEMENT_3D ( 'NONE', #17020, #10199, #40472 ) ;
#33636 = CARTESIAN_POINT ( 'NONE',  ( 98.55462967347544634, -43.85305904914448405, 67.86895860924497015 ) ) ;
#33637 = CARTESIAN_POINT ( 'NONE',  ( 25.56670390244797275, -48.82844715994099971, 257.2178068554150059 ) ) ;
#33638 = ORIENTED_EDGE ( 'NONE', *, *, #6719, .F. ) ;
#33639 = ORIENTED_EDGE ( 'NONE', *, *, #19453, .T. ) ;
#33640 = ORIENTED_EDGE ( 'NONE', *, *, #50512, .T. ) ;
#33641 = CARTESIAN_POINT ( 'NONE',  ( 97.33768314765580953, -34.07170803572739715, 161.1146346061390204 ) ) ;
#33642 = LINE ( 'NONE', #12307, #80498 ) ;
#33643 = CYLINDRICAL_SURFACE ( 'NONE', #40758, 5.041900000000001825 ) ;
#33644 = FACE_OUTER_BOUND ( 'NONE', #58650, .T. ) ;
#33645 = CARTESIAN_POINT ( 'NONE',  ( 115.4711811475381467, -34.66499115051416169, 161.8242808457819706 ) ) ;
#33646 = CARTESIAN_POINT ( 'NONE',  ( 96.74182981399745529, -35.13608925046722220, 262.2041967044821149 ) ) ;
#33647 = VECTOR ( 'NONE', #53361, 1000.000000000000000 ) ;
#33648 = LINE ( 'NONE', #81376, #37825 ) ;
#33649 = ORIENTED_EDGE ( 'NONE', *, *, #59260, .F. ) ;
#33650 = CARTESIAN_POINT ( 'NONE',  ( 162.7131505118539962, -33.70561438052110503, 342.9256252759109884 ) ) ;
#33651 = LINE ( 'NONE', #20030, #56300 ) ;
#33652 = ORIENTED_EDGE ( 'NONE', *, *, #74809, .F. ) ;
#33654 = ORIENTED_EDGE ( 'NONE', *, *, #24979, .F. ) ;
#33653 = CIRCLE ( 'NONE', #4608, 0.9999999999999800160 ) ;
#33655 = AXIS2_PLACEMENT_3D ( 'NONE', #25719, #19808, #88860 ) ;
#33656 = PLANE ( 'NONE',  #5353 ) ;
#33657 = ORIENTED_EDGE ( 'NONE', *, *, #306, .T. ) ;
#33658 = VERTEX_POINT ( 'NONE', #61333 ) ;
#33659 = DIRECTION ( 'NONE',  ( 1.000000000000000078E-15, -1.000000000000000000, 0.000000000000000000 ) ) ;
#33660 = DIRECTION ( 'NONE',  ( 1.000000000000000000, 4.163336342344333240E-14, 0.000000000000000000 ) ) ;
#33661 = CARTESIAN_POINT ( 'NONE',  ( 107.0667039024470313, -104.2784471599409528, 45.21780685541799727 ) ) ;
#33662 = CARTESIAN_POINT ( 'NONE',  ( 100.1253875378072848, -39.57043109886186727, 9.635625275910941312 ) ) ;
#33663 = CARTESIAN_POINT ( 'NONE',  ( 113.1794296094924874, -30.05060732774411036, 153.8971817328389875 ) ) ;
#33664 = VECTOR ( 'NONE', #50304, 1000.000000000000000 ) ;
#33665 = CARTESIAN_POINT ( 'NONE',  ( 97.76994516709639527, -29.29956314839395048, 45.78991099019697231 ) ) ;
#33666 = CARTESIAN_POINT ( 'NONE',  ( 162.7131505118553321, -33.70561438051485936, 193.9678068554149775 ) ) ;
#33667 = ORIENTED_EDGE ( 'NONE', *, *, #41864, .F. ) ;
#33668 = DIRECTION ( 'NONE',  ( 0.000000000000000000, 0.000000000000000000, 1.000000000000000000 ) ) ;
#33669 = AXIS2_PLACEMENT_3D ( 'NONE', #48731, #42818, #6979 ) ;
#33670 = VERTEX_POINT ( 'NONE', #66358 ) ;
#33671 = FACE_OUTER_BOUND ( 'NONE', #79051, .T. ) ;
#33672 = ORIENTED_EDGE ( 'NONE', *, *, #73310, .T. ) ;
#33673 = DIRECTION ( 'NONE',  ( 0.000000000000000000, 0.000000000000000000, 1.000000000000000000 ) ) ;
#33674 = CARTESIAN_POINT ( 'NONE',  ( 145.2084014158841399, -138.9257025692045033, 247.5112265945679724 ) ) ;
#33675 = CARTESIAN_POINT ( 'NONE',  ( 108.3322807220838655, -46.73499201940651204, 132.6772426970024128 ) ) ;
#33676 = CARTESIAN_POINT ( 'NONE',  ( 45.77381068356854144, -48.62134037881681081, 129.9678068554150911 ) ) ;
#33677 = EDGE_LOOP ( 'NONE', ( #17873, #26054 ) ) ;
#33678 = CARTESIAN_POINT ( 'NONE',  ( 112.9757402841042904, -28.11393523324086985, 44.59848241876795782 ) ) ;
#33679 = CARTESIAN_POINT ( 'NONE',  ( 116.7149026195978792, -32.57661448200846621, 75.14991099019697174 ) ) ;
#33680 =( NAMED_UNIT ( * ) PLANE_ANGLE_UNIT ( ) SI_UNIT ( $, .RADIAN. ) );
#33681 = EDGE_CURVE ( 'NONE', #43910, #22374, #33642, .T. ) ;
#33683 = CARTESIAN_POINT ( 'NONE',  ( 86.06670390244796920, -50.82844715994100682, 10.91780685541499807 ) ) ;
#33682 = DIRECTION ( 'NONE',  ( -1.000000000000000000, -1.541976423090496028E-15, 0.000000000000000000 ) ) ;
#33684 = CARTESIAN_POINT ( 'NONE',  ( 177.1649999999999920, 5.112500000000000711, -7.937500000000000000 ) ) ;
#33685 = ADVANCED_FACE ( 'NONE', ( #68171 ), #87711, .F. ) ;
#33686 = CARTESIAN_POINT ( 'NONE',  ( 132.0298243561156539, -16.87939921900816387, 2.327894594454689603 ) ) ;
#33687 = VERTEX_POINT ( 'NONE', #39554 ) ;
#33688 = EDGE_CURVE ( 'NONE', #55859, #11211, #52880, .T. ) ;
#33689 = DIRECTION ( 'NONE',  ( -0.000000000000000000, 1.000000000000000000, -0.000000000000000000 ) ) ;
#33690 = DIRECTION ( 'NONE',  ( 0.000000000000000000, 0.000000000000000000, -1.000000000000000000 ) ) ;
#33691 = PLANE ( 'NONE',  #39753 ) ;
#33692 = EDGE_CURVE ( 'NONE', #40190, #71887, #64547, .T. ) ;
#33693 = ORIENTED_EDGE ( 'NONE', *, *, #28549, .T. ) ;
#33694 = CARTESIAN_POINT ( 'NONE',  ( 96.63486483157898022, -37.29388950852173679, 72.36991099019596163 ) ) ;
#33695 = VECTOR ( 'NONE', #27105, 1000.000000000000114 ) ;
#33697 = DIRECTION ( 'NONE',  ( 4.194175870806139918E-14, -1.000000000000000000, 0.000000000000000000 ) ) ;
#33696 = CARTESIAN_POINT ( 'NONE',  ( 194.5664832912739826, 15.62155284005900491, 323.8756252759109202 ) ) ;
#33698 = DIRECTION ( 'NONE',  ( 0.000000000000000000, 0.000000000000000000, -1.000000000000000000 ) ) ;
#33699 = ADVANCED_FACE ( 'NONE', ( #59981 ), #25038, .T. ) ;
#33700 = AXIS2_PLACEMENT_3D ( 'NONE', #39758, #67471, #38869 ) ;
#33701 = CARTESIAN_POINT ( 'NONE',  ( 36.65249034007445772, -49.32844715994130524, 180.4678068554150911 ) ) ;
#33702 = ORIENTED_EDGE ( 'NONE', *, *, #86017, .F. ) ;
#33703 = EDGE_CURVE ( 'NONE', #76607, #18319, #67258, .T. ) ;
#33704 = CARTESIAN_POINT ( 'NONE',  ( 109.6029845306728134, -46.78454271877401283, 88.78514908543394313 ) ) ;
#33706 = VERTEX_POINT ( 'NONE', #60436 ) ;
#33705 = CARTESIAN_POINT ( 'NONE',  ( 8.220576097192926923, 92.23944561992415458, 130.2971762513506917 ) ) ;
#33707 = CARTESIAN_POINT ( 'NONE',  ( 115.6772654923306902, -42.56752007954064965, 269.3527681330536439 ) ) ;
#33708 = CARTESIAN_POINT ( 'NONE',  ( -55.89999999999999858, 95.97500000000000853, 70.79999999999999716 ) ) ;
#33709 = FACE_OUTER_BOUND ( 'NONE', #45669, .T. ) ;
#33710 = DIRECTION ( 'NONE',  ( 0.000000000000000000, -1.000000000000000000, 0.000000000000000000 ) ) ;
#33711 = DIRECTION ( 'NONE',  ( 0.000000000000000000, 0.000000000000000000, -1.000000000000000000 ) ) ;
#33713 = EDGE_CURVE ( 'NONE', #23612, #60182, #28160, .T. ) ;
#33712 = AXIS2_PLACEMENT_3D ( 'NONE', #25682, #81575, #80667 ) ;
#33714 = DIRECTION ( 'NONE',  ( 1.000000000000000000, 4.101809204280141026E-14, 0.000000000000000000 ) ) ;
#33715 = DIRECTION ( 'NONE',  ( 1.000000000000000078E-15, -1.000000000000000083E-30, -1.000000000000000000 ) ) ;
#33716 = CARTESIAN_POINT ( 'NONE',  ( 98.71823956546961654, -31.63334453281603587, 170.8899109901969950 ) ) ;
#33717 = ORIENTED_EDGE ( 'NONE', *, *, #57812, .T. ) ;
#33718 = ORIENTED_EDGE ( 'NONE', *, *, #27640, .T. ) ;
#33719 = ADVANCED_FACE ( 'NONE', ( #82712 ), #75436, .T. ) ;
#33720 = CARTESIAN_POINT ( 'NONE',  ( 100.2558307937446074, -42.39895253252459639, 113.3101547344679574 ) ) ;
#33721 = CIRCLE ( 'NONE', #71479, 2.500000000000002220 ) ;
#33722 = CARTESIAN_POINT ( 'NONE',  ( 194.5664832912729878, 15.62155284005731204, 361.9756252759109998 ) ) ;
#33724 = DIRECTION ( 'NONE',  ( 1.000000000000000000, 4.299999999999999979E-14, 1.000000000000000078E-15 ) ) ;
#33723 = CARTESIAN_POINT ( 'NONE',  ( 110.5064767540468011, -26.94654216138288660, 250.8194347997200850 ) ) ;
#33725 = CARTESIAN_POINT ( 'NONE',  ( 67.06670390244700286, -67.87844715994098976, 247.2178068554179902 ) ) ;
#33726 = VECTOR ( 'NONE', #47052, 1000.000000000000000 ) ;
#33727 = CARTESIAN_POINT ( 'NONE',  ( 6.938893903907228378E-15, 149.3723753486177088, 96.88262577854611379 ) ) ;
#33728 = CARTESIAN_POINT ( 'NONE',  ( 107.0667039024470313, -104.2784471599409528, 19.21780685541800437 ) ) ;
#33729 = CARTESIAN_POINT ( 'NONE',  ( 76.06670390244703128, -104.2784471599409812, 45.21780685541799727 ) ) ;
#33730 = CARTESIAN_POINT ( 'NONE',  ( 194.5664832912729878, 25.62155284005700295, 361.9756252759109998 ) ) ;
#33731 = CARTESIAN_POINT ( 'NONE',  ( 98.56907362037662779, -44.95393718666142746, 191.9384824187679612 ) ) ;
#33732 = FACE_OUTER_BOUND ( 'NONE', #36806, .T. ) ;
#33733 = EDGE_LOOP ( 'NONE', ( #36295, #30634, #64589, #25035 ) ) ;
#33734 = ORIENTED_EDGE ( 'NONE', *, *, #38012, .F. ) ;
#33735 = CARTESIAN_POINT ( 'NONE',  ( -100.8594679592206802, 82.54999999999999716, -82.89895571708333932 ) ) ;
#33736 = CARTESIAN_POINT ( 'NONE',  ( 80.44329752326743233, -21.47944369576872603, 8.225625303283912615 ) ) ;
#33737 = CARTESIAN_POINT ( 'NONE',  ( 115.8259672271617120, -31.73094390465656289, 184.2401262212665642 ) ) ;
#33739 = EDGE_CURVE ( 'NONE', #40033, #34033, #76771, .T. ) ;
#33738 = DIRECTION ( 'NONE',  ( -1.000000000000000078E-15, 1.000000000000000083E-30, 1.000000000000000000 ) ) ;
#33740 = DIRECTION ( 'NONE',  ( 0.000000000000000000, 1.000000000000000000, 0.000000000000000000 ) ) ;
#33741 = ORIENTED_EDGE ( 'NONE', *, *, #47725, .T. ) ;
#33742 = CARTESIAN_POINT ( 'NONE',  ( 101.9929316774952497, -45.44564633532985454, 62.15639494301799317 ) ) ;
#33743 = CARTESIAN_POINT ( 'NONE',  ( 102.2371489609593880, -45.96874152625851906, 212.1927681330539599 ) ) ;
#33744 = ORIENTED_EDGE ( 'NONE', *, *, #7693, .F. ) ;
#33745 = AXIS2_PLACEMENT_3D ( 'NONE', #82658, #20415, #75818 ) ;
#33746 = CARTESIAN_POINT ( 'NONE',  ( -12.37524867428841091, 79.66590588004265783, 117.9083757119989428 ) ) ;
#33747 = CARTESIAN_POINT ( 'NONE',  ( -98.60478223830740774, 120.6499999999999915, -1.074461880482445986E-12 ) ) ;
#33748 = DIRECTION ( 'NONE',  ( 1.000000000000000000, 0.000000000000000000, 6.878358445406130340E-15 ) ) ;
#33749 = CARTESIAN_POINT ( 'NONE',  ( 107.4895849179006575, -45.99858499349326735, 40.43094751244896656 ) ) ;
#33750 = CARTESIAN_POINT ( 'NONE',  ( 114.5431187036783740, -28.56067750227894564, 150.4746728949579619 ) ) ;
#33751 = CARTESIAN_POINT ( 'NONE',  ( 41.56648329127399677, 0.2215528400590013880, 256.8086252759120498 ) ) ;
#33752 = ORIENTED_EDGE ( 'NONE', *, *, #68372, .F. ) ;
#33753 = EDGE_CURVE ( 'NONE', #78550, #49825, #39880, .T. ) ;
#33754 = CARTESIAN_POINT ( 'NONE',  ( 107.0667039024470313, -104.2784471599409528, 23.21780685541800082 ) ) ;
#33755 = CARTESIAN_POINT ( 'NONE',  ( 104.1327126252334665, -46.37477890040964468, 67.34360547614434722 ) ) ;
#33756 = ORIENTED_EDGE ( 'NONE', *, *, #37285, .F. ) ;
#33757 = ORIENTED_EDGE ( 'NONE', *, *, #40449, .T. ) ;
#33758 = EDGE_CURVE ( 'NONE', #34233, #26191, #82263, .T. ) ;
#33759 = CARTESIAN_POINT ( 'NONE',  ( 97.81168895331838087, -40.51742574516882200, 287.6356252759109680 ) ) ;
#33760 = ORIENTED_EDGE ( 'NONE', *, *, #87447, .T. ) ;
#33761 = ORIENTED_EDGE ( 'NONE', *, *, #21302, .T. ) ;
#33762 = CARTESIAN_POINT ( 'NONE',  ( 140.0667039024470455, -118.2784471599408960, 222.2178068554179902 ) ) ;
#33763 = CARTESIAN_POINT ( 'NONE',  ( 113.5850730991778619, -42.29362625859309333, 62.68670554236294379 ) ) ;
#33764 = CARTESIAN_POINT ( 'NONE',  ( 96.75080816152406271, -34.86525579675927844, 241.1841967044819626 ) ) ;
#33765 = CARTESIAN_POINT ( 'NONE',  ( 97.42226921825827901, -40.63044708855872500, 206.6327681330539860 ) ) ;
#33767 = CARTESIAN_POINT ( 'NONE',  ( 117.4903696573863385, -37.28369426754698424, 14.78419670448294454 ) ) ;
#33766 = CARTESIAN_POINT ( 'NONE',  ( 162.8913605087226415, -31.76306994223245539, 237.4678068554150059 ) ) ;
#33768 = DIRECTION ( 'NONE',  ( 0.000000000000000000, 0.000000000000000000, -1.000000000000000000 ) ) ;
#33769 = CARTESIAN_POINT ( 'NONE',  ( 131.0667039024480403, -42.97311385573999587, 207.5838068554170377 ) ) ;
#33770 = EDGE_LOOP ( 'NONE', ( #64522, #48801, #25662, #1350 ) ) ;
#33771 = CARTESIAN_POINT ( 'NONE',  ( 110.8343066518040416, -26.26926122352943338, 99.80133956162498521 ) ) ;
#33772 = VECTOR ( 'NONE', #70778, 1000.000000000000000 ) ;
#33773 = CARTESIAN_POINT ( 'NONE',  ( 103.9442172157761917, -47.38141121271982570, 62.33753003781600199 ) ) ;
#33774 = CARTESIAN_POINT ( 'NONE',  ( 106.1344186357298867, -47.79037565197016590, 262.4975300378158067 ) ) ;
#33775 = EDGE_LOOP ( 'NONE', ( #2907, #29785, #66610, #75197 ) ) ;
#33776 = CARTESIAN_POINT ( 'NONE',  ( 97.09604340039788895, -41.50117806558871791, 216.6937205140059461 ) ) ;
#33777 = DIRECTION ( 'NONE',  ( 1.000000000000000078E-15, -1.000000000000000083E-30, -1.000000000000000000 ) ) ;
#33778 = FILL_AREA_STYLE ('',( #88760 ) ) ;
#33779 = CARTESIAN_POINT ( 'NONE',  ( 115.7825283181106926, -41.80329352439114388, 24.40636741810707733 ) ) ;
#33780 = CARTESIAN_POINT ( 'NONE',  ( 113.5891433990094157, -44.41776597164441398, 29.13712086416463976 ) ) ;
#33781 = ADVANCED_FACE ( 'NONE', ( #20021 ), #21364, .T. ) ;
#33783 = PLANE ( 'NONE',  #58689 ) ;
#33782 = CARTESIAN_POINT ( 'NONE',  ( 111.5783628878732401, -44.33946045148141479, 277.6356252759111953 ) ) ;
#33784 = CARTESIAN_POINT ( 'NONE',  ( 117.0608881454332675, -38.08051539367706084, 174.7189536622046546 ) ) ;
#33785 = EDGE_CURVE ( 'NONE', #32749, #77919, #54451, .T. ) ;
#33786 = CARTESIAN_POINT ( 'NONE',  ( 106.5656518807525117, -24.23945688555024702, 323.2548426863285727 ) ) ;
#33787 = AXIS2_PLACEMENT_3D ( 'NONE', #3851, #31544, #59247 ) ;
#33788 = FACE_OUTER_BOUND ( 'NONE', #54666, .T. ) ;
#33789 = EDGE_CURVE ( 'NONE', #62770, #22460, #82067, .T. ) ;
#33790 = CARTESIAN_POINT ( 'NONE',  ( 47.62500000000000000, 69.84999999999999432, 283.4005000000000223 ) ) ;
#33791 = CARTESIAN_POINT ( 'NONE',  ( 109.7166342287432315, -26.99862646155922263, 39.86461898627592149 ) ) ;
#33792 = CARTESIAN_POINT ( 'NONE',  ( 100.9546728209955688, -28.70702572003537512, 76.59395860829201297 ) ) ;
#33794 = ORIENTED_EDGE ( 'NONE', *, *, #36461, .T. ) ;
#33793 = FACE_OUTER_BOUND ( 'NONE', #4823, .T. ) ;
#33795 = ADVANCED_FACE ( 'NONE', ( #7290 ), #77228, .F. ) ;
#33796 = PLANE ( 'NONE',  #17644 ) ;
#33797 = CARTESIAN_POINT ( 'NONE',  ( 97.45268567403179816, -40.90835349962023315, 231.6527681330539679 ) ) ;
#33798 = CARTESIAN_POINT ( 'NONE',  ( 109.5084879329568679, -46.86449036543412205, 128.7641967044819751 ) ) ;
#33799 = CARTESIAN_POINT ( 'NONE',  ( 100.2197142693901668, -28.81018370247272742, 256.6441967044821695 ) ) ;
#33800 = CARTESIAN_POINT ( 'NONE',  ( 113.2454987156834108, -28.75867295938290624, 154.5522919407626716 ) ) ;
#33801 = CARTESIAN_POINT ( 'NONE',  ( 186.6899999999999977, 59.08750000000000568, -38.10000000000000142 ) ) ;
#33803 = DIRECTION ( 'NONE',  ( 1.907762142705490052E-15, 7.167082501179359715E-16, -1.000000000000000000 ) ) ;
#33802 = CARTESIAN_POINT ( 'NONE',  ( -7.661254700127833495, 82.54999999999999716, 320.6630000000000109 ) ) ;
#33804 = LINE ( 'NONE', #33357, #20409 ) ;
#33805 = CARTESIAN_POINT ( 'NONE',  ( 132.1570028294930523, -20.71057579844040930, 2.232988688760512375 ) ) ;
#33806 = EDGE_CURVE ( 'NONE', #52459, #71638, #49038, .T. ) ;
#33807 = CIRCLE ( 'NONE', #45395, 32.50000000000001421 ) ;
#33808 = EDGE_LOOP ( 'NONE', ( #80748, #55777, #59944, #84979 ) ) ;
#33809 = ORIENTED_EDGE ( 'NONE', *, *, #18736, .T. ) ;
#33810 = EDGE_CURVE ( 'NONE', #59070, #51539, #13207, .T. ) ;
#33811 = CARTESIAN_POINT ( 'NONE',  ( 105.6324958909751075, -46.33196107771311745, 146.8809912566479738 ) ) ;
#33813 = ORIENTED_EDGE ( 'NONE', *, *, #74509, .T. ) ;
#33812 = CARTESIAN_POINT ( 'NONE',  ( 0.000000000000000000, 184.0000000000000000, 85.23828826961327820 ) ) ;
#33814 = AXIS2_PLACEMENT_3D ( 'NONE', #85238, #71598, #57501 ) ;
#33815 = CARTESIAN_POINT ( 'NONE',  ( 115.8253432708642094, -31.72986461983916939, 89.23953976385652709 ) ) ;
#33816 = CARTESIAN_POINT ( 'NONE',  ( 116.8835868046512587, -40.17228670562622739, 129.5584824187679658 ) ) ;
#33817 = LINE ( 'NONE', #631, #48244 ) ;
#33818 = B_SPLINE_CURVE_WITH_KNOTS ( 'NONE', 3,
 ( #43423, #63438, #62982, #35272, #760, #1224, #28928, #28461, #21673, #49347, #77078, #22126, #6680, #15304, #42971, #34378, #62086, #29824 ),
 .UNSPECIFIED., .F., .F.,
 ( 4, 2, 2, 2, 2, 2, 2, 2, 4 ),
 ( 0.000000000000000000, 0.06250000002945982347, 0.1250000000589196469, 0.1875000000883794704, 0.2500000001178392939, 0.3125000001472991173, 0.3750000001767589408, 0.4375000002062187643, 0.5000000002356785878 ),
 .UNSPECIFIED. ) ;
#33819 = CARTESIAN_POINT ( 'NONE',  ( 70.63919639214310564, 100.5999999999999659, 56.85413200336923012 ) ) ;
#33820 = CARTESIAN_POINT ( 'NONE',  ( 51.06670390244899238, -32.29483332968430886, 342.9256252759119548 ) ) ;
#33821 = LINE ( 'NONE', #88359, #4840 ) ;
#33822 = CARTESIAN_POINT ( 'NONE',  ( 96.07333748454163924, -35.06730156692549372, 71.20705384733993526 ) ) ;
#33823 = ORIENTED_EDGE ( 'NONE', *, *, #15858, .F. ) ;
#33824 = ORIENTED_EDGE ( 'NONE', *, *, #4259, .T. ) ;
#33825 = EDGE_LOOP ( 'NONE', ( #69288, #33192, #61622, #40114, #58972, #58919 ) ) ;
#33826 = VECTOR ( 'NONE', #18392, 999.9999999999998863 ) ;
#33827 = LINE ( 'NONE', #67001, #34174 ) ;
#33829 = DIRECTION ( 'NONE',  ( -0.7071067812160279908, 0.7071067811570671546, -6.612322856135836109E-17 ) ) ;
#33828 = CARTESIAN_POINT ( 'NONE',  ( 102.0969121991173125, -45.15362633196975395, 158.1527681330539963 ) ) ;
#33830 = CARTESIAN_POINT ( 'NONE',  ( 107.0664832912739968, -36.72944715994100306, 287.6356252759109680 ) ) ;
#33831 = CARTESIAN_POINT ( 'NONE',  ( 0.000000000000000000, 82.54999999999999716, 92.46299999999996544 ) ) ;
#33832 = CARTESIAN_POINT ( 'NONE',  ( 168.3664380525668491, -48.62818131005517586, 129.9678068554150059 ) ) ;
#33833 = CARTESIAN_POINT ( 'NONE',  ( 83.24642779537398951, 95.23005795263748041, 84.41404664249461121 ) ) ;
#33834 = CARTESIAN_POINT ( 'NONE',  ( 123.6837132603319560, -53.34645651782485487, 229.5838068554170093 ) ) ;
#33835 = CARTESIAN_POINT ( 'NONE',  ( 109.7644292386350457, -47.42453529627131559, 92.78514908543495210 ) ) ;
#33836 = ORIENTED_EDGE ( 'NONE', *, *, #5420, .T. ) ;
#33837 = VERTEX_POINT ( 'NONE', #27723 ) ;
#33838 = ORIENTED_EDGE ( 'NONE', *, *, #28361, .T. ) ;
#33839 = CARTESIAN_POINT ( 'NONE',  ( 25.56670390244734747, -42.82844715994178131, 139.7178068554150627 ) ) ;
#33840 = DIRECTION ( 'NONE',  ( 0.000000000000000000, 0.000000000000000000, -1.000000000000000000 ) ) ;
#33842 = EDGE_CURVE ( 'NONE', #43699, #79942, #55847, .T. ) ;
#33841 = FACE_OUTER_BOUND ( 'NONE', #43919, .T. ) ;
#33843 = CARTESIAN_POINT ( 'NONE',  ( 99.78156907347540994, -40.47280301881529851, 194.5223760838769920 ) ) ;
#33844 = VECTOR ( 'NONE', #23535, 1000.000000000000000 ) ;
#33845 = AXIS2_PLACEMENT_3D ( 'NONE', #89636, #84171, #9203 ) ;
#33846 = CARTESIAN_POINT ( 'NONE',  ( -29.99999999999996092, 172.0000000000000000, 183.8826257785461280 ) ) ;
#33847 = ORIENTED_EDGE ( 'NONE', *, *, #11179, .F. ) ;
#33849 = ORIENTED_EDGE ( 'NONE', *, *, #33244, .T. ) ;
#33848 = EDGE_LOOP ( 'NONE', ( #58763, #14446, #5574, #78457 ) ) ;
#33850 = PLANE ( 'NONE',  #67091 ) ;
#33851 = CYLINDRICAL_SURFACE ( 'NONE', #57854, 88.90000000000000568 ) ;
#33852 = ORIENTED_EDGE ( 'NONE', *, *, #48411, .T. ) ;
#33853 = ORIENTED_EDGE ( 'NONE', *, *, #7241, .F. ) ;
#33854 = CARTESIAN_POINT ( 'NONE',  ( 77.76062680957342366, -20.22815166920278429, 7.286367513305838095 ) ) ;
#33855 = CARTESIAN_POINT ( 'NONE',  ( 115.1079044709731676, -40.52387399376650734, 224.9072975916109840 ) ) ;
#33856 = LINE ( 'NONE', #28384, #79880 ) ;
#33857 = CARTESIAN_POINT ( 'NONE',  ( -112.8531487064678913, 68.31472480788332291, 65.64348722659526914 ) ) ;
#33858 = EDGE_LOOP ( 'NONE', ( #20033, #64483, #44105, #52212 ) ) ;
#33859 = ORIENTED_EDGE ( 'NONE', *, *, #26501, .F. ) ;
#33860 = EDGE_CURVE ( 'NONE', #31965, #76782, #83597, .T. ) ;
#33861 = DIRECTION ( 'NONE',  ( 2.900000000000000265E-14, -2.000000000000000155E-15, 1.000000000000000000 ) ) ;
#33862 = AXIS2_PLACEMENT_3D ( 'NONE', #38060, #50789, #17619 ) ;
#33863 = ORIENTED_EDGE ( 'NONE', *, *, #18983, .T. ) ;
#33864 = ORIENTED_EDGE ( 'NONE', *, *, #30684, .T. ) ;
#33865 = CARTESIAN_POINT ( 'NONE',  ( 111.2517653011026226, -44.30469234039772886, 250.7842808457816375 ) ) ;
#33867 = CARTESIAN_POINT ( 'NONE',  ( 95.65096329713743728, -33.45531905120653704, 141.1041967044829732 ) ) ;
#33866 = VECTOR ( 'NONE', #16849, 1000.000000000000000 ) ;
#33868 = CARTESIAN_POINT ( 'NONE',  ( 103.9639062230918825, -47.31423993612443724, 62.33753003781600199 ) ) ;
#33869 = CARTESIAN_POINT ( 'NONE',  ( 105.3771735659821616, -28.36731242524880159, 249.5838068554170661 ) ) ;
#33870 = DIRECTION ( 'NONE',  ( 0.000000000000000000, 1.000000000000000000, 0.000000000000000000 ) ) ;
#33871 = CARTESIAN_POINT ( 'NONE',  ( 108.0719115850922236, -25.31448365300273551, 321.8079557531246451 ) ) ;
#33872 = CARTESIAN_POINT ( 'NONE',  ( 96.74313874428034410, -35.27650366090898615, 177.2156252759109805 ) ) ;
#33873 = DIRECTION ( 'NONE',  ( 0.000000000000000000, 0.000000000000000000, 1.000000000000000000 ) ) ;
#33874 = ORIENTED_EDGE ( 'NONE', *, *, #84353, .T. ) ;
#33875 = DIRECTION ( 'NONE',  ( 0.000000000000000000, 0.000000000000000000, 1.000000000000000000 ) ) ;
#33876 = VERTEX_POINT ( 'NONE', #26818 ) ;
#33877 = ORIENTED_EDGE ( 'NONE', *, *, #70721, .T. ) ;
#33878 = DIRECTION ( 'NONE',  ( 0.000000000000000000, 0.000000000000000000, 1.000000000000000000 ) ) ;
#33879 = ORIENTED_EDGE ( 'NONE', *, *, #63660, .F. ) ;
#33880 = AXIS2_PLACEMENT_3D ( 'NONE', #2925, #22936, #78796 ) ;
#33881 = DIRECTION ( 'NONE',  ( 1.000000000000000000, 1.000000000000000078E-15, 0.000000000000000000 ) ) ;
#33882 = CARTESIAN_POINT ( 'NONE',  ( 97.22546204445637841, -31.69621874537715556, 95.96229194257799122 ) ) ;
#33883 = CARTESIAN_POINT ( 'NONE',  ( -10.19015296090227274, 74.96840031402189197, 130.1578716281692607 ) ) ;
#33884 = CARTESIAN_POINT ( 'NONE',  ( 136.5887892044395926, -35.63370978841413006, 7.053538376721769865 ) ) ;
#33885 = DIRECTION ( 'NONE',  ( 1.000000000000000078E-15, -1.000000000000000083E-30, -1.000000000000000000 ) ) ;
#33888 = CARTESIAN_POINT ( 'NONE',  ( 106.3035372762157493, -47.10473409126645805, 218.5184824187679453 ) ) ;
#33887 = DIRECTION ( 'NONE',  ( 1.000000000000000078E-15, 1.000000000000000083E-30, -1.000000000000000000 ) ) ;
#33886 = DIRECTION ( 'NONE',  ( 1.000000000000000078E-15, -1.000000000000000083E-30, -1.000000000000000000 ) ) ;
#33889 = DIRECTION ( 'NONE',  ( 0.000000000000000000, 1.000000000000000000, 1.056314557550181068E-14 ) ) ;
#33890 = EDGE_CURVE ( 'NONE', #12535, #3336, #23, .T. ) ;
#33891 = CARTESIAN_POINT ( 'NONE',  ( 0.000000000000000000, 60.82030000000000314, 259.9944000000000415 ) ) ;
#33892 = VERTEX_POINT ( 'NONE', #48142 ) ;
#33893 = LINE ( 'NONE', #18927, #39668 ) ;
#33894 = ADVANCED_FACE ( 'NONE', ( #75877, #56303 ), #83157, .T. ) ;
#33895 = DIRECTION ( 'NONE',  ( -0.5000000000000008882, 0.000000000000000000, 0.8660254037844382635 ) ) ;
#33896 = EDGE_CURVE ( 'NONE', #62011, #49381, #66079, .T. ) ;
#33897 = DIRECTION ( 'NONE',  ( 0.000000000000000000, 0.000000000000000000, -1.000000000000000000 ) ) ;
#33898 = DIRECTION ( 'NONE',  ( 0.000000000000000000, 0.000000000000000000, -1.000000000000000000 ) ) ;
#33900 = ORIENTED_EDGE ( 'NONE', *, *, #88928, .T. ) ;
#33899 = CARTESIAN_POINT ( 'NONE',  ( 96.73248008985177648, -40.78176272772311250, 246.6118157521009664 ) ) ;
#33901 = EDGE_CURVE ( 'NONE', #77829, #72800, #69060, .T. ) ;
#33902 = CARTESIAN_POINT ( 'NONE',  ( 119.0814029968458811, -31.76540601701525901, 292.6356252759106837 ) ) ;
#33903 = CARTESIAN_POINT ( 'NONE',  ( 100.2329966457367334, -45.44659500335379221, 273.0594347997205773 ) ) ;
#33904 = CARTESIAN_POINT ( 'NONE',  ( 98.05313438099307177, -42.12366292992533801, 157.7556252759109725 ) ) ;
#33905 = CARTESIAN_POINT ( 'NONE',  ( 104.4899543326152127, -26.97880761473700417, 31.28145861894176960 ) ) ;
#33906 = FACE_OUTER_BOUND ( 'NONE', #58369, .T. ) ;
#33908 = DIRECTION ( 'NONE',  ( -1.000000000000000000, -4.299999999999999979E-14, -1.000000000000000078E-15 ) ) ;
#33907 = CARTESIAN_POINT ( 'NONE',  ( 47.62500000000000000, 94.53880000000000905, 254.7937499999999886 ) ) ;
#33909 = CARTESIAN_POINT ( 'NONE',  ( 115.0889047299720431, -30.61763668903771674, 189.3439586083947290 ) ) ;
#33910 = LINE ( 'NONE', #40272, #72676 ) ;
#33911 = ORIENTED_EDGE ( 'NONE', *, *, #21719, .T. ) ;
#33912 = CIRCLE ( 'NONE', #84707, 39.10000000000005116 ) ;
#33913 = VECTOR ( 'NONE', #33098, 1000.000000000000000 ) ;
#33914 = ORIENTED_EDGE ( 'NONE', *, *, #83532, .T. ) ;
#33915 = ORIENTED_EDGE ( 'NONE', *, *, #61620, .F. ) ;
#33916 = EDGE_CURVE ( 'NONE', #25068, #45031, #41778, .T. ) ;
#33917 = VERTEX_POINT ( 'NONE', #78589 ) ;
#33918 = CARTESIAN_POINT ( 'NONE',  ( 93.91125933621934507, -111.8737466215625744, -11.78219314458178779 ) ) ;
#33919 = CARTESIAN_POINT ( 'NONE',  ( 101.3960830062750631, -28.00733582429768376, 21.53562527591096298 ) ) ;
#33920 = LINE ( 'NONE', #32571, #71623 ) ;
#33921 = CARTESIAN_POINT ( 'NONE',  ( 145.4224990655192187, -139.2862363000336074, 245.9798482249633764 ) ) ;
#33922 = CARTESIAN_POINT ( 'NONE',  ( 20.56670390244743984, -48.82844715994200158, 180.4678068554150911 ) ) ;
#33923 = CARTESIAN_POINT ( 'NONE',  ( 110.3936857311090023, -28.86269079874493571, 244.1809912566479568 ) ) ;
#33924 = ORIENTED_EDGE ( 'NONE', *, *, #78426, .F. ) ;
#33925 = ORIENTED_EDGE ( 'NONE', *, *, #78216, .F. ) ;
#33926 = ORIENTED_EDGE ( 'NONE', *, *, #25159, .T. ) ;
#33927 = VECTOR ( 'NONE', #75850, 1000.000000000000000 ) ;
#33928 = CARTESIAN_POINT ( 'NONE',  ( 133.5842039024480528, -51.22944715994092491, 231.5838068554170093 ) ) ;
#33929 = VECTOR ( 'NONE', #58223, 1000.000000000000000 ) ;
#33930 = CARTESIAN_POINT ( 'NONE',  ( 108.3335946874162374, -46.73484295057657789, 102.6771468619035517 ) ) ;
#33931 = LINE ( 'NONE', #61628, #31017 ) ;
#33932 = LINE ( 'NONE', #41630, #46033 ) ;
#33933 = CARTESIAN_POINT ( 'NONE',  ( -185.9961463128564958, 20.32000000000000028, -3.174999999999514877 ) ) ;
#33934 = AXIS2_PLACEMENT_3D ( 'NONE', #78878, #30705, #65662 ) ;
#33935 = CARTESIAN_POINT ( 'NONE',  ( 172.5664832912729878, -27.82844715994070484, 255.9256252759120116 ) ) ;
#33936 = CARTESIAN_POINT ( 'NONE',  ( 116.8470136369842720, -36.79772195930841150, 263.8213395616257912 ) ) ;
#33937 = DIRECTION ( 'NONE',  ( 0.000000000000000000, 0.000000000000000000, -1.000000000000000000 ) ) ;
#33938 = EDGE_LOOP ( 'NONE', ( #9095, #89325, #33168, #26753 ) ) ;
#33939 = CARTESIAN_POINT ( 'NONE',  ( 0.000000000000000000, 82.54999999999999716, 92.46299999999996544 ) ) ;
#33941 = EDGE_CURVE ( 'NONE', #81819, #50094, #48622, .T. ) ;
#33940 = LINE ( 'NONE', #20337, #82949 ) ;
#33942 = CARTESIAN_POINT ( 'NONE',  ( 115.1095529034481331, -33.53414494269306800, 96.95761417911496949 ) ) ;
#33943 = ADVANCED_FACE ( 'NONE', ( #77675 ), #44467, .F. ) ;
#33944 = LINE ( 'NONE', #39859, #4046 ) ;
#33945 = CARTESIAN_POINT ( 'NONE',  ( 104.4899544499527053, -26.97880758519347211, 45.28145860940914957 ) ) ;
#33946 = ORIENTED_EDGE ( 'NONE', *, *, #54154, .F. ) ;
#33947 = CARTESIAN_POINT ( 'NONE',  ( 77.85525873416803222, -35.08426237656984625, 7.378668740741173515 ) ) ;
#33948 = ORIENTED_EDGE ( 'NONE', *, *, #58355, .F. ) ;
#33949 = CARTESIAN_POINT ( 'NONE',  ( 107.6530059321349455, -47.12789624220987150, 152.6213395616249500 ) ) ;
#33950 = VERTEX_POINT ( 'NONE', #44019 ) ;
#33951 = CARTESIAN_POINT ( 'NONE',  ( 109.6430121650047909, -46.48008672573308786, 68.78145861206645861 ) ) ;
#33952 = CARTESIAN_POINT ( 'NONE',  ( 112.9486100676287208, -29.40298074535265727, 115.9577737820869601 ) ) ;
#33953 = DIRECTION ( 'NONE',  ( 1.000000000000000078E-15, -1.000000000000000083E-30, -1.000000000000000000 ) ) ;
#33954 = CARTESIAN_POINT ( 'NONE',  ( 150.5667039024485234, -47.82844715993594065, 180.4678068554149775 ) ) ;
#33955 = CARTESIAN_POINT ( 'NONE',  ( 116.1426067713721437, -29.07136428874337142, 70.38419670448192278 ) ) ;
#33956 = AXIS2_PLACEMENT_3D ( 'NONE', #56592, #63877, #88556 ) ;
#33957 = CARTESIAN_POINT ( 'NONE',  ( -47.18030668273772221, 100.5999999999999659, 75.34738655934135920 ) ) ;
#33958 = ORIENTED_EDGE ( 'NONE', *, *, #50558, .F. ) ;
#33959 = EDGE_CURVE ( 'NONE', #69055, #11886, #79022, .T. ) ;
#33960 = DIRECTION ( 'NONE',  ( 4.299999999999999979E-14, -1.000000000000000000, 4.400000000000000367E-29 ) ) ;
#33961 = VECTOR ( 'NONE', #6856, 1000.000000000000000 ) ;
#33962 = ORIENTED_EDGE ( 'NONE', *, *, #54665, .F. ) ;
#33963 = VERTEX_POINT ( 'NONE', #36784 ) ;
#33964 = DIRECTION ( 'NONE',  ( 0.000000000000000000, -1.000000000000000000, 0.000000000000000000 ) ) ;
#33965 = VERTEX_POINT ( 'NONE', #71757 ) ;
#33966 = CARTESIAN_POINT ( 'NONE',  ( 112.1213531720970309, -45.14146623880455422, 238.0070538473399324 ) ) ;
#33967 = CARTESIAN_POINT ( 'NONE',  ( 98.07189402449054683, -42.11243585264244160, 157.7556252759109725 ) ) ;
#33968 = CARTESIAN_POINT ( 'NONE',  ( 2.884119045937113768, 70.17489121805367347, -118.5216098345816960 ) ) ;
#33969 = CARTESIAN_POINT ( 'NONE',  ( 97.07207206070478378, -35.37844118697538676, 142.2189586082815822 ) ) ;
#33970 = CARTESIAN_POINT ( 'NONE',  ( 103.3624612311685809, -47.14358183654965018, 98.31657765686297523 ) ) ;
#33971 = CARTESIAN_POINT ( 'NONE',  ( -3.175000000000109956, 24.56180297284579694, -31.75000000000000000 ) ) ;
#33972 = ORIENTED_EDGE ( 'NONE', *, *, #76668, .T. ) ;
#33973 = CARTESIAN_POINT ( 'NONE',  ( 107.0667039024470171, -89.08784823670032438, -11.78219314458248057 ) ) ;
#33974 = EDGE_CURVE ( 'NONE', #62958, #24524, #37058, .T. ) ;
#33975 = LINE ( 'NONE', #48475, #85402 ) ;
#33976 = ORIENTED_EDGE ( 'NONE', *, *, #63864, .F. ) ;
#33977 = CARTESIAN_POINT ( 'NONE',  ( 123.6837132603318565, -20.11243780205705534, 229.5838068554170093 ) ) ;
#33978 = CIRCLE ( 'NONE', #60098, 5.041900000000001825 ) ;
#33979 = CIRCLE ( 'NONE', #3525, 2.117000000000000881 ) ;
#33980 = CARTESIAN_POINT ( 'NONE',  ( 176.7738106835050758, -48.62134037887501847, 300.4678068554149490 ) ) ;
#33981 = CARTESIAN_POINT ( 'NONE',  ( 97.79211192542227593, -40.52543860420435351, 11.63562527591094309 ) ) ;
#33982 = CARTESIAN_POINT ( 'NONE',  ( -187.8075999999999794, 20.32000000000000028, -9.525000000000000355 ) ) ;
#33983 = CIRCLE ( 'NONE', #73146, 2.500000000000002220 ) ;
#33984 = CARTESIAN_POINT ( 'NONE',  ( 154.4532655810166091, -72.54279768053238797, 542.9756252759101471 ) ) ;
#33985 = CARTESIAN_POINT ( 'NONE',  ( 113.1806887538930795, -44.75007787370592638, 93.09499265662630307 ) ) ;
#33986 = CARTESIAN_POINT ( 'NONE',  ( 110.6828660728576637, -28.42687563832788200, 284.1600388756959887 ) ) ;
#33988 = CARTESIAN_POINT ( 'NONE',  ( 98.16825066461163374, -43.24752039522706326, 102.8175300378159847 ) ) ;
#33987 = FACE_OUTER_BOUND ( 'NONE', #16127, .T. ) ;
#33989 = CARTESIAN_POINT ( 'NONE',  ( 142.8679068202682458, 10.65431904611001634, 396.9756252759102040 ) ) ;
#33990 = CARTESIAN_POINT ( 'NONE',  ( 105.7147172347987407, -24.90567422487873017, 160.1670538473389627 ) ) ;
#33991 = CARTESIAN_POINT ( 'NONE',  ( -492.0614999999999668, 14.28749999999982201, 95.25000000000000000 ) ) ;
#33992 = ORIENTED_EDGE ( 'NONE', *, *, #70618, .T. ) ;
#33993 = CARTESIAN_POINT ( 'NONE',  ( 3.944304526105059924E-28, 95.25000000000000000, 130.5560000000000116 ) ) ;
#33994 = AXIS2_PLACEMENT_3D ( 'NONE', #59681, #66508, #79722 ) ;
#33995 = VECTOR ( 'NONE', #43755, 1000.000000000000000 ) ;
#33996 = FACE_BOUND ( 'NONE', #51786, .T. ) ;
#33997 = DIRECTION ( 'NONE',  ( -1.000000000000000000, -1.000000000000000078E-15, -1.000000000000000078E-15 ) ) ;
#33999 = EDGE_LOOP ( 'NONE', ( #79968, #75068, #84505, #31493, #29753, #56640 ) ) ;
#33998 = EDGE_CURVE ( 'NONE', #88268, #76542, #85407, .T. ) ;
#34000 = DIRECTION ( 'NONE',  ( 0.000000000000000000, 0.000000000000000000, 1.000000000000000000 ) ) ;
#34002 = EDGE_LOOP ( 'NONE', ( #7051, #26374, #4835, #61303, #61711, #68831, #9600, #89405 ) ) ;
#34001 = CARTESIAN_POINT ( 'NONE',  ( 97.96866571142417968, -30.36999819975766357, 160.8289586092449497 ) ) ;
#34003 = DIRECTION ( 'NONE',  ( 0.000000000000000000, 0.000000000000000000, 1.000000000000000000 ) ) ;
#34004 = CARTESIAN_POINT ( 'NONE',  ( -130.0134714785365304, 87.03008507238369873, 11.89083589963811072 ) ) ;
#34005 = DIRECTION ( 'NONE',  ( 0.000000000000000000, 0.000000000000000000, 1.000000000000000000 ) ) ;
#34006 = CARTESIAN_POINT ( 'NONE',  ( 107.0667039024469886, -70.87844715994094713, 133.2178068554180186 ) ) ;
#34007 = ORIENTED_EDGE ( 'NONE', *, *, #74300, .T. ) ;
#34008 = ITEM_DEFINED_TRANSFORMATION ( 'NONE', 'NONE', #87043,  #50656 ) ;
#34009 = ORIENTED_EDGE ( 'NONE', *, *, #77471, .T. ) ;
#34010 = ORIENTED_EDGE ( 'NONE', *, *, #25100, .F. ) ;
#34011 = EDGE_CURVE ( 'NONE', #58534, #1672, #57325, .T. ) ;
#34012 = VERTEX_POINT ( 'NONE', #50393 ) ;
#34013 = CARTESIAN_POINT ( 'NONE',  ( 51.34673845256598668, -36.02818131005800950, -5.074374724088000832 ) ) ;
#34014 = CARTESIAN_POINT ( 'NONE',  ( 111.9958537464713970, -27.96271286943853696, 249.6692924242317417 ) ) ;
#34015 = ADVANCED_FACE ( 'NONE', ( #49943 ), #85845, .T. ) ;
#34016 = CARTESIAN_POINT ( 'NONE',  ( 72.96458098368650269, 117.4749999999999943, 78.00648098368728256 ) ) ;
#34018 = CARTESIAN_POINT ( 'NONE',  ( 45.66030316258350297, 82.54999999999999716, 346.9005000000000223 ) ) ;
#34017 = DIRECTION ( 'NONE',  ( -4.299999999999999979E-14, 1.000000000000000000, -4.400000000000000367E-29 ) ) ;
#34019 = LINE ( 'NONE', #28553, #10917 ) ;
#34020 = EDGE_LOOP ( 'NONE', ( #57766, #80262, #77792, #88453 ) ) ;
#34021 = CIRCLE ( 'NONE', #79056, 4.749999999999976907 ) ;
#34022 = ORIENTED_EDGE ( 'NONE', *, *, #20701, .F. ) ;
#34023 = DIRECTION ( 'NONE',  ( 0.000000000000000000, 0.000000000000000000, -1.000000000000000000 ) ) ;
#34024 = AXIS2_PLACEMENT_3D ( 'NONE', #11784, #4964, #39917 ) ;
#34025 = DIRECTION ( 'NONE',  ( 0.000000000000000000, 0.000000000000000000, 1.000000000000000000 ) ) ;
#34026 = CARTESIAN_POINT ( 'NONE',  ( 101.2327472597882263, -44.62129728587211730, 253.0699109901961492 ) ) ;
#34027 = CARTESIAN_POINT ( 'NONE',  ( 1.598849875094819542E-14, 44.45000000000000284, -130.5560000000000116 ) ) ;
#34028 = CARTESIAN_POINT ( 'NONE',  ( 100.7170190823677132, -45.85612711270987774, 83.09276813305294240 ) ) ;
#34029 = CARTESIAN_POINT ( 'NONE',  ( 0.000000000000000000, 82.54999999999999716, -179.8908777604655143 ) ) ;
#34030 = CARTESIAN_POINT ( 'NONE',  ( 103.4635681255033433, -27.40063510583546957, 21.36976600060490838 ) ) ;
#34031 = ORIENTED_EDGE ( 'NONE', *, *, #16010, .T. ) ;
#34032 = CARTESIAN_POINT ( 'NONE',  ( 76.06670390244796920, -26.72944715994109899, 239.5838068554169809 ) ) ;
#34033 = VERTEX_POINT ( 'NONE', #29971 ) ;
#34034 = VERTEX_POINT ( 'NONE', #16786 ) ;
#34035 = CARTESIAN_POINT ( 'NONE',  ( 107.0667039024470313, -104.2784471599420755, -19.78219314458201694 ) ) ;
#34036 = CARTESIAN_POINT ( 'NONE',  ( 105.4026065362546802, -27.48239143091520020, 271.6377737820876632 ) ) ;
#34037 = LINE ( 'NONE', #62656, #9617 ) ;
#34038 = VECTOR ( 'NONE', #59825, 1000.000000000000000 ) ;
#34039 = AXIS2_PLACEMENT_3D ( 'NONE', #16737, #4889, #79428 ) ;
#34040 = CARTESIAN_POINT ( 'NONE',  ( -117.9189176348423160, 85.83559868056555331, 12.27472195321796278 ) ) ;
#34041 = CIRCLE ( 'NONE', #29728, 2.517499999999998739 ) ;
#34042 = CARTESIAN_POINT ( 'NONE',  ( 97.31584371262773914, -39.30597598611567633, 81.53145860817606660 ) ) ;
#34043 = LINE ( 'NONE', #42205, #67652 ) ;
#34044 = AXIS2_PLACEMENT_3D ( 'NONE', #50538, #57806, #2856 ) ;
#34045 = ORIENTED_EDGE ( 'NONE', *, *, #55087, .T. ) ;
#34046 = FACE_BOUND ( 'NONE', #57229, .T. ) ;
#34047 = AXIS2_PLACEMENT_3D ( 'NONE', #25001, #39065, #66772 ) ;
#34048 = FACE_OUTER_BOUND ( 'NONE', #58288, .T. ) ;
#34049 = ORIENTED_EDGE ( 'NONE', *, *, #303, .F. ) ;
#34050 = CARTESIAN_POINT ( 'NONE',  ( 115.0227918137121037, -43.52084328818016701, 63.26419670448196797 ) ) ;
#34051 = ORIENTED_EDGE ( 'NONE', *, *, #24492, .T. ) ;
#34052 = CARTESIAN_POINT ( 'NONE',  ( 98.59685088459899305, -34.95005064942726136, 258.9918998934010119 ) ) ;
#34053 = FACE_BOUND ( 'NONE', #10363, .T. ) ;
#34054 = CARTESIAN_POINT ( 'NONE',  ( 108.2857792741417882, -47.02760743735412063, 162.6822919425779617 ) ) ;
#34055 = CARTESIAN_POINT ( 'NONE',  ( 23.08506796337472622, 77.94149302405480739, 304.1359325411505097 ) ) ;
#34056 = DIRECTION ( 'NONE',  ( -4.237773401492740281E-14, 1.000000000000000000, 0.000000000000000000 ) ) ;
#34057 = CARTESIAN_POINT ( 'NONE',  ( 75.61066417432020614, 101.5999999999999943, 177.0380000000000109 ) ) ;
#34058 = PLANE ( 'NONE',  #74076 ) ;
#34059 = CARTESIAN_POINT ( 'NONE',  ( 111.1444126100616927, -27.08769046218140986, 240.7584824187679544 ) ) ;
#34060 = CARTESIAN_POINT ( 'NONE',  ( 91.91945768840240305, 86.64222086580514315, -74.87617104506203702 ) ) ;
#34061 = VERTEX_POINT ( 'NONE', #29076 ) ;
#34062 = EDGE_LOOP ( 'NONE', ( #29137, #21853, #16142, #59762 ) ) ;
#34063 = CARTESIAN_POINT ( 'NONE',  ( 107.9492956907162267, -25.66517399690753720, 111.0251490854349754 ) ) ;
#34064 = EDGE_CURVE ( 'NONE', #57667, #54435, #86397, .T. ) ;
#34065 = CARTESIAN_POINT ( 'NONE',  ( 124.6708583049006194, 47.20033540421172802, -38.75675120859585121 ) ) ;
#34066 = ORIENTED_EDGE ( 'NONE', *, *, #60157, .F. ) ;
#34067 = VERTEX_POINT ( 'NONE', #43126 ) ;
#34068 = ORIENTED_EDGE ( 'NONE', *, *, #37668, .F. ) ;
#34069 = EDGE_CURVE ( 'NONE', #76220, #2396, #67505, .T. ) ;
#34070 = LINE ( 'NONE', #61774, #52046 ) ;
#34071 = DIRECTION ( 'NONE',  ( 4.299999999999999979E-14, -1.000000000000000000, 4.400000000000000367E-29 ) ) ;
#34072 = DIRECTION ( 'NONE',  ( 0.7071067811868710917, -0.7071067811862240537, 0.000000000000000000 ) ) ;
#34073 = CARTESIAN_POINT ( 'NONE',  ( -141.3509999999999991, 101.5999999999999943, 141.3509999999999991 ) ) ;
#34074 = CARTESIAN_POINT ( 'NONE',  ( 104.5146602464430714, -28.97587216416100375, 163.1480903695919551 ) ) ;
#34075 = CARTESIAN_POINT ( 'NONE',  ( 106.2251562910655309, -47.77378392694726017, 263.5280062282920994 ) ) ;
#34076 = EDGE_CURVE ( 'NONE', #17700, #38989, #19663, .T. ) ;
#34077 = CARTESIAN_POINT ( 'NONE',  ( 98.58946256649485917, -108.5954344580491835, 2.217806855418142042 ) ) ;
#34078 = ORIENTED_EDGE ( 'NONE', *, *, #32243, .T. ) ;
#34079 = CARTESIAN_POINT ( 'NONE',  ( 130.5150051272323140, 94.82199753261677699, -3.295598630355848879 ) ) ;
#34080 = EDGE_CURVE ( 'NONE', #78334, #15725, #15897, .T. ) ;
#34081 = CARTESIAN_POINT ( 'NONE',  ( 29.56670390244797630, -67.87844715994100397, 300.9178068554150514 ) ) ;
#34082 = VERTEX_POINT ( 'NONE', #1372 ) ;
#34083 = EDGE_LOOP ( 'NONE', ( #40417, #64828, #40779, #21568 ) ) ;
#34084 = ADVANCED_FACE ( 'NONE', ( #56762 ), #22268, .T. ) ;
#34085 = AXIS2_PLACEMENT_3D ( 'NONE', #87437, #39712, #26996 ) ;
#34086 = LINE ( 'NONE', #82278, #19878 ) ;
#34087 = ORIENTED_EDGE ( 'NONE', *, *, #72053, .T. ) ;
#34088 = ORIENTED_EDGE ( 'NONE', *, *, #19731, .T. ) ;
#34089 = DIRECTION ( 'NONE',  ( 0.8571673007021091140, -8.250245410175212261E-16, 0.5150380749100597066 ) ) ;
#34090 = VECTOR ( 'NONE', #7546, 1000.000000000000000 ) ;
#34091 = CARTESIAN_POINT ( 'NONE',  ( -10.33379165269208499, 75.15577250977247559, -130.1465911299492006 ) ) ;
#34092 = ADVANCED_FACE ( 'NONE', ( #31699, #58945, #86683 ), #4900, .F. ) ;
#34093 = CARTESIAN_POINT ( 'NONE',  ( 142.0664832912740394, -56.72944715994099596, -4.824374724088994704 ) ) ;
#34094 = DIRECTION ( 'NONE',  ( 0.000000000000000000, 0.000000000000000000, 1.000000000000000000 ) ) ;
#34095 = CARTESIAN_POINT ( 'NONE',  ( 109.8786884439187759, -28.66423582349726118, 209.2324198280769849 ) ) ;
#34096 = CARTESIAN_POINT ( 'NONE',  ( 96.88405369895032493, -39.16353706000892032, 56.51276813305394597 ) ) ;
#34097 = ORIENTED_EDGE ( 'NONE', *, *, #52196, .T. ) ;
#34098 = DIRECTION ( 'NONE',  ( 3.999999999999999995E-14, -1.000000000000000000, 4.100000000000000342E-29 ) ) ;
#34099 = ORIENTED_EDGE ( 'NONE', *, *, #52082, .F. ) ;
#34100 = DIRECTION ( 'NONE',  ( 0.000000000000000000, 0.000000000000000000, 1.000000000000000000 ) ) ;
#34102 = ORIENTED_EDGE ( 'NONE', *, *, #25891, .F. ) ;
#34101 = EDGE_CURVE ( 'NONE', #55129, #46554, #45750, .T. ) ;
#34103 = LINE ( 'NONE', #27749, #85332 ) ;
#34104 = EDGE_LOOP ( 'NONE', ( #69603, #61441, #59946, #10435 ) ) ;
#34105 = DIRECTION ( 'NONE',  ( -0.000000000000000000, -0.000000000000000000, -1.000000000000000000 ) ) ;
#34106 = CARTESIAN_POINT ( 'NONE',  ( 101.5797435165433598, -139.8917819456133600, 247.5112265945679724 ) ) ;
#34107 = CARTESIAN_POINT ( 'NONE',  ( 116.3743287984549966, -40.51183142128556369, 133.5190709745654658 ) ) ;
#34109 = CIRCLE ( 'NONE', #15278, 0.9999999999999731326 ) ;
#34108 = LINE ( 'NONE', #82298, #30716 ) ;
#34110 = ORIENTED_EDGE ( 'NONE', *, *, #20438, .T. ) ;
#34111 = CARTESIAN_POINT ( 'NONE',  ( 97.78948648769619467, -29.31518076255846239, 45.78991099019697231 ) ) ;
#34112 = AXIS2_PLACEMENT_3D ( 'NONE', #85348, #65751, #3539 ) ;
#34113 = CIRCLE ( 'NONE', #8009, 7.837499999999996803 ) ;
#34114 = FILL_AREA_STYLE ('',( #40036 ) ) ;
#34115 = AXIS2_PLACEMENT_3D ( 'NONE', #74080, #11862, #39105 ) ;
#34117 = CARTESIAN_POINT ( 'NONE',  ( 83.52520760052966864, 78.07027470200927155, -100.3415888741734818 ) ) ;
#34116 = CARTESIAN_POINT ( 'NONE',  ( 75.31670390244798341, -57.40094715994099772, 60.91780685541480267 ) ) ;
#34118 = LINE ( 'NONE', #76813, #40813 ) ;
#34119 = CARTESIAN_POINT ( 'NONE',  ( 131.3834856945508989, -18.12003772029462922, 3.004064388422935661 ) ) ;
#34120 = VERTEX_POINT ( 'NONE', #12165 ) ;
#34121 = EDGE_CURVE ( 'NONE', #31404, #14173, #34175, .T. ) ;
#34122 = CARTESIAN_POINT ( 'NONE',  ( 107.0664832912739968, 25.62155284005901379, 333.4006252759110112 ) ) ;
#34123 = ADVANCED_FACE ( 'NONE', ( #73033 ), #39850, .F. ) ;
#34124 = EDGE_CURVE ( 'NONE', #27744, #79856, #33044, .T. ) ;
#34125 = CARTESIAN_POINT ( 'NONE',  ( 115.0439452383992318, -109.4614598618335890, 2.217806855418169576 ) ) ;
#34126 = FACE_OUTER_BOUND ( 'NONE', #53602, .T. ) ;
#34127 = ORIENTED_EDGE ( 'NONE', *, *, #21925, .T. ) ;
#34128 = CARTESIAN_POINT ( 'NONE',  ( 98.84076182955313072, -43.22688528923472262, 87.85848241876792031 ) ) ;
#34129 = ADVANCED_FACE ( 'NONE', ( #80765 ), #18518, .F. ) ;
#34131 = LINE ( 'NONE', #5096, #6438 ) ;
#34130 = CARTESIAN_POINT ( 'NONE',  ( 59.56670390244699576, -67.87844715994098976, 155.2178068554179902 ) ) ;
#34132 = CARTESIAN_POINT ( 'NONE',  ( 188.5667039024479834, -58.35344715994099829, 257.2178068554150059 ) ) ;
#34133 = VECTOR ( 'NONE', #65540, 1000.000000000000000 ) ;
#34134 = VECTOR ( 'NONE', #48725, 1000.000000000000000 ) ;
#34135 = CARTESIAN_POINT ( 'NONE',  ( 129.9953678291896040, -88.62578511436512940, 250.2191008560389776 ) ) ;
#34136 = VERTEX_POINT ( 'NONE', #87129 ) ;
#34137 = CARTESIAN_POINT ( 'NONE',  ( 112.7054497023526238, -28.73785826246146158, 125.5870538473389502 ) ) ;
#34139 = ORIENTED_EDGE ( 'NONE', *, *, #68472, .F. ) ;
#34138 = PLANE ( 'NONE',  #42806 ) ;
#34140 = CARTESIAN_POINT ( 'NONE',  ( 96.91023542590100703, -30.67149048741791262, 276.8984824187680829 ) ) ;
#34141 = CARTESIAN_POINT ( 'NONE',  ( 83.56670559755329464, -33.43837296219065536, 239.5838068554176914 ) ) ;
#34142 = CARTESIAN_POINT ( 'NONE',  ( 47.62500000000000000, 94.53880000000000905, 250.8250000000000171 ) ) ;
#34143 = LINE ( 'NONE', #75047, #52940 ) ;
#34144 = DIRECTION ( 'NONE',  ( 1.000000000000000000, 4.299999999999999979E-14, 1.000000000000000078E-15 ) ) ;
#34145 = CARTESIAN_POINT ( 'NONE',  ( 105.4788588808464027, 120.6499999999999915, 3.968750000000405009 ) ) ;
#34146 = CARTESIAN_POINT ( 'NONE',  ( -100.8594679592212344, 82.54999999999999716, 82.89895571708261457 ) ) ;
#34147 = CARTESIAN_POINT ( 'NONE',  ( 109.4488926988246646, -27.20905326525207357, 199.8813395616259925 ) ) ;
#34148 = ORIENTED_EDGE ( 'NONE', *, *, #10421, .T. ) ;
#34149 = ORIENTED_EDGE ( 'NONE', *, *, #38305, .T. ) ;
#34150 = VECTOR ( 'NONE', #4164, 1000.000000000000114 ) ;
#34151 = CARTESIAN_POINT ( 'NONE',  ( 98.17580767689473475, -36.86367352702462341, 132.7701547344679511 ) ) ;
#34152 = CARTESIAN_POINT ( 'NONE',  ( 173.9900000000000091, 36.86249999999999716, -35.28456447661465489 ) ) ;
#34154 = CARTESIAN_POINT ( 'NONE',  ( 107.0664832912739968, -36.72944715994100306, 293.2242906452868851 ) ) ;
#34153 = CARTESIAN_POINT ( 'NONE',  ( 98.57375871705461634, -34.19924797442281772, 27.52729759161093170 ) ) ;
#34155 = VECTOR ( 'NONE', #12015, 1000.000000000000114 ) ;
#34156 = DIRECTION ( 'NONE',  ( 0.000000000000000000, 7.536132396315209176E-17, -1.000000000000000000 ) ) ;
#34157 = DIRECTION ( 'NONE',  ( 0.5000000000000008882, 0.000000000000000000, -0.8660254037844382635 ) ) ;
#34158 = DIRECTION ( 'NONE',  ( -1.000000000000000000, -4.299999999999999979E-14, -1.000000000000000078E-15 ) ) ;
#34159 = LINE ( 'NONE', #61863, #4337 ) ;
#34160 = CARTESIAN_POINT ( 'NONE',  ( 51.06648329127400388, -8.350947159940998787, 335.9181252759120184 ) ) ;
#34161 = CARTESIAN_POINT ( 'NONE',  ( 115.3705510513157861, -30.46277945167181045, 219.3413395616249773 ) ) ;
#34162 = DIRECTION ( 'NONE',  ( 0.000000000000000000, 0.000000000000000000, 1.000000000000000000 ) ) ;
#34163 = ORIENTED_EDGE ( 'NONE', *, *, #48192, .T. ) ;
#34164 = ORIENTED_EDGE ( 'NONE', *, *, #3428, .F. ) ;
#34165 = CARTESIAN_POINT ( 'NONE',  ( -86.68128281353534703, 72.47310549519059464, -97.62852612868761071 ) ) ;
#34166 = CARTESIAN_POINT ( 'NONE',  ( 77.51853161617800936, -17.69475198630787105, 2.828485944707570088 ) ) ;
#34167 = CARTESIAN_POINT ( 'NONE',  ( 19.56648329127303043, -81.37844715994266664, 342.9256252759109884 ) ) ;
#34168 = DIRECTION ( 'NONE',  ( 1.000000000000000000, 0.000000000000000000, 0.000000000000000000 ) ) ;
#34170 = CARTESIAN_POINT ( 'NONE',  ( -148.0533267522752112, 20.32000000000000028, 160.2664750769289697 ) ) ;
#34169 = AXIS2_PLACEMENT_3D ( 'NONE', #34487, #48993, #7689 ) ;
#34171 = ORIENTED_EDGE ( 'NONE', *, *, #2514, .T. ) ;
#34172 = VECTOR ( 'NONE', #22893, 1000.000000000000000 ) ;
#34173 = CARTESIAN_POINT ( 'NONE',  ( 97.75353936551157119, -40.54122631656009190, 7.635625275910939536 ) ) ;
#34174 = VECTOR ( 'NONE', #89706, 1000.000000000000114 ) ;
#34175 = CIRCLE ( 'NONE', #31258, 11.49999999999999645 ) ;
#34176 = CARTESIAN_POINT ( 'NONE',  ( 95.40772882630993479, -38.85404833720006224, 201.4699109901969791 ) ) ;
#34177 = EDGE_CURVE ( 'NONE', #2296, #67030, #16755, .T. ) ;
#34178 = ORIENTED_EDGE ( 'NONE', *, *, #40683, .T. ) ;
#34179 = CIRCLE ( 'NONE', #7863, 34.13125000000000142 ) ;
#34180 = EDGE_CURVE ( 'NONE', #36750, #76187, #18167, .T. ) ;
#34181 = CARTESIAN_POINT ( 'NONE',  ( -11.65927676768451171, 87.37969543255378824, 117.9816103563385781 ) ) ;
#34182 = CARTESIAN_POINT ( 'NONE',  ( 114.5988951105837117, -99.35238426914628462, 2.217806855417836509 ) ) ;
#34183 = CARTESIAN_POINT ( 'NONE',  ( 110.8572222768187174, -45.98311135449077369, 167.8858617136263263 ) ) ;
#34184 = CARTESIAN_POINT ( 'NONE',  ( 106.7484768184134083, -28.57294068349449034, 82.92523322673494590 ) ) ;
#34186 = AXIS2_PLACEMENT_3D ( 'NONE', #36517, #193, #62414 ) ;
#34185 = CARTESIAN_POINT ( 'NONE',  ( 95.54549022710490647, -39.60850420455695087, 162.5213395616259788 ) ) ;
#34187 = EDGE_CURVE ( 'NONE', #20192, #44506, #60291, .T. ) ;
#34188 = DIRECTION ( 'NONE',  ( -1.000000000000000000, 0.000000000000000000, 0.000000000000000000 ) ) ;
#34189 = ORIENTED_EDGE ( 'NONE', *, *, #8505, .F. ) ;
#34190 = EDGE_CURVE ( 'NONE', #48357, #32010, #80322, .T. ) ;
#34191 = AXIS2_PLACEMENT_3D ( 'NONE', #56715, #3112, #17192 ) ;
#34192 = CARTESIAN_POINT ( 'NONE',  ( 3.175000000000334666, 24.56180297284579694, 31.75000000000000000 ) ) ;
#34193 = CARTESIAN_POINT ( 'NONE',  ( 97.82591666500863425, -40.55218698018725831, 66.63908578027370311 ) ) ;
#34194 = ORIENTED_EDGE ( 'NONE', *, *, #5196, .F. ) ;
#34195 = ORIENTED_EDGE ( 'NONE', *, *, #64204, .T. ) ;
#34196 = EDGE_CURVE ( 'NONE', #44232, #28660, #25431, .T. ) ;
#34197 = CARTESIAN_POINT ( 'NONE',  ( 12.70000000000000107, 82.54999999999999716, 117.8738102209307641 ) ) ;
#34198 = ORIENTED_EDGE ( 'NONE', *, *, #45349, .F. ) ;
#34199 = ORIENTED_EDGE ( 'NONE', *, *, #23098, .T. ) ;
#34200 = CARTESIAN_POINT ( 'NONE',  ( -158.9822249764580135, 20.32000000000000028, 107.9500000000000028 ) ) ;
#34201 = VECTOR ( 'NONE', #2769, 1000.000000000000000 ) ;
#34202 = EDGE_CURVE ( 'NONE', #3477, #48525, #25783, .T. ) ;
#34203 = CARTESIAN_POINT ( 'NONE',  ( 98.64819939953339656, -38.17465580927972724, 90.88384839950496996 ) ) ;
#34204 = CARTESIAN_POINT ( 'NONE',  ( 116.9057501799638601, -41.81710558299434410, 243.4346728949589647 ) ) ;
#34205 = CARTESIAN_POINT ( 'NONE',  ( 98.55548742614587354, -30.74683778668241985, 205.8384824187679669 ) ) ;
#34207 = CARTESIAN_POINT ( 'NONE',  ( 96.36668125800727580, -39.40815171121896299, 12.53372051400597442 ) ) ;
#34206 = DIRECTION ( 'NONE',  ( 1.000000000000000078E-15, 0.000000000000000000, -1.000000000000000000 ) ) ;
#34208 = DIRECTION ( 'NONE',  ( 0.000000000000000000, 0.000000000000000000, -1.000000000000000000 ) ) ;
#34209 = CARTESIAN_POINT ( 'NONE',  ( 105.7137777181048079, -46.72360065728855716, 93.46882327081740982 ) ) ;
#34210 = ADVANCED_FACE ( 'NONE', ( #47103 ), #795, .T. ) ;
#34211 = ORIENTED_EDGE ( 'NONE', *, *, #38604, .F. ) ;
#34212 = ADVANCED_FACE ( 'NONE', ( #79884 ), #39411, .T. ) ;
#34213 = CARTESIAN_POINT ( 'NONE',  ( 109.7352083718000415, -46.17358189742688523, 72.79562527591099297 ) ) ;
#34214 = CARTESIAN_POINT ( 'NONE',  ( 111.9494872540039694, -27.46861899264377982, 59.68991099019693536 ) ) ;
#34215 = CARTESIAN_POINT ( 'NONE',  ( 117.5348925983358583, -35.85526142194976273, 253.8927681330537780 ) ) ;
#34216 = VERTEX_POINT ( 'NONE', #38958 ) ;
#34217 = CARTESIAN_POINT ( 'NONE',  ( 110.0520778049922939, -26.08682939676148038, 219.8708633711489711 ) ) ;
#34218 = FACE_OUTER_BOUND ( 'NONE', #31151, .T. ) ;
#34219 = VECTOR ( 'NONE', #81590, 1000.000000000000000 ) ;
#34220 = CARTESIAN_POINT ( 'NONE',  ( 134.0664832912739826, -18.72944715994100306, -5.074374724089001809 ) ) ;
#34221 = CARTESIAN_POINT ( 'NONE',  ( -31.75000000000000000, 124.5870000000000033, 3.174999999999779998 ) ) ;
#34222 = CARTESIAN_POINT ( 'NONE',  ( 102.3066985797795354, -45.62759501947567031, 28.18602549569725824 ) ) ;
#34224 = CARTESIAN_POINT ( 'NONE',  ( 172.5664832912740110, -32.07844715994070839, 314.1756252759120116 ) ) ;
#34223 = CARTESIAN_POINT ( 'NONE',  ( 102.7374329129088295, -29.76594532732805476, 277.6356252759111953 ) ) ;
#34225 = FACE_OUTER_BOUND ( 'NONE', #58932, .T. ) ;
#34226 = LINE ( 'NONE', #60584, #65677 ) ;
#34227 = CARTESIAN_POINT ( 'NONE',  ( 12.67976775996874395, 83.37995484863286322, -117.8759955821573016 ) ) ;
#34228 = CARTESIAN_POINT ( 'NONE',  ( 188.5667039024479834, -58.35344715994099829, 290.4678068554150627 ) ) ;
#34229 = CARTESIAN_POINT ( 'NONE',  ( 112.1310993758104928, -28.00810349215226580, 39.65633506902878480 ) ) ;
#34230 = CARTESIAN_POINT ( 'NONE',  ( 115.8254323922487856, -31.73001882956195985, 75.23979194250962621 ) ) ;
#34231 = EDGE_CURVE ( 'NONE', #60225, #65413, #66669, .T. ) ;
#34233 = VERTEX_POINT ( 'NONE', #87572 ) ;
#34232 = DIRECTION ( 'NONE',  ( 0.000000000000000000, 0.000000000000000000, 1.000000000000000000 ) ) ;
#34234 = FACE_OUTER_BOUND ( 'NONE', #43403, .T. ) ;
#34235 = CARTESIAN_POINT ( 'NONE',  ( 116.9463234969885974, -41.73785994705047386, 248.4651490854349731 ) ) ;
#34236 = CARTESIAN_POINT ( 'NONE',  ( 117.2380278806138278, -39.01742120631563893, 144.6499109901969859 ) ) ;
#34237 = CARTESIAN_POINT ( 'NONE',  ( 96.49300521333343283, -40.10570368261699059, 277.5603871806730467 ) ) ;
#34238 = EDGE_CURVE ( 'NONE', #89758, #12738, #25331, .T. ) ;
#34239 = AXIS2_PLACEMENT_3D ( 'NONE', #73734, #38757, #53706 ) ;
#34240 = DIRECTION ( 'NONE',  ( -6.493183223601999383E-14, 1.000000000000000000, -6.593183223602000791E-29 ) ) ;
#34242 = DIRECTION ( 'NONE',  ( -1.175184669632759901E-16, 1.000000000000000000, 2.000000000000003705E-15 ) ) ;
#34241 = DIRECTION ( 'NONE',  ( 0.000000000000000000, -1.000000000000000000, 0.000000000000000000 ) ) ;
#34243 = LINE ( 'NONE', #74254, #84226 ) ;
#34244 = CARTESIAN_POINT ( 'NONE',  ( 142.8838050580813785, -82.11588141944041297, 542.9756252759101471 ) ) ;
#34245 = VECTOR ( 'NONE', #2905, 1000.000000000000000 ) ;
#34246 = AXIS2_PLACEMENT_3D ( 'NONE', #65442, #10039, #59047 ) ;
#34247 = VECTOR ( 'NONE', #81344, 1000.000000000000000 ) ;
#34248 = VECTOR ( 'NONE', #83909, 1000.000000000000000 ) ;
#34249 = VERTEX_POINT ( 'NONE', #54353 ) ;
#34250 = LINE ( 'NONE', #25761, #65047 ) ;
#34251 = ORIENTED_EDGE ( 'NONE', *, *, #37377, .F. ) ;
#34252 = CARTESIAN_POINT ( 'NONE',  ( 97.73346832622766556, -34.05261013000342274, 140.5267055423629756 ) ) ;
#34254 = ORIENTED_EDGE ( 'NONE', *, *, #48976, .T. ) ;
#34253 = DIRECTION ( 'NONE',  ( 1.000000000000000000, 0.000000000000000000, 0.000000000000000000 ) ) ;
#34255 = DIRECTION ( 'NONE',  ( 0.000000000000000000, 0.000000000000000000, -1.000000000000000000 ) ) ;
#34256 = CARTESIAN_POINT ( 'NONE',  ( 117.0473132972741013, -39.66401662079133672, 179.5984824187679294 ) ) ;
#34257 = CARTESIAN_POINT ( 'NONE',  ( 67.65734841870819594, 69.84999999999999432, 346.9005000000000223 ) ) ;
#34258 = LINE ( 'NONE', #81550, #19675 ) ;
#34259 = CARTESIAN_POINT ( 'NONE',  ( -92.27899210470870628, 80.89685143461889538, 74.43211355457145828 ) ) ;
#34260 = CARTESIAN_POINT ( 'NONE',  ( 83.56670390244703128, -104.2784471599409670, 23.21780685541800082 ) ) ;
#34262 = CARTESIAN_POINT ( 'NONE',  ( 109.5220866130624984, -46.80460460589471694, 87.75467289495897205 ) ) ;
#34261 = VECTOR ( 'NONE', #55256, 1000.000000000000000 ) ;
#34263 = ORIENTED_EDGE ( 'NONE', *, *, #19561, .F. ) ;
#34264 = VERTEX_POINT ( 'NONE', #28468 ) ;
#34265 = ORIENTED_EDGE ( 'NONE', *, *, #61698, .F. ) ;
#34266 = EDGE_CURVE ( 'NONE', #58704, #11027, #28346, .T. ) ;
#34267 = FACE_OUTER_BOUND ( 'NONE', #57597, .T. ) ;
#34269 = PLANE ( 'NONE',  #14305 ) ;
#34268 = CARTESIAN_POINT ( 'NONE',  ( 99.59366209610200826, -44.96145431533973635, 152.9899109901959946 ) ) ;
#34270 = CIRCLE ( 'NONE', #67668, 5.600000000000000533 ) ;
#34271 = CARTESIAN_POINT ( 'NONE',  ( 122.2221484686747317, -96.68314769832130651, -19.26696060647622843 ) ) ;
#34272 = CARTESIAN_POINT ( 'NONE',  ( 90.44969454456439450, -50.04645651782492166, 249.5838068554174640 ) ) ;
#34273 = DIRECTION ( 'NONE',  ( 0.000000000000000000, 1.000000000000000000, 0.000000000000000000 ) ) ;
#34274 = CARTESIAN_POINT ( 'NONE',  ( 34.96670390244699433, -26.71338133339301635, -5.074374724088000832 ) ) ;
#34275 = CARTESIAN_POINT ( 'NONE',  ( 38.10000000000000142, 95.25000000000000000, 358.0130000000000337 ) ) ;
#34276 = CARTESIAN_POINT ( 'NONE',  ( 104.1140010245780445, -46.70499295924816607, 107.3470538473389411 ) ) ;
#34277 = ORIENTED_EDGE ( 'NONE', *, *, #50166, .T. ) ;
#34278 = ORIENTED_EDGE ( 'NONE', *, *, #14718, .F. ) ;
#34279 = ORIENTED_EDGE ( 'NONE', *, *, #30684, .F. ) ;
#34280 = CYLINDRICAL_SURFACE ( 'NONE', #29986, 10.00000000000000888 ) ;
#34281 = CARTESIAN_POINT ( 'NONE',  ( 9.749037034254362410, 238.5000000000000000, 152.4294779587682740 ) ) ;
#34282 = CARTESIAN_POINT ( 'NONE',  ( 70.06670417066790435, -69.62844715994098976, 55.21780685541800437 ) ) ;
#34283 = CARTESIAN_POINT ( 'NONE',  ( 99.51751092519847930, -40.96193357599213414, 179.5633284648289703 ) ) ;
#34284 = ADVANCED_FACE ( 'NONE', ( #20333 ), #83446, .F. ) ;
#34285 = EDGE_CURVE ( 'NONE', #42299, #77564, #82121, .T. ) ;
#34286 = EDGE_CURVE ( 'NONE', #5714, #12855, #13508, .T. ) ;
#34287 = CARTESIAN_POINT ( 'NONE',  ( 172.5664832912740110, 0.2215528400590013880, 201.0426252759120018 ) ) ;
#34288 = VERTEX_POINT ( 'NONE', #28019 ) ;
#34290 = ORIENTED_EDGE ( 'NONE', *, *, #40048, .F. ) ;
#34289 = EDGE_LOOP ( 'NONE', ( #13930, #83060, #72411, #58336 ) ) ;
#34291 = EDGE_CURVE ( 'NONE', #43353, #78013, #47269, .T. ) ;
#34292 = CARTESIAN_POINT ( 'NONE',  ( 107.0664832912739968, 19.62155284005901024, 339.0006252759110339 ) ) ;
#34293 = EDGE_LOOP ( 'NONE', ( #47136, #32065, #84884, #83078 ) ) ;
#34294 = ORIENTED_EDGE ( 'NONE', *, *, #16766, .T. ) ;
#34295 = CARTESIAN_POINT ( 'NONE',  ( 97.81168895331838087, -40.51742574516882200, 287.6356252759109680 ) ) ;
#34296 = CARTESIAN_POINT ( 'NONE',  ( 97.88747888210261294, -34.72385408216754143, 252.5749166392305938 ) ) ;
#34298 = ORIENTED_EDGE ( 'NONE', *, *, #6926, .T. ) ;
#34297 = EDGE_CURVE ( 'NONE', #34136, #32236, #40018, .T. ) ;
#34299 = CIRCLE ( 'NONE', #69132, 13.49999999999999822 ) ;
#34300 = DIRECTION ( 'NONE',  ( 0.000000000000000000, 0.000000000000000000, 1.000000000000000000 ) ) ;
#34301 = CARTESIAN_POINT ( 'NONE',  ( -122.1472860046453945, 74.08167498906739468, 46.10177541449112226 ) ) ;
#34302 = ORIENTED_EDGE ( 'NONE', *, *, #23475, .F. ) ;
#34303 = ORIENTED_EDGE ( 'NONE', *, *, #29119, .T. ) ;
#34304 = EDGE_CURVE ( 'NONE', #12226, #28034, #61634, .T. ) ;
#34305 = AXIS2_PLACEMENT_3D ( 'NONE', #76588, #27533, #55211 ) ;
#34306 = CIRCLE ( 'NONE', #85113, 4.750000000000004441 ) ;
#34307 = FACE_OUTER_BOUND ( 'NONE', #40673, .T. ) ;
#34308 = ORIENTED_EDGE ( 'NONE', *, *, #69193, .F. ) ;
#34309 = ORIENTED_EDGE ( 'NONE', *, *, #53470, .T. ) ;
#34310 = ADVANCED_FACE ( 'NONE', ( #68017 ), #55697, .F. ) ;
#34311 = CARTESIAN_POINT ( 'NONE',  ( 114.7541070161690158, -40.70454043057743121, 241.2528522743529606 ) ) ;
#34312 = CARTESIAN_POINT ( 'NONE',  ( 117.1474210844629766, -33.86219250605441999, 149.0470538473389581 ) ) ;
#34313 = CARTESIAN_POINT ( 'NONE',  ( 113.3016265961370408, -28.35762455946448668, 104.5670538473399347 ) ) ;
#34314 = CARTESIAN_POINT ( 'NONE',  ( 109.9155554066019391, -44.68685817540732330, 249.5838068554167819 ) ) ;
#34315 = CARTESIAN_POINT ( 'NONE',  ( 132.3573525511381774, -16.57277629269280794, 7.749696248599565962 ) ) ;
#34316 = CARTESIAN_POINT ( 'NONE',  ( 112.7801043229996338, -45.44936815460292934, 174.0384824187679556 ) ) ;
#34317 = DIRECTION ( 'NONE',  ( 1.000000000000000000, 4.163336342344333240E-14, 0.000000000000000000 ) ) ;
#34318 = ORIENTED_EDGE ( 'NONE', *, *, #44395, .T. ) ;
#34319 = CARTESIAN_POINT ( 'NONE',  ( 130.2059614519578190, 74.16222525595217974, 9.571858562770211520 ) ) ;
#34320 = ORIENTED_EDGE ( 'NONE', *, *, #71358, .T. ) ;
#34321 = EDGE_CURVE ( 'NONE', #68627, #31158, #19873, .T. ) ;
#34322 = EDGE_LOOP ( 'NONE', ( #61501, #64681, #48578, #58871 ) ) ;
#34323 = DIRECTION ( 'NONE',  ( -0.7071067812159675947, -0.7071067811571274397, -7.071067812159669175E-16 ) ) ;
#34324 = AXIS2_PLACEMENT_3D ( 'NONE', #75095, #62794, #12883 ) ;
#34325 = ORIENTED_EDGE ( 'NONE', *, *, #45922, .T. ) ;
#34326 = DIRECTION ( 'NONE',  ( 1.000000000000000000, 4.163336342344333240E-14, 0.000000000000000000 ) ) ;
#34327 = CLOSED_SHELL ( 'NONE', ( #23058, #70736, #46128, #75833 ) ) ;
#34328 = CARTESIAN_POINT ( 'NONE',  ( 102.3022244709477775, -27.41667396567568815, 120.4527681330539792 ) ) ;
#34329 = CARTESIAN_POINT ( 'NONE',  ( 115.0921084478398058, -30.62179353620878430, 254.3439423599735392 ) ) ;
#34330 = DIRECTION ( 'NONE',  ( 0.000000000000000000, 1.000000000000000000, 0.000000000000000000 ) ) ;
#34331 = DIRECTION ( 'NONE',  ( 1.000000000000000000, 2.999999999999999839E-15, 1.000000000000000078E-15 ) ) ;
#34334 = CARTESIAN_POINT ( 'NONE',  ( 113.0129699484215564, -46.01939436189636012, 214.0175300378159591 ) ) ;
#34333 = DIRECTION ( 'NONE',  ( 0.000000000000000000, 0.000000000000000000, -1.000000000000000000 ) ) ;
#34332 = FACE_OUTER_BOUND ( 'NONE', #61108, .T. ) ;
#34335 = DIRECTION ( 'NONE',  ( 0.000000000000000000, 1.000000000000000000, 0.000000000000000000 ) ) ;
#34336 = CARTESIAN_POINT ( 'NONE',  ( 163.0959832912770082, -23.42844715993521021, 313.9678068554149490 ) ) ;
#34337 = ORIENTED_EDGE ( 'NONE', *, *, #60873, .T. ) ;
#34338 = CARTESIAN_POINT ( 'NONE',  ( 142.8698897858160706, -0.9167816978817300289, 394.9756252759102040 ) ) ;
#34339 = LINE ( 'NONE', #62045, #26835 ) ;
#34340 = CARTESIAN_POINT ( 'NONE',  ( 70.63919639214310564, 100.5999999999999659, 0.000000000000000000 ) ) ;
#34341 = LINE ( 'NONE', #12119, #47664 ) ;
#34343 = VERTEX_POINT ( 'NONE', #40749 ) ;
#34342 = CARTESIAN_POINT ( 'NONE',  ( 96.84578370412310733, -30.63304659132085206, 280.8984824187681397 ) ) ;
#34344 = FACE_OUTER_BOUND ( 'NONE', #31664, .T. ) ;
#34345 = CARTESIAN_POINT ( 'NONE',  ( 98.82253044624914651, -28.18127440817969287, 115.6870538473389587 ) ) ;
#34346 = CARTESIAN_POINT ( 'NONE',  ( 99.06589935993768847, -44.35602157064030848, 32.92038718067297509 ) ) ;
#34347 = CARTESIAN_POINT ( 'NONE',  ( 111.4354466870268539, -47.79847022207366081, 168.8756252759109486 ) ) ;
#34348 = DIRECTION ( 'NONE',  ( 0.000000000000000000, -1.000000000000000000, 0.000000000000000000 ) ) ;
#34349 = ADVANCED_FACE ( 'NONE', ( #89369, #83012 ), #62989, .F. ) ;
#34350 = CARTESIAN_POINT ( 'NONE',  ( 104.4901659694147895, -26.97874889091799488, 101.2814670705812432 ) ) ;
#34352 = CARTESIAN_POINT ( 'NONE',  ( 31.75000000000000000, 66.67499999999999716, 292.1000000000000227 ) ) ;
#34351 = CARTESIAN_POINT ( 'NONE',  ( 19.56670390244744695, -47.82844715994204421, 129.9678068554150627 ) ) ;
#34353 = DIRECTION ( 'NONE',  ( -1.000000000000000078E-15, 1.000000000000000083E-30, 1.000000000000000000 ) ) ;
#34354 = PLANE ( 'NONE',  #10482 ) ;
#34355 = ORIENTED_EDGE ( 'NONE', *, *, #58382, .F. ) ;
#34356 = AXIS2_PLACEMENT_3D ( 'NONE', #53531, #74463, #12237 ) ;
#34357 = ORIENTED_EDGE ( 'NONE', *, *, #41906, .T. ) ;
#34358 = ORIENTED_EDGE ( 'NONE', *, *, #44746, .F. ) ;
#34359 = ORIENTED_EDGE ( 'NONE', *, *, #84582, .T. ) ;
#34360 = CARTESIAN_POINT ( 'NONE',  ( -126.9262659221376310, 49.86651706459634426, 30.57119546983337344 ) ) ;
#34361 = CARTESIAN_POINT ( 'NONE',  ( 96.21590750669005843, -38.71157422997261932, 47.48229194257797303 ) ) ;
#34362 = DIRECTION ( 'NONE',  ( 4.299999999999999979E-14, -1.000000000000000000, 4.400000000000000367E-29 ) ) ;
#34363 = CARTESIAN_POINT ( 'NONE',  ( 116.3183510266638336, -32.94967450325654568, 119.1356252759109537 ) ) ;
#34364 = EDGE_CURVE ( 'NONE', #73742, #84106, #34384, .T. ) ;
#34365 = CARTESIAN_POINT ( 'NONE',  ( 102.6652156630552355, -27.23093027504711117, 176.4213395616249898 ) ) ;
#34366 = CIRCLE ( 'NONE', #25679, 0.5000000000000004441 ) ;
#34367 = DIRECTION ( 'NONE',  ( 1.000000000000000078E-15, 1.000000000000000083E-30, -1.000000000000000000 ) ) ;
#34368 = AXIS2_PLACEMENT_3D ( 'NONE', #32701, #19076, #25002 ) ;
#34369 = CARTESIAN_POINT ( 'NONE',  ( 110.9231077663976066, -44.92578233336853799, 287.3371817328388147 ) ) ;
#34370 = ORIENTED_EDGE ( 'NONE', *, *, #16874, .T. ) ;
#34371 = ORIENTED_EDGE ( 'NONE', *, *, #77603, .F. ) ;
#34372 = ORIENTED_EDGE ( 'NONE', *, *, #62097, .T. ) ;
#34373 = EDGE_CURVE ( 'NONE', #6566, #61739, #5806, .T. ) ;
#34374 = AXIS2_PLACEMENT_3D ( 'NONE', #77367, #35572, #15147 ) ;
#34375 = CIRCLE ( 'NONE', #53208, 81.91591158490091118 ) ;
#34376 = LINE ( 'NONE', #5341, #80496 ) ;
#34377 = CARTESIAN_POINT ( 'NONE',  ( 117.0887403345581390, -37.65561820057894948, 183.7527465225524566 ) ) ;
#34378 = CARTESIAN_POINT ( 'NONE',  ( 97.06107109887885542, -37.99641197720560370, 76.42729194365786327 ) ) ;
#34379 = CARTESIAN_POINT ( 'NONE',  ( 115.8228748906893770, -31.72559827117937203, 274.2397737358683116 ) ) ;
#34380 = CARTESIAN_POINT ( 'NONE',  ( 94.12733899296569007, -42.07533762155324553, 293.6369201390379544 ) ) ;
#34381 = DIRECTION ( 'NONE',  ( 1.000000000000000000, 4.510281037539788691E-14, 0.000000000000000000 ) ) ;
#34382 = DIRECTION ( 'NONE',  ( 0.000000000000000000, 0.000000000000000000, 1.000000000000000000 ) ) ;
#34383 = CARTESIAN_POINT ( 'NONE',  ( 110.6561457788925793, -27.59554888373224557, 269.7784824187687605 ) ) ;
#34384 = LINE ( 'NONE', #76177, #41432 ) ;
#34385 = ORIENTED_EDGE ( 'NONE', *, *, #24700, .T. ) ;
#34386 = CYLINDRICAL_SURFACE ( 'NONE', #52055, 8.636000000000004562 ) ;
#34387 = AXIS2_PLACEMENT_3D ( 'NONE', #69254, #7025, #21110 ) ;
#34388 = B_SPLINE_CURVE_WITH_KNOTS ( 'NONE', 3,
 ( #20553, #62314, #55026, #75954, #13727, #69141, #34610, #29036, #1784, #49902, #77632, #43083, #31250, #58947, #88023, #3117, #67122, #37641, #30819, #86685, #53460, #31702, #65339, #80324, #38511, #38078, #59398, #51688, #79435, #66671, #87132, #24901, #81230, #32591, #86236, #65770, #58510, #32147, #11720, #24013, #52565, #73484, #18976, #17199, #46661, #18069, #79886, #11260 ),
 .UNSPECIFIED., .F., .F.,
 ( 4, 2, 1, 1, 1, 1, 1, 2, 2, 2, 2, 2, 2, 2, 1, 1, 1, 1, 1, 1, 1, 2, 2, 2, 2, 2, 2, 2, 2, 4 ),
 ( 0.5000149529902581103, 0.5002590863139874111, 0.5005032196377168230, 0.5009914862851752027, 0.5019680195800924061, 0.5039210861699265909, 0.5078272193495947384, 0.5156394857089309225, 0.5312640184276032906, 0.5625130838649480269, 0.6250112147396373885, 0.6875093456143268611, 0.7500074764890162227, 0.7500685098199482148, 0.7501295431508803180, 0.7502516098127460786, 0.7504957431364880360, 0.7509840097839701745, 0.7519605430789346734, 0.7539136096688627831, 0.7578197428487252196, 0.7656320092084450968, 0.7812565419278810763, 0.8125056073667551448, 0.8437546728056293244, 0.8750037382445035039, 0.9062528036833776834, 0.9375018691222517520, 0.9687509345611258205, 1.000000000000000000 ),
 .UNSPECIFIED. ) ;
#34389 = CIRCLE ( 'NONE', #86600, 4.762500000000000178 ) ;
#34390 = DIRECTION ( 'NONE',  ( -0.9586846635221889512, 0.000000000000000000, 0.2844709403917162205 ) ) ;
#34391 = CARTESIAN_POINT ( 'NONE',  ( 104.1662843248667230, -44.88357317080683373, 100.1347570362589892 ) ) ;
#34392 = AXIS2_PLACEMENT_3D ( 'NONE', #84137, #7371, #42314 ) ;
#34393 = CARTESIAN_POINT ( 'NONE',  ( 57.14999999999999858, 60.86974387893089755, 300.8629999999999995 ) ) ;
#34394 = ADVANCED_FACE ( 'NONE', ( #21222 ), #69821, .T. ) ;
#34395 = CARTESIAN_POINT ( 'NONE',  ( 188.5667039024483529, -42.82844715993430640, 137.2178068554150059 ) ) ;
#34396 = VERTEX_POINT ( 'NONE', #82571 ) ;
#34397 = CARTESIAN_POINT ( 'NONE',  ( 79.00802158143936538, -34.19118199975294914, 8.051357469096430464 ) ) ;
#34398 = ADVANCED_FACE ( 'NONE', ( #75734 ), #33495, .F. ) ;
#34399 = ORIENTED_EDGE ( 'NONE', *, *, #34304, .T. ) ;
#34400 = CARTESIAN_POINT ( 'NONE',  ( 114.5276809309653459, -28.57754439525472989, 154.4746728949589851 ) ) ;
#34401 = ORIENTED_EDGE ( 'NONE', *, *, #79318, .T. ) ;
#34402 = ADVANCED_FACE ( 'NONE', ( #55260 ), #62095, .F. ) ;
#34403 = CARTESIAN_POINT ( 'NONE',  ( 145.3334424738984012, -69.47022780016817478, 247.4823562763598090 ) ) ;
#34404 = CARTESIAN_POINT ( 'NONE',  ( 113.5773531717103282, -42.74084067657960162, 119.6644404487539646 ) ) ;
#34405 = EDGE_CURVE ( 'NONE', #51500, #14773, #321, .T. ) ;
#34406 = CARTESIAN_POINT ( 'NONE',  ( 72.96458098368701428, 117.4749999999999943, -80.90208098368670164 ) ) ;
#34407 = PLANE ( 'NONE',  #26620 ) ;
#34408 = CARTESIAN_POINT ( 'NONE',  ( 115.5915050065794247, -42.76776344903117888, 49.33562527591095659 ) ) ;
#34409 = FACE_OUTER_BOUND ( 'NONE', #36471, .T. ) ;
#34410 = ORIENTED_EDGE ( 'NONE', *, *, #51200, .T. ) ;
#34411 = ADVANCED_FACE ( 'NONE', ( #59179 ), #16976, .F. ) ;
#34412 = CARTESIAN_POINT ( 'NONE',  ( 133.6498166246059895, 12.92155284005730387, 355.9756252759109998 ) ) ;
#34413 = ORIENTED_EDGE ( 'NONE', *, *, #82118, .F. ) ;
#34414 = VERTEX_POINT ( 'NONE', #45101 ) ;
#34415 = EDGE_CURVE ( 'NONE', #76903, #42953, #64471, .T. ) ;
#34416 = CARTESIAN_POINT ( 'NONE',  ( 83.73314995793998605, 12.92155284005730387, 358.9756252759109998 ) ) ;
#34417 = EDGE_LOOP ( 'NONE', ( #23793, #62355 ) ) ;
#34418 = CARTESIAN_POINT ( 'NONE',  ( 105.2300248619626757, -26.52326248392216357, 275.2061014663877927 ) ) ;
#34419 = CARTESIAN_POINT ( 'NONE',  ( 108.3688181871424945, -47.72895317076035582, 158.6822919425779617 ) ) ;
#34420 = DIRECTION ( 'NONE',  ( 4.554376769437570034E-14, -1.000000000000000000, 0.000000000000000000 ) ) ;
#34421 = CARTESIAN_POINT ( 'NONE',  ( 116.3212776292297406, -32.94146857471347545, 140.1356252759109680 ) ) ;
#34422 = CARTESIAN_POINT ( 'NONE',  ( 117.3712488531672165, -32.73122415481606851, 90.10895860924395606 ) ) ;
#34423 = DIRECTION ( 'NONE',  ( 0.000000000000000000, 0.000000000000000000, 1.000000000000000000 ) ) ;
#34424 = ORIENTED_EDGE ( 'NONE', *, *, #20573, .T. ) ;
#34425 = PLANE ( 'NONE',  #64141 ) ;
#34426 = CIRCLE ( 'NONE', #54768, 2.500000000000002220 ) ;
#34427 = CARTESIAN_POINT ( 'NONE',  ( 117.0609834333835977, -38.07982572155707146, 159.7188531337575910 ) ) ;
#34428 = VERTEX_POINT ( 'NONE', #30601 ) ;
#34429 = VECTOR ( 'NONE', #7333, 1000.000000000000000 ) ;
#34430 = CARTESIAN_POINT ( 'NONE',  ( -479.3614999999999782, 3.174999999999999822, 101.5999999999999943 ) ) ;
#34431 = AXIS2_PLACEMENT_3D ( 'NONE', #51256, #78569, #9065 ) ;
#34432 = PLANE ( 'NONE',  #24642 ) ;
#34433 = CARTESIAN_POINT ( 'NONE',  ( 96.99990081654250673, -39.35482002063354656, 276.5299109901967540 ) ) ;
#34434 = DIRECTION ( 'NONE',  ( 0.000000000000000000, 0.000000000000000000, 1.000000000000000000 ) ) ;
#34435 = CONICAL_SURFACE ( 'NONE', #85254, 24.63800000000000168, 0.7853981633974710386 ) ;
#34436 = CARTESIAN_POINT ( 'NONE',  ( 123.6837132603318423, -17.59493780205705704, 229.5838068554170093 ) ) ;
#34437 = CARTESIAN_POINT ( 'NONE',  ( 41.56670390244695312, -36.32844715994109208, 129.9678068554150911 ) ) ;
#34438 = CARTESIAN_POINT ( 'NONE',  ( 103.2261711710990824, -45.64430683061108596, 286.6752769709340782 ) ) ;
#34440 = CARTESIAN_POINT ( 'NONE',  ( 117.3423061886548027, -38.35306328171702717, 109.7013395616249767 ) ) ;
#34439 = CARTESIAN_POINT ( 'NONE',  ( 97.86195078277592074, -32.64092898360054562, 100.9941899314778198 ) ) ;
#34441 = DIRECTION ( 'NONE',  ( 1.092739197465703932E-16, -1.000000000000000000, 0.000000000000000000 ) ) ;
#34442 = CARTESIAN_POINT ( 'NONE',  ( 117.5314631938956182, -40.43040369381473198, 178.5680062282919778 ) ) ;
#34443 = CARTESIAN_POINT ( 'NONE',  ( 0.000000000000000000, 8.255000000000000782, 0.000000000000000000 ) ) ;
#34444 = ORIENTED_EDGE ( 'NONE', *, *, #24792, .T. ) ;
#34445 = LINE ( 'NONE', #57118, #25086 ) ;
#34446 = FACE_BOUND ( 'NONE', #52255, .T. ) ;
#34447 = DIRECTION ( 'NONE',  ( 0.000000000000000000, 0.000000000000000000, -1.000000000000000000 ) ) ;
#34448 = ORIENTED_EDGE ( 'NONE', *, *, #6410, .F. ) ;
#34449 = VECTOR ( 'NONE', #27626, 1000.000000000000000 ) ;
#34450 = LINE ( 'NONE', #69434, #76675 ) ;
#34452 = ORIENTED_EDGE ( 'NONE', *, *, #84057, .F. ) ;
#34451 = CARTESIAN_POINT ( 'NONE',  ( 108.2818241440822788, -26.29514120620494921, 129.9841967044819739 ) ) ;
#34453 = DIRECTION ( 'NONE',  ( -3.100000000000000258E-29, 3.100000000000000044E-14, 1.000000000000000000 ) ) ;
#34454 = CARTESIAN_POINT ( 'NONE',  ( 113.0378785334839193, -46.05830800173890793, 214.0175300378159591 ) ) ;
#34455 = AXIS2_PLACEMENT_3D ( 'NONE', #74501, #81346, #12278 ) ;
#34456 = DIRECTION ( 'NONE',  ( 3.999999999999999995E-14, -1.000000000000000000, 4.100000000000000342E-29 ) ) ;
#34457 = AXIS2_PLACEMENT_3D ( 'NONE', #85305, #23080, #78487 ) ;
#34458 = EDGE_CURVE ( 'NONE', #22713, #65669, #2313, .T. ) ;
#34459 = DIRECTION ( 'NONE',  ( -0.7071067811865779928, 0.7071067811865171526, -7.071067811865785947E-16 ) ) ;
#34460 = CARTESIAN_POINT ( 'NONE',  ( 164.9212702847350158, -29.73316016639540749, -5.074374724088000832 ) ) ;
#34461 = ORIENTED_EDGE ( 'NONE', *, *, #37491, .F. ) ;
#34462 = CIRCLE ( 'NONE', #43201, 0.4999999999999933387 ) ;
#34463 = CONTEXT_DEPENDENT_SHAPE_REPRESENTATION ( #55599, #17704 ) ;
#34464 = EDGE_CURVE ( 'NONE', #16194, #46234, #64671, .T. ) ;
#34465 = ORIENTED_EDGE ( 'NONE', *, *, #38830, .T. ) ;
#34466 = ORIENTED_EDGE ( 'NONE', *, *, #13524, .T. ) ;
#34467 = ORIENTED_EDGE ( 'NONE', *, *, #48728, .T. ) ;
#34468 = DIRECTION ( 'NONE',  ( 0.000000000000000000, 0.000000000000000000, 1.000000000000000000 ) ) ;
#34469 = CARTESIAN_POINT ( 'NONE',  ( 118.7901020289055225, -38.45900758189035429, 219.7099109901969882 ) ) ;
#34470 = DIRECTION ( 'NONE',  ( -1.000000000000000000, 0.000000000000000000, -3.491481338843133355E-15 ) ) ;
#34471 = CARTESIAN_POINT ( 'NONE',  ( 103.3797721312301547, -105.8297479413482876, -19.78219314458196010 ) ) ;
#34473 = CARTESIAN_POINT ( 'NONE',  ( 92.27764637677411486, 80.88465057165900873, 74.43377912862234780 ) ) ;
#34472 = CARTESIAN_POINT ( 'NONE',  ( 163.0667039024470171, -32.29483332968611364, -5.074374724088000832 ) ) ;
#34474 = CARTESIAN_POINT ( 'NONE',  ( 21.56670390244609692, -23.42844715994195326, 129.9678068554150627 ) ) ;
#34475 = ORIENTED_EDGE ( 'NONE', *, *, #80153, .F. ) ;
#34476 = AXIS2_PLACEMENT_3D ( 'NONE', #61335, #89062, #76321 ) ;
#34477 = VERTEX_POINT ( 'NONE', #31927 ) ;
#34478 = EDGE_CURVE ( 'NONE', #26191, #33658, #70264, .T. ) ;
#34479 = DIRECTION ( 'NONE',  ( -0.7071067811864671926, -0.7071067811866279529, -7.071067811864976379E-16 ) ) ;
#34480 = DIRECTION ( 'NONE',  ( -1.000000000000000078E-15, 0.000000000000000000, 1.000000000000000000 ) ) ;
#34481 = CARTESIAN_POINT ( 'NONE',  ( 97.32398421004042177, -35.86507053846868587, 227.2556252759109725 ) ) ;
#34482 = PLANE ( 'NONE',  #60259 ) ;
#34483 = CARTESIAN_POINT ( 'NONE',  ( 101.3216544293210291, -28.81361639883588310, 71.57562527591099411 ) ) ;
#34484 = DIRECTION ( 'NONE',  ( 0.000000000000000000, -5.300584669389750404E-15, 1.000000000000000000 ) ) ;
#34485 = CARTESIAN_POINT ( 'NONE',  ( 104.5953338484273161, -27.03378288979946475, 21.27505383609677381 ) ) ;
#34486 = ORIENTED_EDGE ( 'NONE', *, *, #28792, .F. ) ;
#34487 = CARTESIAN_POINT ( 'NONE',  ( -47.18030668273772221, 100.5999999999999659, 75.34738655934135920 ) ) ;
#34488 = CIRCLE ( 'NONE', #21476, 9.525000000000000355 ) ;
#34489 = VERTEX_POINT ( 'NONE', #86031 ) ;
#34490 = ORIENTED_EDGE ( 'NONE', *, *, #55304, .F. ) ;
#34491 = DIRECTION ( 'NONE',  ( -6.831565154159360295E-14, 1.000000000000000000, 0.000000000000000000 ) ) ;
#34492 = CARTESIAN_POINT ( 'NONE',  ( 113.3129409812876389, -28.82675956000495887, 270.9758690201826425 ) ) ;
#34493 = AXIS2_PLACEMENT_3D ( 'NONE', #16281, #9028, #24437 ) ;
#34494 = FACE_BOUND ( 'NONE', #44349, .T. ) ;
#34495 = CIRCLE ( 'NONE', #72191, 15.99999999999999822 ) ;
#34496 = CARTESIAN_POINT ( 'NONE',  ( -118.4860461769941935, 94.58006533271584715, 4.091503224720273835 ) ) ;
#34497 = FACE_OUTER_BOUND ( 'NONE', #73097, .T. ) ;
#34498 = EDGE_CURVE ( 'NONE', #26842, #18243, #17857, .T. ) ;
#34499 = CARTESIAN_POINT ( 'NONE',  ( 77.68655577178724059, 72.98405218941671535, -89.55818655986089993 ) ) ;
#34500 = EDGE_LOOP ( 'NONE', ( #69244, #33496, #28628, #12947 ) ) ;
#34501 = LINE ( 'NONE', #42643, #1486 ) ;
#34502 = CIRCLE ( 'NONE', #38850, 2.030000000000003801 ) ;
#34503 = CARTESIAN_POINT ( 'NONE',  ( 162.7866693523297670, -36.02818131005322755, 313.9678068554149490 ) ) ;
#34504 = VERTEX_POINT ( 'NONE', #65565 ) ;
#34505 = CARTESIAN_POINT ( 'NONE',  ( 110.3541591212943445, -25.34385655279935534, 64.85276813305395649 ) ) ;
#34506 = VERTEX_POINT ( 'NONE', #73256 ) ;
#34507 = EDGE_CURVE ( 'NONE', #15778, #9020, #51468, .T. ) ;
#34508 = CARTESIAN_POINT ( 'NONE',  ( 115.6248209149117940, -37.18450138507482450, 18.20670554236297889 ) ) ;
#34509 = VECTOR ( 'NONE', #30878, 1000.000000000000000 ) ;
#34510 = CARTESIAN_POINT ( 'NONE',  ( 113.1795509746323773, -44.75092164323887545, 128.0941733130784428 ) ) ;
#34511 = CARTESIAN_POINT ( 'NONE',  ( 98.82386243697609984, -31.40279086140550291, 145.8699109901969848 ) ) ;
#34512 = DIRECTION ( 'NONE',  ( 1.000000000000000000, 0.000000000000000000, 0.000000000000000000 ) ) ;
#34513 = EDGE_CURVE ( 'NONE', #33658, #64390, #48689, .T. ) ;
#34514 = DIRECTION ( 'NONE',  ( 1.000000000000000078E-15, -1.000000000000000083E-30, -1.000000000000000000 ) ) ;
#34515 = PLANE ( 'NONE',  #18744 ) ;
#34516 = VECTOR ( 'NONE', #52064, 1000.000000000000000 ) ;
#34517 = CARTESIAN_POINT ( 'NONE',  ( 0.7859143630660275770, 69.84999999999999432, 130.5560000000000684 ) ) ;
#34518 = CARTESIAN_POINT ( 'NONE',  ( 109.9722659835539389, -48.26927123350142779, 238.7727681330539724 ) ) ;
#34519 = CARTESIAN_POINT ( 'NONE',  ( 90.66710916952493449, 90.29828471680515634, -76.38857008572948359 ) ) ;
#34520 = AXIS2_PLACEMENT_3D ( 'NONE', #10695, #45207, #37082 ) ;
#34521 = VERTEX_POINT ( 'NONE', #31040 ) ;
#34522 = VERTEX_POINT ( 'NONE', #8035 ) ;
#34523 = CARTESIAN_POINT ( 'NONE',  ( 114.0511858335762270, -28.93156859308855644, 110.4956252759109816 ) ) ;
#34524 = CARTESIAN_POINT ( 'NONE',  ( 33.81648329127399677, 12.92155284005802685, 349.2756252759108406 ) ) ;
#34525 = ORIENTED_EDGE ( 'NONE', *, *, #74313, .F. ) ;
#34526 = EDGE_LOOP ( 'NONE', ( #31349, #63131, #1464, #28924 ) ) ;
#34527 = B_SPLINE_CURVE_WITH_KNOTS ( 'NONE', 3,
 ( #44596, #65508, #24620, #52286, #38682, #66387, #27302, #80950, #60465, #53179, #26851, #33228, #18698, #47733, #88209, #25968, #60926, #81842, #53633, #54086, #19591, #82746, #89545, #12796, #88654, #81406 ),
 .UNSPECIFIED., .F., .F.,
 ( 4, 2, 2, 2, 2, 2, 2, 2, 2, 2, 2, 2, 4 ),
 ( 0.01971515547648590785, 0.02094678046519103318, 0.02217840545389616197, 0.02464165543130641262, 0.02587328042001153100, 0.02710490540871664938, 0.02956815538612688615, 0.03203140536353712292, 0.03326303035224223437, 0.03449465534094735275, 0.03695790531835754789, 0.03818953030706266627, 0.03942115529576777772 ),
 .UNSPECIFIED. ) ;
#34528 = ORIENTED_EDGE ( 'NONE', *, *, #45193, .F. ) ;
#34529 = EDGE_CURVE ( 'NONE', #88820, #46473, #84364, .T. ) ;
#34530 = AXIS2_PLACEMENT_3D ( 'NONE', #6840, #81817, #7739 ) ;
#34531 = CARTESIAN_POINT ( 'NONE',  ( 144.0667039024470171, -102.7784471599409102, 222.2178068554179902 ) ) ;
#34533 = ADVANCED_FACE ( 'NONE', ( #22135 ), #58730, .T. ) ;
#34532 = DIRECTION ( 'NONE',  ( 1.387778780781444492E-15, 0.000000000000000000, -1.000000000000000000 ) ) ;
#34534 = CARTESIAN_POINT ( 'NONE',  ( -254.0000000000000000, 14.28750000000026077, 11.11249999999970051 ) ) ;
#34535 = LINE ( 'NONE', #28162, #54815 ) ;
#34536 = CARTESIAN_POINT ( 'NONE',  ( 105.1059768409772062, -45.79875505096494237, 180.2252332267349857 ) ) ;
#34537 = CARTESIAN_POINT ( 'NONE',  ( 111.0012107362514939, -46.40699640104500645, 278.8841967044824059 ) ) ;
#34538 = CARTESIAN_POINT ( 'NONE',  ( 109.6412602768308489, -46.48053052121719730, 58.78131275420368951 ) ) ;
#34539 = ORIENTED_EDGE ( 'NONE', *, *, #36885, .T. ) ;
#34540 = CARTESIAN_POINT ( 'NONE',  ( 2.884098104289768205, 70.17475223863472422, 118.5216239073115929 ) ) ;
#34541 = CIRCLE ( 'NONE', #76635, 2.000000000000001776 ) ;
#34542 = DIRECTION ( 'NONE',  ( -4.237773401492740281E-14, 1.000000000000000000, 0.000000000000000000 ) ) ;
#34543 = ORIENTED_EDGE ( 'NONE', *, *, #24127, .F. ) ;
#34545 = ORIENTED_EDGE ( 'NONE', *, *, #15848, .T. ) ;
#34544 = AXIS2_PLACEMENT_3D ( 'NONE', #44759, #79313, #37520 ) ;
#34546 = CARTESIAN_POINT ( 'NONE',  ( 118.2946795739112531, -90.36568251306729849, -9.274842254011062437 ) ) ;
#34547 = LINE ( 'NONE', #13224, #87546 ) ;
#34548 = CARTESIAN_POINT ( 'NONE',  ( 107.0664832912739399, -36.72944715994095333, 302.6356252759109680 ) ) ;
#34549 = LINE ( 'NONE', #39, #47745 ) ;
#34550 = CARTESIAN_POINT ( 'NONE',  ( 165.3359832912748004, -36.32844715993531537, 237.4678068554150059 ) ) ;
#34551 = CARTESIAN_POINT ( 'NONE',  ( 114.6728154972408475, -42.76387655025251888, 197.7152769709339566 ) ) ;
#34552 = CARTESIAN_POINT ( 'NONE',  ( 110.4709766755849643, -47.29459308529762041, 57.83657765686300678 ) ) ;
#34553 = FACE_OUTER_BOUND ( 'NONE', #87819, .T. ) ;
#34554 = ORIENTED_EDGE ( 'NONE', *, *, #73261, .T. ) ;
#34555 = CARTESIAN_POINT ( 'NONE',  ( -87.71317827224427788, 71.15456258041353976, -79.76251016565912266 ) ) ;
#34556 = ORIENTED_EDGE ( 'NONE', *, *, #29189, .F. ) ;
#34557 = CARTESIAN_POINT ( 'NONE',  ( 98.34958594530606035, -31.65707425139662590, 261.9065036680587468 ) ) ;
#34558 = ORIENTED_EDGE ( 'NONE', *, *, #11600, .T. ) ;
#34559 = CARTESIAN_POINT ( 'NONE',  ( 36.74138383868079671, -48.33240602328870494, 180.4678068554150911 ) ) ;
#34560 = DIRECTION ( 'NONE',  ( -0.8660254037844379305, 0.000000000000000000, 0.5000000000000011102 ) ) ;
#34561 = CARTESIAN_POINT ( 'NONE',  ( 171.4664832912730219, 12.92155284005730387, 358.9756252759109998 ) ) ;
#34562 = B_SPLINE_CURVE_WITH_KNOTS ( 'NONE', 3,
 ( #79481, #38121, #31293, #2724, #3600, #79029, #24059, #64939, #37233, #2275, #17241, #31746, #44920, #37685, #72206, #9532, #72651, #66252, #79926, #29977, #9980, #17680, #45359, #44474, #59442, #73080, #16794, #30865, #10417, #23189, #50857, #65813, #10859, #38557, #86727, #3166, #78595, #16348, #51728, #78145, #58986, #65385, #58551, #44026, #86280, #24500, #30422, #51281, #71764 ),
 .UNSPECIFIED., .F., .F.,
 ( 4, 2, 1, 1, 1, 1, 2, 2, 2, 2, 2, 2, 2, 1, 1, 1, 1, 1, 1, 1, 2, 2, 2, 2, 2, 2, 2, 2, 2, 4 ),
 ( 0.5000301082837493860, 0.5005183601311320452, 0.5010066119785148153, 0.5019831156732802446, 0.5039361230628114363, 0.5078421378418741527, 0.5156541673999998077, 0.5312782265162505624, 0.5625263447487519608, 0.6250225812137547576, 0.6875188176787576655, 0.7500150541437604623, 0.7500760856246835306, 0.7501371171056067100, 0.7502591800674560663, 0.7505033059911569993, 0.7509915578385393253, 0.7519680615332882123, 0.7539210689227870965, 0.7578270837017879735, 0.7656391132597950566, 0.7812631723758085567, 0.8125112906078360009, 0.8437594088398633341, 0.8750075270718906673, 0.9062556453039180004, 0.9375037635359453336, 0.9687518817679727778, 0.9843759408839864999, 1.000000000000000000 ),
 .UNSPECIFIED. ) ;
#34564 = CARTESIAN_POINT ( 'NONE',  ( 180.1667039024460166, -28.27351298637340093, -5.074374724088000832 ) ) ;
#34563 = AXIS2_PLACEMENT_3D ( 'NONE', #85562, #35589, #78748 ) ;
#34565 = VERTEX_POINT ( 'NONE', #81893 ) ;
#34566 = VECTOR ( 'NONE', #78512, 1000.000000000000000 ) ;
#34567 = CARTESIAN_POINT ( 'NONE',  ( 115.0395865772315034, -43.53517906860128051, 63.26419670448196797 ) ) ;
#34568 =( BOUNDED_CURVE ( )  B_SPLINE_CURVE ( 3, ( #46847, #21873, #7340, #8236 ),
 .UNSPECIFIED., .F., .T. ) 
 B_SPLINE_CURVE_WITH_KNOTS ( ( 4, 4 ),
 ( 1.570796326793646225, 3.141592653589124318 ),
 .UNSPECIFIED. ) 
 CURVE ( )  GEOMETRIC_REPRESENTATION_ITEM ( )  RATIONAL_B_SPLINE_CURVE ( ( 1.000000000000000000, 0.8047378541242278249, 0.8047378541242278249, 1.000000000000000000 ) ) 
 REPRESENTATION_ITEM ( '' )  );
#34571 = ADVANCED_FACE ( 'NONE', ( #68256 ), #89145, .T. ) ;
#34570 = CARTESIAN_POINT ( 'NONE',  ( 88.25674559704616229, 71.15434825076370373, -96.20681132576072514 ) ) ;
#34569 = CARTESIAN_POINT ( 'NONE',  ( 141.3509999999999991, 101.5999999999999943, 132.7150000000000034 ) ) ;
#34572 = CARTESIAN_POINT ( 'NONE',  ( 68.76053423562146349, -136.8603496727827746, 247.4879725229279757 ) ) ;
#34573 = CARTESIAN_POINT ( 'NONE',  ( 131.3325396840767496, -18.38436945697832670, 3.076560175367930139 ) ) ;
#34574 = VERTEX_POINT ( 'NONE', #12850 ) ;
#34575 = CIRCLE ( 'NONE', #7026, 7.937500000000000000 ) ;
#34576 = DIRECTION ( 'NONE',  ( 0.000000000000000000, 0.000000000000000000, -1.000000000000000000 ) ) ;
#34577 = VECTOR ( 'NONE', #33829, 1000.000000000000114 ) ;
#34578 = FACE_OUTER_BOUND ( 'NONE', #71081, .T. ) ;
#34579 = DIRECTION ( 'NONE',  ( -0.4999999999999998890, -0.8660254037844387076, 0.000000000000000000 ) ) ;
#34580 = VERTEX_POINT ( 'NONE', #25561 ) ;
#34581 = CARTESIAN_POINT ( 'NONE',  ( 103.2709630098024576, -47.13517786649186547, 93.28610146638693834 ) ) ;
#34582 = VECTOR ( 'NONE', #74456, 1000.000000000000000 ) ;
#34584 = FACE_OUTER_BOUND ( 'NONE', #83133, .T. ) ;
#34583 = DIRECTION ( 'NONE',  ( -1.000000000000000000, 0.000000000000000000, 0.000000000000000000 ) ) ;
#34585 = CARTESIAN_POINT ( 'NONE',  ( 116.3191307872214821, -32.94748812527954840, 115.1356252759109822 ) ) ;
#34586 = EDGE_CURVE ( 'NONE', #19483, #36508, #57462, .T. ) ;
#34587 = CARTESIAN_POINT ( 'NONE',  ( 134.2858849160865589, -126.1915520417814207, 249.3055338466990065 ) ) ;
#34588 = EDGE_LOOP ( 'NONE', ( #63414, #81806, #33652, #66237 ) ) ;
#34589 = CARTESIAN_POINT ( 'NONE',  ( 103.1701080265564912, -27.72257962874998327, 151.4013395616249511 ) ) ;
#34590 = CIRCLE ( 'NONE', #27390, 2.999999999999988898 ) ;
#34592 = ORIENTED_EDGE ( 'NONE', *, *, #21954, .T. ) ;
#34591 = DIRECTION ( 'NONE',  ( 0.000000000000000000, 0.000000000000000000, -1.000000000000000000 ) ) ;
#34593 = CARTESIAN_POINT ( 'NONE',  ( 100.8614382317055345, -45.12360235833653377, 253.0699109901968882 ) ) ;
#34594 = CYLINDRICAL_SURFACE ( 'NONE', #75902, 11.57110091390437034 ) ;
#34595 = B_SPLINE_CURVE_WITH_KNOTS ( 'NONE', 3,
 ( #48046, #19464, #33539, #34427, #74882, #41230, #88524, #19916, #6284, #76218, #75781, #74433, #83059, #81714, #13546, #68066, #12657, #21260 ),
 .UNSPECIFIED., .F., .F.,
 ( 4, 2, 2, 2, 2, 2, 2, 2, 4 ),
 ( 0.000000000000000000, 0.06250388370504290914, 0.1250077674100858183, 0.1875116511151287413, 0.2500155348201716365, 0.3125194185252145318, 0.3750233022302574826, 0.4375271859353003778, 0.5000310696403432731 ),
 .UNSPECIFIED. ) ;
#34596 = CARTESIAN_POINT ( 'NONE',  ( 7.661254700127842376, 69.45253841614081125, 317.6630000000000109 ) ) ;
#34597 = LINE ( 'NONE', #39614, #51553 ) ;
#34598 = CARTESIAN_POINT ( 'NONE',  ( 105.4788588808462038, 120.6499999999999915, -3.968749999999580336 ) ) ;
#34599 = ADVANCED_FACE ( 'NONE', ( #6038 ), #61417, .F. ) ;
#34600 = EDGE_CURVE ( 'NONE', #73188, #28045, #60065, .T. ) ;
#34601 = DIRECTION ( 'NONE',  ( 0.8660254037844387076, 0.000000000000000000, 0.4999999999999998890 ) ) ;
#34602 = DIRECTION ( 'NONE',  ( -0.2588190451025194072, 0.000000000000000000, -0.9659258262890686453 ) ) ;
#34603 = CARTESIAN_POINT ( 'NONE',  ( 110.2867295656602664, -27.49400189596543242, 209.8099109901969541 ) ) ;
#34604 = ORIENTED_EDGE ( 'NONE', *, *, #63169, .T. ) ;
#34605 = ORIENTED_EDGE ( 'NONE', *, *, #27032, .T. ) ;
#34606 = AXIS2_PLACEMENT_3D ( 'NONE', #38727, #81441, #4218 ) ;
#34607 = CARTESIAN_POINT ( 'NONE',  ( 97.29374130088892514, -39.17162219779756782, 162.9530118773259630 ) ) ;
#34608 = LINE ( 'NONE', #55475, #80631 ) ;
#34610 = CARTESIAN_POINT ( 'NONE',  ( 97.75828504134041452, -40.38463153286905793, 57.62423291007743131 ) ) ;
#34609 = CARTESIAN_POINT ( 'NONE',  ( 111.2075884809769803, -27.22220029719803591, 280.7375300378151337 ) ) ;
#34611 = CARTESIAN_POINT ( 'NONE',  ( 72.96458098368650269, 101.5999999999999943, 72.96458098368729850 ) ) ;
#34612 = EDGE_CURVE ( 'NONE', #51571, #72171, #32758, .T. ) ;
#34613 = DIRECTION ( 'NONE',  ( 1.000000000000000000, -9.073094938289460781E-13, 0.000000000000000000 ) ) ;
#34614 = CARTESIAN_POINT ( 'NONE',  ( 134.0664832912740110, 0.2215528400590013880, 308.6356252759119911 ) ) ;
#34615 = CARTESIAN_POINT ( 'NONE',  ( 63.03715912545640521, -24.89890238295017255, 180.4678068554151196 ) ) ;
#34616 = DIRECTION ( 'NONE',  ( -1.000000000000000078E-15, 1.000000000000000083E-30, 1.000000000000000000 ) ) ;
#34617 = CARTESIAN_POINT ( 'NONE',  ( 100.8363305107023251, -45.83159080358284854, 242.1108633711489517 ) ) ;
#34618 = CARTESIAN_POINT ( 'NONE',  ( 48.79742451362098166, -36.32844715994040996, -5.074374724088000832 ) ) ;
#34619 = ORIENTED_EDGE ( 'NONE', *, *, #75743, .F. ) ;
#34621 = VERTEX_POINT ( 'NONE', #87797 ) ;
#34620 = EDGE_CURVE ( 'NONE', #46082, #65478, #5212, .T. ) ;
#34622 = AXIS2_PLACEMENT_3D ( 'NONE', #61146, #68423, #48386 ) ;
#34623 = CARTESIAN_POINT ( 'NONE',  ( 115.7831076660190206, -41.80230951752221813, 88.40645860859268623 ) ) ;
#34624 = CARTESIAN_POINT ( 'NONE',  ( -89.55756476669488109, 92.11680164986012187, -77.68727430815000901 ) ) ;
#34625 = CARTESIAN_POINT ( 'NONE',  ( 105.7159130685152206, -46.72393690838458724, 123.4674154773381503 ) ) ;
#34626 = CARTESIAN_POINT ( 'NONE',  ( 107.5667039024470171, -96.29408744860640468, -19.78219314458226563 ) ) ;
#34628 = LINE ( 'NONE', #54595, #10774 ) ;
#34627 = AXIS2_PLACEMENT_3D ( 'NONE', #23672, #51334, #16843 ) ;
#34629 = VECTOR ( 'NONE', #27366, 1000.000000000000000 ) ;
#34630 = ORIENTED_EDGE ( 'NONE', *, *, #51344, .F. ) ;
#34631 = CARTESIAN_POINT ( 'NONE',  ( 116.7674666963954309, -31.33607907186020824, 25.24229194257798881 ) ) ;
#34632 = CARTESIAN_POINT ( 'NONE',  ( 108.0141129856239957, -24.91663700320364327, 265.0127681330535552 ) ) ;
#34633 = ORIENTED_EDGE ( 'NONE', *, *, #64456, .F. ) ;
#34634 = ADVANCED_FACE ( 'NONE', ( #53236 ), #75063, .F. ) ;
#34635 = VECTOR ( 'NONE', #89733, 1000.000000000000000 ) ;
#34636 = DIRECTION ( 'NONE',  ( 0.000000000000000000, -1.000000000000000000, 0.000000000000000000 ) ) ;
#34638 = EDGE_CURVE ( 'NONE', #83829, #41798, #47782, .T. ) ;
#34637 = CARTESIAN_POINT ( 'NONE',  ( 46.03715912545432332, -48.62818131006086020, 249.9678068554150343 ) ) ;
#34639 = CARTESIAN_POINT ( 'NONE',  ( 110.8538671553213817, -45.98448489464616529, 167.8855732625641224 ) ) ;
#34640 = ADVANCED_FACE ( 'NONE', ( #81455 ), #39632, .T. ) ;
#34641 = CARTESIAN_POINT ( 'NONE',  ( 100.4744175226576886, -42.33708426910433076, 74.71761417911493197 ) ) ;
#34642 = CARTESIAN_POINT ( 'NONE',  ( 114.4782738979392747, -28.49838154746453256, 155.5051490854349652 ) ) ;
#34643 = DIRECTION ( 'NONE',  ( 0.000000000000000000, 0.000000000000000000, 1.000000000000000000 ) ) ;
#34644 = ORIENTED_EDGE ( 'NONE', *, *, #65774, .T. ) ;
#34645 = ADVANCED_FACE ( 'NONE', ( #67335 ), #5124, .T. ) ;
#34646 = VECTOR ( 'NONE', #65729, 1000.000000000000000 ) ;
#34647 = DIRECTION ( 'NONE',  ( 0.000000000000000000, 0.000000000000000000, -1.000000000000000000 ) ) ;
#34648 = ORIENTED_EDGE ( 'NONE', *, *, #46466, .T. ) ;
#34649 = ORIENTED_EDGE ( 'NONE', *, *, #59314, .T. ) ;
#34650 = CARTESIAN_POINT ( 'NONE',  ( 6.350224805574143261, 93.55624312175208956, 118.3863781049609543 ) ) ;
#34651 = VERTEX_POINT ( 'NONE', #60517 ) ;
#34652 = ORIENTED_EDGE ( 'NONE', *, *, #57519, .T. ) ;
#34653 = CARTESIAN_POINT ( 'NONE',  ( 106.5667039024470455, -112.2628068712777036, -19.78219314458176825 ) ) ;
#34654 = VECTOR ( 'NONE', #39466, 1000.000000000000000 ) ;
#34655 = CARTESIAN_POINT ( 'NONE',  ( 107.8593070027901746, -27.70813345913228076, 109.4171817328389551 ) ) ;
#34656 = CARTESIAN_POINT ( 'NONE',  ( 100.7367085078155640, -45.81951824476916357, 237.0803871806729717 ) ) ;
#34657 = CARTESIAN_POINT ( 'NONE',  ( 114.7977927517518566, -29.71579763117545880, 209.4127681330539872 ) ) ;
#34658 = CARTESIAN_POINT ( 'NONE',  ( 107.1951288810177090, -26.32694189238808491, 31.06705384733893283 ) ) ;
#34659 = CARTESIAN_POINT ( 'NONE',  ( 152.0368932755770288, -23.42844715993588522, 313.9678068554149490 ) ) ;
#34660 = CARTESIAN_POINT ( 'NONE',  ( 0.000000000000000000, 82.54999999999999716, 97.46299999999996544 ) ) ;
#34661 = ORIENTED_EDGE ( 'NONE', *, *, #70576, .F. ) ;
#34662 = AXIS2_PLACEMENT_3D ( 'NONE', #85590, #44206, #2007 ) ;
#34663 = CARTESIAN_POINT ( 'NONE',  ( 113.4935171807054246, -28.59114140144088623, 124.5565776568639507 ) ) ;
#34664 = CARTESIAN_POINT ( 'NONE',  ( 107.2329094490511068, -25.63056496568808029, 80.07657765686299456 ) ) ;
#34665 = CARTESIAN_POINT ( 'NONE',  ( 117.5355484441921163, -36.80252840376058288, 263.8213395616250523 ) ) ;
#34666 = ORIENTED_EDGE ( 'NONE', *, *, #85515, .T. ) ;
#34667 = CARTESIAN_POINT ( 'NONE',  ( 118.0511761103140316, -35.49834556997346624, 233.9032443235299752 ) ) ;
#34668 = CARTESIAN_POINT ( 'NONE',  ( 19.56670390244796920, -67.87844715994100397, 10.91780685541479734 ) ) ;
#34669 = CARTESIAN_POINT ( 'NONE',  ( 98.15082878629252150, -41.26132049930647128, 22.70069694779929037 ) ) ;
#34670 = LINE ( 'NONE', #75121, #51418 ) ;
#34672 = DIRECTION ( 'NONE',  ( 0.7071067811864661934, 0.7071067811866289521, 7.071067811864654918E-16 ) ) ;
#34671 = DIRECTION ( 'NONE',  ( 0.000000000000000000, 1.000000000000000000, 0.000000000000000000 ) ) ;
#34673 = CARTESIAN_POINT ( 'NONE',  ( -103.1875000000000000, 117.4749999999999943, -7.143750000001079847 ) ) ;
#34674 = DIRECTION ( 'NONE',  ( 1.094868876412250136E-15, 0.000000000000000000, 1.000000000000000000 ) ) ;
#34675 = DIRECTION ( 'NONE',  ( 0.000000000000000000, 0.000000000000000000, 1.000000000000000000 ) ) ;
#34676 = DIRECTION ( 'NONE',  ( 1.000000000000000078E-15, 1.000000000000000083E-30, -1.000000000000000000 ) ) ;
#34677 = DIRECTION ( 'NONE',  ( -0.0001211784769727627432, 0.7071067708032326982, -0.7071067811865484609 ) ) ;
#34678 = CARTESIAN_POINT ( 'NONE',  ( 151.5667039024483813, -48.82844715993591223, 249.9678068554149490 ) ) ;
#34680 = ORIENTED_EDGE ( 'NONE', *, *, #40667, .F. ) ;
#34679 = CARTESIAN_POINT ( 'NONE',  ( 97.81171236172070849, -40.51746256574213589, 261.6350867226296941 ) ) ;
#34681 = CIRCLE ( 'NONE', #72375, 2.517499999999998739 ) ;
#34682 = CARTESIAN_POINT ( 'NONE',  ( 154.5667039024469886, -67.87844715994090450, 190.2178068554179902 ) ) ;
#34683 = CARTESIAN_POINT ( 'NONE',  ( 115.0717820980658814, -30.01665675799653599, 269.3813395616251682 ) ) ;
#34684 = CARTESIAN_POINT ( 'NONE',  ( 96.69923704014651378, -37.82612059164544860, 122.4099109901969626 ) ) ;
#34685 = CARTESIAN_POINT ( 'NONE',  ( 105.6260786687505657, -47.09854616955767881, 253.4670538473393719 ) ) ;
#34686 = LINE ( 'NONE', #61052, #70809 ) ;
#34688 = CARTESIAN_POINT ( 'NONE',  ( -22.62762465138237999, 172.0000000000000000, 113.8826257785461280 ) ) ;
#34687 = DIRECTION ( 'NONE',  ( 1.000000000000000000, 0.000000000000000000, 0.000000000000000000 ) ) ;
#34689 = DIRECTION ( 'NONE',  ( -0.6893610196960194836, -0.7071067811865346942, 0.1574210421884011946 ) ) ;
#34690 = LINE ( 'NONE', #179, #32595 ) ;
#34691 = CIRCLE ( 'NONE', #85496, 2.750000000000002665 ) ;
#34692 = VECTOR ( 'NONE', #14078, 1000.000000000000000 ) ;
#34693 = EDGE_CURVE ( 'NONE', #78030, #52268, #31333, .T. ) ;
#34694 = VERTEX_POINT ( 'NONE', #6465 ) ;
#34695 = EDGE_CURVE ( 'NONE', #88388, #57559, #60981, .T. ) ;
#34696 = DIRECTION ( 'NONE',  ( 1.000000000000000000, 6.145690160522480771E-16, 0.000000000000000000 ) ) ;
#34697 = VERTEX_POINT ( 'NONE', #45986 ) ;
#34698 = CARTESIAN_POINT ( 'NONE',  ( 113.5990078486005217, -30.45738264864434441, 188.8457531614099594 ) ) ;
#34700 = EDGE_CURVE ( 'NONE', #18701, #3477, #40080, .T. ) ;
#34699 = VECTOR ( 'NONE', #55401, 1000.000000000000000 ) ;
#34702 = EDGE_LOOP ( 'NONE', ( #72042, #29361 ) ) ;
#34701 = CARTESIAN_POINT ( 'NONE',  ( 104.4059374613178335, -46.45745470167850044, 187.3651553329266335 ) ) ;
#34703 = CARTESIAN_POINT ( 'NONE',  ( 160.7738106836360146, -48.62134037874781001, 300.4678068554149490 ) ) ;
#34704 = CARTESIAN_POINT ( 'NONE',  ( 103.0581626738562306, -26.45339789934171293, 166.3603871806729444 ) ) ;
#34705 = DIRECTION ( 'NONE',  ( -1.000000000000000078E-15, 1.000000000000000083E-30, 1.000000000000000000 ) ) ;
#34706 = CIRCLE ( 'NONE', #11500, 1.000000000000000888 ) ;
#34707 = CARTESIAN_POINT ( 'NONE',  ( 69.94614915224266838, -138.0587248278177697, 247.6570847665630026 ) ) ;
#34708 = CARTESIAN_POINT ( 'NONE',  ( 160.0667039024470171, -79.67844715994088745, 222.2178068554179902 ) ) ;
#34709 = EDGE_CURVE ( 'NONE', #40401, #64957, #5584, .T. ) ;
#34710 = EDGE_CURVE ( 'NONE', #78458, #53618, #83934, .T. ) ;
#34711 = CARTESIAN_POINT ( 'NONE',  ( -83.24493215373352939, 69.84937538953987257, 84.41866557162701667 ) ) ;
#34712 = FACE_OUTER_BOUND ( 'NONE', #42013, .T. ) ;
#34713 = AXIS2_PLACEMENT_3D ( 'NONE', #87423, #78840, #65629 ) ;
#34714 = CARTESIAN_POINT ( 'NONE',  ( 97.83387747045368599, -32.00739517038274329, 95.96229194257799122 ) ) ;
#34715 = ORIENTED_EDGE ( 'NONE', *, *, #57682, .F. ) ;
#34716 = ORIENTED_EDGE ( 'NONE', *, *, #68142, .T. ) ;
#34717 = VERTEX_POINT ( 'NONE', #18299 ) ;
#34718 = EDGE_CURVE ( 'NONE', #63421, #41468, #41856, .T. ) ;
#34719 = FACE_OUTER_BOUND ( 'NONE', #85021, .T. ) ;
#34721 = CARTESIAN_POINT ( 'NONE',  ( 107.0667039024470313, -104.2784471599413791, 2.217806855418003043 ) ) ;
#34720 = CARTESIAN_POINT ( 'NONE',  ( 112.6540662323891837, -44.79745133516134104, 199.0584824187679374 ) ) ;
#34722 = FACE_OUTER_BOUND ( 'NONE', #47461, .T. ) ;
#34723 = EDGE_CURVE ( 'NONE', #17392, #78195, #15408, .T. ) ;
#34724 = DIRECTION ( 'NONE',  ( 0.000000000000000000, 0.000000000000000000, 1.000000000000000000 ) ) ;
#34725 = VECTOR ( 'NONE', #23084, 1000.000000000000000 ) ;
#34726 = FACE_OUTER_BOUND ( 'NONE', #67157, .T. ) ;
#34727 = LINE ( 'NONE', #8376, #71000 ) ;
#34728 = DIRECTION ( 'NONE',  ( 1.000000000000000000, 0.000000000000000000, 0.000000000000000000 ) ) ;
#34729 = CARTESIAN_POINT ( 'NONE',  ( 96.04673288144547882, -37.20790665022158805, 116.3489586092439652 ) ) ;
#34730 = ORIENTED_EDGE ( 'NONE', *, *, #17250, .T. ) ;
#34731 = ORIENTED_EDGE ( 'NONE', *, *, #70431, .T. ) ;
#34733 = ORIENTED_EDGE ( 'NONE', *, *, #13138, .F. ) ;
#34732 = EDGE_CURVE ( 'NONE', #2851, #60793, #56390, .T. ) ;
#34734 = CARTESIAN_POINT ( 'NONE',  ( -33.98325472291460159, 24.56180297284579694, 3.175000000000234746 ) ) ;
#34735 = CARTESIAN_POINT ( 'NONE',  ( -86.68005309089119237, 92.64985122628466740, -97.63151088911729403 ) ) ;
#34736 = DIRECTION ( 'NONE',  ( 0.000000000000000000, 0.000000000000000000, 1.000000000000000000 ) ) ;
#34737 = CARTESIAN_POINT ( 'NONE',  ( 104.3071780974205183, -29.01783752938878180, 188.1680903695909706 ) ) ;
#34738 = AXIS2_PLACEMENT_3D ( 'NONE', #14638, #1458, #70043 ) ;
#34739 = LINE ( 'NONE', #28835, #50884 ) ;
#34740 = CARTESIAN_POINT ( 'NONE',  ( 116.3115597373110290, -32.94279827685361539, 270.1356252759109680 ) ) ;
#34741 = ORIENTED_EDGE ( 'NONE', *, *, #22130, .F. ) ;
#34743 = ORIENTED_EDGE ( 'NONE', *, *, #60276, .T. ) ;
#34742 = VERTEX_POINT ( 'NONE', #1898 ) ;
#34744 = AXIS2_PLACEMENT_3D ( 'NONE', #54578, #66893, #6463 ) ;
#34745 = CARTESIAN_POINT ( 'NONE',  ( 136.8164832912739826, -18.72944715994099951, 3.101481641215532825 ) ) ;
#34746 = ORIENTED_EDGE ( 'NONE', *, *, #29925, .F. ) ;
#34747 = ORIENTED_EDGE ( 'NONE', *, *, #31531, .T. ) ;
#34748 = LINE ( 'NONE', #77438, #40527 ) ;
#34749 = EDGE_CURVE ( 'NONE', #75698, #8926, #38594, .T. ) ;
#34750 = CARTESIAN_POINT ( 'NONE',  ( 105.4042388664825722, -28.02512512522124410, 231.6587261630399439 ) ) ;
#34751 = VECTOR ( 'NONE', #28196, 1000.000000000000000 ) ;
#34752 = ORIENTED_EDGE ( 'NONE', *, *, #59207, .F. ) ;
#34753 = EDGE_CURVE ( 'NONE', #69198, #29300, #28414, .T. ) ;
#34754 = DIRECTION ( 'NONE',  ( 0.000000000000000000, 1.000000000000000000, 0.000000000000000000 ) ) ;
#34755 = CARTESIAN_POINT ( 'NONE',  ( -113.0572828966228514, 68.66927669777484766, 65.29107463701845404 ) ) ;
#34756 = AXIS2_PLACEMENT_3D ( 'NONE', #34888, #88972, #81281 ) ;
#34757 = EDGE_LOOP ( 'NONE', ( #24334, #40413, #43853, #28810 ) ) ;
#34759 = ORIENTED_EDGE ( 'NONE', *, *, #79443, .F. ) ;
#34758 = VECTOR ( 'NONE', #15666, 999.9999999999998863 ) ;
#34760 = CYLINDRICAL_SURFACE ( 'NONE', #46355, 10.04999999999999361 ) ;
#34761 = VERTEX_POINT ( 'NONE', #69595 ) ;
#34762 = ORIENTED_EDGE ( 'NONE', *, *, #23972, .T. ) ;
#34763 = CARTESIAN_POINT ( 'NONE',  ( 114.1709767417603132, -32.67596046159766132, 287.0566617981627360 ) ) ;
#34764 = AXIS2_PLACEMENT_3D ( 'NONE', #37892, #26047, #19233 ) ;
#34765 = CARTESIAN_POINT ( 'NONE',  ( 117.7261736041901372, -39.74048882516440528, 143.6194347997209775 ) ) ;
#34766 = CARTESIAN_POINT ( 'NONE',  ( 97.24623519876071498, -31.70684325556592853, 95.96229194257799122 ) ) ;
#34767 = CARTESIAN_POINT ( 'NONE',  ( 102.2827366117606402, -43.22316888111082989, 249.5838068554171798 ) ) ;
#34768 = CARTESIAN_POINT ( 'NONE',  ( 132.8008218761672765, -16.28157759252032122, 7.978179524061537187 ) ) ;
#34769 =( GEOMETRIC_REPRESENTATION_CONTEXT ( 3 ) GLOBAL_UNCERTAINTY_ASSIGNED_CONTEXT ( ( #49630 ) ) GLOBAL_UNIT_ASSIGNED_CONTEXT ( ( #38593, #86763, #50888 ) ) REPRESENTATION_CONTEXT ( 'NONE', 'WORKASPACE' ) );
#34770 = CARTESIAN_POINT ( 'NONE',  ( 96.67410449796260252, -35.53789531767939991, 202.2356252759109623 ) ) ;
#34771 = DIRECTION ( 'NONE',  ( -1.000000000000000000, 0.000000000000000000, 0.000000000000000000 ) ) ;
#34772 = LINE ( 'NONE', #56553, #74128 ) ;
#34773 = VERTEX_POINT ( 'NONE', #49571 ) ;
#34774 = CARTESIAN_POINT ( 'NONE',  ( -129.9368274816651478, 82.54999999999999716, 12.69999999999954809 ) ) ;
#34775 = ORIENTED_EDGE ( 'NONE', *, *, #34961, .F. ) ;
#34776 = VERTEX_POINT ( 'NONE', #77304 ) ;
#34777 = AXIS2_PLACEMENT_3D ( 'NONE', #63366, #62013, #54729 ) ;
#34778 = CARTESIAN_POINT ( 'NONE',  ( 3.174999999999889688, 17.78000000000000114, -31.75000000000000000 ) ) ;
#34779 = CARTESIAN_POINT ( 'NONE',  ( 106.5069774953447990, -26.72368516806847794, 136.1209971908085663 ) ) ;
#34780 = CARTESIAN_POINT ( 'NONE',  ( 98.83989573471103540, -28.19928051380002287, 115.6870538473389587 ) ) ;
#34781 = CARTESIAN_POINT ( 'NONE',  ( -11.72449278718255172, 77.66876991058626345, 130.0284793542324167 ) ) ;
#34782 = CARTESIAN_POINT ( 'NONE',  ( 179.8585841295808052, -30.08671355699668126, 117.4678068554150627 ) ) ;
#34783 = DIRECTION ( 'NONE',  ( -0.7071067811865671127, -0.7071067811865279218, -7.071067811865664660E-16 ) ) ;
#34786 = CARTESIAN_POINT ( 'NONE',  ( 97.49318720818088480, -40.89074837367928694, 227.6527681330539679 ) ) ;
#34785 = CARTESIAN_POINT ( 'NONE',  ( 115.8503464879663198, -41.61300288441327666, 58.42257506363554853 ) ) ;
#34784 = DIRECTION ( 'NONE',  ( -1.000000000000000000, 0.000000000000000000, 0.000000000000000000 ) ) ;
#34787 = DIRECTION ( 'NONE',  ( 3.100000000000000258E-29, -3.100000000000000044E-14, -1.000000000000000000 ) ) ;
#34788 = DIRECTION ( 'NONE',  ( -0.000000000000000000, 1.000000000000000000, -0.000000000000000000 ) ) ;
#34789 = VERTEX_POINT ( 'NONE', #35054 ) ;
#34790 = AXIS2_PLACEMENT_3D ( 'NONE', #15806, #2624, #63950 ) ;
#34791 = CARTESIAN_POINT ( 'NONE',  ( 33.78309357196401663, -29.99615139349950965, -5.074374724088000832 ) ) ;
#34792 = PLANE ( 'NONE',  #83392 ) ;
#34793 = DIRECTION ( 'NONE',  ( 1.000000000000000078E-15, -1.000000000000000083E-30, -1.000000000000000000 ) ) ;
#34794 = LINE ( 'NONE', #62047, #62200 ) ;
#34796 = ORIENTED_EDGE ( 'NONE', *, *, #23576, .T. ) ;
#34795 = CARTESIAN_POINT ( 'NONE',  ( 96.71965009938165281, -35.13266635363193302, 266.2041967044820581 ) ) ;
#34797 = DIRECTION ( 'NONE',  ( 1.000000000000000078E-15, 1.000000000000000083E-30, -1.000000000000000000 ) ) ;
#34798 = CARTESIAN_POINT ( 'NONE',  ( 114.3594209402202182, -29.19941241435835266, 174.4641967044819637 ) ) ;
#34799 = CARTESIAN_POINT ( 'NONE',  ( 106.6068465219953794, -25.68577410589699994, 36.09753003781596448 ) ) ;
#34800 = CARTESIAN_POINT ( 'NONE',  ( 117.5007279078441655, -40.51415819784174488, 169.5375300378159693 ) ) ;
#34801 = CARTESIAN_POINT ( 'NONE',  ( 116.3214877775586018, -32.94188667902410117, 30.13562527591096085 ) ) ;
#34802 = CARTESIAN_POINT ( 'NONE',  ( 98.34990339064583509, -31.65650299388843436, 101.9063771684363360 ) ) ;
#34804 = DIRECTION ( 'NONE',  ( 1.000000000000000078E-15, -1.000000000000000083E-30, -1.000000000000000000 ) ) ;
#34803 = DIRECTION ( 'NONE',  ( 0.000000000000000000, 0.000000000000000000, 1.000000000000000000 ) ) ;
#34805 = PLANE ( 'NONE',  #29225 ) ;
#34806 = LINE ( 'NONE', #14385, #45286 ) ;
#34807 = ORIENTED_EDGE ( 'NONE', *, *, #10807, .T. ) ;
#34808 = DIRECTION ( 'NONE',  ( -1.825781832977094422E-16, -0.4999999999999998890, 0.8660254037844387076 ) ) ;
#34809 = EDGE_CURVE ( 'NONE', #56684, #84817, #70493, .T. ) ;
#34810 = ORIENTED_EDGE ( 'NONE', *, *, #81525, .T. ) ;
#34811 = EDGE_CURVE ( 'NONE', #13215, #82109, #75959, .T. ) ;
#34812 = VERTEX_POINT ( 'NONE', #69145 ) ;
#34813 = CIRCLE ( 'NONE', #85608, 2.116999999999993776 ) ;
#34814 = ADVANCED_FACE ( 'NONE', ( #13730 ), #82795, .F. ) ;
#34815 = ORIENTED_EDGE ( 'NONE', *, *, #55714, .T. ) ;
#34816 = CARTESIAN_POINT ( 'NONE',  ( 97.79189512308838061, -32.01662636557821173, 46.95276813305393659 ) ) ;
#34817 = LINE ( 'NONE', #69799, #81802 ) ;
#34819 = CARTESIAN_POINT ( 'NONE',  ( 145.1716789765235660, -139.0389598750564915, 246.8368799019731910 ) ) ;
#34818 = VECTOR ( 'NONE', #42499, 1000.000000000000000 ) ;
#34820 = EDGE_CURVE ( 'NONE', #40908, #19584, #54577, .T. ) ;
#34821 = CARTESIAN_POINT ( 'NONE',  ( 95.52146136750830863, -39.61450893497475079, 162.5213395616259788 ) ) ;
#34822 = DIRECTION ( 'NONE',  ( 0.000000000000000000, 0.000000000000000000, 1.000000000000000000 ) ) ;
#34823 = CARTESIAN_POINT ( 'NONE',  ( 115.5964019700117973, -42.63146254436634308, 13.35657765686398868 ) ) ;
#34824 = ORIENTED_EDGE ( 'NONE', *, *, #16990, .T. ) ;
#34825 = EDGE_LOOP ( 'NONE', ( #20513, #14840, #1419, #49707 ) ) ;
#34827 = EDGE_LOOP ( 'NONE', ( #51781, #14580 ) ) ;
#34826 = VECTOR ( 'NONE', #51407, 1000.000000000000000 ) ;
#34828 = EDGE_CURVE ( 'NONE', #46354, #81580, #64733, .T. ) ;
#34829 = DIRECTION ( 'NONE',  ( 0.000000000000000000, 1.000000000000000000, 0.000000000000000000 ) ) ;
#34830 = LINE ( 'NONE', #313, #4302 ) ;
#34831 = LINE ( 'NONE', #62538, #79653 ) ;
#34832 = CARTESIAN_POINT ( 'NONE',  ( 51.06648329127400388, 19.62155284005901024, 327.8006252759110453 ) ) ;
#34833 = CARTESIAN_POINT ( 'NONE',  ( 94.61838531165655297, 94.82199753261677699, 89.95770503246943406 ) ) ;
#34834 = FACE_OUTER_BOUND ( 'NONE', #64642, .T. ) ;
#34835 = ADVANCED_FACE ( 'NONE', ( #22346 ), #63306, .F. ) ;
#34836 = CARTESIAN_POINT ( 'NONE',  ( 76.20505178924389611, 120.6499999999999915, -76.20505178924359768 ) ) ;
#34837 = AXIS2_PLACEMENT_3D ( 'NONE', #61004, #13755, #82368 ) ;
#34838 = CARTESIAN_POINT ( 'NONE',  ( -11.80546680113316071, 87.23253990012126735, 130.0211617397174848 ) ) ;
#34839 = PRODUCT_DEFINITION_FORMATION_WITH_SPECIFIED_SOURCE ( 'ANY', '', #36229, .NOT_KNOWN. ) ;
#34840 = CARTESIAN_POINT ( 'NONE',  ( 118.1852327621007532, -40.75705396371412803, 23.54991099019593292 ) ) ;
#34841 = DIRECTION ( 'NONE',  ( 1.000000000000000078E-15, -1.000000000000000083E-30, -1.000000000000000000 ) ) ;
#34843 = EDGE_LOOP ( 'NONE', ( #88186, #83262, #2340 ) ) ;
#34842 = EDGE_CURVE ( 'NONE', #62184, #72426, #82198, .T. ) ;
#34844 = CARTESIAN_POINT ( 'NONE',  ( -141.3509999999999991, 101.5999999999999943, 141.3509999999999991 ) ) ;
#34845 = CARTESIAN_POINT ( 'NONE',  ( 41.56648329127398966, -27.82844715994070484, 258.9256252759120116 ) ) ;
#34846 = CARTESIAN_POINT ( 'NONE',  ( 104.8330862573783122, -27.72345643971313578, 88.08809036959192440 ) ) ;
#34847 = B_SPLINE_CURVE_WITH_KNOTS ( 'NONE', 3,
 ( #77994, #4695, #37097, #53250, #57071, #32377, #74182, #25575, #10275, #23484, #51151, #37545, #36655, #29391, #60077, #39203, #17101, #64356, #58415, #2133, #11962, #87810, #29840, #3018, #72067, #23920, #2585, #57529, #84815, #64801 ),
 .UNSPECIFIED., .F., .F.,
 ( 4, 2, 2, 2, 2, 2, 2, 2, 2, 2, 1, 1, 1, 1, 1, 1, 2, 4 ),
 ( 0.000000000000000000, 0.06250180752313003185, 0.1250036150462600637, 0.1875054225693900956, 0.2500072300925201274, 0.3125090376156501315, 0.3750108451387801911, 0.4375126526619102507, 0.4687635564234753915, 0.4843890083042580175, 0.4922017342446494137, 0.4961080972148451118, 0.4980612786999429331, 0.4990378694424920103, 0.4995261648137667154, 0.4997703124994041790, 0.4998923863422226610, 0.5000144601850410320 ),
 .UNSPECIFIED. ) ;
#34848 = DIRECTION ( 'NONE',  ( 0.000000000000000000, 0.000000000000000000, 1.000000000000000000 ) ) ;
#34849 = CARTESIAN_POINT ( 'NONE',  ( 97.33784131013395324, -34.07106453330637663, 46.11479194286231120 ) ) ;
#34850 = VERTEX_POINT ( 'NONE', #48671 ) ;
#34851 = EDGE_LOOP ( 'NONE', ( #23922, #52667, #80532, #75552 ) ) ;
#34852 = CARTESIAN_POINT ( 'NONE',  ( 78.42773927739702344, -34.51875925605449424, 7.791169830173473976 ) ) ;
#34853 = VERTEX_POINT ( 'NONE', #76404 ) ;
#34854 = CARTESIAN_POINT ( 'NONE',  ( 97.95630822081318456, -30.46975087157407458, 165.8594347997199634 ) ) ;
#34855 = EDGE_LOOP ( 'NONE', ( #87346, #83839 ) ) ;
#34856 = CARTESIAN_POINT ( 'NONE',  ( 116.7951252747353408, -39.38782977664463658, 69.61479194366307865 ) ) ;
#34857 = CARTESIAN_POINT ( 'NONE',  ( 103.5362709388849254, -28.56900242483978047, 151.8330118773259585 ) ) ;
#34858 = CARTESIAN_POINT ( 'NONE',  ( -11.00058663074870680, 88.91008943578141555, 118.0447001808843766 ) ) ;
#34859 = ADVANCED_FACE ( 'NONE', ( #50020, #77756 ), #28239, .T. ) ;
#34860 = CARTESIAN_POINT ( 'NONE',  ( 99.03746950336261534, -43.41317339962571253, 112.8784824187679732 ) ) ;
#34861 = CARTESIAN_POINT ( 'NONE',  ( 142.8690268918515471, 4.118420757222291506, 542.9756252759101471 ) ) ;
#34862 = ORIENTED_EDGE ( 'NONE', *, *, #28995, .T. ) ;
#34863 = CARTESIAN_POINT ( 'NONE',  ( 162.7131505118679797, -31.94127993907790852, 117.4678068554150485 ) ) ;
#34864 = EDGE_LOOP ( 'NONE', ( #53381, #41420, #19733, #77073 ) ) ;
#34865 = VERTEX_POINT ( 'NONE', #83678 ) ;
#34866 = FACE_BOUND ( 'NONE', #29146, .T. ) ;
#34867 = VERTEX_POINT ( 'NONE', #21451 ) ;
#34868 = CARTESIAN_POINT ( 'NONE',  ( 104.7413500955949672, -27.22895272701804359, 285.2670538473402075 ) ) ;
#34869 = CARTESIAN_POINT ( 'NONE',  ( 99.40614514399899804, -27.65486269830070398, 146.6356252759109395 ) ) ;
#34870 = CARTESIAN_POINT ( 'NONE',  ( 104.4899544585065030, -26.97880758303967852, 141.2814586087148427 ) ) ;
#34871 = CARTESIAN_POINT ( 'NONE',  ( 96.03574380810476896, -41.06042880536169548, 92.62419670448296927 ) ) ;
#34872 = CARTESIAN_POINT ( 'NONE',  ( 112.0659116397137325, -45.48839625046556989, 262.9897919441546605 ) ) ;
#34873 = ORIENTED_EDGE ( 'NONE', *, *, #10513, .F. ) ;
#34874 = LINE ( 'NONE', #49836, #328 ) ;
#34875 = AXIS2_PLACEMENT_3D ( 'NONE', #80071, #31442, #11002 ) ;
#34876 = EDGE_CURVE ( 'NONE', #16565, #52873, #76854, .T. ) ;
#34877 = FACE_OUTER_BOUND ( 'NONE', #14386, .T. ) ;
#34878 = ORIENTED_EDGE ( 'NONE', *, *, #40290, .T. ) ;
#34879 = VECTOR ( 'NONE', #14130, 1000.000000000000000 ) ;
#34880 = ADVANCED_FACE ( 'NONE', ( #7809 ), #63221, .F. ) ;
#34881 = DIRECTION ( 'NONE',  ( 0.000000000000000000, 0.000000000000000000, 1.000000000000000000 ) ) ;
#34882 = CARTESIAN_POINT ( 'NONE',  ( 12.51828547952651682, 84.20585872486917367, 117.8933604834281539 ) ) ;
#34883 = CARTESIAN_POINT ( 'NONE',  ( 104.7356349775885320, -47.53436426244870461, 32.41943479972098174 ) ) ;
#34884 = DIRECTION ( 'NONE',  ( 0.000000000000000000, 1.000000000000000000, 0.000000000000000000 ) ) ;
#34885 = DIRECTION ( 'NONE',  ( -0.7071067811865487940, 0.7071067811865463515, 0.000000000000000000 ) ) ;
#34886 = CARTESIAN_POINT ( 'NONE',  ( 109.6452928465588741, -46.47951212188701220, 92.78246786428896087 ) ) ;
#34887 = CARTESIAN_POINT ( 'NONE',  ( 98.07879527422882404, -32.87106628761745952, 16.00419670448294340 ) ) ;
#34889 = CARTESIAN_POINT ( 'NONE',  ( 104.9672558511366276, -25.09151557957609668, 121.2184824187679766 ) ) ;
#34888 = CARTESIAN_POINT ( 'NONE',  ( 143.0664832912740110, -18.82844715994099971, 284.9256252759119548 ) ) ;
#34890 = CARTESIAN_POINT ( 'NONE',  ( -194.1576000000000022, 101.5999999999999943, -45.33899999999999864 ) ) ;
#34891 = DIRECTION ( 'NONE',  ( -2.900000000000000265E-14, 2.000000000000000155E-15, -1.000000000000000000 ) ) ;
#34892 = ORIENTED_EDGE ( 'NONE', *, *, #36332, .T. ) ;
#34893 = AXIS2_PLACEMENT_3D ( 'NONE', #59095, #3704, #10082 ) ;
#34894 = CARTESIAN_POINT ( 'NONE',  ( 34.67381068360400320, -28.98061976758901892, -5.074374724088000832 ) ) ;
#34895 = FACE_BOUND ( 'NONE', #17625, .T. ) ;
#34896 = FACE_OUTER_BOUND ( 'NONE', #76992, .T. ) ;
#34897 = ORIENTED_EDGE ( 'NONE', *, *, #82944, .T. ) ;
#34898 = CARTESIAN_POINT ( 'NONE',  ( 116.3279290549545806, -32.94269076977911226, 60.13562527591098927 ) ) ;
#34900 = ORIENTED_EDGE ( 'NONE', *, *, #55917, .T. ) ;
#34899 = CARTESIAN_POINT ( 'NONE',  ( 95.99995219064309993, -35.86644482699779246, 191.2765776568629690 ) ) ;
#34901 = CARTESIAN_POINT ( 'NONE',  ( 41.56648329127398966, -18.82844715994071194, 315.9256252759120684 ) ) ;
#34902 = CARTESIAN_POINT ( 'NONE',  ( 107.2496171063691577, -24.85558036374148472, 226.0641967044829812 ) ) ;
#34903 =( GEOMETRIC_REPRESENTATION_CONTEXT ( 3 ) GLOBAL_UNCERTAINTY_ASSIGNED_CONTEXT ( ( #39922 ) ) GLOBAL_UNIT_ASSIGNED_CONTEXT ( ( #70093, #28765, #13785 ) ) REPRESENTATION_CONTEXT ( 'NONE', 'WORKASPACE' ) );
#34904 = CARTESIAN_POINT ( 'NONE',  ( 96.94335780202260366, 71.76234181793742550, 87.44698480207861735 ) ) ;
#34905 = CARTESIAN_POINT ( 'NONE',  ( 172.5664832912740110, -9.303447159940999356, 196.8086252759119645 ) ) ;
#34906 = DIRECTION ( 'NONE',  ( 1.000000000000000000, 0.000000000000000000, 0.000000000000000000 ) ) ;
#34907 = VERTEX_POINT ( 'NONE', #44544 ) ;
#34908 = EDGE_CURVE ( 'NONE', #41047, #20369, #86359, .T. ) ;
#34909 = VERTEX_POINT ( 'NONE', #79104 ) ;
#34910 = ADVANCED_FACE ( 'NONE', ( #9162 ), #52236, .F. ) ;
#34912 = EDGE_LOOP ( 'NONE', ( #67647, #27998 ) ) ;
#34911 = AXIS2_PLACEMENT_3D ( 'NONE', #83583, #27260, #26367 ) ;
#34913 = VECTOR ( 'NONE', #31560, 1000.000000000000000 ) ;
#34914 = EDGE_CURVE ( 'NONE', #20800, #69845, #85482, .T. ) ;
#34915 = ORIENTED_EDGE ( 'NONE', *, *, #62805, .T. ) ;
#34916 = CARTESIAN_POINT ( 'NONE',  ( 70.63919639214310564, 100.5999999999999659, 56.85413200336923012 ) ) ;
#34917 = CARTESIAN_POINT ( 'NONE',  ( 98.94264532560653436, -30.19601435972772308, 236.7870538473399336 ) ) ;
#34918 = CARTESIAN_POINT ( 'NONE',  ( -215.9000000000000057, 0.000000000000000000, 146.9389999999999930 ) ) ;
#34919 = LINE ( 'NONE', #14497, #36796 ) ;
#34920 = ADVANCED_FACE ( 'NONE', ( #44993 ), #43660, .F. ) ;
#34922 = DIRECTION ( 'NONE',  ( -4.237773401492740281E-14, 1.000000000000000000, 0.000000000000000000 ) ) ;
#34921 = CARTESIAN_POINT ( 'NONE',  ( 86.06670390244796920, -50.82844715994100682, 310.9178068554150514 ) ) ;
#34923 = DIRECTION ( 'NONE',  ( 1.000000000000000078E-15, 1.000000000000000083E-30, -1.000000000000000000 ) ) ;
#34924 = AXIS2_PLACEMENT_3D ( 'NONE', #220, #69721, #42435 ) ;
#34925 = CARTESIAN_POINT ( 'NONE',  ( 115.7470646134707266, -43.61006842878475709, 48.30514908543492680 ) ) ;
#34926 = ORIENTED_EDGE ( 'NONE', *, *, #7956, .T. ) ;
#34927 = ORIENTED_EDGE ( 'NONE', *, *, #22516, .T. ) ;
#34928 = DIRECTION ( 'NONE',  ( 0.000000000000000000, 1.000000000000000000, 0.000000000000000000 ) ) ;
#34929 = CARTESIAN_POINT ( 'NONE',  ( 97.80474605953816081, -40.50046288348590195, 17.63384904215703131 ) ) ;
#34930 = CARTESIAN_POINT ( 'NONE',  ( 109.7813264909552231, -47.51098736074720108, 238.7727681330529776 ) ) ;
#34931 = EDGE_CURVE ( 'NONE', #86212, #14684, #44098, .T. ) ;
#34932 = DIRECTION ( 'NONE',  ( 0.000000000000000000, 0.000000000000000000, -1.000000000000000000 ) ) ;
#34933 = CARTESIAN_POINT ( 'NONE',  ( 98.20607846729137691, -32.50961293922097894, 71.97276813305397525 ) ) ;
#34934 = DIRECTION ( 'NONE',  ( -1.000000000000000000, 0.000000000000000000, -3.491481338843133355E-15 ) ) ;
#34935 = CARTESIAN_POINT ( 'NONE',  ( 97.06383915561490028, -37.34216361049876554, 22.37517802614766183 ) ) ;
#34937 = VERTEX_POINT ( 'NONE', #45430 ) ;
#34936 = AXIS2_PLACEMENT_3D ( 'NONE', #22207, #42611, #70343 ) ;
#34938 = CARTESIAN_POINT ( 'NONE',  ( 180.2121375201600131, -29.73316016639650172, -5.074374724088000832 ) ) ;
#34939 = ORIENTED_EDGE ( 'NONE', *, *, #83020, .F. ) ;
#34940 = ORIENTED_EDGE ( 'NONE', *, *, #29390, .F. ) ;
#34941 = CARTESIAN_POINT ( 'NONE',  ( -3.174999999999664979, 104.3431970271541616, -31.75000000000000000 ) ) ;
#34942 = CARTESIAN_POINT ( 'NONE',  ( 113.8567361903355675, -31.03552547285496388, 265.8130118773257777 ) ) ;
#34943 = FACE_OUTER_BOUND ( 'NONE', #46993, .T. ) ;
#34944 = CARTESIAN_POINT ( 'NONE',  ( 113.2450767973898280, -28.75835022255681750, 139.5523338186963827 ) ) ;
#34945 = DIRECTION ( 'NONE',  ( 0.4999999999999998890, 0.8660254037844387076, 0.000000000000000000 ) ) ;
#34946 = VECTOR ( 'NONE', #63837, 1000.000000000000000 ) ;
#34947 = CARTESIAN_POINT ( 'NONE',  ( 75.00102098090802372, 78.06989712577870932, -91.81719692706813873 ) ) ;
#34948 = EDGE_LOOP ( 'NONE', ( #19318, #83116, #3660, #80228 ) ) ;
#34949 = DIRECTION ( 'NONE',  ( -1.000000000000000000, -3.999999999999999995E-14, -1.000000000000000078E-15 ) ) ;
#34950 = LINE ( 'NONE', #69487, #33927 ) ;
#34951 = VERTEX_POINT ( 'NONE', #50475 ) ;
#34952 = CARTESIAN_POINT ( 'NONE',  ( 97.35142178662984236, -32.85085377626895564, 41.02419670448193045 ) ) ;
#34953 = ORIENTED_EDGE ( 'NONE', *, *, #1443, .T. ) ;
#34955 = VECTOR ( 'NONE', #71228, 1000.000000000000000 ) ;
#34954 = CARTESIAN_POINT ( 'NONE',  ( 110.3271547037548004, -45.17815799167961899, 17.28003887569495944 ) ) ;
#34956 = DIRECTION ( 'NONE',  ( 1.000000000000000000, 0.000000000000000000, 0.000000000000000000 ) ) ;
#34957 = CARTESIAN_POINT ( 'NONE',  ( 101.5632356570520756, -44.81509498605974784, 197.1013395616259913 ) ) ;
#34958 = DIRECTION ( 'NONE',  ( 0.000000000000000000, -1.000000000000000000, 2.048885995248199879E-16 ) ) ;
#34959 = CARTESIAN_POINT ( 'NONE',  ( 29.77381068363392913, -48.62134037875510018, 180.4678068554150911 ) ) ;
#34960 = DIRECTION ( 'NONE',  ( 0.000000000000000000, 1.000000000000000000, 0.000000000000000000 ) ) ;
#34961 = EDGE_CURVE ( 'NONE', #7607, #3590, #8202, .T. ) ;
#34962 = DIRECTION ( 'NONE',  ( 0.000000000000000000, 0.000000000000000000, -1.000000000000000000 ) ) ;
#34963 = CARTESIAN_POINT ( 'NONE',  ( 97.43303641489029587, -40.91689460032421266, 227.6527681330539679 ) ) ;
#34964 = CARTESIAN_POINT ( 'NONE',  ( 144.8545562996767444, -1.932463243632626781, 361.9756252759100335 ) ) ;
#34965 = ORIENTED_EDGE ( 'NONE', *, *, #52266, .F. ) ;
#34966 = CARTESIAN_POINT ( 'NONE',  ( 136.7282109818851552, -37.44060378570205216, 6.877169033949778409 ) ) ;
#34967 = ORIENTED_EDGE ( 'NONE', *, *, #74300, .F. ) ;
#34968 = CARTESIAN_POINT ( 'NONE',  ( 102.3408129182306823, -46.07080783562200565, 123.2041967044829818 ) ) ;
#34969 = CARTESIAN_POINT ( 'NONE',  ( 123.0962380253862705, 44.85295700224565962, -43.50008466296358023 ) ) ;
#34970 = VERTEX_POINT ( 'NONE', #86801 ) ;
#34971 = ORIENTED_EDGE ( 'NONE', *, *, #70161, .T. ) ;
#34972 = ORIENTED_EDGE ( 'NONE', *, *, #22576, .T. ) ;
#34973 = CIRCLE ( 'NONE', #30642, 5.041900000000001825 ) ;
#34974 = CARTESIAN_POINT ( 'NONE',  ( 109.6430120328528233, -46.48008676205834178, 122.7814586012382847 ) ) ;
#34975 = CARTESIAN_POINT ( 'NONE',  ( 112.1393497837960638, -28.01282533620751636, 265.6564582266507841 ) ) ;
#34976 = DIRECTION ( 'NONE',  ( -1.825781832977093682E-16, -0.5000000000000003331, 0.8660254037844384856 ) ) ;
#34977 = DIRECTION ( 'NONE',  ( 4.299999999999999979E-14, -1.000000000000000000, 4.400000000000000367E-29 ) ) ;
#34978 = CARTESIAN_POINT ( 'NONE',  ( 29.77381068363392913, -48.62134037875510018, 180.4678068554150911 ) ) ;
#34979 = CARTESIAN_POINT ( 'NONE',  ( 103.9214495108435017, -28.66658863671924706, 168.1785665600669688 ) ) ;
#34980 = CARTESIAN_POINT ( 'NONE',  ( 111.4896171341011666, -26.57472070863446589, 280.7375300378156453 ) ) ;
#34981 = DIRECTION ( 'NONE',  ( 0.000000000000000000, 1.000000000000000000, 0.000000000000000000 ) ) ;
#34982 = ORIENTED_EDGE ( 'NONE', *, *, #71960, .T. ) ;
#34983 = CARTESIAN_POINT ( 'NONE',  ( 106.1656040943334602, -121.2545485715093463, -19.18411693322849487 ) ) ;
#34984 = FACE_OUTER_BOUND ( 'NONE', #72599, .T. ) ;
#34985 = AXIS2_PLACEMENT_3D ( 'NONE', #45544, #31942, #79229 ) ;
#34986 = VERTEX_POINT ( 'NONE', #2348 ) ;
#34987 = ORIENTED_EDGE ( 'NONE', *, *, #15452, .F. ) ;
#34988 = CIRCLE ( 'NONE', #68395, 0.5000000000000016653 ) ;
#34989 = ADVANCED_FACE ( 'NONE', ( #37308 ), #3240, .T. ) ;
#34990 = CARTESIAN_POINT ( 'NONE',  ( 57.56670390244829605, -48.82844715994039575, 295.7178068554150627 ) ) ;
#34991 = DIRECTION ( 'NONE',  ( -1.000000000000000000, -1.000000000000000078E-15, 0.000000000000000000 ) ) ;
#34992 = FACE_OUTER_BOUND ( 'NONE', #55413, .T. ) ;
#34993 = FACE_OUTER_BOUND ( 'NONE', #78093, .T. ) ;
#34994 = LINE ( 'NONE', #48163, #30163 ) ;
#34995 = CARTESIAN_POINT ( 'NONE',  ( 98.55184737119530780, -35.75319039346454986, 205.6581341137909646 ) ) ;
#34996 = CARTESIAN_POINT ( 'NONE',  ( 97.58231912995226764, -32.21254287871169453, 75.97276813305397525 ) ) ;
#34997 = ORIENTED_EDGE ( 'NONE', *, *, #20251, .F. ) ;
#34998 = DIRECTION ( 'NONE',  ( -0.7071067811869841124, 0.7071067811861110330, 0.000000000000000000 ) ) ;
#34999 = ORIENTED_EDGE ( 'NONE', *, *, #89482, .T. ) ;
#35000 = CARTESIAN_POINT ( 'NONE',  ( 131.0667039024480118, -67.87844715994100397, 225.9838068554150254 ) ) ;
#35001 = ORIENTED_EDGE ( 'NONE', *, *, #18218, .T. ) ;
#35002 = CIRCLE ( 'NONE', #61071, 1.999999999999995781 ) ;
#35003 = CARTESIAN_POINT ( 'NONE',  ( 87.06648329127315833, -54.72944906728996273, 14.82207188531695863 ) ) ;
#35004 = ORIENTED_EDGE ( 'NONE', *, *, #79906, .F. ) ;
#35005 = CARTESIAN_POINT ( 'NONE',  ( 29.56670390244797630, -67.87844715994100397, 300.9178068554150514 ) ) ;
#35006 = CARTESIAN_POINT ( 'NONE',  ( 88.18995264527245581, -124.3682898089926709, 250.2203867545810283 ) ) ;
#35007 = CARTESIAN_POINT ( 'NONE',  ( 73.10937651008708826, -8.833000550533901318, -5.074374724088975164 ) ) ;
#35008 = VECTOR ( 'NONE', #88778, 1000.000000000000000 ) ;
#35009 = LINE ( 'NONE', #62722, #20546 ) ;
#35010 = ORIENTED_EDGE ( 'NONE', *, *, #52118, .F. ) ;
#35011 = CARTESIAN_POINT ( 'NONE',  ( 99.11053040751089327, -44.43647348971805400, 41.95086337114900488 ) ) ;
#35013 = CARTESIAN_POINT ( 'NONE',  ( 84.91200770515678187, 74.81660785136578795, -99.17101862044572158 ) ) ;
#35012 = DIRECTION ( 'NONE',  ( 0.000000000000000000, 0.000000000000000000, -1.000000000000000000 ) ) ;
#35014 = LINE ( 'NONE', #77720, #20647 ) ;
#35015 = CARTESIAN_POINT ( 'NONE',  ( 132.8830524875716605, -16.24700279812585180, 1.845048209623397995 ) ) ;
#35016 = EDGE_LOOP ( 'NONE', ( #14388, #87117, #73195, #40130, #3059 ) ) ;
#35017 = ADVANCED_FACE ( 'NONE', ( #24129 ), #51358, .T. ) ;
#35018 = AXIS2_PLACEMENT_3D ( 'NONE', #63615, #84074, #23639 ) ;
#35019 = EDGE_CURVE ( 'NONE', #9633, #51660, #48756, .T. ) ;
#35020 = DIRECTION ( 'NONE',  ( 0.7071067811865784369, -0.7071067811865165975, 7.071067811865791864E-16 ) ) ;
#35021 = EDGE_CURVE ( 'NONE', #49608, #67615, #53083, .T. ) ;
#35022 = CIRCLE ( 'NONE', #72770, 3.249999999999975131 ) ;
#35023 = CARTESIAN_POINT ( 'NONE',  ( -446.0240000000000009, 93.66249999999999432, 85.72499999999999432 ) ) ;
#35024 = CARTESIAN_POINT ( 'NONE',  ( 60.32499999999999574, 82.54999999999999716, 358.0130000000000337 ) ) ;
#35025 = ORIENTED_EDGE ( 'NONE', *, *, #80768, .T. ) ;
#35026 = CARTESIAN_POINT ( 'NONE',  ( 102.6068629045982021, -46.86833229348674479, 128.2346728949589760 ) ) ;
#35027 = EDGE_CURVE ( 'NONE', #86462, #87604, #50255, .T. ) ;
#35029 = DIRECTION ( 'NONE',  ( 0.7071067811866516006, -0.7071067811864434338, 0.000000000000000000 ) ) ;
#35028 = CYLINDRICAL_SURFACE ( 'NONE', #20371, 12.60000000000000142 ) ;
#35030 = LINE ( 'NONE', #75, #85780 ) ;
#35031 = FACE_BOUND ( 'NONE', #57506, .T. ) ;
#35032 = CARTESIAN_POINT ( 'NONE',  ( 97.25364341294459791, -36.87759583893578963, 132.3384824187679669 ) ) ;
#35033 = ADVANCED_FACE ( 'NONE', ( #2796 ), #17753, .F. ) ;
#35035 = VERTEX_POINT ( 'NONE', #57286 ) ;
#35034 = DIRECTION ( 'NONE',  ( -4.554376769437570034E-14, 1.000000000000000000, 0.000000000000000000 ) ) ;
#35036 = VECTOR ( 'NONE', #76601, 1000.000000000000000 ) ;
#35037 = CARTESIAN_POINT ( 'NONE',  ( 100.1532602078033278, -44.50350736857013345, 262.9984824187678782 ) ) ;
#35038 = DIRECTION ( 'NONE',  ( -1.472650733923983947E-14, 0.000000000000000000, 1.000000000000000000 ) ) ;
#35039 = DIRECTION ( 'NONE',  ( 1.000000000000000078E-15, 1.000000000000000083E-30, -1.000000000000000000 ) ) ;
#35040 = CARTESIAN_POINT ( 'NONE',  ( 183.5150000000000148, 5.588000000000000078, 50.79999999999999716 ) ) ;
#35041 = DIRECTION ( 'NONE',  ( 3.100000000000000258E-29, -3.100000000000000044E-14, -1.000000000000000000 ) ) ;
#35042 = CARTESIAN_POINT ( 'NONE',  ( 69.95929469538086209, -138.0461895383714932, 247.6591799766680140 ) ) ;
#35043 = CARTESIAN_POINT ( 'NONE',  ( -94.61736061587603785, 70.27756284692561906, 89.95878776288257939 ) ) ;
#35044 = CARTESIAN_POINT ( 'NONE',  ( 108.5755967597531821, -27.06580334247533770, 189.9527681330539792 ) ) ;
#35045 = VERTEX_POINT ( 'NONE', #30494 ) ;
#35046 = CIRCLE ( 'NONE', #85855, 1.000000000000003775 ) ;
#35047 = ORIENTED_EDGE ( 'NONE', *, *, #20971, .T. ) ;
#35048 = CARTESIAN_POINT ( 'NONE',  ( 103.3408556358882890, -28.68905057859731755, 176.8530118773259687 ) ) ;
#35049 = CIRCLE ( 'NONE', #36568, 5.599999999999994316 ) ;
#35050 = FACE_OUTER_BOUND ( 'NONE', #19279, .T. ) ;
#35051 = CARTESIAN_POINT ( 'NONE',  ( 100.8575770528253628, -43.09432028306430595, 18.39301187732595011 ) ) ;
#35052 = DIRECTION ( 'NONE',  ( 0.000000000000000000, 0.000000000000000000, -1.000000000000000000 ) ) ;
#35053 = CARTESIAN_POINT ( 'NONE',  ( 85.53617444537002257, -18.82844715994099971, 342.9256252759119548 ) ) ;
#35054 = CARTESIAN_POINT ( 'NONE',  ( 67.06670390244700286, -67.87844716047356997, 245.4920193514540188 ) ) ;
#35055 = DIRECTION ( 'NONE',  ( -1.000000000000000000, -8.540177112501204385E-16, 0.000000000000000000 ) ) ;
#35056 = LINE ( 'NONE', #76406, #66198 ) ;
#35057 = CARTESIAN_POINT ( 'NONE',  ( 109.3321198358312074, -26.57584895156206173, 224.9013395616249511 ) ) ;
#35058 = CARTESIAN_POINT ( 'NONE',  ( 97.39153615373059836, -39.27944949574720113, 171.5316118837727686 ) ) ;
#35059 = ORIENTED_EDGE ( 'NONE', *, *, #57276, .T. ) ;
#35060 = ORIENTED_EDGE ( 'NONE', *, *, #9289, .F. ) ;
#35061 = AXIS2_PLACEMENT_3D ( 'NONE', #70601, #8373, #63787 ) ;
#35062 = CARTESIAN_POINT ( 'NONE',  ( -83.24642779537455795, 95.23005795263746620, -84.41404664249405698 ) ) ;
#35063 = CARTESIAN_POINT ( 'NONE',  ( 33.96670390244699433, -26.71338133339301635, -5.074374724088000832 ) ) ;
#35064 = DIRECTION ( 'NONE',  ( 1.000000000000000000, 0.000000000000000000, 0.000000000000000000 ) ) ;
#35065 = ADVANCED_FACE ( 'NONE', ( #15980 ), #71397, .T. ) ;
#35066 = AXIS2_PLACEMENT_3D ( 'NONE', #69000, #13583, #26319 ) ;
#35067 = LINE ( 'NONE', #43223, #32488 ) ;
#35068 = ORIENTED_EDGE ( 'NONE', *, *, #40845, .F. ) ;
#35069 = VECTOR ( 'NONE', #44004, 1000.000000000000000 ) ;
#35070 = DIRECTION ( 'NONE',  ( 1.748382715945130353E-14, 0.000000000000000000, -1.000000000000000000 ) ) ;
#35071 = EDGE_CURVE ( 'NONE', #33225, #34343, #66203, .T. ) ;
#35072 = CARTESIAN_POINT ( 'NONE',  ( 115.3236443966936235, -45.23002221789283084, 268.1899109901965517 ) ) ;
#35073 = ORIENTED_EDGE ( 'NONE', *, *, #21518, .F. ) ;
#35074 = AXIS2_PLACEMENT_3D ( 'NONE', #22631, #63957, #1735 ) ;
#35075 = CARTESIAN_POINT ( 'NONE',  ( 77.68755387133397505, -38.11069332323667425, 7.213126773494069610 ) ) ;
#35076 = FACE_BOUND ( 'NONE', #4281, .T. ) ;
#35077 = CARTESIAN_POINT ( 'NONE',  ( 113.2492417207108417, -44.60456355013358376, 168.1061584034887915 ) ) ;
#35078 = CIRCLE ( 'NONE', #10463, 161.5439999999999827 ) ;
#35079 = CARTESIAN_POINT ( 'NONE',  ( 98.96126485936372319, -37.90763323093077020, 64.25951894101994810 ) ) ;
#35080 = CARTESIAN_POINT ( 'NONE',  ( 97.65507918845807467, -41.26406199109977280, 167.6841967044829573 ) ) ;
#35081 = CARTESIAN_POINT ( 'NONE',  ( 61.06670390244706681, -137.6784471599409869, 55.21780685541800437 ) ) ;
#35082 = ORIENTED_EDGE ( 'NONE', *, *, #34529, .T. ) ;
#35083 = CIRCLE ( 'NONE', #38016, 16.09746158385918946 ) ;
#35084 = LINE ( 'NONE', #26944, #82856 ) ;
#35085 = EDGE_LOOP ( 'NONE', ( #5687, #53813, #83782, #21538 ) ) ;
#35086 = VERTEX_POINT ( 'NONE', #80892 ) ;
#35087 = EDGE_CURVE ( 'NONE', #55007, #79794, #11383, .T. ) ;
#35088 = DIRECTION ( 'NONE',  ( 0.000000000000000000, 0.000000000000000000, -1.000000000000000000 ) ) ;
#35089 =( BOUNDED_CURVE ( )  B_SPLINE_CURVE ( 3, ( #39919, #81738, #19488, #47171 ),
 .UNSPECIFIED., .F., .F. ) 
 B_SPLINE_CURVE_WITH_KNOTS ( ( 4, 4 ),
 ( 1.570796326787725850, 3.141592653584011519 ),
 .UNSPECIFIED. ) 
 CURVE ( )  GEOMETRIC_REPRESENTATION_ITEM ( )  RATIONAL_B_SPLINE_CURVE ( ( 1.000000000000000000, 0.8047378541240375327, 0.8047378541240375327, 1.000000000000000000 ) ) 
 REPRESENTATION_ITEM ( '' )  );
#35090 = ORIENTED_EDGE ( 'NONE', *, *, #56017, .F. ) ;
#35091 = ORIENTED_EDGE ( 'NONE', *, *, #4865, .T. ) ;
#35092 = CARTESIAN_POINT ( 'NONE',  ( 36.74138383868084645, -48.33240602328870494, 129.9678068554150911 ) ) ;
#35093 = CARTESIAN_POINT ( 'NONE',  ( 112.2681825743621431, -29.31628353742046755, 84.00003887569602057 ) ) ;
#35094 = CARTESIAN_POINT ( 'NONE',  ( 107.2496247454619152, -24.85508506706595000, 230.0641967044819580 ) ) ;
#35095 = CARTESIAN_POINT ( 'NONE',  ( 113.0097079652340568, -45.31096836313454190, 203.0584824187679374 ) ) ;
#35096 = CARTESIAN_POINT ( 'NONE',  ( 110.3472192523918238, -25.36789009815987228, 60.85276813305395649 ) ) ;
#35097 = LINE ( 'NONE', #69637, #87602 ) ;
#35098 = LINE ( 'NONE', #21041, #30869 ) ;
#35099 = EDGE_CURVE ( 'NONE', #37640, #23174, #39528, .T. ) ;
#35100 = ORIENTED_EDGE ( 'NONE', *, *, #84936, .F. ) ;
#35101 = DIRECTION ( 'NONE',  ( 0.000000000000000000, 0.000000000000000000, 1.000000000000000000 ) ) ;
#35102 = LINE ( 'NONE', #28287, #57969 ) ;
#35103 = DIRECTION ( 'NONE',  ( 0.000000000000000000, 0.000000000000000000, -1.000000000000000000 ) ) ;
#35104 = AXIS2_PLACEMENT_3D ( 'NONE', #45659, #38420, #39319 ) ;
#35105 = CARTESIAN_POINT ( 'NONE',  ( 97.28626111821314737, -36.62605694204433604, 111.3184824187689657 ) ) ;
#35106 = CARTESIAN_POINT ( 'NONE',  ( 100.9172270114722494, -28.25635367234391992, 75.57562527591093726 ) ) ;
#35107 = CARTESIAN_POINT ( 'NONE',  ( 106.2233489284451338, -47.79750968570053971, 267.5280062282920994 ) ) ;
#35108 = ORIENTED_EDGE ( 'NONE', *, *, #40528, .F. ) ;
#35109 = UNCERTAINTY_MEASURE_WITH_UNIT (LENGTH_MEASURE( 1.000000000000000082E-05 ), #20515, 'distance_accuracy_value', 'NONE');
#35110 = CARTESIAN_POINT ( 'NONE',  ( 97.47293644110631305, -40.89955093664978136, 231.6527681330539679 ) ) ;
#35111 = CARTESIAN_POINT ( 'NONE',  ( 97.31584374709767360, -39.30597611958086190, 36.53145861904452829 ) ) ;
#35112 = DIRECTION ( 'NONE',  ( -1.000000000000000000, 0.000000000000000000, 0.000000000000000000 ) ) ;
#35113 = CARTESIAN_POINT ( 'NONE',  ( 46.83715912545429205, -47.82818131006082751, 249.9678068554150343 ) ) ;
#35115 = CARTESIAN_POINT ( 'NONE',  ( 68.69356659899807482, -139.3022005417465436, 245.7546487670440740 ) ) ;
#35114 = LINE ( 'NONE', #55536, #69454 ) ;
#35116 = FACE_OUTER_BOUND ( 'NONE', #24393, .T. ) ;
#35117 = FACE_OUTER_BOUND ( 'NONE', #46413, .T. ) ;
#35118 = CARTESIAN_POINT ( 'NONE',  ( 10.78716141056406741, 89.26551436951581309, -118.0644550036098508 ) ) ;
#35119 = CARTESIAN_POINT ( 'NONE',  ( -8.387211759491222551, 92.12327290876403652, 130.2876699444761073 ) ) ;
#35120 = DIRECTION ( 'NONE',  ( 0.000000000000000000, 0.000000000000000000, 1.000000000000000000 ) ) ;
#35121 = EDGE_CURVE ( 'NONE', #11288, #8413, #77841, .T. ) ;
#35122 = DIRECTION ( 'NONE',  ( 1.000000000000000078E-15, -1.000000000000000000, 0.000000000000000000 ) ) ;
#35124 = ORIENTED_EDGE ( 'NONE', *, *, #2514, .F. ) ;
#35123 = DIRECTION ( 'NONE',  ( 0.000000000000000000, 1.000000000000000000, 0.000000000000000000 ) ) ;
#35125 = CARTESIAN_POINT ( 'NONE',  ( 99.51799851144285469, -130.7908339518065191, 250.2178068554179902 ) ) ;
#35126 = CARTESIAN_POINT ( 'NONE',  ( 99.38058175836560793, -28.75308465796231516, 265.6746728949588032 ) ) ;
#35127 = CARTESIAN_POINT ( 'NONE',  ( 114.2533759015650787, -44.28132150547345702, 154.1813395616249807 ) ) ;
#35128 = CARTESIAN_POINT ( 'NONE',  ( 111.0545523236672807, -47.06291463499678684, 13.85753003781498016 ) ) ;
#35129 = CARTESIAN_POINT ( 'NONE',  ( 107.0664832912739968, -18.82844715994099971, 168.9256252759119832 ) ) ;
#35131 = CARTESIAN_POINT ( 'NONE',  ( 82.73027604518235023, -36.02416100035765112, 6.874390491354032129 ) ) ;
#35130 = DIRECTION ( 'NONE',  ( 0.000000000000000000, 0.000000000000000000, 1.000000000000000000 ) ) ;
#35132 = CARTESIAN_POINT ( 'NONE',  ( 97.81489200343717982, -40.52525142474216580, 137.6362986401610158 ) ) ;
#35133 = CARTESIAN_POINT ( 'NONE',  ( 129.9368274816649489, 82.96445444011519044, 12.70000000000135998 ) ) ;
#35134 = AXIS2_PLACEMENT_3D ( 'NONE', #13003, #66148, #73417 ) ;
#35135 = VERTEX_POINT ( 'NONE', #18643 ) ;
#35136 = DIRECTION ( 'NONE',  ( 0.000000000000000000, 0.000000000000000000, -1.000000000000000000 ) ) ;
#35137 = ORIENTED_EDGE ( 'NONE', *, *, #82429, .T. ) ;
#35138 = AXIS2_PLACEMENT_3D ( 'NONE', #85761, #51195, #17149 ) ;
#35139 = CARTESIAN_POINT ( 'NONE',  ( 99.64399296875224366, -31.54106566633107533, 160.2514674471249521 ) ) ;
#35140 = EDGE_CURVE ( 'NONE', #22043, #88630, #29929, .T. ) ;
#35142 = ORIENTED_EDGE ( 'NONE', *, *, #64773, .F. ) ;
#35141 = CARTESIAN_POINT ( 'NONE',  ( 177.4809174648215730, -49.32844715993478246, 180.4678068554150059 ) ) ;
#35143 = CARTESIAN_POINT ( 'NONE',  ( 107.0664832912739968, -36.72944715994100306, 287.6356252759109680 ) ) ;
#35144 = CARTESIAN_POINT ( 'NONE',  ( 101.7806060443209049, -45.68981339355057969, 158.1527681330539963 ) ) ;
#35145 = CARTESIAN_POINT ( 'NONE',  ( -473.2019999999999982, 53.97500000000000142, -2.412999999999919876 ) ) ;
#35146 = ADVANCED_FACE ( 'NONE', ( #88149 ), #22734, .T. ) ;
#35147 = CARTESIAN_POINT ( 'NONE',  ( 57.56670390244747892, -48.82844715994040286, 134.7178068554150911 ) ) ;
#35148 = CARTESIAN_POINT ( 'NONE',  ( 51.56670390244699576, -22.48495420874030515, 342.9256252759109884 ) ) ;
#35149 = LINE ( 'NONE', #65105, #38948 ) ;
#35150 = CYLINDRICAL_SURFACE ( 'NONE', #78855, 18.00000000000000000 ) ;
#35151 = CARTESIAN_POINT ( 'NONE',  ( 98.65123886609826798, -31.74476095556097377, 85.90133956162593165 ) ) ;
#35152 = EDGE_LOOP ( 'NONE', ( #60545, #72505, #42566, #52058 ) ) ;
#35153 = ORIENTED_EDGE ( 'NONE', *, *, #79778, .F. ) ;
#35154 = EDGE_LOOP ( 'NONE', ( #86037, #62216, #85338, #57217 ) ) ;
#35155 = CARTESIAN_POINT ( 'NONE',  ( 115.5880482615279163, -32.77224410791782816, 55.59205949637296840 ) ) ;
#35156 = DIRECTION ( 'NONE',  ( 1.000000000000000078E-15, 1.000000000000000083E-30, -1.000000000000000000 ) ) ;
#35158 = DIRECTION ( 'NONE',  ( -1.000000000000000000, 0.000000000000000000, 0.000000000000000000 ) ) ;
#35157 = CARTESIAN_POINT ( 'NONE',  ( 116.4500618263485592, -39.48841239489304655, 179.5984824187679294 ) ) ;
#35159 = CARTESIAN_POINT ( 'NONE',  ( -7.205548786489490269E-13, 127.0000000000000000, 103.1875000000000000 ) ) ;
#35160 = DIRECTION ( 'NONE',  ( 0.000000000000000000, 0.000000000000000000, -1.000000000000000000 ) ) ;
#35161 = LINE ( 'NONE', #76513, #51814 ) ;
#35162 = CIRCLE ( 'NONE', #64172, 10.00000000000000888 ) ;
#35163 = LINE ( 'NONE', #77869, #49174 ) ;
#35164 = CARTESIAN_POINT ( 'NONE',  ( 67.75193203802449204, -68.53543518790235112, 247.0040750501697744 ) ) ;
#35165 = CARTESIAN_POINT ( 'NONE',  ( 116.7751801856528147, -32.99181816784836485, 139.1184824187679396 ) ) ;
#35166 = ORIENTED_EDGE ( 'NONE', *, *, #49052, .T. ) ;
#35167 = ORIENTED_EDGE ( 'NONE', *, *, #67321, .T. ) ;
#35168 = ORIENTED_EDGE ( 'NONE', *, *, #67460, .F. ) ;
#35169 = CARTESIAN_POINT ( 'NONE',  ( 11.41387019979801387, 76.91918732108555901, 130.0565070412864372 ) ) ;
#35170 = CARTESIAN_POINT ( 'NONE',  ( -100.8069756963041499, 84.21449860606321636, -82.96293804092829305 ) ) ;
#35171 = CARTESIAN_POINT ( 'NONE',  ( 41.56648329127398966, -27.82844715994070484, 78.92562527591199739 ) ) ;
#35172 = LINE ( 'NONE', #62883, #4731 ) ;
#35173 = CARTESIAN_POINT ( 'NONE',  ( 111.7296936849409406, -43.46273440104761221, 200.8766617981629565 ) ) ;
#35174 = VECTOR ( 'NONE', #3261, 1000.000000000000000 ) ;
#35175 = DIRECTION ( 'NONE',  ( 0.000000000000000000, 0.000000000000000000, 1.000000000000000000 ) ) ;
#35176 = B_SPLINE_CURVE_WITH_KNOTS ( 'NONE', 3,
 ( #76281, #69472, #7248, #76732, #84006, #21780, #49448, #77188, #70364, #8139, #35829, #63546, #82225, #84908 ),
 .UNSPECIFIED., .F., .F.,
 ( 4, 2, 2, 2, 2, 2, 4 ),
 ( 0.000000000000000000, 0.0004142211558018930786, 0.0008284423116037861572, 0.001242663467405679236, 0.001656884623207572314, 0.002485326934811326813, 0.003313769246415081311 ),
 .UNSPECIFIED. ) ;
#35177 = ADVANCED_FACE ( 'NONE', ( #25911 ), #19532, .T. ) ;
#35178 = CARTESIAN_POINT ( 'NONE',  ( 183.5150000000000148, 68.61249999999999716, -53.61543552338530105 ) ) ;
#35179 = ORIENTED_EDGE ( 'NONE', *, *, #61243, .T. ) ;
#35181 = ORIENTED_EDGE ( 'NONE', *, *, #38118, .T. ) ;
#35180 = VERTEX_POINT ( 'NONE', #33167 ) ;
#35182 = PLANE ( 'NONE',  #33148 ) ;
#35183 = ORIENTED_EDGE ( 'NONE', *, *, #72238, .F. ) ;
#35184 = ORIENTED_EDGE ( 'NONE', *, *, #32449, .T. ) ;
#35185 = CARTESIAN_POINT ( 'NONE',  ( 79.31518617682141326, -21.40257939794846109, 8.160477455077044695 ) ) ;
#35186 = CIRCLE ( 'NONE', #23621, 2.999999999999929834 ) ;
#35187 = CARTESIAN_POINT ( 'NONE',  ( 114.4699299399979395, -31.85941057575024971, 250.7215833058968997 ) ) ;
#35188 = LINE ( 'NONE', #18544, #43957 ) ;
#35189 = VERTEX_POINT ( 'NONE', #26352 ) ;
#35190 = CARTESIAN_POINT ( 'NONE',  ( 158.0667039024470171, -79.67844715994088745, 190.2178068554179902 ) ) ;
#35191 = CARTESIAN_POINT ( 'NONE',  ( -125.1495029386209552, 69.48255809094938229, 37.18183539621997369 ) ) ;
#35192 = ORIENTED_EDGE ( 'NONE', *, *, #41464, .F. ) ;
#35193 = EDGE_LOOP ( 'NONE', ( #11474, #70125 ) ) ;
#35194 = AXIS2_PLACEMENT_3D ( 'NONE', #5173, #31973, #39680 ) ;
#35195 = ADVANCED_FACE ( 'NONE', ( #53576 ), #85114, .F. ) ;
#35196 = CARTESIAN_POINT ( 'NONE',  ( 106.6019379103756535, -25.27972995136449441, 322.9014499992877631 ) ) ;
#35197 = ORIENTED_EDGE ( 'NONE', *, *, #32446, .T. ) ;
#35198 = ORIENTED_EDGE ( 'NONE', *, *, #74531, .T. ) ;
#35199 = EDGE_CURVE ( 'NONE', #36669, #9938, #51680, .T. ) ;
#35200 = VECTOR ( 'NONE', #89213, 1000.000000000000000 ) ;
#35201 = CARTESIAN_POINT ( 'NONE',  ( 101.0613286755868359, -30.49734935201787422, 263.4928522743534813 ) ) ;
#35202 = EDGE_CURVE ( 'NONE', #43121, #5764, #47673, .T. ) ;
#35203 = CARTESIAN_POINT ( 'NONE',  ( 96.58491273044850800, -36.88769195468244533, 136.3384824187679385 ) ) ;
#35204 = CARTESIAN_POINT ( 'NONE',  ( 107.3333893024683903, -26.32957087652219741, 120.0556252759109555 ) ) ;
#35205 = CARTESIAN_POINT ( 'NONE',  ( 41.56648329127398966, -18.82844715994071194, 135.9256252759120684 ) ) ;
#35206 = DIRECTION ( 'NONE',  ( 0.000000000000000000, 0.000000000000000000, -1.000000000000000000 ) ) ;
#35207 = CARTESIAN_POINT ( 'NONE',  ( 96.12521010412353917, -35.16020481777900386, 222.2251490854349640 ) ) ;
#35208 = DIRECTION ( 'NONE',  ( -1.000000000000000000, -8.163404592832032979E-16, 0.000000000000000000 ) ) ;
#35209 = CARTESIAN_POINT ( 'NONE',  ( 168.3664380525666218, -48.62818131005488453, 249.9678068554149775 ) ) ;
#35210 = ORIENTED_EDGE ( 'NONE', *, *, #1029, .F. ) ;
#35211 = CARTESIAN_POINT ( 'NONE',  ( 130.2867309503043884, 73.00415124681448731, 8.386992461123922382 ) ) ;
#35213 = VERTEX_POINT ( 'NONE', #42641 ) ;
#35212 = EDGE_CURVE ( 'NONE', #18895, #25576, #6860, .T. ) ;
#35214 = EDGE_CURVE ( 'NONE', #73928, #88034, #34043, .T. ) ;
#35215 = EDGE_LOOP ( 'NONE', ( #48316, #54464, #79207, #84974, #63323, #62348 ) ) ;
#35216 = CARTESIAN_POINT ( 'NONE',  ( 89.06648329127401098, -18.82844715994099971, 323.8756252759120002 ) ) ;
#35217 = EDGE_CURVE ( 'NONE', #5997, #20800, #27694, .T. ) ;
#35218 = ADVANCED_FACE ( 'NONE', ( #28126 ), #57528, .F. ) ;
#35219 = LINE ( 'NONE', #7973, #14233 ) ;
#35220 = ORIENTED_EDGE ( 'NONE', *, *, #63054, .F. ) ;
#35221 = CARTESIAN_POINT ( 'NONE',  ( 117.5811103608870383, -33.32038496654947579, 134.0880062282919880 ) ) ;
#35222 = CARTESIAN_POINT ( 'NONE',  ( 184.3595971212625386, -48.62134037874549364, 180.4678068554150343 ) ) ;
#35223 = ADVANCED_FACE ( 'NONE', ( #13617 ), #28581, .F. ) ;
#35224 = DIRECTION ( 'NONE',  ( -8.538276166416950255E-16, 1.000000000000000000, -3.100000000000000044E-14 ) ) ;
#35225 = DIRECTION ( 'NONE',  ( -4.554376769437570034E-14, 1.000000000000000000, 0.000000000000000000 ) ) ;
#35228 = CARTESIAN_POINT ( 'NONE',  ( 118.0844448206163833, -36.21142561920247971, 264.8518157521014587 ) ) ;
#35227 = LINE ( 'NONE', #62491, #606 ) ;
#35226 = CARTESIAN_POINT ( 'NONE',  ( 27.27158787008325902, 184.0000000000000000, -5.920431057502157584E-15 ) ) ;
#35229 = LINE ( 'NONE', #29335, #16187 ) ;
#35230 = DIRECTION ( 'NONE',  ( -1.000000000000000000, 0.000000000000000000, 0.000000000000000000 ) ) ;
#35231 = EDGE_LOOP ( 'NONE', ( #33667, #83473, #77449, #24802 ) ) ;
#35232 = CARTESIAN_POINT ( 'NONE',  ( 242.3160000000000025, 40.03750000000000142, -63.94449999999999790 ) ) ;
#35233 = CARTESIAN_POINT ( 'NONE',  ( 188.5667039024481255, -42.82844715993431350, 254.7178068554150059 ) ) ;
#35234 = DIRECTION ( 'NONE',  ( 1.000000000000000000, 4.443626637970152463E-14, 0.000000000000000000 ) ) ;
#35235 = ADVANCED_FACE ( 'NONE', ( #56271 ), #20443, .T. ) ;
#35236 = FACE_BOUND ( 'NONE', #61569, .T. ) ;
#35238 = EDGE_LOOP ( 'NONE', ( #785, #51298, #30589, #81772 ) ) ;
#35237 = CARTESIAN_POINT ( 'NONE',  ( 116.5766284862631466, -42.45395780223795157, 278.3832443235297660 ) ) ;
#35239 = CARTESIAN_POINT ( 'NONE',  ( 88.90000000000000568, 69.84999999999999432, 342.8999999999999773 ) ) ;
#35240 = CARTESIAN_POINT ( 'NONE',  ( 108.2803926554762626, -47.73958771823362213, 157.6518157521019532 ) ) ;
#35241 = CARTESIAN_POINT ( 'NONE',  ( 99.14357900773808296, -43.50514455292471894, 27.88991099019694175 ) ) ;
#35242 = CARTESIAN_POINT ( 'NONE',  ( 114.2047867640113594, -45.22899916922247598, 144.1203871806729637 ) ) ;
#35243 = CARTESIAN_POINT ( 'NONE',  ( -487.2989999999999782, 7.143750000000280487, 15.23694598552305024 ) ) ;
#35244 = CARTESIAN_POINT ( 'NONE',  ( 97.12553229912508357, -37.99667850842347860, 102.4272513145173491 ) ) ;
#35246 = CARTESIAN_POINT ( 'NONE',  ( 125.9611475301391721, -58.72944715994100306, 239.5838068554164124 ) ) ;
#35245 = CARTESIAN_POINT ( 'NONE',  ( 107.0667039024470313, -104.2784471599418197, -11.78219314458200984 ) ) ;
#35247 = CARTESIAN_POINT ( 'NONE',  ( 115.8254323922932940, -31.73001882967317044, 69.23979194249955071 ) ) ;
#35248 = DIRECTION ( 'NONE',  ( 1.157009245868378063E-15, -1.000000000000000000, 3.100000000000000044E-14 ) ) ;
#35249 = ORIENTED_EDGE ( 'NONE', *, *, #59816, .F. ) ;
#35250 = VECTOR ( 'NONE', #38109, 1000.000000000000000 ) ;
#35251 = CARTESIAN_POINT ( 'NONE',  ( 194.0371591254572934, -24.42818131005407878, 300.4678068554149490 ) ) ;
#35252 = VERTEX_POINT ( 'NONE', #55372 ) ;
#35253 = ORIENTED_EDGE ( 'NONE', *, *, #73704, .T. ) ;
#35254 = EDGE_CURVE ( 'NONE', #9436, #75690, #5913, .T. ) ;
#35256 = ORIENTED_EDGE ( 'NONE', *, *, #76557, .T. ) ;
#35255 = FACE_OUTER_BOUND ( 'NONE', #60492, .T. ) ;
#35257 = CARTESIAN_POINT ( 'NONE',  ( 117.4328057974122714, -37.95573561897357706, 49.73276813305393773 ) ) ;
#35258 = FACE_OUTER_BOUND ( 'NONE', #6500, .T. ) ;
#35259 = ADVANCED_FACE ( 'NONE', ( #3562 ), #72618, .F. ) ;
#35260 = CARTESIAN_POINT ( 'NONE',  ( 36.65249034007530327, -49.32844715994124130, 300.4678068554150059 ) ) ;
#35261 = CARTESIAN_POINT ( 'NONE',  ( 96.69998679698829847, -35.27043030541812385, 177.2156252759109805 ) ) ;
#35262 = EDGE_CURVE ( 'NONE', #62736, #58734, #15870, .T. ) ;
#35263 = CARTESIAN_POINT ( 'NONE',  ( 110.6828660728576637, -28.42687563832788200, 284.1600388756959887 ) ) ;
#35264 = ORIENTED_EDGE ( 'NONE', *, *, #80391, .F. ) ;
#35265 = ORIENTED_EDGE ( 'NONE', *, *, #46147, .T. ) ;
#35266 = ORIENTED_EDGE ( 'NONE', *, *, #89164, .F. ) ;
#35267 = AXIS2_PLACEMENT_3D ( 'NONE', #89887, #27639, #76236 ) ;
#35268 = ORIENTED_EDGE ( 'NONE', *, *, #7485, .F. ) ;
#35269 = DIRECTION ( 'NONE',  ( 9.030537910253610117E-13, -1.000000000000000000, 9.040537910253610592E-28 ) ) ;
#35271 = CIRCLE ( 'NONE', #25087, 20.00000000000000355 ) ;
#35270 = CARTESIAN_POINT ( 'NONE',  ( 48.45959712129000252, -28.98061976758940617, -5.074374724088000832 ) ) ;
#35272 = CARTESIAN_POINT ( 'NONE',  ( 113.2454986961229935, -28.75867294318174316, 74.55229194277401916 ) ) ;
#35273 = CARTESIAN_POINT ( 'NONE',  ( 83.90854149456365008, 88.17609398443094904, 100.0213216842708732 ) ) ;
#35274 = DIRECTION ( 'NONE',  ( 1.000000000000000000, 0.000000000000000000, 0.000000000000000000 ) ) ;
#35275 = AXIS2_PLACEMENT_3D ( 'NONE', #56068, #60770, #74864 ) ;
#35276 = CARTESIAN_POINT ( 'NONE',  ( 116.3219235766278672, -32.94275373074044211, 34.13562527591096085 ) ) ;
#35277 = CARTESIAN_POINT ( 'NONE',  ( -11.75417947995160795, 87.35930891448199986, 130.0257995324023170 ) ) ;
#35278 = CARTESIAN_POINT ( 'NONE',  ( 113.3428377330624954, -29.55695056567750711, 289.5032443235305664 ) ) ;
#35279 = DIRECTION ( 'NONE',  ( -0.7071067811571960515, 0.7071067812158990940, 0.000000000000000000 ) ) ;
#35280 = ORIENTED_EDGE ( 'NONE', *, *, #88611, .T. ) ;
#35281 = FACE_OUTER_BOUND ( 'NONE', #16403, .T. ) ;
#35282 = DIRECTION ( 'NONE',  ( 0.000000000000000000, -1.000000000000000000, 0.000000000000000000 ) ) ;
#35283 = CARTESIAN_POINT ( 'NONE',  ( 109.1158479366964684, -45.13783758831200998, 85.57285227435401964 ) ) ;
#35284 = AXIS2_PLACEMENT_3D ( 'NONE', #67873, #32002, #59696 ) ;
#35285 = FACE_OUTER_BOUND ( 'NONE', #35807, .T. ) ;
#35286 = CARTESIAN_POINT ( 'NONE',  ( -487.2989999999999782, 93.66249999999999432, 82.23860802895320887 ) ) ;
#35287 = ORIENTED_EDGE ( 'NONE', *, *, #35928, .T. ) ;
#35288 = ORIENTED_EDGE ( 'NONE', *, *, #44690, .F. ) ;
#35289 = CARTESIAN_POINT ( 'NONE',  ( 77.45242755740702023, -35.85322059724175858, 6.943211687812227417 ) ) ;
#35290 = VECTOR ( 'NONE', #2781, 1000.000000000000000 ) ;
#35291 = ORIENTED_EDGE ( 'NONE', *, *, #37400, .T. ) ;
#35292 = EDGE_LOOP ( 'NONE', ( #7481, #88635, #28492, #89784 ) ) ;
#35293 = CARTESIAN_POINT ( 'NONE',  ( 113.4085779730985166, -29.80024602262787425, 150.9063452106589693 ) ) ;
#35294 = DIRECTION ( 'NONE',  ( 0.000000000000000000, 0.000000000000000000, 1.000000000000000000 ) ) ;
#35295 = CARTESIAN_POINT ( 'NONE',  ( 117.3927859964040437, -32.72286779764937847, 90.10895860924395606 ) ) ;
#35296 = CIRCLE ( 'NONE', #19366, 2.116999999999993776 ) ;
#35297 = CARTESIAN_POINT ( 'NONE',  ( 109.6430121127644952, -46.48008674009260233, 83.78145860778620602 ) ) ;
#35298 = VERTEX_POINT ( 'NONE', #30827 ) ;
#35299 = CARTESIAN_POINT ( 'NONE',  ( -118.0639734269500565, 75.84278307195158675, -10.79247489890467193 ) ) ;
#35300 = ORIENTED_EDGE ( 'NONE', *, *, #18209, .T. ) ;
#35302 = EDGE_CURVE ( 'NONE', #60117, #45, #64457, .T. ) ;
#35301 = ORIENTED_EDGE ( 'NONE', *, *, #70202, .T. ) ;
#35303 = EDGE_CURVE ( 'NONE', #64498, #25149, #58956, .T. ) ;
#35304 = EDGE_CURVE ( 'NONE', #59900, #84828, #79444, .T. ) ;
#35305 = CARTESIAN_POINT ( 'NONE',  ( 22.49563609058250435, -48.82844715994099971, 13.84673904354932361 ) ) ;
#35306 = EDGE_LOOP ( 'NONE', ( #54141, #43369, #6346, #28230 ) ) ;
#35307 = CARTESIAN_POINT ( 'NONE',  ( 115.1244435679684699, -31.12738977229718884, 279.3099109901971815 ) ) ;
#35308 = CARTESIAN_POINT ( 'NONE',  ( 117.9712535577395869, -34.78749165583555225, 194.9546728949589749 ) ) ;
#35309 = DIRECTION ( 'NONE',  ( 0.000000000000000000, 1.000000000000000000, 0.000000000000000000 ) ) ;
#35310 = CARTESIAN_POINT ( 'NONE',  ( -109.2774118001976120, 53.97500000000000142, 71.43750000000000000 ) ) ;
#35311 = CARTESIAN_POINT ( 'NONE',  ( 116.7955140328789412, -32.98399009599280873, 135.1184824187679396 ) ) ;
#35312 = CARTESIAN_POINT ( 'NONE',  ( 33.96670390244699433, -26.71338133339301635, -5.074374724088000832 ) ) ;
#35313 = EDGE_LOOP ( 'NONE', ( #36570, #55621, #36881, #71674 ) ) ;
#35314 = CARTESIAN_POINT ( 'NONE',  ( -30.89999999999999858, 53.97500000000000142, 70.79999999999999716 ) ) ;
#35315 = EDGE_CURVE ( 'NONE', #71030, #70034, #64017, .T. ) ;
#35316 = ADVANCED_FACE ( 'NONE', ( #30385 ), #58516, .T. ) ;
#35317 = CARTESIAN_POINT ( 'NONE',  ( 51.06648329127400388, 19.62155284005901024, 333.4006252759110112 ) ) ;
#35318 = VERTEX_POINT ( 'NONE', #3127 ) ;
#35319 = EDGE_CURVE ( 'NONE', #76564, #86303, #86244, .T. ) ;
#35320 = VECTOR ( 'NONE', #31099, 1000.000000000000000 ) ;
#35321 = CARTESIAN_POINT ( 'NONE',  ( 41.56648329127381203, -18.82844715994071194, 201.9256252759118979 ) ) ;
#35322 = APPLICATION_CONTEXT ( 'automotive_design' ) ;
#35323 = LINE ( 'NONE', #71220, #27569 ) ;
#35324 = CARTESIAN_POINT ( 'NONE',  ( 100.4790876285538275, -27.85333844968608830, 35.59657765686397113 ) ) ;
#35325 = DIRECTION ( 'NONE',  ( -0.000000000000000000, -0.000000000000000000, -1.000000000000000000 ) ) ;
#35326 = CIRCLE ( 'NONE', #70160, 4.875000000000017764 ) ;
#35327 = ADVANCED_FACE ( 'NONE', ( #79892 ), #24024, .T. ) ;
#35328 = LINE ( 'NONE', #13119, #10034 ) ;
#35329 = DIRECTION ( 'NONE',  ( 0.7071067811873671394, 0.7071067811857280061, 6.612322855862553737E-17 ) ) ;
#35330 = CARTESIAN_POINT ( 'NONE',  ( 112.5471327968798221, -30.46552556802231138, 288.9257531614101708 ) ) ;
#35332 = CARTESIAN_POINT ( 'NONE',  ( 96.04673288144557830, -37.20790665022158805, 112.3489586092449599 ) ) ;
#35331 = CARTESIAN_POINT ( 'NONE',  ( 100.9543307028228583, -28.70728144113564539, 110.5939921354201374 ) ) ;
#35333 = LINE ( 'NONE', #8093, #24855 ) ;
#35334 = DIRECTION ( 'NONE',  ( 0.000000000000000000, 1.000000000000000000, 0.000000000000000000 ) ) ;
#35335 = VERTEX_POINT ( 'NONE', #1793 ) ;
#35336 = FACE_OUTER_BOUND ( 'NONE', #58497, .T. ) ;
#35337 = FACE_BOUND ( 'NONE', #42964, .T. ) ;
#35338 = FACE_OUTER_BOUND ( 'NONE', #67739, .T. ) ;
#35339 = ORIENTED_EDGE ( 'NONE', *, *, #36654, .T. ) ;
#35340 = ADVANCED_FACE ( 'NONE', ( #24466 ), #2240, .F. ) ;
#35341 = CARTESIAN_POINT ( 'NONE',  ( 92.82872956494375671, -30.11307588647346023, 9.425625275910956447 ) ) ;
#35343 = ORIENTED_EDGE ( 'NONE', *, *, #57648, .T. ) ;
#35342 = CARTESIAN_POINT ( 'NONE',  ( 95.86269369446621624, -32.71648115089089259, 176.0527681330539735 ) ) ;
#35344 = DIRECTION ( 'NONE',  ( 0.9825752044328148749, 0.1858654557302456822, 0.000000000000000000 ) ) ;
#35345 = CARTESIAN_POINT ( 'NONE',  ( 113.1126646695910409, -46.01001268607183903, 219.0480062282919960 ) ) ;
#35346 = CARTESIAN_POINT ( 'NONE',  ( 104.4799455178094405, -46.91020534057368963, 43.37848241876896083 ) ) ;
#35347 = CARTESIAN_POINT ( 'NONE',  ( 77.65064691800776586, -139.0649736490145187, 247.5503376965620532 ) ) ;
#35348 = CARTESIAN_POINT ( 'NONE',  ( 160.2664750769284865, 101.5999999999999943, -148.0533267522753818 ) ) ;
#35349 = ADVANCED_FACE ( 'NONE', ( #78991 ), #16312, .T. ) ;
#35350 = CARTESIAN_POINT ( 'NONE',  ( 90.44969454456416713, -53.34645651782494724, 218.8274735512160589 ) ) ;
#35351 = ORIENTED_EDGE ( 'NONE', *, *, #53648, .F. ) ;
#35352 = B_SPLINE_CURVE_WITH_KNOTS ( 'NONE', 3,
 ( #50446, #50899, #60385, #4989, #47191, #26327, #80410, #33586, #67206, #82210, #87221, #61284, #19966, #54443, #74931, #53553, #81321, #67665, #52653, #68564, #89007, #19065, #59932, #47645, #75380, #18161, #25427, #26761, #45845 ),
 .UNSPECIFIED., .F., .F.,
 ( 4, 2, 2, 2, 2, 2, 2, 2, 2, 2, 1, 1, 1, 1, 1, 2, 4 ),
 ( 0.000000000000000000, 0.06250186238324358101, 0.1250037247664871620, 0.1875055871497307569, 0.2500074495329743240, 0.3125093119162178912, 0.3750111742994615138, 0.4375130366827050810, 0.4687639678743268368, 0.4843894334701378535, 0.4922021662680436394, 0.4961085326669965601, 0.4980617158664727984, 0.4990383074662109175, 0.4995266032660801714, 0.4997707511660147706, 0.5000148990659494252 ),
 .UNSPECIFIED. ) ;
#35353 = CONICAL_SURFACE ( 'NONE', #86142, 1.624999999999987566, 1.029744258676650093 ) ;
#35354 = AXIS2_PLACEMENT_3D ( 'NONE', #7672, #41273, #1761 ) ;
#35355 = ORIENTED_EDGE ( 'NONE', *, *, #16889, .T. ) ;
#35356 = ORIENTED_EDGE ( 'NONE', *, *, #35217, .F. ) ;
#35357 = VECTOR ( 'NONE', #53451, 1000.000000000000000 ) ;
#35358 = ORIENTED_EDGE ( 'NONE', *, *, #19109, .T. ) ;
#35359 = CARTESIAN_POINT ( 'NONE',  ( 49.16670390244738797, -26.71338133339273924, 313.9678068554150059 ) ) ;
#35360 = CARTESIAN_POINT ( 'NONE',  ( 113.7992560408602145, -26.97729936261201900, 235.5956252759109759 ) ) ;
#35361 = LINE ( 'NONE', #69901, #5464 ) ;
#35362 = CARTESIAN_POINT ( 'NONE',  ( 31.56670390244800828, -33.35206098992711077, 313.9678068554150059 ) ) ;
#35363 = EDGE_CURVE ( 'NONE', #42590, #33552, #77904, .T. ) ;
#35366 = EDGE_CURVE ( 'NONE', #32980, #54776, #48021, .T. ) ;
#35365 = CARTESIAN_POINT ( 'NONE',  ( 107.0664832912739399, -36.72944715994095333, 294.6356252759106837 ) ) ;
#35364 = DIRECTION ( 'NONE',  ( 0.000000000000000000, -1.000000000000000000, 0.000000000000000000 ) ) ;
#35367 = LINE ( 'NONE', #14949, #41381 ) ;
#35368 = CARTESIAN_POINT ( 'NONE',  ( 109.6173639926175269, -25.13086864565549661, 29.90419670448196854 ) ) ;
#35369 = ORIENTED_EDGE ( 'NONE', *, *, #40169, .T. ) ;
#35370 = ORIENTED_EDGE ( 'NONE', *, *, #66045, .T. ) ;
#35371 = DIRECTION ( 'NONE',  ( -0.8660254037844382635, -0.5000000000000008882, 1.550000000000000022E-14 ) ) ;
#35372 = DIRECTION ( 'NONE',  ( 1.000000000000000000, 0.000000000000000000, 0.000000000000000000 ) ) ;
#35373 = CARTESIAN_POINT ( 'NONE',  ( 116.8464009251321301, -35.91275531464980730, 249.8927681330532664 ) ) ;
#35374 = DIRECTION ( 'NONE',  ( -0.8660254037844387076, 0.000000000000000000, 0.4999999999999998890 ) ) ;
#35375 = CARTESIAN_POINT ( 'NONE',  ( 117.1895451461016648, -38.97942580829903392, 99.64038718067195077 ) ) ;
#35376 = CARTESIAN_POINT ( 'NONE',  ( -97.46299999999996544, 82.54999999999999716, -3.402902457276681768E-13 ) ) ;
#35377 = CARTESIAN_POINT ( 'NONE',  ( 116.3162594664470788, -32.94075446336835000, 20.13562527591095019 ) ) ;
#35378 = EDGE_LOOP ( 'NONE', ( #33638, #30208, #4732, #51242 ) ) ;
#35379 = LINE ( 'NONE', #5911, #8059 ) ;
#35380 = ORIENTED_EDGE ( 'NONE', *, *, #17599, .F. ) ;
#35381 = ORIENTED_EDGE ( 'NONE', *, *, #51621, .T. ) ;
#35382 = CARTESIAN_POINT ( 'NONE',  ( -92.07164801315005320, 85.85031469618033384, 74.68844285250203541 ) ) ;
#35383 = CARTESIAN_POINT ( 'NONE',  ( 101.2707639275114815, -30.02587231748817231, 257.0758690201828927 ) ) ;
#35385 = EDGE_CURVE ( 'NONE', #26589, #64680, #12176, .T. ) ;
#35384 = CIRCLE ( 'NONE', #57104, 0.4999999999999982236 ) ;
#35386 = CARTESIAN_POINT ( 'NONE',  ( 104.4081005726111187, -46.45808911662692964, 192.3647919353561804 ) ) ;
#35387 = DIRECTION ( 'NONE',  ( 0.000000000000000000, 0.000000000000000000, -1.000000000000000000 ) ) ;
#35388 = VECTOR ( 'NONE', #78713, 1000.000000000000000 ) ;
#35389 = CARTESIAN_POINT ( 'NONE',  ( 104.4899544645860061, -26.97880758150905223, 85.28145860822031921 ) ) ;
#35390 = DIRECTION ( 'NONE',  ( -1.000000000000000000, 0.000000000000000000, 0.000000000000000000 ) ) ;
#35391 = ORIENTED_EDGE ( 'NONE', *, *, #8903, .F. ) ;
#35392 = DIRECTION ( 'NONE',  ( 0.000000000000000000, 0.000000000000000000, 1.000000000000000000 ) ) ;
#35393 = LINE ( 'NONE', #68594, #62905 ) ;
#35394 = EDGE_LOOP ( 'NONE', ( #7737, #25033, #6045, #61254 ) ) ;
#35395 = CARTESIAN_POINT ( 'NONE',  ( 100.9409889914183225, -46.87433776650586736, 52.14419670448194921 ) ) ;
#35396 = EDGE_LOOP ( 'NONE', ( #37706, #28869, #47646, #23829 ) ) ;
#35397 = CARTESIAN_POINT ( 'NONE',  ( 98.90470121413369498, -39.24767091914073802, 20.98670554236298358 ) ) ;
#35398 = CARTESIAN_POINT ( 'NONE',  ( 6.938893903907229955E-15, 50.79999999999999716, 209.1689999999999827 ) ) ;
#35399 = CARTESIAN_POINT ( 'NONE',  ( 109.2982854457139581, -26.60236246699145113, 179.8918157521019339 ) ) ;
#35400 = CARTESIAN_POINT ( 'NONE',  ( 107.0667039024469886, -70.87844715994094713, 173.2178068554179902 ) ) ;
#35401 = LINE ( 'NONE', #901, #58852 ) ;
#35402 = DIRECTION ( 'NONE',  ( 0.000000000000000000, 0.000000000000000000, 1.000000000000000000 ) ) ;
#35403 = LINE ( 'NONE', #77215, #62466 ) ;
#35404 = EDGE_CURVE ( 'NONE', #11233, #1571, #48816, .T. ) ;
#35405 = CARTESIAN_POINT ( 'NONE',  ( 111.8841015539045713, -46.06371569386821818, 268.9556252759110180 ) ) ;
#35406 = CARTESIAN_POINT ( 'NONE',  ( 101.5000928429637526, -45.09554281357727490, 117.1111000679451735 ) ) ;
#35407 = ORIENTED_EDGE ( 'NONE', *, *, #50231, .T. ) ;
#35408 = CARTESIAN_POINT ( 'NONE',  ( 136.4532669483771485, -38.09809895854112227, 7.205238605741180358 ) ) ;
#35409 = AXIS2_PLACEMENT_3D ( 'NONE', #48443, #13963, #27588 ) ;
#35410 = ORIENTED_EDGE ( 'NONE', *, *, #61194, .F. ) ;
#35411 = CARTESIAN_POINT ( 'NONE',  ( 106.0723295733845362, -48.58789440604735432, 108.5099109901969712 ) ) ;
#35412 = DIRECTION ( 'NONE',  ( 0.000000000000000000, 1.000000000000000000, 0.000000000000000000 ) ) ;
#35413 = AXIS2_PLACEMENT_3D ( 'NONE', #66162, #46153, #45701 ) ;
#35414 = ORIENTED_EDGE ( 'NONE', *, *, #24527, .F. ) ;
#35415 = DIRECTION ( 'NONE',  ( 0.000000000000000000, 1.000000000000000000, 0.000000000000000000 ) ) ;
#35417 = EDGE_CURVE ( 'NONE', #79159, #22206, #5818, .T. ) ;
#35416 = ORIENTED_EDGE ( 'NONE', *, *, #558, .T. ) ;
#35419 = VERTEX_POINT ( 'NONE', #12625 ) ;
#35418 = EDGE_CURVE ( 'NONE', #35754, #60336, #72066, .T. ) ;
#35420 = DIRECTION ( 'NONE',  ( 0.9999999853157766072, 0.0001713722456134972175, 0.000000000000000000 ) ) ;
#35421 = EDGE_CURVE ( 'NONE', #25045, #59341, #76401, .T. ) ;
#35422 = CARTESIAN_POINT ( 'NONE',  ( 97.06106854294668551, -37.99639079834587108, 267.4272902591680463 ) ) ;
#35423 = CARTESIAN_POINT ( 'NONE',  ( 69.67078994678415427, -0.9293259921821603875, 540.9756252759101471 ) ) ;
#35424 = DIRECTION ( 'NONE',  ( 0.000000000000000000, -1.000000000000000000, 0.000000000000000000 ) ) ;
#35425 = CARTESIAN_POINT ( 'NONE',  ( 68.53801554307449351, 120.6499999999999915, -74.15067561874229796 ) ) ;
#35426 = CARTESIAN_POINT ( 'NONE',  ( 110.9006160922534150, -26.97349402997008383, 265.7784824187680783 ) ) ;
#35427 = PLANE ( 'NONE',  #42147 ) ;
#35428 = VERTEX_POINT ( 'NONE', #18986 ) ;
#35429 = DIRECTION ( 'NONE',  ( 3.100000000000000258E-29, -3.100000000000000044E-14, -1.000000000000000000 ) ) ;
#35430 = EDGE_CURVE ( 'NONE', #88399, #24119, #46213, .T. ) ;
#35431 = CARTESIAN_POINT ( 'NONE',  ( 116.3212776292271258, -32.94146857470711609, 44.13562527591097506 ) ) ;
#35432 = ORIENTED_EDGE ( 'NONE', *, *, #73566, .F. ) ;
#35433 = ORIENTED_EDGE ( 'NONE', *, *, #15046, .T. ) ;
#35434 = EDGE_CURVE ( 'NONE', #3872, #54700, #53145, .T. ) ;
#35435 = CARTESIAN_POINT ( 'NONE',  ( 82.27374021058859910, -20.37320971852071594, 2.471387388688038644 ) ) ;
#35436 = DIRECTION ( 'NONE',  ( -3.100000000000000258E-29, 3.100000000000000044E-14, 1.000000000000000000 ) ) ;
#35437 = CARTESIAN_POINT ( 'NONE',  ( 108.4174480110805661, -26.73502967738932767, 14.96896184951245345 ) ) ;
#35438 = CARTESIAN_POINT ( 'NONE',  ( 143.0664832912740110, -18.82844715994099971, 17.92562527591199739 ) ) ;
#35439 = LINE ( 'NONE', #82285, #46080 ) ;
#35440 = EDGE_CURVE ( 'NONE', #42953, #74494, #54610, .T. ) ;
#35441 = CARTESIAN_POINT ( 'NONE',  ( 104.3272728202184538, -28.09756461201434874, 204.7314674471249702 ) ) ;
#35442 = CARTESIAN_POINT ( 'NONE',  ( 127.0239848601436563, 54.68407512302287188, 30.16250000000001563 ) ) ;
#35443 = CARTESIAN_POINT ( 'NONE',  ( 107.6054179116733707, -26.23843464447702090, 95.03562527591097364 ) ) ;
#35444 = ORIENTED_EDGE ( 'NONE', *, *, #72598, .F. ) ;
#35445 = DIRECTION ( 'NONE',  ( 1.000000000000000000, 1.765660420430506939E-15, 0.000000000000000000 ) ) ;
#35446 = ORIENTED_EDGE ( 'NONE', *, *, #47258, .T. ) ;
#35447 = CARTESIAN_POINT ( 'NONE',  ( -80.88853703239314541, 70.52018178143197247, -86.67600044576322205 ) ) ;
#35448 = VERTEX_POINT ( 'NONE', #24909 ) ;
#35449 = CARTESIAN_POINT ( 'NONE',  ( 115.8245126124521391, -31.72842839644282620, 260.2397945930957803 ) ) ;
#35450 = VERTEX_POINT ( 'NONE', #32599 ) ;
#35451 = CARTESIAN_POINT ( 'NONE',  ( 107.0667036193247696, -67.87844715994094713, 90.21780599115065513 ) ) ;
#35452 = CARTESIAN_POINT ( 'NONE',  ( -31.75000000000000000, 8.255000000000000782, 3.175000000000219647 ) ) ;
#35453 = CARTESIAN_POINT ( 'NONE',  ( 108.3350409249663926, -46.73467830386606181, 273.6769742538326682 ) ) ;
#35454 = VECTOR ( 'NONE', #53085, 1000.000000000000000 ) ;
#35455 = FACE_OUTER_BOUND ( 'NONE', #84833, .T. ) ;
#35456 = ORIENTED_EDGE ( 'NONE', *, *, #12572, .T. ) ;
#35457 = CARTESIAN_POINT ( 'NONE',  ( 118.1065893711158594, -37.63027948749972751, 38.77372051400595865 ) ) ;
#35458 = AXIS2_PLACEMENT_3D ( 'NONE', #15373, #58030, #78503 ) ;
#35460 = DIRECTION ( 'NONE',  ( 0.7071067811865779928, -0.7071067811865171526, 7.071067811865786933E-16 ) ) ;
#35459 = CYLINDRICAL_SURFACE ( 'NONE', #24577, 2.117000000000000881 ) ;
#35461 = CARTESIAN_POINT ( 'NONE',  ( 107.0667039024470313, -104.2784471599409528, 19.21780685541800437 ) ) ;
#35462 = CARTESIAN_POINT ( 'NONE',  ( 132.3549177285000269, -16.56918551487757085, 2.099346190920966748 ) ) ;
#35463 = VERTEX_POINT ( 'NONE', #46670 ) ;
#35464 = LINE ( 'NONE', #29120, #75034 ) ;
#35465 = FACE_OUTER_BOUND ( 'NONE', #85146, .T. ) ;
#35466 = DIRECTION ( 'NONE',  ( 0.000000000000000000, 0.000000000000000000, -1.000000000000000000 ) ) ;
#35467 = CARTESIAN_POINT ( 'NONE',  ( 113.8705839548662908, -44.65670854160515546, 104.1413395616249744 ) ) ;
#35470 = EDGE_CURVE ( 'NONE', #86726, #10270, #73493, .T. ) ;
#35469 = LINE ( 'NONE', #55899, #63034 ) ;
#35468 = DIRECTION ( 'NONE',  ( 0.000000000000000000, 0.000000000000000000, 1.000000000000000000 ) ) ;
#35471 = CARTESIAN_POINT ( 'NONE',  ( 56.06670390244699576, -67.87844715994098976, 190.2178068554179902 ) ) ;
#35472 = AXIS2_PLACEMENT_3D ( 'NONE', #8934, #8018, #9360 ) ;
#35473 = VERTEX_POINT ( 'NONE', #63454 ) ;
#35474 = VECTOR ( 'NONE', #57255, 1000.000000000000000 ) ;
#35475 = VECTOR ( 'NONE', #14506, 1000.000000000000000 ) ;
#35476 = VECTOR ( 'NONE', #54641, 1000.000000000000000 ) ;
#35477 = LINE ( 'NONE', #85009, #8515 ) ;
#35478 = CARTESIAN_POINT ( 'NONE',  ( 114.2526777242400726, -43.36435822665418982, 119.2327681330529714 ) ) ;
#35480 = ORIENTED_EDGE ( 'NONE', *, *, #77095, .T. ) ;
#35479 = DIRECTION ( 'NONE',  ( -1.000000000000000000, -1.181088324069315053E-15, 0.000000000000000000 ) ) ;
#35481 = VECTOR ( 'NONE', #75016, 1000.000000000000000 ) ;
#35482 = AXIS2_PLACEMENT_3D ( 'NONE', #62750, #84571, #63659 ) ;
#35483 = CARTESIAN_POINT ( 'NONE',  ( 118.3173389373706925, -33.08695204176930105, 280.0756252759109657 ) ) ;
#35484 = CARTESIAN_POINT ( 'NONE',  ( 98.15039990372359568, -41.26047703464855232, 252.7008027240838999 ) ) ;
#35485 = PLANE ( 'NONE',  #86732 ) ;
#35486 = CARTESIAN_POINT ( 'NONE',  ( 82.54999999999999716, 69.84999999999999432, 280.2255000000000109 ) ) ;
#35487 = CYLINDRICAL_SURFACE ( 'NONE', #42734, 7.143750000000004263 ) ;
#35488 = CARTESIAN_POINT ( 'NONE',  ( 68.96011658976357239, -139.1256438676158780, 247.0684195519230002 ) ) ;
#35489 = PLANE ( 'NONE',  #9484 ) ;
#35490 = CARTESIAN_POINT ( 'NONE',  ( 96.12852455334814294, -38.72269610271991525, 201.4699109901969791 ) ) ;
#35491 = VERTEX_POINT ( 'NONE', #21232 ) ;
#35492 = ORIENTED_EDGE ( 'NONE', *, *, #38684, .F. ) ;
#35493 = CARTESIAN_POINT ( 'NONE',  ( 100.5685618138929271, -29.03188392736010570, 147.0672975916109806 ) ) ;
#35494 = ADVANCED_FACE ( 'NONE', ( #1240 ), #7603, .T. ) ;
#35495 = DIRECTION ( 'NONE',  ( -0.9347835805883503157, 0.000000000000000000, 0.3552177606235690788 ) ) ;
#35496 = CARTESIAN_POINT ( 'NONE',  ( 115.8371248229627639, -37.99598801341877419, 25.14444044875396855 ) ) ;
#35497 = CARTESIAN_POINT ( 'NONE',  ( 226.4410000000000025, 40.03750000000000142, 10.66800000000000104 ) ) ;
#35498 = AXIS2_PLACEMENT_3D ( 'NONE', #72443, #59239, #72002 ) ;
#35499 = DIRECTION ( 'NONE',  ( 0.7071067811575898476, -0.7071067812155052978, 0.000000000000000000 ) ) ;
#35500 = CARTESIAN_POINT ( 'NONE',  ( 3.174999999999879918, 111.1250000000000000, 33.98325472291465132 ) ) ;
#35501 = DIRECTION ( 'NONE',  ( 0.1858654558203329255, -0.9825752044157738396, 0.000000000000000000 ) ) ;
#35502 = DIRECTION ( 'NONE',  ( 0.7071067811865507924, 0.7071067811865441310, -0.000000000000000000 ) ) ;
#35503 = CARTESIAN_POINT ( 'NONE',  ( 105.1150531980676277, -26.51080800785435443, 235.2270538473399313 ) ) ;
#35504 = CARTESIAN_POINT ( 'NONE',  ( 5.580981516429890377, 93.85413957563092424, 118.2249067917183396 ) ) ;
#35505 = ORIENTED_EDGE ( 'NONE', *, *, #82944, .F. ) ;
#35506 = ORIENTED_EDGE ( 'NONE', *, *, #7673, .T. ) ;
#35507 = CARTESIAN_POINT ( 'NONE',  ( 52.38749999999999574, 94.53880000000000905, 250.8250000000000171 ) ) ;
#35508 = CARTESIAN_POINT ( 'NONE',  ( 82.76352869194700190, -19.26660482608858160, 6.827192804310135976 ) ) ;
#35509 = CARTESIAN_POINT ( 'NONE',  ( 97.81262911421374895, -40.51702269960655656, 122.6351715870756323 ) ) ;
#35510 = LINE ( 'NONE', #14649, #34629 ) ;
#35512 = CARTESIAN_POINT ( 'NONE',  ( 104.6499073705539473, -46.24122592705968771, 43.37848241876795896 ) ) ;
#35511 = VECTOR ( 'NONE', #89681, 1000.000000000000000 ) ;
#35513 = LINE ( 'NONE', #63689, #60035 ) ;
#35514 = ORIENTED_EDGE ( 'NONE', *, *, #87438, .T. ) ;
#35515 = CARTESIAN_POINT ( 'NONE',  ( 96.29945253806019423, -39.42498279898523350, 12.53372051400597442 ) ) ;
#35516 = CARTESIAN_POINT ( 'NONE',  ( 180.1667039024474377, -28.27351298636767396, 313.9678068554149490 ) ) ;
#35517 = AXIS2_PLACEMENT_3D ( 'NONE', #69772, #42486, #29339 ) ;
#35518 = CARTESIAN_POINT ( 'NONE',  ( 116.0552987087602048, -42.01037774571695849, 238.4041967044829562 ) ) ;
#35520 = ORIENTED_EDGE ( 'NONE', *, *, #52777, .T. ) ;
#35519 = ADVANCED_FACE ( 'NONE', ( #14877 ), #76640, .T. ) ;
#35521 = ADVANCED_FACE ( 'NONE', ( #41201 ), #62997, .T. ) ;
#35522 = CARTESIAN_POINT ( 'NONE',  ( 77.41433294703958268, -37.45719076514816948, 6.889371645759243989 ) ) ;
#35523 = DIRECTION ( 'NONE',  ( 0.000000000000000000, 1.000000000000000000, 0.000000000000000000 ) ) ;
#35524 = ADVANCED_FACE ( 'NONE', ( #68928 ), #47565, .F. ) ;
#35525 = CARTESIAN_POINT ( 'NONE',  ( 116.3159136950847170, -32.94903743517052419, 150.1356252759109680 ) ) ;
#35526 = CARTESIAN_POINT ( 'NONE',  ( 107.6943352634791182, -28.59092592337147209, 67.83380465530596837 ) ) ;
#35527 = CARTESIAN_POINT ( 'NONE',  ( 117.0439256081559165, -39.94344854842797332, 154.5784824187679476 ) ) ;
#35528 = CARTESIAN_POINT ( 'NONE',  ( 33.98325472291465132, 17.78000000000000114, 3.174999999999999822 ) ) ;
#35529 = ORIENTED_EDGE ( 'NONE', *, *, #3959, .T. ) ;
#35530 = EDGE_CURVE ( 'NONE', #38211, #43566, #82258, .T. ) ;
#35531 = CARTESIAN_POINT ( 'NONE',  ( 34.33598329127499227, -36.32844715994100682, -5.074374724088000832 ) ) ;
#35532 = ORIENTED_EDGE ( 'NONE', *, *, #36972, .F. ) ;
#35533 = ORIENTED_EDGE ( 'NONE', *, *, #61915, .T. ) ;
#35534 = VECTOR ( 'NONE', #38387, 1000.000000000000114 ) ;
#35535 = AXIS2_PLACEMENT_3D ( 'NONE', #11242, #46641, #26217 ) ;
#35536 = CARTESIAN_POINT ( 'NONE',  ( 167.6524903400755306, -48.32844715993520879, 180.4678068554150059 ) ) ;
#35537 = CIRCLE ( 'NONE', #64546, 2.517500000000005844 ) ;
#35538 = ORIENTED_EDGE ( 'NONE', *, *, #22128, .T. ) ;
#35539 = ORIENTED_EDGE ( 'NONE', *, *, #65176, .F. ) ;
#35540 = LINE ( 'NONE', #22836, #51212 ) ;
#35541 = VECTOR ( 'NONE', #75537, 1000.000000000000000 ) ;
#35542 = CARTESIAN_POINT ( 'NONE',  ( 6.123233995736768255E-16, 223.9999999999999716, 149.6557476874258441 ) ) ;
#35543 = EDGE_CURVE ( 'NONE', #65069, #82508, #31447, .T. ) ;
#35544 = CARTESIAN_POINT ( 'NONE',  ( 104.0317209996959065, -45.26190801010356779, 101.7390864947439724 ) ) ;
#35546 = CARTESIAN_POINT ( 'NONE',  ( 99.38058175836560793, -28.75308465796231516, 265.6746728949588032 ) ) ;
#35545 = AXIS2_PLACEMENT_3D ( 'NONE', #30785, #46627, #73007 ) ;
#35547 = CARTESIAN_POINT ( 'NONE',  ( 101.4371718687637838, -46.21494532752030437, 207.1622919425779514 ) ) ;
#35548 = B_SPLINE_CURVE_WITH_KNOTS ( 'NONE', 3,
 ( #71882, #44590, #65058, #2841, #36903, #10097, #63718, #23737, #84627, #8766, #57789, #58239, #79598, #85967, #37802, #65502, #29640, #3286, #30977, #51845, #17357, #45038, #72768, #10537, #1499 ),
 .UNSPECIFIED., .F., .F.,
 ( 4, 2, 2, 2, 2, 2, 2, 2, 2, 1, 2, 2, 4 ),
 ( 2.608264963112508895E-18, 0.002483666291998854608, 0.003725499437998279744, 0.004967332583997703145, 0.007450998875996568162, 0.008692832021995991129, 0.009934665167995411494, 0.01241833145999425222, 0.01366016460599367086, 0.01490199775199309122, 0.01614383089799251159, 0.01738566404399193022, 0.01986933033599076748 ),
 .UNSPECIFIED. ) ;
#35549 = CARTESIAN_POINT ( 'NONE',  ( -160.2664750769284865, 20.32000000000000028, 148.0533267522753818 ) ) ;
#35550 = B_SPLINE_CURVE_WITH_KNOTS ( 'NONE', 3,
 ( #64308, #63861, #42938, #85216, #16160, #55653, #71576, #22091, #8447, #37039, #7550, #49756, #56111, #43839, #35688, #720, #281, #83404, #70672 ),
 .UNSPECIFIED., .F., .F.,
 ( 4, 2, 2, 2, 1, 1, 1, 2, 2, 2, 4 ),
 ( 0.000000000000000000, 0.2499999999998125944, 0.3749999999997070121, 0.4374999999996485589, 0.4687499999996253552, 0.4843749999996137534, 0.4921874999995934363, 0.4960937499995964339, 0.4999999999995994315, 0.7499999999997997158, 1.000000000000000000 ),
 .UNSPECIFIED. ) ;
#35551 = CARTESIAN_POINT ( 'NONE',  ( 109.6407213914652345, -46.48066322255345284, 93.78127252070859754 ) ) ;
#35552 = ORIENTED_EDGE ( 'NONE', *, *, #69111, .T. ) ;
#35553 = CARTESIAN_POINT ( 'NONE',  ( 131.0667039024480687, -58.72944715994092491, 231.5838068554170093 ) ) ;
#35554 = CARTESIAN_POINT ( 'NONE',  ( 156.5667039024480971, -42.82844715993568485, 290.7178068554149490 ) ) ;
#35555 = CARTESIAN_POINT ( 'NONE',  ( 142.8679068202682458, 10.65431904611001634, 542.9756252759101471 ) ) ;
#35556 = VECTOR ( 'NONE', #22323, 1000.000000000000000 ) ;
#35557 = CARTESIAN_POINT ( 'NONE',  ( 98.98846131648976154, -42.30253745798197684, 126.8070538473399580 ) ) ;
#35558 = CARTESIAN_POINT ( 'NONE',  ( 96.04102276344947597, -38.01478905114413465, 86.43086337114897333 ) ) ;
#35559 = CARTESIAN_POINT ( 'NONE',  ( 118.7030916724021665, -39.22306760090339139, 258.6584824187677896 ) ) ;
#35560 = VERTEX_POINT ( 'NONE', #6254 ) ;
#35561 = CARTESIAN_POINT ( 'NONE',  ( 115.8553914792215380, -44.67901184617146981, 233.2413395616259493 ) ) ;
#35562 = FACE_OUTER_BOUND ( 'NONE', #82704, .T. ) ;
#35563 = CARTESIAN_POINT ( 'NONE',  ( 12.38957946698288026, 79.72838755146472067, 129.9671884813441807 ) ) ;
#35564 = CARTESIAN_POINT ( 'NONE',  ( 130.5667039024480118, -36.72944715994093912, 218.0711402470151370 ) ) ;
#35565 = VECTOR ( 'NONE', #11908, 1000.000000000000000 ) ;
#35567 = DIRECTION ( 'NONE',  ( 1.000000000000000078E-15, -1.000000000000000083E-30, -1.000000000000000000 ) ) ;
#35566 = CARTESIAN_POINT ( 'NONE',  ( 107.8173249548519692, -46.71069529603006032, 277.6356222035115024 ) ) ;
#35568 = CARTESIAN_POINT ( 'NONE',  ( 105.1200014541032601, -25.43661125475656704, 321.6731097870184044 ) ) ;
#35569 = DIRECTION ( 'NONE',  ( 0.000000000000000000, -1.000000000000000000, 0.000000000000000000 ) ) ;
#35570 = DIRECTION ( 'NONE',  ( 0.000000000000000000, 0.000000000000000000, -1.000000000000000000 ) ) ;
#35571 = DIRECTION ( 'NONE',  ( 0.000000000000000000, 0.000000000000000000, 1.000000000000000000 ) ) ;
#35572 = DIRECTION ( 'NONE',  ( 1.000000000000000078E-15, -1.000000000000000000, 0.000000000000000000 ) ) ;
#35573 = LINE ( 'NONE', #84205, #75308 ) ;
#35575 = ORIENTED_EDGE ( 'NONE', *, *, #88582, .T. ) ;
#35574 = DIRECTION ( 'NONE',  ( 1.000000000000000000, 0.000000000000000000, 0.000000000000000000 ) ) ;
#35576 = CARTESIAN_POINT ( 'NONE',  ( 92.53858863555701930, -127.7054288962555830, 250.2178068554179902 ) ) ;
#35577 = CARTESIAN_POINT ( 'NONE',  ( 109.9954698844069156, -26.70111721404902383, 259.8499109901965767 ) ) ;
#35578 = CARTESIAN_POINT ( 'NONE',  ( 102.3604841619309411, -46.03192315517718214, 123.2041967044829818 ) ) ;
#35579 = CARTESIAN_POINT ( 'NONE',  ( 112.1278237076712543, -26.87713336146359211, 15.71086337114896381 ) ) ;
#35580 = PLANE ( 'NONE',  #24374 ) ;
#35583 = EDGE_CURVE ( 'NONE', #37091, #87995, #21021, .T. ) ;
#35582 = DIRECTION ( 'NONE',  ( 0.000000000000000000, 0.000000000000000000, 1.000000000000000000 ) ) ;
#35581 = DIRECTION ( 'NONE',  ( 0.000000000000000000, -0.8660254037844390407, 0.4999999999999995004 ) ) ;
#35584 = CARTESIAN_POINT ( 'NONE',  ( 98.15094550295600584, -41.26155033938827188, 137.7007176044859307 ) ) ;
#35585 = PRESENTATION_LAYER_ASSIGNMENT (  '', '', ( #3690 ) ) ;
#35586 = AXIS2_PLACEMENT_3D ( 'NONE', #80400, #60373, #88112 ) ;
#35587 = ADVANCED_FACE ( 'NONE', ( #77099 ), #20779, .F. ) ;
#35588 = ORIENTED_EDGE ( 'NONE', *, *, #72694, .F. ) ;
#35589 = DIRECTION ( 'NONE',  ( -0.000000000000000000, 1.000000000000000000, 0.000000000000000000 ) ) ;
#35590 = ORIENTED_EDGE ( 'NONE', *, *, #58591, .T. ) ;
#35591 = B_SPLINE_CURVE_WITH_KNOTS ( 'NONE', 3,
 ( #71464, #50541, #37371, #65077, #1522, #36028, #50990, #30997, #86430, #9227, #78283, #16488, #79174, #58257, #79617, #9662, #23758, #2859, #30559, #17374, #85987, #8789, #16934, #70558, #8330, #63742, #56911, #50088, #77822, #15600, #25978, #73673, #52297, #11455, #10996, #81418, #38696, #80060 ),
 .UNSPECIFIED., .F., .F.,
 ( 4, 2, 2, 1, 2, 2, 2, 2, 1, 1, 2, 2, 2, 1, 2, 2, 1, 2, 1, 2, 2, 4 ),
 ( 0.000000000000000000, 0.04166793602361257287, 0.05208492002951500832, 0.05729341203246553910, 0.05989765803394084265, 0.06250190403541615314, 0.08333587204722690822, 0.1041698400590376355, 0.1145868240649424580, 0.1197953160678960766, 0.1223995620693742042, 0.1250038080708523180, 0.1666717440944873729, 0.1770887281003949987, 0.1822972201033483952, 0.1875057121063017640, 0.2083396801181268687, 0.2291736481299520012, 0.2395906321358649282, 0.2447991241388212946, 0.2500076161417776888, 0.3333434881890902091 ),
 .UNSPECIFIED. ) ;
#35592 = B_SPLINE_CURVE_WITH_KNOTS ( 'NONE', 3,
 ( #27860, #62825, #36026, #55538, #56452, #83292, #55993, #21971, #83739, #21516, #49186, #35568, #49637, #63739, #29222, #56909, #84645, #22409, #65518, #79615, #16932, #79172, #38693, #51423, #45055, #65953, #44610, #16045 ),
 .UNSPECIFIED., .F., .F.,
 ( 4, 2, 2, 2, 2, 2, 2, 2, 2, 2, 2, 2, 2, 4 ),
 ( 0.000000000000000000, 0.0002934189718615978055, 0.0005868379437231956109, 0.0008802569155847934706, 0.001173675887446391222, 0.001760513831169494784, 0.002347351774892598129, 0.002640770746754149152, 0.002934189718615699740, 0.003521027662338802652, 0.003814446634200298163, 0.004107865606061793240, 0.004401284577923288317, 0.004694703549784783395 ),
 .UNSPECIFIED. ) ;
#35593 = CARTESIAN_POINT ( 'NONE',  ( 99.16725398249624845, -41.15831232534042528, 181.1676579233149482 ) ) ;
#35595 = ORIENTED_EDGE ( 'NONE', *, *, #72825, .F. ) ;
#35594 = DIRECTION ( 'NONE',  ( 0.000000000000000000, -1.000000000000000000, -8.792068030499130893E-15 ) ) ;
#35596 = CARTESIAN_POINT ( 'NONE',  ( 147.0667039024470171, -79.67844715994090166, 96.96780685541800437 ) ) ;
#35597 = CARTESIAN_POINT ( 'NONE',  ( 97.69433714244412670, -41.24514667321082584, 167.6841967044829573 ) ) ;
#35598 = CARTESIAN_POINT ( 'NONE',  ( 115.0351528678677226, -42.91113197315783623, 149.3027457930269861 ) ) ;
#35599 = DIRECTION ( 'NONE',  ( 1.000000000000000078E-15, -1.000000000000000000, 0.000000000000000000 ) ) ;
#35600 = CARTESIAN_POINT ( 'NONE',  ( 114.8717157601983132, -30.43847619068483468, 85.36600443824613649 ) ) ;
#35601 = CARTESIAN_POINT ( 'NONE',  ( -79.76251016565881002, 71.15456258041352555, 87.71317827224459052 ) ) ;
#35602 = CARTESIAN_POINT ( 'NONE',  ( 31.56670390244700641, -22.48495420874110806, -5.074374724088000832 ) ) ;
#35603 = CARTESIAN_POINT ( 'NONE',  ( 116.7039036015866031, -32.90075090702271865, 99.13943479972198247 ) ) ;
#35604 = ORIENTED_EDGE ( 'NONE', *, *, #81399, .F. ) ;
#35605 = ORIENTED_EDGE ( 'NONE', *, *, #622, .T. ) ;
#35606 = EDGE_LOOP ( 'NONE', ( #44857, #54870, #58070, #61183 ) ) ;
#35607 = VECTOR ( 'NONE', #59503, 999.9999999999998863 ) ;
#35608 = CARTESIAN_POINT ( 'NONE',  ( 102.0296606431220994, -28.79805742369273958, 61.94634521065894717 ) ) ;
#35609 = EDGE_CURVE ( 'NONE', #86449, #65439, #35741, .T. ) ;
#35610 = VECTOR ( 'NONE', #28331, 1000.000000000000000 ) ;
#35611 = CYLINDRICAL_SURFACE ( 'NONE', #48621, 2.517499999999998739 ) ;
#35613 = DIRECTION ( 'NONE',  ( -1.000000000000000000, 0.000000000000000000, 0.000000000000000000 ) ) ;
#35612 = CARTESIAN_POINT ( 'NONE',  ( 114.3351522754912963, -30.13549343754564092, 205.4127681330539872 ) ) ;
#35614 = VECTOR ( 'NONE', #61775, 1000.000000000000000 ) ;
#35615 = LINE ( 'NONE', #77408, #30606 ) ;
#35616 = CARTESIAN_POINT ( 'NONE',  ( 141.8664832912729992, -1.929447159941394263, 342.9256252759109316 ) ) ;
#35618 = DIRECTION ( 'NONE',  ( -3.100000000000000258E-29, 3.100000000000000044E-14, 1.000000000000000000 ) ) ;
#35617 = VECTOR ( 'NONE', #4318, 1000.000000000000000 ) ;
#35619 = CARTESIAN_POINT ( 'NONE',  ( 142.8821648370248170, -72.54478064608022692, 542.9756252759101471 ) ) ;
#35620 = CARTESIAN_POINT ( 'NONE',  ( 68.14696562930211599, -68.91192709141064654, 247.2707748063552344 ) ) ;
#35621 = CARTESIAN_POINT ( 'NONE',  ( 102.3122812202564376, -27.43633205498510108, 120.4527681330539792 ) ) ;
#35622 = ORIENTED_EDGE ( 'NONE', *, *, #27074, .T. ) ;
#35623 = EDGE_LOOP ( 'NONE', ( #67040, #85913, #40967, #56173, #1996 ) ) ;
#35624 = ORIENTED_EDGE ( 'NONE', *, *, #38941, .T. ) ;
#35625 = VECTOR ( 'NONE', #14343, 1000.000000000000000 ) ;
#35626 = ORIENTED_CLOSED_SHELL ( 'NONE', *, #60448, .F. );
#35627 = CARTESIAN_POINT ( 'NONE',  ( -12.59999999999999964, 82.54999999999999716, 117.8845415480757595 ) ) ;
#35628 = DIRECTION ( 'NONE',  ( -0.7071067811866279529, 0.7071067811864671926, -7.071067811865978232E-16 ) ) ;
#35629 = CARTESIAN_POINT ( 'NONE',  ( 116.8171344286183029, -34.15294656915441607, 105.0314561802934321 ) ) ;
#35631 = CARTESIAN_POINT ( 'NONE',  ( 103.2852591291245830, -43.96353797031052579, 210.0109475124489506 ) ) ;
#35630 = AXIS2_PLACEMENT_3D ( 'NONE', #58173, #58603, #37286 ) ;
#35632 = B_SPLINE_CURVE_WITH_KNOTS ( 'NONE', 3,
 ( #50478, #38198, #43664, #65894, #29156, #56840, #84586, #9165, #36862, #22349, #52679, #73156, #12285, #80895, #67691, #32262, #80439, #38634, #67235, #18195, #45433, #10932, #59515, #45874, #54025, #60410, #88154, #59066, #3679 ),
 .UNSPECIFIED., .F., .F.,
 ( 4, 2, 1, 1, 1, 1, 1, 2, 2, 2, 2, 2, 2, 2, 2, 2, 4 ),
 ( 0.5000592588468526500, 0.5003033705368687967, 0.5005474822268849433, 0.5010357056069173476, 0.5020121523669820451, 0.5039650458871114402, 0.5078708329273705635, 0.5156824070078886990, 0.5313055551689245259, 0.5625518514909964018, 0.6250444441351398206, 0.6875370367792832393, 0.7500296294234265471, 0.8125222220675698548, 0.8750148147117132735, 0.9375074073558566923, 1.000000000000000000 ),
 .UNSPECIFIED. ) ;
#35633 = DIRECTION ( 'NONE',  ( -0.9963424814100679816, 0.08544974978095716545, 0.000000000000000000 ) ) ;
#35634 = AXIS2_PLACEMENT_3D ( 'NONE', #46294, #59484, #66303 ) ;
#35635 = DIRECTION ( 'NONE',  ( -3.999999999999999995E-14, 1.000000000000000000, -4.100000000000000342E-29 ) ) ;
#35636 = ORIENTED_EDGE ( 'NONE', *, *, #25443, .T. ) ;
#35638 = ORIENTED_EDGE ( 'NONE', *, *, #88125, .F. ) ;
#35637 = VERTEX_POINT ( 'NONE', #54817 ) ;
#35639 = DIRECTION ( 'NONE',  ( 0.000000000000000000, 0.000000000000000000, 1.000000000000000000 ) ) ;
#35640 = ORIENTED_EDGE ( 'NONE', *, *, #42514, .T. ) ;
#35641 = ORIENTED_EDGE ( 'NONE', *, *, #61973, .F. ) ;
#35642 = CARTESIAN_POINT ( 'NONE',  ( 78.34779240611281637, -20.87777042261386740, 7.743969477059374107 ) ) ;
#35643 = EDGE_CURVE ( 'NONE', #71592, #88986, #20341, .T. ) ;
#35644 = CARTESIAN_POINT ( 'NONE',  ( 114.7070687854681807, -41.21829243659817621, 234.8358690201829404 ) ) ;
#35645 = CARTESIAN_POINT ( 'NONE',  ( 172.5664832912729878, -27.82844715994070484, 198.9256252759119832 ) ) ;
#35646 = ORIENTED_EDGE ( 'NONE', *, *, #5615, .F. ) ;
#35647 = DIRECTION ( 'NONE',  ( -0.000000000000000000, -1.000000000000000000, -0.000000000000000000 ) ) ;
#35648 = AXIS2_PLACEMENT_3D ( 'NONE', #30432, #79036, #9987 ) ;
#35649 = CARTESIAN_POINT ( 'NONE',  ( -117.1541088471463041, 73.49112389501519260, 57.63291976239248271 ) ) ;
#35650 = ORIENTED_EDGE ( 'NONE', *, *, #40374, .F. ) ;
#35651 = ORIENTED_EDGE ( 'NONE', *, *, #9500, .F. ) ;
#35652 = DIRECTION ( 'NONE',  ( 0.7071067811865671127, 0.7071067811865279218, 7.071067811865664660E-16 ) ) ;
#35653 = ORIENTED_EDGE ( 'NONE', *, *, #27531, .T. ) ;
#35654 = ORIENTED_EDGE ( 'NONE', *, *, #39952, .T. ) ;
#35655 = EDGE_CURVE ( 'NONE', #58384, #35419, #75748, .T. ) ;
#35656 = CARTESIAN_POINT ( 'NONE',  ( 114.4813385407417741, -41.19272473522806166, 276.2014237029247852 ) ) ;
#35657 = CARTESIAN_POINT ( 'NONE',  ( 105.3125257651413307, -48.47460025707392361, 147.4584824187679715 ) ) ;
#35658 = CARTESIAN_POINT ( 'NONE',  ( 109.2504006710444315, -46.93703897017543625, 107.7441967044829880 ) ) ;
#35659 = CARTESIAN_POINT ( 'NONE',  ( 116.1386594504526357, -39.99393533005606827, 249.5838068554177482 ) ) ;
#35660 = ADVANCED_FACE ( 'NONE', ( #28028 ), #72516, .F. ) ;
#35661 = DIRECTION ( 'NONE',  ( 0.000000000000000000, 0.000000000000000000, 1.000000000000000000 ) ) ;
#35662 = CARTESIAN_POINT ( 'NONE',  ( 115.5173804941753133, -29.60510038635626273, 220.3718157521019521 ) ) ;
#35663 = DIRECTION ( 'NONE',  ( 0.000000000000000000, 0.000000000000000000, 1.000000000000000000 ) ) ;
#35664 = FACE_OUTER_BOUND ( 'NONE', #23124, .T. ) ;
#35665 = ORIENTED_EDGE ( 'NONE', *, *, #5103, .T. ) ;
#35666 = CARTESIAN_POINT ( 'NONE',  ( 130.4793906290846337, 70.66229531820916065, 4.488385961154077286 ) ) ;
#35667 = EDGE_LOOP ( 'NONE', ( #49450, #85341, #67039 ) ) ;
#35668 = VERTEX_POINT ( 'NONE', #23037 ) ;
#35669 = DIRECTION ( 'NONE',  ( 0.000000000000000000, 0.000000000000000000, 1.000000000000000000 ) ) ;
#35670 = VECTOR ( 'NONE', #60983, 1000.000000000000000 ) ;
#35671 = DIRECTION ( 'NONE',  ( -0.7071067811865789920, 0.7071067811865159314, 0.000000000000000000 ) ) ;
#35672 = AXIS2_PLACEMENT_3D ( 'NONE', #46307, #81331, #48098 ) ;
#35673 = ORIENTED_EDGE ( 'NONE', *, *, #10674, .T. ) ;
#35674 = AXIS2_PLACEMENT_3D ( 'NONE', #15073, #28232, #43202 ) ;
#35675 = CARTESIAN_POINT ( 'NONE',  ( 117.6792309033718027, -39.81954026856703877, 138.5889586092439743 ) ) ;
#35676 = CARTESIAN_POINT ( 'NONE',  ( 97.07216983056154902, -35.37748917612672273, 256.2188997677546922 ) ) ;
#35677 = VECTOR ( 'NONE', #34158, 1000.000000000000000 ) ;
#35678 = CARTESIAN_POINT ( 'NONE',  ( -148.0533267522752112, 101.5999999999999943, 160.2664750769289697 ) ) ;
#35679 = FACE_OUTER_BOUND ( 'NONE', #14398, .T. ) ;
#35682 = CARTESIAN_POINT ( 'NONE',  ( 111.1189502094634776, -27.14789314160936229, 240.7584824187679544 ) ) ;
#35681 = DIRECTION ( 'NONE',  ( 0.000000000000000000, 0.000000000000000000, 1.000000000000000000 ) ) ;
#35680 = DIRECTION ( 'NONE',  ( 1.000000000000000000, 0.000000000000000000, -0.000000000000000000 ) ) ;
#35683 = DIRECTION ( 'NONE',  ( -0.000000000000000000, 1.000000000000000000, -0.000000000000000000 ) ) ;
#35684 = CARTESIAN_POINT ( 'NONE',  ( 33.92127028473468187, -29.73316016639587644, 117.4678068554150485 ) ) ;
#35685 = CARTESIAN_POINT ( 'NONE',  ( 29.56648329127298069, 15.62155284005731204, 361.9756252759109998 ) ) ;
#35686 = DIRECTION ( 'NONE',  ( 0.000000000000000000, 1.000000000000000000, 0.000000000000000000 ) ) ;
#35687 = CARTESIAN_POINT ( 'NONE',  ( 108.4174892396751630, -26.73503592576763666, 255.9689586102375642 ) ) ;
#35688 = CARTESIAN_POINT ( 'NONE',  ( 146.7350708469755602, -137.4719268671379098, 246.6379283462439673 ) ) ;
#35690 = ORIENTED_EDGE ( 'NONE', *, *, #68724, .T. ) ;
#35689 = CARTESIAN_POINT ( 'NONE',  ( 116.6223143332234997, -42.37736834728454483, 283.4137205140060018 ) ) ;
#35691 = CYLINDRICAL_SURFACE ( 'NONE', #77109, 218.1859999999999786 ) ;
#35692 = CARTESIAN_POINT ( 'NONE',  ( 103.0412047595748959, -26.40992324271003966, 170.3603871806729444 ) ) ;
#35693 = CARTESIAN_POINT ( 'NONE',  ( 104.6489182489307552, -47.51505607846939938, 23.38895860924494841 ) ) ;
#35694 = CARTESIAN_POINT ( 'NONE',  ( 115.0109179074633374, -28.97809521412381883, 190.4537205140059655 ) ) ;
#35695 = CARTESIAN_POINT ( 'NONE',  ( 99.09570896555410968, -30.55043189343225052, 31.80229195668304953 ) ) ;
#35696 = CARTESIAN_POINT ( 'NONE',  ( -48.67264380398863466, 64.60000000000000853, 66.68100227564390536 ) ) ;
#35697 = VECTOR ( 'NONE', #85800, 999.9999999999998863 ) ;
#35699 = CARTESIAN_POINT ( 'NONE',  ( -185.9961463128564958, 20.32000000000000028, -3.174999999999349676 ) ) ;
#35698 = LINE ( 'NONE', #50216, #60874 ) ;
#35700 = CARTESIAN_POINT ( 'NONE',  ( 49.35031423293201414, -29.99615139349890569, 237.4678068554150059 ) ) ;
#35701 = DIRECTION ( 'NONE',  ( 0.000000000000000000, 0.000000000000000000, -1.000000000000000000 ) ) ;
#35702 = ORIENTED_EDGE ( 'NONE', *, *, #4254, .T. ) ;
#35703 = CARTESIAN_POINT ( 'NONE',  ( -55.89999999999999858, 53.97500000000000142, 70.79999999999999716 ) ) ;
#35704 = AXIS2_PLACEMENT_3D ( 'NONE', #21658, #2098, #84784 ) ;
#35705 = EDGE_CURVE ( 'NONE', #80877, #8011, #50325, .T. ) ;
#35706 = ORIENTED_EDGE ( 'NONE', *, *, #31826, .F. ) ;
#35707 = ORIENTED_EDGE ( 'NONE', *, *, #64702, .F. ) ;
#35709 = EDGE_LOOP ( 'NONE', ( #76148, #81839, #82583, #72857 ) ) ;
#35708 = CARTESIAN_POINT ( 'NONE',  ( 154.4532655810166091, -72.54279768053238797, 540.9756252759101471 ) ) ;
#35710 = CARTESIAN_POINT ( 'NONE',  ( 103.9639062230919251, -47.31423993612432355, 58.33753003781600199 ) ) ;
#35711 = CARTESIAN_POINT ( 'NONE',  ( 37.36643805256586859, -48.62818131006087441, 180.4678068554150911 ) ) ;
#35712 = DIRECTION ( 'NONE',  ( 0.000000000000000000, 0.000000000000000000, -1.000000000000000000 ) ) ;
#35713 = CARTESIAN_POINT ( 'NONE',  ( 99.97865438147567829, -27.17048309217152990, 181.5841967044829630 ) ) ;
#35714 = CARTESIAN_POINT ( 'NONE',  ( 114.8626455990942361, -41.33732585285711991, 282.8362293518863453 ) ) ;
#35715 = EDGE_LOOP ( 'NONE', ( #65657, #8891, #60620, #73844 ) ) ;
#35716 = ORIENTED_EDGE ( 'NONE', *, *, #14734, .T. ) ;
#35717 = ORIENTED_EDGE ( 'NONE', *, *, #53043, .T. ) ;
#35718 = ADVANCED_FACE ( 'NONE', ( #78893 ), #73536, .F. ) ;
#35719 = EDGE_LOOP ( 'NONE', ( #30727, #55672, #47487, #43338 ) ) ;
#35720 = CARTESIAN_POINT ( 'NONE',  ( 99.04406186213515184, -42.84125764447927054, 106.8439586097051688 ) ) ;
#35721 = DIRECTION ( 'NONE',  ( -1.000000000000000078E-15, 1.000000000000000000, 0.000000000000000000 ) ) ;
#35722 = CARTESIAN_POINT ( 'NONE',  ( 72.26949937496598864, -71.54137415153812185, 361.9756252759101471 ) ) ;
#35723 = CARTESIAN_POINT ( 'NONE',  ( 0.000000000000000000, 92.07499999999998863, 9.525000000000000355 ) ) ;
#35724 = CARTESIAN_POINT ( 'NONE',  ( 96.20559720633507084, 93.94653598907720493, 88.25806911646444064 ) ) ;
#35725 = DIRECTION ( 'NONE',  ( 1.000000000000000000, 0.000000000000000000, 0.000000000000000000 ) ) ;
#35726 = FACE_OUTER_BOUND ( 'NONE', #64253, .T. ) ;
#35727 = CARTESIAN_POINT ( 'NONE',  ( -10.86025490963659301, 89.13458635777121231, 130.1035480231986980 ) ) ;
#35728 = CARTESIAN_POINT ( 'NONE',  ( 115.8731522275743941, -31.19128430790902584, 34.27276813305396530 ) ) ;
#35729 = DIRECTION ( 'NONE',  ( 2.973811673103097665E-16, 0.000000000000000000, 1.000000000000000000 ) ) ;
#35730 = EDGE_CURVE ( 'NONE', #45118, #9390, #50257, .T. ) ;
#35731 = VERTEX_POINT ( 'NONE', #10277 ) ;
#35732 = EDGE_CURVE ( 'NONE', #45, #89358, #65245, .T. ) ;
#35733 = CARTESIAN_POINT ( 'NONE',  ( 115.0889047923113964, -30.61763678268615863, 269.3439585996102892 ) ) ;
#35734 = DIRECTION ( 'NONE',  ( -4.237773401492740281E-14, 1.000000000000000000, 0.000000000000000000 ) ) ;
#35735 = CARTESIAN_POINT ( 'NONE',  ( 115.1210532203963766, -38.21490719095142197, 86.49951894101998562 ) ) ;
#35736 = VECTOR ( 'NONE', #30938, 1000.000000000000000 ) ;
#35737 = COLOUR_RGB ( '', 0.40784314, 0.44705882, 0.49803922) ;
#35738 = AXIS2_PLACEMENT_3D ( 'NONE', #59063, #58193, #24568 ) ;
#35739 = ADVANCED_FACE ( 'NONE', ( #51594 ), #85710, .T. ) ;
#35740 = CARTESIAN_POINT ( 'NONE',  ( 70.06670417066790435, -71.37844715994097555, 55.21780685541800437 ) ) ;
#35741 = LINE ( 'NONE', #13964, #89508 ) ;
#35742 = ORIENTED_EDGE ( 'NONE', *, *, #55213, .T. ) ;
#35743 = ORIENTED_EDGE ( 'NONE', *, *, #48753, .T. ) ;
#35744 = LINE ( 'NONE', #44338, #51133 ) ;
#35745 = ORIENTED_EDGE ( 'NONE', *, *, #32362, .F. ) ;
#35746 = ORIENTED_EDGE ( 'NONE', *, *, #23257, .F. ) ;
#35747 = ADVANCED_FACE ( 'NONE', ( #42988 ), #64358, .T. ) ;
#35748 = CARTESIAN_POINT ( 'NONE',  ( 115.7737780547358710, -35.08282516751891933, 155.4072975916109556 ) ) ;
#35749 = DIRECTION ( 'NONE',  ( 0.000000000000000000, -1.000000000000000000, 0.000000000000000000 ) ) ;
#35750 = AXIS2_PLACEMENT_3D ( 'NONE', #51390, #16015, #7840 ) ;
#35751 = CARTESIAN_POINT ( 'NONE',  ( 116.9955931624231624, -33.48136526131695234, 85.07848241876791917 ) ) ;
#35752 = CARTESIAN_POINT ( 'NONE',  ( 59.67079009362632291, -0.9310397146383332379, 542.9756252759101471 ) ) ;
#35753 = VERTEX_POINT ( 'NONE', #1690 ) ;
#35754 = VERTEX_POINT ( 'NONE', #43439 ) ;
#35755 = ORIENTED_EDGE ( 'NONE', *, *, #1851, .T. ) ;
#35756 = EDGE_CURVE ( 'NONE', #83168, #43607, #45952, .T. ) ;
#35757 = FACE_OUTER_BOUND ( 'NONE', #19105, .T. ) ;
#35758 = VERTEX_POINT ( 'NONE', #16213 ) ;
#35759 = CARTESIAN_POINT ( 'NONE',  ( 105.3240584539683766, -26.47319898023375728, 15.20991099019697401 ) ) ;
#35760 = CARTESIAN_POINT ( 'NONE',  ( 116.6808514842340259, -40.81615526105927927, 164.5070538473399608 ) ) ;
#35761 = EDGE_CURVE ( 'NONE', #23447, #2591, #29990, .T. ) ;
#35762 = FACE_BOUND ( 'NONE', #69585, .T. ) ;
#35763 = CARTESIAN_POINT ( 'NONE',  ( -109.8429120651473454, 48.03328757174836738, 70.56492720431617727 ) ) ;
#35764 = CARTESIAN_POINT ( 'NONE',  ( 108.0341493669268260, -25.71865232712709215, 105.9946728949589811 ) ) ;
#35766 = ADVANCED_FACE ( 'NONE', ( #16652 ), #71183, .T. ) ;
#35765 = CARTESIAN_POINT ( 'NONE',  ( 194.0667039024475571, -24.92844715993407334, 129.9678068554150343 ) ) ;
#35767 = ORIENTED_EDGE ( 'NONE', *, *, #69390, .F. ) ;
#35768 = CARTESIAN_POINT ( 'NONE',  ( 0.000000000000000000, 215.0000000000000000, 159.6557476874258441 ) ) ;
#35769 = EDGE_CURVE ( 'NONE', #33407, #24965, #36200, .T. ) ;
#35770 = ORIENTED_EDGE ( 'NONE', *, *, #24475, .T. ) ;
#35771 = CARTESIAN_POINT ( 'NONE',  ( 117.0610774055309093, -38.07918021125614416, 134.7195873375643203 ) ) ;
#35772 = ORIENTED_EDGE ( 'NONE', *, *, #254, .F. ) ;
#35773 = ORIENTED_EDGE ( 'NONE', *, *, #32250, .T. ) ;
#35774 = DIRECTION ( 'NONE',  ( -0.7071067811865487940, 0.000000000000000000, 0.7071067811865463515 ) ) ;
#35775 = CARTESIAN_POINT ( 'NONE',  ( 10.00863283467136711, 90.24885462885215759, 118.1336793349710632 ) ) ;
#35776 = CARTESIAN_POINT ( 'NONE',  ( 111.4155313275575168, -46.20429869645016652, 27.91848241876792969 ) ) ;
#35777 = CARTESIAN_POINT ( 'NONE',  ( 21.80448803080050979, 60.57658380354070715, 31.24433384097766719 ) ) ;
#35778 = CARTESIAN_POINT ( 'NONE',  ( 71.25416588882602298, -72.55705569728901594, 540.9756252759101471 ) ) ;
#35779 = LINE ( 'NONE', #49850, #57136 ) ;
#35780 = CARTESIAN_POINT ( 'NONE',  ( 114.3402351757609665, -43.26825200597438226, 38.24419670448392594 ) ) ;
#35782 = CARTESIAN_POINT ( 'NONE',  ( 117.2167691715782070, -39.01263929987993606, 144.6499109901969859 ) ) ;
#35781 = LINE ( 'NONE', #1280, #78297 ) ;
#35783 = CARTESIAN_POINT ( 'NONE',  ( 34.27482367531500529, -30.08671355700301575, -5.074374724088000832 ) ) ;
#35784 = DIRECTION ( 'NONE',  ( 0.000000000000000000, 0.000000000000000000, -1.000000000000000000 ) ) ;
#35785 = ORIENTED_EDGE ( 'NONE', *, *, #69069, .F. ) ;
#35786 = CARTESIAN_POINT ( 'NONE',  ( -487.2989999999999782, 10.16305401447645984, 83.34375000000000000 ) ) ;
#35787 = CARTESIAN_POINT ( 'NONE',  ( 0.000000000000000000, 92.07499999999998863, 0.000000000000000000 ) ) ;
#35788 = DIRECTION ( 'NONE',  ( -2.108231265501709878E-16, 0.000000000000000000, 1.000000000000000000 ) ) ;
#35789 = ORIENTED_EDGE ( 'NONE', *, *, #63004, .T. ) ;
#35790 = CARTESIAN_POINT ( 'NONE',  ( 24.79284581386643183, 127.0000000000000000, 85.23828826961327820 ) ) ;
#35792 = ORIENTED_EDGE ( 'NONE', *, *, #19651, .F. ) ;
#35791 = CARTESIAN_POINT ( 'NONE',  ( 99.25559070964938257, -29.75831933708737864, 190.7470538473399415 ) ) ;
#35793 = DIRECTION ( 'NONE',  ( 1.000000000000000000, 4.299999999999999979E-14, 1.000000000000000078E-15 ) ) ;
#35794 = CARTESIAN_POINT ( 'NONE',  ( 100.6429626219512983, -44.96811459249982335, 228.0499109901969348 ) ) ;
#35795 = CARTESIAN_POINT ( 'NONE',  ( 112.5370353716610055, -27.80386372334747236, 90.63848241876793566 ) ) ;
#35796 = VECTOR ( 'NONE', #75761, 999.9999999999998863 ) ;
#35797 = CARTESIAN_POINT ( 'NONE',  ( 91.71670967179916545, 69.85063703626885001, 92.91726854070194008 ) ) ;
#35798 = CARTESIAN_POINT ( 'NONE',  ( 57.56670390244735103, -48.82844715994040286, 139.7178068554150911 ) ) ;
#35799 = CARTESIAN_POINT ( 'NONE',  ( 176.7669697523278955, -48.62818131005232658, 249.9678068554149775 ) ) ;
#35800 = EDGE_LOOP ( 'NONE', ( #6378, #39229 ) ) ;
#35801 = VECTOR ( 'NONE', #86093, 1000.000000000000114 ) ;
#35802 = AXIS2_PLACEMENT_3D ( 'NONE', #88715, #6047, #40543 ) ;
#35803 = CONTEXT_DEPENDENT_SHAPE_REPRESENTATION ( #66640, #32949 ) ;
#35804 = AXIS2_PLACEMENT_3D ( 'NONE', #85818, #38086, #84921 ) ;
#35805 = B_SPLINE_CURVE_WITH_KNOTS ( 'NONE', 3,
 ( #43051, #10343, #67087, #80732, #52089, #66180, #18942, #24863, #59806, #38477, #11224, #3970, #86651, #79849, #72576, #87097, #52531, #3518, #10770, #24427, #53877, #73006, #58914, #18482, #80293, #17607, #38929, #81192, #87540, #45287, #73449, #25300, #31218, #38049, #46625 ),
 .UNSPECIFIED., .F., .F.,
 ( 4, 2, 2, 1, 1, 2, 2, 2, 2, 2, 2, 1, 1, 2, 2, 2, 1, 1, 1, 2, 4 ),
 ( 0.3333434881890895429, 0.4166701562234092493, 0.4218780729755542414, 0.4270859897276991779, 0.4375018232319922706, 0.4583334902405750699, 0.4999968242577399469, 0.5208284912663228017, 0.5416601582749056565, 0.5624918252834885113, 0.5650957836595601469, 0.5676997420356317825, 0.5729076587877761639, 0.5833234922920649268, 0.6249868263092226428, 0.6275907846852966099, 0.6301947430613705770, 0.6354026598135189552, 0.6458184933178172660, 0.6562343268221155768, 0.6666501603264138875 ),
 .UNSPECIFIED. ) ;
#35806 = ORIENTED_EDGE ( 'NONE', *, *, #75488, .F. ) ;
#35807 = EDGE_LOOP ( 'NONE', ( #89890, #85321, #12180, #76050, #46900 ) ) ;
#35808 = EDGE_LOOP ( 'NONE', ( #76493, #80141, #5614, #49706 ) ) ;
#35809 = DIRECTION ( 'NONE',  ( 1.000000000000000078E-15, -1.000000000000000083E-30, -1.000000000000000000 ) ) ;
#35810 = CARTESIAN_POINT ( 'NONE',  ( 113.2200137887798235, -45.14470412949270184, 224.0784824187679476 ) ) ;
#35811 = CARTESIAN_POINT ( 'NONE',  ( 41.56648329127399677, -18.82844715994099971, 198.9256252759119832 ) ) ;
#35812 = CARTESIAN_POINT ( 'NONE',  ( 180.1667039024460166, -28.27351298637340093, 342.9256252759119548 ) ) ;
#35814 = CARTESIAN_POINT ( 'NONE',  ( -12.60000000000000142, 82.54999999999999716, 89.46299999999996544 ) ) ;
#35813 = DIRECTION ( 'NONE',  ( 0.000000000000000000, 0.000000000000000000, -1.000000000000000000 ) ) ;
#35815 = LINE ( 'NONE', #63532, #21116 ) ;
#35816 = AXIS2_PLACEMENT_3D ( 'NONE', #57675, #42684, #23196 ) ;
#35817 = CARTESIAN_POINT ( 'NONE',  ( 117.5344697633125577, -37.28603910398157240, 18.78419670448294809 ) ) ;
#35818 = ORIENTED_EDGE ( 'NONE', *, *, #19603, .T. ) ;
#35819 = ORIENTED_EDGE ( 'NONE', *, *, #29915, .T. ) ;
#35820 = CLOSED_SHELL ( 'NONE', ( #54060, #59708, #77498, #75862 ) ) ;
#35821 = EDGE_CURVE ( 'NONE', #82548, #16017, #14030, .T. ) ;
#35822 = CARTESIAN_POINT ( 'NONE',  ( 97.06380509542137247, -37.34170171876225908, 17.37620855293377886 ) ) ;
#35823 = EDGE_CURVE ( 'NONE', #67197, #2317, #44787, .T. ) ;
#35824 = CARTESIAN_POINT ( 'NONE',  ( 110.0587659310071302, -27.38278898179171605, 230.8299109901959412 ) ) ;
#35825 = DIRECTION ( 'NONE',  ( 1.000000000000000078E-15, -1.000000000000000000, 0.000000000000000000 ) ) ;
#35826 = ADVANCED_FACE ( 'NONE', ( #71625 ), #25622, .T. ) ;
#35827 = CARTESIAN_POINT ( 'NONE',  ( 116.3126599349420900, -33.43976754494801185, 110.0984824187669631 ) ) ;
#35828 = CARTESIAN_POINT ( 'NONE',  ( 34.92499999999999716, 82.54999999999999716, 302.8950000000000387 ) ) ;
#35829 = CARTESIAN_POINT ( 'NONE',  ( -75.64365119985745878, 54.20154546050554956, 30.80107733549443694 ) ) ;
#35830 = EDGE_CURVE ( 'NONE', #33306, #15468, #24274, .T. ) ;
#35831 = VERTEX_POINT ( 'NONE', #78451 ) ;
#35832 = CARTESIAN_POINT ( 'NONE',  ( 162.7131505118547352, -33.70561438051439040, 237.4678068554150059 ) ) ;
#35833 = EDGE_CURVE ( 'NONE', #2950, #44520, #9389, .T. ) ;
#35834 = ORIENTED_EDGE ( 'NONE', *, *, #58310, .T. ) ;
#35835 = ORIENTED_EDGE ( 'NONE', *, *, #36390, .T. ) ;
#35836 = CARTESIAN_POINT ( 'NONE',  ( -80.31773373136844896, 94.30044247306078375, 87.20679752240629057 ) ) ;
#35837 = CARTESIAN_POINT ( 'NONE',  ( 105.1749981762835802, -28.04127050161159218, 256.6787261630399826 ) ) ;
#35838 = CIRCLE ( 'NONE', #5372, 2.517499999999998739 ) ;
#35839 = EDGE_CURVE ( 'NONE', #70760, #82741, #17544, .T. ) ;
#35840 = CARTESIAN_POINT ( 'NONE',  ( 108.3334480201780963, -46.73485936414270725, 192.6772919366305246 ) ) ;
#35841 = CARTESIAN_POINT ( 'NONE',  ( 7.661254700127844153, 66.45253841614081125, 317.6630000000000109 ) ) ;
#35842 = EDGE_CURVE ( 'NONE', #35871, #33311, #17973, .T. ) ;
#35843 = CARTESIAN_POINT ( 'NONE',  ( 97.81169818311565223, -40.51742792548894556, 86.63555527419073599 ) ) ;
#35844 = DIRECTION ( 'NONE',  ( -0.4999999999999931166, -0.8660254037844425934, 2.684678751731770391E-14 ) ) ;
#35845 = ORIENTED_EDGE ( 'NONE', *, *, #67614, .T. ) ;
#35846 = CARTESIAN_POINT ( 'NONE',  ( 105.7809510460201210, -24.27257308096163868, 321.6188579224977389 ) ) ;
#35847 = LINE ( 'NONE', #15430, #57134 ) ;
#35848 = ORIENTED_EDGE ( 'NONE', *, *, #64640, .F. ) ;
#35849 = CARTESIAN_POINT ( 'NONE',  ( 96.95653860995706452, -32.26087848594701057, 55.98324432352897162 ) ) ;
#35850 = VERTEX_POINT ( 'NONE', #74296 ) ;
#35851 = CARTESIAN_POINT ( 'NONE',  ( 99.21763626795888058, -33.35996782468227195, 15.42670554236297242 ) ) ;
#35852 = ADVANCED_FACE ( 'NONE', ( #60642 ), #74739, .F. ) ;
#35853 = CARTESIAN_POINT ( 'NONE',  ( -458.3598257906459708, 60.32499999999999574, -3.174999999999999822 ) ) ;
#35854 = CARTESIAN_POINT ( 'NONE',  ( 102.3610132369663148, -45.97051510703457922, 172.2137205140069511 ) ) ;
#35855 = CARTESIAN_POINT ( 'NONE',  ( -23.75871628398702384, 82.54999999999999716, 317.6630000000000109 ) ) ;
#35856 = VECTOR ( 'NONE', #10665, 1000.000000000000000 ) ;
#35857 = CARTESIAN_POINT ( 'NONE',  ( 131.0667039024480403, -43.72944715994093201, 207.5838068554170377 ) ) ;
#35858 = CYLINDRICAL_SURFACE ( 'NONE', #59320, 218.1859999999999786 ) ;
#35859 = AXIS2_PLACEMENT_3D ( 'NONE', #66319, #73591, #52663 ) ;
#35860 = CARTESIAN_POINT ( 'NONE',  ( 177.0371591254543659, -48.62818131005480637, 249.9678068554149775 ) ) ;
#35861 = CARTESIAN_POINT ( 'NONE',  ( 105.1596118751612323, -47.03031267540156080, 8.429910990196965770 ) ) ;
#35862 = DIRECTION ( 'NONE',  ( 1.000000000000000078E-15, 0.000000000000000000, 1.000000000000000000 ) ) ;
#35863 = VERTEX_POINT ( 'NONE', #45221 ) ;
#35864 = CARTESIAN_POINT ( 'NONE',  ( 136.5037707043280477, -38.00325133682356693, 7.150416387934964035 ) ) ;
#35865 = VECTOR ( 'NONE', #64092, 1000.000000000000000 ) ;
#35866 = VERTEX_POINT ( 'NONE', #73839 ) ;
#35867 = CARTESIAN_POINT ( 'NONE',  ( 117.2518684062627727, -39.29770432102194633, 119.6299109901969615 ) ) ;
#35868 = AXIS2_PLACEMENT_3D ( 'NONE', #54928, #14073, #20452 ) ;
#35869 = CARTESIAN_POINT ( 'NONE',  ( 120.5298512137159008, 47.23280909986927156, -50.17433177954229961 ) ) ;
#35870 = AXIS2_PLACEMENT_3D ( 'NONE', #3908, #31603, #81130 ) ;
#35871 = VERTEX_POINT ( 'NONE', #46561 ) ;
#35872 = ORIENTED_EDGE ( 'NONE', *, *, #3731, .T. ) ;
#35873 = ORIENTED_EDGE ( 'NONE', *, *, #43037, .F. ) ;
#35874 = CARTESIAN_POINT ( 'NONE',  ( 98.30753410070099108, -41.72887533559486428, 121.7397919284131547 ) ) ;
#35875 = DIRECTION ( 'NONE',  ( -1.000000000000000000, -4.163336342344333240E-14, 0.000000000000000000 ) ) ;
#35876 = CARTESIAN_POINT ( 'NONE',  ( 52.38749999999999574, 94.53880000000000905, 225.4249999999999829 ) ) ;
#35877 = CARTESIAN_POINT ( 'NONE',  ( 107.0664832912739257, -50.36908288530316469, 302.6356252759109680 ) ) ;
#35878 = DIRECTION ( 'NONE',  ( 1.000000000000000078E-15, 1.000000000000000083E-30, -1.000000000000000000 ) ) ;
#35879 = CARTESIAN_POINT ( 'NONE',  ( 112.1172674779030558, -26.89768192312349271, 15.71086337114896381 ) ) ;
#35881 = EDGE_CURVE ( 'NONE', #37766, #5375, #84474, .T. ) ;
#35880 = LINE ( 'NONE', #63597, #75494 ) ;
#35882 = EDGE_LOOP ( 'NONE', ( #8352, #52732, #82166, #46597 ) ) ;
#35883 = AXIS2_PLACEMENT_3D ( 'NONE', #54406, #53960, #62592 ) ;
#35884 = CARTESIAN_POINT ( 'NONE',  ( 106.0667039024470455, -121.2010968907524529, -19.26696060647547881 ) ) ;
#35885 = VECTOR ( 'NONE', #4346, 1000.000000000000000 ) ;
#35886 = ADVANCED_FACE ( 'NONE', ( #40201 ), #34435, .T. ) ;
#35887 = AXIS2_PLACEMENT_3D ( 'NONE', #82167, #6287, #13997 ) ;
#35888 = CARTESIAN_POINT ( 'NONE',  ( -103.1875000000000000, 117.4749999999999943, -1.080832317973422076E-12 ) ) ;
#35889 = EDGE_LOOP ( 'NONE', ( #47, #59639, #38898, #56327 ) ) ;
#35890 = ORIENTED_EDGE ( 'NONE', *, *, #42995, .T. ) ;
#35891 = AXIS2_PLACEMENT_3D ( 'NONE', #53692, #13293, #11952 ) ;
#35892 = DIRECTION ( 'NONE',  ( 1.000000000000000000, 0.000000000000000000, 0.000000000000000000 ) ) ;
#35893 = PLANE ( 'NONE',  #16480 ) ;
#35894 = CARTESIAN_POINT ( 'NONE',  ( 61.00843881761244347, 49.07499999999999574, -33.74458626278666884 ) ) ;
#35895 = DIRECTION ( 'NONE',  ( 0.000000000000000000, 1.000000000000000000, 0.000000000000000000 ) ) ;
#35896 = DIRECTION ( 'NONE',  ( 1.000000000000000078E-15, -1.000000000000000083E-30, -1.000000000000000000 ) ) ;
#35898 = CARTESIAN_POINT ( 'NONE',  ( 99.16725398249624845, -41.15831232534042528, 181.1676579233149482 ) ) ;
#35897 = B_SPLINE_CURVE_WITH_KNOTS ( 'NONE', 3,
 ( #45588, #18354, #86529, #38798, #45155, #66504, #4293, #3841, #87408, #43489, #77589, #31537, #59240, #31983, #25169, #52832, #15372, #80606, #46040, #73772, #43038, #70780, #26078, #5185, #46939, #67392, #74669, #48275, #12006, #32878, #75118, #39251, #12903, #82849 ),
 .UNSPECIFIED., .F., .F.,
 ( 4, 2, 2, 2, 2, 2, 2, 2, 2, 2, 2, 2, 2, 2, 2, 2, 4 ),
 ( 0.05204795639664543117, 0.05411398420652786811, 0.05618001201641030506, 0.06031206763617517896, 0.06237809544605762285, 0.06444412325594006674, 0.06857617887570495452, 0.07064220668558740535, 0.07270823449546987005, 0.07477426230535232088, 0.07580727621029356711, 0.07684029011523479946, 0.07890631792511729192, 0.08097234573499978438, 0.08303837354488227684, 0.08407138744982353695, 0.08510440135476479706 ),
 .UNSPECIFIED. ) ;
#35899 = CARTESIAN_POINT ( 'NONE',  ( 41.56648329127499153, -32.07844715994070839, 138.9256252759119832 ) ) ;
#35900 = CARTESIAN_POINT ( 'NONE',  ( 124.9629318080292251, -56.47944715994101728, 14.92562527591098842 ) ) ;
#35901 = CARTESIAN_POINT ( 'NONE',  ( 98.05881815954255387, -31.39384645160161469, 85.90133956162493689 ) ) ;
#35902 = VERTEX_POINT ( 'NONE', #11159 ) ;
#35903 = CARTESIAN_POINT ( 'NONE',  ( 90.44969454456408187, -16.81243780205710436, 239.5838068554175209 ) ) ;
#35904 = VERTEX_POINT ( 'NONE', #25236 ) ;
#35905 = CARTESIAN_POINT ( 'NONE',  ( 121.3042370176062548, -43.34581843340460239, 9.425625275910984868 ) ) ;
#35906 = ORIENTED_EDGE ( 'NONE', *, *, #34076, .T. ) ;
#35907 = CARTESIAN_POINT ( 'NONE',  ( 102.0668449664933064, -27.97061517841426692, 50.48981082298863754 ) ) ;
#35908 = ORIENTED_EDGE ( 'NONE', *, *, #1323, .F. ) ;
#35909 = PLANE ( 'NONE',  #79909 ) ;
#35910 = CARTESIAN_POINT ( 'NONE',  ( 67.30555758892512586, -104.4393591762123918, 246.9440934771770060 ) ) ;
#35911 = CIRCLE ( 'NONE', #79440, 5.600000000000000533 ) ;
#35912 = CARTESIAN_POINT ( 'NONE',  ( 188.5667039024485518, -48.82844715993430640, 173.2178068554150059 ) ) ;
#35913 = ORIENTED_EDGE ( 'NONE', *, *, #76000, .F. ) ;
#35914 = CARTESIAN_POINT ( 'NONE',  ( 116.1429853652930149, -29.07104484579759784, 74.38419670448293175 ) ) ;
#35916 = CARTESIAN_POINT ( 'NONE',  ( 92.91726854070162744, 69.85063703626886422, -91.71670967179946388 ) ) ;
#35915 = CARTESIAN_POINT ( 'NONE',  ( 115.0884034490740362, -30.61698329126820894, 164.3440238799496456 ) ) ;
#35917 = LINE ( 'NONE', #1417, #42289 ) ;
#35918 = CARTESIAN_POINT ( 'NONE',  ( 115.7831076650244881, -41.80230951930585093, 143.4064586084350879 ) ) ;
#35919 = ORIENTED_EDGE ( 'NONE', *, *, #12101, .F. ) ;
#35920 = LINE ( 'NONE', #28662, #32939 ) ;
#35921 = CYLINDRICAL_SURFACE ( 'NONE', #28025, 2.750000000000002665 ) ;
#35922 = DIRECTION ( 'NONE',  ( 1.639958061481212836E-42, -4.100000000000000342E-29, -1.000000000000000000 ) ) ;
#35923 = CARTESIAN_POINT ( 'NONE',  ( 117.8979321085648877, -39.04567734339117635, 104.6708633711489824 ) ) ;
#35924 = CIRCLE ( 'NONE', #61985, 2.517500000000005844 ) ;
#35926 = DIRECTION ( 'NONE',  ( 1.000000000000000000, 4.163336342344333240E-14, 0.000000000000000000 ) ) ;
#35925 = DIRECTION ( 'NONE',  ( 1.000000000000000000, 4.299999999999999979E-14, 1.000000000000000078E-15 ) ) ;
#35927 = CARTESIAN_POINT ( 'NONE',  ( 38.10000000000000142, 95.25000000000000000, 283.4005000000000223 ) ) ;
#35928 = EDGE_CURVE ( 'NONE', #78144, #36708, #79788, .T. ) ;
#35929 = AXIS2_PLACEMENT_3D ( 'NONE', #50893, #39047, #4085 ) ;
#35930 = ORIENTED_EDGE ( 'NONE', *, *, #36276, .F. ) ;
#35931 = AXIS2_PLACEMENT_3D ( 'NONE', #20510, #82296, #20053 ) ;
#35932 = B_SPLINE_CURVE_WITH_KNOTS ( 'NONE', 3,
 ( #77830, #69664, #62836, #35576, #56463, #8798, #35125, #612, #28309, #56001, #83751, #15607, #43280, #15152, #84209, #49196, #42828, #14708 ),
 .UNSPECIFIED., .F., .F.,
 ( 4, 2, 2, 2, 2, 2, 2, 2, 4 ),
 ( 0.000000000000000000, 0.1250000000000000000, 0.2500000000000000000, 0.3750000000000000000, 0.5000000000000000000, 0.6250000000000000000, 0.7500000000000000000, 0.8750000000000000000, 1.000000000000000000 ),
 .UNSPECIFIED. ) ;
#35933 = ADVANCED_FACE ( 'NONE', ( #11626 ), #87480, .F. ) ;
#35934 = DIRECTION ( 'NONE',  ( 9.912705577010326536E-16, 1.000000000000000000, 0.000000000000000000 ) ) ;
#35935 = EDGE_CURVE ( 'NONE', #28327, #85809, #17014, .T. ) ;
#35936 = CARTESIAN_POINT ( 'NONE',  ( 96.47668441219811086, -40.11591174724600251, 127.5727681330529606 ) ) ;
#35938 = ORIENTED_EDGE ( 'NONE', *, *, #82036, .F. ) ;
#35937 = DIRECTION ( 'NONE',  ( 5.512527431108029424E-15, -1.000000000000000000, 0.000000000000000000 ) ) ;
#35940 = EDGE_CURVE ( 'NONE', #57034, #78275, #54708, .T. ) ;
#35939 = AXIS2_PLACEMENT_3D ( 'NONE', #59739, #33840, #87916 ) ;
#35941 = CARTESIAN_POINT ( 'NONE',  ( 100.8863495415024829, -28.40209871822986543, 31.59657765686296926 ) ) ;
#35942 = LINE ( 'NONE', #30033, #73031 ) ;
#35943 = CARTESIAN_POINT ( 'NONE',  ( 143.0664832912740110, -18.82844715994099971, 284.9256252759119548 ) ) ;
#35944 = CARTESIAN_POINT ( 'NONE',  ( 123.6837132603321692, -50.04645651782492166, 249.5838068554164693 ) ) ;
#35945 = CARTESIAN_POINT ( 'NONE',  ( 107.0664832912739257, -50.22944715994096043, 315.6356252759111953 ) ) ;
#35946 = AXIS2_PLACEMENT_3D ( 'NONE', #29540, #84529, #78158 ) ;
#35947 = ADVANCED_FACE ( 'NONE', ( #12070 ), #25687, .F. ) ;
#35948 = FACE_OUTER_BOUND ( 'NONE', #33999, .T. ) ;
#35949 = CARTESIAN_POINT ( 'NONE',  ( 97.33793063222405806, -34.07070140586845497, 31.11498729261382934 ) ) ;
#35951 = CARTESIAN_POINT ( 'NONE',  ( 97.17009264939167679, -31.66255117090383564, 245.9499109901979637 ) ) ;
#35950 = AXIS2_PLACEMENT_3D ( 'NONE', #88418, #47041, #41134 ) ;
#35952 = ORIENTED_EDGE ( 'NONE', *, *, #80356, .F. ) ;
#35953 = VERTEX_POINT ( 'NONE', #66119 ) ;
#35954 = CARTESIAN_POINT ( 'NONE',  ( 113.1640969444738971, -43.88191609279036243, 149.5825356868499512 ) ) ;
#35956 = ADVANCED_FACE ( 'NONE', ( #53811 ), #66330, .F. ) ;
#35955 = AXIS2_PLACEMENT_3D ( 'NONE', #34596, #55913, #28684 ) ;
#35957 = CYLINDRICAL_SURFACE ( 'NONE', #82130, 7.937500000000000000 ) ;
#35958 = CARTESIAN_POINT ( 'NONE',  ( 101.5678104218880549, -29.74196420480149072, 12.03872616303996956 ) ) ;
#35959 = CARTESIAN_POINT ( 'NONE',  ( 147.0667039024470739, -137.6766936010357938, 245.4930511039999885 ) ) ;
#35960 = EDGE_CURVE ( 'NONE', #64446, #59215, #39316, .T. ) ;
#35961 = LINE ( 'NONE', #62764, #83819 ) ;
#35962 = DIRECTION ( 'NONE',  ( 0.000000000000000000, 0.000000000000000000, 1.000000000000000000 ) ) ;
#35963 = CARTESIAN_POINT ( 'NONE',  ( 107.0664832912739968, -36.72944715994100306, 9.635625275910941312 ) ) ;
#35964 = PLANE ( 'NONE',  #38647 ) ;
#35965 = CARTESIAN_POINT ( 'NONE',  ( 110.4916936757735471, -26.90617889774101812, 209.8099109901969541 ) ) ;
#35966 = DIRECTION ( 'NONE',  ( -1.000000000000000000, -4.237773401492740281E-14, 0.000000000000000000 ) ) ;
#35967 = VERTEX_POINT ( 'NONE', #4806 ) ;
#35968 = ORIENTED_EDGE ( 'NONE', *, *, #67811, .T. ) ;
#35969 = EDGE_CURVE ( 'NONE', #76086, #48254, #32943, .T. ) ;
#35970 = CARTESIAN_POINT ( 'NONE',  ( 116.8171228669754242, -34.15291832173085140, 89.03145860915122967 ) ) ;
#35971 = CARTESIAN_POINT ( 'NONE',  ( -87.20679752240603477, 94.30044247306076954, -80.31773373136881844 ) ) ;
#35972 = DIRECTION ( 'NONE',  ( 0.7071067811865046071, 0.7071067811865904273, 7.071067811865039488E-16 ) ) ;
#35973 = DIRECTION ( 'NONE',  ( 0.000000000000000000, 0.000000000000000000, 1.000000000000000000 ) ) ;
#35974 = CIRCLE ( 'NONE', #86758, 2.117000000000007987 ) ;
#35975 = VECTOR ( 'NONE', #21071, 1000.000000000000000 ) ;
#35976 = CARTESIAN_POINT ( 'NONE',  ( 110.8778723966665751, -46.37372517157803742, 18.88800622829095488 ) ) ;
#35977 = CYLINDRICAL_SURFACE ( 'NONE', #13700, 0.4999999999999994449 ) ;
#35978 = VERTEX_POINT ( 'NONE', #47005 ) ;
#35979 = CARTESIAN_POINT ( 'NONE',  ( 104.6388127410885005, -47.56014030727299513, 23.38895860924494841 ) ) ;
#35980 = FACE_OUTER_BOUND ( 'NONE', #12364, .T. ) ;
#35981 = B_SPLINE_CURVE_WITH_KNOTS ( 'NONE', 3,
 ( #51964, #37475, #52397, #24733, #66506, #45158, #60125, #31093, #72881, #51527, #38354, #44268, #79277, #37919, #10214, #65619, #10648, #87410, #9772, #73322, #78828, #39253, #87859, #66053, #23855, #17037, #4295, #44717, #3844 ),
 .UNSPECIFIED., .F., .F.,
 ( 4, 2, 2, 2, 1, 1, 2, 2, 2, 2, 1, 1, 1, 2, 2, 2, 4 ),
 ( 0.000000000000000000, 0.2500000000002285949, 0.3750000000003456679, 0.4375000000003927969, 0.4687500000004163891, 0.4843750000004282130, 0.4921875000004340972, 0.5000000000004399814, 0.6250000000006787904, 0.6875000000008131273, 0.7187500000008804069, 0.7343750000009092727, 0.7421875000009192647, 0.7460937500009182655, 0.7500000000009172663, 0.8750000000004586331, 1.000000000000000000 ),
 .UNSPECIFIED. ) ;
#35982 = CARTESIAN_POINT ( 'NONE',  ( 105.6320445689042486, -47.05559920284586184, 257.4670538473393435 ) ) ;
#35983 = ORIENTED_EDGE ( 'NONE', *, *, #39717, .T. ) ;
#35984 = FACE_OUTER_BOUND ( 'NONE', #29, .T. ) ;
#35985 = CARTESIAN_POINT ( 'NONE',  ( 114.2313622454166904, -100.7192800061664570, -19.78219314458212708 ) ) ;
#35986 = FACE_OUTER_BOUND ( 'NONE', #3884, .T. ) ;
#35987 = CARTESIAN_POINT ( 'NONE',  ( 115.6288848908637732, -37.98889302744424867, 71.54047132197199232 ) ) ;
#35988 = CARTESIAN_POINT ( 'NONE',  ( 96.65238424151439744, -35.53540495314400260, 202.2356252759109623 ) ) ;
#35989 = DIRECTION ( 'NONE',  ( 1.000000000000000078E-15, 0.000000000000000000, 1.000000000000000000 ) ) ;
#35990 = ORIENTED_EDGE ( 'NONE', *, *, #50746, .F. ) ;
#35991 = VECTOR ( 'NONE', #74891, 1000.000000000000000 ) ;
#35992 = EDGE_CURVE ( 'NONE', #83707, #20491, #67920, .T. ) ;
#35993 = CARTESIAN_POINT ( 'NONE',  ( 182.0374245136174522, -23.42844715993458848, 193.9678068554150343 ) ) ;
#35994 = ORIENTED_EDGE ( 'NONE', *, *, #34612, .F. ) ;
#35995 = EDGE_LOOP ( 'NONE', ( #60367, #21296, #51004, #81914 ) ) ;
#35996 = CIRCLE ( 'NONE', #57777, 17.33514202138210791 ) ;
#35997 = CARTESIAN_POINT ( 'NONE',  ( 0.000000000000000000, 103.1240000000000236, 190.5000000000000000 ) ) ;
#35998 = ORIENTED_EDGE ( 'NONE', *, *, #51307, .F. ) ;
#35999 = VERTEX_POINT ( 'NONE', #58855 ) ;
#36000 = DIRECTION ( 'NONE',  ( -0.8660254037844381525, 0.000000000000000000, -0.5000000000000007772 ) ) ;
#36001 = CARTESIAN_POINT ( 'NONE',  ( 107.9191913915661871, -25.30201086838711788, 321.3423205873733082 ) ) ;
#36002 = CARTESIAN_POINT ( 'NONE',  ( 104.7294611837924094, -27.30559681290521112, 89.69241982807696445 ) ) ;
#36003 = CARTESIAN_POINT ( 'NONE',  ( 111.7836659179374408, -46.75466717335095268, 287.9146728949587555 ) ) ;
#36004 = AXIS2_PLACEMENT_3D ( 'NONE', #75183, #32936, #67462 ) ;
#36005 = DIRECTION ( 'NONE',  ( -1.150535366796005147E-15, 1.000000000000000000, -3.100000000000000044E-14 ) ) ;
#36006 = CARTESIAN_POINT ( 'NONE',  ( 138.8167039024479834, -57.40094715994099772, 33.40080685541480676 ) ) ;
#36007 = VERTEX_POINT ( 'NONE', #59304 ) ;
#36008 = EDGE_CURVE ( 'NONE', #49936, #72873, #52468, .T. ) ;
#36009 = VERTEX_POINT ( 'NONE', #82474 ) ;
#36010 = CARTESIAN_POINT ( 'NONE',  ( 188.5667039024479834, -58.35344715994099829, 175.9678068554150059 ) ) ;
#36011 = AXIS2_PLACEMENT_3D ( 'NONE', #55371, #63104, #62207 ) ;
#36012 = VECTOR ( 'NONE', #3192, 1000.000000000000000 ) ;
#36013 = LINE ( 'NONE', #49172, #28941 ) ;
#36014 = CARTESIAN_POINT ( 'NONE',  ( 70.38652669525582439, -140.1242979453984390, 246.9157945169867787 ) ) ;
#36015 = CARTESIAN_POINT ( 'NONE',  ( 113.5587197313314505, -28.64306037466250743, 119.5261014663879564 ) ) ;
#36016 = EDGE_CURVE ( 'NONE', #29733, #66334, #38740, .T. ) ;
#36017 = CARTESIAN_POINT ( 'NONE',  ( 95.43890296797121664, -34.19406290021405681, 106.1556252759109640 ) ) ;
#36018 = CARTESIAN_POINT ( 'NONE',  ( 111.4991187713021219, -26.55290587224241960, 284.7375300378155316 ) ) ;
#36019 = ORIENTED_EDGE ( 'NONE', *, *, #75379, .T. ) ;
#36020 = CARTESIAN_POINT ( 'NONE',  ( 113.7993967570077700, -26.97709554098909024, 239.5956252759109759 ) ) ;
#36021 = DIRECTION ( 'NONE',  ( 0.7071067811865489050, -0.7071067811865462405, 0.000000000000000000 ) ) ;
#36022 = PLANE ( 'NONE',  #13145 ) ;
#36023 = DIRECTION ( 'NONE',  ( -1.000000000000000000, 0.000000000000000000, -0.000000000000000000 ) ) ;
#36025 = CARTESIAN_POINT ( 'NONE',  ( 63.06670390244799052, -40.32844715994017548, 249.9678068554150343 ) ) ;
#36024 = CARTESIAN_POINT ( 'NONE',  ( 108.0925365931996680, -46.37966058722595619, 277.6356252759107406 ) ) ;
#36026 = CARTESIAN_POINT ( 'NONE',  ( 106.3547972878507579, -25.29203239850954787, 320.5499541688668614 ) ) ;
#36027 = FACE_OUTER_BOUND ( 'NONE', #20342, .T. ) ;
#36028 = CARTESIAN_POINT ( 'NONE',  ( 131.4052890608956545, -37.42303004212691775, 6.877070700249918289 ) ) ;
#36029 = AXIS2_PLACEMENT_3D ( 'NONE', #63147, #85854, #50860 ) ;
#36030 = CARTESIAN_POINT ( 'NONE',  ( -4.090559613967782226, 94.60197653454001454, 130.4941709638410146 ) ) ;
#36031 = DIRECTION ( 'NONE',  ( -0.000000000000000000, -0.000000000000000000, 1.000000000000000000 ) ) ;
#36032 = DIRECTION ( 'NONE',  ( 0.000000000000000000, 1.000000000000000000, 0.000000000000000000 ) ) ;
#36034 = ORIENTED_EDGE ( 'NONE', *, *, #45880, .F. ) ;
#36033 = LINE ( 'NONE', #55999, #70406 ) ;
#36035 = PLANE ( 'NONE',  #36526 ) ;
#36036 = CARTESIAN_POINT ( 'NONE',  ( 112.4231589263966526, -46.42488254349225940, 252.9661014663871015 ) ) ;
#36037 = CARTESIAN_POINT ( 'NONE',  ( 116.6607991934174322, -40.80763178269008762, 164.5070538473399608 ) ) ;
#36038 = CARTESIAN_POINT ( 'NONE',  ( 114.1052656684236979, -46.29384956339717405, 29.08133956162595268 ) ) ;
#36039 = CARTESIAN_POINT ( 'NONE',  ( 139.9417039024470455, -127.9034471599408960, 45.21780685541799727 ) ) ;
#36040 = AXIS2_PLACEMENT_3D ( 'NONE', #76754, #42653, #14077 ) ;
#36042 = LINE ( 'NONE', #7889, #3524 ) ;
#36041 = CARTESIAN_POINT ( 'NONE',  ( 172.5667039024480687, -36.32844715993499563, 129.9678068554150059 ) ) ;
#36043 = CARTESIAN_POINT ( 'NONE',  ( 99.50482035239026857, -43.30589195511487333, 137.8960310260671633 ) ) ;
#36044 = ORIENTED_EDGE ( 'NONE', *, *, #24812, .T. ) ;
#36045 = EDGE_CURVE ( 'NONE', #78613, #75146, #11230, .T. ) ;
#36046 = CARTESIAN_POINT ( 'NONE',  ( 172.5664832912729878, -27.82844715994070484, 138.9256252759119832 ) ) ;
#36047 = ORIENTED_EDGE ( 'NONE', *, *, #38105, .F. ) ;
#36048 = EDGE_CURVE ( 'NONE', #60674, #54334, #47459, .T. ) ;
#36049 = CARTESIAN_POINT ( 'NONE',  ( 112.3908963168805712, -43.44530362507355647, 167.5324198280769963 ) ) ;
#36051 = ORIENTED_EDGE ( 'NONE', *, *, #15576, .F. ) ;
#36050 = FACE_OUTER_BOUND ( 'NONE', #40584, .T. ) ;
#36052 = CARTESIAN_POINT ( 'NONE',  ( 121.3140869715381314, -95.00417761012944595, -11.78219314458228695 ) ) ;
#36053 = EDGE_CURVE ( 'NONE', #86385, #58881, #22858, .T. ) ;
#36054 = CARTESIAN_POINT ( 'NONE',  ( 95.33621695423336462, -38.27597901479983733, 147.4299109901969871 ) ) ;
#36055 = CARTESIAN_POINT ( 'NONE',  ( 135.3756687995053483, -12.91806617559082504, 361.9756252759100335 ) ) ;
#36056 = DIRECTION ( 'NONE',  ( 0.000000000000000000, 0.000000000000000000, 1.000000000000000000 ) ) ;
#36057 = CARTESIAN_POINT ( 'NONE',  ( 104.5015244207571357, -26.97598608851367530, 86.28151539219055621 ) ) ;
#36058 = AXIS2_PLACEMENT_3D ( 'NONE', #12110, #5300, #82517 ) ;
#36059 = CARTESIAN_POINT ( 'NONE',  ( 61.56670390244730839, -23.42844715994043980, 249.9678068554150343 ) ) ;
#36060 = ADVANCED_FACE ( 'NONE', ( #14314 ), #47900, .F. ) ;
#36061 = DIRECTION ( 'NONE',  ( 0.000000000000000000, 1.000000000000000000, 0.000000000000000000 ) ) ;
#36062 = CARTESIAN_POINT ( 'NONE',  ( 116.4859054502389881, -39.36344060769046393, 98.60991099019695127 ) ) ;
#36063 = VERTEX_POINT ( 'NONE', #7045 ) ;
#36064 = ORIENTED_EDGE ( 'NONE', *, *, #84263, .T. ) ;
#36065 = VERTEX_POINT ( 'NONE', #27924 ) ;
#36066 = AXIS2_PLACEMENT_3D ( 'NONE', #70926, #8699, #36400 ) ;
#36067 = CARTESIAN_POINT ( 'NONE',  ( 99.03873739112161445, -32.90617299384241790, 72.40444044875393104 ) ) ;
#36068 = AXIS2_PLACEMENT_3D ( 'NONE', #49130, #70503, #89155 ) ;
#36069 = CARTESIAN_POINT ( 'NONE',  ( 107.0667039024469886, -67.87844715994094713, 93.21780685541800437 ) ) ;
#36071 = CARTESIAN_POINT ( 'NONE',  ( 6.938893903907229955E-15, 60.82030000000000314, 210.4643999999999835 ) ) ;
#36070 = CARTESIAN_POINT ( 'NONE',  ( 97.31640351007386869, -35.61153895465465524, 202.2356252759109623 ) ) ;
#36072 = CARTESIAN_POINT ( 'NONE',  ( 99.09600433706673073, -30.55004372760710041, 55.80090408730614371 ) ) ;
#36073 = CARTESIAN_POINT ( 'NONE',  ( 105.7995095144211462, -26.72403595622594707, 111.1776164158398643 ) ) ;
#36074 = EDGE_CURVE ( 'NONE', #62004, #65745, #76078, .T. ) ;
#36075 = DIRECTION ( 'NONE',  ( -0.9254794337955620787, -0.3787978585227822492, 0.000000000000000000 ) ) ;
#36076 = CIRCLE ( 'NONE', #75244, 1.000000000000000888 ) ;
#36077 = DIRECTION ( 'NONE',  ( -1.000000000000000000, -4.299999999999999979E-14, -1.000000000000000078E-15 ) ) ;
#36078 = LINE ( 'NONE', #34275, #9612 ) ;
#36079 = CARTESIAN_POINT ( 'NONE',  ( 108.2741602056595411, -26.36093993100598354, 129.9841967044819739 ) ) ;
#36080 = VERTEX_POINT ( 'NONE', #34740 ) ;
#36081 = ORIENTED_EDGE ( 'NONE', *, *, #40872, .T. ) ;
#36082 = ORIENTED_EDGE ( 'NONE', *, *, #66602, .T. ) ;
#36083 = AXIS2_PLACEMENT_3D ( 'NONE', #53684, #68694, #39627 ) ;
#36084 = CARTESIAN_POINT ( 'NONE',  ( 2.899933897858971488, 70.17843983949715891, 130.5244343740981776 ) ) ;
#36085 = PLANE ( 'NONE',  #54836 ) ;
#36086 = CIRCLE ( 'NONE', #46226, 3.000000000000002665 ) ;
#36087 = CARTESIAN_POINT ( 'NONE',  ( 22.49563609058249725, -67.87844715994100397, 307.9888746672805269 ) ) ;
#36088 = DIRECTION ( 'NONE',  ( -1.000000000000000000, 0.000000000000000000, 0.000000000000000000 ) ) ;
#36089 = CARTESIAN_POINT ( 'NONE',  ( 115.4521610479674081, -32.75750308622325946, 211.9966617981629611 ) ) ;
#36090 = DIRECTION ( 'NONE',  ( -1.000000000000000000, 0.000000000000000000, 0.000000000000000000 ) ) ;
#36091 = PLANE ( 'NONE',  #31510 ) ;
#36092 = ORIENTED_EDGE ( 'NONE', *, *, #6909, .T. ) ;
#36094 = ORIENTED_EDGE ( 'NONE', *, *, #42100, .T. ) ;
#36093 = ORIENTED_EDGE ( 'NONE', *, *, #69440, .F. ) ;
#36095 = VECTOR ( 'NONE', #82612, 1000.000000000000114 ) ;
#36096 = PLANE ( 'NONE',  #72326 ) ;
#36097 = ORIENTED_EDGE ( 'NONE', *, *, #20866, .F. ) ;
#36098 = VERTEX_POINT ( 'NONE', #69722 ) ;
#36099 = CARTESIAN_POINT ( 'NONE',  ( 163.0959832912772924, -23.42844715993538074, 237.4678068554150059 ) ) ;
#36100 = DIRECTION ( 'NONE',  ( 0.000000000000000000, 0.000000000000000000, 1.000000000000000000 ) ) ;
#36101 = CARTESIAN_POINT ( 'NONE',  ( 109.7775653660112596, -28.26114369521987868, 231.2615833058969770 ) ) ;
#36102 = CARTESIAN_POINT ( 'NONE',  ( 98.30753348724731211, -41.72887427465273191, 271.7397918317862491 ) ) ;
#36103 = ORIENTED_EDGE ( 'NONE', *, *, #87758, .F. ) ;
#36104 = EDGE_CURVE ( 'NONE', #86177, #47225, #7493, .T. ) ;
#36105 = CARTESIAN_POINT ( 'NONE',  ( 101.7541625622157540, -42.82727082765900661, 9.635625275910939536 ) ) ;
#36106 = VECTOR ( 'NONE', #40302, 1000.000000000000000 ) ;
#36107 = DIRECTION ( 'NONE',  ( 1.027984282060330356E-15, 1.000000000000000000, 0.000000000000000000 ) ) ;
#36108 = VERTEX_POINT ( 'NONE', #88830 ) ;
#36109 = ORIENTED_EDGE ( 'NONE', *, *, #67740, .T. ) ;
#36110 = CARTESIAN_POINT ( 'NONE',  ( 0.000000000000000000, 82.54999999999999716, 92.46299999999996544 ) ) ;
#36111 = ORIENTED_EDGE ( 'NONE', *, *, #8810, .F. ) ;
#36112 = VERTEX_POINT ( 'NONE', #666 ) ;
#36113 = EDGE_CURVE ( 'NONE', #51823, #8449, #1057, .T. ) ;
#36114 = CARTESIAN_POINT ( 'NONE',  ( 115.2289877667042930, -36.78642703073501252, 261.6395189410197872 ) ) ;
#36115 = CARTESIAN_POINT ( 'NONE',  ( 117.0383059485392607, -33.61350157978694142, 174.0670538473389399 ) ) ;
#36116 = CARTESIAN_POINT ( 'NONE',  ( 111.0741232671659304, -25.60348521778444209, 99.80133956162498521 ) ) ;
#36117 = CARTESIAN_POINT ( 'NONE',  ( 37.03715912545425937, -48.62818131006122258, 313.9678068554150059 ) ) ;
#36118 = LINE ( 'NONE', #84292, #39461 ) ;
#36119 = CARTESIAN_POINT ( 'NONE',  ( 104.3244243092125032, -26.02173531178284804, 241.2880062282919482 ) ) ;
#36120 = CARTESIAN_POINT ( 'NONE',  ( 74.15067561874209900, 127.0000000000000000, 68.53801554307469246 ) ) ;
#36121 = DIRECTION ( 'NONE',  ( -1.000000000000000000, 0.000000000000000000, 0.000000000000000000 ) ) ;
#36122 = VERTEX_POINT ( 'NONE', #6592 ) ;
#36123 = CARTESIAN_POINT ( 'NONE',  ( 4.665904304751420031E-15, 92.07499999999998863, -38.10000000000000142 ) ) ;
#36124 = ORIENTED_EDGE ( 'NONE', *, *, #65670, .T. ) ;
#36125 = VECTOR ( 'NONE', #53642, 1000.000000000000000 ) ;
#36126 = ORIENTED_EDGE ( 'NONE', *, *, #16573, .F. ) ;
#36127 = VECTOR ( 'NONE', #54901, 1000.000000000000000 ) ;
#36128 = AXIS2_PLACEMENT_3D ( 'NONE', #83581, #21345, #62222 ) ;
#36129 = EDGE_CURVE ( 'NONE', #18171, #36809, #70709, .T. ) ;
#36130 = CARTESIAN_POINT ( 'NONE',  ( 103.5274535807004384, -26.83869072616077744, 190.3499109901969746 ) ) ;
#36131 = ORIENTED_EDGE ( 'NONE', *, *, #4895, .F. ) ;
#36132 = CARTESIAN_POINT ( 'NONE',  ( 109.2014631304945027, -26.52509060526352869, 139.9127681330539872 ) ) ;
#36133 = CARTESIAN_POINT ( 'NONE',  ( 52.06670390244699576, -67.87844715994100397, 55.21780685541800437 ) ) ;
#36134 = LINE ( 'NONE', #22080, #49305 ) ;
#36135 = CARTESIAN_POINT ( 'NONE',  ( 182.2738106836200132, -23.19206098993950604, -5.074374724088000832 ) ) ;
#36138 = CARTESIAN_POINT ( 'NONE',  ( 100.8614382317055345, -45.12360235833653377, 253.0699109901968882 ) ) ;
#36137 = DIRECTION ( 'NONE',  ( 0.000000000000000000, 1.000000000000000000, 0.000000000000000000 ) ) ;
#36136 = CARTESIAN_POINT ( 'NONE',  ( 74.38348329127296665, -71.52944715994141234, 361.9756252759109998 ) ) ;
#36139 = CARTESIAN_POINT ( 'NONE',  ( 107.0667039024470313, -104.2784471599413934, 2.217806855418003043 ) ) ;
#36140 = CARTESIAN_POINT ( 'NONE',  ( 103.1875000000000000, 127.0000000000000000, 3.602774393244745134E-13 ) ) ;
#36141 = DIRECTION ( 'NONE',  ( -1.000000000000000078E-15, 1.000000000000000000, 0.000000000000000000 ) ) ;
#36142 = AXIS2_PLACEMENT_3D ( 'NONE', #81808, #13206, #20020 ) ;
#36143 = CARTESIAN_POINT ( 'NONE',  ( 177.8371591254545194, -47.82818131005477369, 180.4678068554150343 ) ) ;
#36144 = DIRECTION ( 'NONE',  ( 0.9130365726098601531, 0.000000000000000000, 0.4078776986755214828 ) ) ;
#36145 = PRODUCT_RELATED_PRODUCT_CATEGORY ( 'part', '', ( #60378 ) ) ;
#36146 = LINE ( 'NONE', #42048, #27382 ) ;
#36148 = ORIENTED_EDGE ( 'NONE', *, *, #48222, .F. ) ;
#36147 = CARTESIAN_POINT ( 'NONE',  ( 100.1093887754828984, -44.55284168805902567, 266.9984824187678782 ) ) ;
#36149 = CARTESIAN_POINT ( 'NONE',  ( 134.0664832912740110, -36.72944715994100306, -5.074374724089001809 ) ) ;
#36150 = CARTESIAN_POINT ( 'NONE',  ( 117.0544076763083297, -30.30483159375883062, 144.2813395616249750 ) ) ;
#36151 = CARTESIAN_POINT ( 'NONE',  ( 96.17756896972203151, -38.62826926382330583, 42.45181575210199298 ) ) ;
#36152 = CARTESIAN_POINT ( 'NONE',  ( 107.6569575903311318, -47.81316668278100224, 193.6308633711489620 ) ) ;
#36153 = DIRECTION ( 'NONE',  ( 0.000000000000000000, 0.000000000000000000, 1.000000000000000000 ) ) ;
#36154 = VECTOR ( 'NONE', #31435, 1000.000000000000000 ) ;
#36155 = DIRECTION ( 'NONE',  ( 0.000000000000000000, 1.000000000000000000, 0.000000000000000000 ) ) ;
#36157 = CARTESIAN_POINT ( 'NONE',  ( 107.0667039024470313, -104.2784471599409528, 45.21780685541799727 ) ) ;
#36156 = LINE ( 'NONE', #77492, #34818 ) ;
#36158 = LINE ( 'NONE', #15723, #8946 ) ;
#36159 = LINE ( 'NONE', #70684, #40748 ) ;
#36160 = ORIENTED_EDGE ( 'NONE', *, *, #8465, .F. ) ;
#36161 = FACE_OUTER_BOUND ( 'NONE', #6157, .T. ) ;
#36162 = ORIENTED_EDGE ( 'NONE', *, *, #71384, .T. ) ;
#36163 = VERTEX_POINT ( 'NONE', #34287 ) ;
#36164 = EDGE_CURVE ( 'NONE', #50049, #45547, #61994, .T. ) ;
#36165 = AXIS2_PLACEMENT_3D ( 'NONE', #58128, #36353, #23631 ) ;
#36167 = ORIENTED_EDGE ( 'NONE', *, *, #40677, .F. ) ;
#36166 = DIRECTION ( 'NONE',  ( -1.000000000000000000, 0.000000000000000000, 0.000000000000000000 ) ) ;
#36168 = EDGE_CURVE ( 'NONE', #44336, #40469, #27478, .T. ) ;
#36169 = CARTESIAN_POINT ( 'NONE',  ( 99.31004196827758790, -43.71529311364903947, 52.90991099019698396 ) ) ;
#36170 = DIRECTION ( 'NONE',  ( 0.000000000000000000, 0.000000000000000000, 1.000000000000000000 ) ) ;
#36171 = EDGE_CURVE ( 'NONE', #82352, #58613, #61100, .T. ) ;
#36172 = LINE ( 'NONE', #57044, #60227 ) ;
#36173 = CARTESIAN_POINT ( 'NONE',  ( 104.5521338839504608, -48.36083399734661725, 178.4070538473399665 ) ) ;
#36174 = ADVANCED_FACE ( 'NONE', ( #58318 ), #57871, .T. ) ;
#36175 = CARTESIAN_POINT ( 'NONE',  ( 114.5003125304781122, -32.48770244606883040, 288.6609912566482308 ) ) ;
#36176 = ORIENTED_EDGE ( 'NONE', *, *, #84353, .F. ) ;
#36177 = AXIS2_PLACEMENT_3D ( 'NONE', #35619, #41974, #50133 ) ;
#36178 = EDGE_LOOP ( 'NONE', ( #51229, #33222, #62000, #33702 ) ) ;
#36179 = EDGE_LOOP ( 'NONE', ( #55323, #71213, #18134 ) ) ;
#36180 = VERTEX_POINT ( 'NONE', #42883 ) ;
#36181 = CARTESIAN_POINT ( 'NONE',  ( 131.0667039024480687, -58.72944715994092491, 231.5838068554170093 ) ) ;
#36182 = CARTESIAN_POINT ( 'NONE',  ( 181.8884939055940038, -32.11662333284530746, -5.074374724088000832 ) ) ;
#36183 = CARTESIAN_POINT ( 'NONE',  ( 100.9544197307436093, -28.70722375064775278, 161.5939840054776653 ) ) ;
#36184 = FACE_OUTER_BOUND ( 'NONE', #48972, .T. ) ;
#36185 = DIRECTION ( 'NONE',  ( 0.000000000000000000, -1.000000000000000000, 0.000000000000000000 ) ) ;
#36186 = DIRECTION ( 'NONE',  ( 0.5000000000000015543, 0.8660254037844377084, -2.688821387764056676E-14 ) ) ;
#36187 = ADVANCED_FACE ( 'NONE', ( #63347 ), #70616, .T. ) ;
#36188 = DIRECTION ( 'NONE',  ( 0.000000000000000000, -1.000000000000000000, 0.000000000000000000 ) ) ;
#36189 = DIRECTION ( 'NONE',  ( 0.000000000000000000, 0.000000000000000000, 1.000000000000000000 ) ) ;
#36190 = EDGE_CURVE ( 'NONE', #7721, #2591, #23383, .T. ) ;
#36191 = CARTESIAN_POINT ( 'NONE',  ( 114.8031991714177451, -43.68443766454706889, 38.24419670448192221 ) ) ;
#36192 = ORIENTED_EDGE ( 'NONE', *, *, #51672, .T. ) ;
#36193 = VECTOR ( 'NONE', #21862, 1000.000000000000000 ) ;
#36194 = FACE_OUTER_BOUND ( 'NONE', #80357, .T. ) ;
#36195 = CARTESIAN_POINT ( 'NONE',  ( 114.1400169897070924, -40.01656155057797548, 9.425625275910977763 ) ) ;
#36196 = CARTESIAN_POINT ( 'NONE',  ( 100.1260263088618103, -41.89964850235647020, 109.6661856076859607 ) ) ;
#36197 = CIRCLE ( 'NONE', #52107, 2.749999999999974687 ) ;
#36198 = CIRCLE ( 'NONE', #81214, 3.174999999999997158 ) ;
#36199 = FACE_OUTER_BOUND ( 'NONE', #16176, .T. ) ;
#36200 = LINE ( 'NONE', #29841, #86590 ) ;
#36201 = ORIENTED_EDGE ( 'NONE', *, *, #23070, .T. ) ;
#36202 = ORIENTED_EDGE ( 'NONE', *, *, #12697, .T. ) ;
#36203 = CARTESIAN_POINT ( 'NONE',  ( 98.15098810655345574, -41.26163425357335512, 136.7008391909870113 ) ) ;
#36204 = ORIENTED_EDGE ( 'NONE', *, *, #10565, .T. ) ;
#36205 = ORIENTED_EDGE ( 'NONE', *, *, #15570, .T. ) ;
#36206 = STYLED_ITEM ( 'NONE', ( #8224 ), #3408 ) ;
#36207 = CARTESIAN_POINT ( 'NONE',  ( 103.0939887460847189, -28.21499987170311385, 131.8434880678019567 ) ) ;
#36208 = DIRECTION ( 'NONE',  ( 0.000000000000000000, -1.000000000000000000, 0.000000000000000000 ) ) ;
#36209 = AXIS2_PLACEMENT_3D ( 'NONE', #33417, #30853, #58110 ) ;
#36211 = EDGE_CURVE ( 'NONE', #72546, #31377, #22926, .T. ) ;
#36210 = CARTESIAN_POINT ( 'NONE',  ( 96.00057345886969529, -37.20991081664785582, 112.3489586092449599 ) ) ;
#36212 = CARTESIAN_POINT ( 'NONE',  ( 112.0733969452682004, -45.39207061711373825, 17.99352580270544522 ) ) ;
#36213 = ORIENTED_EDGE ( 'NONE', *, *, #4599, .F. ) ;
#36214 = CIRCLE ( 'NONE', #43455, 2.517500000000000071 ) ;
#36215 = ORIENTED_EDGE ( 'NONE', *, *, #62372, .T. ) ;
#36216 = ORIENTED_EDGE ( 'NONE', *, *, #50859, .F. ) ;
#36217 = EDGE_CURVE ( 'NONE', #2787, #66733, #64693, .T. ) ;
#36218 = CIRCLE ( 'NONE', #44888, 179.8898777604655095 ) ;
#36219 = CARTESIAN_POINT ( 'NONE',  ( 96.69274360309970007, -38.23738870492909570, 66.44133956162495735 ) ) ;
#36220 = ORIENTED_EDGE ( 'NONE', *, *, #79231, .F. ) ;
#36221 = CARTESIAN_POINT ( 'NONE',  ( 105.1675567143510079, -46.98732170830152910, 12.42991099019596923 ) ) ;
#36222 = CARTESIAN_POINT ( 'NONE',  ( 97.36185206511996171, -42.06848625969246314, 172.7146728949589942 ) ) ;
#36223 = CARTESIAN_POINT ( 'NONE',  ( 7.661254700127833495, 82.54999999999999716, 320.6630000000000109 ) ) ;
#36224 = CYLINDRICAL_SURFACE ( 'NONE', #38768, 4.750000000000004441 ) ;
#36225 = CARTESIAN_POINT ( 'NONE',  ( 108.5897967589408495, -47.07840195076833112, 138.6927681330539883 ) ) ;
#36226 = LINE ( 'NONE', #49388, #69795 ) ;
#36227 = ORIENTED_EDGE ( 'NONE', *, *, #54677, .T. ) ;
#36228 = CARTESIAN_POINT ( 'NONE',  ( 168.5667039024483529, -48.82844715993517326, 300.4678068554149490 ) ) ;
#36229 = PRODUCT ( 'Rotary Table Central Base', 'Rotary Table Central Base', '', ( #25868 ) ) ;
#36230 = ORIENTED_EDGE ( 'NONE', *, *, #63006, .F. ) ;
#36231 = CARTESIAN_POINT ( 'NONE',  ( 97.92324688886398576, -40.78073627936089451, 132.6587986620884863 ) ) ;
#36232 = VERTEX_POINT ( 'NONE', #56971 ) ;
#36234 = ORIENTED_EDGE ( 'NONE', *, *, #61861, .F. ) ;
#36233 = CIRCLE ( 'NONE', #41986, 29.00000000000000000 ) ;
#36235 = LINE ( 'NONE', #63946, #73620 ) ;
#36236 = EDGE_CURVE ( 'NONE', #70138, #51366, #16546, .T. ) ;
#36237 = DIRECTION ( 'NONE',  ( 0.000000000000000000, 0.000000000000000000, -1.000000000000000000 ) ) ;
#36238 = CARTESIAN_POINT ( 'NONE',  ( 105.3203727031265373, -26.45150370518939198, 15.20991099019697401 ) ) ;
#36239 = CARTESIAN_POINT ( 'NONE',  ( 20.83015309964465800, 62.29495534028188786, 31.90425691968162170 ) ) ;
#36240 = DIRECTION ( 'NONE',  ( -1.000000000000000000, -4.163336342344333240E-14, 0.000000000000000000 ) ) ;
#36241 = LINE ( 'NONE', #85756, #7867 ) ;
#36242 = CARTESIAN_POINT ( 'NONE',  ( 99.61812512063040970, -43.94476044465314857, 41.95086337115000674 ) ) ;
#36244 = CARTESIAN_POINT ( 'NONE',  ( 97.85535806214043930, -31.89376338832687097, 131.9413395616259947 ) ) ;
#36243 = CARTESIAN_POINT ( 'NONE',  ( 34.96670390244699433, -28.27351298637401200, -5.074374724088000832 ) ) ;
#36245 = DIRECTION ( 'NONE',  ( 1.000000000000000000, 0.000000000000000000, 0.000000000000000000 ) ) ;
#36246 = FACE_OUTER_BOUND ( 'NONE', #14856, .T. ) ;
#36247 = ORIENTED_EDGE ( 'NONE', *, *, #4165, .T. ) ;
#36248 = DIRECTION ( 'NONE',  ( -3.100000000000000258E-29, 3.100000000000000044E-14, 1.000000000000000000 ) ) ;
#36249 = AXIS2_PLACEMENT_3D ( 'NONE', #13284, #67794, #73715 ) ;
#36250 = DIRECTION ( 'NONE',  ( -0.4214249218767880945, -0.9068632946707806397, -4.214249218767889924E-16 ) ) ;
#36251 = CARTESIAN_POINT ( 'NONE',  ( 97.06670390244701707, -98.59953881414064369, 19.21780685541782319 ) ) ;
#36252 = ORIENTED_EDGE ( 'NONE', *, *, #35839, .F. ) ;
#36253 = CIRCLE ( 'NONE', #14475, 13.09746158385919124 ) ;
#36254 = ADVANCED_FACE ( 'NONE', ( #44224 ), #71965, .F. ) ;
#36255 = CARTESIAN_POINT ( 'NONE',  ( 87.06648329127402519, -54.72944906728955061, 14.92562527591094934 ) ) ;
#36257 = ORIENTED_EDGE ( 'NONE', *, *, #41084, .T. ) ;
#36256 = CARTESIAN_POINT ( 'NONE',  ( 102.6649408499558689, -27.23033719207987602, 180.4213395616249898 ) ) ;
#36258 = LINE ( 'NONE', #21284, #69789 ) ;
#36259 = CARTESIAN_POINT ( 'NONE',  ( 118.8146046005060015, -38.46262239392275717, 219.7099109901969882 ) ) ;
#36260 = CARTESIAN_POINT ( 'NONE',  ( 113.4418579183357849, -27.64362872000679516, 80.57753003781597556 ) ) ;
#36261 = CARTESIAN_POINT ( 'NONE',  ( 95.69968022530667895, 70.80031561532538831, 88.80809839403396211 ) ) ;
#36262 = CARTESIAN_POINT ( 'NONE',  ( 106.0667039024470455, -121.2010968907525239, -21.78219314458149114 ) ) ;
#36263 = DIRECTION ( 'NONE',  ( 0.7071067811869841124, -0.7071067811861110330, 0.000000000000000000 ) ) ;
#36264 = ORIENTED_EDGE ( 'NONE', *, *, #40858, .T. ) ;
#36265 = CIRCLE ( 'NONE', #68159, 179.8898777604655095 ) ;
#36266 = ADVANCED_FACE ( 'NONE', ( #43336 ), #36091, .F. ) ;
#36267 = ORIENTED_EDGE ( 'NONE', *, *, #34507, .T. ) ;
#36268 = VERTEX_POINT ( 'NONE', #29286 ) ;
#36269 = AXIS2_PLACEMENT_3D ( 'NONE', #7834, #1027, #78251 ) ;
#36270 = ORIENTED_EDGE ( 'NONE', *, *, #36381, .T. ) ;
#36271 = DIRECTION ( 'NONE',  ( 1.000000000000000000, -5.337610695313248426E-16, 0.000000000000000000 ) ) ;
#36272 = CARTESIAN_POINT ( 'NONE',  ( 112.4893506266177070, -46.36098340020668473, 253.9965776568634510 ) ) ;
#36273 = CARTESIAN_POINT ( 'NONE',  ( 34.96670390244738513, -26.71338133339315490, 313.9678068554150059 ) ) ;
#36274 = CARTESIAN_POINT ( 'NONE',  ( 136.4174407532304940, -17.29868422071827183, 2.608896314067475242 ) ) ;
#36275 = CARTESIAN_POINT ( 'NONE',  ( 74.36911441044796334, 82.54999999999999716, -92.32962665258483526 ) ) ;
#36276 = EDGE_CURVE ( 'NONE', #45648, #60002, #14091, .T. ) ;
#36277 = VECTOR ( 'NONE', #78614, 1000.000000000000000 ) ;
#36279 = FACE_OUTER_BOUND ( 'NONE', #77126, .T. ) ;
#36278 = FACE_OUTER_BOUND ( 'NONE', #62522, .T. ) ;
#36280 = FACE_OUTER_BOUND ( 'NONE', #3027, .T. ) ;
#36281 = CARTESIAN_POINT ( 'NONE',  ( 118.0989925035467252, -37.71898322177068508, 33.74324432352998571 ) ) ;
#36282 = ORIENTED_EDGE ( 'NONE', *, *, #58108, .F. ) ;
#36283 = VERTEX_POINT ( 'NONE', #1584 ) ;
#36284 = ORIENTED_EDGE ( 'NONE', *, *, #41980, .F. ) ;
#36285 = LINE ( 'NONE', #22671, #73210 ) ;
#36286 = DIRECTION ( 'NONE',  ( -1.000000000000000000, 0.000000000000000000, 0.000000000000000000 ) ) ;
#36287 = CARTESIAN_POINT ( 'NONE',  ( 115.4101910119109533, -30.57141770992062035, 255.3203871806724123 ) ) ;
#36288 = AXIS2_PLACEMENT_3D ( 'NONE', #73321, #72444, #37918 ) ;
#36289 = DIRECTION ( 'NONE',  ( 1.000000000000000000, 4.299999999999999979E-14, 1.000000000000000078E-15 ) ) ;
#36290 = EDGE_CURVE ( 'NONE', #78258, #56977, #88080, .T. ) ;
#36291 = CARTESIAN_POINT ( 'NONE',  ( 96.47668441219811086, -40.11591174724600251, 127.5727681330529606 ) ) ;
#36292 = ADVANCED_FACE ( 'NONE', ( #2475 ), #30617, .F. ) ;
#36293 = EDGE_CURVE ( 'NONE', #86673, #57650, #23816, .T. ) ;
#36294 = FACE_OUTER_BOUND ( 'NONE', #43085, .T. ) ;
#36295 = ORIENTED_EDGE ( 'NONE', *, *, #22226, .F. ) ;
#36296 = DIRECTION ( 'NONE',  ( 0.000000000000000000, 0.000000000000000000, 1.000000000000000000 ) ) ;
#36297 = CARTESIAN_POINT ( 'NONE',  ( 77.80861903141534697, -35.15582774928859067, 2.518078172607126408 ) ) ;
#36298 = EDGE_CURVE ( 'NONE', #4135, #22294, #60490, .T. ) ;
#36299 = EDGE_LOOP ( 'NONE', ( #59383, #82039 ) ) ;
#36300 = ORIENTED_EDGE ( 'NONE', *, *, #21734, .F. ) ;
#36301 = AXIS2_PLACEMENT_3D ( 'NONE', #82239, #437, #54475 ) ;
#36302 = CARTESIAN_POINT ( 'NONE',  ( -87.45628510944614220, 94.12556101775332706, 80.04418453221629193 ) ) ;
#36303 = CARTESIAN_POINT ( 'NONE',  ( 101.0802515965118573, -30.15484820110618358, 282.0958690201827039 ) ) ;
#36304 = DIRECTION ( 'NONE',  ( 0.000000000000000000, 0.000000000000000000, -1.000000000000000000 ) ) ;
#36305 = CARTESIAN_POINT ( 'NONE',  ( 108.4174892614935004, -26.73503592907457005, 84.96895860849961934 ) ) ;
#36306 = DIRECTION ( 'NONE',  ( 0.000000000000000000, 1.000000000000000000, 0.000000000000000000 ) ) ;
#36307 = EDGE_LOOP ( 'NONE', ( #45398, #72943, #24001 ) ) ;
#36308 = AXIS2_PLACEMENT_3D ( 'NONE', #60750, #81234, #59847 ) ;
#36309 = CARTESIAN_POINT ( 'NONE',  ( 19.56648329127303043, -71.37844715994266664, 342.9256252759109884 ) ) ;
#36310 = LINE ( 'NONE', #43549, #9240 ) ;
#36311 = EDGE_LOOP ( 'NONE', ( #34892, #43070 ) ) ;
#36312 = CARTESIAN_POINT ( 'NONE',  ( 104.7595363604009435, -46.89630637601933927, 72.39848241876795498 ) ) ;
#36313 = ORIENTED_EDGE ( 'NONE', *, *, #69379, .F. ) ;
#36314 = CARTESIAN_POINT ( 'NONE',  ( 102.5950791370611768, -45.34791940167762192, 16.61813411379198158 ) ) ;
#36315 = CIRCLE ( 'NONE', #79841, 3.499999999999996003 ) ;
#36316 = LINE ( 'NONE', #76751, #25619 ) ;
#36317 = CARTESIAN_POINT ( 'NONE',  ( 104.7173522264389334, -47.59653351925024367, 182.4070538473399665 ) ) ;
#36318 = DIRECTION ( 'NONE',  ( 0.000000000000000000, 0.000000000000000000, -1.000000000000000000 ) ) ;
#36319 = DIRECTION ( 'NONE',  ( -2.999999999999999839E-15, 1.000000000000000000, -2.999999999999999900E-30 ) ) ;
#36320 = DIRECTION ( 'NONE',  ( 1.699132800883997481E-15, 0.000000000000000000, -1.000000000000000000 ) ) ;
#36321 = CARTESIAN_POINT ( 'NONE',  ( 68.90655442492621319, -69.55252416307811814, 247.4986722481951631 ) ) ;
#36322 = CARTESIAN_POINT ( 'NONE',  ( 116.6217178149748008, -42.37701578139068204, 279.4137205140061724 ) ) ;
#36323 = CARTESIAN_POINT ( 'NONE',  ( 78.17042387453767560, 92.64232203292142742, -89.13693605261687480 ) ) ;
#36324 = VECTOR ( 'NONE', #78620, 999.9999999999998863 ) ;
#36325 = VERTEX_POINT ( 'NONE', #9285 ) ;
#36326 = DIRECTION ( 'NONE',  ( -1.000000000000000078E-15, 0.000000000000000000, -1.000000000000000000 ) ) ;
#36327 = ORIENTED_EDGE ( 'NONE', *, *, #32450, .F. ) ;
#36328 = CARTESIAN_POINT ( 'NONE',  ( 97.70743813507087339, -42.69650533217181021, 137.7661014663869992 ) ) ;
#36329 = DIRECTION ( 'NONE',  ( -1.000000000000000000, 0.000000000000000000, 0.000000000000000000 ) ) ;
#36330 = ORIENTED_EDGE ( 'NONE', *, *, #7082, .T. ) ;
#36331 = ORIENTED_EDGE ( 'NONE', *, *, #48971, .F. ) ;
#36332 = EDGE_CURVE ( 'NONE', #22610, #24378, #32942, .T. ) ;
#36333 = ORIENTED_EDGE ( 'NONE', *, *, #3684, .F. ) ;
#36334 = CIRCLE ( 'NONE', #53729, 0.5000000000000004441 ) ;
#36335 = FACE_OUTER_BOUND ( 'NONE', #86783, .T. ) ;
#36336 = CARTESIAN_POINT ( 'NONE',  ( 97.31583813429813290, -39.30595438711576151, 267.5314568493160436 ) ) ;
#36337 = DIRECTION ( 'NONE',  ( -1.175184669632759901E-16, 1.000000000000000000, 2.000000000000003705E-15 ) ) ;
#36338 = DIRECTION ( 'NONE',  ( 1.000000000000000000, 0.000000000000000000, 0.000000000000000000 ) ) ;
#36339 = DIRECTION ( 'NONE',  ( -1.000000000000000000, -4.299999999999999979E-14, -1.000000000000000078E-15 ) ) ;
#36340 = CARTESIAN_POINT ( 'NONE',  ( 113.7700232194324883, -29.06831460768450626, 285.5032443235299979 ) ) ;
#36341 = LINE ( 'NONE', #57666, #72585 ) ;
#36342 = EDGE_LOOP ( 'NONE', ( #18800, #76051, #44238, #14331 ) ) ;
#36343 = DIRECTION ( 'NONE',  ( 1.000000000000000000, 1.000000000000000078E-15, 0.000000000000000000 ) ) ;
#36344 = MECHANICAL_DESIGN_GEOMETRIC_PRESENTATION_REPRESENTATION (  '', ( #31789 ), #78247 ) ;
#36345 = DIRECTION ( 'NONE',  ( 0.7071067811566161820, 0.7071067812164789634, 0.000000000000000000 ) ) ;
#36346 = ORIENTED_EDGE ( 'NONE', *, *, #84172, .T. ) ;
#36347 = ORIENTED_EDGE ( 'NONE', *, *, #41285, .T. ) ;
#36348 = CARTESIAN_POINT ( 'NONE',  ( 80.81785596311139841, -21.40256188477534138, 1.690787648075373850 ) ) ;
#36349 = EDGE_CURVE ( 'NONE', #31634, #61394, #7935, .T. ) ;
#36350 = DIRECTION ( 'NONE',  ( -1.000000000000000000, 0.000000000000000000, -9.713237310806269221E-16 ) ) ;
#36351 = PLANE ( 'NONE',  #13868 ) ;
#36352 = ADVANCED_FACE ( 'NONE', ( #22036 ), #57452, .F. ) ;
#36353 = DIRECTION ( 'NONE',  ( -4.237773401492740281E-14, 1.000000000000000000, 0.000000000000000000 ) ) ;
#36354 = CARTESIAN_POINT ( 'NONE',  ( -179.8898777604655095, 0.000000000000000000, 114.2999999999999972 ) ) ;
#36355 = CIRCLE ( 'NONE', #66810, 16.33514202138210791 ) ;
#36356 = CARTESIAN_POINT ( 'NONE',  ( 113.9432952986174854, -30.83689873488770061, 228.8248007804579629 ) ) ;
#36357 = DIRECTION ( 'NONE',  ( 0.000000000000000000, 0.000000000000000000, -1.000000000000000000 ) ) ;
#36358 = CARTESIAN_POINT ( 'NONE',  ( 124.7484337486687593, 70.55550032976780983, 38.50686379248426761 ) ) ;
#36359 = CARTESIAN_POINT ( 'NONE',  ( 113.5334051825838202, -28.49624685289517245, 79.54705384733995288 ) ) ;
#36360 = ORIENTED_EDGE ( 'NONE', *, *, #15464, .T. ) ;
#36361 = DIRECTION ( 'NONE',  ( 0.000000000000000000, 0.000000000000000000, 1.000000000000000000 ) ) ;
#36362 = ORIENTED_EDGE ( 'NONE', *, *, #34513, .F. ) ;
#36363 = ADVANCED_FACE ( 'NONE', ( #31945 ), #3363, .T. ) ;
#36364 = VECTOR ( 'NONE', #58378, 1000.000000000000000 ) ;
#36365 = CARTESIAN_POINT ( 'NONE',  ( 97.81219807385008380, -40.51719912245609123, 147.6362401243850115 ) ) ;
#36366 = DIRECTION ( 'NONE',  ( -4.237773401492740281E-14, 1.000000000000000000, 0.000000000000000000 ) ) ;
#36367 = ORIENTED_EDGE ( 'NONE', *, *, #66428, .T. ) ;
#36368 = EDGE_CURVE ( 'NONE', #65418, #78803, #52358, .T. ) ;
#36369 = ADVANCED_FACE ( 'NONE', ( #3804 ), #25580, .F. ) ;
#36370 = DIRECTION ( 'NONE',  ( 9.351236661543306751E-17, -3.725950533538267725E-29, -1.000000000000000000 ) ) ;
#36371 = ORIENTED_EDGE ( 'NONE', *, *, #56729, .F. ) ;
#36372 = DIRECTION ( 'NONE',  ( 0.000000000000000000, 0.000000000000000000, -1.000000000000000000 ) ) ;
#36373 = CARTESIAN_POINT ( 'NONE',  ( 104.4091780781909335, -46.45840484912275059, 273.3644384837980965 ) ) ;
#36374 = VECTOR ( 'NONE', #33055, 1000.000000000000000 ) ;
#36375 = EDGE_CURVE ( 'NONE', #59958, #56065, #66012, .T. ) ;
#36376 = DIRECTION ( 'NONE',  ( 0.7071067811865473507, 0.7071067811865476838, 0.000000000000000000 ) ) ;
#36377 = EDGE_CURVE ( 'NONE', #20562, #60619, #53255, .T. ) ;
#36378 = ORIENTED_EDGE ( 'NONE', *, *, #11997, .F. ) ;
#36379 = CARTESIAN_POINT ( 'NONE',  ( 97.60225484043094468, -32.22203741027808377, 75.97276813305397525 ) ) ;
#36380 = SURFACE_STYLE_FILL_AREA ( #7770 ) ;
#36381 = EDGE_CURVE ( 'NONE', #86672, #64424, #11513, .T. ) ;
#36382 = CARTESIAN_POINT ( 'NONE',  ( 193.0371591254575208, -23.42818131005411075, 117.4678068554150627 ) ) ;
#36383 = LINE ( 'NONE', #15498, #26353 ) ;
#36384 = DIRECTION ( 'NONE',  ( 1.000000000000000000, 0.000000000000000000, 0.000000000000000000 ) ) ;
#36385 = ORIENTED_EDGE ( 'NONE', *, *, #42084, .F. ) ;
#36386 = EDGE_CURVE ( 'NONE', #3581, #32750, #72409, .T. ) ;
#36387 = CARTESIAN_POINT ( 'NONE',  ( 108.5609052613744012, -26.81332519519535040, 120.9559658802212567 ) ) ;
#36388 = CARTESIAN_POINT ( 'NONE',  ( 149.4409906032288404, -0.9156555935619370423, 361.9756252759100335 ) ) ;
#36389 = AXIS2_PLACEMENT_3D ( 'NONE', #17082, #44770, #72496 ) ;
#36390 = EDGE_CURVE ( 'NONE', #54558, #35318, #4699, .T. ) ;
#36391 = LINE ( 'NONE', #63640, #61746 ) ;
#36392 = AXIS2_PLACEMENT_3D ( 'NONE', #71370, #23232, #9136 ) ;
#36393 = VECTOR ( 'NONE', #30355, 1000.000000000000000 ) ;
#36394 = CARTESIAN_POINT ( 'NONE',  ( 101.4892552882362793, -27.89588691190665060, 106.5241967044819944 ) ) ;
#36396 = DIRECTION ( 'NONE',  ( 0.000000000000000000, 0.000000000000000000, -1.000000000000000000 ) ) ;
#36395 = LINE ( 'NONE', #83203, #78424 ) ;
#36397 = DIRECTION ( 'NONE',  ( -2.999999999999999839E-15, 1.000000000000000000, -2.999999999999999900E-30 ) ) ;
#36398 = AXIS2_PLACEMENT_3D ( 'NONE', #45826, #10005, #60361 ) ;
#36399 = ORIENTED_EDGE ( 'NONE', *, *, #27843, .F. ) ;
#36400 = DIRECTION ( 'NONE',  ( -1.000000000000000078E-15, 1.000000000000000083E-30, 1.000000000000000000 ) ) ;
#36401 = CARTESIAN_POINT ( 'NONE',  ( 117.1372161989436904, -34.25576096370540569, 160.0061014663869798 ) ) ;
#36402 = AXIS2_PLACEMENT_3D ( 'NONE', #78024, #28501, #55735 ) ;
#36404 = ORIENTED_EDGE ( 'NONE', *, *, #83252, .T. ) ;
#36403 = DIRECTION ( 'NONE',  ( 0.000000000000000000, -1.000000000000000000, 0.000000000000000000 ) ) ;
#36405 = ADVANCED_FACE ( 'NONE', ( #66459 ), #86488, .F. ) ;
#36406 = CARTESIAN_POINT ( 'NONE',  ( 99.56037394151449860, -43.88466257697679396, 32.92038718067297509 ) ) ;
#36407 = CARTESIAN_POINT ( 'NONE',  ( 47.62500000000000000, 94.53880000000000905, 246.8562499999999886 ) ) ;
#36408 = CARTESIAN_POINT ( 'NONE',  ( 80.06648329127401098, -41.22944715994105280, 4.925625275910944012 ) ) ;
#36410 = ADVANCED_FACE ( 'NONE', ( #25133 ), #18770, .T. ) ;
#36409 = CARTESIAN_POINT ( 'NONE',  ( 119.9305508289310609, -79.89790063748476712, 250.2178068554179902 ) ) ;
#36411 = CYLINDRICAL_SURFACE ( 'NONE', #89191, 2.517500000000005844 ) ;
#36412 = AXIS2_PLACEMENT_3D ( 'NONE', #36701, #69872, #37145 ) ;
#36413 = EDGE_CURVE ( 'NONE', #62685, #76826, #17435, .T. ) ;
#36414 = PLANE ( 'NONE',  #25491 ) ;
#36415 = EDGE_CURVE ( 'NONE', #16965, #79928, #4249, .T. ) ;
#36416 = CARTESIAN_POINT ( 'NONE',  ( 110.5849939505706772, -26.97450646431652643, 249.7889586092449576 ) ) ;
#36417 = ORIENTED_EDGE ( 'NONE', *, *, #22350, .F. ) ;
#36418 = ORIENTED_EDGE ( 'NONE', *, *, #23450, .F. ) ;
#36419 = CARTESIAN_POINT ( 'NONE',  ( 102.8032110495234264, -45.10208326393837552, 168.6453928297069353 ) ) ;
#36420 = DIRECTION ( 'NONE',  ( 0.000000000000000000, 1.000000000000000000, 0.000000000000000000 ) ) ;
#36421 = CARTESIAN_POINT ( 'NONE',  ( 98.44769980935930676, -38.78975051229773641, 52.94444044875496047 ) ) ;
#36422 = CARTESIAN_POINT ( 'NONE',  ( -96.20686424029877060, 93.94566094357732311, 88.25669247804634665 ) ) ;
#36423 = VECTOR ( 'NONE', #6066, 1000.000000000000000 ) ;
#36424 = DIRECTION ( 'NONE',  ( 0.000000000000000000, 0.000000000000000000, 1.000000000000000000 ) ) ;
#36425 = DIRECTION ( 'NONE',  ( 1.000000000000000000, 0.000000000000000000, 0.000000000000000000 ) ) ;
#36426 = VECTOR ( 'NONE', #76824, 1000.000000000000000 ) ;
#36427 = LINE ( 'NONE', #84585, #76887 ) ;
#36428 = CYLINDRICAL_SURFACE ( 'NONE', #11084, 0.4999999999999982236 ) ;
#36429 = CARTESIAN_POINT ( 'NONE',  ( 103.9458437887065827, -26.80522050874817808, 250.3184824187678714 ) ) ;
#36430 = CARTESIAN_POINT ( 'NONE',  ( 97.12563415398577149, -37.99750651866536089, 171.4272510260306603 ) ) ;
#36431 = ORIENTED_EDGE ( 'NONE', *, *, #4992, .F. ) ;
#36432 = ORIENTED_EDGE ( 'NONE', *, *, #58489, .T. ) ;
#36433 = CARTESIAN_POINT ( 'NONE',  ( -82.89895571708224509, 81.72130195885952730, -100.8594679592214902 ) ) ;
#36434 = CARTESIAN_POINT ( 'NONE',  ( -76.79137032886092129, 90.93965867633431799, -90.32698471909156979 ) ) ;
#36435 = DIRECTION ( 'NONE',  ( -1.000000000000000078E-15, 1.000000000000000083E-30, 1.000000000000000000 ) ) ;
#36436 = DIRECTION ( 'NONE',  ( 0.000000000000000000, 0.000000000000000000, 1.000000000000000000 ) ) ;
#36437 = CIRCLE ( 'NONE', #81380, 2.517500000000005844 ) ;
#36438 = CARTESIAN_POINT ( 'NONE',  ( 97.46604185887804306, -38.76544784714101155, 27.49276813305395706 ) ) ;
#36439 = CARTESIAN_POINT ( 'NONE',  ( 12.59999999999999964, 81.72717280875430390, 117.6834004267382028 ) ) ;
#36440 = VERTEX_POINT ( 'NONE', #45116 ) ;
#36441 = AXIS2_PLACEMENT_3D ( 'NONE', #50502, #24157, #8748 ) ;
#36442 = CARTESIAN_POINT ( 'NONE',  ( 110.8100519147795922, -46.50588177123592715, 58.86705384733998159 ) ) ;
#36443 = CARTESIAN_POINT ( 'NONE',  ( 21.03689327557613709, -23.42844715994197813, 193.9678068554150627 ) ) ;
#36444 = CARTESIAN_POINT ( 'NONE',  ( 117.4908834113230682, -35.85893649831510999, 253.8927681330538348 ) ) ;
#36445 = EDGE_LOOP ( 'NONE', ( #43343, #4169, #42708, #15098 ) ) ;
#36446 = CARTESIAN_POINT ( 'NONE',  ( 107.0667039024470171, -89.08784823670032438, -11.78219314458248057 ) ) ;
#36447 = LINE ( 'NONE', #44572, #47134 ) ;
#36448 = DIRECTION ( 'NONE',  ( 1.000000000000000078E-15, -1.000000000000000083E-30, -1.000000000000000000 ) ) ;
#36449 = CARTESIAN_POINT ( 'NONE',  ( 111.5571307036148312, -44.84917726517733882, 100.7966617981629582 ) ) ;
#36450 = CARTESIAN_POINT ( 'NONE',  ( 99.27233432241882838, -29.77326281039884037, 186.7470538473389752 ) ) ;
#36451 = DIRECTION ( 'NONE',  ( 1.000000000000000000, 0.000000000000000000, -0.000000000000000000 ) ) ;
#36452 = ORIENTED_EDGE ( 'NONE', *, *, #35440, .F. ) ;
#36453 = FACE_OUTER_BOUND ( 'NONE', #19586, .T. ) ;
#36454 = EDGE_LOOP ( 'NONE', ( #29648, #7882, #47193, #56181 ) ) ;
#36456 = ORIENTED_EDGE ( 'NONE', *, *, #31318, .T. ) ;
#36455 = TOROIDAL_SURFACE ( 'NONE', #33587, 10.00000000000000355, 10.00000000000000000 ) ;
#36457 = CYLINDRICAL_SURFACE ( 'NONE', #87960, 1.000000000000000888 ) ;
#36458 = VERTEX_POINT ( 'NONE', #10606 ) ;
#36459 = ORIENTED_EDGE ( 'NONE', *, *, #52457, .T. ) ;
#36460 = DIRECTION ( 'NONE',  ( -1.821299053822143307E-16, 0.000000000000000000, 1.000000000000000000 ) ) ;
#36461 = EDGE_CURVE ( 'NONE', #7095, #65449, #17872, .T. ) ;
#36462 = EDGE_CURVE ( 'NONE', #17437, #28847, #70118, .T. ) ;
#36463 = CARTESIAN_POINT ( 'NONE',  ( 108.4152994148071514, -26.73475809017443794, 24.96913296066860255 ) ) ;
#36464 = CARTESIAN_POINT ( 'NONE',  ( 113.3421067344362996, -42.52364098839497331, 122.6552769709339827 ) ) ;
#36465 = CARTESIAN_POINT ( 'NONE',  ( 110.9007760261032871, -26.97308707819648887, 269.7784824187680783 ) ) ;
#36466 = EDGE_CURVE ( 'NONE', #7668, #80899, #453, .T. ) ;
#36467 = PLANE ( 'NONE',  #67293 ) ;
#36468 = AXIS2_PLACEMENT_3D ( 'NONE', #85210, #28882, #22976 ) ;
#36469 = VERTEX_POINT ( 'NONE', #1813 ) ;
#36470 = EDGE_CURVE ( 'NONE', #34937, #37435, #50185, .T. ) ;
#36471 = EDGE_LOOP ( 'NONE', ( #85678, #56540 ) ) ;
#36472 = CARTESIAN_POINT ( 'NONE',  ( 25.56670390244797275, -67.87844715994100397, 257.2178068554150059 ) ) ;
#36473 = CARTESIAN_POINT ( 'NONE',  ( 83.06670390244796920, -61.87844715994100397, 207.5838068554149913 ) ) ;
#36474 = CARTESIAN_POINT ( 'NONE',  ( 70.61455841086757346, -139.6273172416246950, 247.2949093517953827 ) ) ;
#36475 = EDGE_CURVE ( 'NONE', #32010, #8825, #12526, .T. ) ;
#36476 = CARTESIAN_POINT ( 'NONE',  ( 99.65330034922125435, -46.03930839343899351, 122.0413395616249659 ) ) ;
#36477 = CARTESIAN_POINT ( 'NONE',  ( 80.54920390244805617, -43.72944715994108833, 207.5838068554169809 ) ) ;
#36478 = VERTEX_POINT ( 'NONE', #84036 ) ;
#36479 = CARTESIAN_POINT ( 'NONE',  ( 111.8641478345923019, -46.02505481121716002, 272.9556252759110180 ) ) ;
#36480 = CARTESIAN_POINT ( 'NONE',  ( 98.38769172161842391, -42.09058819985752109, 7.768006228291934434 ) ) ;
#36481 = DIRECTION ( 'NONE',  ( 0.000000000000000000, 0.000000000000000000, -1.000000000000000000 ) ) ;
#36482 = CARTESIAN_POINT ( 'NONE',  ( 31.75000000000000000, 69.84999999999999432, 292.1000000000000227 ) ) ;
#36483 = EDGE_CURVE ( 'NONE', #76542, #42554, #63297, .T. ) ;
#36485 = DIRECTION ( 'NONE',  ( 0.000000000000000000, 0.000000000000000000, -1.000000000000000000 ) ) ;
#36484 = CARTESIAN_POINT ( 'NONE',  ( -487.2989999999999782, 85.41360802895360393, 11.11250000000036131 ) ) ;
#36486 = CARTESIAN_POINT ( 'NONE',  ( 154.5667039024470171, -79.67844715994088745, 120.2178068554179902 ) ) ;
#36487 = DIRECTION ( 'NONE',  ( 0.000000000000000000, 0.000000000000000000, -1.000000000000000000 ) ) ;
#36488 = FACE_OUTER_BOUND ( 'NONE', #45909, .T. ) ;
#36489 = AXIS2_PLACEMENT_3D ( 'NONE', #46628, #60709, #47068 ) ;
#36490 = CARTESIAN_POINT ( 'NONE',  ( -12.59759614370980252, 84.21308071816545748, 129.9468022370901394 ) ) ;
#36491 = DIRECTION ( 'NONE',  ( 4.299999999999999979E-14, -1.000000000000000000, 0.000000000000000000 ) ) ;
#36492 = DIRECTION ( 'NONE',  ( 0.7071067811866279529, -0.7071067811864671926, 7.071067811866286874E-16 ) ) ;
#36493 = EDGE_CURVE ( 'NONE', #12394, #1981, #56753, .T. ) ;
#36495 = ORIENTED_EDGE ( 'NONE', *, *, #81168, .F. ) ;
#36494 = PLANE ( 'NONE',  #74738 ) ;
#36496 = FACE_OUTER_BOUND ( 'NONE', #28611, .T. ) ;
#36497 = CARTESIAN_POINT ( 'NONE',  ( 104.6386611584700432, -47.56081657070318158, 27.38895860924395009 ) ) ;
#36498 = CARTESIAN_POINT ( 'NONE',  ( 117.8006386470660658, -34.09280371250640940, 160.0061014663869798 ) ) ;
#36499 = CARTESIAN_POINT ( 'NONE',  ( 96.81221355789537597, -38.90410760351644370, 27.49276813305395706 ) ) ;
#36500 = AXIS2_PLACEMENT_3D ( 'NONE', #34564, #83631, #81845 ) ;
#36502 = CARTESIAN_POINT ( 'NONE',  ( 107.0664832912739541, -36.72944715994095333, 305.0306255462182321 ) ) ;
#36501 = LINE ( 'NONE', #42387, #52224 ) ;
#36503 = DIRECTION ( 'NONE',  ( 1.054009200593500181E-15, 1.000000000000000000, 0.000000000000000000 ) ) ;
#36504 = EDGE_CURVE ( 'NONE', #89615, #34853, #64726, .T. ) ;
#36505 = VECTOR ( 'NONE', #49944, 1000.000000000000000 ) ;
#36506 = ORIENTED_EDGE ( 'NONE', *, *, #17802, .F. ) ;
#36507 = DIRECTION ( 'NONE',  ( 1.000000000000000000, 0.000000000000000000, 0.000000000000000000 ) ) ;
#36508 = VERTEX_POINT ( 'NONE', #77665 ) ;
#36509 = CARTESIAN_POINT ( 'NONE',  ( 104.2296407737279935, -46.70397019442127373, 63.36800622829197494 ) ) ;
#36511 = ORIENTED_EDGE ( 'NONE', *, *, #60787, .F. ) ;
#36510 = CARTESIAN_POINT ( 'NONE',  ( 4.773412683384191446, 94.31885047369215158, 130.4687102160306438 ) ) ;
#36512 = DIRECTION ( 'NONE',  ( 1.000000000000000000, 4.299999999999999979E-14, 1.000000000000000078E-15 ) ) ;
#36513 = CARTESIAN_POINT ( 'NONE',  ( 100.0229104548316883, -27.23016881827670943, 181.5841967044829630 ) ) ;
#36514 = CARTESIAN_POINT ( 'NONE',  ( 170.2205283966864897, 20.32000000000000028, 79.24800000000000466 ) ) ;
#36515 = CARTESIAN_POINT ( 'NONE',  ( 110.8543535328673073, -45.98428584226713411, 147.8856150920996413 ) ) ;
#36516 = CARTESIAN_POINT ( 'NONE',  ( 122.2221484686746322, -104.2784471599418055, -11.78219314458200984 ) ) ;
#36517 = CARTESIAN_POINT ( 'NONE',  ( 177.8371591254545478, -47.82818131005477369, 129.9678068554150059 ) ) ;
#36518 = AXIS2_PLACEMENT_3D ( 'NONE', #59401, #52568, #85810 ) ;
#36519 = ADVANCED_FACE ( 'NONE', ( #43114 ), #70859, .T. ) ;
#36520 = CARTESIAN_POINT ( 'NONE',  ( 145.1595140859767810, -137.8496423039705121, 247.5170369397599757 ) ) ;
#36521 = CARTESIAN_POINT ( 'NONE',  ( 114.7254303483478992, -43.19231997828638470, 98.26877717035283410 ) ) ;
#36522 = EDGE_CURVE ( 'NONE', #70069, #36736, #62228, .T. ) ;
#36523 = CARTESIAN_POINT ( 'NONE',  ( 117.0231039428183522, -39.62849705588583760, 138.5889586092449690 ) ) ;
#36524 = EDGE_LOOP ( 'NONE', ( #76373, #59409, #20739, #46567 ) ) ;
#36525 = ORIENTED_EDGE ( 'NONE', *, *, #72051, .T. ) ;
#36526 = AXIS2_PLACEMENT_3D ( 'NONE', #6988, #69216, #1530 ) ;
#36527 = CARTESIAN_POINT ( 'NONE',  ( 104.1188366437555288, -45.08645965563772506, 53.73872616303998484 ) ) ;
#36528 = LINE ( 'NONE', #14292, #67501 ) ;
#36530 = CARTESIAN_POINT ( 'NONE',  ( 74.06670390244701707, -90.27844715994098124, 230.7030882296565721 ) ) ;
#36529 = CARTESIAN_POINT ( 'NONE',  ( 98.48461633480667388, -41.42146110206439147, 217.7241967044819546 ) ) ;
#36531 = DIRECTION ( 'NONE',  ( 1.000000000000000078E-15, 1.000000000000000083E-30, -1.000000000000000000 ) ) ;
#36532 = DIRECTION ( 'NONE',  ( 0.7071067811865835440, 0.000000000000000000, 0.7071067811865114905 ) ) ;
#36533 = AXIS2_PLACEMENT_3D ( 'NONE', #68977, #61255, #82629 ) ;
#36534 = LINE ( 'NONE', #57400, #5484 ) ;
#36535 = DIRECTION ( 'NONE',  ( -0.7071067811856560636, -0.7071067811874389708, 0.000000000000000000 ) ) ;
#36536 = LINE ( 'NONE', #45103, #83609 ) ;
#36537 = CARTESIAN_POINT ( 'NONE',  ( 97.59110611908489830, -31.08311649095515250, 130.9108633711489915 ) ) ;
#36538 = ORIENTED_EDGE ( 'NONE', *, *, #52222, .F. ) ;
#36539 = EDGE_LOOP ( 'NONE', ( #5989, #11638, #39936, #10740 ) ) ;
#36540 = VECTOR ( 'NONE', #29778, 1000.000000000000000 ) ;
#36541 = EDGE_LOOP ( 'NONE', ( #16083, #76418, #15817, #17466 ) ) ;
#36542 = EDGE_CURVE ( 'NONE', #19234, #86883, #64035, .T. ) ;
#36543 = CARTESIAN_POINT ( 'NONE',  ( 145.5097900936629856, -69.34210384614996769, 247.4498248016565469 ) ) ;
#36544 = CARTESIAN_POINT ( 'NONE',  ( 97.12560902511589234, -37.99725552183497967, 131.4273394659764449 ) ) ;
#36545 = DIRECTION ( 'NONE',  ( 0.000000000000000000, 0.000000000000000000, -1.000000000000000000 ) ) ;
#36546 = CARTESIAN_POINT ( 'NONE',  ( 109.7539934464052465, -29.02185251678796618, 207.6280903695909501 ) ) ;
#36547 = EDGE_CURVE ( 'NONE', #61434, #39757, #84942, .T. ) ;
#36548 = FACE_OUTER_BOUND ( 'NONE', #60193, .T. ) ;
#36549 = CARTESIAN_POINT ( 'NONE',  ( 103.4683284843053883, -46.51414440030927011, 142.2956252759109645 ) ) ;
#36550 = CARTESIAN_POINT ( 'NONE',  ( 83.73314995794051185, 12.92155284005802685, 335.5992267699911054 ) ) ;
#36551 = EDGE_LOOP ( 'NONE', ( #78747, #83980, #34265, #61151 ) ) ;
#36553 = ORIENTED_EDGE ( 'NONE', *, *, #10406, .F. ) ;
#36552 = VERTEX_POINT ( 'NONE', #14 ) ;
#36554 = AXIS2_PLACEMENT_3D ( 'NONE', #49767, #7562, #83875 ) ;
#36555 = LINE ( 'NONE', #76991, #79597 ) ;
#36556 = VERTEX_POINT ( 'NONE', #27714 ) ;
#36557 = ORIENTED_EDGE ( 'NONE', *, *, #43012, .T. ) ;
#36558 = DIRECTION ( 'NONE',  ( -6.193183223602000661E-14, 1.000000000000000000, -6.293183223602000206E-29 ) ) ;
#36559 = CARTESIAN_POINT ( 'NONE',  ( 131.5565945955609095, -35.60518703966645404, 7.068229416965921885 ) ) ;
#36560 = CARTESIAN_POINT ( 'NONE',  ( 116.0742395100671871, -34.51300936444170020, 11.83666179816295028 ) ) ;
#36561 = DIRECTION ( 'NONE',  ( 0.000000000000000000, 1.000000000000000000, 0.000000000000000000 ) ) ;
#36562 = VERTEX_POINT ( 'NONE', #7720 ) ;
#36563 = VECTOR ( 'NONE', #3628, 1000.000000000000000 ) ;
#36564 = CARTESIAN_POINT ( 'NONE',  ( 115.8237480606924379, -40.07876769136255035, 9.635625275910941312 ) ) ;
#36565 = CARTESIAN_POINT ( 'NONE',  ( 152.4409905591762424, -0.9151414768250908383, 542.9756252759101471 ) ) ;
#36566 = ORIENTED_EDGE ( 'NONE', *, *, #63331, .T. ) ;
#36567 = VERTEX_POINT ( 'NONE', #48577 ) ;
#36568 = AXIS2_PLACEMENT_3D ( 'NONE', #47483, #248, #40684 ) ;
#36569 = CARTESIAN_POINT ( 'NONE',  ( 101.9936682836478639, -45.44610077275940085, 112.1565371792481329 ) ) ;
#36570 = ORIENTED_EDGE ( 'NONE', *, *, #43633, .F. ) ;
#36571 = ORIENTED_EDGE ( 'NONE', *, *, #61756, .T. ) ;
#36572 = EDGE_CURVE ( 'NONE', #89295, #2919, #15399, .T. ) ;
#36573 = EDGE_CURVE ( 'NONE', #51954, #45647, #83587, .T. ) ;
#36574 = CARTESIAN_POINT ( 'NONE',  ( 112.8202834993214481, -29.45004372636961065, 272.3623760838771091 ) ) ;
#36575 = CARTESIAN_POINT ( 'NONE',  ( 117.3318588842742685, -34.78817910010258174, 158.9756252759109714 ) ) ;
#36576 = ADVANCED_FACE ( 'NONE', ( #24043 ), #79464, .T. ) ;
#36577 = CARTESIAN_POINT ( 'NONE',  ( 117.5589153096732105, -33.32758106675089493, 134.0880062282919880 ) ) ;
#36578 = PLANE ( 'NONE',  #77685 ) ;
#36579 = DIRECTION ( 'NONE',  ( 1.000000000000000000, 1.000000000000000078E-15, 0.000000000000000000 ) ) ;
#36580 = CARTESIAN_POINT ( 'NONE',  ( 113.2200137887798235, -45.14470412949270184, 224.0784824187679476 ) ) ;
#36581 = CARTESIAN_POINT ( 'NONE',  ( 116.3185177584062444, -32.94221225046054968, 100.1356252759109680 ) ) ;
#36582 = LINE ( 'NONE', #57900, #75628 ) ;
#36583 = EDGE_LOOP ( 'NONE', ( #57907, #66550, #87485, #85593 ) ) ;
#36584 = CARTESIAN_POINT ( 'NONE',  ( -129.9368274816650626, 81.72130195885952730, -12.70000000000045404 ) ) ;
#36585 = EDGE_LOOP ( 'NONE', ( #16193, #83299 ) ) ;
#36586 = EDGE_CURVE ( 'NONE', #29924, #64928, #78127, .T. ) ;
#36587 = ORIENTED_EDGE ( 'NONE', *, *, #13757, .F. ) ;
#36588 = AXIS2_PLACEMENT_3D ( 'NONE', #44402, #72138, #9913 ) ;
#36589 = ADVANCED_FACE ( 'NONE', ( #30403 ), #17227, .T. ) ;
#36590 = AXIS2_PLACEMENT_3D ( 'NONE', #25834, #46245, #19017 ) ;
#36591 = CARTESIAN_POINT ( 'NONE',  ( 103.6240789207236475, -26.17659276989511596, 210.3394347997209763 ) ) ;
#36592 = ORIENTED_EDGE ( 'NONE', *, *, #33860, .F. ) ;
#36593 = CARTESIAN_POINT ( 'NONE',  ( 114.5123156819773698, -29.42664080734638787, 149.4441967044819819 ) ) ;
#36594 = CARTESIAN_POINT ( 'NONE',  ( 100.9565531848881079, -28.70555496000909912, 255.5938937405331615 ) ) ;
#36595 = CARTESIAN_POINT ( 'NONE',  ( 134.8062005078064090, -34.05355276379778218, 8.162233076793905084 ) ) ;
#36596 = FACE_OUTER_BOUND ( 'NONE', #40216, .T. ) ;
#36599 = CARTESIAN_POINT ( 'NONE',  ( 103.9458437887066111, -26.80522050874827755, 246.3184824187679567 ) ) ;
#36598 = DIRECTION ( 'NONE',  ( 0.000000000000000000, 0.000000000000000000, -1.000000000000000000 ) ) ;
#36597 = DIRECTION ( 'NONE',  ( 0.000000000000000000, 1.000000000000000000, 0.000000000000000000 ) ) ;
#36600 = CARTESIAN_POINT ( 'NONE',  ( 116.3130905035090876, -32.93898513502411163, 35.13562527591096796 ) ) ;
#36602 = EDGE_CURVE ( 'NONE', #11834, #85625, #50840, .T. ) ;
#36601 = CARTESIAN_POINT ( 'NONE',  ( -7.661254700127832606, 95.64746158385918307, 317.6630000000000109 ) ) ;
#36603 = CIRCLE ( 'NONE', #87354, 2.117000000000007987 ) ;
#36604 = CARTESIAN_POINT ( 'NONE',  ( 131.3179999999999836, 53.97500000000000142, 50.79999999999999716 ) ) ;
#36605 = FACE_OUTER_BOUND ( 'NONE', #4270, .T. ) ;
#36606 = LINE ( 'NONE', #57922, #56075 ) ;
#36607 = AXIS2_PLACEMENT_3D ( 'NONE', #3741, #24192, #43723 ) ;
#36608 = FACE_OUTER_BOUND ( 'NONE', #59947, .T. ) ;
#36610 = ORIENTED_EDGE ( 'NONE', *, *, #50798, .T. ) ;
#36609 = CARTESIAN_POINT ( 'NONE',  ( 103.6824468220397080, -44.03050751637072580, 195.5838068554171230 ) ) ;
#36611 = DIRECTION ( 'NONE',  ( 0.000000000000000000, 0.000000000000000000, -1.000000000000000000 ) ) ;
#36612 = CARTESIAN_POINT ( 'NONE',  ( 116.6812525300504291, -40.81632573062672265, 168.5070538473399608 ) ) ;
#36613 = CARTESIAN_POINT ( 'NONE',  ( 96.79170515468972269, -38.49336940632627346, 87.46133956162493917 ) ) ;
#36614 = CARTESIAN_POINT ( 'NONE',  ( 108.6817352505430705, -26.38614300430984372, 185.9527681330539792 ) ) ;
#36615 = LINE ( 'NONE', #2085, #72317 ) ;
#36616 = CARTESIAN_POINT ( 'NONE',  ( 51.56670390244799762, -33.35206098992650681, 313.9678068554150059 ) ) ;
#36619 = B_SPLINE_CURVE_WITH_KNOTS ( 'NONE', 3,
 ( #13967, #40764, #88932, #13519, #7161, #68487, #42107, #69832, #34397, #41203, #76188, #68930, #34852, #6256, #19431, #26686, #47567, #33947, #7606, #48448, #41647, #12627, #27592, #40314, #27147, #62558, #35289, #89841, #61645, #55271, #63001 ),
 .UNSPECIFIED., .F., .F.,
 ( 4, 2, 2, 1, 2, 2, 2, 2, 2, 2, 2, 1, 1, 2, 2, 2, 4 ),
 ( 0.000000000000000000, 0.1249999999999550360, 0.1874999999999277245, 0.2187499999999183153, 0.2343749999999145128, 0.2499999999999106826, 0.3749999999999218958, 0.4374999999999263367, 0.4999999999999307221, 0.6249999999999393818, 0.6874999999999438227, 0.7187499999999441558, 0.7343749999999424904, 0.7421874999999451550, 0.7499999999999479305, 0.8749999999999739098, 1.000000000000000000 ),
 .UNSPECIFIED. ) ;
#36618 = FACE_OUTER_BOUND ( 'NONE', #82921, .T. ) ;
#36617 = LINE ( 'NONE', #28437, #53587 ) ;
#36620 = DIRECTION ( 'NONE',  ( 0.000000000000000000, 0.000000000000000000, 1.000000000000000000 ) ) ;
#36621 = DIRECTION ( 'NONE',  ( 0.000000000000000000, -1.000000000000000000, 0.000000000000000000 ) ) ;
#36622 = ORIENTED_EDGE ( 'NONE', *, *, #40010, .F. ) ;
#36623 = CARTESIAN_POINT ( 'NONE',  ( 97.07208351798986712, -35.37818212751453473, 66.21999532449092385 ) ) ;
#36624 = ORIENTED_EDGE ( 'NONE', *, *, #15576, .T. ) ;
#36625 = ORIENTED_EDGE ( 'NONE', *, *, #19744, .T. ) ;
#36627 = VERTEX_POINT ( 'NONE', #3582 ) ;
#36626 = CARTESIAN_POINT ( 'NONE',  ( 107.0664832912739968, -36.72944715994100306, 287.6356252759109680 ) ) ;
#36628 = VECTOR ( 'NONE', #51223, 999.9999999999998863 ) ;
#36629 = CARTESIAN_POINT ( 'NONE',  ( 117.3423061886548027, -38.35306328171702717, 109.7013395616249767 ) ) ;
#36630 = CARTESIAN_POINT ( 'NONE',  ( 131.0667039024480687, -51.22944715994093201, 207.5838068554170377 ) ) ;
#36631 = LINE ( 'NONE', #42515, #83349 ) ;
#36632 = CARTESIAN_POINT ( 'NONE',  ( 98.34985892603175728, -31.65658478673192278, 176.9064586071441170 ) ) ;
#36633 = EDGE_CURVE ( 'NONE', #18008, #52712, #86710, .T. ) ;
#36634 = CARTESIAN_POINT ( 'NONE',  ( 115.8929839771518573, -32.51563103440816604, 19.18133956162593279 ) ) ;
#36635 = ORIENTED_EDGE ( 'NONE', *, *, #87123, .T. ) ;
#36636 = ORIENTED_EDGE ( 'NONE', *, *, #19955, .T. ) ;
#36637 = ORIENTED_EDGE ( 'NONE', *, *, #78627, .T. ) ;
#36638 = VECTOR ( 'NONE', #25239, 1000.000000000000000 ) ;
#36639 = CYLINDRICAL_SURFACE ( 'NONE', #28272, 6.571100913904396101 ) ;
#36640 = CARTESIAN_POINT ( 'NONE',  ( 193.5667039024485803, -48.82844715993409324, 180.4678068554150343 ) ) ;
#36641 = DIRECTION ( 'NONE',  ( 0.000000000000000000, 0.000000000000000000, -1.000000000000000000 ) ) ;
#36642 = CARTESIAN_POINT ( 'NONE',  ( 176.5667039024410769, -48.82844715994099971, 300.4678068554149490 ) ) ;
#36643 = CARTESIAN_POINT ( 'NONE',  ( 83.02643542997934389, 84.62817240485476589, 100.7545871043113408 ) ) ;
#36644 = DIRECTION ( 'NONE',  ( -1.000000000000000078E-15, 0.000000000000000000, -1.000000000000000000 ) ) ;
#36645 = DIRECTION ( 'NONE',  ( 0.7071067811865482389, -0.7071067811865467956, 0.000000000000000000 ) ) ;
#36646 = CARTESIAN_POINT ( 'NONE',  ( -11.76970797181927431, 87.32129802024908827, 130.0243965492825566 ) ) ;
#36647 = CARTESIAN_POINT ( 'NONE',  ( 116.7496603916997202, -31.44741115753626204, 24.21181575210196257 ) ) ;
#36649 = ORIENTED_EDGE ( 'NONE', *, *, #82547, .F. ) ;
#36648 = VECTOR ( 'NONE', #21119, 1000.000000000000000 ) ;
#36650 = CARTESIAN_POINT ( 'NONE',  ( 106.5667039024470171, -95.29234678213566667, 2.217806855417725487 ) ) ;
#36651 = CARTESIAN_POINT ( 'NONE',  ( 71.24189083761808661, -0.9290567490904538817, 542.9756252759101471 ) ) ;
#36652 = CARTESIAN_POINT ( 'NONE',  ( 112.3828903148906306, -42.92343960232698663, 105.9595189410199652 ) ) ;
#36654 = EDGE_CURVE ( 'NONE', #88172, #59914, #44007, .T. ) ;
#36653 = AXIS2_PLACEMENT_3D ( 'NONE', #83718, #48715, #6512 ) ;
#36655 = CARTESIAN_POINT ( 'NONE',  ( 98.34892672930283197, -31.65823485578066965, 95.90661232045958684 ) ) ;
#36656 = AXIS2_PLACEMENT_3D ( 'NONE', #23323, #30996, #80059 ) ;
#36657 = DIRECTION ( 'NONE',  ( 0.000000000000000000, 0.000000000000000000, 1.000000000000000000 ) ) ;
#36658 = ORIENTED_EDGE ( 'NONE', *, *, #30569, .F. ) ;
#36659 = VERTEX_POINT ( 'NONE', #23607 ) ;
#36660 = DIRECTION ( 'NONE',  ( 0.7071067811575828532, -0.7071067812155121812, 0.000000000000000000 ) ) ;
#36661 = ORIENTED_EDGE ( 'NONE', *, *, #79338, .F. ) ;
#36662 = EDGE_LOOP ( 'NONE', ( #44008, #23056, #41151, #53818 ) ) ;
#36663 = CARTESIAN_POINT ( 'NONE',  ( 113.0289363901617889, -43.32575541760495241, 129.5930118773259778 ) ) ;
#36664 = CARTESIAN_POINT ( 'NONE',  ( 49.16670390244701139, -26.71338133339240528, -5.074374724088000832 ) ) ;
#36665 = CARTESIAN_POINT ( 'NONE',  ( 107.6042626387647090, -26.26092342527675072, 91.03562527591097364 ) ) ;
#36666 = B_SPLINE_CURVE_WITH_KNOTS ( 'NONE', 3,
 ( #82282, #89533, #75894, #41793, #21381, #27737, #35437, #55864, #14574, #13663, #63154, #41348, #49055, #27289, #42249, #61349, #935, #20493, #54964, #6847, #55420, #83172, #13225, #20930, #69978, #7745, #76337, #69530 ),
 .UNSPECIFIED., .F., .F.,
 ( 4, 2, 2, 2, 2, 2, 2, 2, 2, 2, 1, 1, 1, 1, 2, 4 ),
 ( 0.000000000000000000, 0.06250189622662993827, 0.1250037924532598765, 0.1875056886798898148, 0.2500075849065197531, 0.3125094811331496913, 0.3750113773597796296, 0.4375132735864095679, 0.4687642216997245370, 0.4843896957563820771, 0.4922024327847105973, 0.4961088012988748019, 0.4980619855559567100, 0.4990385776844978305, 0.4995268737487682520, 0.5000151698130386180 ),
 .UNSPECIFIED. ) ;
#36667 = CARTESIAN_POINT ( 'NONE',  ( 110.8549796485604020, -45.98402957564880467, 17.88566890375461327 ) ) ;
#36668 = VERTEX_POINT ( 'NONE', #44457 ) ;
#36669 = VERTEX_POINT ( 'NONE', #24487 ) ;
#36670 = ORIENTED_EDGE ( 'NONE', *, *, #5457, .T. ) ;
#36671 = EDGE_CURVE ( 'NONE', #46473, #64475, #58536, .T. ) ;
#36672 = CARTESIAN_POINT ( 'NONE',  ( 112.1934831763302896, -30.37778608165438854, 162.3538046553059644 ) ) ;
#36674 = CARTESIAN_POINT ( 'NONE',  ( 116.7655018478977951, -32.84674153052576884, 54.12991099019698282 ) ) ;
#36673 = AXIS2_PLACEMENT_3D ( 'NONE', #84673, #22437, #9689 ) ;
#36675 = ORIENTED_EDGE ( 'NONE', *, *, #43477, .T. ) ;
#36676 = EDGE_CURVE ( 'NONE', #26317, #54219, #45827, .T. ) ;
#36677 = CARTESIAN_POINT ( 'NONE',  ( 105.9906760191434358, -26.38192068051316141, 50.15848241876796720 ) ) ;
#36678 = CARTESIAN_POINT ( 'NONE',  ( 102.9585648456520772, -26.44303807861259870, 171.3908633711489813 ) ) ;
#36679 = FACE_OUTER_BOUND ( 'NONE', #70979, .T. ) ;
#36680 = CARTESIAN_POINT ( 'NONE',  ( 270.8910000000000196, 40.03750000000000142, -67.11950000000000216 ) ) ;
#36681 = EDGE_CURVE ( 'NONE', #75662, #86124, #79912, .T. ) ;
#36682 = CARTESIAN_POINT ( 'NONE',  ( 106.0764678730365063, -48.53853201145131635, 108.5099109901969712 ) ) ;
#36683 = CARTESIAN_POINT ( 'NONE',  ( 98.30753421155790761, -41.72887552731712901, 261.7397919458750835 ) ) ;
#36684 = ORIENTED_EDGE ( 'NONE', *, *, #69295, .T. ) ;
#36685 = DIRECTION ( 'NONE',  ( 1.000000000000000000, 0.000000000000000000, 0.000000000000000000 ) ) ;
#36686 = ADVANCED_FACE ( 'NONE', ( #17667 ), #85393, .F. ) ;
#36687 = ORIENTED_EDGE ( 'NONE', *, *, #12157, .F. ) ;
#36688 = CARTESIAN_POINT ( 'NONE',  ( 70.06670390244705970, -124.7784471599409670, 222.2178068554179902 ) ) ;
#36689 = ORIENTED_EDGE ( 'NONE', *, *, #39535, .F. ) ;
#36690 = VERTEX_POINT ( 'NONE', #73064 ) ;
#36691 = VECTOR ( 'NONE', #85396, 1000.000000000000000 ) ;
#36692 = DIRECTION ( 'NONE',  ( -0.000000000000000000, 1.000000000000000000, 0.000000000000000000 ) ) ;
#36693 = CARTESIAN_POINT ( 'NONE',  ( 8.311119758860220585, 92.02930930504943774, 118.2647611583656300 ) ) ;
#36694 = CARTESIAN_POINT ( 'NONE',  ( 107.1954010100577364, -26.30493706674213428, 35.06705384733893283 ) ) ;
#36695 = CARTESIAN_POINT ( 'NONE',  ( 23.09780390562728414, 56.38017385884855770, 30.30024197629754923 ) ) ;
#36696 = CYLINDRICAL_SURFACE ( 'NONE', #8685, 38.10000000000000142 ) ;
#36697 = CARTESIAN_POINT ( 'NONE',  ( 21.56670390244604718, -23.42844715994195326, 180.4678068554150911 ) ) ;
#36698 = CARTESIAN_POINT ( 'NONE',  ( 116.8124865092211451, -37.88235468918158944, 53.73276813305394484 ) ) ;
#36700 = CARTESIAN_POINT ( 'NONE',  ( 95.59354794629810215, -39.59649474372135813, 162.5213395616259788 ) ) ;
#36699 = FACE_OUTER_BOUND ( 'NONE', #13146, .T. ) ;
#36701 = CARTESIAN_POINT ( 'NONE',  ( 25.56670390244828894, -48.82844715994168183, 293.2178068554150059 ) ) ;
#36703 = ADVANCED_FACE ( 'NONE', ( #37669 ), #71742, .T. ) ;
#36702 = DIRECTION ( 'NONE',  ( 0.000000000000000000, 0.000000000000000000, -1.000000000000000000 ) ) ;
#36704 = ORIENTED_EDGE ( 'NONE', *, *, #6531, .T. ) ;
#36705 = LINE ( 'NONE', #43937, #89024 ) ;
#36706 = FACE_OUTER_BOUND ( 'NONE', #19088, .T. ) ;
#36707 = DIRECTION ( 'NONE',  ( 0.000000000000000000, 0.000000000000000000, -1.000000000000000000 ) ) ;
#36708 = VERTEX_POINT ( 'NONE', #4027 ) ;
#36709 = DIRECTION ( 'NONE',  ( -4.299999999999999979E-14, 1.000000000000000000, -4.400000000000000367E-29 ) ) ;
#36711 = ORIENTED_EDGE ( 'NONE', *, *, #55169, .T. ) ;
#36710 = CARTESIAN_POINT ( 'NONE',  ( 108.8564100269821608, -47.04462182233018552, 167.7127681330539701 ) ) ;
#36712 = FACE_OUTER_BOUND ( 'NONE', #23989, .T. ) ;
#36713 = CARTESIAN_POINT ( 'NONE',  ( 99.52368306943544951, -29.45034277662237443, 246.7156252759109520 ) ) ;
#36714 = CARTESIAN_POINT ( 'NONE',  ( 96.59565658895887452, -37.56598942197172164, 97.38991099019594344 ) ) ;
#36715 = CARTESIAN_POINT ( 'NONE',  ( 97.06097963517905214, -37.99593394772350052, 252.4290318010866656 ) ) ;
#36716 = B_SPLINE_CURVE_WITH_KNOTS ( 'NONE', 3,
 ( #15309, #55695, #43427, #42975, #71174, #69369, #7143, #8947, #69819, #34838, #36646, #35277, #766, #56156, #83907, #49351, #70262, #8033, #35727, #78441, #45211, #50700, #24348, #38405, #86135, #30274, #65234, #3893, #87022, #37968, #59292, #72928, #57516, #66109, #23911, #58843, #3452, #79326, #23026, #44322, #17088, #30710, #16204, #72054, #9828, #2573, #78882, #51142, #16643, #29830, #44775, #79775, #31589, #85260, #80215, #10698, #10267, #24788, #43880, #31148, #51580 ),
 .UNSPECIFIED., .F., .F.,
 ( 4, 2, 2, 2, 1, 1, 1, 2, 2, 2, 2, 1, 1, 1, 1, 1, 2, 2, 2, 2, 2, 2, 2, 1, 1, 1, 1, 2, 2, 2, 2, 1, 1, 1, 2, 2, 2, 4 ),
 ( 0.000000000000000000, 0.1250000000003168854, 0.1875000000004742595, 0.2187500000005539458, 0.2343750000005937750, 0.2421875000006136758, 0.2460937500006236400, 0.2480468750006286638, 0.2500000000006336598, 0.3125000000007292500, 0.3437500000007759904, 0.3593750000008001932, 0.3671875000008131829, 0.3710937500008197332, 0.3730468750008228973, 0.3740234375008252288, 0.3745117187508265055, 0.3750000000008277823, 0.4375000000008258949, 0.5000000000008238965, 0.5625000000008220091, 0.5937500000008211209, 0.6093750000008205658, 0.6171875000008203438, 0.6210937500008208989, 0.6230468750008205658, 0.6240234375008203438, 0.6245117187508192336, 0.6250000000008181233, 0.6875000000006927792, 0.7187500000006302736, 0.7343750000005995204, 0.7421875000005839773, 0.7460937500005763168, 0.7480468750005724310, 0.7500000000005684342, 0.8750000000002843281, 1.000000000000000000 ),
 .UNSPECIFIED. ) ;
#36717 = CARTESIAN_POINT ( 'NONE',  ( 105.7973883670204600, -26.72432487108696009, 191.1772404832683208 ) ) ;
#36718 = CARTESIAN_POINT ( 'NONE',  ( 112.0659116283640060, -45.48839625712076185, 77.98979194311773711 ) ) ;
#36719 = EDGE_LOOP ( 'NONE', ( #14112, #56539, #35835, #12960 ) ) ;
#36720 = VECTOR ( 'NONE', #62155, 1000.000000000000000 ) ;
#36721 = AXIS2_PLACEMENT_3D ( 'NONE', #13325, #5624, #54620 ) ;
#36722 = VERTEX_POINT ( 'NONE', #31730 ) ;
#36723 = EDGE_LOOP ( 'NONE', ( #72364, #40929, #13, #80440 ) ) ;
#36724 = VECTOR ( 'NONE', #60789, 1000.000000000000000 ) ;
#36725 = ORIENTED_EDGE ( 'NONE', *, *, #16230, .F. ) ;
#36726 = CARTESIAN_POINT ( 'NONE',  ( 49.16670390244701139, -26.71338133339240528, -5.074374724088000832 ) ) ;
#36727 = CARTESIAN_POINT ( 'NONE',  ( 98.83931482081872844, -29.34787013040062931, 231.7565776568629587 ) ) ;
#36728 = FACE_OUTER_BOUND ( 'NONE', #61920, .T. ) ;
#36729 = CARTESIAN_POINT ( 'NONE',  ( -7.661254700127832606, 98.64746158385918307, 275.4630000000000223 ) ) ;
#36731 = DIRECTION ( 'NONE',  ( 1.000000000000000078E-15, -1.000000000000000083E-30, -1.000000000000000000 ) ) ;
#36730 = DIRECTION ( 'NONE',  ( 0.000000000000000000, 0.000000000000000000, -1.000000000000000000 ) ) ;
#36732 = LINE ( 'NONE', #86222, #31209 ) ;
#36733 = ADVANCED_FACE ( 'NONE', ( #37217 ), #2258, .T. ) ;
#36734 = CARTESIAN_POINT ( 'NONE',  ( 96.69266203715996255, -37.96645829736812061, 41.42133956162496844 ) ) ;
#36735 = ORIENTED_EDGE ( 'NONE', *, *, #39026, .F. ) ;
#36736 = VERTEX_POINT ( 'NONE', #22708 ) ;
#36737 = ORIENTED_EDGE ( 'NONE', *, *, #9289, .T. ) ;
#36738 = CARTESIAN_POINT ( 'NONE',  ( 107.0664832912739257, -49.89611382660765315, 357.5272416190308604 ) ) ;
#36739 = CIRCLE ( 'NONE', #13514, 10.00000000000000355 ) ;
#36740 = CARTESIAN_POINT ( 'NONE',  ( 107.0667039024470313, -104.2784471599409528, 55.21780685541800437 ) ) ;
#36741 = EDGE_CURVE ( 'NONE', #10572, #73470, #64921, .T. ) ;
#36742 = CARTESIAN_POINT ( 'NONE',  ( 102.6690082227317475, -46.93785447722112281, 283.2527681330534506 ) ) ;
#36743 = DIRECTION ( 'NONE',  ( -0.000000000000000000, 1.000000000000000000, 0.000000000000000000 ) ) ;
#36744 = AXIS2_PLACEMENT_3D ( 'NONE', #28222, #54560, #83659 ) ;
#36745 = CARTESIAN_POINT ( 'NONE',  ( 116.5825849560771417, -39.12894369053751120, 119.6299109901959525 ) ) ;
#36746 = CARTESIAN_POINT ( 'NONE',  ( 7.661254700127833495, 82.54999999999999716, 317.6630000000000109 ) ) ;
#36747 = ORIENTED_EDGE ( 'NONE', *, *, #7241, .T. ) ;
#36748 = CARTESIAN_POINT ( 'NONE',  ( 51.42025729302798709, -31.94127993907680718, 313.9678068554150059 ) ) ;
#36749 = CARTESIAN_POINT ( 'NONE',  ( 77.66889017809432971, -35.37024878622109725, 2.654395752959056498 ) ) ;
#36750 = VERTEX_POINT ( 'NONE', #50379 ) ;
#36751 = CARTESIAN_POINT ( 'NONE',  ( -81.46927207886238875, 94.82191660594814664, 86.13037352894157550 ) ) ;
#36752 = CARTESIAN_POINT ( 'NONE',  ( 102.0014872285204035, -30.29305903553749602, 13.42523322673394581 ) ) ;
#36753 = EDGE_CURVE ( 'NONE', #89702, #82107, #85835, .T. ) ;
#36754 = CYLINDRICAL_SURFACE ( 'NONE', #44977, 7.143749999999999822 ) ;
#36755 = DIRECTION ( 'NONE',  ( -4.237773401492740281E-14, 1.000000000000000000, 0.000000000000000000 ) ) ;
#36756 = CARTESIAN_POINT ( 'NONE',  ( 116.3263622980238097, -32.93962144782776846, 195.1356252759109680 ) ) ;
#36757 = ORIENTED_EDGE ( 'NONE', *, *, #47214, .T. ) ;
#36758 = DIRECTION ( 'NONE',  ( 1.000000000000000000, 0.000000000000000000, 0.000000000000000000 ) ) ;
#36759 = DIRECTION ( 'NONE',  ( 1.000000000000000000, 4.510281037539819615E-14, 0.000000000000000000 ) ) ;
#36760 = ORIENTED_EDGE ( 'NONE', *, *, #30746, .T. ) ;
#36761 = CARTESIAN_POINT ( 'NONE',  ( 103.8412645720801493, -46.68052101597508852, 82.32705384733995402 ) ) ;
#36762 = VERTEX_POINT ( 'NONE', #9964 ) ;
#36763 = CARTESIAN_POINT ( 'NONE',  ( 98.75426529987753099, -33.13504840779251737, 60.43622935188691514 ) ) ;
#36764 = EDGE_CURVE ( 'NONE', #74855, #8105, #65366, .T. ) ;
#36765 = LINE ( 'NONE', #72627, #54707 ) ;
#36766 = CARTESIAN_POINT ( 'NONE',  ( 117.1170091337237551, -34.17489915221370467, 169.0365776568639831 ) ) ;
#36767 = DIRECTION ( 'NONE',  ( 0.000000000000000000, -1.000000000000000000, 0.000000000000000000 ) ) ;
#36768 = DIRECTION ( 'NONE',  ( 1.000000000000000078E-15, 1.000000000000000083E-30, -1.000000000000000000 ) ) ;
#36769 = LINE ( 'NONE', #1807, #1318 ) ;
#36770 = DIRECTION ( 'NONE',  ( 4.299999999999999979E-14, -1.000000000000000000, 4.400000000000000367E-29 ) ) ;
#36772 = B_SPLINE_CURVE_WITH_KNOTS ( 'NONE', 3,
 ( #77292, #16410, #58181, #85471, #86348, #44086, #71821, #78206, #85911, #3227, #15967, #23683, #9590, #35949, #79092, #43648, #65447, #42741 ),
 .UNSPECIFIED., .F., .F.,
 ( 4, 2, 2, 2, 2, 2, 2, 2, 4 ),
 ( 0.000000000000000000, 0.06250441113620554268, 0.1250088222724110854, 0.1875132334086166419, 0.2500176445448221707, 0.3125220556810276995, 0.3750264668172332838, 0.4375308779534388126, 0.5000352890896443414 ),
 .UNSPECIFIED. ) ;
#36771 = CARTESIAN_POINT ( 'NONE',  ( 108.0180542234412684, -24.86750695335871697, 261.0127681330534415 ) ) ;
#36773 = ORIENTED_EDGE ( 'NONE', *, *, #27471, .F. ) ;
#36774 = DIRECTION ( 'NONE',  ( 0.000000000000000000, 0.000000000000000000, 1.000000000000000000 ) ) ;
#36775 = VERTEX_POINT ( 'NONE', #13092 ) ;
#36776 = CARTESIAN_POINT ( 'NONE',  ( 114.2047867640113594, -45.22899916922247598, 144.1203871806729637 ) ) ;
#36777 = CARTESIAN_POINT ( 'NONE',  ( 125.3463460965257354, 52.19566713291690263, -36.51250000000000995 ) ) ;
#36778 = AXIS2_PLACEMENT_3D ( 'NONE', #64061, #35436, #56317 ) ;
#36779 = ORIENTED_EDGE ( 'NONE', *, *, #49156, .F. ) ;
#36780 = ORIENTED_EDGE ( 'NONE', *, *, #80153, .T. ) ;
#36781 = ORIENTED_EDGE ( 'NONE', *, *, #6288, .T. ) ;
#36782 = CARTESIAN_POINT ( 'NONE',  ( 41.56648329127398966, -27.82844715994070484, 318.9256252759120116 ) ) ;
#36783 = DIRECTION ( 'NONE',  ( 1.000000000000000000, -6.938893903907232322E-15, -2.775557561562892929E-14 ) ) ;
#36784 = CARTESIAN_POINT ( 'NONE',  ( 97.81168921572486852, -40.51740600946125426, 16.63579259794490284 ) ) ;
#36785 = DIRECTION ( 'NONE',  ( 0.000000000000000000, 1.000000000000000000, 0.000000000000000000 ) ) ;
#36786 = DIRECTION ( 'NONE',  ( 0.000000000000000000, -1.000000000000000000, 0.000000000000000000 ) ) ;
#36787 = EDGE_CURVE ( 'NONE', #72226, #82610, #52591, .T. ) ;
#36788 = CARTESIAN_POINT ( 'NONE',  ( 116.7699407904022451, -31.43634848722146202, 20.21181575210195902 ) ) ;
#36789 = DIRECTION ( 'NONE',  ( 1.907762142705490052E-15, 7.167082501179359715E-16, -1.000000000000000000 ) ) ;
#36790 = ORIENTED_EDGE ( 'NONE', *, *, #79689, .F. ) ;
#36791 = FILL_AREA_STYLE_COLOUR ( '', #41278 ) ;
#36792 = CARTESIAN_POINT ( 'NONE',  ( -41.60202597009397607, 65.59999999999998010, 50.85338361873603219 ) ) ;
#36793 = ORIENTED_EDGE ( 'NONE', *, *, #14957, .T. ) ;
#36794 = ORIENTED_EDGE ( 'NONE', *, *, #3907, .F. ) ;
#36795 = CARTESIAN_POINT ( 'NONE',  ( 0.000000000000000000, 92.07499999999998863, 39.10000000000005116 ) ) ;
#36796 = VECTOR ( 'NONE', #69453, 999.9999999999998863 ) ;
#36797 = FACE_OUTER_BOUND ( 'NONE', #84845, .T. ) ;
#36798 = LINE ( 'NONE', #71329, #25468 ) ;
#36799 = FACE_OUTER_BOUND ( 'NONE', #685, .T. ) ;
#36800 = DIRECTION ( 'NONE',  ( -0.5000000000000061062, 0.000000000000000000, 0.8660254037844351549 ) ) ;
#36801 = CARTESIAN_POINT ( 'NONE',  ( 100.4104977919876802, -31.37650509455747283, 240.2095626852199928 ) ) ;
#36803 = CARTESIAN_POINT ( 'NONE',  ( 101.9712125536871383, -27.65933791914800111, 56.48419670448296159 ) ) ;
#36802 = CARTESIAN_POINT ( 'NONE',  ( 142.0664832912740394, -56.47944715994099596, 14.67562527591100441 ) ) ;
#36804 = CARTESIAN_POINT ( 'NONE',  ( 127.0239848601435995, 53.97500000000000142, 30.16249999999999787 ) ) ;
#36805 = CARTESIAN_POINT ( 'NONE',  ( 104.0952645214482430, -46.76829794407347407, 107.3470538473389411 ) ) ;
#36806 = EDGE_LOOP ( 'NONE', ( #3071, #27581, #9905, #74823, #68727 ) ) ;
#36808 = EDGE_CURVE ( 'NONE', #41573, #83210, #21225, .T. ) ;
#36807 = LINE ( 'NONE', #77699, #81474 ) ;
#36809 = VERTEX_POINT ( 'NONE', #88507 ) ;
#36810 = AXIS2_PLACEMENT_3D ( 'NONE', #3003, #71611, #51575 ) ;
#36811 = DIRECTION ( 'NONE',  ( 0.000000000000000000, 0.000000000000000000, -1.000000000000000000 ) ) ;
#36812 = ADVANCED_FACE ( 'NONE', ( #53488 ), #83605, .F. ) ;
#36813 = CARTESIAN_POINT ( 'NONE',  ( 104.6390307648651117, -27.02259228910022415, 276.2714668963693043 ) ) ;
#36814 = EDGE_LOOP ( 'NONE', ( #45026, #49275, #50769, #38731, #27004, #40293 ) ) ;
#36815 = CARTESIAN_POINT ( 'NONE',  ( 107.0664832912750057, -36.72944715993903486, 9.125625275910969947 ) ) ;
#36816 = ORIENTED_EDGE ( 'NONE', *, *, #349, .T. ) ;
#36817 = CARTESIAN_POINT ( 'NONE',  ( 0.000000000000000000, 0.000000000000000000, 0.000000000000000000 ) ) ;
#36818 = CARTESIAN_POINT ( 'NONE',  ( 188.5667039024483529, -48.82844715993431350, 290.7178068554150059 ) ) ;
#36819 = VECTOR ( 'NONE', #52585, 1000.000000000000000 ) ;
#36820 = DIRECTION ( 'NONE',  ( -8.673617379884035472E-16, -1.000000000000000000, 0.000000000000000000 ) ) ;
#36821 = VERTEX_POINT ( 'NONE', #73966 ) ;
#36822 = CARTESIAN_POINT ( 'NONE',  ( 111.0910783018720025, -25.55641485417826431, 99.80133956162498521 ) ) ;
#36823 = CARTESIAN_POINT ( 'NONE',  ( -1.040396286424043573E-12, 1.527609608640607000E-59, 2.170823869927923866 ) ) ;
#36824 = CARTESIAN_POINT ( 'NONE',  ( 97.81167943543778165, -40.51737693692245301, 166.6360185166829808 ) ) ;
#36825 = CARTESIAN_POINT ( 'NONE',  ( 51.06670390244760682, -32.29483332968566600, 313.9678068554150059 ) ) ;
#36826 = CARTESIAN_POINT ( 'NONE',  ( 196.2150000000000034, 30.98800000000000310, 57.14999999999999858 ) ) ;
#36827 = ORIENTED_EDGE ( 'NONE', *, *, #79981, .F. ) ;
#36828 = CARTESIAN_POINT ( 'NONE',  ( 63.06670390244711655, -40.32844715994016838, 129.9678068554150911 ) ) ;
#36829 = DIRECTION ( 'NONE',  ( 0.000000000000000000, 0.000000000000000000, -1.000000000000000000 ) ) ;
#36830 = DIRECTION ( 'NONE',  ( 0.000000000000000000, 1.000000000000000000, 0.000000000000000000 ) ) ;
#36832 = CARTESIAN_POINT ( 'NONE',  ( 67.06670390244707392, -137.6782278263010824, 245.4503596485529897 ) ) ;
#36831 = DIRECTION ( 'NONE',  ( 0.000000000000000000, 1.000000000000000000, 0.000000000000000000 ) ) ;
#36833 = CARTESIAN_POINT ( 'NONE',  ( 87.06648329127402519, -54.72944906728955061, 14.67562527591094934 ) ) ;
#36834 = AXIS2_PLACEMENT_3D ( 'NONE', #33238, #26427, #53193 ) ;
#36835 = ORIENTED_EDGE ( 'NONE', *, *, #64868, .T. ) ;
#36836 = AXIS2_PLACEMENT_3D ( 'NONE', #6407, #55872, #34100 ) ;
#36837 = DIRECTION ( 'NONE',  ( 1.000000000000000000, 0.000000000000000000, 0.000000000000000000 ) ) ;
#36838 = EDGE_CURVE ( 'NONE', #49620, #86172, #79266, .T. ) ;
#36839 = CARTESIAN_POINT ( 'NONE',  ( 105.8036208730406003, -25.68330614324009886, 156.1670538473389627 ) ) ;
#36841 = ORIENTED_EDGE ( 'NONE', *, *, #37538, .T. ) ;
#36840 = CARTESIAN_POINT ( 'NONE',  ( 270.8910000000000196, 65.43750000000000000, -67.11950000000000216 ) ) ;
#36842 = CARTESIAN_POINT ( 'NONE',  ( 115.3963619165045458, -41.85549553236474196, 14.38705384733895976 ) ) ;
#36843 = CARTESIAN_POINT ( 'NONE',  ( 158.0667039024469886, -67.87844715994090450, 85.21780685541799016 ) ) ;
#36844 = DIRECTION ( 'NONE',  ( 0.000000000000000000, 0.000000000000000000, -1.000000000000000000 ) ) ;
#36845 = DIRECTION ( 'NONE',  ( 0.000000000000000000, 0.000000000000000000, 1.000000000000000000 ) ) ;
#36846 = FACE_OUTER_BOUND ( 'NONE', #30963, .T. ) ;
#36847 = CARTESIAN_POINT ( 'NONE',  ( 100.2051353121704835, -29.75912871662441361, 225.6956252759109702 ) ) ;
#36848 = ORIENTED_EDGE ( 'NONE', *, *, #85198, .T. ) ;
#36849 = VERTEX_POINT ( 'NONE', #66697 ) ;
#36850 = CARTESIAN_POINT ( 'NONE',  ( 116.3029726692365813, -35.00788115540211010, 200.4168214011349676 ) ) ;
#36851 = VECTOR ( 'NONE', #51699, 1000.000000000000000 ) ;
#36852 = DIRECTION ( 'NONE',  ( 1.000000000000000078E-15, 0.000000000000000000, 1.000000000000000000 ) ) ;
#36853 = EDGE_CURVE ( 'NONE', #75906, #1995, #81867, .T. ) ;
#36854 = CARTESIAN_POINT ( 'NONE',  ( 112.0788320361856307, -29.42159941445254390, 41.03015473446897232 ) ) ;
#36855 = AXIS2_PLACEMENT_3D ( 'NONE', #76207, #77115, #70289 ) ;
#36856 = CARTESIAN_POINT ( 'NONE',  ( -92.60677566276767436, 95.25015599858943460, 92.02731164704691480 ) ) ;
#36857 = LINE ( 'NONE', #50473, #76543 ) ;
#36858 = ADVANCED_FACE ( 'NONE', ( #68500 ), #11744, .T. ) ;
#36859 = CARTESIAN_POINT ( 'NONE',  ( 161.5667039024469886, -68.37844715994089029, 96.96780685541800437 ) ) ;
#36860 = EDGE_LOOP ( 'NONE', ( #19395, #4442, #87100, #87382 ) ) ;
#36861 = DIRECTION ( 'NONE',  ( 1.000000000000000078E-15, -1.000000000000000083E-30, -1.000000000000000000 ) ) ;
#36862 = CARTESIAN_POINT ( 'NONE',  ( 97.60794579242353564, -39.98258380600313444, 37.58978887728247287 ) ) ;
#36863 = CARTESIAN_POINT ( 'NONE',  ( 106.1402962346845982, -47.72062544595571154, 262.4975300378158636 ) ) ;
#36864 = CARTESIAN_POINT ( 'NONE',  ( 12.60000000000000142, 82.96121956631253624, 117.6834004267381744 ) ) ;
#36865 = ORIENTED_EDGE ( 'NONE', *, *, #46691, .T. ) ;
#36866 = VERTEX_POINT ( 'NONE', #81253 ) ;
#36867 = EDGE_CURVE ( 'NONE', #40115, #7001, #32616, .T. ) ;
#36868 = EDGE_CURVE ( 'NONE', #29421, #26390, #24205, .T. ) ;
#36869 = CYLINDRICAL_SURFACE ( 'NONE', #21293, 2.030000000001310312 ) ;
#36870 = DIRECTION ( 'NONE',  ( -1.000000000000000078E-15, 1.000000000000000083E-30, 1.000000000000000000 ) ) ;
#36871 = CARTESIAN_POINT ( 'NONE',  ( 141.8664832912729992, -1.929447159941394263, 352.4506252759079530 ) ) ;
#36872 = DIRECTION ( 'NONE',  ( 1.000000000000000000, 0.000000000000000000, 0.000000000000000000 ) ) ;
#36873 = ADVANCED_FACE ( 'NONE', ( #67145 ), #68048, .F. ) ;
#36874 = CARTESIAN_POINT ( 'NONE',  ( 109.4837483930865289, -46.20680252518636166, 43.77562527591094721 ) ) ;
#36875 = CARTESIAN_POINT ( 'NONE',  ( 9.493161119239731605, 74.22443474232989047, 117.9761073818194603 ) ) ;
#36876 = ORIENTED_EDGE ( 'NONE', *, *, #55411, .T. ) ;
#36877 = CARTESIAN_POINT ( 'NONE',  ( 115.7648065088891371, -43.62413145733483333, 44.30514908543492680 ) ) ;
#36878 = DIRECTION ( 'NONE',  ( -1.000000000000000078E-15, 1.000000000000000083E-30, 1.000000000000000000 ) ) ;
#36879 = ADVANCED_FACE ( 'NONE', ( #60771 ), #60316, .T. ) ;
#36880 = CARTESIAN_POINT ( 'NONE',  ( 96.32141381413643444, -39.41948438522342713, 16.53372051400597798 ) ) ;
#36881 = ORIENTED_EDGE ( 'NONE', *, *, #53258, .F. ) ;
#36882 = DIRECTION ( 'NONE',  ( 0.000000000000000000, 0.000000000000000000, -1.000000000000000000 ) ) ;
#36883 = DIRECTION ( 'NONE',  ( 0.000000000000000000, 0.000000000000000000, 1.000000000000000000 ) ) ;
#36884 = DIRECTION ( 'NONE',  ( 1.000000000000000000, 0.000000000000000000, 0.000000000000000000 ) ) ;
#36885 = EDGE_CURVE ( 'NONE', #16110, #53327, #25815, .T. ) ;
#36886 = CARTESIAN_POINT ( 'NONE',  ( 107.8241526860280430, -28.10814435038363968, 107.8128522743529771 ) ) ;
#36887 = CARTESIAN_POINT ( 'NONE',  ( 101.3372171518963398, -46.20893634704900421, 198.1318157521009482 ) ) ;
#36888 = CARTESIAN_POINT ( 'NONE',  ( 31.75000000000000000, 111.1250000000000000, 3.174999999999999822 ) ) ;
#36889 = ORIENTED_EDGE ( 'NONE', *, *, #57852, .T. ) ;
#36890 = CARTESIAN_POINT ( 'NONE',  ( 71.06648329127399677, -18.82844715994099971, 323.8756252759120002 ) ) ;
#36891 = ORIENTED_EDGE ( 'NONE', *, *, #72556, .F. ) ;
#36892 = VERTEX_POINT ( 'NONE', #81696 ) ;
#36893 = AXIS2_PLACEMENT_3D ( 'NONE', #46738, #10457, #66751 ) ;
#36894 = CARTESIAN_POINT ( 'NONE',  ( 131.0667039024480118, -61.87844715994100397, 237.1838068554150141 ) ) ;
#36895 = VERTEX_POINT ( 'NONE', #67597 ) ;
#36896 = ORIENTED_EDGE ( 'NONE', *, *, #20683, .T. ) ;
#36897 = CARTESIAN_POINT ( 'NONE',  ( 204.2160000000000082, 52.73749999999999716, -44.45000000000000284 ) ) ;
#36898 = CARTESIAN_POINT ( 'NONE',  ( 0.000000000000000000, 224.4999999999999432, 154.6557476874258441 ) ) ;
#36899 = CARTESIAN_POINT ( 'NONE',  ( 112.7653361951733473, -30.36711996764882571, 113.9181341137909556 ) ) ;
#36900 = CARTESIAN_POINT ( 'NONE',  ( 115.6735817710496264, -30.74561775548394849, 279.3099109901964994 ) ) ;
#36901 = ADVANCED_FACE ( 'NONE', ( #22155 ), #77548, .T. ) ;
#36902 = EDGE_CURVE ( 'NONE', #62685, #86125, #28042, .T. ) ;
#36903 = CARTESIAN_POINT ( 'NONE',  ( -3.286472755014015146, 70.27551020174914242, 130.5152393712291428 ) ) ;
#36904 = VERTEX_POINT ( 'NONE', #13976 ) ;
#36905 = EDGE_CURVE ( 'NONE', #40524, #65725, #76197, .T. ) ;
#36906 = VERTEX_POINT ( 'NONE', #89851 ) ;
#36907 = DIRECTION ( 'NONE',  ( 1.000000000000000078E-15, -1.000000000000000000, 0.000000000000000000 ) ) ;
#36908 = EDGE_CURVE ( 'NONE', #82784, #73516, #83466, .T. ) ;
#36909 = DIRECTION ( 'NONE',  ( 1.000000000000000000, -5.337610695313248426E-16, 0.000000000000000000 ) ) ;
#36910 = CARTESIAN_POINT ( 'NONE',  ( 194.0371591254574923, -24.42818131005417115, 193.9678068554150343 ) ) ;
#36912 = AXIS2_PLACEMENT_3D ( 'NONE', #9840, #78449, #85708 ) ;
#36911 = CARTESIAN_POINT ( 'NONE',  ( 161.4809174648183614, -49.32844715993547879, 300.4678068554149490 ) ) ;
#36913 = ORIENTED_EDGE ( 'NONE', *, *, #10669, .F. ) ;
#36914 = UNCERTAINTY_MEASURE_WITH_UNIT (LENGTH_MEASURE( 1.000000000000000082E-05 ), #36918, 'distance_accuracy_value', 'NONE');
#36915 = CARTESIAN_POINT ( 'NONE',  ( 116.6059430675273063, -40.93488859202243901, 253.4956252759109532 ) ) ;
#36916 = VECTOR ( 'NONE', #39600, 1000.000000000000000 ) ;
#36917 = FACE_OUTER_BOUND ( 'NONE', #55603, .T. ) ;
#36918 =( LENGTH_UNIT ( ) NAMED_UNIT ( * ) SI_UNIT ( .MILLI., .METRE. ) );
#36919 = CIRCLE ( 'NONE', #48484, 2.999999999999988898 ) ;
#36920 = CARTESIAN_POINT ( 'NONE',  ( 69.25310000000000343, 82.54999999999999716, 344.4418053999999643 ) ) ;
#36922 = CARTESIAN_POINT ( 'NONE',  ( 68.88219323916185033, -139.1179055681215573, 246.6639347725188145 ) ) ;
#36921 = DIRECTION ( 'NONE',  ( 1.000000000000000078E-15, -1.000000000000000000, 0.000000000000000000 ) ) ;
#36923 = CARTESIAN_POINT ( 'NONE',  ( -44.45000000000000284, 50.79999999999999716, 275.4630000000000223 ) ) ;
#36924 = DIRECTION ( 'NONE',  ( 4.299999999999999979E-14, -1.000000000000000000, 4.400000000000000367E-29 ) ) ;
#36925 = DIRECTION ( 'NONE',  ( -0.7071067811864687469, -0.7071067811866262875, -7.071067811864681542E-16 ) ) ;
#36926 = CIRCLE ( 'NONE', #29734, 5.041900000000001825 ) ;
#36927 = AXIS2_PLACEMENT_3D ( 'NONE', #51513, #50633, #45579 ) ;
#36928 = CARTESIAN_POINT ( 'NONE',  ( 97.07207205096092650, -35.37844125572550524, 12.21895861363828040 ) ) ;
#36929 = PLANE ( 'NONE',  #63705 ) ;
#36930 = FACE_OUTER_BOUND ( 'NONE', #37344, .T. ) ;
#36931 = LINE ( 'NONE', #25420, #42322 ) ;
#36932 = CARTESIAN_POINT ( 'NONE',  ( 96.61485869678695337, -32.99094118449985302, 26.06514908543494613 ) ) ;
#36933 = CARTESIAN_POINT ( 'NONE',  ( 118.8773263846236148, -37.69826137473897631, 184.7613395616249647 ) ) ;
#36934 = CARTESIAN_POINT ( 'NONE',  ( 104.5778203770529586, -26.56076746289640411, 281.2670538473396959 ) ) ;
#36936 = DIRECTION ( 'NONE',  ( 0.000000000000000000, -1.000000000000000000, 0.000000000000000000 ) ) ;
#36935 = CARTESIAN_POINT ( 'NONE',  ( 168.0371591254546217, -48.62818131005518296, 117.4678068554150485 ) ) ;
#36937 = CARTESIAN_POINT ( 'NONE',  ( 82.59704509974031339, -35.65293374834178053, 2.807537076564044387 ) ) ;
#36938 = VERTEX_POINT ( 'NONE', #20793 ) ;
#36939 = LINE ( 'NONE', #43291, #79526 ) ;
#36940 = ORIENTED_EDGE ( 'NONE', *, *, #16230, .T. ) ;
#36941 = CARTESIAN_POINT ( 'NONE',  ( 99.96923091713372855, -43.45941328387849723, 77.92991099019597812 ) ) ;
#36943 = VERTEX_POINT ( 'NONE', #21243 ) ;
#36942 = FACE_OUTER_BOUND ( 'NONE', #78624, .T. ) ;
#36944 = FACE_OUTER_BOUND ( 'NONE', #65945, .T. ) ;
#36945 = CARTESIAN_POINT ( 'NONE',  ( 98.56907362037671305, -44.95393718666134930, 187.9384824187679612 ) ) ;
#36946 = DIRECTION ( 'NONE',  ( 0.000000000000000000, 0.000000000000000000, 1.000000000000000000 ) ) ;
#36947 = CARTESIAN_POINT ( 'NONE',  ( 34.92499999999999716, 91.71543552338529537, 302.8950000000000387 ) ) ;
#36948 = CARTESIAN_POINT ( 'NONE',  ( 104.4904853333757586, -26.97866173706016824, 150.2818345845702765 ) ) ;
#36949 = DIRECTION ( 'NONE',  ( 0.000000000000000000, -0.7071067811865291430, -0.7071067811865660024 ) ) ;
#36950 = DIRECTION ( 'NONE',  ( 0.000000000000000000, 0.000000000000000000, -1.000000000000000000 ) ) ;
#36951 = CARTESIAN_POINT ( 'NONE',  ( 97.81554761001611098, -40.52684041789147074, 96.63643476469849247 ) ) ;
#36952 = CARTESIAN_POINT ( 'NONE',  ( 116.1942131220466621, -33.21547736372279758, 139.1184824187689628 ) ) ;
#36953 = VERTEX_POINT ( 'NONE', #7613 ) ;
#36954 = ORIENTED_EDGE ( 'NONE', *, *, #6776, .T. ) ;
#36955 = CARTESIAN_POINT ( 'NONE',  ( 102.3355707743008765, -29.23633396390525618, 106.9558690201829734 ) ) ;
#36956 = CARTESIAN_POINT ( 'NONE',  ( -100.8961411191535973, 120.6499999999999915, 3.968749999998880451 ) ) ;
#36957 = EDGE_CURVE ( 'NONE', #73636, #37760, #62568, .T. ) ;
#36959 = CARTESIAN_POINT ( 'NONE',  ( 107.0664832912740252, -46.47944715994103149, -4.824374724089029343 ) ) ;
#36958 = CARTESIAN_POINT ( 'NONE',  ( 110.0587659310071302, -27.38278898179171605, 230.8299109901959412 ) ) ;
#36960 = VECTOR ( 'NONE', #13022, 1000.000000000000000 ) ;
#36961 = DIRECTION ( 'NONE',  ( 1.000000000000000000, 1.000000000000000078E-15, 0.000000000000000000 ) ) ;
#36962 = CARTESIAN_POINT ( 'NONE',  ( -7.196800215918080040E-13, 127.0000000000000000, 110.3312500000000114 ) ) ;
#36963 = EDGE_CURVE ( 'NONE', #42066, #68825, #41656, .T. ) ;
#36964 = LINE ( 'NONE', #2456, #86666 ) ;
#36965 = EDGE_CURVE ( 'NONE', #23110, #45437, #7171, .T. ) ;
#36966 = CARTESIAN_POINT ( 'NONE',  ( -3.175000000000109956, 111.1250000000000000, 31.75000000000000000 ) ) ;
#36967 = CARTESIAN_POINT ( 'NONE',  ( 10.93445099564298317, 76.23525864503069727, 118.0515728341300559 ) ) ;
#36968 = CARTESIAN_POINT ( 'NONE',  ( 107.6517678568360594, -47.10594642807022581, 152.6213395616249500 ) ) ;
#36969 = VERTEX_POINT ( 'NONE', #34861 ) ;
#36970 = ORIENTED_EDGE ( 'NONE', *, *, #2189, .F. ) ;
#36971 = ORIENTED_EDGE ( 'NONE', *, *, #69580, .F. ) ;
#36972 = EDGE_CURVE ( 'NONE', #40524, #71527, #82596, .T. ) ;
#36973 = ADVANCED_FACE ( 'NONE', ( #34409 ), #77110, .T. ) ;
#36974 = CARTESIAN_POINT ( 'NONE',  ( 88.17226027475679473, -58.72944715994100306, 239.5838068554174924 ) ) ;
#36975 = CARTESIAN_POINT ( 'NONE',  ( 77.31651910784952975, -18.55813574388988485, 3.101427645696272606 ) ) ;
#36976 = CARTESIAN_POINT ( 'NONE',  ( 105.7154773167319206, -46.72385839048828160, 78.46895860815600088 ) ) ;
#36977 = DIRECTION ( 'NONE',  ( 0.000000000000000000, -0.000000000000000000, -1.000000000000000000 ) ) ;
#36978 = CARTESIAN_POINT ( 'NONE',  ( 102.1208986914200665, -43.83170863157916131, 234.8985665600679624 ) ) ;
#36979 = EDGE_CURVE ( 'NONE', #31161, #58675, #1250, .T. ) ;
#36980 = AXIS2_PLACEMENT_3D ( 'NONE', #88906, #54338, #82104 ) ;
#36981 = AXIS2_PLACEMENT_3D ( 'NONE', #60383, #89006, #82209 ) ;
#36982 = PLANE ( 'NONE',  #49436 ) ;
#36983 = AXIS2_PLACEMENT_3D ( 'NONE', #81661, #25774, #13496 ) ;
#36984 = VECTOR ( 'NONE', #14202, 1000.000000000000000 ) ;
#36985 = EDGE_CURVE ( 'NONE', #18226, #22928, #40127, .T. ) ;
#36986 = CARTESIAN_POINT ( 'NONE',  ( 113.6143417880574020, -45.63476223351307226, 183.0689586092439640 ) ) ;
#36987 = DIRECTION ( 'NONE',  ( 1.000000000000000078E-15, -1.000000000000000000, 0.000000000000000000 ) ) ;
#36988 = ORIENTED_EDGE ( 'NONE', *, *, #26232, .T. ) ;
#36990 = EDGE_LOOP ( 'NONE', ( #37774, #43059, #88511, #25251, #81271 ) ) ;
#36989 = ORIENTED_EDGE ( 'NONE', *, *, #28895, .F. ) ;
#36991 = VECTOR ( 'NONE', #70028, 1000.000000000000000 ) ;
#36992 = CARTESIAN_POINT ( 'NONE',  ( 31.89136050872298966, -31.76306994223740432, -5.074374724088000832 ) ) ;
#36993 = ORIENTED_EDGE ( 'NONE', *, *, #3006, .F. ) ;
#36994 = ORIENTED_EDGE ( 'NONE', *, *, #8596, .T. ) ;
#36995 = DIRECTION ( 'NONE',  ( 1.000000000000000078E-15, 0.000000000000000000, 1.000000000000000000 ) ) ;
#36996 = CARTESIAN_POINT ( 'NONE',  ( -487.2989999999999782, 93.66249999999999432, 11.11250000000040217 ) ) ;
#36997 = EDGE_CURVE ( 'NONE', #16194, #24603, #76652, .T. ) ;
#36998 = CARTESIAN_POINT ( 'NONE',  ( 105.9698521113164844, -27.93594508925886188, 266.6072975916113705 ) ) ;
#36999 = CARTESIAN_POINT ( 'NONE',  ( 113.1782932911942936, -44.75186896820116544, 273.0939585610741460 ) ) ;
#37000 = ORIENTED_EDGE ( 'NONE', *, *, #54805, .F. ) ;
#37001 = CIRCLE ( 'NONE', #73290, 1.000000000000000888 ) ;
#37002 = CARTESIAN_POINT ( 'NONE',  ( 106.3677493097285662, -44.90353489983662172, 9.635625275910937759 ) ) ;
#37003 = EDGE_CURVE ( 'NONE', #27372, #29714, #83929, .T. ) ;
#37004 = FACE_OUTER_BOUND ( 'NONE', #8869, .T. ) ;
#37005 = ORIENTED_EDGE ( 'NONE', *, *, #33602, .T. ) ;
#37006 = ORIENTED_EDGE ( 'NONE', *, *, #18037, .F. ) ;
#37007 = LINE ( 'NONE', #49725, #38609 ) ;
#37008 = VERTEX_POINT ( 'NONE', #8514 ) ;
#37009 = ORIENTED_EDGE ( 'NONE', *, *, #72553, .F. ) ;
#37010 = AXIS2_PLACEMENT_3D ( 'NONE', #34668, #18809, #26077 ) ;
#37011 = CARTESIAN_POINT ( 'NONE',  ( 114.1180452634077369, -42.41171291218270767, 42.69718173283898466 ) ) ;
#37012 = CARTESIAN_POINT ( 'NONE',  ( 97.40467406345878487, -42.14653896106843689, 181.7451490854349743 ) ) ;
#37013 = CARTESIAN_POINT ( 'NONE',  ( 97.85535806214033983, -31.89376338832682123, 135.9413395616259947 ) ) ;
#37014 = LINE ( 'NONE', #70648, #59744 ) ;
#37015 = CARTESIAN_POINT ( 'NONE',  ( 100.7501737310821994, -45.80018108968007340, 233.0803871806729717 ) ) ;
#37016 = CARTESIAN_POINT ( 'NONE',  ( 193.0371591254585724, -47.82818131005411999, 129.9678068554150343 ) ) ;
#37017 = CARTESIAN_POINT ( 'NONE',  ( 74.76628479679460781, -74.85678555694860847, 248.3919653347779786 ) ) ;
#37018 = CARTESIAN_POINT ( 'NONE',  ( -129.9681501387584035, 79.66749569656610674, -12.37561169055459231 ) ) ;
#37019 = EDGE_LOOP ( 'NONE', ( #13722, #66904 ) ) ;
#37020 = EDGE_CURVE ( 'NONE', #11193, #42810, #89396, .T. ) ;
#37021 = EDGE_LOOP ( 'NONE', ( #79599, #874, #19349, #16244 ) ) ;
#37022 = EDGE_CURVE ( 'NONE', #61208, #59170, #84129, .T. ) ;
#37023 = CARTESIAN_POINT ( 'NONE',  ( 117.4576385420935338, -35.45251388149282690, 193.9241967044829664 ) ) ;
#37024 = VERTEX_POINT ( 'NONE', #16663 ) ;
#37025 = CARTESIAN_POINT ( 'NONE',  ( 112.4862084254573631, -26.19061110901967382, 169.6984824187679521 ) ) ;
#37026 = DIRECTION ( 'NONE',  ( 1.000000000000000078E-15, -1.000000000000000083E-30, -1.000000000000000000 ) ) ;
#37027 = AXIS2_PLACEMENT_3D ( 'NONE', #2527, #56109, #63858 ) ;
#37028 = CARTESIAN_POINT ( 'NONE',  ( 135.2364670978292907, -34.23881677343971575, 8.012604158001305876 ) ) ;
#37029 = CARTESIAN_POINT ( 'NONE',  ( 0.000000000000000000, 82.54999999999999716, -190.5010000000000048 ) ) ;
#37032 = CARTESIAN_POINT ( 'NONE',  ( 104.3301552612371523, -26.04411461992211230, 241.2880062282919482 ) ) ;
#37031 = DIRECTION ( 'NONE',  ( 1.000000000000000000, 1.780283607454400635E-15, 0.000000000000000000 ) ) ;
#37030 = CARTESIAN_POINT ( 'NONE',  ( -31.46309309085269845, 53.97500000000000142, 37.49170920442474397 ) ) ;
#37033 = DIRECTION ( 'NONE',  ( 0.000000000000000000, -1.000000000000000000, 0.000000000000000000 ) ) ;
#37034 = DIRECTION ( 'NONE',  ( -1.000000000000000000, 0.000000000000000000, 0.000000000000000000 ) ) ;
#37035 = LINE ( 'NONE', #86090, #46914 ) ;
#37036 = CARTESIAN_POINT ( 'NONE',  ( 133.5825581355576901, -151.1625929302300051, 73.15139425029549614 ) ) ;
#37037 = B_SPLINE_CURVE_WITH_KNOTS ( 'NONE', 3,
 ( #62539, #63899, #70257, #56613, #13945, #27573, #77523, #315, #89821, #57056, #84802, #48887, #76625, #14407, #77977, #42082, #15750, #83902 ),
 .UNSPECIFIED., .F., .F.,
 ( 4, 2, 2, 2, 2, 2, 2, 2, 4 ),
 ( 0.000000000000000000, 0.06249209452423747091, 0.1249841890484749418, 0.1874762835727123989, 0.2499683780969498836, 0.3124604726211873684, 0.3749525671454247977, 0.4374446616696622825, 0.4999367561938997673 ),
 .UNSPECIFIED. ) ;
#37038 = CARTESIAN_POINT ( 'NONE',  ( 115.0372575140148115, -42.90846255661264053, 259.3022919435708218 ) ) ;
#37039 = CARTESIAN_POINT ( 'NONE',  ( 146.5419990862876034, -137.3788609484426786, 246.8585042003560375 ) ) ;
#37041 = EDGE_LOOP ( 'NONE', ( #78052, #37576, #3542, #19825, #59633, #2651, #11691, #13387, #87065, #40304, #88189, #19295 ) ) ;
#37040 = CARTESIAN_POINT ( 'NONE',  ( 113.6372100165067422, -30.15837270650189339, 195.5838068554168103 ) ) ;
#37042 = CARTESIAN_POINT ( 'NONE',  ( 136.7660003837314946, -19.25405382162758272, 6.823682607503624098 ) ) ;
#37043 = CARTESIAN_POINT ( 'NONE',  ( 109.4503794976336764, -25.91221646008812840, 179.8918157521019339 ) ) ;
#37044 = CARTESIAN_POINT ( 'NONE',  ( 113.5060836576900272, -28.53103057085638383, 75.54705384733995288 ) ) ;
#37045 = CARTESIAN_POINT ( 'NONE',  ( 109.3680554845995232, -25.87125837001184081, 180.9222919425779708 ) ) ;
#37046 = CARTESIAN_POINT ( 'NONE',  ( 163.0667039024470171, -32.29483332968611364, 342.9256252759119548 ) ) ;
#37047 = CARTESIAN_POINT ( 'NONE',  ( 161.4809174648185603, -48.32844715993547169, 180.4678068554150059 ) ) ;
#37049 = CARTESIAN_POINT ( 'NONE',  ( -178.3658777604659917, 101.5999999999999943, 122.9960808104842016 ) ) ;
#37048 = CARTESIAN_POINT ( 'NONE',  ( 44.45000000000000284, 69.84999999999999432, 219.0749999999999886 ) ) ;
#37050 = CARTESIAN_POINT ( 'NONE',  ( 182.5667039024459939, -22.48495420874030515, -5.074374724088000832 ) ) ;
#37051 = CARTESIAN_POINT ( 'NONE',  ( 107.0664832912739968, -36.72944715994100306, 287.6356252759109680 ) ) ;
#37052 = ORIENTED_EDGE ( 'NONE', *, *, #41875, .T. ) ;
#37053 = ADVANCED_FACE ( 'NONE', ( #52041 ), #9401, .F. ) ;
#37054 = CARTESIAN_POINT ( 'NONE',  ( 80.06648329127398256, -9.029447159941060619, 4.925625275910944012 ) ) ;
#37055 = CIRCLE ( 'NONE', #57391, 8.999999999999994671 ) ;
#37056 = AXIS2_PLACEMENT_3D ( 'NONE', #18734, #33710, #75942 ) ;
#37057 = VECTOR ( 'NONE', #31917, 1000.000000000000000 ) ;
#37058 = CIRCLE ( 'NONE', #77717, 10.00000000000000888 ) ;
#37059 = ORIENTED_EDGE ( 'NONE', *, *, #50171, .T. ) ;
#37060 = VERTEX_POINT ( 'NONE', #9854 ) ;
#37061 = VECTOR ( 'NONE', #33012, 1000.000000000000000 ) ;
#37062 = CARTESIAN_POINT ( 'NONE',  ( 112.6295607727957133, -43.21082823627408231, 107.5638483995059715 ) ) ;
#37064 = EDGE_LOOP ( 'NONE', ( #88055, #9866, #68386, #10290 ) ) ;
#37063 = CARTESIAN_POINT ( 'NONE',  ( -10.08079905861141690, 90.28579524239222565, -130.1664991954058905 ) ) ;
#37065 = CARTESIAN_POINT ( 'NONE',  ( 118.8180844208008722, -35.40729807334668777, 79.91562527591095488 ) ) ;
#37066 = DIRECTION ( 'NONE',  ( 0.000000000000000000, 1.000000000000000000, 0.000000000000000000 ) ) ;
#37067 = VECTOR ( 'NONE', #40836, 1000.000000000000000 ) ;
#37068 = PLANE ( 'NONE',  #86261 ) ;
#37069 = CARTESIAN_POINT ( 'NONE',  ( 115.0889047256920463, -30.61763668260735116, 175.3439586089972408 ) ) ;
#37071 = CARTESIAN_POINT ( 'NONE',  ( 111.8651074766111861, -28.16866562884735004, 34.66991099019695355 ) ) ;
#37070 = VECTOR ( 'NONE', #59938, 1000.000000000000000 ) ;
#37072 = ORIENTED_EDGE ( 'NONE', *, *, #59216, .F. ) ;
#37073 = EDGE_CURVE ( 'NONE', #33963, #68797, #22343, .T. ) ;
#37074 = VERTEX_POINT ( 'NONE', #78905 ) ;
#37075 = ORIENTED_EDGE ( 'NONE', *, *, #71031, .T. ) ;
#37076 = APPLICATION_CONTEXT ( 'automotive_design' ) ;
#37077 = DIRECTION ( 'NONE',  ( 0.000000000000000000, 0.000000000000000000, -1.000000000000000000 ) ) ;
#37078 = DIRECTION ( 'NONE',  ( 0.000000000000000000, 1.000000000000000000, 0.000000000000000000 ) ) ;
#37079 = CARTESIAN_POINT ( 'NONE',  ( 112.1393456437007501, -28.01282278244291746, 115.6564586090561590 ) ) ;
#37080 = CARTESIAN_POINT ( 'NONE',  ( -544.5124999999999318, 53.97500000000000142, 50.79999999999999716 ) ) ;
#37081 = TOROIDAL_SURFACE ( 'NONE', #86357, 15.84999999999999964, 0.1499999999999999944 ) ;
#37082 = DIRECTION ( 'NONE',  ( -1.000000000000000000, -4.510281037539694659E-14, 0.000000000000000000 ) ) ;
#37083 = ADVANCED_FACE ( 'NONE', ( #33414 ), #3920, .F. ) ;
#37084 = CARTESIAN_POINT ( 'NONE',  ( 160.2664750769284865, 20.32000000000000028, -148.0533267522753818 ) ) ;
#37085 = EDGE_CURVE ( 'NONE', #30354, #25238, #66194, .T. ) ;
#37086 = DIRECTION ( 'NONE',  ( -0.7071067811865460184, 0.000000000000000000, -0.7071067811865489050 ) ) ;
#37087 = EDGE_CURVE ( 'NONE', #9949, #5742, #59317, .T. ) ;
#37088 = CARTESIAN_POINT ( 'NONE',  ( 75.85717701425106441, 89.26692529358290074, 91.11128979799275385 ) ) ;
#37089 = CARTESIAN_POINT ( 'NONE',  ( 109.9050689397999889, -46.77468768478704675, 72.79562527591099297 ) ) ;
#37090 = VECTOR ( 'NONE', #58281, 1000.000000000000000 ) ;
#37091 = VERTEX_POINT ( 'NONE', #59760 ) ;
#37092 = DIRECTION ( 'NONE',  ( 0.000000000000000000, 0.000000000000000000, 1.000000000000000000 ) ) ;
#37093 = CARTESIAN_POINT ( 'NONE',  ( 85.58879520791425932, -121.5356829788755562, 250.2178068554179902 ) ) ;
#37094 = CARTESIAN_POINT ( 'NONE',  ( 99.66770068389166681, -32.23957622922084454, 123.6985665600679738 ) ) ;
#37095 = ADVANCED_FACE ( 'NONE', ( #46573 ), #74310, .F. ) ;
#37096 = AXIS2_PLACEMENT_3D ( 'NONE', #80853, #46286, #39496 ) ;
#37097 = CARTESIAN_POINT ( 'NONE',  ( 115.0860330880669551, -30.61390894146469677, 94.34433169324587709 ) ) ;
#37098 = EDGE_CURVE ( 'NONE', #87386, #73279, #12081, .T. ) ;
#37099 = CARTESIAN_POINT ( 'NONE',  ( 19.56670390244796920, -67.87844715994100397, 20.91780685541479912 ) ) ;
#37100 = ORIENTED_EDGE ( 'NONE', *, *, #77867, .F. ) ;
#37101 = ORIENTED_EDGE ( 'NONE', *, *, #27435, .F. ) ;
#37102 = CARTESIAN_POINT ( 'NONE',  ( 97.81942511135183338, -40.53627538877582026, 136.6376214459276639 ) ) ;
#37103 = VERTEX_POINT ( 'NONE', #87490 ) ;
#37104 = ORIENTED_EDGE ( 'NONE', *, *, #71880, .F. ) ;
#37105 = EDGE_CURVE ( 'NONE', #19551, #29192, #51729, .T. ) ;
#37106 = CARTESIAN_POINT ( 'NONE',  ( 103.6521623672117158, -27.97622271609356659, 166.7920594963739802 ) ) ;
#37107 = DIRECTION ( 'NONE',  ( 1.025452301070035257E-14, -1.000000000000000000, 0.000000000000000000 ) ) ;
#37108 = CARTESIAN_POINT ( 'NONE',  ( 109.5135917660753506, -46.88567278592853427, 128.7641967044819751 ) ) ;
#37109 = CARTESIAN_POINT ( 'NONE',  ( 28.57499999999999929, 91.71543552338529537, 302.8950000000000387 ) ) ;
#37110 = CARTESIAN_POINT ( 'NONE',  ( 116.3521921512060686, -40.56741147027513250, 18.51432941078872929 ) ) ;
#37111 = VECTOR ( 'NONE', #50810, 1000.000000000000000 ) ;
#37112 = ORIENTED_EDGE ( 'NONE', *, *, #13699, .F. ) ;
#37113 = CIRCLE ( 'NONE', #8130, 0.9999999999999974465 ) ;
#37114 = VECTOR ( 'NONE', #45533, 999.9999999999998863 ) ;
#37115 = ORIENTED_EDGE ( 'NONE', *, *, #4887, .F. ) ;
#37116 = B_SPLINE_CURVE_WITH_KNOTS ( 'NONE', 3,
 ( #44378, #16696, #42578, #8543, #70314, #71667, #63951, #9430, #72107, #1278, #9881, #823, #28983, #29431, #24406, #65719, #72555, #12109 ),
 .UNSPECIFIED., .F., .F.,
 ( 4, 2, 2, 2, 2, 2, 2, 2, 4 ),
 ( 0.000000000000000000, 0.06249999997324977991, 0.1249999999464995598, 0.1874999999197493328, 0.2499999998929991196, 0.3124999998662488787, 0.3749999998394986656, 0.4374999998127484524, 0.4999999997859982392 ),
 .UNSPECIFIED. ) ;
#37117 = ORIENTED_EDGE ( 'NONE', *, *, #51022, .F. ) ;
#37118 = CARTESIAN_POINT ( 'NONE',  ( 97.93802767643609286, -38.39294625876189571, 199.2880903695909751 ) ) ;
#37119 = CARTESIAN_POINT ( 'NONE',  ( 110.4638204314202881, -47.27238515144596676, 57.83657765686300678 ) ) ;
#37120 = ORIENTED_EDGE ( 'NONE', *, *, #9101, .T. ) ;
#37121 = CARTESIAN_POINT ( 'NONE',  ( 104.6539710028518897, -47.49251396406771164, 27.38895860924395009 ) ) ;
#37122 = CARTESIAN_POINT ( 'NONE',  ( 113.7646124051505154, -44.74644941934948861, 189.1299109901969757 ) ) ;
#37123 = CARTESIAN_POINT ( 'NONE',  ( 173.9900000000000091, 21.46300000000000097, 59.96543552338529537 ) ) ;
#37124 = LINE ( 'NONE', #43014, #77896 ) ;
#37125 = CARTESIAN_POINT ( 'NONE',  ( 116.9217636815068033, -33.22305568060546932, 110.0984824187679578 ) ) ;
#37126 = DIRECTION ( 'NONE',  ( -1.000000000000000000, -4.299999999999999979E-14, -1.000000000000000078E-15 ) ) ;
#37127 = ORIENTED_EDGE ( 'NONE', *, *, #58975, .F. ) ;
#37128 = LINE ( 'NONE', #17130, #69974 ) ;
#37129 = ORIENTED_EDGE ( 'NONE', *, *, #72553, .T. ) ;
#37130 = DIRECTION ( 'NONE',  ( 0.000000000000000000, -1.000000000000000000, 0.000000000000000000 ) ) ;
#37131 = ORIENTED_EDGE ( 'NONE', *, *, #51724, .F. ) ;
#37132 = EDGE_CURVE ( 'NONE', #57830, #71968, #74963, .T. ) ;
#37133 = CIRCLE ( 'NONE', #8144, 2.999999999999999112 ) ;
#37134 = VERTEX_POINT ( 'NONE', #24815 ) ;
#37135 = CARTESIAN_POINT ( 'NONE',  ( 108.0667039024470171, -87.35579742913164125, -19.26696060647653397 ) ) ;
#37136 = DIRECTION ( 'NONE',  ( 1.000000000000000000, 0.000000000000000000, 0.000000000000000000 ) ) ;
#37137 = CARTESIAN_POINT ( 'NONE',  ( 117.0917326185583676, -32.07397045188266560, 59.16038718067295576 ) ) ;
#37138 = CARTESIAN_POINT ( 'NONE',  ( 9.506033823739755917, 69.25266161161103184, 36.92015570084876686 ) ) ;
#37139 = VECTOR ( 'NONE', #4196, 1000.000000000000000 ) ;
#37140 = DIRECTION ( 'NONE',  ( 0.000000000000000000, 1.000000000000000000, 0.000000000000000000 ) ) ;
#37141 = DIRECTION ( 'NONE',  ( 0.000000000000000000, 0.000000000000000000, 1.000000000000000000 ) ) ;
#37142 = CARTESIAN_POINT ( 'NONE',  ( 96.86520444330096780, -38.59296402346417665, 51.48229194257797303 ) ) ;
#37144 = CARTESIAN_POINT ( 'NONE',  ( 113.6008039948045649, -28.63430547549730676, 160.5356252759109736 ) ) ;
#37143 = CARTESIAN_POINT ( 'NONE',  ( 97.33768507753748622, -34.07162146941007563, 111.1148373774395850 ) ) ;
#37145 = DIRECTION ( 'NONE',  ( 1.387778780781444492E-15, 0.000000000000000000, -1.000000000000000000 ) ) ;
#37146 = PLANE ( 'NONE',  #77181 ) ;
#37147 = ORIENTED_EDGE ( 'NONE', *, *, #64870, .T. ) ;
#37148 = CARTESIAN_POINT ( 'NONE',  ( 71.06648329127399677, -8.729447159940999512, 17.92562527591199739 ) ) ;
#37149 = CARTESIAN_POINT ( 'NONE',  ( -487.2989999999999782, 100.8062500000000057, 86.36305401447658880 ) ) ;
#37150 = FACE_OUTER_BOUND ( 'NONE', #6789, .T. ) ;
#37151 = CARTESIAN_POINT ( 'NONE',  ( 34.67381068362025331, -26.00627455219402506, 117.4678068554150485 ) ) ;
#37152 = EDGE_CURVE ( 'NONE', #20562, #28735, #67038, .T. ) ;
#37154 = ORIENTED_EDGE ( 'NONE', *, *, #1423, .T. ) ;
#37153 = CARTESIAN_POINT ( 'NONE',  ( 101.4014481618761181, -46.27514046166531614, 207.1622919425779514 ) ) ;
#37155 = CARTESIAN_POINT ( 'NONE',  ( 72.96458098368701428, 117.4749999999999943, -78.00648098368678518 ) ) ;
#37156 = CARTESIAN_POINT ( 'NONE',  ( 100.8102337077607871, -45.86971777371983450, 238.1108633711489517 ) ) ;
#37157 = CARTESIAN_POINT ( 'NONE',  ( 109.7813809329710040, -47.49173451690833048, 88.78514908543493789 ) ) ;
#37158 = CARTESIAN_POINT ( 'NONE',  ( -3.174999999999664979, 8.255000000000000782, 31.75000000000000000 ) ) ;
#37159 = DIRECTION ( 'NONE',  ( -2.108231265501709878E-16, 0.000000000000000000, 1.000000000000000000 ) ) ;
#37160 = DIRECTION ( 'NONE',  ( 0.000000000000000000, 0.000000000000000000, 1.000000000000000000 ) ) ;
#37161 = ORIENTED_EDGE ( 'NONE', *, *, #28319, .T. ) ;
#37162 = EDGE_CURVE ( 'NONE', #64576, #46976, #11637, .T. ) ;
#37163 = VERTEX_POINT ( 'NONE', #18436 ) ;
#37164 = ORIENTED_EDGE ( 'NONE', *, *, #82165, .F. ) ;
#37165 = EDGE_LOOP ( 'NONE', ( #48817, #24572, #7768, #16813, #2478 ) ) ;
#37166 = CARTESIAN_POINT ( 'NONE',  ( 29.56670390244797630, -67.87844715994100397, 20.91780685541479912 ) ) ;
#37167 = CARTESIAN_POINT ( 'NONE',  ( 110.2773916389477478, -46.62487827714361543, 8.827053847339950465 ) ) ;
#37168 = DIRECTION ( 'NONE',  ( 4.299999999999999979E-14, -1.000000000000000000, 0.000000000000000000 ) ) ;
#37169 = LINE ( 'NONE', #3099, #55619 ) ;
#37171 = CARTESIAN_POINT ( 'NONE',  ( 83.23139715273200068, 69.85063172184842983, 84.43201024598489823 ) ) ;
#37170 = CARTESIAN_POINT ( 'NONE',  ( 182.4202572930400379, -33.70561438051982606, 342.9256252759109884 ) ) ;
#37172 = AXIS2_PLACEMENT_3D ( 'NONE', #22259, #15445, #21813 ) ;
#37173 = DIRECTION ( 'NONE',  ( 0.000000000000000000, 0.000000000000000000, -1.000000000000000000 ) ) ;
#37174 = CARTESIAN_POINT ( 'NONE',  ( 98.10212974493634874, -35.44374275293071008, 225.6476579233149948 ) ) ;
#37175 = ORIENTED_EDGE ( 'NONE', *, *, #29678, .F. ) ;
#37176 = VERTEX_POINT ( 'NONE', #45668 ) ;
#37177 = CIRCLE ( 'NONE', #73401, 3.500000000000003109 ) ;
#37178 = VERTEX_POINT ( 'NONE', #73400 ) ;
#37179 = AXIS2_PLACEMENT_3D ( 'NONE', #89780, #61155, #20725 ) ;
#37180 = AXIS2_PLACEMENT_3D ( 'NONE', #21117, #8843, #7486 ) ;
#37181 = DIRECTION ( 'NONE',  ( -1.000000000000000078E-15, 1.000000000000000083E-30, 1.000000000000000000 ) ) ;
#37182 = AXIS2_PLACEMENT_3D ( 'NONE', #10051, #65456, #18191 ) ;
#37183 = FACE_OUTER_BOUND ( 'NONE', #83764, .T. ) ;
#37184 = CARTESIAN_POINT ( 'NONE',  ( 97.83217745605955429, -40.05230289513912822, 262.6013395616248545 ) ) ;
#37185 = EDGE_CURVE ( 'NONE', #66356, #4943, #38565, .T. ) ;
#37186 = DIRECTION ( 'NONE',  ( 0.000000000000000000, 0.000000000000000000, 1.000000000000000000 ) ) ;
#37187 = CARTESIAN_POINT ( 'NONE',  ( 102.6819511611811180, -27.33185899950651887, 131.4118157521009778 ) ) ;
#37188 = ADVANCED_FACE ( 'NONE', ( #23398 ), #22489, .T. ) ;
#37189 = CARTESIAN_POINT ( 'NONE',  ( 87.06648329127403940, -54.72944906728955061, -4.824374724089049771 ) ) ;
#37190 = ORIENTED_EDGE ( 'NONE', *, *, #11535, .T. ) ;
#37191 = ADVANCED_FACE ( 'NONE', ( #15220 ), #30633, .F. ) ;
#37192 = CARTESIAN_POINT ( 'NONE',  ( 77.38348569455061465, -36.12003772029492410, 3.004064388423448584 ) ) ;
#37193 = VERTEX_POINT ( 'NONE', #36565 ) ;
#37194 = VECTOR ( 'NONE', #11420, 1000.000000000000000 ) ;
#37195 = CARTESIAN_POINT ( 'NONE',  ( 41.56648329127399677, -9.303447159940999356, 201.0426252759120018 ) ) ;
#37196 = CARTESIAN_POINT ( 'NONE',  ( 104.8541313898159757, -44.58662387026339502, 20.17666179816296435 ) ) ;
#37197 = ADVANCED_FACE ( 'NONE', ( #86058 ), #2931, .F. ) ;
#37198 = CARTESIAN_POINT ( 'NONE',  ( 136.8164806451551669, -18.72944715939129523, 6.749772901088581634 ) ) ;
#37199 = AXIS2_PLACEMENT_3D ( 'NONE', #61063, #47869, #27003 ) ;
#37200 = DIRECTION ( 'NONE',  ( 0.000000000000000000, -1.000000000000000000, 0.000000000000000000 ) ) ;
#37201 = ADVANCED_FACE ( 'NONE', ( #37004 ), #3900, .F. ) ;
#37202 = CARTESIAN_POINT ( 'NONE',  ( 91.90683392111127148, 78.46407912418312947, -74.89107914305729707 ) ) ;
#37203 = VERTEX_POINT ( 'NONE', #44693 ) ;
#37204 = CARTESIAN_POINT ( 'NONE',  ( 103.8797721312301405, -101.8611209747514010, -19.78219314458209865 ) ) ;
#37205 = DIRECTION ( 'NONE',  ( 0.000000000000000000, 0.000000000000000000, -1.000000000000000000 ) ) ;
#37206 = ORIENTED_EDGE ( 'NONE', *, *, #81117, .F. ) ;
#37207 = CARTESIAN_POINT ( 'NONE',  ( 118.8429430416104680, -35.40450127974935413, 83.91562527591095488 ) ) ;
#37208 = VERTEX_POINT ( 'NONE', #30189 ) ;
#37209 = CARTESIAN_POINT ( 'NONE',  ( 100.5114817196218411, -42.97801697403279775, 36.34289601855395091 ) ) ;
#37210 = CARTESIAN_POINT ( 'NONE',  ( 109.2888275139916203, -46.51057382167308418, 88.75361627338941162 ) ) ;
#37211 = CARTESIAN_POINT ( 'NONE',  ( 116.0163176773587708, -41.35234337494321721, 89.87872616303998541 ) ) ;
#37212 = CARTESIAN_POINT ( 'NONE',  ( 28.99999999999998224, 172.0000000000000000, -8.624053851998977755E-15 ) ) ;
#37213 = CARTESIAN_POINT ( 'NONE',  ( 130.5667039024480118, -34.21194715994094082, 239.5838068554170377 ) ) ;
#37214 = CARTESIAN_POINT ( 'NONE',  ( 100.4515265478786574, -44.84261285976553779, 8.032768133053981074 ) ) ;
#37215 = CARTESIAN_POINT ( 'NONE',  ( -41.60202597009397607, 40.59999999999997300, 50.85338361873603219 ) ) ;
#37216 = ORIENTED_EDGE ( 'NONE', *, *, #31686, .T. ) ;
#37217 = FACE_OUTER_BOUND ( 'NONE', #56607, .T. ) ;
#37218 = VERTEX_POINT ( 'NONE', #78802 ) ;
#37219 = CARTESIAN_POINT ( 'NONE',  ( 99.39016829297771949, -27.63593621212785933, 146.6356252759109395 ) ) ;
#37220 = CARTESIAN_POINT ( 'NONE',  ( -7.205548786489490269E-13, 127.0000000000000000, 111.1250000000000000 ) ) ;
#37221 = ORIENTED_EDGE ( 'NONE', *, *, #17193, .F. ) ;
#37222 = ORIENTED_EDGE ( 'NONE', *, *, #13138, .T. ) ;
#37223 = ORIENTED_EDGE ( 'NONE', *, *, #89391, .F. ) ;
#37224 = FACE_OUTER_BOUND ( 'NONE', #82108, .T. ) ;
#37225 = LINE ( 'NONE', #30854, #14492 ) ;
#37226 = CARTESIAN_POINT ( 'NONE',  ( 98.91665286848242999, -30.31703347128389225, 200.8080062282919869 ) ) ;
#37227 = DIRECTION ( 'NONE',  ( -2.900000000000000265E-14, 2.000000000000000155E-15, -1.000000000000000000 ) ) ;
#37228 = CARTESIAN_POINT ( 'NONE',  ( 144.0716631786001471, -138.9592723264545953, 247.5160078862170110 ) ) ;
#37229 = CYLINDRICAL_SURFACE ( 'NONE', #89680, 2.517500000000005844 ) ;
#37230 = CARTESIAN_POINT ( 'NONE',  ( 100.4653332305737905, -44.82571634032018437, 8.032768133053981074 ) ) ;
#37231 = DIRECTION ( 'NONE',  ( -1.000000000000000000, -1.000000000000000078E-15, -1.000000000000000078E-15 ) ) ;
#37232 = ORIENTED_EDGE ( 'NONE', *, *, #52435, .T. ) ;
#37233 = CARTESIAN_POINT ( 'NONE',  ( 97.53183428581748160, -39.74892342586570493, 172.5705140066459933 ) ) ;
#37234 = VECTOR ( 'NONE', #88944, 1000.000000000000000 ) ;
#37235 = LINE ( 'NONE', #84958, #46112 ) ;
#37236 = ADVANCED_FACE ( 'NONE', ( #44241 ), #77898, .F. ) ;
#37237 = VERTEX_POINT ( 'NONE', #16559 ) ;
#37238 = VECTOR ( 'NONE', #77306, 1000.000000000000000 ) ;
#37239 = CIRCLE ( 'NONE', #11156, 2.116999999999993776 ) ;
#37240 = CARTESIAN_POINT ( 'NONE',  ( 81.48476992307091393, -21.08750326150235210, 1.944748881532749163 ) ) ;
#37241 = VECTOR ( 'NONE', #78229, 1000.000000000000000 ) ;
#37242 = CARTESIAN_POINT ( 'NONE',  ( 83.73314995793998605, 12.92155284005730387, 355.9756252759109998 ) ) ;
#37243 = CARTESIAN_POINT ( 'NONE',  ( 97.49318720818078532, -40.89074837367932957, 231.6527681330539679 ) ) ;
#37244 =( LENGTH_UNIT ( ) NAMED_UNIT ( * ) SI_UNIT ( .MILLI., .METRE. ) );
#37245 = VECTOR ( 'NONE', #86693, 999.9999999999998863 ) ;
#37246 = EDGE_CURVE ( 'NONE', #21321, #27069, #80746, .T. ) ;
#37247 = FACE_BOUND ( 'NONE', #5883, .T. ) ;
#37248 = CYLINDRICAL_SURFACE ( 'NONE', #37426, 1.499999999999987788 ) ;
#37249 = CARTESIAN_POINT ( 'NONE',  ( 113.7727705757230297, -31.39298644294678908, 243.7838483995059562 ) ) ;
#37251 = CARTESIAN_POINT ( 'NONE',  ( 97.79189512308838061, -32.01662636557821173, 46.95276813305393659 ) ) ;
#37250 = DIRECTION ( 'NONE',  ( -2.761895400282000234E-15, 0.000000000000000000, -1.000000000000000000 ) ) ;
#37252 = DIRECTION ( 'NONE',  ( 0.000000000000000000, 0.000000000000000000, -1.000000000000000000 ) ) ;
#37253 = CARTESIAN_POINT ( 'NONE',  ( 101.4772741282170472, -27.87691040622789274, 110.5241967044819944 ) ) ;
#37254 = ORIENTED_EDGE ( 'NONE', *, *, #66289, .F. ) ;
#37255 = CARTESIAN_POINT ( 'NONE',  ( 131.7676426598729904, -20.23887630718033392, 7.293197373621852719 ) ) ;
#37256 = ORIENTED_EDGE ( 'NONE', *, *, #44027, .F. ) ;
#37257 = LINE ( 'NONE', #85434, #11635 ) ;
#37258 = DIRECTION ( 'NONE',  ( 0.000000000000000000, 0.000000000000000000, -1.000000000000000000 ) ) ;
#37259 = ORIENTED_EDGE ( 'NONE', *, *, #60049, .F. ) ;
#37260 = DIRECTION ( 'NONE',  ( -1.000000000000000000, 0.000000000000000000, 0.000000000000000000 ) ) ;
#37261 = ORIENTED_EDGE ( 'NONE', *, *, #13599, .T. ) ;
#37262 = DIRECTION ( 'NONE',  ( -0.000000000000000000, -0.000000000000000000, -1.000000000000000000 ) ) ;
#37263 = CARTESIAN_POINT ( 'NONE',  ( 41.56648329127398966, -27.82844715994070484, 78.92562527591199739 ) ) ;
#37264 = CIRCLE ( 'NONE', #42999, 2.517499999999998739 ) ;
#37265 = CYLINDRICAL_SURFACE ( 'NONE', #19101, 3.299999999999997158 ) ;
#37266 = ORIENTED_EDGE ( 'NONE', *, *, #87474, .T. ) ;
#37267 = VECTOR ( 'NONE', #58886, 1000.000000000000000 ) ;
#37268 = EDGE_CURVE ( 'NONE', #58881, #23612, #15677, .T. ) ;
#37269 = CARTESIAN_POINT ( 'NONE',  ( 117.3606796971436523, -32.63983085838949449, 99.13943479972098771 ) ) ;
#37270 = CARTESIAN_POINT ( 'NONE',  ( 87.06648329127403940, -54.72944906728955061, -4.824374724089049771 ) ) ;
#37271 = DIRECTION ( 'NONE',  ( -0.7071067811865436870, 0.7071067811865513475, -7.071067811865430960E-16 ) ) ;
#37272 = LINE ( 'NONE', #71361, #4990 ) ;
#37273 = ORIENTED_EDGE ( 'NONE', *, *, #75188, .T. ) ;
#37274 = DIRECTION ( 'NONE',  ( 0.000000000000000000, 0.000000000000000000, -1.000000000000000000 ) ) ;
#37275 = FACE_OUTER_BOUND ( 'NONE', #72193, .T. ) ;
#37276 = DIRECTION ( 'NONE',  ( 1.000000000000000000, 1.000000000000000078E-15, -0.000000000000000000 ) ) ;
#37278 = CARTESIAN_POINT ( 'NONE',  ( 107.0664832912739968, -8.350947159940998787, 330.8831252759119934 ) ) ;
#37277 = DIRECTION ( 'NONE',  ( -1.000000000000000000, 0.000000000000000000, 0.000000000000000000 ) ) ;
#37279 = DIRECTION ( 'NONE',  ( 0.000000000000000000, 0.000000000000000000, 1.000000000000000000 ) ) ;
#37280 = AXIS2_PLACEMENT_3D ( 'NONE', #14023, #55770, #34005 ) ;
#37281 = VERTEX_POINT ( 'NONE', #8412 ) ;
#37282 = B_SPLINE_CURVE_WITH_KNOTS ( 'NONE', 3,
 ( #72661, #53056, #18126, #33102, #74442, #52614, #4508, #18575, #86738, #24509, #73991, #53511, #12218, #60343, #66724, #31755, #60799, #4056, #87625, #52173, #25389, #39906, #80376, #10869, #79935, #17691, #88532, #73091, #38567, #46255, #10428 ),
 .UNSPECIFIED., .F., .F.,
 ( 4, 2, 2, 1, 2, 2, 2, 2, 2, 2, 2, 1, 1, 2, 2, 2, 4 ),
 ( 0.000000000000000000, 0.1249999999999873990, 0.1874999999999810985, 0.2187499999999738542, 0.2343749999999741318, 0.2499999999999744094, 0.3749999999999857336, 0.4374999999999914513, 0.4999999999999972244, 0.6250000000000086597, 0.6875000000000128786, 0.7187500000000148770, 0.7343750000000159872, 0.7421875000000164313, 0.7500000000000168754, 0.8750000000000083267, 1.000000000000000000 ),
 .UNSPECIFIED. ) ;
#37283 = DIRECTION ( 'NONE',  ( -6.831565154159360295E-14, 1.000000000000000000, 0.000000000000000000 ) ) ;
#37284 = CARTESIAN_POINT ( 'NONE',  ( 104.0088209277215867, -27.43890701233904394, 161.3299109901969643 ) ) ;
#37285 = EDGE_CURVE ( 'NONE', #59268, #27442, #27050, .T. ) ;
#37287 = VERTEX_POINT ( 'NONE', #71537 ) ;
#37286 = DIRECTION ( 'NONE',  ( 1.000000000000000000, 0.000000000000000000, 1.261617073437676668E-15 ) ) ;
#37288 = CARTESIAN_POINT ( 'NONE',  ( 113.6564618781686136, -45.68400828401183844, 29.08133956162495082 ) ) ;
#37289 = FACE_OUTER_BOUND ( 'NONE', #43445, .T. ) ;
#37290 = CARTESIAN_POINT ( 'NONE',  ( 98.38057243704078303, -41.69553627151279329, 51.73981168366587013 ) ) ;
#37291 = EDGE_CURVE ( 'NONE', #9592, #48907, #34299, .T. ) ;
#37292 = DIRECTION ( 'NONE',  ( 0.000000000000000000, 0.000000000000000000, -1.000000000000000000 ) ) ;
#37293 = FACE_OUTER_BOUND ( 'NONE', #12243, .T. ) ;
#37294 = EDGE_CURVE ( 'NONE', #8449, #51823, #45885, .T. ) ;
#37295 = AXIS2_PLACEMENT_3D ( 'NONE', #37046, #2538, #58374 ) ;
#37296 = VECTOR ( 'NONE', #70294, 1000.000000000000000 ) ;
#37297 = CARTESIAN_POINT ( 'NONE',  ( 104.5747221139661320, -26.66317121150808944, 240.2575300378159682 ) ) ;
#37298 = VERTEX_POINT ( 'NONE', #71094 ) ;
#37299 = ORIENTED_EDGE ( 'NONE', *, *, #39113, .F. ) ;
#37300 = CARTESIAN_POINT ( 'NONE',  ( 115.8619398590553260, -35.64860379657582712, 190.3558690201829506 ) ) ;
#37301 = DIRECTION ( 'NONE',  ( 1.000000000000000000, 0.000000000000000000, 0.000000000000000000 ) ) ;
#37302 = AXIS2_PLACEMENT_3D ( 'NONE', #41313, #69042, #43103 ) ;
#37303 = CARTESIAN_POINT ( 'NONE',  ( 114.9896934147946013, -32.69399539773264252, 40.63301187732598407 ) ) ;
#37304 = AXIS2_PLACEMENT_3D ( 'NONE', #62889, #41098, #83352 ) ;
#37305 = CARTESIAN_POINT ( 'NONE',  ( -88.80956239834375765, 94.30053025434482095, 95.69832483115281718 ) ) ;
#37306 = DIRECTION ( 'NONE',  ( 0.9825752044328147639, 0.1858654557302462929, 0.000000000000000000 ) ) ;
#37307 = EDGE_CURVE ( 'NONE', #7607, #63584, #64267, .T. ) ;
#37308 = FACE_OUTER_BOUND ( 'NONE', #10460, .T. ) ;
#37309 = EDGE_LOOP ( 'NONE', ( #17724, #73438 ) ) ;
#37310 = CARTESIAN_POINT ( 'NONE',  ( 0.000000000000000000, 198.8420489685532004, -25.39999999999999858 ) ) ;
#37311 = FACE_OUTER_BOUND ( 'NONE', #38079, .T. ) ;
#37312 = ADVANCED_FACE ( 'NONE', ( #2490, #45561 ), #66027, .T. ) ;
#37313 = CARTESIAN_POINT ( 'NONE',  ( 101.6619702986602505, -45.61876124157287649, 247.1413395616249602 ) ) ;
#37314 = CARTESIAN_POINT ( 'NONE',  ( 11.74674901193918330, 87.43010368066354943, 117.9729399478468252 ) ) ;
#37315 = VERTEX_POINT ( 'NONE', #74204 ) ;
#37316 = CARTESIAN_POINT ( 'NONE',  ( 108.3334480867816296, -46.73485935508681166, 82.67729194192742170 ) ) ;
#37317 = CARTESIAN_POINT ( 'NONE',  ( 107.0667039024470313, -104.2784471599409528, 25.71780685541800437 ) ) ;
#37318 = DIRECTION ( 'NONE',  ( 0.000000000000000000, 0.000000000000000000, -1.000000000000000000 ) ) ;
#37319 = AXIS2_PLACEMENT_3D ( 'NONE', #61523, #55138, #76062 ) ;
#37320 = DIRECTION ( 'NONE',  ( 1.000000000000000078E-15, 1.000000000000000083E-30, -1.000000000000000000 ) ) ;
#37321 = AXIS2_PLACEMENT_3D ( 'NONE', #61790, #89529, #54960 ) ;
#37322 = CARTESIAN_POINT ( 'NONE',  ( 117.4022237771661281, -37.57280582802024327, 34.77372051400595865 ) ) ;
#37323 = CARTESIAN_POINT ( 'NONE',  ( 90.44969454456422397, -56.64645651782490177, 239.5838068554174356 ) ) ;
#37324 = VECTOR ( 'NONE', #702, 1000.000000000000000 ) ;
#37325 = EDGE_LOOP ( 'NONE', ( #27111, #39670, #64374, #49338 ) ) ;
#37326 = CARTESIAN_POINT ( 'NONE',  ( 111.9491823805485922, -27.46919719833538309, 55.68991099019693536 ) ) ;
#37327 = CARTESIAN_POINT ( 'NONE',  ( 72.31648329127399677, -9.833000550534366724, -5.074374724089063982 ) ) ;
#37328 = CARTESIAN_POINT ( 'NONE',  ( 105.7763445623522500, -26.38427570067176831, 270.1756252759109884 ) ) ;
#37329 = ORIENTED_EDGE ( 'NONE', *, *, #44569, .T. ) ;
#37330 = DIRECTION ( 'NONE',  ( 0.7071067811865692221, 0.7071067811865259234, 7.071067811865685367E-16 ) ) ;
#37331 = DIRECTION ( 'NONE',  ( 0.000000000000000000, -0.000000000000000000, 1.000000000000000000 ) ) ;
#37332 = CARTESIAN_POINT ( 'NONE',  ( 36.23715912545424089, -47.82818131006125384, 300.4678068554150059 ) ) ;
#37333 = CARTESIAN_POINT ( 'NONE',  ( 98.90209562501077301, -37.38172185807169967, 99.20809036959194316 ) ) ;
#37334 = CARTESIAN_POINT ( 'NONE',  ( 97.74302678327005367, -41.52030872683848628, 192.7041967044819728 ) ) ;
#37335 = FACE_BOUND ( 'NONE', #56786, .T. ) ;
#37336 = DIRECTION ( 'NONE',  ( 0.9963424814100688698, -0.08544974978094983797, 0.000000000000000000 ) ) ;
#37337 = VERTEX_POINT ( 'NONE', #88296 ) ;
#37338 = VECTOR ( 'NONE', #80791, 1000.000000000000000 ) ;
#37339 = DIRECTION ( 'NONE',  ( 0.000000000000000000, 0.000000000000000000, -1.000000000000000000 ) ) ;
#37340 = ORIENTED_EDGE ( 'NONE', *, *, #43316, .F. ) ;
#37342 = EDGE_LOOP ( 'NONE', ( #85563, #21097, #5726, #40589 ) ) ;
#37341 = CIRCLE ( 'NONE', #76505, 7.000000000000006217 ) ;
#37343 = DIRECTION ( 'NONE',  ( 2.900000000000000265E-14, -2.000000000000000155E-15, 1.000000000000000000 ) ) ;
#37344 = EDGE_LOOP ( 'NONE', ( #45479, #88849, #62081, #67271 ) ) ;
#37345 = ORIENTED_EDGE ( 'NONE', *, *, #10852, .T. ) ;
#37346 = CARTESIAN_POINT ( 'NONE',  ( 107.0667039024470313, -104.2784471599420471, -19.18411693322902423 ) ) ;
#37347 = EDGE_CURVE ( 'NONE', #69712, #23413, #39665, .T. ) ;
#37348 = CARTESIAN_POINT ( 'NONE',  ( 97.75828744068094522, -40.38463776613766498, 42.62423351867927579 ) ) ;
#37349 = CARTESIAN_POINT ( 'NONE',  ( 112.6189512620115778, -30.20087909038965535, 138.9381341137909658 ) ) ;
#37350 = CARTESIAN_POINT ( 'NONE',  ( 96.24499046374883449, -34.36497383161641039, 256.1432443235299843 ) ) ;
#37351 = DIRECTION ( 'NONE',  ( 0.000000000000000000, 0.000000000000000000, -1.000000000000000000 ) ) ;
#37352 = VERTEX_POINT ( 'NONE', #17884 ) ;
#37353 = CARTESIAN_POINT ( 'NONE',  ( 103.2779182987110005, -27.47489285962728545, 136.3856765722742352 ) ) ;
#37354 = ORIENTED_EDGE ( 'NONE', *, *, #83334, .F. ) ;
#37355 = CARTESIAN_POINT ( 'NONE',  ( 71.06670390244701707, -90.27844715994098124, 230.7030882296565721 ) ) ;
#37356 = CYLINDRICAL_SURFACE ( 'NONE', #66200, 9.999999999999998224 ) ;
#37357 = DIRECTION ( 'NONE',  ( 0.000000000000000000, 0.000000000000000000, 1.000000000000000000 ) ) ;
#37359 = LINE ( 'NONE', #23746, #68330 ) ;
#37358 = AXIS2_PLACEMENT_3D ( 'NONE', #44513, #79969, #73119 ) ;
#37360 = ORIENTED_EDGE ( 'NONE', *, *, #10249, .F. ) ;
#37362 = EDGE_CURVE ( 'NONE', #30460, #49742, #66475, .T. ) ;
#37361 = VECTOR ( 'NONE', #55566, 999.9999999999998863 ) ;
#37363 = CARTESIAN_POINT ( 'NONE',  ( 106.8364329414440874, -47.15221585624544787, 272.5584824187680510 ) ) ;
#37364 = CARTESIAN_POINT ( 'NONE',  ( 116.5137666388868780, -32.21926627522912412, 15.18133956162492915 ) ) ;
#37365 =( NAMED_UNIT ( * ) SI_UNIT ( $, .STERADIAN. ) SOLID_ANGLE_UNIT ( ) );
#37366 = CARTESIAN_POINT ( 'NONE',  ( 116.3212776292293995, -32.94146857471267253, 120.1356252759109537 ) ) ;
#37368 = CYLINDRICAL_SURFACE ( 'NONE', #34044, 0.4999999999999933387 ) ;
#37367 = CARTESIAN_POINT ( 'NONE',  ( 7.620115932400929327E-15, 67.86880000000000734, 221.5895999999999901 ) ) ;
#37369 = DIRECTION ( 'NONE',  ( 0.000000000000000000, 0.000000000000000000, 1.000000000000000000 ) ) ;
#37370 = FACE_OUTER_BOUND ( 'NONE', #48137, .T. ) ;
#37371 = CARTESIAN_POINT ( 'NONE',  ( 131.3333327974764870, -37.08363404521318785, 6.775960187534245449 ) ) ;
#37372 = CIRCLE ( 'NONE', #70779, 0.5000000000000004441 ) ;
#37373 = FACE_OUTER_BOUND ( 'NONE', #3873, .T. ) ;
#37374 = EDGE_CURVE ( 'NONE', #31479, #64725, #64793, .T. ) ;
#37375 = CARTESIAN_POINT ( 'NONE',  ( 0.000000000000000000, 20.32000000000000028, 0.000000000000000000 ) ) ;
#37376 = CARTESIAN_POINT ( 'NONE',  ( 141.0667039024479834, -48.82844715994099971, 310.9178068554150514 ) ) ;
#37377 = EDGE_CURVE ( 'NONE', #44246, #34853, #46012, .T. ) ;
#37378 = LINE ( 'NONE', #44172, #39418 ) ;
#37379 = CARTESIAN_POINT ( 'NONE',  ( 104.5828969173064849, -26.58150870143000688, 285.2670538473396391 ) ) ;
#37380 = CARTESIAN_POINT ( 'NONE',  ( 101.9720301123653883, -46.53865341315756154, 163.1832443235299763 ) ) ;
#37381 = CARTESIAN_POINT ( 'NONE',  ( 110.5624684038761814, -46.61161715960605534, 33.84705384733993583 ) ) ;
#37382 = AXIS2_PLACEMENT_3D ( 'NONE', #75062, #68697, #89596 ) ;
#37383 = CIRCLE ( 'NONE', #32958, 11.45913725231036118 ) ;
#37385 = LINE ( 'NONE', #72797, #79151 ) ;
#37384 = CARTESIAN_POINT ( 'NONE',  ( 172.5667039024478413, -36.32844715993500273, 249.9678068554149775 ) ) ;
#37386 = FACE_OUTER_BOUND ( 'NONE', #34293, .T. ) ;
#37387 = CIRCLE ( 'NONE', #8415, 11.49999999999999645 ) ;
#37388 = EDGE_CURVE ( 'NONE', #48723, #54028, #26052, .T. ) ;
#37389 = ORIENTED_EDGE ( 'NONE', *, *, #77289, .T. ) ;
#37390 = CARTESIAN_POINT ( 'NONE',  ( 188.5667039024480971, -42.82844715993431350, 293.2178068554150059 ) ) ;
#37391 = VERTEX_POINT ( 'NONE', #11067 ) ;
#37392 = CARTESIAN_POINT ( 'NONE',  ( 116.4719273984280790, -32.36179259691363796, 55.16038718067301261 ) ) ;
#37394 = ORIENTED_EDGE ( 'NONE', *, *, #66024, .F. ) ;
#37393 = CARTESIAN_POINT ( 'NONE',  ( 116.3135867418571650, -32.94878190598771539, 189.1356252759109680 ) ) ;
#37395 = CARTESIAN_POINT ( 'NONE',  ( 148.0533267522752112, 20.32000000000000028, 160.2664750769284865 ) ) ;
#37396 = CARTESIAN_POINT ( 'NONE',  ( 98.55548742614595881, -30.74683778668247669, 201.8384824187679385 ) ) ;
#37397 = LINE ( 'NONE', #36055, #27974 ) ;
#37398 = CYLINDRICAL_SURFACE ( 'NONE', #66676, 10.04999999999999361 ) ;
#37399 = DIRECTION ( 'NONE',  ( 0.7071067811985215501, -0.7071067811745735954, 0.000000000000000000 ) ) ;
#37400 = EDGE_CURVE ( 'NONE', #8859, #74897, #38770, .T. ) ;
#37401 = PLANE ( 'NONE',  #26940 ) ;
#37402 = DIRECTION ( 'NONE',  ( 1.000000000000000000, 0.000000000000000000, 0.000000000000000000 ) ) ;
#37403 = CARTESIAN_POINT ( 'NONE',  ( 112.5642669466485586, -45.09754247072631728, 98.03899555326725590 ) ) ;
#37404 = CARTESIAN_POINT ( 'NONE',  ( 97.33998274022607688, -37.75834089694785689, 126.4099109901969626 ) ) ;
#37405 = ORIENTED_EDGE ( 'NONE', *, *, #54042, .T. ) ;
#37406 = VERTEX_POINT ( 'NONE', #72855 ) ;
#37407 = CARTESIAN_POINT ( 'NONE',  ( 98.73617028912649118, -32.38405755445656808, 87.36348806780198117 ) ) ;
#37408 = DIRECTION ( 'NONE',  ( -1.000000000000000000, -6.814610998690690172E-14, -1.000000000000000078E-15 ) ) ;
#37410 = CARTESIAN_POINT ( 'NONE',  ( 83.96770390244800808, -18.82844715994099971, 239.5838068554169809 ) ) ;
#37409 = CARTESIAN_POINT ( 'NONE',  ( 114.9410966442421795, -29.98191058901456074, 225.4022919425769658 ) ) ;
#37411 = DIRECTION ( 'NONE',  ( 0.7071067811874389708, -0.7071067811856560636, 0.000000000000000000 ) ) ;
#37412 = CARTESIAN_POINT ( 'NONE',  ( 106.5462518941686909, -24.40236651281373526, 322.0356252759110021 ) ) ;
#37413 = B_SPLINE_CURVE_WITH_KNOTS ( 'NONE', 3,
 ( #53839, #27068, #54738, #67492, #81158, #88858, #46589, #81609, #80699, #73867 ),
 .UNSPECIFIED., .F., .F.,
 ( 4, 2, 2, 2, 4 ),
 ( 0.4999378446604081927, 0.5499671847885604370, 0.5999965249167127368, 0.6500258650448649256, 0.7000552051730172254 ),
 .UNSPECIFIED. ) ;
#37414 = CARTESIAN_POINT ( 'NONE',  ( 118.5472164932298256, 69.93120980984943458, -1.660430599528443851 ) ) ;
#37415 = EDGE_CURVE ( 'NONE', #59219, #9306, #46108, .T. ) ;
#37416 = CARTESIAN_POINT ( 'NONE',  ( -12.59749777234951651, 80.88611186001949704, 117.8848162280639684 ) ) ;
#37417 = DIRECTION ( 'NONE',  ( -0.000000000000000000, 1.000000000000000000, -0.000000000000000000 ) ) ;
#37418 = CARTESIAN_POINT ( 'NONE',  ( 1.640888995811506934, 70.02979118506246436, 118.5474374850178094 ) ) ;
#37419 = CARTESIAN_POINT ( 'NONE',  ( 114.2383551682310525, -44.26553795382362466, 158.1813395616249807 ) ) ;
#37420 = ORIENTED_EDGE ( 'NONE', *, *, #29814, .F. ) ;
#37421 = VERTEX_POINT ( 'NONE', #61896 ) ;
#37422 = EDGE_CURVE ( 'NONE', #2509, #65246, #58048, .T. ) ;
#37423 = CARTESIAN_POINT ( 'NONE',  ( 193.0371591254584018, -47.82818131005411999, 300.4678068554149490 ) ) ;
#37424 = CARTESIAN_POINT ( 'NONE',  ( 77.48363092588481038, -17.78502016655210838, 2.871594975604033539 ) ) ;
#37425 = ADVANCED_FACE ( 'NONE', ( #11369, #74942 ), #80875, .F. ) ;
#37426 = AXIS2_PLACEMENT_3D ( 'NONE', #51292, #3177, #1390 ) ;
#37427 = DIRECTION ( 'NONE',  ( -1.000000000000000000, 0.000000000000000000, 2.170915417798913171E-16 ) ) ;
#37428 = CARTESIAN_POINT ( 'NONE',  ( 83.56670390244703128, -104.2784471599409670, 23.21780685541800082 ) ) ;
#37429 = CARTESIAN_POINT ( 'NONE',  ( 114.9986391697397607, -34.80314782265816831, 206.8338046553059826 ) ) ;
#37430 = AXIS2_PLACEMENT_3D ( 'NONE', #32570, #60270, #53437 ) ;
#37431 = AXIS2_PLACEMENT_3D ( 'NONE', #30099, #52730, #58247 ) ;
#37432 = FACE_OUTER_BOUND ( 'NONE', #1603, .T. ) ;
#37433 = CARTESIAN_POINT ( 'NONE',  ( 109.6058900474308757, -26.58167301968400764, 199.8813395616249977 ) ) ;
#37434 = CARTESIAN_POINT ( 'NONE',  ( 50.03799999999999670, 101.5999999999999943, 206.3750000000000000 ) ) ;
#37435 = VERTEX_POINT ( 'NONE', #45859 ) ;
#37437 = ORIENTED_EDGE ( 'NONE', *, *, #17484, .F. ) ;
#37436 = EDGE_LOOP ( 'NONE', ( #35060, #74487, #31480, #88100 ) ) ;
#37438 = CIRCLE ( 'NONE', #88222, 130.5560000000000116 ) ;
#37439 = CARTESIAN_POINT ( 'NONE',  ( 194.0371591254575492, -24.42818131005407167, 117.4678068554150627 ) ) ;
#37440 = DIRECTION ( 'NONE',  ( -0.7071067811571960515, 0.7071067812158990940, 0.000000000000000000 ) ) ;
#37441 = CARTESIAN_POINT ( 'NONE',  ( 131.7155263566292547, -35.29868341352990768, 7.242354772856963052 ) ) ;
#37442 = CARTESIAN_POINT ( 'NONE',  ( 111.1445474647120051, -44.63080920614596181, 269.3872975916115706 ) ) ;
#37443 = AXIS2_PLACEMENT_3D ( 'NONE', #38569, #65399, #87187 ) ;
#37444 = LINE ( 'NONE', #23824, #17336 ) ;
#37445 = VERTEX_POINT ( 'NONE', #87236 ) ;
#37446 = AXIS2_PLACEMENT_3D ( 'NONE', #24023, #38085, #16756 ) ;
#37447 = VECTOR ( 'NONE', #32524, 1000.000000000000000 ) ;
#37448 = CARTESIAN_POINT ( 'NONE',  ( 102.4743188866377039, -43.40982696052134315, 9.635625275910939536 ) ) ;
#37449 = DIRECTION ( 'NONE',  ( 1.777766061779359009E-15, -1.000000000000000000, 3.100000000000000044E-14 ) ) ;
#37450 = ORIENTED_EDGE ( 'NONE', *, *, #36654, .F. ) ;
#37451 = VERTEX_POINT ( 'NONE', #18632 ) ;
#37452 = CARTESIAN_POINT ( 'NONE',  ( 116.7497567485386156, -34.15833269763940194, 114.0330597662738938 ) ) ;
#37453 = VERTEX_POINT ( 'NONE', #33153 ) ;
#37454 = ORIENTED_EDGE ( 'NONE', *, *, #89619, .F. ) ;
#37455 = EDGE_CURVE ( 'NONE', #52482, #29231, #46759, .T. ) ;
#37456 = AXIS2_PLACEMENT_3D ( 'NONE', #22373, #50050, #87278 ) ;
#37457 = CARTESIAN_POINT ( 'NONE',  ( 109.1520131464112069, -27.24676858702523674, 29.32670554236194249 ) ) ;
#37458 = CARTESIAN_POINT ( 'NONE',  ( 113.6281634912633223, -45.65356023013480780, 183.0689586092439640 ) ) ;
#37459 = CARTESIAN_POINT ( 'NONE',  ( 117.1882713363357169, -39.28166824301213467, 123.6299109901969615 ) ) ;
#37460 = DIRECTION ( 'NONE',  ( 0.000000000000000000, -1.000000000000000000, 0.000000000000000000 ) ) ;
#37461 = CARTESIAN_POINT ( 'NONE',  ( 116.6057436952887372, -40.93480069938575383, 249.4956252759109532 ) ) ;
#37462 = CARTESIAN_POINT ( 'NONE',  ( 117.0609360745339984, -38.08016024203720207, 99.71977895578028495 ) ) ;
#37463 = CARTESIAN_POINT ( 'NONE',  ( 115.8240617383016797, -31.72764908460863609, 125.2400077891570902 ) ) ;
#37464 = CARTESIAN_POINT ( 'NONE',  ( 141.8164832912739826, -9.833000550534297446, 14.92562527591100618 ) ) ;
#37465 = EDGE_LOOP ( 'NONE', ( #67342, #28091 ) ) ;
#37466 = EDGE_LOOP ( 'NONE', ( #56461, #14552, #8023, #23452 ) ) ;
#37467 = AXIS2_PLACEMENT_3D ( 'NONE', #10062, #37318, #65022 ) ;
#37468 = AXIS2_PLACEMENT_3D ( 'NONE', #30859, #80808, #17237 ) ;
#37469 = CARTESIAN_POINT ( 'NONE',  ( 96.63001237737263693, -35.53283987767252228, 206.2356252759109623 ) ) ;
#37470 = ORIENTED_EDGE ( 'NONE', *, *, #40901, .F. ) ;
#37471 = ADVANCED_FACE ( 'NONE', ( #12720 ), #59943, .T. ) ;
#37472 = CARTESIAN_POINT ( 'NONE',  ( 102.9670468844020235, -26.46427747797763175, 175.3908633711489813 ) ) ;
#37473 = CARTESIAN_POINT ( 'NONE',  ( 106.5580495140764015, -24.23977772305836709, 322.9014499992877631 ) ) ;
#37474 = CARTESIAN_POINT ( 'NONE',  ( 91.91125933621934507, -111.8737466215628160, -19.26696060647578435 ) ) ;
#37475 = CARTESIAN_POINT ( 'NONE',  ( 144.0491476497456915, -140.6784470014346198, 245.7567723467967653 ) ) ;
#37476 = EDGE_CURVE ( 'NONE', #76957, #72320, #60848, .T. ) ;
#37479 = CARTESIAN_POINT ( 'NONE',  ( 96.91023542590100703, -30.67149048741791262, 276.8984824187680829 ) ) ;
#37478 = LINE ( 'NONE', #31541, #26737 ) ;
#37477 = DIRECTION ( 'NONE',  ( -1.000000000000000000, 0.000000000000000000, 0.000000000000000000 ) ) ;
#37480 = DIRECTION ( 'NONE',  ( 0.000000000000000000, 0.000000000000000000, 1.000000000000000000 ) ) ;
#37481 = CARTESIAN_POINT ( 'NONE',  ( 106.5667039024470313, -108.2470741265389620, -19.78219314458190681 ) ) ;
#37482 = CARTESIAN_POINT ( 'NONE',  ( 182.5667039024469886, -33.35206098992650681, -5.074374724088000832 ) ) ;
#37483 = EDGE_CURVE ( 'NONE', #69399, #64426, #15584, .T. ) ;
#37484 = CARTESIAN_POINT ( 'NONE',  ( 67.46744162048150883, -137.4384689103915207, 246.7095008466345405 ) ) ;
#37485 = DIRECTION ( 'NONE',  ( -0.2884130866282256234, -0.7071067811865451302, 0.6456143519637580486 ) ) ;
#37486 = EDGE_CURVE ( 'NONE', #84622, #85514, #88071, .T. ) ;
#37487 = DIRECTION ( 'NONE',  ( -4.237773401492740281E-14, 1.000000000000000000, 0.000000000000000000 ) ) ;
#37489 = EDGE_LOOP ( 'NONE', ( #87161, #33090 ) ) ;
#37488 = CARTESIAN_POINT ( 'NONE',  ( 108.7127106255978219, -44.55865754719168592, 195.5838068554167819 ) ) ;
#37490 = CIRCLE ( 'NONE', #59254, 0.5000000000000004441 ) ;
#37491 = EDGE_CURVE ( 'NONE', #81899, #57373, #31805, .T. ) ;
#37492 = CARTESIAN_POINT ( 'NONE',  ( 135.1909174281126980, -21.23916151080255688, 8.028235474617199330 ) ) ;
#37493 = CARTESIAN_POINT ( 'NONE',  ( 116.8159443494545826, -40.58124828358739222, 193.5270538473389479 ) ) ;
#37494 = CARTESIAN_POINT ( 'NONE',  ( 117.0915230934440103, -32.07406775014006683, 55.16038718067301261 ) ) ;
#37495 = CARTESIAN_POINT ( 'NONE',  ( 117.9780035659441495, -34.69567636304840619, 199.9851490854349549 ) ) ;
#37496 = DIRECTION ( 'NONE',  ( 8.659560562355169516E-17, -0.7071067811865280328, 0.7071067811865670016 ) ) ;
#37497 = DIRECTION ( 'NONE',  ( 0.000000000000000000, 0.000000000000000000, 1.000000000000000000 ) ) ;
#37499 = DIRECTION ( 'NONE',  ( -1.000000000000000000, 0.000000000000000000, 0.000000000000000000 ) ) ;
#37498 = CARTESIAN_POINT ( 'NONE',  ( 165.9667039024473922, -26.71338133338714016, 313.9678068554149490 ) ) ;
#37500 = DIRECTION ( 'NONE',  ( -0.7071067811567310901, 0.7071067812163639443, 0.000000000000000000 ) ) ;
#37501 = CARTESIAN_POINT ( 'NONE',  ( 34.67381068360426610, -28.98061976759052527, 313.9678068554150059 ) ) ;
#37502 = ORIENTED_EDGE ( 'NONE', *, *, #85077, .T. ) ;
#37503 = EDGE_CURVE ( 'NONE', #16163, #42342, #85170, .T. ) ;
#37504 = CARTESIAN_POINT ( 'NONE',  ( 7.661254700127833495, 82.54999999999999716, 320.6630000000000109 ) ) ;
#37505 = AXIS2_PLACEMENT_3D ( 'NONE', #65865, #17292, #4097 ) ;
#37506 = AXIS2_PLACEMENT_3D ( 'NONE', #17712, #44054, #9558 ) ;
#37507 =( BOUNDED_CURVE ( )  B_SPLINE_CURVE ( 2, ( #86455, #65979, #24222 ),
 .UNSPECIFIED., .F., .T. ) 
 B_SPLINE_CURVE_WITH_KNOTS ( ( 3, 3 ),
 ( 0.000000000000000000, 0.5053286420056760653 ),
 .UNSPECIFIED. ) 
 CURVE ( )  GEOMETRIC_REPRESENTATION_ITEM ( )  RATIONAL_B_SPLINE_CURVE ( ( 1.000000000000000000, 1.009299002520659849, 1.000420656333769864 ) ) 
 REPRESENTATION_ITEM ( '' )  );
#37508 = EDGE_CURVE ( 'NONE', #75109, #83315, #39066, .T. ) ;
#37509 = ORIENTED_EDGE ( 'NONE', *, *, #22979, .F. ) ;
#37510 = ORIENTED_EDGE ( 'NONE', *, *, #45576, .F. ) ;
#37511 = CARTESIAN_POINT ( 'NONE',  ( 107.5061752250017264, -28.17031325930595642, 94.45813411379100444 ) ) ;
#37512 = AXIS2_PLACEMENT_3D ( 'NONE', #16769, #36767, #29956 ) ;
#37514 = ORIENTED_EDGE ( 'NONE', *, *, #2277, .T. ) ;
#37513 = CARTESIAN_POINT ( 'NONE',  ( -9.270409258063830649, 91.24028187095998987, -130.2267823906806257 ) ) ;
#37515 = CARTESIAN_POINT ( 'NONE',  ( 102.5676158828201778, -27.34920955258912301, 91.43276813305395478 ) ) ;
#37516 = CARTESIAN_POINT ( 'NONE',  ( -479.3614999999999782, 7.143750000000280487, 15.23694598552305024 ) ) ;
#37517 = EDGE_CURVE ( 'NONE', #43582, #22883, #60396, .T. ) ;
#37518 = AXIS2_PLACEMENT_3D ( 'NONE', #89256, #40182, #26565 ) ;
#37519 = LINE ( 'NONE', #39288, #28269 ) ;
#37520 = DIRECTION ( 'NONE',  ( -1.000000000000000000, -1.541976423090496028E-15, 0.000000000000000000 ) ) ;
#37521 = AXIS2_PLACEMENT_3D ( 'NONE', #11786, #53525, #10882 ) ;
#37522 = CARTESIAN_POINT ( 'NONE',  ( 97.30224646447496184, -33.23681714893609751, 26.06514908543594444 ) ) ;
#37523 = VERTEX_POINT ( 'NONE', #54011 ) ;
#37524 = ORIENTED_EDGE ( 'NONE', *, *, #84167, .F. ) ;
#37525 = ORIENTED_EDGE ( 'NONE', *, *, #84078, .F. ) ;
#37526 = DIRECTION ( 'NONE',  ( 0.000000000000000000, 0.000000000000000000, -1.000000000000000000 ) ) ;
#37527 = LINE ( 'NONE', #86572, #43253 ) ;
#37528 = FACE_OUTER_BOUND ( 'NONE', #45380, .T. ) ;
#37529 = DIRECTION ( 'NONE',  ( 1.000000000000000000, 0.000000000000000000, 0.000000000000000000 ) ) ;
#37530 = CARTESIAN_POINT ( 'NONE',  ( 179.7974245136210527, -36.32844715993471141, 117.4678068554150627 ) ) ;
#37531 = DIRECTION ( 'NONE',  ( 0.9961946980917455452, -1.067350013832299363E-17, -0.08715574274765836016 ) ) ;
#37532 = B_SPLINE_CURVE_WITH_KNOTS ( 'NONE', 3,
 ( #75017, #19164, #73670, #88664, #47741, #19604, #74568, #60936, #12808, #4636, #89103, #66856, #46838, #4188, #67296, #74125, #59575, #33237 ),
 .UNSPECIFIED., .F., .F.,
 ( 4, 2, 2, 2, 2, 2, 2, 2, 4 ),
 ( 0.4999597063510836659, 0.5624647430571981799, 0.6249697797633126939, 0.6874748164694273189, 0.7499798531755418329, 0.8124848898816563469, 0.8749899265877709720, 0.9374949632938854860, 1.000000000000000000 ),
 .UNSPECIFIED. ) ;
#37533 = VECTOR ( 'NONE', #56196, 1000.000000000000000 ) ;
#37534 = DIRECTION ( 'NONE',  ( 0.000000000000000000, 0.000000000000000000, 1.000000000000000000 ) ) ;
#37535 = CARTESIAN_POINT ( 'NONE',  ( 74.36911441044604487, 82.54999999999999716, 92.32962665258637003 ) ) ;
#37536 = CARTESIAN_POINT ( 'NONE',  ( 96.20032699425225076, -38.62430069186631698, 46.45181575210094138 ) ) ;
#37537 = ORIENTED_EDGE ( 'NONE', *, *, #13524, .F. ) ;
#37538 = EDGE_CURVE ( 'NONE', #15300, #56710, #59499, .T. ) ;
#37539 = CARTESIAN_POINT ( 'NONE',  ( 4.867771054587877622, 94.30191638479369942, 130.4669033451685891 ) ) ;
#37540 = DIRECTION ( 'NONE',  ( 0.000000000000000000, -1.000000000000000000, 0.000000000000000000 ) ) ;
#37541 = EDGE_CURVE ( 'NONE', #12734, #45673, #48876, .T. ) ;
#37542 = CARTESIAN_POINT ( 'NONE',  ( 79.72329571771361145, -100.8945472140120501, 250.2178068554180470 ) ) ;
#37543 = CARTESIAN_POINT ( 'NONE',  ( 105.4193742293517460, -27.59801994936882252, 123.0366617981629673 ) ) ;
#37544 = VECTOR ( 'NONE', #51685, 1000.000000000000000 ) ;
#37545 = CARTESIAN_POINT ( 'NONE',  ( 99.09444862205589288, -30.55209741447661287, 95.80246077065771715 ) ) ;
#37546 = DIRECTION ( 'NONE',  ( -6.831565154159360295E-14, 1.000000000000000000, 0.000000000000000000 ) ) ;
#37547 = ORIENTED_EDGE ( 'NONE', *, *, #82457, .T. ) ;
#37548 = ORIENTED_EDGE ( 'NONE', *, *, #15262, .T. ) ;
#37549 = CARTESIAN_POINT ( 'NONE',  ( 100.8874983018639426, -44.70024987288356755, 137.0511845485476101 ) ) ;
#37550 = ORIENTED_EDGE ( 'NONE', *, *, #1404, .F. ) ;
#37551 = EDGE_LOOP ( 'NONE', ( #56724, #49891, #22599, #72919 ) ) ;
#37552 = CARTESIAN_POINT ( 'NONE',  ( 115.5682375124590635, -39.22913789569613385, 180.0301547344689936 ) ) ;
#37553 = VECTOR ( 'NONE', #44607, 1000.000000000000000 ) ;
#37554 = CYLINDRICAL_SURFACE ( 'NONE', #42337, 7.874000000000186184 ) ;
#37555 = CARTESIAN_POINT ( 'NONE',  ( 114.1899296859532171, -45.21130890035909999, 144.1203871806729637 ) ) ;
#37556 = CARTESIAN_POINT ( 'NONE',  ( -7.205548786489490269E-13, 117.4749999999999943, 108.2293999999999983 ) ) ;
#37557 = CARTESIAN_POINT ( 'NONE',  ( 97.81503796907703929, -40.52560807623309813, 16.63632852797828221 ) ) ;
#37558 = VECTOR ( 'NONE', #40509, 1000.000000000000000 ) ;
#37559 = ORIENTED_EDGE ( 'NONE', *, *, #43340, .T. ) ;
#37560 = CIRCLE ( 'NONE', #62183, 1.000000000000000888 ) ;
#37561 = ORIENTED_EDGE ( 'NONE', *, *, #52564, .T. ) ;
#37562 = ORIENTED_EDGE ( 'NONE', *, *, #22033, .T. ) ;
#37563 = CARTESIAN_POINT ( 'NONE',  ( 107.4574165340472263, -45.37514529517124373, 190.4185665600669779 ) ) ;
#37564 = VECTOR ( 'NONE', #21928, 1000.000000000000000 ) ;
#37565 = CARTESIAN_POINT ( 'NONE',  ( 111.9392231810069944, -27.48808525092397304, 59.68991099019693536 ) ) ;
#37566 = EDGE_LOOP ( 'NONE', ( #8396, #49758, #20154, #54831 ) ) ;
#37567 = CARTESIAN_POINT ( 'NONE',  ( 101.1541078795467996, -28.12664281037970682, 50.55562527591095545 ) ) ;
#37568 = CARTESIAN_POINT ( 'NONE',  ( 0.000000000000000000, 61.59999999999999432, 0.000000000000000000 ) ) ;
#37569 = DIRECTION ( 'NONE',  ( 0.000000000000000000, 0.000000000000000000, 1.000000000000000000 ) ) ;
#37570 = CARTESIAN_POINT ( 'NONE',  ( 107.7349035034188489, -25.28961927740925830, 323.0034242383203491 ) ) ;
#37571 = CARTESIAN_POINT ( 'NONE',  ( 117.1259760753171548, -33.86829196857838298, 145.0470538473399529 ) ) ;
#37572 = CARTESIAN_POINT ( 'NONE',  ( 117.0718954846165616, -35.46248235265727544, 263.9272919428643718 ) ) ;
#37573 = ORIENTED_EDGE ( 'NONE', *, *, #66295, .F. ) ;
#37574 = AXIS2_PLACEMENT_3D ( 'NONE', #9264, #9707, #38292 ) ;
#37575 = FACE_OUTER_BOUND ( 'NONE', #3487, .T. ) ;
#37576 = ORIENTED_EDGE ( 'NONE', *, *, #45869, .F. ) ;
#37577 = CIRCLE ( 'NONE', #57864, 2.117000000000007987 ) ;
#37578 = DIRECTION ( 'NONE',  ( 0.000000000000000000, 0.000000000000000000, -1.000000000000000000 ) ) ;
#37579 = CARTESIAN_POINT ( 'NONE',  ( 91.91125933621933086, -96.68314769832132072, -19.26696060647622843 ) ) ;
#37580 = ORIENTED_EDGE ( 'NONE', *, *, #84154, .T. ) ;
#37581 = DIRECTION ( 'NONE',  ( 0.000000000000000000, 1.000000000000000000, 0.000000000000000000 ) ) ;
#37582 = CARTESIAN_POINT ( 'NONE',  ( 59.56670390244699576, -67.87844715994098976, 85.21780685541799016 ) ) ;
#37583 = CARTESIAN_POINT ( 'NONE',  ( 115.0227918137121037, -43.52084328818016701, 63.26419670448196797 ) ) ;
#37584 = DIRECTION ( 'NONE',  ( 4.194175870806139918E-14, -1.000000000000000000, 0.000000000000000000 ) ) ;
#37585 = EDGE_CURVE ( 'NONE', #5375, #20111, #32247, .T. ) ;
#37586 = LINE ( 'NONE', #57566, #7176 ) ;
#37587 = DIRECTION ( 'NONE',  ( -0.000000000000000000, 1.000000000000000000, 0.000000000000000000 ) ) ;
#37588 = ADVANCED_FACE ( 'NONE', ( #26342 ), #79399, .F. ) ;
#37589 = CARTESIAN_POINT ( 'NONE',  ( 117.3137205126584348, -38.32096045344801638, 68.69181575210198787 ) ) ;
#37591 = CARTESIAN_POINT ( 'NONE',  ( 113.5515132932710713, -44.90922781482908732, 164.1099109901969655 ) ) ;
#37590 = CARTESIAN_POINT ( 'NONE',  ( 182.3467384525658588, -36.02818131005238200, 237.4678068554150059 ) ) ;
#37592 = PLANE ( 'NONE',  #4497 ) ;
#37593 = CARTESIAN_POINT ( 'NONE',  ( 177.0371591254545649, -48.62818131005479927, 180.4678068554150059 ) ) ;
#37594 = ORIENTED_EDGE ( 'NONE', *, *, #54344, .F. ) ;
#37595 = CIRCLE ( 'NONE', #23092, 1.000000000000000888 ) ;
#37596 = LINE ( 'NONE', #78939, #30927 ) ;
#37597 = EDGE_CURVE ( 'NONE', #27593, #27929, #51789, .T. ) ;
#37598 = CARTESIAN_POINT ( 'NONE',  ( 60.32499999999999574, 82.54999999999999716, 335.3740053999999304 ) ) ;
#37599 = CYLINDRICAL_SURFACE ( 'NONE', #8197, 5.600000000000000533 ) ;
#37600 = EDGE_CURVE ( 'NONE', #51011, #73231, #78491, .T. ) ;
#37601 = DIRECTION ( 'NONE',  ( 0.000000000000000000, 1.000000000000000000, 0.000000000000000000 ) ) ;
#37603 = ORIENTED_EDGE ( 'NONE', *, *, #1386, .F. ) ;
#37602 = CARTESIAN_POINT ( 'NONE',  ( 96.63001237737263693, -35.53283987767252228, 206.2356252759109623 ) ) ;
#37604 = CARTESIAN_POINT ( 'NONE',  ( 97.12558495679242299, -37.99709113623088541, 146.4273255808599856 ) ) ;
#37605 = CARTESIAN_POINT ( 'NONE',  ( 112.6753912189806073, -45.54292608213916793, 259.0270538473393458 ) ) ;
#37606 = CARTESIAN_POINT ( 'NONE',  ( 100.2704505754038706, -46.49802187830721323, 83.09276813305294240 ) ) ;
#37607 = CARTESIAN_POINT ( 'NONE',  ( 98.35067263469487386, -31.65512584675276386, 251.9111731073708143 ) ) ;
#37608 = DIRECTION ( 'NONE',  ( 0.000000000000000000, 1.000000000000000000, 0.000000000000000000 ) ) ;
#37609 = AXIS2_PLACEMENT_3D ( 'NONE', #32037, #42421, #69708 ) ;
#37610 = CARTESIAN_POINT ( 'NONE',  ( 151.0667039024469886, -79.67844715994088745, 155.2178068554179902 ) ) ;
#37611 = CARTESIAN_POINT ( 'NONE',  ( 99.04399605877385682, -42.84115830957615145, 262.8440304599521369 ) ) ;
#37612 = EDGE_LOOP ( 'NONE', ( #55574, #4336, #45752, #76191 ) ) ;
#37613 = EDGE_CURVE ( 'NONE', #74740, #8011, #42628, .T. ) ;
#37614 = VERTEX_POINT ( 'NONE', #54908 ) ;
#37615 = EDGE_CURVE ( 'NONE', #73753, #75146, #55360, .T. ) ;
#37616 = VERTEX_POINT ( 'NONE', #48539 ) ;
#37617 = ORIENTED_EDGE ( 'NONE', *, *, #64091, .F. ) ;
#37618 = FACE_OUTER_BOUND ( 'NONE', #29207, .T. ) ;
#37619 = CARTESIAN_POINT ( 'NONE',  ( 101.0866664386429647, -45.26901348810219616, 278.0899109901965858 ) ) ;
#37620 = FACE_OUTER_BOUND ( 'NONE', #61966, .T. ) ;
#37621 = DIRECTION ( 'NONE',  ( 2.999999999999999839E-15, -1.000000000000000000, 2.999999999999999900E-30 ) ) ;
#37622 = EDGE_CURVE ( 'NONE', #47878, #67868, #35176, .T. ) ;
#37623 = AXIS2_PLACEMENT_3D ( 'NONE', #56120, #21649, #57030 ) ;
#37625 = CARTESIAN_POINT ( 'NONE',  ( 91.26337341211373655, 76.18740257834571139, 75.67519899969754249 ) ) ;
#37624 = CARTESIAN_POINT ( 'NONE',  ( 53.97500000000000142, 95.25000000000000000, 283.4005000000000223 ) ) ;
#37626 = CARTESIAN_POINT ( 'NONE',  ( 107.0664832912750057, -36.72944715993903486, 9.425625275910970657 ) ) ;
#37627 = CARTESIAN_POINT ( 'NONE',  ( 111.2765704384832759, -44.16122339008717290, 212.4095626852199530 ) ) ;
#37628 = EDGE_LOOP ( 'NONE', ( #30285, #10713, #79953, #48119 ) ) ;
#37629 = ORIENTED_EDGE ( 'NONE', *, *, #7761, .T. ) ;
#37630 = AXIS2_PLACEMENT_3D ( 'NONE', #81324, #61287, #88127 ) ;
#37632 = ORIENTED_EDGE ( 'NONE', *, *, #52901, .T. ) ;
#37631 = AXIS2_PLACEMENT_3D ( 'NONE', #65903, #88610, #4585 ) ;
#37633 = FACE_BOUND ( 'NONE', #6514, .T. ) ;
#37634 = CARTESIAN_POINT ( 'NONE',  ( 97.81361814658107789, -40.52213659492726805, 181.6360300764658291 ) ) ;
#37635 = CARTESIAN_POINT ( 'NONE',  ( 99.87094702832897042, -29.26198151734326203, 261.6746728949581779 ) ) ;
#37636 = CARTESIAN_POINT ( 'NONE',  ( 107.0664832912739399, -36.72944715994095333, 302.6356252759109680 ) ) ;
#37637 = AXIS2_PLACEMENT_3D ( 'NONE', #36182, #85253, #8941 ) ;
#37638 = CARTESIAN_POINT ( 'NONE',  ( 142.0664832912740394, -46.72944715994099596, -5.074374724088994704 ) ) ;
#37639 = PLANE ( 'NONE',  #54703 ) ;
#37640 = VERTEX_POINT ( 'NONE', #85803 ) ;
#37641 = CARTESIAN_POINT ( 'NONE',  ( 99.09473700806925933, -30.55172784210162362, 56.80234965928513446 ) ) ;
#37642 = ORIENTED_EDGE ( 'NONE', *, *, #19847, .T. ) ;
#37643 = EDGE_CURVE ( 'NONE', #52987, #17905, #77629, .T. ) ;
#37644 = CARTESIAN_POINT ( 'NONE',  ( -3.175000000000109956, 104.3431970271541900, 31.75000000000000000 ) ) ;
#37645 = CARTESIAN_POINT ( 'NONE',  ( 98.93870468184483968, -41.20551083899233902, 24.54523322673496466 ) ) ;
#37646 = CARTESIAN_POINT ( 'NONE',  ( 172.5664832912729878, -18.82844715994071194, 78.92562527591199739 ) ) ;
#37647 = DIRECTION ( 'NONE',  ( 0.000000000000000000, 0.000000000000000000, 1.000000000000000000 ) ) ;
#37648 = AXIS2_PLACEMENT_3D ( 'NONE', #32531, #10752, #11204 ) ;
#37649 = DIRECTION ( 'NONE',  ( 1.000000000000000000, 4.163336342344333240E-14, 0.000000000000000000 ) ) ;
#37650 = VERTEX_POINT ( 'NONE', #78089 ) ;
#37651 = DIRECTION ( 'NONE',  ( 0.8543009526837940237, 0.03605348183280988883, -0.5185267868599396923 ) ) ;
#37652 = FACE_OUTER_BOUND ( 'NONE', #22380, .T. ) ;
#37653 = ORIENTED_EDGE ( 'NONE', *, *, #38599, .F. ) ;
#37654 = CARTESIAN_POINT ( 'NONE',  ( 98.85774631673514534, -43.21346936515602266, 91.85848241876892928 ) ) ;
#37655 = ORIENTED_EDGE ( 'NONE', *, *, #84824, .F. ) ;
#37656 = B_SPLINE_CURVE_WITH_KNOTS ( 'NONE', 3,
 ( #48348, #47010, #82029, #13861, #26588, #76084 ),
 .UNSPECIFIED., .F., .F.,
 ( 4, 2, 4 ),
 ( 0.000000000000000000, 0.0009145665419566550210, 0.001828735834957770194 ),
 .UNSPECIFIED. ) ;
#37657 = CARTESIAN_POINT ( 'NONE',  ( 115.6047007430436366, -36.96391350797230757, 43.22670554236196239 ) ) ;
#37658 = DIRECTION ( 'NONE',  ( 1.000000000000000078E-15, 0.000000000000000000, -1.000000000000000000 ) ) ;
#37659 = CARTESIAN_POINT ( 'NONE',  ( 110.2353755222631833, -45.00509823041481638, 59.29872616303999422 ) ) ;
#37660 = EDGE_CURVE ( 'NONE', #27566, #79794, #15854, .T. ) ;
#37661 = DIRECTION ( 'NONE',  ( 2.900000000000000265E-14, -2.000000000000000155E-15, 1.000000000000000000 ) ) ;
#37662 = CARTESIAN_POINT ( 'NONE',  ( 96.67439905703393777, -115.7784471599421323, -21.78219314458165812 ) ) ;
#37663 = CARTESIAN_POINT ( 'NONE',  ( 89.89934876040919676, -68.97671693066587295, 247.5435304005999910 ) ) ;
#37664 = CIRCLE ( 'NONE', #7189, 4.762500000000002842 ) ;
#37665 = CARTESIAN_POINT ( 'NONE',  ( 107.6079817216441796, -48.59237387041279987, 38.61276813305397582 ) ) ;
#37666 = CARTESIAN_POINT ( 'NONE',  ( 51.24204729617298426, -31.76306994223730840, -5.074374724088000832 ) ) ;
#37667 = ORIENTED_EDGE ( 'NONE', *, *, #4534, .T. ) ;
#37668 = EDGE_CURVE ( 'NONE', #8698, #86124, #43534, .T. ) ;
#37669 = FACE_OUTER_BOUND ( 'NONE', #15844, .T. ) ;
#37670 = EDGE_LOOP ( 'NONE', ( #8216, #71112, #18142, #41428 ) ) ;
#37671 = CARTESIAN_POINT ( 'NONE',  ( 107.6554453082189013, -47.17114389581161049, 148.6213395616249784 ) ) ;
#37672 = DIRECTION ( 'NONE',  ( -4.237773401492740281E-14, 1.000000000000000000, 0.000000000000000000 ) ) ;
#37673 = EDGE_LOOP ( 'NONE', ( #6687, #13428, #79553, #336 ) ) ;
#37674 = ORIENTED_EDGE ( 'NONE', *, *, #260, .T. ) ;
#37676 = AXIS2_PLACEMENT_3D ( 'NONE', #28347, #36531, #42416 ) ;
#37675 = CARTESIAN_POINT ( 'NONE',  ( 162.0667039024469886, -67.87844715994089029, 222.2178068554179902 ) ) ;
#37677 = LINE ( 'NONE', #65377, #27500 ) ;
#37678 = CARTESIAN_POINT ( 'NONE',  ( 104.3638673426610666, -27.29495504168057707, 225.2984824187689981 ) ) ;
#37679 = DIRECTION ( 'NONE',  ( 8.881784197001252323E-16, 0.000000000000000000, -1.000000000000000000 ) ) ;
#37680 = CARTESIAN_POINT ( 'NONE',  ( 145.5504341359485636, -139.1947169264394120, 246.0943807925750093 ) ) ;
#37681 = CARTESIAN_POINT ( 'NONE',  ( 124.0667039024470313, -106.9675116026789254, -9.937637710809946512 ) ) ;
#37682 = CARTESIAN_POINT ( 'NONE',  ( 99.12745497205600032, -44.42007846243786418, 37.95086337114900488 ) ) ;
#37683 = DIRECTION ( 'NONE',  ( 0.000000000000000000, -1.000000000000000000, 0.000000000000000000 ) ) ;
#37684 = ORIENTED_EDGE ( 'NONE', *, *, #83337, .F. ) ;
#37685 = CARTESIAN_POINT ( 'NONE',  ( 97.07202416812739898, -35.37890067388282489, 172.2189264459942990 ) ) ;
#37686 = AXIS2_PLACEMENT_3D ( 'NONE', #46516, #48296, #41492 ) ;
#37687 = DIRECTION ( 'NONE',  ( 1.000000000000000078E-15, -1.000000000000000083E-30, -1.000000000000000000 ) ) ;
#37688 = VERTEX_POINT ( 'NONE', #86234 ) ;
#37689 = AXIS2_PLACEMENT_3D ( 'NONE', #42804, #77348, #8313 ) ;
#37690 = AXIS2_PLACEMENT_3D ( 'NONE', #4256, #54156, #81917 ) ;
#37691 = DIRECTION ( 'NONE',  ( 0.3535533905932745080, -0.6123724356957719328, 0.7071067811865667796 ) ) ;
#37692 = CARTESIAN_POINT ( 'NONE',  ( 118.5667039024470313, -104.2784471599408533, 19.21780685541799016 ) ) ;
#37693 = CARTESIAN_POINT ( 'NONE',  ( 98.85650974919595058, -29.36329775763224603, 235.7565776568629872 ) ) ;
#37694 = CYLINDRICAL_SURFACE ( 'NONE', #32728, 7.143750000000004263 ) ;
#37695 = EDGE_CURVE ( 'NONE', #37421, #30351, #50350, .T. ) ;
#37696 = CARTESIAN_POINT ( 'NONE',  ( 107.0667039024479834, -67.87844715994100397, 160.9178068554150229 ) ) ;
#37697 = DIRECTION ( 'NONE',  ( 0.000000000000000000, 0.000000000000000000, 1.000000000000000000 ) ) ;
#37698 = ADVANCED_FACE ( 'NONE', ( #36294 ), #72608, .T. ) ;
#37699 = CARTESIAN_POINT ( 'NONE',  ( 113.8843833678302389, -31.58431642611541434, 218.7638483995049796 ) ) ;
#37701 = CARTESIAN_POINT ( 'NONE',  ( 99.31004196827758790, -43.71529311364903947, 52.90991099019698396 ) ) ;
#37700 = CARTESIAN_POINT ( 'NONE',  ( -24.20305689751608824, 64.60000000000000853, 58.62596543806478877 ) ) ;
#37702 = CARTESIAN_POINT ( 'NONE',  ( 121.3880544210665988, 74.44113218321618319, 48.06552997551920470 ) ) ;
#37703 = CARTESIAN_POINT ( 'NONE',  ( 97.94803474170373647, -41.87343025248883777, 136.7356252759109623 ) ) ;
#37704 = ORIENTED_EDGE ( 'NONE', *, *, #48226, .F. ) ;
#37705 = DIRECTION ( 'NONE',  ( 0.7071067811865491270, -0.7071067811865459074, 7.071067811865492096E-16 ) ) ;
#37706 = ORIENTED_EDGE ( 'NONE', *, *, #58306, .F. ) ;
#37707 = AXIS2_PLACEMENT_3D ( 'NONE', #31956, #46007, #60544 ) ;
#37708 = DIRECTION ( 'NONE',  ( -0.8660254037844392627, 0.4999999999999990008, -1.549999999999999706E-14 ) ) ;
#37709 = EDGE_CURVE ( 'NONE', #66435, #29549, #8597, .T. ) ;
#37710 = CARTESIAN_POINT ( 'NONE',  ( 102.0670549289058471, -27.97049807668956944, 66.48979194539977300 ) ) ;
#37711 = AXIS2_PLACEMENT_3D ( 'NONE', #24093, #15938, #51764 ) ;
#37712 = DIRECTION ( 'NONE',  ( 1.000000000000000078E-15, 1.000000000000000083E-30, -1.000000000000000000 ) ) ;
#37713 = VERTEX_POINT ( 'NONE', #78980 ) ;
#37714 = DIRECTION ( 'NONE',  ( 0.8660254037844392627, -0.4999999999999990008, 1.549999999999999706E-14 ) ) ;
#37715 = ADVANCED_FACE ( 'NONE', ( #24011 ), #37639, .T. ) ;
#37716 = EDGE_LOOP ( 'NONE', ( #22758, #23385, #70623, #49576 ) ) ;
#37717 = CARTESIAN_POINT ( 'NONE',  ( 179.7974245136208538, -36.32844715993469009, 237.4678068554150059 ) ) ;
#37718 = CIRCLE ( 'NONE', #82657, 2.029999999999997140 ) ;
#37719 = CARTESIAN_POINT ( 'NONE',  ( 142.8698897858160706, -0.9167816978817300289, 394.9756252759100903 ) ) ;
#37720 = CARTESIAN_POINT ( 'NONE',  ( 184.3595971212628228, -48.62134037874749737, 300.4678068554149490 ) ) ;
#37721 = EDGE_LOOP ( 'NONE', ( #23153, #201, #54039, #62292 ) ) ;
#37722 = EDGE_CURVE ( 'NONE', #45890, #7448, #85091, .T. ) ;
#37723 = CARTESIAN_POINT ( 'NONE',  ( 98.31770816264274515, -42.43955203770550355, 101.7870538473399620 ) ) ;
#37724 = DIRECTION ( 'NONE',  ( 0.000000000000000000, 0.000000000000000000, 1.000000000000000000 ) ) ;
#37725 = CYLINDRICAL_SURFACE ( 'NONE', #3155, 0.2500000000000039968 ) ;
#37726 = DIRECTION ( 'NONE',  ( 0.000000000000000000, 0.000000000000000000, 1.000000000000000000 ) ) ;
#37727 = ORIENTED_EDGE ( 'NONE', *, *, #26301, .T. ) ;
#37728 = EDGE_CURVE ( 'NONE', #26842, #84840, #70820, .T. ) ;
#37729 = VECTOR ( 'NONE', #6975, 1000.000000000000000 ) ;
#37730 = CARTESIAN_POINT ( 'NONE',  ( 173.9899999999999807, 52.73749999999999716, -36.61250000000000426 ) ) ;
#37731 = CARTESIAN_POINT ( 'NONE',  ( 177.0371591254543659, -48.62818131005480637, 249.9678068554149775 ) ) ;
#37732 = CARTESIAN_POINT ( 'NONE',  ( 141.8164832912740110, -45.62589376934770513, 14.92562527591100618 ) ) ;
#37734 = CARTESIAN_POINT ( 'NONE',  ( -479.3614999999999782, 89.53805401447691281, 18.25625000000039933 ) ) ;
#37733 = CARTESIAN_POINT ( 'NONE',  ( 31.75000000000000000, 69.84999999999999432, 346.0750000000000455 ) ) ;
#37735 = CYLINDRICAL_SURFACE ( 'NONE', #42231, 2.030000000001310312 ) ;
#37736 = AXIS2_PLACEMENT_3D ( 'NONE', #74504, #38633, #80894 ) ;
#37737 = VERTEX_POINT ( 'NONE', #44881 ) ;
#37738 = DIRECTION ( 'NONE',  ( 1.000000000000000078E-15, -1.000000000000000000, 0.000000000000000000 ) ) ;
#37739 = CARTESIAN_POINT ( 'NONE',  ( 116.7860849611260647, -31.33117650353040062, 175.2299109901959753 ) ) ;
#37741 = VERTEX_POINT ( 'NONE', #23134 ) ;
#37740 = DIRECTION ( 'NONE',  ( 0.000000000000000000, 0.000000000000000000, -1.000000000000000000 ) ) ;
#37742 = CARTESIAN_POINT ( 'NONE',  ( 99.63325261332707328, -43.08637385293071276, 27.88991099019594344 ) ) ;
#37743 = DIRECTION ( 'NONE',  ( -0.7071067811874389708, 0.7071067811856560636, 0.000000000000000000 ) ) ;
#37744 = CARTESIAN_POINT ( 'NONE',  ( 75.31670390244798341, -57.40094715994099772, 37.63480685541480852 ) ) ;
#37745 = DIRECTION ( 'NONE',  ( 0.000000000000000000, -1.000000000000000000, 0.000000000000000000 ) ) ;
#37746 = VECTOR ( 'NONE', #15050, 1000.000000000000114 ) ;
#37747 = ORIENTED_EDGE ( 'NONE', *, *, #3074, .F. ) ;
#37748 = CARTESIAN_POINT ( 'NONE',  ( 41.56648329127399677, -18.82844715994099971, 136.8086252759119645 ) ) ;
#37749 = ORIENTED_EDGE ( 'NONE', *, *, #72053, .F. ) ;
#37750 = ORIENTED_EDGE ( 'NONE', *, *, #29084, .F. ) ;
#37751 = EDGE_CURVE ( 'NONE', #27014, #11575, #83722, .T. ) ;
#37752 = CARTESIAN_POINT ( 'NONE',  ( 110.1519232268686181, -46.31854332990749867, 204.2558690201829847 ) ) ;
#37753 = AXIS2_PLACEMENT_3D ( 'NONE', #37582, #11201, #17580 ) ;
#37754 = CYLINDRICAL_SURFACE ( 'NONE', #58869, 3.000000000000002665 ) ;
#37755 = CARTESIAN_POINT ( 'NONE',  ( 110.0319707555399447, -45.11204900458633915, 34.27872616304095033 ) ) ;
#37756 = CARTESIAN_POINT ( 'NONE',  ( 23.12955879343030574, 87.00686711072398793, 301.2092494891036267 ) ) ;
#37757 = DIRECTION ( 'NONE',  ( 1.000000000000000000, 4.299999999999999979E-14, 1.000000000000000078E-15 ) ) ;
#37758 = VECTOR ( 'NONE', #47806, 1000.000000000000000 ) ;
#37759 = DIRECTION ( 'NONE',  ( 0.8571673007021091140, -8.250245410175212261E-16, 0.5150380749100597066 ) ) ;
#37760 = VERTEX_POINT ( 'NONE', #65766 ) ;
#37761 = CARTESIAN_POINT ( 'NONE',  ( 21.03715912545738220, -47.82818131006197149, 193.9678068554150627 ) ) ;
#37762 = DIRECTION ( 'NONE',  ( -0.7071067811855900054, -0.7071067811875051401, 0.000000000000000000 ) ) ;
#37763 = ORIENTED_EDGE ( 'NONE', *, *, #27973, .T. ) ;
#37764 = CARTESIAN_POINT ( 'NONE',  ( 118.6297112294784029, -39.20734283244436114, 258.6584824187679033 ) ) ;
#37765 = CARTESIAN_POINT ( 'NONE',  ( 2.881808223710723649, 94.92563399540007651, 118.5216647685501670 ) ) ;
#37766 = VERTEX_POINT ( 'NONE', #37189 ) ;
#37767 = FILL_AREA_STYLE_COLOUR ( '', #40131 ) ;
#37768 = DIRECTION ( 'NONE',  ( 1.000000000000000078E-15, -1.000000000000000083E-30, -1.000000000000000000 ) ) ;
#37769 = CIRCLE ( 'NONE', #39180, 7.499999999999996447 ) ;
#37770 = CARTESIAN_POINT ( 'NONE',  ( 182.2420472961722737, -31.76306994223702418, 342.9256252759109884 ) ) ;
#37771 = DIRECTION ( 'NONE',  ( 0.000000000000000000, 0.000000000000000000, 1.000000000000000000 ) ) ;
#37772 = CARTESIAN_POINT ( 'NONE',  ( 109.3463552500793554, -26.51205201248422583, 220.9013395616249795 ) ) ;
#37773 = CARTESIAN_POINT ( 'NONE',  ( 6.314153984315725943, 71.61522187350405488, 118.1894436584348824 ) ) ;
#37774 = ORIENTED_EDGE ( 'NONE', *, *, #72997, .F. ) ;
#37775 = EDGE_CURVE ( 'NONE', #35252, #57634, #43080, .T. ) ;
#37776 = CARTESIAN_POINT ( 'NONE',  ( 104.7259408665080116, -47.57930243624250721, 28.41943479971997988 ) ) ;
#37777 = PLANE ( 'NONE',  #43923 ) ;
#37778 = CARTESIAN_POINT ( 'NONE',  ( 110.8926993666852496, -26.99363814275770679, 269.7784824187681920 ) ) ;
#37779 = ORIENTED_EDGE ( 'NONE', *, *, #42893, .F. ) ;
#37780 = AXIS2_PLACEMENT_3D ( 'NONE', #89288, #76091, #70173 ) ;
#37781 = CARTESIAN_POINT ( 'NONE',  ( 78.21292805806618276, -38.76093376056942930, 7.655955902689210113 ) ) ;
#37782 = CARTESIAN_POINT ( 'NONE',  ( 115.7840071928116004, -41.80079596848010937, 19.40698120903841684 ) ) ;
#37783 = DIRECTION ( 'NONE',  ( -1.000000000000000000, 0.000000000000000000, 0.000000000000000000 ) ) ;
#37784 = CARTESIAN_POINT ( 'NONE',  ( 113.4089301560035068, -41.86784124614906233, 86.10237608387694763 ) ) ;
#37785 = CARTESIAN_POINT ( 'NONE',  ( 117.7987307161850907, -31.64603138916173464, 210.1784824187679703 ) ) ;
#37786 = DIRECTION ( 'NONE',  ( 0.7071067811865524577, 0.000000000000000000, 0.7071067811865425767 ) ) ;
#37787 = ORIENTED_EDGE ( 'NONE', *, *, #36415, .T. ) ;
#37788 = CARTESIAN_POINT ( 'NONE',  ( 0.000000000000000000, 92.07499999999998863, 0.000000000000000000 ) ) ;
#37789 = CIRCLE ( 'NONE', #10234, 6.571100913904384555 ) ;
#37790 = ORIENTED_EDGE ( 'NONE', *, *, #6036, .F. ) ;
#37791 = VERTEX_POINT ( 'NONE', #3114 ) ;
#37792 = DIRECTION ( 'NONE',  ( 8.659560562354778784E-17, 0.7071067811865600072, -0.7071067811865350272 ) ) ;
#37793 = ORIENTED_EDGE ( 'NONE', *, *, #84660, .T. ) ;
#37794 = EDGE_LOOP ( 'NONE', ( #13044, #10727, #41515, #46809 ) ) ;
#37795 = CARTESIAN_POINT ( 'NONE',  ( 108.3349140068648637, -46.73468863093219738, 168.6781975528624002 ) ) ;
#37796 = B_SPLINE_CURVE_WITH_KNOTS ( 'NONE', 3,
 ( #7778, #12923, #20183, #33800, #64537, #43173, #63185, #29122, #962, #63638, #54211, #89226, #84554, #15945, #19720, #22768, #82422, #49086 ),
 .UNSPECIFIED., .F., .F.,
 ( 4, 2, 2, 2, 2, 2, 2, 2, 4 ),
 ( 0.000000000000000000, 0.06249999972775545365, 0.1249999994555109073, 0.1874999991832663748, 0.2499999989110218146, 0.3124999986387772544, 0.3749999983665327496, 0.4374999980942881894, 0.4999999978220436292 ),
 .UNSPECIFIED. ) ;
#37797 = CARTESIAN_POINT ( 'NONE',  ( 97.39129913838408470, -39.27854586558702721, 42.53143958753435783 ) ) ;
#37798 = EDGE_CURVE ( 'NONE', #33917, #14322, #86649, .T. ) ;
#37799 = CARTESIAN_POINT ( 'NONE',  ( 108.0930535991856800, -45.20896867503704897, 117.0952769709339663 ) ) ;
#37800 = CARTESIAN_POINT ( 'NONE',  ( 96.67081033544403113, -37.96906397156782731, 41.42133956162496844 ) ) ;
#37801 = EDGE_CURVE ( 'NONE', #73518, #33311, #31501, .T. ) ;
#37802 = CARTESIAN_POINT ( 'NONE',  ( -10.09455232642977052, 74.79837219561763106, 130.1659940687516723 ) ) ;
#37803 = EDGE_CURVE ( 'NONE', #58395, #55190, #26708, .T. ) ;
#37804 = ORIENTED_EDGE ( 'NONE', *, *, #27560, .T. ) ;
#37805 = AXIS2_PLACEMENT_3D ( 'NONE', #60382, #39505, #26325 ) ;
#37806 = CARTESIAN_POINT ( 'NONE',  ( 97.53181971261398076, -39.74887774678698804, 137.5705102554088626 ) ) ;
#37807 = EDGE_CURVE ( 'NONE', #64886, #2396, #40342, .T. ) ;
#37808 = ORIENTED_EDGE ( 'NONE', *, *, #64836, .F. ) ;
#37809 = CYLINDRICAL_SURFACE ( 'NONE', #68227, 4.762500000000002842 ) ;
#37810 = LINE ( 'NONE', #59565, #29984 ) ;
#37811 = CARTESIAN_POINT ( 'NONE',  ( 1.166476076187854022E-15, 12.27000000000000313, 9.525000000000000355 ) ) ;
#37812 = VECTOR ( 'NONE', #19590, 1000.000000000000000 ) ;
#37813 = CARTESIAN_POINT ( 'NONE',  ( 99.99420790045508056, -28.96206233275049158, 285.6641967044822650 ) ) ;
#37814 = ORIENTED_EDGE ( 'NONE', *, *, #27308, .F. ) ;
#37815 = UNCERTAINTY_MEASURE_WITH_UNIT (LENGTH_MEASURE( 1.000000000000000082E-05 ), #41919, 'distance_accuracy_value', 'NONE');
#37816 = CARTESIAN_POINT ( 'NONE',  ( 112.6638099339533028, -45.52472799210174514, 263.0270538473394595 ) ) ;
#37817 = CARTESIAN_POINT ( 'NONE',  ( 100.5235407922616133, -27.76354498484767674, 26.56610146638793779 ) ) ;
#37818 = CARTESIAN_POINT ( 'NONE',  ( 105.7154773228390781, -46.72385839126379636, 118.4689586086422253 ) ) ;
#37820 = CARTESIAN_POINT ( 'NONE',  ( 69.57274467425236253, -138.4326786319161329, 247.5388220368722045 ) ) ;
#37819 = CARTESIAN_POINT ( 'NONE',  ( 134.0664832912740110, -46.72944715994100306, -0.5743747240890021422 ) ) ;
#37821 = DIRECTION ( 'NONE',  ( -0.7071067811864676367, -0.7071067811866273978, -7.071067811864669709E-16 ) ) ;
#37822 = DIRECTION ( 'NONE',  ( 2.761895400282000234E-15, 0.000000000000000000, 1.000000000000000000 ) ) ;
#37823 = DIRECTION ( 'NONE',  ( 0.000000000000000000, 0.000000000000000000, -1.000000000000000000 ) ) ;
#37824 = EDGE_CURVE ( 'NONE', #81352, #26573, #18415, .T. ) ;
#37825 = VECTOR ( 'NONE', #26824, 1000.000000000000000 ) ;
#37826 = EDGE_CURVE ( 'NONE', #18319, #14989, #12656, .T. ) ;
#37827 = LINE ( 'NONE', #45061, #85175 ) ;
#37828 = B_SPLINE_CURVE_WITH_KNOTS ( 'NONE', 3,
 ( #44277, #73785, #86542, #9781 ),
 .UNSPECIFIED., .F., .F.,
 ( 4, 4 ),
 ( -0.3438257506183129975, -0.1481392554759810298 ),
 .UNSPECIFIED. ) ;
#37829 = FACE_BOUND ( 'NONE', #82975, .T. ) ;
#37830 = CARTESIAN_POINT ( 'NONE',  ( 50.06333974046790303, 82.54999999999999716, 344.4418053999999643 ) ) ;
#37831 = CARTESIAN_POINT ( 'NONE',  ( 104.2289649446409783, -46.80690502001216657, 22.35848241876792031 ) ) ;
#37832 = CARTESIAN_POINT ( 'NONE',  ( 96.65005459693196599, -37.15429219901626823, 157.3584824187679487 ) ) ;
#37833 = CARTESIAN_POINT ( 'NONE',  ( 96.17045672112728028, -38.71987694442820782, 47.48229194257797303 ) ) ;
#37835 = CARTESIAN_POINT ( 'NONE',  ( 151.0371591254573218, -24.95799193692592866, 300.4678068554149490 ) ) ;
#37834 = DIRECTION ( 'NONE',  ( -1.000000000000000000, 0.000000000000000000, 0.000000000000000000 ) ) ;
#37836 = CARTESIAN_POINT ( 'NONE',  ( 82.57637212003993454, -35.60518726036713133, 2.783021291302837152 ) ) ;
#37837 = ORIENTED_EDGE ( 'NONE', *, *, #85582, .F. ) ;
#37838 = CARTESIAN_POINT ( 'NONE',  ( 98.34985896129799698, -31.65658472717509397, 186.9064586016984038 ) ) ;
#37839 = ORIENTED_EDGE ( 'NONE', *, *, #38532, .T. ) ;
#37840 = AXIS2_PLACEMENT_3D ( 'NONE', #76429, #69174, #84616 ) ;
#37841 = CARTESIAN_POINT ( 'NONE',  ( 109.7352083718000131, -46.17358189742679286, 68.79562527591099297 ) ) ;
#37843 = ORIENTED_EDGE ( 'NONE', *, *, #72446, .F. ) ;
#37842 = CARTESIAN_POINT ( 'NONE',  ( 6.884321588596717945, 93.22247119488908140, 130.3743772813626549 ) ) ;
#37844 = AXIS2_PLACEMENT_3D ( 'NONE', #41940, #56924, #36503 ) ;
#37845 = CARTESIAN_POINT ( 'NONE',  ( 134.0664832912740110, -46.72944715994100306, -0.8743747240890020755 ) ) ;
#37846 = CARTESIAN_POINT ( 'NONE',  ( 114.7977927517517855, -29.71579763117551565, 205.4127681330539872 ) ) ;
#37847 = DIRECTION ( 'NONE',  ( 0.000000000000000000, -1.000000000000000000, 0.000000000000000000 ) ) ;
#37848 = LINE ( 'NONE', #78310, #79176 ) ;
#37849 = CARTESIAN_POINT ( 'NONE',  ( 50.56670390244699576, -18.82844715994031048, 335.8680179914122732 ) ) ;
#37850 = CIRCLE ( 'NONE', #1808, 2.500000000000002220 ) ;
#37851 = DIRECTION ( 'NONE',  ( 1.000000000000000000, 0.000000000000000000, 0.000000000000000000 ) ) ;
#37852 = FACE_BOUND ( 'NONE', #28837, .T. ) ;
#37853 = CARTESIAN_POINT ( 'NONE',  ( 99.50454240397225192, -43.30556165129220858, 96.89604753381240698 ) ) ;
#37854 = CARTESIAN_POINT ( 'NONE',  ( 102.5967720069230324, -27.99243076246517603, 120.4527681330539792 ) ) ;
#37855 = VERTEX_POINT ( 'NONE', #12202 ) ;
#37856 = ORIENTED_EDGE ( 'NONE', *, *, #41781, .F. ) ;
#37857 = EDGE_CURVE ( 'NONE', #17090, #39460, #83053, .T. ) ;
#37858 = CARTESIAN_POINT ( 'NONE',  ( 116.2543158056996333, -38.69420140005939857, 105.1025356868499614 ) ) ;
#37859 = AXIS2_PLACEMENT_3D ( 'NONE', #37332, #50045, #79578 ) ;
#37860 = CARTESIAN_POINT ( 'NONE',  ( 68.06670390244705970, -121.7784471599409954, 55.21780685541800437 ) ) ;
#37862 = CARTESIAN_POINT ( 'NONE',  ( -6.706703101270981046E-13, 127.0000000000000000, 96.04375000000000284 ) ) ;
#37861 = CARTESIAN_POINT ( 'NONE',  ( 101.7545977962314652, -44.98157700518526525, 218.1213395616249784 ) ) ;
#37863 = LINE ( 'NONE', #71942, #53578 ) ;
#37865 = EDGE_CURVE ( 'NONE', #12019, #19567, #88955, .T. ) ;
#37864 = CARTESIAN_POINT ( 'NONE',  ( 97.06107378353082993, -37.99643432997152814, 112.4278404525605737 ) ) ;
#37866 = CARTESIAN_POINT ( 'NONE',  ( 118.4576332894986734, 70.80054595721395572, -4.873637472994857056 ) ) ;
#37867 = DIRECTION ( 'NONE',  ( 0.000000000000000000, 0.000000000000000000, 1.000000000000000000 ) ) ;
#37868 = CARTESIAN_POINT ( 'NONE',  ( -69.72411017812909506, 127.0000000000000000, -69.72411017813089984 ) ) ;
#37869 = LINE ( 'NONE', #71509, #24089 ) ;
#37870 = CARTESIAN_POINT ( 'NONE',  ( 97.81366378802354689, -42.73395665195503312, 146.7965776568629508 ) ) ;
#37871 = EDGE_LOOP ( 'NONE', ( #50782, #81355, #10902, #24839 ) ) ;
#37872 = ORIENTED_EDGE ( 'NONE', *, *, #11566, .F. ) ;
#37873 = CIRCLE ( 'NONE', #88650, 2.517500000000005844 ) ;
#37874 = CARTESIAN_POINT ( 'NONE',  ( 97.08661802161040555, -77.52859162019140626, 250.2201230397200220 ) ) ;
#37875 = CARTESIAN_POINT ( 'NONE',  ( 113.2454987164303901, -28.75867296000128093, 150.5522919406864162 ) ) ;
#37876 = CARTESIAN_POINT ( 'NONE',  ( 120.2221484686747317, -111.8737466215625602, -11.78219314458178779 ) ) ;
#37877 = CARTESIAN_POINT ( 'NONE',  ( 97.81820226091151937, -40.53330621887679541, 102.6369915585742092 ) ) ;
#37878 = EDGE_CURVE ( 'NONE', #66869, #10930, #1582, .T. ) ;
#37879 = CARTESIAN_POINT ( 'NONE',  ( 112.0659024056236603, -45.48840166505959104, 268.9897911008726510 ) ) ;
#37880 = CARTESIAN_POINT ( 'NONE',  ( 117.0684261367714072, -39.67022423017687771, 183.5984824187679578 ) ) ;
#37881 = CARTESIAN_POINT ( 'NONE',  ( 135.4471649165523672, -39.11090284777271364, 7.925007058950424010 ) ) ;
#37882 = ORIENTED_EDGE ( 'NONE', *, *, #28768, .F. ) ;
#37884 = ORIENTED_EDGE ( 'NONE', *, *, #74918, .T. ) ;
#37883 = ORIENTED_EDGE ( 'NONE', *, *, #1621, .F. ) ;
#37885 = AXIS2_PLACEMENT_3D ( 'NONE', #85740, #72970, #58880 ) ;
#37886 = CARTESIAN_POINT ( 'NONE',  ( 98.82648729870214765, -42.42054397291916956, 62.80801425164322893 ) ) ;
#37887 = LINE ( 'NONE', #58752, #1384 ) ;
#37888 = CARTESIAN_POINT ( 'NONE',  ( 131.9645448811436950, -34.94667115357206910, 7.474641677891152192 ) ) ;
#37889 = AXIS2_PLACEMENT_3D ( 'NONE', #40808, #82627, #81727 ) ;
#37890 = CARTESIAN_POINT ( 'NONE',  ( 98.69997382787508400, -39.74003663468293013, 263.0330118773257482 ) ) ;
#37891 = ADVANCED_FACE ( 'NONE', ( #62130 ), #75325, .F. ) ;
#37892 = CARTESIAN_POINT ( 'NONE',  ( 80.06648329127402519, -46.72944715994105991, 4.925625275910944012 ) ) ;
#37893 = ORIENTED_EDGE ( 'NONE', *, *, #80306, .T. ) ;
#37894 = CARTESIAN_POINT ( 'NONE',  ( 111.4380389023045552, -44.06754350613674376, 9.635625275910941312 ) ) ;
#37895 = CARTESIAN_POINT ( 'NONE',  ( 188.5667039024486087, -48.82844715993430640, 137.2178068554150059 ) ) ;
#37896 = ORIENTED_EDGE ( 'NONE', *, *, #7663, .F. ) ;
#37897 = ORIENTED_EDGE ( 'NONE', *, *, #6613, .F. ) ;
#37898 = CARTESIAN_POINT ( 'NONE',  ( 110.8587645964465338, -45.98247965540819848, 112.8859944073334844 ) ) ;
#37899 = ORIENTED_EDGE ( 'NONE', *, *, #23966, .F. ) ;
#37900 = ORIENTED_EDGE ( 'NONE', *, *, #84779, .F. ) ;
#37901 = CARTESIAN_POINT ( 'NONE',  ( 115.5202298134134367, -37.95022619834508504, 28.13527697093398672 ) ) ;
#37902 = CARTESIAN_POINT ( 'NONE',  ( 104.5572623809163701, -48.33710955716689028, 182.4070538473399665 ) ) ;
#37903 = VECTOR ( 'NONE', #82768, 1000.000000000000000 ) ;
#37904 = CARTESIAN_POINT ( 'NONE',  ( 117.1049515565469221, -33.87427183379790563, 149.0470538473389581 ) ) ;
#37905 = CARTESIAN_POINT ( 'NONE',  ( 48.79742451361996558, -36.32844715994077944, 117.4678068554150485 ) ) ;
#37906 = CARTESIAN_POINT ( 'NONE',  ( 100.1387811872355371, -44.51978932219680019, 262.9984824187678782 ) ) ;
#37907 = DIRECTION ( 'NONE',  ( -1.000000000000000000, -1.206764157201257538E-15, 0.000000000000000000 ) ) ;
#37908 = ADVANCED_FACE ( 'NONE', ( #83481 ), #89409, .F. ) ;
#37909 = CARTESIAN_POINT ( 'NONE',  ( -130.5150461639146044, 70.27756284692560484, -3.294108455003483815 ) ) ;
#37910 = ORIENTED_EDGE ( 'NONE', *, *, #19643, .T. ) ;
#37911 = EDGE_LOOP ( 'NONE', ( #57408, #20507, #75097, #69372, #40865, #48214, #44398, #87942 ) ) ;
#37912 = AXIS2_PLACEMENT_3D ( 'NONE', #58150, #71790, #78176 ) ;
#37913 = VECTOR ( 'NONE', #43127, 1000.000000000000000 ) ;
#37914 = CARTESIAN_POINT ( 'NONE',  ( 97.38432216341050207, -42.15794967186695175, 181.7451490854349743 ) ) ;
#37915 = ORIENTED_EDGE ( 'NONE', *, *, #82792, .F. ) ;
#37916 = CARTESIAN_POINT ( 'NONE',  ( 96.64983689172015602, -37.15430107835312157, 161.3584824187679487 ) ) ;
#37917 = DIRECTION ( 'NONE',  ( 0.000000000000000000, 0.000000000000000000, 1.000000000000000000 ) ) ;
#37918 = DIRECTION ( 'NONE',  ( 0.9825752044328147639, 0.1858654557302462929, 0.000000000000000000 ) ) ;
#37919 = CARTESIAN_POINT ( 'NONE',  ( 143.7437383847394301, -140.1181772184977490, 246.9254612266167612 ) ) ;
#37922 = CARTESIAN_POINT ( 'NONE',  ( 116.8666056714781973, -37.25052799200011577, 14.78419670448194445 ) ) ;
#37921 = CARTESIAN_POINT ( 'NONE',  ( -454.6936515812919879, 53.97500000000000142, -3.174999999999999822 ) ) ;
#37920 = DIRECTION ( 'NONE',  ( 3.999999999999999995E-14, -1.000000000000000000, 4.100000000000000342E-29 ) ) ;
#37923 = DIRECTION ( 'NONE',  ( 0.000000000000000000, 0.000000000000000000, 1.000000000000000000 ) ) ;
#37924 = LINE ( 'NONE', #23429, #27946 ) ;
#37925 = CARTESIAN_POINT ( 'NONE',  ( 116.3115597373110290, -32.94279827685361539, 270.1356252759109680 ) ) ;
#37926 = EDGE_CURVE ( 'NONE', #86883, #85398, #23319, .T. ) ;
#37927 = CYLINDRICAL_SURFACE ( 'NONE', #25415, 9.999999999999998224 ) ;
#37928 = ADVANCED_FACE ( 'NONE', ( #57094 ), #36224, .F. ) ;
#37929 = CARTESIAN_POINT ( 'NONE',  ( 76.06670390244805446, -58.72944715994109544, 239.5838068554169809 ) ) ;
#37930 = DIRECTION ( 'NONE',  ( 0.000000000000000000, 0.000000000000000000, 1.000000000000000000 ) ) ;
#37932 = ORIENTED_EDGE ( 'NONE', *, *, #18, .F. ) ;
#37931 = CARTESIAN_POINT ( 'NONE',  ( 98.80107334477645509, -37.99123951698243928, 195.5838068554173219 ) ) ;
#37933 = CARTESIAN_POINT ( 'NONE',  ( 136.3179110785966088, -20.31136518417599035, 7.339178645738122952 ) ) ;
#37934 = CARTESIAN_POINT ( 'NONE',  ( 96.02321403599634664, -35.86825885766610611, 191.2765776568629690 ) ) ;
#37935 = CARTESIAN_POINT ( 'NONE',  ( 103.9574082008755198, -47.33640867427461529, 58.33753003781600199 ) ) ;
#37936 = CARTESIAN_POINT ( 'NONE',  ( 115.8919449742516861, -44.71207447090664999, 229.2413395616249545 ) ) ;
#37937 = DIRECTION ( 'NONE',  ( 1.000000000000000000, 0.000000000000000000, 0.000000000000000000 ) ) ;
#37938 = CARTESIAN_POINT ( 'NONE',  ( 133.6498166246070127, 12.92155284005802507, 349.2756252759110680 ) ) ;
#37940 = DIRECTION ( 'NONE',  ( 0.000000000000000000, 0.000000000000000000, 1.000000000000000000 ) ) ;
#37939 = LINE ( 'NONE', #60143, #69639 ) ;
#37941 = DIRECTION ( 'NONE',  ( 0.000000000000000000, 0.000000000000000000, -1.000000000000000000 ) ) ;
#37942 = CARTESIAN_POINT ( 'NONE',  ( 32.15435173583699680, -31.62489322948790971, 313.9678068554150059 ) ) ;
#37943 = CIRCLE ( 'NONE', #49526, 5.599999999999994316 ) ;
#37944 = CARTESIAN_POINT ( 'NONE',  ( 70.06670417066790435, -69.62844715994098976, 222.2178068554179902 ) ) ;
#37945 = ORIENTED_EDGE ( 'NONE', *, *, #75957, .F. ) ;
#37946 = ORIENTED_EDGE ( 'NONE', *, *, #63878, .T. ) ;
#37947 = CARTESIAN_POINT ( 'NONE',  ( 115.5093363421805606, -33.45364150533647063, 93.53146744712398686 ) ) ;
#37949 = ORIENTED_EDGE ( 'NONE', *, *, #17001, .F. ) ;
#37948 = CARTESIAN_POINT ( 'NONE',  ( -12.61760061281886003, 84.21489741558211506, -129.9449561063389638 ) ) ;
#37950 = CARTESIAN_POINT ( 'NONE',  ( 101.7670726180548542, -27.05576796868586698, 96.46324432352997746 ) ) ;
#37951 = DIRECTION ( 'NONE',  ( 5.512527431108029424E-15, -1.000000000000000000, 0.000000000000000000 ) ) ;
#37952 = AXIS2_PLACEMENT_3D ( 'NONE', #84757, #34787, #42930 ) ;
#37953 = CARTESIAN_POINT ( 'NONE',  ( 78.22143491580753505, -16.68812225915645797, 7.662832107308280349 ) ) ;
#37954 = DIRECTION ( 'NONE',  ( -1.000000000000000078E-15, 1.000000000000000000, 0.000000000000000000 ) ) ;
#37955 = CARTESIAN_POINT ( 'NONE',  ( 97.33063403691424753, -33.15845143124434458, 21.03467289495897319 ) ) ;
#37956 = ORIENTED_EDGE ( 'NONE', *, *, #20202, .F. ) ;
#37957 = VERTEX_POINT ( 'NONE', #49832 ) ;
#37958 = ORIENTED_EDGE ( 'NONE', *, *, #84883, .F. ) ;
#37959 = FACE_OUTER_BOUND ( 'NONE', #53938, .T. ) ;
#37960 = FACE_OUTER_BOUND ( 'NONE', #19153, .T. ) ;
#37961 = CARTESIAN_POINT ( 'NONE',  ( 6.349999999999999645, 82.54999999999999716, 302.8950000000000387 ) ) ;
#37962 = CARTESIAN_POINT ( 'NONE',  ( 27.27158787008327678, 184.0000000000000000, 90.32146847885336172 ) ) ;
#37963 = CARTESIAN_POINT ( 'NONE',  ( 0.000000000000000000, 127.0000000000000000, -98.14560000000000173 ) ) ;
#37965 = EDGE_CURVE ( 'NONE', #89588, #32260, #22607, .T. ) ;
#37964 = DIRECTION ( 'NONE',  ( 0.000000000000000000, 0.000000000000000000, 1.000000000000000000 ) ) ;
#37966 = FACE_OUTER_BOUND ( 'NONE', #43041, .T. ) ;
#37967 = VECTOR ( 'NONE', #14139, 1000.000000000000000 ) ;
#37968 = CARTESIAN_POINT ( 'NONE',  ( -9.690133600363056487, 90.76968238247971499, 130.1963199222103356 ) ) ;
#37969 = CARTESIAN_POINT ( 'NONE',  ( 101.1533894386775074, -27.41820966596953468, 65.51467289495799662 ) ) ;
#37970 = VERTEX_POINT ( 'NONE', #1713 ) ;
#37971 = ORIENTED_EDGE ( 'NONE', *, *, #29692, .F. ) ;
#37972 = DIRECTION ( 'NONE',  ( -1.000000000000000078E-15, 1.000000000000000000, 0.000000000000000000 ) ) ;
#37973 = LINE ( 'NONE', #11621, #28891 ) ;
#37974 = VECTOR ( 'NONE', #36263, 999.9999999999998863 ) ;
#37975 = CARTESIAN_POINT ( 'NONE',  ( 84.56587091301774706, -88.37796714256990072, 250.2178068554180470 ) ) ;
#37976 = CARTESIAN_POINT ( 'NONE',  ( 98.22859028455410169, -39.55567757615634861, 129.3909475124479798 ) ) ;
#37977 = AXIS2_PLACEMENT_3D ( 'NONE', #63374, #50631, #36579 ) ;
#37978 = EDGE_CURVE ( 'NONE', #64854, #16883, #77966, .T. ) ;
#37979 = EDGE_CURVE ( 'NONE', #28373, #6171, #37124, .T. ) ;
#37980 = DIRECTION ( 'NONE',  ( -0.7071067811892183252, 0.7071067811838767092, -7.071067811892191094E-16 ) ) ;
#37981 = EDGE_LOOP ( 'NONE', ( #62663, #38789 ) ) ;
#37982 = EDGE_LOOP ( 'NONE', ( #56693, #80663, #51882, #2846 ) ) ;
#37983 = EDGE_CURVE ( 'NONE', #56634, #9037, #64382, .T. ) ;
#37984 = DIRECTION ( 'NONE',  ( 1.000000000000000000, 0.000000000000000000, 0.000000000000000000 ) ) ;
#37985 = ORIENTED_EDGE ( 'NONE', *, *, #79026, .F. ) ;
#37986 = ORIENTED_EDGE ( 'NONE', *, *, #35643, .F. ) ;
#37987 = EDGE_CURVE ( 'NONE', #40995, #54369, #63475, .T. ) ;
#37988 = VECTOR ( 'NONE', #41296, 1000.000000000000000 ) ;
#37989 = CARTESIAN_POINT ( 'NONE',  ( 97.29374130088892514, -39.17162219779756782, 162.9530118773259630 ) ) ;
#37990 = EDGE_CURVE ( 'NONE', #7552, #66356, #45934, .T. ) ;
#37991 = CARTESIAN_POINT ( 'NONE',  ( 31.78666935232982738, -36.02818131005922453, 237.4678068554150059 ) ) ;
#37992 = CARTESIAN_POINT ( 'NONE',  ( 107.3345073157536689, -26.28600797661530208, 116.0556252759109555 ) ) ;
#37993 = CARTESIAN_POINT ( 'NONE',  ( 97.07207208091389816, -35.37844104438559611, 121.2189585969273509 ) ) ;
#37994 = VECTOR ( 'NONE', #56236, 1000.000000000000000 ) ;
#37995 = EDGE_CURVE ( 'NONE', #41588, #30196, #14897, .T. ) ;
#37996 = CARTESIAN_POINT ( 'NONE',  ( 97.83900511596046101, -40.58358500529822521, 16.64132214453083947 ) ) ;
#37997 = ORIENTED_EDGE ( 'NONE', *, *, #42821, .F. ) ;
#37998 = ADVANCED_FACE ( 'NONE', ( #71649, #71205 ), #64825, .T. ) ;
#37999 = ORIENTED_EDGE ( 'NONE', *, *, #65936, .F. ) ;
#38000 = EDGE_LOOP ( 'NONE', ( #41407, #47348, #76885, #88836 ) ) ;
#38001 = EDGE_CURVE ( 'NONE', #69623, #74022, #76667, .T. ) ;
#38002 = CIRCLE ( 'NONE', #88794, 1.000000000000000888 ) ;
#38003 = CARTESIAN_POINT ( 'NONE',  ( 106.6101046285737510, -27.46188816740816918, 192.9338046553059485 ) ) ;
#38004 = CARTESIAN_POINT ( 'NONE',  ( 109.9170780819575839, -46.81718586395340509, 72.79562527591099297 ) ) ;
#38005 = ORIENTED_EDGE ( 'NONE', *, *, #37307, .F. ) ;
#38006 = CARTESIAN_POINT ( 'NONE',  ( 105.4244226815142156, -47.00233879195506148, 37.44991099019695469 ) ) ;
#38007 = CARTESIAN_POINT ( 'NONE',  ( 116.7939007044644200, -39.39219064343244980, 253.6148464904360367 ) ) ;
#38008 = DIRECTION ( 'NONE',  ( 1.000000000000000078E-15, -1.000000000000000083E-30, -1.000000000000000000 ) ) ;
#38009 = CARTESIAN_POINT ( 'NONE',  ( 113.6324552648963504, -29.12879861577680529, 195.5092680403551810 ) ) ;
#38010 = CARTESIAN_POINT ( 'NONE',  ( 118.9175753851156401, -36.92810247848812821, 149.8127681330539644 ) ) ;
#38011 = AXIS2_PLACEMENT_3D ( 'NONE', #80058, #10551, #58685 ) ;
#38012 = EDGE_CURVE ( 'NONE', #61339, #29424, #41618, .T. ) ;
#38013 = CARTESIAN_POINT ( 'NONE',  ( 117.0608945242948238, -38.08045311361057372, 263.7189586098177756 ) ) ;
#38014 = ORIENTED_EDGE ( 'NONE', *, *, #73041, .F. ) ;
#38015 = FACE_BOUND ( 'NONE', #14691, .T. ) ;
#38016 = AXIS2_PLACEMENT_3D ( 'NONE', #42998, #17111, #65687 ) ;
#38017 = ORIENTED_EDGE ( 'NONE', *, *, #72583, .T. ) ;
#38018 = FACE_OUTER_BOUND ( 'NONE', #75619, .T. ) ;
#38019 = ORIENTED_EDGE ( 'NONE', *, *, #47452, .F. ) ;
#38020 = ORIENTED_EDGE ( 'NONE', *, *, #68766, .F. ) ;
#38021 = CARTESIAN_POINT ( 'NONE',  ( 28.57499999999999929, 87.13271776169270311, 294.9574999999999818 ) ) ;
#38022 =( BOUNDED_CURVE ( )  B_SPLINE_CURVE ( 2, ( #39371, #38916, #79390 ),
 .UNSPECIFIED., .F., .T. ) 
 B_SPLINE_CURVE_WITH_KNOTS ( ( 3, 3 ),
 ( 0.01169420784673960018, 0.5170228498526600047 ),
 .UNSPECIFIED. ) 
 CURVE ( )  GEOMETRIC_REPRESENTATION_ITEM ( )  RATIONAL_B_SPLINE_CURVE ( ( 1.000420656333759872, 1.009299002520659849, 1.000000000000000000 ) ) 
 REPRESENTATION_ITEM ( '' )  );
#38023 = CARTESIAN_POINT ( 'NONE',  ( 98.30753417268519456, -41.72887546008843884, 176.7397919400707167 ) ) ;
#38024 = CARTESIAN_POINT ( 'NONE',  ( 110.4566641872556403, -47.25017721759432732, 57.83657765686300678 ) ) ;
#38025 = DIRECTION ( 'NONE',  ( 0.9963424814100680926, -0.08544974978095730422, 0.000000000000000000 ) ) ;
#38026 = LINE ( 'NONE', #67067, #85527 ) ;
#38027 = CARTESIAN_POINT ( 'NONE',  ( 0.000000000000000000, 61.59999999999999432, 0.000000000000000000 ) ) ;
#38028 = CARTESIAN_POINT ( 'NONE',  ( 113.9027609268606369, -43.72435554967460547, 73.19276813305496887 ) ) ;
#38030 = CARTESIAN_POINT ( 'NONE',  ( 95.93334478249057895, -32.74178691125834462, 172.0527681330539735 ) ) ;
#38029 = LINE ( 'NONE', #39364, #33327 ) ;
#38031 = CYLINDRICAL_SURFACE ( 'NONE', #56742, 5.599999999999994316 ) ;
#38032 = CARTESIAN_POINT ( 'NONE',  ( 46.03715912545432332, -48.62818131006086020, 249.9678068554150343 ) ) ;
#38033 = ORIENTED_EDGE ( 'NONE', *, *, #87139, .F. ) ;
#38034 = LINE ( 'NONE', #23093, #12133 ) ;
#38035 = EDGE_CURVE ( 'NONE', #84821, #44708, #28499, .T. ) ;
#38036 = CARTESIAN_POINT ( 'NONE',  ( 83.06670390244796920, -67.87844715994100397, 231.5838068554150198 ) ) ;
#38037 = EDGE_CURVE ( 'NONE', #21182, #38055, #1262, .T. ) ;
#38038 = LINE ( 'NONE', #18473, #32814 ) ;
#38039 = ADVANCED_FACE ( 'NONE', ( #84398 ), #22165, .T. ) ;
#38040 = LINE ( 'NONE', #10336, #86858 ) ;
#38042 = ORIENTED_EDGE ( 'NONE', *, *, #9386, .T. ) ;
#38041 = CARTESIAN_POINT ( 'NONE',  ( 99.72210660708088881, -29.26842865273154004, 225.6956252759109702 ) ) ;
#38043 = CARTESIAN_POINT ( 'NONE',  ( 97.79835618974222200, -40.48471054006801495, 146.6328135905738179 ) ) ;
#38044 = CARTESIAN_POINT ( 'NONE',  ( 110.9006160922534150, -26.97349402997008383, 265.7784824187680783 ) ) ;
#38045 = CARTESIAN_POINT ( 'NONE',  ( 117.6248412043677121, -33.30620651169719082, 130.0880062282919880 ) ) ;
#38046 = EDGE_CURVE ( 'NONE', #19093, #26394, #35924, .T. ) ;
#38047 = CARTESIAN_POINT ( 'NONE',  ( 104.4929451592478955, -26.97798605588400278, 251.2871328988943844 ) ) ;
#38048 = VECTOR ( 'NONE', #24866, 1000.000000000000000 ) ;
#38049 = CARTESIAN_POINT ( 'NONE',  ( 82.81647637678393892, -36.77596264856293828, 6.749779334551927690 ) ) ;
#38050 = PLANE ( 'NONE',  #6575 ) ;
#38051 = CARTESIAN_POINT ( 'NONE',  ( 151.0371591254584871, -46.82818131005592477, 180.4678068554149775 ) ) ;
#38052 = ORIENTED_EDGE ( 'NONE', *, *, #64363, .T. ) ;
#38053 = AXIS2_PLACEMENT_3D ( 'NONE', #5254, #74742, #61104 ) ;
#38054 = ORIENTED_EDGE ( 'NONE', *, *, #30857, .T. ) ;
#38055 = VERTEX_POINT ( 'NONE', #3931 ) ;
#38056 = VERTEX_POINT ( 'NONE', #30748 ) ;
#38057 = CARTESIAN_POINT ( 'NONE',  ( 101.9936209245900756, -45.44607152936009697, 72.15645860776081122 ) ) ;
#38058 = CARTESIAN_POINT ( 'NONE',  ( 116.5819428025096585, -42.35350697836285860, 279.4137205140061724 ) ) ;
#38059 = CARTESIAN_POINT ( 'NONE',  ( 134.0664832912740110, -46.72944715994100306, 1.625625275910997480 ) ) ;
#38060 = CARTESIAN_POINT ( 'NONE',  ( 177.0664832912740110, 12.92155284005802685, 336.5756252759111362 ) ) ;
#38061 = VECTOR ( 'NONE', #85266, 1000.000000000000000 ) ;
#38063 = CARTESIAN_POINT ( 'NONE',  ( 172.5667039024480687, -36.32844715993499563, 129.9678068554150059 ) ) ;
#38062 = CYLINDRICAL_SURFACE ( 'NONE', #48187, 20.00000000000000355 ) ;
#38064 = CARTESIAN_POINT ( 'NONE',  ( 99.44356389104279970, -40.64648710652873831, 196.1267055423629699 ) ) ;
#38065 = ORIENTED_EDGE ( 'NONE', *, *, #43405, .T. ) ;
#38066 = ORIENTED_EDGE ( 'NONE', *, *, #34076, .F. ) ;
#38067 = ORIENTED_EDGE ( 'NONE', *, *, #74199, .F. ) ;
#38068 = VECTOR ( 'NONE', #41021, 1000.000000000000000 ) ;
#38069 = LINE ( 'NONE', #24889, #28213 ) ;
#38070 = CARTESIAN_POINT ( 'NONE',  ( 70.63919639214310564, 93.07500000000001705, 56.85413200336923012 ) ) ;
#38071 = CARTESIAN_POINT ( 'NONE',  ( 186.6899999999999977, 46.38749999999999574, -38.10000000000000142 ) ) ;
#38072 = CARTESIAN_POINT ( 'NONE',  ( 105.4490071354754406, -45.46730099742844544, 8.861583305896925111 ) ) ;
#38073 = VECTOR ( 'NONE', #71125, 1000.000000000000000 ) ;
#38074 = CARTESIAN_POINT ( 'NONE',  ( 118.1709372608869160, 90.93089219781630561, -9.551212252128932434 ) ) ;
#38075 = DIRECTION ( 'NONE',  ( -0.7071067811865487940, 0.000000000000000000, 0.7071067811865463515 ) ) ;
#38076 = DIRECTION ( 'NONE',  ( 1.000000000000000000, -8.621103231412346209E-16, 0.000000000000000000 ) ) ;
#38077 = ORIENTED_EDGE ( 'NONE', *, *, #3745, .F. ) ;
#38078 = CARTESIAN_POINT ( 'NONE',  ( 103.2781190732607115, -27.47481063885592434, 56.38565936678559609 ) ) ;
#38079 = EDGE_LOOP ( 'NONE', ( #56396, #15489, #43955 ) ) ;
#38080 = LINE ( 'NONE', #65772, #27807 ) ;
#38081 = CARTESIAN_POINT ( 'NONE',  ( 110.4716576677765119, -44.14797218061634254, 25.73666179816297372 ) ) ;
#38082 = DIRECTION ( 'NONE',  ( 0.000000000000000000, 1.000000000000000000, 1.914177628664063178E-15 ) ) ;
#38083 = ADVANCED_FACE ( 'NONE', ( #65270 ), #18446, .F. ) ;
#38084 = EDGE_CURVE ( 'NONE', #21668, #48266, #83798, .T. ) ;
#38085 = DIRECTION ( 'NONE',  ( -0.7071067811865443531, -0.7071067811865506814, -7.071067811865450681E-16 ) ) ;
#38086 = DIRECTION ( 'NONE',  ( 0.000000000000000000, 0.000000000000000000, -1.000000000000000000 ) ) ;
#38087 = ORIENTED_EDGE ( 'NONE', *, *, #75396, .T. ) ;
#38088 = DIRECTION ( 'NONE',  ( 0.000000000000000000, 0.000000000000000000, 1.000000000000000000 ) ) ;
#38089 = EDGE_CURVE ( 'NONE', #1768, #29470, #11185, .T. ) ;
#38090 = LINE ( 'NONE', #46673, #48427 ) ;
#38091 = VECTOR ( 'NONE', #82556, 1000.000000000000000 ) ;
#38092 = ORIENTED_EDGE ( 'NONE', *, *, #22027, .F. ) ;
#38093 = CARTESIAN_POINT ( 'NONE',  ( 98.58988425959138624, -43.82355431373886034, 71.86895860924397539 ) ) ;
#38094 = ORIENTED_EDGE ( 'NONE', *, *, #36349, .F. ) ;
#38095 = CARTESIAN_POINT ( 'NONE',  ( 104.1257281832662613, -27.47619977921510781, 54.74384839950496939 ) ) ;
#38096 = EDGE_CURVE ( 'NONE', #80398, #63665, #34426, .T. ) ;
#38097 = CARTESIAN_POINT ( 'NONE',  ( 102.8437810223914255, -45.83527424000978812, 88.23010560950143599 ) ) ;
#38098 = CARTESIAN_POINT ( 'NONE',  ( 98.44267559312871185, -33.00030968290830202, 57.44539282970595195 ) ) ;
#38099 = CARTESIAN_POINT ( 'NONE',  ( 113.1772940493579966, -44.75261571957639717, 14.09386025446782753 ) ) ;
#38100 = EDGE_CURVE ( 'NONE', #37203, #82603, #24826, .T. ) ;
#38101 = DIRECTION ( 'NONE',  ( 1.000000000000000000, 0.000000000000000000, 0.000000000000000000 ) ) ;
#38102 = CARTESIAN_POINT ( 'NONE',  ( 147.0665937085389032, -67.87844715994090450, 245.5130139786259917 ) ) ;
#38103 = CARTESIAN_POINT ( 'NONE',  ( 112.1919128969917097, -27.58564230820396190, 30.66991099019694644 ) ) ;
#38105 = EDGE_CURVE ( 'NONE', #12226, #84394, #10303, .T. ) ;
#38104 = CARTESIAN_POINT ( 'NONE',  ( 194.5667039024485803, -47.82844715993405060, 129.9678068554150343 ) ) ;
#38106 = ORIENTED_EDGE ( 'NONE', *, *, #47577, .T. ) ;
#38107 = DIRECTION ( 'NONE',  ( -1.000000000000000078E-15, 1.000000000000000083E-30, 1.000000000000000000 ) ) ;
#38108 = ORIENTED_EDGE ( 'NONE', *, *, #86610, .T. ) ;
#38109 = DIRECTION ( 'NONE',  ( -0.8660254037844392627, 0.4999999999999990008, -1.549999999999999706E-14 ) ) ;
#38110 = EDGE_LOOP ( 'NONE', ( #12367, #46909, #56425, #23372 ) ) ;
#38111 = ORIENTED_EDGE ( 'NONE', *, *, #55670, .F. ) ;
#38112 = EDGE_CURVE ( 'NONE', #15662, #55859, #72967, .T. ) ;
#38113 = CARTESIAN_POINT ( 'NONE',  ( 53.56670390244828184, -48.82844715994055917, 300.4678068554150059 ) ) ;
#38114 = CARTESIAN_POINT ( 'NONE',  ( 112.6540662323892263, -44.79745133516141209, 203.0584824187689605 ) ) ;
#38115 = CARTESIAN_POINT ( 'NONE',  ( 98.08598099046197660, -32.25672833729997535, 125.9577075789795373 ) ) ;
#38116 = CARTESIAN_POINT ( 'NONE',  ( 163.2449138992999735, -32.11662333284611748, -5.074374724088000832 ) ) ;
#38117 = CARTESIAN_POINT ( 'NONE',  ( 114.3531094850664260, -44.18515411228707279, 69.19276813305397411 ) ) ;
#38118 = EDGE_CURVE ( 'NONE', #35473, #12869, #38888, .T. ) ;
#38119 = CARTESIAN_POINT ( 'NONE',  ( 115.0371363339966280, -42.90862416454874051, 44.30227608399194139 ) ) ;
#38120 = ORIENTED_EDGE ( 'NONE', *, *, #37388, .T. ) ;
#38121 = CARTESIAN_POINT ( 'NONE',  ( 97.80863031437060329, -40.50995291785646657, 172.6349830369815663 ) ) ;
#38122 = CARTESIAN_POINT ( 'NONE',  ( 184.5664832912729878, -71.37844715994266664, 342.9256252759109884 ) ) ;
#38124 = ORIENTED_EDGE ( 'NONE', *, *, #6118, .T. ) ;
#38123 = EDGE_CURVE ( 'NONE', #60056, #47600, #66595, .T. ) ;
#38125 = AXIS2_PLACEMENT_3D ( 'NONE', #88979, #61257, #88092 ) ;
#38126 = DIRECTION ( 'NONE',  ( 1.000000000000000000, -6.836348673800234255E-15, 0.000000000000000000 ) ) ;
#38127 = DIRECTION ( 'NONE',  ( 0.000000000000000000, 0.000000000000000000, -1.000000000000000000 ) ) ;
#38128 = CARTESIAN_POINT ( 'NONE',  ( 106.9407056411434951, -47.75886249174727283, 232.5794347997199907 ) ) ;
#38129 = LINE ( 'NONE', #39011, #6604 ) ;
#38130 = CARTESIAN_POINT ( 'NONE',  ( 173.9900000000000091, 52.73749999999999716, -52.38749999999999574 ) ) ;
#38131 = CARTESIAN_POINT ( 'NONE',  ( 19.56670390244796920, -48.82844715994099971, 300.9178068554150514 ) ) ;
#38132 = CARTESIAN_POINT ( 'NONE',  ( 114.4310042120387862, -41.05610445278038156, 237.8267055423629586 ) ) ;
#38135 = CARTESIAN_POINT ( 'NONE',  ( 104.2200364793041700, -25.25138339198311144, 86.26991099019699050 ) ) ;
#38134 = DIRECTION ( 'NONE',  ( 0.000000000000000000, 0.000000000000000000, -1.000000000000000000 ) ) ;
#38133 = AXIS2_PLACEMENT_3D ( 'NONE', #4745, #75125, #20170 ) ;
#38136 = CARTESIAN_POINT ( 'NONE',  ( 109.6076600728624015, 58.52556248408083661, 70.92975744315074849 ) ) ;
#38137 = CARTESIAN_POINT ( 'NONE',  ( 114.0516219551475245, -28.93108169718528444, 114.4956252759109816 ) ) ;
#38138 = ORIENTED_EDGE ( 'NONE', *, *, #11367, .T. ) ;
#38139 = CARTESIAN_POINT ( 'NONE',  ( 132.8827458516715581, -21.21170328187201903, 8.006085407567432810 ) ) ;
#38140 = EDGE_LOOP ( 'NONE', ( #9403, #18368, #11188, #69345 ) ) ;
#38141 = CARTESIAN_POINT ( 'NONE',  ( 6.938893903907229955E-15, 50.79999999999999716, 209.1689999999999827 ) ) ;
#38142 = CARTESIAN_POINT ( 'NONE',  ( 107.0667039024469886, -70.87844715994094713, 93.21780685541800437 ) ) ;
#38143 = DIRECTION ( 'NONE',  ( -3.999999999999999995E-14, 1.000000000000000000, -4.100000000000000342E-29 ) ) ;
#38144 = EDGE_LOOP ( 'NONE', ( #7725, #57541 ) ) ;
#38145 = EDGE_CURVE ( 'NONE', #31941, #62004, #22848, .T. ) ;
#38146 = CARTESIAN_POINT ( 'NONE',  ( 97.07202004682035579, -35.37880823152836030, 51.21898755952398830 ) ) ;
#38148 = VERTEX_POINT ( 'NONE', #11650 ) ;
#38147 = CARTESIAN_POINT ( 'NONE',  ( 109.2642598482130154, -47.00181652296804913, 107.7441967044829880 ) ) ;
#38149 = DIRECTION ( 'NONE',  ( -1.000000000000000000, -4.299999999999999979E-14, -1.000000000000000078E-15 ) ) ;
#38150 = EDGE_CURVE ( 'NONE', #10055, #71324, #4388, .T. ) ;
#38151 = CARTESIAN_POINT ( 'NONE',  ( 116.3175913315759402, -32.94491325663879877, 165.1356252759109680 ) ) ;
#38152 = DIRECTION ( 'NONE',  ( -2.999999999999999839E-15, 1.000000000000000000, -2.999999999999999900E-30 ) ) ;
#38153 = ORIENTED_EDGE ( 'NONE', *, *, #32446, .F. ) ;
#38154 = CARTESIAN_POINT ( 'NONE',  ( 103.1971861921166038, -46.47197777470199753, 117.2756252759109543 ) ) ;
#38155 = DIRECTION ( 'NONE',  ( 0.000000000000000000, 0.000000000000000000, -1.000000000000000000 ) ) ;
#38156 = CARTESIAN_POINT ( 'NONE',  ( 141.8664832912729992, -71.52944715994142655, 342.9256252759109884 ) ) ;
#38157 = CARTESIAN_POINT ( 'NONE',  ( 41.56648329127399677, 0.2215528400590013880, 196.8086252759119645 ) ) ;
#38158 = FACE_OUTER_BOUND ( 'NONE', #60040, .T. ) ;
#38159 = DIRECTION ( 'NONE',  ( 1.000000000000000000, 6.145690160522480771E-16, 0.000000000000000000 ) ) ;
#38160 = ORIENTED_EDGE ( 'NONE', *, *, #40796, .F. ) ;
#38161 = TOROIDAL_SURFACE ( 'NONE', #22222, 11.75000000000000000, 2.550000000000000266 ) ;
#38162 = ORIENTED_EDGE ( 'NONE', *, *, #75316, .T. ) ;
#38163 = DIRECTION ( 'NONE',  ( -1.000000000000000000, -1.734723475976808672E-15, 0.000000000000000000 ) ) ;
#38164 = B_SPLINE_CURVE_WITH_KNOTS ( 'NONE', 3,
 ( #20717, #69317, #32535, #60240, #25733, #18921, #53408, #12111, #67511, #270, #8897, #29776, #62933, #83851, #69766, #78391, #49301, #2071, #56569, #22518, #50649, #57467, #712, #7091, #57013, #16153, #84312, #70211, #7981, #84755, #28419, #50198, #8440, #55645, #7538, #34785, #43828, #77931, #22083, #42479, #56103, #71122 ),
 .UNSPECIFIED., .F., .F.,
 ( 4, 2, 1, 1, 1, 1, 1, 1, 2, 2, 2, 2, 2, 2, 2, 2, 2, 2, 2, 2, 2, 2, 2, 4 ),
 ( 0.4999355867161964229, 0.5000576727545975597, 0.5001797587929986966, 0.5004239308697975286, 0.5009122750233935273, 0.5018889633305889664, 0.5038423399449779572, 0.5077490931737559388, 0.5155625996313152326, 0.5311896125464334872, 0.5624436383766713288, 0.6249516900371467898, 0.6562057158673846313, 0.6874597416976223618, 0.7187137675278600923, 0.7499677933580979339, 0.7812218191883356644, 0.8124758450185733949, 0.8437298708488112364, 0.8749838966790488559, 0.9062379225092866974, 0.9374919483395244280, 0.9687459741697621585, 1.000000000000000000 ),
 .UNSPECIFIED. ) ;
#38165 = CARTESIAN_POINT ( 'NONE',  ( 97.81169951533574647, -40.51743117454552134, 102.6356342116286413 ) ) ;
#38166 = LINE ( 'NONE', #74027, #83634 ) ;
#38168 = DIRECTION ( 'NONE',  ( 0.000000000000000000, 0.000000000000000000, 1.000000000000000000 ) ) ;
#38167 = CARTESIAN_POINT ( 'NONE',  ( 116.6018603435394141, -39.73108032723776972, 249.5838075904518121 ) ) ;
#38169 = CYLINDRICAL_SURFACE ( 'NONE', #1609, 1.000000000002049694 ) ;
#38170 = CIRCLE ( 'NONE', #77334, 18.00000000000000000 ) ;
#38171 = EDGE_CURVE ( 'NONE', #43446, #83511, #85244, .T. ) ;
#38172 = ORIENTED_EDGE ( 'NONE', *, *, #60114, .F. ) ;
#38173 = CARTESIAN_POINT ( 'NONE',  ( 108.3334482501379767, -46.73485933287561522, 33.67729195491988747 ) ) ;
#38174 = CARTESIAN_POINT ( 'NONE',  ( 102.9544237342424395, -27.85507949283302764, 176.4213395616249898 ) ) ;
#38176 = ORIENTED_EDGE ( 'NONE', *, *, #10088, .T. ) ;
#38175 = CARTESIAN_POINT ( 'NONE',  ( 83.06670390244796920, -58.35344715994099829, 207.5838068554149913 ) ) ;
#38177 = CARTESIAN_POINT ( 'NONE',  ( 111.6283393632454022, -28.07768985461837730, 55.68991099019593349 ) ) ;
#38178 = LINE ( 'NONE', #16407, #15405 ) ;
#38179 = DIRECTION ( 'NONE',  ( 9.351236661543306751E-17, -3.725950533538267725E-29, -1.000000000000000000 ) ) ;
#38180 = ORIENTED_EDGE ( 'NONE', *, *, #65431, .F. ) ;
#38181 = CARTESIAN_POINT ( 'NONE',  ( 41.56648329127399677, 0.2215528400590013880, 261.0426252759119734 ) ) ;
#38182 = ORIENTED_EDGE ( 'NONE', *, *, #15955, .T. ) ;
#38183 = ORIENTED_EDGE ( 'NONE', *, *, #61358, .F. ) ;
#38184 = EDGE_CURVE ( 'NONE', #75304, #26158, #41675, .T. ) ;
#38185 = CARTESIAN_POINT ( 'NONE',  ( 109.2250051346758113, -28.10373483931914151, 196.3130118773259767 ) ) ;
#38186 = VECTOR ( 'NONE', #88432, 1000.000000000000000 ) ;
#38187 = CARTESIAN_POINT ( 'NONE',  ( 59.68306514483412428, -72.55903866283681225, 396.9756252759102040 ) ) ;
#38188 = CARTESIAN_POINT ( 'NONE',  ( -100.4448767513717513, 86.64186789594789673, 83.40142812120620874 ) ) ;
#38189 = AXIS2_PLACEMENT_3D ( 'NONE', #20038, #48600, #12322 ) ;
#38190 = B_SPLINE_CURVE_WITH_KNOTS ( 'NONE', 3,
 ( #53854, #26627, #54303, #81623, #82070, #19820, #19373, #67966, #74782, #61583, #89320, #87970, #60239, #47501, #89772, #62038, #75238, #13013 ),
 .UNSPECIFIED., .F., .F.,
 ( 4, 2, 2, 2, 2, 2, 2, 2, 4 ),
 ( 0.000000000000000000, 0.06250000002888209116, 0.1250000000577641823, 0.1875000000866462735, 0.2500000001155283647, 0.3125000001444104836, 0.3750000001732925470, 0.4375000002021746104, 0.5000000002310567293 ),
 .UNSPECIFIED. ) ;
#38191 = EDGE_CURVE ( 'NONE', #42224, #32980, #14612, .T. ) ;
#38192 = EDGE_CURVE ( 'NONE', #39230, #63968, #67686, .T. ) ;
#38193 = FACE_OUTER_BOUND ( 'NONE', #27834, .T. ) ;
#38194 = CARTESIAN_POINT ( 'NONE',  ( 107.0664832912739968, -36.72944715994100306, 287.6356252759109680 ) ) ;
#38195 = VERTEX_POINT ( 'NONE', #81156 ) ;
#38196 = DIRECTION ( 'NONE',  ( -1.000000000000000078E-15, 1.000000000000000083E-30, 1.000000000000000000 ) ) ;
#38197 = ADVANCED_FACE ( 'NONE', ( #49162 ), #74324, .T. ) ;
#38198 = CARTESIAN_POINT ( 'NONE',  ( 97.81045233035079889, -40.51440448977106001, 37.63507460729699972 ) ) ;
#38199 = EDGE_LOOP ( 'NONE', ( #83213, #78619, #32480, #18047 ) ) ;
#38200 = CARTESIAN_POINT ( 'NONE',  ( 115.7579298488887076, -31.01215564512770229, 254.2899109901966028 ) ) ;
#38201 = CARTESIAN_POINT ( 'NONE',  ( 12.60000000000000142, 82.54999999999999716, 117.6834004267381744 ) ) ;
#38202 = ORIENTED_EDGE ( 'NONE', *, *, #87592, .F. ) ;
#38203 = EDGE_CURVE ( 'NONE', #28839, #8744, #76894, .T. ) ;
#38204 = CARTESIAN_POINT ( 'NONE',  ( 116.3170820643562564, -32.94538914428453324, 169.1356252759109680 ) ) ;
#38205 = CARTESIAN_POINT ( 'NONE',  ( 48.45959712129000252, -28.98061976758940617, 313.9678068554150059 ) ) ;
#38206 = CYLINDRICAL_SURFACE ( 'NONE', #79565, 7.143749999999999822 ) ;
#38207 = DIRECTION ( 'NONE',  ( 0.000000000000000000, 0.000000000000000000, 1.000000000000000000 ) ) ;
#38208 = CARTESIAN_POINT ( 'NONE',  ( 109.6164515631795524, -26.53946793531281756, 195.8813395616249977 ) ) ;
#38209 = LINE ( 'NONE', #17767, #44151 ) ;
#38210 = ADVANCED_FACE ( 'NONE', ( #75217 ), #55971, .T. ) ;
#38211 = VERTEX_POINT ( 'NONE', #74764 ) ;
#38212 = CARTESIAN_POINT ( 'NONE',  ( 112.8417677104678063, -27.25086138798909374, 45.62895860924398761 ) ) ;
#38213 = CARTESIAN_POINT ( 'NONE',  ( 163.1639762274897976, -34.03355364505781466, 237.4678068554150059 ) ) ;
#38214 = AXIS2_PLACEMENT_3D ( 'NONE', #39503, #67202, #62176 ) ;
#38215 = CARTESIAN_POINT ( 'NONE',  ( 115.6554515427140473, -30.75822225795367970, 279.3099109901966131 ) ) ;
#38216 = ORIENTED_EDGE ( 'NONE', *, *, #34914, .T. ) ;
#38217 = ADVANCED_FACE ( 'NONE', ( #70076 ), #26169, .F. ) ;
#38218 = VECTOR ( 'NONE', #72808, 1000.000000000000000 ) ;
#38219 = CARTESIAN_POINT ( 'NONE',  ( 80.94673009889297077, -16.12360705087681012, 1.744847597652003701 ) ) ;
#38220 = CARTESIAN_POINT ( 'NONE',  ( 98.15087327529982986, -41.26140878761783881, 17.70046935524347376 ) ) ;
#38221 = CARTESIAN_POINT ( 'NONE',  ( 105.7138906618339433, -46.72361789148295941, 152.4694709838751692 ) ) ;
#38222 = CARTESIAN_POINT ( 'NONE',  ( 104.0433210460927000, -44.34148882339519560, 115.0938046553049503 ) ) ;
#38223 = CARTESIAN_POINT ( 'NONE',  ( 107.2496171063691577, -24.85558036374148472, 226.0641967044829812 ) ) ;
#38224 = CARTESIAN_POINT ( 'NONE',  ( -29.99999999999998224, 172.0000000000000000, 114.8826257785461280 ) ) ;
#38225 = EDGE_LOOP ( 'NONE', ( #23149, #88742, #50780, #29950 ) ) ;
#38226 = CARTESIAN_POINT ( 'NONE',  ( 136.2737402105819911, -38.37320971852938101, 2.471387388682165565 ) ) ;
#38227 = ORIENTED_EDGE ( 'NONE', *, *, #15110, .T. ) ;
#38228 = ORIENTED_EDGE ( 'NONE', *, *, #1414, .F. ) ;
#38229 = AXIS2_PLACEMENT_3D ( 'NONE', #81692, #30626, #71087 ) ;
#38230 = DIRECTION ( 'NONE',  ( 0.7071067811865171526, 0.7071067811865779928, 7.071067811865164719E-16 ) ) ;
#38231 = ORIENTED_EDGE ( 'NONE', *, *, #20579, .T. ) ;
#38232 = ORIENTED_EDGE ( 'NONE', *, *, #20769, .T. ) ;
#38233 = CARTESIAN_POINT ( 'NONE',  ( 194.5667039024479834, -67.87844715994100397, 20.91780685541479912 ) ) ;
#38234 = DIRECTION ( 'NONE',  ( -1.000000000000000000, -8.163404592832032979E-16, 0.000000000000000000 ) ) ;
#38235 = DIRECTION ( 'NONE',  ( -3.100000000000000258E-29, 3.100000000000000044E-14, 1.000000000000000000 ) ) ;
#38236 = CARTESIAN_POINT ( 'NONE',  ( 99.80400324059088746, -42.13953531443270606, 111.2705150661719671 ) ) ;
#38237 = CARTESIAN_POINT ( 'NONE',  ( 97.03298259997053776, -33.74021148472603215, 31.09562527591097592 ) ) ;
#38238 = ORIENTED_EDGE ( 'NONE', *, *, #86441, .F. ) ;
#38239 = DIRECTION ( 'NONE',  ( 4.299999999999999979E-14, -1.000000000000000000, 0.000000000000000000 ) ) ;
#38240 = ORIENTED_EDGE ( 'NONE', *, *, #41219, .F. ) ;
#38241 = CARTESIAN_POINT ( 'NONE',  ( 107.0667039024470313, -104.2784471599409528, 22.21780685541800082 ) ) ;
#38242 = ORIENTED_EDGE ( 'NONE', *, *, #10913, .F. ) ;
#38243 = DIRECTION ( 'NONE',  ( 0.000000000000000000, -1.000000000000000000, 0.000000000000000000 ) ) ;
#38244 = CARTESIAN_POINT ( 'NONE',  ( 107.0664832912739968, -36.72944715994100306, 287.6356252759109680 ) ) ;
#38245 = EDGE_CURVE ( 'NONE', #9096, #77101, #46587, .T. ) ;
#38246 = FACE_OUTER_BOUND ( 'NONE', #83781, .T. ) ;
#38247 = AXIS2_PLACEMENT_3D ( 'NONE', #13020, #67516, #68430 ) ;
#38248 = CARTESIAN_POINT ( 'NONE',  ( 76.20505178924339873, 120.6499999999999915, 76.20505178924419454 ) ) ;
#38249 = ORIENTED_EDGE ( 'NONE', *, *, #76975, .T. ) ;
#38250 = CARTESIAN_POINT ( 'NONE',  ( 104.8412335932644766, -26.50818645216173408, 260.2470538473397710 ) ) ;
#38251 = CARTESIAN_POINT ( 'NONE',  ( 96.64589536673427972, -32.90729728488415162, 17.03467289495896964 ) ) ;
#38252 =( NAMED_UNIT ( * ) PLANE_ANGLE_UNIT ( ) SI_UNIT ( $, .RADIAN. ) );
#38253 = VECTOR ( 'NONE', #26834, 1000.000000000000000 ) ;
#38255 = CARTESIAN_POINT ( 'NONE',  ( 69.32970740376067909, -138.6740805926116593, 247.3339793106913760 ) ) ;
#38254 = LINE ( 'NONE', #3739, #28868 ) ;
#38256 = DIRECTION ( 'NONE',  ( 1.000000000000000000, 0.000000000000000000, 0.000000000000000000 ) ) ;
#38257 = CARTESIAN_POINT ( 'NONE',  ( -29.99999999999996092, 127.0000000000000000, 182.8826257785461280 ) ) ;
#38258 = CYLINDRICAL_SURFACE ( 'NONE', #51389, 5.599999999999994316 ) ;
#38259 = DIRECTION ( 'NONE',  ( -0.7071067811865336949, -0.7071067811865614505, 0.000000000000000000 ) ) ;
#38260 = CARTESIAN_POINT ( 'NONE',  ( 107.3678158256761179, -26.30747296201684549, 321.5865679059475610 ) ) ;
#38261 = CARTESIAN_POINT ( 'NONE',  ( 163.0664832912739826, -18.82844715994099971, 333.4006252759120343 ) ) ;
#38262 = CARTESIAN_POINT ( 'NONE',  ( 101.5858402103170590, -47.29319095008832363, 17.19562527591095247 ) ) ;
#38263 = CARTESIAN_POINT ( 'NONE',  ( 97.40207042353749500, -40.63861732370358482, 202.6327681330539860 ) ) ;
#38264 = CARTESIAN_POINT ( 'NONE',  ( 96.93562038266055936, -32.25163268508860881, 51.98324432352996638 ) ) ;
#38266 = CARTESIAN_POINT ( 'NONE',  ( 46.83715912545429205, -47.82818131006082751, 249.9678068554150343 ) ) ;
#38265 = DIRECTION ( 'NONE',  ( 0.000000000000000000, 0.000000000000000000, 1.000000000000000000 ) ) ;
#38267 = CARTESIAN_POINT ( 'NONE',  ( 81.14852608520830302, -34.20116861175197442, 1.807989644435456400 ) ) ;
#38268 = EDGE_CURVE ( 'NONE', #44745, #31084, #21944, .T. ) ;
#38269 = VECTOR ( 'NONE', #21336, 1000.000000000000000 ) ;
#38270 = VECTOR ( 'NONE', #83426, 1000.000000000000000 ) ;
#38271 = ORIENTED_EDGE ( 'NONE', *, *, #4477, .F. ) ;
#38272 = CARTESIAN_POINT ( 'NONE',  ( 183.6524903400783444, -48.32844715993452667, 249.9678068554149775 ) ) ;
#38273 = VERTEX_POINT ( 'NONE', #88856 ) ;
#38274 = CARTESIAN_POINT ( 'NONE',  ( 98.20607846729137691, -32.50961293922097894, 71.97276813305397525 ) ) ;
#38276 = ORIENTED_EDGE ( 'NONE', *, *, #84094, .F. ) ;
#38275 = CARTESIAN_POINT ( 'NONE',  ( 41.56670390244695312, -36.32844715994109208, 129.9678068554150911 ) ) ;
#38277 = CIRCLE ( 'NONE', #64362, 7.499999999999992895 ) ;
#38278 = PLANE ( 'NONE',  #2619 ) ;
#38279 = CARTESIAN_POINT ( 'NONE',  ( 103.7301789885933943, -26.21598454391068600, 201.3089586092439731 ) ) ;
#38280 = CARTESIAN_POINT ( 'NONE',  ( 97.81021718220807770, -40.51802218317752846, 192.6354414398782353 ) ) ;
#38281 = CARTESIAN_POINT ( 'NONE',  ( 110.8542886837690702, -45.98431238365922269, 147.8856095171690868 ) ) ;
#38282 = PLANE ( 'NONE',  #38516 ) ;
#38283 = DIRECTION ( 'NONE',  ( 1.000000000000000000, 0.000000000000000000, 0.000000000000000000 ) ) ;
#38284 = FACE_BOUND ( 'NONE', #45352, .T. ) ;
#38285 = CARTESIAN_POINT ( 'NONE',  ( -82.89895571708294142, 81.71102547120851511, 100.8594679592209644 ) ) ;
#38286 = CARTESIAN_POINT ( 'NONE',  ( 116.5394839232220505, -34.29517225379350975, 124.0270538473399426 ) ) ;
#38287 = ORIENTED_EDGE ( 'NONE', *, *, #3742, .F. ) ;
#38288 = EDGE_LOOP ( 'NONE', ( #33045, #77514, #52566, #83049, #47703, #76566 ) ) ;
#38289 = CARTESIAN_POINT ( 'NONE',  ( 111.6972492074939396, -29.17403283370891032, 91.07015473446894305 ) ) ;
#38290 = LINE ( 'NONE', #64667, #16753 ) ;
#38292 = DIRECTION ( 'NONE',  ( 0.000000000000000000, 0.000000000000000000, 1.000000000000000000 ) ) ;
#38291 = CARTESIAN_POINT ( 'NONE',  ( 102.5357197525642192, -45.39752751535328201, 208.1927681330529651 ) ) ;
#38293 = DIRECTION ( 'NONE',  ( 0.000000000000000000, -1.000000000000000000, 0.000000000000000000 ) ) ;
#38294 = DIRECTION ( 'NONE',  ( 3.100000000000000258E-29, -3.100000000000000044E-14, -1.000000000000000000 ) ) ;
#38295 = ADVANCED_FACE ( 'NONE', ( #8303 ), #12543, .F. ) ;
#38296 = CARTESIAN_POINT ( 'NONE',  ( 118.3661894536416526, 71.76236341257998674, -6.714990428327953786 ) ) ;
#38297 = CARTESIAN_POINT ( 'NONE',  ( -7.746754343058400494, 72.45238928964013780, 118.3046374534493026 ) ) ;
#38298 = DIRECTION ( 'NONE',  ( 0.000000000000000000, -1.000000000000000000, 0.000000000000000000 ) ) ;
#38299 = EDGE_CURVE ( 'NONE', #18892, #56405, #7845, .T. ) ;
#38300 = CARTESIAN_POINT ( 'NONE',  ( 6.657252557472873811, 71.84426888462246552, 118.3694437465256328 ) ) ;
#38301 = CARTESIAN_POINT ( 'NONE',  ( 117.6812658759005217, -39.72780374360938538, 143.6194347997209775 ) ) ;
#38302 = EDGE_CURVE ( 'NONE', #42810, #15084, #68405, .T. ) ;
#38303 = ORIENTED_EDGE ( 'NONE', *, *, #1604, .T. ) ;
#38304 = ORIENTED_EDGE ( 'NONE', *, *, #14781, .F. ) ;
#38305 = EDGE_CURVE ( 'NONE', #2705, #72232, #50222, .T. ) ;
#38306 = CARTESIAN_POINT ( 'NONE',  ( 124.2517790421138102, -76.23676170112041461, 249.3134381260879877 ) ) ;
#38307 = CARTESIAN_POINT ( 'NONE',  ( 116.3159136950847170, -32.94903743517052419, 150.1356252759109680 ) ) ;
#38308 = CARTESIAN_POINT ( 'NONE',  ( 173.9900000000000091, 68.61249999999999716, -35.28456447661465489 ) ) ;
#38309 = PLANE ( 'NONE',  #54030 ) ;
#38310 = VECTOR ( 'NONE', #34675, 1000.000000000000000 ) ;
#38311 = PLANE ( 'NONE',  #62550 ) ;
#38312 = VECTOR ( 'NONE', #24178, 1000.000000000000000 ) ;
#38313 = CARTESIAN_POINT ( 'NONE',  ( 107.9182787209079919, -47.15539321873765743, 177.6413395616249886 ) ) ;
#38314 = CARTESIAN_POINT ( 'NONE',  ( 151.5667039024485518, -48.82844715993590512, 180.4678068554149775 ) ) ;
#38315 = ORIENTED_EDGE ( 'NONE', *, *, #42308, .F. ) ;
#38317 = EDGE_LOOP ( 'NONE', ( #43572, #5337, #44310, #48514, #72136 ) ) ;
#38316 = EDGE_LOOP ( 'NONE', ( #73296, #72755, #59668, #72709 ) ) ;
#38318 = EDGE_CURVE ( 'NONE', #15093, #81490, #65435, .T. ) ;
#38319 = CARTESIAN_POINT ( 'NONE',  ( 102.6169236507442974, -45.73916775254092215, 63.21228203591902428 ) ) ;
#38320 = FACE_OUTER_BOUND ( 'NONE', #68652, .T. ) ;
#38321 = CARTESIAN_POINT ( 'NONE',  ( 132.1570028295015220, -34.74831852142843047, 7.618261863067814943 ) ) ;
#38322 = CARTESIAN_POINT ( 'NONE',  ( 101.2106992548341822, -44.07698544542078167, 268.4606309249448941 ) ) ;
#38323 = CARTESIAN_POINT ( 'NONE',  ( 87.31648329127402519, -36.72944715994105991, -4.824374724089048883 ) ) ;
#38324 = ORIENTED_EDGE ( 'NONE', *, *, #79233, .T. ) ;
#38325 = DIRECTION ( 'NONE',  ( -1.000000000000000000, 0.000000000000000000, 9.299908063537896936E-17 ) ) ;
#38326 = CARTESIAN_POINT ( 'NONE',  ( 81.50686229671583760, -16.38644903112324869, 7.895285856720303919 ) ) ;
#38327 = ORIENTED_EDGE ( 'NONE', *, *, #34187, .T. ) ;
#38328 = ORIENTED_EDGE ( 'NONE', *, *, #36190, .F. ) ;
#38329 = AXIS2_PLACEMENT_3D ( 'NONE', #85556, #38706, #45948 ) ;
#38330 = CARTESIAN_POINT ( 'NONE',  ( 69.63919639214310564, 101.5999999999999943, 94.70900412239863897 ) ) ;
#38331 = VERTEX_POINT ( 'NONE', #16020 ) ;
#38332 = ORIENTED_EDGE ( 'NONE', *, *, #85334, .F. ) ;
#38333 = CARTESIAN_POINT ( 'NONE',  ( 0.000000000000000000, 82.54999999999999716, -190.5010000000000048 ) ) ;
#38334 = VECTOR ( 'NONE', #51638, 1000.000000000000000 ) ;
#38335 = CARTESIAN_POINT ( 'NONE',  ( 105.1568233002730182, -45.58189704936153674, 31.84194363760095570 ) ) ;
#38337 = CARTESIAN_POINT ( 'NONE',  ( 117.2187229798756363, -34.26400738748503727, 209.0156252759109634 ) ) ;
#38336 = AXIS2_PLACEMENT_3D ( 'NONE', #40701, #55203, #27524 ) ;
#38338 = CONICAL_SURFACE ( 'NONE', #58827, 11.57110091390439699, 0.7853981633974452814 ) ;
#38339 = CARTESIAN_POINT ( 'NONE',  ( 102.7067583520260712, -46.86140753836549777, 137.2651490854349561 ) ) ;
#38340 = CARTESIAN_POINT ( 'NONE',  ( 25.56670390244797275, -62.87844715994099687, 295.9678068554150059 ) ) ;
#38341 = CARTESIAN_POINT ( 'NONE',  ( 111.6084932380418735, -46.11308361340533679, 243.9356252759109509 ) ) ;
#38342 = DIRECTION ( 'NONE',  ( 0.7071067811865157093, 0.7071067811865794361, 7.071067811865461528E-16 ) ) ;
#38343 = LINE ( 'NONE', #24722, #78746 ) ;
#38344 = ORIENTED_EDGE ( 'NONE', *, *, #72118, .F. ) ;
#38345 = ORIENTED_EDGE ( 'NONE', *, *, #72068, .F. ) ;
#38346 = EDGE_CURVE ( 'NONE', #5969, #48953, #70759, .T. ) ;
#38347 = CARTESIAN_POINT ( 'NONE',  ( 115.5532354207493171, -29.57487366316678745, 224.3718157521009573 ) ) ;
#38348 = ORIENTED_EDGE ( 'NONE', *, *, #2499, .T. ) ;
#38349 = CARTESIAN_POINT ( 'NONE',  ( 97.67451187568107684, -41.25469890874477841, 171.6841967044819626 ) ) ;
#38350 = DIRECTION ( 'NONE',  ( -1.000000000000000000, 0.000000000000000000, 0.000000000000000000 ) ) ;
#38351 = CARTESIAN_POINT ( 'NONE',  ( 1.387778780781445676E-14, 239.0000000000000000, 97.27542076772557778 ) ) ;
#38352 = ADVANCED_FACE ( 'NONE', ( #10093 ), #56195, .T. ) ;
#38353 = DIRECTION ( 'NONE',  ( 1.000000000000000000, 0.000000000000000000, 9.462128050782575008E-16 ) ) ;
#38354 = CARTESIAN_POINT ( 'NONE',  ( 143.7865590713107338, -140.2063866955903393, 246.8245229315576807 ) ) ;
#38357 = CARTESIAN_POINT ( 'NONE',  ( 102.3890460933095454, -47.58756240099337731, 283.2527681330539053 ) ) ;
#38356 = CARTESIAN_POINT ( 'NONE',  ( 142.8698897858160706, -0.9167816978817300289, 540.9756252759101471 ) ) ;
#38355 = CARTESIAN_POINT ( 'NONE',  ( 41.56648329127398966, -27.82844715994070484, 18.92562527591200094 ) ) ;
#38358 = PLANE ( 'NONE',  #61214 ) ;
#38359 = CARTESIAN_POINT ( 'NONE',  ( 50.79999999999999716, 69.84999999999999432, 219.0749999999999886 ) ) ;
#38360 = CARTESIAN_POINT ( 'NONE',  ( -3.175000000000120171, 24.56180297284579694, -33.98325472291460159 ) ) ;
#38361 = CARTESIAN_POINT ( 'NONE',  ( -487.2989999999999782, 10.16305401447644030, 97.63125000000000853 ) ) ;
#38362 = CARTESIAN_POINT ( 'NONE',  ( 167.6524903400755306, -48.32844715993520879, 180.4678068554150059 ) ) ;
#38363 = CYLINDRICAL_SURFACE ( 'NONE', #33289, 2.517500000000005844 ) ;
#38365 = EDGE_LOOP ( 'NONE', ( #73036, #27900 ) ) ;
#38364 = CARTESIAN_POINT ( 'NONE',  ( 98.61271160274297642, -35.32052061661691056, 195.5838068554172082 ) ) ;
#38366 = DIRECTION ( 'NONE',  ( -0.7071067812163274180, 0.7071067811567677275, -2.899137802742863655E-29 ) ) ;
#38367 = CARTESIAN_POINT ( 'NONE',  ( 113.7648918053778715, -44.74678383396227588, 193.1299109901969757 ) ) ;
#38368 = CARTESIAN_POINT ( 'NONE',  ( 115.1668113632844808, -43.29200554620488361, 84.28419670448195689 ) ) ;
#38369 = CARTESIAN_POINT ( 'NONE',  ( 107.2499990610067329, -24.83081552997016317, 226.0641967044829812 ) ) ;
#38370 = DIRECTION ( 'NONE',  ( 0.000000000000000000, 0.000000000000000000, -1.000000000000000000 ) ) ;
#38371 = DIRECTION ( 'NONE',  ( 0.000000000000000000, 1.000000000000000000, 0.000000000000000000 ) ) ;
#38373 = CARTESIAN_POINT ( 'NONE',  ( 115.9153499428093568, -41.43328348718500820, 39.43728031067852413 ) ) ;
#38372 = CARTESIAN_POINT ( 'NONE',  ( -72.96458098368600531, 127.0000000000000000, -72.96458098368781009 ) ) ;
#38374 = CARTESIAN_POINT ( 'NONE',  ( 80.06648329127399677, -18.72944715994105991, -5.074374724089057764 ) ) ;
#38375 = CARTESIAN_POINT ( 'NONE',  ( 62.03715912545744260, -47.82818131006020934, 117.4678068554150485 ) ) ;
#38376 = AXIS2_PLACEMENT_3D ( 'NONE', #18153, #60374, #24975 ) ;
#38377 = CARTESIAN_POINT ( 'NONE',  ( 97.70663229711287556, -40.25150714490782633, 66.61337454916048273 ) ) ;
#38378 = EDGE_CURVE ( 'NONE', #13645, #45890, #63177, .T. ) ;
#38379 = VECTOR ( 'NONE', #38578, 1000.000000000000000 ) ;
#38380 = VERTEX_POINT ( 'NONE', #32300 ) ;
#38381 = ORIENTED_EDGE ( 'NONE', *, *, #89567, .T. ) ;
#38382 = CARTESIAN_POINT ( 'NONE',  ( 100.3410792892688761, -42.04179533522079026, 91.28099125664796532 ) ) ;
#38384 = ORIENTED_EDGE ( 'NONE', *, *, #15684, .F. ) ;
#38383 = DIRECTION ( 'NONE',  ( -1.000000000000000000, 0.000000000000000000, 0.000000000000000000 ) ) ;
#38385 = CARTESIAN_POINT ( 'NONE',  ( 113.3016265961369697, -28.35762455946455773, 100.5670538473389684 ) ) ;
#38386 = FACE_OUTER_BOUND ( 'NONE', #68713, .T. ) ;
#38387 = DIRECTION ( 'NONE',  ( 0.7071067811874278686, -0.7071067811856670549, 6.612322855868390075E-17 ) ) ;
#38388 = LINE ( 'NONE', #3437, #67934 ) ;
#38389 = CARTESIAN_POINT ( 'NONE',  ( 115.3963617111076445, -41.85549503053864839, 18.38705384734096171 ) ) ;
#38390 = ORIENTED_EDGE ( 'NONE', *, *, #15110, .F. ) ;
#38391 = ORIENTED_EDGE ( 'NONE', *, *, #72483, .F. ) ;
#38392 = ORIENTED_EDGE ( 'NONE', *, *, #68168, .F. ) ;
#38393 = AXIS2_PLACEMENT_3D ( 'NONE', #72736, #17329, #44561 ) ;
#38394 = DIRECTION ( 'NONE',  ( 0.000000000000000000, 1.000000000000000000, 0.000000000000000000 ) ) ;
#38395 = VECTOR ( 'NONE', #35371, 999.9999999999998863 ) ;
#38396 = LINE ( 'NONE', #52879, #81032 ) ;
#38397 = CARTESIAN_POINT ( 'NONE',  ( 188.5667039024479834, -48.82844715994099971, 293.2178068554150627 ) ) ;
#38398 = VECTOR ( 'NONE', #31985, 1000.000000000000000 ) ;
#38399 = FACE_OUTER_BOUND ( 'NONE', #60775, .T. ) ;
#38400 = CARTESIAN_POINT ( 'NONE',  ( 72.26949937496601706, -71.54137415153812185, 394.9756252759101471 ) ) ;
#38401 = EDGE_CURVE ( 'NONE', #33618, #11918, #46813, .T. ) ;
#38403 = CARTESIAN_POINT ( 'NONE',  ( 71.06648329127399677, -8.729447159940999512, 17.92562527591199739 ) ) ;
#38402 = AXIS2_PLACEMENT_3D ( 'NONE', #88765, #26523, #55092 ) ;
#38404 = CIRCLE ( 'NONE', #31147, 7.937500000000000000 ) ;
#38405 = CARTESIAN_POINT ( 'NONE',  ( -10.57225270112366822, 89.58687159901970176, 130.1272325585186991 ) ) ;
#38406 = DIRECTION ( 'NONE',  ( -1.000000000000000078E-15, 1.000000000000000083E-30, 1.000000000000000000 ) ) ;
#38407 = CARTESIAN_POINT ( 'NONE',  ( 100.4250012405661039, -28.72198927997973783, 40.62705384733894221 ) ) ;
#38408 = VERTEX_POINT ( 'NONE', #45471 ) ;
#38409 = ADVANCED_FACE ( 'NONE', ( #25500, #80478 ), #12326, .T. ) ;
#38410 = ORIENTED_EDGE ( 'NONE', *, *, #71354, .F. ) ;
#38411 = CARTESIAN_POINT ( 'NONE',  ( 12.37532827966387927, 85.43317223346194567, 129.9681767497193334 ) ) ;
#38412 = CARTESIAN_POINT ( 'NONE',  ( 127.0239848601436279, 53.14682735907139488, 30.16250000000001563 ) ) ;
#38413 = DIRECTION ( 'NONE',  ( -0.000000000000000000, 1.000000000000000000, -0.000000000000000000 ) ) ;
#38414 = CARTESIAN_POINT ( 'NONE',  ( 108.3053489883007927, -28.16931545225084221, 147.7918998934009664 ) ) ;
#38415 = AXIS2_PLACEMENT_3D ( 'NONE', #27406, #12902, #19264 ) ;
#38416 = DIRECTION ( 'NONE',  ( 1.000000000000000000, 0.000000000000000000, 0.000000000000000000 ) ) ;
#38417 = ORIENTED_EDGE ( 'NONE', *, *, #69091, .T. ) ;
#38418 = ORIENTED_EDGE ( 'NONE', *, *, #53536, .T. ) ;
#38419 = EDGE_CURVE ( 'NONE', #70942, #74787, #31408, .T. ) ;
#38420 = DIRECTION ( 'NONE',  ( 0.000000000000000000, -1.000000000000000000, 0.000000000000000000 ) ) ;
#38421 = EDGE_LOOP ( 'NONE', ( #87159, #66098, #55395, #52270 ) ) ;
#38422 = ORIENTED_EDGE ( 'NONE', *, *, #7573, .T. ) ;
#38423 = EDGE_CURVE ( 'NONE', #55083, #22706, #4166, .T. ) ;
#38424 = CARTESIAN_POINT ( 'NONE',  ( 156.5667039024481255, -42.82844715993568485, 254.7178068554149490 ) ) ;
#38425 = CARTESIAN_POINT ( 'NONE',  ( 113.7804517773139708, -30.94577135814159519, 180.8244404487539612 ) ) ;
#38426 = DIRECTION ( 'NONE',  ( 0.7071067811865171526, 0.7071067811865779928, 7.071067811865475333E-16 ) ) ;
#38427 = CARTESIAN_POINT ( 'NONE',  ( 25.56670390244797275, -62.87844715994099687, 293.2178068554150627 ) ) ;
#38428 = VECTOR ( 'NONE', #78414, 1000.000000000000000 ) ;
#38429 = CARTESIAN_POINT ( 'NONE',  ( -111.5664126600051418, 65.66542280838000067, 67.80711950243038189 ) ) ;
#38430 = ORIENTED_EDGE ( 'NONE', *, *, #70071, .F. ) ;
#38431 = EDGE_LOOP ( 'NONE', ( #37223, #26036, #39783, #58328 ) ) ;
#38432 = ORIENTED_EDGE ( 'NONE', *, *, #33170, .F. ) ;
#38433 = CARTESIAN_POINT ( 'NONE',  ( 114.3567987304369495, -40.40109894280344349, 201.2738046553059803 ) ) ;
#38434 = CARTESIAN_POINT ( 'NONE',  ( 109.2596401224901541, -46.98022400537049492, 107.7441967044829880 ) ) ;
#38435 = CARTESIAN_POINT ( 'NONE',  ( 103.4847015977353379, -25.45917443855071838, 55.32133956162594046 ) ) ;
#38436 = CARTESIAN_POINT ( 'NONE',  ( 108.3310854594628125, -46.73512723405534075, 252.6774446765812172 ) ) ;
#38437 = CARTESIAN_POINT ( 'NONE',  ( 116.3232968930447839, -32.93863405887816498, 194.1356252759109680 ) ) ;
#38438 = DIRECTION ( 'NONE',  ( 1.000000000000000000, 4.163336342344333240E-14, 0.000000000000000000 ) ) ;
#38439 = CARTESIAN_POINT ( 'NONE',  ( 117.0170930581839457, -33.62013007832896960, 170.0670538473399631 ) ) ;
#38440 = FACE_BOUND ( 'NONE', #63821, .T. ) ;
#38441 = ORIENTED_EDGE ( 'NONE', *, *, #81037, .F. ) ;
#38442 = PLANE ( 'NONE',  #48156 ) ;
#38443 = EDGE_LOOP ( 'NONE', ( #4037, #80466 ) ) ;
#38444 = ORIENTED_EDGE ( 'NONE', *, *, #57475, .F. ) ;
#38445 = DIRECTION ( 'NONE',  ( 1.000000000000000000, 2.999999999999999839E-15, 1.000000000000000078E-15 ) ) ;
#38446 = EDGE_LOOP ( 'NONE', ( #15241, #5116, #26885, #5789 ) ) ;
#38447 = ORIENTED_EDGE ( 'NONE', *, *, #84885, .T. ) ;
#38448 = LINE ( 'NONE', #24838, #83757 ) ;
#38449 = ORIENTED_EDGE ( 'NONE', *, *, #2499, .F. ) ;
#38450 = CIRCLE ( 'NONE', #84917, 4.762500000000002842 ) ;
#38451 = AXIS2_PLACEMENT_3D ( 'NONE', #28008, #8484, #49344 ) ;
#38452 = DIRECTION ( 'NONE',  ( -1.000000000000000000, 0.000000000000000000, 0.000000000000000000 ) ) ;
#38453 = CARTESIAN_POINT ( 'NONE',  ( 105.9884003220067399, -26.36003215364494423, 50.15848241876796720 ) ) ;
#38454 = DIRECTION ( 'NONE',  ( 1.000000000000000000, 0.000000000000000000, 7.867884063170659983E-16 ) ) ;
#38455 = VECTOR ( 'NONE', #30074, 1000.000000000000000 ) ;
#38456 = ADVANCED_FACE ( 'NONE', ( #40019 ), #73646, .F. ) ;
#38457 = DIRECTION ( 'NONE',  ( -1.000000000000000078E-15, 1.000000000000000083E-30, 1.000000000000000000 ) ) ;
#38458 = DIRECTION ( 'NONE',  ( 0.000000000000000000, 0.000000000000000000, -1.000000000000000000 ) ) ;
#38459 = CARTESIAN_POINT ( 'NONE',  ( 96.71749658230658042, -40.79275330125902599, 96.62419670448296927 ) ) ;
#38461 = CARTESIAN_POINT ( 'NONE',  ( 116.9962961068553113, -33.62662860631130712, 170.0670538473399631 ) ) ;
#38460 = DIRECTION ( 'NONE',  ( 1.639958061481212836E-42, -4.100000000000000342E-29, -1.000000000000000000 ) ) ;
#38462 = CARTESIAN_POINT ( 'NONE',  ( 83.06670390244796920, -64.87844715994098976, 231.5838068554150198 ) ) ;
#38463 = LINE ( 'NONE', #66167, #16297 ) ;
#38464 = VERTEX_POINT ( 'NONE', #73192 ) ;
#38465 = CARTESIAN_POINT ( 'NONE',  ( 164.9190312289449878, -35.91149509761181235, -5.074374724088000832 ) ) ;
#38466 = VECTOR ( 'NONE', #33236, 1000.000000000000000 ) ;
#38467 = CARTESIAN_POINT ( 'NONE',  ( 33.78309357196401663, -29.99615139349950965, 237.4678068554150059 ) ) ;
#38468 = LINE ( 'NONE', #26194, #41497 ) ;
#38469 = AXIS2_PLACEMENT_3D ( 'NONE', #69007, #55349, #27670 ) ;
#38470 = DIRECTION ( 'NONE',  ( -1.000000000000000078E-15, 1.000000000000000083E-30, 1.000000000000000000 ) ) ;
#38472 = ORIENTED_EDGE ( 'NONE', *, *, #57358, .T. ) ;
#38471 = CARTESIAN_POINT ( 'NONE',  ( 101.1758151987629333, -45.38431258166273352, 197.1013395616249966 ) ) ;
#38473 = CARTESIAN_POINT ( 'NONE',  ( -103.1875000000000000, 127.0000000000000000, -1.080832317973422076E-12 ) ) ;
#38474 = CARTESIAN_POINT ( 'NONE',  ( 103.9327720845255669, -26.76365000536165439, 246.3184824187679567 ) ) ;
#38475 = CARTESIAN_POINT ( 'NONE',  ( 114.0511858335762270, -28.93156859308855644, 110.4956252759109816 ) ) ;
#38476 = LINE ( 'NONE', #66179, #1042 ) ;
#38477 = CARTESIAN_POINT ( 'NONE',  ( 81.77795131940523277, -38.88977919477280665, 7.751962620090976586 ) ) ;
#38478 = CIRCLE ( 'NONE', #64562, 10.00000000000000711 ) ;
#38479 = PLANE ( 'NONE',  #67450 ) ;
#38480 = CARTESIAN_POINT ( 'NONE',  ( 140.0667039024470171, -90.27844715994091018, 230.7030882296565721 ) ) ;
#38481 = ORIENTED_EDGE ( 'NONE', *, *, #4149, .T. ) ;
#38482 = ADVANCED_FACE ( 'NONE', ( #11426 ), #67733, .F. ) ;
#38483 = VECTOR ( 'NONE', #26091, 1000.000000000000000 ) ;
#38484 = VERTEX_POINT ( 'NONE', #80039 ) ;
#38485 = ORIENTED_EDGE ( 'NONE', *, *, #65102, .T. ) ;
#38486 = ORIENTED_EDGE ( 'NONE', *, *, #75361, .T. ) ;
#38487 = CARTESIAN_POINT ( 'NONE',  ( 117.0608945231560654, -38.08045312473117860, 73.71895860893197039 ) ) ;
#38488 = CARTESIAN_POINT ( 'NONE',  ( 115.0547525607699697, -30.03093676393617173, 265.3813395616251682 ) ) ;
#38489 = CARTESIAN_POINT ( 'NONE',  ( 119.0814029968458811, -31.76540601701525901, 293.6369201390379544 ) ) ;
#38490 = CARTESIAN_POINT ( 'NONE',  ( 124.7998166246059810, 12.92155284005730387, 358.9756252759109998 ) ) ;
#38491 = ADVANCED_FACE ( 'NONE', ( #81827 ), #60915, .F. ) ;
#38492 = EDGE_CURVE ( 'NONE', #87073, #17863, #46366, .T. ) ;
#38494 = CARTESIAN_POINT ( 'NONE',  ( 112.1400416112072946, -28.01322161120737064, 149.6567520850730943 ) ) ;
#38493 = DIRECTION ( 'NONE',  ( 4.299999999999999979E-14, -1.000000000000000000, 4.400000000000000367E-29 ) ) ;
#38495 = CARTESIAN_POINT ( 'NONE',  ( 115.0883484252707376, -39.66301350383546520, 217.9695626852199837 ) ) ;
#38496 = ORIENTED_EDGE ( 'NONE', *, *, #74313, .T. ) ;
#38497 = EDGE_LOOP ( 'NONE', ( #43797, #74853, #13295 ) ) ;
#38498 = AXIS2_PLACEMENT_3D ( 'NONE', #81824, #19138, #74996 ) ;
#38499 = ORIENTED_EDGE ( 'NONE', *, *, #17102, .T. ) ;
#38500 = CARTESIAN_POINT ( 'NONE',  ( 33.98325472291465132, 24.56180297284579694, 3.174999999999999822 ) ) ;
#38501 = VECTOR ( 'NONE', #11569, 1000.000000000000000 ) ;
#38503 = EDGE_CURVE ( 'NONE', #24616, #30145, #86705, .T. ) ;
#38502 = CARTESIAN_POINT ( 'NONE',  ( 99.50485777685048561, -43.30593340888767528, 181.8960846843701802 ) ) ;
#38504 = CARTESIAN_POINT ( 'NONE',  ( 0.000000000000000000, 17.78000000000000114, 0.000000000000000000 ) ) ;
#38505 = CARTESIAN_POINT ( 'NONE',  ( 106.3742716537777113, -27.86474340539431793, 21.57015473446893949 ) ) ;
#38506 = CARTESIAN_POINT ( 'NONE',  ( 117.9423201497064611, 86.64222086580515736, 12.05142355921225317 ) ) ;
#38507 = CARTESIAN_POINT ( 'NONE',  ( 45.77381068363526850, -48.62134037875087245, 300.4678068554150059 ) ) ;
#38508 = ADVANCED_FACE ( 'NONE', ( #25956 ), #74998, .F. ) ;
#38509 = DIRECTION ( 'NONE',  ( 0.000000000000000000, -1.000000000000000000, 0.000000000000000000 ) ) ;
#38510 = EDGE_LOOP ( 'NONE', ( #39491, #82999, #2575, #65213, #56992, #20013, #11823, #65780, #20125, #86839, #9008, #5326, #66212, #33293, #69473, #89296, #57088, #18228, #26354, #20267 ) ) ;
#38511 = CARTESIAN_POINT ( 'NONE',  ( 103.2771927011866637, -27.47518992547664141, 56.38573900610595047 ) ) ;
#38512 = ORIENTED_EDGE ( 'NONE', *, *, #55287, .T. ) ;
#38513 = CARTESIAN_POINT ( 'NONE',  ( 1.232595164407830946E-29, 69.95000000000000284, 118.3560000000000088 ) ) ;
#38514 = CARTESIAN_POINT ( 'NONE',  ( 105.0496896133374918, -44.66766052993097702, 45.19666179816294971 ) ) ;
#38515 = VECTOR ( 'NONE', #53110, 1000.000000000000000 ) ;
#38516 = AXIS2_PLACEMENT_3D ( 'NONE', #51886, #79642, #66426 ) ;
#38517 = VECTOR ( 'NONE', #68692, 1000.000000000000000 ) ;
#38518 = CARTESIAN_POINT ( 'NONE',  ( -127.5252020268932114, 0.000000000000000000, 177.0380000000000109 ) ) ;
#38519 = VECTOR ( 'NONE', #31248, 1000.000000000000114 ) ;
#38520 = CARTESIAN_POINT ( 'NONE',  ( 23.75871628398702384, 82.54999999999999716, 317.6630000000000109 ) ) ;
#38521 = CARTESIAN_POINT ( 'NONE',  ( -11.00625354133475042, 88.90020661696165405, 118.0441705883949908 ) ) ;
#38522 = AXIS2_PLACEMENT_3D ( 'NONE', #61497, #76031, #82872 ) ;
#38523 = ORIENTED_EDGE ( 'NONE', *, *, #44746, .T. ) ;
#38524 = CARTESIAN_POINT ( 'NONE',  ( 107.0664832912750057, -36.72944715993903486, 9.125625275910969947 ) ) ;
#38525 = EDGE_CURVE ( 'NONE', #11319, #753, #32759, .T. ) ;
#38526 = CARTESIAN_POINT ( 'NONE',  ( 125.3463460965257070, 52.73749999999999716, -36.51249999999992468 ) ) ;
#38527 = VERTEX_POINT ( 'NONE', #88197 ) ;
#38528 = CARTESIAN_POINT ( 'NONE',  ( 114.7262375871959392, -43.80158930977980702, 123.2327681330539519 ) ) ;
#38529 = ORIENTED_EDGE ( 'NONE', *, *, #38419, .F. ) ;
#38530 = ADVANCED_FACE ( 'NONE', ( #53622 ), #88643, .F. ) ;
#38531 = CARTESIAN_POINT ( 'NONE',  ( 98.14502816950557929, -38.28518133910327492, 45.87432458998197404 ) ) ;
#38532 = EDGE_CURVE ( 'NONE', #64255, #40462, #75897, .T. ) ;
#38533 = AXIS2_PLACEMENT_3D ( 'NONE', #68792, #6129, #74267 ) ;
#38534 = CARTESIAN_POINT ( 'NONE',  ( 115.7201795117171628, -41.77810559249323319, 89.40546331780193157 ) ) ;
#38535 = CARTESIAN_POINT ( 'NONE',  ( 99.86128698970316009, -42.75951115570669714, 68.30063092494498278 ) ) ;
#38536 = CARTESIAN_POINT ( 'NONE',  ( 135.9140641843780202, -20.77438500681861910, 2.186796636981966468 ) ) ;
#38537 = CARTESIAN_POINT ( 'NONE',  ( 33.91903122894598965, -35.91149509761320502, 342.9256252759109884 ) ) ;
#38538 = ADVANCED_FACE ( 'NONE', ( #49058 ), #84068, .T. ) ;
#38539 = CARTESIAN_POINT ( 'NONE',  ( 147.0789628650053089, -69.17499946017579759, 247.4285673639549827 ) ) ;
#38540 = CARTESIAN_POINT ( 'NONE',  ( 111.4245298313290107, -46.22390286880558818, 23.91848241876792969 ) ) ;
#38541 = FACE_BOUND ( 'NONE', #78517, .T. ) ;
#38542 = VERTEX_POINT ( 'NONE', #61352 ) ;
#38543 = DIRECTION ( 'NONE',  ( -0.7071067811865463515, -0.7071067811865487940, 0.000000000000000000 ) ) ;
#38544 = ORIENTED_EDGE ( 'NONE', *, *, #8097, .F. ) ;
#38545 = CARTESIAN_POINT ( 'NONE',  ( 77.58678459499434155, -19.92005462651998826, 2.747931806390634168 ) ) ;
#38546 = ORIENTED_EDGE ( 'NONE', *, *, #39896, .F. ) ;
#38547 = VECTOR ( 'NONE', #56358, 1000.000000000000000 ) ;
#38548 = ORIENTED_EDGE ( 'NONE', *, *, #52113, .T. ) ;
#38549 = FACE_OUTER_BOUND ( 'NONE', #10189, .T. ) ;
#38550 = ORIENTED_EDGE ( 'NONE', *, *, #25364, .F. ) ;
#38551 = CARTESIAN_POINT ( 'NONE',  ( 103.5361331145922890, -27.60804031003065262, 215.3699109901969848 ) ) ;
#38552 = CARTESIAN_POINT ( 'NONE',  ( -27.27158787008326968, 127.0000000000000000, -0.000000000000000000 ) ) ;
#38553 = CARTESIAN_POINT ( 'NONE',  ( 74.68590766205718978, -67.87844715994097555, 245.5622121773279787 ) ) ;
#38554 = CARTESIAN_POINT ( 'NONE',  ( 103.4771999316985500, -25.43557003456049870, 51.32133956162493149 ) ) ;
#38555 = CARTESIAN_POINT ( 'NONE',  ( 71.77848634863079269, 127.0000000000000000, 77.39114642429989033 ) ) ;
#38556 = ORIENTED_EDGE ( 'NONE', *, *, #59814, .F. ) ;
#38557 = CARTESIAN_POINT ( 'NONE',  ( 103.9658006590860992, -27.21632154753857691, 171.3272140054234853 ) ) ;
#38558 = DIRECTION ( 'NONE',  ( 1.639958061481212836E-42, -4.100000000000000342E-29, -1.000000000000000000 ) ) ;
#38559 = VERTEX_POINT ( 'NONE', #76790 ) ;
#38560 = DIRECTION ( 'NONE',  ( 9.351236661543306751E-17, -3.725950533538267725E-29, -1.000000000000000000 ) ) ;
#38561 = CARTESIAN_POINT ( 'NONE',  ( 179.7974245136209959, -36.32844715993469009, 193.9678068554150059 ) ) ;
#38563 = AXIS2_PLACEMENT_3D ( 'NONE', #12527, #24814, #46474 ) ;
#38562 = CARTESIAN_POINT ( 'NONE',  ( 117.4688788178166732, -35.86077403649778006, 253.8927681330538348 ) ) ;
#38564 = CARTESIAN_POINT ( 'NONE',  ( 32.06670390244660496, -32.29483332968541731, 313.9678068554150059 ) ) ;
#38565 = B_SPLINE_CURVE_WITH_KNOTS ( 'NONE', 3,
 ( #67935, #26594, #54273, #4376, #4818, #5720, #82038, #46123, #38878, #19788, #32064, #73850, #80237, #32961, #60656, #81591, #39330, #10724, #52913, #53378, #11173, #19342, #47017, #17988, #80682, #12528, #38429, #70174, #41111, #6169, #21595, #33857, #7950, #28850, #34755, #82488, #47915, #681, #13426, #7061, #27053, #27938, #14329, #20242, #75657, #7507, #77001, #35649, #83822, #234, #55166, #56533, #27491, #83367, #68837, #21139, #49267, #63361, #22052, #69287, #28386, #75203, #6605, #34301, #48810, #61553, #12984, #40671, #14784, #42006, #76546, #76092, #69737, #89289, #62902, #84279, #13869, #56072, #62460, #62009, #68392, #35191, #42449, #1144, #41549, #54725, #89744, #55614, #82929, #20688, #48356, #84728, #71978, #51498, #72421, #58331, #64710, #29749, #31065, #2041, #57887, #85620, #23828, #10186 ),
 .UNSPECIFIED., .F., .F.,
 ( 4, 2, 1, 1, 2, 2, 2, 1, 1, 1, 2, 2, 2, 1, 1, 1, 2, 2, 2, 1, 1, 2, 2, 2, 1, 1, 2, 2, 2, 2, 2, 1, 1, 1, 2, 2, 1, 1, 2, 2, 2, 1, 1, 2, 2, 2, 1, 2, 2, 2, 1, 2, 2, 2, 1, 2, 2, 2, 2, 2, 2, 2, 4 ),
 ( 0.000000000000000000, 0.03124999999999297784, 0.04687499999998949451, 0.05468749999998755856, 0.05859374999998673977, 0.06249999999998591405, 0.09374999999997923883, 0.1093749999999759082, 0.1171874999999741596, 0.1210937499999732714, 0.1230468749999728273, 0.1249999999999723832, 0.1562499999999672207, 0.1718749999999646949, 0.1796874999999637790, 0.1835937499999631961, 0.1855468749999625577, 0.1874999999999619194, 0.2187499999999570899, 0.2343749999999545641, 0.2421874999999530931, 0.2460937499999527045, 0.2499999999999522604, 0.2812499999999505396, 0.2968749999999500400, 0.3046874999999500400, 0.3085937499999499845, 0.3124999999999499289, 0.3437499999999493738, 0.3749999999999488742, 0.4374999999999475975, 0.4687499999999467648, 0.4843749999999463207, 0.4921874999999461542, 0.4960937499999459876, 0.4999999999999458211, 0.5312499999999467093, 0.5468749999999470424, 0.5546874999999472644, 0.5624999999999474865, 0.5937499999999481526, 0.6093749999999482636, 0.6171874999999482636, 0.6210937499999483746, 0.6249999999999484857, 0.6562499999999525935, 0.6718749999999547029, 0.6796874999999555911, 0.6874999999999564793, 0.7187499999999598099, 0.7343749999999615863, 0.7421874999999624745, 0.7499999999999633626, 0.7812499999999671374, 0.7968749999999690248, 0.8046874999999700240, 0.8124999999999710232, 0.8437499999999762412, 0.8749999999999814593, 0.9062499999999863443, 0.9218749999999886757, 0.9374999999999910072, 1.000000000000000000 ),
 .UNSPECIFIED. ) ;
#38566 = DIRECTION ( 'NONE',  ( 0.000000000000000000, -1.000000000000000000, 0.000000000000000000 ) ) ;
#38567 = CARTESIAN_POINT ( 'NONE',  ( 77.33253953643580303, -37.07457063615774473, 3.076560393663061443 ) ) ;
#38568 = CARTESIAN_POINT ( 'NONE',  ( 105.3911398957759076, -27.82967838469355115, 279.6590864947435762 ) ) ;
#38570 = CARTESIAN_POINT ( 'NONE',  ( 115.1902516771092451, -44.19056033372781656, 74.22324432352993995 ) ) ;
#38569 = CARTESIAN_POINT ( 'NONE',  ( 119.5435152932140426, -31.57448135767196362, 290.1356252759106837 ) ) ;
#38571 = CARTESIAN_POINT ( 'NONE',  ( 116.2447374730602547, 72.73035545477121389, 59.43458213646708543 ) ) ;
#38572 = CARTESIAN_POINT ( 'NONE',  ( 98.42220671263785903, -30.82325138971081557, 120.8499109901969604 ) ) ;
#38573 = EDGE_LOOP ( 'NONE', ( #66133, #60164, #83433, #68475, #78547, #25003, #53534, #49778, #573, #14199, #89047, #51718 ) ) ;
#38574 = DIRECTION ( 'NONE',  ( 0.000000000000000000, 1.000000000000000000, 0.000000000000000000 ) ) ;
#38575 = VERTEX_POINT ( 'NONE', #61798 ) ;
#38576 = LINE ( 'NONE', #59461, #83091 ) ;
#38577 = FACE_BOUND ( 'NONE', #40905, .T. ) ;
#38578 = DIRECTION ( 'NONE',  ( -0.7071067811864676367, -0.7071067811866273978, -7.071067811864981309E-16 ) ) ;
#38579 = VERTEX_POINT ( 'NONE', #20041 ) ;
#38580 = CARTESIAN_POINT ( 'NONE',  ( 97.81169138727440782, -40.51741131469341184, 51.63568823874075520 ) ) ;
#38582 = VERTEX_POINT ( 'NONE', #89535 ) ;
#38581 = CARTESIAN_POINT ( 'NONE',  ( 118.9539009387050186, -36.16544432761327954, 118.8641967044819836 ) ) ;
#38583 = CARTESIAN_POINT ( 'NONE',  ( 63.03715912545741418, -46.82818131006016671, 116.4678068554151054 ) ) ;
#38584 = VECTOR ( 'NONE', #10173, 1000.000000000000114 ) ;
#38585 = DIRECTION ( 'NONE',  ( 0.000000000000000000, 1.000000000000000000, 0.000000000000000000 ) ) ;
#38587 = AXIS2_PLACEMENT_3D ( 'NONE', #31929, #12852, #60519 ) ;
#38586 = CARTESIAN_POINT ( 'NONE',  ( 134.0664832912740110, -8.350947159940998787, 296.1531252759119752 ) ) ;
#38588 = ORIENTED_EDGE ( 'NONE', *, *, #63517, .F. ) ;
#38589 = CARTESIAN_POINT ( 'NONE',  ( 98.43795593625375773, -42.68233540891471023, 126.8070538473389490 ) ) ;
#38590 = VECTOR ( 'NONE', #31803, 1000.000000000000000 ) ;
#38592 = EDGE_CURVE ( 'NONE', #36440, #27470, #14119, .T. ) ;
#38591 = AXIS2_PLACEMENT_3D ( 'NONE', #25009, #52672, #32709 ) ;
#38593 =( LENGTH_UNIT ( ) NAMED_UNIT ( * ) SI_UNIT ( .MILLI., .METRE. ) );
#38594 = CIRCLE ( 'NONE', #67579, 13.09746158385919124 ) ;
#38595 = LINE ( 'NONE', #4080, #54432 ) ;
#38596 = ADVANCED_FACE ( 'NONE', ( #41795 ), #47717, .T. ) ;
#38597 = DIRECTION ( 'NONE',  ( 1.000000000000000000, 0.000000000000000000, 0.000000000000000000 ) ) ;
#38598 = ORIENTED_EDGE ( 'NONE', *, *, #19953, .F. ) ;
#38599 = EDGE_CURVE ( 'NONE', #64255, #44076, #56321, .T. ) ;
#38600 = ORIENTED_EDGE ( 'NONE', *, *, #81571, .T. ) ;
#38601 = DIRECTION ( 'NONE',  ( 0.000000000000000000, 1.000000000000000000, 0.000000000000000000 ) ) ;
#38602 = CARTESIAN_POINT ( 'NONE',  ( -72.96458098368600531, 117.4749999999999943, -80.90208098368781009 ) ) ;
#38603 = CARTESIAN_POINT ( 'NONE',  ( 180.3503142329310265, -29.99615139349890569, -5.074374724088000832 ) ) ;
#38604 = EDGE_CURVE ( 'NONE', #87723, #40273, #60547, .T. ) ;
#38605 = EDGE_CURVE ( 'NONE', #5006, #56141, #56593, .T. ) ;
#38607 = DIRECTION ( 'NONE',  ( -1.000000000000000078E-15, 0.000000000000000000, 1.000000000000000000 ) ) ;
#38606 = DIRECTION ( 'NONE',  ( 0.000000000000000000, -0.9961946980917455452, -0.08715574274765836016 ) ) ;
#38608 = LINE ( 'NONE', #17731, #63980 ) ;
#38609 = VECTOR ( 'NONE', #15224, 999.9999999999998863 ) ;
#38610 = EDGE_CURVE ( 'NONE', #57647, #46563, #72182, .T. ) ;
#38611 = VERTEX_POINT ( 'NONE', #40 ) ;
#38612 = AXIS2_PLACEMENT_3D ( 'NONE', #51119, #50680, #17941 ) ;
#38614 = EDGE_CURVE ( 'NONE', #8963, #12604, #56261, .T. ) ;
#38613 = CYLINDRICAL_SURFACE ( 'NONE', #34627, 0.5000000000000004441 ) ;
#38615 = CARTESIAN_POINT ( 'NONE',  ( 113.3375292005773929, -44.23527279707077042, 189.1299109901959525 ) ) ;
#38617 = ORIENTED_EDGE ( 'NONE', *, *, #74580, .T. ) ;
#38616 = LINE ( 'NONE', #81764, #9509 ) ;
#38618 = CARTESIAN_POINT ( 'NONE',  ( 116.8124865092210456, -37.88235468918157522, 49.73276813305294297 ) ) ;
#38619 = CARTESIAN_POINT ( 'NONE',  ( 104.4079370647588547, -46.45804145048838052, 52.36485282198370328 ) ) ;
#38620 = DIRECTION ( 'NONE',  ( 4.194175870806139918E-14, -1.000000000000000000, 0.000000000000000000 ) ) ;
#38621 = EDGE_CURVE ( 'NONE', #62011, #13421, #82731, .T. ) ;
#38622 = CARTESIAN_POINT ( 'NONE',  ( 179.8608231853568213, -35.55794170701179269, 237.4678068554150059 ) ) ;
#38623 = VERTEX_POINT ( 'NONE', #54521 ) ;
#38624 = CARTESIAN_POINT ( 'NONE',  ( -160.2664750769294812, 20.32000000000000028, -148.0533267522755807 ) ) ;
#38625 = ORIENTED_EDGE ( 'NONE', *, *, #22638, .F. ) ;
#38626 = ORIENTED_EDGE ( 'NONE', *, *, #28415, .T. ) ;
#38627 = CARTESIAN_POINT ( 'NONE',  ( 107.2166699364993292, -45.61986748510933865, 209.0215833058969963 ) ) ;
#38628 = DIRECTION ( 'NONE',  ( 0.7071067811865046071, 0.7071067811865904273, 7.071067811865039488E-16 ) ) ;
#38629 = CARTESIAN_POINT ( 'NONE',  ( -118.5451175586562158, 95.14807216649715826, -1.659552426423821503 ) ) ;
#38630 = DIRECTION ( 'NONE',  ( 0.000000000000000000, 0.000000000000000000, -1.000000000000000000 ) ) ;
#38631 = DIRECTION ( 'NONE',  ( -1.000000000000000000, 0.000000000000000000, 0.000000000000000000 ) ) ;
#38632 = ORIENTED_EDGE ( 'NONE', *, *, #63522, .T. ) ;
#38633 = DIRECTION ( 'NONE',  ( -0.000000000000000000, -1.000000000000000000, -0.000000000000000000 ) ) ;
#38634 = CARTESIAN_POINT ( 'NONE',  ( 99.09325496367249286, -30.55370301960245527, 36.80227106180009145 ) ) ;
#38635 = ORIENTED_EDGE ( 'NONE', *, *, #41981, .F. ) ;
#38636 = CARTESIAN_POINT ( 'NONE',  ( 102.7552189479022928, -25.69072042043729098, 20.37276813305294354 ) ) ;
#38637 = CARTESIAN_POINT ( 'NONE',  ( 7.394472951914207393, 92.88361795698580181, 118.3256787633386296 ) ) ;
#38638 = ORIENTED_EDGE ( 'NONE', *, *, #21220, .F. ) ;
#38639 = EDGE_CURVE ( 'NONE', #74526, #19430, #6401, .T. ) ;
#38640 = CARTESIAN_POINT ( 'NONE',  ( 107.7702177616926065, 120.6499999999999915, 4.179089330879380409E-13 ) ) ;
#38641 = CARTESIAN_POINT ( 'NONE',  ( 31.71315051185499811, -33.70561438052090608, -5.074374724088000832 ) ) ;
#38642 = DIRECTION ( 'NONE',  ( -0.7071067811866279529, 0.7071067811864671926, -7.071067811866286874E-16 ) ) ;
#38644 = EDGE_CURVE ( 'NONE', #51938, #73307, #34994, .T. ) ;
#38643 = CARTESIAN_POINT ( 'NONE',  ( 115.0439452383991892, -99.09543445804983719, -19.78219314458218392 ) ) ;
#38645 = AXIS2_PLACEMENT_3D ( 'NONE', #63820, #1598, #29303 ) ;
#38646 = CARTESIAN_POINT ( 'NONE',  ( 110.7114656039092893, -48.05751922203765503, 203.8241967044819489 ) ) ;
#38648 = DIRECTION ( 'NONE',  ( 0.000000000000000000, 0.000000000000000000, 1.000000000000000000 ) ) ;
#38647 = AXIS2_PLACEMENT_3D ( 'NONE', #41858, #62767, #62321 ) ;
#38649 = ORIENTED_EDGE ( 'NONE', *, *, #83858, .F. ) ;
#38650 = VECTOR ( 'NONE', #34560, 1000.000000000000114 ) ;
#38651 = CARTESIAN_POINT ( 'NONE',  ( 96.67154112854022685, -38.24047072676557946, 62.44133956162495025 ) ) ;
#38652 = VECTOR ( 'NONE', #56961, 1000.000000000000000 ) ;
#38653 = DIRECTION ( 'NONE',  ( 0.000000000000000000, 0.000000000000000000, -1.000000000000000000 ) ) ;
#38654 = AXIS2_PLACEMENT_3D ( 'NONE', #12733, #4571, #67688 ) ;
#38655 = VERTEX_POINT ( 'NONE', #28176 ) ;
#38656 = ORIENTED_EDGE ( 'NONE', *, *, #85183, .T. ) ;
#38657 = ORIENTED_EDGE ( 'NONE', *, *, #53234, .F. ) ;
#38658 = CARTESIAN_POINT ( 'NONE',  ( 80.06648329127399677, -15.97944715994105813, 1.625625275910943746 ) ) ;
#38659 = CARTESIAN_POINT ( 'NONE',  ( 116.8182710663954254, -34.15736811344609691, 154.0318915783644513 ) ) ;
#38660 = CARTESIAN_POINT ( 'NONE',  ( 111.9717725103620722, -43.25385221418022752, 140.9080903695919460 ) ) ;
#38661 = CARTESIAN_POINT ( 'NONE',  ( 107.5109549264149251, -47.16686560604517098, 233.6099109901969655 ) ) ;
#38662 = CARTESIAN_POINT ( 'NONE',  ( -487.2989999999999782, 93.66249999999999432, 90.48749999999999716 ) ) ;
#38663 = VERTEX_POINT ( 'NONE', #41351 ) ;
#38664 = CIRCLE ( 'NONE', #5288, 2.517500000000005844 ) ;
#38665 = CARTESIAN_POINT ( 'NONE',  ( 136.6368519841214777, -37.70758306363786971, 2.855952960430258258 ) ) ;
#38666 = ORIENTED_EDGE ( 'NONE', *, *, #82015, .T. ) ;
#38667 = ORIENTED_EDGE ( 'NONE', *, *, #13261, .F. ) ;
#38668 = FACE_OUTER_BOUND ( 'NONE', #18583, .T. ) ;
#38669 = ORIENTED_EDGE ( 'NONE', *, *, #22463, .F. ) ;
#38670 = VERTEX_POINT ( 'NONE', #33662 ) ;
#38671 = FACE_OUTER_BOUND ( 'NONE', #25458, .T. ) ;
#38672 = CARTESIAN_POINT ( 'NONE',  ( -479.3614999999999782, 22.53639197104660141, 90.48749999999999716 ) ) ;
#38673 = CARTESIAN_POINT ( 'NONE',  ( 99.09504479792080645, -30.55131775994448873, 25.80237912473876349 ) ) ;
#38674 = CARTESIAN_POINT ( 'NONE',  ( 113.1264120695652622, -29.99967374510735141, 158.9276579233149391 ) ) ;
#38675 = CARTESIAN_POINT ( 'NONE',  ( 116.1968789481791191, -43.04691504047773520, 13.35657765686298859 ) ) ;
#38676 = EDGE_LOOP ( 'NONE', ( #5589, #21526, #12030, #148 ) ) ;
#38677 = CARTESIAN_POINT ( 'NONE',  ( -89.55818655986118415, 72.98405218941672956, -77.68655577178692795 ) ) ;
#38678 = VERTEX_POINT ( 'NONE', #69980 ) ;
#38679 = DIRECTION ( 'NONE',  ( 0.000000000000000000, 0.000000000000000000, -1.000000000000000000 ) ) ;
#38680 = ORIENTED_EDGE ( 'NONE', *, *, #74708, .T. ) ;
#38681 = CARTESIAN_POINT ( 'NONE',  ( 83.06670390244802604, -43.72944715994108122, 231.5838068554169524 ) ) ;
#38682 = CARTESIAN_POINT ( 'NONE',  ( -2.061562449364020999, 70.11297175739061061, 118.5387631950859344 ) ) ;
#38683 = DIRECTION ( 'NONE',  ( 0.000000000000000000, 0.000000000000000000, 1.000000000000000000 ) ) ;
#38684 = EDGE_CURVE ( 'NONE', #38195, #84879, #35439, .T. ) ;
#38685 = AXIS2_PLACEMENT_3D ( 'NONE', #8782, #1517, #77360 ) ;
#38686 = LINE ( 'NONE', #39583, #10360 ) ;
#38687 = ORIENTED_EDGE ( 'NONE', *, *, #19453, .F. ) ;
#38688 = CARTESIAN_POINT ( 'NONE',  ( 99.04884357002234196, -44.37228004027687689, 36.92038718067297509 ) ) ;
#38689 = CARTESIAN_POINT ( 'NONE',  ( 115.7091107927249283, -43.69381994074442588, 39.27467289495895386 ) ) ;
#38690 = EDGE_CURVE ( 'NONE', #13441, #72100, #44668, .T. ) ;
#38692 = CARTESIAN_POINT ( 'NONE',  ( 68.74524693519704499, -139.2530727251857456, 246.1985092402615862 ) ) ;
#38691 = LINE ( 'NONE', #37367, #44795 ) ;
#38693 = CARTESIAN_POINT ( 'NONE',  ( 105.9487191471789060, -25.32458681355470276, 323.3977233678749030 ) ) ;
#38694 = ADVANCED_FACE ( 'NONE', ( #21839 ), #12781, .F. ) ;
#38695 = DIRECTION ( 'NONE',  ( 0.000000000000000000, 0.000000000000000000, 1.000000000000000000 ) ) ;
#38696 = CARTESIAN_POINT ( 'NONE',  ( 133.6896269580427656, -39.47945062088879808, 8.225625248534990774 ) ) ;
#38697 = ADVANCED_FACE ( 'NONE', ( #84526 ), #37248, .T. ) ;
#38698 = DIRECTION ( 'NONE',  ( 0.000000000000000000, 0.000000000000000000, 1.000000000000000000 ) ) ;
#38699 = CARTESIAN_POINT ( 'NONE',  ( 145.6354771369172170, -101.1103950255152171, 247.6425393530529959 ) ) ;
#38700 = EDGE_CURVE ( 'NONE', #71527, #28720, #22284, .T. ) ;
#38701 = CARTESIAN_POINT ( 'NONE',  ( 115.6474790210939290, -28.48352029850561706, 39.43562527591099354 ) ) ;
#38702 = CARTESIAN_POINT ( 'NONE',  ( 101.3491664457538945, -46.18916536780651683, 198.1318157521009482 ) ) ;
#38703 = CARTESIAN_POINT ( 'NONE',  ( 104.0364404988798270, -47.38327494250712135, 63.36800622829197494 ) ) ;
#38704 = VECTOR ( 'NONE', #2157, 1000.000000000000000 ) ;
#38706 = DIRECTION ( 'NONE',  ( 0.000000000000000000, 0.000000000000000000, 1.000000000000000000 ) ) ;
#38705 = DIRECTION ( 'NONE',  ( 1.000000000000000000, 0.000000000000000000, 2.108231265501709878E-16 ) ) ;
#38707 = LINE ( 'NONE', #61390, #78456 ) ;
#38708 = EDGE_CURVE ( 'NONE', #52826, #30532, #80949, .T. ) ;
#38709 = AXIS2_PLACEMENT_3D ( 'NONE', #70217, #7989, #28890 ) ;
#38710 = VECTOR ( 'NONE', #60988, 1000.000000000000000 ) ;
#38711 = AXIS2_PLACEMENT_3D ( 'NONE', #74850, #38971, #18526 ) ;
#38712 = ORIENTED_EDGE ( 'NONE', *, *, #82732, .F. ) ;
#38713 = CARTESIAN_POINT ( 'NONE',  ( 97.31584368363401438, -39.30597587385430103, 187.5314585990350906 ) ) ;
#38714 = ORIENTED_EDGE ( 'NONE', *, *, #53476, .T. ) ;
#38715 = EDGE_CURVE ( 'NONE', #43667, #43353, #12795, .T. ) ;
#38716 = CARTESIAN_POINT ( 'NONE',  ( 102.5967720069230893, -27.99243076246528261, 116.4527681330529703 ) ) ;
#38718 = ORIENTED_EDGE ( 'NONE', *, *, #53885, .T. ) ;
#38717 = CARTESIAN_POINT ( 'NONE',  ( 11.53693603528213529, 87.86025992443330779, 130.0452829984675134 ) ) ;
#38719 = CARTESIAN_POINT ( 'NONE',  ( 21.03689327557705369, -23.42844715994186089, 313.9678068554150059 ) ) ;
#38720 = CARTESIAN_POINT ( 'NONE',  ( 111.1189502094634776, -27.14789314160936229, 240.7584824187679544 ) ) ;
#38721 = DIRECTION ( 'NONE',  ( 0.000000000000000000, 0.000000000000000000, -1.000000000000000000 ) ) ;
#38722 = PRODUCT ( 'Pneumatic Toggle Clamp Unit', 'Pneumatic Toggle Clamp Unit', '', ( #39039 ) ) ;
#38723 = DIRECTION ( 'NONE',  ( -0.7071067811865444641, 0.000000000000000000, 0.7071067811865505703 ) ) ;
#38724 = CARTESIAN_POINT ( 'NONE',  ( 69.72411017813010403, 120.6499999999999915, -69.72411017812979139 ) ) ;
#38725 = DIRECTION ( 'NONE',  ( 0.000000000000000000, 0.000000000000000000, 1.000000000000000000 ) ) ;
#38726 = ADVANCED_FACE ( 'NONE', ( #9989 ), #30875, .F. ) ;
#38727 = CARTESIAN_POINT ( 'NONE',  ( 107.0667039024470313, -104.2784471599418197, -11.78219314458200984 ) ) ;
#38728 = CARTESIAN_POINT ( 'NONE',  ( -84.19388261207966195, 76.18750001922977333, 99.78212687779766554 ) ) ;
#38730 = CARTESIAN_POINT ( 'NONE',  ( 98.64540312569886282, -41.76920806142285159, 161.7556252759109725 ) ) ;
#38729 = VECTOR ( 'NONE', #72655, 1000.000000000000000 ) ;
#38731 = ORIENTED_EDGE ( 'NONE', *, *, #10532, .T. ) ;
#38732 = ORIENTED_EDGE ( 'NONE', *, *, #39133, .T. ) ;
#38733 = CARTESIAN_POINT ( 'NONE',  ( 112.4631721614844651, -29.03839555594388955, 81.00920235351600240 ) ) ;
#38734 = AXIS2_PLACEMENT_3D ( 'NONE', #32828, #54587, #61866 ) ;
#38735 = LINE ( 'NONE', #30149, #22597 ) ;
#38737 = FACE_OUTER_BOUND ( 'NONE', #41504, .T. ) ;
#38736 = CARTESIAN_POINT ( 'NONE',  ( 97.17009264939177626, -31.66255117090388538, 241.9499109901959741 ) ) ;
#38738 = DIRECTION ( 'NONE',  ( 1.821299053822143307E-16, 0.000000000000000000, -1.000000000000000000 ) ) ;
#38739 = CARTESIAN_POINT ( 'NONE',  ( 107.0667039024470313, -104.2784471599413791, 2.217806855418003043 ) ) ;
#38740 = B_SPLINE_CURVE_WITH_KNOTS ( 'NONE', 3,
 ( #76986, #82914, #40657, #6156, #48796, #61540, #55153, #75189, #12970, #221, #20675, #48343, #14766, #56059, #19774, #89276, #82024, #55602 ),
 .UNSPECIFIED., .F., .F.,
 ( 4, 2, 2, 2, 2, 2, 2, 2, 4 ),
 ( 0.4999695546683612934, 0.5624733603348160971, 0.6249771660012709562, 0.6874809716677258153, 0.7499847773341805635, 0.8124885830006354226, 0.8749923886670902817, 0.9374961943335451409, 1.000000000000000000 ),
 .UNSPECIFIED. ) ;
#38741 = CARTESIAN_POINT ( 'NONE',  ( 118.2594037030538772, 73.00424585431355240, 8.387096233284163205 ) ) ;
#38742 = CARTESIAN_POINT ( 'NONE',  ( -10.09803707135884210, 74.80381226467314093, 118.1260670069656271 ) ) ;
#38743 = LINE ( 'NONE', #53237, #1429 ) ;
#38744 = FACE_OUTER_BOUND ( 'NONE', #17150, .T. ) ;
#38745 = CARTESIAN_POINT ( 'NONE',  ( 109.3536845750984412, -25.93905639472648872, 184.9222919425779708 ) ) ;
#38746 = VERTEX_POINT ( 'NONE', #65395 ) ;
#38747 = ORIENTED_EDGE ( 'NONE', *, *, #70202, .F. ) ;
#38748 = DIRECTION ( 'NONE',  ( 0.000000000000000000, 0.000000000000000000, -1.000000000000000000 ) ) ;
#38749 = CARTESIAN_POINT ( 'NONE',  ( 146.8415613695535171, -68.09268944053143002, 246.4109134068758067 ) ) ;
#38750 = DIRECTION ( 'NONE',  ( 0.000000000000000000, 0.000000000000000000, 1.000000000000000000 ) ) ;
#38752 = EDGE_CURVE ( 'NONE', #223, #55129, #15476, .T. ) ;
#38751 = CARTESIAN_POINT ( 'NONE',  ( 115.0439452383992318, -109.4614598618342853, -19.78219314458184996 ) ) ;
#38753 = AXIS2_PLACEMENT_3D ( 'NONE', #12581, #27988, #40268 ) ;
#38754 = ORIENTED_EDGE ( 'NONE', *, *, #2732, .T. ) ;
#38755 = DIRECTION ( 'NONE',  ( 1.000000000000000000, 0.000000000000000000, 0.000000000000000000 ) ) ;
#38756 = CARTESIAN_POINT ( 'NONE',  ( 106.9749943965245365, -47.15435292659226718, 187.5699109901969734 ) ) ;
#38757 = DIRECTION ( 'NONE',  ( 0.000000000000000000, 0.000000000000000000, -1.000000000000000000 ) ) ;
#38758 = ORIENTED_EDGE ( 'NONE', *, *, #13176, .T. ) ;
#38760 = EDGE_LOOP ( 'NONE', ( #63978, #48879, #70858 ) ) ;
#38759 = ORIENTED_EDGE ( 'NONE', *, *, #40752, .F. ) ;
#38761 = CARTESIAN_POINT ( 'NONE',  ( 98.40642892645681172, -41.73694030736349703, 62.74414883732655568 ) ) ;
#38762 = LINE ( 'NONE', #73738, #57261 ) ;
#38763 = DIRECTION ( 'NONE',  ( 1.000000000000000000, 4.163336342344333240E-14, 0.000000000000000000 ) ) ;
#38764 = CARTESIAN_POINT ( 'NONE',  ( 106.2223766104409037, -28.61050573088338922, 47.97666179816295795 ) ) ;
#38765 = CARTESIAN_POINT ( 'NONE',  ( 188.5667039024479834, -65.37844715994100397, 142.0928068554150059 ) ) ;
#38766 = ORIENTED_EDGE ( 'NONE', *, *, #47399, .T. ) ;
#38767 = EDGE_CURVE ( 'NONE', #9022, #14474, #23632, .T. ) ;
#38768 = AXIS2_PLACEMENT_3D ( 'NONE', #63934, #8072, #57550 ) ;
#38769 = DIRECTION ( 'NONE',  ( -0.9254794337955620787, -0.3787978585227822492, 0.000000000000000000 ) ) ;
#38770 = LINE ( 'NONE', #81039, #28530 ) ;
#38771 = ORIENTED_EDGE ( 'NONE', *, *, #24983, .T. ) ;
#38772 = ORIENTED_EDGE ( 'NONE', *, *, #27601, .T. ) ;
#38773 = VECTOR ( 'NONE', #65079, 1000.000000000000114 ) ;
#38774 = VECTOR ( 'NONE', #81097, 1000.000000000000000 ) ;
#38775 = PLANE ( 'NONE',  #66215 ) ;
#38776 = ORIENTED_EDGE ( 'NONE', *, *, #10196, .T. ) ;
#38777 = ORIENTED_EDGE ( 'NONE', *, *, #36905, .F. ) ;
#38778 = FACE_OUTER_BOUND ( 'NONE', #9554, .T. ) ;
#38779 = CARTESIAN_POINT ( 'NONE',  ( 97.39259002536323351, -35.90094442973985167, 35.68099125664797810 ) ) ;
#38780 = CARTESIAN_POINT ( 'NONE',  ( 107.6557532049571932, -47.79055931493532938, 197.6308633711489620 ) ) ;
#38781 = CARTESIAN_POINT ( 'NONE',  ( 101.9826776100855454, -46.51815199768669373, 167.1832443235299763 ) ) ;
#38782 = CARTESIAN_POINT ( 'NONE',  ( -479.3614999999999782, 18.41194598552324990, 83.34375000000000000 ) ) ;
#38784 = CARTESIAN_POINT ( 'NONE',  ( 117.4297252914212066, -35.59555830959087075, 274.9127681330538735 ) ) ;
#38783 = FACE_OUTER_BOUND ( 'NONE', #22806, .T. ) ;
#38785 = CARTESIAN_POINT ( 'NONE',  ( 42.66648329127298922, 12.92155284005730387, 358.9756252759109998 ) ) ;
#38786 = LINE ( 'NONE', #52386, #29389 ) ;
#38787 = ORIENTED_EDGE ( 'NONE', *, *, #32415, .F. ) ;
#38788 = VECTOR ( 'NONE', #4949, 999.9999999999998863 ) ;
#38789 = ORIENTED_EDGE ( 'NONE', *, *, #67409, .T. ) ;
#38790 = VECTOR ( 'NONE', #25909, 1000.000000000000000 ) ;
#38791 = VECTOR ( 'NONE', #47601, 1000.000000000000000 ) ;
#38792 = CIRCLE ( 'NONE', #38734, 3.300000000000000711 ) ;
#38793 = CARTESIAN_POINT ( 'NONE',  ( 97.81556692073944248, -40.52688746123195074, 111.6364388057383792 ) ) ;
#38794 = CARTESIAN_POINT ( 'NONE',  ( 104.3127904766024443, -25.97630531626002437, 245.2880062282919482 ) ) ;
#38795 = ORIENTED_EDGE ( 'NONE', *, *, #22416, .T. ) ;
#38796 = CARTESIAN_POINT ( 'NONE',  ( 96.67388729539801773, -35.53787041403403180, 206.2356252759109623 ) ) ;
#38797 = CARTESIAN_POINT ( 'NONE',  ( 134.0664832912740110, 0.2215528400590013880, 311.1531252759119752 ) ) ;
#38798 = CARTESIAN_POINT ( 'NONE',  ( -2.767668950682794282, 70.16797056649836861, 38.00561040827691528 ) ) ;
#38799 = FACE_OUTER_BOUND ( 'NONE', #45906, .T. ) ;
#38800 = CARTESIAN_POINT ( 'NONE',  ( 176.7669697523282935, -48.62818131005432321, 300.4678068554149490 ) ) ;
#38801 = ADVANCED_FACE ( 'NONE', ( #2288 ), #8657, .F. ) ;
#38804 = CARTESIAN_POINT ( 'NONE',  ( 100.2615012876618295, -45.41023301258249489, 273.0594347997205773 ) ) ;
#38803 = DIRECTION ( 'NONE',  ( 0.000000000000000000, 0.000000000000000000, 1.000000000000000000 ) ) ;
#38802 = CARTESIAN_POINT ( 'NONE',  ( 191.6377717143134873, -67.87844715994100397, 13.84673904354932006 ) ) ;
#38805 = CARTESIAN_POINT ( 'NONE',  ( 163.2449138992999735, -32.11662333284611748, -5.074374724088000832 ) ) ;
#38806 = EDGE_CURVE ( 'NONE', #7755, #29308, #78156, .T. ) ;
#38807 = CARTESIAN_POINT ( 'NONE',  ( 71.06670390244701707, -90.27844715994098124, 222.2178068554179902 ) ) ;
#38808 = DIRECTION ( 'NONE',  ( 0.000000000000000000, 0.000000000000000000, 1.000000000000000000 ) ) ;
#38809 = ADVANCED_FACE ( 'NONE', ( #57223 ), #72218, .T. ) ;
#38810 = FACE_OUTER_BOUND ( 'NONE', #11978, .T. ) ;
#38811 = DIRECTION ( 'NONE',  ( -0.4999999999999998890, 0.8660254037844387076, 0.000000000000000000 ) ) ;
#38812 = CARTESIAN_POINT ( 'NONE',  ( -492.0614999999999668, 14.28750000000026077, 11.11249999999970051 ) ) ;
#38814 = VERTEX_POINT ( 'NONE', #29093 ) ;
#38813 = CARTESIAN_POINT ( 'NONE',  ( -5.617021782840702748, 93.94788616487885236, -118.4234307144629241 ) ) ;
#38815 = ADVANCED_FACE ( 'NONE', ( #42689 ), #58560, .T. ) ;
#38816 = DIRECTION ( 'NONE',  ( 0.000000000000000000, 1.000000000000000000, 0.000000000000000000 ) ) ;
#38817 = CARTESIAN_POINT ( 'NONE',  ( 114.1397626436471171, -29.04081378529519597, 199.4841967044819739 ) ) ;
#38818 = CARTESIAN_POINT ( 'NONE',  ( 96.02786343543940006, -37.29764797185995207, 117.3794347997199594 ) ) ;
#38819 = CARTESIAN_POINT ( 'NONE',  ( 109.9722659835539389, -48.26927123350142779, 238.7727681330539724 ) ) ;
#38820 = DIRECTION ( 'NONE',  ( 1.000000000000000078E-15, 0.000000000000000000, -1.000000000000000000 ) ) ;
#38821 = DIRECTION ( 'NONE',  ( 4.299999999999999979E-14, -1.000000000000000000, 0.000000000000000000 ) ) ;
#38823 = CARTESIAN_POINT ( 'NONE',  ( 173.9900000000000091, 53.21300000000000097, 59.96543552338529537 ) ) ;
#38822 = DIRECTION ( 'NONE',  ( -1.907762142705490052E-15, -7.167082501179359715E-16, 1.000000000000000000 ) ) ;
#38824 = DIRECTION ( 'NONE',  ( 0.000000000000000000, 1.000000000000000000, 0.000000000000000000 ) ) ;
#38825 = DIRECTION ( 'NONE',  ( 3.100000000000000258E-29, -3.100000000000000044E-14, -1.000000000000000000 ) ) ;
#38826 = AXIS2_PLACEMENT_3D ( 'NONE', #48144, #6384, #27273 ) ;
#38827 = CARTESIAN_POINT ( 'NONE',  ( 132.3573525511424691, -20.88611802718810395, 2.101554303219792086 ) ) ;
#38828 = VERTEX_POINT ( 'NONE', #56778 ) ;
#38829 = EDGE_LOOP ( 'NONE', ( #60278, #84943, #2532, #76537, #5253 ) ) ;
#38830 = EDGE_CURVE ( 'NONE', #89346, #29480, #79522, .T. ) ;
#38831 = CARTESIAN_POINT ( 'NONE',  ( 106.2553484193443865, -46.40481216151710697, 111.9324198280769735 ) ) ;
#38833 = EDGE_LOOP ( 'NONE', ( #12786, #71605, #35717, #1955 ) ) ;
#38832 = CARTESIAN_POINT ( 'NONE',  ( -12.37532827966388282, 85.43317223346198830, -129.9681767497193903 ) ) ;
#38834 = CARTESIAN_POINT ( 'NONE',  ( 98.29923130492889527, -31.06375673945267124, 141.8699109901969564 ) ) ;
#38835 = CARTESIAN_POINT ( 'NONE',  ( 182.3467384525650061, -29.62846900982231446, -5.074374724088000832 ) ) ;
#38836 = CARTESIAN_POINT ( 'NONE',  ( 79.32178306376293619, -16.08035908359608612, 8.141856907855881786 ) ) ;
#38837 = DIRECTION ( 'NONE',  ( -1.000000000000000078E-15, 1.000000000000000083E-30, 1.000000000000000000 ) ) ;
#38838 = CARTESIAN_POINT ( 'NONE',  ( 151.5667039024485518, -48.82844715993590512, 180.4678068554149775 ) ) ;
#38839 = CARTESIAN_POINT ( 'NONE',  ( 114.7041265136728612, -43.74408836545399737, 78.22324432353094892 ) ) ;
#38840 = VERTEX_POINT ( 'NONE', #64508 ) ;
#38841 = ORIENTED_EDGE ( 'NONE', *, *, #87626, .T. ) ;
#38842 = ORIENTED_EDGE ( 'NONE', *, *, #5310, .T. ) ;
#38843 = CIRCLE ( 'NONE', #62064, 130.5560000000000116 ) ;
#38844 = CYLINDRICAL_SURFACE ( 'NONE', #737, 4.762500000000002842 ) ;
#38846 = CARTESIAN_POINT ( 'NONE',  ( 25.56670390244797275, -67.87844715994100397, 137.2178068554150059 ) ) ;
#38845 = CARTESIAN_POINT ( 'NONE',  ( 107.8912859324307192, -26.39220933555703752, 111.0251490854339806 ) ) ;
#38847 = DIRECTION ( 'NONE',  ( 4.237773401492740281E-14, -1.000000000000000000, 0.000000000000000000 ) ) ;
#38848 = CARTESIAN_POINT ( 'NONE',  ( 154.4628380807770327, -130.5939552399572108, 126.9238073912448925 ) ) ;
#38849 = CARTESIAN_POINT ( 'NONE',  ( 32.16397622746000451, -34.03355364505800651, -5.074374724088000832 ) ) ;
#38850 = AXIS2_PLACEMENT_3D ( 'NONE', #39853, #47559, #82124 ) ;
#38851 = CARTESIAN_POINT ( 'NONE',  ( 74.68844285250109749, 85.85031469618033384, 92.07164801315086322 ) ) ;
#38852 = FACE_OUTER_BOUND ( 'NONE', #88958, .T. ) ;
#38853 = CARTESIAN_POINT ( 'NONE',  ( 107.8666756518570935, -26.35696637107986717, 70.01562527591099183 ) ) ;
#38854 = ORIENTED_EDGE ( 'NONE', *, *, #70925, .F. ) ;
#38855 = EDGE_LOOP ( 'NONE', ( #39864, #25332, #68907, #35789 ) ) ;
#38856 = CIRCLE ( 'NONE', #44615, 2.999999999999999112 ) ;
#38857 = LINE ( 'NONE', #66564, #41554 ) ;
#38858 = DIRECTION ( 'NONE',  ( -1.000000000000000000, -1.000000000000000078E-15, -1.000000000000000078E-15 ) ) ;
#38859 = AXIS2_PLACEMENT_3D ( 'NONE', #72168, #37200, #37647 ) ;
#38860 = VECTOR ( 'NONE', #68645, 1000.000000000000000 ) ;
#38862 = ADVANCED_FACE ( 'NONE', ( #15916 ), #70430, .T. ) ;
#38861 = DIRECTION ( 'NONE',  ( 0.000000000000000000, 0.000000000000000000, 1.000000000000000000 ) ) ;
#38863 = CARTESIAN_POINT ( 'NONE',  ( 99.93348902297414327, -31.82829241803101894, 163.6776141791149826 ) ) ;
#38864 = CIRCLE ( 'NONE', #50468, 12.99999999999999822 ) ;
#38865 = EDGE_CURVE ( 'NONE', #69445, #41770, #71772, .T. ) ;
#38866 = CARTESIAN_POINT ( 'NONE',  ( 87.06648329127389729, -54.72944906728955772, -4.970821333495855754 ) ) ;
#38867 = ORIENTED_EDGE ( 'NONE', *, *, #39421, .F. ) ;
#38868 = VERTEX_POINT ( 'NONE', #2734 ) ;
#38869 = DIRECTION ( 'NONE',  ( 1.000000000000000000, 4.272717921125146745E-14, 0.000000000000000000 ) ) ;
#38870 = ORIENTED_EDGE ( 'NONE', *, *, #32706, .F. ) ;
#38871 = ORIENTED_EDGE ( 'NONE', *, *, #38830, .F. ) ;
#38872 = DIRECTION ( 'NONE',  ( -0.3787978585227821382, 0.9254794337955621897, 0.000000000000000000 ) ) ;
#38873 = CARTESIAN_POINT ( 'NONE',  ( 107.2218274976867463, -26.65737820016106951, 226.4958690201829654 ) ) ;
#38874 = CARTESIAN_POINT ( 'NONE',  ( 173.9900000000000091, 37.33800000000000097, 42.86249999999999716 ) ) ;
#38875 = VECTOR ( 'NONE', #12860, 1000.000000000000000 ) ;
#38876 = DIRECTION ( 'NONE',  ( 0.000000000000000000, 0.000000000000000000, 1.000000000000000000 ) ) ;
#38877 = VECTOR ( 'NONE', #28786, 1000.000000000000000 ) ;
#38878 = CARTESIAN_POINT ( 'NONE',  ( -109.5466416834841539, 58.08661539045247935, 71.02395987518927711 ) ) ;
#38879 = ORIENTED_EDGE ( 'NONE', *, *, #37801, .F. ) ;
#38880 = ORIENTED_EDGE ( 'NONE', *, *, #56517, .T. ) ;
#38881 = ADVANCED_FACE ( 'NONE', ( #9103 ), #58129, .F. ) ;
#38882 = ORIENTED_EDGE ( 'NONE', *, *, #22230, .T. ) ;
#38883 = ORIENTED_EDGE ( 'NONE', *, *, #69307, .F. ) ;
#38884 = CARTESIAN_POINT ( 'NONE',  ( 114.3355458017429811, -42.49630604348746488, 196.1109475124489450 ) ) ;
#38885 = CARTESIAN_POINT ( 'NONE',  ( 114.7877796877764922, -44.67155160988957618, 118.2022919425779719 ) ) ;
#38886 = CARTESIAN_POINT ( 'NONE',  ( 117.4257108620838181, -37.68603989742254612, 78.75276813305399060 ) ) ;
#38887 = CARTESIAN_POINT ( 'NONE',  ( 87.68693475024628015, -140.6784471599409585, 245.6812587119739817 ) ) ;
#38888 = LINE ( 'NONE', #10734, #8387 ) ;
#38889 = CARTESIAN_POINT ( 'NONE',  ( 117.7034974245586483, -39.73408348695345182, 139.6194347997199827 ) ) ;
#38890 = DIRECTION ( 'NONE',  ( 0.000000000000000000, -0.8660254037844351549, -0.5000000000000061062 ) ) ;
#38891 = ORIENTED_EDGE ( 'NONE', *, *, #8731, .F. ) ;
#38892 = CARTESIAN_POINT ( 'NONE',  ( -215.9000000000000057, 101.5999999999999943, -45.33899999999999864 ) ) ;
#38893 = ORIENTED_EDGE ( 'NONE', *, *, #36787, .F. ) ;
#38894 = ORIENTED_EDGE ( 'NONE', *, *, #70304, .F. ) ;
#38895 = CYLINDRICAL_SURFACE ( 'NONE', #50608, 2.117000000000007987 ) ;
#38896 = LINE ( 'NONE', #5744, #66350 ) ;
#38897 = B_SPLINE_CURVE_WITH_KNOTS ( 'NONE', 3,
 ( #31683, #60721, #33477, #3986 ),
 .UNSPECIFIED., .F., .F.,
 ( 4, 4 ),
 ( -0.6035999334370359959, -0.5903216970416030884 ),
 .UNSPECIFIED. ) ;
#38898 = ORIENTED_EDGE ( 'NONE', *, *, #2014, .F. ) ;
#38899 = CARTESIAN_POINT ( 'NONE',  ( 107.0664832912739968, -36.72944715994100306, 311.6356252759112522 ) ) ;
#38900 = ORIENTED_EDGE ( 'NONE', *, *, #1912, .T. ) ;
#38901 = CARTESIAN_POINT ( 'NONE',  ( 116.3247715116346939, -32.94624160847306626, 99.13562527591096796 ) ) ;
#38902 = CARTESIAN_POINT ( 'NONE',  ( 118.0022803299065686, -38.33799637688264994, 73.72229194257801055 ) ) ;
#38903 = FACE_OUTER_BOUND ( 'NONE', #21392, .T. ) ;
#38904 = DIRECTION ( 'NONE',  ( 0.000000000000000000, 0.000000000000000000, -1.000000000000000000 ) ) ;
#38905 = CARTESIAN_POINT ( 'NONE',  ( 83.73314995794051185, 12.92155284005802685, 336.5756252759109657 ) ) ;
#38906 = CARTESIAN_POINT ( 'NONE',  ( 97.42673588038233845, -38.38435052442954998, 91.46133956162594814 ) ) ;
#38908 = CARTESIAN_POINT ( 'NONE',  ( 113.0097079652340000, -45.31096836313445664, 199.0584824187679374 ) ) ;
#38907 = CARTESIAN_POINT ( 'NONE',  ( 106.5510518188671227, -25.28190781890620542, 320.5359728645732389 ) ) ;
#38909 = CARTESIAN_POINT ( 'NONE',  ( 25.56670390244797275, -62.87844715994099687, 257.2178068554150059 ) ) ;
#38910 = EDGE_CURVE ( 'NONE', #73307, #40784, #5406, .T. ) ;
#38911 = DIRECTION ( 'NONE',  ( 0.000000000000000000, 0.000000000000000000, 1.000000000000000000 ) ) ;
#38912 = VERTEX_POINT ( 'NONE', #38131 ) ;
#38913 = DIRECTION ( 'NONE',  ( -1.000000000000000078E-15, 1.000000000000000000, 0.000000000000000000 ) ) ;
#38914 = CIRCLE ( 'NONE', #69401, 3.000000000000002665 ) ;
#38915 = EDGE_CURVE ( 'NONE', #27899, #45930, #80826, .T. ) ;
#38916 = CARTESIAN_POINT ( 'NONE',  ( 104.1009375265828538, -120.0661611444834023, -21.02845593540877189 ) ) ;
#38917 = EDGE_CURVE ( 'NONE', #25576, #71344, #37282, .T. ) ;
#38918 = CARTESIAN_POINT ( 'NONE',  ( 274.0659999999999741, 40.03750000000000142, -7.937500000000000000 ) ) ;
#38919 = CIRCLE ( 'NONE', #70847, 0.5000000000000004441 ) ;
#38920 = DIRECTION ( 'NONE',  ( 1.000000000000000000, 0.000000000000000000, 0.000000000000000000 ) ) ;
#38922 = ORIENTED_EDGE ( 'NONE', *, *, #60951, .T. ) ;
#38921 = CARTESIAN_POINT ( 'NONE',  ( 96.81521419041753518, -34.60385362728553815, 216.1641967044819808 ) ) ;
#38923 = EDGE_CURVE ( 'NONE', #79764, #24976, #67622, .T. ) ;
#38924 = DIRECTION ( 'NONE',  ( -1.000000000000000000, -1.541976423090496028E-15, 0.000000000000000000 ) ) ;
#38925 = CARTESIAN_POINT ( 'NONE',  ( 111.7488185767529245, -27.39065688012293265, 275.7070538473396937 ) ) ;
#38926 = CARTESIAN_POINT ( 'NONE',  ( 117.7233698349432132, -39.83239211553974712, 134.5889586092439743 ) ) ;
#38927 = CARTESIAN_POINT ( 'NONE',  ( -72.96458098368751166, 117.4749999999999943, 67.92268098368620599 ) ) ;
#38928 = CIRCLE ( 'NONE', #33094, 7.143750000000004263 ) ;
#38929 = CARTESIAN_POINT ( 'NONE',  ( 82.76600038373194934, -37.25405382162458068, 6.823682607502961517 ) ) ;
#38930 = LINE ( 'NONE', #72577, #23970 ) ;
#38931 = CARTESIAN_POINT ( 'NONE',  ( 52.06670390244699576, -68.87844715994100397, 55.21780685541800437 ) ) ;
#38932 = ORIENTED_EDGE ( 'NONE', *, *, #29398, .F. ) ;
#38933 = ORIENTED_EDGE ( 'NONE', *, *, #64640, .T. ) ;
#38934 = VERTEX_POINT ( 'NONE', #67169 ) ;
#38935 = EDGE_CURVE ( 'NONE', #54796, #28391, #88208, .T. ) ;
#38936 = AXIS2_PLACEMENT_3D ( 'NONE', #30424, #71323, #58121 ) ;
#38937 = ORIENTED_EDGE ( 'NONE', *, *, #72510, .T. ) ;
#38938 = CARTESIAN_POINT ( 'NONE',  ( 140.0667039024470171, -90.27844715994091018, 51.21780685541800437 ) ) ;
#38939 = CARTESIAN_POINT ( 'NONE',  ( 117.5188882057536830, -36.54585972124053939, 284.8413395616252615 ) ) ;
#38940 = LINE ( 'NONE', #69230, #78096 ) ;
#38941 = EDGE_CURVE ( 'NONE', #86581, #87871, #4952, .T. ) ;
#38942 = CARTESIAN_POINT ( 'NONE',  ( 77.10067130038136440, -139.0587715636908683, 247.5465134696939913 ) ) ;
#38944 = LINE ( 'NONE', #67102, #41299 ) ;
#38943 = CARTESIAN_POINT ( 'NONE',  ( 3.175000000000334666, 111.1250000000000000, -31.75000000000000000 ) ) ;
#38945 = VECTOR ( 'NONE', #33180, 1000.000000000000000 ) ;
#38946 = CARTESIAN_POINT ( 'NONE',  ( 98.70294500015674544, -34.99527330041078699, 215.5867055423629779 ) ) ;
#38947 = ORIENTED_EDGE ( 'NONE', *, *, #82096, .T. ) ;
#38948 = VECTOR ( 'NONE', #51021, 1000.000000000000000 ) ;
#38949 = VERTEX_POINT ( 'NONE', #45370 ) ;
#38950 = EDGE_LOOP ( 'NONE', ( #76891, #44961, #9925, #68580 ) ) ;
#38951 = DIRECTION ( 'NONE',  ( 0.000000000000000000, 0.000000000000000000, 1.000000000000000000 ) ) ;
#38952 = CARTESIAN_POINT ( 'NONE',  ( 137.0667039024470739, -118.2784471599408960, 230.7030882296565721 ) ) ;
#38953 = DIRECTION ( 'NONE',  ( 8.503806984168930281E-16, 0.000000000000000000, -1.000000000000000000 ) ) ;
#38954 = CARTESIAN_POINT ( 'NONE',  ( 111.3597915011938539, -28.37217101237177985, 16.14253568684992501 ) ) ;
#38955 = CARTESIAN_POINT ( 'NONE',  ( 118.4232034889089249, 93.94553785444266225, 5.621872244392114304 ) ) ;
#38956 = DIRECTION ( 'NONE',  ( -1.000000000000000078E-15, 1.000000000000000083E-30, 1.000000000000000000 ) ) ;
#38957 = CARTESIAN_POINT ( 'NONE',  ( 117.3720538532507618, -35.57445771113444977, 233.9032443235299752 ) ) ;
#38958 = CARTESIAN_POINT ( 'NONE',  ( 34.67381068361984120, -26.00627455219439099, 193.9678068554150911 ) ) ;
#38959 = VERTEX_POINT ( 'NONE', #51740 ) ;
#38960 = CIRCLE ( 'NONE', #34622, 3.000000000000002665 ) ;
#38961 = LINE ( 'NONE', #3554, #30312 ) ;
#38962 = VERTEX_POINT ( 'NONE', #79490 ) ;
#38964 = EDGE_CURVE ( 'NONE', #81381, #3053, #56731, .T. ) ;
#38963 = CARTESIAN_POINT ( 'NONE',  ( 71.06648329127399677, -18.82844715994099971, 323.8756252759120002 ) ) ;
#38965 = CARTESIAN_POINT ( 'NONE',  ( 113.7569007282865101, -30.30027569836345336, 37.25380465530597718 ) ) ;
#38966 = AXIS2_PLACEMENT_3D ( 'NONE', #81868, #54112, #26880 ) ;
#38967 = CIRCLE ( 'NONE', #86836, 5.000000000000004441 ) ;
#38968 = CARTESIAN_POINT ( 'NONE',  ( 135.6382054840660487, -16.47341874818684104, 7.827313014939066171 ) ) ;
#38969 = EDGE_CURVE ( 'NONE', #78219, #52482, #59451, .T. ) ;
#38970 = DIRECTION ( 'NONE',  ( 0.000000000000000000, 0.000000000000000000, -1.000000000000000000 ) ) ;
#38971 = DIRECTION ( 'NONE',  ( -1.000000000000000078E-15, 1.000000000000000083E-30, 1.000000000000000000 ) ) ;
#38972 = VERTEX_POINT ( 'NONE', #3609 ) ;
#38973 = CARTESIAN_POINT ( 'NONE',  ( 182.0667039024469886, -33.35206098992630075, -5.074374724088000832 ) ) ;
#38974 = CONICAL_SURFACE ( 'NONE', #12870, 1.258750000000002922, 1.029744258676650093 ) ;
#38975 = CARTESIAN_POINT ( 'NONE',  ( 122.9150858762449587, 60.67894162041066153, -44.01180387395123006 ) ) ;
#38976 = ORIENTED_EDGE ( 'NONE', *, *, #79800, .F. ) ;
#38977 = CARTESIAN_POINT ( 'NONE',  ( 97.57106248370669732, -31.07117258718254149, 130.9108633711489915 ) ) ;
#38978 = EDGE_LOOP ( 'NONE', ( #18033, #89718, #88007, #57496 ) ) ;
#38979 = CARTESIAN_POINT ( 'NONE',  ( 102.0495883242188171, -29.81664044981240025, 74.99813411379096806 ) ) ;
#38980 = CIRCLE ( 'NONE', #63639, 0.5000000000000004441 ) ;
#38981 = CARTESIAN_POINT ( 'NONE',  ( 97.89409425326189762, -40.71365990706227223, 87.65209274241340154 ) ) ;
#38982 = CARTESIAN_POINT ( 'NONE',  ( 113.9519893150074239, -42.30780582616069552, 84.71586902018296428 ) ) ;
#38983 = FACE_OUTER_BOUND ( 'NONE', #29407, .T. ) ;
#38984 = DIRECTION ( 'NONE',  ( -0.000000000000000000, 1.000000000000000000, 0.000000000000000000 ) ) ;
#38985 = CARTESIAN_POINT ( 'NONE',  ( 102.7462986198438273, -25.66788047019655394, 16.37276813305293999 ) ) ;
#38986 = LINE ( 'NONE', #79910, #35069 ) ;
#38987 = EDGE_LOOP ( 'NONE', ( #57975, #50052, #85851, #77484 ) ) ;
#38988 = CARTESIAN_POINT ( 'NONE',  ( 100.8874123674214189, -44.70017568039049394, 257.0521985988731899 ) ) ;
#38989 = VERTEX_POINT ( 'NONE', #45810 ) ;
#38990 = EDGE_CURVE ( 'NONE', #11421, #68641, #19901, .T. ) ;
#38991 = CARTESIAN_POINT ( 'NONE',  ( -118.4241986436612564, 71.14137858619480426, -5.641441481138969039 ) ) ;
#38992 = ORIENTED_EDGE ( 'NONE', *, *, #10072, .F. ) ;
#38993 = ORIENTED_EDGE ( 'NONE', *, *, #18727, .F. ) ;
#38994 = CIRCLE ( 'NONE', #17232, 3.299999999999997158 ) ;
#38995 = DIRECTION ( 'NONE',  ( 1.000000000000000000, 1.000000000000000078E-15, 0.000000000000000000 ) ) ;
#38996 = ORIENTED_EDGE ( 'NONE', *, *, #6749, .T. ) ;
#38997 = CARTESIAN_POINT ( 'NONE',  ( 114.7458293810857128, -30.61868467657531312, 244.3613395616259822 ) ) ;
#38998 = CARTESIAN_POINT ( 'NONE',  ( 97.66901493533356415, -40.15138444804937023, 126.6038837173656901 ) ) ;
#38999 = CARTESIAN_POINT ( 'NONE',  ( 117.0608945212723739, -38.08045314311991802, 189.7189586074687497 ) ) ;
#39000 = CARTESIAN_POINT ( 'NONE',  ( 99.98074987894446508, -44.37633341885192095, 42.98133956162492098 ) ) ;
#39001 = CARTESIAN_POINT ( 'NONE',  ( 98.54755185453446131, -41.97681824699740361, 42.76578874115597273 ) ) ;
#39002 = VERTEX_POINT ( 'NONE', #12668 ) ;
#39003 = CARTESIAN_POINT ( 'NONE',  ( 44.45000000000000284, 114.2999999999999972, 206.3750000000000000 ) ) ;
#39004 = ADVANCED_FACE ( 'NONE', ( #19927 ), #13120, .T. ) ;
#39005 = LINE ( 'NONE', #45803, #33111 ) ;
#39007 = EDGE_LOOP ( 'NONE', ( #89531, #14122, #34807, #54570, #2587, #25597 ) ) ;
#39006 = AXIS2_PLACEMENT_3D ( 'NONE', #65336, #38075, #65765 ) ;
#39008 = DIRECTION ( 'NONE',  ( -1.000000000000000078E-15, 1.000000000000000083E-30, 1.000000000000000000 ) ) ;
#39009 = CARTESIAN_POINT ( 'NONE',  ( 113.1760029588135410, -44.75358003032814480, 114.0945772493509764 ) ) ;
#39010 = CARTESIAN_POINT ( 'NONE',  ( 116.5068947302722222, -41.18400185692905069, 228.4756252759109714 ) ) ;
#39011 = CARTESIAN_POINT ( 'NONE',  ( 82.81648329127402519, -36.72944715994107412, -5.074374724089055100 ) ) ;
#39012 = ADVANCED_FACE ( 'NONE', ( #81723 ), #83497, .T. ) ;
#39013 = CARTESIAN_POINT ( 'NONE',  ( -30.86579703273522668, 53.97499999999997300, 73.54054752236280024 ) ) ;
#39014 = CARTESIAN_POINT ( 'NONE',  ( 121.2542869028164176, -94.96965202435542608, -19.23816181211529397 ) ) ;
#39015 = CARTESIAN_POINT ( 'NONE',  ( 101.4222765643661006, -43.81150905960179642, 271.4514674471243438 ) ) ;
#39017 = CARTESIAN_POINT ( 'NONE',  ( 95.37363933861288956, -34.96150835630653120, 67.20705384733894050 ) ) ;
#39016 = CARTESIAN_POINT ( 'NONE',  ( 172.5664832912729878, -27.82844715994070484, 254.1756252759120400 ) ) ;
#39018 = CARTESIAN_POINT ( 'NONE',  ( 110.3758871135606796, 62.19865536329562872, 69.72828050043732162 ) ) ;
#39019 = CARTESIAN_POINT ( 'NONE',  ( 95.62691733261443972, -33.44842233792613229, 141.1041967044829732 ) ) ;
#39020 = ORIENTED_EDGE ( 'NONE', *, *, #36104, .T. ) ;
#39021 = CARTESIAN_POINT ( 'NONE',  ( 134.0664828118825938, -21.47944715903993540, 8.225259175038406312 ) ) ;
#39022 = ORIENTED_EDGE ( 'NONE', *, *, #37775, .T. ) ;
#39023 = DIRECTION ( 'NONE',  ( 1.000000000000000000, 4.101809204280141026E-14, 0.000000000000000000 ) ) ;
#39024 = CARTESIAN_POINT ( 'NONE',  ( 180.3521107875713199, -35.65087443489230878, 313.9678068554149490 ) ) ;
#39025 = CARTESIAN_POINT ( 'NONE',  ( 76.06670390244799762, -26.72944715994109899, 199.5838068554169524 ) ) ;
#39027 = ORIENTED_EDGE ( 'NONE', *, *, #15902, .T. ) ;
#39026 = EDGE_CURVE ( 'NONE', #75933, #76329, #69421, .T. ) ;
#39028 = AXIS2_PLACEMENT_3D ( 'NONE', #87308, #82303, #59572 ) ;
#39029 = LINE ( 'NONE', #58574, #41827 ) ;
#39031 = ORIENTED_EDGE ( 'NONE', *, *, #12561, .F. ) ;
#39030 = CARTESIAN_POINT ( 'NONE',  ( 95.98102948456921979, -37.30005869795228080, 121.3794347997209684 ) ) ;
#39032 = FACE_OUTER_BOUND ( 'NONE', #43792, .T. ) ;
#39033 = CARTESIAN_POINT ( 'NONE',  ( -130.2060295542616757, 90.93932679091003024, -9.571439627454301657 ) ) ;
#39035 = DIRECTION ( 'NONE',  ( -4.299999999999999979E-14, 1.000000000000000000, 0.000000000000000000 ) ) ;
#39034 = VECTOR ( 'NONE', #73027, 999.9999999999998863 ) ;
#39036 = ORIENTED_EDGE ( 'NONE', *, *, #28757, .F. ) ;
#39037 = CIRCLE ( 'NONE', #7153, 3.000000000000002665 ) ;
#39038 = CARTESIAN_POINT ( 'NONE',  ( 114.0958560388892380, -44.50609692678638396, 133.1613395616249989 ) ) ;
#39039 = PRODUCT_CONTEXT ( 'NONE', #71799, 'mechanical' ) ;
#39040 = DIRECTION ( 'NONE',  ( 3.999999999999999995E-14, -1.000000000000000000, 4.100000000000000342E-29 ) ) ;
#39041 = DIRECTION ( 'NONE',  ( 0.000000000000000000, 0.000000000000000000, -1.000000000000000000 ) ) ;
#39042 = ORIENTED_EDGE ( 'NONE', *, *, #54168, .T. ) ;
#39043 = EDGE_CURVE ( 'NONE', #11705, #9815, #26726, .T. ) ;
#39044 = VECTOR ( 'NONE', #78137, 1000.000000000000000 ) ;
#39045 = ORIENTED_EDGE ( 'NONE', *, *, #31635, .T. ) ;
#39046 = DIRECTION ( 'NONE',  ( -1.000000000000000000, -3.360405532702990443E-14, 0.000000000000000000 ) ) ;
#39047 = DIRECTION ( 'NONE',  ( 0.000000000000000000, 1.000000000000000000, 0.000000000000000000 ) ) ;
#39048 = EDGE_CURVE ( 'NONE', #26574, #43857, #34488, .T. ) ;
#39049 = CARTESIAN_POINT ( 'NONE',  ( 138.0667039024479550, -26.72944715994091069, 239.5838068554170377 ) ) ;
#39050 = DIRECTION ( 'NONE',  ( 0.000000000000000000, 0.000000000000000000, -1.000000000000000000 ) ) ;
#39051 = B_SPLINE_CURVE_WITH_KNOTS ( 'NONE', 3,
 ( #75856, #77654, #1803, #84026, #82692, #49472, #42649, #48566, #70388, #6807, #34510, #8163, #76302, #63571, #27703, #55380, #1352, #29055 ),
 .UNSPECIFIED., .F., .F.,
 ( 4, 2, 2, 2, 2, 2, 2, 2, 4 ),
 ( 0.4999487719651097284, 0.5624551754694709915, 0.6249615789738323102, 0.6874679824781936288, 0.7499743859825549475, 0.8124807894869161551, 0.8749871929912774737, 0.9374935964956387924, 1.000000000000000000 ),
 .UNSPECIFIED. ) ;
#39052 = AXIS2_PLACEMENT_3D ( 'NONE', #72457, #10658, #51537 ) ;
#39054 = CARTESIAN_POINT ( 'NONE',  ( -254.0000000000000000, 93.66249999999999432, 11.11250000000040217 ) ) ;
#39053 = CARTESIAN_POINT ( 'NONE',  ( 24.79284581386629327, 184.0000000000000000, -3.384395586952189366E-14 ) ) ;
#39055 = FACE_BOUND ( 'NONE', #39445, .T. ) ;
#39056 = ORIENTED_EDGE ( 'NONE', *, *, #89798, .F. ) ;
#39057 = CARTESIAN_POINT ( 'NONE',  ( 226.4410000000000025, 40.03750000000000142, -7.937500000000000000 ) ) ;
#39058 = VECTOR ( 'NONE', #6079, 1000.000000000000000 ) ;
#39059 = CARTESIAN_POINT ( 'NONE',  ( 107.6181574201208520, -47.08485352040289484, 193.6308633711479672 ) ) ;
#39060 = VECTOR ( 'NONE', #21838, 1000.000000000000000 ) ;
#39062 = VERTEX_POINT ( 'NONE', #76683 ) ;
#39061 = DIRECTION ( 'NONE',  ( -1.000000000000000000, 0.000000000000000000, -0.000000000000000000 ) ) ;
#39063 = CARTESIAN_POINT ( 'NONE',  ( 112.4622727538958316, -27.87370092883246286, 45.62895860924398761 ) ) ;
#39064 = DIRECTION ( 'NONE',  ( 1.000000000000000000, 0.000000000000000000, 0.000000000000000000 ) ) ;
#39065 = DIRECTION ( 'NONE',  ( 9.299908063537909262E-17, 0.000000000000000000, 1.000000000000000000 ) ) ;
#39066 = LINE ( 'NONE', #12265, #73527 ) ;
#39067 = ORIENTED_EDGE ( 'NONE', *, *, #72502, .T. ) ;
#39068 = LINE ( 'NONE', #52665, #2306 ) ;
#39069 = EDGE_LOOP ( 'NONE', ( #28874, #59435, #80095, #73444 ) ) ;
#39070 = ORIENTED_EDGE ( 'NONE', *, *, #20270, .T. ) ;
#39071 = VECTOR ( 'NONE', #70715, 1000.000000000000000 ) ;
#39072 = CARTESIAN_POINT ( 'NONE',  ( 98.38943151359886485, -34.93026649658274607, 212.5958690201829597 ) ) ;
#39073 = CARTESIAN_POINT ( 'NONE',  ( 67.06670390244701707, -79.67844715994098692, 55.21780685541800437 ) ) ;
#39074 = CARTESIAN_POINT ( 'NONE',  ( -83.52531662946618951, 87.03008507238368452, 100.3414980266876739 ) ) ;
#39075 = EDGE_CURVE ( 'NONE', #58180, #80800, #85299, .T. ) ;
#39076 = FACE_OUTER_BOUND ( 'NONE', #7891, .T. ) ;
#39077 = DIRECTION ( 'NONE',  ( 1.000000000000000000, 0.000000000000000000, 0.000000000000000000 ) ) ;
#39078 = ORIENTED_EDGE ( 'NONE', *, *, #13451, .T. ) ;
#39079 = DIRECTION ( 'NONE',  ( 0.000000000000000000, 0.000000000000000000, -1.000000000000000000 ) ) ;
#39080 = DIRECTION ( 'NONE',  ( -3.100000000000000258E-29, 3.100000000000000044E-14, 1.000000000000000000 ) ) ;
#39081 = VERTEX_POINT ( 'NONE', #40804 ) ;
#39082 = CARTESIAN_POINT ( 'NONE',  ( 105.0259480979001410, -25.88970440745768542, 280.2365776568631759 ) ) ;
#39083 = VERTEX_POINT ( 'NONE', #7196 ) ;
#39084 = VERTEX_POINT ( 'NONE', #6294 ) ;
#39085 = CARTESIAN_POINT ( 'NONE',  ( 106.6756582537710187, -44.91051946355214852, 245.3566617981629463 ) ) ;
#39086 = LINE ( 'NONE', #60416, #51734 ) ;
#39087 = CARTESIAN_POINT ( 'NONE',  ( 23.11247487853312066, 78.03298490982817270, 301.3540638256986313 ) ) ;
#39088 = DIRECTION ( 'NONE',  ( 0.000000000000000000, -1.000000000000000000, 0.000000000000000000 ) ) ;
#39089 = DIRECTION ( 'NONE',  ( 1.000000000000000000, 6.193183223602000661E-14, -8.992470601956076883E-43 ) ) ;
#39090 = CARTESIAN_POINT ( 'NONE',  ( 106.4811776831737262, -24.84380329649774666, 191.1156252759109861 ) ) ;
#39092 = CARTESIAN_POINT ( 'NONE',  ( 69.72411017813010403, 127.0000000000000000, -69.72411017812979139 ) ) ;
#39091 = AXIS2_PLACEMENT_3D ( 'NONE', #44316, #85255, #85692 ) ;
#39093 = VECTOR ( 'NONE', #74632, 1000.000000000000000 ) ;
#39094 = VERTEX_POINT ( 'NONE', #33546 ) ;
#39095 = CARTESIAN_POINT ( 'NONE',  ( 112.7836381133937067, -27.91740111342080866, 65.61848241876793963 ) ) ;
#39096 = EDGE_CURVE ( 'NONE', #74209, #67921, #27629, .T. ) ;
#39097 = DIRECTION ( 'NONE',  ( 1.000000000000000000, 8.953411488912556626E-16, 0.000000000000000000 ) ) ;
#39098 = EDGE_LOOP ( 'NONE', ( #58088, #67939, #71377, #18677 ) ) ;
#39100 = ADVANCED_FACE ( 'NONE', ( #89422 ), #21268, .T. ) ;
#39099 = ORIENTED_EDGE ( 'NONE', *, *, #88661, .T. ) ;
#39101 = ORIENTED_EDGE ( 'NONE', *, *, #38245, .T. ) ;
#39103 = EDGE_CURVE ( 'NONE', #78613, #41873, #13555, .T. ) ;
#39102 = VECTOR ( 'NONE', #9972, 1000.000000000000000 ) ;
#39104 = CARTESIAN_POINT ( 'NONE',  ( 97.06670390244703128, -104.2784471599409244, 17.71780685541799016 ) ) ;
#39105 = DIRECTION ( 'NONE',  ( 0.000000000000000000, 0.000000000000000000, 1.000000000000000000 ) ) ;
#39106 = DIRECTION ( 'NONE',  ( 0.000000000000000000, 0.000000000000000000, 1.000000000000000000 ) ) ;
#39107 = CARTESIAN_POINT ( 'NONE',  ( 100.1874667927473439, -32.28399744105692548, 143.6880903695909524 ) ) ;
#39108 = CARTESIAN_POINT ( 'NONE',  ( 116.0738972362454149, -42.02130438377608357, 234.4041967044819899 ) ) ;
#39109 = EDGE_CURVE ( 'NONE', #8960, #40724, #89121, .T. ) ;
#39110 = CARTESIAN_POINT ( 'NONE',  ( 117.0604620818703410, -38.08351184708308779, 59.71871305607316316 ) ) ;
#39111 = EDGE_LOOP ( 'NONE', ( #29024, #68086, #87692, #18178 ) ) ;
#39112 = FILL_AREA_STYLE_COLOUR ( '', #58721 ) ;
#39113 = EDGE_CURVE ( 'NONE', #31056, #19557, #82622, .T. ) ;
#39114 = AXIS2_PLACEMENT_3D ( 'NONE', #16783, #60659, #88398 ) ;
#39115 = FACE_OUTER_BOUND ( 'NONE', #80893, .T. ) ;
#39116 = VERTEX_POINT ( 'NONE', #20384 ) ;
#39117 = ORIENTED_EDGE ( 'NONE', *, *, #47633, .T. ) ;
#39118 = EDGE_CURVE ( 'NONE', #62403, #23016, #41240, .T. ) ;
#39119 = EDGE_CURVE ( 'NONE', #66356, #60724, #26286, .T. ) ;
#39120 = LINE ( 'NONE', #72318, #76356 ) ;
#39121 = VECTOR ( 'NONE', #89195, 1000.000000000000000 ) ;
#39122 = VERTEX_POINT ( 'NONE', #36697 ) ;
#39123 = EDGE_LOOP ( 'NONE', ( #10346, #37893, #33448, #15312 ) ) ;
#39124 = DIRECTION ( 'NONE',  ( -1.000000000000000000, 6.036837696399451257E-13, 0.000000000000000000 ) ) ;
#39125 = FACE_OUTER_BOUND ( 'NONE', #39111, .T. ) ;
#39126 = EDGE_CURVE ( 'NONE', #1430, #76359, #56669, .T. ) ;
#39127 = CARTESIAN_POINT ( 'NONE',  ( -57.91199999999999903, 20.32000000000000028, 178.6098374884404905 ) ) ;
#39128 = VECTOR ( 'NONE', #55642, 1000.000000000000000 ) ;
#39129 = CARTESIAN_POINT ( 'NONE',  ( 115.5798344143896372, -39.81741137289535004, 172.9600388756959717 ) ) ;
#39130 = CARTESIAN_POINT ( 'NONE',  ( 104.6386611584700432, -47.56081657070318158, 27.38895860924395009 ) ) ;
#39131 = CARTESIAN_POINT ( 'NONE',  ( 71.69596173992542276, -99.94637129117697327, 248.3919653347779786 ) ) ;
#39132 = ORIENTED_EDGE ( 'NONE', *, *, #61262, .F. ) ;
#39133 = EDGE_CURVE ( 'NONE', #60854, #9592, #74582, .T. ) ;
#39134 = CARTESIAN_POINT ( 'NONE',  ( 107.0667039024470313, -104.2784471599420755, -19.78219314458201694 ) ) ;
#39136 = VERTEX_POINT ( 'NONE', #50299 ) ;
#39135 = EDGE_CURVE ( 'NONE', #64336, #19304, #57567, .T. ) ;
#39137 = FACE_OUTER_BOUND ( 'NONE', #43802, .T. ) ;
#39138 = EDGE_LOOP ( 'NONE', ( #14270, #79423, #33132, #52540 ) ) ;
#39139 = CARTESIAN_POINT ( 'NONE',  ( 97.41723905860696675, -33.98881011871176838, 167.1061884298218843 ) ) ;
#39140 = CARTESIAN_POINT ( 'NONE',  ( 104.0667030381796963, -70.87844715994094713, 93.21780742166239975 ) ) ;
#39141 = CARTESIAN_POINT ( 'NONE',  ( 110.8585676902739436, -45.98256027422110748, 132.8859773635041961 ) ) ;
#39142 = FACE_OUTER_BOUND ( 'NONE', #78045, .T. ) ;
#39143 = ORIENTED_EDGE ( 'NONE', *, *, #65389, .F. ) ;
#39144 = CARTESIAN_POINT ( 'NONE',  ( 111.4247116192842810, -46.22429891269226943, 27.91848241876792969 ) ) ;
#39145 = CARTESIAN_POINT ( 'NONE',  ( 104.7259408665080116, -47.57930243624250721, 28.41943479971997988 ) ) ;
#39147 = DIRECTION ( 'NONE',  ( 0.000000000000000000, 0.000000000000000000, 1.000000000000000000 ) ) ;
#39146 = CYLINDRICAL_SURFACE ( 'NONE', #73847, 3.174999999999983391 ) ;
#39148 = DIRECTION ( 'NONE',  ( -4.237773401492740281E-14, 1.000000000000000000, 0.000000000000000000 ) ) ;
#39149 = CARTESIAN_POINT ( 'NONE',  ( 107.0664832912739399, -36.72944715994095333, 315.1356252759112522 ) ) ;
#39150 = FACE_OUTER_BOUND ( 'NONE', #41485, .T. ) ;
#39151 = VECTOR ( 'NONE', #40532, 1000.000000000000000 ) ;
#39152 = EDGE_CURVE ( 'NONE', #45292, #66416, #35779, .T. ) ;
#39153 = CARTESIAN_POINT ( 'NONE',  ( 172.5664832912740110, -27.82844715994070484, 83.67562527591201160 ) ) ;
#39154 = ADVANCED_FACE ( 'NONE', ( #28513 ), #9308, .F. ) ;
#39155 = EDGE_CURVE ( 'NONE', #37435, #19551, #14913, .T. ) ;
#39156 = AXIS2_PLACEMENT_3D ( 'NONE', #63872, #14382, #22992 ) ;
#39157 = ORIENTED_EDGE ( 'NONE', *, *, #59534, .F. ) ;
#39158 = CARTESIAN_POINT ( 'NONE',  ( 115.7096504343579539, -43.69425479293489900, 43.27467289495795200 ) ) ;
#39159 = CARTESIAN_POINT ( 'NONE',  ( 117.4126858048608000, -35.18755665659306686, 214.9441967044829767 ) ) ;
#39160 = CARTESIAN_POINT ( 'NONE',  ( 101.1286207290677908, -27.37920684556040740, 61.51467289495899138 ) ) ;
#39161 = ADVANCED_FACE ( 'NONE', ( #2625 ), #15364, .T. ) ;
#39163 = DIRECTION ( 'NONE',  ( 0.000000000000000000, 1.000000000000000000, 0.000000000000000000 ) ) ;
#39162 = LINE ( 'NONE', #5095, #40650 ) ;
#39164 = CARTESIAN_POINT ( 'NONE',  ( -492.0614999999999668, 14.28750000000026077, 11.11249999999970051 ) ) ;
#39165 = VECTOR ( 'NONE', #77347, 1000.000000000000000 ) ;
#39166 = ORIENTED_EDGE ( 'NONE', *, *, #76284, .F. ) ;
#39167 = DIRECTION ( 'NONE',  ( 0.000000000000000000, 2.048885995248194949E-16, 1.000000000000000000 ) ) ;
#39168 = ORIENTED_EDGE ( 'NONE', *, *, #27048, .T. ) ;
#39169 = CARTESIAN_POINT ( 'NONE',  ( 110.8343066518039990, -26.26926122352955062, 95.80133956162396203 ) ) ;
#39170 = CIRCLE ( 'NONE', #40600, 2.500000000000002220 ) ;
#39172 = ORIENTED_EDGE ( 'NONE', *, *, #78107, .T. ) ;
#39171 = CARTESIAN_POINT ( 'NONE',  ( 11.41096683840008552, 88.12842719786394241, 130.0564362339166280 ) ) ;
#39173 = CARTESIAN_POINT ( 'NONE',  ( 113.2071528006339918, -45.12711609280817271, 224.0784824187679476 ) ) ;
#39174 = FACE_OUTER_BOUND ( 'NONE', #41253, .T. ) ;
#39175 = CARTESIAN_POINT ( 'NONE',  ( 111.4688792442139089, -45.71428781796094398, 147.9390134094296911 ) ) ;
#39176 = CARTESIAN_POINT ( 'NONE',  ( 50.96943157743499597, -34.03355364505720360, -5.074374724088000832 ) ) ;
#39177 = CARTESIAN_POINT ( 'NONE',  ( 108.4174892451278822, -26.73503592659411510, 45.96895860979116577 ) ) ;
#39178 = DIRECTION ( 'NONE',  ( 0.000000000000000000, 1.000000000000000000, 0.000000000000000000 ) ) ;
#39179 = DIRECTION ( 'NONE',  ( -3.100000000000000258E-29, 3.100000000000000044E-14, 1.000000000000000000 ) ) ;
#39180 = AXIS2_PLACEMENT_3D ( 'NONE', #30445, #8666, #3619 ) ;
#39181 = CARTESIAN_POINT ( 'NONE',  ( 111.1483613326457913, -47.07112276671761464, 172.8756252759109771 ) ) ;
#39182 = ORIENTED_EDGE ( 'NONE', *, *, #86849, .T. ) ;
#39183 = ORIENTED_EDGE ( 'NONE', *, *, #51400, .F. ) ;
#39184 = CARTESIAN_POINT ( 'NONE',  ( 113.6158397245882128, -43.46609735470438807, 114.6339642582779561 ) ) ;
#39185 = DIRECTION ( 'NONE',  ( 0.000000000000000000, 1.000000000000000000, 0.000000000000000000 ) ) ;
#39187 = DIRECTION ( 'NONE',  ( 0.000000000000000000, -1.000000000000000000, 0.000000000000000000 ) ) ;
#39186 = CARTESIAN_POINT ( 'NONE',  ( 105.7207279102414077, -46.41719084699259668, 253.4670538473389740 ) ) ;
#39188 = DIRECTION ( 'NONE',  ( -4.237773401492740281E-14, 1.000000000000000000, 0.000000000000000000 ) ) ;
#39189 = CARTESIAN_POINT ( 'NONE',  ( 131.0667039024480118, -58.35344715994099829, 204.3338068554149913 ) ) ;
#39190 = AXIS2_PLACEMENT_3D ( 'NONE', #35678, #57010, #84752 ) ;
#39191 = PLANE ( 'NONE',  #54721 ) ;
#39192 = DIRECTION ( 'NONE',  ( 0.000000000000000000, 1.000000000000000000, 0.000000000000000000 ) ) ;
#39193 = DIRECTION ( 'NONE',  ( 1.000000000000000078E-15, 0.000000000000000000, -1.000000000000000000 ) ) ;
#39194 = FACE_OUTER_BOUND ( 'NONE', #12740, .T. ) ;
#39195 = CARTESIAN_POINT ( 'NONE',  ( 114.9613132280022683, -29.02649429439048134, 194.4537205140059370 ) ) ;
#39196 = ORIENTED_EDGE ( 'NONE', *, *, #31824, .F. ) ;
#39197 = ORIENTED_EDGE ( 'NONE', *, *, #86507, .T. ) ;
#39198 = CARTESIAN_POINT ( 'NONE',  ( 111.1574783714308978, -73.49652949099265697, 249.3134381260879877 ) ) ;
#39199 = CARTESIAN_POINT ( 'NONE',  ( 78.35491772851318615, -16.56918551487918734, 2.099346190912949162 ) ) ;
#39200 = LINE ( 'NONE', #34167, #46119 ) ;
#39201 = DIRECTION ( 'NONE',  ( 0.000000000000000000, 0.000000000000000000, -1.000000000000000000 ) ) ;
#39202 = VECTOR ( 'NONE', #14527, 1000.000000000000000 ) ;
#39203 = CARTESIAN_POINT ( 'NONE',  ( 97.06389154151803211, -37.34296565923806099, 96.37529339840247644 ) ) ;
#39204 = EDGE_LOOP ( 'NONE', ( #86049, #2936 ) ) ;
#39205 = CARTESIAN_POINT ( 'NONE',  ( 116.7942972139657059, -39.39077959468326640, 63.61454998365505276 ) ) ;
#39206 = EDGE_CURVE ( 'NONE', #10945, #40908, #15137, .T. ) ;
#39207 = CARTESIAN_POINT ( 'NONE',  ( 110.4989391570660473, -26.88539935475378684, 209.8099109901969541 ) ) ;
#39208 = EDGE_CURVE ( 'NONE', #51309, #16242, #15807, .T. ) ;
#39209 = CARTESIAN_POINT ( 'NONE',  ( 259.3340000000000032, 52.73749999999999716, 10.66800000000000104 ) ) ;
#39210 = VERTEX_POINT ( 'NONE', #64842 ) ;
#39211 = ORIENTED_EDGE ( 'NONE', *, *, #13693, .F. ) ;
#39212 = AXIS2_PLACEMENT_3D ( 'NONE', #26350, #81345, #11830 ) ;
#39213 = ADVANCED_FACE ( 'NONE', ( #2176 ), #10777, .F. ) ;
#39214 = CARTESIAN_POINT ( 'NONE',  ( -12.27293249669208919, 79.25788962028573792, 117.9191036749242301 ) ) ;
#39215 = CARTESIAN_POINT ( 'NONE',  ( 184.5664832912740110, 15.62155284005900491, 328.6381252759109088 ) ) ;
#39216 = CARTESIAN_POINT ( 'NONE',  ( 115.7824585771272012, -41.80340552830423917, 164.4063582027085602 ) ) ;
#39217 = CARTESIAN_POINT ( 'NONE',  ( 99.05427501747529107, -38.42862543901446060, 29.31094751244794949 ) ) ;
#39218 = AXIS2_PLACEMENT_3D ( 'NONE', #75486, #53656, #6005 ) ;
#39219 = EDGE_CURVE ( 'NONE', #62140, #30523, #65886, .T. ) ;
#39220 = DIRECTION ( 'NONE',  ( 0.000000000000000000, 0.000000000000000000, 1.000000000000000000 ) ) ;
#39221 = ORIENTED_EDGE ( 'NONE', *, *, #147, .F. ) ;
#39222 = DIRECTION ( 'NONE',  ( 1.000000000000000000, 4.299999999999999979E-14, 1.000000000000000078E-15 ) ) ;
#39223 = CARTESIAN_POINT ( 'NONE',  ( 81.23646709784242148, -16.23881677343980812, 8.012604157996248588 ) ) ;
#39224 = VERTEX_POINT ( 'NONE', #58020 ) ;
#39226 = ORIENTED_EDGE ( 'NONE', *, *, #60623, .T. ) ;
#39225 = CIRCLE ( 'NONE', #4430, 10.66800000000000459 ) ;
#39227 = EDGE_CURVE ( 'NONE', #87130, #44336, #36241, .T. ) ;
#39228 = CARTESIAN_POINT ( 'NONE',  ( 41.56648329127398966, -27.57844715994070484, 255.9256252759120116 ) ) ;
#39229 = ORIENTED_EDGE ( 'NONE', *, *, #79184, .F. ) ;
#39230 = VERTEX_POINT ( 'NONE', #16254 ) ;
#39231 = FACE_OUTER_BOUND ( 'NONE', #16334, .T. ) ;
#39232 = EDGE_CURVE ( 'NONE', #55351, #89686, #43929, .T. ) ;
#39233 = CARTESIAN_POINT ( 'NONE',  ( 100.1685590971342776, -42.59726720982692427, 76.32194363760098099 ) ) ;
#39234 = AXIS2_PLACEMENT_3D ( 'NONE', #9090, #36789, #85411 ) ;
#39235 = CARTESIAN_POINT ( 'NONE',  ( 116.3972416472496434, -41.42873566659991269, 203.4556252759109611 ) ) ;
#39236 = CARTESIAN_POINT ( 'NONE',  ( 95.93334478249045105, -32.74178691125829488, 176.0527681330539735 ) ) ;
#39238 = CARTESIAN_POINT ( 'NONE',  ( 100.0240874364964299, -28.99487838171179632, 281.6641967044822650 ) ) ;
#39237 = CARTESIAN_POINT ( 'NONE',  ( 108.8425424519434159, -46.66004013212315016, 22.71840272409394146 ) ) ;
#39239 = CARTESIAN_POINT ( 'NONE',  ( 138.8167039024479834, -50.82844715994100682, 88.43480685541499042 ) ) ;
#39240 = CARTESIAN_POINT ( 'NONE',  ( 165.3359832912740046, -36.32844715994100682, -5.074374724088000832 ) ) ;
#39241 = EDGE_LOOP ( 'NONE', ( #88525, #28865, #32737, #87191 ) ) ;
#39242 = EDGE_CURVE ( 'NONE', #81785, #37024, #37116, .T. ) ;
#39243 = ORIENTED_EDGE ( 'NONE', *, *, #55714, .F. ) ;
#39244 = AXIS2_PLACEMENT_3D ( 'NONE', #13346, #60578, #41033 ) ;
#39245 = EDGE_CURVE ( 'NONE', #8740, #82586, #25234, .T. ) ;
#39246 = CARTESIAN_POINT ( 'NONE',  ( 1.154229608196380665E-15, 152.3879256507328250, 9.425000000000000711 ) ) ;
#39247 = CARTESIAN_POINT ( 'NONE',  ( 113.0507064547910829, -46.07834852625790489, 218.0175300378159591 ) ) ;
#39248 = ORIENTED_EDGE ( 'NONE', *, *, #68560, .T. ) ;
#39249 = CARTESIAN_POINT ( 'NONE',  ( 104.4536708109005332, -26.63686367483539996, 200.2784824187679362 ) ) ;
#39250 = DIRECTION ( 'NONE',  ( 4.194175870806139918E-14, -1.000000000000000000, 0.000000000000000000 ) ) ;
#39251 = CARTESIAN_POINT ( 'NONE',  ( -23.26572343534745357, 54.67490044792280202, 30.17145907252543324 ) ) ;
#39252 = CARTESIAN_POINT ( 'NONE',  ( 248.6659999999999968, 52.73749999999999716, -2.903194600000015502 ) ) ;
#39253 = CARTESIAN_POINT ( 'NONE',  ( 143.5351098994992469, -139.6638757450721755, 247.2744478881182317 ) ) ;
#39255 = CARTESIAN_POINT ( 'NONE',  ( 0.000000000000000000, 223.9999999999999716, 0.000000000000000000 ) ) ;
#39254 = CARTESIAN_POINT ( 'NONE',  ( 104.3811196497008211, -29.05541074625367060, 277.6356252759112522 ) ) ;
#39256 = CARTESIAN_POINT ( 'NONE',  ( 116.3212776292303090, -32.94146857471486811, 175.1356252759109680 ) ) ;
#39257 = CARTESIAN_POINT ( 'NONE',  ( -487.2989999999999782, 14.28749999999982201, 85.72499999999999432 ) ) ;
#39258 = CIRCLE ( 'NONE', #7362, 9.425000000000000711 ) ;
#39259 = CARTESIAN_POINT ( 'NONE',  ( 51.42025729302567072, -31.94127993907664020, 193.9678068554150911 ) ) ;
#39260 = AXIS2_PLACEMENT_3D ( 'NONE', #5665, #40157, #19289 ) ;
#39261 = CARTESIAN_POINT ( 'NONE',  ( 68.06364636000260759, -137.1614519753756838, 247.2373024094184188 ) ) ;
#39262 = CARTESIAN_POINT ( 'NONE',  ( 88.90000000000000568, 69.84999999999999432, 244.4749999999999943 ) ) ;
#39263 = CARTESIAN_POINT ( 'NONE',  ( 80.06648329127402519, -46.72944715994105991, 4.925625275910944012 ) ) ;
#39264 = ADVANCED_FACE ( 'NONE', ( #30766, #86186 ), #67068, .T. ) ;
#39266 = ORIENTED_EDGE ( 'NONE', *, *, #48527, .F. ) ;
#39265 = CARTESIAN_POINT ( 'NONE',  ( -11.02155491792549391, 88.91427639974091335, -118.0434862571549957 ) ) ;
#39267 = CARTESIAN_POINT ( 'NONE',  ( 136.8164763767836121, -18.77596264856166997, 6.749779334552346022 ) ) ;
#39268 = CARTESIAN_POINT ( 'NONE',  ( 104.4049122349322545, -25.97716923158638735, 240.2575300378159682 ) ) ;
#39269 = CARTESIAN_POINT ( 'NONE',  ( 98.33631928459364246, -42.42740502779041378, 97.78705384733993355 ) ) ;
#39270 = CARTESIAN_POINT ( 'NONE',  ( 112.4768706805521248, -45.73309770202773450, 234.0070538473389377 ) ) ;
#39271 = LINE ( 'NONE', #61051, #75891 ) ;
#39272 = EDGE_CURVE ( 'NONE', #45837, #67341, #58620, .T. ) ;
#39273 = CARTESIAN_POINT ( 'NONE',  ( 182.0374245136172249, -23.42844715993459559, 237.4678068554150059 ) ) ;
#39275 = CARTESIAN_POINT ( 'NONE',  ( 98.36167194966670024, -41.66165578274063819, 37.73640923713256257 ) ) ;
#39274 = DIRECTION ( 'NONE',  ( 0.000000000000000000, -1.000000000000000000, 0.000000000000000000 ) ) ;
#39276 = DIRECTION ( 'NONE',  ( -0.9254794337955620787, -0.3787978585227822492, 0.000000000000000000 ) ) ;
#39277 = FACE_OUTER_BOUND ( 'NONE', #28484, .T. ) ;
#39278 = EDGE_LOOP ( 'NONE', ( #61302, #32053, #68894, #40725, #38108 ) ) ;
#39279 = ORIENTED_EDGE ( 'NONE', *, *, #14863, .T. ) ;
#39280 = B_SPLINE_CURVE_WITH_KNOTS ( 'NONE', 3,
 ( #77702, #50422, #79048, #9999, #16814, #29547, #57232, #44496, #37710, #78165, #65407, #30886, #68084, #25400, #67634, #67180, #26298, #53974 ),
 .UNSPECIFIED., .F., .F.,
 ( 4, 2, 2, 2, 2, 2, 2, 2, 4 ),
 ( 0.4999999989579788640, 0.5624999990882315615, 0.6249999992184841480, 0.6874999993487367345, 0.7499999994789894320, 0.8124999996092421295, 0.8749999997394947160, 0.9374999998697473025, 1.000000000000000000 ),
 .UNSPECIFIED. ) ;
#39281 = CARTESIAN_POINT ( 'NONE',  ( 99.62716111080935377, -40.92618603589043147, 136.1581341137909646 ) ) ;
#39283 = VERTEX_POINT ( 'NONE', #79830 ) ;
#39282 = DIRECTION ( 'NONE',  ( 0.000000000000000000, -1.000000000000000000, 0.000000000000000000 ) ) ;
#39284 = CARTESIAN_POINT ( 'NONE',  ( 97.31588645854830588, -39.30608289716393244, 91.53079023596599484 ) ) ;
#39285 = CARTESIAN_POINT ( 'NONE',  ( 99.43809884604152671, -27.69271567064635065, 146.6356252759109395 ) ) ;
#39286 = DIRECTION ( 'NONE',  ( -1.000000000000000078E-15, -1.000000000000000083E-30, 1.000000000000000000 ) ) ;
#39287 = VECTOR ( 'NONE', #73371, 1000.000000000000000 ) ;
#39288 = CARTESIAN_POINT ( 'NONE',  ( 110.7536356736639220, -105.8297479413482733, -19.78219314458196010 ) ) ;
#39289 = CIRCLE ( 'NONE', #32216, 2.116999999999993776 ) ;
#39290 = ADVANCED_FACE ( 'NONE', ( #52509 ), #87969, .T. ) ;
#39291 = DIRECTION ( 'NONE',  ( 0.000000000000000000, 0.000000000000000000, 1.000000000000000000 ) ) ;
#39292 = CARTESIAN_POINT ( 'NONE',  ( 193.0374249753374443, -23.42844715993432558, 300.4678068554149490 ) ) ;
#39293 = CARTESIAN_POINT ( 'NONE',  ( 115.0479362680066515, -42.38275094372912122, 53.33562527591095659 ) ) ;
#39294 = EDGE_LOOP ( 'NONE', ( #13231, #71807, #4653, #50515 ) ) ;
#39295 = ORIENTED_EDGE ( 'NONE', *, *, #9847, .F. ) ;
#39297 = ORIENTED_EDGE ( 'NONE', *, *, #18249, .F. ) ;
#39296 = AXIS2_PLACEMENT_3D ( 'NONE', #11789, #80843, #53073 ) ;
#39298 = EDGE_CURVE ( 'NONE', #48100, #55376, #59349, .T. ) ;
#39299 = DIRECTION ( 'NONE',  ( -1.087812297297669405E-15, 1.000000000000000000, -3.100000000000000044E-14 ) ) ;
#39301 = CARTESIAN_POINT ( 'NONE',  ( 31.75000000000000000, 111.1250000000000000, 3.174999999999999822 ) ) ;
#39300 = CARTESIAN_POINT ( 'NONE',  ( 117.0460787713798965, -39.54838250520747778, 139.6194347997199827 ) ) ;
#39302 = DIRECTION ( 'NONE',  ( 0.5000000000000016653, -0.8660254037844377084, 2.684678751731758716E-14 ) ) ;
#39303 = CARTESIAN_POINT ( 'NONE',  ( 182.0667039024469886, -33.35206098992630075, -5.074374724088000832 ) ) ;
#39304 = DIRECTION ( 'NONE',  ( 0.000000000000000000, 0.000000000000000000, 1.000000000000000000 ) ) ;
#39305 = CARTESIAN_POINT ( 'NONE',  ( 88.44471653959712398, 93.33860577356861654, 78.95047879920433331 ) ) ;
#39306 = CARTESIAN_POINT ( 'NONE',  ( 67.06801713577654311, -67.87892521913008181, 245.5556493635576487 ) ) ;
#39307 = CARTESIAN_POINT ( 'NONE',  ( 113.3292761056179359, -27.64973082387871628, 89.60800622829195561 ) ) ;
#39308 = ORIENTED_EDGE ( 'NONE', *, *, #66210, .F. ) ;
#39309 = EDGE_LOOP ( 'NONE', ( #56107, #35370 ) ) ;
#39310 = DIRECTION ( 'NONE',  ( 0.7071067811866258435, -0.7071067811864693020, 7.071067811866266166E-16 ) ) ;
#39311 = DIRECTION ( 'NONE',  ( 0.000000000000000000, 0.000000000000000000, -1.000000000000000000 ) ) ;
#39312 = DIRECTION ( 'NONE',  ( 0.000000000000000000, 0.000000000000000000, -1.000000000000000000 ) ) ;
#39313 = CARTESIAN_POINT ( 'NONE',  ( 107.8028422452843387, -28.59910946728008341, 152.8223760838769749 ) ) ;
#39314 = EDGE_CURVE ( 'NONE', #14684, #51499, #29594, .T. ) ;
#39315 = EDGE_CURVE ( 'NONE', #37614, #9481, #42666, .T. ) ;
#39316 = LINE ( 'NONE', #67024, #6884 ) ;
#39317 = ORIENTED_EDGE ( 'NONE', *, *, #4246, .T. ) ;
#39318 = ORIENTED_EDGE ( 'NONE', *, *, #17993, .T. ) ;
#39319 = DIRECTION ( 'NONE',  ( 0.000000000000000000, 0.000000000000000000, -1.000000000000000000 ) ) ;
#39320 = AXIS2_PLACEMENT_3D ( 'NONE', #27327, #73688, #66868 ) ;
#39321 = EDGE_CURVE ( 'NONE', #14135, #29287, #25731, .T. ) ;
#39322 = EDGE_LOOP ( 'NONE', ( #342, #50286, #24820, #74899 ) ) ;
#39323 = ORIENTED_EDGE ( 'NONE', *, *, #24270, .F. ) ;
#39324 = DIRECTION ( 'NONE',  ( 0.000000000000000000, 0.000000000000000000, -1.000000000000000000 ) ) ;
#39325 = CARTESIAN_POINT ( 'NONE',  ( 117.0318879909729048, -38.19962202173364574, 220.1415833058969724 ) ) ;
#39326 = EDGE_CURVE ( 'NONE', #22294, #4135, #54254, .T. ) ;
#39327 = CARTESIAN_POINT ( 'NONE',  ( 97.81168895331838087, -40.51742574516882200, 287.6356252759109680 ) ) ;
#39328 = VECTOR ( 'NONE', #55047, 1000.000000000000000 ) ;
#39329 = CARTESIAN_POINT ( 'NONE',  ( 181.8884939055940038, -32.11662333284530746, -5.074374724088000832 ) ) ;
#39330 = CARTESIAN_POINT ( 'NONE',  ( -110.3398647909624515, 62.06622433141639306, 69.78526909086103558 ) ) ;
#39331 = EDGE_LOOP ( 'NONE', ( #73402, #78485, #20706, #24098 ) ) ;
#39332 = VERTEX_POINT ( 'NONE', #52070 ) ;
#39333 = ADVANCED_FACE ( 'NONE', ( #18018 ), #74338, .F. ) ;
#39334 = VECTOR ( 'NONE', #50951, 1000.000000000000000 ) ;
#39335 = VERTEX_POINT ( 'NONE', #81173 ) ;
#39336 = ORIENTED_EDGE ( 'NONE', *, *, #61358, .T. ) ;
#39337 = EDGE_CURVE ( 'NONE', #51959, #34521, #31075, .T. ) ;
#39338 = CARTESIAN_POINT ( 'NONE',  ( 110.6228153916969603, -44.07670705792993715, 245.7538046553059701 ) ) ;
#39339 = CARTESIAN_POINT ( 'NONE',  ( 109.7758433794879664, -47.46978277150036263, 92.78514908543495210 ) ) ;
#39340 = CARTESIAN_POINT ( 'NONE',  ( 103.6060256796756534, -46.54035428658124118, 57.30705384733997221 ) ) ;
#39341 = DIRECTION ( 'NONE',  ( 0.000000000000000000, 0.000000000000000000, -1.000000000000000000 ) ) ;
#39342 = B_SPLINE_SURFACE_WITH_KNOTS ( 'NONE', 3, 3, ( 
 ( #65549, #17405, #15629, #86016 ),
 ( #51453, #23789, #36520, #50572 ),
 ( #16960, #51888, #84678, #85575 ),
 ( #71047, #1992, #50117, #71494 ),
 ( #8822, #77853, #31025, #79647 ) ),
 .UNSPECIFIED., .F., .F., .F.,
 ( 4, 1, 4 ),
 ( 4, 4 ),
 ( -2.333654191434229903E-06, 0.5714285714285709528, 1.000000000000000000 ),
 ( 0.1538195221703859972, 0.4047106084325320374 ),
 .UNSPECIFIED. ) ;
#39343 = LINE ( 'NONE', #51619, #65472 ) ;
#39344 = CARTESIAN_POINT ( 'NONE',  ( 115.4866590905505603, -31.25382064240195845, 195.2850823816886532 ) ) ;
#39345 = CARTESIAN_POINT ( 'NONE',  ( 98.85664311730629095, -30.30429143764317601, 151.7984824187679465 ) ) ;
#39346 = DIRECTION ( 'NONE',  ( 0.000000000000000000, -1.000000000000000000, 0.000000000000000000 ) ) ;
#39347 = VERTEX_POINT ( 'NONE', #66615 ) ;
#39348 = DIRECTION ( 'NONE',  ( -0.7071067811865171526, -0.7071067811865779928, -6.612322855854603498E-17 ) ) ;
#39349 = EDGE_LOOP ( 'NONE', ( #13534, #41645, #58597, #29532 ) ) ;
#39350 = CIRCLE ( 'NONE', #46593, 2.116999999999980009 ) ;
#39351 = ORIENTED_EDGE ( 'NONE', *, *, #9732, .T. ) ;
#39352 = CARTESIAN_POINT ( 'NONE',  ( 116.3251085584666527, -32.94148239642360210, 265.1356252759109680 ) ) ;
#39353 = CARTESIAN_POINT ( 'NONE',  ( 3.175000000000334666, 24.56180297284579694, 31.75000000000000000 ) ) ;
#39354 = VERTEX_POINT ( 'NONE', #58456 ) ;
#39355 = VECTOR ( 'NONE', #78402, 1000.000000000000000 ) ;
#39356 = LINE ( 'NONE', #73876, #2648 ) ;
#39357 = ORIENTED_EDGE ( 'NONE', *, *, #7427, .F. ) ;
#39358 = CARTESIAN_POINT ( 'NONE',  ( 0.000000000000000000, 91.07499999999996021, 0.000000000000000000 ) ) ;
#39359 = CARTESIAN_POINT ( 'NONE',  ( 95.48778530930356112, -34.20472165425801592, 106.1556252759109640 ) ) ;
#39360 = CARTESIAN_POINT ( 'NONE',  ( 88.90000000000000568, 66.67499999999999716, 244.4749999999999943 ) ) ;
#39361 = LINE ( 'NONE', #3947, #14444 ) ;
#39362 = CARTESIAN_POINT ( 'NONE',  ( 80.06648329127399677, 0.2215528400590013880, 4.925625275911999168 ) ) ;
#39363 = CARTESIAN_POINT ( 'NONE',  ( 102.0841886111852261, -27.63463957783707770, 100.4632443235309580 ) ) ;
#39365 = CARTESIAN_POINT ( 'NONE',  ( 113.7366723824214318, -44.71300795807891149, 189.1299109901969757 ) ) ;
#39364 = CARTESIAN_POINT ( 'NONE',  ( 41.56648329127499153, -32.07844715994070839, 203.6756252759119832 ) ) ;
#39366 = LINE ( 'NONE', #61586, #46617 ) ;
#39367 = DIRECTION ( 'NONE',  ( 1.000000000000000000, 0.000000000000000000, 0.000000000000000000 ) ) ;
#39368 = ORIENTED_EDGE ( 'NONE', *, *, #2004, .T. ) ;
#39369 = VECTOR ( 'NONE', #2947, 1000.000000000000000 ) ;
#39370 = CARTESIAN_POINT ( 'NONE',  ( 163.0664832912739826, -0.7548456658610993575, 335.0256252759120343 ) ) ;
#39371 = CARTESIAN_POINT ( 'NONE',  ( 106.0667039024470455, -121.2010968907524529, -19.26696060647547881 ) ) ;
#39372 = CARTESIAN_POINT ( 'NONE',  ( 113.2475547418459598, -28.76023609674211201, 134.5522767884087898 ) ) ;
#39373 = AXIS2_PLACEMENT_3D ( 'NONE', #13457, #27086, #39796 ) ;
#39374 = CARTESIAN_POINT ( 'NONE',  ( 123.6837132603321692, -16.81243780205712568, 249.5838068554165261 ) ) ;
#39376 = ORIENTED_EDGE ( 'NONE', *, *, #27435, .T. ) ;
#39375 = CARTESIAN_POINT ( 'NONE',  ( 115.4954577264304731, -29.50689403799194110, 229.4022919425779605 ) ) ;
#39377 = CARTESIAN_POINT ( 'NONE',  ( 97.78494874870966669, -40.45152301011977158, 146.6299652419585584 ) ) ;
#39378 = CARTESIAN_POINT ( 'NONE',  ( 118.5708186345730724, -33.89864261627929665, 10.01848241876795953 ) ) ;
#39379 = CARTESIAN_POINT ( 'NONE',  ( 103.1584010082818850, -27.01760528431355368, 126.3813395616259783 ) ) ;
#39380 = DIRECTION ( 'NONE',  ( 0.7071067811865531239, 0.000000000000000000, 0.7071067811865420216 ) ) ;
#39381 = EDGE_CURVE ( 'NONE', #36556, #75352, #45269, .T. ) ;
#39382 = CARTESIAN_POINT ( 'NONE',  ( 5.624702496966087928, 93.94413577832827400, -130.4352985349313201 ) ) ;
#39383 = CARTESIAN_POINT ( 'NONE',  ( 62.03715912545824551, -47.82818131006021645, 300.4678068554150627 ) ) ;
#39384 = DIRECTION ( 'NONE',  ( 4.299999999999999979E-14, -1.000000000000000000, 4.400000000000000367E-29 ) ) ;
#39385 = ORIENTED_EDGE ( 'NONE', *, *, #36547, .T. ) ;
#39386 = ORIENTED_EDGE ( 'NONE', *, *, #29878, .F. ) ;
#39387 = ORIENTED_EDGE ( 'NONE', *, *, #77021, .T. ) ;
#39388 = AXIS2_PLACEMENT_3D ( 'NONE', #84992, #25750, #53427 ) ;
#39389 = ORIENTED_EDGE ( 'NONE', *, *, #34753, .T. ) ;
#39390 = DIRECTION ( 'NONE',  ( 1.000000000000000078E-15, -1.000000000000000000, 0.000000000000000000 ) ) ;
#39391 = CARTESIAN_POINT ( 'NONE',  ( 97.82856912889593559, -29.34641599088761765, 41.78991099019596334 ) ) ;
#39392 = DIRECTION ( 'NONE',  ( 0.000000000000000000, 0.000000000000000000, -1.000000000000000000 ) ) ;
#39393 = CARTESIAN_POINT ( 'NONE',  ( -487.2989999999999782, 14.28750000000023945, 19.36139197104649767 ) ) ;
#39395 = LINE ( 'NONE', #46187, #34038 ) ;
#39394 = DIRECTION ( 'NONE',  ( 1.000000000000000000, 4.163336342344333240E-14, 0.000000000000000000 ) ) ;
#39396 = CIRCLE ( 'NONE', #26308, 3.000000000000002665 ) ;
#39397 = CARTESIAN_POINT ( 'NONE',  ( 104.8904560483511545, -27.93868065388478428, 239.6800388756959705 ) ) ;
#39398 = ORIENTED_EDGE ( 'NONE', *, *, #51410, .F. ) ;
#39399 = EDGE_LOOP ( 'NONE', ( #14425, #49903, #45960, #56314 ) ) ;
#39400 = EDGE_LOOP ( 'NONE', ( #52974, #4069, #64714, #14851 ) ) ;
#39401 = AXIS2_PLACEMENT_3D ( 'NONE', #54841, #48468, #13540 ) ;
#39402 = EDGE_CURVE ( 'NONE', #53017, #87676, #72985, .T. ) ;
#39403 = CARTESIAN_POINT ( 'NONE',  ( -76.76779673090611311, 55.97500000000000142, 30.90025125786759830 ) ) ;
#39404 = CARTESIAN_POINT ( 'NONE',  ( 97.84203259209142800, -40.59156174939596440, 101.6424438322808896 ) ) ;
#39405 = DIRECTION ( 'NONE',  ( 1.000000000000000078E-15, -1.000000000000000083E-30, -1.000000000000000000 ) ) ;
#39406 = DIRECTION ( 'NONE',  ( -1.000000000000000000, -1.206764157201257538E-15, 0.000000000000000000 ) ) ;
#39407 = CARTESIAN_POINT ( 'NONE',  ( 110.4493835822141676, -45.49486465592072904, 14.28920235351599466 ) ) ;
#39408 = CARTESIAN_POINT ( 'NONE',  ( 117.9083627453487821, 85.43299024555679466, -12.37536754217405033 ) ) ;
#39409 = LINE ( 'NONE', #33491, #60792 ) ;
#39410 = CARTESIAN_POINT ( 'NONE',  ( 105.7207279102414077, -46.41719084699269615, 257.4670538473400825 ) ) ;
#39411 = CYLINDRICAL_SURFACE ( 'NONE', #83472, 9.999999999999998224 ) ;
#39412 = PRODUCT_RELATED_PRODUCT_CATEGORY ( 'part', '', ( #73550 ) ) ;
#39414 = EDGE_LOOP ( 'NONE', ( #21717, #2136, #66255, #76735 ) ) ;
#39413 = AXIS2_PLACEMENT_3D ( 'NONE', #34941, #15862, #28575 ) ;
#39415 = FACE_OUTER_BOUND ( 'NONE', #13148, .T. ) ;
#39416 = FACE_OUTER_BOUND ( 'NONE', #49066, .T. ) ;
#39417 = CARTESIAN_POINT ( 'NONE',  ( 114.6445280793269603, -33.69580855137893138, 51.94809036959197357 ) ) ;
#39418 = VECTOR ( 'NONE', #11802, 1000.000000000000000 ) ;
#39419 = DIRECTION ( 'NONE',  ( -1.000000000000000000, -3.999999999999999995E-14, -1.000000000000000078E-15 ) ) ;
#39420 = FACE_BOUND ( 'NONE', #11657, .T. ) ;
#39421 = EDGE_CURVE ( 'NONE', #75636, #28680, #49874, .T. ) ;
#39422 = VECTOR ( 'NONE', #35334, 1000.000000000000000 ) ;
#39423 = CARTESIAN_POINT ( 'NONE',  ( -1.665381768328644485, 95.16753744185723463, 118.5470859077611863 ) ) ;
#39424 = ORIENTED_EDGE ( 'NONE', *, *, #65582, .F. ) ;
#39425 = FACE_OUTER_BOUND ( 'NONE', #71556, .T. ) ;
#39426 = CARTESIAN_POINT ( 'NONE',  ( 120.0660739680716915, 56.80016398518806398, -51.27402828685031011 ) ) ;
#39427 = EDGE_CURVE ( 'NONE', #24990, #17829, #3948, .T. ) ;
#39428 = ORIENTED_EDGE ( 'NONE', *, *, #14771, .F. ) ;
#39429 = CARTESIAN_POINT ( 'NONE',  ( 108.3194705677269809, -47.07918403323724021, 117.6727681330539639 ) ) ;
#39430 = ORIENTED_EDGE ( 'NONE', *, *, #45969, .F. ) ;
#39431 = ADVANCED_FACE ( 'NONE', ( #73432 ), #4406, .F. ) ;
#39433 = AXIS2_PLACEMENT_3D ( 'NONE', #32425, #19708, #25627 ) ;
#39432 = CARTESIAN_POINT ( 'NONE',  ( 99.88917683200891418, -30.19057113389683167, 80.16099125664798919 ) ) ;
#39434 = LINE ( 'NONE', #18996, #86656 ) ;
#39435 = CARTESIAN_POINT ( 'NONE',  ( 103.7844689056781675, -44.99325446404193940, 113.7072975916109669 ) ) ;
#39436 = EDGE_CURVE ( 'NONE', #59657, #85115, #45506, .T. ) ;
#39437 = CARTESIAN_POINT ( 'NONE',  ( -17.13243906362141900, 148.4450814996825443, 42.79834678115690849 ) ) ;
#39438 = CARTESIAN_POINT ( 'NONE',  ( 143.2674661430137917, -68.27559814658837922, 247.0029128788180230 ) ) ;
#39439 = CARTESIAN_POINT ( 'NONE',  ( 104.7308122791112908, -47.55672043936114335, 28.41943479971997988 ) ) ;
#39440 = CARTESIAN_POINT ( 'NONE',  ( 109.7253519077453632, -27.00093404018718246, 180.8651952712820332 ) ) ;
#39441 = ORIENTED_EDGE ( 'NONE', *, *, #14660, .T. ) ;
#39442 = CARTESIAN_POINT ( 'NONE',  ( 130.5667039024482960, -36.72944715994102438, 249.5838068554162987 ) ) ;
#39443 = ORIENTED_EDGE ( 'NONE', *, *, #42244, .F. ) ;
#39444 = CARTESIAN_POINT ( 'NONE',  ( 77.53592152231151147, -19.80596063775423588, 2.807537029278938334 ) ) ;
#39445 = EDGE_LOOP ( 'NONE', ( #74542, #86490 ) ) ;
#39446 = EDGE_LOOP ( 'NONE', ( #80944, #50607, #27659, #33852, #18246, #86569 ) ) ;
#39447 = ADVANCED_FACE ( 'NONE', ( #88870 ), #268, .T. ) ;
#39448 = DIRECTION ( 'NONE',  ( 1.000000000000000078E-15, -1.000000000000000000, 0.000000000000000000 ) ) ;
#39449 = ORIENTED_EDGE ( 'NONE', *, *, #13507, .T. ) ;
#39450 = CARTESIAN_POINT ( 'NONE',  ( 97.17009264939167679, -31.66255117090383564, 245.9499109901979637 ) ) ;
#39451 = B_SPLINE_CURVE_WITH_KNOTS ( 'NONE', 3,
 ( #75324, #5844, #62129, #33968, #12650, #55732, #89862, #27612, #26271, #83052, #42125, #69852, #68059, #20804, #26707, #89408, #7623, #53947, #27166, #77558, #15788, #43463, #49384, #8071, #28967 ),
 .UNSPECIFIED., .F., .F.,
 ( 4, 2, 2, 2, 2, 2, 2, 2, 2, 1, 2, 2, 4 ),
 ( 6.610103225985008611E-19, 0.002483982529268030041, 0.003725973793902044844, 0.004967965058536060081, 0.007451947587804091423, 0.008693938852438104492, 0.009935930117072118428, 0.01241991264634014977, 0.01366190391097416197, 0.01490389517560817417, 0.01614588644024218464, 0.01738787770487619858, 0.01987186023414422298 ),
 .UNSPECIFIED. ) ;
#39452 = CARTESIAN_POINT ( 'NONE',  ( 97.04389485639831037, -36.22610523983841091, 126.2859809355158518 ) ) ;
#39453 = CARTESIAN_POINT ( 'NONE',  ( 108.3334480168114311, -46.73485936460039625, 188.6772919363633321 ) ) ;
#39454 = CARTESIAN_POINT ( 'NONE',  ( 113.4595210239597520, -46.70760751678911049, 64.02991099019695298 ) ) ;
#39455 = CARTESIAN_POINT ( 'NONE',  ( 113.2489316331219413, -28.76130024733460999, 95.55172767996501193 ) ) ;
#39456 = ORIENTED_EDGE ( 'NONE', *, *, #71437, .F. ) ;
#39457 = DIRECTION ( 'NONE',  ( 1.000000000000000000, 4.163336342344333240E-14, 0.000000000000000000 ) ) ;
#39458 = CARTESIAN_POINT ( 'NONE',  ( 182.2300522401179705, -33.89581943343660697, 117.4678068554150627 ) ) ;
#39459 = AXIS2_PLACEMENT_3D ( 'NONE', #44505, #59472, #4529 ) ;
#39460 = VERTEX_POINT ( 'NONE', #60686 ) ;
#39461 = VECTOR ( 'NONE', #63833, 1000.000000000000000 ) ;
#39462 = DIRECTION ( 'NONE',  ( -1.000000000000000078E-15, 1.000000000000000083E-30, 1.000000000000000000 ) ) ;
#39463 = DIRECTION ( 'NONE',  ( 0.7071067811868666508, 0.7071067811862283836, 7.071067811868969987E-16 ) ) ;
#39464 = CARTESIAN_POINT ( 'NONE',  ( 116.5620552962771654, -42.34175257684902505, 283.4137205140060587 ) ) ;
#39465 = LINE ( 'NONE', #53509, #38788 ) ;
#39466 = DIRECTION ( 'NONE',  ( -1.000000000000000078E-15, 1.000000000000000083E-30, 1.000000000000000000 ) ) ;
#39467 = DIRECTION ( 'NONE',  ( 0.000000000000000000, 0.000000000000000000, -1.000000000000000000 ) ) ;
#39468 = CARTESIAN_POINT ( 'NONE',  ( 115.6077113496922948, -36.78907078068826308, 263.2438483995052820 ) ) ;
#39470 = CARTESIAN_POINT ( 'NONE',  ( 115.2499566122392736, -44.12502604085369029, 79.25372051400697160 ) ) ;
#39469 = DIRECTION ( 'NONE',  ( 0.000000000000000000, 1.000000000000000000, 0.000000000000000000 ) ) ;
#39471 = CARTESIAN_POINT ( 'NONE',  ( 113.1543859615763949, 68.83350072574626211, 65.12264306354134646 ) ) ;
#39472 = CARTESIAN_POINT ( 'NONE',  ( 114.7398264468854592, -44.75021323582976862, 113.1718157521009687 ) ) ;
#39473 = ORIENTED_EDGE ( 'NONE', *, *, #74088, .T. ) ;
#39474 = CARTESIAN_POINT ( 'NONE',  ( 163.0664832912739826, -8.350947159940998787, 333.4006252759120343 ) ) ;
#39475 = ORIENTED_EDGE ( 'NONE', *, *, #14262, .F. ) ;
#39476 = DIRECTION ( 'NONE',  ( -0.7071067811865456854, -7.071067811865457584E-16, 0.7071067811865493491 ) ) ;
#39477 = CARTESIAN_POINT ( 'NONE',  ( 38.10000000000000142, 95.25000000000000000, 358.0130000000000337 ) ) ;
#39478 = PRODUCT_DEFINITION_SHAPE ( 'NONE', 'NONE',  #89940 ) ;
#39479 = CARTESIAN_POINT ( 'NONE',  ( 63.03715912545733602, -46.82818131006016671, 193.9678068554150911 ) ) ;
#39480 = ORIENTED_EDGE ( 'NONE', *, *, #17869, .T. ) ;
#39481 = AXIS2_PLACEMENT_3D ( 'NONE', #18873, #74291, #59741 ) ;
#39482 = CARTESIAN_POINT ( 'NONE',  ( 107.9678037105606023, -87.30234574837474781, -19.18411693322955003 ) ) ;
#39484 = VERTEX_POINT ( 'NONE', #27521 ) ;
#39483 = CARTESIAN_POINT ( 'NONE',  ( 98.82181093208917844, -30.27703119756231942, 155.7984824187679465 ) ) ;
#39485 = CARTESIAN_POINT ( 'NONE',  ( -27.27158787008326968, 127.0000000000000000, 85.23828826961327820 ) ) ;
#39486 = CARTESIAN_POINT ( 'NONE',  ( -130.4513346304067909, 94.12569442554141119, -5.240856348472988202 ) ) ;
#39487 = EDGE_CURVE ( 'NONE', #21457, #11589, #33442, .T. ) ;
#39488 = DIRECTION ( 'NONE',  ( -0.7071067811874389708, 0.7071067811856560636, 0.000000000000000000 ) ) ;
#39489 = VECTOR ( 'NONE', #48416, 1000.000000000000000 ) ;
#39490 = LINE ( 'NONE', #18147, #29237 ) ;
#39491 = ORIENTED_EDGE ( 'NONE', *, *, #62919, .T. ) ;
#39492 = VECTOR ( 'NONE', #46591, 1000.000000000000000 ) ;
#39493 = CARTESIAN_POINT ( 'NONE',  ( 117.2437917682886592, -42.84961121563711828, 128.3956252759109873 ) ) ;
#39494 = SHAPE_DEFINITION_REPRESENTATION ( #45226, #885 ) ;
#39495 = EDGE_CURVE ( 'NONE', #42455, #33402, #89771, .T. ) ;
#39496 = DIRECTION ( 'NONE',  ( 0.000000000000000000, 0.000000000000000000, -1.000000000000000000 ) ) ;
#39497 = DIRECTION ( 'NONE',  ( -1.000000000000000078E-15, 1.000000000000000000, 0.000000000000000000 ) ) ;
#39498 = ORIENTED_EDGE ( 'NONE', *, *, #61973, .T. ) ;
#39499 = AXIS2_PLACEMENT_3D ( 'NONE', #12114, #61150, #81178 ) ;
#39500 = EDGE_LOOP ( 'NONE', ( #27385, #72535 ) ) ;
#39501 = CARTESIAN_POINT ( 'NONE',  ( 37.06648329127400388, 12.92155284005802685, 334.6228282640712450 ) ) ;
#39502 = CARTESIAN_POINT ( 'NONE',  ( 108.9650027145310673, -26.85270947969657129, 249.9258047739795359 ) ) ;
#39503 = CARTESIAN_POINT ( 'NONE',  ( 183.5150000000000148, 14.63749999999999929, -52.38749999999999574 ) ) ;
#39504 = DIRECTION ( 'NONE',  ( -0.7071067811866258435, 0.7071067811864693020, -7.071067811866266166E-16 ) ) ;
#39506 = DIRECTION ( 'NONE',  ( 0.000000000000000000, 0.000000000000000000, 1.000000000000000000 ) ) ;
#39505 = DIRECTION ( 'NONE',  ( 1.000000000000000000, 1.000000000000000078E-15, -0.000000000000000000 ) ) ;
#39507 = CARTESIAN_POINT ( 'NONE',  ( 194.0371591254584587, -46.82818131005407736, 180.4678068554150343 ) ) ;
#39508 = ORIENTED_EDGE ( 'NONE', *, *, #53663, .F. ) ;
#39509 = EDGE_CURVE ( 'NONE', #72918, #88176, #6635, .T. ) ;
#39510 = LINE ( 'NONE', #13159, #5596 ) ;
#39511 = CARTESIAN_POINT ( 'NONE',  ( 101.7740290765682829, -45.64733444449320388, 203.1622919425769567 ) ) ;
#39513 = ORIENTED_EDGE ( 'NONE', *, *, #42504, .T. ) ;
#39512 = FACE_BOUND ( 'NONE', #42553, .T. ) ;
#39514 = CIRCLE ( 'NONE', #62732, 10.00000000000000888 ) ;
#39515 = CARTESIAN_POINT ( 'NONE',  ( 117.3261810260835603, -38.23854875528750341, 69.72229194257801055 ) ) ;
#39516 = DIRECTION ( 'NONE',  ( -1.000000000000000000, 0.000000000000000000, 0.000000000000000000 ) ) ;
#39517 = CARTESIAN_POINT ( 'NONE',  ( 117.0724228248738257, -35.46685996557965126, 13.92770122325937443 ) ) ;
#39518 = CARTESIAN_POINT ( 'NONE',  ( 0.000000000000000000, 67.86880000000000734, 265.5569999999999595 ) ) ;
#39519 = ORIENTED_EDGE ( 'NONE', *, *, #74827, .F. ) ;
#39520 = CARTESIAN_POINT ( 'NONE',  ( 0.000000000000000000, 125.7300000000000040, 0.000000000000000000 ) ) ;
#39521 = ORIENTED_EDGE ( 'NONE', *, *, #66895, .F. ) ;
#39522 = ORIENTED_EDGE ( 'NONE', *, *, #53995, .F. ) ;
#39523 = CARTESIAN_POINT ( 'NONE',  ( 112.2971567814265512, -43.88265157833087926, 224.5101547344679886 ) ) ;
#39524 = CIRCLE ( 'NONE', #74363, 0.5000000000000004441 ) ;
#39525 = CARTESIAN_POINT ( 'NONE',  ( 41.56648329127499153, -36.32844715994070839, 143.6756252759119832 ) ) ;
#39526 = DIRECTION ( 'NONE',  ( -0.000000000000000000, -0.000000000000000000, 1.000000000000000000 ) ) ;
#39527 = CARTESIAN_POINT ( 'NONE',  ( 163.2569089553707329, -33.54226604284440327, 237.4678068554150059 ) ) ;
#39528 = LINE ( 'NONE', #61309, #9619 ) ;
#39529 = ORIENTED_EDGE ( 'NONE', *, *, #68360, .T. ) ;
#39530 = CARTESIAN_POINT ( 'NONE',  ( 172.5664832912729878, -27.57844715994070484, 141.9256252759119832 ) ) ;
#39531 = DIRECTION ( 'NONE',  ( -1.000000000000000078E-15, 1.000000000000000000, 0.000000000000000000 ) ) ;
#39532 = ORIENTED_EDGE ( 'NONE', *, *, #6017, .T. ) ;
#39533 = CARTESIAN_POINT ( 'NONE',  ( 116.2977993645976227, -41.52656014244018223, 288.4441967044823514 ) ) ;
#39534 = ORIENTED_EDGE ( 'NONE', *, *, #28485, .F. ) ;
#39536 = ORIENTED_EDGE ( 'NONE', *, *, #15223, .F. ) ;
#39535 = EDGE_CURVE ( 'NONE', #37970, #51377, #64422, .T. ) ;
#39537 = CARTESIAN_POINT ( 'NONE',  ( 109.3322008939200458, -45.72736107978396092, 240.5909475124479684 ) ) ;
#39538 = CIRCLE ( 'NONE', #56915, 0.5000000000000004441 ) ;
#39539 = CARTESIAN_POINT ( 'NONE',  ( 96.37928053093608582, -33.66421044892479131, 141.1041967044829732 ) ) ;
#39540 = DIRECTION ( 'NONE',  ( -0.7759704746411383303, 0.6307692307692303046, 0.000000000000000000 ) ) ;
#39541 = DIRECTION ( 'NONE',  ( 0.000000000000000000, 0.000000000000000000, 1.000000000000000000 ) ) ;
#39542 = CARTESIAN_POINT ( 'NONE',  ( 135.2444258376725941, 0.000000000000000000, 147.4575741623265799 ) ) ;
#39543 = CARTESIAN_POINT ( 'NONE',  ( 113.1252749404788034, -46.02936877844707197, 219.0480062282919960 ) ) ;
#39544 = CARTESIAN_POINT ( 'NONE',  ( 0.000000000000000000, 184.0000000000000000, 106.1020876358972629 ) ) ;
#39545 = ORIENTED_EDGE ( 'NONE', *, *, #56240, .T. ) ;
#39546 = AXIS2_PLACEMENT_3D ( 'NONE', #75566, #20599, #81945 ) ;
#39547 = CARTESIAN_POINT ( 'NONE',  ( 108.9932425643425802, -47.01927604342903777, 78.72419670448194040 ) ) ;
#39548 = FACE_OUTER_BOUND ( 'NONE', #13424, .T. ) ;
#39549 = ORIENTED_EDGE ( 'NONE', *, *, #34364, .F. ) ;
#39550 = ORIENTED_EDGE ( 'NONE', *, *, #75766, .T. ) ;
#39551 = ORIENTED_EDGE ( 'NONE', *, *, #28883, .T. ) ;
#39552 = ADVANCED_FACE ( 'NONE', ( #55201 ), #26185, .F. ) ;
#39553 = LINE ( 'NONE', #67257, #8593 ) ;
#39555 = ADVANCED_FACE ( 'NONE', ( #19819 ), #54751, .F. ) ;
#39554 = CARTESIAN_POINT ( 'NONE',  ( 188.5667039024479834, -62.87844715994099687, 259.9678068554150059 ) ) ;
#39556 = PLANE ( 'NONE',  #27734 ) ;
#39557 = CARTESIAN_POINT ( 'NONE',  ( 108.3053489883007927, -28.16931545225084221, 147.7918998934009664 ) ) ;
#39558 = CARTESIAN_POINT ( 'NONE',  ( 101.3928372362931896, -45.54357991663450633, 218.1213395616249784 ) ) ;
#39559 = DIRECTION ( 'NONE',  ( -1.000000000000000000, 0.000000000000000000, 0.000000000000000000 ) ) ;
#39560 = ORIENTED_EDGE ( 'NONE', *, *, #84615, .T. ) ;
#39561 = DIRECTION ( 'NONE',  ( 0.000000000000000000, 0.000000000000000000, -1.000000000000000000 ) ) ;
#39562 = ORIENTED_EDGE ( 'NONE', *, *, #84842, .T. ) ;
#39563 = ORIENTED_EDGE ( 'NONE', *, *, #74293, .T. ) ;
#39564 = CARTESIAN_POINT ( 'NONE',  ( 32.09598329127638294, -23.42844715994147364, 117.4678068554150485 ) ) ;
#39565 = EDGE_LOOP ( 'NONE', ( #80896, #57656, #15402, #47978, #86761 ) ) ;
#39566 = ORIENTED_EDGE ( 'NONE', *, *, #73258, .T. ) ;
#39567 = CARTESIAN_POINT ( 'NONE',  ( 105.7167123138976024, -46.72404028231114381, 168.4698306292383734 ) ) ;
#39568 = DIRECTION ( 'NONE',  ( 3.100000000000000258E-29, -3.100000000000000044E-14, -1.000000000000000000 ) ) ;
#39569 = CARTESIAN_POINT ( 'NONE',  ( 163.0664832912739826, 19.62155284005901024, 333.4006252759110112 ) ) ;
#39570 = CARTESIAN_POINT ( 'NONE',  ( 112.4313655287739948, -30.08308194412713021, 163.9581341137909476 ) ) ;
#39571 = CARTESIAN_POINT ( 'NONE',  ( 100.4373464023292826, -44.86011580501824625, 12.03276813305398463 ) ) ;
#39572 = CARTESIAN_POINT ( 'NONE',  ( 115.0873078068954243, -30.61556636850841073, 125.3441650706716928 ) ) ;
#39573 = ORIENTED_EDGE ( 'NONE', *, *, #67301, .T. ) ;
#39574 = AXIS2_PLACEMENT_3D ( 'NONE', #62411, #7456, #41953 ) ;
#39575 = DIRECTION ( 'NONE',  ( 0.000000000000000000, 6.920681583949466031E-15, -1.000000000000000000 ) ) ;
#39576 = ORIENTED_EDGE ( 'NONE', *, *, #65477, .T. ) ;
#39577 = CARTESIAN_POINT ( 'NONE',  ( 156.5667039024483529, -48.82844715993569196, 293.2178068554149490 ) ) ;
#39578 = ORIENTED_EDGE ( 'NONE', *, *, #83520, .T. ) ;
#39579 = DIRECTION ( 'NONE',  ( 0.7071067811989671936, 0.7071067811741279519, 6.612322855971028274E-17 ) ) ;
#39580 = CARTESIAN_POINT ( 'NONE',  ( 139.2773854306074668, -133.5313011236452212, 248.4142799812389910 ) ) ;
#39581 = CARTESIAN_POINT ( 'NONE',  ( 68.76551873680897131, -137.6861246176283942, 247.4844277398459838 ) ) ;
#39582 = VECTOR ( 'NONE', #49029, 1000.000000000000000 ) ;
#39583 = CARTESIAN_POINT ( 'NONE',  ( 51.56670390244799762, -33.35206098992650681, -5.074374724088000832 ) ) ;
#39584 = ORIENTED_EDGE ( 'NONE', *, *, #16374, .T. ) ;
#39585 = CARTESIAN_POINT ( 'NONE',  ( 96.66386919200992622, -42.45828961175909200, 26.72705384733997747 ) ) ;
#39586 = CARTESIAN_POINT ( 'NONE',  ( 117.1334281162953346, -32.05460809866745109, 55.16038718067301261 ) ) ;
#39589 = EDGE_CURVE ( 'NONE', #75243, #3441, #82515, .T. ) ;
#39588 = DIRECTION ( 'NONE',  ( 0.000000000000000000, 1.000000000000000000, 0.000000000000000000 ) ) ;
#39587 = DIRECTION ( 'NONE',  ( 1.000000000000000078E-15, 1.000000000000000083E-30, -1.000000000000000000 ) ) ;
#39590 = CARTESIAN_POINT ( 'NONE',  ( 1.598849875094818280E-14, 61.59999999999999432, -130.5560000000000116 ) ) ;
#39591 = CARTESIAN_POINT ( 'NONE',  ( 106.0962982257710792, -25.30864543579675896, 322.6234344337125890 ) ) ;
#39592 = FACE_BOUND ( 'NONE', #20408, .T. ) ;
#39593 = CARTESIAN_POINT ( 'NONE',  ( 162.7131505118679797, -31.94127993907790852, -5.074374724088000832 ) ) ;
#39594 = CARTESIAN_POINT ( 'NONE',  ( 145.3678890680851623, -137.6861246176283089, 247.4844277398459838 ) ) ;
#39595 = VERTEX_POINT ( 'NONE', #5751 ) ;
#39596 = CARTESIAN_POINT ( 'NONE',  ( 96.14704956656235879, -38.72415284237285960, 51.48229194257797303 ) ) ;
#39597 = CARTESIAN_POINT ( 'NONE',  ( 106.8516137164961464, -47.78059241960190207, 223.5489586092439538 ) ) ;
#39598 = CARTESIAN_POINT ( 'NONE',  ( 117.3927859964040437, -32.72286779764937847, 90.10895860924395606 ) ) ;
#39600 = DIRECTION ( 'NONE',  ( -0.7071067811865506814, 0.7071067811865443531, -7.071067811865500971E-16 ) ) ;
#39599 = DIRECTION ( 'NONE',  ( 0.000000000000000000, 0.000000000000000000, -1.000000000000000000 ) ) ;
#39601 = DIRECTION ( 'NONE',  ( -0.000000000000000000, 1.000000000000000000, -0.000000000000000000 ) ) ;
#39602 = VECTOR ( 'NONE', #5871, 1000.000000000000000 ) ;
#39603 = EDGE_CURVE ( 'NONE', #82293, #76316, #20278, .T. ) ;
#39604 = VECTOR ( 'NONE', #10968, 1000.000000000000000 ) ;
#39605 = PLANE ( 'NONE',  #76653 ) ;
#39606 = EDGE_LOOP ( 'NONE', ( #59723, #64645 ) ) ;
#39607 = CARTESIAN_POINT ( 'NONE',  ( 112.9545114599701492, -28.19305977888952697, 85.60800622829195561 ) ) ;
#39608 = ADVANCED_FACE ( 'NONE', ( #7089 ), #6198, .T. ) ;
#39610 = ORIENTED_EDGE ( 'NONE', *, *, #14332, .F. ) ;
#39609 = CARTESIAN_POINT ( 'NONE',  ( 10.53542287845765557, 89.64189664627865284, 130.1302201369519196 ) ) ;
#39611 = CARTESIAN_POINT ( 'NONE',  ( 110.0457755916377494, -26.10929462018219382, 215.8708633711489711 ) ) ;
#39612 = PLANE ( 'NONE',  #39633 ) ;
#39613 = FACE_OUTER_BOUND ( 'NONE', #15523, .T. ) ;
#39614 = CARTESIAN_POINT ( 'NONE',  ( 38.10000000000000142, 69.84999999999999432, 358.0130000000000337 ) ) ;
#39615 = DIRECTION ( 'NONE',  ( -1.000000000000000078E-15, 1.000000000000000083E-30, 1.000000000000000000 ) ) ;
#39616 = EDGE_CURVE ( 'NONE', #19496, #53446, #18046, .T. ) ;
#39617 = ADVANCED_FACE ( 'NONE', ( #13453 ), #55643, .F. ) ;
#39618 = DIRECTION ( 'NONE',  ( 0.000000000000000000, 1.000000000000000000, 0.000000000000000000 ) ) ;
#39619 = DIRECTION ( 'NONE',  ( 1.000000000000000078E-15, -1.000000000000000000, 0.000000000000000000 ) ) ;
#39620 = CARTESIAN_POINT ( 'NONE',  ( 97.26456095925928480, -36.24355304347522377, 171.2870538473399620 ) ) ;
#39621 = EDGE_LOOP ( 'NONE', ( #33, #7799, #1855, #33813 ) ) ;
#39622 = EDGE_LOOP ( 'NONE', ( #71250, #12259, #79993, #34308, #67470, #39117, #30882, #19451 ) ) ;
#39623 = EDGE_CURVE ( 'NONE', #76096, #32183, #87370, .T. ) ;
#39624 = CARTESIAN_POINT ( 'NONE',  ( 115.4287739208600527, -39.66208659201188880, 129.9901547344679500 ) ) ;
#39625 = CARTESIAN_POINT ( 'NONE',  ( 134.0664832912740110, -41.22944715994101017, 4.925625275910997303 ) ) ;
#39627 = DIRECTION ( 'NONE',  ( 0.000000000000000000, 0.000000000000000000, -1.000000000000000000 ) ) ;
#39626 = CARTESIAN_POINT ( 'NONE',  ( 111.5675350091814266, -45.45035926415653194, 268.9556252759110180 ) ) ;
#39628 = VECTOR ( 'NONE', #72246, 1000.000000000000000 ) ;
#39629 = DIRECTION ( 'NONE',  ( 0.000000000000000000, -0.8660254037844387076, -0.4999999999999998890 ) ) ;
#39630 = EDGE_CURVE ( 'NONE', #65123, #16063, #61145, .T. ) ;
#39631 = PLANE ( 'NONE',  #46032 ) ;
#39632 = CYLINDRICAL_SURFACE ( 'NONE', #42924, 2.000000000000001776 ) ;
#39633 = AXIS2_PLACEMENT_3D ( 'NONE', #73700, #10575, #31907 ) ;
#39634 = DIRECTION ( 'NONE',  ( 1.000000000000000000, 1.261617073437676668E-15, 9.462128050782575008E-16 ) ) ;
#39635 = DIRECTION ( 'NONE',  ( 0.000000000000000000, 0.000000000000000000, -1.000000000000000000 ) ) ;
#39636 = CARTESIAN_POINT ( 'NONE',  ( 98.68348088377346983, -30.50934295487596515, 180.8184824187679567 ) ) ;
#39637 = DIRECTION ( 'NONE',  ( 0.7071067811865165975, 0.7071067811865784369, 7.071067811865158803E-16 ) ) ;
#39638 = ORIENTED_EDGE ( 'NONE', *, *, #60749, .F. ) ;
#39640 = ORIENTED_EDGE ( 'NONE', *, *, #16299, .F. ) ;
#39639 = EDGE_CURVE ( 'NONE', #60931, #47557, #79014, .T. ) ;
#39641 = CARTESIAN_POINT ( 'NONE',  ( -93.48535127324140603, 69.93117631934791234, -91.13743891206647163 ) ) ;
#39642 = CARTESIAN_POINT ( 'NONE',  ( 77.80861903143292579, -17.15582774925911735, 2.518078172590604957 ) ) ;
#39643 = DIRECTION ( 'NONE',  ( -9.299908063537919123E-17, 0.000000000000000000, -1.000000000000000000 ) ) ;
#39644 = DIRECTION ( 'NONE',  ( 0.4999999999999998335, 0.8660254037844387076, -2.684678751731758400E-14 ) ) ;
#39645 = DIRECTION ( 'NONE',  ( -6.982966722218760189E-15, 0.000000000000000000, -1.000000000000000000 ) ) ;
#39646 = ORIENTED_EDGE ( 'NONE', *, *, #31428, .T. ) ;
#39647 = CARTESIAN_POINT ( 'NONE',  ( 152.5667039024470171, -23.42844715993586036, 249.9678068554149490 ) ) ;
#39648 = B_SPLINE_CURVE_WITH_KNOTS ( 'NONE', 3,
 ( #61278, #34014, #11804, #39502, #5889, #33578, #89001, #61715, #32683, #89453, #27211, #89912, #48975, #70801, #22209, #83988, #28547, #55780 ),
 .UNSPECIFIED., .F., .F.,
 ( 4, 2, 2, 2, 2, 2, 2, 2, 4 ),
 ( 0.08963260634764534662, 0.1409350762971974258, 0.1922375462467494911, 0.2435400161963015564, 0.2948424861458536217, 0.3461449560954056870, 0.3974474260449577523, 0.4487498959945098176, 0.5000523659440618829 ),
 .UNSPECIFIED. ) ;
#39649 = CARTESIAN_POINT ( 'NONE',  ( 101.4045521927434805, -45.52538047655821885, 222.1213395616249784 ) ) ;
#39650 = CARTESIAN_POINT ( 'NONE',  ( 134.4432975232679439, -39.47944369577152912, 8.225625303283962353 ) ) ;
#39651 = ORIENTED_EDGE ( 'NONE', *, *, #35404, .T. ) ;
#39652 = ORIENTED_EDGE ( 'NONE', *, *, #85613, .T. ) ;
#39653 = EDGE_CURVE ( 'NONE', #28842, #71659, #71565, .T. ) ;
#39654 = CARTESIAN_POINT ( 'NONE',  ( -2.860914336036568528, 94.82778141605180622, 118.5221612204686608 ) ) ;
#39656 = ADVANCED_FACE ( 'NONE', ( #2069 ), #29774, .T. ) ;
#39655 = DIRECTION ( 'NONE',  ( 4.299999999999999979E-14, -1.000000000000000000, 0.000000000000000000 ) ) ;
#39657 = CARTESIAN_POINT ( 'NONE',  ( 97.81167943543778165, -40.51737693692245301, 166.6360185166829808 ) ) ;
#39658 = EDGE_CURVE ( 'NONE', #77506, #51500, #31140, .T. ) ;
#39659 = CARTESIAN_POINT ( 'NONE',  ( 98.91757684337089529, -33.81461462136097396, 23.88332846482899186 ) ) ;
#39660 = CARTESIAN_POINT ( 'NONE',  ( 117.6028659061361736, -33.31333136338176359, 130.0880062282919880 ) ) ;
#39661 = DIRECTION ( 'NONE',  ( 0.000000000000000000, 1.000000000000000000, 0.000000000000000000 ) ) ;
#39662 = ORIENTED_EDGE ( 'NONE', *, *, #49263, .F. ) ;
#39663 = ADVANCED_FACE ( 'NONE', ( #35679 ), #64298, .F. ) ;
#39664 = CARTESIAN_POINT ( 'NONE',  ( 107.0664832912739968, -36.72944715994100306, 287.6356252759109680 ) ) ;
#39665 = LINE ( 'NONE', #67364, #32870 ) ;
#39666 = ORIENTED_EDGE ( 'NONE', *, *, #53114, .F. ) ;
#39667 = ORIENTED_EDGE ( 'NONE', *, *, #33326, .T. ) ;
#39668 = VECTOR ( 'NONE', #82076, 1000.000000000000000 ) ;
#39669 = DIRECTION ( 'NONE',  ( 1.000000000000000000, 0.000000000000000000, 0.000000000000000000 ) ) ;
#39670 = ORIENTED_EDGE ( 'NONE', *, *, #50811, .T. ) ;
#39671 = ORIENTED_EDGE ( 'NONE', *, *, #35202, .F. ) ;
#39672 = DIRECTION ( 'NONE',  ( -0.7071067811865849873, 0.7071067811865101582, 0.000000000000000000 ) ) ;
#39673 = VECTOR ( 'NONE', #65391, 1000.000000000000000 ) ;
#39674 = CARTESIAN_POINT ( 'NONE',  ( 98.78342310422263495, -33.06835657602663758, 55.40575316140994033 ) ) ;
#39675 = CARTESIAN_POINT ( 'NONE',  ( 107.2435442917537500, -47.21071675017731906, 212.5899109901969837 ) ) ;
#39676 = CARTESIAN_POINT ( 'NONE',  ( 102.6926969729869938, -27.29023857175969781, 180.4213395616249898 ) ) ;
#39678 = CARTESIAN_POINT ( 'NONE',  ( 96.85498737197835339, -38.89503640450122646, 27.49276813305395706 ) ) ;
#39677 = DIRECTION ( 'NONE',  ( -2.195856868753399715E-16, -1.000000000000000000, 0.000000000000000000 ) ) ;
#39679 = DIRECTION ( 'NONE',  ( 0.000000000000000000, 1.000000000000000000, 0.000000000000000000 ) ) ;
#39680 = DIRECTION ( 'NONE',  ( 0.000000000000000000, 0.000000000000000000, -1.000000000000000000 ) ) ;
#39681 = ORIENTED_EDGE ( 'NONE', *, *, #87736, .T. ) ;
#39682 = ORIENTED_EDGE ( 'NONE', *, *, #58592, .T. ) ;
#39683 = CARTESIAN_POINT ( 'NONE',  ( 163.1639762274590169, -34.03355364505800651, -5.074374724088000832 ) ) ;
#39685 = AXIS2_PLACEMENT_3D ( 'NONE', #10822, #17212, #32602 ) ;
#39684 = CARTESIAN_POINT ( 'NONE',  ( 96.09181007874647662, -35.06528625842698688, 221.1946728949589840 ) ) ;
#39686 = VERTEX_POINT ( 'NONE', #57464 ) ;
#39687 = CARTESIAN_POINT ( 'NONE',  ( 97.05801352979682406, -41.42088835504144839, 211.6632443235299945 ) ) ;
#39688 = CARTESIAN_POINT ( 'NONE',  ( 102.0670548988634891, -27.97049809344460769, 35.48979194811688842 ) ) ;
#39689 = VECTOR ( 'NONE', #72590, 999.9999999999998863 ) ;
#39690 = CARTESIAN_POINT ( 'NONE',  ( 98.38037815814482201, -41.69519609451472775, 22.73975804005023704 ) ) ;
#39691 = CARTESIAN_POINT ( 'NONE',  ( -479.3614999999999782, 6.038608028953039941, 90.48749999999999716 ) ) ;
#39693 = CARTESIAN_POINT ( 'NONE',  ( 125.0664851986225159, -56.72944715994101728, 14.67562527591098842 ) ) ;
#39692 = CARTESIAN_POINT ( 'NONE',  ( 107.9134447035117432, -28.68416811027461222, 277.6356252759110248 ) ) ;
#39694 = LINE ( 'NONE', #18815, #40920 ) ;
#39695 = CARTESIAN_POINT ( 'NONE',  ( 98.58946256649485917, -108.5954344580498514, -19.78219314458187839 ) ) ;
#39696 = CARTESIAN_POINT ( 'NONE',  ( 31.71315051185499811, -33.70561438052090608, 237.4678068554150059 ) ) ;
#39697 = CARTESIAN_POINT ( 'NONE',  ( 30.00000000000003553, 172.0000000000000000, 182.8826257785461280 ) ) ;
#39698 = DIRECTION ( 'NONE',  ( 1.000000000000000078E-15, -1.000000000000000000, 0.000000000000000000 ) ) ;
#39699 = DIRECTION ( 'NONE',  ( -1.000000000000000000, -2.756263715554006823E-15, 0.000000000000000000 ) ) ;
#39701 = ORIENTED_EDGE ( 'NONE', *, *, #50181, .F. ) ;
#39700 = DIRECTION ( 'NONE',  ( -1.000000000000000000, -8.163404592832032979E-16, 0.000000000000000000 ) ) ;
#39702 = DIRECTION ( 'NONE',  ( 1.000000000000000078E-15, -1.000000000000000083E-30, -1.000000000000000000 ) ) ;
#39703 = CARTESIAN_POINT ( 'NONE',  ( 112.2159804458396479, -45.81949903116512246, 212.9870538473389558 ) ) ;
#39704 = CARTESIAN_POINT ( 'NONE',  ( 96.02365317015762969, -37.20890873343472549, 112.3489586092449599 ) ) ;
#39705 = CARTESIAN_POINT ( 'NONE',  ( 114.6369858128092858, -29.49892357452570124, 230.4327681330539690 ) ) ;
#39706 = LINE ( 'NONE', #17930, #10589 ) ;
#39707 = PLANE ( 'NONE',  #69246 ) ;
#39709 = CARTESIAN_POINT ( 'NONE',  ( 97.81169418859235520, -40.51741816698509524, 47.63568902202231925 ) ) ;
#39708 = CARTESIAN_POINT ( 'NONE',  ( 165.2725846195380086, -35.55794170701810941, -5.074374724088000832 ) ) ;
#39710 = CARTESIAN_POINT ( 'NONE',  ( 93.79911539042399227, -35.59159216677125670, 299.5571190294419921 ) ) ;
#39711 = AXIS2_PLACEMENT_3D ( 'NONE', #29296, #19894, #61219 ) ;
#39712 = DIRECTION ( 'NONE',  ( 1.000000000000000000, 0.000000000000000000, 3.062684205862500216E-15 ) ) ;
#39713 = ORIENTED_EDGE ( 'NONE', *, *, #15688, .F. ) ;
#39714 = EDGE_CURVE ( 'NONE', #6819, #40280, #87685, .T. ) ;
#39715 = ORIENTED_EDGE ( 'NONE', *, *, #47910, .F. ) ;
#39716 = CARTESIAN_POINT ( 'NONE',  ( 115.2241057928380599, -39.35723584706951783, 158.0009912566479500 ) ) ;
#39717 = EDGE_CURVE ( 'NONE', #14045, #54558, #26788, .T. ) ;
#39719 = ORIENTED_EDGE ( 'NONE', *, *, #24060, .T. ) ;
#39718 = CARTESIAN_POINT ( 'NONE',  ( 2.036081061455522238E-14, 184.0000000000000000, 80.02307622376218887 ) ) ;
#39720 = CARTESIAN_POINT ( 'NONE',  ( 180.3164832912730162, 12.92155284005730387, 355.9756252759109998 ) ) ;
#39721 = CARTESIAN_POINT ( 'NONE',  ( 102.3226935662337524, -26.77152163616663927, 136.4422919425779526 ) ) ;
#39722 = LINE ( 'NONE', #53783, #7684 ) ;
#39723 = DIRECTION ( 'NONE',  ( 1.000000000000000000, 0.000000000000000000, 0.000000000000000000 ) ) ;
#39724 = ADVANCED_FACE ( 'NONE', ( #51090, #49746 ), #15253, .F. ) ;
#39725 = EDGE_CURVE ( 'NONE', #59751, #9320, #49299, .T. ) ;
#39726 = CARTESIAN_POINT ( 'NONE',  ( -75.37281393334444601, 76.91656954603718077, 91.51265874544296253 ) ) ;
#39727 = CARTESIAN_POINT ( 'NONE',  ( 98.30753419510237734, -41.72887549885788872, 107.7397919432831799 ) ) ;
#39728 = CARTESIAN_POINT ( 'NONE',  ( 97.54819157151548836, -32.61351373332768588, 61.01372051400699803 ) ) ;
#39729 = ORIENTED_EDGE ( 'NONE', *, *, #58306, .T. ) ;
#39730 = EDGE_LOOP ( 'NONE', ( #236, #32918, #76068, #74713, #15351, #53603, #49718, #53015, #27321, #87507, #46895, #42884 ) ) ;
#39731 = ORIENTED_EDGE ( 'NONE', *, *, #22843, .T. ) ;
#39732 = ADVANCED_FACE ( 'NONE', ( #14359 ), #69764, .T. ) ;
#39733 = VECTOR ( 'NONE', #57017, 1000.000000000000000 ) ;
#39734 = CARTESIAN_POINT ( 'NONE',  ( 44.45000000000000284, 66.67499999999999716, 292.1000000000000227 ) ) ;
#39736 = FACE_BOUND ( 'NONE', #45000, .T. ) ;
#39735 = CARTESIAN_POINT ( 'NONE',  ( 101.2684584845352163, -45.32493232151062301, 148.0918157521009562 ) ) ;
#39737 = CIRCLE ( 'NONE', #16544, 37.00000000000000711 ) ;
#39738 = FACE_OUTER_BOUND ( 'NONE', #2788, .T. ) ;
#39739 = EDGE_CURVE ( 'NONE', #25266, #51283, #56101, .T. ) ;
#39740 = CARTESIAN_POINT ( 'NONE',  ( 12.70000000000000107, 82.54999999999999716, -129.9368274816650910 ) ) ;
#39741 = LINE ( 'NONE', #54241, #60504 ) ;
#39742 = LINE ( 'NONE', #74727, #68067 ) ;
#39743 = CARTESIAN_POINT ( 'NONE',  ( 72.26648329127297643, -71.52944715994142655, 342.9256252759110453 ) ) ;
#39744 = CARTESIAN_POINT ( 'NONE',  ( 112.5028774994482035, -27.85959465031275784, 94.63848241876793566 ) ) ;
#39745 = ORIENTED_EDGE ( 'NONE', *, *, #48437, .F. ) ;
#39747 = ORIENTED_EDGE ( 'NONE', *, *, #89616, .F. ) ;
#39746 = EDGE_CURVE ( 'NONE', #84162, #5960, #9374, .T. ) ;
#39748 = FACE_BOUND ( 'NONE', #48502, .T. ) ;
#39749 = CARTESIAN_POINT ( 'NONE',  ( -95.16508291382886853, 94.58014758961630264, -89.37916159652625936 ) ) ;
#39750 = DIRECTION ( 'NONE',  ( 1.000000000000000000, 0.000000000000000000, 0.000000000000000000 ) ) ;
#39751 = CARTESIAN_POINT ( 'NONE',  ( 103.1635642379172850, -29.56027560196853088, 143.2909475124489518 ) ) ;
#39752 = AXIS2_PLACEMENT_3D ( 'NONE', #8044, #28944, #55267 ) ;
#39753 = AXIS2_PLACEMENT_3D ( 'NONE', #61385, #75483, #19454 ) ;
#39754 = VECTOR ( 'NONE', #82172, 1000.000000000000000 ) ;
#39755 = DIRECTION ( 'NONE',  ( -0.7071067811734105257, 0.7071067811996846197, 0.000000000000000000 ) ) ;
#39756 = ORIENTED_EDGE ( 'NONE', *, *, #37152, .F. ) ;
#39757 = VERTEX_POINT ( 'NONE', #23424 ) ;
#39758 = CARTESIAN_POINT ( 'NONE',  ( 31.78666935232860169, -29.62846900982351528, 193.9678068554150911 ) ) ;
#39759 = ORIENTED_EDGE ( 'NONE', *, *, #78100, .T. ) ;
#39760 = ORIENTED_EDGE ( 'NONE', *, *, #19731, .F. ) ;
#39761 = CARTESIAN_POINT ( 'NONE',  ( -454.6936515812919879, 53.97500000000000142, 3.174999999999999822 ) ) ;
#39762 = EDGE_CURVE ( 'NONE', #63148, #11683, #33983, .T. ) ;
#39763 = CARTESIAN_POINT ( 'NONE',  ( 98.23266987703472353, -35.71659467859123538, 202.6672975916109465 ) ) ;
#39764 = CARTESIAN_POINT ( 'NONE',  ( 107.0664832912739541, -36.72944715994095333, 308.7195067599733420 ) ) ;
#39765 = ADVANCED_FACE ( 'NONE', ( #28878 ), #56567, .F. ) ;
#39766 = CYLINDRICAL_SURFACE ( 'NONE', #31300, 0.5000000000000079936 ) ;
#39767 = CARTESIAN_POINT ( 'NONE',  ( 107.0664832912739399, -36.72944715994096754, 300.2406250056037038 ) ) ;
#39768 = ORIENTED_EDGE ( 'NONE', *, *, #11458, .F. ) ;
#39769 = ORIENTED_EDGE ( 'NONE', *, *, #52457, .F. ) ;
#39770 = ORIENTED_EDGE ( 'NONE', *, *, #74811, .T. ) ;
#39771 = ORIENTED_EDGE ( 'NONE', *, *, #37374, .T. ) ;
#39772 = CARTESIAN_POINT ( 'NONE',  ( 104.6179474607139213, -28.94263790944830106, 248.1366617981629474 ) ) ;
#39773 = CARTESIAN_POINT ( 'NONE',  ( 112.8139912305532704, -47.12176010715679553, 102.9784824187679817 ) ) ;
#39774 = CARTESIAN_POINT ( 'NONE',  ( 110.7866772467784955, -46.44483816919306918, 62.86705384733992474 ) ) ;
#39775 = CARTESIAN_POINT ( 'NONE',  ( 99.75758940074024395, -33.13488748790386751, 249.5838068554174072 ) ) ;
#39776 = CARTESIAN_POINT ( 'NONE',  ( 134.0664832912739826, -15.97944715994100306, 8.225625275910998013 ) ) ;
#39777 = DIRECTION ( 'NONE',  ( -3.100000000000000258E-29, 3.100000000000000044E-14, 1.000000000000000000 ) ) ;
#39778 = CARTESIAN_POINT ( 'NONE',  ( 98.53766203808953605, -30.73430783891158669, 201.8384824187679385 ) ) ;
#39779 = CARTESIAN_POINT ( 'NONE',  ( 237.9979999999999905, 52.73749999999999716, 10.66800000000000104 ) ) ;
#39780 = VERTEX_POINT ( 'NONE', #36135 ) ;
#39781 = CARTESIAN_POINT ( 'NONE',  ( 61.67079006425790766, -0.9306969701470987344, 542.9756252759101471 ) ) ;
#39782 = ORIENTED_EDGE ( 'NONE', *, *, #75235, .F. ) ;
#39783 = ORIENTED_EDGE ( 'NONE', *, *, #2132, .F. ) ;
#39784 = DIRECTION ( 'NONE',  ( 0.7071067811874278686, -0.7071067811856670549, 6.612322855868390075E-17 ) ) ;
#39785 = VERTEX_POINT ( 'NONE', #77032 ) ;
#39786 = DIRECTION ( 'NONE',  ( -1.000000000000000000, 0.000000000000000000, 0.000000000000000000 ) ) ;
#39787 = CARTESIAN_POINT ( 'NONE',  ( 113.1782937589909181, -44.75186860218948937, 178.0939586081543666 ) ) ;
#39788 = CARTESIAN_POINT ( 'NONE',  ( 109.6839073351967642, -47.46854297047285343, 87.75467289495897205 ) ) ;
#39789 = CARTESIAN_POINT ( 'NONE',  ( 113.2492940411024449, -28.76157773499452119, 254.5522619721145645 ) ) ;
#39790 = AXIS2_PLACEMENT_3D ( 'NONE', #8099, #36707, #29893 ) ;
#39791 = CARTESIAN_POINT ( 'NONE',  ( -492.0614999999999668, 14.28750000000026077, 6.349999999999710099 ) ) ;
#39792 = DIRECTION ( 'NONE',  ( 6.938893903907227392E-16, 0.000000000000000000, -1.000000000000000000 ) ) ;
#39795 = CARTESIAN_POINT ( 'NONE',  ( 98.27975524859429868, -42.29919363830185119, 182.7756252759109543 ) ) ;
#39794 = CARTESIAN_POINT ( 'NONE',  ( 126.0667039024479266, -14.72944715994094977, 239.5838068554170377 ) ) ;
#39793 = DIRECTION ( 'NONE',  ( 0.000000000000000000, -1.000000000000000000, 0.000000000000000000 ) ) ;
#39796 = DIRECTION ( 'NONE',  ( 8.673617379884035472E-16, 1.000000000000000000, 0.000000000000000000 ) ) ;
#39797 = CARTESIAN_POINT ( 'NONE',  ( 123.6837132603319560, -53.34645651782485487, 219.5838068554170093 ) ) ;
#39798 = ORIENTED_EDGE ( 'NONE', *, *, #68772, .F. ) ;
#39799 = CARTESIAN_POINT ( 'NONE',  ( 34.96670390244699433, -26.71338133339301635, -5.074374724088000832 ) ) ;
#39800 = DIRECTION ( 'NONE',  ( 1.000000000000000078E-15, -1.000000000000000000, 0.000000000000000000 ) ) ;
#39801 = CARTESIAN_POINT ( 'NONE',  ( 97.12563366290001454, -37.99751694395044410, 136.4276054474069326 ) ) ;
#39802 = DIRECTION ( 'NONE',  ( 0.000000000000000000, 0.000000000000000000, 1.000000000000000000 ) ) ;
#39804 = EDGE_LOOP ( 'NONE', ( #86618, #33401 ) ) ;
#39803 = CARTESIAN_POINT ( 'NONE',  ( 113.8278214188052999, -26.93592357317604424, 239.5956252759109759 ) ) ;
#39805 = DIRECTION ( 'NONE',  ( -1.000000000000000078E-15, 1.000000000000000000, 0.000000000000000000 ) ) ;
#39806 = CARTESIAN_POINT ( 'NONE',  ( 105.8911342260945645, -47.14568079332288875, 278.4870538473395527 ) ) ;
#39807 = CARTESIAN_POINT ( 'NONE',  ( 112.1411864721344642, -47.49320580990715968, 133.9270538473399768 ) ) ;
#39808 = CARTESIAN_POINT ( 'NONE',  ( 186.6899999999999977, 59.08750000000000568, -38.10000000000000142 ) ) ;
#39809 = CARTESIAN_POINT ( 'NONE',  ( 1.663881452865401345, 95.14749909259209915, -130.5460625349953148 ) ) ;
#39810 = ADVANCED_FACE ( 'NONE', ( #36596 ), #19530, .T. ) ;
#39812 = CARTESIAN_POINT ( 'NONE',  ( 188.5667039024479834, -48.82844715994099971, 257.2178068554150059 ) ) ;
#39811 = CARTESIAN_POINT ( 'NONE',  ( 38.10000000000000142, 69.84999999999999432, 358.0130000000000337 ) ) ;
#39813 = CARTESIAN_POINT ( 'NONE',  ( 107.0664832912739968, -36.72944715994100306, 249.5838068554170093 ) ) ;
#39814 = DIRECTION ( 'NONE',  ( 4.299999999999999979E-14, -1.000000000000000000, 4.400000000000000367E-29 ) ) ;
#39815 = EDGE_LOOP ( 'NONE', ( #29372, #11321 ) ) ;
#39816 = CIRCLE ( 'NONE', #54327, 9.525000000000000355 ) ;
#39817 = AXIS2_PLACEMENT_3D ( 'NONE', #19512, #33590, #61725 ) ;
#39818 = AXIS2_PLACEMENT_3D ( 'NONE', #74671, #33336, #19705 ) ;
#39819 = EDGE_CURVE ( 'NONE', #37855, #80877, #62931, .T. ) ;
#39820 = VERTEX_POINT ( 'NONE', #83849 ) ;
#39821 = EDGE_CURVE ( 'NONE', #40115, #60827, #77575, .T. ) ;
#39822 = VERTEX_POINT ( 'NONE', #45590 ) ;
#39823 = CIRCLE ( 'NONE', #26791, 2.749999999999974687 ) ;
#39825 = EDGE_CURVE ( 'NONE', #84501, #55506, #32421, .T. ) ;
#39824 = VECTOR ( 'NONE', #57274, 1000.000000000000000 ) ;
#39826 = ORIENTED_EDGE ( 'NONE', *, *, #75022, .F. ) ;
#39827 = DIRECTION ( 'NONE',  ( 0.000000000000000000, -1.000000000000000000, 0.000000000000000000 ) ) ;
#39828 = CARTESIAN_POINT ( 'NONE',  ( 107.1951288810177090, -26.32694189238808491, 31.06705384733893283 ) ) ;
#39829 = DIRECTION ( 'NONE',  ( 0.000000000000000000, 0.000000000000000000, 1.000000000000000000 ) ) ;
#39830 = CARTESIAN_POINT ( 'NONE',  ( 145.3595637443018234, -69.45303146431501773, 247.4784022495120155 ) ) ;
#39831 = CARTESIAN_POINT ( 'NONE',  ( 144.1872411114284773, -138.0587426716868151, 247.6570821702239869 ) ) ;
#39832 = EDGE_CURVE ( 'NONE', #69459, #37218, #57200, .T. ) ;
#39834 = CARTESIAN_POINT ( 'NONE',  ( 49.65699999999999648, 82.54999999999999716, 358.0130000000000337 ) ) ;
#39833 = CARTESIAN_POINT ( 'NONE',  ( 59.67078992371374113, -0.9290567490904538817, 396.9756252759102040 ) ) ;
#39835 = CARTESIAN_POINT ( 'NONE',  ( 112.5827476457113079, -28.73936235024410024, 239.0181341137909783 ) ) ;
#39836 = EDGE_LOOP ( 'NONE', ( #65935, #28257, #40571, #48982 ) ) ;
#39837 = ORIENTED_EDGE ( 'NONE', *, *, #25076, .T. ) ;
#39838 = ORIENTED_EDGE ( 'NONE', *, *, #81919, .F. ) ;
#39839 = EDGE_CURVE ( 'NONE', #37337, #74190, #35981, .T. ) ;
#39840 = PLANE ( 'NONE',  #2112 ) ;
#39841 = DIRECTION ( 'NONE',  ( 1.000000000000000000, 0.000000000000000000, 0.000000000000000000 ) ) ;
#39842 = DIRECTION ( 'NONE',  ( 0.000000000000000000, 0.000000000000000000, 1.000000000000000000 ) ) ;
#39843 = VECTOR ( 'NONE', #22512, 1000.000000000000000 ) ;
#39844 = CARTESIAN_POINT ( 'NONE',  ( 98.34910283431410960, -31.65794092288606976, 275.9061490951863789 ) ) ;
#39845 = CARTESIAN_POINT ( 'NONE',  ( 110.5196960824274868, -45.46740155661881033, 19.31967854399191253 ) ) ;
#39846 = EDGE_CURVE ( 'NONE', #51283, #23552, #76077, .T. ) ;
#39847 = CARTESIAN_POINT ( 'NONE',  ( 117.8738102209309204, 83.38952084682853183, -12.69999999999877005 ) ) ;
#39848 = DIRECTION ( 'NONE',  ( 0.02150753337724187197, 0.0009076677972194977960, 0.9997682742251811083 ) ) ;
#39849 = CARTESIAN_POINT ( 'NONE',  ( 111.5675350091857325, -45.45035926415926752, 272.9556252759110180 ) ) ;
#39850 = CYLINDRICAL_SURFACE ( 'NONE', #84990, 3.249999999999975131 ) ;
#39852 = ORIENTED_EDGE ( 'NONE', *, *, #87544, .T. ) ;
#39851 = EDGE_CURVE ( 'NONE', #36809, #35978, #17911, .T. ) ;
#39853 = CARTESIAN_POINT ( 'NONE',  ( 182.3467384525654893, -29.62846900981658393, 313.9678068554149490 ) ) ;
#39854 = FACE_OUTER_BOUND ( 'NONE', #85201, .T. ) ;
#39855 = CARTESIAN_POINT ( 'NONE',  ( 113.8053744393198485, -42.15975756917345763, 41.09285227435299959 ) ) ;
#39856 = CIRCLE ( 'NONE', #16662, 11.45913725231036118 ) ;
#39857 = CARTESIAN_POINT ( 'NONE',  ( 136.7302760451841266, -18.02416100036293400, 6.874390491351639376 ) ) ;
#39858 = AXIS2_PLACEMENT_3D ( 'NONE', #5760, #7098, #278 ) ;
#39859 = CARTESIAN_POINT ( 'NONE',  ( 163.0822201311030142, 20.32000000000000028, -75.92468371870729982 ) ) ;
#39860 = CARTESIAN_POINT ( 'NONE',  ( 71.24025061656124080, 8.642044024269639024, 542.9756252759101471 ) ) ;
#39861 = VERTEX_POINT ( 'NONE', #24298 ) ;
#39862 = DIRECTION ( 'NONE',  ( 0.7071067811861728725, -0.7071067811869222730, 0.000000000000000000 ) ) ;
#39863 = CARTESIAN_POINT ( 'NONE',  ( 121.9913672821676869, 60.41918071833632098, -46.51076114057810429 ) ) ;
#39864 = ORIENTED_EDGE ( 'NONE', *, *, #2652, .F. ) ;
#39865 = CARTESIAN_POINT ( 'NONE',  ( 113.0770494671172628, -28.21122406429266150, 129.5870538473399449 ) ) ;
#39866 = ORIENTED_EDGE ( 'NONE', *, *, #50617, .F. ) ;
#39867 = CARTESIAN_POINT ( 'NONE',  ( 113.7032067727884197, -42.10625226631949403, 87.70670554236198768 ) ) ;
#39868 = CARTESIAN_POINT ( 'NONE',  ( 167.7413838386819123, -48.33240602328260849, 180.4678068554150059 ) ) ;
#39869 = CARTESIAN_POINT ( 'NONE',  ( 102.3355707743008765, -29.23633396390525618, 106.9558690201829734 ) ) ;
#39870 = CARTESIAN_POINT ( 'NONE',  ( 34.33598329127390514, -36.32844715994140472, 117.4678068554150485 ) ) ;
#39871 = EDGE_CURVE ( 'NONE', #56606, #23728, #2957, .T. ) ;
#39872 = FACE_OUTER_BOUND ( 'NONE', #13142, .T. ) ;
#39873 = CARTESIAN_POINT ( 'NONE',  ( 113.5195425369480233, -28.51389573442233427, 75.54705384733995288 ) ) ;
#39874 = FACE_OUTER_BOUND ( 'NONE', #25934, .T. ) ;
#39875 = CARTESIAN_POINT ( 'NONE',  ( 0.000000000000000000, 44.45000000000000284, 0.000000000000000000 ) ) ;
#39876 = VECTOR ( 'NONE', #20543, 1000.000000000000000 ) ;
#39877 = ORIENTED_EDGE ( 'NONE', *, *, #52302, .F. ) ;
#39878 = CARTESIAN_POINT ( 'NONE',  ( 188.5667039024479834, -62.87844715994099687, 139.9678068554150059 ) ) ;
#39879 = VECTOR ( 'NONE', #23017, 999.9999999999998863 ) ;
#39880 = CIRCLE ( 'NONE', #12347, 2.500000000000002220 ) ;
#39881 = ORIENTED_EDGE ( 'NONE', *, *, #11437, .F. ) ;
#39882 = ORIENTED_EDGE ( 'NONE', *, *, #43674, .F. ) ;
#39883 = VECTOR ( 'NONE', #18944, 1000.000000000000000 ) ;
#39884 = VECTOR ( 'NONE', #9826, 1000.000000000000114 ) ;
#39885 = DIRECTION ( 'NONE',  ( 0.000000000000000000, 0.000000000000000000, 1.000000000000000000 ) ) ;
#39886 = ORIENTED_EDGE ( 'NONE', *, *, #60978, .T. ) ;
#39887 = CARTESIAN_POINT ( 'NONE',  ( 113.3831382903590992, -27.58002901871518020, 239.5956252759109759 ) ) ;
#39888 = CARTESIAN_POINT ( 'NONE',  ( 117.7011894673193382, -39.82593390098057284, 134.5889586092439743 ) ) ;
#39889 = B_SPLINE_CURVE_WITH_KNOTS ( 'NONE', 3,
 ( #50748, #22171, #83950, #35771, #23077, #78483, #16245, #43920, #21720, #50287, #85747, #63482, #49392, #48932, #1270, #28974, #56660, #77565, #15352, #43021, #8534, #36231, #63942, #57100, #15799, #71214, #60223, #11658, #3938 ),
 .UNSPECIFIED., .F., .F.,
 ( 4, 2, 2, 2, 2, 2, 2, 2, 2, 2, 1, 1, 1, 1, 1, 2, 4 ),
 ( 0.000000000000000000, 0.06249314710935460759, 0.1249862942187092152, 0.1874794413280638228, 0.2499725884374184304, 0.3124657355467730380, 0.3749588826561276456, 0.4374520297654822532, 0.4686986033201598345, 0.4843218900974986529, 0.4921335334861677846, 0.4960393551805025170, 0.4979922660276701052, 0.4989687214512539271, 0.4994569491630460045, 0.4997010630189421820, 0.4999451768748383040 ),
 .UNSPECIFIED. ) ;
#39890 = CARTESIAN_POINT ( 'NONE',  ( 103.5243996547270626, -27.35269840695457688, 125.3628851967883975 ) ) ;
#39891 = CARTESIAN_POINT ( 'NONE',  ( -469.3583484187089994, 53.97500000000000142, 3.174999999999999822 ) ) ;
#39892 = CARTESIAN_POINT ( 'NONE',  ( 108.5379568639253449, -26.40872756427751611, 100.9641967044829727 ) ) ;
#39893 = DIRECTION ( 'NONE',  ( 0.000000000000000000, -1.000000000000000000, 0.000000000000000000 ) ) ;
#39894 = ORIENTED_EDGE ( 'NONE', *, *, #56888, .F. ) ;
#39895 = DIRECTION ( 'NONE',  ( 1.000000000000000078E-15, -1.000000000000000083E-30, -1.000000000000000000 ) ) ;
#39896 = EDGE_CURVE ( 'NONE', #41501, #64928, #36919, .T. ) ;
#39897 = CARTESIAN_POINT ( 'NONE',  ( 131.3164832912739826, -18.72944715994100662, 14.92562527591099553 ) ) ;
#39898 = AXIS2_PLACEMENT_3D ( 'NONE', #17834, #58276, #72366 ) ;
#39899 = ORIENTED_EDGE ( 'NONE', *, *, #12175, .T. ) ;
#39900 = EDGE_CURVE ( 'NONE', #7066, #58062, #89186, .T. ) ;
#39901 = DIRECTION ( 'NONE',  ( 0.000000000000000000, 0.000000000000000000, 1.000000000000000000 ) ) ;
#39902 = DIRECTION ( 'NONE',  ( -1.000000000000000000, 0.000000000000000000, 0.000000000000000000 ) ) ;
#39903 = CARTESIAN_POINT ( 'NONE',  ( 100.4652087429556815, -44.82591848225601439, 12.03276813305398463 ) ) ;
#39904 = DIRECTION ( 'NONE',  ( 4.299999999999999979E-14, -1.000000000000000000, 4.400000000000000367E-29 ) ) ;
#39905 = CARTESIAN_POINT ( 'NONE',  ( 152.0371591254582881, -47.82818131005588214, 300.4678068554149490 ) ) ;
#39906 = CARTESIAN_POINT ( 'NONE',  ( 77.58678459498953828, -37.92005462650905656, 2.747931806396151977 ) ) ;
#39907 = CARTESIAN_POINT ( 'NONE',  ( 106.3786087989843736, -45.75936958534449417, 266.9505150661723860 ) ) ;
#39909 = CARTESIAN_POINT ( 'NONE',  ( 118.8180844208008722, -35.40729807334668777, 79.91562527591095488 ) ) ;
#39908 = CARTESIAN_POINT ( 'NONE',  ( 80.06648329127398256, -9.029447159941060619, 4.925625275910944012 ) ) ;
#39910 = CARTESIAN_POINT ( 'NONE',  ( 163.2569089553709603, -33.54226604284439617, 117.4678068554150485 ) ) ;
#39911 = CARTESIAN_POINT ( 'NONE',  ( 109.8678013061348508, -26.64186650728397865, 174.8613395616249591 ) ) ;
#39912 = ORIENTED_EDGE ( 'NONE', *, *, #22510, .F. ) ;
#39913 = DIRECTION ( 'NONE',  ( -1.000000000000000000, 0.000000000000000000, 0.000000000000000000 ) ) ;
#39914 = EDGE_LOOP ( 'NONE', ( #10858, #48543, #3555, #11375 ) ) ;
#39915 = DIRECTION ( 'NONE',  ( -1.000000000000000078E-15, 0.000000000000000000, 1.000000000000000000 ) ) ;
#39916 = CARTESIAN_POINT ( 'NONE',  ( 32.15435173583698969, -31.62489322948785997, 342.9256252759109884 ) ) ;
#39917 = DIRECTION ( 'NONE',  ( 0.000000000000000000, 0.000000000000000000, -1.000000000000000000 ) ) ;
#39918 = VERTEX_POINT ( 'NONE', #3402 ) ;
#39919 = CARTESIAN_POINT ( 'NONE',  ( 140.9629299006807059, -46.47944715994099596, 14.92562527591100618 ) ) ;
#39921 = ORIENTED_EDGE ( 'NONE', *, *, #58303, .T. ) ;
#39920 = CARTESIAN_POINT ( 'NONE',  ( 117.6526747975261458, -33.39096950974673916, 129.0575300378159795 ) ) ;
#39923 = DIRECTION ( 'NONE',  ( 0.000000000000000000, 1.000000000000000000, 0.000000000000000000 ) ) ;
#39922 = UNCERTAINTY_MEASURE_WITH_UNIT (LENGTH_MEASURE( 1.000000000000000082E-05 ), #70093, 'distance_accuracy_value', 'NONE');
#39924 = CARTESIAN_POINT ( 'NONE',  ( -130.4942851453020296, 94.60320878023492241, -4.086962795941524007 ) ) ;
#39925 = LINE ( 'NONE', #2407, #70686 ) ;
#39926 = AXIS2_PLACEMENT_3D ( 'NONE', #59997, #53168, #38234 ) ;
#39927 = CYLINDRICAL_SURFACE ( 'NONE', #53954, 0.5000000000000031086 ) ;
#39928 = EDGE_LOOP ( 'NONE', ( #77539, #82588, #39747, #352 ) ) ;
#39929 = DIRECTION ( 'NONE',  ( -1.000000000000000000, 0.000000000000000000, -6.982962677686266711E-15 ) ) ;
#39930 = VECTOR ( 'NONE', #61933, 1000.000000000000000 ) ;
#39931 = DIRECTION ( 'NONE',  ( 0.000000000000000000, 1.000000000000000000, 0.000000000000000000 ) ) ;
#39932 = DIRECTION ( 'NONE',  ( -0.7071067811864666375, -0.7071067811866283970, -7.071067811864659848E-16 ) ) ;
#39933 = ORIENTED_EDGE ( 'NONE', *, *, #6124, .F. ) ;
#39934 = ADVANCED_FACE ( 'NONE', ( #86532 ), #58786, .T. ) ;
#39935 = ADVANCED_FACE ( 'NONE', ( #86972 ), #46042, .F. ) ;
#39936 = ORIENTED_EDGE ( 'NONE', *, *, #15960, .T. ) ;
#39937 = DIRECTION ( 'NONE',  ( 0.000000000000000000, 0.000000000000000000, 1.000000000000000000 ) ) ;
#39938 = CARTESIAN_POINT ( 'NONE',  ( 82.89895571708365196, 82.54999999999999716, -100.8594679592203818 ) ) ;
#39939 = DIRECTION ( 'NONE',  ( 0.5000000000000008882, -0.8660254037844382635, 2.684678751731760294E-14 ) ) ;
#39940 = CARTESIAN_POINT ( 'NONE',  ( 20.03715912545735378, -24.42818131006189830, 249.9678068554150059 ) ) ;
#39941 = EDGE_CURVE ( 'NONE', #42715, #22615, #61609, .T. ) ;
#39943 = DIRECTION ( 'NONE',  ( 0.000000000000000000, 0.000000000000000000, 1.000000000000000000 ) ) ;
#39942 = DIRECTION ( 'NONE',  ( -0.5000000000000003331, 0.8660254037844383745, 0.000000000000000000 ) ) ;
#39944 = PLANE ( 'NONE',  #61105 ) ;
#39945 = AXIS2_PLACEMENT_3D ( 'NONE', #40415, #89472, #54910 ) ;
#39946 = EDGE_LOOP ( 'NONE', ( #50616, #50068 ) ) ;
#39947 = AXIS2_PLACEMENT_3D ( 'NONE', #31023, #51450, #87780 ) ;
#39948 = VECTOR ( 'NONE', #62422, 1000.000000000000114 ) ;
#39949 = VECTOR ( 'NONE', #19421, 1000.000000000000000 ) ;
#39950 = DIRECTION ( 'NONE',  ( 0.000000000000000000, 0.000000000000000000, 1.000000000000000000 ) ) ;
#39951 = CARTESIAN_POINT ( 'NONE',  ( 103.9298229712114363, -26.84510867568836545, 201.3089586092439731 ) ) ;
#39952 = EDGE_CURVE ( 'NONE', #19365, #67921, #6092, .T. ) ;
#39954 = EDGE_LOOP ( 'NONE', ( #47708, #49563, #74539, #10640 ) ) ;
#39953 = CARTESIAN_POINT ( 'NONE',  ( 0.000000000000000000, 127.0000000000000000, 106.1020876358972629 ) ) ;
#39955 = AXIS2_PLACEMENT_3D ( 'NONE', #38266, #2871, #31443 ) ;
#39956 = CARTESIAN_POINT ( 'NONE',  ( 112.5987260342904648, -28.66361022110277545, 40.59848241876795782 ) ) ;
#39957 = CARTESIAN_POINT ( 'NONE',  ( 165.2748236753148205, -30.08671355699731009, 117.4678068554150485 ) ) ;
#39958 = DIRECTION ( 'NONE',  ( -0.000000000000000000, 1.000000000000000000, -0.000000000000000000 ) ) ;
#39959 = AXIS2_PLACEMENT_3D ( 'NONE', #8882, #1615, #8424 ) ;
#39960 = CARTESIAN_POINT ( 'NONE',  ( 1.387778780781445676E-14, 239.0000000000000000, 90.27542076772557778 ) ) ;
#39961 = VERTEX_POINT ( 'NONE', #46494 ) ;
#39962 = DIRECTION ( 'NONE',  ( 1.000000000000000000, 0.000000000000000000, 0.000000000000000000 ) ) ;
#39963 = ORIENTED_EDGE ( 'NONE', *, *, #59032, .F. ) ;
#39964 = EDGE_LOOP ( 'NONE', ( #63915, #7357, #28359, #62462 ) ) ;
#39965 = CIRCLE ( 'NONE', #47217, 0.5000000000000016653 ) ;
#39966 = CARTESIAN_POINT ( 'NONE',  ( 116.4035850909244090, -35.68299815489336879, 230.3349166392299594 ) ) ;
#39967 = APPLICATION_CONTEXT ( 'automotive_design' ) ;
#39968 = CARTESIAN_POINT ( 'NONE',  ( 32.16397622746000451, -34.03355364505800651, -5.074374724088000832 ) ) ;
#39969 = FACE_OUTER_BOUND ( 'NONE', #33825, .T. ) ;
#39970 = VECTOR ( 'NONE', #16836, 1000.000000000000114 ) ;
#39971 = CARTESIAN_POINT ( 'NONE',  ( 179.4595971212906704, -28.98061976758350511, 237.4678068554150059 ) ) ;
#39972 = CARTESIAN_POINT ( 'NONE',  ( 82.61444500289060500, -37.76411817599981902, 2.828498113172249084 ) ) ;
#39973 = ORIENTED_EDGE ( 'NONE', *, *, #22203, .F. ) ;
#39974 = DIRECTION ( 'NONE',  ( 1.000000000000000000, 0.000000000000000000, 0.000000000000000000 ) ) ;
#39975 = CARTESIAN_POINT ( 'NONE',  ( 70.30580606644517161, 91.40839032569790845, -53.86233103605738393 ) ) ;
#39976 = ORIENTED_EDGE ( 'NONE', *, *, #20860, .T. ) ;
#39977 = CARTESIAN_POINT ( 'NONE',  ( 97.23737678141878860, -33.32131919061083636, 286.0613395616252888 ) ) ;
#39978 = VERTEX_POINT ( 'NONE', #81065 ) ;
#39979 = AXIS2_PLACEMENT_3D ( 'NONE', #87047, #80235, #11168 ) ;
#39980 = ORIENTED_EDGE ( 'NONE', *, *, #56428, .F. ) ;
#39981 = CARTESIAN_POINT ( 'NONE',  ( 115.7114656938015429, -36.32299383444259888, 266.6699951314962505 ) ) ;
#39982 = DIRECTION ( 'NONE',  ( 0.000000000000000000, -1.000000000000000000, 0.000000000000000000 ) ) ;
#39983 = CARTESIAN_POINT ( 'NONE',  ( 102.6065612795739952, -27.36740250608067626, 140.4422919425779526 ) ) ;
#39984 = DIRECTION ( 'NONE',  ( 0.000000000000000000, 0.000000000000000000, 1.000000000000000000 ) ) ;
#39985 = CARTESIAN_POINT ( 'NONE',  ( 122.7090602494120049, -38.07100823150197755, 293.6356252759109680 ) ) ;
#39986 = CARTESIAN_POINT ( 'NONE',  ( 0.000000000000000000, 127.0000000000000000, -103.1875000000000000 ) ) ;
#39987 = EDGE_CURVE ( 'NONE', #69327, #59306, #5012, .T. ) ;
#39989 = CARTESIAN_POINT ( 'NONE',  ( 100.7971853062899896, -45.88878125878837011, 238.1108633711489517 ) ) ;
#39988 = CIRCLE ( 'NONE', #63212, 4.000000000000006217 ) ;
#39990 = DIRECTION ( 'NONE',  ( -1.000000000000000078E-15, 1.000000000000000083E-30, 1.000000000000000000 ) ) ;
#39991 = ORIENTED_EDGE ( 'NONE', *, *, #35099, .T. ) ;
#39992 = CARTESIAN_POINT ( 'NONE',  ( 116.1615364674122333, -29.05539214145830229, 70.38419670448192278 ) ) ;
#39993 = CARTESIAN_POINT ( 'NONE',  ( 25.56670390244828894, -48.82844715994168183, 293.2178068554150059 ) ) ;
#39994 = VECTOR ( 'NONE', #51603, 1000.000000000000114 ) ;
#39995 = EDGE_CURVE ( 'NONE', #12231, #56697, #88762, .T. ) ;
#39996 = ORIENTED_EDGE ( 'NONE', *, *, #29084, .T. ) ;
#39997 = EDGE_LOOP ( 'NONE', ( #45468, #36459, #78252, #74112 ) ) ;
#39998 = EDGE_LOOP ( 'NONE', ( #28694, #89177, #39560, #34320, #52138 ) ) ;
#39999 = CARTESIAN_POINT ( 'NONE',  ( 80.06648329127402519, -46.72944715994105991, 4.925625275910944012 ) ) ;
#40000 = DIRECTION ( 'NONE',  ( -1.000000000000000078E-15, 0.000000000000000000, 1.000000000000000000 ) ) ;
#40001 = CARTESIAN_POINT ( 'NONE',  ( 113.1760499632551529, -44.75354527206816613, 153.0944392216708536 ) ) ;
#40002 = CARTESIAN_POINT ( 'NONE',  ( 116.3457274436100164, -36.88499157630047165, 151.6309475124489552 ) ) ;
#40003 = CARTESIAN_POINT ( 'NONE',  ( 118.1046235831494755, -32.34975429571041161, 245.1270538473389706 ) ) ;
#40004 = DIRECTION ( 'NONE',  ( 4.299999999999999979E-14, -1.000000000000000000, 4.400000000000000367E-29 ) ) ;
#40005 = ORIENTED_EDGE ( 'NONE', *, *, #16860, .F. ) ;
#40006 = CARTESIAN_POINT ( 'NONE',  ( 130.0580535164677656, 88.17609398443094904, 11.39345613591001793 ) ) ;
#40007 = CARTESIAN_POINT ( 'NONE',  ( 136.7495928495827968, -37.33856210726968072, 3.004220725469414432 ) ) ;
#40008 = ORIENTED_EDGE ( 'NONE', *, *, #82573, .F. ) ;
#40009 = VERTEX_POINT ( 'NONE', #67856 ) ;
#40010 = EDGE_CURVE ( 'NONE', #16561, #76973, #47840, .T. ) ;
#40011 = VECTOR ( 'NONE', #68577, 1000.000000000000000 ) ;
#40012 = DIRECTION ( 'NONE',  ( 1.000000000000000000, 0.000000000000000000, 0.000000000000000000 ) ) ;
#40013 = AXIS2_PLACEMENT_3D ( 'NONE', #70037, #76846, #55927 ) ;
#40014 = ORIENTED_EDGE ( 'NONE', *, *, #53641, .T. ) ;
#40015 = ORIENTED_EDGE ( 'NONE', *, *, #58094, .T. ) ;
#40016 = CARTESIAN_POINT ( 'NONE',  ( 172.5667039024480118, -36.32844715993499563, 180.4678068554150059 ) ) ;
#40017 = DIRECTION ( 'NONE',  ( -0.7071067811866258435, 0.7071067811864693020, -7.071067811866266166E-16 ) ) ;
#40018 = CIRCLE ( 'NONE', #25499, 7.143750000000004263 ) ;
#40019 = FACE_OUTER_BOUND ( 'NONE', #58658, .T. ) ;
#40020 = CARTESIAN_POINT ( 'NONE',  ( 115.6043783821399558, -39.74888713174190968, 177.9905150661719802 ) ) ;
#40021 = CARTESIAN_POINT ( 'NONE',  ( 99.95068698205643898, -44.40877713917536340, 46.98133956162592284 ) ) ;
#40022 = DIRECTION ( 'NONE',  ( 0.000000000000000000, 0.000000000000000000, -1.000000000000000000 ) ) ;
#40023 = ORIENTED_EDGE ( 'NONE', *, *, #67638, .T. ) ;
#40024 = DIRECTION ( 'NONE',  ( 0.7071067811862279395, -0.7071067811868672059, 7.071067811862286363E-16 ) ) ;
#40025 = ORIENTED_EDGE ( 'NONE', *, *, #27745, .T. ) ;
#40026 = DIRECTION ( 'NONE',  ( -0.000000000000000000, -0.000000000000000000, -1.000000000000000000 ) ) ;
#40027 = ORIENTED_EDGE ( 'NONE', *, *, #15251, .F. ) ;
#40028 = CARTESIAN_POINT ( 'NONE',  ( 108.2977246876245374, -26.73284728312218661, 165.9788891058625779 ) ) ;
#40029 = CARTESIAN_POINT ( 'NONE',  ( 89.89403304293395536, -132.3042147552770302, 249.3173333679100097 ) ) ;
#40030 = CARTESIAN_POINT ( 'NONE',  ( 109.6417562379821931, -46.48040302697471304, 132.7813811145545344 ) ) ;
#40031 = VECTOR ( 'NONE', #62091, 1000.000000000000114 ) ;
#40032 = DIRECTION ( 'NONE',  ( 0.000000000000000000, 1.000000000000000000, 0.000000000000000000 ) ) ;
#40033 = VERTEX_POINT ( 'NONE', #12008 ) ;
#40034 = CARTESIAN_POINT ( 'NONE',  ( 104.2349294074198411, -46.78572220631293277, 22.35848241876792031 ) ) ;
#40035 = CARTESIAN_POINT ( 'NONE',  ( 107.8717034087400322, -26.29179415218835913, 66.01562527591097762 ) ) ;
#40036 = FILL_AREA_STYLE_COLOUR ( '', #75374 ) ;
#40038 = CARTESIAN_POINT ( 'NONE',  ( 143.0664832912740110, -18.82844715994099971, 284.9256252759119548 ) ) ;
#40037 = FACE_OUTER_BOUND ( 'NONE', #17787, .T. ) ;
#40039 = CARTESIAN_POINT ( 'NONE',  ( 76.24325998657066350, -5.906223855237660914, 14.67562527591093868 ) ) ;
#40040 = CARTESIAN_POINT ( 'NONE',  ( 179.4595971212733900, -26.00627455218473472, 237.4678068554150059 ) ) ;
#40041 = ADVANCED_FACE ( 'NONE', ( #61927 ), #5644, .F. ) ;
#40042 = CARTESIAN_POINT ( 'NONE',  ( 108.0667039024470455, -121.2010968907524529, -19.26696060647547881 ) ) ;
#40043 = EDGE_CURVE ( 'NONE', #77842, #88397, #34670, .T. ) ;
#40044 = DIRECTION ( 'NONE',  ( 0.000000000000000000, 0.000000000000000000, 1.000000000000000000 ) ) ;
#40045 = EDGE_LOOP ( 'NONE', ( #36362, #51070, #64696, #43225 ) ) ;
#40046 = CARTESIAN_POINT ( 'NONE',  ( 101.1165878437261227, -28.07204926635110098, 50.55562527591095545 ) ) ;
#40047 = CARTESIAN_POINT ( 'NONE',  ( 109.6893229801689813, -47.49076295823797267, 83.75467289495897205 ) ) ;
#40048 = EDGE_CURVE ( 'NONE', #76657, #82662, #55089, .T. ) ;
#40050 = DIRECTION ( 'NONE',  ( 0.000000000000000000, 1.000000000000000000, 0.000000000000000000 ) ) ;
#40049 = LINE ( 'NONE', #61388, #7335 ) ;
#40051 = DIRECTION ( 'NONE',  ( -1.000000000000000000, 0.000000000000000000, 0.000000000000000000 ) ) ;
#40052 = CARTESIAN_POINT ( 'NONE',  ( 130.3998166246059895, 12.92155284005730387, 355.9756252759109998 ) ) ;
#40053 = ORIENTED_EDGE ( 'NONE', *, *, #29490, .F. ) ;
#40054 = CARTESIAN_POINT ( 'NONE',  ( 107.3174176841070846, -26.95189801805073060, 116.0556252759109555 ) ) ;
#40055 = ADVANCED_FACE ( 'NONE', ( #81956, #48279 ), #61032, .T. ) ;
#40057 = ORIENTED_EDGE ( 'NONE', *, *, #67405, .T. ) ;
#40056 = LINE ( 'NONE', #80982, #87769 ) ;
#40058 = CARTESIAN_POINT ( 'NONE',  ( 96.14807755961388125, -35.16348456217431107, 222.2251490854349640 ) ) ;
#40059 = CARTESIAN_POINT ( 'NONE',  ( 116.8172402583773390, -34.15334170113332135, 255.0318177960892854 ) ) ;
#40060 = CARTESIAN_POINT ( 'NONE',  ( 117.0885934270242217, -37.65783532839622438, 148.7525704246621103 ) ) ;
#40061 = EDGE_CURVE ( 'NONE', #55274, #19496, #19267, .T. ) ;
#40062 = CARTESIAN_POINT ( 'NONE',  ( 25.56670390244797275, -65.37844715994100397, 137.2178068554150059 ) ) ;
#40063 = CARTESIAN_POINT ( 'NONE',  ( 74.36911441044796334, 82.54999999999999716, -92.32962665258483526 ) ) ;
#40064 = CARTESIAN_POINT ( 'NONE',  ( 131.3164832912740110, -36.72944715994100306, 3.101481641215535046 ) ) ;
#40065 = CARTESIAN_POINT ( 'NONE',  ( 63.06670390244699576, -67.87844715994098976, 120.2178068554179902 ) ) ;
#40066 = AXIS2_PLACEMENT_3D ( 'NONE', #26696, #4926, #47128 ) ;
#40067 = CARTESIAN_POINT ( 'NONE',  ( 102.2868918306627961, -45.93239726994513461, 167.1832443235309995 ) ) ;
#40068 = VERTEX_POINT ( 'NONE', #53300 ) ;
#40069 = ORIENTED_EDGE ( 'NONE', *, *, #59086, .T. ) ;
#40070 = VECTOR ( 'NONE', #54585, 999.9999999999998863 ) ;
#40071 = CARTESIAN_POINT ( 'NONE',  ( 102.8293847037436421, -28.94642981657014147, 141.9044404487549684 ) ) ;
#40072 = AXIS2_PLACEMENT_3D ( 'NONE', #18029, #60696, #4856 ) ;
#40073 = LINE ( 'NONE', #67791, #79143 ) ;
#40074 = AXIS2_PLACEMENT_3D ( 'NONE', #40191, #82909, #67913 ) ;
#40076 = LINE ( 'NONE', #59615, #84005 ) ;
#40075 = CARTESIAN_POINT ( 'NONE',  ( 99.85651329999866732, -30.12038005271842422, 271.7356252759109907 ) ) ;
#40077 = VECTOR ( 'NONE', #42309, 1000.000000000000000 ) ;
#40078 = CARTESIAN_POINT ( 'NONE',  ( 151.0371591254575776, -24.42818131005592264, 129.9678068554149775 ) ) ;
#40079 = PLANE ( 'NONE',  #67847 ) ;
#40080 = LINE ( 'NONE', #67797, #35677 ) ;
#40081 = DIRECTION ( 'NONE',  ( -0.7071067811865779928, 0.7071067811865171526, -6.612322855860441069E-17 ) ) ;
#40082 = DIRECTION ( 'NONE',  ( 0.000000000000000000, 0.000000000000000000, 1.000000000000000000 ) ) ;
#40083 = PRODUCT_DEFINITION_SHAPE ( 'NONE', 'NONE',  #69989 ) ;
#40084 = CARTESIAN_POINT ( 'NONE',  ( 95.43233898611173061, -38.84956357215551748, 201.4699109901969791 ) ) ;
#40085 = DIRECTION ( 'NONE',  ( 3.491483361109380094E-15, 0.000000000000000000, 1.000000000000000000 ) ) ;
#40086 = VERTEX_POINT ( 'NONE', #75578 ) ;
#40087 = VERTEX_POINT ( 'NONE', #39691 ) ;
#40088 = CARTESIAN_POINT ( 'NONE',  ( -91.71670967179979073, 69.85063703626885001, -92.91726854070125796 ) ) ;
#40089 = CARTESIAN_POINT ( 'NONE',  ( 182.3467384525650061, -29.62846900982231446, -5.074374724088000832 ) ) ;
#40090 = CARTESIAN_POINT ( 'NONE',  ( 168.5667039024481255, -48.82844715993497431, 300.4678068554149490 ) ) ;
#40091 = CARTESIAN_POINT ( 'NONE',  ( 95.83872823098278104, -90.36568251306732691, -9.274842254011060660 ) ) ;
#40092 = CIRCLE ( 'NONE', #53159, 9.525000000000000355 ) ;
#40093 = DIRECTION ( 'NONE',  ( 0.000000000000000000, 0.000000000000000000, 1.000000000000000000 ) ) ;
#40094 = EDGE_LOOP ( 'NONE', ( #10311, #20643, #24562, #13144, #88383, #28469 ) ) ;
#40095 = CARTESIAN_POINT ( 'NONE',  ( -9.473967051880050505, 90.86722304825821084, 117.9765084014371865 ) ) ;
#40096 = EDGE_CURVE ( 'NONE', #43857, #26574, #86267, .T. ) ;
#40097 = CARTESIAN_POINT ( 'NONE',  ( 101.3490469528152715, -46.18936307759902604, 202.1318157521019430 ) ) ;
#40098 = CARTESIAN_POINT ( 'NONE',  ( 136.7703230406660566, -37.23127003359719822, 6.817519769821919873 ) ) ;
#40099 = ORIENTED_EDGE ( 'NONE', *, *, #73141, .F. ) ;
#40100 = CARTESIAN_POINT ( 'NONE',  ( -12.17631415595668010, 85.81613294202711018, 117.9291186787848176 ) ) ;
#40101 = CYLINDRICAL_SURFACE ( 'NONE', #62311, 10.00000000000002487 ) ;
#40102 = CARTESIAN_POINT ( 'NONE',  ( 116.3175913315759402, -32.94491325663879877, 165.1356252759109680 ) ) ;
#40103 = CARTESIAN_POINT ( 'NONE',  ( 101.3472728536945198, -42.59232338312836674, 19.77951894102097796 ) ) ;
#40104 = CARTESIAN_POINT ( 'NONE',  ( 95.75547692839532488, -40.34654347423973775, 127.5727681330539554 ) ) ;
#40105 = CARTESIAN_POINT ( 'NONE',  ( 75.31670390244798341, -67.87844715994100397, 33.40080685541480676 ) ) ;
#40106 = ORIENTED_EDGE ( 'NONE', *, *, #72238, .T. ) ;
#40107 = VECTOR ( 'NONE', #25809, 1000.000000000000000 ) ;
#40108 = LINE ( 'NONE', #80133, #84222 ) ;
#40109 = CARTESIAN_POINT ( 'NONE',  ( 82.45780623542046328, -17.36823420008072105, 7.200493380652300601 ) ) ;
#40110 = ORIENTED_EDGE ( 'NONE', *, *, #69602, .T. ) ;
#40111 = ORIENTED_EDGE ( 'NONE', *, *, #75212, .F. ) ;
#40112 = EDGE_CURVE ( 'NONE', #29186, #70844, #7934, .T. ) ;
#40113 = PLANE ( 'NONE',  #15492 ) ;
#40114 = ORIENTED_EDGE ( 'NONE', *, *, #71993, .T. ) ;
#40115 = VERTEX_POINT ( 'NONE', #60580 ) ;
#40116 = CARTESIAN_POINT ( 'NONE',  ( 193.0374249753374443, -23.42844715993432558, 313.9678068554149490 ) ) ;
#40117 = CARTESIAN_POINT ( 'NONE',  ( 97.46629167631436985, -35.27791395320982559, 70.62956268521996606 ) ) ;
#40118 = CARTESIAN_POINT ( 'NONE',  ( 113.8136090879065563, -26.95650955708257257, 239.5956252759109759 ) ) ;
#40119 = CARTESIAN_POINT ( 'NONE',  ( 100.0229104548316172, -27.23016881827663127, 185.5841967044829630 ) ) ;
#40121 = CARTESIAN_POINT ( 'NONE',  ( 96.53701874497966173, -40.09164955422465937, 277.5603871806729899 ) ) ;
#40120 = CARTESIAN_POINT ( 'NONE',  ( 116.8768348252332174, -39.04445432745385602, 23.64277192200612276 ) ) ;
#40122 = LINE ( 'NONE', #47374, #39121 ) ;
#40123 = DIRECTION ( 'NONE',  ( 1.000000000000000000, 0.000000000000000000, 0.000000000000000000 ) ) ;
#40124 = ORIENTED_EDGE ( 'NONE', *, *, #14429, .T. ) ;
#40125 = EDGE_CURVE ( 'NONE', #57293, #29733, #47864, .T. ) ;
#40126 = ORIENTED_EDGE ( 'NONE', *, *, #41869, .F. ) ;
#40127 = CIRCLE ( 'NONE', #47377, 0.5000000000000172085 ) ;
#40128 = DIRECTION ( 'NONE',  ( 0.000000000000000000, 0.000000000000000000, 1.000000000000000000 ) ) ;
#40129 = CARTESIAN_POINT ( 'NONE',  ( 97.99847537351134008, -44.43658864837386346, 226.8870538473399563 ) ) ;
#40130 = ORIENTED_EDGE ( 'NONE', *, *, #37613, .T. ) ;
#40131 = COLOUR_RGB ( '', 0.72549020, 0.75294118, 0.79215686) ;
#40132 = CARTESIAN_POINT ( 'NONE',  ( 106.4836019150615840, -24.89303152268002606, 195.1156252759109861 ) ) ;
#40133 = PLANE ( 'NONE',  #31156 ) ;
#40134 = EDGE_CURVE ( 'NONE', #10599, #76633, #82297, .T. ) ;
#40135 = CARTESIAN_POINT ( 'NONE',  ( 97.86658156426001653, -40.64923495551180821, 22.64698795026609446 ) ) ;
#40136 = DIRECTION ( 'NONE',  ( -0.7071067811865270336, 0.7071067811865680008, -7.071067811865277132E-16 ) ) ;
#40138 = CARTESIAN_POINT ( 'NONE',  ( 163.0667039024470171, -32.29483332968611364, -5.074374724088000832 ) ) ;
#40137 = CARTESIAN_POINT ( 'NONE',  ( 113.5672778988914757, -32.00674077076433832, 277.6356252759110248 ) ) ;
#40139 = CARTESIAN_POINT ( 'NONE',  ( 99.50469279378565091, -43.30574573221327483, 172.8960156217824249 ) ) ;
#40140 = LINE ( 'NONE', #67860, #78751 ) ;
#40141 = DIRECTION ( 'NONE',  ( -1.000000000000000000, -1.000000000000000078E-15, 0.000000000000000000 ) ) ;
#40142 = CARTESIAN_POINT ( 'NONE',  ( -72.96458098368600531, 127.0000000000000000, -80.90208098368781009 ) ) ;
#40143 = CARTESIAN_POINT ( 'NONE',  ( 51.23005224011598102, -33.89581943344511217, 237.4678068554150059 ) ) ;
#40144 = ADVANCED_FACE ( 'NONE', ( #8325 ), #14245, .T. ) ;
#40145 = PLANE ( 'NONE',  #81163 ) ;
#40147 = ORIENTED_EDGE ( 'NONE', *, *, #55926, .F. ) ;
#40146 = CARTESIAN_POINT ( 'NONE',  ( -28.99999999999999289, 172.0000000000000000, 113.8826257785461280 ) ) ;
#40148 = CARTESIAN_POINT ( 'NONE',  ( 136.7895896102216113, -19.11755991740597693, 6.789748280179294326 ) ) ;
#40149 = CARTESIAN_POINT ( 'NONE',  ( 96.75080816152406271, -34.86525579675927844, 241.1841967044819626 ) ) ;
#40150 = CARTESIAN_POINT ( 'NONE',  ( 102.9710815734590454, -46.31642646611675218, 88.25562527591095829 ) ) ;
#40151 = CARTESIAN_POINT ( 'NONE',  ( 96.84642183402544902, -30.63342722027062592, 276.8984824187680829 ) ) ;
#40152 = CARTESIAN_POINT ( 'NONE',  ( 188.5667039024485518, -48.82844715993430640, 173.2178068554150059 ) ) ;
#40153 = CARTESIAN_POINT ( 'NONE',  ( 107.0664832912739968, 22.62155284005901024, 339.0006252759110339 ) ) ;
#40154 = VECTOR ( 'NONE', #58656, 1000.000000000000000 ) ;
#40156 = CARTESIAN_POINT ( 'NONE',  ( 219.9639999999999986, 40.03750000000000142, -7.937500000000000000 ) ) ;
#40155 = DIRECTION ( 'NONE',  ( 0.000000000000000000, 1.000000000000000000, 0.000000000000000000 ) ) ;
#40157 = DIRECTION ( 'NONE',  ( -0.7071067811607679721, 0.7071067812123270624, 0.000000000000000000 ) ) ;
#40158 = DIRECTION ( 'NONE',  ( -1.000000000000000078E-15, 1.000000000000000083E-30, 1.000000000000000000 ) ) ;
#40159 = CLOSED_SHELL ( 'NONE', ( #57160, #40447, #39732, #45501, #17611, #45740, #48639, #33894, #4116, #5933, #81900, #62943, #39213, #38491, #7875, #60226, #79340, #38456, #9799, #29593, #18403, #77496, #86723, #59823, #67217, #80651, #30571, #15362, #74074, #53049, #82431, #66661, #71884, #30728, #56260, #64980, #56949, #17198, #79751, #63528, #41853, #23990, #70218, #21406, #84096, #65591, #77532, #6853, #52413, #35852, #68782, #50387, #33719, #47441, #5496, #16844, #70824, #10033, #37588, #49798, #66897, #3079, #23665, #89581, #23744, #12866, #60398, #49546, #80309, #78761, #7807, #79050, #9908, #17470, #21280, #10908, #29701, #21709, #69615, #32533, #80, #11919, #74192, #79254, #61720, #54771, #59647, #42591, #69553, #40234, #43514, #77419, #39154, #34835, #25182, #31038, #64332, #47599, #42933, #80479 ) ) ;
#40160 = ORIENTED_EDGE ( 'NONE', *, *, #87316, .F. ) ;
#40161 = VERTEX_POINT ( 'NONE', #71009 ) ;
#40162 = CARTESIAN_POINT ( 'NONE',  ( 103.2107857629706018, -44.35110894017614669, 126.6267055423619610 ) ) ;
#40163 = ADVANCED_FACE ( 'NONE', ( #22406 ), #21968, .T. ) ;
#40165 = EDGE_LOOP ( 'NONE', ( #6188, #25050, #73763, #227 ) ) ;
#40164 = CARTESIAN_POINT ( 'NONE',  ( 23.18381393575008786, 52.19607888965136056, 30.23446726999232226 ) ) ;
#40166 = DIRECTION ( 'NONE',  ( -1.000000000000000078E-15, 0.000000000000000000, -1.000000000000000000 ) ) ;
#40167 = CARTESIAN_POINT ( 'NONE',  ( 103.4759237351581049, -46.49349013887657378, 138.2956252759109645 ) ) ;
#40168 = DIRECTION ( 'NONE',  ( -0.9834602067153815907, -0.1811243269341220596, 0.000000000000000000 ) ) ;
#40169 = EDGE_CURVE ( 'NONE', #45628, #85065, #49183, .T. ) ;
#40170 = EDGE_CURVE ( 'NONE', #16891, #14442, #49634, .T. ) ;
#40171 = CYLINDRICAL_SURFACE ( 'NONE', #22413, 7.143749999999999822 ) ;
#40172 = CARTESIAN_POINT ( 'NONE',  ( 38.10000000000000142, 69.84999999999999432, 283.4005000000000223 ) ) ;
#40173 = CARTESIAN_POINT ( 'NONE',  ( 0.000000000000000000, 127.0000000000000000, 0.000000000000000000 ) ) ;
#40174 = EDGE_CURVE ( 'NONE', #42012, #42564, #1961, .T. ) ;
#40175 = CARTESIAN_POINT ( 'NONE',  ( 115.1932381579440943, -43.17108053757048935, 48.30514908543492680 ) ) ;
#40176 = ORIENTED_EDGE ( 'NONE', *, *, #52741, .T. ) ;
#40177 = VERTEX_POINT ( 'NONE', #29657 ) ;
#40179 = ORIENTED_EDGE ( 'NONE', *, *, #82123, .F. ) ;
#40178 = CIRCLE ( 'NONE', #88050, 1.000000000000000888 ) ;
#40180 = CARTESIAN_POINT ( 'NONE',  ( 41.56648329127399677, -9.303447159940999356, 76.80862527591200717 ) ) ;
#40182 = DIRECTION ( 'NONE',  ( 0.000000000000000000, -1.000000000000000000, 0.000000000000000000 ) ) ;
#40181 = CARTESIAN_POINT ( 'NONE',  ( 103.2204921605864314, -27.09891563476517717, 171.3908633711489813 ) ) ;
#40183 = DIRECTION ( 'NONE',  ( 0.000000000000000000, 0.000000000000000000, 1.000000000000000000 ) ) ;
#40184 = DIRECTION ( 'NONE',  ( 1.000000000000000078E-15, -1.000000000000000000, 0.000000000000000000 ) ) ;
#40185 = DIRECTION ( 'NONE',  ( 0.000000000000000000, 1.000000000000000000, 0.000000000000000000 ) ) ;
#40186 = FACE_OUTER_BOUND ( 'NONE', #55339, .T. ) ;
#40187 = CARTESIAN_POINT ( 'NONE',  ( 138.8167039024479834, -67.87844715994100397, 58.80080685541479824 ) ) ;
#40188 = CARTESIAN_POINT ( 'NONE',  ( 117.5733473178508319, -42.15660255127708211, 93.44705384733897802 ) ) ;
#40189 = ORIENTED_EDGE ( 'NONE', *, *, #52011, .T. ) ;
#40190 = VERTEX_POINT ( 'NONE', #85090 ) ;
#40191 = CARTESIAN_POINT ( 'NONE',  ( -103.1875000000000000, 117.4749999999999943, -1.080832317973422076E-12 ) ) ;
#40192 = AXIS2_PLACEMENT_3D ( 'NONE', #22098, #89338, #49763 ) ;
#40193 = CARTESIAN_POINT ( 'NONE',  ( -82.97845804870345887, 84.21348395916258767, -100.7940789023224823 ) ) ;
#40194 = VECTOR ( 'NONE', #18177, 1000.000000000000000 ) ;
#40195 = DIRECTION ( 'NONE',  ( 0.000000000000000000, 1.000000000000000000, 0.000000000000000000 ) ) ;
#40196 = CARTESIAN_POINT ( 'NONE',  ( 103.0775956431641305, -44.40992243120454930, 165.0014237029239439 ) ) ;
#40197 = CIRCLE ( 'NONE', #30100, 0.5000000000000004441 ) ;
#40198 = VECTOR ( 'NONE', #32164, 1000.000000000000000 ) ;
#40199 = VECTOR ( 'NONE', #28836, 1000.000000000000000 ) ;
#40200 = EDGE_CURVE ( 'NONE', #22706, #75722, #40178, .T. ) ;
#40201 = FACE_OUTER_BOUND ( 'NONE', #80189, .T. ) ;
#40202 = ORIENTED_EDGE ( 'NONE', *, *, #50070, .T. ) ;
#40203 = ORIENTED_EDGE ( 'NONE', *, *, #18529, .T. ) ;
#40204 = DIRECTION ( 'NONE',  ( -1.000000000000000000, -3.999999999999999995E-14, -1.000000000000000078E-15 ) ) ;
#40205 = CARTESIAN_POINT ( 'NONE',  ( 136.1637134159087168, -20.51083119282026246, 2.376725019081067369 ) ) ;
#40206 = ORIENTED_EDGE ( 'NONE', *, *, #60667, .T. ) ;
#40207 = ORIENTED_EDGE ( 'NONE', *, *, #17484, .T. ) ;
#40208 = CARTESIAN_POINT ( 'NONE',  ( 77.41433294703951162, -19.45719076514804868, 6.889371645759243101 ) ) ;
#40209 = CARTESIAN_POINT ( 'NONE',  ( 102.2066036383193222, -44.77047292137198298, 198.5634880678019272 ) ) ;
#40210 = AXIS2_PLACEMENT_3D ( 'NONE', #51635, #86630, #23958 ) ;
#40211 = CIRCLE ( 'NONE', #34387, 18.00000000000000355 ) ;
#40212 = AXIS2_PLACEMENT_3D ( 'NONE', #11198, #32087, #23954 ) ;
#40213 = CARTESIAN_POINT ( 'NONE',  ( 69.72411017812960665, 120.6499999999999915, 69.72411017813040246 ) ) ;
#40214 = DIRECTION ( 'NONE',  ( -1.000000000000000000, 0.000000000000000000, 0.000000000000000000 ) ) ;
#40215 = ORIENTED_EDGE ( 'NONE', *, *, #50310, .F. ) ;
#40216 = EDGE_LOOP ( 'NONE', ( #13537, #73079, #70827, #77888, #30485, #35605 ) ) ;
#40217 = AXIS2_PLACEMENT_3D ( 'NONE', #59069, #78676, #17321 ) ;
#40218 = ADVANCED_FACE ( 'NONE', ( #28298 ), #64621, .F. ) ;
#40219 = DIRECTION ( 'NONE',  ( 0.000000000000000000, 0.000000000000000000, -1.000000000000000000 ) ) ;
#40220 = ORIENTED_EDGE ( 'NONE', *, *, #35214, .T. ) ;
#40221 = ORIENTED_EDGE ( 'NONE', *, *, #14758, .F. ) ;
#40222 = EDGE_CURVE ( 'NONE', #59530, #36232, #50536, .T. ) ;
#40223 = CARTESIAN_POINT ( 'NONE',  ( 109.3322008939200458, -45.72736107978396092, 240.5909475124479684 ) ) ;
#40224 = EDGE_CURVE ( 'NONE', #56759, #69797, #7869, .T. ) ;
#40225 = CARTESIAN_POINT ( 'NONE',  ( 98.18350318933659082, -43.34670532666833509, 111.8480062282919647 ) ) ;
#40226 = CARTESIAN_POINT ( 'NONE',  ( 114.3378803067696765, -44.16957155219879638, 73.19276813305397411 ) ) ;
#40227 = CARTESIAN_POINT ( 'NONE',  ( 100.1629373784320762, -32.34215477114681647, 249.5838068554172082 ) ) ;
#40228 = CARTESIAN_POINT ( 'NONE',  ( 133.6902059199458677, -15.99866847873243358, 8.209451181316913093 ) ) ;
#40229 = CARTESIAN_POINT ( 'NONE',  ( 108.0801309524341463, -25.31521737950549067, 322.2013064277864487 ) ) ;
#40230 = CARTESIAN_POINT ( 'NONE',  ( 98.26135236841564335, -42.31085888804770434, 182.7756252759109543 ) ) ;
#40231 = CARTESIAN_POINT ( 'NONE',  ( 164.9212702847356127, -29.73316016638977644, 237.4678068554150059 ) ) ;
#40232 = EDGE_LOOP ( 'NONE', ( #65583, #2610, #41659, #84208 ) ) ;
#40233 = CARTESIAN_POINT ( 'NONE',  ( 130.2266331669276838, 73.86195533656251655, -9.272499861614344141 ) ) ;
#40235 = VERTEX_POINT ( 'NONE', #35564 ) ;
#40234 = ADVANCED_FACE ( 'NONE', ( #55990, #78278 ), #70553, .F. ) ;
#40236 = ADVANCED_FACE ( 'NONE', ( #55535, #63282 ), #1058, .T. ) ;
#40237 = ORIENTED_EDGE ( 'NONE', *, *, #54046, .F. ) ;
#40238 = CARTESIAN_POINT ( 'NONE',  ( -24.20305689751608824, 54.97499999999995879, 75.96110745944689313 ) ) ;
#40239 = ORIENTED_EDGE ( 'NONE', *, *, #23370, .F. ) ;
#40240 = VECTOR ( 'NONE', #46958, 1000.000000000000000 ) ;
#40241 = EDGE_CURVE ( 'NONE', #14889, #76782, #88551, .T. ) ;
#40242 = DIRECTION ( 'NONE',  ( 0.000000000000000000, 0.000000000000000000, -1.000000000000000000 ) ) ;
#40243 = CARTESIAN_POINT ( 'NONE',  ( 101.9936209152398163, -45.44607152400298844, 177.1564586071733913 ) ) ;
#40244 = CARTESIAN_POINT ( 'NONE',  ( 116.9750915152277884, -33.48807190773455034, 89.07848241876791917 ) ) ;
#40245 = CARTESIAN_POINT ( 'NONE',  ( 112.1432782410116005, -28.01507713225257135, 254.6564226208779473 ) ) ;
#40246 = ADVANCED_FACE ( 'NONE', ( #81303 ), #18595, .F. ) ;
#40247 = CARTESIAN_POINT ( 'NONE',  ( 136.8164812439621016, -36.63640413217029135, 6.749771997051099426 ) ) ;
#40248 = DIRECTION ( 'NONE',  ( -0.7071067811864634178, 0.7071067811866316166, -7.071067811864642099E-16 ) ) ;
#40251 = CARTESIAN_POINT ( 'NONE',  ( 110.1310368924891208, -26.13358316477614451, 210.8403871806729626 ) ) ;
#40250 = CARTESIAN_POINT ( 'NONE',  ( 72.96458098368650269, 127.0000000000000000, 65.82083098368730134 ) ) ;
#40249 = CARTESIAN_POINT ( 'NONE',  ( 210.5660000000000025, 52.73749999999999716, -44.45000000000000284 ) ) ;
#40252 = CARTESIAN_POINT ( 'NONE',  ( -492.0614999999999668, 93.66249999999999432, 11.11250000000040217 ) ) ;
#40253 = CARTESIAN_POINT ( 'NONE',  ( 71.24076473329807868, 5.642044068322332961, 361.9756252759101471 ) ) ;
#40254 = ORIENTED_EDGE ( 'NONE', *, *, #44744, .T. ) ;
#40255 = DIRECTION ( 'NONE',  ( 0.000000000000000000, 0.000000000000000000, -1.000000000000000000 ) ) ;
#40256 = ADVANCED_FACE ( 'NONE', ( #81744 ), #2472, .T. ) ;
#40257 = CARTESIAN_POINT ( 'NONE',  ( 33.81648329127400388, 12.92155284005802685, 336.5756252759108520 ) ) ;
#40258 = DIRECTION ( 'NONE',  ( -1.000000000000000000, 0.000000000000000000, 0.000000000000000000 ) ) ;
#40259 = EDGE_CURVE ( 'NONE', #14890, #56634, #39925, .T. ) ;
#40260 = PLANE ( 'NONE',  #11441 ) ;
#40262 = ORIENTED_EDGE ( 'NONE', *, *, #25998, .F. ) ;
#40261 = CARTESIAN_POINT ( 'NONE',  ( 118.7030916724021665, -39.22306760090339139, 258.6584824187677896 ) ) ;
#40263 = DIRECTION ( 'NONE',  ( -1.000000000000000078E-15, -1.000000000000000083E-30, 1.000000000000000000 ) ) ;
#40264 = CARTESIAN_POINT ( 'NONE',  ( 100.5976686157419806, -28.50914727160554207, 11.60705384733995515 ) ) ;
#40265 = CARTESIAN_POINT ( 'NONE',  ( 117.8455077981468122, -34.08178244914028454, 160.0061014663869798 ) ) ;
#40266 = AXIS2_PLACEMENT_3D ( 'NONE', #45247, #72539, #32075 ) ;
#40267 = FACE_BOUND ( 'NONE', #72290, .T. ) ;
#40268 = DIRECTION ( 'NONE',  ( 1.000000000000000000, 0.000000000000000000, 0.000000000000000000 ) ) ;
#40270 = CARTESIAN_POINT ( 'NONE',  ( 49.21437657594998427, -35.91149509761070391, -5.074374724088000832 ) ) ;
#40269 = LINE ( 'NONE', #46626, #41932 ) ;
#40271 = DIRECTION ( 'NONE',  ( 0.000000000000000000, 0.000000000000000000, 1.000000000000000000 ) ) ;
#40272 = CARTESIAN_POINT ( 'NONE',  ( 24.79284581386643183, 184.0000000000000000, 85.23828826961327820 ) ) ;
#40273 = VERTEX_POINT ( 'NONE', #47176 ) ;
#40274 = CIRCLE ( 'NONE', #28673, 7.143750000000004263 ) ;
#40275 = CIRCLE ( 'NONE', #78034, 6.999999999999997335 ) ;
#40276 = EDGE_LOOP ( 'NONE', ( #77104, #82098, #6117, #39498 ) ) ;
#40277 = VERTEX_POINT ( 'NONE', #53983 ) ;
#40278 = EDGE_CURVE ( 'NONE', #55604, #70047, #11792, .T. ) ;
#40279 = VECTOR ( 'NONE', #20772, 1000.000000000000000 ) ;
#40280 = VERTEX_POINT ( 'NONE', #32669 ) ;
#40281 = CARTESIAN_POINT ( 'NONE',  ( -127.0122462326317958, 52.31737473627642743, 30.21206415535068146 ) ) ;
#40282 = CARTESIAN_POINT ( 'NONE',  ( 96.71096103112840581, -32.93116260832598385, 17.03467289495896964 ) ) ;
#40283 = DIRECTION ( 'NONE',  ( 0.000000000000000000, 1.000000000000000000, 0.000000000000000000 ) ) ;
#40284 = EDGE_CURVE ( 'NONE', #28809, #25358, #49957, .T. ) ;
#40285 = EDGE_CURVE ( 'NONE', #81699, #38611, #66235, .T. ) ;
#40286 = AXIS2_PLACEMENT_3D ( 'NONE', #49512, #89641, #55073 ) ;
#40287 = CARTESIAN_POINT ( 'NONE',  ( 117.1097670608697143, -36.65276801037281018, 118.8336923977722250 ) ) ;
#40290 = EDGE_CURVE ( 'NONE', #68161, #17652, #30992, .T. ) ;
#40289 = CARTESIAN_POINT ( 'NONE',  ( 0.000000000000000000, 20.32000000000000028, 0.000000000000000000 ) ) ;
#40288 = DIRECTION ( 'NONE',  ( 1.000000000000000078E-15, 0.000000000000000000, 1.000000000000000000 ) ) ;
#40291 = AXIS2_PLACEMENT_3D ( 'NONE', #20711, #68417, #67062 ) ;
#40292 = CARTESIAN_POINT ( 'NONE',  ( 114.3529501776022244, -31.35170872818512322, 258.7428960185527558 ) ) ;
#40293 = ORIENTED_EDGE ( 'NONE', *, *, #43889, .F. ) ;
#40294 = ORIENTED_EDGE ( 'NONE', *, *, #41530, .F. ) ;
#40295 = EDGE_LOOP ( 'NONE', ( #5943, #72529, #21979, #22264 ) ) ;
#40296 = FACE_OUTER_BOUND ( 'NONE', #4237, .T. ) ;
#40297 = CARTESIAN_POINT ( 'NONE',  ( 138.8167039024479834, -57.40094715994099772, 37.63480685541480852 ) ) ;
#40298 = DIRECTION ( 'NONE',  ( -0.000000000000000000, -0.000000000000000000, 1.000000000000000000 ) ) ;
#40299 = CARTESIAN_POINT ( 'NONE',  ( 116.3251852747984003, -32.94148267319277323, 269.1356252759109680 ) ) ;
#40300 = CARTESIAN_POINT ( 'NONE',  ( 115.8966032383871436, -37.77400989437322210, 50.16444044875395747 ) ) ;
#40301 = DIRECTION ( 'NONE',  ( -4.237773401492740281E-14, 1.000000000000000000, 0.000000000000000000 ) ) ;
#40302 = DIRECTION ( 'NONE',  ( 0.000000000000000000, 1.000000000000000000, 0.000000000000000000 ) ) ;
#40303 = CARTESIAN_POINT ( 'NONE',  ( 115.3604274781777264, -30.50455558986040572, 264.3508633711496714 ) ) ;
#40304 = ORIENTED_EDGE ( 'NONE', *, *, #71386, .F. ) ;
#40305 = DIRECTION ( 'NONE',  ( -0.7071067811856560636, -0.7071067811874389708, 0.000000000000000000 ) ) ;
#40306 = VECTOR ( 'NONE', #42320, 1000.000000000000000 ) ;
#40307 = CARTESIAN_POINT ( 'NONE',  ( 165.2748236753140247, -30.08671355700301575, -5.074374724088000832 ) ) ;
#40308 = CARTESIAN_POINT ( 'NONE',  ( 111.5696292435227122, -29.33873666780462486, 47.44713798863897836 ) ) ;
#40309 = VECTOR ( 'NONE', #68620, 1000.000000000000000 ) ;
#40310 = CARTESIAN_POINT ( 'NONE',  ( 136.1934021726284243, -16.98608769072011881, 7.448832051635106311 ) ) ;
#40311 = FACE_OUTER_BOUND ( 'NONE', #13416, .T. ) ;
#40312 = CARTESIAN_POINT ( 'NONE',  ( 141.8545562996767444, -1.932463243632623229, 361.9756252759100335 ) ) ;
#40313 = ORIENTED_EDGE ( 'NONE', *, *, #77635, .F. ) ;
#40314 = CARTESIAN_POINT ( 'NONE',  ( 77.54412859703519700, -35.63380991825863475, 7.053480412781513387 ) ) ;
#40315 = VERTEX_POINT ( 'NONE', #46733 ) ;
#40316 = CARTESIAN_POINT ( 'NONE',  ( 114.4629700169191580, -28.51537706926042404, 159.5051490854349652 ) ) ;
#40317 = VERTEX_POINT ( 'NONE', #16482 ) ;
#40318 = CARTESIAN_POINT ( 'NONE',  ( 116.7149163912777396, -35.64392129247566032, 83.33813411379098568 ) ) ;
#40319 = CARTESIAN_POINT ( 'NONE',  ( 51.39690000000000225, 82.54999999999999716, 344.4418053999999643 ) ) ;
#40320 = CARTESIAN_POINT ( 'NONE',  ( 113.6158397245882128, -43.46609735470438807, 114.6339642582779561 ) ) ;
#40321 = CARTESIAN_POINT ( 'NONE',  ( 64.68306507141296890, -72.55818180160879649, 361.9756252759101471 ) ) ;
#40322 = AXIS2_PLACEMENT_3D ( 'NONE', #71332, #44037, #49959 ) ;
#40323 = DIRECTION ( 'NONE',  ( 1.000000000000000078E-15, -1.000000000000000083E-30, -1.000000000000000000 ) ) ;
#40324 = CARTESIAN_POINT ( 'NONE',  ( 98.28804800891427362, -28.73186473263583807, 76.73848241876795839 ) ) ;
#40325 = PLANE ( 'NONE',  #58482 ) ;
#40326 = DIRECTION ( 'NONE',  ( 1.000000000000000078E-15, -1.000000000000000083E-30, -1.000000000000000000 ) ) ;
#40327 = VECTOR ( 'NONE', #78301, 1000.000000000000000 ) ;
#40328 = VERTEX_POINT ( 'NONE', #88107 ) ;
#40329 = AXIS2_PLACEMENT_3D ( 'NONE', #67987, #88891, #54318 ) ;
#40330 = DIRECTION ( 'NONE',  ( -0.7071067811865671127, -0.7071067811865279218, -7.071067811865664660E-16 ) ) ;
#40331 = ORIENTED_EDGE ( 'NONE', *, *, #54252, .F. ) ;
#40333 = ADVANCED_FACE ( 'NONE', ( #30554 ), #58252, .F. ) ;
#40332 = ORIENTED_EDGE ( 'NONE', *, *, #63219, .T. ) ;
#40334 = EDGE_CURVE ( 'NONE', #52825, #45687, #67188, .T. ) ;
#40336 = ADVANCED_FACE ( 'NONE', ( #16929 ), #25409, .T. ) ;
#40335 = CIRCLE ( 'NONE', #27315, 0.5000000000000031086 ) ;
#40337 = CARTESIAN_POINT ( 'NONE',  ( 76.06670390244809710, -58.72944715994109544, 199.5838068554169524 ) ) ;
#40338 = ORIENTED_EDGE ( 'NONE', *, *, #3657, .T. ) ;
#40339 = CARTESIAN_POINT ( 'NONE',  ( 110.5849939505706772, -26.97450646431652643, 249.7889586092449576 ) ) ;
#40340 = CARTESIAN_POINT ( 'NONE',  ( 108.0088980509730305, -26.32399177548269620, 151.0041967044829505 ) ) ;
#40341 = DIRECTION ( 'NONE',  ( 0.9068632946707805287, -0.4214249218767882610, 9.493511560072084562E-16 ) ) ;
#40342 = LINE ( 'NONE', #55733, #3968 ) ;
#40343 = CARTESIAN_POINT ( 'NONE',  ( 115.1668113632844808, -43.29200554620488361, 84.28419670448195689 ) ) ;
#40344 = CARTESIAN_POINT ( 'NONE',  ( 97.07216058387446367, -35.37757943919933012, 97.21864571800702493 ) ) ;
#40345 = ORIENTED_EDGE ( 'NONE', *, *, #85922, .F. ) ;
#40346 = CIRCLE ( 'NONE', #33152, 4.000000000000002665 ) ;
#40347 = CARTESIAN_POINT ( 'NONE',  ( 21.03689327557615130, -23.42844715994197813, 180.4678068554150911 ) ) ;
#40348 = EDGE_CURVE ( 'NONE', #85102, #35902, #60467, .T. ) ;
#40349 = VECTOR ( 'NONE', #34945, 1000.000000000000000 ) ;
#40350 = VECTOR ( 'NONE', #59908, 1000.000000000000000 ) ;
#40351 = CARTESIAN_POINT ( 'NONE',  ( 48.79742451362098166, -36.32844715994040996, -5.074374724088000832 ) ) ;
#40352 = ORIENTED_EDGE ( 'NONE', *, *, #46643, .F. ) ;
#40353 = ADVANCED_FACE ( 'NONE', ( #48075 ), #85153, .T. ) ;
#40354 = DIRECTION ( 'NONE',  ( 1.000000000000000078E-15, 0.000000000000000000, 1.000000000000000000 ) ) ;
#40355 = LINE ( 'NONE', #33980, #52674 ) ;
#40356 = CARTESIAN_POINT ( 'NONE',  ( 111.8540205700169139, -46.00543295620339990, 272.9556252759110180 ) ) ;
#40357 = LINE ( 'NONE', #21266, #77985 ) ;
#40358 = CARTESIAN_POINT ( 'NONE',  ( 69.63919639214307722, 92.07499999999998863, 53.63573739454427880 ) ) ;
#40359 = CARTESIAN_POINT ( 'NONE',  ( 117.0614924034066036, -38.07622789054436652, 93.71956107247139300 ) ) ;
#40360 = ADVANCED_FACE ( 'NONE', ( #13572 ), #41262, .F. ) ;
#40361 = CARTESIAN_POINT ( 'NONE',  ( 97.36980136507975203, -37.22440909395530184, 270.7895626852197779 ) ) ;
#40363 = CARTESIAN_POINT ( 'NONE',  ( 95.51222647996985415, -34.21005103128004521, 102.1556252759109640 ) ) ;
#40362 = CARTESIAN_POINT ( 'NONE',  ( 113.2072602631850060, -28.80268442222084602, 99.55275712281951428 ) ) ;
#40364 = CARTESIAN_POINT ( 'NONE',  ( 182.5667039024469886, -33.35206098992650681, -5.074374724088000832 ) ) ;
#40365 = CARTESIAN_POINT ( 'NONE',  ( 105.3088311808849937, -48.49934056980919905, 147.4584824187679715 ) ) ;
#40366 = VERTEX_POINT ( 'NONE', #40823 ) ;
#40367 = CARTESIAN_POINT ( 'NONE',  ( 182.4202572930268502, -31.94127993907054730, 117.4678068554150627 ) ) ;
#40368 = ORIENTED_EDGE ( 'NONE', *, *, #76725, .F. ) ;
#40369 = AXIS2_PLACEMENT_3D ( 'NONE', #41788, #20925, #48594 ) ;
#40370 = LINE ( 'NONE', #32206, #10564 ) ;
#40371 = CARTESIAN_POINT ( 'NONE',  ( 107.0664832912739541, -23.22944715994095688, 312.1356252759112522 ) ) ;
#40372 = DIRECTION ( 'NONE',  ( -1.000000000000000000, -4.299999999999999979E-14, -1.000000000000000078E-15 ) ) ;
#40373 = EDGE_LOOP ( 'NONE', ( #8012, #65968, #86478, #3380, #63350, #77943, #77112, #60136, #15509, #3318, #78633, #41180, #34666, #83837, #60376, #71970, #37580, #17874, #21000, #181, #64778, #80955, #23500, #7324, #37674, #8336, #20, #52388, #55666, #23780, #75466, #34263, #42895, #29519, #41789, #63238, #33078, #70635, #89604, #47215, #75055, #82950, #42647, #20504, #61005, #61464, #81984, #15005 ) ) ;
#40374 = EDGE_CURVE ( 'NONE', #59914, #59817, #89899, .T. ) ;
#40375 = FACE_OUTER_BOUND ( 'NONE', #7133, .T. ) ;
#40377 = ORIENTED_EDGE ( 'NONE', *, *, #69515, .T. ) ;
#40376 = CARTESIAN_POINT ( 'NONE',  ( 114.2052324763531743, -45.22952987728847063, 148.1203871806719405 ) ) ;
#40378 = CARTESIAN_POINT ( 'NONE',  ( 0.000000000000000000, 117.4749999999999943, -103.1875000000000000 ) ) ;
#40379 = CARTESIAN_POINT ( 'NONE',  ( -130.0906791124283473, 88.91243380484085890, 11.02261862230878720 ) ) ;
#40380 = AXIS2_PLACEMENT_3D ( 'NONE', #16876, #44556, #85493 ) ;
#40381 = CARTESIAN_POINT ( 'NONE',  ( 112.0659116179119650, -45.48839626324947005, 118.9897919421637198 ) ) ;
#40382 = EDGE_CURVE ( 'NONE', #52251, #46008, #27651, .T. ) ;
#40383 = DIRECTION ( 'NONE',  ( 4.299999999999999979E-14, -1.000000000000000000, 0.000000000000000000 ) ) ;
#40384 = EDGE_LOOP ( 'NONE', ( #40621, #1786, #27871, #78128 ) ) ;
#40385 = SHAPE_DEFINITION_REPRESENTATION ( #43964, #28740 ) ;
#40386 = PLANE ( 'NONE',  #55719 ) ;
#40387 = ORIENTED_EDGE ( 'NONE', *, *, #22556, .F. ) ;
#40388 = ORIENTED_EDGE ( 'NONE', *, *, #71880, .T. ) ;
#40389 = VERTEX_POINT ( 'NONE', #83977 ) ;
#40390 = DIRECTION ( 'NONE',  ( 0.000000000000000000, -1.000000000000000000, 0.000000000000000000 ) ) ;
#40391 = CARTESIAN_POINT ( 'NONE',  ( 107.0667039024470313, -104.2784471599421323, -21.78219314458201694 ) ) ;
#40392 = CARTESIAN_POINT ( 'NONE',  ( 90.44969454456408187, -20.11243780205710507, 239.5838068554175209 ) ) ;
#40393 = DIRECTION ( 'NONE',  ( -0.7071067811865436870, 0.000000000000000000, -0.7071067811865514585 ) ) ;
#40394 = VECTOR ( 'NONE', #52949, 1000.000000000000000 ) ;
#40397 = EDGE_CURVE ( 'NONE', #4973, #78353, #20839, .T. ) ;
#40396 = DIRECTION ( 'NONE',  ( 0.000000000000000000, 0.000000000000000000, -1.000000000000000000 ) ) ;
#40395 = DIRECTION ( 'NONE',  ( 0.000000000000000000, 0.000000000000000000, 1.000000000000000000 ) ) ;
#40398 = LINE ( 'NONE', #5893, #37067 ) ;
#40399 = VECTOR ( 'NONE', #26768, 1000.000000000000000 ) ;
#40401 = VERTEX_POINT ( 'NONE', #69888 ) ;
#40400 = CIRCLE ( 'NONE', #73801, 6.858000000000003205 ) ;
#40402 =( BOUNDED_CURVE ( )  B_SPLINE_CURVE ( 3, ( #3888, #58836, #79767, #80211 ),
 .UNSPECIFIED., .F., .F. ) 
 B_SPLINE_CURVE_WITH_KNOTS ( ( 4, 4 ),
 ( 5.086905507537815818E-12, 1.570796326801274345 ),
 .UNSPECIFIED. ) 
 CURVE ( )  GEOMETRIC_REPRESENTATION_ITEM ( )  RATIONAL_B_SPLINE_CURVE ( ( 1.000000000000000000, 0.8047378541240607364, 0.8047378541240607364, 1.000000000000000000 ) ) 
 REPRESENTATION_ITEM ( '' )  );
#40403 = DIRECTION ( 'NONE',  ( 4.299999999999999979E-14, -1.000000000000000000, 4.400000000000000367E-29 ) ) ;
#40404 = CARTESIAN_POINT ( 'NONE',  ( 172.5664832912740110, -36.32844715994070839, 323.6756252759119548 ) ) ;
#40405 = CARTESIAN_POINT ( 'NONE',  ( 114.3351522754912963, -30.13549343754564092, 205.4127681330539872 ) ) ;
#40407 = EDGE_LOOP ( 'NONE', ( #25227, #46330 ) ) ;
#40406 = LINE ( 'NONE', #33595, #24039 ) ;
#40408 = VECTOR ( 'NONE', #70621, 1000.000000000000000 ) ;
#40409 = CARTESIAN_POINT ( 'NONE',  ( 106.6854394624702849, -26.95610377642496758, 81.10705384733896040 ) ) ;
#40410 = DIRECTION ( 'NONE',  ( -8.673617379884035472E-16, -1.000000000000000000, 0.000000000000000000 ) ) ;
#40411 = LINE ( 'NONE', #45858, #47079 ) ;
#40412 = CARTESIAN_POINT ( 'NONE',  ( 103.1875000000000000, 127.0000000000000000, 3.602774393244745134E-13 ) ) ;
#40413 = ORIENTED_EDGE ( 'NONE', *, *, #71946, .F. ) ;
#40414 = EDGE_CURVE ( 'NONE', #27495, #56128, #62165, .T. ) ;
#40415 = CARTESIAN_POINT ( 'NONE',  ( 107.0667039024479834, -36.72944715994100306, 239.5838068554170093 ) ) ;
#40416 = ORIENTED_EDGE ( 'NONE', *, *, #53119, .T. ) ;
#40417 = ORIENTED_EDGE ( 'NONE', *, *, #26882, .F. ) ;
#40418 = CARTESIAN_POINT ( 'NONE',  ( 109.5261983718769585, -46.49778922373468504, 239.2044404487539566 ) ) ;
#40419 = ADVANCED_FACE ( 'NONE', ( #33567 ), #61706, .F. ) ;
#40420 = LINE ( 'NONE', #87681, #21164 ) ;
#40421 = CARTESIAN_POINT ( 'NONE',  ( -118.5129862669514580, 94.84303900880915705, -3.295572367532775715 ) ) ;
#40422 = CARTESIAN_POINT ( 'NONE',  ( 116.3215253324775773, -32.93968801256757217, 155.1356252759109680 ) ) ;
#40423 = AXIS2_PLACEMENT_3D ( 'NONE', #44922, #46703, #60335 ) ;
#40424 = CARTESIAN_POINT ( 'NONE',  ( -24.79284581386642827, 184.0000000000000000, 85.23828826961327820 ) ) ;
#40425 = ORIENTED_EDGE ( 'NONE', *, *, #40382, .T. ) ;
#40426 = FACE_OUTER_BOUND ( 'NONE', #56034, .T. ) ;
#40427 = CARTESIAN_POINT ( 'NONE',  ( 179.7974245136200011, -36.32844715994040996, -5.074374724088000832 ) ) ;
#40428 = ORIENTED_EDGE ( 'NONE', *, *, #59083, .T. ) ;
#40429 = CARTESIAN_POINT ( 'NONE',  ( 111.3232390708907786, -27.21277439355663219, 24.74133956162494030 ) ) ;
#40430 = VERTEX_POINT ( 'NONE', #6759 ) ;
#40431 = CARTESIAN_POINT ( 'NONE',  ( 111.2517653011026226, -44.30469234039772886, 250.7842808457816375 ) ) ;
#40432 = DIRECTION ( 'NONE',  ( -0.7071067811865692221, -0.7071067811865259234, -7.071067811865685367E-16 ) ) ;
#40433 = CARTESIAN_POINT ( 'NONE',  ( 112.9441315310009628, -44.54716313336201949, 143.0899109901969553 ) ) ;
#40434 = CARTESIAN_POINT ( 'NONE',  ( 130.0664832912740110, -18.82844715994099971, 199.5838068554170093 ) ) ;
#40435 = LINE ( 'NONE', #74515, #33123 ) ;
#40436 = LINE ( 'NONE', #82249, #53535 ) ;
#40437 = CARTESIAN_POINT ( 'NONE',  ( -41.60202597009397607, 53.97499999999997300, 50.85338361873603219 ) ) ;
#40438 = AXIS2_PLACEMENT_3D ( 'NONE', #12835, #39618, #11021 ) ;
#40439 = CARTESIAN_POINT ( 'NONE',  ( 95.24589774366052097, -38.10235284316662074, 232.4184824187679794 ) ) ;
#40440 = FACE_OUTER_BOUND ( 'NONE', #33614, .T. ) ;
#40441 = ORIENTED_EDGE ( 'NONE', *, *, #2533, .F. ) ;
#40442 = CARTESIAN_POINT ( 'NONE',  ( 103.2630468498471856, -47.15688066943211254, 93.28610146638693834 ) ) ;
#40443 = DIRECTION ( 'NONE',  ( 0.000000000000000000, 0.000000000000000000, -1.000000000000000000 ) ) ;
#40444 = ORIENTED_EDGE ( 'NONE', *, *, #42893, .T. ) ;
#40446 = ADVANCED_FACE ( 'NONE', ( #83516 ), #42159, .F. ) ;
#40445 = ORIENTED_EDGE ( 'NONE', *, *, #36008, .T. ) ;
#40448 = ORIENTED_EDGE ( 'NONE', *, *, #73394, .T. ) ;
#40447 = ADVANCED_FACE ( 'NONE', ( #69441 ), #82643, .F. ) ;
#40449 = EDGE_CURVE ( 'NONE', #87834, #9197, #55332, .T. ) ;
#40450 = FACE_OUTER_BOUND ( 'NONE', #7014, .T. ) ;
#40451 = CARTESIAN_POINT ( 'NONE',  ( 172.5664832912740110, -18.82844715994099971, 136.8086252759119645 ) ) ;
#40452 = CARTESIAN_POINT ( 'NONE',  ( 34.92499999999999716, 66.67499999999999716, 292.1000000000000227 ) ) ;
#40453 = CARTESIAN_POINT ( 'NONE',  ( 48.16670390244701139, -28.27351298637280408, -5.074374724088000832 ) ) ;
#40454 = CARTESIAN_POINT ( 'NONE',  ( 98.41263308787671349, -36.61538842024999241, 154.1461856076869594 ) ) ;
#40455 = CARTESIAN_POINT ( 'NONE',  ( 96.86769303131731590, -30.64611497598638579, 276.8984824187680829 ) ) ;
#40456 = CARTESIAN_POINT ( 'NONE',  ( 98.38040403964905067, -41.69523976407170096, 57.73976173181551275 ) ) ;
#40457 = ORIENTED_EDGE ( 'NONE', *, *, #8162, .T. ) ;
#40458 = CARTESIAN_POINT ( 'NONE',  ( 130.3279567413621862, 92.64985122628465319, 7.743850073004674428 ) ) ;
#40459 = CIRCLE ( 'NONE', #33203, 4.750000000000000888 ) ;
#40460 = EDGE_CURVE ( 'NONE', #41221, #41944, #75360, .T. ) ;
#40461 = DIRECTION ( 'NONE',  ( -2.999999999999999839E-15, 1.000000000000000000, -2.999999999999999900E-30 ) ) ;
#40462 = VERTEX_POINT ( 'NONE', #21289 ) ;
#40463 = ORIENTED_EDGE ( 'NONE', *, *, #36332, .F. ) ;
#40464 = AXIS2_PLACEMENT_3D ( 'NONE', #29823, #65228, #17525 ) ;
#40465 = AXIS2_PLACEMENT_3D ( 'NONE', #71301, #8624, #9069 ) ;
#40466 = EDGE_CURVE ( 'NONE', #30894, #89471, #7216, .T. ) ;
#40467 = CARTESIAN_POINT ( 'NONE',  ( 165.6738106836030227, -28.98061976758901892, -5.074374724088000832 ) ) ;
#40468 = ORIENTED_EDGE ( 'NONE', *, *, #42312, .T. ) ;
#40469 = VERTEX_POINT ( 'NONE', #75807 ) ;
#40470 = CARTESIAN_POINT ( 'NONE',  ( 178.6914832912739826, 12.92155284005802685, 335.5992267699913327 ) ) ;
#40471 = CARTESIAN_POINT ( 'NONE',  ( -9.554664674393775314, 74.17305037928137779, -130.2061759407760633 ) ) ;
#40472 = DIRECTION ( 'NONE',  ( 0.000000000000000000, 0.000000000000000000, 1.000000000000000000 ) ) ;
#40473 = CARTESIAN_POINT ( 'NONE',  ( 141.3509999999999991, 101.5999999999999943, 141.3509999999999991 ) ) ;
#40474 = EDGE_CURVE ( 'NONE', #73333, #7861, #62617, .T. ) ;
#40475 = CARTESIAN_POINT ( 'NONE',  ( 114.9272539996656377, -40.07076659875138347, 167.9295626852199632 ) ) ;
#40476 = CARTESIAN_POINT ( 'NONE',  ( 117.0961560025638306, -31.97355093185684538, 64.19086337114899266 ) ) ;
#40477 = LINE ( 'NONE', #33666, #79982 ) ;
#40478 = ORIENTED_EDGE ( 'NONE', *, *, #41118, .T. ) ;
#40479 = CARTESIAN_POINT ( 'NONE',  ( 164.9212702847350158, -29.73316016639540749, 117.4678068554150485 ) ) ;
#40480 = VERTEX_POINT ( 'NONE', #391 ) ;
#40481 = AXIS2_PLACEMENT_3D ( 'NONE', #48001, #12168, #75739 ) ;
#40482 = CARTESIAN_POINT ( 'NONE',  ( -22.62762465138237999, 172.0000000000000000, 0.000000000000000000 ) ) ;
#40483 = ORIENTED_EDGE ( 'NONE', *, *, #78002, .T. ) ;
#40484 = CARTESIAN_POINT ( 'NONE',  ( -72.96458098368600531, 117.4749999999999943, -65.82083098368781293 ) ) ;
#40485 = AXIS2_PLACEMENT_3D ( 'NONE', #1526, #29228, #56914 ) ;
#40486 = FACE_OUTER_BOUND ( 'NONE', #21428, .T. ) ;
#40487 = CARTESIAN_POINT ( 'NONE',  ( 98.15097650629928694, -41.26161077846109038, 131.7007372803578562 ) ) ;
#40488 = B_SPLINE_CURVE_WITH_KNOTS ( 'NONE', 3,
 ( #40422, #26351, #33611, #60862, #5013, #4570, #46769, #13178, #19990, #5923, #68137, #25453, #89029, #18641, #61747, #20441, #88592, #47671 ),
 .UNSPECIFIED., .F., .F.,
 ( 4, 2, 2, 2, 2, 2, 2, 2, 4 ),
 ( 0.000000000000000000, 0.06250000028368622729, 0.1250000005673724546, 0.1875000008510586680, 0.2500000011347449091, 0.3125000014184311503, 0.3750000017021173360, 0.4375000019858035771, 0.5000000022694898183 ),
 .UNSPECIFIED. ) ;
#40489 = CARTESIAN_POINT ( 'NONE',  ( 69.72411017812960665, 120.6499999999999915, 69.72411017813040246 ) ) ;
#40490 = EDGE_LOOP ( 'NONE', ( #34370, #64864, #10451, #49592 ) ) ;
#40491 = CARTESIAN_POINT ( 'NONE',  ( 115.9104104090373539, -31.16785412357883800, 34.27276813305396530 ) ) ;
#40492 = CARTESIAN_POINT ( 'NONE',  ( 106.9267702420067678, -26.22618599733332090, 56.08705384733997334 ) ) ;
#40494 = FACE_OUTER_BOUND ( 'NONE', #13097, .T. ) ;
#40493 = CARTESIAN_POINT ( 'NONE',  ( 107.0667039024470313, -104.2784471599413934, 2.217806855418003043 ) ) ;
#40495 = CARTESIAN_POINT ( 'NONE',  ( 196.2150000000000034, 30.98800000000000310, 57.14999999999999858 ) ) ;
#40496 = CARTESIAN_POINT ( 'NONE',  ( 142.8682495647594806, 8.654319075478440482, 542.9756252759101471 ) ) ;
#40497 = VERTEX_POINT ( 'NONE', #82191 ) ;
#40498 = AXIS2_PLACEMENT_3D ( 'NONE', #83616, #48603, #47716 ) ;
#40499 = DIRECTION ( 'NONE',  ( 0.000000000000000000, 1.000000000000000000, 0.000000000000000000 ) ) ;
#40500 = CARTESIAN_POINT ( 'NONE',  ( 147.0662307635748220, -124.3843534097310055, 246.1014443220830117 ) ) ;
#40501 = CARTESIAN_POINT ( 'NONE',  ( 37.06648329127400388, 12.92155284005802685, 335.5992267699910485 ) ) ;
#40502 = ORIENTED_EDGE ( 'NONE', *, *, #14423, .F. ) ;
#40503 = CARTESIAN_POINT ( 'NONE',  ( 96.61744970692362244, -37.56424831167382195, 97.38991099019594344 ) ) ;
#40506 = EDGE_CURVE ( 'NONE', #69114, #88820, #48964, .T. ) ;
#40505 = CARTESIAN_POINT ( 'NONE',  ( 3.174999999999889688, 111.1250000000000000, 31.75000000000000000 ) ) ;
#40504 = CARTESIAN_POINT ( 'NONE',  ( -48.02966122971775320, 100.5999999999999659, -8.747637655308301746E-15 ) ) ;
#40507 = DIRECTION ( 'NONE',  ( 0.000000000000000000, -1.000000000000000000, 0.000000000000000000 ) ) ;
#40508 = CONICAL_SURFACE ( 'NONE', #23164, 1.219499999999975159, 1.047197551196598297 ) ;
#40509 = DIRECTION ( 'NONE',  ( 0.000000000000000000, 0.000000000000000000, 1.000000000000000000 ) ) ;
#40510 = ORIENTED_EDGE ( 'NONE', *, *, #60123, .T. ) ;
#40511 = CARTESIAN_POINT ( 'NONE',  ( 106.1376555893193370, -47.80867374849567852, 108.5099109901959622 ) ) ;
#40513 = ORIENTED_EDGE ( 'NONE', *, *, #53976, .T. ) ;
#40512 = CARTESIAN_POINT ( 'NONE',  ( 10.07149677053134162, 90.28936803021488799, 130.1671656890560200 ) ) ;
#40514 = CARTESIAN_POINT ( 'NONE',  ( 100.7633749303631561, -45.78122309449478422, 233.0803871806729717 ) ) ;
#40515 = FACE_OUTER_BOUND ( 'NONE', #5685, .T. ) ;
#40516 = CARTESIAN_POINT ( 'NONE',  ( 110.8966428001789524, -45.96688915401393416, 147.8892538962421952 ) ) ;
#40517 = FACE_OUTER_BOUND ( 'NONE', #792, .T. ) ;
#40518 = FACE_OUTER_BOUND ( 'NONE', #69229, .T. ) ;
#40519 = VECTOR ( 'NONE', #86318, 1000.000000000000000 ) ;
#40520 = CARTESIAN_POINT ( 'NONE',  ( 69.36073695985297149, -137.4541704093869043, 247.5777870314779818 ) ) ;
#40521 = CARTESIAN_POINT ( 'NONE',  ( 161.4809174648185603, -49.32844715993547169, 180.4678068554150059 ) ) ;
#40522 = CARTESIAN_POINT ( 'NONE',  ( 113.8091913586854531, -43.81457933525494042, 158.1813395616259754 ) ) ;
#40523 = ORIENTED_EDGE ( 'NONE', *, *, #89079, .F. ) ;
#40524 = VERTEX_POINT ( 'NONE', #28532 ) ;
#40525 = AXIS2_PLACEMENT_3D ( 'NONE', #73434, #31200, #9883 ) ;
#40526 = CARTESIAN_POINT ( 'NONE',  ( 108.8812380984771835, -28.05563920549329993, 136.3444404487549662 ) ) ;
#40527 = VECTOR ( 'NONE', #7501, 1000.000000000000000 ) ;
#40528 = EDGE_CURVE ( 'NONE', #86394, #71994, #56228, .T. ) ;
#40529 = PLANE ( 'NONE',  #19662 ) ;
#40531 = DIRECTION ( 'NONE',  ( 1.639958061481212836E-42, -4.100000000000000342E-29, -1.000000000000000000 ) ) ;
#40530 = CARTESIAN_POINT ( 'NONE',  ( 110.5849939505706487, -26.97450646431661880, 245.7889586092439629 ) ) ;
#40532 = DIRECTION ( 'NONE',  ( 1.000000000000000078E-15, -1.000000000000000083E-30, -1.000000000000000000 ) ) ;
#40533 = LINE ( 'NONE', #88706, #28691 ) ;
#40534 = AXIS2_PLACEMENT_3D ( 'NONE', #43421, #758, #14405 ) ;
#40535 = DIRECTION ( 'NONE',  ( -3.100000000000000258E-29, 3.100000000000000044E-14, 1.000000000000000000 ) ) ;
#40536 = FACE_OUTER_BOUND ( 'NONE', #47118, .T. ) ;
#40537 = FACE_OUTER_BOUND ( 'NONE', #70594, .T. ) ;
#40539 = CARTESIAN_POINT ( 'NONE',  ( 98.45302666770167832, -29.83944080489365902, 195.7775300378159784 ) ) ;
#40538 = PRESENTATION_LAYER_ASSIGNMENT (  '', '', ( #26025 ) ) ;
#40540 = CARTESIAN_POINT ( 'NONE',  ( 31.71315051185510114, -33.70561438052087055, 313.9678068554150059 ) ) ;
#40541 = ORIENTED_EDGE ( 'NONE', *, *, #77893, .F. ) ;
#40542 = VERTEX_POINT ( 'NONE', #63513 ) ;
#40543 = DIRECTION ( 'NONE',  ( -0.9254794337955620787, -0.3787978585227822492, 0.000000000000000000 ) ) ;
#40544 = CARTESIAN_POINT ( 'NONE',  ( -72.96458098368751166, 117.4749999999999943, 72.96458098368620426 ) ) ;
#40545 = CIRCLE ( 'NONE', #18832, 1.571100913904416307 ) ;
#40546 = CARTESIAN_POINT ( 'NONE',  ( 48.16670390244752298, -28.27351298637377397, 237.4678068554150059 ) ) ;
#40547 = LINE ( 'NONE', #5134, #53464 ) ;
#40548 = DIRECTION ( 'NONE',  ( 0.7071067811865536790, 0.000000000000000000, -0.7071067811865413555 ) ) ;
#40549 = ORIENTED_EDGE ( 'NONE', *, *, #71550, .T. ) ;
#40550 = DIRECTION ( 'NONE',  ( 0.000000000000000000, 0.000000000000000000, -1.000000000000000000 ) ) ;
#40551 = CARTESIAN_POINT ( 'NONE',  ( 116.8576245982602870, -40.31003124190988274, 218.5470538473399529 ) ) ;
#40553 = VERTEX_POINT ( 'NONE', #49868 ) ;
#40552 = EDGE_CURVE ( 'NONE', #84701, #86605, #57560, .T. ) ;
#40554 = VECTOR ( 'NONE', #78038, 1000.000000000000000 ) ;
#40555 = EDGE_CURVE ( 'NONE', #9081, #62285, #35838, .T. ) ;
#40556 = CYLINDRICAL_SURFACE ( 'NONE', #27440, 12.70000000000000107 ) ;
#40557 = DIRECTION ( 'NONE',  ( 0.000000000000000000, 0.000000000000000000, 1.000000000000000000 ) ) ;
#40558 = EDGE_CURVE ( 'NONE', #55655, #13929, #50319, .T. ) ;
#40559 = CARTESIAN_POINT ( 'NONE',  ( 99.04397795006340743, -42.84113160514387886, 162.8439467858095213 ) ) ;
#40560 = CARTESIAN_POINT ( 'NONE',  ( 98.94126815719160106, -33.74921318831734851, 18.85285227435401367 ) ) ;
#40561 = CARTESIAN_POINT ( 'NONE',  ( 96.03095270115332482, -35.77956804193283347, 182.2461014663869889 ) ) ;
#40562 = FACE_OUTER_BOUND ( 'NONE', #66935, .T. ) ;
#40563 = ORIENTED_EDGE ( 'NONE', *, *, #24535, .F. ) ;
#40564 = ADVANCED_FACE ( 'NONE', ( #3088, #9901 ), #79402, .T. ) ;
#40565 = FACE_OUTER_BOUND ( 'NONE', #15085, .T. ) ;
#40566 = CONICAL_SURFACE ( 'NONE', #53571, 88.90000000000000568, 0.7853981633974621568 ) ;
#40567 = CARTESIAN_POINT ( 'NONE',  ( 114.8447031547741943, -43.15207964168884303, 68.27931773607517130 ) ) ;
#40568 = ORIENTED_EDGE ( 'NONE', *, *, #14776, .T. ) ;
#40569 = VERTEX_POINT ( 'NONE', #16716 ) ;
#40570 = DIRECTION ( 'NONE',  ( 1.000000000000000078E-15, 0.000000000000000000, 1.000000000000000000 ) ) ;
#40571 = ORIENTED_EDGE ( 'NONE', *, *, #12473, .T. ) ;
#40572 = EDGE_LOOP ( 'NONE', ( #27109, #22216, #14823, #41677 ) ) ;
#40573 = DIRECTION ( 'NONE',  ( 0.000000000000000000, 1.000000000000000000, 0.000000000000000000 ) ) ;
#40574 = EDGE_CURVE ( 'NONE', #42410, #53519, #76431, .T. ) ;
#40575 = CARTESIAN_POINT ( 'NONE',  ( 104.2253390597007581, -44.78450961640034222, 56.72956268521994616 ) ) ;
#40576 = CARTESIAN_POINT ( 'NONE',  ( 117.5128880048294491, -35.85709896013243281, 253.8927681330537780 ) ) ;
#40577 = CIRCLE ( 'NONE', #36249, 3.000000000000002665 ) ;
#40578 = CARTESIAN_POINT ( 'NONE',  ( 100.6510976905701824, -26.79511100149714764, 220.5327681330539633 ) ) ;
#40580 = CARTESIAN_POINT ( 'NONE',  ( 100.4791399132689236, -44.80881982087480964, 8.032768133053981074 ) ) ;
#40579 = CARTESIAN_POINT ( 'NONE',  ( 116.7834531110833325, -34.06957675735675650, 24.03834616677710656 ) ) ;
#40581 = DIRECTION ( 'NONE',  ( -1.000000000000000078E-15, 1.000000000000000083E-30, 1.000000000000000000 ) ) ;
#40582 = LINE ( 'NONE', #13334, #38068 ) ;
#40583 = CONICAL_SURFACE ( 'NONE', #11618, 1.625000000000001332, 1.029744258676650093 ) ;
#40584 = EDGE_LOOP ( 'NONE', ( #70119, #4064, #89634, #87071 ) ) ;
#40585 = CIRCLE ( 'NONE', #14281, 3.500000000000003109 ) ;
#40586 = AXIS2_PLACEMENT_3D ( 'NONE', #83721, #26181, #56438 ) ;
#40587 = LINE ( 'NONE', #11554, #48700 ) ;
#40588 = CARTESIAN_POINT ( 'NONE',  ( 100.1093887754828984, -44.55284168805902567, 266.9984824187678782 ) ) ;
#40589 = ORIENTED_EDGE ( 'NONE', *, *, #4550, .F. ) ;
#40590 = CARTESIAN_POINT ( 'NONE',  ( 110.4989391570660473, -26.88539935475378684, 209.8099109901969541 ) ) ;
#40591 = LINE ( 'NONE', #47385, #67395 ) ;
#40592 = FACE_OUTER_BOUND ( 'NONE', #5281, .T. ) ;
#40593 = SURFACE_STYLE_FILL_AREA ( #12904 ) ;
#40594 = CARTESIAN_POINT ( 'NONE',  ( 110.1624778137653067, -46.32779280511170583, 28.82556394023509938 ) ) ;
#40596 = LINE ( 'NONE', #82853, #63049 ) ;
#40595 = CARTESIAN_POINT ( 'NONE',  ( 99.76018885984304063, -32.42404554134276395, 277.6356252759108543 ) ) ;
#40597 = DIRECTION ( 'NONE',  ( 0.000000000000000000, -1.000000000000000000, 0.000000000000000000 ) ) ;
#40598 = DIRECTION ( 'NONE',  ( 0.000000000000000000, 0.000000000000000000, 1.000000000000000000 ) ) ;
#40599 = CARTESIAN_POINT ( 'NONE',  ( 164.9190312289455278, -35.91149509760636960, 193.9678068554149775 ) ) ;
#40600 = AXIS2_PLACEMENT_3D ( 'NONE', #22371, #43690, #8751 ) ;
#40601 = CARTESIAN_POINT ( 'NONE',  ( 92.81932083335593120, -113.5527167097541934, -11.78219314458173272 ) ) ;
#40602 = LINE ( 'NONE', #8152, #70852 ) ;
#40603 = PLANE ( 'NONE',  #69196 ) ;
#40604 = CARTESIAN_POINT ( 'NONE',  ( 86.06670390244796920, -48.82844715994099971, 198.9178068554149945 ) ) ;
#40606 = ORIENTED_EDGE ( 'NONE', *, *, #51612, .T. ) ;
#40605 = CARTESIAN_POINT ( 'NONE',  ( 101.0707582237941438, -29.13849289886354299, 195.5838068554168672 ) ) ;
#40607 = CARTESIAN_POINT ( 'NONE',  ( 25.56670390244797275, -65.37844715994100397, 288.3428068554150059 ) ) ;
#40608 = CARTESIAN_POINT ( 'NONE',  ( 106.8511556536399780, -47.80415145147887301, 227.5489586092439538 ) ) ;
#40609 = CARTESIAN_POINT ( 'NONE',  ( 114.0221110621602492, -28.96402831996850225, 110.4956252759109816 ) ) ;
#40610 = CARTESIAN_POINT ( 'NONE',  ( 110.8324567285566076, -26.28842506301429083, 245.7889586092439629 ) ) ;
#40611 = LINE ( 'NONE', #61494, #74467 ) ;
#40612 = AXIS2_PLACEMENT_3D ( 'NONE', #81291, #5872, #5417 ) ;
#40613 = LINE ( 'NONE', #68329, #78081 ) ;
#40616 = EDGE_CURVE ( 'NONE', #64816, #12332, #85333, .T. ) ;
#40615 = FACE_OUTER_BOUND ( 'NONE', #31841, .T. ) ;
#40614 = LINE ( 'NONE', #46959, #63816 ) ;
#40617 = DIRECTION ( 'NONE',  ( 0.000000000000000000, 0.000000000000000000, -1.000000000000000000 ) ) ;
#40618 = CYLINDRICAL_SURFACE ( 'NONE', #12318, 3.499999999999996003 ) ;
#40619 = ADVANCED_FACE ( 'NONE', ( #58044 ), #15825, .T. ) ;
#40620 = ORIENTED_EDGE ( 'NONE', *, *, #68160, .F. ) ;
#40621 = ORIENTED_EDGE ( 'NONE', *, *, #79860, .T. ) ;
#40622 = MECHANICAL_DESIGN_GEOMETRIC_PRESENTATION_REPRESENTATION (  '', ( #72532 ), #29029 ) ;
#40623 = CARTESIAN_POINT ( 'NONE',  ( 115.1266331755855958, -39.55612640683342107, 132.9809912566479397 ) ) ;
#40625 = ORIENTED_EDGE ( 'NONE', *, *, #87090, .F. ) ;
#40624 = LINE ( 'NONE', #32909, #32840 ) ;
#40626 = DIRECTION ( 'NONE',  ( -6.982966722218760189E-15, 0.000000000000000000, -1.000000000000000000 ) ) ;
#40627 = CARTESIAN_POINT ( 'NONE',  ( 114.7100688122352494, -43.78666090992606996, 119.2327681330539804 ) ) ;
#40628 = CARTESIAN_POINT ( 'NONE',  ( 107.5667039024470171, -95.29234678213566667, 2.217806855417725487 ) ) ;
#40629 = DIRECTION ( 'NONE',  ( 1.000000000000000078E-15, -1.000000000000000083E-30, -1.000000000000000000 ) ) ;
#40630 = DIRECTION ( 'NONE',  ( 0.000000000000000000, 0.000000000000000000, 1.000000000000000000 ) ) ;
#40631 = CARTESIAN_POINT ( 'NONE',  ( 107.0664832912739541, -23.72944715994095688, 315.6356252759111953 ) ) ;
#40632 = CARTESIAN_POINT ( 'NONE',  ( 104.9021620152489191, -46.26774620671726268, 72.39848241876894974 ) ) ;
#40633 = ORIENTED_EDGE ( 'NONE', *, *, #85204, .F. ) ;
#40634 = VECTOR ( 'NONE', #29599, 1000.000000000000000 ) ;
#40635 = ORIENTED_EDGE ( 'NONE', *, *, #28135, .F. ) ;
#40636 = ORIENTED_EDGE ( 'NONE', *, *, #9194, .T. ) ;
#40637 = EDGE_CURVE ( 'NONE', #11683, #63148, #44519, .T. ) ;
#40638 = CARTESIAN_POINT ( 'NONE',  ( 107.0664832912750057, -36.72944715993903486, 9.425625275910970657 ) ) ;
#40640 = CARTESIAN_POINT ( 'NONE',  ( 49.21213752015764697, -29.73316016639473958, 117.4678068554150485 ) ) ;
#40639 = CARTESIAN_POINT ( 'NONE',  ( 102.2868918306628387, -45.93239726994502803, 163.1832443235289816 ) ) ;
#40641 = CARTESIAN_POINT ( 'NONE',  ( 9.261585182541649530, 223.9999999999999716, 152.5407914452011369 ) ) ;
#40642 = DIRECTION ( 'NONE',  ( -1.000000000000000000, -4.299999999999999979E-14, -1.000000000000000078E-15 ) ) ;
#40643 = VECTOR ( 'NONE', #9942, 1000.000000000000000 ) ;
#40644 = LINE ( 'NONE', #46095, #1358 ) ;
#40645 = DIRECTION ( 'NONE',  ( -0.000000000000000000, -0.000000000000000000, 1.000000000000000000 ) ) ;
#40646 = CARTESIAN_POINT ( 'NONE',  ( 116.6546583390153131, -32.60254457568996855, 79.14991099019697174 ) ) ;
#40647 = VERTEX_POINT ( 'NONE', #29004 ) ;
#40648 = ORIENTED_EDGE ( 'NONE', *, *, #16064, .T. ) ;
#40649 = EDGE_LOOP ( 'NONE', ( #67582, #30079 ) ) ;
#40650 = VECTOR ( 'NONE', #82315, 1000.000000000000114 ) ;
#40651 = EDGE_CURVE ( 'NONE', #54776, #7655, #4446, .T. ) ;
#40652 = CARTESIAN_POINT ( 'NONE',  ( -240.5296158183964792, 14.28750000000026077, 15.87499999999969802 ) ) ;
#40653 = CARTESIAN_POINT ( 'NONE',  ( -91.73195104381140652, 95.23006786499111342, -92.89936586972014254 ) ) ;
#40654 = PLANE ( 'NONE',  #25021 ) ;
#40655 = CARTESIAN_POINT ( 'NONE',  ( 108.8610815749077574, -28.26302276435299987, 182.7404713219719667 ) ) ;
#40656 = VECTOR ( 'NONE', #56336, 1000.000000000000000 ) ;
#40657 = CARTESIAN_POINT ( 'NONE',  ( 97.06104777439192333, -37.99628893422420362, 27.42740443400874994 ) ) ;
#40658 = EDGE_LOOP ( 'NONE', ( #87345, #27106 ) ) ;
#40660 = ORIENTED_EDGE ( 'NONE', *, *, #31694, .T. ) ;
#40659 = ORIENTED_EDGE ( 'NONE', *, *, #61465, .F. ) ;
#40661 = AXIS2_PLACEMENT_3D ( 'NONE', #54396, #82609, #53950 ) ;
#40662 = DIRECTION ( 'NONE',  ( 0.000000000000000000, 0.000000000000000000, -1.000000000000000000 ) ) ;
#40663 = CARTESIAN_POINT ( 'NONE',  ( 136.5411229421876271, -19.94037323191022892, 2.740176903249453844 ) ) ;
#40664 = ORIENTED_EDGE ( 'NONE', *, *, #88146, .F. ) ;
#40665 = VERTEX_POINT ( 'NONE', #35798 ) ;
#40666 = CARTESIAN_POINT ( 'NONE',  ( 194.0371591254582313, -46.82818131005407736, 300.4678068554149490 ) ) ;
#40667 = EDGE_CURVE ( 'NONE', #11533, #70410, #56689, .T. ) ;
#40668 = CARTESIAN_POINT ( 'NONE',  ( 112.1317502087781293, -44.64270164792750961, 214.4492023535159717 ) ) ;
#40669 = CIRCLE ( 'NONE', #14568, 9.810460662156732070 ) ;
#40670 = FACE_BOUND ( 'NONE', #25581, .T. ) ;
#40671 = CARTESIAN_POINT ( 'NONE',  ( -122.9597727627798918, 73.41921189914249624, 43.88359923157533871 ) ) ;
#40672 = EDGE_LOOP ( 'NONE', ( #23567, #63537, #46148, #64373 ) ) ;
#40673 = EDGE_LOOP ( 'NONE', ( #15618, #65330, #11661, #71691 ) ) ;
#40674 = CARTESIAN_POINT ( 'NONE',  ( 63.03715912545820999, -46.82818131006018092, 300.4678068554150627 ) ) ;
#40675 = ORIENTED_EDGE ( 'NONE', *, *, #76363, .T. ) ;
#40676 = ORIENTED_EDGE ( 'NONE', *, *, #38192, .T. ) ;
#40677 = EDGE_CURVE ( 'NONE', #62184, #36627, #22647, .T. ) ;
#40678 = CARTESIAN_POINT ( 'NONE',  ( 101.1728908740289512, -31.04189437634028437, 248.5338046553059428 ) ) ;
#40679 = CARTESIAN_POINT ( 'NONE',  ( 108.6520877210037952, -25.77347123183324484, 149.9737205140059473 ) ) ;
#40680 = AXIS2_PLACEMENT_3D ( 'NONE', #57935, #10237, #37941 ) ;
#40681 = CARTESIAN_POINT ( 'NONE',  ( 117.3319688044107920, -38.62265419183311366, 88.68133956162493803 ) ) ;
#40682 = CARTESIAN_POINT ( 'NONE',  ( 105.9148582384516999, -44.85806553849772627, 249.5838068554170945 ) ) ;
#40683 = EDGE_CURVE ( 'NONE', #2544, #54712, #50778, .T. ) ;
#40684 = DIRECTION ( 'NONE',  ( 0.000000000000000000, 0.000000000000000000, -1.000000000000000000 ) ) ;
#40685 = DIRECTION ( 'NONE',  ( 0.000000000000000000, 0.000000000000000000, -1.000000000000000000 ) ) ;
#40686 = CARTESIAN_POINT ( 'NONE',  ( 96.64436219916188975, -36.48069147925158262, 192.3070538473399438 ) ) ;
#40687 = CARTESIAN_POINT ( 'NONE',  ( 41.56670390244718050, -42.82844715994109208, 180.4678068554150911 ) ) ;
#40688 = ORIENTED_EDGE ( 'NONE', *, *, #30314, .T. ) ;
#40689 = CARTESIAN_POINT ( 'NONE',  ( 138.8167039024479834, -67.87844715994100397, 86.31780685541500020 ) ) ;
#40690 = ORIENTED_EDGE ( 'NONE', *, *, #79360, .F. ) ;
#40691 = ORIENTED_EDGE ( 'NONE', *, *, #71641, .F. ) ;
#40692 = LINE ( 'NONE', #12100, #66218 ) ;
#40694 = ORIENTED_EDGE ( 'NONE', *, *, #86615, .F. ) ;
#40693 = VECTOR ( 'NONE', #77881, 1000.000000000000000 ) ;
#40695 = CARTESIAN_POINT ( 'NONE',  ( 36.65249034007450746, -49.32844715994130524, 129.9678068554150911 ) ) ;
#40696 = CARTESIAN_POINT ( 'NONE',  ( 117.3640430381357334, -38.35649778030718693, 113.7013395616249767 ) ) ;
#40697 = CARTESIAN_POINT ( 'NONE',  ( -6.304597144436756118, 71.52322690941528549, 130.4037788038045846 ) ) ;
#40698 = CARTESIAN_POINT ( 'NONE',  ( 136.5970563715325170, -35.65296049054685312, 7.043700149390024201 ) ) ;
#40699 = CARTESIAN_POINT ( 'NONE',  ( 41.56648329127399677, 0.2215528400590013880, 318.9256252759120116 ) ) ;
#40702 = CARTESIAN_POINT ( 'NONE',  ( 98.55548742614595881, -30.74683778668247669, 201.8384824187679385 ) ) ;
#40701 = CARTESIAN_POINT ( 'NONE',  ( 107.0667039024470313, -104.2784471599413934, 2.217806855418003043 ) ) ;
#40700 = CARTESIAN_POINT ( 'NONE',  ( 188.5667039024484097, -48.82844715993431350, 257.2178068554150059 ) ) ;
#40703 = DIRECTION ( 'NONE',  ( -0.000000000000000000, 1.000000000000000000, 0.000000000000000000 ) ) ;
#40704 = CARTESIAN_POINT ( 'NONE',  ( 116.3215253324775773, -32.93968801256757217, 155.1356252759109680 ) ) ;
#40705 = EDGE_LOOP ( 'NONE', ( #45251, #68832, #796, #52900 ) ) ;
#40706 = CARTESIAN_POINT ( 'NONE',  ( -48.26476610531311451, 53.97499999999997300, 65.76796570303405076 ) ) ;
#40707 = CARTESIAN_POINT ( 'NONE',  ( 186.6899999999999977, 52.73749999999999716, -44.45000000000000284 ) ) ;
#40708 = DIRECTION ( 'NONE',  ( 2.900000000000000265E-14, -2.000000000000000155E-15, 1.000000000000000000 ) ) ;
#40709 = AXIS2_PLACEMENT_3D ( 'NONE', #51772, #79523, #15947 ) ;
#40710 = CARTESIAN_POINT ( 'NONE',  ( 106.5667039024470171, -94.77844715994206126, -19.78219314458232247 ) ) ;
#40712 = ORIENTED_EDGE ( 'NONE', *, *, #20798, .F. ) ;
#40711 = CARTESIAN_POINT ( 'NONE',  ( 106.9399074540173871, -47.82885535071048366, 232.5794347997199907 ) ) ;
#40713 = CARTESIAN_POINT ( 'NONE',  ( 115.6649034994425307, -31.56786279214498947, 194.2562958305554162 ) ) ;
#40714 = CARTESIAN_POINT ( 'NONE',  ( 111.1289525437170056, -47.00905435842401658, 18.88800622829195319 ) ) ;
#40715 = CARTESIAN_POINT ( 'NONE',  ( 116.7009037750506053, -40.82467873942847802, 164.5070538473399608 ) ) ;
#40716 = CARTESIAN_POINT ( 'NONE',  ( 112.1393455939420249, -28.01282275174989422, 30.65645861365223723 ) ) ;
#40717 = LINE ( 'NONE', #76137, #48913 ) ;
#40719 = FACE_OUTER_BOUND ( 'NONE', #70777, .T. ) ;
#40718 = LINE ( 'NONE', #19391, #82636 ) ;
#40720 = CARTESIAN_POINT ( 'NONE',  ( 109.7248659574642318, -27.00080519035325111, 189.8647919396041459 ) ) ;
#40721 = DIRECTION ( 'NONE',  ( 1.000000000000000000, 0.000000000000000000, 2.108231265501709878E-16 ) ) ;
#40722 = ORIENTED_EDGE ( 'NONE', *, *, #86004, .T. ) ;
#40723 = AXIS2_PLACEMENT_3D ( 'NONE', #87741, #74555, #86413 ) ;
#40724 = VERTEX_POINT ( 'NONE', #78065 ) ;
#40725 = ORIENTED_EDGE ( 'NONE', *, *, #58740, .T. ) ;
#40726 = CIRCLE ( 'NONE', #52298, 15.69999999999999041 ) ;
#40727 = EDGE_LOOP ( 'NONE', ( #57203, #12628, #70593, #2832 ) ) ;
#40728 = DIRECTION ( 'NONE',  ( 0.000000000000000000, 1.000000000000000000, 0.000000000000000000 ) ) ;
#40729 = CARTESIAN_POINT ( 'NONE',  ( 112.1705331031350283, -27.62378402076942763, 30.66991099019694644 ) ) ;
#40730 = DIRECTION ( 'NONE',  ( 0.000000000000000000, 0.000000000000000000, -1.000000000000000000 ) ) ;
#40731 = DIRECTION ( 'NONE',  ( 3.999999999999999995E-14, -1.000000000000000000, 4.100000000000000342E-29 ) ) ;
#40732 = DIRECTION ( 'NONE',  ( -0.000000000000000000, -1.000000000000000000, 0.000000000000000000 ) ) ;
#40733 = CARTESIAN_POINT ( 'NONE',  ( 98.55846751192062527, -35.97459669770627499, 230.6781341137909465 ) ) ;
#40734 = EDGE_LOOP ( 'NONE', ( #11605, #43279, #83406, #82299 ) ) ;
#40735 = ORIENTED_EDGE ( 'NONE', *, *, #71436, .F. ) ;
#40736 = ORIENTED_EDGE ( 'NONE', *, *, #85310, .T. ) ;
#40737 = EDGE_CURVE ( 'NONE', #72283, #86684, #35805, .T. ) ;
#40738 = FACE_OUTER_BOUND ( 'NONE', #56783, .T. ) ;
#40739 = CARTESIAN_POINT ( 'NONE',  ( 114.5914593468340712, -43.34783535320182324, 183.2524815427824763 ) ) ;
#40740 = DIRECTION ( 'NONE',  ( 0.000000000000000000, 0.000000000000000000, 1.000000000000000000 ) ) ;
#40741 = DIRECTION ( 'NONE',  ( 0.000000000000000000, 0.000000000000000000, -1.000000000000000000 ) ) ;
#40742 = AXIS2_PLACEMENT_3D ( 'NONE', #22829, #77788, #77331 ) ;
#40743 = DIRECTION ( 'NONE',  ( -4.237773401492740281E-14, 1.000000000000000000, 0.000000000000000000 ) ) ;
#40744 = ADVANCED_FACE ( 'NONE', ( #53425 ), #31671, .T. ) ;
#40745 = CIRCLE ( 'NONE', #39320, 3.999999999999992895 ) ;
#40746 = LINE ( 'NONE', #68470, #36106 ) ;
#40747 = CARTESIAN_POINT ( 'NONE',  ( 115.4101910119110386, -30.57141770992054219, 259.3203871806734355 ) ) ;
#40748 = VECTOR ( 'NONE', #35248, 1000.000000000000000 ) ;
#40749 = CARTESIAN_POINT ( 'NONE',  ( -254.0000000000000000, 93.66249999999999432, 85.72499999999999432 ) ) ;
#40750 = EDGE_CURVE ( 'NONE', #35831, #24268, #79275, .T. ) ;
#40751 = ORIENTED_EDGE ( 'NONE', *, *, #55906, .F. ) ;
#40752 = EDGE_CURVE ( 'NONE', #48213, #28502, #55224, .T. ) ;
#40753 = CARTESIAN_POINT ( 'NONE',  ( 34.33598329127499227, -36.32844715994100682, -5.074374724088000832 ) ) ;
#40754 = VECTOR ( 'NONE', #44218, 1000.000000000000000 ) ;
#40755 = CYLINDRICAL_SURFACE ( 'NONE', #45169, 12.70000000000000107 ) ;
#40756 = CARTESIAN_POINT ( 'NONE',  ( 112.7718126367562093, -42.56716444297848767, 71.01094751244896486 ) ) ;
#40757 = ADVANCED_FACE ( 'NONE', ( #62511 ), #55661, .F. ) ;
#40758 = AXIS2_PLACEMENT_3D ( 'NONE', #82714, #41779, #63140 ) ;
#40759 = PLANE ( 'NONE',  #30538 ) ;
#40760 = ADVANCED_FACE ( 'NONE', ( #82982, #69335 ), #47521, .F. ) ;
#40761 = FACE_OUTER_BOUND ( 'NONE', #11826, .T. ) ;
#40762 = CARTESIAN_POINT ( 'NONE',  ( 100.9546728091797974, -28.70702572886692039, 45.59395860945408430 ) ) ;
#40763 = ORIENTED_EDGE ( 'NONE', *, *, #28672, .F. ) ;
#40764 = CARTESIAN_POINT ( 'NONE',  ( 79.87807227644366037, -33.97944715994105991, 8.225625275910942946 ) ) ;
#40765 = ORIENTED_EDGE ( 'NONE', *, *, #58407, .T. ) ;
#40766 = CARTESIAN_POINT ( 'NONE',  ( 108.9452245070828411, -26.43885738637160543, 164.9327681330529742 ) ) ;
#40767 = EDGE_LOOP ( 'NONE', ( #60321, #86847, #81287, #37629 ) ) ;
#40768 = EDGE_CURVE ( 'NONE', #53177, #64680, #82493, .T. ) ;
#40769 = VECTOR ( 'NONE', #69705, 1000.000000000000000 ) ;
#40770 = CARTESIAN_POINT ( 'NONE',  ( 97.98128717666138243, -40.91104618832473250, 87.66925762342037842 ) ) ;
#40771 = CARTESIAN_POINT ( 'NONE',  ( 99.53176374547611260, -42.34233651421938305, 108.2796785439919773 ) ) ;
#40772 = CARTESIAN_POINT ( 'NONE',  ( -11.39384497175739064, 88.17529471328431612, 118.0073914794113819 ) ) ;
#40773 = CARTESIAN_POINT ( 'NONE',  ( 112.7927988201233944, -69.16395658370822730, 247.7076816059330042 ) ) ;
#40774 = CARTESIAN_POINT ( 'NONE',  ( 107.8700274897790479, -26.31351822515222949, 66.01562527591097762 ) ) ;
#40775 = VECTOR ( 'NONE', #34003, 1000.000000000000000 ) ;
#40776 = CARTESIAN_POINT ( 'NONE',  ( 109.6428311413115750, -46.48013238632621125, 257.7813333649102105 ) ) ;
#40777 = VERTEX_POINT ( 'NONE', #13034 ) ;
#40778 = LINE ( 'NONE', #68502, #1934 ) ;
#40779 = ORIENTED_EDGE ( 'NONE', *, *, #24991, .T. ) ;
#40780 = ORIENTED_EDGE ( 'NONE', *, *, #67005, .F. ) ;
#40781 = AXIS2_PLACEMENT_3D ( 'NONE', #84975, #28640, #21846 ) ;
#40782 = EDGE_CURVE ( 'NONE', #10976, #79006, #40717, .T. ) ;
#40783 = DIRECTION ( 'NONE',  ( 0.000000000000000000, 0.000000000000000000, -1.000000000000000000 ) ) ;
#40784 = VERTEX_POINT ( 'NONE', #289 ) ;
#40785 = CARTESIAN_POINT ( 'NONE',  ( 116.8470136369842720, -36.79772195930841150, 263.8213395616257912 ) ) ;
#40786 = CARTESIAN_POINT ( 'NONE',  ( 112.1306244020896941, -47.47080300746646486, 133.9270538473399768 ) ) ;
#40787 = ADVANCED_FACE ( 'NONE', ( #33906 ), #61600, .F. ) ;
#40788 = CARTESIAN_POINT ( 'NONE',  ( 104.0667030381796963, -70.87844715994094713, 93.21780742166239975 ) ) ;
#40789 = CARTESIAN_POINT ( 'NONE',  ( 98.34985891780978307, -31.65658480061700430, 141.9064586084259645 ) ) ;
#40790 = CARTESIAN_POINT ( 'NONE',  ( 98.33631928459364246, -42.42740502779041378, 97.78705384733993355 ) ) ;
#40791 = VECTOR ( 'NONE', #31653, 1000.000000000000000 ) ;
#40793 = EDGE_CURVE ( 'NONE', #64462, #11195, #27101, .T. ) ;
#40792 = CARTESIAN_POINT ( 'NONE',  ( 41.56648329127399677, -18.82844715994099971, 316.8086252759120498 ) ) ;
#40794 = ORIENTED_EDGE ( 'NONE', *, *, #41066, .F. ) ;
#40795 = DIRECTION ( 'NONE',  ( -0.7071067811865758834, 0.7071067811865192621, -2.899137802864845566E-29 ) ) ;
#40796 = EDGE_CURVE ( 'NONE', #31578, #12738, #82540, .T. ) ;
#40797 = CARTESIAN_POINT ( 'NONE',  ( 107.0664832912739399, -36.72944715994095333, 357.5272416190308604 ) ) ;
#40798 = EDGE_LOOP ( 'NONE', ( #57995, #77158, #11125, #63469 ) ) ;
#40799 = LINE ( 'NONE', #88075, #44559 ) ;
#40800 = CARTESIAN_POINT ( 'NONE',  ( 96.67439905703392355, -92.77844715994214653, -21.78219314458237932 ) ) ;
#40801 = CARTESIAN_POINT ( 'NONE',  ( 113.7419942178973287, -29.10023054337252546, 289.5032443235301116 ) ) ;
#40802 = CYLINDRICAL_SURFACE ( 'NONE', #1067, 3.499999999999996003 ) ;
#40803 = CARTESIAN_POINT ( 'NONE',  ( 80.06648329127399677, 0.2215528400590013880, 308.6356252759119911 ) ) ;
#40804 = CARTESIAN_POINT ( 'NONE',  ( 45.76696975232907505, -48.62818131005967359, 249.9678068554150343 ) ) ;
#40805 = CARTESIAN_POINT ( 'NONE',  ( 105.2812310726300922, -46.37359664056156561, 12.42991099019696932 ) ) ;
#40807 = CARTESIAN_POINT ( 'NONE',  ( 116.5783909117431136, -29.70293872869714846, 105.3327681330539463 ) ) ;
#40806 = CARTESIAN_POINT ( 'NONE',  ( 115.6667067228004129, -31.57200485274490376, 99.25677482824653453 ) ) ;
#40808 = CARTESIAN_POINT ( 'NONE',  ( 0.000000000000000000, 20.32000000000000028, 0.000000000000000000 ) ) ;
#40809 = CARTESIAN_POINT ( 'NONE',  ( 98.24359417337518607, -31.02780217081950909, 145.8699109901969848 ) ) ;
#40810 = DIRECTION ( 'NONE',  ( -0.8660254037844382635, -0.5000000000000008882, 1.550000000000000022E-14 ) ) ;
#40811 = ORIENTED_EDGE ( 'NONE', *, *, #28361, .F. ) ;
#40812 = CARTESIAN_POINT ( 'NONE',  ( -479.3614999999999782, 53.97500000000000142, 50.79999999999999716 ) ) ;
#40813 = VECTOR ( 'NONE', #70455, 1000.000000000000000 ) ;
#40814 = CARTESIAN_POINT ( 'NONE',  ( 82.81648329127402519, -36.72944715994107412, -5.074374724089055100 ) ) ;
#40815 = DIRECTION ( 'NONE',  ( 0.000000000000000000, -1.000000000000000000, -1.365923996832131856E-16 ) ) ;
#40816 = ORIENTED_EDGE ( 'NONE', *, *, #30250, .F. ) ;
#40817 = DIRECTION ( 'NONE',  ( 1.639958061481212836E-42, -4.100000000000000342E-29, -1.000000000000000000 ) ) ;
#40819 = ORIENTED_EDGE ( 'NONE', *, *, #32422, .F. ) ;
#40818 = CARTESIAN_POINT ( 'NONE',  ( 102.2925893952339749, -26.70832846991215703, 140.4422919425769578 ) ) ;
#40820 = LINE ( 'NONE', #82188, #4481 ) ;
#40821 = CARTESIAN_POINT ( 'NONE',  ( -130.5401660959919354, 95.08644067748863904, -2.073645319394354036 ) ) ;
#40822 = CIRCLE ( 'NONE', #39459, 2.116999999999993776 ) ;
#40823 = CARTESIAN_POINT ( 'NONE',  ( 52.38749999999999574, 94.53880000000000905, 229.3937500000000114 ) ) ;
#40824 = CARTESIAN_POINT ( 'NONE',  ( 32.06670390244800473, -32.29483332968611364, -5.074374724088000832 ) ) ;
#40825 = EDGE_LOOP ( 'NONE', ( #3082, #49952, #26685, #22722 ) ) ;
#40826 = VERTEX_POINT ( 'NONE', #6655 ) ;
#40827 = ORIENTED_EDGE ( 'NONE', *, *, #27173, .F. ) ;
#40828 = ORIENTED_EDGE ( 'NONE', *, *, #20945, .T. ) ;
#40829 = CARTESIAN_POINT ( 'NONE',  ( 19.56648329127400032, 0.2215528400590013880, -5.074374724088000832 ) ) ;
#40830 = CARTESIAN_POINT ( 'NONE',  ( 90.25311968877677771, 94.92443974548206143, -94.33669211993671411 ) ) ;
#40831 = CARTESIAN_POINT ( 'NONE',  ( 117.0718954874996172, -35.46248236767254980, 158.9272919416701200 ) ) ;
#40832 = CARTESIAN_POINT ( 'NONE',  ( 72.25757238336808541, -1.944390235229867425, 361.9756252759101471 ) ) ;
#40833 = AXIS2_PLACEMENT_3D ( 'NONE', #45320, #9482, #2680 ) ;
#40835 = CARTESIAN_POINT ( 'NONE',  ( -4.880114330320866500, 70.80325516146916698, -118.4573640576558660 ) ) ;
#40834 = CARTESIAN_POINT ( 'NONE',  ( 56.06670390244699576, -67.87844715994098976, 120.2178068554179902 ) ) ;
#40836 = DIRECTION ( 'NONE',  ( 0.000000000000000000, 0.000000000000000000, -1.000000000000000000 ) ) ;
#40837 = ORIENTED_EDGE ( 'NONE', *, *, #84078, .T. ) ;
#40838 = ORIENTED_EDGE ( 'NONE', *, *, #10212, .F. ) ;
#40839 = DIRECTION ( 'NONE',  ( 0.000000000000000000, 0.000000000000000000, -1.000000000000000000 ) ) ;
#40840 = CARTESIAN_POINT ( 'NONE',  ( 107.0664832912739399, -36.72944715994095333, 315.6356252759111953 ) ) ;
#40841 = EDGE_CURVE ( 'NONE', #58498, #64389, #31562, .T. ) ;
#40842 = CARTESIAN_POINT ( 'NONE',  ( 97.17009264939177626, -31.66255117090388538, 241.9499109901959741 ) ) ;
#40843 = AXIS2_PLACEMENT_3D ( 'NONE', #70319, #377, #43485 ) ;
#40844 = CARTESIAN_POINT ( 'NONE',  ( 223.2659999999999911, 52.73749999999999716, -55.11800000000000210 ) ) ;
#40845 = EDGE_CURVE ( 'NONE', #78707, #14442, #86689, .T. ) ;
#40846 = CARTESIAN_POINT ( 'NONE',  ( 99.96923091713372855, -43.45941328387849723, 77.92991099019597812 ) ) ;
#40847 = CARTESIAN_POINT ( 'NONE',  ( 113.2129946629323882, -44.63276428892469028, 53.10250874954972033 ) ) ;
#40848 = AXIS2_PLACEMENT_3D ( 'NONE', #81177, #53857, #76123 ) ;
#40849 = CARTESIAN_POINT ( 'NONE',  ( 103.9512555245577659, -27.22114335906981708, 21.32843223802335331 ) ) ;
#40850 = ADVANCED_FACE ( 'NONE', ( #57029 ), #64317, .F. ) ;
#40851 = ORIENTED_EDGE ( 'NONE', *, *, #43316, .T. ) ;
#40852 = DIRECTION ( 'NONE',  ( 1.000000000000000000, 1.000000000000000078E-15, -0.000000000000000000 ) ) ;
#40853 = EDGE_CURVE ( 'NONE', #52054, #16163, #29791, .T. ) ;
#40854 = VERTEX_POINT ( 'NONE', #8917 ) ;
#40855 = ORIENTED_EDGE ( 'NONE', *, *, #29915, .F. ) ;
#40856 = DIRECTION ( 'NONE',  ( 0.000000000000000000, 1.000000000000000000, 0.000000000000000000 ) ) ;
#40857 = CARTESIAN_POINT ( 'NONE',  ( 100.5340721669357009, -30.74146890971161739, 272.1672975916113160 ) ) ;
#40858 = EDGE_CURVE ( 'NONE', #78957, #46739, #85230, .T. ) ;
#40859 = CARTESIAN_POINT ( 'NONE',  ( 121.3178890780284291, -95.01002112898649443, -11.78219314458228695 ) ) ;
#40860 = FACE_OUTER_BOUND ( 'NONE', #15648, .T. ) ;
#40861 = ADVANCED_FACE ( 'NONE', ( #50214 ), #49318, .F. ) ;
#40862 = CARTESIAN_POINT ( 'NONE',  ( -40.89999999999999858, 53.97500000000000142, 40.79999999999999716 ) ) ;
#40863 = CARTESIAN_POINT ( 'NONE',  ( 81.24991378862220870, -39.21189172704054471, 1.845048092478625001 ) ) ;
#40865 = ORIENTED_EDGE ( 'NONE', *, *, #56626, .T. ) ;
#40864 = AXIS2_PLACEMENT_3D ( 'NONE', #48863, #1195, #64756 ) ;
#40866 = DIRECTION ( 'NONE',  ( 0.000000000000000000, -1.000000000000000000, 0.000000000000000000 ) ) ;
#40867 = CARTESIAN_POINT ( 'NONE',  ( 34.96670390244745619, -26.71338133339230581, 237.4678068554150059 ) ) ;
#40868 = ORIENTED_EDGE ( 'NONE', *, *, #74317, .F. ) ;
#40869 = CARTESIAN_POINT ( 'NONE',  ( 110.7945467183388502, -46.46538951521414873, 62.86705384733992474 ) ) ;
#40870 = ORIENTED_EDGE ( 'NONE', *, *, #3907, .T. ) ;
#40871 = CARTESIAN_POINT ( 'NONE',  ( 115.2284764178246661, -36.04786338006340429, 251.7109475124485414 ) ) ;
#40872 = EDGE_CURVE ( 'NONE', #18180, #25402, #15720, .T. ) ;
#40873 = FACE_BOUND ( 'NONE', #10765, .T. ) ;
#40874 = CARTESIAN_POINT ( 'NONE',  ( 101.2684584845351736, -45.32493232151070828, 152.0918157521019509 ) ) ;
#40875 = CARTESIAN_POINT ( 'NONE',  ( 23.30821534676788787, 78.76419614706141203, 305.8009406276586333 ) ) ;
#40876 = LINE ( 'NONE', #12295, #51956 ) ;
#40877 = CARTESIAN_POINT ( 'NONE',  ( 80.06648329127399677, -8.350947159940998787, 311.1531252759119752 ) ) ;
#40878 = VECTOR ( 'NONE', #4867, 1000.000000000000000 ) ;
#40879 = DIRECTION ( 'NONE',  ( 1.000000000000000078E-15, 1.000000000000000083E-30, -1.000000000000000000 ) ) ;
#40880 = ADVANCED_FACE ( 'NONE', ( #9789 ), #2539, .F. ) ;
#40881 = CARTESIAN_POINT ( 'NONE',  ( 101.6280127420326522, -45.67461444920139257, 243.1413395616249886 ) ) ;
#40882 = PLANE ( 'NONE',  #71806 ) ;
#40883 = ORIENTED_EDGE ( 'NONE', *, *, #30020, .T. ) ;
#40884 = CIRCLE ( 'NONE', #48133, 4.874999999999990230 ) ;
#40885 = CARTESIAN_POINT ( 'NONE',  ( 113.3408031569382644, -28.30502284670691182, 100.5670538473389684 ) ) ;
#40886 = LINE ( 'NONE', #49485, #23670 ) ;
#40887 = EDGE_LOOP ( 'NONE', ( #80566, #10107 ) ) ;
#40888 = VERTEX_POINT ( 'NONE', #36616 ) ;
#40889 = ORIENTED_EDGE ( 'NONE', *, *, #18028, .T. ) ;
#40890 = DIRECTION ( 'NONE',  ( -3.100000000000000258E-29, 3.100000000000000044E-14, 1.000000000000000000 ) ) ;
#40891 = CARTESIAN_POINT ( 'NONE',  ( 33.78129701732998313, -35.65087443492610930, -5.074374724088000832 ) ) ;
#40892 = CARTESIAN_POINT ( 'NONE',  ( 80.06648329127399677, 0.2215528400590013880, 291.1181252759119502 ) ) ;
#40893 = CARTESIAN_POINT ( 'NONE',  ( 63.03715912545729338, -24.42818131006027826, 313.9678068554150059 ) ) ;
#40894 = CARTESIAN_POINT ( 'NONE',  ( 103.1394548971403680, -44.44173430692483606, 170.0318998934009755 ) ) ;
#40895 = CARTESIAN_POINT ( 'NONE',  ( 106.8359569501641744, -47.17378133968975362, 268.5584824187679374 ) ) ;
#40896 = VECTOR ( 'NONE', #10706, 1000.000000000000000 ) ;
#40898 = ADVANCED_FACE ( 'NONE', ( #1192 ), #44286, .T. ) ;
#40897 = CARTESIAN_POINT ( 'NONE',  ( 99.08953455931535359, -42.79546436554615241, 57.84391660217934827 ) ) ;
#40899 = VERTEX_POINT ( 'NONE', #85224 ) ;
#40900 = CARTESIAN_POINT ( 'NONE',  ( 130.2872239869710427, 92.11674985319544362, -8.393624206580007296 ) ) ;
#40901 = EDGE_CURVE ( 'NONE', #25043, #43140, #12710, .T. ) ;
#40902 = CYLINDRICAL_SURFACE ( 'NONE', #85340, 10.00000000000002665 ) ;
#40903 = ORIENTED_EDGE ( 'NONE', *, *, #87419, .T. ) ;
#40905 = EDGE_LOOP ( 'NONE', ( #12355, #86620 ) ) ;
#40904 = CIRCLE ( 'NONE', #22075, 3.299999999999997158 ) ;
#40906 = VECTOR ( 'NONE', #33538, 1000.000000000000000 ) ;
#40907 = DIRECTION ( 'NONE',  ( 1.000000000000000000, 0.000000000000000000, 0.000000000000000000 ) ) ;
#40908 = VERTEX_POINT ( 'NONE', #28902 ) ;
#40909 = ORIENTED_EDGE ( 'NONE', *, *, #46420, .F. ) ;
#40910 = PLANE ( 'NONE',  #38189 ) ;
#40911 = CARTESIAN_POINT ( 'NONE',  ( -8.398107354775891764, 72.98722500879387098, -130.2869324835649536 ) ) ;
#40912 = DIRECTION ( 'NONE',  ( 1.000000000000000078E-15, 0.000000000000000000, 1.000000000000000000 ) ) ;
#40913 = DIRECTION ( 'NONE',  ( 0.000000000000000000, 0.000000000000000000, 1.000000000000000000 ) ) ;
#40914 = CARTESIAN_POINT ( 'NONE',  ( 115.9692459539148643, -35.07008363779494431, 203.4076579233149573 ) ) ;
#40915 = AXIS2_PLACEMENT_3D ( 'NONE', #42931, #2074, #15708 ) ;
#40916 = CARTESIAN_POINT ( 'NONE',  ( 118.0351107906133876, -38.43300062509310067, 68.69181575210198787 ) ) ;
#40917 = LINE ( 'NONE', #5976, #72764 ) ;
#40918 = ORIENTED_EDGE ( 'NONE', *, *, #33860, .T. ) ;
#40919 = DIRECTION ( 'NONE',  ( 1.000000000000000000, -6.745093096447288888E-17, -4.496403249731880833E-15 ) ) ;
#40920 = VECTOR ( 'NONE', #53303, 1000.000000000000000 ) ;
#40921 = ORIENTED_EDGE ( 'NONE', *, *, #26709, .T. ) ;
#40922 = LINE ( 'NONE', #47729, #78064 ) ;
#40923 = ORIENTED_EDGE ( 'NONE', *, *, #40555, .T. ) ;
#40924 = DIRECTION ( 'NONE',  ( 0.000000000000000000, -3.785359618865284342E-16, -1.000000000000000000 ) ) ;
#40925 = CARTESIAN_POINT ( 'NONE',  ( 127.4153857849114644, -122.7425179094934151, 250.2203867545820231 ) ) ;
#40926 = CARTESIAN_POINT ( 'NONE',  ( 182.2300522401149863, -33.89581943344511217, -5.074374724088000832 ) ) ;
#40927 = ADVANCED_FACE ( 'NONE', ( #42498 ), #71138, .F. ) ;
#40928 = DIRECTION ( 'NONE',  ( 0.000000000000000000, 1.000000000000000000, 0.000000000000000000 ) ) ;
#40929 = ORIENTED_EDGE ( 'NONE', *, *, #32043, .T. ) ;
#40930 = CARTESIAN_POINT ( 'NONE',  ( 106.9270552135175620, -26.24760940922973163, 60.08705384733897858 ) ) ;
#40931 =( BOUNDED_CURVE ( )  B_SPLINE_CURVE ( 3, ( #55585, #48782, #7023, #48324 ),
 .UNSPECIFIED., .F., .T. ) 
 B_SPLINE_CURVE_WITH_KNOTS ( ( 4, 4 ),
 ( 0.000000000000000000, 0.4701579599232050821 ),
 .UNSPECIFIED. ) 
 CURVE ( )  GEOMETRIC_REPRESENTATION_ITEM ( )  RATIONAL_B_SPLINE_CURVE ( ( 1.000000000000000000, 0.9816639655796102204, 0.9816639655796102204, 1.000000000000000000 ) ) 
 REPRESENTATION_ITEM ( '' )  );
#40933 = LINE ( 'NONE', #13246, #29806 ) ;
#40932 = CARTESIAN_POINT ( 'NONE',  ( 160.7738106836348209, -48.62134037874901082, 300.4678068554149490 ) ) ;
#40934 = DIRECTION ( 'NONE',  ( 0.000000000000000000, 0.000000000000000000, -1.000000000000000000 ) ) ;
#40935 = CARTESIAN_POINT ( 'NONE',  ( 41.56648329127399677, -18.82844715994099971, 18.92562527591200094 ) ) ;
#40936 = ORIENTED_EDGE ( 'NONE', *, *, #27978, .F. ) ;
#40937 = CIRCLE ( 'NONE', #54007, 2.117000000000007987 ) ;
#40938 = CARTESIAN_POINT ( 'NONE',  ( 69.56670390244704549, -118.2784471599409812, 51.21780685541800437 ) ) ;
#40939 = DIRECTION ( 'NONE',  ( -0.000000000000000000, 1.000000000000000000, -0.000000000000000000 ) ) ;
#40940 = CARTESIAN_POINT ( 'NONE',  ( 12.69999999999999929, 81.71107837960109066, 117.8738102209307499 ) ) ;
#40941 = EDGE_LOOP ( 'NONE', ( #62575, #78316, #44196, #34592, #5090 ) ) ;
#40942 = CARTESIAN_POINT ( 'NONE',  ( 103.8345913547307333, -46.70111052772084292, 78.32705384733995402 ) ) ;
#40943 = CIRCLE ( 'NONE', #88824, 0.5000000000000004441 ) ;
#40945 = DIRECTION ( 'NONE',  ( 0.000000000000000000, 0.000000000000000000, -1.000000000000000000 ) ) ;
#40944 = PLANE ( 'NONE',  #1502 ) ;
#40946 = DIRECTION ( 'NONE',  ( 0.000000000000000000, 0.4999999999999994449, -0.8660254037844389297 ) ) ;
#40947 = EDGE_CURVE ( 'NONE', #22043, #84439, #23442, .T. ) ;
#40948 = CIRCLE ( 'NONE', #33700, 2.029999999999997140 ) ;
#40949 = EDGE_CURVE ( 'NONE', #11998, #36895, #56119, .T. ) ;
#40950 = CARTESIAN_POINT ( 'NONE',  ( 140.3886392338172300, -80.20257156670452048, 248.3919668373590071 ) ) ;
#40951 = ORIENTED_EDGE ( 'NONE', *, *, #56137, .T. ) ;
#40952 = EDGE_CURVE ( 'NONE', #60508, #54515, #84329, .T. ) ;
#40953 = CARTESIAN_POINT ( 'NONE',  ( 108.4956486572523602, -46.43878675094416764, 138.6927681330529936 ) ) ;
#40955 = ORIENTED_EDGE ( 'NONE', *, *, #5522, .T. ) ;
#40954 = CARTESIAN_POINT ( 'NONE',  ( 34.96670390244699433, -26.71338133339301635, -5.074374724088000832 ) ) ;
#40956 = EDGE_CURVE ( 'NONE', #52594, #51252, #49764, .T. ) ;
#40957 = CARTESIAN_POINT ( 'NONE',  ( 118.6297112294782892, -39.20734283244433982, 254.6584824187681022 ) ) ;
#40958 = PLANE ( 'NONE',  #71573 ) ;
#40959 = CARTESIAN_POINT ( 'NONE',  ( 74.15067561874269586, 120.6499999999999915, -68.53801554307419508 ) ) ;
#40960 = DIRECTION ( 'NONE',  ( -0.000000000000000000, 1.000000000000000000, 0.000000000000000000 ) ) ;
#40961 = CARTESIAN_POINT ( 'NONE',  ( 115.0889047229540836, -30.61763667849448822, 45.34395860938102629 ) ) ;
#40962 = AXIS2_PLACEMENT_3D ( 'NONE', #73268, #52354, #60991 ) ;
#40963 = CARTESIAN_POINT ( 'NONE',  ( 44.45000000000000284, 69.84999999999999432, 219.0749999999999886 ) ) ;
#40964 = EDGE_CURVE ( 'NONE', #72082, #47060, #57932, .T. ) ;
#40965 = LINE ( 'NONE', #56379, #23953 ) ;
#40966 = CARTESIAN_POINT ( 'NONE',  ( 98.33750497493203113, -41.21483588869663350, 196.7041967044829676 ) ) ;
#40967 = ORIENTED_EDGE ( 'NONE', *, *, #89737, .T. ) ;
#40968 = ORIENTED_EDGE ( 'NONE', *, *, #2900, .T. ) ;
#40969 = CARTESIAN_POINT ( 'NONE',  ( 109.1422557193553047, -45.34451810791325954, 129.1958690201829825 ) ) ;
#40970 = EDGE_CURVE ( 'NONE', #41295, #79108, #19969, .T. ) ;
#40971 = CIRCLE ( 'NONE', #65675, 7.873999999999991672 ) ;
#40972 = CARTESIAN_POINT ( 'NONE',  ( 24.79284581386643183, 127.0000000000000000, 90.32146847885336172 ) ) ;
#40974 = DIRECTION ( 'NONE',  ( 0.000000000000000000, 1.000000000000000000, 0.000000000000000000 ) ) ;
#40973 = CARTESIAN_POINT ( 'NONE',  ( 101.5279499456468528, -29.13990343739101974, 26.99777378208800727 ) ) ;
#40975 = DIRECTION ( 'NONE',  ( 1.000000000000000000, -1.025452301070031786E-14, 0.000000000000000000 ) ) ;
#40976 = EDGE_CURVE ( 'NONE', #46082, #61174, #78407, .T. ) ;
#40977 = CIRCLE ( 'NONE', #33787, 34.13125000000000142 ) ;
#40978 = DIRECTION ( 'NONE',  ( 1.000000000000000000, 0.000000000000000000, 0.000000000000000000 ) ) ;
#40979 = CARTESIAN_POINT ( 'NONE',  ( 24.79284581386629327, 184.0000000000000000, -3.384395586952189366E-14 ) ) ;
#40980 = DIRECTION ( 'NONE',  ( 1.000000000000000000, 2.999999999999999839E-15, 1.000000000000000078E-15 ) ) ;
#40981 = CARTESIAN_POINT ( 'NONE',  ( 107.0664832912739968, -36.72944715994100306, 287.6356252759109680 ) ) ;
#40982 = CARTESIAN_POINT ( 'NONE',  ( 117.4525030917818782, -36.13006561810994555, 228.8727681330539667 ) ) ;
#40983 = DIRECTION ( 'NONE',  ( 0.000000000000000000, -1.000000000000000000, 0.000000000000000000 ) ) ;
#40984 = ORIENTED_EDGE ( 'NONE', *, *, #89792, .F. ) ;
#40985 = EDGE_LOOP ( 'NONE', ( #28935, #11874, #66712, #43571 ) ) ;
#40986 = EDGE_CURVE ( 'NONE', #60225, #85887, #23875, .T. ) ;
#40987 = CARTESIAN_POINT ( 'NONE',  ( -89.08909376920014722, 70.66229531820913223, -95.43663006862824716 ) ) ;
#40988 = CARTESIAN_POINT ( 'NONE',  ( 80.06648281188262217, -21.47944715903999224, 8.225259175037979986 ) ) ;
#40989 = CARTESIAN_POINT ( 'NONE',  ( 105.8001629020714489, -26.72394735792939713, 185.1776961641718913 ) ) ;
#40990 = FACE_OUTER_BOUND ( 'NONE', #55327, .T. ) ;
#40991 = CYLINDRICAL_SURFACE ( 'NONE', #81863, 7.499999999999996447 ) ;
#40992 = ORIENTED_EDGE ( 'NONE', *, *, #75188, .F. ) ;
#40993 = CARTESIAN_POINT ( 'NONE',  ( -7.690723789128298016, 92.56496522704115648, 118.1078823055163838 ) ) ;
#40994 = CARTESIAN_POINT ( 'NONE',  ( 117.7765707488592710, -31.65652763686493998, 214.1784824187679419 ) ) ;
#40995 = VERTEX_POINT ( 'NONE', #65637 ) ;
#40996 = CIRCLE ( 'NONE', #1865, 5.599999999999994316 ) ;
#40997 = DIRECTION ( 'NONE',  ( -1.000000000000000078E-15, 0.000000000000000000, 1.000000000000000000 ) ) ;
#40998 = CARTESIAN_POINT ( 'NONE',  ( 34.67381068362099228, -26.00627455219321860, -5.074374724088000832 ) ) ;
#40999 = CARTESIAN_POINT ( 'NONE',  ( 111.0302909011776507, -45.91071616320562043, 167.9007897230142987 ) ) ;
#41000 = CARTESIAN_POINT ( 'NONE',  ( 112.0721450080970669, -44.54221119967598241, 65.84809036959194373 ) ) ;
#41001 = CARTESIAN_POINT ( 'NONE',  ( 118.9423443782970082, -36.92851767163586629, 149.8127681330539644 ) ) ;
#41002 = CARTESIAN_POINT ( 'NONE',  ( 0.000000000000000000, 101.5999999999999943, 130.5560000000000116 ) ) ;
#41003 = VERTEX_POINT ( 'NONE', #53316 ) ;
#41004 = EDGE_CURVE ( 'NONE', #26689, #63598, #18374, .T. ) ;
#41005 = DIRECTION ( 'NONE',  ( 0.2588190451025154659, 0.000000000000000000, 0.9659258262890696445 ) ) ;
#41006 = CARTESIAN_POINT ( 'NONE',  ( 98.13538023319908632, -41.23056087969936101, 66.69855942027353990 ) ) ;
#41007 = ORIENTED_EDGE ( 'NONE', *, *, #40010, .T. ) ;
#41008 = EDGE_LOOP ( 'NONE', ( #47788, #17536, #11487, #39449 ) ) ;
#41009 = VECTOR ( 'NONE', #5493, 1000.000000000000000 ) ;
#41010 = DIRECTION ( 'NONE',  ( 1.000000000000000000, 0.000000000000000000, 0.000000000000000000 ) ) ;
#41011 = EDGE_LOOP ( 'NONE', ( #64907, #25471, #62214 ) ) ;
#41012 = VERTEX_POINT ( 'NONE', #67415 ) ;
#41013 = CARTESIAN_POINT ( 'NONE',  ( 162.5667039024460223, -22.48495420874110806, 342.9256252759109884 ) ) ;
#41014 = CARTESIAN_POINT ( 'NONE',  ( 109.7746843348460857, -45.37110888865593239, 52.22861030426695095 ) ) ;
#41015 = CARTESIAN_POINT ( 'NONE',  ( 104.4049122349322545, -25.97716923158638735, 240.2575300378159682 ) ) ;
#41016 = CARTESIAN_POINT ( 'NONE',  ( 109.3321198358312074, -26.57584895156206173, 224.9013395616249511 ) ) ;
#41018 = CARTESIAN_POINT ( 'NONE',  ( 116.1393041698827346, -43.00708073170991952, 9.356577656862985037 ) ) ;
#41017 = CARTESIAN_POINT ( 'NONE',  ( 90.44969454456405344, -20.11243780205715481, 229.5838068554169809 ) ) ;
#41019 = DIRECTION ( 'NONE',  ( -0.9254794337955623007, -0.3787978585227819162, 0.000000000000000000 ) ) ;
#41020 = CARTESIAN_POINT ( 'NONE',  ( 52.38749999999999574, 94.53880000000000905, 225.4249999999999829 ) ) ;
#41021 = DIRECTION ( 'NONE',  ( 1.000000000000000000, 0.000000000000000000, 0.000000000000000000 ) ) ;
#41022 = EDGE_CURVE ( 'NONE', #15321, #10458, #87432, .T. ) ;
#41023 = ORIENTED_EDGE ( 'NONE', *, *, #67005, .T. ) ;
#41024 = ORIENTED_EDGE ( 'NONE', *, *, #65658, .T. ) ;
#41025 = CARTESIAN_POINT ( 'NONE',  ( 101.4370486012140020, -28.02035706366309853, 70.54514908543596619 ) ) ;
#41027 = EDGE_CURVE ( 'NONE', #59691, #23038, #63465, .T. ) ;
#41026 = TOROIDAL_SURFACE ( 'NONE', #51211, 9.000000000000007105, 1.000000000000000000 ) ;
#41028 = CARTESIAN_POINT ( 'NONE',  ( 113.5334051825838202, -28.49624685289517245, 79.54705384733995288 ) ) ;
#41029 = CARTESIAN_POINT ( 'NONE',  ( 115.6917119993852054, -30.73301325301421016, 279.3099109901964994 ) ) ;
#41030 = VERTEX_POINT ( 'NONE', #86991 ) ;
#41031 = CARTESIAN_POINT ( 'NONE',  ( 100.8231516252168234, -45.85084492350206631, 242.1108633711489517 ) ) ;
#41032 = DIRECTION ( 'NONE',  ( -1.000000000000000000, 0.000000000000000000, 0.000000000000000000 ) ) ;
#41033 = DIRECTION ( 'NONE',  ( 1.000000000000000000, 8.953411488912556626E-16, 0.000000000000000000 ) ) ;
#41034 = CIRCLE ( 'NONE', #49794, 17.00000000000000000 ) ;
#41035 = CARTESIAN_POINT ( 'NONE',  ( 21.03715912545824551, -47.82818131006186491, 300.4678068554150059 ) ) ;
#41036 = CARTESIAN_POINT ( 'NONE',  ( 0.000000000000000000, 95.25000000000000000, 0.000000000000000000 ) ) ;
#41038 = CARTESIAN_POINT ( 'NONE',  ( 120.0664832912739399, -36.72944715994095333, 294.6356252759106837 ) ) ;
#41037 = CARTESIAN_POINT ( 'NONE',  ( 98.24075285659111501, -36.10665116910172401, 277.6356252759110816 ) ) ;
#41039 = CARTESIAN_POINT ( 'NONE',  ( 97.82711386317197366, -40.55490885176772764, 172.6388511831666506 ) ) ;
#41040 = CARTESIAN_POINT ( 'NONE',  ( 141.3509999999999991, 20.32000000000000028, -141.3509999999999991 ) ) ;
#41041 = VECTOR ( 'NONE', #32169, 1000.000000000000000 ) ;
#41042 = CARTESIAN_POINT ( 'NONE',  ( 114.5988951105837259, -109.2045100507364594, 2.217806855418169576 ) ) ;
#41043 = CARTESIAN_POINT ( 'NONE',  ( 97.81168895331838087, -40.51742574516882200, 287.6356252759109680 ) ) ;
#41044 = CARTESIAN_POINT ( 'NONE',  ( 172.5664832912728457, -27.82844715994070484, 21.92562527591199739 ) ) ;
#41045 = FACE_OUTER_BOUND ( 'NONE', #30173, .T. ) ;
#41047 = VERTEX_POINT ( 'NONE', #24316 ) ;
#41046 = DIRECTION ( 'NONE',  ( -1.000000000000000000, -1.734723475976808672E-15, 0.000000000000000000 ) ) ;
#41048 = DIRECTION ( 'NONE',  ( 0.9659258262890704216, 0.000000000000000000, -0.2588190451025129124 ) ) ;
#41049 = CARTESIAN_POINT ( 'NONE',  ( 110.0583800183467957, -26.06436417334086642, 219.8708633711489711 ) ) ;
#41050 = CARTESIAN_POINT ( 'NONE',  ( 117.1259760753171548, -33.86829196857838298, 145.0470538473399529 ) ) ;
#41051 = CARTESIAN_POINT ( 'NONE',  ( 105.1008636489907673, -25.80544433381534475, 271.2061014663873380 ) ) ;
#41052 = FACE_OUTER_BOUND ( 'NONE', #18506, .T. ) ;
#41054 = CARTESIAN_POINT ( 'NONE',  ( 162.5667039024470171, -33.35206098992711077, -5.074374724088000832 ) ) ;
#41053 = DIRECTION ( 'NONE',  ( -1.000000000000000078E-15, 1.000000000000000083E-30, 1.000000000000000000 ) ) ;
#41055 = CYLINDRICAL_SURFACE ( 'NONE', #87126, 15.99999999999999822 ) ;
#41056 = CARTESIAN_POINT ( 'NONE',  ( 129.9388103550932669, 83.38002811471483255, 12.67976361810990760 ) ) ;
#41057 = AXIS2_PLACEMENT_3D ( 'NONE', #60380, #39939, #60830 ) ;
#41058 = EDGE_LOOP ( 'NONE', ( #18009, #15693, #81596, #26912 ) ) ;
#41059 = EDGE_LOOP ( 'NONE', ( #35650, #43789, #81980, #31784 ) ) ;
#41060 = ADVANCED_FACE ( 'NONE', ( #51982 ), #57627, .F. ) ;
#41061 = CARTESIAN_POINT ( 'NONE',  ( 103.1716831446340166, -28.55367798840643090, 139.8648007804579549 ) ) ;
#41063 = EDGE_LOOP ( 'NONE', ( #38381, #79527 ) ) ;
#41062 = CYLINDRICAL_SURFACE ( 'NONE', #83430, 27.49999999999999645 ) ;
#41064 = AXIS2_PLACEMENT_3D ( 'NONE', #50007, #15962, #71380 ) ;
#41065 = LINE ( 'NONE', #87891, #17012 ) ;
#41066 = EDGE_CURVE ( 'NONE', #54710, #59900, #59261, .T. ) ;
#41067 = CARTESIAN_POINT ( 'NONE',  ( 96.03721982003250446, -36.58408020053186505, 152.3280062282919971 ) ) ;
#41068 = CARTESIAN_POINT ( 'NONE',  ( 116.7940342761296932, -39.39171570160217328, 149.6152268520635857 ) ) ;
#41069 = EDGE_CURVE ( 'NONE', #55351, #24376, #53249, .T. ) ;
#41070 = PLANE ( 'NONE',  #38533 ) ;
#41071 = CARTESIAN_POINT ( 'NONE',  ( -86.12934247706235169, 70.27763793881260312, 81.47036787067852970 ) ) ;
#41072 = EDGE_CURVE ( 'NONE', #1305, #36080, #58375, .T. ) ;
#41073 = DIRECTION ( 'NONE',  ( 0.000000000000000000, 0.000000000000000000, -1.000000000000000000 ) ) ;
#41074 = CARTESIAN_POINT ( 'NONE',  ( 107.8912859324307334, -26.39220933555693094, 115.0251490854349612 ) ) ;
#41075 = EDGE_LOOP ( 'NONE', ( #18048, #20753 ) ) ;
#41076 = ORIENTED_EDGE ( 'NONE', *, *, #52461, .T. ) ;
#41077 = ORIENTED_EDGE ( 'NONE', *, *, #87574, .T. ) ;
#41078 = EDGE_CURVE ( 'NONE', #59338, #61529, #66977, .T. ) ;
#41079 = CARTESIAN_POINT ( 'NONE',  ( 150.5667039024485234, -47.82844715993594065, 180.4678068554149775 ) ) ;
#41081 = DIRECTION ( 'NONE',  ( 1.000000000000000000, 0.000000000000000000, 0.000000000000000000 ) ) ;
#41080 = CARTESIAN_POINT ( 'NONE',  ( 108.8290724220007206, -27.07506712556666173, 160.9327681330529742 ) ) ;
#41082 = CARTESIAN_POINT ( 'NONE',  ( 113.2462102393686081, -28.75921903332401541, 54.55156195206926384 ) ) ;
#41083 = LINE ( 'NONE', #82899, #40769 ) ;
#41084 = EDGE_CURVE ( 'NONE', #43582, #17076, #37341, .T. ) ;
#41085 = CYLINDRICAL_SURFACE ( 'NONE', #79417, 9.999999999999998224 ) ;
#41086 = PLANE ( 'NONE',  #37609 ) ;
#41087 = CARTESIAN_POINT ( 'NONE',  ( 67.28117739324572710, -68.08513503999283500, 246.4020950495498994 ) ) ;
#41088 = CARTESIAN_POINT ( 'NONE',  ( 109.6783822832554449, -47.44587409406599932, 87.75467289495897205 ) ) ;
#41089 = ORIENTED_EDGE ( 'NONE', *, *, #24666, .T. ) ;
#41090 = ORIENTED_EDGE ( 'NONE', *, *, #48221, .F. ) ;
#41091 = VERTEX_POINT ( 'NONE', #52419 ) ;
#41092 = LINE ( 'NONE', #19320, #2368 ) ;
#41093 = CARTESIAN_POINT ( 'NONE',  ( -84.90178614994256634, 90.29814575435203494, -99.18048580889426091 ) ) ;
#41094 = DIRECTION ( 'NONE',  ( 1.000000000000000078E-15, -1.000000000000000000, 0.000000000000000000 ) ) ;
#41095 = CARTESIAN_POINT ( 'NONE',  ( 105.0207293620135118, -28.82725652202227096, 198.0966617981629554 ) ) ;
#41096 = AXIS2_PLACEMENT_3D ( 'NONE', #77477, #83401, #7096 ) ;
#41097 = AXIS2_PLACEMENT_3D ( 'NONE', #81718, #26282, #19922 ) ;
#41098 = DIRECTION ( 'NONE',  ( -0.000000000000000000, -1.000000000000000000, 0.000000000000000000 ) ) ;
#41099 = ORIENTED_EDGE ( 'NONE', *, *, #81656, .T. ) ;
#41101 = EDGE_LOOP ( 'NONE', ( #8172, #21756, #41162, #67743 ) ) ;
#41100 = ORIENTED_EDGE ( 'NONE', *, *, #4259, .F. ) ;
#41102 = CARTESIAN_POINT ( 'NONE',  ( 46.48091746482126041, -48.32844715994084339, 300.4678068554150059 ) ) ;
#41103 = DIRECTION ( 'NONE',  ( -0.000000000000000000, 1.000000000000000000, 0.000000000000000000 ) ) ;
#41104 = EDGE_LOOP ( 'NONE', ( #39386, #77889, #13782, #52861 ) ) ;
#41105 = ORIENTED_EDGE ( 'NONE', *, *, #58108, .T. ) ;
#41106 = DIRECTION ( 'NONE',  ( 0.000000000000000000, 0.000000000000000000, -1.000000000000000000 ) ) ;
#41107 = CARTESIAN_POINT ( 'NONE',  ( 115.1751221500829701, -40.30411560180680652, 249.9272975916113637 ) ) ;
#41108 = ORIENTED_EDGE ( 'NONE', *, *, #77466, .T. ) ;
#41109 = ADVANCED_FACE ( 'NONE', ( #59697 ), #39707, .T. ) ;
#41110 = DIRECTION ( 'NONE',  ( -0.000000000000000000, 1.000000000000000000, 0.000000000000000000 ) ) ;
#41111 = CARTESIAN_POINT ( 'NONE',  ( -112.0489691580589096, 66.76700720547121648, 67.00851989138369902 ) ) ;
#41112 = ORIENTED_EDGE ( 'NONE', *, *, #21911, .T. ) ;
#41113 = ORIENTED_EDGE ( 'NONE', *, *, #80777, .T. ) ;
#41114 = DIRECTION ( 'NONE',  ( 1.000000000000000078E-15, 1.000000000000000083E-30, -1.000000000000000000 ) ) ;
#41115 = VECTOR ( 'NONE', #21661, 1000.000000000000000 ) ;
#41116 = ORIENTED_EDGE ( 'NONE', *, *, #567, .F. ) ;
#41117 = ORIENTED_EDGE ( 'NONE', *, *, #81409, .F. ) ;
#41118 = EDGE_CURVE ( 'NONE', #76706, #9747, #18833, .T. ) ;
#41119 = CARTESIAN_POINT ( 'NONE',  ( 112.3381529121750191, -29.09364788469061480, 237.4138046553059951 ) ) ;
#41121 = CARTESIAN_POINT ( 'NONE',  ( 96.00433110544545912, -37.29885927265511469, 121.3794347997209684 ) ) ;
#41120 = AXIS2_PLACEMENT_3D ( 'NONE', #13713, #68236, #6019 ) ;
#41122 = CARTESIAN_POINT ( 'NONE',  ( 116.5783909117432842, -29.70293872869703833, 109.3327681330539605 ) ) ;
#41123 = CARTESIAN_POINT ( 'NONE',  ( 108.1460423962843578, -44.98105793649955331, 249.5838068554170093 ) ) ;
#41124 = DIRECTION ( 'NONE',  ( 1.000000000000000078E-15, -1.000000000000000083E-30, -1.000000000000000000 ) ) ;
#41125 = CARTESIAN_POINT ( 'NONE',  ( 116.7952044851831488, -40.57305441194377948, 189.5270538473389479 ) ) ;
#41126 = CARTESIAN_POINT ( 'NONE',  ( 161.4809174648186172, -49.32844715993547169, 129.9678068554149775 ) ) ;
#41127 = ORIENTED_EDGE ( 'NONE', *, *, #2460, .T. ) ;
#41128 = CARTESIAN_POINT ( 'NONE',  ( -130.0906838859329184, 76.18750001922980175, 11.02255322708127849 ) ) ;
#41129 = ORIENTED_EDGE ( 'NONE', *, *, #40112, .T. ) ;
#41130 = ORIENTED_EDGE ( 'NONE', *, *, #18534, .F. ) ;
#41131 = CARTESIAN_POINT ( 'NONE',  ( 107.0664832912739968, -36.72944715994100306, 287.6356252759109680 ) ) ;
#41132 = EDGE_LOOP ( 'NONE', ( #45148, #80967 ) ) ;
#41133 = AXIS2_PLACEMENT_3D ( 'NONE', #54827, #82593, #20350 ) ;
#41134 = DIRECTION ( 'NONE',  ( -1.000000000000000000, 0.000000000000000000, 0.000000000000000000 ) ) ;
#41135 = EDGE_CURVE ( 'NONE', #42703, #2727, #9795, .T. ) ;
#41136 = CARTESIAN_POINT ( 'NONE',  ( 98.09668637883959263, -31.41627731406707724, 85.90133956162493689 ) ) ;
#41137 = CARTESIAN_POINT ( 'NONE',  ( -4.809187206306169138, 70.79577073431487122, 130.4673938299285396 ) ) ;
#41138 = CARTESIAN_POINT ( 'NONE',  ( -57.91199999999999903, 20.32000000000000028, 191.3008000794699797 ) ) ;
#41139 = DIRECTION ( 'NONE',  ( 1.000000000000000078E-15, 0.000000000000000000, -1.000000000000000000 ) ) ;
#41142 = CARTESIAN_POINT ( 'NONE',  ( 114.5897159479185490, -29.54407062678539830, 230.4327681330539690 ) ) ;
#41141 = DIRECTION ( 'NONE',  ( 0.000000000000000000, 0.000000000000000000, -1.000000000000000000 ) ) ;
#41140 = FACE_BOUND ( 'NONE', #75568, .T. ) ;
#41143 = DIRECTION ( 'NONE',  ( -0.7071067811865758834, 0.7071067811865192621, -7.071067811865765240E-16 ) ) ;
#41144 = CARTESIAN_POINT ( 'NONE',  ( 121.2221484686747459, -113.6057974291314423, -11.78219314458173272 ) ) ;
#41145 = ORIENTED_EDGE ( 'NONE', *, *, #43798, .F. ) ;
#41146 = FACE_OUTER_BOUND ( 'NONE', #53577, .T. ) ;
#41147 = FACE_OUTER_BOUND ( 'NONE', #7212, .T. ) ;
#41148 = CARTESIAN_POINT ( 'NONE',  ( -103.1875000000000000, 101.5999999999999943, -1.080832317973422076E-12 ) ) ;
#41149 = LINE ( 'NONE', #33453, #81107 ) ;
#41151 = ORIENTED_EDGE ( 'NONE', *, *, #20153, .T. ) ;
#41150 = CARTESIAN_POINT ( 'NONE',  ( 111.1446672340677111, -27.08708843538706645, 244.7584824187679544 ) ) ;
#41152 = CARTESIAN_POINT ( 'NONE',  ( -76.20505178924278766, 120.6499999999999915, -76.20505178924469192 ) ) ;
#41153 = CARTESIAN_POINT ( 'NONE',  ( 116.8162545570497741, -32.97600546270004429, 139.1184824187679396 ) ) ;
#41154 = CARTESIAN_POINT ( 'NONE',  ( 96.19318211390864803, -38.71572558720041712, 47.48229194257797303 ) ) ;
#41155 = CARTESIAN_POINT ( 'NONE',  ( 97.91841856125127208, -30.44371649139010927, 161.8594347997199918 ) ) ;
#41156 = CARTESIAN_POINT ( 'NONE',  ( 115.8254323877286822, -31.73001881851844530, 30.23979194345921684 ) ) ;
#41157 = CARTESIAN_POINT ( 'NONE',  ( 97.06382073701963975, -37.34192062437319493, 102.3751593848355270 ) ) ;
#41159 = DIRECTION ( 'NONE',  ( -0.9254794337955620787, -0.3787978585227822492, 0.000000000000000000 ) ) ;
#41158 = DIRECTION ( 'NONE',  ( 0.000000000000000000, -1.000000000000000000, 0.000000000000000000 ) ) ;
#41160 = CARTESIAN_POINT ( 'NONE',  ( 63.03715912545740707, -46.82818131006016671, 129.9678068554150911 ) ) ;
#41161 = DIRECTION ( 'NONE',  ( 0.7071067811865192621, 0.7071067811865758834, 7.071067811865186413E-16 ) ) ;
#41162 = ORIENTED_EDGE ( 'NONE', *, *, #63270, .T. ) ;
#41163 = AXIS2_PLACEMENT_3D ( 'NONE', #50202, #9778, #64741 ) ;
#41164 = VECTOR ( 'NONE', #68521, 1000.000000000000000 ) ;
#41165 = ORIENTED_EDGE ( 'NONE', *, *, #73855, .T. ) ;
#41166 = EDGE_LOOP ( 'NONE', ( #72398, #62109, #28479, #57236 ) ) ;
#41167 = EDGE_CURVE ( 'NONE', #16580, #68878, #10233, .T. ) ;
#41168 = ORIENTED_EDGE ( 'NONE', *, *, #73481, .T. ) ;
#41169 = CYLINDRICAL_SURFACE ( 'NONE', #327, 7.143750000000004263 ) ;
#41170 = CARTESIAN_POINT ( 'NONE',  ( 110.5478855402367913, -46.57039549162846015, 33.84705384733993583 ) ) ;
#41171 = LINE ( 'NONE', #63886, #38270 ) ;
#41172 = ADVANCED_FACE ( 'NONE', ( #3421 ), #52854, .F. ) ;
#41173 = CARTESIAN_POINT ( 'NONE',  ( 115.7706392458028262, -41.72622577560414925, 118.4133232042899664 ) ) ;
#41174 = CARTESIAN_POINT ( 'NONE',  ( 107.9218213793745633, -47.19875523359718983, 173.6413395616249886 ) ) ;
#41175 = EDGE_CURVE ( 'NONE', #43691, #66199, #73339, .T. ) ;
#41176 = LINE ( 'NONE', #6232, #88879 ) ;
#41177 = CARTESIAN_POINT ( 'NONE',  ( 114.2024335102360908, -32.03537151136463734, 253.7124198280768042 ) ) ;
#41178 = ORIENTED_EDGE ( 'NONE', *, *, #64590, .T. ) ;
#41179 = ORIENTED_EDGE ( 'NONE', *, *, #63223, .T. ) ;
#41180 = ORIENTED_EDGE ( 'NONE', *, *, #43515, .T. ) ;
#41181 = VECTOR ( 'NONE', #29494, 1000.000000000000000 ) ;
#41182 = DIRECTION ( 'NONE',  ( 0.000000000000000000, 0.000000000000000000, 1.000000000000000000 ) ) ;
#41183 = VECTOR ( 'NONE', #34579, 1000.000000000000000 ) ;
#41184 = CARTESIAN_POINT ( 'NONE',  ( 117.0609387842264795, -38.08014165370412485, 103.7187873333342623 ) ) ;
#41185 = AXIS2_PLACEMENT_3D ( 'NONE', #38027, #11205, #52947 ) ;
#41186 = DIRECTION ( 'NONE',  ( 4.299999999999999979E-14, -1.000000000000000000, 4.400000000000000367E-29 ) ) ;
#41187 = CARTESIAN_POINT ( 'NONE',  ( 104.4871749466078086, -26.97957198089340025, 275.2812583354421463 ) ) ;
#41188 = FACE_OUTER_BOUND ( 'NONE', #50975, .T. ) ;
#41189 = LINE ( 'NONE', #68916, #40031 ) ;
#41190 = EDGE_CURVE ( 'NONE', #79915, #34970, #35911, .T. ) ;
#41191 = VECTOR ( 'NONE', #11711, 1000.000000000000227 ) ;
#41192 = CARTESIAN_POINT ( 'NONE',  ( 97.33767738115261636, -34.07173134274512449, 176.1148459244018909 ) ) ;
#41193 = EDGE_CURVE ( 'NONE', #68797, #73231, #27876, .T. ) ;
#41194 = CARTESIAN_POINT ( 'NONE',  ( 98.19951187208806687, -40.85743130997450834, 256.6727681330542623 ) ) ;
#41195 = DIRECTION ( 'NONE',  ( 0.000000000000000000, 0.000000000000000000, -1.000000000000000000 ) ) ;
#41196 = ORIENTED_EDGE ( 'NONE', *, *, #44023, .F. ) ;
#41197 = DIRECTION ( 'NONE',  ( 0.000000000000000000, 0.000000000000000000, -1.000000000000000000 ) ) ;
#41198 = DIRECTION ( 'NONE',  ( 1.000000000000000078E-15, 0.000000000000000000, 1.000000000000000000 ) ) ;
#41199 = CARTESIAN_POINT ( 'NONE',  ( 101.1433531317129280, -42.34605246296819558, 79.74809036959096886 ) ) ;
#41200 = CARTESIAN_POINT ( 'NONE',  ( 177.1649999999999920, 14.63749999999999929, -57.14999999999999858 ) ) ;
#41201 = FACE_OUTER_BOUND ( 'NONE', #76395, .T. ) ;
#41202 = ORIENTED_EDGE ( 'NONE', *, *, #676, .F. ) ;
#41203 = CARTESIAN_POINT ( 'NONE',  ( 78.98444042533645870, -34.20116865955463936, 8.043260881865755607 ) ) ;
#41204 = ORIENTED_EDGE ( 'NONE', *, *, #45961, .T. ) ;
#41205 = CARTESIAN_POINT ( 'NONE',  ( 116.7957173713512873, -32.98391181527420457, 139.1184824187679396 ) ) ;
#41206 = ORIENTED_EDGE ( 'NONE', *, *, #61640, .T. ) ;
#41207 = LINE ( 'NONE', #21238, #18487 ) ;
#41208 = CARTESIAN_POINT ( 'NONE',  ( 115.1688055144990415, -30.74420868983300537, 105.7644404487539589 ) ) ;
#41209 = CARTESIAN_POINT ( 'NONE',  ( -11.57394144444448436, 87.79471777913512653, 117.9898073157514489 ) ) ;
#41210 = DIRECTION ( 'NONE',  ( 0.000000000000000000, 1.000000000000000000, 0.000000000000000000 ) ) ;
#41211 = CARTESIAN_POINT ( 'NONE',  ( 103.5915305487281302, -46.58145011825330783, 53.30705384733997221 ) ) ;
#41212 = AXIS2_PLACEMENT_3D ( 'NONE', #84336, #42954, #76604 ) ;
#41213 = CARTESIAN_POINT ( 'NONE',  ( 113.1782937600539896, -44.75186860135764988, 84.09395860812267642 ) ) ;
#41214 = EDGE_LOOP ( 'NONE', ( #53726, #21653 ) ) ;
#41215 = CYLINDRICAL_SURFACE ( 'NONE', #58449, 3.299999999999997158 ) ;
#41216 = CIRCLE ( 'NONE', #25220, 3.250000000000002665 ) ;
#41217 = VERTEX_POINT ( 'NONE', #48747 ) ;
#41218 = ORIENTED_EDGE ( 'NONE', *, *, #36787, .T. ) ;
#41219 = EDGE_CURVE ( 'NONE', #21567, #6566, #54213, .T. ) ;
#41220 = FACE_OUTER_BOUND ( 'NONE', #57075, .T. ) ;
#41221 = VERTEX_POINT ( 'NONE', #61495 ) ;
#41222 = CARTESIAN_POINT ( 'NONE',  ( 113.9608400058234849, -28.00707201207230668, 274.5441967044828857 ) ) ;
#41223 = CARTESIAN_POINT ( 'NONE',  ( 103.8005819418147411, -26.80618422321597194, 161.3299109901969643 ) ) ;
#41224 = DIRECTION ( 'NONE',  ( -0.7071067811865460184, 0.000000000000000000, 0.7071067811865489050 ) ) ;
#41225 = CARTESIAN_POINT ( 'NONE',  ( 102.0670549670224858, -27.97049805543147372, 141.4897919419518644 ) ) ;
#41226 = CARTESIAN_POINT ( 'NONE',  ( 115.2670960386832775, -44.14051530504124088, 79.25372051400697160 ) ) ;
#41227 = CARTESIAN_POINT ( 'NONE',  ( 109.7284190798694539, -27.00174801899234822, 95.86393833725837510 ) ) ;
#41228 = ORIENTED_EDGE ( 'NONE', *, *, #45632, .T. ) ;
#41229 = CARTESIAN_POINT ( 'NONE',  ( 0.000000000000000000, 12.27000000000000313, -9.425000000000000711 ) ) ;
#41230 = CARTESIAN_POINT ( 'NONE',  ( 115.7833820338481559, -41.80184616455515823, 159.4063391417902267 ) ) ;
#41231 = ORIENTED_EDGE ( 'NONE', *, *, #60236, .T. ) ;
#41232 = DIRECTION ( 'NONE',  ( -1.000000000000000000, -3.999999999999999995E-14, -1.000000000000000078E-15 ) ) ;
#41233 = ADVANCED_FACE ( 'NONE', ( #6109 ), #74688, .T. ) ;
#41234 = CIRCLE ( 'NONE', #16631, 2.999999999999919176 ) ;
#41235 = VECTOR ( 'NONE', #83999, 1000.000000000000000 ) ;
#41236 = DIRECTION ( 'NONE',  ( 0.9999999853157766072, 0.0001713722456134502174, -0.000000000000000000 ) ) ;
#41237 = CARTESIAN_POINT ( 'NONE',  ( 110.8846227072672121, -27.01418920731891404, 269.7784824187681920 ) ) ;
#41238 = CARTESIAN_POINT ( 'NONE',  ( 140.0667039024470455, -118.2784471599408960, 230.7030882296565721 ) ) ;
#41239 = DIRECTION ( 'NONE',  ( 4.299999999999999979E-14, -1.000000000000000000, 4.400000000000000367E-29 ) ) ;
#41240 = LINE ( 'NONE', #68526, #12216 ) ;
#41241 = CARTESIAN_POINT ( 'NONE',  ( 115.8929839771518573, -32.51563103440816604, 19.18133956162593279 ) ) ;
#41243 = CARTESIAN_POINT ( 'NONE',  ( 117.5589153096731110, -33.32758106675091625, 130.0880062282919880 ) ) ;
#41242 = CARTESIAN_POINT ( 'NONE',  ( 97.15605172367796172, -34.93424641287688104, 101.1850621333696694 ) ) ;
#41244 = LINE ( 'NONE', #5865, #75567 ) ;
#41245 = CARTESIAN_POINT ( 'NONE',  ( 117.0593108693811786, -33.60693806652478344, 174.0670538473389399 ) ) ;
#41246 = DIRECTION ( 'NONE',  ( -1.000000000000000000, -4.299999999999999979E-14, -1.000000000000000078E-15 ) ) ;
#41247 = ORIENTED_EDGE ( 'NONE', *, *, #55853, .T. ) ;
#41248 = DIRECTION ( 'NONE',  ( -1.000000000000000078E-15, 0.000000000000000000, 1.000000000000000000 ) ) ;
#41249 = VECTOR ( 'NONE', #72448, 1000.000000000000000 ) ;
#41250 = AXIS2_PLACEMENT_3D ( 'NONE', #55125, #68345, #41508 ) ;
#41251 = DIRECTION ( 'NONE',  ( 0.000000000000000000, 0.000000000000000000, -1.000000000000000000 ) ) ;
#41252 = DIRECTION ( 'NONE',  ( 0.000000000000000000, 0.000000000000000000, 1.000000000000000000 ) ) ;
#41253 = EDGE_LOOP ( 'NONE', ( #63944, #62652, #86211, #19360 ) ) ;
#41254 = ADVANCED_FACE ( 'NONE', ( #81973 ), #54658, .F. ) ;
#41255 = EDGE_CURVE ( 'NONE', #71209, #70634, #68777, .T. ) ;
#41256 = CARTESIAN_POINT ( 'NONE',  ( 100.9560082937595666, -28.70598565321984452, 61.59410917070462688 ) ) ;
#41258 = VERTEX_POINT ( 'NONE', #69222 ) ;
#41257 = CARTESIAN_POINT ( 'NONE',  ( 97.94803474170373647, -41.87343025248883777, 136.7356252759109623 ) ) ;
#41259 = CARTESIAN_POINT ( 'NONE',  ( 181.9790560690580037, -31.62489322948711035, -5.074374724088000832 ) ) ;
#41260 = CARTESIAN_POINT ( 'NONE',  ( 97.90015701271006776, -41.74100594024375965, 217.7241967044829494 ) ) ;
#41261 = CARTESIAN_POINT ( 'NONE',  ( 86.68128281353467912, 72.47310549519058043, 97.62852612868820756 ) ) ;
#41262 = CYLINDRICAL_SURFACE ( 'NONE', #8297, 2.517499999999998739 ) ;
#41263 = B_SPLINE_CURVE_WITH_KNOTS ( 'NONE', 3,
 ( #75051, #38285, #52327, #11023, #31912, #65982, #80092, #73243, #38728, #66430, #4219, #59606, #45970, #25104, #28690, #75946, #28227, #7354, #61405, #14625, #48211, #91, #49109, #82333, #49559, #985, #83219, #35043, #68242, #55468, #42297, #63208, #54567, #62305, #89135, #6025, #13719, #55919, #6454, #70031, #26892, #82782, #12836, #27787, #62753, #75503, #61844, #34146 ),
 .UNSPECIFIED., .F., .F.,
 ( 4, 2, 2, 2, 2, 2, 2, 2, 2, 1, 2, 2, 2, 2, 2, 2, 2, 2, 2, 2, 2, 1, 2, 2, 4 ),
 ( 0.05959919981814693762, 0.06208168506169071260, 0.06332292768346260703, 0.06456417030523449452, 0.06704665554877825562, 0.06828789817055014311, 0.06952914079232203060, 0.07201162603586583333, 0.07325286865763772082, 0.07449411127940962218, 0.07573535390118150967, 0.07697659652295341104, 0.07945908176649719989, 0.08194156701004098875, 0.08318280963181286236, 0.08442405225358473597, 0.08690653749712842768, 0.08814778011890027354, 0.08938902274067211939, 0.09187150798421574172, 0.09311275060598753206, 0.09435399322775930853, 0.09559523584953109887, 0.09683647847130288921, 0.09931896371484645603 ),
 .UNSPECIFIED. ) ;
#41264 = DIRECTION ( 'NONE',  ( 0.000000000000000000, 0.000000000000000000, 1.000000000000000000 ) ) ;
#41265 = ORIENTED_EDGE ( 'NONE', *, *, #21524, .F. ) ;
#41266 = ADVANCED_FACE ( 'NONE', ( #33354 ), #48295, .T. ) ;
#41267 = ORIENTED_EDGE ( 'NONE', *, *, #80513, .T. ) ;
#41268 = ORIENTED_EDGE ( 'NONE', *, *, #4663, .F. ) ;
#41269 = VERTEX_POINT ( 'NONE', #67874 ) ;
#41270 = DIRECTION ( 'NONE',  ( -0.000000000000000000, 1.000000000000000000, -0.000000000000000000 ) ) ;
#41271 = CARTESIAN_POINT ( 'NONE',  ( 96.67410449796260252, -35.53789531767939991, 202.2356252759109623 ) ) ;
#41272 = CARTESIAN_POINT ( 'NONE',  ( 86.67213519546683642, 92.64237678566777845, -97.63858630140124717 ) ) ;
#41273 = DIRECTION ( 'NONE',  ( 9.351236661543306751E-17, -3.725950533538267725E-29, -1.000000000000000000 ) ) ;
#41274 = ADVANCED_FACE ( 'NONE', ( #27428 ), #75138, .F. ) ;
#41276 = CARTESIAN_POINT ( 'NONE',  ( 107.5667039024470171, -94.77844715994206126, -19.78219314458232247 ) ) ;
#41275 = CARTESIAN_POINT ( 'NONE',  ( 29.56670390244797630, -48.82844715994099971, 20.91780685541479912 ) ) ;
#41277 = VERTEX_POINT ( 'NONE', #6543 ) ;
#41278 = COLOUR_RGB ( '', 0.09019608, 0.27058824, 0.51372549) ;
#41279 = ORIENTED_EDGE ( 'NONE', *, *, #43782, .F. ) ;
#41280 = FACE_OUTER_BOUND ( 'NONE', #55590, .T. ) ;
#41281 = CIRCLE ( 'NONE', #25338, 3.000000000000002665 ) ;
#41282 = LINE ( 'NONE', #55354, #67958 ) ;
#41283 = CARTESIAN_POINT ( 'NONE',  ( 110.8764511561472119, -27.72125199330416478, 240.7584824187679544 ) ) ;
#41284 = CARTESIAN_POINT ( 'NONE',  ( 186.6899999999999977, 52.73749999999999716, -44.45000000000000284 ) ) ;
#41285 = EDGE_CURVE ( 'NONE', #84828, #69678, #76029, .T. ) ;
#41286 = CARTESIAN_POINT ( 'NONE',  ( 112.1775644307543587, -28.39036538331633963, 90.63848241876793566 ) ) ;
#41288 = EDGE_CURVE ( 'NONE', #4876, #89309, #13807, .T. ) ;
#41287 = FACE_OUTER_BOUND ( 'NONE', #87214, .T. ) ;
#41289 = EDGE_CURVE ( 'NONE', #22204, #58575, #56246, .T. ) ;
#41290 = CARTESIAN_POINT ( 'NONE',  ( 86.72755763596094880, -122.7870702624433221, 250.2178068554179902 ) ) ;
#41291 = ORIENTED_EDGE ( 'NONE', *, *, #5463, .T. ) ;
#41292 = DIRECTION ( 'NONE',  ( 0.000000000000000000, 0.000000000000000000, -1.000000000000000000 ) ) ;
#41293 = EDGE_CURVE ( 'NONE', #12282, #30848, #34686, .T. ) ;
#41294 = ORIENTED_EDGE ( 'NONE', *, *, #56546, .F. ) ;
#41295 = VERTEX_POINT ( 'NONE', #89228 ) ;
#41296 = DIRECTION ( 'NONE',  ( 0.000000000000000000, 0.000000000000000000, -1.000000000000000000 ) ) ;
#41297 = CARTESIAN_POINT ( 'NONE',  ( 115.9273305379513062, -35.98950415022901694, 250.3244404487543022 ) ) ;
#41298 = CARTESIAN_POINT ( 'NONE',  ( 101.9936208522100003, -45.44607148789093287, 192.1564586011733411 ) ) ;
#41299 = VECTOR ( 'NONE', #18959, 1000.000000000000000 ) ;
#41300 = DIRECTION ( 'NONE',  ( 0.9659258262890670910, 0.000000000000000000, 0.2588190451025250693 ) ) ;
#41301 = AXIS2_PLACEMENT_3D ( 'NONE', #80461, #5952, #4598 ) ;
#41302 = FACE_OUTER_BOUND ( 'NONE', #39123, .T. ) ;
#41303 = CARTESIAN_POINT ( 'NONE',  ( 90.66736180499694342, 74.80137413886471620, -76.38829385798599958 ) ) ;
#41304 = VECTOR ( 'NONE', #32883, 1000.000000000000000 ) ;
#41305 = VERTEX_POINT ( 'NONE', #12924 ) ;
#41306 = DIRECTION ( 'NONE',  ( 1.047445008332813989E-14, 0.000000000000000000, 1.000000000000000000 ) ) ;
#41307 = AXIS2_PLACEMENT_3D ( 'NONE', #80874, #88133, #68124 ) ;
#41308 = CARTESIAN_POINT ( 'NONE',  ( 80.06648329127402519, -46.72944715994105991, 4.925625275910944012 ) ) ;
#41309 = ORIENTED_EDGE ( 'NONE', *, *, #38268, .T. ) ;
#41310 = CARTESIAN_POINT ( 'NONE',  ( 112.1813298990327183, -27.60452245592377807, 34.66991099019695355 ) ) ;
#41311 = VERTEX_POINT ( 'NONE', #88783 ) ;
#41312 = CARTESIAN_POINT ( 'NONE',  ( 103.3964814340166498, -45.24903370896166876, 285.0709475124485266 ) ) ;
#41313 = CARTESIAN_POINT ( 'NONE',  ( 107.0664832912739399, -36.72944715994095333, 289.6356252759107406 ) ) ;
#41314 = CARTESIAN_POINT ( 'NONE',  ( 102.8912152862169762, -46.22186109533351583, 132.2346728949589760 ) ) ;
#41315 = DIRECTION ( 'NONE',  ( -0.000000000000000000, 1.000000000000000000, 0.000000000000000000 ) ) ;
#41316 = DIRECTION ( 'NONE',  ( 1.000000000000000000, 0.000000000000000000, 0.000000000000000000 ) ) ;
#41317 = DIRECTION ( 'NONE',  ( -4.237773401492740281E-14, 1.000000000000000000, 0.000000000000000000 ) ) ;
#41318 = CARTESIAN_POINT ( 'NONE',  ( 5.165685852724023697, 70.94733280150917665, 130.4538059770566747 ) ) ;
#41319 = CIRCLE ( 'NONE', #70394, 23.50000000000000711 ) ;
#41320 = CARTESIAN_POINT ( 'NONE',  ( 97.57588284487002284, -41.14775938459609250, 252.6727681330536655 ) ) ;
#41321 = CARTESIAN_POINT ( 'NONE',  ( 91.24829632406253666, 88.91144712388910420, -75.69222284415423019 ) ) ;
#41322 = ORIENTED_EDGE ( 'NONE', *, *, #61454, .F. ) ;
#41323 = VERTEX_POINT ( 'NONE', #81533 ) ;
#41324 = CARTESIAN_POINT ( 'NONE',  ( 118.9531587402301511, -36.16547954148851574, 114.8641967044819694 ) ) ;
#41325 = CARTESIAN_POINT ( 'NONE',  ( 75.31670390244798341, -50.82844715994100682, 35.51780685541480409 ) ) ;
#41326 = VERTEX_POINT ( 'NONE', #82423 ) ;
#41327 = CIRCLE ( 'NONE', #9454, 2.125000000000001776 ) ;
#41328 = ORIENTED_EDGE ( 'NONE', *, *, #55195, .T. ) ;
#41329 = ORIENTED_EDGE ( 'NONE', *, *, #45242, .T. ) ;
#41330 = CARTESIAN_POINT ( 'NONE',  ( 115.0889058099493951, -30.61763831142564740, 265.3439584562066784 ) ) ;
#41331 = DIRECTION ( 'NONE',  ( -0.7071067811567310901, 0.7071067812163639443, 0.000000000000000000 ) ) ;
#41332 = CARTESIAN_POINT ( 'NONE',  ( 107.0664832912739399, -36.72944715994095333, 293.6356252759106837 ) ) ;
#41333 = DIRECTION ( 'NONE',  ( 0.000000000000000000, -1.000000000000000000, 0.000000000000000000 ) ) ;
#41334 = CARTESIAN_POINT ( 'NONE',  ( 99.48373692063242402, -40.90112338471579534, 174.5328522743529618 ) ) ;
#41335 = CARTESIAN_POINT ( 'NONE',  ( 118.3644662943939636, -33.07169432158188727, 280.0756252759109657 ) ) ;
#41336 = FACE_OUTER_BOUND ( 'NONE', #70875, .T. ) ;
#41337 = ORIENTED_EDGE ( 'NONE', *, *, #10802, .F. ) ;
#41338 = CARTESIAN_POINT ( 'NONE',  ( 6.710101316248270109, 71.75931113341763989, 118.3664676705691505 ) ) ;
#41339 = CARTESIAN_POINT ( 'NONE',  ( 98.30752531352220558, -41.72886023108350884, 41.73921390539881315 ) ) ;
#41340 = ORIENTED_EDGE ( 'NONE', *, *, #85346, .T. ) ;
#41341 = ORIENTED_EDGE ( 'NONE', *, *, #35530, .T. ) ;
#41342 = AXIS2_PLACEMENT_3D ( 'NONE', #74099, #25498, #25955 ) ;
#41343 = CARTESIAN_POINT ( 'NONE',  ( 172.5664832912740110, -18.82844715994099971, 198.9256252759119832 ) ) ;
#41344 = EDGE_CURVE ( 'NONE', #15378, #1971, #61943, .T. ) ;
#41345 = EDGE_LOOP ( 'NONE', ( #73013, #46214, #17942, #17949 ) ) ;
#41346 = CYLINDRICAL_SURFACE ( 'NONE', #46919, 3.499999999999996003 ) ;
#41347 = VECTOR ( 'NONE', #58365, 1000.000000000000000 ) ;
#41348 = CARTESIAN_POINT ( 'NONE',  ( 99.09565760681786628, -30.55049705524844583, 15.80229833326679945 ) ) ;
#41349 = EDGE_CURVE ( 'NONE', #10009, #59609, #40613, .T. ) ;
#41350 = DIRECTION ( 'NONE',  ( 0.000000000000000000, 0.000000000000000000, 1.000000000000000000 ) ) ;
#41351 = CARTESIAN_POINT ( 'NONE',  ( 13.40680633928208465, 223.9999999999999716, 102.7987842159323151 ) ) ;
#41352 = CARTESIAN_POINT ( 'NONE',  ( 115.9822952273240304, -35.14169155943780964, 198.3771817328379825 ) ) ;
#41353 = CARTESIAN_POINT ( 'NONE',  ( 101.0407447616467351, -27.40725005837418138, 70.54514908543497143 ) ) ;
#41354 = LINE ( 'NONE', #20044, #4553 ) ;
#41355 = ORIENTED_EDGE ( 'NONE', *, *, #7156, .F. ) ;
#41356 = EDGE_CURVE ( 'NONE', #66655, #12481, #89675, .T. ) ;
#41357 = DIRECTION ( 'NONE',  ( 0.7071067811865473507, 0.7071067811865476838, 0.000000000000000000 ) ) ;
#41358 = EDGE_LOOP ( 'NONE', ( #87389, #50491, #33574, #28556 ) ) ;
#41359 = EDGE_CURVE ( 'NONE', #61092, #74286, #47859, .T. ) ;
#41360 = ADVANCED_FACE ( 'NONE', ( #41052, #69669 ), #49201, .F. ) ;
#41361 = EDGE_LOOP ( 'NONE', ( #20606, #24322, #26470, #61500 ) ) ;
#41362 = CARTESIAN_POINT ( 'NONE',  ( 74.98969683741650272, 82.54999999999999716, 346.9005000000000223 ) ) ;
#41363 = LINE ( 'NONE', #5070, #12531 ) ;
#41364 = CARTESIAN_POINT ( 'NONE',  ( 67.06670390244701707, -81.17316614790567542, 245.5580738794290028 ) ) ;
#41365 = ADVANCED_FACE ( 'NONE', ( #77378, #8342 ), #35580, .F. ) ;
#41367 = AXIS2_PLACEMENT_3D ( 'NONE', #31129, #44756, #58828 ) ;
#41366 = DIRECTION ( 'NONE',  ( 1.000000000000000078E-15, -1.000000000000000083E-30, -1.000000000000000000 ) ) ;
#41368 = ORIENTED_EDGE ( 'NONE', *, *, #62596, .T. ) ;
#41369 = CARTESIAN_POINT ( 'NONE',  ( 112.8299879122683791, -27.27019477826133453, 49.62895860924498947 ) ) ;
#41370 = AXIS2_PLACEMENT_3D ( 'NONE', #15181, #55581, #1560 ) ;
#41371 = AXIS2_PLACEMENT_3D ( 'NONE', #69514, #84048, #13649 ) ;
#41372 = EDGE_CURVE ( 'NONE', #68199, #25814, #49651, .T. ) ;
#41374 = CARTESIAN_POINT ( 'NONE',  ( 99.63271100832268701, 75.84295037288960373, -84.36969927706125816 ) ) ;
#41373 = DIRECTION ( 'NONE',  ( 1.000000000000000000, 0.000000000000000000, 0.000000000000000000 ) ) ;
#41375 = FACE_OUTER_BOUND ( 'NONE', #85617, .T. ) ;
#41376 = CARTESIAN_POINT ( 'NONE',  ( 132.7641780748903670, -16.30680158338876140, 1.893168945964847083 ) ) ;
#41377 = ORIENTED_EDGE ( 'NONE', *, *, #58143, .F. ) ;
#41378 = CIRCLE ( 'NONE', #87759, 218.1859999999999786 ) ;
#41379 = CARTESIAN_POINT ( 'NONE',  ( 97.46090605037130672, -39.66038733884047929, 122.5612088153949770 ) ) ;
#41380 = ADVANCED_FACE ( 'NONE', ( #21984, #15156 ), #42832, .F. ) ;
#41381 = VECTOR ( 'NONE', #34923, 1000.000000000000000 ) ;
#41382 = PLANE ( 'NONE',  #87906 ) ;
#41383 = CARTESIAN_POINT ( 'NONE',  ( 7.760001168987765929, 72.46196594926868784, 118.3038028359265894 ) ) ;
#41384 = EDGE_LOOP ( 'NONE', ( #77401, #71836, #47655, #7701 ) ) ;
#41385 = CARTESIAN_POINT ( 'NONE',  ( 100.9304087016431453, -28.27451679452656919, 71.57562527591099411 ) ) ;
#41387 = DIRECTION ( 'NONE',  ( 0.000000000000000000, 0.000000000000000000, 1.000000000000000000 ) ) ;
#41386 = CARTESIAN_POINT ( 'NONE',  ( 71.09939861440099662, 20.32000000000000028, 177.8662485265279827 ) ) ;
#41388 = DIRECTION ( 'NONE',  ( 0.000000000000000000, 1.000000000000000000, 0.000000000000000000 ) ) ;
#41389 = VECTOR ( 'NONE', #5563, 1000.000000000000114 ) ;
#41390 = CONICAL_SURFACE ( 'NONE', #26879, 6.857999999999975671, 0.02993239667170383839 ) ;
#41391 = CARTESIAN_POINT ( 'NONE',  ( 136.6924846587446609, -119.7509759656530122, 249.3055338466990065 ) ) ;
#41392 = ORIENTED_EDGE ( 'NONE', *, *, #29582, .F. ) ;
#41393 = CARTESIAN_POINT ( 'NONE',  ( 96.03815445040697796, -38.18343476501374312, 147.4299109901959923 ) ) ;
#41395 = ORIENTED_EDGE ( 'NONE', *, *, #75910, .T. ) ;
#41394 = DIRECTION ( 'NONE',  ( 0.000000000000000000, 1.000000000000000000, 0.000000000000000000 ) ) ;
#41396 = CARTESIAN_POINT ( 'NONE',  ( 110.8846227072671979, -27.01418920731900641, 265.7784824187680783 ) ) ;
#41397 = CARTESIAN_POINT ( 'NONE',  ( 97.81217157231137094, -40.51860488209471356, 252.6356829567330067 ) ) ;
#41398 = DIRECTION ( 'NONE',  ( 0.000000000000000000, -1.000000000000000000, 0.000000000000000000 ) ) ;
#41399 = FACE_OUTER_BOUND ( 'NONE', #22372, .T. ) ;
#41400 = DIRECTION ( 'NONE',  ( 0.000000000000000000, 1.000000000000000000, 0.000000000000000000 ) ) ;
#41401 = EDGE_CURVE ( 'NONE', #41538, #23885, #83756, .T. ) ;
#41402 = CARTESIAN_POINT ( 'NONE',  ( 68.36620405317147231, -138.5332053212122787, 246.9855906375420034 ) ) ;
#41403 = DIRECTION ( 'NONE',  ( -1.000000000000000000, 6.036837696399451257E-13, 0.000000000000000000 ) ) ;
#41404 = EDGE_CURVE ( 'NONE', #37614, #11261, #616, .T. ) ;
#41405 = CARTESIAN_POINT ( 'NONE',  ( 97.28849942844331622, -36.49606577720025768, 196.3070538473399438 ) ) ;
#41406 = ORIENTED_EDGE ( 'NONE', *, *, #78726, .T. ) ;
#41407 = ORIENTED_EDGE ( 'NONE', *, *, #23422, .F. ) ;
#41408 = VECTOR ( 'NONE', #80374, 1000.000000000000000 ) ;
#41409 = CARTESIAN_POINT ( 'NONE',  ( 103.5819202103828474, -28.00394742224748157, 171.8225356868499603 ) ) ;
#41410 = PLANE ( 'NONE',  #47264 ) ;
#41412 = CARTESIAN_POINT ( 'NONE',  ( 78.88305248756961419, -34.24700279812927306, 1.845048209624124524 ) ) ;
#41411 = CARTESIAN_POINT ( 'NONE',  ( 97.18779024860596394, -39.88384922728100435, 277.5603871806723646 ) ) ;
#41413 = CARTESIAN_POINT ( 'NONE',  ( -23.27731929905162289, 53.97500000000000142, 30.16249999999999076 ) ) ;
#41414 = CARTESIAN_POINT ( 'NONE',  ( 107.0664832912739968, -36.72944715994100306, 287.6356252759109680 ) ) ;
#41415 = DIRECTION ( 'NONE',  ( 1.000000000000000000, 0.000000000000000000, 0.000000000000000000 ) ) ;
#41416 = DIRECTION ( 'NONE',  ( -1.000000000000000000, -4.299999999999999979E-14, -1.000000000000000078E-15 ) ) ;
#41417 = CARTESIAN_POINT ( 'NONE',  ( -41.60202597009397607, 76.06518036156089124, 50.85338361873603219 ) ) ;
#41418 = CARTESIAN_POINT ( 'NONE',  ( 97.19046783542276557, -39.99946004141662570, 241.5813395616249863 ) ) ;
#41419 = CARTESIAN_POINT ( 'NONE',  ( 104.4905646008501492, -26.97862835665753067, 170.2804552535220353 ) ) ;
#41420 = ORIENTED_EDGE ( 'NONE', *, *, #41453, .F. ) ;
#41421 = EDGE_LOOP ( 'NONE', ( #29817, #28423, #17446, #81212 ) ) ;
#41422 = CARTESIAN_POINT ( 'NONE',  ( 113.1782937619596936, -44.75186859986670385, 88.09395860831342873 ) ) ;
#41423 = CARTESIAN_POINT ( 'NONE',  ( 82.72821098188319411, -19.44060378571146330, 6.877169033952460708 ) ) ;
#41424 = CARTESIAN_POINT ( 'NONE',  ( 0.000000000000000000, 8.255000000000000782, 0.000000000000000000 ) ) ;
#41425 = FACE_OUTER_BOUND ( 'NONE', #10074, .T. ) ;
#41427 = DIRECTION ( 'NONE',  ( 0.000000000000000000, 0.000000000000000000, 1.000000000000000000 ) ) ;
#41426 = VECTOR ( 'NONE', #18179, 1000.000000000000000 ) ;
#41428 = ORIENTED_EDGE ( 'NONE', *, *, #39152, .F. ) ;
#41429 = VECTOR ( 'NONE', #82669, 1000.000000000000000 ) ;
#41430 = CARTESIAN_POINT ( 'NONE',  ( 115.4796304032075653, -43.01888039838633659, 24.31562527591096767 ) ) ;
#41431 = AXIS2_PLACEMENT_3D ( 'NONE', #27691, #69029, #76290 ) ;
#41432 = VECTOR ( 'NONE', #48893, 1000.000000000000000 ) ;
#41433 = CARTESIAN_POINT ( 'NONE',  ( 97.01631923850186467, -33.95794342121210718, 251.1127681330538337 ) ) ;
#41434 = ORIENTED_EDGE ( 'NONE', *, *, #85507, .T. ) ;
#41435 = CARTESIAN_POINT ( 'NONE',  ( -3.260447369053748545, 94.72788168350989224, 118.5118207592319379 ) ) ;
#41436 = LINE ( 'NONE', #21929, #54384 ) ;
#41437 = CARTESIAN_POINT ( 'NONE',  ( 113.6980717437190833, -44.24279107308028358, 168.1518506361709626 ) ) ;
#41438 = CARTESIAN_POINT ( 'NONE',  ( 104.6989491262461769, -45.05385146434951338, 65.18618560768597092 ) ) ;
#41439 = CARTESIAN_POINT ( 'NONE',  ( 117.3314307007336481, -34.78826007317788083, 154.9756252759109714 ) ) ;
#41440 = CARTESIAN_POINT ( 'NONE',  ( 51.06648329127400388, -0.2185775633790978945, 333.4006252759120343 ) ) ;
#41441 = ORIENTED_EDGE ( 'NONE', *, *, #36236, .F. ) ;
#41442 = VECTOR ( 'NONE', #66311, 1000.000000000000000 ) ;
#41443 = PLANE ( 'NONE',  #37840 ) ;
#41444 = EDGE_CURVE ( 'NONE', #63459, #83484, #42386, .T. ) ;
#41445 = ORIENTED_EDGE ( 'NONE', *, *, #44793, .T. ) ;
#41446 = VERTEX_POINT ( 'NONE', #14562 ) ;
#41447 = CARTESIAN_POINT ( 'NONE',  ( 69.25757238336807120, -1.944390235229864539, 361.9756252759101471 ) ) ;
#41448 = VERTEX_POINT ( 'NONE', #81811 ) ;
#41449 = ORIENTED_EDGE ( 'NONE', *, *, #13286, .T. ) ;
#41450 = CARTESIAN_POINT ( 'NONE',  ( 161.4809174648184182, -49.32844715993547879, 249.9678068554149490 ) ) ;
#41451 = CIRCLE ( 'NONE', #13928, 3.174999999999983391 ) ;
#41452 = EDGE_CURVE ( 'NONE', #14599, #51171, #66436, .T. ) ;
#41453 = EDGE_CURVE ( 'NONE', #19998, #10951, #47699, .T. ) ;
#41454 = CARTESIAN_POINT ( 'NONE',  ( 98.52328466580365784, -37.41198607556916755, 100.8124198280769832 ) ) ;
#41455 = CARTESIAN_POINT ( 'NONE',  ( 104.1796880194223576, -26.65200820554803585, 225.2984824187679749 ) ) ;
#41456 = EDGE_CURVE ( 'NONE', #29419, #87456, #50430, .T. ) ;
#41457 = CARTESIAN_POINT ( 'NONE',  ( 106.4848323041101850, -24.91801670280273129, 195.1156252759109861 ) ) ;
#41458 = CARTESIAN_POINT ( 'NONE',  ( 112.9508454419805332, -28.15023113465295879, 40.59848241876795782 ) ) ;
#41459 = DIRECTION ( 'NONE',  ( -7.570719237730541270E-15, -1.000000000000000000, 0.000000000000000000 ) ) ;
#41460 = CARTESIAN_POINT ( 'NONE',  ( 0.000000000000000000, 127.0000000000000000, -103.1875000000000000 ) ) ;
#41461 = EDGE_CURVE ( 'NONE', #17964, #27454, #88190, .T. ) ;
#41462 = VERTEX_POINT ( 'NONE', #20476 ) ;
#41463 = B_SPLINE_CURVE_WITH_KNOTS ( 'NONE', 3,
 ( #69700, #62867, #28815, #63783, #64228, #83328, #56497, #28342, #7469, #56036, #83784, #84240, #70597, #29261, #56944, #84687, #22903, #22448 ),
 .UNSPECIFIED., .F., .F.,
 ( 4, 2, 2, 2, 2, 2, 2, 2, 4 ),
 ( 0.000000000000000000, 0.1250000000000000000, 0.2500000000000000000, 0.3750000000000000000, 0.5000000000000000000, 0.6250000000000000000, 0.7500000000000000000, 0.8750000000000000000, 1.000000000000000000 ),
 .UNSPECIFIED. ) ;
#41464 = EDGE_CURVE ( 'NONE', #72856, #86673, #12764, .T. ) ;
#41465 = CARTESIAN_POINT ( 'NONE',  ( 116.9564367646783722, -33.61053620760070260, 129.0575300378169743 ) ) ;
#41466 = CARTESIAN_POINT ( 'NONE',  ( 117.1340566916381789, -32.05431620389533265, 59.16038718067295576 ) ) ;
#41467 = CARTESIAN_POINT ( 'NONE',  ( 116.9671346634708442, -41.74840980516093936, 248.4651490854349731 ) ) ;
#41468 = VERTEX_POINT ( 'NONE', #68173 ) ;
#41469 = CARTESIAN_POINT ( 'NONE',  ( 103.8197072928965810, -48.12676840017521585, 217.3556252759109668 ) ) ;
#41470 = CARTESIAN_POINT ( 'NONE',  ( 98.34985886569381819, -31.65658488862931819, 35.90645861648791737 ) ) ;
#41471 =( NAMED_UNIT ( * ) SI_UNIT ( $, .STERADIAN. ) SOLID_ANGLE_UNIT ( ) );
#41472 = CARTESIAN_POINT ( 'NONE',  ( 101.9930969677325407, -45.44575997282210267, 23.15640987073907553 ) ) ;
#41473 = CARTESIAN_POINT ( 'NONE',  ( 29.56670390244743629, -48.82844715994161078, 180.4678068554150911 ) ) ;
#41475 = DIRECTION ( 'NONE',  ( 1.000000000000000000, 4.163336342344333240E-14, 0.000000000000000000 ) ) ;
#41474 = CARTESIAN_POINT ( 'NONE',  ( 107.0664832912739257, -18.82844715994099971, 239.5838068554170093 ) ) ;
#41476 = FACE_BOUND ( 'NONE', #29965, .T. ) ;
#41478 = EDGE_CURVE ( 'NONE', #31607, #22927, #6925, .T. ) ;
#41477 = CARTESIAN_POINT ( 'NONE',  ( 107.0664832912740252, -46.47944715994103149, -4.824374724089029343 ) ) ;
#41479 = CARTESIAN_POINT ( 'NONE',  ( 12.29197255332129579, 85.84955738763291322, -117.9171711396470386 ) ) ;
#41480 = CARTESIAN_POINT ( 'NONE',  ( 134.0664832912740110, -8.729447159940999512, 311.1531252759119752 ) ) ;
#41481 = LINE ( 'NONE', #69211, #25616 ) ;
#41482 = LINE ( 'NONE', #70106, #65199 ) ;
#41483 = EDGE_CURVE ( 'NONE', #9653, #16775, #20917, .T. ) ;
#41485 = EDGE_LOOP ( 'NONE', ( #30508, #51677, #39545, #15160 ) ) ;
#41484 = CARTESIAN_POINT ( 'NONE',  ( 71.25416588882602298, -72.55705569728901594, 542.9756252759101471 ) ) ;
#41486 = DIRECTION ( 'NONE',  ( -1.000000000000000078E-15, 1.000000000000000000, 0.000000000000000000 ) ) ;
#41487 = CARTESIAN_POINT ( 'NONE',  ( 116.9057501799638601, -41.81710558299434410, 243.4346728949589647 ) ) ;
#41488 = CARTESIAN_POINT ( 'NONE',  ( 114.2399097434533246, -45.14383888093294672, 149.1508633711489722 ) ) ;
#41489 = CARTESIAN_POINT ( 'NONE',  ( 96.97452011921430426, -33.94641660286638540, 247.1127681330539758 ) ) ;
#41490 = VECTOR ( 'NONE', #51713, 1000.000000000000000 ) ;
#41491 = DIRECTION ( 'NONE',  ( 0.7071067811865475727, -0.7071067811865475727, 0.000000000000000000 ) ) ;
#41493 = DIRECTION ( 'NONE',  ( 0.000000000000000000, -1.000000000000000000, 0.000000000000000000 ) ) ;
#41492 = DIRECTION ( 'NONE',  ( 0.000000000000000000, 0.000000000000000000, -1.000000000000000000 ) ) ;
#41494 = CARTESIAN_POINT ( 'NONE',  ( 116.3289480479917017, -32.94026123176625731, 29.13562527591096085 ) ) ;
#41495 = DIRECTION ( 'NONE',  ( 0.0001713722456129695634, -0.9999999853157764962, 0.000000000000000000 ) ) ;
#41496 = VECTOR ( 'NONE', #19208, 1000.000000000000000 ) ;
#41497 = VECTOR ( 'NONE', #32102, 1000.000000000000000 ) ;
#41498 = AXIS2_PLACEMENT_3D ( 'NONE', #44437, #9490, #37649 ) ;
#41499 = ORIENTED_EDGE ( 'NONE', *, *, #84347, .T. ) ;
#41500 = CARTESIAN_POINT ( 'NONE',  ( 71.09939861440099662, 101.5999999999999943, 177.8662485265279827 ) ) ;
#41501 = VERTEX_POINT ( 'NONE', #14100 ) ;
#41502 = CARTESIAN_POINT ( 'NONE',  ( 115.0466524894680731, -42.26004630958951935, 162.7667055423629847 ) ) ;
#41504 = EDGE_LOOP ( 'NONE', ( #31749, #64385, #14071, #70528 ) ) ;
#41503 = CARTESIAN_POINT ( 'NONE',  ( 97.81151477712479902, -40.51751189930152464, 186.6359914586728337 ) ) ;
#41505 = LINE ( 'NONE', #27890, #5466 ) ;
#41506 = CARTESIAN_POINT ( 'NONE',  ( 98.02603654163385727, -30.41010087969375775, 156.8289586092439549 ) ) ;
#41507 = CARTESIAN_POINT ( 'NONE',  ( 61.67079006425790766, -0.9306969701460061639, 542.9756252759101471 ) ) ;
#41508 = DIRECTION ( 'NONE',  ( -1.110223024625155531E-13, -1.000000000000000000, 0.000000000000000000 ) ) ;
#41509 = CARTESIAN_POINT ( 'NONE',  ( -91.25368348339000590, 76.20320268897033600, 75.68572508987546144 ) ) ;
#41510 = DIRECTION ( 'NONE',  ( 0.000000000000000000, 0.000000000000000000, 1.000000000000000000 ) ) ;
#41511 = ADVANCED_FACE ( 'NONE', ( #5954, #33644 ), #54053, .F. ) ;
#41513 = CARTESIAN_POINT ( 'NONE',  ( 97.42673588038233845, -38.38435052442954998, 91.46133956162594814 ) ) ;
#41512 = AXIS2_PLACEMENT_3D ( 'NONE', #47378, #81058, #75113 ) ;
#41514 = ORIENTED_EDGE ( 'NONE', *, *, #88693, .T. ) ;
#41515 = ORIENTED_EDGE ( 'NONE', *, *, #5798, .T. ) ;
#41516 = ORIENTED_EDGE ( 'NONE', *, *, #51323, .F. ) ;
#41517 = DIRECTION ( 'NONE',  ( -1.000000000000000000, 0.000000000000000000, 0.000000000000000000 ) ) ;
#41519 = DIRECTION ( 'NONE',  ( -1.000000000000000000, 0.000000000000000000, -6.982966722218760189E-15 ) ) ;
#41518 = CARTESIAN_POINT ( 'NONE',  ( 112.7790632652331482, -27.19118669266625687, 200.6470538473389809 ) ) ;
#41520 = AXIS2_PLACEMENT_3D ( 'NONE', #22109, #29808, #47641 ) ;
#41521 = CARTESIAN_POINT ( 'NONE',  ( 137.0667039024470171, -90.27844715994091018, 222.2178068554179902 ) ) ;
#41522 = CARTESIAN_POINT ( 'NONE',  ( 75.61066417432020614, 0.000000000000000000, 189.7379999999999995 ) ) ;
#41523 = DIRECTION ( 'NONE',  ( 1.000000000000000000, 0.000000000000000000, 0.000000000000000000 ) ) ;
#41524 = DIRECTION ( 'NONE',  ( 0.000000000000000000, -1.000000000000000000, 0.000000000000000000 ) ) ;
#41525 = CARTESIAN_POINT ( 'NONE',  ( 68.64392107045537728, -69.36643247059872408, 247.4587235857139831 ) ) ;
#41526 = CARTESIAN_POINT ( 'NONE',  ( 96.62907006607237292, -36.88702529232764249, 136.3384824187679385 ) ) ;
#41527 = EDGE_LOOP ( 'NONE', ( #55710, #52152, #17159, #20728 ) ) ;
#41528 = ORIENTED_EDGE ( 'NONE', *, *, #69189, .T. ) ;
#41529 = ORIENTED_EDGE ( 'NONE', *, *, #27908, .F. ) ;
#41530 = EDGE_CURVE ( 'NONE', #28914, #34067, #69965, .T. ) ;
#41531 = CARTESIAN_POINT ( 'NONE',  ( 177.8371591254543205, -47.82818131005477369, 300.4678068554149490 ) ) ;
#41532 = CARTESIAN_POINT ( 'NONE',  ( -86.19814306825452377, 92.12504059357189590, -98.05663017059063691 ) ) ;
#41533 = CARTESIAN_POINT ( 'NONE',  ( 0.000000000000000000, 124.9679999999999893, 0.000000000000000000 ) ) ;
#41534 = CARTESIAN_POINT ( 'NONE',  ( 98.43814749271325582, -36.05658283995993685, 189.0947570362579597 ) ) ;
#41535 = EDGE_CURVE ( 'NONE', #27470, #85514, #88625, .T. ) ;
#41536 = CARTESIAN_POINT ( 'NONE',  ( 123.6837132603318565, -20.11243780205705534, 229.5838068554170093 ) ) ;
#41537 = DIRECTION ( 'NONE',  ( 1.000000000000000078E-15, -1.000000000000000000, 0.000000000000000000 ) ) ;
#41538 = VERTEX_POINT ( 'NONE', #26380 ) ;
#41540 = ORIENTED_EDGE ( 'NONE', *, *, #2221, .T. ) ;
#41539 = ORIENTED_EDGE ( 'NONE', *, *, #58701, .F. ) ;
#41541 = FACE_OUTER_BOUND ( 'NONE', #51879, .T. ) ;
#41542 = ORIENTED_EDGE ( 'NONE', *, *, #85853, .T. ) ;
#41543 = ORIENTED_EDGE ( 'NONE', *, *, #17193, .T. ) ;
#41544 = CARTESIAN_POINT ( 'NONE',  ( 255.9983484187079910, 65.43750000000000000, -2.032000000000000028 ) ) ;
#41545 = CARTESIAN_POINT ( 'NONE',  ( 110.1832024441707460, -27.86589328696400969, 251.2511071154212061 ) ) ;
#41546 = ORIENTED_EDGE ( 'NONE', *, *, #38123, .F. ) ;
#41547 = AXIS2_PLACEMENT_3D ( 'NONE', #49823, #14887, #56180 ) ;
#41548 = LINE ( 'NONE', #61552, #11714 ) ;
#41549 = CARTESIAN_POINT ( 'NONE',  ( -125.4478282125672877, 68.54351064866861520, 36.16615773164556913 ) ) ;
#41550 = AXIS2_PLACEMENT_3D ( 'NONE', #79555, #78222, #70953 ) ;
#41551 = ORIENTED_EDGE ( 'NONE', *, *, #75159, .T. ) ;
#41552 = ORIENTED_EDGE ( 'NONE', *, *, #49249, .T. ) ;
#41553 = VECTOR ( 'NONE', #71905, 1000.000000000000000 ) ;
#41554 = VECTOR ( 'NONE', #58847, 1000.000000000000000 ) ;
#41555 = CARTESIAN_POINT ( 'NONE',  ( 119.2637946045969954, -42.39761235918182791, 25.56312527591098416 ) ) ;
#41556 = EDGE_LOOP ( 'NONE', ( #73650, #55713 ) ) ;
#41557 = ORIENTED_EDGE ( 'NONE', *, *, #13817, .F. ) ;
#41558 = EDGE_CURVE ( 'NONE', #34951, #60793, #19563, .T. ) ;
#41559 = ADVANCED_FACE ( 'NONE', ( #74980 ), #54948, .T. ) ;
#41560 = CARTESIAN_POINT ( 'NONE',  ( 110.7520593201813597, -44.56232478875543990, 285.7328522743533767 ) ) ;
#41561 = CARTESIAN_POINT ( 'NONE',  ( 97.55101884832849635, -31.05922868340991627, 130.9108633711489915 ) ) ;
#41562 = EDGE_CURVE ( 'NONE', #75590, #83000, #82265, .T. ) ;
#41563 = CARTESIAN_POINT ( 'NONE',  ( 101.6894933626719819, -27.09867346898205298, 105.4937205140069665 ) ) ;
#41564 = CARTESIAN_POINT ( 'NONE',  ( 101.3006676746225310, -42.31480118910680233, 249.5838068554172651 ) ) ;
#41565 = CARTESIAN_POINT ( 'NONE',  ( 57.14999999999999858, 95.25000000000000000, 323.0879999999999654 ) ) ;
#41566 = CARTESIAN_POINT ( 'NONE',  ( 118.8773263846236148, -37.69826137473897631, 184.7613395616249647 ) ) ;
#41567 = CARTESIAN_POINT ( 'NONE',  ( 32.06670390244571678, -32.29483332968550258, 193.9678068554150911 ) ) ;
#41568 = DIRECTION ( 'NONE',  ( 0.000000000000000000, 1.000000000000000000, 0.000000000000000000 ) ) ;
#41569 = ORIENTED_EDGE ( 'NONE', *, *, #40667, .T. ) ;
#41570 = CARTESIAN_POINT ( 'NONE',  ( 129.9778716492872945, 79.25971567868506895, 12.27341459163532811 ) ) ;
#41571 = VERTEX_POINT ( 'NONE', #62691 ) ;
#41572 = ADVANCED_FACE ( 'NONE', ( #75439 ), #13651, .F. ) ;
#41573 = VERTEX_POINT ( 'NONE', #34978 ) ;
#41574 = LINE ( 'NONE', #76569, #77991 ) ;
#41575 = AXIS2_PLACEMENT_3D ( 'NONE', #87722, #59104, #17347 ) ;
#41576 = FACE_BOUND ( 'NONE', #19885, .T. ) ;
#41577 = AXIS2_PLACEMENT_3D ( 'NONE', #18454, #33878, #47036 ) ;
#41578 = CARTESIAN_POINT ( 'NONE',  ( 98.45854724665603896, -30.84808103350501085, 120.8499109901969604 ) ) ;
#41579 = CARTESIAN_POINT ( 'NONE',  ( -7.053076781563553332, 71.98855499260324109, 130.3653452852127828 ) ) ;
#41580 = LINE ( 'NONE', #75683, #27529 ) ;
#41581 = DIRECTION ( 'NONE',  ( 0.000000000000000000, 0.000000000000000000, -1.000000000000000000 ) ) ;
#41584 = CARTESIAN_POINT ( 'NONE',  ( 115.4423046205436094, -29.55243945206544609, 225.4022919425769658 ) ) ;
#41583 = DIRECTION ( 'NONE',  ( 1.000000000000000000, 0.000000000000000000, 0.000000000000000000 ) ) ;
#41582 = CARTESIAN_POINT ( 'NONE',  ( 68.91678303834669350, -69.56165394957326953, 247.5002289977139753 ) ) ;
#41585 = DIRECTION ( 'NONE',  ( 0.000000000000000000, 1.000000000000000000, 0.000000000000000000 ) ) ;
#41587 = EDGE_CURVE ( 'NONE', #87914, #78380, #69062, .T. ) ;
#41586 = DIRECTION ( 'NONE',  ( 1.000000000000000000, 4.163336342344333240E-14, 0.000000000000000000 ) ) ;
#41588 = VERTEX_POINT ( 'NONE', #6831 ) ;
#41589 = CARTESIAN_POINT ( 'NONE',  ( 98.06670390244704549, -104.2784471599408818, 19.21780685541799016 ) ) ;
#41590 = DIRECTION ( 'NONE',  ( 1.000000000000000000, 0.000000000000000000, -9.299908063537909262E-17 ) ) ;
#41591 = FACE_OUTER_BOUND ( 'NONE', #48231, .T. ) ;
#41592 = FACE_BOUND ( 'NONE', #57950, .T. ) ;
#41594 = ORIENTED_EDGE ( 'NONE', *, *, #84094, .T. ) ;
#41593 = CARTESIAN_POINT ( 'NONE',  ( 105.0129988258793645, -25.82091521352475283, 280.2365776568630622 ) ) ;
#41595 = CARTESIAN_POINT ( 'NONE',  ( -185.9961463128564958, 20.32000000000000028, -3.174999999999349676 ) ) ;
#41596 = CARTESIAN_POINT ( 'NONE',  ( 117.0443417989465758, -39.94358261462815562, 158.5784824187679476 ) ) ;
#41597 = CARTESIAN_POINT ( 'NONE',  ( 99.29379691555868703, -43.72992423520055638, 52.90991099019698396 ) ) ;
#41598 = CARTESIAN_POINT ( 'NONE',  ( 113.6418603426413938, -28.58344220020606130, 160.5356252759109736 ) ) ;
#41599 = CARTESIAN_POINT ( 'NONE',  ( 97.81168736999980240, -40.51740164104307240, 32.63591986563997693 ) ) ;
#41600 = CARTESIAN_POINT ( 'NONE',  ( 112.1392343750146381, -28.01276493709994853, 100.6565439726868760 ) ) ;
#41601 = AXIS2_PLACEMENT_3D ( 'NONE', #58967, #86255, #22702 ) ;
#41603 = DIRECTION ( 'NONE',  ( 0.000000000000000000, 0.000000000000000000, 1.000000000000000000 ) ) ;
#41602 = DIRECTION ( 'NONE',  ( 1.000000000000000000, 0.000000000000000000, -3.491483361109380094E-15 ) ) ;
#41604 = FACE_OUTER_BOUND ( 'NONE', #15009, .T. ) ;
#41605 = LINE ( 'NONE', #13476, #65409 ) ;
#41606 = ORIENTED_EDGE ( 'NONE', *, *, #50817, .F. ) ;
#41607 = AXIS2_PLACEMENT_3D ( 'NONE', #50082, #56449, #76463 ) ;
#41608 = ORIENTED_EDGE ( 'NONE', *, *, #64708, .F. ) ;
#41609 = ORIENTED_EDGE ( 'NONE', *, *, #53554, .T. ) ;
#41610 = EDGE_LOOP ( 'NONE', ( #55496, #9003, #25495, #72743 ) ) ;
#41611 = CARTESIAN_POINT ( 'NONE',  ( 136.8164832912739826, -36.72944715994100306, 14.92562527591100263 ) ) ;
#41612 = CARTESIAN_POINT ( 'NONE',  ( 98.73996931189277859, -42.96625968561437503, 62.83848241876793850 ) ) ;
#41613 = DIRECTION ( 'NONE',  ( 0.000000000000000000, 1.000000000000000000, 0.000000000000000000 ) ) ;
#41614 = CARTESIAN_POINT ( 'NONE',  ( 145.2442745643976423, -139.1110834320304832, 246.6806061270391126 ) ) ;
#41615 = CARTESIAN_POINT ( 'NONE',  ( 103.7937703862009613, -26.78548768338485075, 161.3299109901969643 ) ) ;
#41616 = AXIS2_PLACEMENT_3D ( 'NONE', #10232, #37937, #44284 ) ;
#41617 = CARTESIAN_POINT ( 'NONE',  ( 3.968749999999215294, 120.6499999999999915, 105.4788588808464027 ) ) ;
#41618 = CIRCLE ( 'NONE', #2488, 2.750000000000002665 ) ;
#41619 = EDGE_CURVE ( 'NONE', #59006, #79006, #34535, .T. ) ;
#41620 = CARTESIAN_POINT ( 'NONE',  ( 98.46141696562543189, -39.55439615822902510, 286.0133722090292849 ) ) ;
#41621 = EDGE_LOOP ( 'NONE', ( #63795, #83164, #18108, #83383 ) ) ;
#41622 = EDGE_LOOP ( 'NONE', ( #9968, #47731, #79480, #84575 ) ) ;
#41623 = EDGE_LOOP ( 'NONE', ( #11384, #65838, #31734, #45434 ) ) ;
#41624 = AXIS2_PLACEMENT_3D ( 'NONE', #18822, #66062, #3855 ) ;
#41625 = VECTOR ( 'NONE', #76864, 1000.000000000000000 ) ;
#41626 = CARTESIAN_POINT ( 'NONE',  ( 131.0667039024480118, -61.87844715994100397, 231.5838068554150198 ) ) ;
#41627 = VECTOR ( 'NONE', #10712, 1000.000000000000000 ) ;
#41628 = CARTESIAN_POINT ( 'NONE',  ( 115.0884725098965049, -30.61707623100678077, 160.3440144957833127 ) ) ;
#41629 = DIRECTION ( 'NONE',  ( 1.000000000000000078E-15, -1.000000000000000000, 0.000000000000000000 ) ) ;
#41630 = CARTESIAN_POINT ( 'NONE',  ( 76.06670390244809710, -58.72944715994109544, 199.5838068554169524 ) ) ;
#41631 = CARTESIAN_POINT ( 'NONE',  ( 72.96458098368650269, 127.0000000000000000, 80.10833098368729566 ) ) ;
#41632 = DIRECTION ( 'NONE',  ( 0.000000000000000000, 0.000000000000000000, -1.000000000000000000 ) ) ;
#41633 = PLANE ( 'NONE',  #2790 ) ;
#41634 = CARTESIAN_POINT ( 'NONE',  ( 105.1675567143510079, -46.98732170830152910, 12.42991099019596923 ) ) ;
#41635 = DIRECTION ( 'NONE',  ( 0.000000000000000000, 0.000000000000000000, 1.000000000000000000 ) ) ;
#41636 = ORIENTED_EDGE ( 'NONE', *, *, #79124, .F. ) ;
#41637 = DIRECTION ( 'NONE',  ( 0.000000000000000000, 0.000000000000000000, -1.000000000000000000 ) ) ;
#41638 = VECTOR ( 'NONE', #72213, 1000.000000000000000 ) ;
#41639 = DIRECTION ( 'NONE',  ( 0.000000000000000000, 0.000000000000000000, -1.000000000000000000 ) ) ;
#41640 = CARTESIAN_POINT ( 'NONE',  ( 112.1086029179114547, -30.31019831854434443, 77.36523322673394887 ) ) ;
#41641 = CIRCLE ( 'NONE', #19951, 218.1859999999999786 ) ;
#41642 = EDGE_CURVE ( 'NONE', #62557, #80300, #82428, .T. ) ;
#41643 = CYLINDRICAL_SURFACE ( 'NONE', #16562, 2.500000000000002220 ) ;
#41644 = CARTESIAN_POINT ( 'NONE',  ( 63.03715912545737865, -24.89890238295017966, 249.9678068554150343 ) ) ;
#41645 = ORIENTED_EDGE ( 'NONE', *, *, #52464, .F. ) ;
#41646 = ORIENTED_EDGE ( 'NONE', *, *, #65376, .F. ) ;
#41647 = CARTESIAN_POINT ( 'NONE',  ( 77.61460381940253228, -35.48272374588488276, 7.134497377257247308 ) ) ;
#41648 = VERTEX_POINT ( 'NONE', #15899 ) ;
#41649 = CARTESIAN_POINT ( 'NONE',  ( 101.7694246217487972, -45.70876760617753831, 162.1527681330539679 ) ) ;
#41650 = ORIENTED_EDGE ( 'NONE', *, *, #59736, .T. ) ;
#41651 = DIRECTION ( 'NONE',  ( 0.000000000000000000, 0.000000000000000000, -1.000000000000000000 ) ) ;
#41652 = CARTESIAN_POINT ( 'NONE',  ( 113.3955173535308063, -30.52198670013464010, 145.8758690201829609 ) ) ;
#41653 = CARTESIAN_POINT ( 'NONE',  ( -0.4144849534825577608, 95.25000000000000000, 118.5559999999999974 ) ) ;
#41654 = CARTESIAN_POINT ( 'NONE',  ( 101.1286207290677908, -27.37920684556040740, 61.51467289495899138 ) ) ;
#41655 = VECTOR ( 'NONE', #61164, 1000.000000000000114 ) ;
#41656 = LINE ( 'NONE', #21701, #85107 ) ;
#41657 = ORIENTED_EDGE ( 'NONE', *, *, #30022, .F. ) ;
#41658 = LINE ( 'NONE', #20354, #3360 ) ;
#41659 = ORIENTED_EDGE ( 'NONE', *, *, #50746, .T. ) ;
#41660 = ORIENTED_EDGE ( 'NONE', *, *, #66414, .T. ) ;
#41661 = ADVANCED_FACE ( 'NONE', ( #919 ), #63595, .F. ) ;
#41662 = PLANE ( 'NONE',  #87618 ) ;
#41663 = EDGE_LOOP ( 'NONE', ( #38626, #52190, #68367, #39357 ) ) ;
#41664 = EDGE_CURVE ( 'NONE', #83340, #58908, #42676, .T. ) ;
#41665 = CARTESIAN_POINT ( 'NONE',  ( 97.82554479137630210, -33.52525840161893456, 286.0613395616258572 ) ) ;
#41666 = CARTESIAN_POINT ( 'NONE',  ( 102.0714078572591319, -27.55412165564507632, 141.4727681330539895 ) ) ;
#41667 = DIRECTION ( 'NONE',  ( 0.3818493186865920541, -0.9242245927363030855, 0.000000000000000000 ) ) ;
#41668 = DIRECTION ( 'NONE',  ( 0.000000000000000000, 1.000000000000000000, 0.000000000000000000 ) ) ;
#41669 = EDGE_CURVE ( 'NONE', #85162, #41221, #1166, .T. ) ;
#41670 = CARTESIAN_POINT ( 'NONE',  ( 116.9748844278823015, -33.48813965163778050, 85.07848241876791917 ) ) ;
#41671 = CARTESIAN_POINT ( 'NONE',  ( 105.7154773592118460, -46.72385839588265100, 262.4689586115381985 ) ) ;
#41672 = EDGE_LOOP ( 'NONE', ( #54527, #14504 ) ) ;
#41673 = CARTESIAN_POINT ( 'NONE',  ( 97.78516791111108830, -40.45206948340641162, 116.6303087853498255 ) ) ;
#41674 = EDGE_CURVE ( 'NONE', #81089, #8309, #58115, .T. ) ;
#41675 = CIRCLE ( 'NONE', #31573, 3.250000000000002665 ) ;
#41676 = CARTESIAN_POINT ( 'NONE',  ( -446.0240000000000009, 3.174999999999999822, -1.387778780781445991E-14 ) ) ;
#41677 = ORIENTED_EDGE ( 'NONE', *, *, #41072, .T. ) ;
#41678 = AXIS2_PLACEMENT_3D ( 'NONE', #6428, #20522, #62281 ) ;
#41679 = DIRECTION ( 'NONE',  ( -0.8660254037844380415, -0.5000000000000012212, 1.550000000000001284E-14 ) ) ;
#41680 = CIRCLE ( 'NONE', #2565, 0.5000000000000104361 ) ;
#41681 = DIRECTION ( 'NONE',  ( 0.000000000000000000, 0.000000000000000000, 1.000000000000000000 ) ) ;
#41682 = CARTESIAN_POINT ( 'NONE',  ( 99.12728904495253346, -44.42023919799950704, 41.95086337114900488 ) ) ;
#41683 = DIRECTION ( 'NONE',  ( 4.299999999999999979E-14, -1.000000000000000000, 0.000000000000000000 ) ) ;
#41684 = VECTOR ( 'NONE', #78789, 1000.000000000000000 ) ;
#41685 = DIRECTION ( 'NONE',  ( 0.7071067811865496822, -0.7071067811865453523, 7.071067811865490124E-16 ) ) ;
#41686 = DIRECTION ( 'NONE',  ( -0.9254794337955620787, -0.3787978585227822492, 0.000000000000000000 ) ) ;
#41687 = CARTESIAN_POINT ( 'NONE',  ( 98.36549455146187881, -40.29075363668734155, 11.63562527591094309 ) ) ;
#41689 = CARTESIAN_POINT ( 'NONE',  ( 117.8338636819850365, -39.12263375953639155, 99.64038718067195077 ) ) ;
#41688 = LINE ( 'NONE', #53513, #30426 ) ;
#41690 = FACE_OUTER_BOUND ( 'NONE', #22779, .T. ) ;
#41691 = CARTESIAN_POINT ( 'NONE',  ( 117.2351557800294870, -41.18040025386632408, 208.4861014663869696 ) ) ;
#41693 = ADVANCED_FACE ( 'NONE', ( #85847 ), #51277, .T. ) ;
#41692 = CARTESIAN_POINT ( 'NONE',  ( 32.16397622748888097, -34.03355364506390401, 117.4678068554150485 ) ) ;
#41694 = ORIENTED_EDGE ( 'NONE', *, *, #45278, .T. ) ;
#41695 = CARTESIAN_POINT ( 'NONE',  ( 147.0667039024469886, -67.87844715994090450, 222.2178068554179902 ) ) ;
#41696 = CARTESIAN_POINT ( 'NONE',  ( 109.5221484136284005, 50.04810782126799751, 71.06173480727821357 ) ) ;
#41697 = EDGE_CURVE ( 'NONE', #17090, #5230, #22719, .T. ) ;
#41698 = CARTESIAN_POINT ( 'NONE',  ( 136.8164482479831463, -36.55833207210741165, 3.101428811466717228 ) ) ;
#41699 = ORIENTED_EDGE ( 'NONE', *, *, #15960, .F. ) ;
#41700 = AXIS2_PLACEMENT_3D ( 'NONE', #49744, #64295, #63389 ) ;
#41701 = PLANE ( 'NONE',  #85387 ) ;
#41703 = ORIENTED_EDGE ( 'NONE', *, *, #85234, .T. ) ;
#41702 = CARTESIAN_POINT ( 'NONE',  ( 99.97821182074206092, -27.16988623491039334, 185.5841967044829630 ) ) ;
#41704 = PLANE ( 'NONE',  #46540 ) ;
#41705 = CARTESIAN_POINT ( 'NONE',  ( 110.7038792373522824, -48.03394190404919328, 203.8241967044819489 ) ) ;
#41706 = AXIS2_PLACEMENT_3D ( 'NONE', #53235, #18750, #46435 ) ;
#41707 = CARTESIAN_POINT ( 'NONE',  ( 99.17101862044538052, 74.81660785136577374, 84.91200770515706608 ) ) ;
#41708 = AXIS2_PLACEMENT_3D ( 'NONE', #7191, #75784, #74886 ) ;
#41709 = DIRECTION ( 'NONE',  ( 0.000000000000000000, 0.000000000000000000, -1.000000000000000000 ) ) ;
#41710 = CARTESIAN_POINT ( 'NONE',  ( 57.56670390244829605, -48.82844715994039575, 293.2178068554150627 ) ) ;
#41711 = VERTEX_POINT ( 'NONE', #79024 ) ;
#41712 = AXIS2_PLACEMENT_3D ( 'NONE', #55011, #41398, #13714 ) ;
#41713 = CONTEXT_DEPENDENT_SHAPE_REPRESENTATION ( #49247, #39478 ) ;
#41714 = EDGE_LOOP ( 'NONE', ( #29603, #42697, #60281, #53324 ) ) ;
#41715 = ORIENTED_EDGE ( 'NONE', *, *, #55064, .T. ) ;
#41716 = ORIENTED_EDGE ( 'NONE', *, *, #63963, .F. ) ;
#41717 = DIRECTION ( 'NONE',  ( 1.000000000000000078E-15, -1.000000000000000083E-30, -1.000000000000000000 ) ) ;
#41718 = CARTESIAN_POINT ( 'NONE',  ( 116.0551108448461264, -42.01026737563550029, 234.4041967044819899 ) ) ;
#41719 = CARTESIAN_POINT ( 'NONE',  ( 151.5667039024483813, -48.82844715993591223, 249.9678068554149490 ) ) ;
#41720 = CARTESIAN_POINT ( 'NONE',  ( 136.5461822395285765, -17.53884010538699201, 2.747932095387902063 ) ) ;
#41722 = DIRECTION ( 'NONE',  ( 0.000000000000000000, 1.000000000000000000, 0.000000000000000000 ) ) ;
#41721 = CARTESIAN_POINT ( 'NONE',  ( 37.56670390244801183, -48.82844715994099971, 300.4678068554150059 ) ) ;
#41723 = DIRECTION ( 'NONE',  ( -1.000000000000000078E-15, -1.000000000000000083E-30, 1.000000000000000000 ) ) ;
#41724 = EDGE_CURVE ( 'NONE', #33505, #38464, #51894, .T. ) ;
#41725 = CARTESIAN_POINT ( 'NONE',  ( 115.9640307963821186, -42.20482783266999149, 18.38705384733896153 ) ) ;
#41726 = ORIENTED_EDGE ( 'NONE', *, *, #7549, .T. ) ;
#41727 = AXIS2_PLACEMENT_3D ( 'NONE', #34073, #41333, #62238 ) ;
#41728 = VERTEX_POINT ( 'NONE', #56305 ) ;
#41729 = CARTESIAN_POINT ( 'NONE',  ( 33.98325472291465132, 17.78000000000000114, -3.174999999999999822 ) ) ;
#41730 = DIRECTION ( 'NONE',  ( -0.7071067811865621167, 0.000000000000000000, 0.7071067811865330288 ) ) ;
#41731 = EDGE_CURVE ( 'NONE', #57559, #39820, #79509, .T. ) ;
#41732 = CARTESIAN_POINT ( 'NONE',  ( 117.4008144674644285, -32.62901037329578458, 245.1270538473389706 ) ) ;
#41733 = DIRECTION ( 'NONE',  ( 0.000000000000000000, 0.000000000000000000, -1.000000000000000000 ) ) ;
#41734 = CARTESIAN_POINT ( 'NONE',  ( 116.4859054502388744, -39.36344060769043551, 94.60991099019594230 ) ) ;
#41735 = CARTESIAN_POINT ( 'NONE',  ( 0.000000000000000000, 127.0000000000000000, 0.000000000000000000 ) ) ;
#41736 = CARTESIAN_POINT ( 'NONE',  ( 97.12555970502634750, -37.99686556195802467, 22.42726576103899916 ) ) ;
#41737 = ORIENTED_EDGE ( 'NONE', *, *, #37022, .T. ) ;
#41738 = CARTESIAN_POINT ( 'NONE',  ( 172.5664832912740110, -9.303447159940999356, 78.92562527591199739 ) ) ;
#41739 = ORIENTED_EDGE ( 'NONE', *, *, #21849, .F. ) ;
#41740 = VERTEX_POINT ( 'NONE', #64048 ) ;
#41741 = CARTESIAN_POINT ( 'NONE',  ( -90.32698471909129978, 90.93965867633430378, 76.79137032886123393 ) ) ;
#41742 = CARTESIAN_POINT ( 'NONE',  ( 114.8460652499425123, -41.03528437643323201, 259.8558690201828654 ) ) ;
#41743 = VECTOR ( 'NONE', #85344, 1000.000000000000000 ) ;
#41744 = CARTESIAN_POINT ( 'NONE',  ( 51.42025729304100423, -33.70561438051981185, -5.074374724088000832 ) ) ;
#41746 = ADVANCED_FACE ( 'NONE', ( #84050 ), #29078, .T. ) ;
#41745 = TOROIDAL_SURFACE ( 'NONE', #66392, 29.50000000000000000, 1.500000000000000000 ) ;
#41747 = CARTESIAN_POINT ( 'NONE',  ( 116.3195061320206207, -32.94150711290046729, 139.1356252759109680 ) ) ;
#41748 = CARTESIAN_POINT ( 'NONE',  ( 97.31584370922533367, -39.30597597294169532, 86.53145860710328918 ) ) ;
#41749 = CARTESIAN_POINT ( 'NONE',  ( 81.76234319299427966, 70.17658267799284033, -85.85227416678121415 ) ) ;
#41750 = ORIENTED_EDGE ( 'NONE', *, *, #42602, .F. ) ;
#41751 = CARTESIAN_POINT ( 'NONE',  ( 53.35959712126282994, -48.62134037875357251, 249.9678068554150343 ) ) ;
#41752 = DIRECTION ( 'NONE',  ( 1.000000000000000078E-15, -1.000000000000000000, 0.000000000000000000 ) ) ;
#41753 = ORIENTED_EDGE ( 'NONE', *, *, #32955, .T. ) ;
#41754 = CARTESIAN_POINT ( 'NONE',  ( 117.4547340842499210, -37.95832963484174627, 53.73276813305394484 ) ) ;
#41755 = ORIENTED_EDGE ( 'NONE', *, *, #2698, .F. ) ;
#41756 = CARTESIAN_POINT ( 'NONE',  ( 101.7271154311333135, -43.54062005560803073, 274.8776141791153691 ) ) ;
#41757 = AXIS2_PLACEMENT_3D ( 'NONE', #67172, #52175, #18577 ) ;
#41758 = ADVANCED_FACE ( 'NONE', ( #21825 ), #71759, .F. ) ;
#41759 = CARTESIAN_POINT ( 'NONE',  ( 136.8164832912739826, -18.72944715994099951, -5.074374724088999145 ) ) ;
#41760 = CARTESIAN_POINT ( 'NONE',  ( 103.1049807579881161, -45.67203811392948865, 177.2441967044829596 ) ) ;
#41761 = LINE ( 'NONE', #83579, #47656 ) ;
#41762 = LINE ( 'NONE', #14983, #89741 ) ;
#41763 = PLANE ( 'NONE',  #28873 ) ;
#41764 = AXIS2_PLACEMENT_3D ( 'NONE', #81167, #27077, #53848 ) ;
#41765 = CARTESIAN_POINT ( 'NONE',  ( 1.925672578516905147E-22, 69.84999999999999432, 130.5560000000000116 ) ) ;
#41766 = CARTESIAN_POINT ( 'NONE',  ( 100.6295653500825154, -44.98529764103543727, 228.0499109901969348 ) ) ;
#41767 = CARTESIAN_POINT ( 'NONE',  ( 78.95047879920406331, 93.33860577356860233, -88.44471653959740820 ) ) ;
#41768 = ORIENTED_EDGE ( 'NONE', *, *, #56860, .F. ) ;
#41769 = CARTESIAN_POINT ( 'NONE',  ( 172.5664832912729878, -27.82844715994070484, 138.9256252759119832 ) ) ;
#41770 = VERTEX_POINT ( 'NONE', #16788 ) ;
#41771 = CARTESIAN_POINT ( 'NONE',  ( 97.57754503199339524, -30.97118795507763167, 121.8803871806729546 ) ) ;
#41772 = DIRECTION ( 'NONE',  ( -4.237773401492740281E-14, 1.000000000000000000, 0.000000000000000000 ) ) ;
#41773 = ORIENTED_EDGE ( 'NONE', *, *, #23367, .F. ) ;
#41774 = ORIENTED_EDGE ( 'NONE', *, *, #44649, .F. ) ;
#41775 = ORIENTED_EDGE ( 'NONE', *, *, #16373, .T. ) ;
#41776 = AXIS2_PLACEMENT_3D ( 'NONE', #53160, #86386, #11415 ) ;
#41777 = CARTESIAN_POINT ( 'NONE',  ( 99.09571867114192401, -30.55041957953722687, 266.8022907182795507 ) ) ;
#41778 = LINE ( 'NONE', #51275, #22598 ) ;
#41779 = DIRECTION ( 'NONE',  ( 0.000000000000000000, 1.000000000000000000, 0.000000000000000000 ) ) ;
#41780 = DIRECTION ( 'NONE',  ( -0.7071067811865253683, 0.7071067811865696662, -7.071067811865261355E-16 ) ) ;
#41781 = EDGE_CURVE ( 'NONE', #43903, #32539, #43579, .T. ) ;
#41782 = CARTESIAN_POINT ( 'NONE',  ( 115.2023469127646820, -39.68048904007974897, 171.3557094172109885 ) ) ;
#41783 = CARTESIAN_POINT ( 'NONE',  ( 105.8911342260945645, -47.14568079332288875, 278.4870538473395527 ) ) ;
#41784 = CARTESIAN_POINT ( 'NONE',  ( 163.0667039024470171, -33.35206098992711077, -5.074374724088000832 ) ) ;
#41785 = ORIENTED_EDGE ( 'NONE', *, *, #43636, .T. ) ;
#41786 = FACE_OUTER_BOUND ( 'NONE', #71433, .T. ) ;
#41787 = CIRCLE ( 'NONE', #20029, 25.39999999999999858 ) ;
#41788 = CARTESIAN_POINT ( 'NONE',  ( 68.91674821478362389, 82.54999999999999716, 68.91674821478530077 ) ) ;
#41789 = ORIENTED_EDGE ( 'NONE', *, *, #39118, .T. ) ;
#41790 = ORIENTED_EDGE ( 'NONE', *, *, #67620, .F. ) ;
#41791 = DIRECTION ( 'NONE',  ( 2.900000000000000265E-14, -2.000000000000000155E-15, 1.000000000000000000 ) ) ;
#41792 = CARTESIAN_POINT ( 'NONE',  ( 19.56670390244796920, -67.87844715994100397, 300.9178068554150514 ) ) ;
#41793 = CARTESIAN_POINT ( 'NONE',  ( 113.2454827304145226, -28.75865971940361376, 14.55229357420379976 ) ) ;
#41794 = CARTESIAN_POINT ( 'NONE',  ( 138.8167039024479834, -57.40094715994099772, 35.51780685541480409 ) ) ;
#41795 = FACE_OUTER_BOUND ( 'NONE', #48868, .T. ) ;
#41796 = CARTESIAN_POINT ( 'NONE',  ( 98.86656133049426387, -40.57313681482517609, 211.0857531614099685 ) ) ;
#41797 = CARTESIAN_POINT ( 'NONE',  ( 115.6098187009959304, -42.78073513203698042, 53.33562527591095659 ) ) ;
#41798 = VERTEX_POINT ( 'NONE', #44021 ) ;
#41800 = EDGE_CURVE ( 'NONE', #43325, #34061, #84513, .T. ) ;
#41799 = CARTESIAN_POINT ( 'NONE',  ( 37.36643805256647966, -48.62818131006027755, 180.4678068554150911 ) ) ;
#41801 = ORIENTED_EDGE ( 'NONE', *, *, #59814, .T. ) ;
#41802 = EDGE_CURVE ( 'NONE', #78558, #9584, #63535, .T. ) ;
#41803 = CARTESIAN_POINT ( 'NONE',  ( -82.64146475440728068, 69.93366089391892615, -85.00925061400963045 ) ) ;
#41804 = ORIENTED_EDGE ( 'NONE', *, *, #74250, .F. ) ;
#41805 = PLANE ( 'NONE',  #57732 ) ;
#41806 = EDGE_LOOP ( 'NONE', ( #73183, #37147, #67728, #87270, #72186, #78367 ) ) ;
#41807 = CARTESIAN_POINT ( 'NONE',  ( 116.3181387014812458, -32.94505625723229514, 15.13562527591094664 ) ) ;
#41808 = CARTESIAN_POINT ( 'NONE',  ( 68.92500634596476061, -138.9257026229574876, 247.5112265945679724 ) ) ;
#41809 = CARTESIAN_POINT ( 'NONE',  ( 68.18539514011786196, -127.7157332097851850, 247.4308639981159956 ) ) ;
#41811 = DIRECTION ( 'NONE',  ( -1.000000000000000000, 0.000000000000000000, 7.043400939473319300E-33 ) ) ;
#41810 = AXIS2_PLACEMENT_3D ( 'NONE', #11917, #16949, #80977 ) ;
#41812 = EDGE_LOOP ( 'NONE', ( #22093, #52043, #87050, #70763 ) ) ;
#41813 = AXIS2_PLACEMENT_3D ( 'NONE', #81191, #39380, #32111 ) ;
#41814 = CARTESIAN_POINT ( 'NONE',  ( 97.75265732597522117, -31.99668793782200993, 50.95276813305294183 ) ) ;
#41816 = CARTESIAN_POINT ( 'NONE',  ( 99.18073718829404584, 74.80151635532864418, -84.90151352399627172 ) ) ;
#41815 = DIRECTION ( 'NONE',  ( 0.000000000000000000, 0.000000000000000000, -1.000000000000000000 ) ) ;
#41817 = LINE ( 'NONE', #42273, #9046 ) ;
#41818 = CARTESIAN_POINT ( 'NONE',  ( 131.3164832912739826, -18.72944715994100662, 3.101481641215524832 ) ) ;
#41819 = ORIENTED_EDGE ( 'NONE', *, *, #17984, .T. ) ;
#41820 = AXIS2_PLACEMENT_3D ( 'NONE', #37317, #32270, #53590 ) ;
#41821 = CARTESIAN_POINT ( 'NONE',  ( 107.0667039024470313, -104.2784471599420755, -19.78219314458201694 ) ) ;
#41822 = CONICAL_SURFACE ( 'NONE', #72329, 16.00000000000090239, 0.7853981633974503884 ) ;
#41823 = CARTESIAN_POINT ( 'NONE',  ( 210.2301280605339855, 25.81350000000000477, -7.937500000000000000 ) ) ;
#41824 = CARTESIAN_POINT ( 'NONE',  ( 4.880114330320866500, 70.80325516146916698, 118.4573640576558660 ) ) ;
#41825 = EDGE_LOOP ( 'NONE', ( #78302, #4029, #47736, #38430 ) ) ;
#41826 = CARTESIAN_POINT ( 'NONE',  ( 113.9312237880395600, -28.03689036367077492, 120.5565776568639507 ) ) ;
#41827 = VECTOR ( 'NONE', #32211, 1000.000000000000114 ) ;
#41829 = DIRECTION ( 'NONE',  ( 0.000000000000000000, 0.000000000000000000, 1.000000000000000000 ) ) ;
#41828 = DIRECTION ( 'NONE',  ( 1.000000000000000000, 0.000000000000000000, 0.000000000000000000 ) ) ;
#41830 = DIRECTION ( 'NONE',  ( -3.100000000000000258E-29, 3.100000000000000044E-14, 1.000000000000000000 ) ) ;
#41831 = LINE ( 'NONE', #7342, #37558 ) ;
#41832 = ADVANCED_FACE ( 'NONE', ( #71318 ), #37229, .F. ) ;
#41833 = CARTESIAN_POINT ( 'NONE',  ( 117.0460787713798965, -39.54838250520747778, 139.6194347997199827 ) ) ;
#41834 = AXIS2_PLACEMENT_3D ( 'NONE', #73873, #24395, #37578 ) ;
#41836 = ORIENTED_EDGE ( 'NONE', *, *, #72850, .T. ) ;
#41835 = FACE_OUTER_BOUND ( 'NONE', #47259, .T. ) ;
#41837 = CARTESIAN_POINT ( 'NONE',  ( 105.6350724880777534, -47.03380199863519806, 253.4670538473393719 ) ) ;
#41838 = DIRECTION ( 'NONE',  ( 0.4214249218767882055, 0.9068632946707806397, 4.214249218767890910E-16 ) ) ;
#41839 = LINE ( 'NONE', #83215, #48967 ) ;
#41840 = DIRECTION ( 'NONE',  ( -1.000000000000000000, -8.741913579725640327E-16, -1.514143847546115117E-15 ) ) ;
#41841 = DIRECTION ( 'NONE',  ( 0.000000000000000000, 1.000000000000000000, 0.000000000000000000 ) ) ;
#41842 = FACE_OUTER_BOUND ( 'NONE', #64310, .T. ) ;
#41843 = DIRECTION ( 'NONE',  ( 0.000000000000000000, 0.000000000000000000, -1.000000000000000000 ) ) ;
#41844 = CARTESIAN_POINT ( 'NONE',  ( 116.5710038106515611, -34.42130396933979597, 209.0156252759109634 ) ) ;
#41845 = ORIENTED_EDGE ( 'NONE', *, *, #50957, .T. ) ;
#41846 = ORIENTED_EDGE ( 'NONE', *, *, #18812, .T. ) ;
#41847 = AXIS2_PLACEMENT_3D ( 'NONE', #34145, #34601, #28689 ) ;
#41848 = CARTESIAN_POINT ( 'NONE',  ( 97.67166470235704878, -36.60562237181873257, 152.7596785439919813 ) ) ;
#41849 = CARTESIAN_POINT ( 'NONE',  ( 116.3183510266638336, -32.94967450325654568, 119.1356252759109537 ) ) ;
#41850 = EDGE_CURVE ( 'NONE', #48266, #21668, #59233, .T. ) ;
#41851 = CARTESIAN_POINT ( 'NONE',  ( 105.4490071354754406, -45.46730099742844544, 8.861583305896925111 ) ) ;
#41852 = PLANE ( 'NONE',  #69572 ) ;
#41853 = ADVANCED_FACE ( 'NONE', ( #46696 ), #10854, .T. ) ;
#41854 = DIRECTION ( 'NONE',  ( 1.000000000000000000, 1.816601132648505598E-15, 0.000000000000000000 ) ) ;
#41855 = EDGE_CURVE ( 'NONE', #9196, #88510, #44916, .T. ) ;
#41856 = LINE ( 'NONE', #7365, #77777 ) ;
#41857 = CARTESIAN_POINT ( 'NONE',  ( 177.8371591254543489, -47.82818131005477369, 249.9678068554149775 ) ) ;
#41858 = CARTESIAN_POINT ( 'NONE',  ( -148.0533267522759786, 101.5999999999999943, -160.2664750769289697 ) ) ;
#41859 = CARTESIAN_POINT ( 'NONE',  ( 98.85650974919595058, -29.36329775763224603, 235.7565776568629872 ) ) ;
#41860 = CARTESIAN_POINT ( 'NONE',  ( 98.34975502646139489, -31.65672867875580465, 170.9057125034062778 ) ) ;
#41861 = VERTEX_POINT ( 'NONE', #79922 ) ;
#41862 = ORIENTED_EDGE ( 'NONE', *, *, #1168, .T. ) ;
#41863 = ADVANCED_FACE ( 'NONE', ( #4040 ), #58547, .F. ) ;
#41864 = EDGE_CURVE ( 'NONE', #19262, #13968, #69377, .T. ) ;
#41865 = DIRECTION ( 'NONE',  ( -4.237773401492740281E-14, 1.000000000000000000, 0.000000000000000000 ) ) ;
#41866 = CARTESIAN_POINT ( 'NONE',  ( 82.77032304066598556, -19.23127003359734744, 6.817519769821898556 ) ) ;
#41867 = FACE_OUTER_BOUND ( 'NONE', #46793, .T. ) ;
#41868 = DIRECTION ( 'NONE',  ( 1.000000000000000078E-15, 1.000000000000000083E-30, -1.000000000000000000 ) ) ;
#41869 = EDGE_CURVE ( 'NONE', #58184, #77506, #32631, .T. ) ;
#41871 = FACE_OUTER_BOUND ( 'NONE', #27481, .T. ) ;
#41870 = VECTOR ( 'NONE', #50450, 1000.000000000000000 ) ;
#41872 = EDGE_CURVE ( 'NONE', #7655, #37616, #14092, .T. ) ;
#41873 = VERTEX_POINT ( 'NONE', #72647 ) ;
#41874 = CARTESIAN_POINT ( 'NONE',  ( 96.64589536673427972, -32.90729728488415162, 17.03467289495896964 ) ) ;
#41875 = EDGE_CURVE ( 'NONE', #20346, #12139, #70404, .T. ) ;
#41876 = CARTESIAN_POINT ( 'NONE',  ( 96.77592423366979801, -40.76472679528808385, 246.6118157521009664 ) ) ;
#41877 = VERTEX_POINT ( 'NONE', #81264 ) ;
#41878 = VECTOR ( 'NONE', #5027, 1000.000000000000000 ) ;
#41879 = CARTESIAN_POINT ( 'NONE',  ( 77.59226090854122049, -37.93375462384054941, 7.110117206087036124 ) ) ;
#41880 = ADVANCED_FACE ( 'NONE', ( #4936 ), #80360, .T. ) ;
#41881 = DIRECTION ( 'NONE',  ( -2.900000000000000265E-14, 2.000000000000000155E-15, -1.000000000000000000 ) ) ;
#41882 = CARTESIAN_POINT ( 'NONE',  ( 110.8548770769551908, -45.98407163414527332, 167.8856600767107352 ) ) ;
#41883 = EDGE_CURVE ( 'NONE', #54294, #76096, #72256, .T. ) ;
#41884 = CARTESIAN_POINT ( 'NONE',  ( 113.4406056323916090, -42.58363279299825876, 76.04142370292498754 ) ) ;
#41885 = CARTESIAN_POINT ( 'NONE',  ( 101.7584646134851596, -45.72734648786122591, 158.1527681330539963 ) ) ;
#41886 = DIRECTION ( 'NONE',  ( 1.000000000000000000, 0.000000000000000000, 0.000000000000000000 ) ) ;
#41887 = ORIENTED_EDGE ( 'NONE', *, *, #60535, .T. ) ;
#41888 = AXIS2_PLACEMENT_3D ( 'NONE', #6209, #68876, #89331 ) ;
#41889 = CARTESIAN_POINT ( 'NONE',  ( 41.56648329127499153, -36.32844715994070839, 323.6756252759119548 ) ) ;
#41890 = EDGE_LOOP ( 'NONE', ( #66698, #46299 ) ) ;
#41891 = ORIENTED_EDGE ( 'NONE', *, *, #26429, .T. ) ;
#41892 = CARTESIAN_POINT ( 'NONE',  ( 33.91903122894391487, -35.91149509761189762, 117.4678068554150485 ) ) ;
#41893 = VERTEX_POINT ( 'NONE', #51723 ) ;
#41894 = ORIENTED_EDGE ( 'NONE', *, *, #58672, .F. ) ;
#41895 = DIRECTION ( 'NONE',  ( 0.000000000000000000, 0.000000000000000000, 1.000000000000000000 ) ) ;
#41896 = B_SPLINE_CURVE_WITH_KNOTS ( 'NONE', 3,
 ( #63860, #85214, #16159, #1640, #43837, #29340, #37038, #64743, #42487, #77040, #23432, #44276, #78839, #51099, #9780, #65189, #2968, #30667 ),
 .UNSPECIFIED., .F., .F.,
 ( 4, 2, 2, 2, 2, 2, 2, 2, 4 ),
 ( 0.000000000000000000, 0.06249999992548026240, 0.1249999998509605248, 0.1874999997764407733, 0.2499999997019210496, 0.3124999996274013259, 0.3749999995528815466, 0.4374999994783618229, 0.4999999994038420992 ),
 .UNSPECIFIED. ) ;
#41897 = CIRCLE ( 'NONE', #28912, 3.000000000000002665 ) ;
#41898 = CARTESIAN_POINT ( 'NONE',  ( 113.7363519267670995, -42.85525508308114695, 77.64575316141092287 ) ) ;
#41899 = CARTESIAN_POINT ( 'NONE',  ( 97.89977465614410335, -41.74121498826879417, 221.7241967044819546 ) ) ;
#41900 = ADVANCED_FACE ( 'NONE', ( #65381 ), #11755, .F. ) ;
#41901 = CARTESIAN_POINT ( 'NONE',  ( 97.07914014679025172, -41.41098531455293141, 211.6632443235299945 ) ) ;
#41903 = EDGE_CURVE ( 'NONE', #88510, #8874, #3596, .T. ) ;
#41902 = CARTESIAN_POINT ( 'NONE',  ( 106.9276426037745011, -26.29176787048590214, 56.08705384733997334 ) ) ;
#41904 = DIRECTION ( 'NONE',  ( 0.7071067811578790607, 0.7071067812152160847, 0.000000000000000000 ) ) ;
#41905 = DIRECTION ( 'NONE',  ( -4.299999999999999979E-14, 1.000000000000000000, -4.400000000000000367E-29 ) ) ;
#41906 = EDGE_CURVE ( 'NONE', #23939, #14672, #51565, .T. ) ;
#41907 = VERTEX_POINT ( 'NONE', #10683 ) ;
#41908 = CARTESIAN_POINT ( 'NONE',  ( 117.0718954859017629, -35.46248235935014748, 178.9272919423596591 ) ) ;
#41909 = EDGE_CURVE ( 'NONE', #38962, #60267, #51957, .T. ) ;
#41910 = CARTESIAN_POINT ( 'NONE',  ( 152.0371591254585155, -47.82818131005588214, 193.9678068554149775 ) ) ;
#41911 = CARTESIAN_POINT ( 'NONE',  ( 70.78827404651126187, -139.2284154368976488, 247.4607008287169094 ) ) ;
#41912 = VECTOR ( 'NONE', #50246, 999.9999999999998863 ) ;
#41913 = CARTESIAN_POINT ( 'NONE',  ( 113.5922197990811213, -29.44396856740769408, 114.4956252759109816 ) ) ;
#41914 = CARTESIAN_POINT ( 'NONE',  ( 115.3018890743646665, -44.17195851134204077, 83.25372051400698581 ) ) ;
#41915 = CARTESIAN_POINT ( 'NONE',  ( 101.2695147780440266, -26.33598991146258328, 255.4813395616251626 ) ) ;
#41916 = EDGE_LOOP ( 'NONE', ( #65258, #33562 ) ) ;
#41917 = CARTESIAN_POINT ( 'NONE',  ( 109.9602307476630330, -48.22147533147688847, 242.7727681330539724 ) ) ;
#41918 = DIRECTION ( 'NONE',  ( 0.000000000000000000, -1.000000000000000000, 0.000000000000000000 ) ) ;
#41919 =( LENGTH_UNIT ( ) NAMED_UNIT ( * ) SI_UNIT ( .MILLI., .METRE. ) );
#41920 = CARTESIAN_POINT ( 'NONE',  ( 10.66920567967061650, 75.66061691139891821, 130.1193289296744524 ) ) ;
#41921 = DIRECTION ( 'NONE',  ( 3.100000000000000258E-29, -3.100000000000000044E-14, -1.000000000000000000 ) ) ;
#41923 = DIRECTION ( 'NONE',  ( 0.000000000000000000, 0.000000000000000000, 1.000000000000000000 ) ) ;
#41922 = LINE ( 'NONE', #63283, #68019 ) ;
#41924 = CARTESIAN_POINT ( 'NONE',  ( 63.56670390244796920, -40.82844715994016127, 300.4678068554150627 ) ) ;
#41925 = CARTESIAN_POINT ( 'NONE',  ( 141.3509999999999991, 0.000000000000000000, 132.7150000000000034 ) ) ;
#41926 = DIRECTION ( 'NONE',  ( 0.000000000000000000, -1.000000000000000000, 0.000000000000000000 ) ) ;
#41927 = DIRECTION ( 'NONE',  ( 0.000000000000000000, -1.000000000000000000, 1.682382052829014912E-15 ) ) ;
#41928 = CARTESIAN_POINT ( 'NONE',  ( 113.2375375036158403, -28.75258929711289468, 39.55219311040522001 ) ) ;
#41929 = CARTESIAN_POINT ( 'NONE',  ( 96.20012047777625241, -115.5046222945366310, -11.78219314458164924 ) ) ;
#41931 = VERTEX_POINT ( 'NONE', #17070 ) ;
#41930 = CYLINDRICAL_SURFACE ( 'NONE', #80587, 4.749999999999976907 ) ;
#41932 = VECTOR ( 'NONE', #7112, 1000.000000000000000 ) ;
#41933 = DIRECTION ( 'NONE',  ( 1.000000000000000078E-15, -1.000000000000000083E-30, -1.000000000000000000 ) ) ;
#41934 = CARTESIAN_POINT ( 'NONE',  ( 106.1363778353814666, -47.76712558329867875, 262.4975300378158067 ) ) ;
#41935 = CARTESIAN_POINT ( 'NONE',  ( 107.6529936739636639, -47.12767891731729009, 148.6213395616249784 ) ) ;
#41936 = CARTESIAN_POINT ( 'NONE',  ( 115.7313686325390876, -42.60420177353093862, 269.3527681330536439 ) ) ;
#41937 = DIRECTION ( 'NONE',  ( 0.000000000000000000, 1.000000000000000000, 0.000000000000000000 ) ) ;
#41939 = CARTESIAN_POINT ( 'NONE',  ( 81.78920663580979067, -34.57943358556376978, 7.744922197170968303 ) ) ;
#41938 = CARTESIAN_POINT ( 'NONE',  ( 1.387778780781445676E-14, 223.9999999999999716, 97.27542076772557778 ) ) ;
#41940 = CARTESIAN_POINT ( 'NONE',  ( 107.0664832912739399, -36.72944715994095333, 357.5272416190308604 ) ) ;
#41941 = DIRECTION ( 'NONE',  ( 1.000000000000000078E-15, 0.000000000000000000, 1.000000000000000000 ) ) ;
#41942 = AXIS2_PLACEMENT_3D ( 'NONE', #55791, #14049, #83546 ) ;
#41943 = CIRCLE ( 'NONE', #86901, 7.937500000000000000 ) ;
#41944 = VERTEX_POINT ( 'NONE', #85242 ) ;
#41945 = DIRECTION ( 'NONE',  ( -2.900000000000000265E-14, 2.000000000000000155E-15, -1.000000000000000000 ) ) ;
#41946 = ORIENTED_EDGE ( 'NONE', *, *, #14847, .T. ) ;
#41947 = CARTESIAN_POINT ( 'NONE',  ( 106.9915265980828849, -45.27055441931952373, 186.9924198280769758 ) ) ;
#41948 = AXIS2_PLACEMENT_3D ( 'NONE', #54498, #20473, #67714 ) ;
#41950 = EDGE_LOOP ( 'NONE', ( #89311, #71444, #84698, #21389 ) ) ;
#41949 = CARTESIAN_POINT ( 'NONE',  ( 116.7934678734580132, -39.39373051261830483, 188.6148988220920444 ) ) ;
#41951 = CARTESIAN_POINT ( 'NONE',  ( 135.3838309168194485, -60.54606547621062163, 394.9756252759104314 ) ) ;
#41952 = CARTESIAN_POINT ( 'NONE',  ( 111.4081670832168953, -47.72935575799004226, 168.8756252759109486 ) ) ;
#41953 = DIRECTION ( 'NONE',  ( 0.000000000000000000, 0.000000000000000000, -1.000000000000000000 ) ) ;
#41954 = PLANE ( 'NONE',  #10963 ) ;
#41955 = CARTESIAN_POINT ( 'NONE',  ( -7.941868552260229762E-13, 120.6499999999999915, 107.7702177616926065 ) ) ;
#41956 = LINE ( 'NONE', #48769, #63603 ) ;
#41957 = CYLINDRICAL_SURFACE ( 'NONE', #72978, 12.44599999999999795 ) ;
#41958 = AXIS2_PLACEMENT_3D ( 'NONE', #81073, #5652, #47400 ) ;
#41959 = CARTESIAN_POINT ( 'NONE',  ( 116.9446180447427821, -41.83184233209006209, 93.44705384733997278 ) ) ;
#41960 = VERTEX_POINT ( 'NONE', #44307 ) ;
#41961 = EDGE_LOOP ( 'NONE', ( #32188, #33794, #89054, #66461, #38441, #2550 ) ) ;
#41962 = EDGE_LOOP ( 'NONE', ( #85431, #9860, #81447 ) ) ;
#41963 = CARTESIAN_POINT ( 'NONE',  ( 112.5007446479794453, -45.21116328700192355, 64.46158330589696561 ) ) ;
#41964 = DIRECTION ( 'NONE',  ( 0.9068632946707805287, -0.4214249218767882610, 1.035655806553318316E-15 ) ) ;
#41966 = CARTESIAN_POINT ( 'NONE',  ( 0.000000000000000000, 44.45000000000000284, 0.000000000000000000 ) ) ;
#41965 = CARTESIAN_POINT ( 'NONE',  ( 99.06478422775796844, -31.10483629442216014, 201.8384824187669437 ) ) ;
#41967 = DIRECTION ( 'NONE',  ( 0.000000000000000000, 1.000000000000000000, 0.000000000000000000 ) ) ;
#41968 = EDGE_CURVE ( 'NONE', #22318, #61315, #33125, .T. ) ;
#41969 = DIRECTION ( 'NONE',  ( 0.000000000000000000, -1.000000000000000000, 0.000000000000000000 ) ) ;
#41970 = EDGE_CURVE ( 'NONE', #74884, #56872, #38388, .T. ) ;
#41971 = CIRCLE ( 'NONE', #34790, 4.750000000000004441 ) ;
#41972 = DIRECTION ( 'NONE',  ( 0.000000000000000000, 1.000000000000000000, 0.000000000000000000 ) ) ;
#41973 = ADVANCED_FACE ( 'NONE', ( #17517 ), #23010, .F. ) ;
#41974 = DIRECTION ( 'NONE',  ( 0.000000000000000000, 0.000000000000000000, -1.000000000000000000 ) ) ;
#41975 = DIRECTION ( 'NONE',  ( 1.639958061481212836E-42, -4.100000000000000342E-29, -1.000000000000000000 ) ) ;
#41976 = CARTESIAN_POINT ( 'NONE',  ( 117.6568287320716877, -39.81301747186228113, 138.5889586092439743 ) ) ;
#41977 = ORIENTED_EDGE ( 'NONE', *, *, #10942, .T. ) ;
#41978 = EDGE_LOOP ( 'NONE', ( #71236, #37594, #84351, #77786 ) ) ;
#41979 = ORIENTED_EDGE ( 'NONE', *, *, #43004, .T. ) ;
#41980 = EDGE_CURVE ( 'NONE', #19751, #48239, #51999, .T. ) ;
#41981 = EDGE_CURVE ( 'NONE', #10481, #77722, #75202, .T. ) ;
#41982 = CARTESIAN_POINT ( 'NONE',  ( 4.879617406430184268, 70.80304812169737261, 130.4664555583633501 ) ) ;
#41983 = CARTESIAN_POINT ( 'NONE',  ( -98.82361644294738312, 90.93081950567959382, -85.31607583734439970 ) ) ;
#41984 = DIRECTION ( 'NONE',  ( 1.000000000000000078E-15, -1.000000000000000083E-30, -1.000000000000000000 ) ) ;
#41985 = CARTESIAN_POINT ( 'NONE',  ( 100.3991921706488171, -43.18259834960616672, 189.7566617981629804 ) ) ;
#41986 = AXIS2_PLACEMENT_3D ( 'NONE', #6913, #63674, #42310 ) ;
#41987 = EDGE_CURVE ( 'NONE', #13081, #686, #12969, .T. ) ;
#41988 = FACE_OUTER_BOUND ( 'NONE', #61837, .T. ) ;
#41989 = EDGE_CURVE ( 'NONE', #78359, #21095, #8500, .T. ) ;
#41990 = CARTESIAN_POINT ( 'NONE',  ( 76.06670390244792657, -14.72944715994109899, 239.5838068554169809 ) ) ;
#41991 = VERTEX_POINT ( 'NONE', #58829 ) ;
#41993 = EDGE_LOOP ( 'NONE', ( #48880, #56507, #68933, #61060 ) ) ;
#41992 = ORIENTED_EDGE ( 'NONE', *, *, #21263, .F. ) ;
#41994 = AXIS2_PLACEMENT_3D ( 'NONE', #63329, #22013, #49685 ) ;
#41995 = FACE_BOUND ( 'NONE', #49343, .T. ) ;
#41996 = VERTEX_POINT ( 'NONE', #24772 ) ;
#41997 = ORIENTED_EDGE ( 'NONE', *, *, #4777, .T. ) ;
#41998 = CARTESIAN_POINT ( 'NONE',  ( 78.21292805808276682, -20.76093376058618389, 7.655955902700432247 ) ) ;
#41999 = EDGE_CURVE ( 'NONE', #55592, #15222, #86565, .T. ) ;
#42000 = CARTESIAN_POINT ( 'NONE',  ( 107.4435086560219474, -45.58304137281263024, 234.0415833058969781 ) ) ;
#42001 = AXIS2_PLACEMENT_3D ( 'NONE', #61496, #20628, #61945 ) ;
#42002 = DIRECTION ( 'NONE',  ( 0.7071067811865474617, 0.000000000000000000, 0.7071067811865474617 ) ) ;
#42003 = ORIENTED_EDGE ( 'NONE', *, *, #36048, .T. ) ;
#42004 = CARTESIAN_POINT ( 'NONE',  ( 194.0371591254582313, -46.82818131005407736, 313.9678068554149490 ) ) ;
#42005 = ADVANCED_FACE ( 'NONE', ( #8935 ), #64774, .T. ) ;
#42006 = CARTESIAN_POINT ( 'NONE',  ( -123.0424546654431452, 73.33497890737675107, 43.65123806753916114 ) ) ;
#42007 = VECTOR ( 'NONE', #28755, 1000.000000000000000 ) ;
#42008 = VERTEX_POINT ( 'NONE', #57948 ) ;
#42010 = ORIENTED_EDGE ( 'NONE', *, *, #3023, .T. ) ;
#42009 = CIRCLE ( 'NONE', #27494, 15.50000000000000000 ) ;
#42011 = DIRECTION ( 'NONE',  ( -0.7071067811864691910, -0.7071067811866257324, -7.071067811864685486E-16 ) ) ;
#42012 = VERTEX_POINT ( 'NONE', #85683 ) ;
#42013 = EDGE_LOOP ( 'NONE', ( #87849, #18350, #65683, #41294 ) ) ;
#42014 = B_SPLINE_CURVE_WITH_KNOTS ( 'NONE', 3,
 ( #67420, #32904, #60603, #88343, #26103, #53772, #81538, #46962, #74693, #73799, #12474, #5666, #67880, #38827, #61057, #33805, #61499, #88788, #26544, #54217, #81978, #19727, #47416, #75144, #54663, #25196, #12928, #4321, #32009, #46064, #82430 ),
 .UNSPECIFIED., .F., .F.,
 ( 4, 2, 2, 1, 2, 2, 2, 2, 2, 2, 2, 1, 1, 2, 2, 2, 4 ),
 ( 0.000000000000000000, 0.1250000000000155431, 0.1875000000000143219, 0.2187500000000218991, 0.2343750000000257017, 0.2500000000000294764, 0.3750000000000295874, 0.4375000000000235367, 0.5000000000000174305, 0.6249999999999963363, 0.6874999999999857891, 0.7187499999999805711, 0.7343749999999779066, 0.7421874999999765743, 0.7499999999999752420, 0.8749999999999876765, 1.000000000000000000 ),
 .UNSPECIFIED. ) ;
#42015 = CARTESIAN_POINT ( 'NONE',  ( 115.1807610290764075, -35.84162759104140150, 276.7309475124485516 ) ) ;
#42016 = AXIS2_PLACEMENT_3D ( 'NONE', #63817, #1595, #84724 ) ;
#42017 = CARTESIAN_POINT ( 'NONE',  ( 104.9583746955643448, -25.04227923723010463, 125.2184824187689856 ) ) ;
#42018 = CARTESIAN_POINT ( 'NONE',  ( 118.8789388927533111, -36.16900092901214947, 118.8641967044819836 ) ) ;
#42019 = DIRECTION ( 'NONE',  ( -1.000000000000000078E-15, 1.000000000000000083E-30, 1.000000000000000000 ) ) ;
#42020 = CARTESIAN_POINT ( 'NONE',  ( 62.03742497533751532, -23.42844715994041849, 249.9678068554150343 ) ) ;
#42021 = CARTESIAN_POINT ( 'NONE',  ( 106.9404422130490815, -47.78196244520037084, 228.5794347997199907 ) ) ;
#42022 = CARTESIAN_POINT ( 'NONE',  ( -47.02966122971773189, 65.60000000000000853, 35.44631899411619003 ) ) ;
#42023 = CARTESIAN_POINT ( 'NONE',  ( 107.0664832912739257, -50.04551884050745514, 305.7141315223800007 ) ) ;
#42024 = ORIENTED_EDGE ( 'NONE', *, *, #35421, .T. ) ;
#42025 = CARTESIAN_POINT ( 'NONE',  ( 130.5150461639146044, 70.27756284692561906, 3.294108455004394642 ) ) ;
#42026 = ORIENTED_EDGE ( 'NONE', *, *, #20290, .F. ) ;
#42027 = EDGE_CURVE ( 'NONE', #58396, #45292, #25865, .T. ) ;
#42028 = ORIENTED_EDGE ( 'NONE', *, *, #34364, .T. ) ;
#42029 = CIRCLE ( 'NONE', #2889, 0.5000000000000004441 ) ;
#42030 = DIRECTION ( 'NONE',  ( -1.000000000000000000, 0.000000000000000000, 0.000000000000000000 ) ) ;
#42031 = ADVANCED_FACE ( 'NONE', ( #67435 ), #19746, .T. ) ;
#42032 = FACE_OUTER_BOUND ( 'NONE', #19574, .T. ) ;
#42033 = ORIENTED_EDGE ( 'NONE', *, *, #68571, .F. ) ;
#42034 = CARTESIAN_POINT ( 'NONE',  ( 104.9628152733504720, -25.06689740840304381, 125.2184824187689856 ) ) ;
#42035 = CARTESIAN_POINT ( 'NONE',  ( 71.77848634863079269, 127.0000000000000000, 77.39114642429989033 ) ) ;
#42036 = LINE ( 'NONE', #7534, #1477 ) ;
#42037 = DIRECTION ( 'NONE',  ( 4.299999999999999979E-14, -1.000000000000000000, 4.400000000000000367E-29 ) ) ;
#42040 = CARTESIAN_POINT ( 'NONE',  ( 106.2286657330468245, -47.72771449247510844, 263.5280062282920994 ) ) ;
#42039 = DIRECTION ( 'NONE',  ( 0.9242245927363031965, 0.3818493186865917766, 0.000000000000000000 ) ) ;
#42038 = DIRECTION ( 'NONE',  ( 2.170915417798913171E-16, 0.000000000000000000, 1.000000000000000000 ) ) ;
#42041 = LINE ( 'NONE', #7983, #17656 ) ;
#42042 = FACE_BOUND ( 'NONE', #80231, .T. ) ;
#42043 = ORIENTED_EDGE ( 'NONE', *, *, #62090, .T. ) ;
#42044 = AXIS2_PLACEMENT_3D ( 'NONE', #66505, #86531, #4294 ) ;
#42045 = DIRECTION ( 'NONE',  ( 0.000000000000000000, 0.000000000000000000, 1.000000000000000000 ) ) ;
#42046 = CARTESIAN_POINT ( 'NONE',  ( 87.31648329127402519, -56.72944715994104570, 14.67562527591095112 ) ) ;
#42047 = DIRECTION ( 'NONE',  ( 0.000000000000000000, 0.000000000000000000, 1.000000000000000000 ) ) ;
#42048 = CARTESIAN_POINT ( 'NONE',  ( -72.96458098368751166, 127.0000000000000000, 80.10833098368618721 ) ) ;
#42050 = ORIENTED_EDGE ( 'NONE', *, *, #79660, .F. ) ;
#42049 = CARTESIAN_POINT ( 'NONE',  ( 117.5632142390390555, -36.54506796471968499, 288.8413395616251478 ) ) ;
#42051 = LINE ( 'NONE', #43392, #78553 ) ;
#42052 = CARTESIAN_POINT ( 'NONE',  ( 102.0711994968067984, -27.55373892369285826, 145.4727681330539610 ) ) ;
#42053 = CARTESIAN_POINT ( 'NONE',  ( 116.7270850375765576, -31.35852969783502786, 25.24229194257798881 ) ) ;
#42054 = CARTESIAN_POINT ( 'NONE',  ( 107.6554453082189013, -47.17114389581161049, 148.6213395616249784 ) ) ;
#42055 = CARTESIAN_POINT ( 'NONE',  ( 107.0667039024467613, -36.72944715994091780, 196.8538068554170195 ) ) ;
#42056 = CARTESIAN_POINT ( 'NONE',  ( 97.31301912648670793, -38.96037348457183214, 102.5053915444232047 ) ) ;
#42057 = VECTOR ( 'NONE', #75409, 1000.000000000000000 ) ;
#42059 = DIRECTION ( 'NONE',  ( -0.7071067811855830110, -0.7071067811875120235, 0.000000000000000000 ) ) ;
#42058 = DIRECTION ( 'NONE',  ( -0.7071067811865470176, -0.7071067811865480168, 0.000000000000000000 ) ) ;
#42060 = FACE_OUTER_BOUND ( 'NONE', #15467, .T. ) ;
#42061 = CARTESIAN_POINT ( 'NONE',  ( 144.0667039024470739, -140.6784471599409017, 245.4568581450700151 ) ) ;
#42062 = ORIENTED_EDGE ( 'NONE', *, *, #32059, .F. ) ;
#42063 = EDGE_CURVE ( 'NONE', #33219, #29809, #6130, .T. ) ;
#42064 = CARTESIAN_POINT ( 'NONE',  ( 59.56670390244700997, -79.67844715994098692, 120.2178068554179902 ) ) ;
#42065 = ORIENTED_EDGE ( 'NONE', *, *, #76668, .F. ) ;
#42066 = VERTEX_POINT ( 'NONE', #52869 ) ;
#42067 = VERTEX_POINT ( 'NONE', #12039 ) ;
#42068 = CARTESIAN_POINT ( 'NONE',  ( 96.94826409162261882, -39.14818769109201213, 52.51276813305394597 ) ) ;
#42069 = DIRECTION ( 'NONE',  ( -0.7071067811865779928, 0.7071067811865171526, -7.071067811865785947E-16 ) ) ;
#42071 = CARTESIAN_POINT ( 'NONE',  ( 41.56670390244783420, -36.32844715994104234, 249.9678068554150343 ) ) ;
#42070 = CIRCLE ( 'NONE', #4417, 2.116999999999993776 ) ;
#42072 = CARTESIAN_POINT ( 'NONE',  ( 112.5087493249093455, -26.14677957921270846, 165.6984824187679521 ) ) ;
#42073 = CARTESIAN_POINT ( 'NONE',  ( 111.3857387752846790, -29.74709210828544670, 289.0581341137911409 ) ) ;
#42074 = VERTEX_POINT ( 'NONE', #88358 ) ;
#42075 = EDGE_CURVE ( 'NONE', #44015, #30543, #26117, .T. ) ;
#42076 = VERTEX_POINT ( 'NONE', #25658 ) ;
#42077 = ORIENTED_EDGE ( 'NONE', *, *, #27021, .T. ) ;
#42078 = EDGE_LOOP ( 'NONE', ( #82482, #62908 ) ) ;
#42079 = CARTESIAN_POINT ( 'NONE',  ( 70.06670417066791856, -83.77844715994098124, 55.21780685541800437 ) ) ;
#42080 = LINE ( 'NONE', #62537, #43443 ) ;
#42081 = LINE ( 'NONE', #14859, #20189 ) ;
#42082 = CARTESIAN_POINT ( 'NONE',  ( 97.06102870941442973, -37.99614388472145521, 21.42670149929413626 ) ) ;
#42083 = CARTESIAN_POINT ( 'NONE',  ( 100.3414980266867929, 87.03008507238371294, 83.52531662946728375 ) ) ;
#42084 = EDGE_CURVE ( 'NONE', #41012, #78672, #17946, .T. ) ;
#42085 = PLANE ( 'NONE',  #43627 ) ;
#42086 = EDGE_CURVE ( 'NONE', #26963, #37193, #45625, .T. ) ;
#42087 = DIRECTION ( 'NONE',  ( 1.000000000000000078E-15, -1.000000000000000083E-30, -1.000000000000000000 ) ) ;
#42088 = VECTOR ( 'NONE', #20133, 1000.000000000000114 ) ;
#42089 = DIRECTION ( 'NONE',  ( 1.092739197465705130E-14, 0.000000000000000000, -1.000000000000000000 ) ) ;
#42090 = EDGE_CURVE ( 'NONE', #60002, #56758, #18851, .T. ) ;
#42091 = LINE ( 'NONE', #22133, #18723 ) ;
#42092 = CARTESIAN_POINT ( 'NONE',  ( 111.4827405772851847, -46.11507286351704238, 287.9146728949591534 ) ) ;
#42093 = CARTESIAN_POINT ( 'NONE',  ( -179.8898777604655095, 20.32000000000000028, -12.69999999999999929 ) ) ;
#42094 = ORIENTED_EDGE ( 'NONE', *, *, #66274, .F. ) ;
#42095 = ADVANCED_FACE ( 'NONE', ( #66994 ), #46972, .T. ) ;
#42096 = CARTESIAN_POINT ( 'NONE',  ( -72.96458098368600531, 127.0000000000000000, -72.96458098368781009 ) ) ;
#42097 = VECTOR ( 'NONE', #84977, 1000.000000000000000 ) ;
#42098 = CARTESIAN_POINT ( 'NONE',  ( 172.5664832912740110, -18.82844715994099971, 196.8086252759119645 ) ) ;
#42099 = CARTESIAN_POINT ( 'NONE',  ( 106.7484768184134083, -28.57294068349449034, 82.92523322673494590 ) ) ;
#42100 = EDGE_CURVE ( 'NONE', #46818, #55274, #11336, .T. ) ;
#42101 = CARTESIAN_POINT ( 'NONE',  ( 107.0664832912739968, -36.72944715994100306, 287.6356252759109680 ) ) ;
#42102 = EDGE_CURVE ( 'NONE', #24379, #21876, #53333, .T. ) ;
#42103 = CIRCLE ( 'NONE', #81312, 9.571100913904395213 ) ;
#42104 = CARTESIAN_POINT ( 'NONE',  ( 105.7995184857070541, -26.72403496612070484, 45.17729194272746440 ) ) ;
#42105 = ORIENTED_EDGE ( 'NONE', *, *, #84715, .T. ) ;
#42106 = ORIENTED_EDGE ( 'NONE', *, *, #57899, .T. ) ;
#42107 = CARTESIAN_POINT ( 'NONE',  ( 79.11888855179115865, -34.14703303315388183, 8.087249882927796563 ) ) ;
#42108 = ORIENTED_EDGE ( 'NONE', *, *, #87021, .T. ) ;
#42109 = ORIENTED_EDGE ( 'NONE', *, *, #887, .T. ) ;
#42110 = CARTESIAN_POINT ( 'NONE',  ( 108.3334481331651347, -46.73485934878011250, 68.67729194561684380 ) ) ;
#42111 = CARTESIAN_POINT ( 'NONE',  ( 100.0878889097611335, -31.26788461136058217, 152.2301547344689538 ) ) ;
#42112 = CARTESIAN_POINT ( 'NONE',  ( 99.33030919034192152, -39.89585591585919389, 11.13025956287383700 ) ) ;
#42113 = AXIS2_PLACEMENT_3D ( 'NONE', #85375, #50363, #51698 ) ;
#42114 = CARTESIAN_POINT ( 'NONE',  ( 96.62018903270816850, -36.61901565639288236, 107.3184824187679567 ) ) ;
#42115 = CARTESIAN_POINT ( 'NONE',  ( 115.0372574996102344, -42.90846257582342815, 84.30229194168035178 ) ) ;
#42116 = ORIENTED_EDGE ( 'NONE', *, *, #14288, .T. ) ;
#42117 = CARTESIAN_POINT ( 'NONE',  ( -117.9439354154379203, 78.46407912418312947, -12.03195559056875297 ) ) ;
#42118 = ORIENTED_EDGE ( 'NONE', *, *, #87928, .F. ) ;
#42119 = ORIENTED_EDGE ( 'NONE', *, *, #4083, .T. ) ;
#42120 = AXIS2_PLACEMENT_3D ( 'NONE', #80116, #37427, #66004 ) ;
#42121 = CARTESIAN_POINT ( 'NONE',  ( 182.0667039024480118, -32.29483332968430886, 342.9256252759119548 ) ) ;
#42122 = EDGE_LOOP ( 'NONE', ( #15924, #12645, #41946, #41368 ) ) ;
#42123 = CARTESIAN_POINT ( 'NONE',  ( 110.2773916389478188, -46.62487827714380018, 12.82705384733995402 ) ) ;
#42124 = CARTESIAN_POINT ( 'NONE',  ( 112.7920458925406422, -45.46759294451666022, 174.0384824187679556 ) ) ;
#42125 = CARTESIAN_POINT ( 'NONE',  ( 7.736705052999859333, 72.46990138899384704, -118.3037342042693325 ) ) ;
#42126 = DIRECTION ( 'NONE',  ( 1.000000000000000000, 0.000000000000000000, 1.261617073437676668E-15 ) ) ;
#42127 = CARTESIAN_POINT ( 'NONE',  ( 112.1200623320449097, -47.44840020502576294, 133.9270538473399768 ) ) ;
#42128 = CARTESIAN_POINT ( 'NONE',  ( 82.81648329127399677, -36.72944715994107412, 14.92562527591094579 ) ) ;
#42129 = ORIENTED_EDGE ( 'NONE', *, *, #46892, .T. ) ;
#42130 = LINE ( 'NONE', #20370, #46736 ) ;
#42131 = FACE_OUTER_BOUND ( 'NONE', #33032, .T. ) ;
#42132 = EDGE_CURVE ( 'NONE', #64265, #69742, #5681, .T. ) ;
#42133 = ORIENTED_EDGE ( 'NONE', *, *, #48198, .T. ) ;
#42134 = VECTOR ( 'NONE', #42704, 1000.000000000000000 ) ;
#42135 = DIRECTION ( 'NONE',  ( 2.195856868753399715E-16, 1.000000000000000000, 0.000000000000000000 ) ) ;
#42136 = LINE ( 'NONE', #15358, #43503 ) ;
#42137 = CARTESIAN_POINT ( 'NONE',  ( 109.6119907475197550, -25.15530020966791369, 29.90419670448196854 ) ) ;
#42138 = DIRECTION ( 'NONE',  ( 0.000000000000000000, 0.000000000000000000, 1.000000000000000000 ) ) ;
#42139 = CYLINDRICAL_SURFACE ( 'NONE', #81180, 218.1859999999999786 ) ;
#42140 = CARTESIAN_POINT ( 'NONE',  ( 116.7962177220229307, -39.38393268333770436, 93.61551088916660035 ) ) ;
#42141 = CARTESIAN_POINT ( 'NONE',  ( 114.8626455990942361, -41.33732585285711991, 282.8362293518863453 ) ) ;
#42143 = CARTESIAN_POINT ( 'NONE',  ( 96.72090476913471946, -37.82382852467499390, 122.4099109901969626 ) ) ;
#42142 = CARTESIAN_POINT ( 'NONE',  ( 97.80809361765332710, -40.50863056222199532, 111.6348687641118715 ) ) ;
#42144 = CARTESIAN_POINT ( 'NONE',  ( 0.000000000000000000, 101.5999999999999943, 0.000000000000000000 ) ) ;
#42145 = DIRECTION ( 'NONE',  ( -1.000000000000000078E-15, 1.000000000000000083E-30, 1.000000000000000000 ) ) ;
#42146 = ORIENTED_EDGE ( 'NONE', *, *, #2224, .F. ) ;
#42147 = AXIS2_PLACEMENT_3D ( 'NONE', #63144, #70873, #34981 ) ;
#42148 = DIRECTION ( 'NONE',  ( -1.000000000000000000, 0.000000000000000000, 0.000000000000000000 ) ) ;
#42149 = CARTESIAN_POINT ( 'NONE',  ( 109.6133334940117976, 49.38454753513003226, 70.92099578410642380 ) ) ;
#42150 = FACE_OUTER_BOUND ( 'NONE', #66381, .T. ) ;
#42151 = VERTEX_POINT ( 'NONE', #11598 ) ;
#42152 = DIRECTION ( 'NONE',  ( -0.000000000000000000, -0.000000000000000000, 1.000000000000000000 ) ) ;
#42154 = ORIENTED_EDGE ( 'NONE', *, *, #31459, .F. ) ;
#42153 = CARTESIAN_POINT ( 'NONE',  ( 102.9497400982657069, -26.42094052169726837, 175.3908633711489813 ) ) ;
#42155 = DIRECTION ( 'NONE',  ( 0.000000000000000000, 0.000000000000000000, 1.000000000000000000 ) ) ;
#42156 = CARTESIAN_POINT ( 'NONE',  ( 99.73785018541691727, -29.28442226721861275, 221.6956252759109702 ) ) ;
#42157 = CARTESIAN_POINT ( 'NONE',  ( 114.3835678416600672, -44.21631923246377482, 69.19276813305397411 ) ) ;
#42158 = DIRECTION ( 'NONE',  ( -1.000000000000000000, 0.000000000000000000, 0.000000000000000000 ) ) ;
#42159 = PLANE ( 'NONE',  #54684 ) ;
#42160 = CYLINDRICAL_SURFACE ( 'NONE', #1750, 2.116999999999993776 ) ;
#42161 = ORIENTED_EDGE ( 'NONE', *, *, #11843, .T. ) ;
#42162 = ADVANCED_FACE ( 'NONE', ( #75157 ), #4778, .T. ) ;
#42163 = SHAPE_DEFINITION_REPRESENTATION ( #74302, #87903 ) ;
#42164 = VERTEX_POINT ( 'NONE', #73360 ) ;
#42166 = ORIENTED_EDGE ( 'NONE', *, *, #38492, .F. ) ;
#42165 = AXIS2_PLACEMENT_3D ( 'NONE', #3815, #67363, #45560 ) ;
#42167 = AXIS2_PLACEMENT_3D ( 'NONE', #12927, #18836, #67418 ) ;
#42168 = ORIENTED_EDGE ( 'NONE', *, *, #17189, .F. ) ;
#42169 = CARTESIAN_POINT ( 'NONE',  ( 141.8164832912740394, -36.72944715994099596, -4.824374724088994704 ) ) ;
#42170 = CARTESIAN_POINT ( 'NONE',  ( 117.4906655440605334, -35.85895469176247019, 249.8927681330537780 ) ) ;
#42171 = CARTESIAN_POINT ( 'NONE',  ( 0.000000000000000000, 92.07499999999998863, 0.000000000000000000 ) ) ;
#42172 = CARTESIAN_POINT ( 'NONE',  ( 136.8004280042375456, -18.38432671278184927, 3.076561810304713873 ) ) ;
#42174 = CARTESIAN_POINT ( 'NONE',  ( 107.0667039024470313, -104.2784471599413934, 2.217806855418003043 ) ) ;
#42173 = LINE ( 'NONE', #854, #30831 ) ;
#42175 = CARTESIAN_POINT ( 'NONE',  ( -31.75000000000000000, 104.3431970271541900, -3.175000000000219647 ) ) ;
#42176 = VECTOR ( 'NONE', #15589, 1000.000000000000000 ) ;
#42177 = CARTESIAN_POINT ( 'NONE',  ( 116.7476796835742192, -31.34707987858772427, 29.24229194257799236 ) ) ;
#42178 = VERTEX_POINT ( 'NONE', #4333 ) ;
#42179 = ORIENTED_EDGE ( 'NONE', *, *, #28883, .F. ) ;
#42180 = AXIS2_PLACEMENT_3D ( 'NONE', #25937, #80462, #67716 ) ;
#42181 = CARTESIAN_POINT ( 'NONE',  ( -148.0533267522752112, 20.32000000000000028, 160.2664750769289697 ) ) ;
#42182 = CARTESIAN_POINT ( 'NONE',  ( 105.2318265017784000, -27.12228994480481248, 231.2270538473389649 ) ) ;
#42183 = EDGE_CURVE ( 'NONE', #74787, #50559, #56313, .T. ) ;
#42184 = B_SPLINE_CURVE_WITH_KNOTS ( 'NONE', 3,
 ( #83501, #63045, #15368, #63955, #22185, #84861, #43033, #43484, #63497, #21272, #56210, #28987, #56673, #78043, #84417, #29435, #48945, #8547 ),
 .UNSPECIFIED., .F., .F.,
 ( 4, 2, 2, 2, 2, 2, 2, 2, 4 ),
 ( 0.4999999997859982392, 0.5624999998127484524, 0.6249999998394986100, 0.6874999998662488787, 0.7499999998929991474, 0.8124999999197493050, 0.8749999999464994627, 0.9374999999732497313, 1.000000000000000000 ),
 .UNSPECIFIED. ) ;
#42185 = PLANE ( 'NONE',  #2324 ) ;
#42186 = CARTESIAN_POINT ( 'NONE',  ( 97.30000116515917341, -37.25789978020652171, 72.36991099019596163 ) ) ;
#42187 = EDGE_CURVE ( 'NONE', #11825, #76939, #46122, .T. ) ;
#42188 = CARTESIAN_POINT ( 'NONE',  ( 107.0664832912739968, -36.72944715994100306, 287.6356252759109680 ) ) ;
#42189 = EDGE_CURVE ( 'NONE', #70164, #57201, #55164, .T. ) ;
#42190 = CARTESIAN_POINT ( 'NONE',  ( 97.07203280649774513, -35.37881615147394854, 22.21891955711141264 ) ) ;
#42192 = ORIENTED_EDGE ( 'NONE', *, *, #77186, .F. ) ;
#42191 = AXIS2_PLACEMENT_3D ( 'NONE', #66645, #72587, #86661 ) ;
#42193 = FACE_OUTER_BOUND ( 'NONE', #43171, .T. ) ;
#42194 = ADVANCED_FACE ( 'NONE', ( #84232 ), #15173, .F. ) ;
#42195 = EDGE_LOOP ( 'NONE', ( #17746, #79364, #88310, #80870 ) ) ;
#42196 = ORIENTED_EDGE ( 'NONE', *, *, #18201, .T. ) ;
#42197 = CARTESIAN_POINT ( 'NONE',  ( -75.67533895324345394, 88.91291927174617626, 91.26325766987484656 ) ) ;
#42198 = CARTESIAN_POINT ( 'NONE',  ( 102.1597156073931671, -27.93204209654597037, 251.9130118773254026 ) ) ;
#42199 = AXIS2_PLACEMENT_3D ( 'NONE', #51757, #79505, #53529 ) ;
#42200 = LINE ( 'NONE', #84013, #83543 ) ;
#42201 = CARTESIAN_POINT ( 'NONE',  ( 112.1389085449243765, -28.01257236761306402, 139.6564983914183813 ) ) ;
#42202 = CARTESIAN_POINT ( 'NONE',  ( 48.45959712129000252, -28.98061976758940617, 342.9256252759119548 ) ) ;
#42203 = EDGE_CURVE ( 'NONE', #66001, #13914, #69241, .T. ) ;
#42204 = VECTOR ( 'NONE', #42913, 1000.000000000000000 ) ;
#42205 = CARTESIAN_POINT ( 'NONE',  ( 99.08946256649487339, -99.09543445804985140, -19.78219314458218392 ) ) ;
#42206 = EDGE_LOOP ( 'NONE', ( #13592, #23315 ) ) ;
#42207 = CARTESIAN_POINT ( 'NONE',  ( 12.70000000000000107, 82.54999999999999716, 97.46299999999996544 ) ) ;
#42208 = DIRECTION ( 'NONE',  ( 1.000000000000000000, 0.000000000000000000, 3.491483361109385222E-15 ) ) ;
#42209 = ORIENTED_EDGE ( 'NONE', *, *, #48971, .T. ) ;
#42210 = CARTESIAN_POINT ( 'NONE',  ( 105.4209491665783105, -47.02406944081578644, 37.44991099019695469 ) ) ;
#42211 = ORIENTED_EDGE ( 'NONE', *, *, #10720, .T. ) ;
#42213 = CIRCLE ( 'NONE', #37889, 218.1859999999999786 ) ;
#42212 = CARTESIAN_POINT ( 'NONE',  ( 111.2046685188893775, -28.67413054290084062, 19.13337220902994318 ) ) ;
#42214 = LINE ( 'NONE', #3, #5400 ) ;
#42215 = CARTESIAN_POINT ( 'NONE',  ( 113.6884830475839152, -29.53135334845044468, 199.4841967044829687 ) ) ;
#42216 = CARTESIAN_POINT ( 'NONE',  ( 20.03715912545735378, -24.42818131006189830, 249.9678068554150059 ) ) ;
#42217 = DIRECTION ( 'NONE',  ( 0.000000000000000000, 1.000000000000000000, 0.000000000000000000 ) ) ;
#42218 = DIRECTION ( 'NONE',  ( 0.000000000000000000, 0.000000000000000000, -1.000000000000000000 ) ) ;
#42219 = CARTESIAN_POINT ( 'NONE',  ( 7.060148683296544547, 71.99328113033080001, 130.3649624909047020 ) ) ;
#42220 = CARTESIAN_POINT ( 'NONE',  ( 97.46669833601751520, -32.60829619471579122, 12.00419670448293985 ) ) ;
#42221 = CARTESIAN_POINT ( 'NONE',  ( 74.89049941105147923, 86.63388195152282378, -91.90730674524651533 ) ) ;
#42222 = ORIENTED_EDGE ( 'NONE', *, *, #72995, .F. ) ;
#42223 = DIRECTION ( 'NONE',  ( -1.000000000000000078E-15, 1.000000000000000083E-30, 1.000000000000000000 ) ) ;
#42224 = VERTEX_POINT ( 'NONE', #55126 ) ;
#42225 = CARTESIAN_POINT ( 'NONE',  ( 114.0153296496652615, -28.07433117884028206, 115.5261014663869474 ) ) ;
#42226 = CARTESIAN_POINT ( 'NONE',  ( 123.1844716773658348, 44.88724112343236072, -43.24955686283671952 ) ) ;
#42227 = ORIENTED_EDGE ( 'NONE', *, *, #89737, .F. ) ;
#42228 = PLANE ( 'NONE',  #16801 ) ;
#42229 = ORIENTED_EDGE ( 'NONE', *, *, #58147, .T. ) ;
#42230 = ORIENTED_EDGE ( 'NONE', *, *, #3551, .F. ) ;
#42231 = AXIS2_PLACEMENT_3D ( 'NONE', #58166, #2773, #44074 ) ;
#42232 = CARTESIAN_POINT ( 'NONE',  ( 104.4081005327850846, -46.45808910606737641, 122.3647919321082327 ) ) ;
#42233 = DIRECTION ( 'NONE',  ( 0.4999999999999998890, 0.8660254037844387076, 0.000000000000000000 ) ) ;
#42234 = CARTESIAN_POINT ( 'NONE',  ( 106.5667039024470455, -113.7784471599413791, 2.217806855418308132 ) ) ;
#42235 = DIRECTION ( 'NONE',  ( -4.299999999999999979E-14, 1.000000000000000000, -4.400000000000000367E-29 ) ) ;
#42236 = DIRECTION ( 'NONE',  ( 1.000000000000000000, 0.000000000000000000, 0.000000000000000000 ) ) ;
#42237 = CARTESIAN_POINT ( 'NONE',  ( 99.51751092519847930, -40.96193357599213414, 179.5633284648289703 ) ) ;
#42238 = CARTESIAN_POINT ( 'NONE',  ( 99.36548562555644537, -29.67027625815665104, 271.7356252759109907 ) ) ;
#42239 = LINE ( 'NONE', #44024, #78439 ) ;
#42240 = ORIENTED_EDGE ( 'NONE', *, *, #12443, .T. ) ;
#42241 = CARTESIAN_POINT ( 'NONE',  ( 126.8164832912740394, -54.62589567669621005, -5.074374724089010691 ) ) ;
#42242 = CARTESIAN_POINT ( 'NONE',  ( 31.75000000000000000, 8.255000000000000782, 3.174999999999999822 ) ) ;
#42243 = CIRCLE ( 'NONE', #42300, 2.500000000000002220 ) ;
#42244 = EDGE_CURVE ( 'NONE', #41711, #47853, #49220, .T. ) ;
#42245 = ORIENTED_EDGE ( 'NONE', *, *, #2580, .T. ) ;
#42246 = ORIENTED_EDGE ( 'NONE', *, *, #13085, .T. ) ;
#42247 = CARTESIAN_POINT ( 'NONE',  ( 81.91406418436724834, -20.77438500682750799, 2.186796636973903141 ) ) ;
#42248 = DIRECTION ( 'NONE',  ( -0.04216478779797398074, 0.9991106698809455455, 0.000000000000000000 ) ) ;
#42249 = CARTESIAN_POINT ( 'NONE',  ( 97.07205744801414937, -35.37854429503371989, 16.21896654171250773 ) ) ;
#42250 = EDGE_CURVE ( 'NONE', #82044, #18839, #21548, .T. ) ;
#42251 = FACE_OUTER_BOUND ( 'NONE', #198, .T. ) ;
#42252 = CARTESIAN_POINT ( 'NONE',  ( -446.0240000000000009, 104.7749999999999915, -1.387778780781445991E-14 ) ) ;
#42253 = CARTESIAN_POINT ( 'NONE',  ( 99.94932728663779642, -31.12955780999732980, 200.2305150661719892 ) ) ;
#42254 = CARTESIAN_POINT ( 'NONE',  ( 115.2011789175540741, -43.31984874952732412, 88.28419670448195689 ) ) ;
#42255 = ORIENTED_EDGE ( 'NONE', *, *, #21768, .F. ) ;
#42256 = DIRECTION ( 'NONE',  ( -1.784063995862374817E-16, 0.000000000000000000, -1.000000000000000000 ) ) ;
#42257 = VERTEX_POINT ( 'NONE', #7010 ) ;
#42258 = CARTESIAN_POINT ( 'NONE',  ( -74.89107914305763813, 78.46407912418314368, -91.90683392111100147 ) ) ;
#42259 = EDGE_LOOP ( 'NONE', ( #24012, #84536, #23284, #4084, #12044 ) ) ;
#42260 = VECTOR ( 'NONE', #37531, 1000.000000000000114 ) ;
#42261 = DIRECTION ( 'NONE',  ( 1.000000000000000000, 0.000000000000000000, 0.000000000000000000 ) ) ;
#42262 = EDGE_LOOP ( 'NONE', ( #51717, #30087, #37100, #48905 ) ) ;
#42263 = PLANE ( 'NONE',  #11692 ) ;
#42264 = FACE_OUTER_BOUND ( 'NONE', #72974, .T. ) ;
#42265 = DIRECTION ( 'NONE',  ( 0.000000000000000000, 1.000000000000000000, 0.000000000000000000 ) ) ;
#42266 = VECTOR ( 'NONE', #58370, 1000.000000000000000 ) ;
#42267 = CARTESIAN_POINT ( 'NONE',  ( 0.000000000000000000, 82.54999999999999716, 97.46299999999996544 ) ) ;
#42268 = ORIENTED_EDGE ( 'NONE', *, *, #52800, .F. ) ;
#42269 = EDGE_CURVE ( 'NONE', #16654, #44045, #195, .T. ) ;
#42270 = CARTESIAN_POINT ( 'NONE',  ( 101.0534108623914591, -27.42684531413746285, 70.54514908543497143 ) ) ;
#42272 = LINE ( 'NONE', #77266, #742 ) ;
#42271 = CARTESIAN_POINT ( 'NONE',  ( 117.0667039024470313, -98.59953881414067212, 17.71780685541782319 ) ) ;
#42273 = CARTESIAN_POINT ( 'NONE',  ( 30.00000000000003553, 127.0000000000000000, 182.8826257785461280 ) ) ;
#42274 = CARTESIAN_POINT ( 'NONE',  ( 131.5238707403503327, -17.68172011937277333, 2.822018711113663425 ) ) ;
#42275 = EDGE_LOOP ( 'NONE', ( #39385, #87116, #33925, #3132 ) ) ;
#42276 = LINE ( 'NONE', #50439, #2493 ) ;
#42277 = DIRECTION ( 'NONE',  ( 0.000000000000000000, 0.000000000000000000, 1.000000000000000000 ) ) ;
#42278 = VECTOR ( 'NONE', #67969, 1000.000000000000000 ) ;
#42279 = CARTESIAN_POINT ( 'NONE',  ( -48.02966122971777452, 65.60000000000000853, 106.4272185163641780 ) ) ;
#42280 = CARTESIAN_POINT ( 'NONE',  ( 114.7420861883949215, -43.81622209775510157, 119.2327681330539804 ) ) ;
#42282 = FACE_OUTER_BOUND ( 'NONE', #87900, .T. ) ;
#42281 = DIRECTION ( 'NONE',  ( -0.7071067811865476838, -0.7071067811865473507, 0.000000000000000000 ) ) ;
#42283 = FACE_OUTER_BOUND ( 'NONE', #38110, .T. ) ;
#42284 = ORIENTED_EDGE ( 'NONE', *, *, #6244, .F. ) ;
#42285 = LINE ( 'NONE', #23238, #53463 ) ;
#42286 = CARTESIAN_POINT ( 'NONE',  ( 98.54774150848832903, -41.53511815344519675, 132.7356252759109623 ) ) ;
#42288 = ORIENTED_EDGE ( 'NONE', *, *, #19760, .F. ) ;
#42287 = CARTESIAN_POINT ( 'NONE',  ( 131.0667039024480403, -51.22944715994093201, 231.5838068554170093 ) ) ;
#42289 = VECTOR ( 'NONE', #56801, 1000.000000000000000 ) ;
#42290 = CARTESIAN_POINT ( 'NONE',  ( 111.8540205700168713, -46.00543295620330753, 268.9556252759110180 ) ) ;
#42291 = DIRECTION ( 'NONE',  ( -4.237773401492740281E-14, 1.000000000000000000, 0.000000000000000000 ) ) ;
#42292 = CARTESIAN_POINT ( 'NONE',  ( 150.5667039024473297, -25.42844715993594562, 300.4678068554149490 ) ) ;
#42293 = CARTESIAN_POINT ( 'NONE',  ( 107.0664832912739968, 22.62155284005901024, 333.4006252759110112 ) ) ;
#42294 = EDGE_CURVE ( 'NONE', #79790, #65097, #20649, .T. ) ;
#42295 = LINE ( 'NONE', #15518, #36991 ) ;
#42296 = CARTESIAN_POINT ( 'NONE',  ( 34.27482367531460028, -30.08671355700332839, 237.4678068554150059 ) ) ;
#42297 = CARTESIAN_POINT ( 'NONE',  ( -96.22129751242485440, 71.14122173980733521, 88.24354053934821707 ) ) ;
#42298 = CARTESIAN_POINT ( 'NONE',  ( 106.9806506443342755, -46.50983917909375265, 187.5699109901969734 ) ) ;
#42299 = VERTEX_POINT ( 'NONE', #83321 ) ;
#42300 = AXIS2_PLACEMENT_3D ( 'NONE', #17271, #39035, #32671 ) ;
#42301 = ORIENTED_EDGE ( 'NONE', *, *, #87016, .F. ) ;
#42302 = CARTESIAN_POINT ( 'NONE',  ( 103.5362709388849254, -28.56900242483978047, 151.8330118773259585 ) ) ;
#42303 = AXIS2_PLACEMENT_3D ( 'NONE', #3827, #52383, #51075 ) ;
#42304 = DIRECTION ( 'NONE',  ( 1.000000000000000000, 4.163336342344347755E-14, 0.000000000000000000 ) ) ;
#42305 = CARTESIAN_POINT ( 'NONE',  ( 102.4274648318396146, -45.67098835673295554, 13.62729759161196341 ) ) ;
#42306 = DIRECTION ( 'NONE',  ( -1.000000000000000078E-15, 0.000000000000000000, -1.000000000000000000 ) ) ;
#42307 = CYLINDRICAL_SURFACE ( 'NONE', #89584, 0.9999999999992039701 ) ;
#42308 = EDGE_CURVE ( 'NONE', #1932, #61346, #41956, .T. ) ;
#42309 = DIRECTION ( 'NONE',  ( -3.491483361109385222E-15, 0.000000000000000000, 1.000000000000000000 ) ) ;
#42310 = DIRECTION ( 'NONE',  ( 0.000000000000000000, 1.000000000000000000, 1.914177628664063178E-15 ) ) ;
#42311 = DIRECTION ( 'NONE',  ( 0.000000000000000000, 1.000000000000000000, 0.000000000000000000 ) ) ;
#42312 = EDGE_CURVE ( 'NONE', #51214, #73315, #35149, .T. ) ;
#42313 = CARTESIAN_POINT ( 'NONE',  ( 116.8369567342160451, -40.30247308064095790, 218.5470538473399529 ) ) ;
#42314 = DIRECTION ( 'NONE',  ( 0.000000000000000000, 0.000000000000000000, -1.000000000000000000 ) ) ;
#42315 = EDGE_LOOP ( 'NONE', ( #81043, #2669, #10374, #87115, #10773 ) ) ;
#42316 = ORIENTED_EDGE ( 'NONE', *, *, #52583, .T. ) ;
#42317 = VECTOR ( 'NONE', #40856, 1000.000000000000000 ) ;
#42318 = CARTESIAN_POINT ( 'NONE',  ( -84.36969927706159922, 75.84295037288958952, -99.63271100832238858 ) ) ;
#42319 = CARTESIAN_POINT ( 'NONE',  ( -74.38497350661499752, 83.38015080693121206, -92.31685958143614812 ) ) ;
#42320 = DIRECTION ( 'NONE',  ( -1.000000000000000078E-15, 1.000000000000000083E-30, 1.000000000000000000 ) ) ;
#42321 = CARTESIAN_POINT ( 'NONE',  ( 122.2189888861420286, -96.57077177933014411, -21.78219314458226918 ) ) ;
#42322 = VECTOR ( 'NONE', #64632, 1000.000000000000000 ) ;
#42323 = DIRECTION ( 'NONE',  ( 0.7071067811865171526, 0.7071067811865779928, 7.071067811865164719E-16 ) ) ;
#42324 = EDGE_LOOP ( 'NONE', ( #58946, #77905 ) ) ;
#42325 = CARTESIAN_POINT ( 'NONE',  ( 115.9822161205003397, -42.21601869724081268, 14.38705384733995984 ) ) ;
#42326 = CARTESIAN_POINT ( 'NONE',  ( 118.0409265538620787, -35.41009787725452185, 238.9337205140059552 ) ) ;
#42327 = ORIENTED_EDGE ( 'NONE', *, *, #50979, .T. ) ;
#42328 = VECTOR ( 'NONE', #33109, 999.9999999999998863 ) ;
#42329 = DIRECTION ( 'NONE',  ( 3.100000000000000258E-29, -3.100000000000000044E-14, -1.000000000000000000 ) ) ;
#42330 = PLANE ( 'NONE',  #23959 ) ;
#42331 = CARTESIAN_POINT ( 'NONE',  ( 117.0504484085820707, -35.92752602142036267, 168.8902974104038890 ) ) ;
#42332 = AXIS2_PLACEMENT_3D ( 'NONE', #23755, #37369, #2857 ) ;
#42333 = CARTESIAN_POINT ( 'NONE',  ( 102.3683448235669715, -29.46113098739592928, 68.36332846482901004 ) ) ;
#42334 = CARTESIAN_POINT ( 'NONE',  ( 109.4502800619034417, -25.91266766229690433, 175.8918157521009391 ) ) ;
#42335 = CARTESIAN_POINT ( 'NONE',  ( 41.56648329127399677, -9.303447159940999356, 138.9256252759119832 ) ) ;
#42336 = ORIENTED_EDGE ( 'NONE', *, *, #21954, .F. ) ;
#42337 = AXIS2_PLACEMENT_3D ( 'NONE', #29849, #57082, #16221 ) ;
#42338 = CARTESIAN_POINT ( 'NONE',  ( -77.39114642430010349, 120.6499999999999915, 71.77848634863050847 ) ) ;
#42339 = VERTEX_POINT ( 'NONE', #22441 ) ;
#42340 = VERTEX_POINT ( 'NONE', #71928 ) ;
#42341 = CARTESIAN_POINT ( 'NONE',  ( 8.391666350164339150, 92.11848141222132824, 118.2600956121756752 ) ) ;
#42342 = VERTEX_POINT ( 'NONE', #64222 ) ;
#42343 = ORIENTED_EDGE ( 'NONE', *, *, #60901, .T. ) ;
#42344 = CARTESIAN_POINT ( 'NONE',  ( 115.7842719947117160, -41.80033795913374206, 169.4071411100227920 ) ) ;
#42345 = ADVANCED_FACE ( 'NONE', ( #29693, #86457 ), #30586, .F. ) ;
#42346 = CARTESIAN_POINT ( 'NONE',  ( 107.7585303169594511, -25.29108704099150629, 321.0964939388218227 ) ) ;
#42347 = CARTESIAN_POINT ( 'NONE',  ( 108.6385355886969108, -45.12496878139073431, 82.14670554236298017 ) ) ;
#42348 = CARTESIAN_POINT ( 'NONE',  ( 105.1048729065459355, -25.82772592887830854, 275.2061014663870537 ) ) ;
#42349 = CARTESIAN_POINT ( 'NONE',  ( 97.78191787992076911, -41.50032452247409509, 196.7041967044819728 ) ) ;
#42350 = LINE ( 'NONE', #34659, #64396 ) ;
#42351 = CARTESIAN_POINT ( 'NONE',  ( 101.9927051845395169, -45.44550660328174985, 93.15637402092625052 ) ) ;
#42352 = ORIENTED_EDGE ( 'NONE', *, *, #11373, .T. ) ;
#42353 = CARTESIAN_POINT ( 'NONE',  ( 97.80889870804310249, -40.51851473143300097, 41.63518016758125384 ) ) ;
#42354 = AXIS2_PLACEMENT_3D ( 'NONE', #29006, #29903, #57589 ) ;
#42355 = DIRECTION ( 'NONE',  ( 1.907762142705490052E-15, 7.167082501179359715E-16, -1.000000000000000000 ) ) ;
#42356 = CARTESIAN_POINT ( 'NONE',  ( 70.37150048485119669, -140.1555257716715630, 246.8822094458865308 ) ) ;
#42357 = VECTOR ( 'NONE', #83922, 1000.000000000000000 ) ;
#42358 = CARTESIAN_POINT ( 'NONE',  ( 107.3174176841070846, -26.95189801805063823, 120.0556252759109555 ) ) ;
#42359 = CARTESIAN_POINT ( 'NONE',  ( 96.87811797401508329, -32.32375813437732859, 61.01372051400599616 ) ) ;
#42360 = CARTESIAN_POINT ( 'NONE',  ( 96.22219577434788107, -34.35999324012363587, 256.1432443235299843 ) ) ;
#42361 = ORIENTED_EDGE ( 'NONE', *, *, #14103, .F. ) ;
#42362 = EDGE_CURVE ( 'NONE', #4781, #43151, #10144, .T. ) ;
#42363 = CARTESIAN_POINT ( 'NONE',  ( 106.8516092256838306, -47.78082339050276772, 227.5489586092439538 ) ) ;
#42364 = CARTESIAN_POINT ( 'NONE',  ( 116.3212776292294279, -32.94146857471271517, 75.13562527591093954 ) ) ;
#42365 = SHAPE_REPRESENTATION_RELATIONSHIP ( 'NONE' , 'NONE' ,  #87903, #88996 ) ;
#42366 = CARTESIAN_POINT ( 'NONE',  ( 12.62678658230826123, 80.95407853623918015, 129.9444177315847355 ) ) ;
#42367 = DIRECTION ( 'NONE',  ( -4.299999999999999979E-14, 1.000000000000000000, -4.400000000000000367E-29 ) ) ;
#42369 = DIRECTION ( 'NONE',  ( 1.000000000000000000, 4.299999999999999979E-14, 1.000000000000000078E-15 ) ) ;
#42368 = CARTESIAN_POINT ( 'NONE',  ( -41.60202597009397607, 40.59999999999997300, 50.85338361873603219 ) ) ;
#42370 = CARTESIAN_POINT ( 'NONE',  ( 180.3503142329310265, -29.99615139349890569, 117.4678068554150627 ) ) ;
#42371 = CARTESIAN_POINT ( 'NONE',  ( 0.000000000000000000, 224.4999999999999432, 154.6557476874258441 ) ) ;
#42372 = LINE ( 'NONE', #84201, #48410 ) ;
#42373 = EDGE_CURVE ( 'NONE', #16001, #28030, #79203, .T. ) ;
#42374 = CARTESIAN_POINT ( 'NONE',  ( -0.8301116440131806051, 95.22976338641703364, 130.5540265925895085 ) ) ;
#42375 = CARTESIAN_POINT ( 'NONE',  ( 105.7995184592378024, -26.72403496912623666, 11.17729194477459842 ) ) ;
#42376 = ADVANCED_FACE ( 'NONE', ( #3332 ), #39342, .F. ) ;
#42377 = CARTESIAN_POINT ( 'NONE',  ( 92.87912752678322192, -94.96964819957989334, -19.23816774842029886 ) ) ;
#42378 = CIRCLE ( 'NONE', #52475, 2.999999999999947153 ) ;
#42380 = ORIENTED_EDGE ( 'NONE', *, *, #80871, .F. ) ;
#42379 = CARTESIAN_POINT ( 'NONE',  ( 112.1393456339030337, -28.01282277639932161, 259.6564586099611915 ) ) ;
#42381 = EDGE_CURVE ( 'NONE', #41907, #23638, #14328, .T. ) ;
#42382 = FACE_OUTER_BOUND ( 'NONE', #16009, .T. ) ;
#42383 = CARTESIAN_POINT ( 'NONE',  ( 111.6181759772156994, -46.13308781976898842, 247.9356252759109509 ) ) ;
#42384 = CARTESIAN_POINT ( 'NONE',  ( 108.6487146914112287, -25.79677769486274386, 145.9737205140069420 ) ) ;
#42385 = CARTESIAN_POINT ( 'NONE',  ( 96.66430309996448500, -42.45805065352005414, 22.72705384733997391 ) ) ;
#42386 = LINE ( 'NONE', #84215, #64968 ) ;
#42388 = CARTESIAN_POINT ( 'NONE',  ( 46.32460016641721978, -48.34074026909785005, 300.4678068554150059 ) ) ;
#42387 = CARTESIAN_POINT ( 'NONE',  ( 49.21213752016101495, -29.73316016639650172, -5.074374724088000832 ) ) ;
#42389 = CYLINDRICAL_SURFACE ( 'NONE', #1546, 8.999999999999994671 ) ;
#42390 = ADVANCED_FACE ( 'NONE', ( #57386, #38284 ), #85129, .F. ) ;
#42391 = VECTOR ( 'NONE', #74880, 1000.000000000000000 ) ;
#42392 = ADVANCED_FACE ( 'NONE', ( #43758, #22895 ), #57838, .F. ) ;
#42393 = ORIENTED_EDGE ( 'NONE', *, *, #84378, .F. ) ;
#42394 = CARTESIAN_POINT ( 'NONE',  ( 116.3212776292296127, -32.94146857471318413, 10.13562527591094309 ) ) ;
#42395 = ORIENTED_EDGE ( 'NONE', *, *, #72322, .T. ) ;
#42396 = CIRCLE ( 'NONE', #13375, 3.000000000000002665 ) ;
#42397 = CARTESIAN_POINT ( 'NONE',  ( 105.9636396274569137, -27.08297541922676643, 159.5895626852199598 ) ) ;
#42399 = ORIENTED_EDGE ( 'NONE', *, *, #12479, .T. ) ;
#42398 = CARTESIAN_POINT ( 'NONE',  ( 33.91903122894480305, -35.91149509761181235, 237.4678068554150059 ) ) ;
#42400 = CARTESIAN_POINT ( 'NONE',  ( 103.3797721312301547, -105.8297479413482876, -19.78219314458196010 ) ) ;
#42401 = CARTESIAN_POINT ( 'NONE',  ( 117.0023065291008066, -39.93004192841230804, 154.5784824187679476 ) ) ;
#42402 = CARTESIAN_POINT ( 'NONE',  ( 120.0056275895821898, -31.38355669832866468, 290.1356252759106837 ) ) ;
#42403 = CARTESIAN_POINT ( 'NONE',  ( -3.968749999999935163, 120.6499999999999915, -100.8961411191535973 ) ) ;
#42404 = ADVANCED_FACE ( 'NONE', ( #37852, #58716 ), #78313, .T. ) ;
#42405 = CARTESIAN_POINT ( 'NONE',  ( 115.6778355879448981, -31.59694472422848577, 85.25382685634609459 ) ) ;
#42406 = CARTESIAN_POINT ( 'NONE',  ( -89.75424775947659839, 73.28361289573329884, 77.45828646618677737 ) ) ;
#42407 = PLANE ( 'NONE',  #84619 ) ;
#42408 = CARTESIAN_POINT ( 'NONE',  ( 96.71749658230658042, -40.79275330125902599, 96.62419670448296927 ) ) ;
#42409 = EDGE_LOOP ( 'NONE', ( #89359, #87854, #86808, #65631 ) ) ;
#42410 = VERTEX_POINT ( 'NONE', #2444 ) ;
#42411 = ORIENTED_EDGE ( 'NONE', *, *, #55498, .T. ) ;
#42412 = CARTESIAN_POINT ( 'NONE',  ( 104.4236822747140678, -45.74566190472552307, 58.76920235351595778 ) ) ;
#42413 = CARTESIAN_POINT ( 'NONE',  ( 188.5667039024479834, -67.87844715994100397, 178.0928068554149775 ) ) ;
#42415 = CARTESIAN_POINT ( 'NONE',  ( 135.3756687995053483, -12.91806617559082504, 394.9756252759104314 ) ) ;
#42414 = CARTESIAN_POINT ( 'NONE',  ( 110.4719531740380063, -47.31314961125941210, 203.8241967044819489 ) ) ;
#42416 = DIRECTION ( 'NONE',  ( 1.000000000000000000, 0.000000000000000000, 9.462128050782575008E-16 ) ) ;
#42417 = DIRECTION ( 'NONE',  ( 0.000000000000000000, 0.000000000000000000, 1.000000000000000000 ) ) ;
#42418 = LINE ( 'NONE', #56503, #47470 ) ;
#42419 = ADVANCED_FACE ( 'NONE', ( #29254 ), #23352, .T. ) ;
#42420 = AXIS2_PLACEMENT_3D ( 'NONE', #34472, #48521, #7674 ) ;
#42421 = DIRECTION ( 'NONE',  ( 0.7071067811865442421, -0.7071067811865509034, 0.000000000000000000 ) ) ;
#42422 = CARTESIAN_POINT ( 'NONE',  ( 68.77377604071689632, -69.45229246467815187, 247.4784000562319761 ) ) ;
#42423 = ADVANCED_FACE ( 'NONE', ( #75050 ), #19631, .T. ) ;
#42424 = CARTESIAN_POINT ( 'NONE',  ( 107.9437834512411598, -25.73425880284244016, 115.0251490854349612 ) ) ;
#42425 = ORIENTED_EDGE ( 'NONE', *, *, #25475, .F. ) ;
#42426 = ORIENTED_EDGE ( 'NONE', *, *, #58524, .T. ) ;
#42427 = ORIENTED_EDGE ( 'NONE', *, *, #19389, .T. ) ;
#42428 = EDGE_CURVE ( 'NONE', #71019, #44246, #69442, .T. ) ;
#42429 = SURFACE_STYLE_FILL_AREA ( #1117 ) ;
#42430 = CARTESIAN_POINT ( 'NONE',  ( 0.000000000000000000, 92.07499999999998863, 0.000000000000000000 ) ) ;
#42431 = EDGE_CURVE ( 'NONE', #26572, #49295, #15826, .T. ) ;
#42432 = DIRECTION ( 'NONE',  ( 1.000000000000000000, 4.299999999999999979E-14, 1.000000000000000078E-15 ) ) ;
#42433 = CARTESIAN_POINT ( 'NONE',  ( 131.3179999999999836, 53.97500000000000142, 50.79999999999999716 ) ) ;
#42434 = CARTESIAN_POINT ( 'NONE',  ( 102.6333607924234883, -43.61639954521550067, 219.9395189410199691 ) ) ;
#42435 = DIRECTION ( 'NONE',  ( 1.000000000000000000, 1.000000000000000078E-15, 0.000000000000000000 ) ) ;
#42436 = DIRECTION ( 'NONE',  ( 1.000000000000000078E-15, -1.000000000000000083E-30, -1.000000000000000000 ) ) ;
#42437 = ORIENTED_EDGE ( 'NONE', *, *, #3798, .F. ) ;
#42439 = ORIENTED_EDGE ( 'NONE', *, *, #13605, .F. ) ;
#42438 = ORIENTED_EDGE ( 'NONE', *, *, #71733, .F. ) ;
#42440 = CARTESIAN_POINT ( 'NONE',  ( 116.4818944900138149, -33.33401923526724175, 65.10204591046331757 ) ) ;
#42441 = ORIENTED_EDGE ( 'NONE', *, *, #9559, .F. ) ;
#42442 = ORIENTED_EDGE ( 'NONE', *, *, #73346, .T. ) ;
#42443 = CARTESIAN_POINT ( 'NONE',  ( 78.76282073105750214, -21.15113447711886963, 7.957506268074834743 ) ) ;
#42444 = CIRCLE ( 'NONE', #48209, 0.5000000000000004441 ) ;
#42445 = CARTESIAN_POINT ( 'NONE',  ( 116.9161372654479578, -38.84013935494854763, 255.0901547344684559 ) ) ;
#42446 = DIRECTION ( 'NONE',  ( 1.000000000000000000, 0.000000000000000000, 0.000000000000000000 ) ) ;
#42447 = ORIENTED_EDGE ( 'NONE', *, *, #44609, .F. ) ;
#42448 = CARTESIAN_POINT ( 'NONE',  ( 0.000000000000000000, 101.5999999999999943, 0.000000000000000000 ) ) ;
#42449 = CARTESIAN_POINT ( 'NONE',  ( -125.2253049228147290, 69.25379042415792696, 36.92573596021566829 ) ) ;
#42450 = VERTEX_POINT ( 'NONE', #67781 ) ;
#42451 = VERTEX_POINT ( 'NONE', #45968 ) ;
#42452 = VECTOR ( 'NONE', #17900, 1000.000000000000000 ) ;
#42453 = CARTESIAN_POINT ( 'NONE',  ( 70.63919639214310564, 91.07499999999996021, 53.63573739454427880 ) ) ;
#42454 = ORIENTED_EDGE ( 'NONE', *, *, #74212, .F. ) ;
#42455 = VERTEX_POINT ( 'NONE', #67323 ) ;
#42456 = CIRCLE ( 'NONE', #14939, 3.000000000000002665 ) ;
#42457 = CARTESIAN_POINT ( 'NONE',  ( 97.79975852078015919, -37.20246216128834504, 269.1852332267342831 ) ) ;
#42458 = CARTESIAN_POINT ( 'NONE',  ( 97.77451808712464754, -42.75935979880518545, 146.7965776568629508 ) ) ;
#42459 = CARTESIAN_POINT ( 'NONE',  ( 101.5125196766230289, -27.93273449574867229, 110.5241967044819944 ) ) ;
#42460 = LINE ( 'NONE', #692, #82037 ) ;
#42461 = CARTESIAN_POINT ( 'NONE',  ( 164.9667039024459996, -26.71338133339301635, -5.074374724088000832 ) ) ;
#42462 = CARTESIAN_POINT ( 'NONE',  ( 115.2517161551258766, -30.21613035964762517, 240.3613395616249875 ) ) ;
#42463 = CARTESIAN_POINT ( 'NONE',  ( 48.85858412958059205, -30.08671355700274574, 237.4678068554150059 ) ) ;
#42464 = CARTESIAN_POINT ( 'NONE',  ( 80.06648329127401098, -41.22944715994105280, 10.42562527591094401 ) ) ;
#42465 = ORIENTED_EDGE ( 'NONE', *, *, #18820, .F. ) ;
#42466 = CARTESIAN_POINT ( 'NONE',  ( 130.3273007233323710, 72.45841406287409825, -7.755409066831144393 ) ) ;
#42467 = ORIENTED_EDGE ( 'NONE', *, *, #63237, .F. ) ;
#42468 = ORIENTED_EDGE ( 'NONE', *, *, #4045, .T. ) ;
#42469 = LINE ( 'NONE', #68855, #64887 ) ;
#42470 = CARTESIAN_POINT ( 'NONE',  ( 37.06648329127400388, 12.92155284005802685, 336.5756252759108520 ) ) ;
#42471 = EDGE_LOOP ( 'NONE', ( #16399, #9364, #83586, #31361 ) ) ;
#42472 = ADVANCED_FACE ( 'NONE', ( #31911 ), #86894, .F. ) ;
#42473 = CARTESIAN_POINT ( 'NONE',  ( 105.3162203493976676, -48.44985994433862686, 147.4584824187679715 ) ) ;
#42474 = FACE_OUTER_BOUND ( 'NONE', #72517, .T. ) ;
#42475 = CARTESIAN_POINT ( 'NONE',  ( 136.1531896714324148, -34.93816060012501623, 7.482180659744297024 ) ) ;
#42476 = DIRECTION ( 'NONE',  ( 2.900000000000000265E-14, -2.000000000000000155E-15, 1.000000000000000000 ) ) ;
#42477 = EDGE_CURVE ( 'NONE', #6827, #46578, #52026, .T. ) ;
#42480 = CARTESIAN_POINT ( 'NONE',  ( 115.3062145713271747, -45.21207857638179917, 264.1899109901965517 ) ) ;
#42479 = CARTESIAN_POINT ( 'NONE',  ( 117.0188616982925396, -35.22807495305379888, 58.94555671601543168 ) ) ;
#42478 = DIRECTION ( 'NONE',  ( 0.000000000000000000, 0.000000000000000000, 1.000000000000000000 ) ) ;
#42481 = DIRECTION ( 'NONE',  ( -0.7071067811865774377, 0.7071067811865175967, -7.071067811865470403E-16 ) ) ;
#42482 = CARTESIAN_POINT ( 'NONE',  ( -215.9010000000000105, 52.73749999999999716, -36.51250000000000284 ) ) ;
#42483 = DIRECTION ( 'NONE',  ( 0.000000000000000000, 0.000000000000000000, 1.000000000000000000 ) ) ;
#42484 = EDGE_CURVE ( 'NONE', #72034, #30378, #14022, .T. ) ;
#42485 = CIRCLE ( 'NONE', #3347, 8.999999999999994671 ) ;
#42486 = DIRECTION ( 'NONE',  ( 0.000000000000000000, 0.000000000000000000, 1.000000000000000000 ) ) ;
#42487 = CARTESIAN_POINT ( 'NONE',  ( 112.0659116373989121, -45.48839625182279889, 258.9897919439433167 ) ) ;
#42488 = EDGE_CURVE ( 'NONE', #12869, #68689, #5570, .T. ) ;
#42489 = FACE_OUTER_BOUND ( 'NONE', #44438, .T. ) ;
#42491 = VERTEX_POINT ( 'NONE', #80529 ) ;
#42490 = CARTESIAN_POINT ( 'NONE',  ( 111.8844023637430638, -46.06429852124467317, 272.9556252759110180 ) ) ;
#42492 = EDGE_CURVE ( 'NONE', #24816, #43944, #54122, .T. ) ;
#42493 = FACE_OUTER_BOUND ( 'NONE', #51249, .T. ) ;
#42494 = CARTESIAN_POINT ( 'NONE',  ( 108.3688725116650602, -47.72941199507204146, 162.6822919425769669 ) ) ;
#42495 = CARTESIAN_POINT ( 'NONE',  ( 110.3719271596222882, -47.27686491584164941, 48.80610146638797175 ) ) ;
#42496 = CARTESIAN_POINT ( 'NONE',  ( 97.01638781908712872, -41.44040028630095662, 207.6632443235299661 ) ) ;
#42497 = FACE_OUTER_BOUND ( 'NONE', #41101, .T. ) ;
#42498 = FACE_OUTER_BOUND ( 'NONE', #62307, .T. ) ;
#42500 = DIRECTION ( 'NONE',  ( 0.000000000000000000, 0.000000000000000000, 1.000000000000000000 ) ) ;
#42499 = DIRECTION ( 'NONE',  ( 1.000000000000000000, 0.000000000000000000, 2.108231265501709878E-16 ) ) ;
#42501 = CARTESIAN_POINT ( 'NONE',  ( 97.81169150544869240, -40.51741169384158781, 71.63577594787710723 ) ) ;
#42502 = DIRECTION ( 'NONE',  ( 0.000000000000000000, -1.000000000000000000, 0.000000000000000000 ) ) ;
#42503 = ORIENTED_EDGE ( 'NONE', *, *, #12666, .T. ) ;
#42504 = EDGE_CURVE ( 'NONE', #13582, #12226, #66568, .T. ) ;
#42505 = VECTOR ( 'NONE', #61961, 1000.000000000000000 ) ;
#42506 = DIRECTION ( 'NONE',  ( -1.000000000000000078E-15, 1.000000000000000083E-30, 1.000000000000000000 ) ) ;
#42507 = EDGE_CURVE ( 'NONE', #84121, #63446, #72360, .T. ) ;
#42508 = ORIENTED_EDGE ( 'NONE', *, *, #10297, .T. ) ;
#42509 = ORIENTED_EDGE ( 'NONE', *, *, #70299, .F. ) ;
#42511 = ORIENTED_EDGE ( 'NONE', *, *, #47315, .F. ) ;
#42510 = DIRECTION ( 'NONE',  ( -1.000000000000000000, 0.000000000000000000, -2.108231265501709878E-16 ) ) ;
#42512 = CARTESIAN_POINT ( 'NONE',  ( 101.1533894386775501, -27.41820966596962705, 61.51467289495899138 ) ) ;
#42513 = CARTESIAN_POINT ( 'NONE',  ( 180.3503142329310265, -29.99615139349890569, -5.074374724088000832 ) ) ;
#42514 = EDGE_CURVE ( 'NONE', #23923, #52978, #59301, .T. ) ;
#42515 = CARTESIAN_POINT ( 'NONE',  ( -487.2989999999999782, 101.9113919710471947, 11.11250000000054072 ) ) ;
#42516 = CARTESIAN_POINT ( 'NONE',  ( 117.3342495501102007, -34.51337161069084658, 179.9956252759109532 ) ) ;
#42517 = CARTESIAN_POINT ( 'NONE',  ( 100.7304913082922440, -30.25890808522221320, 270.1276579233149278 ) ) ;
#42518 = ORIENTED_EDGE ( 'NONE', *, *, #59610, .T. ) ;
#42519 = EDGE_LOOP ( 'NONE', ( #88061, #76382, #3279, #68146 ) ) ;
#42520 = ORIENTED_EDGE ( 'NONE', *, *, #76042, .T. ) ;
#42521 = VECTOR ( 'NONE', #65726, 1000.000000000000000 ) ;
#42522 = ORIENTED_EDGE ( 'NONE', *, *, #33467, .F. ) ;
#42523 = CARTESIAN_POINT ( 'NONE',  ( 71.24189083761805819, -0.9290567490904538817, 361.9756252759101471 ) ) ;
#42524 = CARTESIAN_POINT ( 'NONE',  ( 123.6837132603320413, -23.41243780205712710, 249.5838068554165261 ) ) ;
#42526 = AXIS2_PLACEMENT_3D ( 'NONE', #76436, #12886, #41895 ) ;
#42525 = CARTESIAN_POINT ( 'NONE',  ( 68.53801554307449351, 127.0000000000000000, -74.15067561874229796 ) ) ;
#42527 = DIRECTION ( 'NONE',  ( 0.000000000000000000, 1.000000000000000000, 0.000000000000000000 ) ) ;
#42528 = LINE ( 'NONE', #85257, #6968 ) ;
#42529 = LINE ( 'NONE', #83441, #58162 ) ;
#42530 = FACE_OUTER_BOUND ( 'NONE', #23280, .T. ) ;
#42531 = LINE ( 'NONE', #7590, #84032 ) ;
#42532 = CARTESIAN_POINT ( 'NONE',  ( 102.6689224787387502, -46.93780143634764812, 287.2527681330543601 ) ) ;
#42533 = CARTESIAN_POINT ( 'NONE',  ( -3.299561022378064479, 70.25802837517115051, 118.5128751897481436 ) ) ;
#42534 = VERTEX_POINT ( 'NONE', #26891 ) ;
#42535 = ADVANCED_FACE ( 'NONE', ( #41842 ), #32826, .F. ) ;
#42536 = CARTESIAN_POINT ( 'NONE',  ( 115.8254324148542622, -31.73001888479201682, 269.2397919377605717 ) ) ;
#42537 = EDGE_CURVE ( 'NONE', #63160, #87213, #24502, .T. ) ;
#42538 = DIRECTION ( 'NONE',  ( 4.194175870806139918E-14, -1.000000000000000000, 0.000000000000000000 ) ) ;
#42539 = CARTESIAN_POINT ( 'NONE',  ( 112.0375358597863027, -29.64498801284190321, 82.39570941720997155 ) ) ;
#42540 = AXIS2_PLACEMENT_3D ( 'NONE', #6108, #70915, #49539 ) ;
#42541 = FACE_OUTER_BOUND ( 'NONE', #13886, .T. ) ;
#42542 = DIRECTION ( 'NONE',  ( 0.7071067811865969777, -0.7071067811864980568, 0.000000000000000000 ) ) ;
#42543 = ORIENTED_EDGE ( 'NONE', *, *, #26453, .T. ) ;
#42544 = VERTEX_POINT ( 'NONE', #527 ) ;
#42545 = CARTESIAN_POINT ( 'NONE',  ( 117.0609687849609770, -38.07993266210836225, 138.7175048411430396 ) ) ;
#42546 = AXIS2_PLACEMENT_3D ( 'NONE', #52320, #45516, #38721 ) ;
#42547 = ORIENTED_EDGE ( 'NONE', *, *, #191, .T. ) ;
#42548 = ORIENTED_EDGE ( 'NONE', *, *, #2040, .T. ) ;
#42549 = CARTESIAN_POINT ( 'NONE',  ( 116.1082436049511415, -39.28347229878176705, 140.0511071154209617 ) ) ;
#42550 = PLANE ( 'NONE',  #5446 ) ;
#42551 = CARTESIAN_POINT ( 'NONE',  ( 106.6594888599963298, -26.29050016388675104, 81.10705384733896040 ) ) ;
#42552 = DIRECTION ( 'NONE',  ( -1.000000000000000000, 0.000000000000000000, 0.000000000000000000 ) ) ;
#42553 = EDGE_LOOP ( 'NONE', ( #47938, #41355 ) ) ;
#42554 = VERTEX_POINT ( 'NONE', #13718 ) ;
#42555 = VERTEX_POINT ( 'NONE', #6023 ) ;
#42556 = CARTESIAN_POINT ( 'NONE',  ( 41.56648329127499153, -27.82844715994070484, 143.6756252759119832 ) ) ;
#42557 = ORIENTED_EDGE ( 'NONE', *, *, #75434, .T. ) ;
#42558 = CARTESIAN_POINT ( 'NONE',  ( 111.4827405772851847, -46.11507286351704238, 287.9146728949591534 ) ) ;
#42559 = CARTESIAN_POINT ( 'NONE',  ( 112.4974222397575545, -26.16880547358812947, 165.6984824187679521 ) ) ;
#42560 = PLANE ( 'NONE',  #30653 ) ;
#42561 = CARTESIAN_POINT ( 'NONE',  ( 134.0664832912739826, -36.72944715994100306, 14.92562527591099908 ) ) ;
#42562 = CARTESIAN_POINT ( 'NONE',  ( 102.6161641507259219, -46.84718603934155823, 128.2346728949589760 ) ) ;
#42563 = DIRECTION ( 'NONE',  ( 0.000000000000000000, 0.000000000000000000, -1.000000000000000000 ) ) ;
#42564 = VERTEX_POINT ( 'NONE', #14168 ) ;
#42565 = DIRECTION ( 'NONE',  ( 0.000000000000000000, -1.000000000000000000, 0.000000000000000000 ) ) ;
#42566 = ORIENTED_EDGE ( 'NONE', *, *, #67788, .T. ) ;
#42567 = DIRECTION ( 'NONE',  ( 0.000000000000000000, 0.000000000000000000, 1.000000000000000000 ) ) ;
#42569 = ORIENTED_EDGE ( 'NONE', *, *, #40285, .F. ) ;
#42568 = EDGE_CURVE ( 'NONE', #14045, #311, #70943, .T. ) ;
#42570 = CIRCLE ( 'NONE', #67226, 10.00000000000000178 ) ;
#42571 = DIRECTION ( 'NONE',  ( 0.000000000000000000, 0.000000000000000000, 1.000000000000000000 ) ) ;
#42572 = CARTESIAN_POINT ( 'NONE',  ( 194.5664832912739826, 25.62155284005901379, 323.8756252759109202 ) ) ;
#42573 = CARTESIAN_POINT ( 'NONE',  ( 106.2521265061568130, -26.30051002661620885, 25.13848241876792855 ) ) ;
#42574 = DIRECTION ( 'NONE',  ( 0.000000000000000000, 1.000000000000000000, 0.000000000000000000 ) ) ;
#42575 = CIRCLE ( 'NONE', #3446, 38.10000000000000142 ) ;
#42576 = ADVANCED_FACE ( 'NONE', ( #56378 ), #77291, .F. ) ;
#42577 = CARTESIAN_POINT ( 'NONE',  ( 127.0667052882549797, -71.37844715994091871, 55.21780685541800437 ) ) ;
#42578 = CARTESIAN_POINT ( 'NONE',  ( 117.0718954850937052, -35.46248235514278235, 74.92729194266681247 ) ) ;
#42579 = ADVANCED_FACE ( 'NONE', ( #48210, #89134 ), #28226, .T. ) ;
#42580 = CARTESIAN_POINT ( 'NONE',  ( 102.1671273105904447, -43.72604531649727733, 281.5124198280768155 ) ) ;
#42582 = CARTESIAN_POINT ( 'NONE',  ( 112.1095002620001253, -47.42599740258504681, 133.9270538473399768 ) ) ;
#42581 = CARTESIAN_POINT ( 'NONE',  ( 108.4172477039653586, -26.73499932200780549, 109.9689778000439730 ) ) ;
#42583 = DIRECTION ( 'NONE',  ( 1.000000000000000000, 0.000000000000000000, 0.000000000000000000 ) ) ;
#42584 = LINE ( 'NONE', #28989, #13309 ) ;
#42585 = ORIENTED_EDGE ( 'NONE', *, *, #73671, .F. ) ;
#42586 = CARTESIAN_POINT ( 'NONE',  ( 62.03742497533659872, -23.42844715994041493, 129.9678068554150911 ) ) ;
#42587 = EDGE_CURVE ( 'NONE', #15894, #25446, #82332, .T. ) ;
#42588 = CARTESIAN_POINT ( 'NONE',  ( 109.2774118001977826, 53.13983499867891425, 71.43750000000004263 ) ) ;
#42589 = DIRECTION ( 'NONE',  ( 0.000000000000000000, 0.000000000000000000, -1.000000000000000000 ) ) ;
#42590 = VERTEX_POINT ( 'NONE', #47766 ) ;
#42591 = ADVANCED_FACE ( 'NONE', ( #13273 ), #49108, .F. ) ;
#42592 = CARTESIAN_POINT ( 'NONE',  ( 138.8545562996768012, -1.932463243632620342, 394.9756252759100903 ) ) ;
#42594 = VERTEX_POINT ( 'NONE', #68685 ) ;
#42593 = CARTESIAN_POINT ( 'NONE',  ( 116.8478532179160680, -43.50835558345241338, 163.3441967044829823 ) ) ;
#42595 = DIRECTION ( 'NONE',  ( 0.0001484127182338930157, -0.8660253910675250744, 0.5000000000000052180 ) ) ;
#42596 = CARTESIAN_POINT ( 'NONE',  ( 108.1840971438632550, -47.11637154254925974, 198.6613395616249989 ) ) ;
#42597 = CARTESIAN_POINT ( 'NONE',  ( 117.4143231396408851, -32.71451144048268844, 90.10895860924395606 ) ) ;
#42598 = CARTESIAN_POINT ( 'NONE',  ( 96.70122665881119417, 71.54617234588346264, 87.71474477836368067 ) ) ;
#42599 = CARTESIAN_POINT ( 'NONE',  ( 109.7223420879504943, -27.00013639330362381, 190.8647559210611178 ) ) ;
#42600 = CARTESIAN_POINT ( 'NONE',  ( 116.8171228662985470, -34.15291832007721951, 79.03145860929339506 ) ) ;
#42601 = ORIENTED_EDGE ( 'NONE', *, *, #18189, .F. ) ;
#42602 = EDGE_CURVE ( 'NONE', #2492, #74022, #6453, .T. ) ;
#42603 = AXIS2_PLACEMENT_3D ( 'NONE', #30388, #63563, #9494 ) ;
#42604 = ITEM_DEFINED_TRANSFORMATION ( 'NONE', 'NONE', #1460,  #50656 ) ;
#42605 = CIRCLE ( 'NONE', #3462, 2.550000000000006040 ) ;
#42606 = ORIENTED_EDGE ( 'NONE', *, *, #676, .T. ) ;
#42607 = EDGE_CURVE ( 'NONE', #31400, #45771, #83978, .T. ) ;
#42608 = ORIENTED_EDGE ( 'NONE', *, *, #71469, .T. ) ;
#42609 = VECTOR ( 'NONE', #57957, 1000.000000000000000 ) ;
#42610 = ORIENTED_EDGE ( 'NONE', *, *, #89297, .T. ) ;
#42611 = DIRECTION ( 'NONE',  ( 3.100000000000000258E-29, -3.100000000000000044E-14, -1.000000000000000000 ) ) ;
#42612 = CARTESIAN_POINT ( 'NONE',  ( 111.6084932380418735, -46.11308361340533679, 243.9356252759109509 ) ) ;
#42613 = DIRECTION ( 'NONE',  ( 1.000000000000000000, 0.000000000000000000, 0.000000000000000000 ) ) ;
#42614 = CARTESIAN_POINT ( 'NONE',  ( 136.7325000480764743, -18.03188439720356939, 2.979900720422836269 ) ) ;
#42615 = EDGE_CURVE ( 'NONE', #82905, #64449, #30814, .T. ) ;
#42617 = LINE ( 'NONE', #76716, #736 ) ;
#42616 = FACE_OUTER_BOUND ( 'NONE', #67025, .T. ) ;
#42618 = DIRECTION ( 'NONE',  ( 1.000000000000000000, 1.000000000000000078E-15, 1.000000000000000078E-15 ) ) ;
#42619 = CARTESIAN_POINT ( 'NONE',  ( 118.2322726120735155, -40.77409347166903331, 23.54991099019593292 ) ) ;
#42620 = EDGE_LOOP ( 'NONE', ( #84521, #71680, #68514, #84407 ) ) ;
#42621 = VERTEX_POINT ( 'NONE', #9933 ) ;
#42622 = DIRECTION ( 'NONE',  ( 0.000000000000000000, 0.000000000000000000, -1.000000000000000000 ) ) ;
#42623 = CARTESIAN_POINT ( 'NONE',  ( 97.39126582715591951, -39.27842219038148386, 17.53169798143252223 ) ) ;
#42624 = CARTESIAN_POINT ( 'NONE',  ( 114.7458293810856418, -30.61868467657538062, 240.3613395616249875 ) ) ;
#42625 = CARTESIAN_POINT ( 'NONE',  ( 107.0664832912739399, -36.72944715994095333, 293.6369201390379544 ) ) ;
#42626 = CARTESIAN_POINT ( 'NONE',  ( 107.3174176841070846, -26.95189801805073060, 116.0556252759109555 ) ) ;
#42627 = CYLINDRICAL_SURFACE ( 'NONE', #5210, 12.70000000000000107 ) ;
#42628 = LINE ( 'NONE', #41290, #60483 ) ;
#42629 = EDGE_LOOP ( 'NONE', ( #75164, #77279, #26613, #63309 ) ) ;
#42630 = CARTESIAN_POINT ( 'NONE',  ( 32.16397622746000451, -34.03355364505800651, 313.9678068554150059 ) ) ;
#42631 = EDGE_LOOP ( 'NONE', ( #79032, #24351, #49265, #27605 ) ) ;
#42632 = ORIENTED_EDGE ( 'NONE', *, *, #75738, .T. ) ;
#42633 = EDGE_CURVE ( 'NONE', #18458, #18701, #87570, .T. ) ;
#42634 = CARTESIAN_POINT ( 'NONE',  ( -86.13165781700281798, 94.84303900880912863, 81.47101467905625327 ) ) ;
#42635 = CARTESIAN_POINT ( 'NONE',  ( 98.34725308318749626, -40.22966859802066608, 248.0739642582779538 ) ) ;
#42636 = VECTOR ( 'NONE', #12910, 1000.000000000000000 ) ;
#42637 = LINE ( 'NONE', #70373, #50254 ) ;
#42638 = DIRECTION ( 'NONE',  ( -1.000000000000000000, 0.000000000000000000, -2.108231265501709878E-16 ) ) ;
#42639 = VECTOR ( 'NONE', #63265, 1000.000000000000000 ) ;
#42640 = DIRECTION ( 'NONE',  ( 0.5180656453708486486, 0.02186357193551463976, 0.8550613845266940016 ) ) ;
#42641 = CARTESIAN_POINT ( 'NONE',  ( 51.24204729617298426, -31.76306994223730840, 313.9678068554150059 ) ) ;
#42642 = EDGE_LOOP ( 'NONE', ( #35249, #44665, #76410, #38870 ) ) ;
#42643 = CARTESIAN_POINT ( 'NONE',  ( 142.8830277309893404, -77.57998310118428265, 542.9756252759101471 ) ) ;
#42644 = CYLINDRICAL_SURFACE ( 'NONE', #52750, 4.874999999999990230 ) ;
#42645 = ORIENTED_EDGE ( 'NONE', *, *, #82969, .T. ) ;
#42646 = CARTESIAN_POINT ( 'NONE',  ( 104.7356349775885320, -47.53436426244870461, 32.41943479972098174 ) ) ;
#42647 = ORIENTED_EDGE ( 'NONE', *, *, #68497, .T. ) ;
#42648 = CARTESIAN_POINT ( 'NONE',  ( 116.1953253310505119, -40.03623866633203932, 22.97241982807796035 ) ) ;
#42649 = CARTESIAN_POINT ( 'NONE',  ( 105.7166318498146325, -46.72402321261439795, 127.4690705953080965 ) ) ;
#42650 = CARTESIAN_POINT ( 'NONE',  ( 103.2980200187117390, -27.06831524915186904, 170.3603871806729444 ) ) ;
#42651 = ADVANCED_FACE ( 'NONE', ( #35948 ), #51237, .T. ) ;
#42652 = CARTESIAN_POINT ( 'NONE',  ( 143.0664832912740110, -18.82844715994099971, 323.8756252759120002 ) ) ;
#42653 = DIRECTION ( 'NONE',  ( 0.000000000000000000, 1.000000000000000000, 0.000000000000000000 ) ) ;
#42654 = CARTESIAN_POINT ( 'NONE',  ( 107.0664832912739968, -36.72944715994100306, 287.6356252759109680 ) ) ;
#42655 = DIRECTION ( 'NONE',  ( 1.000000000000000000, 4.299999999999999979E-14, 1.000000000000000078E-15 ) ) ;
#42656 = CARTESIAN_POINT ( 'NONE',  ( 100.1487569102796300, -45.40945638099971404, 268.0289586092443415 ) ) ;
#42657 = CARTESIAN_POINT ( 'NONE',  ( 83.24211534968729609, 95.24969287062863543, -84.42134122279055930 ) ) ;
#42658 = EDGE_LOOP ( 'NONE', ( #37949, #7955, #63053, #86622 ) ) ;
#42659 = ADVANCED_FACE ( 'NONE', ( #24453 ), #23575, .F. ) ;
#42660 = CARTESIAN_POINT ( 'NONE',  ( 136.7765779009440621, -37.19711456032074892, 6.808568500765878717 ) ) ;
#42661 = VECTOR ( 'NONE', #40093, 1000.000000000000000 ) ;
#42662 = VERTEX_POINT ( 'NONE', #31246 ) ;
#42663 = CARTESIAN_POINT ( 'NONE',  ( 117.9205228141932054, -39.05050820906062370, 104.6708633711489824 ) ) ;
#42664 = LINE ( 'NONE', #82706, #10544 ) ;
#42665 = AXIS2_PLACEMENT_3D ( 'NONE', #60144, #73797, #23444 ) ;
#42666 = CIRCLE ( 'NONE', #3526, 1.000000000000000888 ) ;
#42667 = ORIENTED_EDGE ( 'NONE', *, *, #14935, .T. ) ;
#42668 = EDGE_LOOP ( 'NONE', ( #35539, #22691, #11416, #45422 ) ) ;
#42669 = EDGE_LOOP ( 'NONE', ( #40918, #81132, #63826, #2463 ) ) ;
#42670 = CIRCLE ( 'NONE', #71693, 4.762500000000002842 ) ;
#42671 = DIRECTION ( 'NONE',  ( 0.000000000000000000, 1.000000000000000000, 0.000000000000000000 ) ) ;
#42672 = AXIS2_PLACEMENT_3D ( 'NONE', #87781, #12373, #33711 ) ;
#42673 = CARTESIAN_POINT ( 'NONE',  ( 115.8254327561651280, -31.73001971868101023, 265.2397918660585105 ) ) ;
#42674 = CARTESIAN_POINT ( 'NONE',  ( 179.1667039024460166, -26.71338133339251542, -5.074374724088000832 ) ) ;
#42675 = CARTESIAN_POINT ( 'NONE',  ( 145.5804755031010700, -139.1646755592869056, 245.6810956053649875 ) ) ;
#42676 = LINE ( 'NONE', #35425, #2596 ) ;
#42677 = CARTESIAN_POINT ( 'NONE',  ( 104.7356836917145699, -47.53413844247978659, 28.41943479971997988 ) ) ;
#42678 = PLANE ( 'NONE',  #69726 ) ;
#42679 = ORIENTED_EDGE ( 'NONE', *, *, #33588, .T. ) ;
#42680 = DIRECTION ( 'NONE',  ( -1.000000000000000000, 0.000000000000000000, 0.000000000000000000 ) ) ;
#42681 = CARTESIAN_POINT ( 'NONE',  ( -74.15067561874319324, 120.6499999999999915, 68.53801554307369770 ) ) ;
#42682 = EDGE_LOOP ( 'NONE', ( #80483, #32248, #16291 ) ) ;
#42683 = ORIENTED_EDGE ( 'NONE', *, *, #9802, .F. ) ;
#42684 = DIRECTION ( 'NONE',  ( 0.000000000000000000, 0.000000000000000000, -1.000000000000000000 ) ) ;
#42685 = DIRECTION ( 'NONE',  ( 0.7071067811865764385, -0.7071067811865187069, 7.071067811865771156E-16 ) ) ;
#42686 =( NAMED_UNIT ( * ) SI_UNIT ( $, .STERADIAN. ) SOLID_ANGLE_UNIT ( ) );
#42687 = EDGE_CURVE ( 'NONE', #19992, #39136, #44880, .T. ) ;
#42688 = CARTESIAN_POINT ( 'NONE',  ( 71.25529199314597406, -79.12815651470189948, 361.9756252759101471 ) ) ;
#42689 = FACE_OUTER_BOUND ( 'NONE', #34289, .T. ) ;
#42690 = EDGE_CURVE ( 'NONE', #22696, #17346, #42740, .T. ) ;
#42691 = CARTESIAN_POINT ( 'NONE',  ( 115.5441482490607257, -35.68765611295631857, 193.3467055423629688 ) ) ;
#42692 = CARTESIAN_POINT ( 'NONE',  ( 107.0667039024467329, -19.99944715994091027, 195.5838068554170093 ) ) ;
#42693 = CARTESIAN_POINT ( 'NONE',  ( 124.6194816332305635, 70.85869709054320253, 38.92310640268541988 ) ) ;
#42694 = CARTESIAN_POINT ( 'NONE',  ( 118.8926602832294037, -35.39890769255473657, 83.91562527591095488 ) ) ;
#42695 = ORIENTED_EDGE ( 'NONE', *, *, #30943, .F. ) ;
#42696 = CARTESIAN_POINT ( 'NONE',  ( 32.24491389930098251, -32.11662333284611748, -5.074374724088000832 ) ) ;
#42697 = ORIENTED_EDGE ( 'NONE', *, *, #81812, .T. ) ;
#42698 = EDGE_CURVE ( 'NONE', #40009, #48304, #32141, .T. ) ;
#42699 = CARTESIAN_POINT ( 'NONE',  ( 98.34844285637596784, -31.65902197265687334, 276.9066052923088250 ) ) ;
#42700 = ORIENTED_EDGE ( 'NONE', *, *, #3038, .F. ) ;
#42701 = CARTESIAN_POINT ( 'NONE',  ( 104.4897565938694584, -26.97885740413062550, 50.28147460018952586 ) ) ;
#42702 = EDGE_CURVE ( 'NONE', #9938, #36669, #25925, .T. ) ;
#42703 = VERTEX_POINT ( 'NONE', #15066 ) ;
#42704 = DIRECTION ( 'NONE',  ( 0.000000000000000000, -1.000000000000007375E-15, -1.000000000000000000 ) ) ;
#42705 = CARTESIAN_POINT ( 'NONE',  ( 68.49250842242263104, -104.4395400694435807, 247.6452922128490002 ) ) ;
#42706 = CIRCLE ( 'NONE', #60076, 9.525000000000000355 ) ;
#42707 = FACE_OUTER_BOUND ( 'NONE', #47460, .T. ) ;
#42708 = ORIENTED_EDGE ( 'NONE', *, *, #49885, .F. ) ;
#42709 = CARTESIAN_POINT ( 'NONE',  ( 109.6484814735558189, -46.85267042889636002, 47.77562527591094721 ) ) ;
#42710 = AXIS2_PLACEMENT_3D ( 'NONE', #49859, #77590, #43039 ) ;
#42712 = CARTESIAN_POINT ( 'NONE',  ( 86.67141577317461554, 72.45841406287409825, -97.63922045723883514 ) ) ;
#42711 = CARTESIAN_POINT ( 'NONE',  ( 68.56670390244700286, -71.37844715994098976, 55.21780685541800437 ) ) ;
#42713 = LINE ( 'NONE', #8227, #84421 ) ;
#42714 = CARTESIAN_POINT ( 'NONE',  ( 101.9936209166423993, -45.44607152480659096, 142.1564586070478526 ) ) ;
#42715 = VERTEX_POINT ( 'NONE', #73032 ) ;
#42716 = EDGE_CURVE ( 'NONE', #19408, #36906, #87128, .T. ) ;
#42717 = CARTESIAN_POINT ( 'NONE',  ( 115.5843262439540808, -31.42642995851512566, 120.2690150466928571 ) ) ;
#42718 = CYLINDRICAL_SURFACE ( 'NONE', #86082, 2.749999999999974687 ) ;
#42719 = DIRECTION ( 'NONE',  ( 6.982966722218760189E-15, 0.000000000000000000, 1.000000000000000000 ) ) ;
#42720 = CARTESIAN_POINT ( 'NONE',  ( 98.13097783494514204, -43.27482323654912477, 102.8175300378159847 ) ) ;
#42722 = DIRECTION ( 'NONE',  ( -8.843517682682131024E-16, 1.000000000000000000, 1.156482317317870556E-31 ) ) ;
#42721 = DIRECTION ( 'NONE',  ( 0.000000000000000000, 0.000000000000000000, -1.000000000000000000 ) ) ;
#42723 = LINE ( 'NONE', #967, #84361 ) ;
#42724 = CIRCLE ( 'NONE', #70305, 16.09746158385918946 ) ;
#42725 = ORIENTED_EDGE ( 'NONE', *, *, #23596, .T. ) ;
#42726 = AXIS2_PLACEMENT_3D ( 'NONE', #15505, #83650, #35926 ) ;
#42727 = VECTOR ( 'NONE', #50345, 1000.000000000000000 ) ;
#42728 = AXIS2_PLACEMENT_3D ( 'NONE', #43826, #63848, #1173 ) ;
#42729 = DIRECTION ( 'NONE',  ( -1.000000000000000000, 0.000000000000000000, -2.108231265501709878E-16 ) ) ;
#42730 = CARTESIAN_POINT ( 'NONE',  ( 113.6473777113567820, -44.00994186338851932, 129.1613395616249704 ) ) ;
#42732 = ORIENTED_EDGE ( 'NONE', *, *, #6009, .F. ) ;
#42731 = CARTESIAN_POINT ( 'NONE',  ( 156.5667039024482108, -42.82844715993568485, 295.7178068554149490 ) ) ;
#42733 = AXIS2_PLACEMENT_3D ( 'NONE', #40138, #6528, #81516 ) ;
#42734 = AXIS2_PLACEMENT_3D ( 'NONE', #77744, #20982, #28225 ) ;
#42735 = CARTESIAN_POINT ( 'NONE',  ( 112.4780167374715631, -46.34085331822165443, 253.9965776568634510 ) ) ;
#42736 = FACE_BOUND ( 'NONE', #38443, .T. ) ;
#42737 = CARTESIAN_POINT ( 'NONE',  ( 184.5667039024483245, -48.82844715993448403, 300.4678068554149490 ) ) ;
#42738 = CARTESIAN_POINT ( 'NONE',  ( 116.4407914430478570, -78.35517403977316064, 250.2178068554180470 ) ) ;
#42739 = PLANE ( 'NONE',  #9439 ) ;
#42740 = LINE ( 'NONE', #66666, #68006 ) ;
#42741 = CARTESIAN_POINT ( 'NONE',  ( 97.81193015299326987, -40.51731617131004271, 31.63594527021773573 ) ) ;
#42742 = CARTESIAN_POINT ( 'NONE',  ( 96.86352172870815025, -32.31225822881502552, 211.0013395616259686 ) ) ;
#42743 = VERTEX_POINT ( 'NONE', #10371 ) ;
#42744 = ORIENTED_EDGE ( 'NONE', *, *, #2457, .F. ) ;
#42745 = EDGE_CURVE ( 'NONE', #25185, #36098, #52119, .T. ) ;
#42746 = CARTESIAN_POINT ( 'NONE',  ( 115.3457950989190408, -42.46736495413998824, 159.7758690201829666 ) ) ;
#42747 = CARTESIAN_POINT ( 'NONE',  ( 83.06670390244801183, -42.97311385574013798, 231.5838068554169524 ) ) ;
#42748 = CARTESIAN_POINT ( 'NONE',  ( 98.59875070808803343, -39.34206841476268579, 17.99586902018296541 ) ) ;
#42749 = CARTESIAN_POINT ( 'NONE',  ( -123.4696824136392053, 0.000000000000000000, -179.8898777604655095 ) ) ;
#42750 = ADVANCED_FACE ( 'NONE', ( #70480 ), #3998, .F. ) ;
#42751 = VECTOR ( 'NONE', #37026, 1000.000000000000000 ) ;
#42752 = CARTESIAN_POINT ( 'NONE',  ( -72.96458098368751166, 117.4749999999999943, 65.82083098368619289 ) ) ;
#42753 = DIRECTION ( 'NONE',  ( 0.000000000000000000, 0.000000000000000000, 1.000000000000000000 ) ) ;
#42754 = CARTESIAN_POINT ( 'NONE',  ( 112.1393456400033699, -28.01282278016224225, 105.6564586093976601 ) ) ;
#42755 = DIRECTION ( 'NONE',  ( 0.000000000000000000, 1.000000000000000000, 0.000000000000000000 ) ) ;
#42756 = CARTESIAN_POINT ( 'NONE',  ( 113.2071528006340628, -45.12711609280825087, 228.0784824187679760 ) ) ;
#42757 = CARTESIAN_POINT ( 'NONE',  ( 97.70686550411159033, -40.25212671267365749, 171.6131552557610860 ) ) ;
#42758 = EDGE_LOOP ( 'NONE', ( #9512, #36167, #89158, #48132 ) ) ;
#42759 = ORIENTED_EDGE ( 'NONE', *, *, #48854, .T. ) ;
#42760 = CARTESIAN_POINT ( 'NONE',  ( 116.7951252700267304, -39.38782979579554677, 88.61479194211217703 ) ) ;
#42761 = CARTESIAN_POINT ( 'NONE',  ( -79.76258624986827783, 93.94553785444264804, -87.71311422381560874 ) ) ;
#42762 = CARTESIAN_POINT ( 'NONE',  ( 3.174999999999889688, 24.56180297284579694, -31.75000000000000000 ) ) ;
#42763 = DIRECTION ( 'NONE',  ( -0.000000000000000000, -1.000000000000000000, -0.000000000000000000 ) ) ;
#42764 = CARTESIAN_POINT ( 'NONE',  ( 115.3461623907573710, -31.52268719801068642, 30.27276813305296344 ) ) ;
#42765 = CARTESIAN_POINT ( 'NONE',  ( 194.5667039024479834, -67.87844715994100397, 300.9178068554150514 ) ) ;
#42766 = ORIENTED_EDGE ( 'NONE', *, *, #11030, .F. ) ;
#42767 = EDGE_CURVE ( 'NONE', #58352, #36440, #16743, .T. ) ;
#42768 = DIRECTION ( 'NONE',  ( -4.237773401492740281E-14, 1.000000000000000000, 0.000000000000000000 ) ) ;
#42770 = LINE ( 'NONE', #8284, #16329 ) ;
#42769 = SHAPE_REPRESENTATION ( 'Pneumatic Workpiece Fixture Plate', ( #50656 ), #89914 ) ;
#42771 = VECTOR ( 'NONE', #32997, 1000.000000000000114 ) ;
#42772 = CARTESIAN_POINT ( 'NONE',  ( 100.8483124575627414, -45.14135884264823773, 257.0699109901967745 ) ) ;
#42773 = ORIENTED_EDGE ( 'NONE', *, *, #39272, .T. ) ;
#42774 = CARTESIAN_POINT ( 'NONE',  ( 25.56670390244797275, -67.87844715994100397, 298.0928068554150627 ) ) ;
#42775 = CARTESIAN_POINT ( 'NONE',  ( -458.3598257906459708, 47.62500000000000000, 3.174999999999999822 ) ) ;
#42776 = CARTESIAN_POINT ( 'NONE',  ( 110.8537518669637194, -45.98453207236645568, 167.8855633520927597 ) ) ;
#42777 = CARTESIAN_POINT ( 'NONE',  ( 106.9575452361726491, -28.53976946500068124, 57.90523322673496409 ) ) ;
#42778 = CARTESIAN_POINT ( 'NONE',  ( 113.7646124051505154, -44.74644941934948861, 189.1299109901969757 ) ) ;
#42779 = LINE ( 'NONE', #70522, #27577 ) ;
#42780 = ORIENTED_EDGE ( 'NONE', *, *, #17087, .F. ) ;
#42781 = CARTESIAN_POINT ( 'NONE',  ( 152.0371591254585724, -47.82818131005588214, 129.9678068554149775 ) ) ;
#42782 = ORIENTED_EDGE ( 'NONE', *, *, #11536, .T. ) ;
#42783 = ORIENTED_EDGE ( 'NONE', *, *, #78215, .F. ) ;
#42784 = VECTOR ( 'NONE', #39619, 1000.000000000000000 ) ;
#42785 = CIRCLE ( 'NONE', #10903, 2.030000000001807248 ) ;
#42786 = FACE_OUTER_BOUND ( 'NONE', #28338, .T. ) ;
#42787 = VECTOR ( 'NONE', #22565, 1000.000000000000000 ) ;
#42788 = ORIENTED_EDGE ( 'NONE', *, *, #58904, .F. ) ;
#42789 = ORIENTED_EDGE ( 'NONE', *, *, #84455, .T. ) ;
#42790 = PLANE ( 'NONE',  #30931 ) ;
#42791 = AXIS2_PLACEMENT_3D ( 'NONE', #81476, #46903, #63248 ) ;
#42792 = CARTESIAN_POINT ( 'NONE',  ( 106.7492034591024890, -25.27298593721235065, 320.5317020237883980 ) ) ;
#42793 = ADVANCED_FACE ( 'NONE', ( #44422, #72158 ), #79883, .F. ) ;
#42794 = CARTESIAN_POINT ( 'NONE',  ( 112.3425469992411649, -30.01235824646559891, 78.96956268521998368 ) ) ;
#42796 = CARTESIAN_POINT ( 'NONE',  ( 102.3692588328596571, -47.63350050119395007, 287.2527681330535643 ) ) ;
#42795 = VECTOR ( 'NONE', #48183, 1000.000000000000000 ) ;
#42797 = DIRECTION ( 'NONE',  ( 1.000000000000000000, 6.508581945447490214E-14, 1.000000000000000078E-15 ) ) ;
#42798 = ADVANCED_FACE ( 'NONE', ( #58506 ), #86232, .F. ) ;
#42799 = LINE ( 'NONE', #70539, #71540 ) ;
#42800 = VERTEX_POINT ( 'NONE', #56823 ) ;
#42801 = EDGE_CURVE ( 'NONE', #73498, #32398, #57453, .T. ) ;
#42802 = VERTEX_POINT ( 'NONE', #20331 ) ;
#42803 = CARTESIAN_POINT ( 'NONE',  ( 131.0667039024480118, -64.87844715994098976, 225.9838068554150254 ) ) ;
#42804 = CARTESIAN_POINT ( 'NONE',  ( 107.0664832912739968, -18.82844715994099971, 333.4006252759120343 ) ) ;
#42805 = CARTESIAN_POINT ( 'NONE',  ( 70.60950597247970961, -139.6386892047443951, 247.2886496850582887 ) ) ;
#42806 = AXIS2_PLACEMENT_3D ( 'NONE', #28217, #6888, #41394 ) ;
#42807 = CARTESIAN_POINT ( 'NONE',  ( 105.0928733274061670, -25.78792777683064585, 125.2184824187689856 ) ) ;
#42808 = CARTESIAN_POINT ( 'NONE',  ( 114.7585751371172051, -43.83144610948713193, 123.2327681330539519 ) ) ;
#42809 = LINE ( 'NONE', #57799, #65416 ) ;
#42810 = VERTEX_POINT ( 'NONE', #47997 ) ;
#42811 = CARTESIAN_POINT ( 'NONE',  ( 99.53925745938779812, -29.46537268684611632, 250.7156252759109520 ) ) ;
#42812 = DIRECTION ( 'NONE',  ( 8.673617379884035472E-16, 1.000000000000000000, 0.000000000000000000 ) ) ;
#42813 = CARTESIAN_POINT ( 'NONE',  ( 11.74129241494043896, 77.70931405037566719, 130.0269635525507965 ) ) ;
#42814 = CARTESIAN_POINT ( 'NONE',  ( 98.42298862519912461, -41.77040527891428923, 27.74721501551390546 ) ) ;
#42815 = CIRCLE ( 'NONE', #45724, 17.00000000000000000 ) ;
#42817 = DIRECTION ( 'NONE',  ( 0.000000000000000000, 0.000000000000000000, 1.000000000000000000 ) ) ;
#42816 = CARTESIAN_POINT ( 'NONE',  ( -492.0614999999999668, 93.66249999999999432, 85.72499999999999432 ) ) ;
#42818 = DIRECTION ( 'NONE',  ( -0.000000000000000000, -0.000000000000000000, 1.000000000000000000 ) ) ;
#42819 = CARTESIAN_POINT ( 'NONE',  ( 3.174999999999879918, 124.5870000000000033, 33.98325472291465132 ) ) ;
#42820 = CARTESIAN_POINT ( 'NONE',  ( 0.4144849534825713055, 95.24999999999998579, -118.5559999999999832 ) ) ;
#42821 = EDGE_CURVE ( 'NONE', #77789, #16763, #50619, .T. ) ;
#42822 = CARTESIAN_POINT ( 'NONE',  ( -12.29205751230851362, 85.84923025428281562, 129.9761558897302791 ) ) ;
#42823 = EDGE_CURVE ( 'NONE', #33432, #79965, #81056, .T. ) ;
#42824 = CARTESIAN_POINT ( 'NONE',  ( -72.96458098368751166, 117.4749999999999943, 65.02708098368620426 ) ) ;
#42825 = DIRECTION ( 'NONE',  ( 0.000000000000000000, -1.000000000000000000, 0.000000000000000000 ) ) ;
#42827 = ORIENTED_EDGE ( 'NONE', *, *, #27206, .F. ) ;
#42826 = CARTESIAN_POINT ( 'NONE',  ( 97.06107110202495392, -37.99641200327471324, 261.4272919457318380 ) ) ;
#42828 = CARTESIAN_POINT ( 'NONE',  ( 126.1218394983597335, -124.1980709993372187, 250.2178068554179902 ) ) ;
#42829 = CARTESIAN_POINT ( 'NONE',  ( 97.53973001301494605, -43.81993288943278486, 261.8356252759109566 ) ) ;
#42830 = CARTESIAN_POINT ( 'NONE',  ( 105.7204281913532355, -24.95562743476950018, 156.1670538473399574 ) ) ;
#42831 = CARTESIAN_POINT ( 'NONE',  ( 100.5841487926172277, -28.49196697857695781, 11.60705384733995515 ) ) ;
#42832 = PLANE ( 'NONE',  #72235 ) ;
#42834 = CARTESIAN_POINT ( 'NONE',  ( 82.45780623542886190, -35.36823420009603325, 7.200493380643411712 ) ) ;
#42833 = FACE_OUTER_BOUND ( 'NONE', #48346, .T. ) ;
#42835 = DIRECTION ( 'NONE',  ( -0.7071067811865170416, -0.7071067811865778818, -7.071067811865162747E-16 ) ) ;
#42836 = VECTOR ( 'NONE', #18684, 1000.000000000000000 ) ;
#42837 = AXIS2_PLACEMENT_3D ( 'NONE', #25630, #78838, #16597 ) ;
#42838 = ORIENTED_EDGE ( 'NONE', *, *, #43090, .F. ) ;
#42839 = CARTESIAN_POINT ( 'NONE',  ( 139.7494832912729805, -71.52944715994142655, 342.9256252759109884 ) ) ;
#42840 = ORIENTED_EDGE ( 'NONE', *, *, #29281, .F. ) ;
#42841 = CARTESIAN_POINT ( 'NONE',  ( 102.9572487778789878, -44.79956872283601399, 171.6362293518859587 ) ) ;
#42843 = ORIENTED_EDGE ( 'NONE', *, *, #45242, .F. ) ;
#42842 = CARTESIAN_POINT ( 'NONE',  ( -487.2989999999999782, 14.28750000000036025, 2.863608028952925100 ) ) ;
#42844 = CARTESIAN_POINT ( 'NONE',  ( 152.0371591254585155, -47.82818131005588214, 180.4678068554149775 ) ) ;
#42845 = CARTESIAN_POINT ( 'NONE',  ( 109.4403364888816981, -25.95778788316477304, 175.8918157521009391 ) ) ;
#42846 = CARTESIAN_POINT ( 'NONE',  ( 63.06670390244699576, -67.87844715994098976, 155.2178068554179902 ) ) ;
#42847 = DIRECTION ( 'NONE',  ( 1.000000000000000000, 0.000000000000000000, 0.000000000000000000 ) ) ;
#42848 = DIRECTION ( 'NONE',  ( 0.000000000000000000, 0.000000000000000000, -1.000000000000000000 ) ) ;
#42849 = CARTESIAN_POINT ( 'NONE',  ( -85.85219768521552908, 70.17671898886891313, 81.76240029069619197 ) ) ;
#42850 = CARTESIAN_POINT ( 'NONE',  ( 172.5664832912740110, -9.303447159940999356, 258.9256252759120116 ) ) ;
#42851 = CARTESIAN_POINT ( 'NONE',  ( 99.36524671511898532, -42.81259845621070781, 91.85848241876892928 ) ) ;
#42852 = ORIENTED_EDGE ( 'NONE', *, *, #65025, .T. ) ;
#42853 = ORIENTED_EDGE ( 'NONE', *, *, #50054, .F. ) ;
#42854 = EDGE_CURVE ( 'NONE', #23593, #79245, #88019, .T. ) ;
#42855 = ORIENTED_EDGE ( 'NONE', *, *, #82005, .T. ) ;
#42856 = AXIS2_PLACEMENT_3D ( 'NONE', #76283, #41292, #7250 ) ;
#42857 = CARTESIAN_POINT ( 'NONE',  ( 113.2603198993755882, -43.06700715444978300, 69.62444044875392990 ) ) ;
#42858 = AXIS2_PLACEMENT_3D ( 'NONE', #46418, #54120, #13271 ) ;
#42859 = FACE_OUTER_BOUND ( 'NONE', #58136, .T. ) ;
#42861 = LINE ( 'NONE', #43313, #1210 ) ;
#42860 = CARTESIAN_POINT ( 'NONE',  ( 114.4768422515204094, -30.34587328852060395, 180.3927681330529538 ) ) ;
#42862 = AXIS2_PLACEMENT_3D ( 'NONE', #59841, #74838, #88479 ) ;
#42863 = CARTESIAN_POINT ( 'NONE',  ( 41.56648329127399677, -9.303447159940999356, 258.9256252759120116 ) ) ;
#42865 = EDGE_CURVE ( 'NONE', #48000, #24335, #40746, .T. ) ;
#42864 = CARTESIAN_POINT ( 'NONE',  ( 239.7378999999999962, 52.73749999999999716, -2.903194600000015502 ) ) ;
#42867 = FACE_OUTER_BOUND ( 'NONE', #12961, .T. ) ;
#42866 = VECTOR ( 'NONE', #47413, 1000.000000000000000 ) ;
#42868 = LINE ( 'NONE', #1566, #20228 ) ;
#42869 = CARTESIAN_POINT ( 'NONE',  ( 67.07045655335387835, -67.88107680039439629, 245.6130415843593937 ) ) ;
#42870 = CARTESIAN_POINT ( 'NONE',  ( 98.47430666977638225, -42.65725675464092603, 126.8070538473389490 ) ) ;
#42871 = ORIENTED_EDGE ( 'NONE', *, *, #45371, .T. ) ;
#42872 = EDGE_LOOP ( 'NONE', ( #47462, #53032 ) ) ;
#42873 = ORIENTED_EDGE ( 'NONE', *, *, #35302, .F. ) ;
#42874 = AXIS2_PLACEMENT_3D ( 'NONE', #72811, #9254, #59602 ) ;
#42875 = CARTESIAN_POINT ( 'NONE',  ( 10.33379165269208499, 75.15577250977247559, 130.1465911299492006 ) ) ;
#42876 = CARTESIAN_POINT ( 'NONE',  ( 134.0667039024469602, -40.87844715994091871, 55.21780685541800437 ) ) ;
#42877 = CARTESIAN_POINT ( 'NONE',  ( 115.0372575023011450, -42.90846257223464022, 79.30229194203350573 ) ) ;
#42878 = CARTESIAN_POINT ( 'NONE',  ( 158.0667039024469886, -67.87844715994090450, 155.2178068554179902 ) ) ;
#42880 = CARTESIAN_POINT ( 'NONE',  ( 115.1674193411231784, -35.52216783720512439, 216.7623760838769726 ) ) ;
#42879 = VECTOR ( 'NONE', #55794, 1000.000000000000000 ) ;
#42881 = CARTESIAN_POINT ( 'NONE',  ( 103.3797721312301547, -105.8297479413476196, 2.217806855418058554 ) ) ;
#42882 = AXIS2_PLACEMENT_3D ( 'NONE', #41823, #75481, #44515 ) ;
#42883 = CARTESIAN_POINT ( 'NONE',  ( 1.926769467660224795E-14, 17.78000000000000114, 154.1697486074984909 ) ) ;
#42884 = ORIENTED_EDGE ( 'NONE', *, *, #23161, .F. ) ;
#42886 = ORIENTED_EDGE ( 'NONE', *, *, #69446, .T. ) ;
#42885 = ORIENTED_EDGE ( 'NONE', *, *, #3523, .T. ) ;
#42887 = DIRECTION ( 'NONE',  ( 1.000000000000000000, 0.000000000000000000, 0.000000000000000000 ) ) ;
#42888 = VERTEX_POINT ( 'NONE', #33935 ) ;
#42889 = ORIENTED_EDGE ( 'NONE', *, *, #1410, .T. ) ;
#42890 = DIRECTION ( 'NONE',  ( 0.000000000000000000, -1.000000000000000000, 0.000000000000000000 ) ) ;
#42891 = DIRECTION ( 'NONE',  ( -1.000000000000000000, -4.299999999999999979E-14, -1.000000000000000078E-15 ) ) ;
#42892 = CARTESIAN_POINT ( 'NONE',  ( 116.4035850909244090, -35.68299815489336879, 230.3349166392299594 ) ) ;
#42893 = EDGE_CURVE ( 'NONE', #78995, #16194, #62224, .T. ) ;
#42894 = CARTESIAN_POINT ( 'NONE',  ( 116.8171228894634481, -34.15291837667594166, 274.0314586044273710 ) ) ;
#42895 = ORIENTED_EDGE ( 'NONE', *, *, #19126, .T. ) ;
#42896 = DIRECTION ( 'NONE',  ( 1.000000000000000000, 0.000000000000000000, 0.000000000000000000 ) ) ;
#42897 = DIRECTION ( 'NONE',  ( 0.000000000000000000, 0.000000000000000000, -1.000000000000000000 ) ) ;
#42898 = ORIENTED_EDGE ( 'NONE', *, *, #57479, .T. ) ;
#42899 = VERTEX_POINT ( 'NONE', #27131 ) ;
#42900 = B_SPLINE_CURVE_WITH_KNOTS ( 'NONE', 3,
 ( #89243, #47428, #54676, #61070, #26116, #25657, #74706, #6559, #13383, #82441 ),
 .UNSPECIFIED., .F., .F.,
 ( 4, 3, 3, 4 ),
 ( 0.000000000000000000, 0.0007422984837643878831, 0.001113447966056068956, 0.001484597482653254429 ),
 .UNSPECIFIED. ) ;
#42901 = CARTESIAN_POINT ( 'NONE',  ( 41.56648329127398966, -18.82844715994071194, 18.92562527591200094 ) ) ;
#42902 = AXIS2_PLACEMENT_3D ( 'NONE', #26155, #46572, #45666 ) ;
#42903 = ORIENTED_EDGE ( 'NONE', *, *, #40048, .T. ) ;
#42904 = ORIENTED_EDGE ( 'NONE', *, *, #51008, .T. ) ;
#42905 = ADVANCED_FACE ( 'NONE', ( #12163 ), #68015, .F. ) ;
#42906 = CARTESIAN_POINT ( 'NONE',  ( 105.1260075982565212, -28.80065313513137326, 283.0852332267343172 ) ) ;
#42907 = CARTESIAN_POINT ( 'NONE',  ( 117.4484615961127218, -30.96329225543088270, 179.2299109901959753 ) ) ;
#42908 = CARTESIAN_POINT ( 'NONE',  ( 101.7670726180548115, -27.05576796868577460, 100.4632443235299633 ) ) ;
#42909 =( LENGTH_UNIT ( ) NAMED_UNIT ( * ) SI_UNIT ( .MILLI., .METRE. ) );
#42910 = CARTESIAN_POINT ( 'NONE',  ( 117.2274905824790778, -41.08006910540670731, 209.5165776568640013 ) ) ;
#42911 = DIRECTION ( 'NONE',  ( 1.000000000000000078E-15, -1.000000000000000083E-30, -1.000000000000000000 ) ) ;
#42912 = ADVANCED_FACE ( 'NONE', ( #54807 ), #40508, .T. ) ;
#42913 = DIRECTION ( 'NONE',  ( -0.000000000000000000, 1.000000000000000000, -0.000000000000000000 ) ) ;
#42914 = ORIENTED_EDGE ( 'NONE', *, *, #25280, .F. ) ;
#42915 = DIRECTION ( 'NONE',  ( -1.000000000000000078E-15, -1.000000000000000083E-30, 1.000000000000000000 ) ) ;
#42916 = ORIENTED_EDGE ( 'NONE', *, *, #41404, .T. ) ;
#42917 = ORIENTED_EDGE ( 'NONE', *, *, #30213, .F. ) ;
#42918 = CARTESIAN_POINT ( 'NONE',  ( 34.67381068360336371, -28.98061976759059988, 193.9678068554150911 ) ) ;
#42919 = VECTOR ( 'NONE', #82460, 1000.000000000000114 ) ;
#42920 = VECTOR ( 'NONE', #28685, 1000.000000000000000 ) ;
#42921 = VERTEX_POINT ( 'NONE', #19871 ) ;
#42922 = CARTESIAN_POINT ( 'NONE',  ( 108.3194705677269809, -47.07918403323724021, 117.6727681330539639 ) ) ;
#42923 = CARTESIAN_POINT ( 'NONE',  ( 97.31575241016307132, -39.30575056309270110, 256.5314103656009479 ) ) ;
#42924 = AXIS2_PLACEMENT_3D ( 'NONE', #18752, #40535, #46436 ) ;
#42925 = CARTESIAN_POINT ( 'NONE',  ( 91.91125933621931665, -109.6038751290247006, -21.02845593540910230 ) ) ;
#42926 = CARTESIAN_POINT ( 'NONE',  ( 52.65249034007830176, -49.32844715994059470, 300.4678068554150059 ) ) ;
#42929 = CARTESIAN_POINT ( 'NONE',  ( 117.4688788178165737, -35.86077403649778716, 249.8927681330537780 ) ) ;
#42928 = PLANE ( 'NONE',  #51359 ) ;
#42927 = CARTESIAN_POINT ( 'NONE',  ( 34.96670390244654669, -26.71338133339322951, 117.4678068554150485 ) ) ;
#42930 = DIRECTION ( 'NONE',  ( 1.000000000000000000, 1.000000000000000078E-15, 0.000000000000000000 ) ) ;
#42931 = CARTESIAN_POINT ( 'NONE',  ( 0.000000000000000000, 101.5999999999999943, 0.000000000000000000 ) ) ;
#42932 = LINE ( 'NONE', #84316, #55598 ) ;
#42933 = ADVANCED_FACE ( 'NONE', ( #11716 ), #44784, .T. ) ;
#42934 = DIRECTION ( 'NONE',  ( 0.000000000000000000, 0.000000000000000000, 1.000000000000000000 ) ) ;
#42935 = EDGE_CURVE ( 'NONE', #88995, #67882, #73905, .T. ) ;
#42936 = FACE_OUTER_BOUND ( 'NONE', #77189, .T. ) ;
#42937 = EDGE_CURVE ( 'NONE', #60387, #66434, #39409, .T. ) ;
#42938 = CARTESIAN_POINT ( 'NONE',  ( 145.9273723978340342, -137.0953762339121340, 247.3295516745586440 ) ) ;
#42940 = ORIENTED_EDGE ( 'NONE', *, *, #55826, .F. ) ;
#42939 = CARTESIAN_POINT ( 'NONE',  ( 115.6917119993852054, -30.73301325301421016, 279.3099109901964994 ) ) ;
#42941 = CARTESIAN_POINT ( 'NONE',  ( 85.58420390244806697, -58.72944715994107412, 231.5838068554169524 ) ) ;
#42942 = CARTESIAN_POINT ( 'NONE',  ( 111.4265353497823128, -47.77589283047310431, 172.8756252759109771 ) ) ;
#42943 = CARTESIAN_POINT ( 'NONE',  ( 107.6068523407233926, -48.56763185392661342, 38.61276813305397582 ) ) ;
#42944 = CARTESIAN_POINT ( 'NONE',  ( 103.2878376434171628, -26.96651641063459337, 211.3699109901969848 ) ) ;
#42945 = ADVANCED_FACE ( 'NONE', ( #88919 ), #4898, .T. ) ;
#42946 = CARTESIAN_POINT ( 'NONE',  ( 32.06670390244683233, -33.35206098992750157, 117.4678068554150485 ) ) ;
#42947 = DIRECTION ( 'NONE',  ( 0.000000000000000000, 1.000000000000000000, 0.000000000000000000 ) ) ;
#42948 = AXIS2_PLACEMENT_3D ( 'NONE', #31532, #80156, #25163 ) ;
#42950 = FACE_OUTER_BOUND ( 'NONE', #13609, .T. ) ;
#42949 = DIRECTION ( 'NONE',  ( 3.100000000000000258E-29, -3.100000000000000044E-14, -1.000000000000000000 ) ) ;
#42951 = CARTESIAN_POINT ( 'NONE',  ( 97.06107109463341942, -37.99641194202747130, 71.42729194085987388 ) ) ;
#42952 = LINE ( 'NONE', #84774, #45085 ) ;
#42953 = VERTEX_POINT ( 'NONE', #54351 ) ;
#42954 = DIRECTION ( 'NONE',  ( -4.299999999999999979E-14, 1.000000000000000000, -4.400000000000000367E-29 ) ) ;
#42955 = ORIENTED_EDGE ( 'NONE', *, *, #70758, .F. ) ;
#42956 = ORIENTED_EDGE ( 'NONE', *, *, #17708, .F. ) ;
#42958 = EDGE_LOOP ( 'NONE', ( #11446, #20638 ) ) ;
#42957 = CYLINDRICAL_SURFACE ( 'NONE', #51636, 9.999999999999998224 ) ;
#42959 = CARTESIAN_POINT ( 'NONE',  ( 105.9906760191434358, -26.38192068051327510, 46.15848241876796720 ) ) ;
#42960 = CARTESIAN_POINT ( 'NONE',  ( 75.31670390244798341, -57.40094715994099772, 88.43480685541499042 ) ) ;
#42961 = CARTESIAN_POINT ( 'NONE',  ( 245.4909999999999854, 40.03750000000000142, -67.11950000000000216 ) ) ;
#42962 = CARTESIAN_POINT ( 'NONE',  ( 117.8455077981468122, -34.08178244914028454, 160.0061014663869798 ) ) ;
#42963 = CARTESIAN_POINT ( 'NONE',  ( 98.99648076951073961, -33.93126856627920773, 285.4838483995053480 ) ) ;
#42964 = EDGE_LOOP ( 'NONE', ( #38776, #36566 ) ) ;
#42965 = ORIENTED_EDGE ( 'NONE', *, *, #71198, .F. ) ;
#42966 = ORIENTED_EDGE ( 'NONE', *, *, #46067, .T. ) ;
#42967 = ORIENTED_EDGE ( 'NONE', *, *, #49494, .F. ) ;
#42968 = CARTESIAN_POINT ( 'NONE',  ( 83.56670559755329464, -40.03837296219064967, 239.5838068554176914 ) ) ;
#42969 = PLANE ( 'NONE',  #55030 ) ;
#42970 = DIRECTION ( 'NONE',  ( 0.000000000000000000, -1.000000000000000000, 0.000000000000000000 ) ) ;
#42971 = CARTESIAN_POINT ( 'NONE',  ( 97.07207205724220955, -35.37844121140676634, 76.21895861022630925 ) ) ;
#42972 = CARTESIAN_POINT ( 'NONE',  ( 92.90667244829660376, 95.24968527363473925, 91.72735010416711532 ) ) ;
#42973 = DIRECTION ( 'NONE',  ( 0.7071067811739204512, -0.7071067811991745833, 0.000000000000000000 ) ) ;
#42974 = DIRECTION ( 'NONE',  ( 0.000000000000000000, 0.000000000000000000, -1.000000000000000000 ) ) ;
#42975 = CARTESIAN_POINT ( 'NONE',  ( -12.39034654063912555, 85.36816127604853932, 129.9671126930435037 ) ) ;
#42976 = CARTESIAN_POINT ( 'NONE',  ( 115.7453557663426409, -41.23947501269460503, 288.4441967044829767 ) ) ;
#42977 = CARTESIAN_POINT ( 'NONE',  ( -0.4144131305978647761, 69.85000000000000853, 118.5560000000000258 ) ) ;
#42978 = ORIENTED_EDGE ( 'NONE', *, *, #88178, .T. ) ;
#42979 = DIRECTION ( 'NONE',  ( 0.1858654558203329255, -0.9825752044157738396, 0.000000000000000000 ) ) ;
#42980 = LINE ( 'NONE', #8498, #6101 ) ;
#42981 = CARTESIAN_POINT ( 'NONE',  ( 98.94907028073869526, -37.58812756235333552, 124.2280903695919818 ) ) ;
#42982 = CIRCLE ( 'NONE', #51676, 5.599999999999994316 ) ;
#42984 = EDGE_CURVE ( 'NONE', #27190, #37008, #85475, .T. ) ;
#42983 = VECTOR ( 'NONE', #82467, 1000.000000000000000 ) ;
#42985 = AXIS2_PLACEMENT_3D ( 'NONE', #79552, #30050, #65889 ) ;
#42986 = ADVANCED_FACE ( 'NONE', ( #13062 ), #21677, .F. ) ;
#42987 = DIRECTION ( 'NONE',  ( 4.299999999999999979E-14, -1.000000000000000000, 4.400000000000000367E-29 ) ) ;
#42988 = FACE_OUTER_BOUND ( 'NONE', #24520, .T. ) ;
#42989 = VERTEX_POINT ( 'NONE', #63904 ) ;
#42990 = ORIENTED_EDGE ( 'NONE', *, *, #55580, .F. ) ;
#42991 = EDGE_CURVE ( 'NONE', #44647, #59006, #42531, .T. ) ;
#42992 = CARTESIAN_POINT ( 'NONE',  ( 113.1785701771607080, -44.75166289368706174, 138.0916005355700236 ) ) ;
#42993 = ORIENTED_EDGE ( 'NONE', *, *, #82007, .T. ) ;
#42994 = ORIENTED_EDGE ( 'NONE', *, *, #57242, .T. ) ;
#42995 = EDGE_CURVE ( 'NONE', #24712, #54590, #11526, .T. ) ;
#42996 = CARTESIAN_POINT ( 'NONE',  ( 108.1711956065674229, -46.05983505851052229, 159.1139642582779459 ) ) ;
#42997 = EDGE_CURVE ( 'NONE', #83770, #63582, #4263, .T. ) ;
#42998 = CARTESIAN_POINT ( 'NONE',  ( -7.661254700127833495, 82.54999999999999716, 317.6630000000000109 ) ) ;
#42999 = AXIS2_PLACEMENT_3D ( 'NONE', #73641, #87282, #31402 ) ;
#43000 = CARTESIAN_POINT ( 'NONE',  ( 97.20510023974232183, -31.68580462152881339, 91.96229194257693962 ) ) ;
#43001 = EDGE_CURVE ( 'NONE', #46234, #19810, #5706, .T. ) ;
#43002 = CARTESIAN_POINT ( 'NONE',  ( 57.56670390244832447, -48.82844715994039575, 254.7178068554150627 ) ) ;
#43003 = ORIENTED_EDGE ( 'NONE', *, *, #56232, .T. ) ;
#43004 = EDGE_CURVE ( 'NONE', #667, #35758, #21219, .T. ) ;
#43005 = ORIENTED_EDGE ( 'NONE', *, *, #48526, .T. ) ;
#43006 = ORIENTED_EDGE ( 'NONE', *, *, #17191, .T. ) ;
#43007 = EDGE_CURVE ( 'NONE', #22595, #57623, #14412, .T. ) ;
#43008 = CARTESIAN_POINT ( 'NONE',  ( 106.8407094991504209, -48.60307516909384873, 77.56133956162491927 ) ) ;
#43009 = ORIENTED_EDGE ( 'NONE', *, *, #25897, .F. ) ;
#43010 = CARTESIAN_POINT ( 'NONE',  ( 115.9511604156667772, -42.07746527209881293, 278.3832443235305618 ) ) ;
#43011 = CARTESIAN_POINT ( 'NONE',  ( 114.9943830143096335, -28.99422824087939432, 190.4537205140059655 ) ) ;
#43012 = EDGE_CURVE ( 'NONE', #30145, #24616, #47754, .T. ) ;
#43013 = DIRECTION ( 'NONE',  ( 0.000000000000000000, 1.000000000000000000, 0.000000000000000000 ) ) ;
#43014 = CARTESIAN_POINT ( 'NONE',  ( -103.1875000000000000, 127.0000000000000000, -7.143750000001079847 ) ) ;
#43015 = CARTESIAN_POINT ( 'NONE',  ( 103.2054172826541816, -46.45125265344608323, 113.2756252759109827 ) ) ;
#43016 = EDGE_CURVE ( 'NONE', #51337, #28246, #55258, .T. ) ;
#43017 = DIRECTION ( 'NONE',  ( 0.000000000000000000, -1.000000000000000000, 0.000000000000000000 ) ) ;
#43018 = ORIENTED_EDGE ( 'NONE', *, *, #23475, .T. ) ;
#43019 = CARTESIAN_POINT ( 'NONE',  ( 138.0667039024470171, -104.2784471599409244, 45.21780685541799727 ) ) ;
#43020 = ORIENTED_EDGE ( 'NONE', *, *, #40224, .F. ) ;
#43021 = CARTESIAN_POINT ( 'NONE',  ( 98.15086158280806217, -41.26138559404058981, 132.7011821357229451 ) ) ;
#43022 = ORIENTED_EDGE ( 'NONE', *, *, #72944, .F. ) ;
#43023 = ORIENTED_EDGE ( 'NONE', *, *, #13070, .T. ) ;
#43024 = DIRECTION ( 'NONE',  ( -1.000000000000000000, -1.000000000000000078E-15, 0.000000000000000000 ) ) ;
#43025 = DIRECTION ( 'NONE',  ( 0.000000000000000000, -1.000000000000000000, 0.000000000000000000 ) ) ;
#43026 = CARTESIAN_POINT ( 'NONE',  ( 100.5975332644244844, -28.50897509465477597, 15.60705384733995871 ) ) ;
#43027 = CARTESIAN_POINT ( 'NONE',  ( 163.2569089553700223, -33.54226604285010893, 342.9256252759119548 ) ) ;
#43028 = CARTESIAN_POINT ( 'NONE',  ( 71.24025061656124080, 8.642044024269713631, 394.9756252759102040 ) ) ;
#43029 = CARTESIAN_POINT ( 'NONE',  ( -24.20305689751608824, 53.97499999999997300, 58.62596543806478877 ) ) ;
#43030 = CARTESIAN_POINT ( 'NONE',  ( 98.38136461969642710, -29.78821554292430207, 45.78991099019597044 ) ) ;
#43032 = CARTESIAN_POINT ( 'NONE',  ( 100.8994224252809033, -45.87202276647009569, 148.0918157521009562 ) ) ;
#43031 = DIRECTION ( 'NONE',  ( -1.000000000000000078E-15, 0.000000000000000000, -1.000000000000000000 ) ) ;
#43033 = CARTESIAN_POINT ( 'NONE',  ( 99.09570907051013933, -30.55043176026986984, 71.80229194329096742 ) ) ;
#43034 = LINE ( 'NONE', #57116, #39422 ) ;
#43035 = ORIENTED_EDGE ( 'NONE', *, *, #67009, .T. ) ;
#43036 = CARTESIAN_POINT ( 'NONE',  ( 116.3212776292296127, -32.94146857471318413, 287.6356252759109680 ) ) ;
#43037 = EDGE_CURVE ( 'NONE', #5230, #1134, #84362, .T. ) ;
#43038 = CARTESIAN_POINT ( 'NONE',  ( -20.44586087093906812, 62.81651420408395126, 32.15007357241096031 ) ) ;
#43039 = DIRECTION ( 'NONE',  ( -0.1250000000000000278, -0.9921567416492215186, 3.079134169858830699E-14 ) ) ;
#43040 = EDGE_CURVE ( 'NONE', #24376, #68890, #42091, .T. ) ;
#43041 = EDGE_LOOP ( 'NONE', ( #68964, #2355, #49483, #33900, #86000, #44747, #12900, #11138, #29484 ) ) ;
#43042 = ADVANCED_FACE ( 'NONE', ( #14865 ), #41633, .F. ) ;
#43043 = CARTESIAN_POINT ( 'NONE',  ( 34.33598329127499227, -36.32844715994100682, 313.9678068554150059 ) ) ;
#43045 = EDGE_LOOP ( 'NONE', ( #18333, #67971, #27489, #88493 ) ) ;
#43044 = CARTESIAN_POINT ( 'NONE',  ( 117.5314631938956182, -40.43040369381473198, 178.5680062282919778 ) ) ;
#43046 = FACE_OUTER_BOUND ( 'NONE', #86237, .T. ) ;
#43047 = CARTESIAN_POINT ( 'NONE',  ( 101.3928372362931896, -45.54357991663450633, 218.1213395616249784 ) ) ;
#43048 = CARTESIAN_POINT ( 'NONE',  ( 97.50257212865312795, -32.47214954040395440, 96.99276813305395706 ) ) ;
#43049 = ADVANCED_FACE ( 'NONE', ( #20766 ), #57886, .T. ) ;
#43050 = CARTESIAN_POINT ( 'NONE',  ( 100.8594679592200976, 81.71102547120852932, 82.89895571708400723 ) ) ;
#43051 = CARTESIAN_POINT ( 'NONE',  ( 80.06648281188265059, -39.47944715903999224, 8.225259175037734849 ) ) ;
#43052 = DIRECTION ( 'NONE',  ( 0.000000000000000000, -1.000000000000000000, 0.000000000000000000 ) ) ;
#43053 = EDGE_LOOP ( 'NONE', ( #77072, #22632, #48015, #16653 ) ) ;
#43054 = AXIS2_PLACEMENT_3D ( 'NONE', #58797, #19712, #76471 ) ;
#43055 = VECTOR ( 'NONE', #39982, 1000.000000000000000 ) ;
#43056 = AXIS2_PLACEMENT_3D ( 'NONE', #7157, #13075, #27590 ) ;
#43057 = EDGE_LOOP ( 'NONE', ( #23356, #63779, #79698, #49971 ) ) ;
#43058 = ORIENTED_EDGE ( 'NONE', *, *, #50231, .F. ) ;
#43059 = ORIENTED_EDGE ( 'NONE', *, *, #44049, .T. ) ;
#43060 = CARTESIAN_POINT ( 'NONE',  ( 75.31670390244798341, -67.87844715994100397, 63.03480685541479289 ) ) ;
#43061 = CARTESIAN_POINT ( 'NONE',  ( 100.2482148738244661, -28.84314871041893014, 256.6441967044821695 ) ) ;
#43062 = CARTESIAN_POINT ( 'NONE',  ( 116.3212776292292716, -32.94146857471233147, 105.1356252759109680 ) ) ;
#43063 = CARTESIAN_POINT ( 'NONE',  ( 134.7196861477300445, -16.05633243510672159, 1.689562801604479692 ) ) ;
#43064 = VECTOR ( 'NONE', #32928, 1000.000000000000000 ) ;
#43066 = DIRECTION ( 'NONE',  ( -0.7071067811865496822, 0.7071067811865453523, 0.000000000000000000 ) ) ;
#43065 = LINE ( 'NONE', #62632, #23590 ) ;
#43067 = DIRECTION ( 'NONE',  ( 3.100000000000000258E-29, -3.100000000000000044E-14, -1.000000000000000000 ) ) ;
#43068 = AXIS2_PLACEMENT_3D ( 'NONE', #4610, #59993, #30969 ) ;
#43069 = CARTESIAN_POINT ( 'NONE',  ( 100.3969032678572262, -28.68811230323557027, 40.62705384733894221 ) ) ;
#43070 = ORIENTED_EDGE ( 'NONE', *, *, #30832, .T. ) ;
#43071 = VERTEX_POINT ( 'NONE', #15754 ) ;
#43072 = ORIENTED_EDGE ( 'NONE', *, *, #76042, .F. ) ;
#43073 = VECTOR ( 'NONE', #75227, 1000.000000000000000 ) ;
#43074 = LINE ( 'NONE', #9472, #29653 ) ;
#43075 = LINE ( 'NONE', #42181, #68023 ) ;
#43076 = CARTESIAN_POINT ( 'NONE',  ( 100.6033219294153724, -44.83909144599376617, 268.0289586092438867 ) ) ;
#43077 = LINE ( 'NONE', #9476, #70525 ) ;
#43078 = CARTESIAN_POINT ( 'NONE',  ( 98.49710108934571906, -31.94619897774425610, 106.9213395616249755 ) ) ;
#43079 = DIRECTION ( 'NONE',  ( -1.000000000000000000, -1.000000000000000078E-15, -1.000000000000000078E-15 ) ) ;
#43080 = LINE ( 'NONE', #58069, #22786 ) ;
#43081 = ORIENTED_EDGE ( 'NONE', *, *, #69897, .F. ) ;
#43082 = CARTESIAN_POINT ( 'NONE',  ( 91.91125933621934507, -107.5284471599419049, -21.78219314458190681 ) ) ;
#43083 = CARTESIAN_POINT ( 'NONE',  ( 97.31307424872157696, -38.96060643753106945, 57.50540973980124448 ) ) ;
#43084 = EDGE_LOOP ( 'NONE', ( #28323, #79803 ) ) ;
#43085 = EDGE_LOOP ( 'NONE', ( #59049, #56183, #84419, #2829 ) ) ;
#43086 = CARTESIAN_POINT ( 'NONE',  ( -90.66710916952438026, 90.29828471680512791, 76.38857008573013729 ) ) ;
#43087 = CARTESIAN_POINT ( 'NONE',  ( 115.2453386458995652, -37.16432389609550313, 16.60237608387699026 ) ) ;
#43088 = AXIS2_PLACEMENT_3D ( 'NONE', #80847, #74012, #65515 ) ;
#43089 = FACE_OUTER_BOUND ( 'NONE', #13002, .T. ) ;
#43090 = EDGE_CURVE ( 'NONE', #85960, #77712, #36716, .T. ) ;
#43091 = EDGE_CURVE ( 'NONE', #55699, #26649, #52454, .T. ) ;
#43092 = CARTESIAN_POINT ( 'NONE',  ( 116.3212776292269268, -32.94146857470660450, 84.13562527591095375 ) ) ;
#43093 = CARTESIAN_POINT ( 'NONE',  ( 88.90442867305986852, 72.22378176823140450, -78.43243611888054545 ) ) ;
#43094 = ORIENTED_EDGE ( 'NONE', *, *, #5310, .F. ) ;
#43095 = CARTESIAN_POINT ( 'NONE',  ( 90.44969454456408187, -53.34645651782490461, 239.5838068554174356 ) ) ;
#43096 = EDGE_CURVE ( 'NONE', #62096, #12394, #20457, .T. ) ;
#43097 = DIRECTION ( 'NONE',  ( 0.7071067811865671127, 0.7071067811865279218, 7.071067811865664660E-16 ) ) ;
#43098 = ORIENTED_EDGE ( 'NONE', *, *, #20808, .F. ) ;
#43099 = CARTESIAN_POINT ( 'NONE',  ( 117.3536837868190332, -38.62665896660388398, 88.68133956162493803 ) ) ;
#43100 = ORIENTED_EDGE ( 'NONE', *, *, #45759, .F. ) ;
#43101 = CARTESIAN_POINT ( 'NONE',  ( 111.1942201901869680, -30.05669425270436790, 287.4538046553057029 ) ) ;
#43102 = EDGE_CURVE ( 'NONE', #81215, #30264, #40644, .T. ) ;
#43103 = DIRECTION ( 'NONE',  ( 0.9242245927363033076, 0.3818493186865918321, 0.000000000000000000 ) ) ;
#43104 = CARTESIAN_POINT ( 'NONE',  ( 113.2764755850018048, -45.03455287549805774, 188.0994347997209672 ) ) ;
#43105 = CARTESIAN_POINT ( 'NONE',  ( 23.75871628398701318, 82.23350611626385387, 298.1325000000000500 ) ) ;
#43106 = CARTESIAN_POINT ( 'NONE',  ( 3.174999999999879918, 17.78000000000000114, -33.98325472291465132 ) ) ;
#43107 = FACE_BOUND ( 'NONE', #83608, .T. ) ;
#43108 = VECTOR ( 'NONE', #47143, 1000.000000000000000 ) ;
#43109 = FACE_OUTER_BOUND ( 'NONE', #20677, .T. ) ;
#43110 = CARTESIAN_POINT ( 'NONE',  ( 112.6870894866849966, -45.56130799126797370, 259.0270538473393458 ) ) ;
#43111 = CARTESIAN_POINT ( 'NONE',  ( 81.46927207886297140, 94.82191660594808980, -86.13037352894103549 ) ) ;
#43112 = EDGE_CURVE ( 'NONE', #16580, #49393, #25989, .T. ) ;
#43113 = ORIENTED_EDGE ( 'NONE', *, *, #20314, .T. ) ;
#43114 = FACE_OUTER_BOUND ( 'NONE', #70483, .T. ) ;
#43115 = AXIS2_PLACEMENT_3D ( 'NONE', #41821, #69558, #508 ) ;
#43116 = VERTEX_POINT ( 'NONE', #19315 ) ;
#43117 = CARTESIAN_POINT ( 'NONE',  ( 117.2805452986850412, -39.02698501918706597, 144.6499109901969859 ) ) ;
#43118 = VECTOR ( 'NONE', #48453, 1000.000000000000000 ) ;
#43119 = CARTESIAN_POINT ( 'NONE',  ( 125.2199481402020353, 50.10030656833554019, -36.94431110519001749 ) ) ;
#43120 = AXIS2_PLACEMENT_3D ( 'NONE', #32491, #18421, #38416 ) ;
#43121 = VERTEX_POINT ( 'NONE', #60178 ) ;
#43122 = VERTEX_POINT ( 'NONE', #61524 ) ;
#43123 = ORIENTED_EDGE ( 'NONE', *, *, #28135, .T. ) ;
#43124 = DIRECTION ( 'NONE',  ( -4.237773401492740281E-14, 1.000000000000000000, 0.000000000000000000 ) ) ;
#43125 = CARTESIAN_POINT ( 'NONE',  ( 102.0670659567350214, -27.97049192634999315, 266.4897909478353881 ) ) ;
#43126 = CARTESIAN_POINT ( 'NONE',  ( 20.03715912545818867, -46.82818131006190043, 313.9678068554150059 ) ) ;
#43127 = DIRECTION ( 'NONE',  ( 0.7071067811989784069, -0.7071067811741166276, 7.071067811989791923E-16 ) ) ;
#43128 = CARTESIAN_POINT ( 'NONE',  ( 57.91199999999999903, 101.5999999999999943, 178.6098374884404905 ) ) ;
#43129 = CARTESIAN_POINT ( 'NONE',  ( 111.4154404335798745, -46.20410067450679037, 23.91848241876792969 ) ) ;
#43130 = EDGE_CURVE ( 'NONE', #89527, #11288, #27026, .T. ) ;
#43131 = FACE_BOUND ( 'NONE', #41916, .T. ) ;
#43132 = VERTEX_POINT ( 'NONE', #4793 ) ;
#43133 = VECTOR ( 'NONE', #88967, 1000.000000000000000 ) ;
#43134 = CARTESIAN_POINT ( 'NONE',  ( 12.61749071809201439, 80.88423752776510867, 117.8827827373610688 ) ) ;
#43135 = AXIS2_PLACEMENT_3D ( 'NONE', #50925, #78670, #37757 ) ;
#43136 = VECTOR ( 'NONE', #15357, 1000.000000000000000 ) ;
#43137 = CARTESIAN_POINT ( 'NONE',  ( 180.2121375201600131, -29.73316016639650172, -5.074374724088000832 ) ) ;
#43138 = ORIENTED_EDGE ( 'NONE', *, *, #48916, .T. ) ;
#43140 = VERTEX_POINT ( 'NONE', #74283 ) ;
#43139 = EDGE_CURVE ( 'NONE', #81096, #85439, #17308, .T. ) ;
#43141 = VECTOR ( 'NONE', #77464, 1000.000000000000000 ) ;
#43142 = CARTESIAN_POINT ( 'NONE',  ( 81.30995888129837113, -21.18301917769388254, 1.868341932364300684 ) ) ;
#43143 = DIRECTION ( 'NONE',  ( 0.000000000000000000, 0.000000000000000000, 1.000000000000000000 ) ) ;
#43144 = FILL_AREA_STYLE_COLOUR ( '', #74751 ) ;
#43145 = PLANE ( 'NONE',  #52077 ) ;
#43146 = CARTESIAN_POINT ( 'NONE',  ( 0.000000000000000000, 111.1250000000000000, 0.000000000000000000 ) ) ;
#43147 = CARTESIAN_POINT ( 'NONE',  ( 101.8145705177301892, -43.46543587290290134, 231.4724198280769940 ) ) ;
#43148 = DIRECTION ( 'NONE',  ( 0.000000000000000000, 0.000000000000000000, -1.000000000000000000 ) ) ;
#43149 = CARTESIAN_POINT ( 'NONE',  ( 126.1219783984286238, 65.58371290633178319, 33.73612174402128971 ) ) ;
#43150 = CARTESIAN_POINT ( 'NONE',  ( 106.8402339230401452, -48.62808610490878891, 77.56133956162491927 ) ) ;
#43151 = VERTEX_POINT ( 'NONE', #47889 ) ;
#43152 = CARTESIAN_POINT ( 'NONE',  ( 41.56648329127499153, -36.32844715994070839, 203.6756252759119832 ) ) ;
#43153 = EDGE_LOOP ( 'NONE', ( #6790, #31029 ) ) ;
#43154 = LINE ( 'NONE', #72228, #36277 ) ;
#43155 = CYLINDRICAL_SURFACE ( 'NONE', #48412, 2.750000000000002665 ) ;
#43156 = ORIENTED_EDGE ( 'NONE', *, *, #10795, .F. ) ;
#43157 = DIRECTION ( 'NONE',  ( 1.000000000000000078E-15, -1.000000000000000000, 0.000000000000000000 ) ) ;
#43158 = VERTEX_POINT ( 'NONE', #4348 ) ;
#43159 = CARTESIAN_POINT ( 'NONE',  ( 25.56670390244832447, -48.82844715994168183, 257.2178068554150059 ) ) ;
#43160 = EDGE_CURVE ( 'NONE', #36969, #63446, #39742, .T. ) ;
#43161 = LINE ( 'NONE', #64081, #82449 ) ;
#43162 = AXIS2_PLACEMENT_3D ( 'NONE', #17166, #5318, #18039 ) ;
#43163 = CARTESIAN_POINT ( 'NONE',  ( 107.0664832912739399, -36.72944715994095333, 311.3356252759109566 ) ) ;
#43164 = ORIENTED_EDGE ( 'NONE', *, *, #2035, .F. ) ;
#43165 = CARTESIAN_POINT ( 'NONE',  ( 108.9893125699443175, -46.99828796752551341, 82.72419670448194040 ) ) ;
#43166 = SURFACE_STYLE_USAGE ( .BOTH. , #48181 ) ;
#43168 = CARTESIAN_POINT ( 'NONE',  ( 98.05713019660848317, 73.00415124681448731, -86.19613171056641932 ) ) ;
#43167 = CARTESIAN_POINT ( 'NONE',  ( 142.0664832912740110, -45.72944715994096754, -4.970821333495747396 ) ) ;
#43169 = CARTESIAN_POINT ( 'NONE',  ( 25.56670390244797275, -58.35344715994099829, 170.4678068554149775 ) ) ;
#43170 = CARTESIAN_POINT ( 'NONE',  ( -10.91394553148466606, 76.24004728773776662, 117.8518844485520987 ) ) ;
#43171 = EDGE_LOOP ( 'NONE', ( #78500, #69738, #39022, #28603 ) ) ;
#43172 = CARTESIAN_POINT ( 'NONE',  ( 194.0371591254575208, -24.89890238294407254, 180.4678068554150343 ) ) ;
#43173 = CARTESIAN_POINT ( 'NONE',  ( 109.7248659599222407, -27.00080519107385157, 154.8647919394014423 ) ) ;
#43174 = PLANE ( 'NONE',  #77735 ) ;
#43175 = EDGE_CURVE ( 'NONE', #62608, #25721, #26569, .T. ) ;
#43176 = CARTESIAN_POINT ( 'NONE',  ( 108.2792189108890568, -26.31750842948725122, 125.9841967044819597 ) ) ;
#43177 = AXIS2_PLACEMENT_3D ( 'NONE', #54073, #52275, #67276 ) ;
#43179 = DIRECTION ( 'NONE',  ( 1.000000000000000000, 4.163336342344333240E-14, 0.000000000000000000 ) ) ;
#43178 = CARTESIAN_POINT ( 'NONE',  ( 116.3149231129805941, -32.94053081170188335, 174.1356252759109680 ) ) ;
#43180 = PLANE ( 'NONE',  #23406 ) ;
#43181 = EDGE_CURVE ( 'NONE', #17890, #27372, #14399, .T. ) ;
#43182 = ORIENTED_EDGE ( 'NONE', *, *, #32220, .F. ) ;
#43183 = CIRCLE ( 'NONE', #24339, 3.250000000000002665 ) ;
#43184 = FACE_OUTER_BOUND ( 'NONE', #51790, .T. ) ;
#43185 = CARTESIAN_POINT ( 'NONE',  ( 102.0969121991173125, -45.15362633196975395, 158.1527681330539963 ) ) ;
#43187 = ORIENTED_EDGE ( 'NONE', *, *, #46724, .F. ) ;
#43186 = CARTESIAN_POINT ( 'NONE',  ( 67.06670390244704549, -104.4389890505713936, 245.7240874041480083 ) ) ;
#43188 = AXIS2_PLACEMENT_3D ( 'NONE', #57966, #8950, #37092 ) ;
#43189 = CARTESIAN_POINT ( 'NONE',  ( 110.3395589168170545, -45.98151452051992294, 33.84705384733993583 ) ) ;
#43190 = PLANE ( 'NONE',  #74472 ) ;
#43191 = DIRECTION ( 'NONE',  ( -1.000000000000000000, 0.000000000000000000, 0.000000000000000000 ) ) ;
#43192 = CYLINDRICAL_SURFACE ( 'NONE', #32751, 5.599999999999994316 ) ;
#43193 = DIRECTION ( 'NONE',  ( 1.000000000000000000, 4.163336342344333240E-14, 0.000000000000000000 ) ) ;
#43194 = FACE_BOUND ( 'NONE', #16382, .T. ) ;
#43195 = VECTOR ( 'NONE', #88486, 1000.000000000000000 ) ;
#43197 = CARTESIAN_POINT ( 'NONE',  ( 101.1405520526759574, -45.23956608920065037, 237.0803871806729717 ) ) ;
#43196 = VECTOR ( 'NONE', #59118, 1000.000000000000000 ) ;
#43198 = ORIENTED_EDGE ( 'NONE', *, *, #60133, .F. ) ;
#43199 = EDGE_LOOP ( 'NONE', ( #31204, #69347, #26040, #40254 ) ) ;
#43200 = CARTESIAN_POINT ( 'NONE',  ( 115.5299003720540014, -39.45574047089768754, 155.0101547344689550 ) ) ;
#43201 = AXIS2_PLACEMENT_3D ( 'NONE', #67111, #64111, #31242 ) ;
#43202 = DIRECTION ( 'NONE',  ( -1.000000000000000000, -4.163336342344333240E-14, 0.000000000000000000 ) ) ;
#43203 = CARTESIAN_POINT ( 'NONE',  ( 114.3823783366371316, -42.62471689273790076, 39.70634521065896649 ) ) ;
#43204 = CARTESIAN_POINT ( 'NONE',  ( 23.62137175363338315, 84.66824784807761262, 298.6181131755103024 ) ) ;
#43205 = EDGE_CURVE ( 'NONE', #59488, #45550, #32929, .T. ) ;
#43206 = ADVANCED_FACE ( 'NONE', ( #40186 ), #41086, .F. ) ;
#43207 = FACE_OUTER_BOUND ( 'NONE', #79763, .T. ) ;
#43208 = DIRECTION ( 'NONE',  ( 0.000000000000000000, 1.000000000000000000, 0.000000000000000000 ) ) ;
#43209 = CARTESIAN_POINT ( 'NONE',  ( 165.3359832912747436, -36.32844715993532958, 313.9678068554149490 ) ) ;
#43210 = EDGE_CURVE ( 'NONE', #4783, #74866, #63790, .T. ) ;
#43211 = DIRECTION ( 'NONE',  ( 0.000000000000000000, 0.000000000000000000, -1.000000000000000000 ) ) ;
#43212 = CARTESIAN_POINT ( 'NONE',  ( 99.39760893136102027, -29.69972230079146769, 275.7356252759109907 ) ) ;
#43213 = FACE_OUTER_BOUND ( 'NONE', #12289, .T. ) ;
#43214 = ORIENTED_EDGE ( 'NONE', *, *, #57465, .T. ) ;
#43215 = ORIENTED_EDGE ( 'NONE', *, *, #78860, .F. ) ;
#43216 = ADVANCED_FACE ( 'NONE', ( #76063 ), #62431, .F. ) ;
#43217 = LINE ( 'NONE', #27808, #56076 ) ;
#43218 = CARTESIAN_POINT ( 'NONE',  ( -78.17826422383528495, 92.64969027323469675, -89.13001032377188437 ) ) ;
#43219 = CARTESIAN_POINT ( 'NONE',  ( 62.03715912545739286, -47.82818131006020934, 180.4678068554151196 ) ) ;
#43220 = DIRECTION ( 'NONE',  ( -1.000000000000000078E-15, 1.000000000000000000, 0.000000000000000000 ) ) ;
#43221 = AXIS2_PLACEMENT_3D ( 'NONE', #15002, #72201, #23619 ) ;
#43222 = CARTESIAN_POINT ( 'NONE',  ( 99.63325261332707328, -43.08637385293071276, 27.88991099019594344 ) ) ;
#43223 = CARTESIAN_POINT ( 'NONE',  ( 128.0667039024480118, -50.82844715994100682, 265.9178068554150514 ) ) ;
#43224 = EDGE_CURVE ( 'NONE', #65312, #61695, #35163, .T. ) ;
#43225 = ORIENTED_EDGE ( 'NONE', *, *, #77867, .T. ) ;
#43226 = CARTESIAN_POINT ( 'NONE',  ( 1.451892259197136103E-14, 61.59999999999999432, -118.5560000000000116 ) ) ;
#43227 = DIRECTION ( 'NONE',  ( 1.000000000000000078E-15, -1.000000000000000083E-30, -1.000000000000000000 ) ) ;
#43228 = CARTESIAN_POINT ( 'NONE',  ( 104.8412335932644766, -26.50818645216173408, 260.2470538473397710 ) ) ;
#43229 = ORIENTED_EDGE ( 'NONE', *, *, #66917, .F. ) ;
#43230 = ADVANCED_FACE ( 'NONE', ( #7477 ), #23108, .F. ) ;
#43231 = CARTESIAN_POINT ( 'NONE',  ( 2.036081061455522238E-14, 184.0000000000000000, 80.02307622376218887 ) ) ;
#43232 = CARTESIAN_POINT ( 'NONE',  ( 0.000000000000000000, 61.59999999999999432, 0.000000000000000000 ) ) ;
#43233 = DIRECTION ( 'NONE',  ( 0.000000000000000000, 1.000000000000000000, 0.000000000000000000 ) ) ;
#43234 = CARTESIAN_POINT ( 'NONE',  ( 112.3828903148906306, -42.92343960232698663, 105.9595189410199652 ) ) ;
#43235 = CARTESIAN_POINT ( 'NONE',  ( 117.2133579748808927, -41.17085908628773439, 204.4861014663869696 ) ) ;
#43236 = DIRECTION ( 'NONE',  ( -0.08544974978095701279, -0.9963424814100680926, 0.000000000000000000 ) ) ;
#43237 = ORIENTED_EDGE ( 'NONE', *, *, #21768, .T. ) ;
#43238 = CARTESIAN_POINT ( 'NONE',  ( 27.27158787008327678, 127.0000000000000000, 101.0189074266571794 ) ) ;
#43239 = ORIENTED_EDGE ( 'NONE', *, *, #64096, .F. ) ;
#43240 = ORIENTED_EDGE ( 'NONE', *, *, #37285, .T. ) ;
#43241 = CIRCLE ( 'NONE', #12799, 2.117000000000007987 ) ;
#43242 = AXIS2_PLACEMENT_3D ( 'NONE', #84431, #390, #42158 ) ;
#43243 = CARTESIAN_POINT ( 'NONE',  ( 97.81168569434709070, -40.51740311210409828, 127.6359003399277441 ) ) ;
#43244 = VERTEX_POINT ( 'NONE', #650 ) ;
#43245 = VERTEX_POINT ( 'NONE', #70603 ) ;
#43246 = FACE_BOUND ( 'NONE', #47615, .T. ) ;
#43247 = CARTESIAN_POINT ( 'NONE',  ( 97.60785294300944770, -39.98231928252738498, 42.59004589039252409 ) ) ;
#43248 = CARTESIAN_POINT ( 'NONE',  ( 115.7032693465968975, -34.00573701374007385, 128.4800388756959819 ) ) ;
#43249 = CARTESIAN_POINT ( 'NONE',  ( 101.0739185617116078, -45.28721829360737416, 282.0899109901967563 ) ) ;
#43250 = CIRCLE ( 'NONE', #64995, 0.9999999999999800160 ) ;
#43251 = CARTESIAN_POINT ( 'NONE',  ( 51.42025729303989579, -33.70561438052008896, 117.4678068554150485 ) ) ;
#43252 = EDGE_LOOP ( 'NONE', ( #56258, #64818, #53662 ) ) ;
#43253 = VECTOR ( 'NONE', #24341, 1000.000000000000000 ) ;
#43254 = ORIENTED_EDGE ( 'NONE', *, *, #39427, .F. ) ;
#43255 = CYLINDRICAL_SURFACE ( 'NONE', #55079, 17.00000000000000000 ) ;
#43256 = AXIS2_PLACEMENT_3D ( 'NONE', #51695, #65778, #3125 ) ;
#43257 = CIRCLE ( 'NONE', #5555, 3.000000864267354572 ) ;
#43258 = LINE ( 'NONE', #70998, #89900 ) ;
#43259 = ADVANCED_FACE ( 'NONE', ( #77412 ), #15643, .F. ) ;
#43260 = CARTESIAN_POINT ( 'NONE',  ( 32.24491389930098251, -32.11662333284611748, 342.9256252759119548 ) ) ;
#43261 = CARTESIAN_POINT ( 'NONE',  ( 98.11178232766683038, -43.28888419983005775, 106.8175300378159704 ) ) ;
#43262 = CARTESIAN_POINT ( 'NONE',  ( 104.5776654613874683, -26.56013282928604724, 285.2670538473396391 ) ) ;
#43263 = ORIENTED_EDGE ( 'NONE', *, *, #82694, .T. ) ;
#43264 = PRODUCT_DEFINITION_CONTEXT ( 'detailed design', #86420, 'design' ) ;
#43265 = CARTESIAN_POINT ( 'NONE',  ( 99.38138666193238180, -29.68485204926252763, 275.7356252759109907 ) ) ;
#43266 = LINE ( 'NONE', #7419, #74672 ) ;
#43267 = DIRECTION ( 'NONE',  ( 0.000000000000000000, -1.000000000000000000, 0.000000000000000000 ) ) ;
#43268 = CARTESIAN_POINT ( 'NONE',  ( 97.93120746083486949, -40.79885511280051702, 27.66041246454429015 ) ) ;
#43270 = CARTESIAN_POINT ( 'NONE',  ( 20.03715912545639100, -24.42818131006202265, 180.4678068554150911 ) ) ;
#43269 = CYLINDRICAL_SURFACE ( 'NONE', #52038, 0.5000000000000079936 ) ;
#43271 = CYLINDRICAL_SURFACE ( 'NONE', #32163, 7.874000000000227928 ) ;
#43272 = DIRECTION ( 'NONE',  ( 0.000000000000000000, 0.000000000000000000, 1.000000000000000000 ) ) ;
#43273 = CARTESIAN_POINT ( 'NONE',  ( -74.15067561874319324, 120.6499999999999915, 68.53801554307369770 ) ) ;
#43274 = CIRCLE ( 'NONE', #30197, 7.937500000000000000 ) ;
#43275 = DIRECTION ( 'NONE',  ( 5.512527431108029424E-15, -1.000000000000000000, 0.000000000000000000 ) ) ;
#43276 = CARTESIAN_POINT ( 'NONE',  ( -27.27158787008326968, 184.0000000000000000, 0.000000000000000000 ) ) ;
#43277 = PLANE ( 'NONE',  #5743 ) ;
#43279 = ORIENTED_EDGE ( 'NONE', *, *, #5174, .T. ) ;
#43278 = DIRECTION ( 'NONE',  ( 0.000000000000000000, 1.000000000000000000, 0.000000000000000000 ) ) ;
#43280 = CARTESIAN_POINT ( 'NONE',  ( 116.4407914430480560, -130.2017202801087024, 250.2178068554180470 ) ) ;
#43281 = CARTESIAN_POINT ( 'NONE',  ( 108.0161133123553725, -24.89170165127225332, 265.0127681330534415 ) ) ;
#43282 = CARTESIAN_POINT ( 'NONE',  ( 109.4453082753925770, -25.93522777273083335, 175.8918157521009391 ) ) ;
#43283 = CARTESIAN_POINT ( 'NONE',  ( 98.40574028604457624, -42.07939390257583767, 7.768006228291934434 ) ) ;
#43284 = VECTOR ( 'NONE', #18655, 1000.000000000000000 ) ;
#43286 = CARTESIAN_POINT ( 'NONE',  ( 82.11134023506164681, -34.88977106732058076, 7.516154048600878212 ) ) ;
#43285 = CARTESIAN_POINT ( 'NONE',  ( 116.3212776292296127, -32.94146857471318413, 287.6356252759109680 ) ) ;
#43287 = DIRECTION ( 'NONE',  ( -0.9130365726098600421, 0.000000000000000000, -0.4078776986755215939 ) ) ;
#43288 = VECTOR ( 'NONE', #38837, 1000.000000000000000 ) ;
#43289 = EDGE_CURVE ( 'NONE', #56032, #2462, #27464, .T. ) ;
#43290 = ORIENTED_EDGE ( 'NONE', *, *, #84809, .F. ) ;
#43291 = CARTESIAN_POINT ( 'NONE',  ( 182.5667039024459939, -19.82844715994031048, -5.074374724088000832 ) ) ;
#43292 = EDGE_LOOP ( 'NONE', ( #29517, #62201, #35355, #73500 ) ) ;
#43293 = CARTESIAN_POINT ( 'NONE',  ( 114.9272539996656377, -40.07076659875138347, 167.9295626852199632 ) ) ;
#43295 = ORIENTED_EDGE ( 'NONE', *, *, #36808, .T. ) ;
#43294 = CARTESIAN_POINT ( 'NONE',  ( 134.0664832912740110, -46.42944715994100591, 10.42562527591099553 ) ) ;
#43296 = LINE ( 'NONE', #27443, #75094 ) ;
#43297 = CARTESIAN_POINT ( 'NONE',  ( 117.3921119255896599, -35.46056622170122807, 189.9241967044829664 ) ) ;
#43298 = DIRECTION ( 'NONE',  ( 0.000000000000000000, 0.000000000000000000, 1.000000000000000000 ) ) ;
#43299 = DIRECTION ( 'NONE',  ( 1.000000000000000000, 4.299999999999999979E-14, 1.000000000000000078E-15 ) ) ;
#43300 = CARTESIAN_POINT ( 'NONE',  ( 162.5667039024470171, -32.29483332968611364, -5.074374724088000832 ) ) ;
#43301 = CARTESIAN_POINT ( 'NONE',  ( 110.8691032742908078, -27.48061958891991807, 85.76620976841263655 ) ) ;
#43302 = CIRCLE ( 'NONE', #9936, 2.500000000000002220 ) ;
#43303 = CARTESIAN_POINT ( 'NONE',  ( 41.56648329127398966, -27.82844715994070484, 198.9256252759119832 ) ) ;
#43304 = CARTESIAN_POINT ( 'NONE',  ( 111.5934792397330568, -45.65282444717340127, 97.95005873871468793 ) ) ;
#43305 = CARTESIAN_POINT ( 'NONE',  ( 98.20106483660278229, -31.34956418181668880, 125.8803871806729546 ) ) ;
#43306 = ORIENTED_EDGE ( 'NONE', *, *, #45559, .F. ) ;
#43307 = ORIENTED_EDGE ( 'NONE', *, *, #4153, .F. ) ;
#43308 = CONICAL_SURFACE ( 'NONE', #24461, 3.299999999999999822, 0.7853981633974602694 ) ;
#43309 = CARTESIAN_POINT ( 'NONE',  ( 106.8749774919903359, -46.80089345537784595, 73.99301187732598351 ) ) ;
#43310 = AXIS2_PLACEMENT_3D ( 'NONE', #75527, #14191, #69608 ) ;
#43311 = CYLINDRICAL_SURFACE ( 'NONE', #26927, 0.2500000000000002220 ) ;
#43313 = CARTESIAN_POINT ( 'NONE',  ( 82.54999999999999716, 95.25000000000000000, 280.2255000000000109 ) ) ;
#43312 = CARTESIAN_POINT ( 'NONE',  ( 115.8019334949657804, -41.12891815432276843, 199.4556252759109611 ) ) ;
#43314 = CARTESIAN_POINT ( 'NONE',  ( 109.7256335582158897, -27.00101042015257136, 54.86366401989379682 ) ) ;
#43315 = CARTESIAN_POINT ( 'NONE',  ( 102.0670441177828849, -27.97050408116591314, 111.4901724250200630 ) ) ;
#43316 = EDGE_CURVE ( 'NONE', #29300, #16763, #22456, .T. ) ;
#43317 = DIRECTION ( 'NONE',  ( 1.000000000000000000, 5.440892098500631367E-15, -1.376676550535195643E-28 ) ) ;
#43318 = VECTOR ( 'NONE', #56283, 1000.000000000000114 ) ;
#43319 = DIRECTION ( 'NONE',  ( 0.000000000000000000, 0.000000000000000000, 1.000000000000000000 ) ) ;
#43320 = ADVANCED_FACE ( 'NONE', ( #69255 ), #75333, .T. ) ;
#43321 = CARTESIAN_POINT ( 'NONE',  ( 4.829302083966705794, 70.89057043354831933, 118.4594231900968850 ) ) ;
#43322 = CARTESIAN_POINT ( 'NONE',  ( 96.72090476913461998, -37.82382852467500811, 126.4099109901969626 ) ) ;
#43323 = ORIENTED_EDGE ( 'NONE', *, *, #3038, .T. ) ;
#43324 = EDGE_CURVE ( 'NONE', #74968, #50079, #86943, .T. ) ;
#43325 = VERTEX_POINT ( 'NONE', #55140 ) ;
#43326 = ORIENTED_EDGE ( 'NONE', *, *, #60537, .T. ) ;
#43327 = AXIS2_PLACEMENT_3D ( 'NONE', #36959, #64670, #72822 ) ;
#43328 = EDGE_CURVE ( 'NONE', #70137, #73627, #42868, .T. ) ;
#43329 = DIRECTION ( 'NONE',  ( 1.000000000000000000, 4.299999999999999979E-14, 1.000000000000000078E-15 ) ) ;
#43330 = CARTESIAN_POINT ( 'NONE',  ( 145.3984757889812442, -69.42761852215946305, 247.4725869789474473 ) ) ;
#43331 = CARTESIAN_POINT ( 'NONE',  ( 97.06386241311420804, -37.34254974993516640, 131.3752592778957080 ) ) ;
#43332 = CARTESIAN_POINT ( 'NONE',  ( 109.6426267301161346, -46.48019266381861314, 103.7814271469466263 ) ) ;
#43333 = CARTESIAN_POINT ( 'NONE',  ( 100.6713832604498577, -30.89818480590637861, 228.5442808457819979 ) ) ;
#43334 = DIRECTION ( 'NONE',  ( -1.000000000000000078E-15, 0.000000000000000000, 1.000000000000000000 ) ) ;
#43335 = CARTESIAN_POINT ( 'NONE',  ( 97.79409093757406879, -42.74665822538010929, 146.7965776568629508 ) ) ;
#43336 = FACE_OUTER_BOUND ( 'NONE', #41806, .T. ) ;
#43337 = ORIENTED_EDGE ( 'NONE', *, *, #28144, .F. ) ;
#43339 = ORIENTED_EDGE ( 'NONE', *, *, #34498, .T. ) ;
#43338 = ORIENTED_EDGE ( 'NONE', *, *, #26709, .F. ) ;
#43340 = EDGE_CURVE ( 'NONE', #50424, #89909, #34727, .T. ) ;
#43341 = LINE ( 'NONE', #36992, #69468 ) ;
#43342 = VERTEX_POINT ( 'NONE', #55587 ) ;
#43343 = ORIENTED_EDGE ( 'NONE', *, *, #89403, .F. ) ;
#43344 = DIRECTION ( 'NONE',  ( -0.9999999853157766072, -0.0001713722456143218888, 0.000000000000000000 ) ) ;
#43345 = CARTESIAN_POINT ( 'NONE',  ( 133.0080215814378732, -34.19118199975286387, 8.051357469095956176 ) ) ;
#43346 = CARTESIAN_POINT ( 'NONE',  ( 106.0694874169909809, -45.56507127853855366, 278.9187261630399917 ) ) ;
#43347 = CARTESIAN_POINT ( 'NONE',  ( 194.0667039024482392, -40.32844715993407192, 129.9678068554150343 ) ) ;
#43348 = ORIENTED_EDGE ( 'NONE', *, *, #21601, .F. ) ;
#43349 = CARTESIAN_POINT ( 'NONE',  ( 110.9723524473886158, -44.29053194721960551, 9.635625275910937759 ) ) ;
#43350 = AXIS2_PLACEMENT_3D ( 'NONE', #9255, #36950, #64658 ) ;
#43351 = DIRECTION ( 'NONE',  ( 4.299999999999999979E-14, -1.000000000000000000, 0.000000000000000000 ) ) ;
#43352 = ORIENTED_EDGE ( 'NONE', *, *, #54779, .T. ) ;
#43353 = VERTEX_POINT ( 'NONE', #83336 ) ;
#43354 = CARTESIAN_POINT ( 'NONE',  ( 115.0521663075109444, -42.80382784462421597, 113.3088412358543309 ) ) ;
#43355 = ORIENTED_EDGE ( 'NONE', *, *, #25093, .T. ) ;
#43356 = EDGE_LOOP ( 'NONE', ( #1005, #49904 ) ) ;
#43357 = CARTESIAN_POINT ( 'NONE',  ( 113.5315931691687439, -43.38514287343249265, 266.0080903695914003 ) ) ;
#43358 = CARTESIAN_POINT ( 'NONE',  ( 107.9200767535970584, -47.17740107552570805, 177.6413395616249886 ) ) ;
#43359 = CARTESIAN_POINT ( 'NONE',  ( 102.9221092647373865, -27.14930527916904168, 155.4013395616249795 ) ) ;
#43360 = FACE_OUTER_BOUND ( 'NONE', #80385, .T. ) ;
#43361 = DIRECTION ( 'NONE',  ( 0.7071067811864676367, 0.7071067811866273978, 7.071067811864981309E-16 ) ) ;
#43362 = CARTESIAN_POINT ( 'NONE',  ( 115.3879430501622636, -30.44965457351534255, 215.3413395616249773 ) ) ;
#43363 = DIRECTION ( 'NONE',  ( 0.000000000000000000, 1.000000000000000000, 0.000000000000000000 ) ) ;
#43364 = CARTESIAN_POINT ( 'NONE',  ( 25.56670390244719471, -42.82844715994178131, 170.7178068554150627 ) ) ;
#43365 = VERTEX_POINT ( 'NONE', #63333 ) ;
#43366 = DIRECTION ( 'NONE',  ( -0.000000000000000000, 1.000000000000000000, -0.000000000000000000 ) ) ;
#43367 = VERTEX_POINT ( 'NONE', #76514 ) ;
#43368 = AXIS2_PLACEMENT_3D ( 'NONE', #74123, #66854, #53189 ) ;
#43369 = ORIENTED_EDGE ( 'NONE', *, *, #82529, .T. ) ;
#43370 = EDGE_CURVE ( 'NONE', #42491, #67284, #28822, .T. ) ;
#43371 = AXIS2_PLACEMENT_3D ( 'NONE', #89497, #34960, #42218 ) ;
#43372 = CARTESIAN_POINT ( 'NONE',  ( 113.1812204092734220, -26.51970732500450012, 204.6470538473399756 ) ) ;
#43373 = EDGE_LOOP ( 'NONE', ( #13622, #40968, #13674, #44197 ) ) ;
#43374 = CARTESIAN_POINT ( 'NONE',  ( 117.8008629928215782, -34.09274860618955216, 164.0061014663869798 ) ) ;
#43375 = PLANE ( 'NONE',  #68913 ) ;
#43376 = ADVANCED_FACE ( 'NONE', ( #82902 ), #56504, .T. ) ;
#43377 = DIRECTION ( 'NONE',  ( 0.7071067811865533459, 0.000000000000000000, -0.7071067811865416886 ) ) ;
#43378 = DIRECTION ( 'NONE',  ( 1.000000000000000000, 0.000000000000000000, 0.000000000000000000 ) ) ;
#43381 = CARTESIAN_POINT ( 'NONE',  ( 112.6519946835718144, -45.50616226388157770, 259.0270538473393458 ) ) ;
#43380 = CARTESIAN_POINT ( 'NONE',  ( 183.5150000000000148, 14.63749999999999929, -14.28749999999999964 ) ) ;
#43379 = LINE ( 'NONE', #78390, #54891 ) ;
#43382 = LINE ( 'NONE', #21173, #36540 ) ;
#43383 = DIRECTION ( 'NONE',  ( 0.7071067811865470176, 2.262741699796953369E-14, 0.7071067811865480168 ) ) ;
#43384 = CYLINDRICAL_SURFACE ( 'NONE', #3493, 20.63750000000000284 ) ;
#43385 = CIRCLE ( 'NONE', #4231, 50.79999999999999716 ) ;
#43386 = CARTESIAN_POINT ( 'NONE',  ( 160.2664750769289697, 101.5999999999999943, 148.0533267522752112 ) ) ;
#43387 = VECTOR ( 'NONE', #29439, 1000.000000000000000 ) ;
#43388 = CARTESIAN_POINT ( 'NONE',  ( 98.34985889887454391, -31.65658483259429445, 256.9064586113552764 ) ) ;
#43389 = CYLINDRICAL_SURFACE ( 'NONE', #69475, 9.999999999999998224 ) ;
#43391 = ORIENTED_EDGE ( 'NONE', *, *, #18321, .F. ) ;
#43390 = CARTESIAN_POINT ( 'NONE',  ( 100.2183167550744685, -45.46532142855728864, 277.0594347997204068 ) ) ;
#43392 = CARTESIAN_POINT ( 'NONE',  ( 208.9149999999999920, 37.33800000000000097, 60.32499999999999574 ) ) ;
#43393 = CARTESIAN_POINT ( 'NONE',  ( 116.8272927809998123, -43.49410631979629471, 163.3441967044829823 ) ) ;
#43394 = CARTESIAN_POINT ( 'NONE',  ( 116.1236770753320542, -29.08733643602844054, 70.38419670448192278 ) ) ;
#43395 = CARTESIAN_POINT ( 'NONE',  ( 101.9632951345543148, -45.91070444983295573, 183.1727681330539781 ) ) ;
#43396 = CARTESIAN_POINT ( 'NONE',  ( 2.314288535156699577E-14, 127.0000000000000000, 188.9759999999999991 ) ) ;
#43397 = VECTOR ( 'NONE', #82863, 1000.000000000000000 ) ;
#43398 = DIRECTION ( 'NONE',  ( 0.000000000000000000, 0.000000000000000000, -1.000000000000000000 ) ) ;
#43400 = DIRECTION ( 'NONE',  ( -4.237773401492740281E-14, 1.000000000000000000, 0.000000000000000000 ) ) ;
#43399 = LINE ( 'NONE', #21189, #65166 ) ;
#43401 = CARTESIAN_POINT ( 'NONE',  ( 104.4899544625536976, -26.97880758202075668, 70.28145860838544934 ) ) ;
#43402 = CARTESIAN_POINT ( 'NONE',  ( -77.39114642429849766, 127.0000000000000000, -71.77848634863219957 ) ) ;
#43403 = EDGE_LOOP ( 'NONE', ( #45358, #49453, #46866, #34997 ) ) ;
#43404 = CARTESIAN_POINT ( 'NONE',  ( 144.0667039024470455, -124.7784471599409102, 55.21780685541800437 ) ) ;
#43405 = EDGE_CURVE ( 'NONE', #40009, #20465, #20662, .T. ) ;
#43406 = ORIENTED_EDGE ( 'NONE', *, *, #32428, .T. ) ;
#43407 = ORIENTED_EDGE ( 'NONE', *, *, #5307, .F. ) ;
#43409 = ORIENTED_EDGE ( 'NONE', *, *, #85672, .F. ) ;
#43408 = CARTESIAN_POINT ( 'NONE',  ( 186.6899999999999977, 46.38749999999999574, -50.79999999999999716 ) ) ;
#43410 = CARTESIAN_POINT ( 'NONE',  ( 98.66494773507974969, -43.87633619481167102, 72.89943479972099283 ) ) ;
#43411 = CARTESIAN_POINT ( 'NONE',  ( -72.96458098368600531, 117.4749999999999943, -78.00648098368779415 ) ) ;
#43412 = PLANE ( 'NONE',  #32558 ) ;
#43413 = EDGE_CURVE ( 'NONE', #35731, #11503, #62423, .T. ) ;
#43414 = DIRECTION ( 'NONE',  ( -0.9999999853157766072, -0.0001713722456133601202, 9.999999853157765648E-16 ) ) ;
#43415 = CARTESIAN_POINT ( 'NONE',  ( 98.43953089107090193, -39.48415132980177589, 280.9828960185531059 ) ) ;
#43416 = EDGE_LOOP ( 'NONE', ( #36103, #86823, #52136, #13562 ) ) ;
#43417 = AXIS2_PLACEMENT_3D ( 'NONE', #67454, #73827, #88816 ) ;
#43418 = VERTEX_POINT ( 'NONE', #83790 ) ;
#43419 = EDGE_LOOP ( 'NONE', ( #31795, #13420, #66340, #47321 ) ) ;
#43420 = CARTESIAN_POINT ( 'NONE',  ( 100.8874678886941894, -44.70022137831526265, 107.0522919429965754 ) ) ;
#43421 = CARTESIAN_POINT ( 'NONE',  ( 41.56648329127398966, -27.82844715994070484, 198.9256252759119832 ) ) ;
#43422 = DIRECTION ( 'NONE',  ( -0.2884130866282254013, 0.7071067811865455743, 0.6456143519637577155 ) ) ;
#43423 = CARTESIAN_POINT ( 'NONE',  ( 116.3212776292269837, -32.94146857470673240, 74.13562527591093954 ) ) ;
#43424 = CARTESIAN_POINT ( 'NONE',  ( 100.8069756963035530, 84.21449860606321636, 82.96293804092898938 ) ) ;
#43425 = CARTESIAN_POINT ( 'NONE',  ( 107.0664832912739399, -36.72944715994095333, 247.7440089327910755 ) ) ;
#43426 = CARTESIAN_POINT ( 'NONE',  ( 139.7494832912729805, -1.929447159941395817, 342.9256252759109316 ) ) ;
#43427 = CARTESIAN_POINT ( 'NONE',  ( -12.62695347127759327, 84.14402871178053545, 129.9443987845095876 ) ) ;
#43428 = CARTESIAN_POINT ( 'NONE',  ( 100.4929927897290014, -27.87207479535954135, 35.59657765686397113 ) ) ;
#43429 = EDGE_CURVE ( 'NONE', #22107, #2953, #73837, .T. ) ;
#43430 = ORIENTED_EDGE ( 'NONE', *, *, #19752, .F. ) ;
#43431 = AXIS2_PLACEMENT_3D ( 'NONE', #39811, #41158, #67533 ) ;
#43432 = CARTESIAN_POINT ( 'NONE',  ( 126.4481529151155996, 44.45000000000000284, 32.49205688096009936 ) ) ;
#43433 = CARTESIAN_POINT ( 'NONE',  ( 73.06670390244801183, -48.82844715994099971, 198.9178068554149945 ) ) ;
#43434 = CARTESIAN_POINT ( 'NONE',  ( 107.7548360709104855, -28.10233318731983232, 112.8433284648289430 ) ) ;
#43435 = CONICAL_SURFACE ( 'NONE', #81213, 3.299999999999999822, 0.7853981633974602694 ) ;
#43436 = VECTOR ( 'NONE', #43344, 1000.000000000000114 ) ;
#43437 = DIRECTION ( 'NONE',  ( 0.7071067811989676377, 0.7071067811741275078, 7.071067811989982236E-16 ) ) ;
#43438 = ADVANCED_BREP_SHAPE_REPRESENTATION ( '', ( #79963, #50656 ), #89914 ) ;
#43439 = CARTESIAN_POINT ( 'NONE',  ( 177.3246001664173264, -48.34074026909179622, 249.9678068554149775 ) ) ;
#43440 = ORIENTED_EDGE ( 'NONE', *, *, #60749, .T. ) ;
#43441 = EDGE_LOOP ( 'NONE', ( #62851, #84110, #79582, #76079 ) ) ;
#43442 = EDGE_CURVE ( 'NONE', #30970, #74824, #9713, .T. ) ;
#43443 = VECTOR ( 'NONE', #15748, 1000.000000000000000 ) ;
#43444 = LINE ( 'NONE', #29397, #32254 ) ;
#43445 = EDGE_LOOP ( 'NONE', ( #1219, #70017 ) ) ;
#43446 = VERTEX_POINT ( 'NONE', #24677 ) ;
#43447 = EDGE_CURVE ( 'NONE', #72639, #13914, #71947, .T. ) ;
#43448 = PRESENTATION_LAYER_ASSIGNMENT (  '', '', ( #50720 ) ) ;
#43449 = CARTESIAN_POINT ( 'NONE',  ( 101.8133294234851860, -44.51716929413077395, 148.5234880678019351 ) ) ;
#43450 = DIRECTION ( 'NONE',  ( -2.999999999999999839E-15, 1.000000000000000000, -2.999999999999999900E-30 ) ) ;
#43451 = AXIS2_PLACEMENT_3D ( 'NONE', #2266, #49036, #5725 ) ;
#43452 = CARTESIAN_POINT ( 'NONE',  ( 109.7757303681923418, -47.46933477669593771, 88.78514908543493789 ) ) ;
#43453 = CARTESIAN_POINT ( 'NONE',  ( 97.81944854975840542, -40.53634262228253959, 16.63725235658089119 ) ) ;
#43454 = ORIENTED_EDGE ( 'NONE', *, *, #30524, .T. ) ;
#43455 = AXIS2_PLACEMENT_3D ( 'NONE', #4660, #89131, #5108 ) ;
#43456 = ORIENTED_EDGE ( 'NONE', *, *, #36386, .F. ) ;
#43457 = ORIENTED_EDGE ( 'NONE', *, *, #41344, .T. ) ;
#43458 = CONICAL_SURFACE ( 'NONE', #46302, 1.571100913904471819, 1.047197551196592302 ) ;
#43459 = CARTESIAN_POINT ( 'NONE',  ( 112.7537747436706184, -27.22417719680832704, 54.65943479971996055 ) ) ;
#43460 = EDGE_LOOP ( 'NONE', ( #78702, #48415, #48439, #52953 ) ) ;
#43461 = CARTESIAN_POINT ( 'NONE',  ( 112.1705331031350994, -27.62378402076933526, 34.66991099019695355 ) ) ;
#43462 = CARTESIAN_POINT ( 'NONE',  ( 111.4263534857568771, -47.77543206737910708, 168.8756252759109486 ) ) ;
#43463 = CARTESIAN_POINT ( 'NONE',  ( 12.37524867428841091, 79.66590588004265783, -117.9083757119989428 ) ) ;
#43464 = CARTESIAN_POINT ( 'NONE',  ( -109.4095239551054419, 50.64688101357703687, 71.23662271831288706 ) ) ;
#43465 = CARTESIAN_POINT ( 'NONE',  ( 97.61704402414061121, -30.99515748980318719, 121.8803871806729546 ) ) ;
#43466 = CARTESIAN_POINT ( 'NONE',  ( 97.81171236172070849, -40.51746256574213589, 261.6350867226296941 ) ) ;
#43467 = ORIENTED_EDGE ( 'NONE', *, *, #77980, .F. ) ;
#43468 = LINE ( 'NONE', #58882, #20634 ) ;
#43469 = ORIENTED_EDGE ( 'NONE', *, *, #68047, .F. ) ;
#43470 = CARTESIAN_POINT ( 'NONE',  ( 0.000000000000000000, 2.031999999999865025, 0.000000000000000000 ) ) ;
#43471 = EDGE_LOOP ( 'NONE', ( #74365, #41247, #58917, #59374 ) ) ;
#43472 = ORIENTED_EDGE ( 'NONE', *, *, #16921, .F. ) ;
#43473 = CARTESIAN_POINT ( 'NONE',  ( 41.56648329127399677, -9.303447159940999356, 256.8086252759120498 ) ) ;
#43474 = CARTESIAN_POINT ( 'NONE',  ( 45.76696975232739817, -48.62818131006041256, 180.4678068554150911 ) ) ;
#43475 = CARTESIAN_POINT ( 'NONE',  ( 96.83338659586634378, -38.89961736000394410, 31.49276813305495892 ) ) ;
#43476 = LINE ( 'NONE', #84854, #28623 ) ;
#43477 = EDGE_CURVE ( 'NONE', #33479, #77555, #75400, .T. ) ;
#43478 = CARTESIAN_POINT ( 'NONE',  ( 263.3306968374159851, 52.73749999999999716, 10.66800000000000104 ) ) ;
#43479 = DIRECTION ( 'NONE',  ( 0.000000000000000000, 0.000000000000000000, -1.000000000000000000 ) ) ;
#43481 = B_SPLINE_CURVE_WITH_KNOTS ( 'NONE', 3,
 ( #45801, #73526, #32635, #66713, #87613, #4500, #25377, #53046, #80813, #60333, #55300, #54847, #63479, #76673, #28972, #55738, #21259, #14454, #48929, #77563, #62585, #56656, #84403, #41673, #83058, #63029, #48473, #83486, #82611 ),
 .UNSPECIFIED., .F., .F.,
 ( 4, 2, 2, 2, 2, 2, 2, 2, 2, 2, 1, 1, 1, 1, 1, 2, 4 ),
 ( 0.000000000000000000, 0.06250785763960332864, 0.1250157152792066573, 0.1875235729188099720, 0.2500314305584133145, 0.3125392881980166848, 0.3750471458376199441, 0.4375550034772233143, 0.4688089322970249717, 0.4844358967069258837, 0.4922493789118762009, 0.4961561200143512762, 0.4981094905655886751, 0.4990861758412074023, 0.4995745184790165716, 0.4998186897979214338, 0.5000628611168262960 ),
 .UNSPECIFIED. ) ;
#43480 = CARTESIAN_POINT ( 'NONE',  ( 118.0115280580378396, -34.77548253539073642, 48.96705384733996169 ) ) ;
#43483 = CARTESIAN_POINT ( 'NONE',  ( 97.97553865104319470, -30.48296430071277641, 161.8594347997199918 ) ) ;
#43482 = DIRECTION ( 'NONE',  ( -0.0001713722456127291687, 0.9999999853157766072, 1.713722456127291814E-19 ) ) ;
#43484 = CARTESIAN_POINT ( 'NONE',  ( 100.9546728049728443, -28.70702573201124252, 71.59395860986847993 ) ) ;
#43485 = DIRECTION ( 'NONE',  ( 0.1250000000000000278, 0.9921567416492215186, -3.079134169858830699E-14 ) ) ;
#43486 = VERTEX_POINT ( 'NONE', #36966 ) ;
#43487 = DIRECTION ( 'NONE',  ( -1.000000000000000078E-15, 1.000000000000000000, 0.000000000000000000 ) ) ;
#43488 = CIRCLE ( 'NONE', #21737, 2.030000000000003801 ) ;
#43489 = CARTESIAN_POINT ( 'NONE',  ( -10.76925785606963437, 68.90738082334692649, 36.55253304027624495 ) ) ;
#43490 = DIRECTION ( 'NONE',  ( -1.000000000000000000, 0.000000000000000000, -0.000000000000000000 ) ) ;
#43491 = ORIENTED_EDGE ( 'NONE', *, *, #64168, .F. ) ;
#43492 = VECTOR ( 'NONE', #57487, 1000.000000000000000 ) ;
#43493 = CARTESIAN_POINT ( 'NONE',  ( 182.5667039024477276, -33.35206098992057377, 237.4678068554150059 ) ) ;
#43495 = ORIENTED_EDGE ( 'NONE', *, *, #87704, .F. ) ;
#43494 = CARTESIAN_POINT ( 'NONE',  ( 97.63486134215516188, -41.27380337981261960, 171.6841967044819626 ) ) ;
#43496 = CARTESIAN_POINT ( 'NONE',  ( 173.9900000000000091, 37.33800000000000097, 69.13087104677069306 ) ) ;
#43497 = CARTESIAN_POINT ( 'NONE',  ( 112.4229354917722787, -46.42447813297522430, 248.9661014663869878 ) ) ;
#43498 = CARTESIAN_POINT ( 'NONE',  ( 98.26973918885833825, -28.71518450514261289, 76.73848241876795839 ) ) ;
#43499 = CARTESIAN_POINT ( 'NONE',  ( 116.3186249068867539, -32.94868901193379429, 250.1356252759109395 ) ) ;
#43500 = DIRECTION ( 'NONE',  ( 5.512527431108029424E-15, -1.000000000000000000, 0.000000000000000000 ) ) ;
#43501 = DIRECTION ( 'NONE',  ( 0.000000000000000000, 0.000000000000000000, 1.000000000000000000 ) ) ;
#43502 = ORIENTED_EDGE ( 'NONE', *, *, #24046, .F. ) ;
#43503 = VECTOR ( 'NONE', #49396, 1000.000000000000000 ) ;
#43504 = EDGE_CURVE ( 'NONE', #54166, #48373, #2904, .T. ) ;
#43505 = VERTEX_POINT ( 'NONE', #72393 ) ;
#43506 = VERTEX_POINT ( 'NONE', #31476 ) ;
#43508 = ADVANCED_FACE ( 'NONE', ( #31041 ), #40566, .F. ) ;
#43507 = VECTOR ( 'NONE', #78699, 1000.000000000000000 ) ;
#43509 = ORIENTED_EDGE ( 'NONE', *, *, #18983, .F. ) ;
#43510 = DIRECTION ( 'NONE',  ( 1.000000000000000078E-15, 0.000000000000000000, -1.000000000000000000 ) ) ;
#43511 = CARTESIAN_POINT ( 'NONE',  ( 96.77613930368880801, -40.76464245898888095, 242.6118157521009664 ) ) ;
#43512 = DIRECTION ( 'NONE',  ( 0.000000000000000000, 1.000000000000000000, 0.000000000000000000 ) ) ;
#43513 = CARTESIAN_POINT ( 'NONE',  ( 131.4961476553979765, -35.75123073100127158, 2.855912073278335406 ) ) ;
#43514 = ADVANCED_FACE ( 'NONE', ( #3348 ), #58731, .F. ) ;
#43515 = EDGE_CURVE ( 'NONE', #71741, #231, #29710, .T. ) ;
#43516 = CIRCLE ( 'NONE', #84213, 4.749999999999976907 ) ;
#43518 = CARTESIAN_POINT ( 'NONE',  ( 51.56670390244899238, -32.29483332968450782, -5.074374724088000832 ) ) ;
#43517 = DIRECTION ( 'NONE',  ( 0.000000000000000000, 1.000000000000000000, 0.000000000000000000 ) ) ;
#43519 = DIRECTION ( 'NONE',  ( 0.000000000000000000, 0.000000000000000000, -1.000000000000000000 ) ) ;
#43520 = B_SPLINE_CURVE_WITH_KNOTS ( 'NONE', 3,
 ( #70426, #14572, #22730, #22279, #78600, #77241, #15011, #16352, #49954, #50408, #7742, #8198, #44030, #77686, #49053, #35435, #15471, #71767, #42247, #64946, #69976, #37240, #63151, #43142, #70883, #30429, #8653, #36348, #64060, #1836 ),
 .UNSPECIFIED., .F., .F.,
 ( 4, 2, 2, 2, 1, 2, 2, 2, 2, 2, 2, 2, 1, 2, 2, 4 ),
 ( 0.5000000000000000000, 0.5624999999999789058, 0.5937499999999682476, 0.6093749999999633626, 0.6171874999999610312, 0.6210937499999602540, 0.6249999999999593658, 0.6874999999999669154, 0.7187499999999722444, 0.7499999999999774625, 0.8124999999999885647, 0.8437499999999955591, 0.8593750000000006661, 0.8671875000000031086, 0.8750000000000056621, 1.000000000000000000 ),
 .UNSPECIFIED. ) ;
#43521 = CARTESIAN_POINT ( 'NONE',  ( 97.33091451745008271, -32.84266655496112008, 41.02419670448193045 ) ) ;
#43522 = ORIENTED_EDGE ( 'NONE', *, *, #12894, .F. ) ;
#43523 = EDGE_CURVE ( 'NONE', #52647, #67095, #58302, .T. ) ;
#43524 = ORIENTED_EDGE ( 'NONE', *, *, #39714, .T. ) ;
#43525 = ORIENTED_EDGE ( 'NONE', *, *, #28775, .T. ) ;
#43526 = SURFACE_SIDE_STYLE ('',( #15407 ) ) ;
#43528 = EDGE_CURVE ( 'NONE', #66670, #53468, #64235, .T. ) ;
#43527 = CYLINDRICAL_SURFACE ( 'NONE', #2809, 218.1859999999999786 ) ;
#43529 = CARTESIAN_POINT ( 'NONE',  ( 100.5669465097398358, -44.03830869352244548, 262.9984824187674235 ) ) ;
#43530 = AXIS2_PLACEMENT_3D ( 'NONE', #41138, #48837, #68862 ) ;
#43531 = CARTESIAN_POINT ( 'NONE',  ( 164.9190312289439930, -35.91149509761220315, -5.074374724088000832 ) ) ;
#43532 = CARTESIAN_POINT ( 'NONE',  ( 116.7274023843878581, -38.25590632018514725, 109.7013395616249767 ) ) ;
#43533 = EDGE_CURVE ( 'NONE', #16628, #8809, #87008, .T. ) ;
#43534 = LINE ( 'NONE', #30815, #28599 ) ;
#43535 = ORIENTED_EDGE ( 'NONE', *, *, #78784, .T. ) ;
#43536 = PLANE ( 'NONE',  #77711 ) ;
#43537 = DIRECTION ( 'NONE',  ( -3.100000000000000258E-29, 3.100000000000000044E-14, 1.000000000000000000 ) ) ;
#43538 = VERTEX_POINT ( 'NONE', #24238 ) ;
#43539 = CIRCLE ( 'NONE', #4397, 0.4999999999999994449 ) ;
#43540 = CARTESIAN_POINT ( 'NONE',  ( -92.32962665258560264, 82.54999999999999716, 74.36911441044701121 ) ) ;
#43541 = CARTESIAN_POINT ( 'NONE',  ( 114.6306032519149198, -32.52409173292234357, 27.06047132197198124 ) ) ;
#43542 = FACE_OUTER_BOUND ( 'NONE', #26946, .T. ) ;
#43543 = DIRECTION ( 'NONE',  ( -6.938893903907222067E-15, -1.000000000000000000, 0.000000000000000000 ) ) ;
#43544 = DIRECTION ( 'NONE',  ( 0.000000000000000000, 0.000000000000000000, -1.000000000000000000 ) ) ;
#43545 = ORIENTED_EDGE ( 'NONE', *, *, #78329, .F. ) ;
#43546 = AXIS2_PLACEMENT_3D ( 'NONE', #57628, #50818, #30382 ) ;
#43547 = CARTESIAN_POINT ( 'NONE',  ( 19.56670390244796920, -48.82844715994099971, 20.91780685541479912 ) ) ;
#43548 = ADVANCED_FACE ( 'NONE', ( #16977 ), #64676, .F. ) ;
#43549 = CARTESIAN_POINT ( 'NONE',  ( 97.46299999999982333, 82.54999999999999716, 12.70000000000102069 ) ) ;
#43550 = EDGE_LOOP ( 'NONE', ( #14545, #55612, #38390, #9857 ) ) ;
#43551 = CARTESIAN_POINT ( 'NONE',  ( 117.5955728976552166, -42.16808282502534411, 93.44705384733897802 ) ) ;
#43552 = ORIENTED_EDGE ( 'NONE', *, *, #72373, .T. ) ;
#43553 = EDGE_CURVE ( 'NONE', #28735, #49139, #50587, .T. ) ;
#43554 = CARTESIAN_POINT ( 'NONE',  ( 97.39259002536323351, -35.90094442973985167, 35.68099125664797810 ) ) ;
#43555 = EDGE_CURVE ( 'NONE', #66470, #57667, #59180, .T. ) ;
#43556 = VECTOR ( 'NONE', #78742, 1000.000000000000000 ) ;
#43557 = CARTESIAN_POINT ( 'NONE',  ( 75.26949937496598864, -71.54137415153812185, 361.9756252759101471 ) ) ;
#43558 = CARTESIAN_POINT ( 'NONE',  ( 107.8656169629272483, -46.51081515578112402, 177.6413395616259834 ) ) ;
#43559 = CARTESIAN_POINT ( 'NONE',  ( -20.89537973703602347, 45.76944718839217074, 31.86023317849521419 ) ) ;
#43560 = DIRECTION ( 'NONE',  ( 1.000000000000000000, -2.914335439641033394E-13, 0.000000000000000000 ) ) ;
#43562 = EDGE_CURVE ( 'NONE', #42410, #60191, #8835, .T. ) ;
#43561 = DIRECTION ( 'NONE',  ( 0.000000000000000000, -1.000000000000000000, 0.000000000000000000 ) ) ;
#43563 = DIRECTION ( 'NONE',  ( 0.000000000000000000, 0.000000000000000000, -1.000000000000000000 ) ) ;
#43564 = CARTESIAN_POINT ( 'NONE',  ( 113.7840377202001036, -29.05235663984046823, 285.5032443235299979 ) ) ;
#43565 = VECTOR ( 'NONE', #74009, 999.9999999999998863 ) ;
#43566 = VERTEX_POINT ( 'NONE', #17421 ) ;
#43567 = DIRECTION ( 'NONE',  ( 0.7071067811865171526, 0.7071067811865779928, 7.071067811865164719E-16 ) ) ;
#43568 = ORIENTED_EDGE ( 'NONE', *, *, #70242, .F. ) ;
#43569 = CARTESIAN_POINT ( 'NONE',  ( 109.5186955991938191, -46.90685520642291806, 128.7641967044819751 ) ) ;
#43570 = CARTESIAN_POINT ( 'NONE',  ( 172.5667039024478413, -36.32844715993500273, 249.9678068554149775 ) ) ;
#43571 = ORIENTED_EDGE ( 'NONE', *, *, #56847, .F. ) ;
#43572 = ORIENTED_EDGE ( 'NONE', *, *, #82410, .F. ) ;
#43573 = ORIENTED_EDGE ( 'NONE', *, *, #39075, .F. ) ;
#43574 = AXIS2_PLACEMENT_3D ( 'NONE', #60900, #89520, #12311 ) ;
#43575 = CARTESIAN_POINT ( 'NONE',  ( 63.06670390244736524, -24.92844715994017690, 249.9678068554150343 ) ) ;
#43576 = DIRECTION ( 'NONE',  ( 3.999999999999999995E-14, -1.000000000000000000, 4.100000000000000342E-29 ) ) ;
#43577 = DIRECTION ( 'NONE',  ( 0.000000000000000000, -1.000000000000000000, 0.000000000000000000 ) ) ;
#43578 = CARTESIAN_POINT ( 'NONE',  ( 144.5373894638221657, -140.2077779303688203, 245.9389812651000113 ) ) ;
#43579 = LINE ( 'NONE', #44470, #17115 ) ;
#43580 = CARTESIAN_POINT ( 'NONE',  ( 118.5708186345730724, -33.89864261627929665, 10.01848241876795953 ) ) ;
#43581 = DIRECTION ( 'NONE',  ( 0.000000000000000000, 0.000000000000000000, -1.000000000000000000 ) ) ;
#43582 = VERTEX_POINT ( 'NONE', #3789 ) ;
#43583 = CARTESIAN_POINT ( 'NONE',  ( 163.0667039024476423, -33.35206098992141222, 313.9678068554149490 ) ) ;
#43584 = CIRCLE ( 'NONE', #39244, 30.99999999999998579 ) ;
#43585 = CARTESIAN_POINT ( 'NONE',  ( 46.32460016641727663, -48.34074026909785005, 249.9678068554150343 ) ) ;
#43586 = ORIENTED_EDGE ( 'NONE', *, *, #49533, .T. ) ;
#43587 = ORIENTED_EDGE ( 'NONE', *, *, #60447, .F. ) ;
#43588 = DIRECTION ( 'NONE',  ( 2.900000000000000265E-14, -2.000000000000000155E-15, 1.000000000000000000 ) ) ;
#43589 = DIRECTION ( 'NONE',  ( 1.000000000000000000, 0.000000000000000000, 0.000000000000000000 ) ) ;
#43590 = CARTESIAN_POINT ( 'NONE',  ( 83.06670390244804025, -42.21678055153920184, 207.5838068554169809 ) ) ;
#43591 = CARTESIAN_POINT ( 'NONE',  ( 139.7494832912729805, -71.52944715994142655, 361.9756252759109998 ) ) ;
#43592 = CARTESIAN_POINT ( 'NONE',  ( 172.5664832912740110, -18.82844715994099971, 258.9256252759120116 ) ) ;
#43593 = AXIS2_PLACEMENT_3D ( 'NONE', #71302, #42655, #36770 ) ;
#43594 = CARTESIAN_POINT ( 'NONE',  ( 111.9487353400944158, -44.35678517904902662, 217.4400388756959615 ) ) ;
#43596 = CARTESIAN_POINT ( 'NONE',  ( 96.21590750669005843, -38.71157422997261932, 47.48229194257797303 ) ) ;
#43595 = DIRECTION ( 'NONE',  ( -1.000000000000000000, -3.999999999999999995E-14, -1.000000000000000078E-15 ) ) ;
#43597 = CARTESIAN_POINT ( 'NONE',  ( 124.3932715389403256, 71.33461644843129079, 39.63843969546147861 ) ) ;
#43598 = CARTESIAN_POINT ( 'NONE',  ( 113.3690198962888758, -27.59211078819982887, 89.60800622829195561 ) ) ;
#43599 = ORIENTED_EDGE ( 'NONE', *, *, #7325, .T. ) ;
#43600 = FACE_OUTER_BOUND ( 'NONE', #24044, .T. ) ;
#43601 = ORIENTED_EDGE ( 'NONE', *, *, #58787, .F. ) ;
#43602 = AXIS2_PLACEMENT_3D ( 'NONE', #46062, #86994, #37500 ) ;
#43603 = CARTESIAN_POINT ( 'NONE',  ( 107.0664832912739968, -36.72944715994100306, 287.6356252759109680 ) ) ;
#43604 = CARTESIAN_POINT ( 'NONE',  ( 97.06141937736202863, -37.99914660572866154, 277.4274653756244220 ) ) ;
#43605 = ORIENTED_EDGE ( 'NONE', *, *, #74093, .F. ) ;
#43606 = LINE ( 'NONE', #56790, #67916 ) ;
#43607 = VERTEX_POINT ( 'NONE', #10159 ) ;
#43608 = DIRECTION ( 'NONE',  ( -9.351236661543306751E-17, 3.725950533538267165E-29, 1.000000000000000000 ) ) ;
#43609 = CARTESIAN_POINT ( 'NONE',  ( -487.2989999999999782, 10.16305401447644030, 97.63125000000000853 ) ) ;
#43610 = VECTOR ( 'NONE', #37651, 1000.000000000000000 ) ;
#43611 = DIRECTION ( 'NONE',  ( 0.000000000000000000, 0.000000000000000000, -1.000000000000000000 ) ) ;
#43612 = VERTEX_POINT ( 'NONE', #37868 ) ;
#43613 = CARTESIAN_POINT ( 'NONE',  ( 96.01222827763220380, -41.06966167057572648, 96.62419670448197451 ) ) ;
#43614 = CARTESIAN_POINT ( 'NONE',  ( 181.5667039024459939, -22.48495420874030515, 342.9256252759119548 ) ) ;
#43615 = LINE ( 'NONE', #8681, #33613 ) ;
#43616 = ADVANCED_FACE ( 'NONE', ( #65566 ), #72828, .T. ) ;
#43617 = CARTESIAN_POINT ( 'NONE',  ( -12.27414673741744089, 79.67290841380474831, 117.7178608090033265 ) ) ;
#43618 = ORIENTED_EDGE ( 'NONE', *, *, #89197, .T. ) ;
#43619 = B_SPLINE_CURVE_WITH_KNOTS ( 'NONE', 3,
 ( #28615, #35874, #1370, #83595, #15895, #42232, #70867, #77226, #34974, #85403, #84508, #22715, #21821, #29521, #69512, #50847, #14998, #22266 ),
 .UNSPECIFIED., .F., .F.,
 ( 4, 2, 2, 2, 2, 2, 2, 2, 4 ),
 ( 0.4999999970439366614, 0.5624999974134445857, 0.6249999977829525655, 0.6874999981524604342, 0.7499999985219683030, 0.8124999988914762827, 0.8749999992609842625, 0.9374999996304921313, 1.000000000000000000 ),
 .UNSPECIFIED. ) ;
#43620 = EDGE_CURVE ( 'NONE', #57999, #4381, #60982, .T. ) ;
#43621 = LINE ( 'NONE', #83643, #61989 ) ;
#43622 = DIRECTION ( 'NONE',  ( 0.000000000000000000, 1.000000000000000000, 0.000000000000000000 ) ) ;
#43623 = VECTOR ( 'NONE', #48781, 1000.000000000000000 ) ;
#43624 = CARTESIAN_POINT ( 'NONE',  ( 143.0664832912740110, -18.82844715994099971, -5.074374724088000832 ) ) ;
#43625 = VECTOR ( 'NONE', #55451, 1000.000000000000000 ) ;
#43626 = ADVANCED_FACE ( 'NONE', ( #66899 ), #87798, .F. ) ;
#43627 = AXIS2_PLACEMENT_3D ( 'NONE', #28014, #76627, #21675 ) ;
#43628 = EDGE_CURVE ( 'NONE', #25323, #28403, #38743, .T. ) ;
#43630 = DIRECTION ( 'NONE',  ( -0.000000000000000000, 1.000000000000000000, 0.000000000000000000 ) ) ;
#43629 = DIRECTION ( 'NONE',  ( 0.0001211784769727619030, -0.7071067708032375831, -0.7071067811865434649 ) ) ;
#43631 = DIRECTION ( 'NONE',  ( -0.7071067811734105257, 0.7071067811996846197, 0.000000000000000000 ) ) ;
#43632 = VECTOR ( 'NONE', #25862, 1000.000000000000000 ) ;
#43633 = EDGE_CURVE ( 'NONE', #13081, #32398, #81007, .T. ) ;
#43634 = EDGE_LOOP ( 'NONE', ( #16686, #24942, #61528, #63419 ) ) ;
#43636 = EDGE_CURVE ( 'NONE', #36627, #27899, #32824, .T. ) ;
#43635 = DIRECTION ( 'NONE',  ( -0.000000000000000000, -0.000000000000000000, -1.000000000000000000 ) ) ;
#43637 = CARTESIAN_POINT ( 'NONE',  ( 102.2986265273211615, -45.30740241592380357, 183.1727681330529833 ) ) ;
#43638 = CIRCLE ( 'NONE', #21946, 0.9999999999999800160 ) ;
#43640 = ORIENTED_EDGE ( 'NONE', *, *, #79294, .F. ) ;
#43639 = DIRECTION ( 'NONE',  ( 1.000000000000000000, 0.000000000000000000, 0.000000000000000000 ) ) ;
#43641 = CARTESIAN_POINT ( 'NONE',  ( 102.3890460933095454, -47.58756240099337731, 283.2527681330539053 ) ) ;
#43642 = CYLINDRICAL_SURFACE ( 'NONE', #41064, 0.5000000000000104361 ) ;
#43643 = LINE ( 'NONE', #29579, #88170 ) ;
#43644 = DIRECTION ( 'NONE',  ( 0.7071067811866279529, -0.7071067811864671926, 7.071067811866286874E-16 ) ) ;
#43645 = CARTESIAN_POINT ( 'NONE',  ( 101.9927642735531919, -45.44554305791272242, 12.15655162758104701 ) ) ;
#43646 = AXIS2_PLACEMENT_3D ( 'NONE', #38909, #10757, #66166 ) ;
#43647 = EDGE_CURVE ( 'NONE', #5214, #65668, #50750, .T. ) ;
#43648 = CARTESIAN_POINT ( 'NONE',  ( 97.06104264810085169, -37.99626338996256436, 31.42750358927145271 ) ) ;
#43649 = CARTESIAN_POINT ( 'NONE',  ( 110.8764511561472546, -27.72125199330407241, 244.7584824187689492 ) ) ;
#43650 = EDGE_LOOP ( 'NONE', ( #13889, #30304, #24869, #42437 ) ) ;
#43651 = ORIENTED_EDGE ( 'NONE', *, *, #8569, .F. ) ;
#43652 = ADVANCED_FACE ( 'NONE', ( #46437 ), #88708, .F. ) ;
#43653 = CARTESIAN_POINT ( 'NONE',  ( 109.6768956016245227, -27.70380185851407973, 211.2720594963729752 ) ) ;
#43654 = CARTESIAN_POINT ( 'NONE',  ( 115.7848594079097211, -41.79936060917356144, 54.40633938901413558 ) ) ;
#43655 = CARTESIAN_POINT ( 'NONE',  ( 100.4594818976507753, -42.68004899263244312, 53.34158330589694685 ) ) ;
#43656 = CARTESIAN_POINT ( 'NONE',  ( -89.95770503246842509, 94.82199753261677699, 94.61838531165750510 ) ) ;
#43657 = B_SPLINE_CURVE_WITH_KNOTS ( 'NONE', 3,
 ( #79321, #50694, #71609, #2114, #3889, #31139, #17080, #16635, #30268, #44768, #52008, #10692, #23467, #37079, #65661, #51136, #58837, #16197 ),
 .UNSPECIFIED., .F., .F.,
 ( 4, 2, 2, 2, 2, 2, 2, 2, 4 ),
 ( 0.5000000001806115257, 0.5625000001580351405, 0.6250000001354586443, 0.6875000001128821481, 0.7500000000903057629, 0.8125000000677293777, 0.8750000000451528814, 0.9375000000225763852, 1.000000000000000000 ),
 .UNSPECIFIED. ) ;
#43658 = VECTOR ( 'NONE', #83260, 1000.000000000000000 ) ;
#43659 = DIRECTION ( 'NONE',  ( 0.0001713722456134502174, -0.9999999853157766072, 0.000000000000000000 ) ) ;
#43660 = CYLINDRICAL_SURFACE ( 'NONE', #76338, 3.250000000000002665 ) ;
#43662 = EDGE_LOOP ( 'NONE', ( #16925, #15682 ) ) ;
#43661 = VECTOR ( 'NONE', #64986, 1000.000000000000000 ) ;
#43663 = CARTESIAN_POINT ( 'NONE',  ( 37.03715912545347777, -48.62818131006128652, 129.9678068554150911 ) ) ;
#43664 = CARTESIAN_POINT ( 'NONE',  ( 97.80786240601167947, -40.50806667358143898, 37.63452979473162685 ) ) ;
#43665 = CARTESIAN_POINT ( 'NONE',  ( 110.8089421659425824, -26.35361831834155311, 249.7889586092445882 ) ) ;
#43666 = CARTESIAN_POINT ( 'NONE',  ( 3.273557253446674142, 94.74519041223615545, 118.3134806149962088 ) ) ;
#43667 = VERTEX_POINT ( 'NONE', #74169 ) ;
#43668 = ORIENTED_EDGE ( 'NONE', *, *, #69173, .F. ) ;
#43669 = EDGE_CURVE ( 'NONE', #71713, #77555, #5585, .T. ) ;
#43670 = CARTESIAN_POINT ( 'NONE',  ( 112.0659116168554164, -45.48839626386907042, 82.98979194206674492 ) ) ;
#43671 = CYLINDRICAL_SURFACE ( 'NONE', #15732, 10.00000000000000711 ) ;
#43672 = FACE_OUTER_BOUND ( 'NONE', #67074, .T. ) ;
#43674 = EDGE_CURVE ( 'NONE', #66320, #87303, #52780, .T. ) ;
#43673 = CARTESIAN_POINT ( 'NONE',  ( 90.52001865076087483, -69.32858309805097008, 247.6470817344352895 ) ) ;
#43675 = AXIS2_PLACEMENT_3D ( 'NONE', #86418, #46384, #73204 ) ;
#43676 = CARTESIAN_POINT ( 'NONE',  ( 115.0479362680065663, -42.38275094372907859, 49.33562527591095659 ) ) ;
#43677 = CARTESIAN_POINT ( 'NONE',  ( 10.70529764341858048, 75.89205320364979457, 117.8710853958748430 ) ) ;
#43678 = ORIENTED_EDGE ( 'NONE', *, *, #77090, .T. ) ;
#43679 = VECTOR ( 'NONE', #43233, 1000.000000000000000 ) ;
#43680 = CARTESIAN_POINT ( 'NONE',  ( 114.1199461662357919, -46.31379764262941023, 29.08133956162595268 ) ) ;
#43681 = LINE ( 'NONE', #36443, #72920 ) ;
#43682 = CARTESIAN_POINT ( 'NONE',  ( 105.3166869522846838, -26.42980843014500181, 15.20991099019697401 ) ) ;
#43683 = ORIENTED_EDGE ( 'NONE', *, *, #18573, .T. ) ;
#43684 = CARTESIAN_POINT ( 'NONE',  ( -12.70000000000000107, 82.54999999999999716, 92.46299999999996544 ) ) ;
#43685 = CARTESIAN_POINT ( 'NONE',  ( 99.50485981225885723, -43.30594324741348089, 17.89604700636049017 ) ) ;
#43686 = CARTESIAN_POINT ( 'NONE',  ( 74.06670390244704549, -118.2784471599409812, 45.21780685541799727 ) ) ;
#43687 = CARTESIAN_POINT ( 'NONE',  ( 104.1662843248667230, -44.88357317080683373, 100.1347570362589892 ) ) ;
#43688 = CARTESIAN_POINT ( 'NONE',  ( 117.9552932246042332, -34.69990928640298478, 199.9851490854349549 ) ) ;
#43689 = CIRCLE ( 'NONE', #23434, 4.750000000000004441 ) ;
#43690 = DIRECTION ( 'NONE',  ( -3.999999999999999995E-14, 1.000000000000000000, -4.100000000000000342E-29 ) ) ;
#43691 = VERTEX_POINT ( 'NONE', #88263 ) ;
#43692 = DIRECTION ( 'NONE',  ( 0.000000000000000000, 0.000000000000000000, 1.000000000000000000 ) ) ;
#43693 = VERTEX_POINT ( 'NONE', #54584 ) ;
#43695 = VERTEX_POINT ( 'NONE', #26023 ) ;
#43694 = CIRCLE ( 'NONE', #59632, 2.750000000000002665 ) ;
#43696 = EDGE_CURVE ( 'NONE', #68029, #22204, #53689, .T. ) ;
#43697 = DIRECTION ( 'NONE',  ( 0.9068632946707807507, -0.4214249218767881500, 9.068605531941956314E-16 ) ) ;
#43698 = ORIENTED_EDGE ( 'NONE', *, *, #23157, .T. ) ;
#43699 = VERTEX_POINT ( 'NONE', #60066 ) ;
#43700 = LINE ( 'NONE', #49613, #29516 ) ;
#43701 = CARTESIAN_POINT ( 'NONE',  ( 97.70650073344890529, -40.25115704673319073, 42.61283759994312703 ) ) ;
#43702 = CARTESIAN_POINT ( 'NONE',  ( 103.8778598771455677, -28.80550795996352420, 129.8038483995049432 ) ) ;
#43703 = AXIS2_PLACEMENT_3D ( 'NONE', #54524, #26404, #75461 ) ;
#43704 = CARTESIAN_POINT ( 'NONE',  ( 115.9256476412969192, -30.08033833575881033, 264.3508633711492735 ) ) ;
#43705 = CARTESIAN_POINT ( 'NONE',  ( -48.02966122971776741, 65.60000000000000853, 75.53254848357481421 ) ) ;
#43706 = AXIS2_PLACEMENT_3D ( 'NONE', #68426, #75688, #5755 ) ;
#43707 = EDGE_LOOP ( 'NONE', ( #64004, #7570, #81836, #73022 ) ) ;
#43708 = VERTEX_POINT ( 'NONE', #46879 ) ;
#43709 = CARTESIAN_POINT ( 'NONE',  ( 107.0667039024470313, -104.2784471599414502, 0.2178068554180012661 ) ) ;
#43710 = CARTESIAN_POINT ( 'NONE',  ( 53.35959712126277310, -48.62134037875357251, 300.4678068554150059 ) ) ;
#43711 = CARTESIAN_POINT ( 'NONE',  ( 70.75848861320156402, -139.2980388182697311, 247.4388078084867573 ) ) ;
#43712 = EDGE_CURVE ( 'NONE', #65595, #85915, #67798, .T. ) ;
#43713 = CARTESIAN_POINT ( 'NONE',  ( 112.8260979389708183, -47.14365076028245483, 102.9784824187679817 ) ) ;
#43714 = CARTESIAN_POINT ( 'NONE',  ( 116.6223143332234997, -42.37736834728454483, 283.4137205140060018 ) ) ;
#43715 = ORIENTED_EDGE ( 'NONE', *, *, #13239, .T. ) ;
#43716 = CARTESIAN_POINT ( 'NONE',  ( 115.7763152052227156, -31.00006163510664337, 254.2899109901966028 ) ) ;
#43717 = CARTESIAN_POINT ( 'NONE',  ( 97.81168731305311326, -40.51740136754563082, 36.63591984386916067 ) ) ;
#43718 = CARTESIAN_POINT ( 'NONE',  ( 11.13113089042260384, 76.43192475021864141, 130.0807045952973908 ) ) ;
#43719 = CARTESIAN_POINT ( 'NONE',  ( 101.1247409750737631, -44.88967807114817532, 28.07730664055660696 ) ) ;
#43720 = ADVANCED_FACE ( 'NONE', ( #80546 ), #33279, .F. ) ;
#43722 = CARTESIAN_POINT ( 'NONE',  ( 69.09827022149127629, -138.9035152955028707, 247.0712714749913061 ) ) ;
#43721 = DIRECTION ( 'NONE',  ( 2.900000000000000265E-14, -2.000000000000000155E-15, 1.000000000000000000 ) ) ;
#43723 = DIRECTION ( 'NONE',  ( -1.000000000000000000, 0.000000000000000000, 0.000000000000000000 ) ) ;
#43724 = EDGE_CURVE ( 'NONE', #75492, #9288, #37664, .T. ) ;
#43725 = DIRECTION ( 'NONE',  ( 1.000000000000000078E-15, -1.000000000000000083E-30, -1.000000000000000000 ) ) ;
#43726 = AXIS2_PLACEMENT_3D ( 'NONE', #70229, #64320, #8003 ) ;
#43727 = EDGE_CURVE ( 'NONE', #30159, #82436, #81193, .T. ) ;
#43728 = CARTESIAN_POINT ( 'NONE',  ( -6.359443759653452766, 93.55095829381066608, 130.4015408541779379 ) ) ;
#43729 = DIRECTION ( 'NONE',  ( 1.000000000000000000, 0.000000000000000000, 0.000000000000000000 ) ) ;
#43730 = CARTESIAN_POINT ( 'NONE',  ( 101.9937722986115176, -45.44616494378649918, 162.1562847702247154 ) ) ;
#43731 = CARTESIAN_POINT ( 'NONE',  ( -254.0000000000000000, 104.7749999999999915, -41.27499999999999858 ) ) ;
#43732 = ADVANCED_FACE ( 'NONE', ( #40536 ), #61419, .F. ) ;
#43733 = CARTESIAN_POINT ( 'NONE',  ( 51.06648329127400388, -18.82844715994099971, 333.4006252759120343 ) ) ;
#43734 = CARTESIAN_POINT ( 'NONE',  ( 109.6227372377152847, -25.10643708164309018, 29.90419670448196854 ) ) ;
#43735 = CARTESIAN_POINT ( 'NONE',  ( 117.4572939498068820, -40.49840382496243052, 169.5375300378159693 ) ) ;
#43736 = CARTESIAN_POINT ( 'NONE',  ( 111.4988423704183020, -26.55354146975621177, 280.7375300378156453 ) ) ;
#43737 = AXIS2_PLACEMENT_3D ( 'NONE', #2305, #49975, #43611 ) ;
#43739 = DIRECTION ( 'NONE',  ( 4.299999999999999979E-14, -1.000000000000000000, 0.000000000000000000 ) ) ;
#43738 = CARTESIAN_POINT ( 'NONE',  ( 0.000000000000000000, 211.0000000000000000, 145.6557476874258441 ) ) ;
#43740 = CARTESIAN_POINT ( 'NONE',  ( 82.27770840670791586, -35.08426318373102504, 2.472582314369259571 ) ) ;
#43741 = ADVANCED_FACE ( 'NONE', ( #59621, #45987 ), #73719, .F. ) ;
#43742 = CIRCLE ( 'NONE', #55336, 0.2999999999999943823 ) ;
#43743 = ORIENTED_EDGE ( 'NONE', *, *, #8871, .T. ) ;
#43744 = DIRECTION ( 'NONE',  ( -0.9254794337955620787, -0.3787978585227822492, 0.000000000000000000 ) ) ;
#43745 = ORIENTED_EDGE ( 'NONE', *, *, #60857, .T. ) ;
#43746 = EDGE_CURVE ( 'NONE', #49287, #79347, #29155, .T. ) ;
#43747 = CARTESIAN_POINT ( 'NONE',  ( 96.75683229781660089, -37.84742820979678868, 77.40038718067299328 ) ) ;
#43749 = ORIENTED_EDGE ( 'NONE', *, *, #85239, .F. ) ;
#43748 = CARTESIAN_POINT ( 'NONE',  ( 7.028760451216134797, 93.12764692289525215, 130.3666587255899287 ) ) ;
#43750 = CARTESIAN_POINT ( 'NONE',  ( 116.3181333158508295, -32.94392590426259204, 50.13562527591097506 ) ) ;
#43751 = CARTESIAN_POINT ( 'NONE',  ( 117.9257662994439499, -34.79559216868042171, 194.9546728949589749 ) ) ;
#43752 = CARTESIAN_POINT ( 'NONE',  ( 150.5667039024482960, -47.82844715993594775, 300.4678068554149490 ) ) ;
#43753 = CARTESIAN_POINT ( 'NONE',  ( 98.04154693352651861, -41.04191595932115888, 146.6812072298401404 ) ) ;
#43754 = LINE ( 'NONE', #57383, #34172 ) ;
#43755 = DIRECTION ( 'NONE',  ( 0.000000000000000000, 0.000000000000000000, 1.000000000000000000 ) ) ;
#43757 = EDGE_CURVE ( 'NONE', #15522, #30970, #75961, .T. ) ;
#43756 = VECTOR ( 'NONE', #16528, 1000.000000000000000 ) ;
#43758 = FACE_BOUND ( 'NONE', #41063, .T. ) ;
#43759 = DIRECTION ( 'NONE',  ( -4.237773401492740281E-14, 1.000000000000000000, 0.000000000000000000 ) ) ;
#43760 = CARTESIAN_POINT ( 'NONE',  ( 116.5042510202519708, -34.04512512578503447, 149.0470538473399529 ) ) ;
#43761 = ORIENTED_EDGE ( 'NONE', *, *, #349, .F. ) ;
#43762 = VERTEX_POINT ( 'NONE', #34615 ) ;
#43763 = VECTOR ( 'NONE', #61277, 999.9999999999998863 ) ;
#43764 = CARTESIAN_POINT ( 'NONE',  ( 98.20303647727408247, -37.43757155718014928, 97.82158330589696504 ) ) ;
#43765 = AXIS2_PLACEMENT_3D ( 'NONE', #1965, #29661, #50540 ) ;
#43766 = DIRECTION ( 'NONE',  ( 0.000000000000000000, 1.000000000000000000, 0.000000000000000000 ) ) ;
#43768 = CYLINDRICAL_SURFACE ( 'NONE', #43327, 0.2500000000000002220 ) ;
#43767 = CARTESIAN_POINT ( 'NONE',  ( 104.5747221139661605, -26.66317121150818892, 236.2575300378149734 ) ) ;
#43769 = DIRECTION ( 'NONE',  ( -1.000000000000000078E-15, 1.000000000000000000, 0.000000000000000000 ) ) ;
#43770 = CARTESIAN_POINT ( 'NONE',  ( 100.9546619336613844, -28.70703383231385430, 111.5943577614134199 ) ) ;
#43771 = VECTOR ( 'NONE', #40810, 999.9999999999998863 ) ;
#43772 = CARTESIAN_POINT ( 'NONE',  ( -179.8898777604655095, 101.5999999999999943, -12.69999999999999929 ) ) ;
#43773 = DIRECTION ( 'NONE',  ( 0.000000000000000000, 0.000000000000000000, 1.000000000000000000 ) ) ;
#43774 = LINE ( 'NONE', #30156, #86463 ) ;
#43775 = CARTESIAN_POINT ( 'NONE',  ( 100.8994224252808323, -45.87202276647018095, 152.0918157521009562 ) ) ;
#43776 = ORIENTED_EDGE ( 'NONE', *, *, #75845, .T. ) ;
#43777 = ORIENTED_EDGE ( 'NONE', *, *, #6513, .F. ) ;
#43778 = ORIENTED_EDGE ( 'NONE', *, *, #3644, .T. ) ;
#43779 = DIRECTION ( 'NONE',  ( -0.1858654557293184517, 0.9825752044329902901, 0.000000000000000000 ) ) ;
#43780 = CARTESIAN_POINT ( 'NONE',  ( 115.0876195537187670, -30.61596616040899832, 129.3441257015518602 ) ) ;
#43782 = EDGE_CURVE ( 'NONE', #68461, #61667, #9671, .T. ) ;
#43781 = CARTESIAN_POINT ( 'NONE',  ( 97.81334898132925559, -40.52147985742783476, 102.6359742825680144 ) ) ;
#43783 = CARTESIAN_POINT ( 'NONE',  ( 113.5820732635001491, -31.81245485458596889, 217.1595189410199396 ) ) ;
#43784 = CARTESIAN_POINT ( 'NONE',  ( 116.8171232307727934, -34.15291921056556390, 270.0314585327250825 ) ) ;
#43785 = CARTESIAN_POINT ( 'NONE',  ( 96.61862839515298162, -36.21153332102672806, 171.2870538473399620 ) ) ;
#43786 = CARTESIAN_POINT ( 'NONE',  ( 107.0664832912739968, -36.72944715994100306, 287.6356252759109680 ) ) ;
#43787 = ORIENTED_EDGE ( 'NONE', *, *, #32615, .F. ) ;
#43789 = ORIENTED_EDGE ( 'NONE', *, *, #7078, .T. ) ;
#43788 = VERTEX_POINT ( 'NONE', #7811 ) ;
#43790 = DIRECTION ( 'NONE',  ( 0.000000000000000000, -1.000000000000000000, 0.000000000000000000 ) ) ;
#43791 = ORIENTED_EDGE ( 'NONE', *, *, #83989, .T. ) ;
#43792 = EDGE_LOOP ( 'NONE', ( #77734, #51942, #5948, #87773 ) ) ;
#43793 = CARTESIAN_POINT ( 'NONE',  ( 0.000000000000000000, 184.0000000000000000, 0.000000000000000000 ) ) ;
#43794 = CARTESIAN_POINT ( 'NONE',  ( 131.3325395364358883, -36.38432368374370185, 6.774690158159009101 ) ) ;
#43795 = CARTESIAN_POINT ( 'NONE',  ( 116.6500553765360451, -33.62673909641207359, 280.5072975916113478 ) ) ;
#43796 = CARTESIAN_POINT ( 'NONE',  ( 99.04406103905903080, -42.84125657712180413, 271.8439585032700734 ) ) ;
#43797 = ORIENTED_EDGE ( 'NONE', *, *, #45886, .F. ) ;
#43798 = EDGE_CURVE ( 'NONE', #10458, #42899, #49572, .T. ) ;
#43799 = AXIS2_PLACEMENT_3D ( 'NONE', #57131, #43052, #76705 ) ;
#43800 = CARTESIAN_POINT ( 'NONE',  ( 108.2227403955006082, -44.96027198985901663, 9.635625275910943088 ) ) ;
#43801 = DIRECTION ( 'NONE',  ( 0.000000000000000000, 0.000000000000000000, -1.000000000000000000 ) ) ;
#43802 = EDGE_LOOP ( 'NONE', ( #83152, #47830 ) ) ;
#43803 = ORIENTED_EDGE ( 'NONE', *, *, #71345, .T. ) ;
#43804 = STYLED_ITEM ( 'NONE', ( #70190 ), #18841 ) ;
#43805 = ADVANCED_FACE ( 'NONE', ( #20996 ), #69596, .T. ) ;
#43806 = CARTESIAN_POINT ( 'NONE',  ( 110.8545864177290099, -45.98419052231162141, 112.8856351242157530 ) ) ;
#43807 = VERTEX_POINT ( 'NONE', #27355 ) ;
#43808 = ORIENTED_EDGE ( 'NONE', *, *, #36129, .F. ) ;
#43809 = CARTESIAN_POINT ( 'NONE',  ( 101.7280645633873775, -29.41412380334073973, 29.98861030426797214 ) ) ;
#43810 = CARTESIAN_POINT ( 'NONE',  ( 109.8619129364321481, -26.66307059906275612, 174.8613395616249591 ) ) ;
#43811 = CARTESIAN_POINT ( 'NONE',  ( 102.3226935662337098, -26.77152163616654335, 140.4422919425769578 ) ) ;
#43812 = CARTESIAN_POINT ( 'NONE',  ( 116.8574199659429098, -40.30995640862995799, 214.5470538473389581 ) ) ;
#43813 = CARTESIAN_POINT ( 'NONE',  ( 116.8170375758959665, -34.15258794555239774, 100.0316818571836137 ) ) ;
#43814 = CARTESIAN_POINT ( 'NONE',  ( 102.0659246755500362, -27.97116092501175189, 126.4898951673323637 ) ) ;
#43815 = CARTESIAN_POINT ( 'NONE',  ( -130.5149182481443404, 70.27892663483460467, 3.298988752046296380 ) ) ;
#43816 = ORIENTED_EDGE ( 'NONE', *, *, #38203, .F. ) ;
#43817 = AXIS2_PLACEMENT_3D ( 'NONE', #65673, #79333, #17098 ) ;
#43818 = ORIENTED_EDGE ( 'NONE', *, *, #57003, .T. ) ;
#43819 = AXIS2_PLACEMENT_3D ( 'NONE', #11697, #39390, #67096 ) ;
#43820 = VECTOR ( 'NONE', #25264, 1000.000000000000114 ) ;
#43821 = CARTESIAN_POINT ( 'NONE',  ( 117.1106518157658343, -39.68263944894788864, 183.5984824187679578 ) ) ;
#43822 = ORIENTED_EDGE ( 'NONE', *, *, #49052, .F. ) ;
#43823 = CARTESIAN_POINT ( 'NONE',  ( 109.4453579932576872, -25.93500217162640453, 179.8918157521019339 ) ) ;
#43824 = LINE ( 'NONE', #30217, #12683 ) ;
#43825 = LINE ( 'NONE', #22514, #24674 ) ;
#43826 = CARTESIAN_POINT ( 'NONE',  ( 51.06648329127400388, 19.62155284005901024, 333.4006252759110112 ) ) ;
#43829 = CARTESIAN_POINT ( 'NONE',  ( 117.4695305279093986, -36.80206755349690440, 259.8213395616249386 ) ) ;
#43828 = CARTESIAN_POINT ( 'NONE',  ( 116.3184051949732805, -40.67301874499263192, 58.50512385792708869 ) ) ;
#43827 = CARTESIAN_POINT ( 'NONE',  ( 97.95414082892358465, -40.28560263849463041, 277.6356252759110248 ) ) ;
#43830 = DIRECTION ( 'NONE',  ( 0.000000000000000000, 0.000000000000000000, 1.000000000000000000 ) ) ;
#43831 = ADVANCED_FACE ( 'NONE', ( #1000 ), #48672, .T. ) ;
#43832 = DIRECTION ( 'NONE',  ( 0.000000000000000000, 0.000000000000000000, -1.000000000000000000 ) ) ;
#43833 = VECTOR ( 'NONE', #29779, 1000.000000000000000 ) ;
#43834 = CARTESIAN_POINT ( 'NONE',  ( 113.2419700359254904, -28.75597482911128822, 270.5522191222117385 ) ) ;
#43835 = EDGE_CURVE ( 'NONE', #31385, #35045, #36233, .T. ) ;
#43836 = LINE ( 'NONE', #83859, #76117 ) ;
#43837 = CARTESIAN_POINT ( 'NONE',  ( 116.7951252733230945, -39.38782978238762666, 259.6147919431981563 ) ) ;
#43838 = VECTOR ( 'NONE', #81852, 1000.000000000000000 ) ;
#43839 = CARTESIAN_POINT ( 'NONE',  ( 146.5623089610532759, -137.3886574699120615, 246.8356538633832997 ) ) ;
#43841 = ORIENTED_EDGE ( 'NONE', *, *, #51318, .F. ) ;
#43840 = CARTESIAN_POINT ( 'NONE',  ( 115.0355867660158538, -32.94440492534615572, 195.5838068554167251 ) ) ;
#43842 = ADVANCED_FACE ( 'NONE', ( #62320 ), #76855, .T. ) ;
#43843 = DIRECTION ( 'NONE',  ( 1.000000000000000000, 0.000000000000000000, 9.462128050782575008E-16 ) ) ;
#43844 = CARTESIAN_POINT ( 'NONE',  ( 101.3369781660191222, -46.20933176663394448, 202.1318157521019430 ) ) ;
#43845 = CARTESIAN_POINT ( 'NONE',  ( 110.3540904097210387, -25.34409450869410563, 60.85276813305395649 ) ) ;
#43846 = CARTESIAN_POINT ( 'NONE',  ( 110.5132149073354242, -26.84445748292755951, 205.8099109901969541 ) ) ;
#43847 = CARTESIAN_POINT ( 'NONE',  ( 194.5667039024482676, -40.82844715993405060, 129.9678068554150343 ) ) ;
#43848 = CARTESIAN_POINT ( 'NONE',  ( 32.06670390244772051, -33.35206098992742341, 237.4678068554150059 ) ) ;
#43850 = DIRECTION ( 'NONE',  ( 0.000000000000000000, 0.000000000000000000, -1.000000000000000000 ) ) ;
#43849 = CARTESIAN_POINT ( 'NONE',  ( 0.000000000000000000, 95.25000000000000000, 42.54500000000000171 ) ) ;
#43851 = DIRECTION ( 'NONE',  ( -4.012088370409549976E-14, 1.000000000000000000, 0.000000000000000000 ) ) ;
#43852 = CARTESIAN_POINT ( 'NONE',  ( 144.0664521793745791, -140.6784471599409017, 245.4721420275650132 ) ) ;
#43853 = ORIENTED_EDGE ( 'NONE', *, *, #10292, .T. ) ;
#43854 = CARTESIAN_POINT ( 'NONE',  ( 113.2480160518910992, -28.76059550239980567, 64.55305391943088011 ) ) ;
#43855 = EDGE_CURVE ( 'NONE', #8294, #51052, #71075, .T. ) ;
#43856 =( BOUNDED_CURVE ( )  B_SPLINE_CURVE ( 3, ( #74281, #26129, #53797, #12502 ),
 .UNSPECIFIED., .F., .F. ) 
 B_SPLINE_CURVE_WITH_KNOTS ( ( 4, 4 ),
 ( 0.1001674211615598831, 3.041425232428233372 ),
 .UNSPECIFIED. ) 
 CURVE ( )  GEOMETRIC_REPRESENTATION_ITEM ( )  RATIONAL_B_SPLINE_CURVE ( ( 1.000000000000000000, 0.3999999999999999667, 0.3999999999999999667, 1.000000000000000000 ) ) 
 REPRESENTATION_ITEM ( '' )  );
#43857 = VERTEX_POINT ( 'NONE', #7367 ) ;
#43858 = ORIENTED_EDGE ( 'NONE', *, *, #62596, .F. ) ;
#43859 = ADVANCED_FACE ( 'NONE', ( #68700 ), #65223, .T. ) ;
#43860 = CARTESIAN_POINT ( 'NONE',  ( 115.2923595980251434, -39.02968425817515197, 98.03241982807698207 ) ) ;
#43862 = VERTEX_POINT ( 'NONE', #28240 ) ;
#43861 = LINE ( 'NONE', #30689, #73429 ) ;
#43863 = AXIS2_PLACEMENT_3D ( 'NONE', #64879, #15837, #16728 ) ;
#43864 = CARTESIAN_POINT ( 'NONE',  ( 117.3319688044106925, -38.62265419183309945, 84.68133956162593279 ) ) ;
#43865 = DIRECTION ( 'NONE',  ( 4.299999999999999979E-14, -1.000000000000000000, 4.400000000000000367E-29 ) ) ;
#43866 = DIRECTION ( 'NONE',  ( -0.7071067812159671506, -0.7071067811571278838, 2.899137802744108569E-29 ) ) ;
#43867 = CARTESIAN_POINT ( 'NONE',  ( 97.33784131910049098, -34.07106450134590858, 177.1147919402304467 ) ) ;
#43868 = CARTESIAN_POINT ( 'NONE',  ( 115.8115096128642136, -32.27542772465447030, 44.20133956162592170 ) ) ;
#43869 = ORIENTED_EDGE ( 'NONE', *, *, #55100, .T. ) ;
#43870 = ORIENTED_EDGE ( 'NONE', *, *, #74595, .T. ) ;
#43871 = ORIENTED_EDGE ( 'NONE', *, *, #89073, .T. ) ;
#43872 = AXIS2_PLACEMENT_3D ( 'NONE', #84600, #54261, #47008 ) ;
#43873 = LINE ( 'NONE', #42079, #55811 ) ;
#43874 = CARTESIAN_POINT ( 'NONE',  ( 21.03689327557613709, -23.42844715994198879, 117.4678068554150343 ) ) ;
#43875 = CARTESIAN_POINT ( 'NONE',  ( 71.25580610988301089, -82.12815647064930147, 542.9756252759101471 ) ) ;
#43876 = DIRECTION ( 'NONE',  ( -0.7071067811865171526, -0.7071067811865779928, -7.071067811865164719E-16 ) ) ;
#43877 = CARTESIAN_POINT ( 'NONE',  ( 93.48397507443749532, 95.16896684734908263, 91.13883569058539535 ) ) ;
#43878 = CARTESIAN_POINT ( 'NONE',  ( 25.56670390244797275, -65.37844715994100397, 252.3428068554150059 ) ) ;
#43879 = FACE_OUTER_BOUND ( 'NONE', #53391, .T. ) ;
#43880 = CARTESIAN_POINT ( 'NONE',  ( -1.596709470477730486, 95.17668143650945467, 130.5484419168967349 ) ) ;
#43881 = CARTESIAN_POINT ( 'NONE',  ( 117.9659426345832713, -38.42225801833666310, 68.69181575210198787 ) ) ;
#43883 = ORIENTED_EDGE ( 'NONE', *, *, #58531, .F. ) ;
#43882 = TOROIDAL_SURFACE ( 'NONE', #27933, 13.50000000000000000, 0.5000000000000000000 ) ;
#43884 = LINE ( 'NONE', #70266, #82383 ) ;
#43886 = EDGE_CURVE ( 'NONE', #10009, #72907, #34159, .T. ) ;
#43885 = CARTESIAN_POINT ( 'NONE',  ( 41.56648329127398966, -27.82844715994070484, 74.17562527591199739 ) ) ;
#43887 = CARTESIAN_POINT ( 'NONE',  ( 103.3817498881349906, -44.01315952142851984, 125.0223760838769778 ) ) ;
#43888 = AXIS2_PLACEMENT_3D ( 'NONE', #71991, #42915, #15694 ) ;
#43889 = EDGE_CURVE ( 'NONE', #66320, #5230, #28704, .T. ) ;
#43890 = CARTESIAN_POINT ( 'NONE',  ( -72.96458098368751166, 117.4749999999999943, 80.90208098368620426 ) ) ;
#43891 = AXIS2_PLACEMENT_3D ( 'NONE', #86977, #47394, #26084 ) ;
#43892 = DIRECTION ( 'NONE',  ( 0.000000000000000000, 0.000000000000000000, 1.000000000000000000 ) ) ;
#43893 = ORIENTED_EDGE ( 'NONE', *, *, #58454, .T. ) ;
#43894 = ORIENTED_EDGE ( 'NONE', *, *, #18321, .T. ) ;
#43895 = DIRECTION ( 'NONE',  ( 0.000000000000000000, 1.000000000000000000, 0.000000000000000000 ) ) ;
#43896 = ORIENTED_EDGE ( 'NONE', *, *, #13213, .T. ) ;
#43897 = VERTEX_POINT ( 'NONE', #72724 ) ;
#43898 = CARTESIAN_POINT ( 'NONE',  ( 99.15781305739687923, -40.79332027783682690, 193.1358690201829518 ) ) ;
#43899 = DIRECTION ( 'NONE',  ( 0.000000000000000000, 0.000000000000000000, 1.000000000000000000 ) ) ;
#43900 = CARTESIAN_POINT ( 'NONE',  ( 106.0743987232105212, -48.56321320874933889, 108.5099109901969712 ) ) ;
#43901 = CARTESIAN_POINT ( 'NONE',  ( 98.34985898019030515, -31.65658469527032182, 120.9064585987749183 ) ) ;
#43902 = CARTESIAN_POINT ( 'NONE',  ( 98.54780627451228270, -41.97722989217538725, 16.76585467579917221 ) ) ;
#43903 = VERTEX_POINT ( 'NONE', #71837 ) ;
#43904 = ADVANCED_FACE ( 'NONE', ( #57747 ), #2350, .F. ) ;
#43905 = EDGE_LOOP ( 'NONE', ( #32777, #39168 ) ) ;
#43906 = ORIENTED_EDGE ( 'NONE', *, *, #45880, .T. ) ;
#43907 = CARTESIAN_POINT ( 'NONE',  ( 98.50976710839005079, -35.43193677023271704, 219.0128522743539747 ) ) ;
#43909 = CARTESIAN_POINT ( 'NONE',  ( 110.8024161898992190, -46.48594086123524960, 62.86705384733992474 ) ) ;
#43908 = VECTOR ( 'NONE', #11596, 1000.000000000000000 ) ;
#43910 = VERTEX_POINT ( 'NONE', #71399 ) ;
#43911 = CARTESIAN_POINT ( 'NONE',  ( 116.7496603916997202, -31.44741115753626204, 24.21181575210196257 ) ) ;
#43912 = CARTESIAN_POINT ( 'NONE',  ( 107.9200411489893412, -47.17696527638128856, 173.6413395616249886 ) ) ;
#43913 = DIRECTION ( 'NONE',  ( 1.000000000000000000, 0.000000000000000000, 0.000000000000000000 ) ) ;
#43914 = CARTESIAN_POINT ( 'NONE',  ( -110.5284195268215228, 45.17989370491086731, 69.48768198397286255 ) ) ;
#43915 = CARTESIAN_POINT ( 'NONE',  ( 109.5084879329568679, -46.86449036543412205, 128.7641967044819751 ) ) ;
#43916 = CARTESIAN_POINT ( 'NONE',  ( 31.75000000000000000, 111.1250000000000000, -3.174999999999999822 ) ) ;
#43917 = ORIENTED_EDGE ( 'NONE', *, *, #78107, .F. ) ;
#43918 = DIRECTION ( 'NONE',  ( 0.000000000000000000, 0.000000000000000000, 1.000000000000000000 ) ) ;
#43919 = EDGE_LOOP ( 'NONE', ( #8650, #18868, #66672, #53431 ) ) ;
#43920 = CARTESIAN_POINT ( 'NONE',  ( 113.1789227100342430, -44.75140297935337230, 134.0951559795896628 ) ) ;
#43921 = EDGE_LOOP ( 'NONE', ( #76285, #73951, #74554, #46029 ) ) ;
#43922 = ORIENTED_EDGE ( 'NONE', *, *, #2118, .F. ) ;
#43923 = AXIS2_PLACEMENT_3D ( 'NONE', #85050, #50493, #9618 ) ;
#43924 = CARTESIAN_POINT ( 'NONE',  ( 0.000000000000000000, 111.1250000000000000, 0.000000000000000000 ) ) ;
#43925 = CARTESIAN_POINT ( 'NONE',  ( 101.3624556188076440, -28.48975351766920738, 131.5580310753099695 ) ) ;
#43926 = CARTESIAN_POINT ( 'NONE',  ( 98.30617374076959436, -28.74837815785401673, 80.73848241876795839 ) ) ;
#43927 = CARTESIAN_POINT ( 'NONE',  ( 21.33963204133176461, 61.45598276206009558, 31.56377395493905524 ) ) ;
#43928 = FACE_OUTER_BOUND ( 'NONE', #65367, .T. ) ;
#43929 = LINE ( 'NONE', #78931, #2049 ) ;
#43930 = CARTESIAN_POINT ( 'NONE',  ( 104.6499073705539331, -46.24122592705978718, 47.37848241876896083 ) ) ;
#43932 = CARTESIAN_POINT ( 'NONE',  ( 103.4759237351581049, -46.49349013887657378, 138.2956252759109645 ) ) ;
#43931 = LINE ( 'NONE', #28069, #76843 ) ;
#43933 = LINE ( 'NONE', #70775, #34955 ) ;
#43934 = EDGE_CURVE ( 'NONE', #64009, #84699, #60855, .T. ) ;
#43935 = DIRECTION ( 'NONE',  ( 0.000000000000000000, 0.000000000000000000, 1.000000000000000000 ) ) ;
#43936 = VERTEX_POINT ( 'NONE', #85484 ) ;
#43937 = CARTESIAN_POINT ( 'NONE',  ( -472.4400000000000546, 53.97500000000000142, -3.174999999999999822 ) ) ;
#43938 = CARTESIAN_POINT ( 'NONE',  ( 51.56670390244699576, -22.48495420874030515, -5.074374724088000832 ) ) ;
#43940 = ORIENTED_EDGE ( 'NONE', *, *, #64575, .T. ) ;
#43939 = EDGE_CURVE ( 'NONE', #50424, #63964, #58625, .T. ) ;
#43941 = PLANE ( 'NONE',  #15470 ) ;
#43942 = DIRECTION ( 'NONE',  ( -1.000000000000000078E-15, 1.000000000000000000, 0.000000000000000000 ) ) ;
#43944 = VERTEX_POINT ( 'NONE', #30052 ) ;
#43943 = CARTESIAN_POINT ( 'NONE',  ( 110.5134301196510620, -26.84384026877932072, 209.8099109901969541 ) ) ;
#43945 = ADVANCED_FACE ( 'NONE', ( #23263 ), #70952, .F. ) ;
#43946 = CARTESIAN_POINT ( 'NONE',  ( -27.27158787008326968, 184.0000000000000000, 0.000000000000000000 ) ) ;
#43947 = CARTESIAN_POINT ( 'NONE',  ( 107.5109549264149251, -47.16686560604517098, 233.6099109901969655 ) ) ;
#43948 = CARTESIAN_POINT ( 'NONE',  ( 104.0954500313802527, -46.76767116204542418, 103.3470538473389411 ) ) ;
#43949 = LINE ( 'NONE', #72575, #46146 ) ;
#43950 = DIRECTION ( 'NONE',  ( 0.000000000000000000, 0.000000000000000000, -1.000000000000000000 ) ) ;
#43951 = LINE ( 'NONE', #70337, #37974 ) ;
#43952 = EDGE_LOOP ( 'NONE', ( #65877, #14478 ) ) ;
#43953 = AXIS2_PLACEMENT_3D ( 'NONE', #59357, #24413, #17594 ) ;
#43954 = CIRCLE ( 'NONE', #42526, 88.90000000000000568 ) ;
#43955 = ORIENTED_EDGE ( 'NONE', *, *, #3649, .F. ) ;
#43956 = VERTEX_POINT ( 'NONE', #1899 ) ;
#43957 = VECTOR ( 'NONE', #42002, 1000.000000000000114 ) ;
#43958 = ADVANCED_FACE ( 'NONE', ( #24131 ), #51802, .T. ) ;
#43959 = ORIENTED_EDGE ( 'NONE', *, *, #82786, .F. ) ;
#43960 = DIRECTION ( 'NONE',  ( 1.000000000000000000, 0.000000000000000000, 0.000000000000000000 ) ) ;
#43961 = CARTESIAN_POINT ( 'NONE',  ( 115.6952998724001560, -42.57974731087075071, 269.3527681330536439 ) ) ;
#43962 = DIRECTION ( 'NONE',  ( 0.000000000000000000, 0.000000000000000000, 1.000000000000000000 ) ) ;
#43963 = DIRECTION ( 'NONE',  ( 1.000000000000000000, -3.885780586187990841E-13, 0.000000000000000000 ) ) ;
#43964 = PRODUCT_DEFINITION_SHAPE ( 'NONE', 'NONE',  #1182 ) ;
#43966 = CARTESIAN_POINT ( 'NONE',  ( 89.55818655986067256, 72.98405218941671535, 77.68655577178756744 ) ) ;
#43965 = DIRECTION ( 'NONE',  ( 0.000000000000000000, -1.000000000000000000, 0.000000000000000000 ) ) ;
#43967 = CYLINDRICAL_SURFACE ( 'NONE', #47210, 2.517500000000005844 ) ;
#43968 = CARTESIAN_POINT ( 'NONE',  ( 104.7063189284543370, -28.49041042582816630, 224.7209912566489720 ) ) ;
#43969 = VERTEX_POINT ( 'NONE', #37761 ) ;
#43970 = ORIENTED_EDGE ( 'NONE', *, *, #64493, .F. ) ;
#43971 = VERTEX_POINT ( 'NONE', #77757 ) ;
#43972 = CARTESIAN_POINT ( 'NONE',  ( 107.0664832912748068, -36.72944715993923381, 13.92562527591097066 ) ) ;
#43973 = AXIS2_PLACEMENT_3D ( 'NONE', #61279, #32230, #89003 ) ;
#43974 = CARTESIAN_POINT ( 'NONE',  ( 110.8553449835648621, -45.98388008209910538, 182.8857003179606409 ) ) ;
#43975 = CARTESIAN_POINT ( 'NONE',  ( 115.6529839569024602, -41.48189714014871043, 259.4241967044819717 ) ) ;
#43976 = CARTESIAN_POINT ( 'NONE',  ( 37.03715912545347777, -48.62818131006128652, 129.9678068554150911 ) ) ;
#43977 = VECTOR ( 'NONE', #15626, 1000.000000000000000 ) ;
#43978 = CARTESIAN_POINT ( 'NONE',  ( 100.1408543393099393, -45.42701269980175738, 118.0413395616249659 ) ) ;
#43979 = CARTESIAN_POINT ( 'NONE',  ( 80.06648329127399677, -8.350947159940998787, 291.1181252759119502 ) ) ;
#43980 = ORIENTED_EDGE ( 'NONE', *, *, #18657, .F. ) ;
#43981 = CARTESIAN_POINT ( 'NONE',  ( 19.56670390244643443, -25.42844715994203852, 180.4678068554150911 ) ) ;
#43982 = CARTESIAN_POINT ( 'NONE',  ( 78.21890182791160839, -34.68450975841992090, 2.186797062532628289 ) ) ;
#43983 = VERTEX_POINT ( 'NONE', #65015 ) ;
#43984 = CARTESIAN_POINT ( 'NONE',  ( 1.166476076187854022E-15, 114.2999999999999972, 9.525000000000000355 ) ) ;
#43985 = CARTESIAN_POINT ( 'NONE',  ( 99.80492824067951574, -39.70159478663597241, 9.453804655305930282 ) ) ;
#43986 = CIRCLE ( 'NONE', #64323, 2.500000000000002220 ) ;
#43987 = CYLINDRICAL_SURFACE ( 'NONE', #79838, 2.750000000000002665 ) ;
#43988 = ADVANCED_FACE ( 'NONE', ( #10053 ), #23697, .T. ) ;
#43989 = CARTESIAN_POINT ( 'NONE',  ( 34.27258461953899626, -35.55794170701810941, -5.074374724088000832 ) ) ;
#43990 = CARTESIAN_POINT ( 'NONE',  ( 115.0371709891030747, -42.90857240100309156, 194.3022695669546067 ) ) ;
#43991 = EDGE_LOOP ( 'NONE', ( #25106, #62973, #52864, #3373, #57842, #22494 ) ) ;
#43992 = LINE ( 'NONE', #2243, #75528 ) ;
#43993 = DIRECTION ( 'NONE',  ( -1.000000000000000078E-15, 1.000000000000000083E-30, 1.000000000000000000 ) ) ;
#43994 = VERTEX_POINT ( 'NONE', #78220 ) ;
#43995 = CARTESIAN_POINT ( 'NONE',  ( 98.30617374076959436, -28.74837815785401673, 80.73848241876795839 ) ) ;
#43996 = ORIENTED_EDGE ( 'NONE', *, *, #13593, .T. ) ;
#43997 = CARTESIAN_POINT ( 'NONE',  ( 114.0673224709094598, -30.00197523691782209, 38.85813411379096749 ) ) ;
#43998 = CARTESIAN_POINT ( 'NONE',  ( 113.7194588667589557, -44.22387875709570437, 89.15331731304537755 ) ) ;
#43999 = CARTESIAN_POINT ( 'NONE',  ( 100.0889724914296863, -42.24093267880301994, 88.29015473446894191 ) ) ;
#44000 = CARTESIAN_POINT ( 'NONE',  ( 98.30750078144184556, -41.72879384224769694, 12.73978492213259450 ) ) ;
#44001 = CARTESIAN_POINT ( 'NONE',  ( 69.56670390244701707, -90.27844715994098124, 45.21780685541799727 ) ) ;
#44002 = LINE ( 'NONE', #77660, #47922 ) ;
#44003 = CARTESIAN_POINT ( 'NONE',  ( 105.8886828556765494, -47.16740550586902003, 278.4870538473396664 ) ) ;
#44004 = DIRECTION ( 'NONE',  ( 0.7071067809773464719, -0.7071067813957485626, 7.071067809773472419E-16 ) ) ;
#44005 = VERTEX_POINT ( 'NONE', #51361 ) ;
#44006 = AXIS2_PLACEMENT_3D ( 'NONE', #39799, #45708, #59796 ) ;
#44007 = LINE ( 'NONE', #10401, #58929 ) ;
#44008 = ORIENTED_EDGE ( 'NONE', *, *, #12726, .F. ) ;
#44009 = CARTESIAN_POINT ( 'NONE',  ( 95.96792091384095613, -36.58316683298836125, 152.3280062282919971 ) ) ;
#44010 = EDGE_CURVE ( 'NONE', #20111, #53395, #78673, .T. ) ;
#44011 = CARTESIAN_POINT ( 'NONE',  ( 125.3463460965257070, 52.73749999999999716, -36.51249999999992468 ) ) ;
#44012 = CIRCLE ( 'NONE', #73067, 17.00000000000000000 ) ;
#44013 = ORIENTED_EDGE ( 'NONE', *, *, #80356, .T. ) ;
#44014 = VERTEX_POINT ( 'NONE', #44101 ) ;
#44015 = VERTEX_POINT ( 'NONE', #58195 ) ;
#44016 = PLANE ( 'NONE',  #71050 ) ;
#44017 = CARTESIAN_POINT ( 'NONE',  ( 152.5667039024472444, -23.42844715993586036, 237.4678068554150059 ) ) ;
#44018 = CARTESIAN_POINT ( 'NONE',  ( 98.59486473514172644, -43.92970144294059054, 226.8870538473399563 ) ) ;
#44019 = CARTESIAN_POINT ( 'NONE',  ( 91.91441891875203396, -96.57077177932983147, -11.78219314458225853 ) ) ;
#44020 = FACE_OUTER_BOUND ( 'NONE', #78646, .T. ) ;
#44021 = CARTESIAN_POINT ( 'NONE',  ( -479.3614999999999782, 93.66249999999999432, 98.73639197104678544 ) ) ;
#44022 = CARTESIAN_POINT ( 'NONE',  ( 109.6119375470732109, -25.15554210634138954, 25.90419670448196143 ) ) ;
#44023 = EDGE_CURVE ( 'NONE', #28006, #76633, #3242, .T. ) ;
#44024 = CARTESIAN_POINT ( 'NONE',  ( -487.2989999999999782, 93.66249999999999432, 98.73639197104678544 ) ) ;
#44025 = ORIENTED_EDGE ( 'NONE', *, *, #45278, .F. ) ;
#44026 = CARTESIAN_POINT ( 'NONE',  ( 113.6007965834298545, -29.07570238281020636, 170.5145071421607668 ) ) ;
#44027 = EDGE_CURVE ( 'NONE', #23091, #87954, #64126, .T. ) ;
#44028 = CARTESIAN_POINT ( 'NONE',  ( 104.4080901167367443, -46.45808640916315824, 42.36430364053295250 ) ) ;
#44029 = ORIENTED_EDGE ( 'NONE', *, *, #16860, .T. ) ;
#44030 = CARTESIAN_POINT ( 'NONE',  ( 82.54112294218050749, -19.94037323192172551, 2.740176903240867379 ) ) ;
#44031 = AXIS2_PLACEMENT_3D ( 'NONE', #69004, #22659, #56239 ) ;
#44032 = CARTESIAN_POINT ( 'NONE',  ( 107.0664832912739968, -8.729447159940999512, 6.425625275911999168 ) ) ;
#44033 = CARTESIAN_POINT ( 'NONE',  ( 100.8614382317054776, -45.12360235833661903, 257.0699109901967745 ) ) ;
#44034 =( NAMED_UNIT ( * ) PLANE_ANGLE_UNIT ( ) SI_UNIT ( $, .RADIAN. ) );
#44035 = ADVANCED_FACE ( 'NONE', ( #30937 ), #79554, .T. ) ;
#44036 = FACE_OUTER_BOUND ( 'NONE', #44884, .T. ) ;
#44037 = DIRECTION ( 'NONE',  ( 0.8660254037844384856, 0.5000000000000003331, 0.000000000000000000 ) ) ;
#44038 = CARTESIAN_POINT ( 'NONE',  ( 112.1081655520365388, -43.62419673505787898, 227.5009912566479784 ) ) ;
#44040 = CARTESIAN_POINT ( 'NONE',  ( 115.8731522275743089, -31.19128430790907913, 30.27276813305396175 ) ) ;
#44039 = CARTESIAN_POINT ( 'NONE',  ( 37.03715912545433042, -48.62818131006122258, 249.9678068554150343 ) ) ;
#44041 = CARTESIAN_POINT ( 'NONE',  ( 126.7473051586034387, 60.90675218994213225, 31.31017718299094454 ) ) ;
#44042 = CARTESIAN_POINT ( 'NONE',  ( 109.6949574390794169, -47.51388072328656165, 87.75467289495897205 ) ) ;
#44043 = ORIENTED_EDGE ( 'NONE', *, *, #32048, .F. ) ;
#44044 = CARTESIAN_POINT ( 'NONE',  ( 131.7293641403231277, -20.17925173417497575, 7.255518600571654986 ) ) ;
#44045 = VERTEX_POINT ( 'NONE', #44995 ) ;
#44046 = AXIS2_PLACEMENT_3D ( 'NONE', #20280, #33887, #81175 ) ;
#44047 = PLANE ( 'NONE',  #52192 ) ;
#44048 = DIRECTION ( 'NONE',  ( 0.000000000000000000, 0.000000000000000000, -1.000000000000000000 ) ) ;
#44050 = ORIENTED_EDGE ( 'NONE', *, *, #61588, .T. ) ;
#44049 = EDGE_CURVE ( 'NONE', #42899, #35086, #36427, .T. ) ;
#44051 = CARTESIAN_POINT ( 'NONE',  ( 83.06670390244796920, -67.87844715994100397, 207.5838068554149913 ) ) ;
#44052 = VERTEX_POINT ( 'NONE', #65892 ) ;
#44053 = CARTESIAN_POINT ( 'NONE',  ( 82.81648329127398256, -18.72944715994105636, 14.92562527591094579 ) ) ;
#44054 = DIRECTION ( 'NONE',  ( -1.000000000000000000, 0.000000000000000000, 0.000000000000000000 ) ) ;
#44055 = CIRCLE ( 'NONE', #57084, 88.90000000000000568 ) ;
#44056 = LINE ( 'NONE', #50431, #7505 ) ;
#44057 = EDGE_LOOP ( 'NONE', ( #26070, #74097, #76841, #10163 ) ) ;
#44058 = CARTESIAN_POINT ( 'NONE',  ( 107.6042850712483698, -26.26048674992130572, 95.03562527591097364 ) ) ;
#44059 = CARTESIAN_POINT ( 'NONE',  ( 0.000000000000000000, 0.000000000000000000, 0.000000000000000000 ) ) ;
#44060 = CARTESIAN_POINT ( 'NONE',  ( 97.07201595580151832, -35.37887681970044440, 166.2189934953664761 ) ) ;
#44061 = FACE_OUTER_BOUND ( 'NONE', #70865, .T. ) ;
#44062 = CARTESIAN_POINT ( 'NONE',  ( -11.93200775504469391, 78.48097692672455139, 117.7530658574009976 ) ) ;
#44063 = ORIENTED_EDGE ( 'NONE', *, *, #86425, .T. ) ;
#44064 = ADVANCED_FACE ( 'NONE', ( #8725 ), #22802, .T. ) ;
#44065 = CARTESIAN_POINT ( 'NONE',  ( 100.1374281256146901, 87.79544278253752054, -83.76986456925365587 ) ) ;
#44066 = EDGE_CURVE ( 'NONE', #37352, #8193, #71139, .T. ) ;
#44067 = DIRECTION ( 'NONE',  ( 0.000000000000000000, 0.000000000000000000, 1.000000000000000000 ) ) ;
#44068 = EDGE_CURVE ( 'NONE', #71033, #46484, #73153, .T. ) ;
#44069 = DIRECTION ( 'NONE',  ( 0.000000000000000000, 0.000000000000000000, 1.000000000000000000 ) ) ;
#44070 = EDGE_CURVE ( 'NONE', #10702, #8698, #79821, .T. ) ;
#44071 = B_SPLINE_CURVE_WITH_KNOTS ( 'NONE', 3,
 ( #59634, #60079, #5139, #6054, #33742, #75531, #88722, #46451, #80559, #74624, #26037, #52791, #61432, #39205, #73732, #18315, #54149, #89159 ),
 .UNSPECIFIED., .F., .F.,
 ( 4, 2, 2, 2, 2, 2, 2, 2, 4 ),
 ( 0.4999874552890923862, 0.5624890233779558102, 0.6249905914668192342, 0.6874921595556827691, 0.7499937276445461931, 0.8124952957334096171, 0.8749968638222731521, 0.9374984319111365760, 1.000000000000000000 ),
 .UNSPECIFIED. ) ;
#44073 = DIRECTION ( 'NONE',  ( 0.000000000000000000, 0.000000000000000000, -1.000000000000000000 ) ) ;
#44072 = DIRECTION ( 'NONE',  ( 0.000000000000000000, 1.000000000000000000, 0.000000000000000000 ) ) ;
#44074 = DIRECTION ( 'NONE',  ( 0.1811243268507065352, -0.9834602067307444129, 0.000000000000000000 ) ) ;
#44075 = AXIS2_PLACEMENT_3D ( 'NONE', #65520, #78732, #64628 ) ;
#44076 = VERTEX_POINT ( 'NONE', #60866 ) ;
#44077 = CIRCLE ( 'NONE', #80413, 5.000000000000004441 ) ;
#44078 = DIRECTION ( 'NONE',  ( 0.7071067811865370256, 0.000000000000000000, -0.7071067811865580088 ) ) ;
#44079 = CARTESIAN_POINT ( 'NONE',  ( 108.8290724220007206, -27.07506712556666173, 160.9327681330529742 ) ) ;
#44081 = ORIENTED_EDGE ( 'NONE', *, *, #9388, .T. ) ;
#44080 = LINE ( 'NONE', #71813, #57338 ) ;
#44082 = CARTESIAN_POINT ( 'NONE',  ( 97.46604185887804306, -38.76544784714101155, 27.49276813305395706 ) ) ;
#44083 = FACE_BOUND ( 'NONE', #49150, .T. ) ;
#44084 = LINE ( 'NONE', #16850, #6693 ) ;
#44085 = CARTESIAN_POINT ( 'NONE',  ( 164.9667039024476765, -26.71338133338732135, 117.4678068554150485 ) ) ;
#44086 = CARTESIAN_POINT ( 'NONE',  ( 109.7260889235150785, -27.00112954045210856, 29.86492210598321506 ) ) ;
#44087 = CARTESIAN_POINT ( 'NONE',  ( 97.63766479707255996, -34.12929003103648284, 251.1127681330543737 ) ) ;
#44088 = EDGE_LOOP ( 'NONE', ( #22242, #14780, #86855, #43803, #36201, #45190, #27993, #83840 ) ) ;
#44089 = VERTEX_POINT ( 'NONE', #12283 ) ;
#44090 = CARTESIAN_POINT ( 'NONE',  ( 98.20738808897236538, -36.51799785534514342, 192.7387261630399564 ) ) ;
#44091 = CARTESIAN_POINT ( 'NONE',  ( 193.0371591254584303, -47.82818131005411999, 249.9678068554149775 ) ) ;
#44092 = CARTESIAN_POINT ( 'NONE',  ( 106.6757791475081376, -27.34201535943007499, 36.52920235351597711 ) ) ;
#44093 = AXIS2_PLACEMENT_3D ( 'NONE', #4932, #32627, #33528 ) ;
#44094 = CARTESIAN_POINT ( 'NONE',  ( -96.70275196374414861, 93.55256755804781221, 87.71306776503882929 ) ) ;
#44095 = AXIS2_PLACEMENT_3D ( 'NONE', #7639, #54858, #48486 ) ;
#44096 = EDGE_CURVE ( 'NONE', #46935, #82352, #17432, .T. ) ;
#44097 = CARTESIAN_POINT ( 'NONE',  ( 113.2454986998394162, -28.75867294625993154, 79.55229194239187507 ) ) ;
#44098 = LINE ( 'NONE', #22800, #89447 ) ;
#44099 = CONICAL_SURFACE ( 'NONE', #19533, 16.00000000000090239, 0.7853981633974503884 ) ;
#44100 = ORIENTED_EDGE ( 'NONE', *, *, #61915, .F. ) ;
#44101 = CARTESIAN_POINT ( 'NONE',  ( 182.5667039024459939, -19.82844715994031048, -5.074374724088000832 ) ) ;
#44102 = CARTESIAN_POINT ( 'NONE',  ( -240.5296158183964792, 93.66249999999999432, 95.25000000000000000 ) ) ;
#44103 = CARTESIAN_POINT ( 'NONE',  ( 97.03753386688401861, -33.96379371595038776, 251.1127681330538337 ) ) ;
#44104 = CARTESIAN_POINT ( 'NONE',  ( 6.359898905133524849, 93.57403044202068543, 118.3873059837162742 ) ) ;
#44105 = ORIENTED_EDGE ( 'NONE', *, *, #33806, .T. ) ;
#44106 = DIRECTION ( 'NONE',  ( 1.000000000000000000, 1.000000000000000078E-15, 0.000000000000000000 ) ) ;
#44107 = DIRECTION ( 'NONE',  ( 1.000000000000000000, 4.163336342344333240E-14, 0.000000000000000000 ) ) ;
#44108 = DIRECTION ( 'NONE',  ( 0.000000000000000000, -1.000000000000000000, 0.000000000000000000 ) ) ;
#44109 = FACE_BOUND ( 'NONE', #56926, .T. ) ;
#44110 = CARTESIAN_POINT ( 'NONE',  ( 100.8863495415024829, -28.40209871822986543, 31.59657765686296926 ) ) ;
#44111 = LINE ( 'NONE', #39092, #68891 ) ;
#44112 = ORIENTED_EDGE ( 'NONE', *, *, #20251, .T. ) ;
#44113 = CARTESIAN_POINT ( 'NONE',  ( 117.5312049024071257, -37.01681686833584450, 39.80419670448193159 ) ) ;
#44114 = EDGE_CURVE ( 'NONE', #27939, #3527, #7322, .T. ) ;
#44115 = CARTESIAN_POINT ( 'NONE',  ( 107.0664832912739257, -52.57944715994094764, 302.6356252759109680 ) ) ;
#44116 = CARTESIAN_POINT ( 'NONE',  ( 116.1397716810727303, -31.55208187140975795, 289.2384824187681716 ) ) ;
#44117 = EDGE_CURVE ( 'NONE', #48818, #45118, #25913, .T. ) ;
#44118 = ORIENTED_EDGE ( 'NONE', *, *, #24154, .F. ) ;
#44119 = EDGE_CURVE ( 'NONE', #33965, #19079, #56586, .T. ) ;
#44120 = PLANE ( 'NONE',  #11496 ) ;
#44121 = CARTESIAN_POINT ( 'NONE',  ( 108.3343131715331822, -46.73476620053450148, 18.67790446994724007 ) ) ;
#44122 = DIRECTION ( 'NONE',  ( 0.000000000000000000, 0.000000000000000000, -1.000000000000000000 ) ) ;
#44123 = CARTESIAN_POINT ( 'NONE',  ( 99.39318122740648676, -32.72677799018995870, 88.74999513149600716 ) ) ;
#44124 = CARTESIAN_POINT ( 'NONE',  ( 115.4053350490088548, -30.43652969535880359, 215.3413395616249773 ) ) ;
#44125 = EDGE_CURVE ( 'NONE', #7095, #84589, #11660, .T. ) ;
#44126 = LINE ( 'NONE', #15104, #1456 ) ;
#44127 = ORIENTED_EDGE ( 'NONE', *, *, #79574, .T. ) ;
#44128 = EDGE_CURVE ( 'NONE', #14756, #63362, #46325, .T. ) ;
#44129 = LINE ( 'NONE', #16902, #70866 ) ;
#44130 = ORIENTED_EDGE ( 'NONE', *, *, #76350, .F. ) ;
#44131 = ORIENTED_EDGE ( 'NONE', *, *, #9873, .T. ) ;
#44132 = EDGE_CURVE ( 'NONE', #64884, #60724, #85665, .T. ) ;
#44133 = AXIS2_PLACEMENT_3D ( 'NONE', #42064, #55668, #70233 ) ;
#44134 = DIRECTION ( 'NONE',  ( 1.000000000000000000, 4.163336342344333240E-14, 0.000000000000000000 ) ) ;
#44135 = ORIENTED_EDGE ( 'NONE', *, *, #39987, .T. ) ;
#44136 = EDGE_LOOP ( 'NONE', ( #84138, #66535, #12642, #83265, #56812, #40675 ) ) ;
#44137 = DIRECTION ( 'NONE',  ( 1.000000000000000000, 0.000000000000000000, 0.000000000000000000 ) ) ;
#44138 = ADVANCED_FACE ( 'NONE', ( #11385 ), #24570, .F. ) ;
#44139 = CARTESIAN_POINT ( 'NONE',  ( 97.07206694318691120, -35.37847583654921380, 42.21889330128750117 ) ) ;
#44140 = CARTESIAN_POINT ( 'NONE',  ( 115.3391490808644875, -34.60362203641794565, 123.4495626852199734 ) ) ;
#44141 = CARTESIAN_POINT ( 'NONE',  ( 106.8359473341788686, -47.17421700602214685, 272.5584824187680510 ) ) ;
#44142 = CARTESIAN_POINT ( 'NONE',  ( 34.96670390244699433, -28.27351298637401200, 342.9256252759119548 ) ) ;
#44144 = ORIENTED_EDGE ( 'NONE', *, *, #80019, .F. ) ;
#44143 = ADVANCED_FACE ( 'NONE', ( #4574 ), #31939, .T. ) ;
#44145 = DIRECTION ( 'NONE',  ( 4.299999999999999979E-14, -1.000000000000000000, 4.400000000000000367E-29 ) ) ;
#44146 = ORIENTED_EDGE ( 'NONE', *, *, #52392, .T. ) ;
#44147 = FACE_OUTER_BOUND ( 'NONE', #88364, .T. ) ;
#44148 = FACE_OUTER_BOUND ( 'NONE', #37566, .T. ) ;
#44149 = CARTESIAN_POINT ( 'NONE',  ( 97.92338214298322896, -40.78104107816966462, 131.6584137149031619 ) ) ;
#44151 = VECTOR ( 'NONE', #65906, 1000.000000000000000 ) ;
#44150 = CARTESIAN_POINT ( 'NONE',  ( 96.84578370412310733, -30.63304659132085206, 280.8984824187681397 ) ) ;
#44152 = VERTEX_POINT ( 'NONE', #10931 ) ;
#44153 = UNCERTAINTY_MEASURE_WITH_UNIT (LENGTH_MEASURE( 1.000000000000000082E-05 ), #50535, 'distance_accuracy_value', 'NONE');
#44154 = CARTESIAN_POINT ( 'NONE',  ( 112.4118754778678380, -46.40445981238691076, 252.9661014663871583 ) ) ;
#44155 = VECTOR ( 'NONE', #49095, 1000.000000000000000 ) ;
#44156 = CARTESIAN_POINT ( 'NONE',  ( 97.06313332029375829, -39.81586545721199144, 17.56419670448195092 ) ) ;
#44157 = MECHANICAL_DESIGN_GEOMETRIC_PRESENTATION_REPRESENTATION (  '', ( #23901 ), #80431 ) ;
#44158 =( NAMED_UNIT ( * ) SI_UNIT ( $, .STERADIAN. ) SOLID_ANGLE_UNIT ( ) );
#44159 = AXIS2_PLACEMENT_3D ( 'NONE', #73774, #58357, #82404 ) ;
#44160 = CARTESIAN_POINT ( 'NONE',  ( 66.21896343372186777, -72.55791859125245935, 542.9756252759101471 ) ) ;
#44162 = CARTESIAN_POINT ( 'NONE',  ( 116.3228127852087113, -32.93589129790882453, 90.13562527591095375 ) ) ;
#44161 = CARTESIAN_POINT ( 'NONE',  ( 53.06670390244700286, -78.67844715994100113, 180.4678068554179902 ) ) ;
#44163 = CARTESIAN_POINT ( 'NONE',  ( 107.0664832912739968, 19.62155284005901024, 327.8006252759110453 ) ) ;
#44164 = DIRECTION ( 'NONE',  ( 0.000000000000000000, -0.000000000000000000, 1.000000000000000000 ) ) ;
#44165 = CARTESIAN_POINT ( 'NONE',  ( 152.5667039024469602, -23.42844715993586036, 300.4678068554149490 ) ) ;
#44166 = AXIS2_PLACEMENT_3D ( 'NONE', #22408, #71011, #14247 ) ;
#44167 = VECTOR ( 'NONE', #26339, 999.9999999999998863 ) ;
#44168 = CARTESIAN_POINT ( 'NONE',  ( 97.81168895331838087, -40.51742574516882200, 287.6356252759109680 ) ) ;
#44169 = CARTESIAN_POINT ( 'NONE',  ( 116.7953080883038552, -39.38717811076809028, 163.6146878284437491 ) ) ;
#44170 = EDGE_CURVE ( 'NONE', #87657, #32855, #17755, .T. ) ;
#44171 = DIRECTION ( 'NONE',  ( 0.000000000000000000, 0.000000000000000000, -1.000000000000000000 ) ) ;
#44172 = CARTESIAN_POINT ( 'NONE',  ( -487.2989999999999782, 10.16305401447645984, 83.34375000000000000 ) ) ;
#44173 = CARTESIAN_POINT ( 'NONE',  ( 112.3495078575228376, -28.18909723048616911, 289.6356252759109680 ) ) ;
#44174 = CARTESIAN_POINT ( 'NONE',  ( 117.0682170987564774, -39.67016276869777869, 179.5984824187679294 ) ) ;
#44175 = CARTESIAN_POINT ( 'NONE',  ( 111.9390199320367145, -27.48847072138506320, 55.68991099019693536 ) ) ;
#44176 = EDGE_CURVE ( 'NONE', #2919, #74183, #46772, .T. ) ;
#44178 = CARTESIAN_POINT ( 'NONE',  ( 119.2637946045970097, -42.39761235918182791, 0.4256252759109831474 ) ) ;
#44177 = CARTESIAN_POINT ( 'NONE',  ( 84.06648329127399677, -18.82844715994099971, 93.42562527591199739 ) ) ;
#44179 = FACE_OUTER_BOUND ( 'NONE', #7943, .T. ) ;
#44180 = CIRCLE ( 'NONE', #47094, 1.000000000000000888 ) ;
#44181 = ORIENTED_EDGE ( 'NONE', *, *, #50186, .F. ) ;
#44182 = DIRECTION ( 'NONE',  ( -1.000000000000000000, -2.999999999999999839E-15, -1.000000000000000078E-15 ) ) ;
#44183 = VERTEX_POINT ( 'NONE', #52238 ) ;
#44184 = CARTESIAN_POINT ( 'NONE',  ( 110.1509004715571507, -26.04776408289600909, 60.85276813305296173 ) ) ;
#44186 = ORIENTED_EDGE ( 'NONE', *, *, #66138, .F. ) ;
#44185 = CARTESIAN_POINT ( 'NONE',  ( 1.595580815131592001, 95.17678229987137684, 130.5484528442787564 ) ) ;
#44187 = LINE ( 'NONE', #71922, #1125 ) ;
#44188 = CARTESIAN_POINT ( 'NONE',  ( 96.66614461754338095, -36.48121138304695421, 192.3070538473399438 ) ) ;
#44189 = CARTESIAN_POINT ( 'NONE',  ( 173.9900000000000091, 5.112500000000000711, -7.937500000000000000 ) ) ;
#44190 = CARTESIAN_POINT ( 'NONE',  ( 34.96670390244699433, -26.71338133339301635, -5.074374724088000832 ) ) ;
#44191 = LINE ( 'NONE', #24656, #44294 ) ;
#44192 = CARTESIAN_POINT ( 'NONE',  ( -74.15067561874319324, 127.0000000000000000, 68.53801554307369770 ) ) ;
#44193 = DIRECTION ( 'NONE',  ( 0.7071067811865192621, 0.7071067811865758834, 7.071067811865186413E-16 ) ) ;
#44194 = CARTESIAN_POINT ( 'NONE',  ( 117.0282276649355993, -35.31238565241870475, 98.93927789852577348 ) ) ;
#44195 = CARTESIAN_POINT ( 'NONE',  ( 98.15811136316399654, -31.42099212808717468, 130.9108633711499863 ) ) ;
#44196 = ORIENTED_EDGE ( 'NONE', *, *, #9847, .T. ) ;
#44197 = ORIENTED_EDGE ( 'NONE', *, *, #15559, .F. ) ;
#44198 = CARTESIAN_POINT ( 'NONE',  ( 115.8107094469502272, -38.34209669562990541, 85.11301187732594542 ) ) ;
#44199 = CARTESIAN_POINT ( 'NONE',  ( 45.76696975232739817, -48.62818131006041256, 180.4678068554150911 ) ) ;
#44201 = DIRECTION ( 'NONE',  ( 1.000000000000000078E-15, -1.000000000000000083E-30, -1.000000000000000000 ) ) ;
#44200 = CARTESIAN_POINT ( 'NONE',  ( 115.9419818307743668, -40.91744192719421847, 224.4756252759109714 ) ) ;
#44202 = AXIS2_PLACEMENT_3D ( 'NONE', #13909, #54310, #20288 ) ;
#44203 = DIRECTION ( 'NONE',  ( 0.000000000000000000, 0.000000000000000000, -1.000000000000000000 ) ) ;
#44204 = LINE ( 'NONE', #50131, #55275 ) ;
#44205 = CARTESIAN_POINT ( 'NONE',  ( 118.0433965939932364, 76.18740257834568297, -11.02250383333830541 ) ) ;
#44206 = DIRECTION ( 'NONE',  ( -0.000000000000000000, -0.000000000000000000, -1.000000000000000000 ) ) ;
#44207 = CARTESIAN_POINT ( 'NONE',  ( 192.5667039024472444, -23.42844715993434335, 300.4678068554149490 ) ) ;
#44208 = CARTESIAN_POINT ( 'NONE',  ( 118.8928063919343998, -36.92768728534039724, 153.8127681330539644 ) ) ;
#44209 = ORIENTED_EDGE ( 'NONE', *, *, #62430, .F. ) ;
#44210 = EDGE_LOOP ( 'NONE', ( #30247, #37561 ) ) ;
#44211 = LINE ( 'NONE', #71954, #38710 ) ;
#44212 = CARTESIAN_POINT ( 'NONE',  ( 146.5379504508059654, -68.38750913315759306, 246.8490270591256035 ) ) ;
#44213 = CYLINDRICAL_SURFACE ( 'NONE', #21462, 2.117000000000000881 ) ;
#44214 = CARTESIAN_POINT ( 'NONE',  ( 70.98999999999998067, 52.73749999999999716, -52.28750000000002274 ) ) ;
#44215 = CARTESIAN_POINT ( 'NONE',  ( 99.07378970379950545, -35.07216769230775810, 213.9823760838769715 ) ) ;
#44216 = VECTOR ( 'NONE', #80643, 1000.000000000000000 ) ;
#44217 = CIRCLE ( 'NONE', #71808, 1.000000000000000888 ) ;
#44218 = DIRECTION ( 'NONE',  ( -1.000000000000000078E-15, -1.000000000000000083E-30, 1.000000000000000000 ) ) ;
#44219 = AXIS2_PLACEMENT_3D ( 'NONE', #41626, #62084, #83003 ) ;
#44220 = AXIS2_PLACEMENT_3D ( 'NONE', #52701, #80920, #18668 ) ;
#44221 = EDGE_CURVE ( 'NONE', #49665, #66874, #80437, .T. ) ;
#44222 = CARTESIAN_POINT ( 'NONE',  ( 116.3504430951951605, -44.09481043651530996, 198.2927681330539542 ) ) ;
#44223 = ADVANCED_FACE ( 'NONE', ( #5017 ), #45432, .F. ) ;
#44224 = FACE_OUTER_BOUND ( 'NONE', #585, .T. ) ;
#44225 = ORIENTED_EDGE ( 'NONE', *, *, #84676, .F. ) ;
#44227 = ORIENTED_EDGE ( 'NONE', *, *, #35319, .T. ) ;
#44226 = ORIENTED_EDGE ( 'NONE', *, *, #21486, .F. ) ;
#44228 = CIRCLE ( 'NONE', #16705, 0.4999999999999982236 ) ;
#44230 = ADVANCED_FACE ( 'NONE', ( #67690 ), #18193, .T. ) ;
#44229 = AXIS2_PLACEMENT_3D ( 'NONE', #70261, #36188, #64347 ) ;
#44231 = DIRECTION ( 'NONE',  ( 4.299999999999999979E-14, -1.000000000000000000, 4.128053709984630540E-29 ) ) ;
#44232 = VERTEX_POINT ( 'NONE', #12735 ) ;
#44233 = CARTESIAN_POINT ( 'NONE',  ( 118.5256205435843526, -36.72944715994100306, 292.6356252759106837 ) ) ;
#44234 = CARTESIAN_POINT ( 'NONE',  ( 134.0664832912739826, -33.97944715994100306, 8.225625275910998013 ) ) ;
#44235 = CARTESIAN_POINT ( 'NONE',  ( 114.7786440655094680, -32.32849264894101537, 285.6701547344685537 ) ) ;
#44236 = ADVANCED_FACE ( 'NONE', ( #40426 ), #68141, .F. ) ;
#44237 = DIRECTION ( 'NONE',  ( -4.237773401492740281E-14, 1.000000000000000000, 0.000000000000000000 ) ) ;
#44238 = ORIENTED_EDGE ( 'NONE', *, *, #18517, .T. ) ;
#44239 = AXIS2_PLACEMENT_3D ( 'NONE', #11473, #53666, #46855 ) ;
#44240 = CARTESIAN_POINT ( 'NONE',  ( 111.4682881893262305, -44.05286453299024885, 9.635625275910939536 ) ) ;
#44241 = FACE_OUTER_BOUND ( 'NONE', #75264, .T. ) ;
#44242 = ORIENTED_EDGE ( 'NONE', *, *, #49885, .T. ) ;
#44243 = ORIENTED_EDGE ( 'NONE', *, *, #46034, .T. ) ;
#44244 = EDGE_CURVE ( 'NONE', #67055, #48933, #55374, .T. ) ;
#44245 = CARTESIAN_POINT ( 'NONE',  ( 114.5728715930965933, -43.36891021780796507, 113.2502506786379968 ) ) ;
#44246 = VERTEX_POINT ( 'NONE', #56273 ) ;
#44247 = ORIENTED_EDGE ( 'NONE', *, *, #34121, .T. ) ;
#44248 = VECTOR ( 'NONE', #4292, 1000.000000000000000 ) ;
#44249 = EDGE_CURVE ( 'NONE', #58867, #26619, #43539, .T. ) ;
#44250 = CARTESIAN_POINT ( 'NONE',  ( 116.1953253310505119, -40.03623866633203932, 22.97241982807796035 ) ) ;
#44251 = CARTESIAN_POINT ( 'NONE',  ( 98.07151883162052286, -42.11266039418816121, 161.7556252759109725 ) ) ;
#44252 = CARTESIAN_POINT ( 'NONE',  ( 100.8994224252808323, -45.87202276647018095, 152.0918157521009562 ) ) ;
#44253 = CARTESIAN_POINT ( 'NONE',  ( 3.175000000000334666, 8.255000000000000782, 31.75000000000000000 ) ) ;
#44254 = CARTESIAN_POINT ( 'NONE',  ( 112.4117637605556297, -46.40425760712833636, 248.9661014663869878 ) ) ;
#44255 = DIRECTION ( 'NONE',  ( -0.000000000000000000, -0.000000000000000000, -1.000000000000000000 ) ) ;
#44256 = FACE_OUTER_BOUND ( 'NONE', #76971, .T. ) ;
#44257 = CARTESIAN_POINT ( 'NONE',  ( 67.06670390244707392, -137.6784471599409869, 55.21780685541800437 ) ) ;
#44258 = ORIENTED_EDGE ( 'NONE', *, *, #39043, .T. ) ;
#44259 = EDGE_CURVE ( 'NONE', #54314, #11434, #34501, .T. ) ;
#44260 = ORIENTED_EDGE ( 'NONE', *, *, #74531, .F. ) ;
#44261 = CIRCLE ( 'NONE', #26896, 1.000000000000000888 ) ;
#44262 = CARTESIAN_POINT ( 'NONE',  ( 103.7090067442367314, -26.14926592973559138, 205.3089586092439731 ) ) ;
#44263 = ORIENTED_EDGE ( 'NONE', *, *, #45775, .F. ) ;
#44264 = CARTESIAN_POINT ( 'NONE',  ( 117.0173010276973287, -33.62006509304910651, 174.0670538473389399 ) ) ;
#44265 = CARTESIAN_POINT ( 'NONE',  ( -31.75000000000000000, 124.5870000000000033, 3.174999999999779998 ) ) ;
#44266 = CIRCLE ( 'NONE', #18214, 2.030000000001869864 ) ;
#44267 = LINE ( 'NONE', #21625, #88487 ) ;
#44268 = CARTESIAN_POINT ( 'NONE',  ( 143.7815414234198101, -140.1960747189870347, 246.8365688484822442 ) ) ;
#44271 = CARTESIAN_POINT ( 'NONE',  ( 117.4970320020026406, -36.54623693216563396, 284.8413395616252615 ) ) ;
#44270 = CYLINDRICAL_SURFACE ( 'NONE', #32495, 9.999999999999998224 ) ;
#44269 = DIRECTION ( 'NONE',  ( -0.9419738712670564507, -1.744347090500093949E-16, -0.3356862014592719157 ) ) ;
#44272 = DIRECTION ( 'NONE',  ( 0.000000000000000000, 0.000000000000000000, -1.000000000000000000 ) ) ;
#44273 = CARTESIAN_POINT ( 'NONE',  ( 150.5667039024475571, -25.42844715993593852, 180.4678068554149775 ) ) ;
#44274 = DIRECTION ( 'NONE',  ( -1.000000000000000000, 0.000000000000000000, -3.491483361109385222E-15 ) ) ;
#44275 = FACE_OUTER_BOUND ( 'NONE', #62295, .T. ) ;
#44276 = CARTESIAN_POINT ( 'NONE',  ( 105.7154773553531015, -46.72385839539258257, 258.4689586112310167 ) ) ;
#44277 = CARTESIAN_POINT ( 'NONE',  ( 68.69171528984767860, -139.3034585473416769, 245.6607614303540004 ) ) ;
#44279 = ORIENTED_EDGE ( 'NONE', *, *, #40348, .T. ) ;
#44278 = CARTESIAN_POINT ( 'NONE',  ( 109.3644549449422954, -44.39418949346432441, 195.5838068554168956 ) ) ;
#44280 = CARTESIAN_POINT ( 'NONE',  ( 134.0664828118825938, -21.47944715903993540, 8.225259175038406312 ) ) ;
#44281 = CARTESIAN_POINT ( 'NONE',  ( 102.8350101556302434, -46.28146260531957523, 177.2441967044819648 ) ) ;
#44282 = CARTESIAN_POINT ( 'NONE',  ( 101.9605410436089699, -27.64034152677590583, 56.48419670448296159 ) ) ;
#44283 = CARTESIAN_POINT ( 'NONE',  ( 104.4428039971878803, -26.59488813107328653, 196.2784824187679362 ) ) ;
#44284 = DIRECTION ( 'NONE',  ( 0.000000000000000000, 0.000000000000000000, -1.000000000000000000 ) ) ;
#44285 = EDGE_CURVE ( 'NONE', #13477, #39062, #21795, .T. ) ;
#44286 = PLANE ( 'NONE',  #82357 ) ;
#44288 = CARTESIAN_POINT ( 'NONE',  ( 183.5150000000000148, 14.63749999999999929, -14.28749999999999964 ) ) ;
#44287 = CARTESIAN_POINT ( 'NONE',  ( 182.3467384525657735, -36.02818131005238200, 313.9678068554149490 ) ) ;
#44289 = DIRECTION ( 'NONE',  ( 1.000000000000000078E-15, 1.000000000000000083E-30, -1.000000000000000000 ) ) ;
#44290 = DIRECTION ( 'NONE',  ( -1.000000000000000078E-15, 0.000000000000000000, 1.000000000000000000 ) ) ;
#44291 = EDGE_LOOP ( 'NONE', ( #78716, #53619, #55392, #22828 ) ) ;
#44292 = CARTESIAN_POINT ( 'NONE',  ( 107.0664832912739968, -36.72944715994100306, 312.6356252759112522 ) ) ;
#44293 = AXIS2_PLACEMENT_3D ( 'NONE', #9049, #28571, #14964 ) ;
#44294 = VECTOR ( 'NONE', #52322, 1000.000000000000000 ) ;
#44295 = VECTOR ( 'NONE', #18290, 1000.000000000000000 ) ;
#44296 = ORIENTED_EDGE ( 'NONE', *, *, #25920, .F. ) ;
#44297 = ORIENTED_EDGE ( 'NONE', *, *, #36753, .T. ) ;
#44298 = VECTOR ( 'NONE', #69671, 1000.000000000000000 ) ;
#44299 = CARTESIAN_POINT ( 'NONE',  ( 99.58293739761768393, -32.55228987500129278, 110.3438483995049495 ) ) ;
#44301 = ORIENTED_EDGE ( 'NONE', *, *, #57401, .F. ) ;
#44300 = DIRECTION ( 'NONE',  ( 0.000000000000000000, 1.000000000000000000, -0.000000000000000000 ) ) ;
#44302 = CARTESIAN_POINT ( 'NONE',  ( 102.9796410358630254, -46.29638950891617100, 88.25562527591095829 ) ) ;
#44303 = LINE ( 'NONE', #51563, #73085 ) ;
#44304 = AXIS2_PLACEMENT_3D ( 'NONE', #7073, #35663, #76562 ) ;
#44305 = DIRECTION ( 'NONE',  ( 0.000000000000000000, 0.000000000000000000, 1.000000000000000000 ) ) ;
#44306 = EDGE_CURVE ( 'NONE', #19042, #19304, #49007, .T. ) ;
#44307 = CARTESIAN_POINT ( 'NONE',  ( 118.4837085360594671, -37.70862757085654238, 296.0306255462182321 ) ) ;
#44309 = CARTESIAN_POINT ( 'NONE',  ( 98.07879527422882404, -32.87106628761745952, 16.00419670448294340 ) ) ;
#44308 = AXIS2_PLACEMENT_3D ( 'NONE', #44421, #51234, #44878 ) ;
#44310 = ORIENTED_EDGE ( 'NONE', *, *, #20064, .T. ) ;
#44311 = EDGE_LOOP ( 'NONE', ( #29289, #44997, #4352, #63070 ) ) ;
#44312 = ORIENTED_EDGE ( 'NONE', *, *, #50039, .T. ) ;
#44313 = EDGE_CURVE ( 'NONE', #18319, #18059, #89033, .T. ) ;
#44314 = CARTESIAN_POINT ( 'NONE',  ( 141.0667039024479834, -50.82844715994100682, 310.9178068554150514 ) ) ;
#44315 = CARTESIAN_POINT ( 'NONE',  ( 134.0664832912740110, -41.22944715994101017, 1.625625275910997480 ) ) ;
#44316 = CARTESIAN_POINT ( 'NONE',  ( 188.5667039024483529, -48.82844715993431350, 293.2178068554150059 ) ) ;
#44317 = CARTESIAN_POINT ( 'NONE',  ( 177.1649999999999920, 14.63749999999999929, -52.38749999999999574 ) ) ;
#44318 = AXIS2_PLACEMENT_3D ( 'NONE', #62388, #35123, #62834 ) ;
#44319 = LINE ( 'NONE', #65230, #11306 ) ;
#44320 = FACE_OUTER_BOUND ( 'NONE', #68826, .T. ) ;
#44321 = DIRECTION ( 'NONE',  ( -1.000000000000000000, 0.000000000000000000, 0.000000000000000000 ) ) ;
#44322 = CARTESIAN_POINT ( 'NONE',  ( -7.105823921952652888, 93.07605504633957594, 130.3624800658744505 ) ) ;
#44323 = CARTESIAN_POINT ( 'NONE',  ( 110.7866772467784955, -46.44483816919306918, 62.86705384733992474 ) ) ;
#44324 = VECTOR ( 'NONE', #38426, 1000.000000000000114 ) ;
#44325 = ORIENTED_EDGE ( 'NONE', *, *, #74809, .T. ) ;
#44326 = DIRECTION ( 'NONE',  ( -1.000000000000000000, 0.000000000000000000, 7.136255983449500255E-16 ) ) ;
#44327 = FACE_OUTER_BOUND ( 'NONE', #85303, .T. ) ;
#44328 = CARTESIAN_POINT ( 'NONE',  ( 226.4410000000000025, 40.03750000000000142, -63.94449999999999790 ) ) ;
#44329 = CARTESIAN_POINT ( 'NONE',  ( 98.00070950526129820, -34.75266269402447250, 103.9738046553059547 ) ) ;
#44330 = AXIS2_PLACEMENT_3D ( 'NONE', #25843, #19023, #59889 ) ;
#44331 = AXIS2_PLACEMENT_3D ( 'NONE', #31167, #72527, #14551 ) ;
#44332 = ADVANCED_FACE ( 'NONE', ( #34046, #33615 ), #68592, .F. ) ;
#44333 = CARTESIAN_POINT ( 'NONE',  ( 163.0664832912739826, 25.62155284005901379, 339.0006252759110339 ) ) ;
#44334 = EDGE_CURVE ( 'NONE', #74274, #38959, #62661, .T. ) ;
#44335 = DIRECTION ( 'NONE',  ( 2.999999999999999839E-15, -1.000000000000000000, 2.999999999999999900E-30 ) ) ;
#44336 = VERTEX_POINT ( 'NONE', #48114 ) ;
#44337 = ORIENTED_EDGE ( 'NONE', *, *, #804, .F. ) ;
#44338 = CARTESIAN_POINT ( 'NONE',  ( -64.50026246089650783, 64.60000000000000853, 59.61038444174924678 ) ) ;
#44339 = ADVANCED_FACE ( 'NONE', ( #13182 ), #75849, .F. ) ;
#44340 = ORIENTED_EDGE ( 'NONE', *, *, #36349, .T. ) ;
#44341 = VERTEX_POINT ( 'NONE', #5927 ) ;
#44342 = CARTESIAN_POINT ( 'NONE',  ( 99.32274084468600961, -31.40864097607868999, 162.2911071154209708 ) ) ;
#44343 = EDGE_CURVE ( 'NONE', #42299, #36892, #78408, .T. ) ;
#44344 = LINE ( 'NONE', #63921, #14824 ) ;
#44345 = CARTESIAN_POINT ( 'NONE',  ( 117.1470005940874728, -33.86231210335883901, 145.0470538473399529 ) ) ;
#44346 = DIRECTION ( 'NONE',  ( 0.000000000000000000, 1.000000000000000000, 0.000000000000000000 ) ) ;
#44347 = DIRECTION ( 'NONE',  ( 0.000000000000000000, 0.000000000000000000, -1.000000000000000000 ) ) ;
#44348 = AXIS2_PLACEMENT_3D ( 'NONE', #64447, #78548, #71279 ) ;
#44349 = EDGE_LOOP ( 'NONE', ( #27776, #47166 ) ) ;
#44350 = EDGE_CURVE ( 'NONE', #55131, #57944, #55819, .T. ) ;
#44351 = VECTOR ( 'NONE', #20880, 1000.000000000000000 ) ;
#44352 = VECTOR ( 'NONE', #35729, 1000.000000000000000 ) ;
#44353 = VERTEX_POINT ( 'NONE', #47675 ) ;
#44354 = VERTEX_POINT ( 'NONE', #76296 ) ;
#44355 = EDGE_CURVE ( 'NONE', #3897, #42802, #13088, .T. ) ;
#44356 = CARTESIAN_POINT ( 'NONE',  ( 99.23015118009998048, -40.40270512654389279, 209.4814237029249568 ) ) ;
#44357 = CARTESIAN_POINT ( 'NONE',  ( 115.2845782536562353, -44.15631435451261666, 83.25372051400698581 ) ) ;
#44358 = ORIENTED_EDGE ( 'NONE', *, *, #59308, .T. ) ;
#44359 = CARTESIAN_POINT ( 'NONE',  ( 106.6078071710152244, -25.70885557892963647, 40.09753003781596448 ) ) ;
#44360 = CARTESIAN_POINT ( 'NONE',  ( 111.9917837115123547, -28.59708332594661684, 249.5838068554156166 ) ) ;
#44361 = DIRECTION ( 'NONE',  ( -0.000000000000000000, 1.000000000000000000, 0.000000000000000000 ) ) ;
#44362 = CARTESIAN_POINT ( 'NONE',  ( 115.9655611776390458, -32.07238166515693933, 195.2103538287998106 ) ) ;
#44363 = CARTESIAN_POINT ( 'NONE',  ( 105.3162569294398168, -48.44961499074708655, 143.4584824187689662 ) ) ;
#44364 = CARTESIAN_POINT ( 'NONE',  ( -160.2664750769284865, 101.5999999999999943, 148.0533267522753818 ) ) ;
#44365 = ORIENTED_EDGE ( 'NONE', *, *, #22960, .T. ) ;
#44366 = DIRECTION ( 'NONE',  ( -0.000000000000000000, 1.000000000000000000, 0.000000000000000000 ) ) ;
#44367 = ORIENTED_EDGE ( 'NONE', *, *, #34373, .T. ) ;
#44368 = DIRECTION ( 'NONE',  ( 0.000000000000000000, 0.000000000000000000, -1.000000000000000000 ) ) ;
#44369 = CYLINDRICAL_SURFACE ( 'NONE', #51762, 7.937500000000000000 ) ;
#44370 = AXIS2_PLACEMENT_3D ( 'NONE', #13948, #5800, #62542 ) ;
#44371 = VERTEX_POINT ( 'NONE', #41751 ) ;
#44372 = CARTESIAN_POINT ( 'NONE',  ( 82.81648064515525220, -36.72944715939136273, 6.749772901088423538 ) ) ;
#44373 = CARTESIAN_POINT ( 'NONE',  ( 48.16670390244701139, -28.27351298637280408, 237.4678068554150059 ) ) ;
#44374 = CARTESIAN_POINT ( 'NONE',  ( 110.3719962439868425, -47.27708535874812412, 52.80610146638697699 ) ) ;
#44375 = CARTESIAN_POINT ( 'NONE',  ( 22.82730048992621263, 57.73250703860936994, 30.50469867578552652 ) ) ;
#44376 = AXIS2_PLACEMENT_3D ( 'NONE', #15047, #42719, #55447 ) ;
#44377 = FACE_OUTER_BOUND ( 'NONE', #80930, .T. ) ;
#44378 = CARTESIAN_POINT ( 'NONE',  ( 116.3212776292294279, -32.94146857471271517, 75.13562527591093954 ) ) ;
#44379 = CARTESIAN_POINT ( 'NONE',  ( 97.54819157151548836, -32.61351373332768588, 61.01372051400699803 ) ) ;
#44381 = CARTESIAN_POINT ( 'NONE',  ( 102.7067583520261138, -46.86140753836539119, 133.2651490854349561 ) ) ;
#44380 = DIRECTION ( 'NONE',  ( -0.9254794337955620787, -0.3787978585227822492, 0.000000000000000000 ) ) ;
#44382 = CARTESIAN_POINT ( 'NONE',  ( 6.938893903907229955E-15, 60.82030000000000314, 216.0269999999999868 ) ) ;
#44383 = CARTESIAN_POINT ( 'NONE',  ( 41.56648329127398966, -18.82844715994071194, 78.92562527591199739 ) ) ;
#44384 = ORIENTED_EDGE ( 'NONE', *, *, #3902, .T. ) ;
#44385 = DIRECTION ( 'NONE',  ( 0.000000000000000000, 1.000000000000000000, 0.000000000000000000 ) ) ;
#44386 = DIRECTION ( 'NONE',  ( 0.000000000000000000, 0.000000000000000000, -1.000000000000000000 ) ) ;
#44387 = DIRECTION ( 'NONE',  ( -4.237773401492740281E-14, 1.000000000000000000, 0.000000000000000000 ) ) ;
#44388 = LINE ( 'NONE', #72998, #59279 ) ;
#44390 = ORIENTED_EDGE ( 'NONE', *, *, #73679, .F. ) ;
#44389 = CARTESIAN_POINT ( 'NONE',  ( 113.1812204092734220, -26.51970732500450012, 204.6470538473399756 ) ) ;
#44391 = CARTESIAN_POINT ( 'NONE',  ( 97.39140141746301538, -39.27893455387799548, 146.5314937606656258 ) ) ;
#44392 = CARTESIAN_POINT ( 'NONE',  ( 117.5124522703044931, -35.85713534702714611, 249.8927681330537780 ) ) ;
#44393 = CARTESIAN_POINT ( 'NONE',  ( 103.3469782872468130, -47.18711328981185460, 98.31657765686297523 ) ) ;
#44394 = CARTESIAN_POINT ( 'NONE',  ( 83.63178471058820662, 77.68489675156565966, 100.2530235599243440 ) ) ;
#44395 = EDGE_CURVE ( 'NONE', #68997, #61226, #69935, .T. ) ;
#44396 = DIRECTION ( 'NONE',  ( 0.000000000000000000, -1.000000000000000000, 0.000000000000000000 ) ) ;
#44397 = FACE_OUTER_BOUND ( 'NONE', #57612, .T. ) ;
#44398 = ORIENTED_EDGE ( 'NONE', *, *, #84045, .F. ) ;
#44399 = ORIENTED_EDGE ( 'NONE', *, *, #36633, .F. ) ;
#44400 = ORIENTED_EDGE ( 'NONE', *, *, #61262, .T. ) ;
#44401 = ORIENTED_EDGE ( 'NONE', *, *, #7301, .T. ) ;
#44402 = CARTESIAN_POINT ( 'NONE',  ( 72.96458098368650269, 117.4749999999999943, 72.96458098368729850 ) ) ;
#44403 = CARTESIAN_POINT ( 'NONE',  ( 115.6552720357279753, -30.75834705514724732, 275.3099109901965562 ) ) ;
#44404 = CARTESIAN_POINT ( 'NONE',  ( 163.1639762274738814, -34.03355364506054315, 342.9256252759109884 ) ) ;
#44405 = LINE ( 'NONE', #78525, #20844 ) ;
#44407 = CARTESIAN_POINT ( 'NONE',  ( 91.81719692706791136, 78.06989712577869511, 75.00102098090833636 ) ) ;
#44406 = LINE ( 'NONE', #79418, #11970 ) ;
#44408 = VECTOR ( 'NONE', #87372, 999.9999999999998863 ) ;
#44409 = CYLINDRICAL_SURFACE ( 'NONE', #86346, 2.500000000000002220 ) ;
#44410 = CARTESIAN_POINT ( 'NONE',  ( 98.86656133049426387, -40.57313681482517609, 211.0857531614099685 ) ) ;
#44411 = EDGE_LOOP ( 'NONE', ( #50516, #18987, #63019, #89543 ) ) ;
#44412 = ORIENTED_EDGE ( 'NONE', *, *, #11329, .T. ) ;
#44413 = VECTOR ( 'NONE', #59622, 1000.000000000000000 ) ;
#44414 = ORIENTED_EDGE ( 'NONE', *, *, #25390, .T. ) ;
#44415 = EDGE_CURVE ( 'NONE', #40497, #28660, #26793, .T. ) ;
#44416 = CIRCLE ( 'NONE', #70574, 11.45913725231036118 ) ;
#44417 = CIRCLE ( 'NONE', #63305, 1.000000000000000888 ) ;
#44418 = CARTESIAN_POINT ( 'NONE',  ( 36.23715912545424089, -47.82818131006125384, 300.4678068554150059 ) ) ;
#44419 = DIRECTION ( 'NONE',  ( -0.000000000000000000, 1.000000000000000000, -0.000000000000000000 ) ) ;
#44420 = CARTESIAN_POINT ( 'NONE',  ( 111.4502655538902758, -27.98611278301861560, 275.7070538473389547 ) ) ;
#44421 = CARTESIAN_POINT ( 'NONE',  ( 0.000000000000000000, 101.5999999999999943, 0.000000000000000000 ) ) ;
#44422 = FACE_BOUND ( 'NONE', #69360, .T. ) ;
#44423 = DIRECTION ( 'NONE',  ( 0.000000000000000000, 0.000000000000000000, 1.000000000000000000 ) ) ;
#44424 = PRODUCT_RELATED_PRODUCT_CATEGORY ( 'part', '', ( #87948 ) ) ;
#44425 = EDGE_LOOP ( 'NONE', ( #38600, #80301 ) ) ;
#44426 = CYLINDRICAL_SURFACE ( 'NONE', #31720, 11.45913725231036118 ) ;
#44427 = ORIENTED_EDGE ( 'NONE', *, *, #41909, .T. ) ;
#44428 = AXIS2_PLACEMENT_3D ( 'NONE', #88299, #81488, #87388 ) ;
#44429 = CARTESIAN_POINT ( 'NONE',  ( 0.000000000000000000, 101.5999999999999943, 0.000000000000000000 ) ) ;
#44430 = CARTESIAN_POINT ( 'NONE',  ( 110.8184301750971485, -28.11564833443670608, 281.1692023535160843 ) ) ;
#44431 = B_SPLINE_CURVE_WITH_KNOTS ( 'NONE', 3,
 ( #22571, #31143, #79324, #24345, #45208, #72926, #77979, #66106, #18862, #12051, #54240, #24785, #73372, #45640, #87017, #46091, #67903, #19313, #88369, #67449, #17958, #31585, #82004, #46985, #39740 ),
 .UNSPECIFIED., .F., .F.,
 ( 4, 2, 2, 2, 2, 2, 2, 2, 2, 1, 2, 2, 4 ),
 ( 2.608264963112508895E-18, 0.002483666291998854608, 0.003725499437998279744, 0.004967332583997703145, 0.007450998875996568162, 0.008692832021995991129, 0.009934665167995411494, 0.01241833145999425222, 0.01366016460599367086, 0.01490199775199309122, 0.01614383089799251159, 0.01738566404399193022, 0.01986933033599076748 ),
 .UNSPECIFIED. ) ;
#44432 = CARTESIAN_POINT ( 'NONE',  ( 163.2449138993006841, -32.11662333284040471, 237.4678068554150059 ) ) ;
#44433 = AXIS2_PLACEMENT_3D ( 'NONE', #56597, #85235, #47188 ) ;
#44434 = CARTESIAN_POINT ( 'NONE',  ( 99.48898161933328765, -117.4034471599418197, -11.78219314458159239 ) ) ;
#44435 = EDGE_CURVE ( 'NONE', #7721, #83824, #75470, .T. ) ;
#44436 = B_SPLINE_CURVE_WITH_KNOTS ( 'NONE', 3,
 ( #76194, #6705, #61652, #54825 ),
 .UNSPECIFIED., .F., .F.,
 ( 4, 4 ),
 ( 0.000000000000000000, 0.001454274669798057921 ),
 .UNSPECIFIED. ) ;
#44437 = CARTESIAN_POINT ( 'NONE',  ( 183.6524903400785718, -49.32844715993451956, 180.4678068554150343 ) ) ;
#44438 = EDGE_LOOP ( 'NONE', ( #28708, #85658, #13360, #29459 ) ) ;
#44439 = CARTESIAN_POINT ( 'NONE',  ( 97.81169962758427516, -40.51743340529665005, 76.63548575323150658 ) ) ;
#44440 = PLANE ( 'NONE',  #32413 ) ;
#44441 = EDGE_CURVE ( 'NONE', #66807, #76993, #78647, .T. ) ;
#44442 = ORIENTED_EDGE ( 'NONE', *, *, #19913, .T. ) ;
#44443 = CARTESIAN_POINT ( 'NONE',  ( 106.6603292229642790, -26.31205452386275212, 85.10705384733896040 ) ) ;
#44444 = ORIENTED_EDGE ( 'NONE', *, *, #60221, .F. ) ;
#44445 = EDGE_CURVE ( 'NONE', #38408, #62285, #49464, .T. ) ;
#44446 = CARTESIAN_POINT ( 'NONE',  ( 98.27686124684872482, -40.85414981714398408, 61.09813411379100501 ) ) ;
#44447 = CARTESIAN_POINT ( 'NONE',  ( 116.6873719206527511, -39.68605214187660124, 89.58883501578704056 ) ) ;
#44448 = CARTESIAN_POINT ( 'NONE',  ( 106.7212481586559392, -27.87455634666363835, 81.53872616303998200 ) ) ;
#44449 = CARTESIAN_POINT ( 'NONE',  ( 100.8871946602138649, -44.69999506278231394, 13.05226384497917458 ) ) ;
#44450 = ADVANCED_FACE ( 'NONE', ( #50823 ), #78993, .F. ) ;
#44451 = CYLINDRICAL_SURFACE ( 'NONE', #41601, 4.762500000000002842 ) ;
#44452 = DIRECTION ( 'NONE',  ( 1.000000000000000000, 0.000000000000000000, 0.000000000000000000 ) ) ;
#44453 = CIRCLE ( 'NONE', #5319, 1.000000000000000888 ) ;
#44454 = CARTESIAN_POINT ( 'NONE',  ( 115.9636596525004677, -42.20459941147550609, 14.38705384733995984 ) ) ;
#44455 = DIRECTION ( 'NONE',  ( -0.7071067811865414665, 0.000000000000000000, -0.7071067811865534569 ) ) ;
#44456 = ORIENTED_EDGE ( 'NONE', *, *, #12848, .F. ) ;
#44457 = CARTESIAN_POINT ( 'NONE',  ( 37.03715912545342093, -48.62818131006128652, 193.9678068554150911 ) ) ;
#44458 = ORIENTED_EDGE ( 'NONE', *, *, #64050, .F. ) ;
#44459 = CARTESIAN_POINT ( 'NONE',  ( 105.3089409210114269, -48.49860570903479129, 143.4584824187689662 ) ) ;
#44460 = LINE ( 'NONE', #78130, #36691 ) ;
#44461 = EDGE_LOOP ( 'NONE', ( #28429, #2149, #78083, #7372 ) ) ;
#44462 = ORIENTED_EDGE ( 'NONE', *, *, #29604, .F. ) ;
#44463 = EDGE_CURVE ( 'NONE', #11800, #73928, #29049, .T. ) ;
#44464 = CARTESIAN_POINT ( 'NONE',  ( 32.06670390244800473, -33.35206098992711077, -5.074374724088000832 ) ) ;
#44465 = DIRECTION ( 'NONE',  ( -0.0001211784769810537456, 0.7071067708032344745, 0.7071067811865466846 ) ) ;
#44466 = CARTESIAN_POINT ( 'NONE',  ( 97.71246005893821973, -41.20616857227592789, 216.6937205140069409 ) ) ;
#44468 = EDGE_CURVE ( 'NONE', #63506, #41573, #43992, .T. ) ;
#44467 = CYLINDRICAL_SURFACE ( 'NONE', #24021, 2.117000000000007987 ) ;
#44469 = DIRECTION ( 'NONE',  ( -4.299999999999999979E-14, 1.000000000000000000, 0.000000000000000000 ) ) ;
#44470 = CARTESIAN_POINT ( 'NONE',  ( 172.5664832912729878, -27.57844715994070484, 315.9256252759120116 ) ) ;
#44471 = CARTESIAN_POINT ( 'NONE',  ( 96.34427168469159142, -39.41376207380771746, 12.53372051400597442 ) ) ;
#44472 = CARTESIAN_POINT ( 'NONE',  ( -7.937500000000730083, 120.6499999999999915, 103.1875000000000000 ) ) ;
#44473 = ORIENTED_EDGE ( 'NONE', *, *, #51566, .F. ) ;
#44474 = CARTESIAN_POINT ( 'NONE',  ( 103.2778153200627713, -27.47493501435859642, 171.3856854448868887 ) ) ;
#44475 = VECTOR ( 'NONE', #61008, 1000.000000000000000 ) ;
#44476 = DIRECTION ( 'NONE',  ( 0.000000000000000000, 0.000000000000000000, -1.000000000000000000 ) ) ;
#44477 = ORIENTED_EDGE ( 'NONE', *, *, #28661, .F. ) ;
#44478 = VECTOR ( 'NONE', #86541, 1000.000000000000000 ) ;
#44479 = CARTESIAN_POINT ( 'NONE',  ( 34.92499999999999716, 77.96728223830730542, 294.9574999999999818 ) ) ;
#44480 = VECTOR ( 'NONE', #41865, 1000.000000000000000 ) ;
#44481 = LINE ( 'NONE', #37692, #39673 ) ;
#44482 = CARTESIAN_POINT ( 'NONE',  ( 97.19046783542276557, -39.99946004141662570, 241.5813395616249863 ) ) ;
#44483 = FACE_OUTER_BOUND ( 'NONE', #88586, .T. ) ;
#44484 = AXIS2_PLACEMENT_3D ( 'NONE', #51153, #30281, #70730 ) ;
#44485 = PLANE ( 'NONE',  #85463 ) ;
#44486 = CARTESIAN_POINT ( 'NONE',  ( 29.56648329127298069, -71.37844715994266664, 361.9756252759109998 ) ) ;
#44487 = CARTESIAN_POINT ( 'NONE',  ( 116.6718245901296171, -38.14650263757180682, 223.1324198280769622 ) ) ;
#44489 = CARTESIAN_POINT ( 'NONE',  ( 117.4658636684176543, -37.01502254527064650, 39.80419670448193159 ) ) ;
#44488 = DIRECTION ( 'NONE',  ( 1.000000000000000000, 0.000000000000000000, 0.000000000000000000 ) ) ;
#44490 = CARTESIAN_POINT ( 'NONE',  ( 116.8422689635382454, 73.23116755977939363, 58.25111782077112110 ) ) ;
#44491 = CARTESIAN_POINT ( 'NONE',  ( 117.0754465142714054, -30.29129860725820222, 144.2813395616249750 ) ) ;
#44492 = VERTEX_POINT ( 'NONE', #9493 ) ;
#44493 = CARTESIAN_POINT ( 'NONE',  ( 180.2143765759491885, -35.91149509761089575, 342.9256252759109884 ) ) ;
#44494 = ORIENTED_EDGE ( 'NONE', *, *, #28687, .F. ) ;
#44495 = CARTESIAN_POINT ( 'NONE',  ( 173.9900000000000091, 20.32000000000000028, -71.37400000000000944 ) ) ;
#44496 = CARTESIAN_POINT ( 'NONE',  ( 100.9546727804262076, -28.70702575035819848, 66.59395861228354363 ) ) ;
#44497 = CARTESIAN_POINT ( 'NONE',  ( 107.9134757390494030, -26.74391507959751735, 276.0090606567454188 ) ) ;
#44498 = ORIENTED_EDGE ( 'NONE', *, *, #45114, .T. ) ;
#44499 = DIRECTION ( 'NONE',  ( 0.000000000000000000, 0.000000000000000000, 1.000000000000000000 ) ) ;
#44500 = VERTEX_POINT ( 'NONE', #30829 ) ;
#44501 = CARTESIAN_POINT ( 'NONE',  ( 38.10000000000000142, 82.54999999999999716, 290.4490000000000123 ) ) ;
#44502 = CARTESIAN_POINT ( 'NONE',  ( 41.56648329127499153, -36.32844715994070839, 258.9256252759120116 ) ) ;
#44503 = AXIS2_PLACEMENT_3D ( 'NONE', #40467, #29533, #2728 ) ;
#44504 = EDGE_CURVE ( 'NONE', #74932, #11728, #15872, .T. ) ;
#44505 = CARTESIAN_POINT ( 'NONE',  ( 41.56648329127399677, 0.2215528400590013880, 78.92562527591199739 ) ) ;
#44506 = VERTEX_POINT ( 'NONE', #44439 ) ;
#44507 = CARTESIAN_POINT ( 'NONE',  ( 113.5198117145332475, -28.51355303769357619, 79.54705384733995288 ) ) ;
#44509 = ADVANCED_FACE ( 'NONE', ( #86246 ), #72172, .F. ) ;
#44508 = CARTESIAN_POINT ( 'NONE',  ( 142.0664832912740394, -45.72944715994099596, -4.824374724088994704 ) ) ;
#44510 = CARTESIAN_POINT ( 'NONE',  ( 4.163101094985349692E-14, 120.6499999999999915, -107.7702177616926065 ) ) ;
#44511 = CARTESIAN_POINT ( 'NONE',  ( 33.91903122894598965, -35.91149509761181235, 313.9678068554150059 ) ) ;
#44512 = ORIENTED_EDGE ( 'NONE', *, *, #9737, .F. ) ;
#44513 = CARTESIAN_POINT ( 'NONE',  ( 0.000000000000000000, 82.54999999999999716, 89.46299999999996544 ) ) ;
#44514 = PLANE ( 'NONE',  #81748 ) ;
#44515 = DIRECTION ( 'NONE',  ( 0.000000000000000000, 0.000000000000000000, 1.000000000000000000 ) ) ;
#44517 = DIRECTION ( 'NONE',  ( 0.000000000000000000, 1.000000000000000000, 0.000000000000000000 ) ) ;
#44516 = DIRECTION ( 'NONE',  ( 0.000000000000000000, -1.000000000000000000, 0.000000000000000000 ) ) ;
#44518 = DIRECTION ( 'NONE',  ( 0.000000000000000000, 0.000000000000000000, -1.000000000000000000 ) ) ;
#44519 = CIRCLE ( 'NONE', #63415, 2.500000000000002220 ) ;
#44520 = VERTEX_POINT ( 'NONE', #43547 ) ;
#44521 = EDGE_CURVE ( 'NONE', #62133, #34136, #24027, .T. ) ;
#44522 = FACE_OUTER_BOUND ( 'NONE', #32397, .T. ) ;
#44523 = CARTESIAN_POINT ( 'NONE',  ( 96.73459541816653484, -35.84013382243349355, 182.2461014663859658 ) ) ;
#44525 = VERTEX_POINT ( 'NONE', #84480 ) ;
#44524 = DIRECTION ( 'NONE',  ( -4.093947403305260305E-16, 1.000000000000000000, -6.162975822039159109E-32 ) ) ;
#44526 = CARTESIAN_POINT ( 'NONE',  ( 115.0831197249979851, -29.02584261466837390, 35.43562527591098643 ) ) ;
#44527 = LINE ( 'NONE', #81664, #84670 ) ;
#44528 = CYLINDRICAL_SURFACE ( 'NONE', #34246, 2.116999999999993776 ) ;
#44529 = DIRECTION ( 'NONE',  ( 0.000000000000000000, 1.000000000000000000, 0.000000000000000000 ) ) ;
#44530 = ADVANCED_FACE ( 'NONE', ( #85820 ), #22243, .T. ) ;
#44531 = ORIENTED_EDGE ( 'NONE', *, *, #57440, .T. ) ;
#44532 = CARTESIAN_POINT ( 'NONE',  ( 107.0664832912739968, -36.72944715994100306, 287.6356252759109680 ) ) ;
#44533 = CIRCLE ( 'NONE', #67764, 3.174999999999983391 ) ;
#44534 = AXIS2_PLACEMENT_3D ( 'NONE', #19459, #61233, #76212 ) ;
#44535 = CARTESIAN_POINT ( 'NONE',  ( 101.0525363619397012, -44.44280425155412217, 232.0499109901969632 ) ) ;
#44536 = ORIENTED_EDGE ( 'NONE', *, *, #52438, .T. ) ;
#44537 = EDGE_LOOP ( 'NONE', ( #41514, #6053, #69540, #13932 ) ) ;
#44538 = CARTESIAN_POINT ( 'NONE',  ( 115.5682375124590635, -39.22913789569613385, 180.0301547344689936 ) ) ;
#44539 = FACE_OUTER_BOUND ( 'NONE', #22666, .T. ) ;
#44540 = AXIS2_PLACEMENT_3D ( 'NONE', #7708, #49015, #443 ) ;
#44541 = CARTESIAN_POINT ( 'NONE',  ( 116.9829645355111154, -34.95910688594825189, 45.39872616303996722 ) ) ;
#44542 = CARTESIAN_POINT ( 'NONE',  ( -100.7940789023221697, 84.21348395916260188, 82.97845804870382835 ) ) ;
#44543 = DIRECTION ( 'NONE',  ( -1.000000000000000000, -1.561055996379579722E-16, 0.000000000000000000 ) ) ;
#44544 = CARTESIAN_POINT ( 'NONE',  ( 33.91903122894489542, -35.91149509761202552, 117.4678068554150485 ) ) ;
#44545 = ORIENTED_EDGE ( 'NONE', *, *, #41558, .F. ) ;
#44546 = DIRECTION ( 'NONE',  ( -1.000000000000000000, -2.756263715554006823E-15, 0.000000000000000000 ) ) ;
#44547 = DIRECTION ( 'NONE',  ( 0.000000000000000000, 0.000000000000000000, 1.000000000000000000 ) ) ;
#44548 = ORIENTED_EDGE ( 'NONE', *, *, #34321, .T. ) ;
#44549 = CARTESIAN_POINT ( 'NONE',  ( 96.79764630557882299, -40.75620882907056597, 246.6118157521009664 ) ) ;
#44550 = CARTESIAN_POINT ( 'NONE',  ( 5.630981057377994148, 93.96377546238062450, 118.4246973091026973 ) ) ;
#44552 = EDGE_LOOP ( 'NONE', ( #71999, #7281, #85749, #79065, #70956, #954 ) ) ;
#44551 = EDGE_CURVE ( 'NONE', #78013, #56843, #9946, .T. ) ;
#44553 = AXIS2_PLACEMENT_3D ( 'NONE', #14000, #48939, #47604 ) ;
#44554 = DIRECTION ( 'NONE',  ( 3.491483361109385222E-15, 0.000000000000000000, -1.000000000000000000 ) ) ;
#44555 = DIRECTION ( 'NONE',  ( 0.000000000000000000, 0.000000000000000000, 1.000000000000000000 ) ) ;
#44556 = DIRECTION ( 'NONE',  ( -0.3535533905932746190, 0.6123724356958156756, 0.7071067811865288100 ) ) ;
#44557 = AXIS2_PLACEMENT_3D ( 'NONE', #55586, #13841, #26132 ) ;
#44558 = CARTESIAN_POINT ( 'NONE',  ( 107.0664832912739968, -0.7548456658612000547, 331.7756252759120343 ) ) ;
#44559 = VECTOR ( 'NONE', #40354, 1000.000000000000000 ) ;
#44560 = CARTESIAN_POINT ( 'NONE',  ( 112.5987260342904648, -28.66361022110277545, 40.59848241876795782 ) ) ;
#44561 = DIRECTION ( 'NONE',  ( 0.000000000000000000, -1.000000000000000000, 0.000000000000000000 ) ) ;
#44562 = AXIS2_PLACEMENT_3D ( 'NONE', #32369, #47339, #26911 ) ;
#44563 = ORIENTED_EDGE ( 'NONE', *, *, #88478, .T. ) ;
#44564 = CARTESIAN_POINT ( 'NONE',  ( 105.4141053104174830, -47.06688527371949249, 33.44991099019695469 ) ) ;
#44565 = LINE ( 'NONE', #1917, #7696 ) ;
#44566 = CARTESIAN_POINT ( 'NONE',  ( 113.7561043996362287, -29.08408549058404091, 289.5032443235301116 ) ) ;
#44567 = EDGE_LOOP ( 'NONE', ( #13065, #6565, #4721, #46774 ) ) ;
#44568 = ADVANCED_BREP_SHAPE_REPRESENTATION ( '', ( #80246, #50656 ), #14432 ) ;
#44569 = EDGE_CURVE ( 'NONE', #4499, #85158, #1346, .T. ) ;
#44570 = LINE ( 'NONE', #39104, #84002 ) ;
#44571 = B_SPLINE_CURVE_WITH_KNOTS ( 'NONE', 3,
 ( #63271, #50074, #83724, #77809, #63725, #41911, #49173, #43711, #57337, #56440, #15127, #1507, #62811, #588, #8772, #64179, #71449, #36474, #42805, #55981, #8315, #1951, #21503, #14687, #84185, #36014, #42356, #21959, #56894, #7856, #29645, #9214, #62366, #149, #21045 ),
 .UNSPECIFIED., .F., .F.,
 ( 4, 2, 2, 1, 1, 1, 2, 2, 2, 1, 1, 2, 2, 2, 2, 1, 1, 2, 2, 2, 4 ),
 ( 0.000000000000000000, 0.06250000000034182379, 0.09375000000052836902, 0.1093750000006312451, 0.1171875000006843554, 0.1210937500007093492, 0.1230468750007258083, 0.1250000000007422951, 0.1875000000008925083, 0.2187500000009702517, 0.2343750000009904300, 0.2421875000010005330, 0.2500000000010105805, 0.3750000000010189627, 0.4375000000010146883, 0.4687500000010152434, 0.4843750000010160761, 0.4921875000010164647, 0.5000000000010168533, 0.7500000000005084821, 1.000000000000000000 ),
 .UNSPECIFIED. ) ;
#44573 = ADVANCED_FACE ( 'NONE', ( #23587, #49913 ), #51250, .T. ) ;
#44572 = CARTESIAN_POINT ( 'NONE',  ( 59.67079009362632291, -0.9310397146383333489, 540.9756252759101471 ) ) ;
#44574 = CARTESIAN_POINT ( 'NONE',  ( 70.63919639214310564, 65.60000000000000853, -53.97512327982435210 ) ) ;
#44575 = CARTESIAN_POINT ( 'NONE',  ( 115.1095529034481331, -33.53414494269306800, 96.95761417911496949 ) ) ;
#44576 = CARTESIAN_POINT ( 'NONE',  ( 113.0346028865331363, -45.34691455509256031, 199.0584824187679374 ) ) ;
#44577 = CARTESIAN_POINT ( 'NONE',  ( -72.96458098368751166, 127.0000000000000000, 80.10833098368618721 ) ) ;
#44578 = DIRECTION ( 'NONE',  ( 0.000000000000000000, 0.000000000000000000, -1.000000000000000000 ) ) ;
#44579 = ORIENTED_EDGE ( 'NONE', *, *, #48870, .F. ) ;
#44580 = DIRECTION ( 'NONE',  ( 0.000000000000000000, 0.000000000000000000, -1.000000000000000000 ) ) ;
#44581 = EDGE_LOOP ( 'NONE', ( #9519, #25752, #43535, #14903, #13658, #39837, #38216, #14026 ) ) ;
#44583 = EDGE_LOOP ( 'NONE', ( #45347, #34648, #52629, #3439, #71704, #82561, #24884, #78562, #48158, #85762 ) ) ;
#44582 = VECTOR ( 'NONE', #84433, 1000.000000000000000 ) ;
#44584 = DIRECTION ( 'NONE',  ( 1.000000000000000000, 6.145690160522439356E-16, 0.000000000000000000 ) ) ;
#44585 = ORIENTED_EDGE ( 'NONE', *, *, #77186, .T. ) ;
#44586 = ORIENTED_EDGE ( 'NONE', *, *, #63680, .F. ) ;
#44587 = CARTESIAN_POINT ( 'NONE',  ( 116.0733447696779592, -32.33582790950384833, 40.18770276530661079 ) ) ;
#44588 = CARTESIAN_POINT ( 'NONE',  ( 115.6810990589499397, -33.93640840262257541, 133.5105150661719620 ) ) ;
#44589 = CARTESIAN_POINT ( 'NONE',  ( 100.3828542815028015, -28.67117381486349004, 40.62705384733894221 ) ) ;
#44590 = CARTESIAN_POINT ( 'NONE',  ( -0.8398470015645936870, 69.84999999999999432, 130.5559999999999832 ) ) ;
#44591 = ORIENTED_EDGE ( 'NONE', *, *, #14435, .F. ) ;
#44592 = DIRECTION ( 'NONE',  ( 0.000000000000000000, 1.000000000000000000, 0.000000000000000000 ) ) ;
#44593 = ORIENTED_EDGE ( 'NONE', *, *, #22455, .F. ) ;
#44594 = DIRECTION ( 'NONE',  ( 1.000000000000000078E-15, -1.000000000000000000, 0.000000000000000000 ) ) ;
#44595 = AXIS2_PLACEMENT_3D ( 'NONE', #7748, #13665, #55422 ) ;
#44596 = CARTESIAN_POINT ( 'NONE',  ( 1.793207055312195196E-22, 69.95000000000000284, 118.5560000000000116 ) ) ;
#44597 = CARTESIAN_POINT ( 'NONE',  ( -107.7702177616926065, 120.6499999999999915, -1.170464777364108012E-12 ) ) ;
#44599 = CARTESIAN_POINT ( 'NONE',  ( 182.0667039024478981, -33.35206098992058799, 193.9678068554150059 ) ) ;
#44598 = VECTOR ( 'NONE', #49883, 1000.000000000000000 ) ;
#44600 = ORIENTED_EDGE ( 'NONE', *, *, #12060, .F. ) ;
#44601 = APPLICATION_CONTEXT ( 'automotive_design' ) ;
#44602 = CIRCLE ( 'NONE', #46086, 2.517500000000005844 ) ;
#44603 = CARTESIAN_POINT ( 'NONE',  ( 100.1386363970297992, -44.51995214173314963, 266.9984824187679919 ) ) ;
#44604 = CARTESIAN_POINT ( 'NONE',  ( 105.3131098409624542, -26.40875552125079295, 11.20991099019697046 ) ) ;
#44605 = SURFACE_STYLE_USAGE ( .BOTH. , #59128 ) ;
#44606 = CARTESIAN_POINT ( 'NONE',  ( 188.5667039024479834, -58.35344715994099829, 137.2178068554150059 ) ) ;
#44609 = EDGE_CURVE ( 'NONE', #54188, #5456, #16759, .T. ) ;
#44608 = CARTESIAN_POINT ( 'NONE',  ( 68.75114609266175592, -139.2473167355539374, 246.2273013858858803 ) ) ;
#44607 = DIRECTION ( 'NONE',  ( -1.000000000000000000, -6.814610998690690172E-14, -1.000000000000000078E-15 ) ) ;
#44610 = CARTESIAN_POINT ( 'NONE',  ( 106.5177191205505665, -25.28303833615382601, 323.5373862996826233 ) ) ;
#44611 = CARTESIAN_POINT ( 'NONE',  ( 156.5667039024485518, -48.82844715993568485, 173.2178068554149775 ) ) ;
#44612 = FACE_OUTER_BOUND ( 'NONE', #43057, .T. ) ;
#44613 = CARTESIAN_POINT ( 'NONE',  ( 107.3428450438784694, -25.27364292152175551, 322.4523926293242653 ) ) ;
#44614 = CARTESIAN_POINT ( 'NONE',  ( 147.0667039024469886, -67.87844715994090450, 247.2178068554179902 ) ) ;
#44615 = AXIS2_PLACEMENT_3D ( 'NONE', #8659, #1843, #36357 ) ;
#44616 = DIRECTION ( 'NONE',  ( 1.000000000000000000, 2.999999999999999839E-15, 1.000000000000000078E-15 ) ) ;
#44617 = CARTESIAN_POINT ( 'NONE',  ( 162.5667039024470171, -32.29483332968611364, -5.074374724088000832 ) ) ;
#44618 = CARTESIAN_POINT ( 'NONE',  ( 96.51457183773001702, -40.09881715592517537, 281.5603871806727625 ) ) ;
#44619 = CARTESIAN_POINT ( 'NONE',  ( 117.2915085808104436, -34.52259632565112213, 179.9956252759109532 ) ) ;
#44620 = CARTESIAN_POINT ( 'NONE',  ( 97.26802889450139844, -33.10625101732204456, 62.04419670448196911 ) ) ;
#44621 = VECTOR ( 'NONE', #26905, 1000.000000000000000 ) ;
#44623 = DIRECTION ( 'NONE',  ( 0.000000000000000000, 0.000000000000000000, -1.000000000000000000 ) ) ;
#44622 = CARTESIAN_POINT ( 'NONE',  ( 41.56648329127499153, -36.32844715994070839, 198.9256252759119832 ) ) ;
#44624 = DIRECTION ( 'NONE',  ( -1.000000000000000000, -4.299999999999999979E-14, -1.000000000000000078E-15 ) ) ;
#44625 = AXIS2_PLACEMENT_3D ( 'NONE', #59834, #87566, #25326 ) ;
#44626 = ADVANCED_FACE ( 'NONE', ( #15429 ), #63561, .F. ) ;
#44627 = VERTEX_POINT ( 'NONE', #57632 ) ;
#44628 = EDGE_CURVE ( 'NONE', #54402, #24467, #27671, .T. ) ;
#44629 = CARTESIAN_POINT ( 'NONE',  ( 0.000000000000000000, 111.1250000000000000, 0.000000000000000000 ) ) ;
#44630 = ORIENTED_EDGE ( 'NONE', *, *, #3745, .T. ) ;
#44631 = CARTESIAN_POINT ( 'NONE',  ( 101.3216544293210291, -28.81361639883588310, 71.57562527591099411 ) ) ;
#44632 = ADVANCED_FACE ( 'NONE', ( #3129 ), #64019, .T. ) ;
#44634 = ORIENTED_EDGE ( 'NONE', *, *, #51902, .F. ) ;
#44633 = CARTESIAN_POINT ( 'NONE',  ( 5.565016159906887694, 93.97330845465467064, 130.4378072086274756 ) ) ;
#44635 = CARTESIAN_POINT ( 'NONE',  ( 0.000000000000000000, 1.270000000000000018, 0.000000000000000000 ) ) ;
#44636 = CARTESIAN_POINT ( 'NONE',  ( 116.3579325164319016, -41.40893824611048757, 199.4556252759109611 ) ) ;
#44637 = CARTESIAN_POINT ( 'NONE',  ( -100.8961411191535973, 120.6499999999999915, 3.968749999998880451 ) ) ;
#44638 = CARTESIAN_POINT ( 'NONE',  ( 29.56670390244797630, -67.87844715994100397, 300.9178068554150514 ) ) ;
#44639 = CARTESIAN_POINT ( 'NONE',  ( 134.0664832912740110, 0.2215528400590013880, 4.925625275911999168 ) ) ;
#44640 = CARTESIAN_POINT ( 'NONE',  ( 108.0345654683053453, -121.2196520243554403, -19.23816181211449106 ) ) ;
#44641 = EDGE_CURVE ( 'NONE', #48031, #26236, #73045, .T. ) ;
#44642 = EDGE_CURVE ( 'NONE', #36469, #27929, #32601, .T. ) ;
#44643 = CARTESIAN_POINT ( 'NONE',  ( 188.5667039024479834, -62.87844715994099687, 293.2178068554150627 ) ) ;
#44644 = CARTESIAN_POINT ( 'NONE',  ( 97.83898487876174954, -40.58353653247343829, 96.64131800056416921 ) ) ;
#44645 = CARTESIAN_POINT ( 'NONE',  ( 98.32242264099468798, -42.30440888850458947, 141.7661014663879655 ) ) ;
#44646 = ORIENTED_EDGE ( 'NONE', *, *, #74819, .T. ) ;
#44647 = VERTEX_POINT ( 'NONE', #72620 ) ;
#44648 = AXIS2_PLACEMENT_3D ( 'NONE', #8185, #35878, #57664 ) ;
#44649 = EDGE_CURVE ( 'NONE', #44152, #61107, #58073, .T. ) ;
#44650 = CARTESIAN_POINT ( 'NONE',  ( 113.9519893150074239, -42.30780582616069552, 84.71586902018296428 ) ) ;
#44651 = ADVANCED_FACE ( 'NONE', ( #39425 ), #18528, .F. ) ;
#44652 = FACE_OUTER_BOUND ( 'NONE', #53492, .T. ) ;
#44654 = CYLINDRICAL_SURFACE ( 'NONE', #15794, 5.599999999999994316 ) ;
#44653 = CARTESIAN_POINT ( 'NONE',  ( 97.78144721833434971, -39.80378292816723018, 237.5813395616249579 ) ) ;
#44655 = PLANE ( 'NONE',  #31887 ) ;
#44656 = ADVANCED_FACE ( 'NONE', ( #24911 ), #46215, .T. ) ;
#44657 = CARTESIAN_POINT ( 'NONE',  ( 47.62500000000000000, 69.84999999999999432, 292.1000000000000227 ) ) ;
#44658 = CARTESIAN_POINT ( 'NONE',  ( 118.4241986436612279, 71.14137858619481847, 5.641441481139795044 ) ) ;
#44659 = CARTESIAN_POINT ( 'NONE',  ( -10.78744120855129118, 75.83493809012784936, 118.0644293552432345 ) ) ;
#44660 = CARTESIAN_POINT ( 'NONE',  ( -215.9000000000000057, 101.5999999999999943, 146.9389999999999930 ) ) ;
#44661 = CARTESIAN_POINT ( 'NONE',  ( 6.299530400837946686, 71.63002361900261405, 118.3890773279586170 ) ) ;
#44662 = CARTESIAN_POINT ( 'NONE',  ( 113.6008039948045933, -28.63430547549723570, 164.5356252759109736 ) ) ;
#44663 = ORIENTED_EDGE ( 'NONE', *, *, #11337, .T. ) ;
#44665 = ORIENTED_EDGE ( 'NONE', *, *, #3028, .F. ) ;
#44664 = EDGE_CURVE ( 'NONE', #78126, #14672, #85720, .T. ) ;
#44666 = CARTESIAN_POINT ( 'NONE',  ( -44.45000000000000284, 114.2999999999999972, 206.3750000000000000 ) ) ;
#44667 = CARTESIAN_POINT ( 'NONE',  ( 146.4037250783899822, -68.51735678003049657, 246.9840931576174796 ) ) ;
#44668 = CIRCLE ( 'NONE', #18541, 50.79999999999999716 ) ;
#44669 = FACE_OUTER_BOUND ( 'NONE', #27484, .T. ) ;
#44670 = FACE_BOUND ( 'NONE', #22006, .T. ) ;
#44671 = AXIS2_PLACEMENT_3D ( 'NONE', #4879, #73459, #34696 ) ;
#44672 = AXIS2_PLACEMENT_3D ( 'NONE', #37263, #87203, #65843 ) ;
#44673 = FACE_OUTER_BOUND ( 'NONE', #59198, .T. ) ;
#44674 = CARTESIAN_POINT ( 'NONE',  ( 112.7802237386950992, -45.44955040250216172, 178.0384824187679556 ) ) ;
#44675 = DIRECTION ( 'NONE',  ( 1.000000000000000000, 0.000000000000000000, 0.000000000000000000 ) ) ;
#44676 = ORIENTED_EDGE ( 'NONE', *, *, #40793, .T. ) ;
#44678 = ORIENTED_EDGE ( 'NONE', *, *, #22576, .F. ) ;
#44677 = ORIENTED_EDGE ( 'NONE', *, *, #35543, .F. ) ;
#44679 = EDGE_CURVE ( 'NONE', #59746, #63259, #73952, .T. ) ;
#44680 = CIRCLE ( 'NONE', #46161, 87.89999999999994884 ) ;
#44681 = CARTESIAN_POINT ( 'NONE',  ( 116.2822504412707474, -40.65736861940501257, 64.50652713745955680 ) ) ;
#44683 = EDGE_CURVE ( 'NONE', #39224, #57751, #4012, .T. ) ;
#44682 = LINE ( 'NONE', #2482, #65243 ) ;
#44684 = CARTESIAN_POINT ( 'NONE',  ( 120.2221484686747317, -111.8737466215625602, -11.78219314458178779 ) ) ;
#44685 = EDGE_CURVE ( 'NONE', #34522, #65168, #60755, .T. ) ;
#44686 = CARTESIAN_POINT ( 'NONE',  ( 111.0839405624553251, -29.06298261359865975, 12.49856656006798161 ) ) ;
#44687 = VECTOR ( 'NONE', #89193, 1000.000000000000000 ) ;
#44688 = DIRECTION ( 'NONE',  ( 1.000000000000000078E-15, -1.000000000000000000, 0.000000000000000000 ) ) ;
#44689 = ORIENTED_EDGE ( 'NONE', *, *, #87422, .T. ) ;
#44690 = EDGE_CURVE ( 'NONE', #46794, #50049, #17650, .T. ) ;
#44691 = AXIS2_PLACEMENT_3D ( 'NONE', #44051, #77705, #71786 ) ;
#44692 = CARTESIAN_POINT ( 'NONE',  ( 114.0862517022053026, -42.18719852450433194, 9.635625275910939536 ) ) ;
#44693 = CARTESIAN_POINT ( 'NONE',  ( 147.0667039024470171, -79.67844715994090166, 55.21780685541800437 ) ) ;
#44694 = EDGE_LOOP ( 'NONE', ( #4251, #30443, #62974, #38771 ) ) ;
#44695 = ORIENTED_EDGE ( 'NONE', *, *, #62088, .T. ) ;
#44696 = CARTESIAN_POINT ( 'NONE',  ( 98.54785696274898044, -41.97731333288708555, 111.7658622444392194 ) ) ;
#44697 = ORIENTED_EDGE ( 'NONE', *, *, #20741, .T. ) ;
#44698 = VERTEX_POINT ( 'NONE', #88490 ) ;
#44699 = AXIS2_PLACEMENT_3D ( 'NONE', #6390, #55412, #76781 ) ;
#44700 = CARTESIAN_POINT ( 'NONE',  ( 111.2570682682515439, -29.25341213619239156, 34.09241982807698434 ) ) ;
#44701 = CARTESIAN_POINT ( 'NONE',  ( 99.99311136543857970, -27.18998042936580362, 185.5841967044829630 ) ) ;
#44702 = CARTESIAN_POINT ( 'NONE',  ( 108.0049669398584911, -26.36739623290726442, 155.0041967044819557 ) ) ;
#44703 = CARTESIAN_POINT ( 'NONE',  ( 41.56648329127499153, -36.32844715994070839, 23.67562527591200094 ) ) ;
#44704 = CARTESIAN_POINT ( 'NONE',  ( 115.7761331719916171, -31.00018137778016936, 250.2899109901966028 ) ) ;
#44705 = DIRECTION ( 'NONE',  ( 1.000000000000000078E-15, -1.000000000000000000, 0.000000000000000000 ) ) ;
#44706 = CARTESIAN_POINT ( 'NONE',  ( 72.18555876632754575, -117.2313175559279728, 248.3919653347779786 ) ) ;
#44707 = CARTESIAN_POINT ( 'NONE',  ( -130.0261942349058586, 77.68489670259145896, -11.75299076262979447 ) ) ;
#44708 = VERTEX_POINT ( 'NONE', #25799 ) ;
#44709 = ORIENTED_EDGE ( 'NONE', *, *, #17626, .F. ) ;
#44710 = VECTOR ( 'NONE', #39088, 1000.000000000000000 ) ;
#44711 = AXIS2_PLACEMENT_3D ( 'NONE', #67154, #86276, #79477 ) ;
#44712 = CARTESIAN_POINT ( 'NONE',  ( 98.22399452165288380, -42.33453934503185678, 186.7756252759109543 ) ) ;
#44713 = ORIENTED_EDGE ( 'NONE', *, *, #75022, .T. ) ;
#44714 = CARTESIAN_POINT ( 'NONE',  ( 116.8067323440835565, -43.47985705614018315, 163.3441967044829823 ) ) ;
#44715 = CARTESIAN_POINT ( 'NONE',  ( 182.3467384525655746, -29.62846900981658393, 237.4678068554150059 ) ) ;
#44716 = LINE ( 'NONE', #17910, #81236 ) ;
#44717 = CARTESIAN_POINT ( 'NONE',  ( 143.3136118988180954, -139.1558145886066882, 247.4862956150515743 ) ) ;
#44720 = CARTESIAN_POINT ( 'NONE',  ( 115.5963437193832277, -42.63132022635295471, 9.356577656862985037 ) ) ;
#44719 = DIRECTION ( 'NONE',  ( 0.000000000000000000, 1.000000000000000000, 0.000000000000000000 ) ) ;
#44718 = DIRECTION ( 'NONE',  ( -1.000000000000000078E-15, 0.000000000000000000, 1.000000000000000000 ) ) ;
#44721 = FACE_OUTER_BOUND ( 'NONE', #39278, .T. ) ;
#44722 = PLANE ( 'NONE',  #75747 ) ;
#44723 = DIRECTION ( 'NONE',  ( -3.491483361109385222E-15, 0.000000000000000000, 1.000000000000000000 ) ) ;
#44724 = CARTESIAN_POINT ( 'NONE',  ( 67.55791682848843038, -137.3945666130911150, 246.8203320373089582 ) ) ;
#44725 = CARTESIAN_POINT ( 'NONE',  ( 128.7748166246070127, 12.92155284005802685, 335.5992267699912190 ) ) ;
#44726 = DIRECTION ( 'NONE',  ( 0.000000000000000000, 0.000000000000000000, -1.000000000000000000 ) ) ;
#44728 = ORIENTED_EDGE ( 'NONE', *, *, #50519, .F. ) ;
#44727 = CARTESIAN_POINT ( 'NONE',  ( 115.3744406058151384, -34.23201694794762062, 195.5838068554167535 ) ) ;
#44729 = CIRCLE ( 'NONE', #73788, 10.00000000000000711 ) ;
#44730 = CARTESIAN_POINT ( 'NONE',  ( 136.1600792930010471, -20.51483178662487816, 7.477467810847014285 ) ) ;
#44731 = CARTESIAN_POINT ( 'NONE',  ( 95.38311866650811055, -38.85853310224461410, 201.4699109901969791 ) ) ;
#44732 = CARTESIAN_POINT ( 'NONE',  ( 101.1410050838726846, -27.39870825576502966, 61.51467289495899138 ) ) ;
#44733 = CARTESIAN_POINT ( 'NONE',  ( 113.0503328260151079, -46.07776482166018184, 214.0175300378159591 ) ) ;
#44734 = DIRECTION ( 'NONE',  ( -0.7071067811892205457, 0.7071067811838745998, -7.071067811891901187E-16 ) ) ;
#44735 = CARTESIAN_POINT ( 'NONE',  ( 1.387778780781445676E-14, 239.0000000000000000, 97.27542076772557778 ) ) ;
#44737 = CARTESIAN_POINT ( 'NONE',  ( 97.81298107105155282, -40.52058258403540236, 37.63560581694255802 ) ) ;
#44736 = DIRECTION ( 'NONE',  ( 0.000000000000000000, 0.000000000000000000, 1.000000000000000000 ) ) ;
#44738 = CARTESIAN_POINT ( 'NONE',  ( -187.8075999999999794, 20.32000000000000028, -9.525000000000000355 ) ) ;
#44739 = FACE_OUTER_BOUND ( 'NONE', #12529, .T. ) ;
#44740 = ORIENTED_EDGE ( 'NONE', *, *, #3664, .F. ) ;
#44741 = CARTESIAN_POINT ( 'NONE',  ( 102.0683761184610603, -27.96971721533909161, 65.49117886461755234 ) ) ;
#44742 = VECTOR ( 'NONE', #13598, 1000.000000000000000 ) ;
#44743 = AXIS2_PLACEMENT_3D ( 'NONE', #67245, #53592, #66346 ) ;
#44744 = EDGE_CURVE ( 'NONE', #50014, #71626, #81239, .T. ) ;
#44745 = VERTEX_POINT ( 'NONE', #65781 ) ;
#44746 = EDGE_CURVE ( 'NONE', #16504, #67149, #37789, .T. ) ;
#44747 = ORIENTED_EDGE ( 'NONE', *, *, #42507, .T. ) ;
#44748 = CARTESIAN_POINT ( 'NONE',  ( 111.7654875973913278, -45.22591620450738503, 102.4009912566479557 ) ) ;
#44750 = EDGE_CURVE ( 'NONE', #54515, #42076, #88035, .T. ) ;
#44749 = VECTOR ( 'NONE', #54484, 1000.000000000000000 ) ;
#44752 = ORIENTED_EDGE ( 'NONE', *, *, #533, .F. ) ;
#44751 = DIRECTION ( 'NONE',  ( 0.7071067811868657627, 0.7071067811862293828, 7.071067811868962098E-16 ) ) ;
#44753 = CARTESIAN_POINT ( 'NONE',  ( 101.5125196766230857, -27.93273449574876111, 106.5241967044819944 ) ) ;
#44754 = DIRECTION ( 'NONE',  ( 3.999999999999999995E-14, -1.000000000000000000, 4.100000000000000342E-29 ) ) ;
#44755 = CIRCLE ( 'NONE', #51931, 130.5560000000000116 ) ;
#44756 = DIRECTION ( 'NONE',  ( 0.000000000000000000, 0.000000000000000000, 1.000000000000000000 ) ) ;
#44757 = EDGE_CURVE ( 'NONE', #45388, #88176, #53469, .T. ) ;
#44758 = EDGE_CURVE ( 'NONE', #20709, #3896, #86695, .T. ) ;
#44759 = CARTESIAN_POINT ( 'NONE',  ( 107.0667039024470313, -104.2784471599413934, 2.217806855418003043 ) ) ;
#44760 = CIRCLE ( 'NONE', #1269, 11.45913725231036118 ) ;
#44761 = CARTESIAN_POINT ( 'NONE',  ( 117.3951115944451402, -37.65585020919953507, 33.74324432352998571 ) ) ;
#44762 = VERTEX_POINT ( 'NONE', #53924 ) ;
#44763 = ORIENTED_EDGE ( 'NONE', *, *, #57679, .T. ) ;
#44764 = VERTEX_POINT ( 'NONE', #81681 ) ;
#44765 = EDGE_CURVE ( 'NONE', #72947, #59883, #32004, .T. ) ;
#44766 = FACE_OUTER_BOUND ( 'NONE', #86984, .T. ) ;
#44767 = DIRECTION ( 'NONE',  ( 1.000000000000000000, 4.163336342344333240E-14, 0.000000000000000000 ) ) ;
#44768 = CARTESIAN_POINT ( 'NONE',  ( 104.4899544570823622, -26.97880758339827878, 116.2814586088303912 ) ) ;
#44769 = CARTESIAN_POINT ( 'NONE',  ( 70.63919639214310564, 91.07499999999996021, 0.000000000000000000 ) ) ;
#44770 = DIRECTION ( 'NONE',  ( -1.000000000000000000, 0.000000000000000000, 0.000000000000000000 ) ) ;
#44771 = ADVANCED_FACE ( 'NONE', ( #80333 ), #2977, .F. ) ;
#44772 = CARTESIAN_POINT ( 'NONE',  ( 97.06381352669615126, -37.34181605626559275, 52.37546128077145369 ) ) ;
#44773 = AXIS2_PLACEMENT_3D ( 'NONE', #65711, #31185, #58885 ) ;
#44774 = DIRECTION ( 'NONE',  ( 3.100000000000000258E-29, -3.100000000000000044E-14, -1.000000000000000000 ) ) ;
#44775 = CARTESIAN_POINT ( 'NONE',  ( -5.170486730135384512, 94.15052322753994929, 130.4536157927243778 ) ) ;
#44776 = CARTESIAN_POINT ( 'NONE',  ( 117.2454586689012359, -38.87819698039184146, 63.66133956162494911 ) ) ;
#44777 = ORIENTED_EDGE ( 'NONE', *, *, #85729, .F. ) ;
#44779 = ORIENTED_EDGE ( 'NONE', *, *, #70745, .F. ) ;
#44778 = ADVANCED_FACE ( 'NONE', ( #18080, #58958 ), #29726, .F. ) ;
#44780 = DIRECTION ( 'NONE',  ( -1.000000000000000078E-15, 1.000000000000000083E-30, 1.000000000000000000 ) ) ;
#44781 = CARTESIAN_POINT ( 'NONE',  ( 44.45000000000000284, 69.84999999999999432, 219.0749999999999886 ) ) ;
#44782 = CARTESIAN_POINT ( 'NONE',  ( 0.000000000000000000, 11.98343896644750117, 0.000000000000000000 ) ) ;
#44783 = CARTESIAN_POINT ( 'NONE',  ( 107.8241526860280430, -28.10814435038363968, 107.8128522743529771 ) ) ;
#44785 = EDGE_CURVE ( 'NONE', #28914, #41711, #70615, .T. ) ;
#44784 = TOROIDAL_SURFACE ( 'NONE', #46247, 13.09746158385919124, 3.000000000000000000 ) ;
#44786 = CARTESIAN_POINT ( 'NONE',  ( 179.4595971212725090, -26.00627455218570105, 193.9678068554150059 ) ) ;
#44787 = LINE ( 'NONE', #84816, #54639 ) ;
#44788 = ORIENTED_EDGE ( 'NONE', *, *, #14206, .F. ) ;
#44789 = VERTEX_POINT ( 'NONE', #7043 ) ;
#44790 = CARTESIAN_POINT ( 'NONE',  ( 29.56670390244797630, -67.87844715994100397, 310.9178068554150514 ) ) ;
#44791 = ORIENTED_EDGE ( 'NONE', *, *, #16790, .T. ) ;
#44792 = ORIENTED_EDGE ( 'NONE', *, *, #10778, .F. ) ;
#44793 = EDGE_CURVE ( 'NONE', #1145, #48357, #7492, .T. ) ;
#44794 = CARTESIAN_POINT ( 'NONE',  ( 99.72946911866242203, -30.86048229651775543, 192.2092023535159626 ) ) ;
#44795 = VECTOR ( 'NONE', #23753, 999.9999999999998863 ) ;
#44796 = LINE ( 'NONE', #72524, #69925 ) ;
#44797 = EDGE_CURVE ( 'NONE', #34742, #89397, #34739, .T. ) ;
#44798 = CARTESIAN_POINT ( 'NONE',  ( 113.0894857754661587, -28.19359922731340262, 125.5870538473399591 ) ) ;
#44799 = CARTESIAN_POINT ( 'NONE',  ( 104.4899545353706856, -26.97880756368666155, 120.2814586024699679 ) ) ;
#44800 = CARTESIAN_POINT ( 'NONE',  ( 105.7154773078611640, -46.72385838936182978, 83.46895860744972140 ) ) ;
#44801 = EDGE_LOOP ( 'NONE', ( #8536, #43552 ) ) ;
#44802 = CIRCLE ( 'NONE', #31779, 14.49999999999997158 ) ;
#44803 = VERTEX_POINT ( 'NONE', #14765 ) ;
#44804 = ORIENTED_EDGE ( 'NONE', *, *, #20585, .F. ) ;
#44805 = CARTESIAN_POINT ( 'NONE',  ( 99.49937927431119533, -39.79027430526630127, 204.4509475124479536 ) ) ;
#44806 = CIRCLE ( 'NONE', #10018, 10.00000000000002665 ) ;
#44807 = CARTESIAN_POINT ( 'NONE',  ( 118.0253644177900156, -38.34139182134431678, 73.72229194257801055 ) ) ;
#44808 = ORIENTED_EDGE ( 'NONE', *, *, #29907, .F. ) ;
#44809 = CARTESIAN_POINT ( 'NONE',  ( 118.0525141433398773, -37.71481444994964960, 33.74324432352998571 ) ) ;
#44810 = FACE_OUTER_BOUND ( 'NONE', #27683, .T. ) ;
#44811 = CARTESIAN_POINT ( 'NONE',  ( 116.3263622980238097, -32.93962144782776846, 195.1356252759109680 ) ) ;
#44812 = CARTESIAN_POINT ( 'NONE',  ( 114.5121600660089030, -29.42679343410769377, 145.4441967044819819 ) ) ;
#44813 = DIRECTION ( 'NONE',  ( 0.000000000000000000, 1.000000000000000000, 0.000000000000000000 ) ) ;
#44814 = ORIENTED_EDGE ( 'NONE', *, *, #80664, .T. ) ;
#44815 = AXIS2_PLACEMENT_3D ( 'NONE', #75060, #6034, #33724 ) ;
#44816 = CARTESIAN_POINT ( 'NONE',  ( 0.000000000000000000, 127.0000000000000000, 0.000000000000000000 ) ) ;
#44817 = ORIENTED_EDGE ( 'NONE', *, *, #14443, .F. ) ;
#44818 = AXIS2_PLACEMENT_3D ( 'NONE', #84870, #14476, #28524 ) ;
#44819 = CARTESIAN_POINT ( 'NONE',  ( 147.0667039024457665, -137.6758868153238780, 245.5072646551060132 ) ) ;
#44820 = CARTESIAN_POINT ( 'NONE',  ( 91.91125933621933086, -96.64603743111524636, -19.23816181211526910 ) ) ;
#44821 = ORIENTED_EDGE ( 'NONE', *, *, #83241, .T. ) ;
#44822 = EDGE_CURVE ( 'NONE', #21130, #22928, #49248, .T. ) ;
#44823 = DIRECTION ( 'NONE',  ( 0.1041461484700691442, -0.008931931031208442673, 0.9945218953682739560 ) ) ;
#44824 = CARTESIAN_POINT ( 'NONE',  ( 199.3900000000000148, 46.38749999999999574, -38.10000000000000142 ) ) ;
#44825 = CARTESIAN_POINT ( 'NONE',  ( 115.7287795988047634, -43.59557489936061359, 48.30514908543492680 ) ) ;
#44826 = CARTESIAN_POINT ( 'NONE',  ( 71.25416588882602298, -72.55705569728901594, 396.9756252759102040 ) ) ;
#44827 = LINE ( 'NONE', #87519, #57941 ) ;
#44828 = DIRECTION ( 'NONE',  ( -4.237773401492740281E-14, 1.000000000000000000, 0.000000000000000000 ) ) ;
#44829 = CARTESIAN_POINT ( 'NONE',  ( 100.7170190823676279, -45.85612711270997011, 87.09276813305393716 ) ) ;
#44831 = CARTESIAN_POINT ( 'NONE',  ( 104.5678333644584228, -48.28820816006142991, 178.4070538473399665 ) ) ;
#44830 = CARTESIAN_POINT ( 'NONE',  ( 168.0371591254545365, -48.62818131005519007, 193.9678068554149775 ) ) ;
#44832 = DIRECTION ( 'NONE',  ( 0.000000000000000000, 1.000000000000000000, 0.000000000000000000 ) ) ;
#44833 = DIRECTION ( 'NONE',  ( 0.000000000000000000, 1.000000000000000000, 0.000000000000000000 ) ) ;
#44834 = EDGE_LOOP ( 'NONE', ( #11285, #35356, #22215, #56293 ) ) ;
#44835 = AXIS2_PLACEMENT_3D ( 'NONE', #37696, #16358, #63608 ) ;
#44836 = CARTESIAN_POINT ( 'NONE',  ( 83.73314995793998605, 12.92155284005730387, 361.9756252759109998 ) ) ;
#44837 = LINE ( 'NONE', #18027, #26767 ) ;
#44838 = CARTESIAN_POINT ( 'NONE',  ( 97.70690373477779644, -40.25222842886677199, 136.6132999708127613 ) ) ;
#44839 = LINE ( 'NONE', #58906, #34646 ) ;
#44841 = ORIENTED_EDGE ( 'NONE', *, *, #11342, .F. ) ;
#44840 = CARTESIAN_POINT ( 'NONE',  ( 106.2986956077118208, -47.17057584017531724, 222.5184824187679453 ) ) ;
#44842 = DIRECTION ( 'NONE',  ( 2.041950104878631501E-14, -0.7071067811865493491, 0.7071067811865455743 ) ) ;
#44843 = CARTESIAN_POINT ( 'NONE',  ( 115.9784307414374780, -30.15203137637957909, 255.3203871806729524 ) ) ;
#44844 = CARTESIAN_POINT ( 'NONE',  ( 113.9455412938869330, -28.01876065682782624, 120.5565776568639507 ) ) ;
#44845 = DIRECTION ( 'NONE',  ( 0.7071067811865171526, 0.7071067811865779928, 7.071067811865164719E-16 ) ) ;
#44846 = CARTESIAN_POINT ( 'NONE',  ( 0.4144590284063602859, 95.24999999999994316, -130.5559999999999832 ) ) ;
#44848 = ADVANCED_FACE ( 'NONE', ( #76984 ), #76529, .F. ) ;
#44847 = VECTOR ( 'NONE', #66558, 1000.000000000000000 ) ;
#44849 = LINE ( 'NONE', #3519, #55817 ) ;
#44850 = CARTESIAN_POINT ( 'NONE',  ( 100.8872838973176584, -44.70006880583113684, 263.0523720315491687 ) ) ;
#44851 = EDGE_LOOP ( 'NONE', ( #655, #30178, #11548, #42010 ) ) ;
#44852 = ADVANCED_FACE ( 'NONE', ( #70159 ), #14590, .T. ) ;
#44853 = ORIENTED_EDGE ( 'NONE', *, *, #8866, .T. ) ;
#44854 = EDGE_CURVE ( 'NONE', #20813, #22549, #8393, .T. ) ;
#44855 = ORIENTED_EDGE ( 'NONE', *, *, #81603, .F. ) ;
#44856 = EDGE_CURVE ( 'NONE', #17803, #61315, #76075, .T. ) ;
#44857 = ORIENTED_EDGE ( 'NONE', *, *, #10429, .F. ) ;
#44858 = CARTESIAN_POINT ( 'NONE',  ( 100.8874678687824229, -44.70022136308342908, 72.05229194101603696 ) ) ;
#44859 = CARTESIAN_POINT ( 'NONE',  ( 105.7763715259175257, -26.38449191207581634, 266.1756252759109884 ) ) ;
#44860 = FACE_OUTER_BOUND ( 'NONE', #18104, .T. ) ;
#44861 = CARTESIAN_POINT ( 'NONE',  ( 131.4836309258849383, -35.78502016655559714, 2.871594975603882993 ) ) ;
#44862 = VECTOR ( 'NONE', #6217, 1000.000000000000000 ) ;
#44863 = ADVANCED_FACE ( 'NONE', ( #28368 ), #1581, .F. ) ;
#44865 = CARTESIAN_POINT ( 'NONE',  ( 81.47036787067760599, 70.27763793881258891, 86.12934247706320434 ) ) ;
#44864 = CARTESIAN_POINT ( 'NONE',  ( 173.9900000000000091, 14.32000000000000028, -71.37400000000000944 ) ) ;
#44866 = CARTESIAN_POINT ( 'NONE',  ( 48.16670390244701139, -26.71338133339251542, -5.074374724088000832 ) ) ;
#44867 = CARTESIAN_POINT ( 'NONE',  ( 112.5429177363308924, -43.28420096851815657, 192.5524198280769781 ) ) ;
#44868 = ORIENTED_EDGE ( 'NONE', *, *, #2468, .F. ) ;
#44869 = ORIENTED_EDGE ( 'NONE', *, *, #48532, .F. ) ;
#44870 = AXIS2_PLACEMENT_3D ( 'NONE', #22628, #43482, #43031 ) ;
#44872 = ORIENTED_EDGE ( 'NONE', *, *, #4901, .T. ) ;
#44871 = CIRCLE ( 'NONE', #63690, 16.33514202138213633 ) ;
#44873 = ADVANCED_FACE ( 'NONE', ( #14311 ), #83805, .F. ) ;
#44874 = DIRECTION ( 'NONE',  ( 0.000000000000000000, 0.000000000000000000, -1.000000000000000000 ) ) ;
#44875 = DIRECTION ( 'NONE',  ( 0.000000000000000000, 1.000000000000000000, 0.000000000000000000 ) ) ;
#44876 = CARTESIAN_POINT ( 'NONE',  ( 97.51798391995397708, -31.03399779358258215, 276.8984824187675713 ) ) ;
#44877 = EDGE_CURVE ( 'NONE', #34343, #33225, #7378, .T. ) ;
#44878 = DIRECTION ( 'NONE',  ( 0.000000000000000000, 0.000000000000000000, -1.000000000000000000 ) ) ;
#44879 = VECTOR ( 'NONE', #53715, 1000.000000000000114 ) ;
#44880 = LINE ( 'NONE', #11255, #23033 ) ;
#44881 = CARTESIAN_POINT ( 'NONE',  ( -3.968750000000770051, 127.0000000000000000, 105.4788588808462038 ) ) ;
#44882 = VERTEX_POINT ( 'NONE', #1126 ) ;
#44883 = CARTESIAN_POINT ( 'NONE',  ( 20.03715912545741418, -46.82818131006202123, 117.4678068554150485 ) ) ;
#44884 = EDGE_LOOP ( 'NONE', ( #1620, #75749, #75884, #17673 ) ) ;
#44885 = CARTESIAN_POINT ( 'NONE',  ( 105.1735626975883662, -45.17443245699572429, 25.20713798863899413 ) ) ;
#44886 = CARTESIAN_POINT ( 'NONE',  ( 165.6738106836199904, -26.00627455219321860, -5.074374724088000832 ) ) ;
#44887 = DIRECTION ( 'NONE',  ( 0.4634479843259246556, 0.000000000000000000, 0.8861241255175470455 ) ) ;
#44888 = AXIS2_PLACEMENT_3D ( 'NONE', #75236, #14358, #267 ) ;
#44889 = CARTESIAN_POINT ( 'NONE',  ( 176.7669697523281229, -48.62818131005231947, 129.9678068554150059 ) ) ;
#44890 = ORIENTED_EDGE ( 'NONE', *, *, #12787, .F. ) ;
#44891 = CARTESIAN_POINT ( 'NONE',  ( 34.92499999999999716, 82.54999999999999716, 302.8950000000000387 ) ) ;
#44892 = CARTESIAN_POINT ( 'NONE',  ( 122.2688682072174942, 60.56780087056017692, -45.77403049370062860 ) ) ;
#44893 = ORIENTED_EDGE ( 'NONE', *, *, #50413, .F. ) ;
#44894 = CARTESIAN_POINT ( 'NONE',  ( 95.34890500915419409, -34.95776856631113105, 71.20705384733993526 ) ) ;
#44895 = ORIENTED_EDGE ( 'NONE', *, *, #3577, .T. ) ;
#44896 = CARTESIAN_POINT ( 'NONE',  ( 116.0863591824327443, -37.53846460971577415, 33.16575316141096152 ) ) ;
#44897 = CARTESIAN_POINT ( 'NONE',  ( 179.8585841295800094, -30.08671355700241179, -5.074374724088000832 ) ) ;
#44898 = CARTESIAN_POINT ( 'NONE',  ( 101.3137116872897820, -44.99844491211269570, 83.52444044875394979 ) ) ;
#44899 = FACE_OUTER_BOUND ( 'NONE', #84380, .T. ) ;
#44900 = CARTESIAN_POINT ( 'NONE',  ( 107.0664832912739968, -18.82844715994099971, 168.9256252759119832 ) ) ;
#44901 = ADVANCED_FACE ( 'NONE', ( #36548 ), #22471, .T. ) ;
#44902 = CARTESIAN_POINT ( 'NONE',  ( 74.68178297942419874, -67.87877198938119250, 246.0920795366729976 ) ) ;
#44903 = VECTOR ( 'NONE', #79219, 1000.000000000000000 ) ;
#44904 = CARTESIAN_POINT ( 'NONE',  ( 100.5371587349295055, -27.78220587661078156, 26.56610146638793779 ) ) ;
#44905 = CARTESIAN_POINT ( 'NONE',  ( 179.8608231853560255, -35.55794170701751256, -5.074374724088000832 ) ) ;
#44906 = ORIENTED_EDGE ( 'NONE', *, *, #77263, .T. ) ;
#44907 = DIRECTION ( 'NONE',  ( 0.000000000000000000, -1.000000000000000000, 0.000000000000000000 ) ) ;
#44908 = ORIENTED_EDGE ( 'NONE', *, *, #78221, .T. ) ;
#44909 = PLANE ( 'NONE',  #17807 ) ;
#44910 = VERTEX_POINT ( 'NONE', #49704 ) ;
#44911 = ORIENTED_EDGE ( 'NONE', *, *, #37983, .F. ) ;
#44913 = CIRCLE ( 'NONE', #7205, 5.041900000000001825 ) ;
#44912 = DIRECTION ( 'NONE',  ( 2.900000000000000265E-14, -2.000000000000000155E-15, 1.000000000000000000 ) ) ;
#44914 = CARTESIAN_POINT ( 'NONE',  ( 106.9482321581270270, -47.09886382165569785, 232.5794347997209854 ) ) ;
#44915 = DIRECTION ( 'NONE',  ( 1.000000000000000000, 0.000000000000000000, 2.108231265501709878E-16 ) ) ;
#44916 = LINE ( 'NONE', #58982, #6997 ) ;
#44917 = CARTESIAN_POINT ( 'NONE',  ( 107.3210293350295501, -25.67914459413323058, 71.04610146638795243 ) ) ;
#44918 = LINE ( 'NONE', #87172, #65374 ) ;
#44919 = ORIENTED_EDGE ( 'NONE', *, *, #925, .T. ) ;
#44920 = CARTESIAN_POINT ( 'NONE',  ( 97.06384307882487406, -37.34221630416103466, 172.3751823342733758 ) ) ;
#44921 = CIRCLE ( 'NONE', #5784, 5.500000000000000888 ) ;
#44922 = CARTESIAN_POINT ( 'NONE',  ( 172.5664832912740110, -36.32844715994070839, 318.9256252759120116 ) ) ;
#44923 = ORIENTED_EDGE ( 'NONE', *, *, #20775, .T. ) ;
#44924 = CIRCLE ( 'NONE', #70898, 2.749999999999974687 ) ;
#44925 = AXIS2_PLACEMENT_3D ( 'NONE', #5715, #61550, #46116 ) ;
#44926 = ADVANCED_FACE ( 'NONE', ( #41988 ), #63803, .F. ) ;
#44927 = DIRECTION ( 'NONE',  ( -0.8944271909999158554, 1.296919426949877873E-14, 0.4472135954999579277 ) ) ;
#44928 = CYLINDRICAL_SURFACE ( 'NONE', #23750, 2.750000000000002665 ) ;
#44929 = CARTESIAN_POINT ( 'NONE',  ( 100.7633749303630850, -45.78122309449486949, 237.0803871806729717 ) ) ;
#44930 = CARTESIAN_POINT ( 'NONE',  ( 160.2664750769284865, 101.5999999999999943, -148.0533267522753818 ) ) ;
#44931 = FACE_OUTER_BOUND ( 'NONE', #68616, .T. ) ;
#44932 = DIRECTION ( 'NONE',  ( 1.000000000000000000, 0.000000000000000000, -7.043400939473319300E-33 ) ) ;
#44933 = CARTESIAN_POINT ( 'NONE',  ( 106.4400806841681231, -45.24788313703638210, 221.9409912566479477 ) ) ;
#44935 = CARTESIAN_POINT ( 'NONE',  ( 114.5517459224756038, -44.00510994954048982, 94.21276813305395592 ) ) ;
#44934 = DIRECTION ( 'NONE',  ( 0.000000000000000000, 0.000000000000000000, 1.000000000000000000 ) ) ;
#44936 = CARTESIAN_POINT ( 'NONE',  ( 110.6772377970183214, 63.23435454354248009, 69.24934357568848498 ) ) ;
#44937 = CARTESIAN_POINT ( 'NONE',  ( 114.7585751371172051, -43.83144610948713193, 123.2327681330539519 ) ) ;
#44938 = ORIENTED_EDGE ( 'NONE', *, *, #46092, .T. ) ;
#44939 = DIRECTION ( 'NONE',  ( 0.5773502691896305050, -0.5773502691896303940, -0.5773502691896164052 ) ) ;
#44940 = ORIENTED_EDGE ( 'NONE', *, *, #34513, .T. ) ;
#44941 = VECTOR ( 'NONE', #66818, 1000.000000000000000 ) ;
#44942 = LINE ( 'NONE', #24079, #14934 ) ;
#44943 = DIRECTION ( 'NONE',  ( -0.7071067812160279908, 0.7071067811570671546, -6.612322856135836109E-17 ) ) ;
#44944 = LINE ( 'NONE', #60810, #38379 ) ;
#44945 = EDGE_LOOP ( 'NONE', ( #21665, #24078, #27120, #33554 ) ) ;
#44946 = DIRECTION ( 'NONE',  ( -1.000000000000000000, -4.299999999999999979E-14, -1.000000000000000078E-15 ) ) ;
#44947 = ORIENTED_EDGE ( 'NONE', *, *, #47214, .F. ) ;
#44948 = DIRECTION ( 'NONE',  ( 0.000000000000000000, -1.000000000000000000, 0.000000000000000000 ) ) ;
#44949 = AXIS2_PLACEMENT_3D ( 'NONE', #29074, #63591, #915 ) ;
#44950 = CARTESIAN_POINT ( 'NONE',  ( 99.48898161933324502, -91.15344715994181968, -11.78219314458242550 ) ) ;
#44951 = DIRECTION ( 'NONE',  ( -0.4999999999999985567, -0.8660254037844395958, 2.688821387764040899E-14 ) ) ;
#44952 = VERTEX_POINT ( 'NONE', #84708 ) ;
#44953 = CARTESIAN_POINT ( 'NONE',  ( 98.18350318933659082, -43.34670532666833509, 111.8480062282919647 ) ) ;
#44954 = CARTESIAN_POINT ( 'NONE',  ( 0.000000000000000000, 0.000000000000000000, 0.000000000000000000 ) ) ;
#44955 = CARTESIAN_POINT ( 'NONE',  ( 97.60795516317995180, -39.98261623142427368, 166.5900807200408735 ) ) ;
#44956 = DIRECTION ( 'NONE',  ( 0.000000000000000000, 1.000000000000000000, 0.000000000000000000 ) ) ;
#44957 = DIRECTION ( 'NONE',  ( -6.524622321627019585E-16, -3.741823817616790462E-31, -1.000000000000000000 ) ) ;
#44958 = EDGE_LOOP ( 'NONE', ( #55249, #15539, #33074, #53541 ) ) ;
#44959 = EDGE_CURVE ( 'NONE', #32600, #87802, #48795, .T. ) ;
#44960 = EDGE_CURVE ( 'NONE', #66809, #29859, #32062, .T. ) ;
#44961 = ORIENTED_EDGE ( 'NONE', *, *, #27025, .T. ) ;
#44962 = FACE_OUTER_BOUND ( 'NONE', #60788, .T. ) ;
#44963 = CARTESIAN_POINT ( 'NONE',  ( 177.8371591254544910, -47.82818131005477369, 193.9678068554150059 ) ) ;
#44964 = ADVANCED_FACE ( 'NONE', ( #78787 ), #59192, .T. ) ;
#44965 = DIRECTION ( 'NONE',  ( -0.1811243269278930978, 0.9834602067165288952, 0.000000000000000000 ) ) ;
#44966 = EDGE_CURVE ( 'NONE', #10962, #20321, #16991, .T. ) ;
#44968 = CARTESIAN_POINT ( 'NONE',  ( -15.89999999999999680, 53.97500000000000142, 70.79999999999999716 ) ) ;
#44967 = CARTESIAN_POINT ( 'NONE',  ( 37.56670390244743629, -48.82844715994126261, 180.4678068554150911 ) ) ;
#44969 = DIRECTION ( 'NONE',  ( 0.7071067811865774377, -0.7071067811865175967, 7.071067811865782003E-16 ) ) ;
#44970 = AXIS2_PLACEMENT_3D ( 'NONE', #64570, #86803, #45873 ) ;
#44971 = ORIENTED_EDGE ( 'NONE', *, *, #63136, .F. ) ;
#44972 = DIRECTION ( 'NONE',  ( 1.000000000000000000, 6.831565154159360295E-14, 0.000000000000000000 ) ) ;
#44973 = CARTESIAN_POINT ( 'NONE',  ( 99.18511857479145988, -30.88155312011797804, 176.8184824187669619 ) ) ;
#44974 = ADVANCED_FACE ( 'NONE', ( #44673 ), #78343, .F. ) ;
#44976 = ORIENTED_EDGE ( 'NONE', *, *, #9007, .T. ) ;
#44975 = CARTESIAN_POINT ( 'NONE',  ( 115.0439452383992318, -109.4614598618335890, 2.217806855418169576 ) ) ;
#44977 = AXIS2_PLACEMENT_3D ( 'NONE', #84918, #17204, #2684 ) ;
#44978 = CARTESIAN_POINT ( 'NONE',  ( 103.0217603822331398, -26.37318333953113836, 16.37276813305293999 ) ) ;
#44979 = CARTESIAN_POINT ( 'NONE',  ( 141.8664832912729992, -1.929447159941394263, 342.9256252759109316 ) ) ;
#44980 = CARTESIAN_POINT ( 'NONE',  ( 138.8545562996767444, -1.932463243632620342, 361.9756252759100335 ) ) ;
#44981 = CARTESIAN_POINT ( 'NONE',  ( 30.00000000000001776, 171.0000000000000000, 114.8826257785461280 ) ) ;
#44982 = VECTOR ( 'NONE', #23768, 1000.000000000000000 ) ;
#44983 = ORIENTED_EDGE ( 'NONE', *, *, #53746, .F. ) ;
#44984 = PLANE ( 'NONE',  #18230 ) ;
#44985 = ORIENTED_EDGE ( 'NONE', *, *, #10468, .T. ) ;
#44986 = ORIENTED_EDGE ( 'NONE', *, *, #25552, .T. ) ;
#44987 = CARTESIAN_POINT ( 'NONE',  ( 113.8438844162330810, -30.22226962059244215, 185.8549166392299696 ) ) ;
#44988 = AXIS2_PLACEMENT_3D ( 'NONE', #87515, #25276, #52942 ) ;
#44989 = LINE ( 'NONE', #50470, #67577 ) ;
#44990 = CARTESIAN_POINT ( 'NONE',  ( 23.30877932141580544, 86.33358099468556190, 299.9857356779602355 ) ) ;
#44991 = LINE ( 'NONE', #24567, #8409 ) ;
#44992 = AXIS2_PLACEMENT_3D ( 'NONE', #5389, #20368, #60786 ) ;
#44993 = FACE_OUTER_BOUND ( 'NONE', #71823, .T. ) ;
#44994 = ORIENTED_EDGE ( 'NONE', *, *, #77395, .F. ) ;
#44995 = CARTESIAN_POINT ( 'NONE',  ( 34.96670390244619853, -28.27351298637401200, 342.9256252759109884 ) ) ;
#44996 = CARTESIAN_POINT ( 'NONE',  ( -254.0000000000000000, 53.97500000000000853, 101.5999999999999943 ) ) ;
#44997 = ORIENTED_EDGE ( 'NONE', *, *, #69352, .T. ) ;
#44998 = CARTESIAN_POINT ( 'NONE',  ( 115.6772654923307613, -42.56752007954070649, 273.3527681330537575 ) ) ;
#44999 = FACE_BOUND ( 'NONE', #48168, .T. ) ;
#45000 = EDGE_LOOP ( 'NONE', ( #78706, #32118 ) ) ;
#45001 = FACE_OUTER_BOUND ( 'NONE', #25634, .T. ) ;
#45002 = DIRECTION ( 'NONE',  ( -0.7759704746411383303, 0.6307692307692303046, 0.000000000000000000 ) ) ;
#45003 = AXIS2_PLACEMENT_3D ( 'NONE', #28993, #36250, #52395 ) ;
#45004 = CARTESIAN_POINT ( 'NONE',  ( -27.27158787008326968, 127.0000000000000000, -0.000000000000000000 ) ) ;
#45005 = CYLINDRICAL_SURFACE ( 'NONE', #33142, 34.13125000000000142 ) ;
#45006 = EDGE_CURVE ( 'NONE', #45258, #66312, #16105, .T. ) ;
#45007 = CARTESIAN_POINT ( 'NONE',  ( 96.14593026560288536, -32.00158989507077223, 207.0013395616249738 ) ) ;
#45008 = DIRECTION ( 'NONE',  ( -0.8660254037844387076, 0.000000000000000000, 0.4999999999999998890 ) ) ;
#45009 = ORIENTED_EDGE ( 'NONE', *, *, #25487, .F. ) ;
#45010 = CARTESIAN_POINT ( 'NONE',  ( 96.88468944541251915, -39.16338508605922186, 52.51276813305394597 ) ) ;
#45011 = DIRECTION ( 'NONE',  ( -2.999999999999999839E-15, 1.000000000000000000, -2.999999999999999900E-30 ) ) ;
#45012 = ADVANCED_FACE ( 'NONE', ( #52356 ), #58316, .T. ) ;
#45013 = CARTESIAN_POINT ( 'NONE',  ( 102.3791524630845799, -47.61053145109372764, 287.2527681330536780 ) ) ;
#45014 = EDGE_LOOP ( 'NONE', ( #87586, #71535, #47894, #7896 ) ) ;
#45015 = AXIS2_PLACEMENT_3D ( 'NONE', #63734, #43267, #36481 ) ;
#45016 = AXIS2_PLACEMENT_3D ( 'NONE', #64638, #4203, #87324 ) ;
#45017 = CARTESIAN_POINT ( 'NONE',  ( 80.71968614772718809, -16.05633243510678554, 1.689562801603858633 ) ) ;
#45018 = CARTESIAN_POINT ( 'NONE',  ( 116.3162594664470788, -32.94075446336835000, 20.13562527591095019 ) ) ;
#45019 = CARTESIAN_POINT ( 'NONE',  ( 154.5667039024470171, -79.67844715994088745, 190.2178068554179902 ) ) ;
#45020 = CARTESIAN_POINT ( 'NONE',  ( 111.3320211711901067, -29.76992759232029329, 92.45666179816296903 ) ) ;
#45021 = CARTESIAN_POINT ( 'NONE',  ( 109.9662181263222891, -48.24525319228295217, 238.7727681330539724 ) ) ;
#45022 = PLANE ( 'NONE',  #56544 ) ;
#45023 = ORIENTED_EDGE ( 'NONE', *, *, #29807, .F. ) ;
#45024 = CARTESIAN_POINT ( 'NONE',  ( 177.1649999999999920, 25.81350000000000477, -7.937500000000000000 ) ) ;
#45025 = AXIS2_PLACEMENT_3D ( 'NONE', #67130, #4466, #38088 ) ;
#45026 = ORIENTED_EDGE ( 'NONE', *, *, #33163, .F. ) ;
#45027 = ORIENTED_EDGE ( 'NONE', *, *, #24762, .T. ) ;
#45028 = EDGE_CURVE ( 'NONE', #8645, #39224, #53640, .T. ) ;
#45029 = CARTESIAN_POINT ( 'NONE',  ( 41.56648329127398966, -27.57844715994070484, 195.9256252759119832 ) ) ;
#45030 = ORIENTED_EDGE ( 'NONE', *, *, #78640, .T. ) ;
#45031 = VERTEX_POINT ( 'NONE', #30169 ) ;
#45032 = CARTESIAN_POINT ( 'NONE',  ( 97.81493411881378108, -40.51644251795452334, 167.6359250042934264 ) ) ;
#45033 = PRESENTATION_STYLE_ASSIGNMENT (( #8422 ) ) ;
#45034 = CARTESIAN_POINT ( 'NONE',  ( 103.3756532791179126, -27.43539013423222173, 41.37728782345830325 ) ) ;
#45035 = CARTESIAN_POINT ( 'NONE',  ( 110.9399543235443559, -27.82625392046294266, 134.1724198280769826 ) ) ;
#45036 = CARTESIAN_POINT ( 'NONE',  ( 116.8111099997371554, -31.41389126640522989, 24.21181575210196257 ) ) ;
#45037 = ORIENTED_EDGE ( 'NONE', *, *, #76850, .T. ) ;
#45038 = CARTESIAN_POINT ( 'NONE',  ( -12.37530111100094743, 79.66613297688917328, 129.9681797613511947 ) ) ;
#45039 = VECTOR ( 'NONE', #39302, 1000.000000000000000 ) ;
#45040 = ORIENTED_EDGE ( 'NONE', *, *, #48793, .T. ) ;
#45041 = AXIS2_PLACEMENT_3D ( 'NONE', #24987, #19063, #19964 ) ;
#45042 = CYLINDRICAL_SURFACE ( 'NONE', #47543, 9.999999999999998224 ) ;
#45043 = ORIENTED_EDGE ( 'NONE', *, *, #60188, .F. ) ;
#45044 = CARTESIAN_POINT ( 'NONE',  ( 97.96455956878604354, -32.51352612137473841, 166.9808845455257824 ) ) ;
#45045 = CARTESIAN_POINT ( 'NONE',  ( 107.3678158256761179, -26.30747296201684549, 321.5865679059475610 ) ) ;
#45046 = FACE_OUTER_BOUND ( 'NONE', #1149, .T. ) ;
#45047 = AXIS2_PLACEMENT_3D ( 'NONE', #20050, #61366, #48174 ) ;
#45048 = CARTESIAN_POINT ( 'NONE',  ( 63.03715912545733602, -46.82818131006016671, 193.9678068554150911 ) ) ;
#45049 = ORIENTED_EDGE ( 'NONE', *, *, #40096, .T. ) ;
#45050 = CARTESIAN_POINT ( 'NONE',  ( 96.76314818047262634, -35.13937921927007579, 266.2041967044821149 ) ) ;
#45051 = CARTESIAN_POINT ( 'NONE',  ( 114.1199461662357919, -46.31379764262941023, 29.08133956162595268 ) ) ;
#45052 = DIRECTION ( 'NONE',  ( 1.000000000000000000, 0.000000000000000000, 0.000000000000000000 ) ) ;
#45054 = CARTESIAN_POINT ( 'NONE',  ( 0.000000000000000000, 65.60000000000000853, 38.10000000000000142 ) ) ;
#45053 = DIRECTION ( 'NONE',  ( -1.000000000000000000, 0.000000000000000000, -2.108231265501709878E-16 ) ) ;
#45055 = CARTESIAN_POINT ( 'NONE',  ( 106.2252769208846530, -25.30081914710235580, 323.4954383871191794 ) ) ;
#45056 = DIRECTION ( 'NONE',  ( 0.000000000000000000, 0.000000000000000000, -1.000000000000000000 ) ) ;
#45057 = B_SPLINE_CURVE_WITH_KNOTS ( 'NONE', 3,
 ( #45949, #53205, #5559, #81862 ),
 .UNSPECIFIED., .F., .F.,
 ( 4, 4 ),
 ( -0.2154603786882610117, -0.01977385131020209519 ),
 .UNSPECIFIED. ) ;
#45058 = PLANE ( 'NONE',  #75988 ) ;
#45059 = ADVANCED_FACE ( 'NONE', ( #16542 ), #69757, .F. ) ;
#45060 = AXIS2_PLACEMENT_3D ( 'NONE', #27169, #43017, #77561 ) ;
#45061 = CARTESIAN_POINT ( 'NONE',  ( 125.9611475301391721, -14.72944715994100484, 239.5838068554164977 ) ) ;
#45062 = ADVANCED_FACE ( 'NONE', ( #51919 ), #38311, .T. ) ;
#45063 = CARTESIAN_POINT ( 'NONE',  ( 116.3268456006857718, -32.93825467094161752, 164.1356252759109680 ) ) ;
#45064 = LINE ( 'NONE', #85991, #761 ) ;
#45065 = CARTESIAN_POINT ( 'NONE',  ( 117.4283214861109457, -38.22576773620406954, 28.71276813305395592 ) ) ;
#45066 = CARTESIAN_POINT ( 'NONE',  ( 117.1971262914088499, -34.26925207598063849, 205.0156252759109634 ) ) ;
#45067 = CARTESIAN_POINT ( 'NONE',  ( 106.5169537372109545, -25.66675205370546919, 41.12800622829193742 ) ) ;
#45069 = DIRECTION ( 'NONE',  ( 0.7071067811864666375, 0.7071067811866283970, 7.071067811864659848E-16 ) ) ;
#45068 = CARTESIAN_POINT ( 'NONE',  ( 50.56670390244699576, -18.82844715994031048, -5.074374724088000832 ) ) ;
#45070 = CARTESIAN_POINT ( 'NONE',  ( -135.1318726873890341, 20.32000000000000028, 118.7423475625884066 ) ) ;
#45071 = ORIENTED_EDGE ( 'NONE', *, *, #3123, .T. ) ;
#45072 = CYLINDRICAL_SURFACE ( 'NONE', #41810, 0.9999999999999974465 ) ;
#45073 = ORIENTED_EDGE ( 'NONE', *, *, #3845, .F. ) ;
#45074 = VECTOR ( 'NONE', #39222, 1000.000000000000000 ) ;
#45075 = CARTESIAN_POINT ( 'NONE',  ( 104.0406618471960627, -46.06530165129700549, 78.32705384733895926 ) ) ;
#45076 = EDGE_CURVE ( 'NONE', #36080, #38972, #78868, .T. ) ;
#45078 = EDGE_LOOP ( 'NONE', ( #3793, #56875, #24490, #25429 ) ) ;
#45077 = CARTESIAN_POINT ( 'NONE',  ( 162.8913605087219878, -31.76306994223740432, -5.074374724088000832 ) ) ;
#45079 = CARTESIAN_POINT ( 'NONE',  ( 134.0664832912740110, -8.729447159940999512, 293.6356252759119911 ) ) ;
#45080 = CARTESIAN_POINT ( 'NONE',  ( 99.10268845779070546, -29.98093639561600909, 211.7670538473399517 ) ) ;
#45081 = CARTESIAN_POINT ( 'NONE',  ( 180.3503142329310265, -29.99615139349890569, 193.9678068554150059 ) ) ;
#45082 = CARTESIAN_POINT ( 'NONE',  ( 110.8554123912721394, -45.98385248439223716, 147.8857061149965375 ) ) ;
#45083 = ADVANCED_FACE ( 'NONE', ( #37432, #45113 ), #36982, .T. ) ;
#45084 = LINE ( 'NONE', #45966, #63175 ) ;
#45085 = VECTOR ( 'NONE', #70230, 1000.000000000000000 ) ;
#45086 = LINE ( 'NONE', #73240, #57410 ) ;
#45087 = DIRECTION ( 'NONE',  ( 0.000000000000000000, 0.000000000000000000, 1.000000000000000000 ) ) ;
#45088 = CARTESIAN_POINT ( 'NONE',  ( 104.4066424557107382, -46.45766250888145521, 97.36474845812441004 ) ) ;
#45089 = CARTESIAN_POINT ( 'NONE',  ( 96.70615320395830850, -37.17927570127479697, 116.3489586092449599 ) ) ;
#45090 = VERTEX_POINT ( 'NONE', #9726 ) ;
#45091 = CIRCLE ( 'NONE', #11791, 5.562600000000000655 ) ;
#45092 = EDGE_LOOP ( 'NONE', ( #10744, #25341, #48173, #74458 ) ) ;
#45093 = CARTESIAN_POINT ( 'NONE',  ( 115.4889021248300196, -33.97424487988631370, 85.51015473446898341 ) ) ;
#45094 = VECTOR ( 'NONE', #53607, 1000.000000000000000 ) ;
#45095 = LINE ( 'NONE', #44199, #86392 ) ;
#45097 = DIRECTION ( 'NONE',  ( -0.7071067812163254196, 0.7071067811567697259, -2.899137802742872063E-29 ) ) ;
#45096 = CARTESIAN_POINT ( 'NONE',  ( 116.7732407090125690, -35.28285290846963562, 214.9441967044819819 ) ) ;
#45098 = CARTESIAN_POINT ( 'NONE',  ( 188.5667039024479834, -62.87844715994099687, 252.3428068554150059 ) ) ;
#45099 = CARTESIAN_POINT ( 'NONE',  ( -487.2989999999999782, 14.28750000000026077, 11.11249999999970051 ) ) ;
#45100 = CARTESIAN_POINT ( 'NONE',  ( 117.9190617242381194, 79.25941250729452747, 12.27333445685097502 ) ) ;
#45101 = CARTESIAN_POINT ( 'NONE',  ( 98.58946256649487339, -99.96145986183361742, 2.217806855417864043 ) ) ;
#45102 = CARTESIAN_POINT ( 'NONE',  ( 21.03689327557706790, -23.42844715994186089, 300.4678068554150059 ) ) ;
#45103 = CARTESIAN_POINT ( 'NONE',  ( 3.174999999999879918, 104.3431970271541900, 33.98325472291465132 ) ) ;
#45104 = CARTESIAN_POINT ( 'NONE',  ( 97.97553865104310944, -30.48296430071270535, 165.8594347997199634 ) ) ;
#45105 = EDGE_LOOP ( 'NONE', ( #76802, #63481, #20653, #39534, #69627 ) ) ;
#45106 = ORIENTED_EDGE ( 'NONE', *, *, #61227, .F. ) ;
#45107 = CIRCLE ( 'NONE', #21934, 3.000000000000002665 ) ;
#45108 = CARTESIAN_POINT ( 'NONE',  ( 80.76543358272510886, -80.39462547777496582, 249.3134381260879877 ) ) ;
#45109 = CARTESIAN_POINT ( 'NONE',  ( 109.7248659615483319, -27.00080519155043035, 150.8647919392679455 ) ) ;
#45110 = CARTESIAN_POINT ( 'NONE',  ( 193.0374249753377001, -23.42844715993435400, 117.4678068554150627 ) ) ;
#45111 = CARTESIAN_POINT ( 'NONE',  ( 100.8869784611931379, -44.69984695892584625, 103.0522436344614192 ) ) ;
#45112 = AXIS2_PLACEMENT_3D ( 'NONE', #61704, #27198, #54874 ) ;
#45113 = FACE_BOUND ( 'NONE', #4261, .T. ) ;
#45114 = EDGE_CURVE ( 'NONE', #74303, #3666, #65132, .T. ) ;
#45115 = CARTESIAN_POINT ( 'NONE',  ( 111.4173512164996254, -47.75262429423162303, 172.8756252759109771 ) ) ;
#45116 = CARTESIAN_POINT ( 'NONE',  ( 165.3359832912747720, -36.32844715993532958, 237.4678068554150059 ) ) ;
#45117 = ORIENTED_EDGE ( 'NONE', *, *, #61886, .F. ) ;
#45119 = ORIENTED_EDGE ( 'NONE', *, *, #84179, .T. ) ;
#45118 = VERTEX_POINT ( 'NONE', #45998 ) ;
#45120 = AXIS2_PLACEMENT_3D ( 'NONE', #15237, #69751, #56999 ) ;
#45121 = CARTESIAN_POINT ( 'NONE',  ( 97.81255050737648560, -40.51953087483806826, 62.63627117197549410 ) ) ;
#45122 = DIRECTION ( 'NONE',  ( 1.000000000000000078E-15, -1.000000000000000000, 0.000000000000000000 ) ) ;
#45123 = CARTESIAN_POINT ( 'NONE',  ( 132.6459363690105135, -34.36767598605985796, 7.908804215159092266 ) ) ;
#45124 = VECTOR ( 'NONE', #78609, 1000.000000000000000 ) ;
#45125 = CARTESIAN_POINT ( 'NONE',  ( 114.9297498758896126, -40.81563990160193356, 284.8758690201828472 ) ) ;
#45126 = DIRECTION ( 'NONE',  ( -0.000000000000000000, -0.000000000000000000, 1.000000000000000000 ) ) ;
#45127 = VERTEX_POINT ( 'NONE', #39647 ) ;
#45128 = CARTESIAN_POINT ( 'NONE',  ( 116.3768930211383150, -39.34642689581756514, 9.635625275910943088 ) ) ;
#45129 = CARTESIAN_POINT ( 'NONE',  ( 82.11134023506700430, -16.88977106732933819, 7.516154048596654036 ) ) ;
#45130 = ORIENTED_EDGE ( 'NONE', *, *, #3471, .F. ) ;
#45131 = ORIENTED_EDGE ( 'NONE', *, *, #20771, .F. ) ;
#45132 = EDGE_CURVE ( 'NONE', #4380, #16856, #10286, .T. ) ;
#45133 = CARTESIAN_POINT ( 'NONE',  ( 69.97242935852821688, 101.2667670336148689, 94.87759905963716278 ) ) ;
#45134 = VERTEX_POINT ( 'NONE', #60532 ) ;
#45135 = ORIENTED_EDGE ( 'NONE', *, *, #5457, .F. ) ;
#45136 = FACE_OUTER_BOUND ( 'NONE', #13443, .T. ) ;
#45137 = CARTESIAN_POINT ( 'NONE',  ( 112.8214380862813755, -44.54936551000075440, 32.50384839950498872 ) ) ;
#45138 = CARTESIAN_POINT ( 'NONE',  ( 96.83676235526975518, -34.60832162431106696, 216.1641967044819808 ) ) ;
#45139 = AXIS2_PLACEMENT_3D ( 'NONE', #8237, #21874, #62289 ) ;
#45140 = CARTESIAN_POINT ( 'NONE',  ( 117.1424269838423839, -34.14023410701941685, 124.0270538473399426 ) ) ;
#45141 = DIRECTION ( 'NONE',  ( 0.000000000000000000, -1.000000000000000000, -3.491483361109380094E-15 ) ) ;
#45142 = CARTESIAN_POINT ( 'NONE',  ( 108.0140931804088211, -24.91688388787635589, 261.0127681330534415 ) ) ;
#45143 = DIRECTION ( 'NONE',  ( -6.524622321627019585E-16, -4.013151879589939944E-16, -1.000000000000000000 ) ) ;
#45144 = LINE ( 'NONE', #25610, #14874 ) ;
#45146 = ORIENTED_EDGE ( 'NONE', *, *, #9911, .F. ) ;
#45145 = EDGE_CURVE ( 'NONE', #394, #31817, #84303, .T. ) ;
#45147 = EDGE_CURVE ( 'NONE', #47135, #27284, #46571, .T. ) ;
#45148 = ORIENTED_EDGE ( 'NONE', *, *, #26899, .F. ) ;
#45149 = VECTOR ( 'NONE', #41811, 1000.000000000000000 ) ;
#45150 = VECTOR ( 'NONE', #4387, 1000.000000000000000 ) ;
#45151 = CARTESIAN_POINT ( 'NONE',  ( 117.3784280654263341, -34.92100556036569259, 243.9641967044819637 ) ) ;
#45152 = ORIENTED_EDGE ( 'NONE', *, *, #59743, .T. ) ;
#45153 = CARTESIAN_POINT ( 'NONE',  ( 114.5276809309653459, -28.57754439525472989, 154.4746728949589851 ) ) ;
#45154 = LINE ( 'NONE', #17907, #687 ) ;
#45155 = CARTESIAN_POINT ( 'NONE',  ( -3.452160436674259536, 70.12364187744314847, 37.94944277985399594 ) ) ;
#45156 = ADVANCED_FACE ( 'NONE', ( #12867 ), #33294, .T. ) ;
#45157 = DIRECTION ( 'NONE',  ( 0.000000000000000000, 0.000000000000000000, -1.000000000000000000 ) ) ;
#45158 = CARTESIAN_POINT ( 'NONE',  ( 143.8697414714609124, -140.3737278804164532, 246.5975155025261074 ) ) ;
#45161 = CARTESIAN_POINT ( 'NONE',  ( 97.00695478131298444, -39.24785563725447446, 12.53372051400597442 ) ) ;
#45160 = CARTESIAN_POINT ( 'NONE',  ( 49.21437657594998427, -35.91149509761070391, 237.4678068554150059 ) ) ;
#45159 = CARTESIAN_POINT ( 'NONE',  ( 21.03689327557619748, -23.42844715994197813, 129.9678068554150627 ) ) ;
#45162 = CARTESIAN_POINT ( 'NONE',  ( 188.5667039024479834, -65.37844715994100397, 257.2178068554150059 ) ) ;
#45163 = FACE_OUTER_BOUND ( 'NONE', #79858, .T. ) ;
#45164 = CARTESIAN_POINT ( 'NONE',  ( 213.4642805167760002, 52.73749999999999716, -34.63953933784325301 ) ) ;
#45165 = CARTESIAN_POINT ( 'NONE',  ( 68.61434409300457560, -136.9218521013149541, 247.4649940182199828 ) ) ;
#45166 = PLANE ( 'NONE',  #5340 ) ;
#45167 = ADVANCED_FACE ( 'NONE', ( #67350 ), #4697, .T. ) ;
#45168 = CARTESIAN_POINT ( 'NONE',  ( 97.06107109496848295, -37.99641194480408757, 77.42729194108127899 ) ) ;
#45169 = AXIS2_PLACEMENT_3D ( 'NONE', #67123, #75292, #47107 ) ;
#45171 = ORIENTED_EDGE ( 'NONE', *, *, #73227, .F. ) ;
#45170 = CARTESIAN_POINT ( 'NONE',  ( 100.5161095773857198, -41.59610960965854787, 195.5838068554171514 ) ) ;
#45172 = CARTESIAN_POINT ( 'NONE',  ( 136.7282109818895037, -19.44060378568062220, 6.877169033943577148 ) ) ;
#45173 = CARTESIAN_POINT ( 'NONE',  ( 101.9737040637596124, -45.89197751792076474, 187.1727681330539781 ) ) ;
#45174 = CARTESIAN_POINT ( 'NONE',  ( 100.9432064590905469, -28.29215089373294489, 71.57562527591099411 ) ) ;
#45175 = CARTESIAN_POINT ( 'NONE',  ( 118.8391071721064662, -38.46623720595516005, 219.7099109901969882 ) ) ;
#45176 = DIRECTION ( 'NONE',  ( 4.299999999999999979E-14, -1.000000000000000000, 0.000000000000000000 ) ) ;
#45177 = CARTESIAN_POINT ( 'NONE',  ( 186.6899999999999977, 46.38749999999999574, -50.79999999999999716 ) ) ;
#45179 = CARTESIAN_POINT ( 'NONE',  ( 116.6494290552723356, -33.84902491101575350, 40.05854322555403968 ) ) ;
#45178 = DIRECTION ( 'NONE',  ( -4.299999999999999979E-14, 1.000000000000000000, -4.400000000000000367E-29 ) ) ;
#45180 = CARTESIAN_POINT ( 'NONE',  ( 41.56648329127399677, 0.2215528400590013880, 318.9256252759120116 ) ) ;
#45181 = FACE_OUTER_BOUND ( 'NONE', #20232, .T. ) ;
#45182 = VECTOR ( 'NONE', #80728, 999.9999999999998863 ) ;
#45183 = CARTESIAN_POINT ( 'NONE',  ( 97.60796143750529552, -39.98263668746941590, 66.59062261628206159 ) ) ;
#45184 = ORIENTED_EDGE ( 'NONE', *, *, #5053, .T. ) ;
#45185 = VERTEX_POINT ( 'NONE', #19661 ) ;
#45186 = VECTOR ( 'NONE', #47165, 1000.000000000000000 ) ;
#45187 = CARTESIAN_POINT ( 'NONE',  ( 98.02882863141191194, -40.27788709084830998, 96.04670554236294322 ) ) ;
#45188 = EDGE_CURVE ( 'NONE', #31084, #44882, #44071, .T. ) ;
#45190 = ORIENTED_EDGE ( 'NONE', *, *, #45961, .F. ) ;
#45189 = CARTESIAN_POINT ( 'NONE',  ( 107.0664832912739968, -36.72944715994100306, 293.2242906452868851 ) ) ;
#45191 = CARTESIAN_POINT ( 'NONE',  ( 108.5348814579965904, -26.43029805172858460, 100.9641967044829727 ) ) ;
#45192 = DIRECTION ( 'NONE',  ( 0.000000000000000000, 0.000000000000000000, -1.000000000000000000 ) ) ;
#45193 = EDGE_CURVE ( 'NONE', #84182, #75853, #12403, .T. ) ;
#45194 = AXIS2_PLACEMENT_3D ( 'NONE', #71569, #31097, #17915 ) ;
#45195 = EDGE_CURVE ( 'NONE', #31278, #8470, #1785, .T. ) ;
#45196 = CARTESIAN_POINT ( 'NONE',  ( 77.31651901074916111, -18.55810522839905019, 6.749822759741312517 ) ) ;
#45197 = CARTESIAN_POINT ( 'NONE',  ( 32.24491389930067697, -32.11662333284641591, 237.4678068554150059 ) ) ;
#45198 = EDGE_CURVE ( 'NONE', #70994, #56609, #19046, .T. ) ;
#45199 = CARTESIAN_POINT ( 'NONE',  ( 111.1466539572802787, -45.61852150023370456, 27.91848241876893155 ) ) ;
#45200 = ORIENTED_EDGE ( 'NONE', *, *, #80174, .T. ) ;
#45201 = ORIENTED_EDGE ( 'NONE', *, *, #54042, .F. ) ;
#45202 = ORIENTED_EDGE ( 'NONE', *, *, #65396, .T. ) ;
#45203 = DIRECTION ( 'NONE',  ( 0.7071067811865449082, 0.7071067811865501263, 7.071067811865448709E-16 ) ) ;
#45204 = FACE_OUTER_BOUND ( 'NONE', #6732, .T. ) ;
#45205 = DIRECTION ( 'NONE',  ( 1.000000000000000000, 0.000000000000000000, -1.821231995776174986E-16 ) ) ;
#45206 = CARTESIAN_POINT ( 'NONE',  ( 46.83715912545339677, -47.82818131006086304, 180.4678068554150911 ) ) ;
#45207 = DIRECTION ( 'NONE',  ( 0.000000000000000000, 0.000000000000000000, 1.000000000000000000 ) ) ;
#45208 = CARTESIAN_POINT ( 'NONE',  ( 3.286472755014015146, 70.27551020174914242, -130.5152393712291428 ) ) ;
#45209 = DIRECTION ( 'NONE',  ( 1.000000000000000000, 0.000000000000000000, 0.000000000000000000 ) ) ;
#45210 = AXIS2_PLACEMENT_3D ( 'NONE', #68888, #7114, #82093 ) ;
#45211 = CARTESIAN_POINT ( 'NONE',  ( -10.66780431135453000, 89.44155629055205736, 130.1194439449466813 ) ) ;
#45212 = CARTESIAN_POINT ( 'NONE',  ( 113.4461594614341777, -46.68675298423774223, 68.02991099019695298 ) ) ;
#45213 = VERTEX_POINT ( 'NONE', #70969 ) ;
#45214 = ORIENTED_EDGE ( 'NONE', *, *, #16864, .T. ) ;
#45215 = CARTESIAN_POINT ( 'NONE',  ( 12.27464498081148214, 85.83590841536246785, 129.9777558447946149 ) ) ;
#45216 = PLANE ( 'NONE',  #48949 ) ;
#45217 = AXIS2_PLACEMENT_3D ( 'NONE', #38480, #17609, #65311 ) ;
#45218 = CARTESIAN_POINT ( 'NONE',  ( 41.56648329127398966, -27.82844715994070484, 318.9256252759120116 ) ) ;
#45219 = CARTESIAN_POINT ( 'NONE',  ( 100.0993174663912697, -32.47640984694866262, 168.7080903695919858 ) ) ;
#45220 = CIRCLE ( 'NONE', #6083, 2.029999999999997140 ) ;
#45221 = CARTESIAN_POINT ( 'NONE',  ( 107.5667039024470171, -94.77844715994206126, -19.78219314458232247 ) ) ;
#45222 = ORIENTED_EDGE ( 'NONE', *, *, #88611, .F. ) ;
#45223 = ORIENTED_EDGE ( 'NONE', *, *, #82554, .F. ) ;
#45224 = FACE_OUTER_BOUND ( 'NONE', #61423, .T. ) ;
#45225 = ORIENTED_EDGE ( 'NONE', *, *, #27471, .T. ) ;
#45226 = PRODUCT_DEFINITION_SHAPE ( 'NONE', 'NONE',  #61043 ) ;
#45227 = EDGE_LOOP ( 'NONE', ( #7706, #25611, #85824, #38667 ) ) ;
#45228 = DIRECTION ( 'NONE',  ( 0.000000000000000000, -1.000000000000000000, 0.000000000000000000 ) ) ;
#45229 = CARTESIAN_POINT ( 'NONE',  ( 103.3408556358882890, -28.68905057859731755, 176.8530118773259687 ) ) ;
#45230 = DIRECTION ( 'NONE',  ( 0.000000000000000000, 0.000000000000000000, 1.000000000000000000 ) ) ;
#45231 = DIRECTION ( 'NONE',  ( 0.000000000000000000, 0.000000000000000000, 1.000000000000000000 ) ) ;
#45232 = VECTOR ( 'NONE', #47185, 1000.000000000000000 ) ;
#45233 = CARTESIAN_POINT ( 'NONE',  ( 111.0245712168574528, -45.91317361515658035, 17.90029448042019666 ) ) ;
#45234 = ORIENTED_EDGE ( 'NONE', *, *, #2860, .F. ) ;
#45235 = VECTOR ( 'NONE', #31633, 1000.000000000000000 ) ;
#45236 = ADVANCED_FACE ( 'NONE', ( #554 ), #77319, .T. ) ;
#45237 = EDGE_LOOP ( 'NONE', ( #14529, #26654, #33019, #67105 ) ) ;
#45238 = ORIENTED_EDGE ( 'NONE', *, *, #52535, .F. ) ;
#45239 = ADVANCED_FACE ( 'NONE', ( #28254 ), #75974, .F. ) ;
#45240 = AXIS2_PLACEMENT_3D ( 'NONE', #29436, #36702, #69873 ) ;
#45241 = CARTESIAN_POINT ( 'NONE',  ( 112.3000890867684234, -42.99355894011079471, 190.9480903695919665 ) ) ;
#45242 = EDGE_CURVE ( 'NONE', #84780, #23774, #63240, .T. ) ;
#45243 = CARTESIAN_POINT ( 'NONE',  ( 98.84041870859987000, -43.22715631800404879, 91.85848241876892928 ) ) ;
#45244 = CARTESIAN_POINT ( 'NONE',  ( 112.7298150101557894, -27.26422151970076158, 54.65943479971996055 ) ) ;
#45245 = CARTESIAN_POINT ( 'NONE',  ( 208.9149999999999920, 43.68799999999999528, 57.14999999999999858 ) ) ;
#45246 = LINE ( 'NONE', #72966, #27849 ) ;
#45247 = CARTESIAN_POINT ( 'NONE',  ( 204.2160000000000082, 52.73749999999999716, -44.45000000000000284 ) ) ;
#45248 = CARTESIAN_POINT ( 'NONE',  ( 102.0818258798731506, -27.57325825325154867, 141.4727681330539895 ) ) ;
#45249 = VECTOR ( 'NONE', #37821, 1000.000000000000000 ) ;
#45250 = FACE_OUTER_BOUND ( 'NONE', #40572, .T. ) ;
#45251 = ORIENTED_EDGE ( 'NONE', *, *, #10248, .T. ) ;
#45252 = DIRECTION ( 'NONE',  ( -6.831565154159360295E-14, 1.000000000000000000, 0.000000000000000000 ) ) ;
#45254 = ORIENTED_EDGE ( 'NONE', *, *, #22463, .T. ) ;
#45253 = EDGE_CURVE ( 'NONE', #43903, #47547, #175, .T. ) ;
#45255 = ADVANCED_FACE ( 'NONE', ( #70509 ), #5276, .F. ) ;
#45256 = ORIENTED_EDGE ( 'NONE', *, *, #57810, .F. ) ;
#45257 = CARTESIAN_POINT ( 'NONE',  ( 164.9190312289453004, -35.91149509760637670, 313.9678068554149490 ) ) ;
#45258 = VERTEX_POINT ( 'NONE', #30101 ) ;
#45259 = EDGE_LOOP ( 'NONE', ( #46274, #67176, #28951, #52903, #44444 ) ) ;
#45260 = EDGE_CURVE ( 'NONE', #85158, #52329, #45091, .T. ) ;
#45261 = EDGE_CURVE ( 'NONE', #64426, #69399, #30652, .T. ) ;
#45262 = DIRECTION ( 'NONE',  ( 0.000000000000000000, 0.000000000000000000, 1.000000000000000000 ) ) ;
#45263 = VERTEX_POINT ( 'NONE', #71453 ) ;
#45264 = CARTESIAN_POINT ( 'NONE',  ( 80.06648329127402519, -46.72944715994105991, 10.42562527591094401 ) ) ;
#45265 = CARTESIAN_POINT ( 'NONE',  ( 115.5739025235967716, -42.75529552070533867, 53.33562527591095659 ) ) ;
#45266 = DIRECTION ( 'NONE',  ( -7.867884063170659983E-16, 0.000000000000000000, 1.000000000000000000 ) ) ;
#45267 = ADVANCED_FACE ( 'NONE', ( #1954, #29647 ), #65510, .T. ) ;
#45268 = DIRECTION ( 'NONE',  ( 0.000000000000000000, 0.000000000000000000, -1.000000000000000000 ) ) ;
#45269 = LINE ( 'NONE', #4848, #38334 ) ;
#45270 = CARTESIAN_POINT ( 'NONE',  ( 97.83387747045368599, -32.00739517038274329, 95.96229194257799122 ) ) ;
#45271 = CARTESIAN_POINT ( 'NONE',  ( 108.1794352217186201, -47.07304438381563472, 198.6613395616249989 ) ) ;
#45272 = DIRECTION ( 'NONE',  ( -0.000000000000000000, 1.000000000000000000, 0.000000000000000000 ) ) ;
#45273 = LINE ( 'NONE', #2631, #80041 ) ;
#45274 = ORIENTED_EDGE ( 'NONE', *, *, #61588, .F. ) ;
#45275 = CARTESIAN_POINT ( 'NONE',  ( 0.000000000000000000, 103.1240000000000236, -190.5000000000000000 ) ) ;
#45276 = CARTESIAN_POINT ( 'NONE',  ( 131.0667039024480118, -58.72944715994098175, 231.5838068554150198 ) ) ;
#45277 = CARTESIAN_POINT ( 'NONE',  ( 163.1543517358360020, -31.62489322948790971, -5.074374724088000832 ) ) ;
#45278 = EDGE_CURVE ( 'NONE', #65138, #85910, #30590, .T. ) ;
#45279 = CYLINDRICAL_SURFACE ( 'NONE', #88360, 4.875000000000017764 ) ;
#45281 = VERTEX_POINT ( 'NONE', #78274 ) ;
#45280 = CARTESIAN_POINT ( 'NONE',  ( 95.35850850670631473, -38.86301786728916596, 201.4699109901969791 ) ) ;
#45282 = CARTESIAN_POINT ( 'NONE',  ( 97.31311150169676694, -38.96077725005761749, 146.5054517158104375 ) ) ;
#45283 = CARTESIAN_POINT ( 'NONE',  ( 109.9662181263222891, -48.24525319228295217, 238.7727681330539724 ) ) ;
#45284 = CARTESIAN_POINT ( 'NONE',  ( 97.57754503199339524, -30.97118795507763167, 121.8803871806729546 ) ) ;
#45285 = CARTESIAN_POINT ( 'NONE',  ( 112.1432778728667614, -28.01507690458955935, 250.6602456620354360 ) ) ;
#45286 = VECTOR ( 'NONE', #35701, 1000.000000000000000 ) ;
#45287 = CARTESIAN_POINT ( 'NONE',  ( 82.78958961022135554, -37.11755991740238159, 6.789748280179635387 ) ) ;
#45288 = DIRECTION ( 'NONE',  ( 1.000000000000000000, 4.299999999999999979E-14, 1.000000000000000078E-15 ) ) ;
#45289 = CARTESIAN_POINT ( 'NONE',  ( 109.6423641557757378, -46.48024981121521648, 263.7815675321390358 ) ) ;
#45290 = ORIENTED_EDGE ( 'NONE', *, *, #52638, .F. ) ;
#45291 = CIRCLE ( 'NONE', #55455, 2.517500000000005844 ) ;
#45292 = VERTEX_POINT ( 'NONE', #64617 ) ;
#45293 = EDGE_LOOP ( 'NONE', ( #11909, #89760, #70655, #78256, #43138, #14161 ) ) ;
#45294 = ORIENTED_EDGE ( 'NONE', *, *, #39219, .T. ) ;
#45295 = CARTESIAN_POINT ( 'NONE',  ( 109.6430121181781630, -46.48008673860459083, 72.78145860822925783 ) ) ;
#45296 = CARTESIAN_POINT ( 'NONE',  ( 100.1775528843425178, -45.37332466565996469, 268.0289586092443415 ) ) ;
#45297 = DIRECTION ( 'NONE',  ( -0.9659258262890675351, 0.000000000000000000, -0.2588190451025234595 ) ) ;
#45298 = CARTESIAN_POINT ( 'NONE',  ( 132.9233478419689334, -34.22821065591859480, 1.829869330583430154 ) ) ;
#45299 = AXIS2_PLACEMENT_3D ( 'NONE', #41533, #56054, #63799 ) ;
#45300 = EDGE_CURVE ( 'NONE', #26394, #19093, #36437, .T. ) ;
#45303 = EDGE_CURVE ( 'NONE', #79111, #51120, #16924, .T. ) ;
#45302 = CARTESIAN_POINT ( 'NONE',  ( 90.31351860656735653, 74.16967745525860778, 76.80536679343944684 ) ) ;
#45301 = DIRECTION ( 'NONE',  ( 0.000000000000000000, 0.000000000000000000, 1.000000000000000000 ) ) ;
#45304 = CARTESIAN_POINT ( 'NONE',  ( 109.8786884439187759, -28.66423582349726118, 209.2324198280769849 ) ) ;
#45305 = ORIENTED_EDGE ( 'NONE', *, *, #74403, .F. ) ;
#45306 = ORIENTED_EDGE ( 'NONE', *, *, #54784, .F. ) ;
#45307 = ORIENTED_EDGE ( 'NONE', *, *, #37294, .T. ) ;
#45308 = CIRCLE ( 'NONE', #68547, 0.5000000000000016653 ) ;
#45309 = FACE_BOUND ( 'NONE', #78453, .T. ) ;
#45310 = CARTESIAN_POINT ( 'NONE',  ( 97.81847205893258490, -40.53396210923573051, 181.6370475531321915 ) ) ;
#45311 = DIRECTION ( 'NONE',  ( -1.000000000000000000, 0.000000000000000000, 0.000000000000000000 ) ) ;
#45312 = CARTESIAN_POINT ( 'NONE',  ( 105.0114852080080254, -45.89751720821543302, 23.82063092494396273 ) ) ;
#45313 = AXIS2_PLACEMENT_3D ( 'NONE', #12566, #47505, #13017 ) ;
#45314 = CARTESIAN_POINT ( 'NONE',  ( 117.8738102209306362, 82.96450994655477018, 12.70000000000123208 ) ) ;
#45315 = DIRECTION ( 'NONE',  ( -1.000000000000000078E-15, 1.000000000000000083E-30, 1.000000000000000000 ) ) ;
#45316 = CARTESIAN_POINT ( 'NONE',  ( 107.0664832912739541, -36.72944715994095333, 307.1356252759109680 ) ) ;
#45317 = VERTEX_POINT ( 'NONE', #71003 ) ;
#45318 = LINE ( 'NONE', #60293, #85454 ) ;
#45319 = ORIENTED_EDGE ( 'NONE', *, *, #51306, .F. ) ;
#45320 = CARTESIAN_POINT ( 'NONE',  ( 44.45000000000000284, 69.84999999999999432, 219.0749999999999886 ) ) ;
#45321 = CARTESIAN_POINT ( 'NONE',  ( 103.0685998583681311, -29.61280089403793525, 58.30237608387695047 ) ) ;
#45322 = CARTESIAN_POINT ( 'NONE',  ( 136.4140944162825804, -17.29397280667294012, 7.245803660783974642 ) ) ;
#45323 = FACE_OUTER_BOUND ( 'NONE', #81044, .T. ) ;
#45324 = CARTESIAN_POINT ( 'NONE',  ( -12.27294214581303500, 85.84208941621251654, 117.9191027095085218 ) ) ;
#45325 = EDGE_LOOP ( 'NONE', ( #77984, #38017, #54026, #68675, #22301 ) ) ;
#45326 = CARTESIAN_POINT ( 'NONE',  ( 51.56670390244683944, -33.35206098992766499, 117.4678068554150485 ) ) ;
#45327 = CARTESIAN_POINT ( 'NONE',  ( 119.7718215552501704, 55.36764569511297651, -51.95798173397368203 ) ) ;
#45328 = CIRCLE ( 'NONE', #85966, 1.000000000000000888 ) ;
#45329 = ORIENTED_EDGE ( 'NONE', *, *, #5463, .F. ) ;
#45330 = CARTESIAN_POINT ( 'NONE',  ( 103.3623838164489541, -47.14379949381606849, 102.3165776568629752 ) ) ;
#45331 = VERTEX_POINT ( 'NONE', #36477 ) ;
#45332 = CARTESIAN_POINT ( 'NONE',  ( 99.45175552060571533, -32.86007347668476086, 50.37527697093396739 ) ) ;
#45333 = DIRECTION ( 'NONE',  ( 0.7071067811868672059, 0.7071067811862279395, 6.612322855857878503E-17 ) ) ;
#45334 = CARTESIAN_POINT ( 'NONE',  ( 113.9863769398668296, -43.08488557356476889, 74.65491663922996679 ) ) ;
#45335 = DIRECTION ( 'NONE',  ( 1.000000000000000000, 0.000000000000000000, 1.248844797103662002E-15 ) ) ;
#45336 = FACE_OUTER_BOUND ( 'NONE', #42122, .T. ) ;
#45337 = CARTESIAN_POINT ( 'NONE',  ( 143.2608543353592836, -67.87860957466101297, 246.0727973265990158 ) ) ;
#45338 = EDGE_CURVE ( 'NONE', #6564, #59781, #37359, .T. ) ;
#45339 = CARTESIAN_POINT ( 'NONE',  ( 118.2318068709390815, -40.77392476355825579, 19.54991099019698453 ) ) ;
#45340 = DIRECTION ( 'NONE',  ( -1.000000000000000000, -1.000000000000000078E-15, -1.000000000000000078E-15 ) ) ;
#45341 = ORIENTED_EDGE ( 'NONE', *, *, #18820, .T. ) ;
#45342 = AXIS2_PLACEMENT_3D ( 'NONE', #11402, #54043, #74522 ) ;
#45343 = CARTESIAN_POINT ( 'NONE',  ( 31.78666935232998725, -36.02818131005891189, -5.074374724088000832 ) ) ;
#45344 = ORIENTED_EDGE ( 'NONE', *, *, #85850, .F. ) ;
#45345 = CARTESIAN_POINT ( 'NONE',  ( -117.9083666784912481, 79.66685870724431595, 12.37533002638040180 ) ) ;
#45346 = VERTEX_POINT ( 'NONE', #65068 ) ;
#45348 = EDGE_CURVE ( 'NONE', #82724, #84701, #64181, .T. ) ;
#45347 = ORIENTED_EDGE ( 'NONE', *, *, #87739, .F. ) ;
#45349 = EDGE_CURVE ( 'NONE', #10055, #69050, #8888, .T. ) ;
#45350 = CARTESIAN_POINT ( 'NONE',  ( 88.90000000000000568, 66.67499999999999716, 342.8999999999999773 ) ) ;
#45351 = EDGE_CURVE ( 'NONE', #48000, #41588, #23314, .T. ) ;
#45352 = EDGE_LOOP ( 'NONE', ( #69723, #7523 ) ) ;
#45353 = CARTESIAN_POINT ( 'NONE',  ( 96.86352172870815025, -32.31225822881502552, 211.0013395616259686 ) ) ;
#45354 = CARTESIAN_POINT ( 'NONE',  ( 138.8167039024479834, -50.82844715994100682, 86.31780685541500020 ) ) ;
#45355 = CARTESIAN_POINT ( 'NONE',  ( 143.2570438357147964, -67.87844715994090450, 245.5376130947089734 ) ) ;
#45356 = CARTESIAN_POINT ( 'NONE',  ( 96.92116189526866776, -32.34237133930066221, 57.01372051400599616 ) ) ;
#45357 = CARTESIAN_POINT ( 'NONE',  ( 97.82506921874286832, -40.54997709253600391, 42.63842632371162722 ) ) ;
#45358 = ORIENTED_EDGE ( 'NONE', *, *, #26500, .F. ) ;
#45359 = CARTESIAN_POINT ( 'NONE',  ( 103.2775475522615665, -27.47504464129099233, 171.3857084645095767 ) ) ;
#45360 = EDGE_CURVE ( 'NONE', #63964, #61092, #42809, .T. ) ;
#45361 = DIRECTION ( 'NONE',  ( 1.000000000000000078E-15, -1.000000000000000000, 0.000000000000000000 ) ) ;
#45362 = ORIENTED_EDGE ( 'NONE', *, *, #68027, .F. ) ;
#45363 = ADVANCED_FACE ( 'NONE', ( #50980 ), #8319, .F. ) ;
#45364 = CIRCLE ( 'NONE', #38125, 5.000000000000004441 ) ;
#45365 = LINE ( 'NONE', #66257, #41638 ) ;
#45366 = CARTESIAN_POINT ( 'NONE',  ( 104.4067455066945200, -46.45769128758091426, 113.3653941873491391 ) ) ;
#45367 = CARTESIAN_POINT ( 'NONE',  ( 116.5858064714421829, -40.92601143571970823, 253.4956252759109532 ) ) ;
#45368 = DIRECTION ( 'NONE',  ( 0.000000000000000000, 0.000000000000000000, -1.000000000000000000 ) ) ;
#45369 = CARTESIAN_POINT ( 'NONE',  ( 99.48898161933328765, -117.4034471599418197, -11.78219314458159239 ) ) ;
#45370 = CARTESIAN_POINT ( 'NONE',  ( 188.5667039024479834, -62.87844715994099687, 170.4678068554149775 ) ) ;
#45371 = EDGE_CURVE ( 'NONE', #11705, #65895, #26238, .T. ) ;
#45372 = CARTESIAN_POINT ( 'NONE',  ( 100.7827017321902758, -30.20819270671951173, 265.0971817328389761 ) ) ;
#45375 = CARTESIAN_POINT ( 'NONE',  ( 117.4257108620837329, -37.68603989742253191, 74.75276813305397638 ) ) ;
#45374 = FACE_BOUND ( 'NONE', #25688, .T. ) ;
#45373 = CIRCLE ( 'NONE', #49728, 10.00000000000000888 ) ;
#45376 = CARTESIAN_POINT ( 'NONE',  ( 118.6191002195142374, 74.28059613835587527, 54.54229135122187699 ) ) ;
#45377 = CARTESIAN_POINT ( 'NONE',  ( 117.2652295300992193, -42.86250289712283745, 128.3956252759109873 ) ) ;
#45378 = ORIENTED_EDGE ( 'NONE', *, *, #27404, .F. ) ;
#45379 = CARTESIAN_POINT ( 'NONE',  ( -46.74837461823508278, 65.31871338851736652, -44.28436222200497241 ) ) ;
#45380 = EDGE_LOOP ( 'NONE', ( #6427, #33175, #70892, #72650 ) ) ;
#45381 = CARTESIAN_POINT ( 'NONE',  ( 1.475953350320055108E-14, 239.0000000000000000, 90.07542076772557493 ) ) ;
#45382 = DIRECTION ( 'NONE',  ( 1.776356839400250465E-15, 0.000000000000000000, 1.000000000000000000 ) ) ;
#45383 = FACE_OUTER_BOUND ( 'NONE', #87092, .T. ) ;
#45384 = EDGE_LOOP ( 'NONE', ( #57117, #7564, #78992, #11405, #65365 ) ) ;
#45385 = ADVANCED_FACE ( 'NONE', ( #5072 ), #65943, .F. ) ;
#45386 = CARTESIAN_POINT ( 'NONE',  ( 91.91125933621943034, -104.2784471599418339, -11.78219314458200984 ) ) ;
#45388 = VERTEX_POINT ( 'NONE', #25971 ) ;
#45387 = CARTESIAN_POINT ( 'NONE',  ( 103.2628093650484828, -47.15753175352042348, 97.28610146638693834 ) ) ;
#45389 = FACE_OUTER_BOUND ( 'NONE', #49291, .T. ) ;
#45390 = CYLINDRICAL_SURFACE ( 'NONE', #5539, 0.9999999999991942001 ) ;
#45391 = CARTESIAN_POINT ( 'NONE',  ( 81.80795390244800558, -42.97311385574014508, 231.5838068554169524 ) ) ;
#45392 = ORIENTED_EDGE ( 'NONE', *, *, #36972, .T. ) ;
#45393 = CARTESIAN_POINT ( 'NONE',  ( 113.0897370140187235, -28.19324317000061697, 129.5870538473399449 ) ) ;
#45394 = DIRECTION ( 'NONE',  ( 1.000000000000000000, 0.000000000000000000, 0.000000000000000000 ) ) ;
#45395 = AXIS2_PLACEMENT_3D ( 'NONE', #76260, #48977, #1309 ) ;
#45396 = CARTESIAN_POINT ( 'NONE',  ( 149.4532656544377289, -72.54365454176046057, 543.8623766218582887 ) ) ;
#45397 = DIRECTION ( 'NONE',  ( -1.000000000000000000, 0.000000000000000000, 0.000000000000000000 ) ) ;
#45398 = ORIENTED_EDGE ( 'NONE', *, *, #25806, .F. ) ;
#45399 = AXIS2_PLACEMENT_3D ( 'NONE', #86563, #66089, #29364 ) ;
#45400 = EDGE_LOOP ( 'NONE', ( #72328, #30265 ) ) ;
#45401 = DIRECTION ( 'NONE',  ( 1.000000000000000078E-15, -1.000000000000000083E-30, -1.000000000000000000 ) ) ;
#45402 = LINE ( 'NONE', #79520, #25112 ) ;
#45403 = CARTESIAN_POINT ( 'NONE',  ( 0.000000000000000000, 0.000000000000000000, 0.000000000000000000 ) ) ;
#45406 = ADVANCED_FACE ( 'NONE', ( #59568, #10986 ), #86861, .T. ) ;
#45405 = LINE ( 'NONE', #37278, #3586 ) ;
#45404 = FACE_OUTER_BOUND ( 'NONE', #33508, .T. ) ;
#45407 = DIRECTION ( 'NONE',  ( -0.000000000000000000, 1.000000000000000000, -0.000000000000000000 ) ) ;
#45408 = AXIS2_PLACEMENT_3D ( 'NONE', #21549, #89245, #49221 ) ;
#45409 = EDGE_LOOP ( 'NONE', ( #84225, #50404, #12166, #19128 ) ) ;
#45410 = DIRECTION ( 'NONE',  ( -0.7071067811578587436, 0.7071067812152364018, 0.000000000000000000 ) ) ;
#45411 = CARTESIAN_POINT ( 'NONE',  ( 104.6152064257953640, -27.26083179018629465, 196.2784824187679362 ) ) ;
#45413 = ORIENTED_EDGE ( 'NONE', *, *, #26843, .T. ) ;
#45412 = DIRECTION ( 'NONE',  ( 0.9068632946707805287, -0.4214249218767882610, 9.061988307341536250E-16 ) ) ;
#45414 = CARTESIAN_POINT ( 'NONE',  ( 97.55373691267115532, -39.00345059616618215, 52.51276813305294411 ) ) ;
#45415 = FACE_OUTER_BOUND ( 'NONE', #25455, .T. ) ;
#45416 = DIRECTION ( 'NONE',  ( 0.000000000000000000, 1.000000000000000000, 0.000000000000000000 ) ) ;
#45417 = CARTESIAN_POINT ( 'NONE',  ( 182.5667039024480118, -32.29483332968450782, -5.074374724088000832 ) ) ;
#45418 = ORIENTED_EDGE ( 'NONE', *, *, #65102, .F. ) ;
#45419 = ADVANCED_FACE ( 'NONE', ( #25067, #60468 ), #66849, .F. ) ;
#45420 = DIRECTION ( 'NONE',  ( -3.100000000000000258E-29, 3.100000000000000044E-14, 1.000000000000000000 ) ) ;
#45421 = ORIENTED_EDGE ( 'NONE', *, *, #34811, .F. ) ;
#45422 = ORIENTED_EDGE ( 'NONE', *, *, #85700, .F. ) ;
#45423 = CARTESIAN_POINT ( 'NONE',  ( 112.6928898907800090, -44.25407833457246909, 184.5311071154209799 ) ) ;
#45425 = EDGE_CURVE ( 'NONE', #43762, #223, #17365, .T. ) ;
#45424 = VECTOR ( 'NONE', #28424, 1000.000000000000000 ) ;
#45426 = CARTESIAN_POINT ( 'NONE',  ( 116.3176178399231873, -32.93748434060082531, 55.13562527591098217 ) ) ;
#45427 = CARTESIAN_POINT ( 'NONE',  ( -100.5986936721440230, 85.85000629251467785, 83.21537498884013928 ) ) ;
#45428 = VECTOR ( 'NONE', #36460, 1000.000000000000000 ) ;
#45429 = CYLINDRICAL_SURFACE ( 'NONE', #88165, 2.517500000000000071 ) ;
#45430 = CARTESIAN_POINT ( 'NONE',  ( 188.5667039024479834, -67.87844715994100397, 288.3428068554150059 ) ) ;
#45431 = VERTEX_POINT ( 'NONE', #59124 ) ;
#45432 = CYLINDRICAL_SURFACE ( 'NONE', #5830, 3.300000000000000711 ) ;
#45433 = CARTESIAN_POINT ( 'NONE',  ( 104.4836364144456979, -26.98054529041288419, 36.28151591486695793 ) ) ;
#45434 = ORIENTED_EDGE ( 'NONE', *, *, #77160, .F. ) ;
#45435 = CARTESIAN_POINT ( 'NONE',  ( 100.0388059118472341, -29.01104360887432776, 285.6641967044823787 ) ) ;
#45436 = CARTESIAN_POINT ( 'NONE',  ( 12.26894765557485023, 85.85687052802856556, 117.9195186832830871 ) ) ;
#45437 = VERTEX_POINT ( 'NONE', #52731 ) ;
#45438 =( LENGTH_UNIT ( ) NAMED_UNIT ( * ) SI_UNIT ( .MILLI., .METRE. ) );
#45439 = DIRECTION ( 'NONE',  ( -1.000000000000000078E-15, 1.000000000000000083E-30, 1.000000000000000000 ) ) ;
#45440 = CARTESIAN_POINT ( 'NONE',  ( -215.9000000000000057, 53.97500000000000142, 50.79999999999999716 ) ) ;
#45441 = FACE_OUTER_BOUND ( 'NONE', #11387, .T. ) ;
#45442 = CARTESIAN_POINT ( 'NONE',  ( 117.9939971868874125, -34.78344139941312108, 194.9546728949589749 ) ) ;
#45443 = CARTESIAN_POINT ( 'NONE',  ( 3.260455919141270087, 70.37212065169552488, 118.3117458384234624 ) ) ;
#45444 = ORIENTED_EDGE ( 'NONE', *, *, #78228, .T. ) ;
#45445 = CARTESIAN_POINT ( 'NONE',  ( 96.87875409107806490, -32.32403320637130406, 57.01372051400599616 ) ) ;
#45446 = CARTESIAN_POINT ( 'NONE',  ( -30.86579703273522668, 65.60000000000000853, 73.54054752236280024 ) ) ;
#45447 = AXIS2_PLACEMENT_3D ( 'NONE', #62072, #1664, #70241 ) ;
#45448 = ORIENTED_EDGE ( 'NONE', *, *, #20090, .T. ) ;
#45449 = EDGE_CURVE ( 'NONE', #36567, #23413, #4182, .T. ) ;
#45451 = ORIENTED_EDGE ( 'NONE', *, *, #41674, .T. ) ;
#45450 = EDGE_CURVE ( 'NONE', #74767, #44052, #5964, .T. ) ;
#45452 = AXIS2_PLACEMENT_3D ( 'NONE', #75498, #75940, #20088 ) ;
#45453 = ADVANCED_FACE ( 'NONE', ( #39142 ), #51854, .F. ) ;
#45454 = CARTESIAN_POINT ( 'NONE',  ( 82.45999417310882507, -17.37149686611859423, 2.653088969735680536 ) ) ;
#45455 = DIRECTION ( 'NONE',  ( 0.000000000000000000, 0.000000000000000000, -1.000000000000000000 ) ) ;
#45456 = CARTESIAN_POINT ( 'NONE',  ( 125.5177273812784762, -131.0330679306342461, 55.21780685541800437 ) ) ;
#45457 = CARTESIAN_POINT ( 'NONE',  ( 115.3203086601475320, -34.12650808536288594, 126.8757094172099613 ) ) ;
#45458 = CARTESIAN_POINT ( 'NONE',  ( 117.4960079497888472, -36.12755493457860467, 224.8727681330539667 ) ) ;
#45459 = LINE ( 'NONE', #25042, #2939 ) ;
#45460 = ORIENTED_EDGE ( 'NONE', *, *, #8266, .T. ) ;
#45461 = EDGE_CURVE ( 'NONE', #30848, #78871, #12338, .T. ) ;
#45462 = CARTESIAN_POINT ( 'NONE',  ( 34.92499999999999716, 82.54999999999999716, 302.8950000000000387 ) ) ;
#45463 = VERTEX_POINT ( 'NONE', #52289 ) ;
#45464 = ORIENTED_EDGE ( 'NONE', *, *, #64868, .F. ) ;
#45465 = VECTOR ( 'NONE', #42891, 1000.000000000000000 ) ;
#45466 = LINE ( 'NONE', #86837, #85131 ) ;
#45467 = ORIENTED_EDGE ( 'NONE', *, *, #74422, .T. ) ;
#45468 = ORIENTED_EDGE ( 'NONE', *, *, #51478, .F. ) ;
#45469 = CARTESIAN_POINT ( 'NONE',  ( 116.7802871385218282, -39.10473973501323286, 9.635625275910941312 ) ) ;
#45470 = FACE_OUTER_BOUND ( 'NONE', #71791, .T. ) ;
#45471 = CARTESIAN_POINT ( 'NONE',  ( 90.44969454456405344, -22.62993780205715311, 239.5838068554169809 ) ) ;
#45472 = ADVANCED_FACE ( 'NONE', ( #73661 ), #80052, .F. ) ;
#45473 = CARTESIAN_POINT ( 'NONE',  ( 113.1668408875787435, -30.74627054922163438, 148.8667055423629790 ) ) ;
#45474 = CARTESIAN_POINT ( 'NONE',  ( 116.7680724212777079, -31.33574231247038355, 29.24229194257799236 ) ) ;
#45475 = ORIENTED_EDGE ( 'NONE', *, *, #17502, .T. ) ;
#45476 = FACE_OUTER_BOUND ( 'NONE', #8840, .T. ) ;
#45477 = ORIENTED_EDGE ( 'NONE', *, *, #49334, .T. ) ;
#45478 = CARTESIAN_POINT ( 'NONE',  ( 4.163101094985349692E-14, 120.6499999999999915, -98.60478223830740774 ) ) ;
#45479 = ORIENTED_EDGE ( 'NONE', *, *, #52968, .F. ) ;
#45480 = CARTESIAN_POINT ( 'NONE',  ( 141.8664832912729992, -71.52944715994142655, 342.9256252759109884 ) ) ;
#45481 = CARTESIAN_POINT ( 'NONE',  ( 183.5150000000000148, 52.73749999999999716, -44.45000000000000284 ) ) ;
#45482 = CARTESIAN_POINT ( 'NONE',  ( 97.81219346325542574, -40.51865836701575319, 131.6357308845718421 ) ) ;
#45483 = VECTOR ( 'NONE', #73781, 1000.000000000000114 ) ;
#45484 = CARTESIAN_POINT ( 'NONE',  ( 164.9667039024473922, -26.71338133338732845, 313.9678068554149490 ) ) ;
#45485 = ORIENTED_EDGE ( 'NONE', *, *, #75533, .T. ) ;
#45486 = CARTESIAN_POINT ( 'NONE',  ( 115.4624701790509391, -43.00605189524043936, 28.31562527591097123 ) ) ;
#45487 = CARTESIAN_POINT ( 'NONE',  ( 106.6049252239556608, -25.63961115983148176, 36.09753003781596448 ) ) ;
#45488 = VECTOR ( 'NONE', #15013, 1000.000000000000000 ) ;
#45490 = DIRECTION ( 'NONE',  ( 1.000000000000000000, 0.000000000000000000, 0.000000000000000000 ) ) ;
#45489 = LINE ( 'NONE', #71900, #83991 ) ;
#45491 = CYLINDRICAL_SURFACE ( 'NONE', #65570, 38.10000000000000142 ) ;
#45492 = CARTESIAN_POINT ( 'NONE',  ( 0.000000000000000000, 184.0000000000000000, 101.0189074266571794 ) ) ;
#45493 = DIRECTION ( 'NONE',  ( -1.000000000000000000, 0.000000000000000000, -9.713237310806269221E-16 ) ) ;
#45494 = LINE ( 'NONE', #10997, #77971 ) ;
#45495 = CARTESIAN_POINT ( 'NONE',  ( 145.9875769262907284, -101.1106333528077954, 247.5368628348080051 ) ) ;
#45496 = CARTESIAN_POINT ( 'NONE',  ( 102.3692588328596571, -47.63350050119395007, 287.2527681330535643 ) ) ;
#45497 = CARTESIAN_POINT ( 'NONE',  ( 107.6544996609965352, -47.76702919738148267, 193.6308633711489620 ) ) ;
#45498 = CARTESIAN_POINT ( 'NONE',  ( 97.33132060198839497, -32.84282867815538509, 37.02419670448292521 ) ) ;
#45501 = ADVANCED_FACE ( 'NONE', ( #17808 ), #74118, .T. ) ;
#45500 = CARTESIAN_POINT ( 'NONE',  ( 20.03715912545820288, -46.82818131006190043, 300.4678068554150059 ) ) ;
#45499 = CARTESIAN_POINT ( 'NONE',  ( 63.06670390244700997, -79.67844715994098692, 85.21780685541799016 ) ) ;
#45502 = PLANE ( 'NONE',  #56632 ) ;
#45503 = AXIS2_PLACEMENT_3D ( 'NONE', #57179, #84481, #72173 ) ;
#45504 = VECTOR ( 'NONE', #28963, 1000.000000000000000 ) ;
#45505 = EDGE_CURVE ( 'NONE', #51700, #45388, #38686, .T. ) ;
#45506 = CIRCLE ( 'NONE', #6376, 2.116999999999980009 ) ;
#45507 = ORIENTED_EDGE ( 'NONE', *, *, #25161, .T. ) ;
#45508 = FACE_OUTER_BOUND ( 'NONE', #511, .T. ) ;
#45509 = VERTEX_POINT ( 'NONE', #30987 ) ;
#45510 = CARTESIAN_POINT ( 'NONE',  ( 107.2219638487720488, -26.36052190073626988, 76.07657765686298035 ) ) ;
#45512 = ORIENTED_EDGE ( 'NONE', *, *, #3195, .F. ) ;
#45511 = DIRECTION ( 'NONE',  ( 1.000000000000000000, 4.299999999999999979E-14, 1.000000000000000078E-15 ) ) ;
#45513 = VECTOR ( 'NONE', #70544, 1000.000000000000000 ) ;
#45514 = CYLINDRICAL_SURFACE ( 'NONE', #83804, 7.143750000000004263 ) ;
#45515 = CARTESIAN_POINT ( 'NONE',  ( 117.3134009501234658, -34.93240959161192905, 239.9641967044819637 ) ) ;
#45516 = DIRECTION ( 'NONE',  ( -4.237773401492740281E-14, 1.000000000000000000, 0.000000000000000000 ) ) ;
#45517 = FACE_OUTER_BOUND ( 'NONE', #45714, .T. ) ;
#45518 = CARTESIAN_POINT ( 'NONE',  ( 165.2748236753147353, -30.08671355699731009, 193.9678068554149775 ) ) ;
#45519 = DIRECTION ( 'NONE',  ( 0.9068632946707807507, -0.4214249218767880945, 9.080193194566099635E-16 ) ) ;
#45520 = CARTESIAN_POINT ( 'NONE',  ( 133.1862368104815175, -39.33528726900525641, 1.744847506583675045 ) ) ;
#45521 = PLANE ( 'NONE',  #50053 ) ;
#45522 = CARTESIAN_POINT ( 'NONE',  ( 96.28008679191512442, -39.42493101749853679, 166.5213395616259788 ) ) ;
#45523 = ORIENTED_EDGE ( 'NONE', *, *, #43139, .F. ) ;
#45524 = ORIENTED_EDGE ( 'NONE', *, *, #40616, .F. ) ;
#45525 = CARTESIAN_POINT ( 'NONE',  ( 112.8380968919016425, -43.45378765227984275, 104.5730118773259534 ) ) ;
#45526 = ADVANCED_FACE ( 'NONE', ( #67750 ), #87302, .F. ) ;
#45527 = CARTESIAN_POINT ( 'NONE',  ( 63.03715912545732181, -24.89890238295017966, 300.4678068554150627 ) ) ;
#45529 = FACE_OUTER_BOUND ( 'NONE', #83178, .T. ) ;
#45528 = CARTESIAN_POINT ( 'NONE',  ( 106.8648936900573148, -47.09757847023101363, 223.5489586092439538 ) ) ;
#45530 = FACE_BOUND ( 'NONE', #3217, .T. ) ;
#45531 = CARTESIAN_POINT ( 'NONE',  ( 107.0667039024470739, -133.7784471599409528, 24.21780685541800082 ) ) ;
#45532 = CARTESIAN_POINT ( 'NONE',  ( 118.0639734269499854, 75.84278307195158675, 10.79247489890550682 ) ) ;
#45533 = DIRECTION ( 'NONE',  ( 0.000000000000000000, -0.8660254037844390407, 0.4999999999999995004 ) ) ;
#45534 = CARTESIAN_POINT ( 'NONE',  ( 80.06648329127399677, -18.72944715994105991, -5.074374724089057764 ) ) ;
#45535 = CARTESIAN_POINT ( 'NONE',  ( 87.06648329127402519, -56.72944715994104570, 14.67562527591094934 ) ) ;
#45536 = CARTESIAN_POINT ( 'NONE',  ( 116.9962961068553966, -33.62662860631126449, 174.0670538473389399 ) ) ;
#45537 = ORIENTED_EDGE ( 'NONE', *, *, #48325, .T. ) ;
#45538 = EDGE_LOOP ( 'NONE', ( #25693, #24275, #53505, #3934 ) ) ;
#45539 = LINE ( 'NONE', #11504, #22731 ) ;
#45540 = CARTESIAN_POINT ( 'NONE',  ( 116.3212776292296127, -32.94146857471318413, 287.6356252759109680 ) ) ;
#45541 = CARTESIAN_POINT ( 'NONE',  ( 25.56670390244797275, -62.87844715994099687, 168.3428068554150059 ) ) ;
#45542 = CARTESIAN_POINT ( 'NONE',  ( 71.06648329127399677, -18.82844715994099971, 284.9256252759119548 ) ) ;
#45543 = AXIS2_PLACEMENT_3D ( 'NONE', #35251, #77500, #21654 ) ;
#45544 = CARTESIAN_POINT ( 'NONE',  ( 125.8897075496517317, -55.55267141831851774, 14.67562527591099020 ) ) ;
#45545 = CARTESIAN_POINT ( 'NONE',  ( 103.0496837167155491, -26.43166057102584077, 170.3603871806729444 ) ) ;
#45546 = CARTESIAN_POINT ( 'NONE',  ( 136.1031364520942475, -38.57950990141236502, 7.523361336355876006 ) ) ;
#45547 = VERTEX_POINT ( 'NONE', #67289 ) ;
#45550 = VERTEX_POINT ( 'NONE', #60930 ) ;
#45549 = ORIENTED_EDGE ( 'NONE', *, *, #19963, .F. ) ;
#45548 = EDGE_CURVE ( 'NONE', #78672, #36722, #27756, .T. ) ;
#45551 = EDGE_CURVE ( 'NONE', #59341, #25045, #39396, .T. ) ;
#45552 = CARTESIAN_POINT ( 'NONE',  ( -8.690994986491583418, 73.28026231907210786, 118.2373793989773247 ) ) ;
#45553 = DIRECTION ( 'NONE',  ( -0.000000000000000000, -0.000000000000000000, 1.000000000000000000 ) ) ;
#45554 = ADVANCED_FACE ( 'NONE', ( #26419 ), #13678, .F. ) ;
#45555 = CARTESIAN_POINT ( 'NONE',  ( 101.9933011300245340, -45.44587426433803046, 163.1564290691892722 ) ) ;
#45556 = CARTESIAN_POINT ( 'NONE',  ( 113.8488019003066825, -42.10541956792432217, 46.12332846482897253 ) ) ;
#45557 = CARTESIAN_POINT ( 'NONE',  ( 97.81168895331838087, -40.51742574516882200, 287.6356252759109680 ) ) ;
#45558 = VERTEX_POINT ( 'NONE', #76358 ) ;
#45559 = EDGE_CURVE ( 'NONE', #35754, #22170, #54979, .T. ) ;
#45560 = DIRECTION ( 'NONE',  ( 0.000000000000000000, -1.000000000000000000, 0.000000000000000000 ) ) ;
#45561 = FACE_OUTER_BOUND ( 'NONE', #85712, .T. ) ;
#45562 = ORIENTED_EDGE ( 'NONE', *, *, #2024, .T. ) ;
#45563 = ORIENTED_EDGE ( 'NONE', *, *, #32609, .T. ) ;
#45564 = VECTOR ( 'NONE', #89564, 1000.000000000000000 ) ;
#45565 = CARTESIAN_POINT ( 'NONE',  ( 37.03715912545343514, -48.62818131006119415, 180.4678068554150911 ) ) ;
#45566 = AXIS2_PLACEMENT_3D ( 'NONE', #68569, #27219, #48529 ) ;
#45567 = EDGE_LOOP ( 'NONE', ( #4594, #66575, #53825, #25419 ) ) ;
#45568 = ORIENTED_EDGE ( 'NONE', *, *, #44027, .T. ) ;
#45569 = CARTESIAN_POINT ( 'NONE',  ( 107.0667039024470029, -74.77844715994095282, 24.21780685541800082 ) ) ;
#45570 = AXIS2_PLACEMENT_3D ( 'NONE', #29331, #84310, #85646 ) ;
#45571 = EDGE_CURVE ( 'NONE', #14989, #51056, #34108, .T. ) ;
#45572 = CARTESIAN_POINT ( 'NONE',  ( 104.7514827670518684, -44.95118086569023319, 21.78099125664900626 ) ) ;
#45574 = CARTESIAN_POINT ( 'NONE',  ( 110.7040309646834970, -48.03441345040916843, 207.8241967044819489 ) ) ;
#45573 = CIRCLE ( 'NONE', #6446, 4.874999999999990230 ) ;
#45575 = CARTESIAN_POINT ( 'NONE',  ( 99.30484619187383544, -29.80227926343058797, 190.7470538473399415 ) ) ;
#45576 = EDGE_CURVE ( 'NONE', #1971, #64816, #28191, .T. ) ;
#45577 = DIRECTION ( 'NONE',  ( 0.04216478779797398074, -0.9991106698809455455, 0.000000000000000000 ) ) ;
#45578 = CARTESIAN_POINT ( 'NONE',  ( 97.22385571422852024, -40.27120027895552568, 262.6013395616254797 ) ) ;
#45579 = DIRECTION ( 'NONE',  ( 1.000000000000000000, 4.299999999999999979E-14, 1.000000000000000078E-15 ) ) ;
#45580 = LINE ( 'NONE', #74661, #25029 ) ;
#45581 = ORIENTED_EDGE ( 'NONE', *, *, #63341, .T. ) ;
#45582 = ORIENTED_EDGE ( 'NONE', *, *, #49597, .F. ) ;
#45583 = DIRECTION ( 'NONE',  ( 0.000000000000000000, 0.000000000000000000, 1.000000000000000000 ) ) ;
#45584 = CARTESIAN_POINT ( 'NONE',  ( 104.3993058286337146, -25.95452033834810024, 240.2575300378159682 ) ) ;
#45585 = ORIENTED_EDGE ( 'NONE', *, *, #39739, .T. ) ;
#45586 = CARTESIAN_POINT ( 'NONE',  ( 116.3504430951951605, -44.09481043651530996, 198.2927681330539542 ) ) ;
#45587 = DIRECTION ( 'NONE',  ( 0.000000000000000000, 0.000000000000000000, -1.000000000000000000 ) ) ;
#45588 = CARTESIAN_POINT ( 'NONE',  ( -1.415542646969860267E-16, 70.24203434096102683, 38.10000000000000142 ) ) ;
#45589 = DIRECTION ( 'NONE',  ( 1.000000000000000078E-15, 1.000000000000000083E-30, -1.000000000000000000 ) ) ;
#45590 = CARTESIAN_POINT ( 'NONE',  ( 184.3595971212628797, -48.62134037874749737, 249.9678068554149775 ) ) ;
#45593 = CARTESIAN_POINT ( 'NONE',  ( 117.8598252335457488, -34.07367295057271406, 10.01848241876795953 ) ) ;
#45592 = FACE_OUTER_BOUND ( 'NONE', #11593, .T. ) ;
#45591 = DIRECTION ( 'NONE',  ( -1.000000000000000000, 0.000000000000000000, 0.000000000000000000 ) ) ;
#45594 = CARTESIAN_POINT ( 'NONE',  ( -187.8075999999999794, 101.5999999999999943, 107.9500000000000028 ) ) ;
#45595 = CARTESIAN_POINT ( 'NONE',  ( 172.5664832912740110, 0.2215528400590013880, 198.9256252759119832 ) ) ;
#45596 = LINE ( 'NONE', #33341, #42636 ) ;
#45597 = CARTESIAN_POINT ( 'NONE',  ( 67.37732175900356424, -137.4831949855723110, 246.5806332000785233 ) ) ;
#45598 = DIRECTION ( 'NONE',  ( -0.8660254037844387076, -0.4999999999999998890, 0.000000000000000000 ) ) ;
#45599 = CARTESIAN_POINT ( 'NONE',  ( -487.2989999999999782, 86.51875000000001137, 94.61194598552339130 ) ) ;
#45601 = ORIENTED_EDGE ( 'NONE', *, *, #48104, .F. ) ;
#45600 = CARTESIAN_POINT ( 'NONE',  ( 101.1610018191305187, -28.81527687121307224, 195.5838068554172366 ) ) ;
#45602 = CARTESIAN_POINT ( 'NONE',  ( 135.4471649165409985, -21.11090284777780113, 7.925007058955543471 ) ) ;
#45603 = CARTESIAN_POINT ( 'NONE',  ( 117.2137812332333766, -41.17104435167765075, 208.4861014663869696 ) ) ;
#45604 = CARTESIAN_POINT ( 'NONE',  ( 116.5333143132291269, -32.36348817604392991, 100.1699109901969535 ) ) ;
#45605 = CARTESIAN_POINT ( 'NONE',  ( 106.9399153568602259, -47.82816235210678002, 228.5794347997199907 ) ) ;
#45606 = CARTESIAN_POINT ( 'NONE',  ( 50.88849390559370534, -32.11662333284569115, 193.9678068554150911 ) ) ;
#45607 = DIRECTION ( 'NONE',  ( 1.000000000000000000, 4.299999999999999979E-14, 1.000000000000000078E-15 ) ) ;
#45610 = EDGE_CURVE ( 'NONE', #36943, #82153, #35009, .T. ) ;
#45609 = CARTESIAN_POINT ( 'NONE',  ( 110.6285399601922848, -46.11599178581295888, 38.86459524923592568 ) ) ;
#45608 = CYLINDRICAL_SURFACE ( 'NONE', #81207, 17.00000000000000000 ) ;
#45611 = FACE_OUTER_BOUND ( 'NONE', #15265, .T. ) ;
#45612 = CARTESIAN_POINT ( 'NONE',  ( 107.0667039024470313, -104.2784471599418197, -11.78219314458200984 ) ) ;
#45613 = VECTOR ( 'NONE', #58813, 1000.000000000000000 ) ;
#45614 = CARTESIAN_POINT ( 'NONE',  ( 97.80456843721749749, -40.50002885529080743, 66.63459087925632218 ) ) ;
#45615 = AXIS2_PLACEMENT_3D ( 'NONE', #45710, #59797, #30774 ) ;
#45616 = EDGE_CURVE ( 'NONE', #67284, #29066, #54089, .T. ) ;
#45617 = ORIENTED_EDGE ( 'NONE', *, *, #69947, .T. ) ;
#45618 = ORIENTED_EDGE ( 'NONE', *, *, #88880, .T. ) ;
#45619 = CARTESIAN_POINT ( 'NONE',  ( 115.4827349520354858, -33.38588942772360468, 98.56194363760096167 ) ) ;
#45621 = ORIENTED_EDGE ( 'NONE', *, *, #62027, .T. ) ;
#45620 = CARTESIAN_POINT ( 'NONE',  ( -5.616699032889719945, 93.94804372660796332, -130.4356411629705121 ) ) ;
#45622 = CARTESIAN_POINT ( 'NONE',  ( 104.9672558511366276, -25.09151557957609668, 121.2184824187679766 ) ) ;
#45623 = DIRECTION ( 'NONE',  ( -0.04216478779797398074, 0.9991106698809455455, 0.000000000000000000 ) ) ;
#45624 = CARTESIAN_POINT ( 'NONE',  ( 77.45242755740714813, -17.85322059724255084, 6.943211687812394395 ) ) ;
#45625 = LINE ( 'NONE', #46077, #79566 ) ;
#45626 = CARTESIAN_POINT ( 'NONE',  ( 257.5940999999999690, 52.73749999999999716, -2.903194600000015502 ) ) ;
#45627 = CARTESIAN_POINT ( 'NONE',  ( 107.5734549334945456, -47.83597508069291138, 42.61276813305398292 ) ) ;
#45628 = VERTEX_POINT ( 'NONE', #47285 ) ;
#45629 = ORIENTED_EDGE ( 'NONE', *, *, #86607, .T. ) ;
#45630 = ORIENTED_EDGE ( 'NONE', *, *, #55961, .F. ) ;
#45631 = VECTOR ( 'NONE', #35862, 1000.000000000000000 ) ;
#45632 = EDGE_CURVE ( 'NONE', #29419, #83459, #8951, .T. ) ;
#45633 = AXIS2_PLACEMENT_3D ( 'NONE', #56242, #15397, #84448 ) ;
#45634 = CARTESIAN_POINT ( 'NONE',  ( -31.75000000000000000, 8.255000000000000782, -3.174999999999779998 ) ) ;
#45635 = VECTOR ( 'NONE', #75280, 1000.000000000000000 ) ;
#45637 = CARTESIAN_POINT ( 'NONE',  ( 57.56670390244744340, -48.82844715994040286, 173.2178068554150911 ) ) ;
#45636 = CARTESIAN_POINT ( 'NONE',  ( 116.1942131220465768, -33.21547736372282600, 135.1184824187679396 ) ) ;
#45638 = CIRCLE ( 'NONE', #87752, 50.79999999999999716 ) ;
#45639 = LINE ( 'NONE', #37530, #78284 ) ;
#45640 = CARTESIAN_POINT ( 'NONE',  ( 9.569027000640168978, 74.15895453169299856, -130.2061718688152610 ) ) ;
#45642 = CARTESIAN_POINT ( 'NONE',  ( 47.62500000000000000, 73.02500000000000568, 219.0749999999999886 ) ) ;
#45641 = VECTOR ( 'NONE', #34672, 1000.000000000000000 ) ;
#45643 = AXIS2_PLACEMENT_3D ( 'NONE', #48208, #70479, #55465 ) ;
#45644 = CARTESIAN_POINT ( 'NONE',  ( 74.49778344313774880, 84.62843115047674303, 92.22587532767886387 ) ) ;
#45645 = LINE ( 'NONE', #15857, #74773 ) ;
#45646 = CARTESIAN_POINT ( 'NONE',  ( 117.4328057974123567, -37.95573561897359838, 53.73276813305394484 ) ) ;
#45647 = VERTEX_POINT ( 'NONE', #48178 ) ;
#45648 = VERTEX_POINT ( 'NONE', #47735 ) ;
#45649 = ADVANCED_FACE ( 'NONE', ( #5537 ), #69099, .F. ) ;
#45650 = CARTESIAN_POINT ( 'NONE',  ( 12.70000000000000107, 82.54999999999999716, 129.9368274816650910 ) ) ;
#45651 = CARTESIAN_POINT ( 'NONE',  ( 126.8694562117858595, 48.85726633079141834, 30.80605124856342414 ) ) ;
#45652 = DIRECTION ( 'NONE',  ( 0.000000000000000000, 0.000000000000000000, 1.000000000000000000 ) ) ;
#45653 = CARTESIAN_POINT ( 'NONE',  ( 104.5146602464430714, -28.97587216416100375, 163.1480903695919551 ) ) ;
#45654 = ADVANCED_FACE ( 'NONE', ( #75011 ), #5988, .F. ) ;
#45655 = AXIS2_PLACEMENT_3D ( 'NONE', #10645, #38350, #32417 ) ;
#45656 = DIRECTION ( 'NONE',  ( 0.000000000000000000, 0.000000000000000000, 1.000000000000000000 ) ) ;
#45657 = EDGE_LOOP ( 'NONE', ( #24187, #3037, #14503, #4077 ) ) ;
#45658 = EDGE_LOOP ( 'NONE', ( #53693, #60605, #17366, #74259, #20502 ) ) ;
#45659 = CARTESIAN_POINT ( 'NONE',  ( 89.60916260784479448, 224.4999999999999432, 134.1927865330827103 ) ) ;
#45660 = EDGE_LOOP ( 'NONE', ( #28734, #52369, #54292, #16620, #30191 ) ) ;
#45661 = EDGE_LOOP ( 'NONE', ( #86697, #78894, #64649, #73494 ) ) ;
#45662 = FACE_OUTER_BOUND ( 'NONE', #19857, .T. ) ;
#45663 = EDGE_CURVE ( 'NONE', #16775, #88540, #19593, .T. ) ;
#45664 = CARTESIAN_POINT ( 'NONE',  ( 110.7647657470428157, -46.09926102310604534, 169.3072975916109613 ) ) ;
#45665 = DIRECTION ( 'NONE',  ( 0.000000000000000000, 0.000000000000000000, -1.000000000000000000 ) ) ;
#45666 = DIRECTION ( 'NONE',  ( 0.000000000000000000, 0.000000000000000000, 1.000000000000000000 ) ) ;
#45667 = AXIS2_PLACEMENT_3D ( 'NONE', #32073, #31177, #24824 ) ;
#45668 = CARTESIAN_POINT ( 'NONE',  ( 116.3212776292269552, -32.94146857470667555, 79.13562527591095375 ) ) ;
#45669 = EDGE_LOOP ( 'NONE', ( #84520, #64485, #59608, #59778, #59795 ) ) ;
#45670 = EDGE_LOOP ( 'NONE', ( #57657, #27653, #5158, #88902 ) ) ;
#45671 = VECTOR ( 'NONE', #50203, 1000.000000000000000 ) ;
#45672 = VERTEX_POINT ( 'NONE', #62270 ) ;
#45673 = VERTEX_POINT ( 'NONE', #89096 ) ;
#45674 = EDGE_CURVE ( 'NONE', #74757, #9163, #35046, .T. ) ;
#45675 = CARTESIAN_POINT ( 'NONE',  ( 115.5744916924636954, -35.14366089088881751, 201.8033284648299457 ) ) ;
#45676 = CARTESIAN_POINT ( 'NONE',  ( 114.0369391955824483, -28.94747385925965943, 114.4956252759109816 ) ) ;
#45677 = CARTESIAN_POINT ( 'NONE',  ( 95.37363933861277587, -34.96150835630652409, 71.20705384733993526 ) ) ;
#45678 = ADVANCED_FACE ( 'NONE', ( #6418, #21402 ), #20946, .F. ) ;
#45679 = CARTESIAN_POINT ( 'NONE',  ( 90.06670390244703128, -104.2784471599417770, -9.937637710810031777 ) ) ;
#45680 = DIRECTION ( 'NONE',  ( 0.000000000000000000, 0.000000000000000000, -1.000000000000000000 ) ) ;
#45681 = CARTESIAN_POINT ( 'NONE',  ( 97.38209261381841486, -42.05735084626116560, 172.7146728949589942 ) ) ;
#45683 = EDGE_CURVE ( 'NONE', #31932, #35863, #49074, .T. ) ;
#45682 = FACE_OUTER_BOUND ( 'NONE', #71731, .T. ) ;
#45684 = ORIENTED_EDGE ( 'NONE', *, *, #63743, .T. ) ;
#45685 = CARTESIAN_POINT ( 'NONE',  ( 274.0659999999999741, 36.86249999999999716, -58.73749999999999716 ) ) ;
#45686 = ORIENTED_EDGE ( 'NONE', *, *, #51920, .T. ) ;
#45687 = VERTEX_POINT ( 'NONE', #14591 ) ;
#45688 = CARTESIAN_POINT ( 'NONE',  ( 49.35211078756498893, -35.65087443492551245, -5.074374724088000832 ) ) ;
#45689 = LINE ( 'NONE', #24834, #5356 ) ;
#45690 = ORIENTED_EDGE ( 'NONE', *, *, #56377, .F. ) ;
#45691 = AXIS2_PLACEMENT_3D ( 'NONE', #2337, #58611, #64558 ) ;
#45692 = CARTESIAN_POINT ( 'NONE',  ( 74.38348329127296665, -71.52944715994141234, 352.4506252759078961 ) ) ;
#45693 = ORIENTED_EDGE ( 'NONE', *, *, #16394, .F. ) ;
#45694 = AXIS2_PLACEMENT_3D ( 'NONE', #53218, #68682, #47314 ) ;
#45695 = AXIS2_PLACEMENT_3D ( 'NONE', #20324, #89819, #20757 ) ;
#45696 = PLANE ( 'NONE',  #75424 ) ;
#45697 = CARTESIAN_POINT ( 'NONE',  ( 116.1238663722925253, -29.08717671455551468, 74.38419670448293175 ) ) ;
#45698 = CARTESIAN_POINT ( 'NONE',  ( -2.818947171159547960, 70.15983271286830814, 130.5258393308032225 ) ) ;
#45699 = AXIS2_PLACEMENT_3D ( 'NONE', #64492, #57662, #50850 ) ;
#45700 = LINE ( 'NONE', #80274, #88431 ) ;
#45701 = DIRECTION ( 'NONE',  ( -0.4999999999999931166, -0.8660254037844425934, 2.684678751731770391E-14 ) ) ;
#45702 = CARTESIAN_POINT ( 'NONE',  ( 103.5129713284349720, -46.47169217660404428, 97.28610146638794731 ) ) ;
#45704 = CARTESIAN_POINT ( 'NONE',  ( 111.4081670832168953, -47.72935575799004226, 168.8756252759109486 ) ) ;
#45703 = DIRECTION ( 'NONE',  ( 0.7071067811865398012, 0.000000000000000000, 0.7071067811865552333 ) ) ;
#45705 = CARTESIAN_POINT ( 'NONE',  ( 100.9528829496750717, -28.70842646451748692, 60.59413823283402678 ) ) ;
#45706 = PLANE ( 'NONE',  #1706 ) ;
#45707 = ORIENTED_EDGE ( 'NONE', *, *, #56356, .T. ) ;
#45708 = DIRECTION ( 'NONE',  ( -1.000000000000000000, -4.554376769437570034E-14, 0.000000000000000000 ) ) ;
#45709 = AXIS2_PLACEMENT_3D ( 'NONE', #60708, #67990, #81642 ) ;
#45710 = CARTESIAN_POINT ( 'NONE',  ( 235.9910211978967141, -11.20588573913161134, -10.97647784993501396 ) ) ;
#45711 = DIRECTION ( 'NONE',  ( 3.062684205862500216E-15, 0.000000000000000000, -1.000000000000000000 ) ) ;
#45712 = CYLINDRICAL_SURFACE ( 'NONE', #49152, 2.500000000000002220 ) ;
#45714 = EDGE_LOOP ( 'NONE', ( #36511, #7373, #83, #5517 ) ) ;
#45713 = CARTESIAN_POINT ( 'NONE',  ( 104.4426401758756100, -26.59425533393106633, 200.2784824187679362 ) ) ;
#45715 = CARTESIAN_POINT ( 'NONE',  ( 107.0667039024467329, -54.09444715994091979, 196.2188068554169433 ) ) ;
#45716 = CARTESIAN_POINT ( 'NONE',  ( 96.95773401446056994, -39.36581715674629578, 272.5299109901966972 ) ) ;
#45717 = CARTESIAN_POINT ( 'NONE',  ( 95.73188602939242742, -40.35408750269280631, 127.5727681330539554 ) ) ;
#45718 = DIRECTION ( 'NONE',  ( 1.000000000000000078E-15, -1.000000000000000083E-30, -1.000000000000000000 ) ) ;
#45719 = CARTESIAN_POINT ( 'NONE',  ( 12.59759614370980785, 84.21308071816548591, -129.9468022370901679 ) ) ;
#45720 = CIRCLE ( 'NONE', #55833, 7.999999999999992895 ) ;
#45721 = FACE_BOUND ( 'NONE', #37465, .T. ) ;
#45722 = CARTESIAN_POINT ( 'NONE',  ( 108.3328468486845821, -46.73492755383839636, 263.6773967463404915 ) ) ;
#45723 = ORIENTED_EDGE ( 'NONE', *, *, #24921, .T. ) ;
#45724 = AXIS2_PLACEMENT_3D ( 'NONE', #25184, #81074, #39700 ) ;
#45725 = EDGE_CURVE ( 'NONE', #83730, #53830, #27790, .T. ) ;
#45726 = ORIENTED_EDGE ( 'NONE', *, *, #7986, .F. ) ;
#45727 = ORIENTED_EDGE ( 'NONE', *, *, #83129, .T. ) ;
#45728 = ORIENTED_EDGE ( 'NONE', *, *, #45360, .T. ) ;
#45729 = DIRECTION ( 'NONE',  ( 0.000000000000000000, 0.000000000000000000, -1.000000000000000000 ) ) ;
#45730 = CARTESIAN_POINT ( 'NONE',  ( 108.0140931804088211, -24.91688388787635589, 261.0127681330534415 ) ) ;
#45731 = CARTESIAN_POINT ( 'NONE',  ( 60.32499999999999574, 82.54999999999999716, 358.0130000000000337 ) ) ;
#45732 = CARTESIAN_POINT ( 'NONE',  ( 129.9732689015971516, -140.6782641201739352, 246.0176313805619941 ) ) ;
#45734 = CARTESIAN_POINT ( 'NONE',  ( 69.89223516763907185, -140.0675090405642891, 246.8991749143359868 ) ) ;
#45733 = DIRECTION ( 'NONE',  ( 0.000000000000000000, 0.000000000000000000, -1.000000000000000000 ) ) ;
#45735 = CARTESIAN_POINT ( 'NONE',  ( 104.3272728202184538, -28.09756461201434874, 204.7314674471249702 ) ) ;
#45736 = ORIENTED_EDGE ( 'NONE', *, *, #54252, .T. ) ;
#45737 = ORIENTED_EDGE ( 'NONE', *, *, #49272, .T. ) ;
#45738 = AXIS2_PLACEMENT_3D ( 'NONE', #37568, #58876, #39341 ) ;
#45739 = ORIENTED_EDGE ( 'NONE', *, *, #34931, .F. ) ;
#45740 = ADVANCED_FACE ( 'NONE', ( #35455, #953, #56341 ), #16822, .F. ) ;
#45741 = CARTESIAN_POINT ( 'NONE',  ( 142.8682495647594806, 8.654319075478467127, 394.9756252759102040 ) ) ;
#45742 = CONICAL_SURFACE ( 'NONE', #66050, 4.799999999999970512, 0.7853981633975198884 ) ;
#45743 = DIRECTION ( 'NONE',  ( 1.639958061481212836E-42, -4.100000000000000342E-29, -1.000000000000000000 ) ) ;
#45744 = FACE_OUTER_BOUND ( 'NONE', #59658, .T. ) ;
#45745 = EDGE_CURVE ( 'NONE', #55155, #41030, #17623, .T. ) ;
#45746 = CARTESIAN_POINT ( 'NONE',  ( 113.6566823882007355, -42.65376606380868196, 34.67586902018199169 ) ) ;
#45747 = CARTESIAN_POINT ( 'NONE',  ( 118.5129862669514296, 94.84303900880917126, 3.295572367533603497 ) ) ;
#45748 = EDGE_CURVE ( 'NONE', #17890, #47593, #84086, .T. ) ;
#45749 = CARTESIAN_POINT ( 'NONE',  ( 164.9667039024459996, -28.27351298637401200, -5.074374724088000832 ) ) ;
#45750 = LINE ( 'NONE', #32588, #52945 ) ;
#45751 = EDGE_CURVE ( 'NONE', #14487, #70410, #21985, .T. ) ;
#45752 = ORIENTED_EDGE ( 'NONE', *, *, #20696, .F. ) ;
#45753 = EDGE_CURVE ( 'NONE', #44014, #18892, #70904, .T. ) ;
#45754 = DIRECTION ( 'NONE',  ( 1.000000000000000078E-15, -1.000000000000000083E-30, -1.000000000000000000 ) ) ;
#45755 = ORIENTED_EDGE ( 'NONE', *, *, #40793, .F. ) ;
#45756 = LINE ( 'NONE', #24015, #69903 ) ;
#45757 = CARTESIAN_POINT ( 'NONE',  ( 105.7780793485435851, -44.78982812472496988, 35.26809036959094357 ) ) ;
#45758 = EDGE_CURVE ( 'NONE', #73852, #37451, #15935, .T. ) ;
#45759 = EDGE_CURVE ( 'NONE', #77606, #70760, #2755, .T. ) ;
#45760 = CIRCLE ( 'NONE', #80558, 7.874000000000186184 ) ;
#45761 = VECTOR ( 'NONE', #16524, 1000.000000000000000 ) ;
#45762 = CARTESIAN_POINT ( 'NONE',  ( 136.1531896714421634, -16.93816060013640268, 7.482180659736330064 ) ) ;
#45763 = AXIS2_PLACEMENT_3D ( 'NONE', #81228, #67119, #24896 ) ;
#45764 = ADVANCED_FACE ( 'NONE', ( #42707 ), #16380, .T. ) ;
#45765 = CARTESIAN_POINT ( 'NONE',  ( 41.56648329127399677, 0.2215528400590013880, 258.9256252759120116 ) ) ;
#45766 = CARTESIAN_POINT ( 'NONE',  ( -7.735768046436663603, 92.63082225456683716, 118.3037957712300283 ) ) ;
#45767 = ORIENTED_EDGE ( 'NONE', *, *, #38145, .T. ) ;
#45768 = DIRECTION ( 'NONE',  ( 0.000000000000000000, 0.000000000000000000, 1.000000000000000000 ) ) ;
#45769 = CARTESIAN_POINT ( 'NONE',  ( 82.56670390244703128, -104.2784471599409670, 23.21780685541800082 ) ) ;
#45770 = EDGE_CURVE ( 'NONE', #20355, #56758, #24882, .T. ) ;
#45771 = VERTEX_POINT ( 'NONE', #8221 ) ;
#45772 = CARTESIAN_POINT ( 'NONE',  ( 109.0723201335305816, -47.59939223872296310, 127.7337205140059382 ) ) ;
#45773 = ORIENTED_EDGE ( 'NONE', *, *, #23364, .F. ) ;
#45774 = CARTESIAN_POINT ( 'NONE',  ( 104.5191702102720939, -45.41989400652479958, 61.76003887569697781 ) ) ;
#45775 = EDGE_CURVE ( 'NONE', #5926, #16504, #44056, .T. ) ;
#45776 = CIRCLE ( 'NONE', #89330, 16.00000000000000000 ) ;
#45777 = CARTESIAN_POINT ( 'NONE',  ( 116.3212776292294421, -32.94146857471278622, 70.13562527591093954 ) ) ;
#45778 = CARTESIAN_POINT ( 'NONE',  ( 99.44206372185087162, -32.21319818083724584, 82.33301187732594428 ) ) ;
#45779 = LINE ( 'NONE', #39437, #28574 ) ;
#45780 = CARTESIAN_POINT ( 'NONE',  ( 112.7890892452997917, -68.16618858916433510, 247.0964967658709952 ) ) ;
#45781 = VECTOR ( 'NONE', #61289, 1000.000000000000114 ) ;
#45782 = CARTESIAN_POINT ( 'NONE',  ( 100.4654578171049337, -27.83497312075872188, 31.59657765686396758 ) ) ;
#45783 = CARTESIAN_POINT ( 'NONE',  ( 89.06648138392552028, -56.72944715994104570, 14.67562527591095289 ) ) ;
#45784 = EDGE_LOOP ( 'NONE', ( #39713, #24646, #73065, #68082 ) ) ;
#45785 = CARTESIAN_POINT ( 'NONE',  ( 115.7829627233165724, -41.80255438717769323, 258.4063611559658398 ) ) ;
#45786 = ORIENTED_EDGE ( 'NONE', *, *, #21202, .F. ) ;
#45787 = CARTESIAN_POINT ( 'NONE',  ( -118.5559323284755067, 69.85063172184842983, -0.8489616598194429375 ) ) ;
#45788 = VERTEX_POINT ( 'NONE', #30454 ) ;
#45789 = VECTOR ( 'NONE', #56807, 1000.000000000000114 ) ;
#45790 = ORIENTED_EDGE ( 'NONE', *, *, #3572, .T. ) ;
#45791 = EDGE_CURVE ( 'NONE', #78823, #82481, #7767, .T. ) ;
#45792 = VERTEX_POINT ( 'NONE', #28651 ) ;
#45793 = CARTESIAN_POINT ( 'NONE',  ( 112.7790632652332050, -27.19118669266615740, 204.6470538473399756 ) ) ;
#45794 = EDGE_CURVE ( 'NONE', #36736, #33407, #81446, .T. ) ;
#45795 = CARTESIAN_POINT ( 'NONE',  ( 186.6899999999999977, 46.38749999999999574, -38.10000000000000142 ) ) ;
#45796 = CARTESIAN_POINT ( 'NONE',  ( 141.8664832912729992, -71.52944715994142655, 361.9756252759109998 ) ) ;
#45797 = CARTESIAN_POINT ( 'NONE',  ( 115.7285985590555129, -43.59543139906921283, 44.30514908543492680 ) ) ;
#45799 = EDGE_CURVE ( 'NONE', #56594, #47280, #77261, .T. ) ;
#45798 = CARTESIAN_POINT ( 'NONE',  ( 109.6426967425594370, -46.48017342192625989, 43.78143288360754326 ) ) ;
#45800 = ORIENTED_EDGE ( 'NONE', *, *, #52461, .F. ) ;
#45801 = CARTESIAN_POINT ( 'NONE',  ( 116.3225472244029817, -32.94146556017791738, 114.1356252759109822 ) ) ;
#45802 = EDGE_CURVE ( 'NONE', #10278, #66199, #68390, .T. ) ;
#45803 = CARTESIAN_POINT ( 'NONE',  ( 179.4595971212889935, -28.98061976758940617, -5.074374724088000832 ) ) ;
#45804 = VERTEX_POINT ( 'NONE', #64527 ) ;
#45805 = DIRECTION ( 'NONE',  ( 0.000000000000000000, 1.000000000000000000, 0.000000000000000000 ) ) ;
#45806 = CARTESIAN_POINT ( 'NONE',  ( 34.96670390244699433, -28.27351298637416122, 193.9678068554150911 ) ) ;
#45807 = CARTESIAN_POINT ( 'NONE',  ( 110.8089421659425824, -26.35361831834155311, 249.7889586092445882 ) ) ;
#45808 = FACE_OUTER_BOUND ( 'NONE', #68632, .T. ) ;
#45809 = CARTESIAN_POINT ( 'NONE',  ( 92.91125933621933086, -94.95109689075221127, -11.78219314458228695 ) ) ;
#45810 = CARTESIAN_POINT ( 'NONE',  ( 50.42303506447345285, 65.60000000000000853, -73.21698938693724301 ) ) ;
#45811 = CARTESIAN_POINT ( 'NONE',  ( 114.3529501776022244, -31.35170872818512322, 258.7428960185527558 ) ) ;
#45813 = CARTESIAN_POINT ( 'NONE',  ( 98.32466564902617279, -28.76522518762223157, 76.73848241876795839 ) ) ;
#45812 = DIRECTION ( 'NONE',  ( 1.000000000000000078E-15, -1.000000000000000083E-30, -1.000000000000000000 ) ) ;
#45814 = CARTESIAN_POINT ( 'NONE',  ( 120.1084960442967002, 74.60926949527541296, 51.17446912123692471 ) ) ;
#45815 = CARTESIAN_POINT ( 'NONE',  ( 117.4075167370973958, -38.36336677748749224, 113.7013395616249767 ) ) ;
#45816 = ORIENTED_EDGE ( 'NONE', *, *, #59644, .F. ) ;
#45817 = CARTESIAN_POINT ( 'NONE',  ( 234.0013031625829854, 52.73749999999999716, -2.032000000000000028 ) ) ;
#45818 = ORIENTED_EDGE ( 'NONE', *, *, #52968, .T. ) ;
#45819 = CARTESIAN_POINT ( 'NONE',  ( 173.9900000000000091, 0.000000000000000000, 131.6533725204182019 ) ) ;
#45820 = CYLINDRICAL_SURFACE ( 'NONE', #40612, 2.500000000000002220 ) ;
#45821 = CARTESIAN_POINT ( 'NONE',  ( 135.4870310422260502, -34.36767655968418467, 1.942446731272566174 ) ) ;
#45822 = EDGE_LOOP ( 'NONE', ( #64806, #27720, #16081, #16455 ) ) ;
#45823 = LINE ( 'NONE', #24963, #65065 ) ;
#45825 = EDGE_LOOP ( 'NONE', ( #78579, #41341 ) ) ;
#45824 = CARTESIAN_POINT ( 'NONE',  ( 108.0382549187111607, -25.67193643048636886, 109.9946728949589811 ) ) ;
#45826 = CARTESIAN_POINT ( 'NONE',  ( 107.0664832912739968, -36.72944715994100306, 287.6356252759109680 ) ) ;
#45827 = CIRCLE ( 'NONE', #26991, 15.50000000000000000 ) ;
#45828 = CARTESIAN_POINT ( 'NONE',  ( 182.0667039024476708, -33.35206098992059509, 313.9678068554149490 ) ) ;
#45830 = VECTOR ( 'NONE', #10160, 1000.000000000000000 ) ;
#45829 = CARTESIAN_POINT ( 'NONE',  ( 46.48091746482041486, -48.32844715994088602, 180.4678068554150911 ) ) ;
#45831 = EDGE_LOOP ( 'NONE', ( #37266, #74391, #58749 ) ) ;
#45832 = CARTESIAN_POINT ( 'NONE',  ( 102.6066768796756037, -46.86875521856975269, 132.2346728949579528 ) ) ;
#45833 = APPLICATION_PROTOCOL_DEFINITION ( 'draft international standard', 'automotive_design', 1998, #1124 ) ;
#45834 = VECTOR ( 'NONE', #37867, 1000.000000000000000 ) ;
#45835 = PLANE ( 'NONE',  #19641 ) ;
#45836 = DIRECTION ( 'NONE',  ( 0.000000000000000000, -1.000000000000000000, 0.000000000000000000 ) ) ;
#45837 = VERTEX_POINT ( 'NONE', #1411 ) ;
#45838 = ORIENTED_EDGE ( 'NONE', *, *, #69221, .F. ) ;
#45839 = B_SPLINE_SURFACE_WITH_KNOTS ( 'NONE', 3, 3, ( 
 ( #88671, #54101, #12815, #87761, #47298 ),
 ( #75023, #40500, #67300, #68218, #11459 ),
 ( #25981, #53195, #80966, #59141, #81422 ),
 ( #53650, #46397, #45495, #18714, #73219 ),
 ( #39594, #10998, #38699, #59580, #25078 ) ),
 .UNSPECIFIED., .F., .F., .F.,
 ( 4, 1, 4 ),
 ( 4, 1, 4 ),
 ( 0.000000000000000000, 0.5714285714285709528, 1.000000000000000000 ),
 ( 0.1438910682813590025, 4.132355267033809731, 7.123703416098150498 ),
 .UNSPECIFIED. ) ;
#45840 = CARTESIAN_POINT ( 'NONE',  ( 144.0667039024470171, -102.7784471599409102, 55.21780685541800437 ) ) ;
#45841 = LINE ( 'NONE', #79069, #39628 ) ;
#45842 = LINE ( 'NONE', #60381, #21195 ) ;
#45844 = CARTESIAN_POINT ( 'NONE',  ( 49.21437657594998427, -35.91149509761070391, -5.074374724088000832 ) ) ;
#45843 = DIRECTION ( 'NONE',  ( -1.000000000000000078E-15, 1.000000000000000083E-30, 1.000000000000000000 ) ) ;
#45845 = CARTESIAN_POINT ( 'NONE',  ( 97.81168844167092402, -40.51740470302234343, 181.6357138554620576 ) ) ;
#45846 = AXIS2_PLACEMENT_3D ( 'NONE', #67565, #80761, #33041 ) ;
#45847 = EDGE_LOOP ( 'NONE', ( #37839, #23112, #75912, #37653 ) ) ;
#45848 = AXIS2_PLACEMENT_3D ( 'NONE', #39718, #60152, #87889 ) ;
#45849 = ADVANCED_FACE ( 'NONE', ( #22300 ), #4586, .T. ) ;
#45850 = CARTESIAN_POINT ( 'NONE',  ( 172.5664832912740110, -32.07844715994070839, 143.6756252759119832 ) ) ;
#45851 = ADVANCED_FACE ( 'NONE', ( #71353 ), #37265, .F. ) ;
#45852 = CARTESIAN_POINT ( 'NONE',  ( 117.2610056464982904, -34.82931580038573571, 199.9851490854349549 ) ) ;
#45854 = ORIENTED_EDGE ( 'NONE', *, *, #85976, .T. ) ;
#45853 = DIRECTION ( 'NONE',  ( 1.000000000000000078E-15, 1.000000000000000083E-30, -1.000000000000000000 ) ) ;
#45855 = EDGE_CURVE ( 'NONE', #5575, #60824, #79057, .T. ) ;
#45856 = CARTESIAN_POINT ( 'NONE',  ( 104.2296407737279935, -46.70397019442127373, 63.36800622829197494 ) ) ;
#45857 = CARTESIAN_POINT ( 'NONE',  ( 110.8542424614423823, -45.98433130124127644, 52.88560554285743365 ) ) ;
#45858 = CARTESIAN_POINT ( 'NONE',  ( -186.2398777604655038, 20.32000000000000028, -6.349999999999999645 ) ) ;
#45859 = CARTESIAN_POINT ( 'NONE',  ( 188.5667039024479834, -67.87844715994100397, 298.0928068554150627 ) ) ;
#45860 = EDGE_CURVE ( 'NONE', #15299, #80043, #66290, .T. ) ;
#45861 = ORIENTED_EDGE ( 'NONE', *, *, #76446, .F. ) ;
#45862 = DIRECTION ( 'NONE',  ( 0.000000000000000000, 0.000000000000000000, -1.000000000000000000 ) ) ;
#45863 = EDGE_LOOP ( 'NONE', ( #44695, #56091, #53527, #67737 ) ) ;
#45864 = EDGE_LOOP ( 'NONE', ( #79872, #47632, #73293, #84044 ) ) ;
#45865 = CARTESIAN_POINT ( 'NONE',  ( 98.10010861879410982, -32.13871408278030373, 242.3815833058969815 ) ) ;
#45866 = EDGE_CURVE ( 'NONE', #25323, #65644, #50999, .T. ) ;
#45867 = CARTESIAN_POINT ( 'NONE',  ( 97.84270335286004183, -40.59238673107780215, 52.64166371051710769 ) ) ;
#45868 = CARTESIAN_POINT ( 'NONE',  ( -118.1705221151483443, 90.93965867633437483, -9.571124722858089129 ) ) ;
#45869 = EDGE_CURVE ( 'NONE', #62271, #39918, #79510, .T. ) ;
#45870 = LINE ( 'NONE', #73602, #70790 ) ;
#45871 = DIRECTION ( 'NONE',  ( 0.000000000000000000, 0.000000000000000000, -1.000000000000000000 ) ) ;
#45872 = EDGE_LOOP ( 'NONE', ( #79372, #36773, #46795, #10400, #36252, #89612, #43295, #21600, #44412, #68292, #32717, #67827 ) ) ;
#45873 = DIRECTION ( 'NONE',  ( 1.000000000000000000, 0.000000000000000000, 0.000000000000000000 ) ) ;
#45874 = CARTESIAN_POINT ( 'NONE',  ( 109.7165975557216342, -26.99861574449257162, 35.86486515683853327 ) ) ;
#45875 = EDGE_LOOP ( 'NONE', ( #86388, #71294 ) ) ;
#45876 = CARTESIAN_POINT ( 'NONE',  ( 96.55902551080266960, -40.08462249002853639, 281.5603871806728762 ) ) ;
#45877 = ORIENTED_EDGE ( 'NONE', *, *, #30746, .F. ) ;
#45878 = ORIENTED_EDGE ( 'NONE', *, *, #69796, .F. ) ;
#45879 = CARTESIAN_POINT ( 'NONE',  ( 98.80728567624888115, -32.50078473314371763, 243.7680903695909649 ) ) ;
#45880 = EDGE_CURVE ( 'NONE', #2296, #86147, #11338, .T. ) ;
#45881 = DIRECTION ( 'NONE',  ( 0.000000000000000000, -1.000000000000000000, 0.000000000000000000 ) ) ;
#45882 = LINE ( 'NONE', #87698, #60694 ) ;
#45883 = DIRECTION ( 'NONE',  ( 1.000000000000000078E-15, -1.000000000000000083E-30, -1.000000000000000000 ) ) ;
#45884 = CARTESIAN_POINT ( 'NONE',  ( -487.2989999999999782, 97.78694598552370110, 18.25625000000050235 ) ) ;
#45885 = CIRCLE ( 'NONE', #38645, 2.500000000000002220 ) ;
#45886 = EDGE_CURVE ( 'NONE', #47492, #72226, #39490, .T. ) ;
#45887 = CARTESIAN_POINT ( 'NONE',  ( 104.1737878132142043, -26.63141132829087354, 221.2984824187679465 ) ) ;
#45889 = LINE ( 'NONE', #71851, #60167 ) ;
#45888 = AXIS2_PLACEMENT_3D ( 'NONE', #18754, #17860, #73259 ) ;
#45890 = VERTEX_POINT ( 'NONE', #87648 ) ;
#45891 = VECTOR ( 'NONE', #19381, 1000.000000000000000 ) ;
#45892 = CARTESIAN_POINT ( 'NONE',  ( 98.68765228159747949, -43.00544673443933874, 62.83848241876793850 ) ) ;
#45893 = CARTESIAN_POINT ( 'NONE',  ( 80.06648329127402519, -46.42944715994105565, 4.925625275910944012 ) ) ;
#45894 = VECTOR ( 'NONE', #6798, 1000.000000000000000 ) ;
#45895 = B_SPLINE_CURVE_WITH_KNOTS ( 'NONE', 3,
 ( #865, #34929, #8589, #14955, #28107, #57154, #28562, #56249, #42623, #63539, #84000, #35822, #1320, #21773, #77178, #70358, #70813, #63998, #7239, #69465, #29027, #8133, #56712, #84457, #22218, #49893, #15847 ),
 .UNSPECIFIED., .F., .F.,
 ( 4, 2, 1, 1, 1, 2, 2, 2, 2, 2, 2, 2, 2, 2, 4 ),
 ( 0.5000609409785667925, 0.5010373844532182153, 0.5020138279278696380, 0.5039667148771719285, 0.5078724887757768425, 0.5156840365729865594, 0.5313071321674062153, 0.5625533233562457491, 0.6250457057339249278, 0.6875380881116041065, 0.7500304704892832852, 0.8125228528669624639, 0.8750152352446416426, 0.9375076176223208213, 1.000000000000000000 ),
 .UNSPECIFIED. ) ;
#45896 = EDGE_LOOP ( 'NONE', ( #51041, #32251, #84712, #10338 ) ) ;
#45897 = ORIENTED_EDGE ( 'NONE', *, *, #15554, .T. ) ;
#45898 = ORIENTED_EDGE ( 'NONE', *, *, #37491, .T. ) ;
#45899 = CARTESIAN_POINT ( 'NONE',  ( 82.54618223952044787, -17.53884010536265237, 2.747932095378487816 ) ) ;
#45900 = CARTESIAN_POINT ( 'NONE',  ( 141.0664832912739826, -8.729447159940953327, -4.970821333495649696 ) ) ;
#45901 = CARTESIAN_POINT ( 'NONE',  ( 108.3314640124533668, -46.73508453131670137, 152.6777937298070640 ) ) ;
#45902 = CARTESIAN_POINT ( 'NONE',  ( 108.3793409795780036, -28.17508408765456096, 142.7614237029239632 ) ) ;
#45903 = CARTESIAN_POINT ( 'NONE',  ( 117.3563231384421357, -34.92488217824808316, 239.9641967044819637 ) ) ;
#45905 = EDGE_CURVE ( 'NONE', #3093, #3392, #42243, .T. ) ;
#45904 = CARTESIAN_POINT ( 'NONE',  ( 117.0722999933526012, -35.46582721381028591, 59.92702479522854730 ) ) ;
#45906 = EDGE_LOOP ( 'NONE', ( #6917, #50104, #81473, #59531 ) ) ;
#45907 = EDGE_CURVE ( 'NONE', #53161, #45331, #62616, .T. ) ;
#45908 = CARTESIAN_POINT ( 'NONE',  ( 134.8178559631103894, -39.40256188477528099, 1.690787648075052552 ) ) ;
#45909 = EDGE_LOOP ( 'NONE', ( #20121, #69755, #20072, #10742, #39782, #60958, #54818, #51849 ) ) ;
#45910 = EDGE_LOOP ( 'NONE', ( #37956, #22158, #74913, #36649 ) ) ;
#45911 = CARTESIAN_POINT ( 'NONE',  ( 148.0533267522749838, 0.000000000000000000, -160.2664750769289697 ) ) ;
#45912 = ORIENTED_EDGE ( 'NONE', *, *, #3035, .T. ) ;
#45913 = ORIENTED_EDGE ( 'NONE', *, *, #80119, .F. ) ;
#45914 = CARTESIAN_POINT ( 'NONE',  ( 107.5667039024470313, -100.3098201933444926, 2.217806855417892020 ) ) ;
#45915 = CARTESIAN_POINT ( 'NONE',  ( 48.45959712127140051, -26.00627455219179751, 193.9678068554150911 ) ) ;
#45916 = DIRECTION ( 'NONE',  ( 0.000000000000000000, 0.000000000000000000, 1.000000000000000000 ) ) ;
#45917 = CARTESIAN_POINT ( 'NONE',  ( 100.8033404080456705, -29.31000718268690619, 150.0581341137909703 ) ) ;
#45918 = CARTESIAN_POINT ( 'NONE',  ( 111.3412100197261765, -27.17259740239810739, 24.74133956162494030 ) ) ;
#45919 = EDGE_LOOP ( 'NONE', ( #24835, #20743, #57000, #64484 ) ) ;
#45920 = CARTESIAN_POINT ( 'NONE',  ( 156.5667039024485518, -48.82844715993568485, 173.2178068554149775 ) ) ;
#45921 = ORIENTED_EDGE ( 'NONE', *, *, #70243, .F. ) ;
#45922 = EDGE_CURVE ( 'NONE', #69972, #22750, #40822, .T. ) ;
#45923 = CARTESIAN_POINT ( 'NONE',  ( 107.0664832912739968, -36.72944715994100306, 287.6356252759109680 ) ) ;
#45924 = ORIENTED_EDGE ( 'NONE', *, *, #31918, .T. ) ;
#45925 = CARTESIAN_POINT ( 'NONE',  ( 25.56670390244797275, -62.87844715994099687, 132.3428068554150343 ) ) ;
#45926 = CARTESIAN_POINT ( 'NONE',  ( 116.3212776292272537, -32.94146857470742162, 144.1356252759109680 ) ) ;
#45927 = CARTESIAN_POINT ( 'NONE',  ( 97.82529165045187369, -40.55051507927917243, 131.6384725568923102 ) ) ;
#45928 = ADVANCED_FACE ( 'NONE', ( #59021 ), #31777, .F. ) ;
#45929 = CARTESIAN_POINT ( 'NONE',  ( 59.56670390244699576, -67.87844715994098976, 120.2178068554179902 ) ) ;
#45930 = VERTEX_POINT ( 'NONE', #24969 ) ;
#45931 = CARTESIAN_POINT ( 'NONE',  ( 97.08353706812128792, -39.80957011747380392, 21.56419670448195092 ) ) ;
#45932 = CARTESIAN_POINT ( 'NONE',  ( 97.31101637507774171, -32.83472251844465717, 37.02419670448292521 ) ) ;
#45933 = SURFACE_STYLE_USAGE ( .BOTH. , #5542 ) ;
#45934 = B_SPLINE_CURVE_WITH_KNOTS ( 'NONE', 3,
 ( #29866, #43914, #84837, #50279, #77559, #35763, #78475, #77120, #85292, #49385, #50740, #43464, #23068, #35310 ),
 .UNSPECIFIED., .F., .F.,
 ( 4, 2, 2, 1, 1, 2, 2, 4 ),
 ( 0.000000000000000000, 0.2499999999999974465, 0.3749999999999963918, 0.4374999999999964473, 0.4687499999999965583, 0.4843749999999975575, 0.4999999999999985567, 1.000000000000000000 ),
 .UNSPECIFIED. ) ;
#45936 = DIRECTION ( 'NONE',  ( 0.000000000000000000, -1.000000000000000000, 0.000000000000000000 ) ) ;
#45935 = LINE ( 'NONE', #46836, #59313 ) ;
#45937 = CARTESIAN_POINT ( 'NONE',  ( 89.33314995793998037, 12.92155284005730387, 361.9756252759109998 ) ) ;
#45938 = CARTESIAN_POINT ( 'NONE',  ( -254.0000000000000000, 3.174999999999999822, -41.27499999999999858 ) ) ;
#45939 = FACE_BOUND ( 'NONE', #11165, .T. ) ;
#45940 = CARTESIAN_POINT ( 'NONE',  ( 53.56670390244828184, -48.82844715994055917, 300.4678068554150059 ) ) ;
#45941 = CARTESIAN_POINT ( 'NONE',  ( -29.99999999999998224, 172.0000000000000000, 114.8826257785461280 ) ) ;
#45942 = CARTESIAN_POINT ( 'NONE',  ( 100.5231322539815153, -27.76298515809465073, 30.56610146638794134 ) ) ;
#45943 = CARTESIAN_POINT ( 'NONE',  ( 110.4988674196275014, -26.88560509280327082, 205.8099109901969541 ) ) ;
#45944 = CARTESIAN_POINT ( 'NONE',  ( 116.2507439086588761, -31.75083131158774918, 65.22133956162595325 ) ) ;
#45945 = CIRCLE ( 'NONE', #14076, 18.00000000000000000 ) ;
#45946 = AXIS2_PLACEMENT_3D ( 'NONE', #5907, #89018, #61298 ) ;
#45948 = DIRECTION ( 'NONE',  ( 1.000000000000000000, 0.000000000000000000, 0.000000000000000000 ) ) ;
#45947 = CARTESIAN_POINT ( 'NONE',  ( 116.7958306881861148, -39.38531486699053374, 173.6120842293531723 ) ) ;
#45949 = CARTESIAN_POINT ( 'NONE',  ( 144.0667039004811443, -140.6784471619068029, 245.4415720117440003 ) ) ;
#45950 = CIRCLE ( 'NONE', #21292, 11.49999999999999645 ) ;
#45951 = AXIS2_PLACEMENT_3D ( 'NONE', #85491, #50936, #2357 ) ;
#45952 = CIRCLE ( 'NONE', #6823, 50.79999999999999716 ) ;
#45953 = ORIENTED_EDGE ( 'NONE', *, *, #78002, .F. ) ;
#45954 = EDGE_CURVE ( 'NONE', #41305, #34264, #18597, .T. ) ;
#45955 = FACE_OUTER_BOUND ( 'NONE', #53369, .T. ) ;
#45956 = VERTEX_POINT ( 'NONE', #10450 ) ;
#45957 = EDGE_CURVE ( 'NONE', #71033, #53038, #80397, .T. ) ;
#45958 = CARTESIAN_POINT ( 'NONE',  ( 98.49710108934571906, -31.94619897774425610, 106.9213395616249755 ) ) ;
#45960 = ORIENTED_EDGE ( 'NONE', *, *, #44468, .F. ) ;
#45959 = CARTESIAN_POINT ( 'NONE',  ( 30.00000000000003553, 127.0000000000000000, 182.8826257785461280 ) ) ;
#45961 = EDGE_CURVE ( 'NONE', #27646, #32492, #24529, .T. ) ;
#45962 = CARTESIAN_POINT ( 'NONE',  ( 96.79764630557892247, -40.75620882907055176, 242.6118157521009664 ) ) ;
#45963 = CARTESIAN_POINT ( 'NONE',  ( 226.4410000000000025, 65.43750000000000000, -63.94449999999999790 ) ) ;
#45964 = PRODUCT_DEFINITION_SHAPE ( 'NONE', 'NONE',  #89946 ) ;
#45965 = CARTESIAN_POINT ( 'NONE',  ( 110.8740616933906864, -45.97620365431721012, 147.8873101108567312 ) ) ;
#45966 = CARTESIAN_POINT ( 'NONE',  ( 179.7974245136207685, -36.32844715993469720, 313.9678068554149490 ) ) ;
#45967 = CARTESIAN_POINT ( 'NONE',  ( 97.81169418859235520, -40.51741816698509524, 47.63568902202231925 ) ) ;
#45968 = CARTESIAN_POINT ( 'NONE',  ( 226.4410000000000025, 65.43750000000000000, -63.94449999999999790 ) ) ;
#45969 = EDGE_CURVE ( 'NONE', #48081, #8213, #52194, .T. ) ;
#45970 = CARTESIAN_POINT ( 'NONE',  ( -85.52748787272784625, 73.86195533656251655, 98.64078293412708831 ) ) ;
#45971 = VECTOR ( 'NONE', #73374, 1000.000000000000114 ) ;
#45973 = CARTESIAN_POINT ( 'NONE',  ( 107.8656169629272483, -46.51081515578112402, 177.6413395616259834 ) ) ;
#45972 = VECTOR ( 'NONE', #39008, 1000.000000000000000 ) ;
#45974 = EDGE_LOOP ( 'NONE', ( #8060, #30402, #85236, #495 ) ) ;
#45975 = EDGE_LOOP ( 'NONE', ( #8854, #49931, #62624, #46137 ) ) ;
#45976 = CARTESIAN_POINT ( 'NONE',  ( 103.2835872187480533, -45.32980894545860906, 128.6663452106589887 ) ) ;
#45978 = EDGE_CURVE ( 'NONE', #28622, #13566, #4972, .T. ) ;
#45977 = AXIS2_PLACEMENT_3D ( 'NONE', #85034, #29602, #69600 ) ;
#45979 = DIRECTION ( 'NONE',  ( 0.000000000000000000, 0.000000000000000000, 1.000000000000000000 ) ) ;
#45981 = DIRECTION ( 'NONE',  ( -1.000000000000000078E-15, 1.000000000000000000, 0.000000000000000000 ) ) ;
#45980 = CARTESIAN_POINT ( 'NONE',  ( 98.14754276252335785, -43.36755551587071977, 257.8356252759109566 ) ) ;
#45982 = CARTESIAN_POINT ( 'NONE',  ( -487.2989999999999782, 100.8062500000000057, 86.36305401447658880 ) ) ;
#45983 = DIRECTION ( 'NONE',  ( -0.7071067811578587436, 0.7071067812152364018, 0.000000000000000000 ) ) ;
#45984 = ADVANCED_FACE ( 'NONE', ( #25411 ), #53533, .T. ) ;
#45985 = LINE ( 'NONE', #17856, #21439 ) ;
#45986 = CARTESIAN_POINT ( 'NONE',  ( 151.0371591254582881, -46.82818131005593187, 249.9678068554149490 ) ) ;
#45987 = FACE_BOUND ( 'NONE', #81822, .T. ) ;
#45988 = CARTESIAN_POINT ( 'NONE',  ( 188.5667039024479834, -65.37844715994100397, 137.2178068554150059 ) ) ;
#45989 = CARTESIAN_POINT ( 'NONE',  ( 108.6716496925947126, -26.45072611336619772, 189.9527681330539792 ) ) ;
#45990 = ORIENTED_EDGE ( 'NONE', *, *, #84936, .T. ) ;
#45991 = ORIENTED_EDGE ( 'NONE', *, *, #68364, .F. ) ;
#45992 = DIRECTION ( 'NONE',  ( 1.000000000000000000, 1.000000000000000078E-15, 0.000000000000000000 ) ) ;
#45993 = CARTESIAN_POINT ( 'NONE',  ( 146.5596880459861779, -68.36644973479313592, 246.8246830390798721 ) ) ;
#45994 = CARTESIAN_POINT ( 'NONE',  ( -48.02966122971776741, 91.07499999999996021, 74.26049396966043048 ) ) ;
#45995 = DIRECTION ( 'NONE',  ( -1.000000000000000078E-15, -1.000000000000000083E-30, 1.000000000000000000 ) ) ;
#45996 = VECTOR ( 'NONE', #57588, 1000.000000000000000 ) ;
#45997 = VERTEX_POINT ( 'NONE', #10008 ) ;
#45998 = CARTESIAN_POINT ( 'NONE',  ( 73.17003668186730181, -46.47944715994106701, 14.92562527591093691 ) ) ;
#45999 = CARTESIAN_POINT ( 'NONE',  ( 97.47293644110631305, -40.89955093664978136, 231.6527681330539679 ) ) ;
#46000 = DIRECTION ( 'NONE',  ( -1.000000000000000000, -1.000000000000000078E-15, 0.000000000000000000 ) ) ;
#46001 = ORIENTED_EDGE ( 'NONE', *, *, #16404, .F. ) ;
#46002 = ORIENTED_EDGE ( 'NONE', *, *, #48760, .F. ) ;
#46003 = CARTESIAN_POINT ( 'NONE',  ( 97.81305373959743577, -40.51655628150228949, 62.63606721061723448 ) ) ;
#46004 = LINE ( 'NONE', #47802, #35541 ) ;
#46005 = CARTESIAN_POINT ( 'NONE',  ( 116.8175535499631792, -34.15458648068190683, 165.0313227694681757 ) ) ;
#46006 = CARTESIAN_POINT ( 'NONE',  ( 110.4716576677765119, -44.14797218061634254, 25.73666179816297372 ) ) ;
#46007 = DIRECTION ( 'NONE',  ( 9.351236661543306751E-17, -3.725950533538267725E-29, -1.000000000000000000 ) ) ;
#46008 = VERTEX_POINT ( 'NONE', #37720 ) ;
#46009 = VECTOR ( 'NONE', #40685, 1000.000000000000000 ) ;
#46010 = EDGE_CURVE ( 'NONE', #638, #13040, #68458, .T. ) ;
#46011 = CARTESIAN_POINT ( 'NONE',  ( 192.5667039024473013, -23.42844715993434335, 249.9678068554149775 ) ) ;
#46012 = LINE ( 'NONE', #19237, #21287 ) ;
#46013 = ORIENTED_EDGE ( 'NONE', *, *, #13347, .T. ) ;
#46014 = EDGE_LOOP ( 'NONE', ( #30083, #33284, #9011, #31801, #29976, #58586, #46426, #44258, #50482, #13336, #67151, #42245 ) ) ;
#46015 = AXIS2_PLACEMENT_3D ( 'NONE', #66756, #32229, #30462 ) ;
#46016 = VECTOR ( 'NONE', #53020, 1000.000000000000000 ) ;
#46017 = CARTESIAN_POINT ( 'NONE',  ( 97.81151477712479902, -40.51751189930152464, 186.6359914586728337 ) ) ;
#46018 = AXIS2_PLACEMENT_3D ( 'NONE', #57530, #85270, #50713 ) ;
#46019 = ORIENTED_EDGE ( 'NONE', *, *, #84663, .T. ) ;
#46020 = ORIENTED_EDGE ( 'NONE', *, *, #44856, .T. ) ;
#46021 = DIRECTION ( 'NONE',  ( 0.000000000000000000, 0.000000000000000000, 1.000000000000000000 ) ) ;
#46022 = CARTESIAN_POINT ( 'NONE',  ( 114.5755952152626946, -32.65889807719148052, 68.64384839950594142 ) ) ;
#46023 = CARTESIAN_POINT ( 'NONE',  ( 103.5348926201861985, -26.85948109348520418, 190.3499109901969746 ) ) ;
#46024 = CARTESIAN_POINT ( 'NONE',  ( 96.67182511810079859, -37.15340426533111895, 161.3584824187679487 ) ) ;
#46026 = CARTESIAN_POINT ( 'NONE',  ( 115.6552720357279753, -30.75834705514724732, 275.3099109901965562 ) ) ;
#46025 = CARTESIAN_POINT ( 'NONE',  ( 41.56648329127399677, -9.303447159940999356, 141.0426252759120018 ) ) ;
#46027 = DIRECTION ( 'NONE',  ( 0.8660254037844381525, 0.000000000000000000, 0.5000000000000007772 ) ) ;
#46028 = DIRECTION ( 'NONE',  ( 0.000000000000000000, 0.000000000000000000, 1.000000000000000000 ) ) ;
#46029 = ORIENTED_EDGE ( 'NONE', *, *, #36741, .F. ) ;
#46030 = TOROIDAL_SURFACE ( 'NONE', #72205, 11.75000000000000000, 2.125000000000000000 ) ;
#46031 = ORIENTED_EDGE ( 'NONE', *, *, #68038, .F. ) ;
#46032 = AXIS2_PLACEMENT_3D ( 'NONE', #67333, #34613, #74608 ) ;
#46033 = VECTOR ( 'NONE', #67563, 1000.000000000000000 ) ;
#46034 = EDGE_CURVE ( 'NONE', #66921, #39084, #72684, .T. ) ;
#46035 = CARTESIAN_POINT ( 'NONE',  ( 72.31648329127399677, -9.833000550534366724, -5.074374724089063982 ) ) ;
#46036 = CARTESIAN_POINT ( 'NONE',  ( 110.0646822317013118, -26.04189894992025955, 219.8708633711489711 ) ) ;
#46037 = ORIENTED_EDGE ( 'NONE', *, *, #9680, .F. ) ;
#46038 = CARTESIAN_POINT ( 'NONE',  ( 101.2005795642084820, -45.34792753215401007, 197.1013395616249966 ) ) ;
#46039 = CARTESIAN_POINT ( 'NONE',  ( 97.33774478695349330, -34.07145668252834980, 266.1148423016875881 ) ) ;
#46040 = CARTESIAN_POINT ( 'NONE',  ( -19.63071693306478949, 63.82648643955351986, 32.65698028270841036 ) ) ;
#46041 = LINE ( 'NONE', #17474, #75458 ) ;
#46042 = CYLINDRICAL_SURFACE ( 'NONE', #44159, 2.750000000000002665 ) ;
#46045 = CARTESIAN_POINT ( 'NONE',  ( 105.1131368864170526, -25.87365329830177529, 271.2061014663872243 ) ) ;
#46044 = PLANE ( 'NONE',  #52883 ) ;
#46043 = CARTESIAN_POINT ( 'NONE',  ( 113.8270003667112746, -32.37296061313053741, 277.6356252759109680 ) ) ;
#46046 = CARTESIAN_POINT ( 'NONE',  ( 100.8872181613150900, -44.70003033885427612, 173.0522674363715510 ) ) ;
#46047 = DIRECTION ( 'NONE',  ( 3.100000000000000258E-29, -3.100000000000000044E-14, -1.000000000000000000 ) ) ;
#46048 = CARTESIAN_POINT ( 'NONE',  ( 180.2143765759489895, -35.91149509761070391, -5.074374724088000832 ) ) ;
#46049 = LINE ( 'NONE', #73783, #38501 ) ;
#46050 = FACE_OUTER_BOUND ( 'NONE', #16617, .T. ) ;
#46051 = CYLINDRICAL_SURFACE ( 'NONE', #85516, 4.750000000000004441 ) ;
#46053 = ORIENTED_EDGE ( 'NONE', *, *, #47530, .T. ) ;
#46052 = LINE ( 'NONE', #67407, #66034 ) ;
#46054 = CARTESIAN_POINT ( 'NONE',  ( 136.7635286919467887, -19.26660482608927083, 6.827192804310395324 ) ) ;
#46055 = CARTESIAN_POINT ( 'NONE',  ( 114.6215443236117153, -29.51367161159714314, 234.4327681330539690 ) ) ;
#46056 = CARTESIAN_POINT ( 'NONE',  ( 101.5008874824296896, -27.91431070382771651, 106.5241967044819944 ) ) ;
#46057 = CARTESIAN_POINT ( 'NONE',  ( 115.5527055449870772, -29.57532036350955806, 220.3718157521019521 ) ) ;
#46058 = DIRECTION ( 'NONE',  ( 1.000000000000000000, 4.163336342344333240E-14, 0.000000000000000000 ) ) ;
#46059 = DIRECTION ( 'NONE',  ( 1.000000000000000000, 2.106816776397999944E-14, 7.761631831580328254E-43 ) ) ;
#46061 = CARTESIAN_POINT ( 'NONE',  ( 114.7049794032198520, -43.22496099079516796, 39.26526583603205722 ) ) ;
#46060 = LINE ( 'NONE', #31111, #84116 ) ;
#46062 = CARTESIAN_POINT ( 'NONE',  ( 32.06670390244800473, -32.29483332968611364, -5.074374724088000832 ) ) ;
#46063 = AXIS2_PLACEMENT_3D ( 'NONE', #174, #14263, #55551 ) ;
#46064 = CARTESIAN_POINT ( 'NONE',  ( 131.3165190107490332, -18.90078909148325792, 3.101427792080756252 ) ) ;
#46065 = ORIENTED_EDGE ( 'NONE', *, *, #53919, .T. ) ;
#46066 = ORIENTED_EDGE ( 'NONE', *, *, #41483, .T. ) ;
#46067 = EDGE_CURVE ( 'NONE', #28660, #44232, #3168, .T. ) ;
#46068 = CARTESIAN_POINT ( 'NONE',  ( 109.0672552851176249, -45.03324407163384535, 132.1867055423619775 ) ) ;
#46070 = EDGE_LOOP ( 'NONE', ( #30790, #19510, #32203, #71079 ) ) ;
#46069 = DIRECTION ( 'NONE',  ( 1.000000000000000000, -0.000000000000000000, 0.000000000000000000 ) ) ;
#46071 = CARTESIAN_POINT ( 'NONE',  ( 145.4416927396864878, -139.3034583227001804, 245.6607614918409865 ) ) ;
#46072 = EDGE_CURVE ( 'NONE', #75711, #15908, #83089, .T. ) ;
#46073 = CARTESIAN_POINT ( 'NONE',  ( 108.6454077996538246, -25.81962716842098970, 145.9737205140069420 ) ) ;
#46074 = LINE ( 'NONE', #61068, #19296 ) ;
#46075 = ADVANCED_FACE ( 'NONE', ( #19949 ), #27652, .T. ) ;
#46076 = LINE ( 'NONE', #16623, #29798 ) ;
#46077 = CARTESIAN_POINT ( 'NONE',  ( 152.4409905591762708, -0.9151414768250908383, 542.9756252759101471 ) ) ;
#46078 = EDGE_CURVE ( 'NONE', #12759, #25005, #14024, .T. ) ;
#46079 = FACE_OUTER_BOUND ( 'NONE', #76066, .T. ) ;
#46080 = VECTOR ( 'NONE', #83174, 1000.000000000000000 ) ;
#46081 = CARTESIAN_POINT ( 'NONE',  ( 117.3261810260836597, -38.23854875528750341, 73.72229194257801055 ) ) ;
#46082 = VERTEX_POINT ( 'NONE', #68992 ) ;
#46083 = VERTEX_POINT ( 'NONE', #68545 ) ;
#46084 = ORIENTED_EDGE ( 'NONE', *, *, #55209, .F. ) ;
#46085 = CIRCLE ( 'NONE', #12728, 2.000000000000001776 ) ;
#46086 = AXIS2_PLACEMENT_3D ( 'NONE', #45079, #31876, #10104 ) ;
#46087 = DIRECTION ( 'NONE',  ( 1.147230458779309805E-16, 3.204747427460360459E-31, 1.000000000000000000 ) ) ;
#46089 = CARTESIAN_POINT ( 'NONE',  ( 97.81168895331838087, -40.51742574516882200, 287.6356252759109680 ) ) ;
#46088 = CARTESIAN_POINT ( 'NONE',  ( 117.1170091337236414, -34.17489915221372598, 165.0365776568629315 ) ) ;
#46090 = CARTESIAN_POINT ( 'NONE',  ( 31.90335556477799628, -33.89581943344391135, -5.074374724088000832 ) ) ;
#46091 = CARTESIAN_POINT ( 'NONE',  ( 10.79079172156231081, 75.84006377869074811, -130.1095006741098530 ) ) ;
#46092 = EDGE_CURVE ( 'NONE', #39136, #18492, #307, .T. ) ;
#46093 = CARTESIAN_POINT ( 'NONE',  ( 151.0371591254582881, -46.82818131005593187, 237.4678068554150059 ) ) ;
#46094 = VECTOR ( 'NONE', #82575, 999.9999999999998863 ) ;
#46095 = CARTESIAN_POINT ( 'NONE',  ( 46.83715912545343940, -47.82818131006086304, 129.9678068554150911 ) ) ;
#46096 = CARTESIAN_POINT ( 'NONE',  ( 41.56648329127398966, -27.82844715994070484, 18.92562527591200094 ) ) ;
#46097 = CARTESIAN_POINT ( 'NONE',  ( 118.8180844208009717, -35.40729807334668067, 83.91562527591095488 ) ) ;
#46098 = ORIENTED_EDGE ( 'NONE', *, *, #82300, .T. ) ;
#46099 = VERTEX_POINT ( 'NONE', #82645 ) ;
#46100 = VECTOR ( 'NONE', #47822, 1000.000000000000000 ) ;
#46101 = CARTESIAN_POINT ( 'NONE',  ( 11.02183147610883829, 88.91382474694671600, 130.0907465706570179 ) ) ;
#46102 = CARTESIAN_POINT ( 'NONE',  ( 126.9648347381352949, 50.67849012603234371, 30.41069370691922558 ) ) ;
#46103 = VECTOR ( 'NONE', #78990, 1000.000000000000000 ) ;
#46104 = CIRCLE ( 'NONE', #60639, 2.030000000000003801 ) ;
#46105 = CARTESIAN_POINT ( 'NONE',  ( 41.56648329127499153, -36.32844715994070839, 74.17562527591199739 ) ) ;
#46106 = CARTESIAN_POINT ( 'NONE',  ( 114.9429295168758784, -34.48920150425379916, 146.8652332267339773 ) ) ;
#46107 = VECTOR ( 'NONE', #79323, 1000.000000000000114 ) ;
#46108 = B_SPLINE_CURVE_WITH_KNOTS ( 'NONE', 3,
 ( #24267, #5157, #53719, #59653, #51937, #31959, #32853, #81485, #60549, #74642, #52371, #60094, #12420, #80134, #87384, #32392, #40109, #67826, #5618, #33309, #25143, #80580, #17448, #45129, #52804, #66933, #18784, #59213, #18329, #46467, #10622, #38326, #73747, #39223, #11528, #25595, #68286 ),
 .UNSPECIFIED., .F., .F.,
 ( 4, 2, 2, 1, 2, 2, 2, 1, 1, 2, 2, 2, 2, 1, 2, 2, 2, 1, 1, 1, 2, 4 ),
 ( 0.6666501603260506226, 0.6874845253056601768, 0.6926931165505625376, 0.6979017077954648984, 0.7083188902852692870, 0.7499876202444850648, 0.7525919158669366338, 0.7551962114893882028, 0.7604048027342921179, 0.7708219852241017245, 0.7916563502037200495, 0.8124907151833384855, 0.8176993064282435109, 0.8229078976731485362, 0.8333250801629586979, 0.8749938101222022313, 0.8775981057446557987, 0.8802024013671094771, 0.8854109926120167229, 0.8958281751018317696, 0.9166625400814643054, 1.000000000000000000 ),
 .UNSPECIFIED. ) ;
#46109 = DIRECTION ( 'NONE',  ( -0.000000000000000000, -1.000000000000000000, -0.000000000000000000 ) ) ;
#46110 = EDGE_LOOP ( 'NONE', ( #23776, #79125, #3567, #25664 ) ) ;
#46111 = VERTEX_POINT ( 'NONE', #6314 ) ;
#46112 = VECTOR ( 'NONE', #56311, 1000.000000000000000 ) ;
#46113 = CARTESIAN_POINT ( 'NONE',  ( 70.63919639214310564, 65.60000000000000853, -33.74458626278666884 ) ) ;
#46114 = ORIENTED_EDGE ( 'NONE', *, *, #86304, .F. ) ;
#46115 = ORIENTED_EDGE ( 'NONE', *, *, #62706, .F. ) ;
#46116 = DIRECTION ( 'NONE',  ( 0.000000000000000000, 0.000000000000000000, 1.000000000000000000 ) ) ;
#46117 = CARTESIAN_POINT ( 'NONE',  ( 115.3890540380527767, -39.77298043176836018, 214.9787261630399655 ) ) ;
#46118 = DIRECTION ( 'NONE',  ( 0.000000000000000000, 0.000000000000000000, 1.000000000000000000 ) ) ;
#46119 = VECTOR ( 'NONE', #81904, 1000.000000000000000 ) ;
#46120 = ADVANCED_FACE ( 'NONE', ( #55771 ), #39927, .T. ) ;
#46121 = CARTESIAN_POINT ( 'NONE',  ( 41.56670390244776314, -36.32844715994104234, 313.9678068554150059 ) ) ;
#46122 = CIRCLE ( 'NONE', #12842, 0.5000000000000004441 ) ;
#46123 = CARTESIAN_POINT ( 'NONE',  ( -109.5351475254747839, 57.99849859213713898, 71.04168492196464513 ) ) ;
#46124 = EDGE_LOOP ( 'NONE', ( #12896, #1043, #28133, #18331 ) ) ;
#46125 = ORIENTED_EDGE ( 'NONE', *, *, #21802, .F. ) ;
#46126 = ORIENTED_EDGE ( 'NONE', *, *, #51222, .T. ) ;
#46127 = EDGE_LOOP ( 'NONE', ( #15281, #52794, #59977, #70163, #42838, #11161, #23952, #7409, #79466, #16267, #78582 ) ) ;
#46128 = ADVANCED_FACE ( 'NONE', ( #46734 ), #19495, .T. ) ;
#46129 = CARTESIAN_POINT ( 'NONE',  ( 99.00928370863422856, -39.88895027456798914, 244.4299951314959571 ) ) ;
#46130 = CARTESIAN_POINT ( 'NONE',  ( 113.3557719660652339, -27.61131746675945209, 89.60800622829195561 ) ) ;
#46131 = CARTESIAN_POINT ( 'NONE',  ( 98.11562048848810491, -31.42749274529980852, 85.90133956162493689 ) ) ;
#46132 = FACE_OUTER_BOUND ( 'NONE', #67894, .T. ) ;
#46133 = CARTESIAN_POINT ( 'NONE',  ( 34.92499999999999716, 87.13271776169270311, 294.9574999999999818 ) ) ;
#46134 = DIRECTION ( 'NONE',  ( -4.237773401492740281E-14, 1.000000000000000000, 0.000000000000000000 ) ) ;
#46135 = CARTESIAN_POINT ( 'NONE',  ( 117.0331605330187728, -30.31849857022486816, 140.2813395616249750 ) ) ;
#46136 = CYLINDRICAL_SURFACE ( 'NONE', #29135, 5.041900000000001825 ) ;
#46137 = ORIENTED_EDGE ( 'NONE', *, *, #65769, .F. ) ;
#46138 = CARTESIAN_POINT ( 'NONE',  ( 130.0134586223094288, 78.07027470200929997, -11.89097723361176762 ) ) ;
#46139 = EDGE_LOOP ( 'NONE', ( #34730, #87603, #46037, #88757 ) ) ;
#46140 = ORIENTED_EDGE ( 'NONE', *, *, #36470, .T. ) ;
#46141 = LINE ( 'NONE', #87067, #11382 ) ;
#46142 = CARTESIAN_POINT ( 'NONE',  ( 32.09598329127620531, -23.42844715994129956, 117.4678068554150485 ) ) ;
#46143 = ORIENTED_EDGE ( 'NONE', *, *, #76553, .T. ) ;
#46144 = CIRCLE ( 'NONE', #62118, 3.968749999999992895 ) ;
#46145 = DIRECTION ( 'NONE',  ( 0.000000000000000000, 0.000000000000000000, -1.000000000000000000 ) ) ;
#46147 = EDGE_CURVE ( 'NONE', #71852, #82635, #49562, .T. ) ;
#46146 = VECTOR ( 'NONE', #51655, 1000.000000000000000 ) ;
#46148 = ORIENTED_EDGE ( 'NONE', *, *, #62505, .T. ) ;
#46149 = FACE_OUTER_BOUND ( 'NONE', #3464, .T. ) ;
#46150 = CARTESIAN_POINT ( 'NONE',  ( 114.5675797908445475, -44.02050044317889643, 98.21276813305395592 ) ) ;
#46151 = DIRECTION ( 'NONE',  ( 0.000000000000000000, 0.000000000000000000, 1.000000000000000000 ) ) ;
#46152 = DIRECTION ( 'NONE',  ( 1.000000000000000078E-15, -1.000000000000000000, 0.000000000000000000 ) ) ;
#46153 = DIRECTION ( 'NONE',  ( -0.8660254037844425934, 0.4999999999999931166, -1.549999999999981405E-14 ) ) ;
#46154 = CARTESIAN_POINT ( 'NONE',  ( 96.76615086495793605, -37.93025403122317130, 86.43086337114897333 ) ) ;
#46156 = CARTESIAN_POINT ( 'NONE',  ( 117.4047238282098249, -30.98758422922437106, 175.2299109901969700 ) ) ;
#46155 = CARTESIAN_POINT ( 'NONE',  ( -72.96458098368600531, 101.5999999999999943, -67.92268098368781182 ) ) ;
#46157 = LINE ( 'NONE', #25286, #77066 ) ;
#46158 = DIRECTION ( 'NONE',  ( 0.000000000000000000, 0.000000000000000000, 1.000000000000000000 ) ) ;
#46159 = ORIENTED_EDGE ( 'NONE', *, *, #76774, .T. ) ;
#46160 = CARTESIAN_POINT ( 'NONE',  ( 188.5667039024479834, -58.35344715994099829, 170.4678068554149775 ) ) ;
#46161 = AXIS2_PLACEMENT_3D ( 'NONE', #42430, #70154, #7926 ) ;
#46162 = CARTESIAN_POINT ( 'NONE',  ( 194.5667039024482676, -40.82844715993405060, 129.9678068554150343 ) ) ;
#46163 = CARTESIAN_POINT ( 'NONE',  ( 116.3197976069899795, -32.94561274469138112, 134.1356252759109680 ) ) ;
#46164 = CIRCLE ( 'NONE', #7034, 7.999999999999992895 ) ;
#46165 = ADVANCED_FACE ( 'NONE', ( #20405 ), #48076, .F. ) ;
#46166 = FACE_OUTER_BOUND ( 'NONE', #69542, .T. ) ;
#46168 = ORIENTED_EDGE ( 'NONE', *, *, #57404, .T. ) ;
#46167 = CARTESIAN_POINT ( 'NONE',  ( 114.6374585114582771, -29.49847210400304576, 234.4327681330539690 ) ) ;
#46169 = CARTESIAN_POINT ( 'NONE',  ( 97.06384626284506112, -37.34233656640287791, 146.3752414903799774 ) ) ;
#46170 = CARTESIAN_POINT ( 'NONE',  ( 97.79230575738172604, -40.52535926896634777, 7.635625275910939536 ) ) ;
#46171 = CARTESIAN_POINT ( 'NONE',  ( 117.7479605218750862, -39.74664297364158472, 139.6194347997199827 ) ) ;
#46172 = CARTESIAN_POINT ( 'NONE',  ( 6.938893903907228378E-15, 149.3723753486177088, 113.8826257785461280 ) ) ;
#46173 = CARTESIAN_POINT ( 'NONE',  ( 12.29205751230852073, 85.84923025428284404, -129.9761558897303644 ) ) ;
#46174 = CARTESIAN_POINT ( 'NONE',  ( 156.5667039024481255, -42.82844715993568485, 257.2178068554149490 ) ) ;
#46175 = CARTESIAN_POINT ( 'NONE',  ( 123.6837132603319560, -52.08770651782484862, 218.8274735512161158 ) ) ;
#46176 = ORIENTED_EDGE ( 'NONE', *, *, #3216, .F. ) ;
#46177 = EDGE_LOOP ( 'NONE', ( #60726, #84629 ) ) ;
#46178 = ORIENTED_EDGE ( 'NONE', *, *, #46010, .F. ) ;
#46179 = VECTOR ( 'NONE', #4501, 1000.000000000000000 ) ;
#46180 = ORIENTED_EDGE ( 'NONE', *, *, #72161, .T. ) ;
#46181 = DIRECTION ( 'NONE',  ( 0.000000000000000000, 0.000000000000000000, -1.000000000000000000 ) ) ;
#46182 = CARTESIAN_POINT ( 'NONE',  ( 101.6204011159890541, -47.22657592904984369, 13.19562527591094891 ) ) ;
#46183 = DIRECTION ( 'NONE',  ( 0.000000000000000000, 0.000000000000000000, -1.000000000000000000 ) ) ;
#46184 = CARTESIAN_POINT ( 'NONE',  ( 188.5667039024479834, -62.87844715994099687, 257.2178068554150059 ) ) ;
#46185 = EDGE_CURVE ( 'NONE', #87456, #78504, #88552, .T. ) ;
#46187 = CARTESIAN_POINT ( 'NONE',  ( 100.8961411191535973, 127.0000000000000000, 3.968750000000400124 ) ) ;
#46186 = CARTESIAN_POINT ( 'NONE',  ( 180.2121375201600131, -29.73316016639650172, -5.074374724088000832 ) ) ;
#46188 = AXIS2_PLACEMENT_3D ( 'NONE', #22252, #34514, #7712 ) ;
#46189 = CARTESIAN_POINT ( 'NONE',  ( 102.6292086192877946, -44.02785282196147421, 246.5638483995049626 ) ) ;
#46190 = EDGE_LOOP ( 'NONE', ( #60201, #43906, #70700, #83113 ) ) ;
#46191 = AXIS2_PLACEMENT_3D ( 'NONE', #76389, #14624, #85802 ) ;
#46192 = ORIENTED_EDGE ( 'NONE', *, *, #64014, .T. ) ;
#46193 = VERTEX_POINT ( 'NONE', #6760 ) ;
#46194 = DIRECTION ( 'NONE',  ( 1.000000000000000078E-15, 1.000000000000000083E-30, -1.000000000000000000 ) ) ;
#46195 = DIRECTION ( 'NONE',  ( -0.000000000000000000, 1.000000000000000000, 0.000000000000000000 ) ) ;
#46196 = DIRECTION ( 'NONE',  ( 0.000000000000000000, 0.000000000000000000, 1.000000000000000000 ) ) ;
#46197 = CARTESIAN_POINT ( 'NONE',  ( 110.6847694559308621, -28.64017749364363397, 21.17301187732595480 ) ) ;
#46198 = CARTESIAN_POINT ( 'NONE',  ( 118.3860192952350161, 93.55239623846827612, 6.356965277240638201 ) ) ;
#46199 = ADVANCED_FACE ( 'NONE', ( #53984 ), #26311, .T. ) ;
#46200 = DIRECTION ( 'NONE',  ( -1.000000000000000000, 0.000000000000000000, 2.820351377559424413E-14 ) ) ;
#46201 = EDGE_CURVE ( 'NONE', #40366, #16110, #11913, .T. ) ;
#46202 = CARTESIAN_POINT ( 'NONE',  ( 116.2779988688840547, -41.49250982992363390, 243.4346728949589647 ) ) ;
#46203 = CARTESIAN_POINT ( 'NONE',  ( 19.56670390244648416, -25.42844715994203852, 129.9678068554150627 ) ) ;
#46204 = ORIENTED_EDGE ( 'NONE', *, *, #69069, .T. ) ;
#46205 = AXIS2_PLACEMENT_3D ( 'NONE', #65620, #58788, #10649 ) ;
#46206 = CARTESIAN_POINT ( 'NONE',  ( -103.1875000000000000, 127.0000000000000000, -5.041900000001080073 ) ) ;
#46207 = DIRECTION ( 'NONE',  ( 0.000000000000000000, 0.000000000000000000, -1.000000000000000000 ) ) ;
#46208 = CARTESIAN_POINT ( 'NONE',  ( 100.8021347340043690, -42.70095134221056554, 34.73856656006796584 ) ) ;
#46209 = AXIS2_PLACEMENT_3D ( 'NONE', #20080, #25992, #68674 ) ;
#46210 = CONICAL_SURFACE ( 'NONE', #17203, 17.00000000000090239, 0.7853981633974447263 ) ;
#46211 = CARTESIAN_POINT ( 'NONE',  ( 136.1113402350857484, -16.88977106734701294, 7.516154048581690006 ) ) ;
#46212 = DIRECTION ( 'NONE',  ( 0.000000000000000000, 1.000000000000000000, 0.000000000000000000 ) ) ;
#46213 = LINE ( 'NONE', #19429, #18420 ) ;
#46214 = ORIENTED_EDGE ( 'NONE', *, *, #15559, .T. ) ;
#46215 = CYLINDRICAL_SURFACE ( 'NONE', #16082, 0.5000000000000079936 ) ;
#46216 = CIRCLE ( 'NONE', #56352, 2.517499999999998739 ) ;
#46217 = CARTESIAN_POINT ( 'NONE',  ( 120.1244329748395643, 57.02142899650635854, -51.13721865063806860 ) ) ;
#46218 = ORIENTED_EDGE ( 'NONE', *, *, #58185, .T. ) ;
#46219 = CARTESIAN_POINT ( 'NONE',  ( 111.0826007845189736, -25.57995003598136208, 99.80133956162498521 ) ) ;
#46220 = EDGE_LOOP ( 'NONE', ( #82687, #43352, #70894, #62181 ) ) ;
#46221 = CARTESIAN_POINT ( 'NONE',  ( 98.53752338633383090, -37.19093893883378144, 75.79241982807700140 ) ) ;
#46222 = VECTOR ( 'NONE', #81888, 1000.000000000000000 ) ;
#46223 = CARTESIAN_POINT ( 'NONE',  ( 97.81554923370184440, -40.52685731699395433, 87.63597259388511418 ) ) ;
#46224 = CARTESIAN_POINT ( 'NONE',  ( 97.69004538871082843, -40.41090301495324155, 93.05586902018298190 ) ) ;
#46225 = CARTESIAN_POINT ( 'NONE',  ( 156.5667039024483529, -48.82844715993569196, 293.2178068554149490 ) ) ;
#46226 = AXIS2_PLACEMENT_3D ( 'NONE', #29895, #42152, #30340 ) ;
#46227 = CARTESIAN_POINT ( 'NONE',  ( 168.3664380525668491, -48.62818131005487743, 129.9678068554150059 ) ) ;
#46228 = CARTESIAN_POINT ( 'NONE',  ( 104.2350475155005114, -46.78530274442771031, 18.35848241876792031 ) ) ;
#46229 = CARTESIAN_POINT ( 'NONE',  ( 97.81151460250711693, -40.51751193867107759, 182.6359910548048333 ) ) ;
#46230 = ORIENTED_EDGE ( 'NONE', *, *, #59029, .T. ) ;
#46231 = DIRECTION ( 'NONE',  ( 1.000000000000000078E-15, -1.000000000000000083E-30, -1.000000000000000000 ) ) ;
#46232 = EDGE_LOOP ( 'NONE', ( #11422, #67315, #60993, #44872 ) ) ;
#46233 = CARTESIAN_POINT ( 'NONE',  ( -118.0433965939931653, 76.18740257834569718, 11.02250383333912787 ) ) ;
#46234 = VERTEX_POINT ( 'NONE', #62618 ) ;
#46235 = VERTEX_POINT ( 'NONE', #12694 ) ;
#46236 = EDGE_CURVE ( 'NONE', #69797, #48853, #65529, .T. ) ;
#46237 = CARTESIAN_POINT ( 'NONE',  ( 80.06648329127402519, -46.72944715994105991, 1.625625275910943746 ) ) ;
#46238 = ORIENTED_EDGE ( 'NONE', *, *, #77372, .T. ) ;
#46239 = CARTESIAN_POINT ( 'NONE',  ( 97.40895461294492463, -34.98419235835273611, 241.1841967044829573 ) ) ;
#46240 = CARTESIAN_POINT ( 'NONE',  ( 97.03505442595846375, -37.08857983863578767, 126.3541045800583049 ) ) ;
#46241 = CARTESIAN_POINT ( 'NONE',  ( 124.0667039024470313, -104.2784471599417486, -9.937637710810031777 ) ) ;
#46242 = CARTESIAN_POINT ( 'NONE',  ( 98.72253030179433608, -42.97932203522270100, 62.83848241876793850 ) ) ;
#46243 = CARTESIAN_POINT ( 'NONE',  ( 99.08951106268413866, -42.79544243366853351, 42.84391520899005457 ) ) ;
#46244 = ORIENTED_EDGE ( 'NONE', *, *, #15338, .T. ) ;
#46245 = DIRECTION ( 'NONE',  ( -4.299999999999999979E-14, 1.000000000000000000, -4.400000000000000367E-29 ) ) ;
#46246 = CARTESIAN_POINT ( 'NONE',  ( 194.5664832912729878, -71.37844715994266664, 361.9756252759109998 ) ) ;
#46248 = ORIENTED_EDGE ( 'NONE', *, *, #4194, .F. ) ;
#46247 = AXIS2_PLACEMENT_3D ( 'NONE', #60737, #67117, #67566 ) ;
#46249 = DIRECTION ( 'NONE',  ( 1.000000000000000078E-15, -1.000000000000000083E-30, -1.000000000000000000 ) ) ;
#46250 = EDGE_CURVE ( 'NONE', #9288, #75492, #62673, .T. ) ;
#46251 = CARTESIAN_POINT ( 'NONE',  ( -492.0614999999999668, 14.28749999999982201, 95.25000000000000000 ) ) ;
#46252 = CARTESIAN_POINT ( 'NONE',  ( 109.2074818670226222, -48.35976665079991221, 277.7213395616254843 ) ) ;
#46253 = DIRECTION ( 'NONE',  ( 0.000000000000000000, 0.000000000000000000, -1.000000000000000000 ) ) ;
#46254 = LINE ( 'NONE', #66264, #62280 ) ;
#46255 = CARTESIAN_POINT ( 'NONE',  ( 77.31651901074906164, -36.90078909148913056, 3.101427792080711843 ) ) ;
#46256 = CARTESIAN_POINT ( 'NONE',  ( 110.2012955024488718, -28.75291567525416170, 269.2009912566482512 ) ) ;
#46258 = CARTESIAN_POINT ( 'NONE',  ( 117.9791962420229794, -38.33460093242096178, 69.72229194257801055 ) ) ;
#46257 = DIRECTION ( 'NONE',  ( 0.000000000000000000, 0.000000000000000000, -1.000000000000000000 ) ) ;
#46259 = CARTESIAN_POINT ( 'NONE',  ( 111.6142026935021079, 65.77908918206766486, 67.72842572080216428 ) ) ;
#46260 = CARTESIAN_POINT ( 'NONE',  ( 108.9929891821633134, -47.66111943275755181, 122.7032443235299723 ) ) ;
#46261 = ORIENTED_EDGE ( 'NONE', *, *, #51430, .T. ) ;
#46262 = CYLINDRICAL_SURFACE ( 'NONE', #71363, 2.517500000000005844 ) ;
#46263 = EDGE_LOOP ( 'NONE', ( #76998, #3760 ) ) ;
#46264 = EDGE_CURVE ( 'NONE', #44506, #37176, #13511, .T. ) ;
#46265 = CARTESIAN_POINT ( 'NONE',  ( 19.56648329127303043, 15.62155284005731204, 361.9756252759109998 ) ) ;
#46266 = DIRECTION ( 'NONE',  ( -1.000000000000000000, -1.000000000000000078E-15, -1.000000000000000078E-15 ) ) ;
#46267 = CARTESIAN_POINT ( 'NONE',  ( 131.0667039024480118, -67.87844715994100397, 231.5838068554150198 ) ) ;
#46268 = ORIENTED_EDGE ( 'NONE', *, *, #64992, .F. ) ;
#46269 = EDGE_CURVE ( 'NONE', #64364, #7616, #58329, .T. ) ;
#46270 = AXIS2_PLACEMENT_3D ( 'NONE', #52294, #85541, #16484 ) ;
#46271 = ADVANCED_FACE ( 'NONE', ( #69889 ), #22648, .T. ) ;
#46272 = CARTESIAN_POINT ( 'NONE',  ( 97.06384492438512268, -37.34231416522206359, 51.37523970808266682 ) ) ;
#46274 = ORIENTED_EDGE ( 'NONE', *, *, #9135, .F. ) ;
#46273 = CARTESIAN_POINT ( 'NONE',  ( 114.5591802247839865, -28.54312911867770808, 154.4746728949589851 ) ) ;
#46275 = CARTESIAN_POINT ( 'NONE',  ( -194.1576000000000022, 101.5999999999999943, -45.33899999999999864 ) ) ;
#46276 = DIRECTION ( 'NONE',  ( 1.000000000000000000, 0.000000000000000000, 2.279500465453769633E-16 ) ) ;
#46277 = DIRECTION ( 'NONE',  ( -0.0001713722455994026977, 0.9999999853157766072, 0.000000000000000000 ) ) ;
#46278 = EDGE_CURVE ( 'NONE', #5529, #36268, #15827, .T. ) ;
#46280 = DIRECTION ( 'NONE',  ( 1.000000000000000078E-15, -1.000000000000000083E-30, -1.000000000000000000 ) ) ;
#46279 = VECTOR ( 'NONE', #415, 1000.000000000000000 ) ;
#46281 = ORIENTED_EDGE ( 'NONE', *, *, #51344, .T. ) ;
#46282 = VECTOR ( 'NONE', #31830, 1000.000000000000000 ) ;
#46283 = CARTESIAN_POINT ( 'NONE',  ( 97.59689953814545049, -30.98293302709309671, 125.8803871806719599 ) ) ;
#46284 = APPLICATION_PROTOCOL_DEFINITION ( 'draft international standard', 'automotive_design', 1998, #44601 ) ;
#46285 = EDGE_CURVE ( 'NONE', #32339, #89909, #43951, .T. ) ;
#46286 = DIRECTION ( 'NONE',  ( 0.000000000000000000, 1.000000000000000000, 0.000000000000000000 ) ) ;
#46287 = FACE_OUTER_BOUND ( 'NONE', #20986, .T. ) ;
#46288 = VERTEX_POINT ( 'NONE', #71686 ) ;
#46289 = ORIENTED_EDGE ( 'NONE', *, *, #32663, .T. ) ;
#46290 = CYLINDRICAL_SURFACE ( 'NONE', #62637, 0.4999999999999976685 ) ;
#46291 = DIRECTION ( 'NONE',  ( 0.000000000000000000, -1.000000000000000000, 0.000000000000000000 ) ) ;
#46292 = DIRECTION ( 'NONE',  ( -0.9254794337955620787, -0.3787978585227822492, 0.000000000000000000 ) ) ;
#46293 = ADVANCED_FACE ( 'NONE', ( #1752 ), #81574, .F. ) ;
#46294 = CARTESIAN_POINT ( 'NONE',  ( -69.72411017812909506, 120.6499999999999915, -69.72411017813089984 ) ) ;
#46295 = CIRCLE ( 'NONE', #52059, 2.517500000000005844 ) ;
#46297 = CARTESIAN_POINT ( 'NONE',  ( 167.7413838386817133, -48.33240602328261559, 300.4678068554149490 ) ) ;
#46296 = CARTESIAN_POINT ( 'NONE',  ( 98.34980471865662821, -31.65668200773688667, 105.9064674098472665 ) ) ;
#46298 = FACE_OUTER_BOUND ( 'NONE', #83895, .T. ) ;
#46299 = ORIENTED_EDGE ( 'NONE', *, *, #87943, .T. ) ;
#46300 = CARTESIAN_POINT ( 'NONE',  ( 57.56670390244722313, -42.82844715994040996, 134.7178068554150911 ) ) ;
#46301 = CARTESIAN_POINT ( 'NONE',  ( 110.2867295656602380, -27.49400189596552835, 205.8099109901959594 ) ) ;
#46302 = AXIS2_PLACEMENT_3D ( 'NONE', #35778, #72106, #63492 ) ;
#46304 = VERTEX_POINT ( 'NONE', #15385 ) ;
#46303 = CARTESIAN_POINT ( 'NONE',  ( 107.0664832912740252, -36.72944715994103149, -5.074374724089029343 ) ) ;
#46305 = EDGE_CURVE ( 'NONE', #87926, #86967, #70794, .T. ) ;
#46306 = CARTESIAN_POINT ( 'NONE',  ( 103.8130989789263765, -45.95327097697893493, 53.30705384733897034 ) ) ;
#46308 = EDGE_CURVE ( 'NONE', #32467, #944, #71389, .T. ) ;
#46307 = CARTESIAN_POINT ( 'NONE',  ( 107.0664832912739968, -36.72944715994100306, 287.6356252759109680 ) ) ;
#46309 = CARTESIAN_POINT ( 'NONE',  ( 69.94830149775677341, -138.0565978109353864, 247.6574394596379989 ) ) ;
#46310 = EDGE_CURVE ( 'NONE', #34506, #16953, #4645, .T. ) ;
#46311 = CARTESIAN_POINT ( 'NONE',  ( 97.81171347387959258, -40.51745984142272761, 22.63530404563221410 ) ) ;
#46312 = ORIENTED_EDGE ( 'NONE', *, *, #12325, .F. ) ;
#46313 = PLANE ( 'NONE',  #86389 ) ;
#46314 = EDGE_CURVE ( 'NONE', #82100, #78126, #29301, .T. ) ;
#46315 = ORIENTED_EDGE ( 'NONE', *, *, #20878, .T. ) ;
#46316 = EDGE_LOOP ( 'NONE', ( #12377, #4367, #8179, #11150 ) ) ;
#46317 = AXIS2_PLACEMENT_3D ( 'NONE', #104, #6466, #35055 ) ;
#46318 = CARTESIAN_POINT ( 'NONE',  ( 111.6463204169710082, -44.35094448583814852, 234.4387261630399450 ) ) ;
#46319 = DIRECTION ( 'NONE',  ( -1.000000000000000000, -4.299999999999999979E-14, -1.000000000000000078E-15 ) ) ;
#46320 = CARTESIAN_POINT ( 'NONE',  ( -85.31607583734405864, 90.93081950567957961, 98.82361644294769576 ) ) ;
#46321 = DIRECTION ( 'NONE',  ( 0.000000000000000000, 1.000000000000000000, 0.000000000000000000 ) ) ;
#46322 = DIRECTION ( 'NONE',  ( -1.907762142705490052E-15, -7.167082501179359715E-16, 1.000000000000000000 ) ) ;
#46323 = ORIENTED_EDGE ( 'NONE', *, *, #78635, .F. ) ;
#46324 = CIRCLE ( 'NONE', #4347, 7.143750000000004263 ) ;
#46325 = LINE ( 'NONE', #31818, #14518 ) ;
#46326 = LINE ( 'NONE', #86804, #3461 ) ;
#46327 = ORIENTED_EDGE ( 'NONE', *, *, #37291, .F. ) ;
#46328 = CARTESIAN_POINT ( 'NONE',  ( 112.3272512417296980, -28.22507648531173530, 289.6356252759109680 ) ) ;
#46329 = ORIENTED_EDGE ( 'NONE', *, *, #80192, .T. ) ;
#46330 = ORIENTED_EDGE ( 'NONE', *, *, #44114, .T. ) ;
#46331 = CARTESIAN_POINT ( 'NONE',  ( 102.5467118750096631, -28.62589253813684209, 253.2995189410198691 ) ) ;
#46332 = VECTOR ( 'NONE', #61165, 999.9999999999998863 ) ;
#46333 = CARTESIAN_POINT ( 'NONE',  ( 0.000000000000000000, 20.32000000000000028, 0.000000000000000000 ) ) ;
#46334 = DIRECTION ( 'NONE',  ( -0.9659258262890706437, 0.000000000000000000, 0.2588190451025119132 ) ) ;
#46335 = CARTESIAN_POINT ( 'NONE',  ( 120.1849926298398401, -37.85453553205690724, 296.5517437918485939 ) ) ;
#46336 = DIRECTION ( 'NONE',  ( 1.000000000000000078E-15, -1.000000000000000083E-30, -1.000000000000000000 ) ) ;
#46337 = CARTESIAN_POINT ( 'NONE',  ( 110.1502920506493552, -26.06700738780482141, 210.8403871806729626 ) ) ;
#46338 = CARTESIAN_POINT ( 'NONE',  ( 131.0667039024480118, -64.87844715994098976, 231.5838068554150198 ) ) ;
#46339 = CIRCLE ( 'NONE', #18804, 10.66800000000000992 ) ;
#46340 = ORIENTED_EDGE ( 'NONE', *, *, #86717, .T. ) ;
#46341 = CARTESIAN_POINT ( 'NONE',  ( 114.3835678416600672, -44.21631923246377482, 69.19276813305397411 ) ) ;
#46342 = CARTESIAN_POINT ( 'NONE',  ( 107.0667039024470313, -104.2784471599409528, 25.71780685541800437 ) ) ;
#46343 = ORIENTED_EDGE ( 'NONE', *, *, #44435, .T. ) ;
#46344 = VERTEX_POINT ( 'NONE', #8112 ) ;
#46345 = ORIENTED_EDGE ( 'NONE', *, *, #35655, .T. ) ;
#46346 = VECTOR ( 'NONE', #25140, 1000.000000000000000 ) ;
#46347 = DIRECTION ( 'NONE',  ( -0.7071067811865774377, 0.7071067811865175967, -7.071067811865782003E-16 ) ) ;
#46348 = CARTESIAN_POINT ( 'NONE',  ( 122.2221484686747459, -108.0760968907521828, -11.78219314458189793 ) ) ;
#46349 = AXIS2_PLACEMENT_3D ( 'NONE', #44059, #3202, #86315 ) ;
#46350 = CARTESIAN_POINT ( 'NONE',  ( 177.1649999999999920, 14.63749999999999929, -14.28749999999999964 ) ) ;
#46351 = CARTESIAN_POINT ( 'NONE',  ( 114.9429295168758784, -34.48920150425379916, 146.8652332267339773 ) ) ;
#46352 = CARTESIAN_POINT ( 'NONE',  ( 111.6179861195847849, -46.13269558042843244, 243.9356252759109509 ) ) ;
#46353 = LINE ( 'NONE', #74085, #17394 ) ;
#46354 = VERTEX_POINT ( 'NONE', #29451 ) ;
#46355 = AXIS2_PLACEMENT_3D ( 'NONE', #28389, #1148, #68841 ) ;
#46356 = CARTESIAN_POINT ( 'NONE',  ( 0.000000000000000000, 12.27000000000000313, -9.525000000000000355 ) ) ;
#46357 = ORIENTED_EDGE ( 'NONE', *, *, #42984, .T. ) ;
#46358 = ORIENTED_EDGE ( 'NONE', *, *, #37728, .F. ) ;
#46359 = DIRECTION ( 'NONE',  ( 0.000000000000000000, 0.000000000000000000, 1.000000000000000000 ) ) ;
#46360 = EDGE_CURVE ( 'NONE', #33131, #75751, #21290, .T. ) ;
#46361 = ORIENTED_EDGE ( 'NONE', *, *, #34180, .T. ) ;
#46362 = VERTEX_POINT ( 'NONE', #64417 ) ;
#46363 = DIRECTION ( 'NONE',  ( 0.000000000000000000, -1.000000000000000000, 0.000000000000000000 ) ) ;
#46364 = CARTESIAN_POINT ( 'NONE',  ( 68.53801554307389665, 120.6499999999999915, 74.15067561874289481 ) ) ;
#46365 = EDGE_CURVE ( 'NONE', #79928, #34694, #69946, .T. ) ;
#46366 = LINE ( 'NONE', #74101, #5459 ) ;
#46367 = CIRCLE ( 'NONE', #65262, 15.99999999999999822 ) ;
#46368 = CARTESIAN_POINT ( 'NONE',  ( 103.7078221352084881, -28.31921139840152435, 174.8133722090289552 ) ) ;
#46369 = CARTESIAN_POINT ( 'NONE',  ( 95.20909952976953150, -35.71394341709248721, 36.25848241876794731 ) ) ;
#46370 = CARTESIAN_POINT ( 'NONE',  ( 72.90080881784491851, -85.71128516271417652, 248.3919653347779786 ) ) ;
#46371 = ORIENTED_EDGE ( 'NONE', *, *, #60662, .F. ) ;
#46372 = EDGE_CURVE ( 'NONE', #15887, #34773, #13337, .T. ) ;
#46373 = CARTESIAN_POINT ( 'NONE',  ( -492.0614999999999668, 14.28750000000026077, 11.11249999999970051 ) ) ;
#46374 = VERTEX_POINT ( 'NONE', #85335 ) ;
#46375 = EDGE_CURVE ( 'NONE', #64021, #3056, #30350, .T. ) ;
#46376 = ADVANCED_FACE ( 'NONE', ( #844 ), #42160, .F. ) ;
#46377 = DIRECTION ( 'NONE',  ( -4.299999999999999979E-14, 1.000000000000000000, -4.400000000000000367E-29 ) ) ;
#46378 = EDGE_LOOP ( 'NONE', ( #66871, #14905, #57858, #86862 ) ) ;
#46379 = DIRECTION ( 'NONE',  ( 1.000000000000000000, 0.000000000000000000, 0.000000000000000000 ) ) ;
#46380 = CARTESIAN_POINT ( 'NONE',  ( 177.8371591254543489, -47.82818131005477369, 237.4678068554150059 ) ) ;
#46381 = CARTESIAN_POINT ( 'NONE',  ( 107.0664832912739968, -36.72944715994100306, -2.364374724089013391 ) ) ;
#46382 = AXIS2_PLACEMENT_3D ( 'NONE', #54024, #87250, #31372 ) ;
#46383 = ADVANCED_FACE ( 'NONE', ( #44397 ), #87542, .F. ) ;
#46384 = DIRECTION ( 'NONE',  ( 3.100000000000000258E-29, -3.100000000000000044E-14, -1.000000000000000000 ) ) ;
#46385 = EDGE_LOOP ( 'NONE', ( #82828, #6068, #50237 ) ) ;
#46386 = CARTESIAN_POINT ( 'NONE',  ( 104.7307148508592007, -47.55717207929887991, 32.41943479972098174 ) ) ;
#46387 = CARTESIAN_POINT ( 'NONE',  ( 118.0344259573852810, -38.43289426264998099, 64.69181575210097890 ) ) ;
#46388 = ADVANCED_FACE ( 'NONE', ( #10345 ), #73451, .F. ) ;
#46390 = DIRECTION ( 'NONE',  ( 0.000000000000000000, 1.000000000000000000, 0.000000000000000000 ) ) ;
#46389 = PLANE ( 'NONE',  #43368 ) ;
#46391 = DIRECTION ( 'NONE',  ( -1.000000000000000000, 0.000000000000000000, 3.596091637922019804E-15 ) ) ;
#46392 = DIRECTION ( 'NONE',  ( 0.000000000000000000, -1.000000000000000000, 0.000000000000000000 ) ) ;
#46393 = DIRECTION ( 'NONE',  ( 0.000000000000000000, 0.000000000000000000, -1.000000000000000000 ) ) ;
#46394 = AXIS2_PLACEMENT_3D ( 'NONE', #44432, #71285, #1791 ) ;
#46395 = DIRECTION ( 'NONE',  ( -0.2588190451025170757, 0.000000000000000000, 0.9659258262890693114 ) ) ;
#46396 = EDGE_CURVE ( 'NONE', #80032, #74036, #11226, .T. ) ;
#46397 = CARTESIAN_POINT ( 'NONE',  ( 145.8343148362385477, -124.3925565579663015, 247.4656831979029903 ) ) ;
#46398 = AXIS2_PLACEMENT_3D ( 'NONE', #60598, #47860, #75598 ) ;
#46399 = ORIENTED_EDGE ( 'NONE', *, *, #40986, .F. ) ;
#46400 = CARTESIAN_POINT ( 'NONE',  ( 115.6098187009959304, -42.78073513203698042, 53.33562527591095659 ) ) ;
#46401 = CARTESIAN_POINT ( 'NONE',  ( 103.3035667682879932, -27.00715593367326406, 211.3699109901969848 ) ) ;
#46402 = CARTESIAN_POINT ( 'NONE',  ( 107.2325526940309288, -25.65435679020650639, 76.07657765686298035 ) ) ;
#46404 = CARTESIAN_POINT ( 'NONE',  ( 41.56648329127398966, -18.82844715994071194, 198.9256252759119832 ) ) ;
#46403 = CARTESIAN_POINT ( 'NONE',  ( 115.7842991311344321, -41.80029728880780482, 173.4030991392274643 ) ) ;
#46405 = DIRECTION ( 'NONE',  ( 1.000000000000000078E-15, -1.000000000000000083E-30, -1.000000000000000000 ) ) ;
#46406 = EDGE_CURVE ( 'NONE', #22588, #89625, #48235, .T. ) ;
#46407 = CIRCLE ( 'NONE', #81272, 50.79999999999999716 ) ;
#46408 = DIRECTION ( 'NONE',  ( 0.000000000000000000, 0.000000000000000000, 1.000000000000000000 ) ) ;
#46409 = ORIENTED_EDGE ( 'NONE', *, *, #6491, .F. ) ;
#46410 = CARTESIAN_POINT ( 'NONE',  ( 117.2073019650708261, -38.89799087863979565, 104.6708633711489824 ) ) ;
#46411 = VECTOR ( 'NONE', #28730, 1000.000000000000000 ) ;
#46413 = EDGE_LOOP ( 'NONE', ( #18673, #5105, #7484, #30723 ) ) ;
#46412 = CARTESIAN_POINT ( 'NONE',  ( 106.0667039024470171, -87.35579742913164125, -19.26696060647653397 ) ) ;
#46414 = CARTESIAN_POINT ( 'NONE',  ( 95.31970492887387536, -38.09378048407035777, 232.4184824187679794 ) ) ;
#46415 = CARTESIAN_POINT ( 'NONE',  ( 163.1543517358493034, -31.62489322948541215, 342.9256252759109884 ) ) ;
#46416 = DIRECTION ( 'NONE',  ( 0.000000000000000000, 0.000000000000000000, 1.000000000000000000 ) ) ;
#46417 = AXIS2_PLACEMENT_3D ( 'NONE', #29654, #14243, #45052 ) ;
#46418 = CARTESIAN_POINT ( 'NONE',  ( 107.0664832912739399, -36.72944715994095333, 292.6356252759106837 ) ) ;
#46419 = CARTESIAN_POINT ( 'NONE',  ( 102.0670549762224226, -27.97049805030057712, 81.48979194111957725 ) ) ;
#46420 = EDGE_CURVE ( 'NONE', #3477, #25056, #73008, .T. ) ;
#46421 = DIRECTION ( 'NONE',  ( 0.000000000000000000, -1.000000000000000000, 0.000000000000000000 ) ) ;
#46422 = DIRECTION ( 'NONE',  ( -4.299999999999999979E-14, 1.000000000000000000, -4.400000000000000367E-29 ) ) ;
#46423 = CIRCLE ( 'NONE', #63842, 16.00000000000090239 ) ;
#46424 = EDGE_CURVE ( 'NONE', #21031, #57125, #66638, .T. ) ;
#46425 = CARTESIAN_POINT ( 'NONE',  ( 116.4077482568849859, -39.73851878533137238, 158.5784824187689708 ) ) ;
#46426 = ORIENTED_EDGE ( 'NONE', *, *, #18105, .T. ) ;
#46427 = ORIENTED_EDGE ( 'NONE', *, *, #55731, .T. ) ;
#46428 = CARTESIAN_POINT ( 'NONE',  ( 112.9789619575112596, -30.12862337550717484, 110.9272975916109658 ) ) ;
#46429 = DIRECTION ( 'NONE',  ( -1.000000000000000000, -4.012088370409549976E-14, 0.000000000000000000 ) ) ;
#46431 = DIRECTION ( 'NONE',  ( 0.000000000000000000, 0.000000000000000000, -1.000000000000000000 ) ) ;
#46430 = CARTESIAN_POINT ( 'NONE',  ( 115.6529839569024602, -41.48189714014871043, 259.4241967044819717 ) ) ;
#46432 = LINE ( 'NONE', #4678, #55071 ) ;
#46433 = CARTESIAN_POINT ( 'NONE',  ( 141.0667039024479834, -58.35344715994099829, 10.91780685541479734 ) ) ;
#46434 = VECTOR ( 'NONE', #27520, 1000.000000000000114 ) ;
#46435 = DIRECTION ( 'NONE',  ( 0.000000000000000000, 0.000000000000000000, 1.000000000000000000 ) ) ;
#46436 = DIRECTION ( 'NONE',  ( -1.000000000000000000, 0.000000000000000000, 0.000000000000000000 ) ) ;
#46437 = FACE_OUTER_BOUND ( 'NONE', #86997, .T. ) ;
#46438 = CARTESIAN_POINT ( 'NONE',  ( -254.0000000000000000, 14.28750000000026077, 15.87499999999969802 ) ) ;
#46439 = CARTESIAN_POINT ( 'NONE',  ( 104.5678333644583944, -48.28820816006152938, 182.4070538473399665 ) ) ;
#46440 = LINE ( 'NONE', #55036, #57613 ) ;
#46441 = ORIENTED_EDGE ( 'NONE', *, *, #78833, .T. ) ;
#46442 = EDGE_LOOP ( 'NONE', ( #53992, #28183, #31317, #60550 ) ) ;
#46443 = CARTESIAN_POINT ( 'NONE',  ( -95.69968022530730423, 70.80031561532538831, -88.80809839403329420 ) ) ;
#46444 = CARTESIAN_POINT ( 'NONE',  ( 82.56634656605380940, -19.87725565068429745, 7.080220459968598945 ) ) ;
#46445 = LINE ( 'NONE', #5133, #5509 ) ;
#46446 = DIRECTION ( 'NONE',  ( 0.000000000000000000, 1.000000000000000000, 0.000000000000000000 ) ) ;
#46447 = B_SPLINE_CURVE_WITH_KNOTS ( 'NONE', 3,
 ( #52643, #4081, #80854, #80401 ),
 .UNSPECIFIED., .F., .F.,
 ( 4, 4 ),
 ( -0.3974825557268100162, -0.3842043193313789962 ),
 .UNSPECIFIED. ) ;
#46448 = ADVANCED_FACE ( 'NONE', ( #79404 ), #10772, .T. ) ;
#46449 = CARTESIAN_POINT ( 'NONE',  ( 163.0664832912739826, -18.82844715994099971, 335.9181252759120184 ) ) ;
#46450 = ORIENTED_EDGE ( 'NONE', *, *, #51420, .T. ) ;
#46451 = CARTESIAN_POINT ( 'NONE',  ( 108.3318470757233030, -46.73504102216281098, 62.67716460038835891 ) ) ;
#46452 = CARTESIAN_POINT ( 'NONE',  ( 114.8141470925876462, -29.70096138442027112, 209.4127681330539872 ) ) ;
#46453 = CARTESIAN_POINT ( 'NONE',  ( 134.0664828118826506, -39.47944715903992829, 8.225259175038003079 ) ) ;
#46454 = ORIENTED_EDGE ( 'NONE', *, *, #81317, .F. ) ;
#46455 = VERTEX_POINT ( 'NONE', #3972 ) ;
#46456 = VECTOR ( 'NONE', #54359, 1000.000000000000000 ) ;
#46457 = CARTESIAN_POINT ( 'NONE',  ( 25.56670390244829250, -48.82844715994168183, 290.7178068554150059 ) ) ;
#46458 = FACE_OUTER_BOUND ( 'NONE', #2600, .T. ) ;
#46459 = CARTESIAN_POINT ( 'NONE',  ( 100.8872385624251535, -44.70003263212168321, 167.0523370925745326 ) ) ;
#46460 = CARTESIAN_POINT ( 'NONE',  ( 109.7980830611816714, -44.45091405062262879, 35.66523322673398155 ) ) ;
#46461 = CARTESIAN_POINT ( 'NONE',  ( 113.8576076518026383, -28.74447221003411812, 135.5156252759109634 ) ) ;
#46462 = VECTOR ( 'NONE', #11914, 1000.000000000000000 ) ;
#46463 = CARTESIAN_POINT ( 'NONE',  ( 134.0664832912740110, -39.47944715994100306, 1.625625275910997480 ) ) ;
#46464 = ORIENTED_EDGE ( 'NONE', *, *, #68491, .T. ) ;
#46465 = FACE_OUTER_BOUND ( 'NONE', #45237, .T. ) ;
#46466 = EDGE_CURVE ( 'NONE', #84388, #73518, #66182, .T. ) ;
#46467 = CARTESIAN_POINT ( 'NONE',  ( 81.60736025278326622, -16.45223222829689647, 7.843813999038339979 ) ) ;
#46468 = VERTEX_POINT ( 'NONE', #72578 ) ;
#46470 = VERTEX_POINT ( 'NONE', #38931 ) ;
#46469 = VECTOR ( 'NONE', #79603, 1000.000000000000000 ) ;
#46471 = FACE_OUTER_BOUND ( 'NONE', #75204, .T. ) ;
#46472 = VERTEX_POINT ( 'NONE', #4428 ) ;
#46473 = VERTEX_POINT ( 'NONE', #59809 ) ;
#46474 = DIRECTION ( 'NONE',  ( 1.000000000000000000, 3.999999999999999995E-14, 1.000000000000000078E-15 ) ) ;
#46475 = EDGE_CURVE ( 'NONE', #39210, #71603, #25302, .T. ) ;
#46476 = CARTESIAN_POINT ( 'NONE',  ( 111.8977291718574065, -29.68564172797395528, 44.02099125664899049 ) ) ;
#46477 = CARTESIAN_POINT ( 'NONE',  ( 98.53312381531716824, -44.98873235655736380, 191.9384824187679612 ) ) ;
#46478 = EDGE_CURVE ( 'NONE', #63468, #82506, #52530, .T. ) ;
#46479 = CARTESIAN_POINT ( 'NONE',  ( 105.7232414704440941, -24.98023492732636441, 160.1670538473389627 ) ) ;
#46481 = CARTESIAN_POINT ( 'NONE',  ( 105.1675567143510364, -46.98732170830142962, 8.429910990196965770 ) ) ;
#46480 = CARTESIAN_POINT ( 'NONE',  ( 99.63323364162300777, -43.45394520487258916, 21.91156745383733195 ) ) ;
#46482 = DIRECTION ( 'NONE',  ( -0.02150753337723538411, -0.0009076677972193728959, -0.9997682742251812194 ) ) ;
#46483 = DIRECTION ( 'NONE',  ( -0.9999999853157766072, -0.0001713722456126752025, 0.000000000000000000 ) ) ;
#46484 = VERTEX_POINT ( 'NONE', #65738 ) ;
#46485 = ORIENTED_EDGE ( 'NONE', *, *, #30250, .T. ) ;
#46486 = EDGE_CURVE ( 'NONE', #24182, #67326, #37850, .T. ) ;
#46487 = DIRECTION ( 'NONE',  ( -1.000000000000000000, 0.000000000000000000, -2.108231265501709878E-16 ) ) ;
#46488 = CARTESIAN_POINT ( 'NONE',  ( 105.1026693892091117, -26.44596034844076371, 235.2270538473399313 ) ) ;
#46489 = EDGE_LOOP ( 'NONE', ( #82615, #87173, #26752, #9051 ) ) ;
#46490 = CARTESIAN_POINT ( 'NONE',  ( 96.05373888820416539, -35.78152935435744553, 186.2461014663869889 ) ) ;
#46491 = DIRECTION ( 'NONE',  ( 1.000000000000000000, 4.163336342344333240E-14, 0.000000000000000000 ) ) ;
#46492 = DIRECTION ( 'NONE',  ( -6.524622321627019585E-16, -4.013151879589939944E-16, -1.000000000000000000 ) ) ;
#46493 = CARTESIAN_POINT ( 'NONE',  ( -487.2989999999999782, 100.8062500000000057, 94.61194598552329182 ) ) ;
#46494 = CARTESIAN_POINT ( 'NONE',  ( 48.16670390244701139, -28.27351298637280408, 313.9678068554150059 ) ) ;
#46496 = CARTESIAN_POINT ( 'NONE',  ( 182.2738106836200132, -23.19206098993950604, -5.074374724088000832 ) ) ;
#46495 = CARTESIAN_POINT ( 'NONE',  ( 114.9409439400435531, -39.43770971423924721, 277.6356252759110248 ) ) ;
#46497 = CARTESIAN_POINT ( 'NONE',  ( 32.24491389930098251, -32.11662333284611748, -5.074374724088000832 ) ) ;
#46499 = ADVANCED_FACE ( 'NONE', ( #58045 ), #86653, .T. ) ;
#46498 = PLANE ( 'NONE',  #38133 ) ;
#46500 = CIRCLE ( 'NONE', #8811, 1.000000000000000888 ) ;
#46501 = DIRECTION ( 'NONE',  ( 0.000000000000000000, 1.000000000000000000, 0.000000000000000000 ) ) ;
#46502 = CONICAL_SURFACE ( 'NONE', #61039, 5.800000000000000711, 0.7853981633974476129 ) ;
#46503 = LINE ( 'NONE', #5650, #74756 ) ;
#46504 = CARTESIAN_POINT ( 'NONE',  ( 83.56670390244801183, -39.24694715994107952, 239.5838068554169809 ) ) ;
#46505 = CARTESIAN_POINT ( 'NONE',  ( 45.77381068356854144, -48.62134037881681081, 129.9678068554150911 ) ) ;
#46506 = EDGE_CURVE ( 'NONE', #34812, #12195, #40943, .T. ) ;
#46508 = ORIENTED_EDGE ( 'NONE', *, *, #40970, .F. ) ;
#46507 = CARTESIAN_POINT ( 'NONE',  ( -6.710838307577465578, 93.34022857041043153, -118.3664257206621784 ) ) ;
#46509 = LINE ( 'NONE', #67869, #22007 ) ;
#46510 = CARTESIAN_POINT ( 'NONE',  ( 117.7991783922927738, -31.64581934375353711, 214.1784824187679419 ) ) ;
#46511 = CARTESIAN_POINT ( 'NONE',  ( 110.1579320793587442, -46.68562272277494429, 93.81562527591097478 ) ) ;
#46512 = CARTESIAN_POINT ( 'NONE',  ( 96.63877784842330243, -35.80427747552585060, 227.2556252759109725 ) ) ;
#46513 = CYLINDRICAL_SURFACE ( 'NONE', #7743, 2.500000000000002220 ) ;
#46514 = DIRECTION ( 'NONE',  ( 0.7071067811865779928, -0.7071067811865171526, 7.071067811865475333E-16 ) ) ;
#46515 = VECTOR ( 'NONE', #84261, 1000.000000000000114 ) ;
#46517 = DIRECTION ( 'NONE',  ( 0.0001713722455994027248, -0.9999999853157766072, 0.000000000000000000 ) ) ;
#46516 = CARTESIAN_POINT ( 'NONE',  ( 172.5664832912729878, -18.82844715994071194, 258.9256252759120116 ) ) ;
#46518 = DIRECTION ( 'NONE',  ( -1.000000000000000078E-15, 1.000000000000000083E-30, 1.000000000000000000 ) ) ;
#46519 = CARTESIAN_POINT ( 'NONE',  ( 59.56670390244699576, -67.87844715994098976, 190.2178068554179902 ) ) ;
#46520 = AXIS2_PLACEMENT_3D ( 'NONE', #89167, #28261, #55956 ) ;
#46521 = B_SPLINE_CURVE_WITH_KNOTS ( 'NONE', 3,
 ( #15641, #50584, #37864, #78324, #51034, #16089, #64674, #43770, #43315, #71060, #36073, #71505, #9266, #56948, #64232, #8833, #65562, #71943 ),
 .UNSPECIFIED., .F., .F.,
 ( 4, 2, 2, 2, 2, 2, 2, 2, 4 ),
 ( 0.4999608178654283974, 0.5624657156322498963, 0.6249706133990713397, 0.6874755111658927831, 0.7499804089327142265, 0.8124853066995356698, 0.8749902044663571132, 0.9374951022331785566, 1.000000000000000000 ),
 .UNSPECIFIED. ) ;
#46522 = ORIENTED_EDGE ( 'NONE', *, *, #45745, .F. ) ;
#46523 = EDGE_LOOP ( 'NONE', ( #426, #18771, #73568, #35792 ) ) ;
#46524 = B_SPLINE_CURVE_WITH_KNOTS ( 'NONE', 3,
 ( #68214, #5996, #89104, #26865, #54543, #20062, #47742, #50437, #49982, #29117, #78632, #23225, #77721, #15499, #70911, #22308, #43170, #23656, #1863, #44062, #58157, #43617, #8683, #65423, #71797 ),
 .UNSPECIFIED., .F., .F.,
 ( 4, 2, 2, 2, 2, 2, 2, 2, 2, 1, 2, 2, 4 ),
 ( 0.05913659445472881082, 0.06159867070730776911, 0.06282970883359724479, 0.06406074695988672740, 0.06652282321246567875, 0.06775386133875516137, 0.06898489946504463011, 0.07144697571762360921, 0.07267801384391310571, 0.07390905197020260220, 0.07514009009649209869, 0.07637112822278158131, 0.07883320447536057429 ),
 .UNSPECIFIED. ) ;
#46525 = CARTESIAN_POINT ( 'NONE',  ( 112.9548150380649503, -42.91681406074877003, 157.6038483995049830 ) ) ;
#46527 = ORIENTED_EDGE ( 'NONE', *, *, #57624, .T. ) ;
#46526 = DIRECTION ( 'NONE',  ( 0.000000000000000000, 1.000000000000000000, 0.000000000000000000 ) ) ;
#46528 = CARTESIAN_POINT ( 'NONE',  ( 145.3595637443018234, -69.45303146431501773, 247.4784022495120155 ) ) ;
#46529 = CARTESIAN_POINT ( 'NONE',  ( 98.47671751366520709, -30.86049585540216711, 116.8499109901969604 ) ) ;
#46530 = DIRECTION ( 'NONE',  ( -0.0001211784769825758164, 0.7071067708032326982, -0.7071067811865484609 ) ) ;
#46531 = CIRCLE ( 'NONE', #11539, 6.349999999999999645 ) ;
#46532 = LINE ( 'NONE', #75613, #49941 ) ;
#46533 = AXIS2_PLACEMENT_3D ( 'NONE', #76153, #40728, #19400 ) ;
#46534 = CARTESIAN_POINT ( 'NONE',  ( -75.00102098090737002, 78.06989712577870932, 91.81719692706870717 ) ) ;
#46535 = CARTESIAN_POINT ( 'NONE',  ( 101.9936209472876527, -45.44607154236431512, 108.1564586098271405 ) ) ;
#46536 = EDGE_CURVE ( 'NONE', #67868, #57892, #74361, .T. ) ;
#46537 = CARTESIAN_POINT ( 'NONE',  ( 101.3196941207356758, -46.24713579373447914, 52.14419670448295108 ) ) ;
#46538 = ORIENTED_EDGE ( 'NONE', *, *, #89339, .F. ) ;
#46539 = ORIENTED_EDGE ( 'NONE', *, *, #60042, .F. ) ;
#46541 = ORIENTED_EDGE ( 'NONE', *, *, #80285, .F. ) ;
#46540 = AXIS2_PLACEMENT_3D ( 'NONE', #55766, #46731, #74460 ) ;
#46542 = LINE ( 'NONE', #74277, #794 ) ;
#46544 = CARTESIAN_POINT ( 'NONE',  ( 125.9611475301394847, -58.72944715994102438, 249.5838068554163840 ) ) ;
#46543 = CARTESIAN_POINT ( 'NONE',  ( 117.1372161989436904, -34.25576096370540569, 160.0061014663869798 ) ) ;
#46545 = DIRECTION ( 'NONE',  ( 0.000000000000000000, 1.000000000000000000, 0.000000000000000000 ) ) ;
#46546 = CARTESIAN_POINT ( 'NONE',  ( 172.5664832912740110, -18.82844715994099971, 318.9256252759120116 ) ) ;
#46547 = AXIS2_PLACEMENT_3D ( 'NONE', #44364, #17128, #71652 ) ;
#46548 = PLANE ( 'NONE',  #83755 ) ;
#46549 = CARTESIAN_POINT ( 'NONE',  ( 75.31670390244798341, -50.82844715994100682, 86.31780685541500020 ) ) ;
#46550 = CARTESIAN_POINT ( 'NONE',  ( 104.4079121328872617, -46.45803387014570518, 178.3647764060284260 ) ) ;
#46551 = CARTESIAN_POINT ( 'NONE',  ( 98.11562048848810491, -31.42749274529980852, 85.90133956162493689 ) ) ;
#46552 = VERTEX_POINT ( 'NONE', #55228 ) ;
#46553 = CIRCLE ( 'NONE', #65444, 4.500000000000003553 ) ;
#46554 = VERTEX_POINT ( 'NONE', #12585 ) ;
#46555 = EDGE_CURVE ( 'NONE', #18695, #86161, #53428, .T. ) ;
#46556 = LINE ( 'NONE', #13407, #6763 ) ;
#46557 = CARTESIAN_POINT ( 'NONE',  ( -88.53717826876616925, 94.12569442554142540, -95.94886839522614252 ) ) ;
#46558 = PLANE ( 'NONE',  #67032 ) ;
#46559 = CARTESIAN_POINT ( 'NONE',  ( 112.8577109034250583, -30.29807625619018197, 157.3233284648299559 ) ) ;
#46560 = EDGE_CURVE ( 'NONE', #18229, #40899, #88626, .T. ) ;
#46561 = CARTESIAN_POINT ( 'NONE',  ( 110.7536356736639078, -102.7271463785358492, -19.78219314458207378 ) ) ;
#46562 = ORIENTED_EDGE ( 'NONE', *, *, #85955, .F. ) ;
#46563 = VERTEX_POINT ( 'NONE', #60710 ) ;
#46564 = LINE ( 'NONE', #59307, #20673 ) ;
#46565 = VECTOR ( 'NONE', #49994, 1000.000000000000000 ) ;
#46566 = ORIENTED_EDGE ( 'NONE', *, *, #54600, .F. ) ;
#46567 = ORIENTED_EDGE ( 'NONE', *, *, #55124, .F. ) ;
#46568 = CARTESIAN_POINT ( 'NONE',  ( 182.4202572930267934, -31.94127993907054019, 193.9678068554150059 ) ) ;
#46569 = CARTESIAN_POINT ( 'NONE',  ( 112.2422220273998477, -28.08754728269216372, 201.0787261630399598 ) ) ;
#46570 = DIRECTION ( 'NONE',  ( -1.000000000000000000, -1.000000000000000078E-15, -1.000000000000000078E-15 ) ) ;
#46571 = CIRCLE ( 'NONE', #61053, 12.44600000000001216 ) ;
#46572 = DIRECTION ( 'NONE',  ( 0.000000000000000000, 1.000000000000000000, 0.000000000000000000 ) ) ;
#46573 = FACE_OUTER_BOUND ( 'NONE', #27914, .T. ) ;
#46574 = VERTEX_POINT ( 'NONE', #75708 ) ;
#46575 = EDGE_LOOP ( 'NONE', ( #15922, #45924, #52769, #60634 ) ) ;
#46576 = VECTOR ( 'NONE', #44915, 1000.000000000000000 ) ;
#46577 = ORIENTED_EDGE ( 'NONE', *, *, #75449, .T. ) ;
#46578 = VERTEX_POINT ( 'NONE', #25751 ) ;
#46579 = EDGE_CURVE ( 'NONE', #34067, #60619, #20303, .T. ) ;
#46580 = CARTESIAN_POINT ( 'NONE',  ( 98.93571844094823575, -36.00806725600566693, 229.0738046553059633 ) ) ;
#46581 = CARTESIAN_POINT ( 'NONE',  ( 113.8708677755033847, -44.65703921284106315, 108.1413395616249744 ) ) ;
#46582 = EDGE_CURVE ( 'NONE', #25046, #39094, #26648, .T. ) ;
#46583 = CARTESIAN_POINT ( 'NONE',  ( 100.3128846869252726, -46.43702735306955276, 87.09276813305393716 ) ) ;
#46584 = CARTESIAN_POINT ( 'NONE',  ( 100.4600951037162559, -41.26014358730922282, 249.5838068554172082 ) ) ;
#46585 = PRODUCT_DEFINITION_SHAPE ( 'NONE', 'NONE',  #68346 ) ;
#46586 = CARTESIAN_POINT ( 'NONE',  ( 117.7221270036566807, -41.68118999199129604, 4.925625275910981316 ) ) ;
#46587 = LINE ( 'NONE', #83713, #50374 ) ;
#46588 = CARTESIAN_POINT ( 'NONE',  ( 114.9778481211559154, -29.01036126763497336, 190.4537205140059655 ) ) ;
#46589 = CARTESIAN_POINT ( 'NONE',  ( 103.6782606442165360, -46.19611297174933640, 277.3022125101787765 ) ) ;
#46590 = ORIENTED_EDGE ( 'NONE', *, *, #26557, .F. ) ;
#46591 = DIRECTION ( 'NONE',  ( 3.999999999999999995E-14, -1.000000000000000000, 4.100000000000000342E-29 ) ) ;
#46592 = ORIENTED_EDGE ( 'NONE', *, *, #53863, .F. ) ;
#46593 = AXIS2_PLACEMENT_3D ( 'NONE', #56042, #76060, #13839 ) ;
#46594 = EDGE_CURVE ( 'NONE', #88352, #72160, #18946, .T. ) ;
#46595 = ORIENTED_EDGE ( 'NONE', *, *, #51843, .F. ) ;
#46596 = CARTESIAN_POINT ( 'NONE',  ( 59.56670390244699576, -67.87844715994098976, 155.2178068554179902 ) ) ;
#46597 = ORIENTED_EDGE ( 'NONE', *, *, #16500, .F. ) ;
#46598 = CIRCLE ( 'NONE', #32086, 3.499999999999996003 ) ;
#46599 = CYLINDRICAL_SURFACE ( 'NONE', #12749, 12.70000000000000107 ) ;
#46600 = EDGE_CURVE ( 'NONE', #50719, #87253, #33464, .T. ) ;
#46601 = CARTESIAN_POINT ( 'NONE',  ( 83.56670390244703128, -104.2784471599409670, 24.21780685541800082 ) ) ;
#46602 = CARTESIAN_POINT ( 'NONE',  ( 98.14942788562998999, -43.26130833009477783, 106.8175300378159704 ) ) ;
#46603 = CARTESIAN_POINT ( 'NONE',  ( -72.96458098368600531, 127.0000000000000000, -80.10833098368780725 ) ) ;
#46604 = CARTESIAN_POINT ( 'NONE',  ( 168.0371591254543375, -48.62818131005519717, 300.4678068554149490 ) ) ;
#46605 = CARTESIAN_POINT ( 'NONE',  ( 181.8884939055948280, -32.11662333283959470, 193.9678068554150059 ) ) ;
#46608 = CARTESIAN_POINT ( 'NONE',  ( 96.07698540226633099, -35.78353028925530310, 182.2461014663869889 ) ) ;
#46607 = CARTESIAN_POINT ( 'NONE',  ( 170.2205283966864897, 20.32000000000000028, -79.24800000000000466 ) ) ;
#46606 = LINE ( 'NONE', #5752, #65043 ) ;
#46609 = CARTESIAN_POINT ( 'NONE',  ( 89.06648329127401098, -14.47844715994100007, 17.92562527591199739 ) ) ;
#46611 = ADVANCED_FACE ( 'NONE', ( #76141 ), #34354, .F. ) ;
#46610 = LINE ( 'NONE', #33447, #56929 ) ;
#46612 = ORIENTED_EDGE ( 'NONE', *, *, #61993, .F. ) ;
#46613 = AXIS2_PLACEMENT_3D ( 'NONE', #83836, #21611, #15692 ) ;
#46614 = CARTESIAN_POINT ( 'NONE',  ( 91.91125933621933086, -96.68314769832107913, -11.78219314458223188 ) ) ;
#46615 = CARTESIAN_POINT ( 'NONE',  ( 138.8167039024479834, -67.87844715994100397, 60.91780685541480267 ) ) ;
#46616 = CYLINDRICAL_SURFACE ( 'NONE', #67649, 0.9999999999999800160 ) ;
#46617 = VECTOR ( 'NONE', #89323, 1000.000000000000000 ) ;
#46618 = CARTESIAN_POINT ( 'NONE',  ( 80.06648329127399677, 0.2215528400590013880, 293.6356252759119911 ) ) ;
#46620 = ORIENTED_EDGE ( 'NONE', *, *, #68942, .T. ) ;
#46619 = CARTESIAN_POINT ( 'NONE',  ( 98.86425576617398292, -29.25038657358478744, 230.7261014663869503 ) ) ;
#46621 = DIRECTION ( 'NONE',  ( 1.000000000000000000, 8.673617379883546378E-16, 9.757819552368989676E-16 ) ) ;
#46622 = CARTESIAN_POINT ( 'NONE',  ( 111.8740745592753427, -46.04428811464656945, 268.9556252759110180 ) ) ;
#46623 = CARTESIAN_POINT ( 'NONE',  ( 98.42274642353920910, -30.82362014679692308, 116.8499109901969604 ) ) ;
#46624 = CARTESIAN_POINT ( 'NONE',  ( 70.63919639214310564, 93.07500000000001705, 56.85413200336923012 ) ) ;
#46625 = CARTESIAN_POINT ( 'NONE',  ( 82.81648064515525220, -36.72944715939136273, 6.749772901088423538 ) ) ;
#46627 = DIRECTION ( 'NONE',  ( -1.000000000000000000, -8.538276166416950255E-16, -4.531343884107452465E-30 ) ) ;
#46626 = CARTESIAN_POINT ( 'NONE',  ( 173.9900000000000091, 68.61249999999999716, -53.61543552338530105 ) ) ;
#46628 = CARTESIAN_POINT ( 'NONE',  ( 193.0371591254585155, -47.82818131005411999, 180.4678068554150343 ) ) ;
#46629 = CARTESIAN_POINT ( 'NONE',  ( 73.06648329127396835, -8.729447159941065237, 14.67562527591093513 ) ) ;
#46630 = ORIENTED_EDGE ( 'NONE', *, *, #88097, .T. ) ;
#46631 = EDGE_LOOP ( 'NONE', ( #87401, #57101, #60306, #12829, #35742, #54084 ) ) ;
#46632 = ORIENTED_EDGE ( 'NONE', *, *, #24977, .T. ) ;
#46633 = CIRCLE ( 'NONE', #69876, 4.500000000000003553 ) ;
#46634 = ORIENTED_EDGE ( 'NONE', *, *, #80806, .T. ) ;
#46635 = CARTESIAN_POINT ( 'NONE',  ( 107.0664832912739541, -23.72944715994095688, 312.6356252759112522 ) ) ;
#46636 = CARTESIAN_POINT ( 'NONE',  ( 96.73636544059199593, -37.96124694896865748, 37.42133956162496844 ) ) ;
#46637 = PLANE ( 'NONE',  #18618 ) ;
#46638 = DIRECTION ( 'NONE',  ( 0.000000000000000000, 0.000000000000000000, -1.000000000000000000 ) ) ;
#46639 = CARTESIAN_POINT ( 'NONE',  ( 145.3524573197677228, -139.2182000785689411, 246.3670265245609983 ) ) ;
#46641 = DIRECTION ( 'NONE',  ( 0.000000000000000000, 1.000000000000000000, 0.000000000000000000 ) ) ;
#46640 = DIRECTION ( 'NONE',  ( 1.000000000000000000, 0.000000000000000000, 0.000000000000000000 ) ) ;
#46642 = AXIS2_PLACEMENT_3D ( 'NONE', #15033, #77710, #30008 ) ;
#46643 = EDGE_CURVE ( 'NONE', #54446, #87703, #33910, .T. ) ;
#46644 = CARTESIAN_POINT ( 'NONE',  ( 98.63544605819593869, -40.03554478408833006, 246.0343245899819919 ) ) ;
#46645 = ORIENTED_EDGE ( 'NONE', *, *, #64316, .F. ) ;
#46646 = ORIENTED_EDGE ( 'NONE', *, *, #85627, .F. ) ;
#46647 = ORIENTED_EDGE ( 'NONE', *, *, #29909, .F. ) ;
#46648 = CIRCLE ( 'NONE', #74225, 9.999999999999994671 ) ;
#46649 = DIRECTION ( 'NONE',  ( 0.000000000000000000, 0.000000000000000000, -1.000000000000000000 ) ) ;
#46650 = PLANE ( 'NONE',  #49131 ) ;
#46651 = EDGE_CURVE ( 'NONE', #5243, #54294, #77214, .T. ) ;
#46652 = DIRECTION ( 'NONE',  ( 0.000000000000000000, 1.000000000000000000, 0.000000000000000000 ) ) ;
#46653 = CARTESIAN_POINT ( 'NONE',  ( 142.8832909413445122, -79.11588146349311046, 361.9756252759100335 ) ) ;
#46654 = CARTESIAN_POINT ( 'NONE',  ( 115.3146942856800337, -32.23016485065021897, 20.64348806780197521 ) ) ;
#46655 = CARTESIAN_POINT ( 'NONE',  ( 122.2221484686747317, -96.68314769832130651, -19.26696060647622843 ) ) ;
#46656 = CARTESIAN_POINT ( 'NONE',  ( 102.0657545461937161, -27.97126071411138781, 175.4899107057300967 ) ) ;
#46657 = CARTESIAN_POINT ( 'NONE',  ( 101.4562478665867928, -44.74122718545263666, 282.0899109901972110 ) ) ;
#46658 = DIRECTION ( 'NONE',  ( -3.100000000000000258E-29, 3.100000000000000044E-14, 1.000000000000000000 ) ) ;
#46660 = ORIENTED_EDGE ( 'NONE', *, *, #49148, .F. ) ;
#46659 = VECTOR ( 'NONE', #2455, 1000.000000000000000 ) ;
#46661 = CARTESIAN_POINT ( 'NONE',  ( 113.6361143365868429, -29.10761691970661857, 55.51073420584606311 ) ) ;
#46662 = CYLINDRICAL_SURFACE ( 'NONE', #14868, 2.517500000000005844 ) ;
#46663 = CARTESIAN_POINT ( 'NONE',  ( 109.7980830611816714, -44.45091405062262879, 35.66523322673398155 ) ) ;
#46664 = AXIS2_PLACEMENT_3D ( 'NONE', #20623, #73790, #21067 ) ;
#46666 = EDGE_CURVE ( 'NONE', #1484, #19859, #41605, .T. ) ;
#46665 = VECTOR ( 'NONE', #85391, 1000.000000000000000 ) ;
#46667 = CARTESIAN_POINT ( 'NONE',  ( 135.5773992616618671, -16.43204134599573507, 7.859568798194228378 ) ) ;
#46668 = CARTESIAN_POINT ( 'NONE',  ( 25.56670390244797275, -48.82844715994099971, 137.2178068554150059 ) ) ;
#46669 = VECTOR ( 'NONE', #64847, 1000.000000000000000 ) ;
#46670 = CARTESIAN_POINT ( 'NONE',  ( 19.56648329127400032, 15.62155284005900491, 323.8756252759109202 ) ) ;
#46671 = EDGE_LOOP ( 'NONE', ( #46508, #11430, #41127, #45537 ) ) ;
#46672 = DIRECTION ( 'NONE',  ( 0.000000000000000000, 0.000000000000000000, 1.000000000000000000 ) ) ;
#46673 = CARTESIAN_POINT ( 'NONE',  ( 152.0371591254583450, -47.82818131005588214, 249.9678068554149490 ) ) ;
#46674 = ORIENTED_EDGE ( 'NONE', *, *, #83021, .T. ) ;
#46675 = CARTESIAN_POINT ( 'NONE',  ( 104.9628152733504720, -25.06689740840304381, 125.2184824187689856 ) ) ;
#46676 = ORIENTED_EDGE ( 'NONE', *, *, #82413, .F. ) ;
#46678 = CIRCLE ( 'NONE', #64153, 30.99999999999998579 ) ;
#46677 = CARTESIAN_POINT ( 'NONE',  ( 113.7853715510712789, -42.80144937323932908, 82.67622935188595079 ) ) ;
#46679 = PLANE ( 'NONE',  #47457 ) ;
#46680 = CARTESIAN_POINT ( 'NONE',  ( 98.97073112826979013, -33.12568863208839076, 97.42444044875497866 ) ) ;
#46681 = AXIS2_PLACEMENT_3D ( 'NONE', #10285, #22591, #71633 ) ;
#46682 = DIRECTION ( 'NONE',  ( 1.000000000000000078E-15, -1.000000000000000000, 0.000000000000000000 ) ) ;
#46683 = FACE_OUTER_BOUND ( 'NONE', #41008, .T. ) ;
#46684 = CARTESIAN_POINT ( 'NONE',  ( 100.9304087016431453, -28.27451679452656919, 71.57562527591099411 ) ) ;
#46685 = LINE ( 'NONE', #70171, #41041 ) ;
#46686 = CARTESIAN_POINT ( 'NONE',  ( 105.7153411597131765, -46.72383786517413284, 257.4688385543852291 ) ) ;
#46687 = EDGE_LOOP ( 'NONE', ( #52347, #6842, #29320, #70499 ) ) ;
#46688 = CARTESIAN_POINT ( 'NONE',  ( -118.4576332894986166, 70.80054595721396993, 4.873637472995685727 ) ) ;
#46689 = ORIENTED_EDGE ( 'NONE', *, *, #55239, .T. ) ;
#46690 = EDGE_LOOP ( 'NONE', ( #29051, #38937, #80690, #9912, #55844, #33924, #47490, #36635, #4562, #28742, #84390, #88096 ) ) ;
#46691 = EDGE_CURVE ( 'NONE', #71543, #84928, #81196, .T. ) ;
#46692 = LINE ( 'NONE', #12197, #55685 ) ;
#46693 = ORIENTED_EDGE ( 'NONE', *, *, #34285, .T. ) ;
#46694 = CARTESIAN_POINT ( 'NONE',  ( 103.3362402991319442, -47.20309360805218546, 252.3041967044827913 ) ) ;
#46695 = DIRECTION ( 'NONE',  ( 0.000000000000000000, 0.000000000000000000, 1.000000000000000000 ) ) ;
#46696 = FACE_OUTER_BOUND ( 'NONE', #49515, .T. ) ;
#46697 = ADVANCED_FACE ( 'NONE', ( #60262 ), #67992, .T. ) ;
#46698 = CARTESIAN_POINT ( 'NONE',  ( 101.1417250294410337, -28.10862513908322313, 46.55562527591094835 ) ) ;
#46699 = CARTESIAN_POINT ( 'NONE',  ( 105.8025202575843764, -26.72362734506296889, 96.17630429063157749 ) ) ;
#46700 = EDGE_LOOP ( 'NONE', ( #69833, #20570, #78429, #22563 ) ) ;
#46701 = CARTESIAN_POINT ( 'NONE',  ( 116.3225472244029817, -32.94146556017791738, 114.1356252759109822 ) ) ;
#46702 = EDGE_CURVE ( 'NONE', #32451, #40665, #88447, .T. ) ;
#46703 = DIRECTION ( 'NONE',  ( -4.237773401492740281E-14, 1.000000000000000000, 0.000000000000000000 ) ) ;
#46704 = VECTOR ( 'NONE', #27203, 1000.000000000000000 ) ;
#46705 = ORIENTED_EDGE ( 'NONE', *, *, #63956, .T. ) ;
#46706 = CIRCLE ( 'NONE', #27921, 12.69999999999998863 ) ;
#46707 = CARTESIAN_POINT ( 'NONE',  ( -178.3658777604659917, 0.000000000000000000, 122.9960808104842016 ) ) ;
#46708 = CYLINDRICAL_SURFACE ( 'NONE', #57109, 3.500000000000003109 ) ;
#46709 = CARTESIAN_POINT ( 'NONE',  ( 96.27200394136420414, -34.46162041542910970, 261.1737205140064475 ) ) ;
#46710 = DIRECTION ( 'NONE',  ( 0.000000000000000000, 0.000000000000000000, 1.000000000000000000 ) ) ;
#46711 = DIRECTION ( 'NONE',  ( 0.000000000000000000, 1.000000000000000000, 0.000000000000000000 ) ) ;
#46712 = DIRECTION ( 'NONE',  ( 1.000000000000000000, 0.000000000000000000, 1.047445008332813989E-14 ) ) ;
#46713 = CARTESIAN_POINT ( 'NONE',  ( 113.6113952709150396, -31.24125447920927101, 268.8038483995053411 ) ) ;
#46715 = CARTESIAN_POINT ( 'NONE',  ( 117.3497117099303892, -32.73958051198275854, 90.10895860924395606 ) ) ;
#46714 = CARTESIAN_POINT ( 'NONE',  ( 97.57298764950955672, -39.87469497683259334, 101.5815513261982943 ) ) ;
#46716 = CARTESIAN_POINT ( 'NONE',  ( 41.56648329127499153, -36.32844715994070839, 198.9256252759119832 ) ) ;
#46717 = CARTESIAN_POINT ( 'NONE',  ( 114.4941961175866254, -28.48069933791915531, 159.5051490854349652 ) ) ;
#46718 = EDGE_LOOP ( 'NONE', ( #43841, #69279, #12330, #70194 ) ) ;
#46720 = EDGE_CURVE ( 'NONE', #3377, #31900, #18914, .T. ) ;
#46719 = CARTESIAN_POINT ( 'NONE',  ( 123.6837132603318992, -20.11243780205710507, 239.5838068554165545 ) ) ;
#46721 = EDGE_LOOP ( 'NONE', ( #88206, #75069, #40202, #51385, #9499, #6598, #55470, #64052, #50138, #79328, #78804, #70692 ) ) ;
#46722 = FACE_BOUND ( 'NONE', #64041, .T. ) ;
#46723 = CARTESIAN_POINT ( 'NONE',  ( 123.6837132603318992, -16.81243780205710436, 239.5838068554165545 ) ) ;
#46724 = EDGE_CURVE ( 'NONE', #1745, #701, #52323, .T. ) ;
#46725 = CARTESIAN_POINT ( 'NONE',  ( 134.9467300988904128, -34.12360705087674972, 1.744847597651338678 ) ) ;
#46726 = ORIENTED_EDGE ( 'NONE', *, *, #17189, .T. ) ;
#46727 = AXIS2_PLACEMENT_3D ( 'NONE', #17541, #79783, #57967 ) ;
#46728 = CARTESIAN_POINT ( 'NONE',  ( 98.58946256649487339, -99.96145986183361742, 2.217806855417864043 ) ) ;
#46730 = ORIENTED_EDGE ( 'NONE', *, *, #54099, .F. ) ;
#46729 = CARTESIAN_POINT ( 'NONE',  ( 108.2829496674670224, -47.76277978039057359, 157.6518157521019532 ) ) ;
#46731 = DIRECTION ( 'NONE',  ( -1.000000000000000000, -4.554376769437570034E-14, 0.000000000000000000 ) ) ;
#46732 = CARTESIAN_POINT ( 'NONE',  ( -129.9468070739258110, 84.21348395916261609, -12.59754631664223723 ) ) ;
#46733 = CARTESIAN_POINT ( 'NONE',  ( 173.9900000000000091, 5.112500000000000711, -58.73749999999999716 ) ) ;
#46734 = FACE_OUTER_BOUND ( 'NONE', #65424, .T. ) ;
#46735 = VERTEX_POINT ( 'NONE', #19394 ) ;
#46736 = VECTOR ( 'NONE', #76217, 1000.000000000000000 ) ;
#46737 = FACE_OUTER_BOUND ( 'NONE', #15166, .T. ) ;
#46738 = CARTESIAN_POINT ( 'NONE',  ( 0.000000000000000000, 239.0000000000000000, 154.6557476874258441 ) ) ;
#46739 = VERTEX_POINT ( 'NONE', #21652 ) ;
#46740 = AXIS2_PLACEMENT_3D ( 'NONE', #36140, #1178, #84315 ) ;
#46741 = VERTEX_POINT ( 'NONE', #7115 ) ;
#46742 = DIRECTION ( 'NONE',  ( 0.8660254037844380415, 0.5000000000000012212, -1.550000000000001284E-14 ) ) ;
#46743 = CARTESIAN_POINT ( 'NONE',  ( 99.62873342662678056, 89.26666702275855414, -84.37439091330300300 ) ) ;
#46744 = CARTESIAN_POINT ( 'NONE',  ( 118.5256205435843526, -36.72944715994100306, 293.2242906452868851 ) ) ;
#46745 = DIRECTION ( 'NONE',  ( 0.4999999999999989453, 0.8660254037844392627, -2.684678751731760294E-14 ) ) ;
#46747 = CARTESIAN_POINT ( 'NONE',  ( -12.70000000000000107, 82.54999999999999716, -117.8738102209307641 ) ) ;
#46746 = DIRECTION ( 'NONE',  ( -0.7071067811865483499, -0.7071067811865466846, -7.071067811865491110E-16 ) ) ;
#46748 = DIRECTION ( 'NONE',  ( 0.3818493186865919986, -0.9242245927363031965, 0.000000000000000000 ) ) ;
#46749 = VERTEX_POINT ( 'NONE', #29355 ) ;
#46750 =( BOUNDED_CURVE ( )  B_SPLINE_CURVE ( 3, ( #2572, #51141, #85697, #71614 ),
 .UNSPECIFIED., .F., .F. ) 
 B_SPLINE_CURVE_WITH_KNOTS ( ( 4, 4 ),
 ( 2.669330456947324848, 2.679444341124444851 ),
 .UNSPECIFIED. ) 
 CURVE ( )  GEOMETRIC_REPRESENTATION_ITEM ( )  RATIONAL_B_SPLINE_CURVE ( ( 1.000000000000000000, 0.9999914757970698176, 0.9999914757970698176, 1.000000000000000000 ) ) 
 REPRESENTATION_ITEM ( '' )  );
#46751 = CARTESIAN_POINT ( 'NONE',  ( 134.0664832912739826, -18.72944715994100306, 14.92562527591099908 ) ) ;
#46752 = EDGE_CURVE ( 'NONE', #70284, #63079, #34806, .T. ) ;
#46753 = CARTESIAN_POINT ( 'NONE',  ( 99.07755742602716964, -44.46178485432842109, 187.9384824187679612 ) ) ;
#46755 = ORIENTED_EDGE ( 'NONE', *, *, #23777, .F. ) ;
#46754 = LINE ( 'NONE', #19070, #37070 ) ;
#46756 = CARTESIAN_POINT ( 'NONE',  ( 97.35459460924926134, -38.14118110200429612, 62.44133956162495025 ) ) ;
#46757 = FACE_OUTER_BOUND ( 'NONE', #2383, .T. ) ;
#46758 = PLANE ( 'NONE',  #34047 ) ;
#46759 = LINE ( 'NONE', #45417, #47453 ) ;
#46760 = EDGE_LOOP ( 'NONE', ( #54955, #19950, #14158, #48686 ) ) ;
#46761 = CARTESIAN_POINT ( 'NONE',  ( -71.77848634863190114, 120.6499999999999915, 77.39114642429879609 ) ) ;
#46762 = EDGE_LOOP ( 'NONE', ( #51240, #50509, #66197 ) ) ;
#46763 = VERTEX_POINT ( 'NONE', #57033 ) ;
#46764 = CARTESIAN_POINT ( 'NONE',  ( 101.6018043438793796, -28.26729678577900273, 216.9644404487539475 ) ) ;
#46765 = VECTOR ( 'NONE', #81366, 1000.000000000000000 ) ;
#46766 = CARTESIAN_POINT ( 'NONE',  ( 97.92313387223457255, -40.78048155489533144, 52.65794466837188992 ) ) ;
#46767 = EDGE_CURVE ( 'NONE', #31965, #81124, #16173, .T. ) ;
#46768 = CARTESIAN_POINT ( 'NONE',  ( -84.91247172076023730, 90.28418055714726620, 99.17062120112684909 ) ) ;
#46769 = CARTESIAN_POINT ( 'NONE',  ( 115.0372574776238110, -42.90846260514542365, 154.3022919387951220 ) ) ;
#46770 = CARTESIAN_POINT ( 'NONE',  ( 82.68803181460157248, -37.56139158947667056, 2.921136715972031617 ) ) ;
#46771 = ORIENTED_EDGE ( 'NONE', *, *, #72453, .F. ) ;
#46772 = LINE ( 'NONE', #39530, #23294 ) ;
#46773 = DIRECTION ( 'NONE',  ( 0.000000000000000000, 0.000000000000000000, -1.000000000000000000 ) ) ;
#46774 = ORIENTED_EDGE ( 'NONE', *, *, #50957, .F. ) ;
#46775 = CARTESIAN_POINT ( 'NONE',  ( 97.48652011608379553, -32.61680585812226241, 16.00419670448194154 ) ) ;
#46776 = ORIENTED_EDGE ( 'NONE', *, *, #30740, .T. ) ;
#46777 = EDGE_LOOP ( 'NONE', ( #75054, #62308 ) ) ;
#46778 = CARTESIAN_POINT ( 'NONE',  ( 106.4091095994060652, -45.35897697767001091, 265.3461856076867207 ) ) ;
#46779 = VECTOR ( 'NONE', #41984, 1000.000000000000000 ) ;
#46780 = EDGE_CURVE ( 'NONE', #37337, #47465, #75291, .T. ) ;
#46781 = FACE_BOUND ( 'NONE', #45847, .T. ) ;
#46782 = CARTESIAN_POINT ( 'NONE',  ( 99.59366209610195142, -44.96145431533982162, 156.9899109901969609 ) ) ;
#46783 = LINE ( 'NONE', #12294, #9889 ) ;
#46784 = DIRECTION ( 'NONE',  ( 0.000000000000000000, 1.000000000000000000, 0.000000000000000000 ) ) ;
#46785 = DIRECTION ( 'NONE',  ( -0.8660254037844379305, -0.5000000000000012212, 1.550000000000001284E-14 ) ) ;
#46786 = CARTESIAN_POINT ( 'NONE',  ( 115.9970180223098311, -30.13831313182449989, 255.3203871806730660 ) ) ;
#46787 = CARTESIAN_POINT ( 'NONE',  ( 89.13001032377211175, 92.64969027323468254, -78.17826422383492968 ) ) ;
#46788 = EDGE_LOOP ( 'NONE', ( #63588, #66112 ) ) ;
#46789 = AXIS2_PLACEMENT_3D ( 'NONE', #66041, #3830, #31523 ) ;
#46790 = CARTESIAN_POINT ( 'NONE',  ( 97.22547384517952196, -31.59602418489684084, 86.93181575210095957 ) ) ;
#46791 = DIRECTION ( 'NONE',  ( 1.000000000000000000, -1.000000000000000078E-15, 0.000000000000000000 ) ) ;
#46792 = EDGE_CURVE ( 'NONE', #33670, #26732, #10283, .T. ) ;
#46793 = EDGE_LOOP ( 'NONE', ( #70121, #15419, #34927, #20320 ) ) ;
#46794 = VERTEX_POINT ( 'NONE', #49323 ) ;
#46795 = ORIENTED_EDGE ( 'NONE', *, *, #13956, .F. ) ;
#46796 = DIRECTION ( 'NONE',  ( -0.7071067811865462405, 0.000000000000000000, 0.7071067811865486830 ) ) ;
#46797 = CARTESIAN_POINT ( 'NONE',  ( 41.56648329127499153, -32.07844715994070839, 78.92562527591199739 ) ) ;
#46798 = CARTESIAN_POINT ( 'NONE',  ( 162.0667039024470171, -77.67844715994088745, 55.21780685541800437 ) ) ;
#46799 = EDGE_CURVE ( 'NONE', #79245, #87954, #28439, .T. ) ;
#46800 = CARTESIAN_POINT ( 'NONE',  ( 103.3443811052163568, -28.91619688769685936, 138.2604713219729717 ) ) ;
#46801 = CARTESIAN_POINT ( 'NONE',  ( 111.1359251431956210, -27.10775802199072970, 240.7584824187679544 ) ) ;
#46802 = DIRECTION ( 'NONE',  ( -1.000000000000000078E-15, 1.000000000000000000, 0.000000000000000000 ) ) ;
#46803 = ORIENTED_EDGE ( 'NONE', *, *, #46994, .T. ) ;
#46804 = CARTESIAN_POINT ( 'NONE',  ( 130.5560151749589295, 95.25015599858943460, 0.4097429349709048596 ) ) ;
#46805 = DIRECTION ( 'NONE',  ( 0.000000000000000000, 1.000000000000000000, 0.000000000000000000 ) ) ;
#46806 = ORIENTED_EDGE ( 'NONE', *, *, #38123, .T. ) ;
#46807 = EDGE_LOOP ( 'NONE', ( #49826, #946, #44135, #29452 ) ) ;
#46808 = FACE_OUTER_BOUND ( 'NONE', #85580, .T. ) ;
#46809 = ORIENTED_EDGE ( 'NONE', *, *, #41372, .F. ) ;
#46810 = ORIENTED_EDGE ( 'NONE', *, *, #55977, .F. ) ;
#46811 = CARTESIAN_POINT ( 'NONE',  ( 107.0664832912739399, -36.72944715994095333, 289.6356252759107406 ) ) ;
#46812 = DIRECTION ( 'NONE',  ( 0.000000000000000000, 0.000000000000000000, 1.000000000000000000 ) ) ;
#46813 = LINE ( 'NONE', #86843, #75088 ) ;
#46814 = CARTESIAN_POINT ( 'NONE',  ( 99.46962827726154899, -41.65933777599243371, 146.2190864947439763 ) ) ;
#46815 = CARTESIAN_POINT ( 'NONE',  ( 117.4985906579250354, -37.96351766657803495, 53.73276813305394484 ) ) ;
#46817 = EDGE_CURVE ( 'NONE', #7174, #64426, #8921, .T. ) ;
#46816 = CARTESIAN_POINT ( 'NONE',  ( 68.77555146766027860, -139.1540193827811152, 247.4783998280180128 ) ) ;
#46818 = VERTEX_POINT ( 'NONE', #62957 ) ;
#46819 = VECTOR ( 'NONE', #67888, 1000.000000000000000 ) ;
#46820 = EDGE_CURVE ( 'NONE', #15124, #51994, #84333, .T. ) ;
#46821 = LINE ( 'NONE', #73651, #15115 ) ;
#46822 = ORIENTED_EDGE ( 'NONE', *, *, #15090, .T. ) ;
#46823 = EDGE_CURVE ( 'NONE', #26639, #13679, #48864, .T. ) ;
#46824 = DIRECTION ( 'NONE',  ( 0.000000000000000000, 0.000000000000000000, -1.000000000000000000 ) ) ;
#46825 = EDGE_LOOP ( 'NONE', ( #136, #12702, #18990, #47053 ) ) ;
#46826 = PLANE ( 'NONE',  #40723 ) ;
#46827 = EDGE_CURVE ( 'NONE', #88034, #9965, #77054, .T. ) ;
#46828 = CARTESIAN_POINT ( 'NONE',  ( 128.9945611041196685, -130.4030827564308197, 249.3173333679100097 ) ) ;
#46829 = DIRECTION ( 'NONE',  ( 0.000000000000000000, 0.000000000000000000, 1.000000000000000000 ) ) ;
#46830 = VECTOR ( 'NONE', #85501, 1000.000000000000000 ) ;
#46831 = CARTESIAN_POINT ( 'NONE',  ( -7.661254700127833495, 82.54999999999999716, 320.6630000000000109 ) ) ;
#46832 = ORIENTED_EDGE ( 'NONE', *, *, #48267, .F. ) ;
#46833 = CARTESIAN_POINT ( 'NONE',  ( 99.12668881670464316, -43.51958910750428089, 31.88991099019594699 ) ) ;
#46834 = CARTESIAN_POINT ( 'NONE',  ( 97.77052560236188583, -29.30002703792375485, 41.78991099019596334 ) ) ;
#46835 = PRESENTATION_STYLE_ASSIGNMENT (( #45933 ) ) ;
#46837 = CARTESIAN_POINT ( 'NONE',  ( -72.96458098368600531, 117.4749999999999943, -67.92268098368781182 ) ) ;
#46836 = CARTESIAN_POINT ( 'NONE',  ( -7.205548786489490269E-13, 127.0000000000000000, 108.2293999999999983 ) ) ;
#46838 = CARTESIAN_POINT ( 'NONE',  ( 109.7248794765007602, -27.00080882144429140, 145.8651687245758808 ) ) ;
#46839 = DIRECTION ( 'NONE',  ( 1.000000000000000000, 0.000000000000000000, 0.000000000000000000 ) ) ;
#46840 = DIRECTION ( 'NONE',  ( 0.000000000000000000, 1.000000000000000000, 1.914177628664063178E-15 ) ) ;
#46841 = LINE ( 'NONE', #45941, #70470 ) ;
#46842 = ORIENTED_EDGE ( 'NONE', *, *, #89398, .F. ) ;
#46843 = CARTESIAN_POINT ( 'NONE',  ( 118.1222316836501705, -37.72106760768119216, 33.74324432352998571 ) ) ;
#46844 = CARTESIAN_POINT ( 'NONE',  ( 117.9485099285917613, -34.79154191225799053, 194.9546728949589749 ) ) ;
#46845 = CARTESIAN_POINT ( 'NONE',  ( 106.8407189164991706, -48.60257990303799858, 73.56133956162497611 ) ) ;
#46847 = CARTESIAN_POINT ( 'NONE',  ( 126.8164832912740110, -46.47944715994101017, 14.92562527591099020 ) ) ;
#46846 = CARTESIAN_POINT ( 'NONE',  ( 98.54792498091607911, -41.97742571765204644, 171.7652816990279234 ) ) ;
#46848 = CARTESIAN_POINT ( 'NONE',  ( 7.661254700127822836, 98.64746158385918307, 275.4630000000000223 ) ) ;
#46849 = VECTOR ( 'NONE', #49408, 1000.000000000000000 ) ;
#46850 = AXIS2_PLACEMENT_3D ( 'NONE', #65927, #18683, #24608 ) ;
#46851 = PLANE ( 'NONE',  #63623 ) ;
#46852 = ORIENTED_EDGE ( 'NONE', *, *, #23860, .F. ) ;
#46853 = EDGE_CURVE ( 'NONE', #24378, #81580, #42952, .T. ) ;
#46854 = CARTESIAN_POINT ( 'NONE',  ( 116.0091996907507195, -30.12340400999218559, 105.3327681330529515 ) ) ;
#46856 = ORIENTED_EDGE ( 'NONE', *, *, #14554, .T. ) ;
#46855 = DIRECTION ( 'NONE',  ( 0.000000000000000000, 6.982966722218760189E-15, -1.000000000000000000 ) ) ;
#46857 = CARTESIAN_POINT ( 'NONE',  ( 96.79426660377265534, -34.87310936442968057, 237.1841967044819626 ) ) ;
#46858 = CARTESIAN_POINT ( 'NONE',  ( 112.0651709148995678, -45.48882515156851269, 253.9919150860570198 ) ) ;
#46859 = DIRECTION ( 'NONE',  ( 0.7349399772593249169, 0.6687953793059874252, 0.1121426343770439288 ) ) ;
#46860 = DIRECTION ( 'NONE',  ( 1.000000000000000000, 6.831565154159360295E-14, 0.000000000000000000 ) ) ;
#46861 = CARTESIAN_POINT ( 'NONE',  ( 109.7248659154506640, -27.00080517803650437, 45.86479194305611884 ) ) ;
#46862 = CARTESIAN_POINT ( 'NONE',  ( 131.9645448811542678, -38.51222316632535581, 2.376608873922943843 ) ) ;
#46863 = FACE_BOUND ( 'NONE', #84169, .T. ) ;
#46864 = CARTESIAN_POINT ( 'NONE',  ( 107.9488082096507213, -26.98745991040259895, 155.0041967044829505 ) ) ;
#46865 = ORIENTED_EDGE ( 'NONE', *, *, #52378, .T. ) ;
#46866 = ORIENTED_EDGE ( 'NONE', *, *, #74131, .F. ) ;
#46867 = CARTESIAN_POINT ( 'NONE',  ( 108.4917517584632236, -27.44263408611272936, 141.3749166392299514 ) ) ;
#46868 = CARTESIAN_POINT ( 'NONE',  ( 142.8696205427243626, 0.6543191929522240713, 540.9756252759101471 ) ) ;
#46869 = EDGE_CURVE ( 'NONE', #15433, #16125, #293, .T. ) ;
#46871 = FACE_OUTER_BOUND ( 'NONE', #32994, .T. ) ;
#46870 = CARTESIAN_POINT ( 'NONE',  ( 116.0161715043949471, -40.67488961668902192, 249.4956252759109532 ) ) ;
#46872 = AXIS2_PLACEMENT_3D ( 'NONE', #57711, #64979, #52206 ) ;
#46873 = LINE ( 'NONE', #26018, #62359 ) ;
#46874 = ADVANCED_FACE ( 'NONE', ( #28906 ), #2090, .F. ) ;
#46875 = CARTESIAN_POINT ( 'NONE',  ( 255.9983484187079910, 65.43750000000000000, -2.032000000000000028 ) ) ;
#46876 = EDGE_CURVE ( 'NONE', #65403, #27030, #77495, .T. ) ;
#46877 = DIRECTION ( 'NONE',  ( 0.000000000000000000, 0.000000000000000000, -1.000000000000000000 ) ) ;
#46878 = AXIS2_PLACEMENT_3D ( 'NONE', #88689, #32344, #87335 ) ;
#46879 = CARTESIAN_POINT ( 'NONE',  ( 162.8913605087219878, -31.76306994223740432, 342.9256252759109884 ) ) ;
#46880 = CARTESIAN_POINT ( 'NONE',  ( 21.03689327557619748, -23.42844715994197813, 129.9678068554150627 ) ) ;
#46881 = CARTESIAN_POINT ( 'NONE',  ( 101.2129617469312564, -45.32973500739964834, 197.1013395616249966 ) ) ;
#46882 = CARTESIAN_POINT ( 'NONE',  ( 107.0664832912739399, -36.72944715994095333, 302.7856252759109452 ) ) ;
#46883 = ORIENTED_EDGE ( 'NONE', *, *, #49820, .F. ) ;
#46884 = ORIENTED_EDGE ( 'NONE', *, *, #77664, .T. ) ;
#46885 = ADVANCED_FACE ( 'NONE', ( #55665 ), #77954, .F. ) ;
#46886 = EDGE_CURVE ( 'NONE', #32183, #13040, #36159, .T. ) ;
#46887 = DIRECTION ( 'NONE',  ( 0.000000000000000000, -1.000000000000000000, 0.000000000000000000 ) ) ;
#46888 = CARTESIAN_POINT ( 'NONE',  ( 82.10313645208317723, -20.57950990142240144, 7.523361336364036589 ) ) ;
#46889 = CARTESIAN_POINT ( 'NONE',  ( 112.1401101529673667, -28.01326083308519088, 184.6568239736689350 ) ) ;
#46890 = DIRECTION ( 'NONE',  ( -1.000000000000000000, -3.999999999999999995E-14, -1.000000000000000078E-15 ) ) ;
#46891 = B_SPLINE_CURVE_WITH_KNOTS ( 'NONE', 3,
 ( #17903, #74664, #73313, #38793, #61026, #66499, #67850, #88755, #54185, #71541, #77903, #77447, #44696, #8872, #64271, #17013, #36569, #50623, #78365, #71981, #2045, #29752, #43806, #78807, #15681, #56990, #22492, #30194, #84283, #57890, #37898, #22056, #65598, #57437, #29307, #16563, #9750, #85178, #72424, #50167, #31070, #44245, #43354, #30636, #10191, #22949, #71098, #16126, #65152, #37452, #3379, #9305 ),
 .UNSPECIFIED., .F., .F.,
 ( 4, 2, 1, 1, 1, 1, 1, 1, 2, 2, 2, 2, 2, 2, 2, 2, 1, 1, 1, 1, 1, 1, 2, 2, 2, 2, 2, 2, 2, 2, 2, 4 ),
 ( 0.5000152423139874180, 0.5001779712831790903, 0.5003407002523706515, 0.5006661581907546621, 0.5013170740675219061, 0.5026189058210562832, 0.5052225693281247043, 0.5104298963422607693, 0.5208445503705330104, 0.5416738584270778256, 0.5833324745401682332, 0.6666497067663494924, 0.7499669389925306406, 0.8332841712187117889, 0.8333655357033079580, 0.8334469001879041272, 0.8335282646725001854, 0.8336909936415386468, 0.8340164515796154587, 0.8346673674557795186, 0.8359691992081024203, 0.8385728627127363444, 0.8437801897220043035, 0.8541948437405375572, 0.8750241517776036204, 0.8958534598146696837, 0.9166827678517357469, 0.9375120758888018102, 0.9583413839258678735, 0.9791706919629339367, 0.9895853459814669684, 1.000000000000000000 ),
 .UNSPECIFIED. ) ;
#46892 = EDGE_CURVE ( 'NONE', #20155, #18276, #8004, .T. ) ;
#46893 = AXIS2_PLACEMENT_3D ( 'NONE', #12193, #87162, #81698 ) ;
#46894 = DIRECTION ( 'NONE',  ( -7.136255983449500255E-16, 0.000000000000000000, -1.000000000000000000 ) ) ;
#46895 = ORIENTED_EDGE ( 'NONE', *, *, #29298, .T. ) ;
#46896 = CARTESIAN_POINT ( 'NONE',  ( 172.5664832912740110, -18.82844715994099971, 78.92562527591199739 ) ) ;
#46897 = EDGE_CURVE ( 'NONE', #50846, #21614, #1654, .T. ) ;
#46898 = CARTESIAN_POINT ( 'NONE',  ( 96.19116125691978425, -32.02117184027007113, 211.0013395616249738 ) ) ;
#46899 = CARTESIAN_POINT ( 'NONE',  ( 136.7895896102205597, -37.11755991741181759, 6.789748280180922357 ) ) ;
#46900 = ORIENTED_EDGE ( 'NONE', *, *, #27108, .F. ) ;
#46901 = CARTESIAN_POINT ( 'NONE',  ( 168.5667039024486087, -48.82844715993516616, 129.9678068554150059 ) ) ;
#46902 = EDGE_CURVE ( 'NONE', #61996, #48953, #86995, .T. ) ;
#46903 = DIRECTION ( 'NONE',  ( 0.000000000000000000, 0.000000000000000000, 1.000000000000000000 ) ) ;
#46904 = DIRECTION ( 'NONE',  ( -0.000000000000000000, 1.000000000000000000, -0.000000000000000000 ) ) ;
#46905 = EDGE_CURVE ( 'NONE', #5529, #59590, #72471, .T. ) ;
#46906 = CARTESIAN_POINT ( 'NONE',  ( 100.8503319422675020, -42.75110701849109063, 39.76904275054393878 ) ) ;
#46907 = CARTESIAN_POINT ( 'NONE',  ( 114.0955628336689500, -44.50577255156974843, 129.1613395616249704 ) ) ;
#46908 = CARTESIAN_POINT ( 'NONE',  ( -135.1318726873890341, 101.5999999999999943, 118.7423475625884066 ) ) ;
#46909 = ORIENTED_EDGE ( 'NONE', *, *, #21390, .F. ) ;
#46910 = CYLINDRICAL_SURFACE ( 'NONE', #68254, 9.999999999999998224 ) ;
#46911 = CARTESIAN_POINT ( 'NONE',  ( 63.03715912545732181, -24.89890238295017966, 300.4678068554150627 ) ) ;
#46912 = ORIENTED_EDGE ( 'NONE', *, *, #86638, .F. ) ;
#46913 = VERTEX_POINT ( 'NONE', #31561 ) ;
#46914 = VECTOR ( 'NONE', #22522, 1000.000000000000000 ) ;
#46915 = LINE ( 'NONE', #18332, #19812 ) ;
#46916 = ORIENTED_EDGE ( 'NONE', *, *, #72739, .F. ) ;
#46917 = ORIENTED_EDGE ( 'NONE', *, *, #59587, .T. ) ;
#46918 = CARTESIAN_POINT ( 'NONE',  ( 97.31589304778225369, -39.30609602821265725, 157.5312681354445488 ) ) ;
#46919 = AXIS2_PLACEMENT_3D ( 'NONE', #82281, #33659, #74544 ) ;
#46920 = CARTESIAN_POINT ( 'NONE',  ( 110.1208792074641991, -44.70608788829420632, 62.28956268521896078 ) ) ;
#46921 = CARTESIAN_POINT ( 'NONE',  ( 103.8128537583787363, -48.15082670742215498, 217.3556252759109668 ) ) ;
#46922 = CARTESIAN_POINT ( 'NONE',  ( 117.2701380961606645, -34.52720868313122082, 183.9956252759109532 ) ) ;
#46925 = ADVANCED_FACE ( 'NONE', ( #44739 ), #17058, .T. ) ;
#46924 = CARTESIAN_POINT ( 'NONE',  ( 110.9930042498355363, -46.38681234365495953, 278.8841967044824059 ) ) ;
#46923 = CARTESIAN_POINT ( 'NONE',  ( 115.9905926440153792, -41.41586665309425541, 23.44146406657679194 ) ) ;
#46926 = DIRECTION ( 'NONE',  ( 1.000000000000000000, 0.000000000000000000, 0.000000000000000000 ) ) ;
#46927 = CARTESIAN_POINT ( 'NONE',  ( 192.5667039024472444, -23.42844715993434335, 300.4678068554149490 ) ) ;
#46928 = ORIENTED_EDGE ( 'NONE', *, *, #347, .F. ) ;
#46929 = ADVANCED_FACE ( 'NONE', ( #45181 ), #71588, .T. ) ;
#46930 = ORIENTED_EDGE ( 'NONE', *, *, #80565, .T. ) ;
#46931 = EDGE_CURVE ( 'NONE', #79308, #46344, #52751, .T. ) ;
#46932 = CYLINDRICAL_SURFACE ( 'NONE', #51630, 0.2500000000000039968 ) ;
#46934 = CIRCLE ( 'NONE', #77446, 10.04999999999999361 ) ;
#46933 = CARTESIAN_POINT ( 'NONE',  ( 96.07878916947804271, -35.15354693665655361, 226.2251490854349640 ) ) ;
#46935 = VERTEX_POINT ( 'NONE', #86555 ) ;
#46936 = CARTESIAN_POINT ( 'NONE',  ( 96.04647588134957914, -35.87007288833441976, 191.2765776568629690 ) ) ;
#46937 = CARTESIAN_POINT ( 'NONE',  ( 52.65249034007830176, -49.32844715994059470, 300.4678068554150059 ) ) ;
#46938 = CIRCLE ( 'NONE', #9241, 6.557978799109520196 ) ;
#46939 = CARTESIAN_POINT ( 'NONE',  ( -21.81213075493552012, 60.58772898943853846, 31.24010949910693924 ) ) ;
#46940 = CARTESIAN_POINT ( 'NONE',  ( 97.81171347387959258, -40.51745984142272761, 22.63530404563221410 ) ) ;
#46941 = CARTESIAN_POINT ( 'NONE',  ( 116.3214877775586018, -32.94188667902410117, 30.13562527591096085 ) ) ;
#46943 = CARTESIAN_POINT ( 'NONE',  ( 48.45959712127301344, -26.00627455219131789, -5.074374724088000832 ) ) ;
#46942 = CARTESIAN_POINT ( 'NONE',  ( 103.9608317090438874, -29.20111914701857714, 277.6356252759112522 ) ) ;
#46944 = CARTESIAN_POINT ( 'NONE',  ( 108.3332299252464708, -46.73488901547833763, 173.6772747286529750 ) ) ;
#46945 = FACE_OUTER_BOUND ( 'NONE', #35606, .T. ) ;
#46946 = DIRECTION ( 'NONE',  ( 0.7071067811865692221, 0.7071067811865259234, 7.071067811865685367E-16 ) ) ;
#46947 = CIRCLE ( 'NONE', #81807, 1.571100913904471819 ) ;
#46948 = CARTESIAN_POINT ( 'NONE',  ( 25.56670390244797275, -48.82844715994099971, 170.4678068554149775 ) ) ;
#46949 = CARTESIAN_POINT ( 'NONE',  ( 34.27258461953899626, -35.55794170701810941, -5.074374724088000832 ) ) ;
#46950 = CARTESIAN_POINT ( 'NONE',  ( 31.75000000000000000, 24.56180297284579694, 3.174999999999999822 ) ) ;
#46952 = EDGE_LOOP ( 'NONE', ( #5910, #45451, #56230, #42168 ) ) ;
#46951 = CARTESIAN_POINT ( 'NONE',  ( -7.752335291937824557, 92.64399975678504973, -118.3043120271755413 ) ) ;
#46953 = DIRECTION ( 'NONE',  ( -0.7071067811865692221, -0.7071067811865259234, -7.071067811865685367E-16 ) ) ;
#46954 = CARTESIAN_POINT ( 'NONE',  ( 107.2435442917537500, -47.21071675017731906, 212.5899109901969837 ) ) ;
#46955 = CARTESIAN_POINT ( 'NONE',  ( 103.2788791697577295, -47.11347506355160419, 93.28610146638693834 ) ) ;
#46956 = CARTESIAN_POINT ( 'NONE',  ( 112.6870894866849966, -45.56130799126797370, 259.0270538473393458 ) ) ;
#46957 = DIRECTION ( 'NONE',  ( 0.000000000000000000, 0.000000000000000000, -1.000000000000000000 ) ) ;
#46958 = DIRECTION ( 'NONE',  ( 0.000000000000000000, 0.000000000000000000, 1.000000000000000000 ) ) ;
#46960 = FACE_OUTER_BOUND ( 'NONE', #14148, .T. ) ;
#46959 = CARTESIAN_POINT ( 'NONE',  ( 76.20505178924339873, 120.6499999999999915, 76.20505178924419454 ) ) ;
#46961 = DIRECTION ( 'NONE',  ( -1.000000000000000078E-15, 1.000000000000000000, 0.000000000000000000 ) ) ;
#46962 = CARTESIAN_POINT ( 'NONE',  ( 133.0522658619956928, -21.28573230649608661, 1.785258109344280975 ) ) ;
#46963 = ORIENTED_EDGE ( 'NONE', *, *, #82023, .T. ) ;
#46964 = VERTEX_POINT ( 'NONE', #37942 ) ;
#46965 = CARTESIAN_POINT ( 'NONE',  ( 112.6189512620115778, -30.20087909038965535, 138.9381341137909658 ) ) ;
#46967 = EDGE_LOOP ( 'NONE', ( #85173, #73512, #40468, #38841 ) ) ;
#46966 = CARTESIAN_POINT ( 'NONE',  ( 68.53801554307449351, 120.6499999999999915, -74.15067561874229796 ) ) ;
#46968 = CARTESIAN_POINT ( 'NONE',  ( 100.9546086862564920, -28.70707578211034061, 90.59232038796342579 ) ) ;
#46969 = CARTESIAN_POINT ( 'NONE',  ( 97.85535806214043930, -31.89376338832687097, 131.9413395616259947 ) ) ;
#46970 = LINE ( 'NONE', #81100, #23660 ) ;
#46971 = DIRECTION ( 'NONE',  ( -0.7071067811578587436, 0.7071067812152364018, 0.000000000000000000 ) ) ;
#46972 = PLANE ( 'NONE',  #54878 ) ;
#46973 = CARTESIAN_POINT ( 'NONE',  ( 117.0608945237148646, -38.08045311927313747, 109.7189586093670215 ) ) ;
#46974 = CARTESIAN_POINT ( 'NONE',  ( 116.6363502066643321, -38.74961609181406175, 63.66133956162595098 ) ) ;
#46975 = ORIENTED_EDGE ( 'NONE', *, *, #21162, .F. ) ;
#46976 = VERTEX_POINT ( 'NONE', #65204 ) ;
#46977 = VERTEX_POINT ( 'NONE', #9348 ) ;
#46978 = VECTOR ( 'NONE', #38808, 1000.000000000000000 ) ;
#46979 = LINE ( 'NONE', #81997, #18102 ) ;
#46981 = CARTESIAN_POINT ( 'NONE',  ( 107.0664832912730020, -27.87844715994269862, 361.9756252759109998 ) ) ;
#46980 = CARTESIAN_POINT ( 'NONE',  ( 109.6835627966674878, -27.30531164764932939, 170.8613395616249591 ) ) ;
#46982 = VECTOR ( 'NONE', #84177, 1000.000000000000000 ) ;
#46983 = CARTESIAN_POINT ( 'NONE',  ( -215.9000000000000057, 104.7749999999999915, -41.27499999999999858 ) ) ;
#46984 = ADVANCED_FACE ( 'NONE', ( #24755 ), #64757, .T. ) ;
#46985 = CARTESIAN_POINT ( 'NONE',  ( 12.70000000000000462, 81.72090770373000623, -129.9368274816651194 ) ) ;
#46986 = EDGE_CURVE ( 'NONE', #73517, #41893, #81865, .T. ) ;
#46987 = CARTESIAN_POINT ( 'NONE',  ( 72.06648329127401098, -46.47944715994106701, 14.67562527591093513 ) ) ;
#46988 = ADVANCED_FACE ( 'NONE', ( #58812, #80187 ), #24320, .T. ) ;
#46989 = DIRECTION ( 'NONE',  ( 0.000000000000000000, 0.000000000000000000, 1.000000000000000000 ) ) ;
#46990 = DIRECTION ( 'NONE',  ( 0.000000000000000000, 0.000000000000000000, 1.000000000000000000 ) ) ;
#46991 = CARTESIAN_POINT ( 'NONE',  ( 116.9541756933415257, -33.49491404195858735, 89.07848241876791917 ) ) ;
#46992 = ORIENTED_EDGE ( 'NONE', *, *, #28129, .F. ) ;
#46993 = EDGE_LOOP ( 'NONE', ( #44414, #84453, #22509, #5639 ) ) ;
#46994 = EDGE_CURVE ( 'NONE', #85940, #37406, #17935, .T. ) ;
#46995 = CARTESIAN_POINT ( 'NONE',  ( 90.44969454456422397, -56.64645651782492308, 249.5838068554174640 ) ) ;
#46996 = CARTESIAN_POINT ( 'NONE',  ( -83.02643542998004023, 84.62817240485476589, -100.7545871043107581 ) ) ;
#46997 = PRODUCT_DEFINITION_SHAPE ( 'NONE', 'NONE',  #80551 ) ;
#46998 = DIRECTION ( 'NONE',  ( 0.000000000000000000, 1.000000000000000000, 0.000000000000000000 ) ) ;
#46999 = CARTESIAN_POINT ( 'NONE',  ( 99.97311099609123630, -31.77112186149751949, 158.6471379886389741 ) ) ;
#47000 = EDGE_CURVE ( 'NONE', #51570, #5050, #30681, .T. ) ;
#47001 = CIRCLE ( 'NONE', #70458, 11.45913725231036118 ) ;
#47002 = AXIS2_PLACEMENT_3D ( 'NONE', #79132, #16898, #38995 ) ;
#47003 = AXIS2_PLACEMENT_3D ( 'NONE', #18919, #24844, #10323 ) ;
#47004 = EDGE_CURVE ( 'NONE', #55605, #770, #32008, .T. ) ;
#47005 = CARTESIAN_POINT ( 'NONE',  ( 70.06202783732103967, -36.73691869758536654, 394.9756252759101471 ) ) ;
#47006 = ORIENTED_EDGE ( 'NONE', *, *, #26616, .F. ) ;
#47007 = EDGE_LOOP ( 'NONE', ( #89504, #38922, #61240, #52605 ) ) ;
#47008 = DIRECTION ( 'NONE',  ( 0.000000000000000000, 0.000000000000000000, -1.000000000000000000 ) ) ;
#47009 = AXIS2_PLACEMENT_3D ( 'NONE', #38356, #57913, #37031 ) ;
#47010 = CARTESIAN_POINT ( 'NONE',  ( 144.1763536145585647, -138.0482283979624185, 247.6588381036639817 ) ) ;
#47011 = VERTEX_POINT ( 'NONE', #51112 ) ;
#47012 = ORIENTED_EDGE ( 'NONE', *, *, #74133, .F. ) ;
#47013 = CARTESIAN_POINT ( 'NONE',  ( 151.0667039024469886, -67.87844715994090450, 120.2178068554179902 ) ) ;
#47014 = EDGE_CURVE ( 'NONE', #50621, #3837, #17501, .T. ) ;
#47015 = CARTESIAN_POINT ( 'NONE',  ( 102.2537836627552821, -44.20608088590525853, 218.5530118773259574 ) ) ;
#47016 = DIRECTION ( 'NONE',  ( 0.000000000000000000, 1.000000000000000000, 0.000000000000000000 ) ) ;
#47017 = CARTESIAN_POINT ( 'NONE',  ( -111.3778403937640604, 65.20424434049171225, 68.11656773419859690 ) ) ;
#47018 = VERTEX_POINT ( 'NONE', #23879 ) ;
#47019 = ORIENTED_EDGE ( 'NONE', *, *, #69839, .F. ) ;
#47020 = DIRECTION ( 'NONE',  ( 0.000000000000000000, 0.000000000000000000, -1.000000000000000000 ) ) ;
#47021 = ORIENTED_EDGE ( 'NONE', *, *, #49953, .F. ) ;
#47022 = ORIENTED_EDGE ( 'NONE', *, *, #16649, .F. ) ;
#47023 = B_SPLINE_CURVE_WITH_KNOTS ( 'NONE', 3,
 ( #2775, #86779, #59935, #32237, #10471, #86333, #30910, #18168, #24993, #80866, #38173, #80414, #24550, #24111, #18621, #87224, #87667, #58600 ),
 .UNSPECIFIED., .F., .F.,
 ( 4, 2, 2, 2, 2, 2, 2, 2, 4 ),
 ( 0.000000000000000000, 0.06249999947104563358, 0.1249999989420912672, 0.1874999984131369146, 0.2499999978841825343, 0.3124999973552281540, 0.3749999968262738292, 0.4374999962973194489, 0.4999999957683650686 ),
 .UNSPECIFIED. ) ;
#47024 = CARTESIAN_POINT ( 'NONE',  ( 106.8982433325019059, -45.38234380569505788, 225.3671379886389730 ) ) ;
#47025 = CARTESIAN_POINT ( 'NONE',  ( 96.61975328461473111, -36.61901104994432643, 111.3184824187679567 ) ) ;
#47026 = CARTESIAN_POINT ( 'NONE',  ( 96.73644666290614680, -38.23103596604165944, 66.44133956162495735 ) ) ;
#47027 = CARTESIAN_POINT ( 'NONE',  ( 113.4712900281284362, -42.87177457074936626, 249.5838068554168672 ) ) ;
#47028 = CARTESIAN_POINT ( 'NONE',  ( 68.91674821478362389, 82.54999999999999716, 68.91674821478530077 ) ) ;
#47029 = DIRECTION ( 'NONE',  ( -1.000000000000000000, -1.000000000000000078E-15, 0.000000000000000000 ) ) ;
#47030 = CARTESIAN_POINT ( 'NONE',  ( 97.40207042353749500, -40.63861732370358482, 202.6327681330539860 ) ) ;
#47031 = CARTESIAN_POINT ( 'NONE',  ( 134.0664828118825938, -21.47944715903993540, 8.225259175038406312 ) ) ;
#47032 = VERTEX_POINT ( 'NONE', #51549 ) ;
#47033 = DIRECTION ( 'NONE',  ( 0.000000000000000000, 0.000000000000000000, -1.000000000000000000 ) ) ;
#47034 = ORIENTED_EDGE ( 'NONE', *, *, #86010, .F. ) ;
#47035 = ORIENTED_EDGE ( 'NONE', *, *, #55788, .T. ) ;
#47036 = DIRECTION ( 'NONE',  ( 0.7071067811866516006, -0.7071067811864434338, 0.000000000000000000 ) ) ;
#47037 = VECTOR ( 'NONE', #9852, 1000.000000000000000 ) ;
#47038 = ADVANCED_FACE ( 'NONE', ( #2981 ), #85669, .F. ) ;
#47039 = ORIENTED_EDGE ( 'NONE', *, *, #81421, .T. ) ;
#47040 = CIRCLE ( 'NONE', #26764, 3.000000000000002665 ) ;
#47041 = DIRECTION ( 'NONE',  ( -0.000000000000000000, -0.000000000000000000, -1.000000000000000000 ) ) ;
#47042 = LINE ( 'NONE', #12555, #10188 ) ;
#47043 = CARTESIAN_POINT ( 'NONE',  ( 108.0341695913198521, -25.71842219955733810, 109.9946728949589811 ) ) ;
#47044 = CARTESIAN_POINT ( 'NONE',  ( -10.55578339146518196, 75.48845273559737734, 130.1285694115591696 ) ) ;
#47045 = AXIS2_PLACEMENT_3D ( 'NONE', #82634, #34447, #68085 ) ;
#47046 = CARTESIAN_POINT ( 'NONE',  ( 37.56670390244716629, -48.82844715994126261, 180.4678068554150911 ) ) ;
#47047 = DIRECTION ( 'NONE',  ( 1.000000000000000000, 0.000000000000000000, -2.127927463864879951E-15 ) ) ;
#47050 = CARTESIAN_POINT ( 'NONE',  ( 103.8265608274144398, -48.10271009292816302, 213.3556252759109668 ) ) ;
#47049 = LINE ( 'NONE', #54304, #78961 ) ;
#47048 = DIRECTION ( 'NONE',  ( -1.000000000000000000, 0.000000000000000000, 0.000000000000000000 ) ) ;
#47051 = DIRECTION ( 'NONE',  ( 0.000000000000000000, 0.000000000000000000, -1.000000000000000000 ) ) ;
#47052 = DIRECTION ( 'NONE',  ( 0.7071067811864661934, 0.7071067811866289521, 7.071067811864966518E-16 ) ) ;
#47053 = ORIENTED_EDGE ( 'NONE', *, *, #3163, .F. ) ;
#47054 = CARTESIAN_POINT ( 'NONE',  ( -487.2989999999999782, 101.9113919710471947, 11.11250000000054072 ) ) ;
#47055 = DIRECTION ( 'NONE',  ( 0.000000000000000000, 1.000000000000000000, 0.000000000000000000 ) ) ;
#47056 = CARTESIAN_POINT ( 'NONE',  ( 19.56670390244648416, -25.42844715994203852, 129.9678068554150627 ) ) ;
#47057 = CARTESIAN_POINT ( 'NONE',  ( 172.5664832912729878, -18.82844715994071194, 255.9256252759120684 ) ) ;
#47058 = ADVANCED_FACE ( 'NONE', ( #66075 ), #81856, .T. ) ;
#47060 = VERTEX_POINT ( 'NONE', #79300 ) ;
#47059 = CARTESIAN_POINT ( 'NONE',  ( 100.8220609092773117, -45.17687181127147511, 257.0699109901966608 ) ) ;
#47061 = CARTESIAN_POINT ( 'NONE',  ( 101.7228746988208030, -28.24295021050552990, 195.5233366543221223 ) ) ;
#47062 = CARTESIAN_POINT ( 'NONE',  ( 117.5122013968931327, -37.28485508719111863, 14.78419670448294454 ) ) ;
#47063 = CARTESIAN_POINT ( 'NONE',  ( 108.0108636065302932, -26.30228954677034992, 151.0041967044829505 ) ) ;
#47064 = PLANE ( 'NONE',  #41813 ) ;
#47065 = CARTESIAN_POINT ( 'NONE',  ( 97.80783988303282683, -40.50800889367277335, 102.6348159224356920 ) ) ;
#47067 = CARTESIAN_POINT ( 'NONE',  ( 274.0659999999999741, 40.03750000000000142, -7.937500000000000000 ) ) ;
#47066 = CARTESIAN_POINT ( 'NONE',  ( 51.56670390244799762, -33.35206098992650681, 342.9256252759109884 ) ) ;
#47068 = DIRECTION ( 'NONE',  ( -1.000000000000000078E-15, 1.000000000000000083E-30, 1.000000000000000000 ) ) ;
#47069 = DIRECTION ( 'NONE',  ( -0.000000000000000000, -1.000000000000000000, -0.000000000000000000 ) ) ;
#47070 = EDGE_LOOP ( 'NONE', ( #60206, #53459 ) ) ;
#47071 = EDGE_CURVE ( 'NONE', #40995, #20045, #26871, .T. ) ;
#47072 = CIRCLE ( 'NONE', #74645, 9.525000000000000355 ) ;
#47073 = AXIS2_PLACEMENT_3D ( 'NONE', #60485, #75487, #40945 ) ;
#47074 = AXIS2_PLACEMENT_3D ( 'NONE', #29928, #57614, #85356 ) ;
#47075 = AXIS2_PLACEMENT_3D ( 'NONE', #41036, #62376, #67394 ) ;
#47076 = ORIENTED_EDGE ( 'NONE', *, *, #4901, .F. ) ;
#47077 = ORIENTED_EDGE ( 'NONE', *, *, #3042, .F. ) ;
#47078 = AXIS2_PLACEMENT_3D ( 'NONE', #5646, #89660, #61478 ) ;
#47079 = VECTOR ( 'NONE', #53107, 1000.000000000000000 ) ;
#47080 = ORIENTED_EDGE ( 'NONE', *, *, #7965, .T. ) ;
#47081 = CARTESIAN_POINT ( 'NONE',  ( -126.6438945437297292, 45.91417521994105755, 31.73029632275546774 ) ) ;
#47082 = CARTESIAN_POINT ( 'NONE',  ( 114.0759046727995241, -46.25395340493271590, 29.08133956162595268 ) ) ;
#47083 = CARTESIAN_POINT ( 'NONE',  ( 33.98325472291465132, 104.3431970271542042, 3.174999999999999822 ) ) ;
#47084 = CARTESIAN_POINT ( 'NONE',  ( 116.3212776292293995, -32.94146857471265122, 80.13562527591095375 ) ) ;
#47086 = CARTESIAN_POINT ( 'NONE',  ( 22.49541547940852837, 22.69262065192447864, 323.8756252759109202 ) ) ;
#47085 = CARTESIAN_POINT ( 'NONE',  ( 107.0620278373210255, -36.73691869758540207, 361.9756252759100903 ) ) ;
#47087 = CARTESIAN_POINT ( 'NONE',  ( 98.66229053285113082, -40.10320091580625501, 251.0648007804577730 ) ) ;
#47088 = EDGE_LOOP ( 'NONE', ( #3165, #9768 ) ) ;
#47089 = ORIENTED_EDGE ( 'NONE', *, *, #52118, .T. ) ;
#47090 = VERTEX_POINT ( 'NONE', #20957 ) ;
#47091 = LINE ( 'NONE', #12606, #77641 ) ;
#47092 = CARTESIAN_POINT ( 'NONE',  ( -492.0614999999999668, 93.66249999999999432, 11.11250000000040217 ) ) ;
#47093 = CARTESIAN_POINT ( 'NONE',  ( -7.205548786489490269E-13, 127.0000000000000000, 103.1875000000000000 ) ) ;
#47094 = AXIS2_PLACEMENT_3D ( 'NONE', #46937, #33777, #46491 ) ;
#47095 = CARTESIAN_POINT ( 'NONE',  ( 90.06670420047025516, -131.9777253117771636, 55.21780685541800437 ) ) ;
#47096 = ADVANCED_FACE ( 'NONE', ( #21416 ), #29591, .F. ) ;
#47097 = CARTESIAN_POINT ( 'NONE',  ( 114.5680773229086782, -32.01199386431652272, 30.70444044875397793 ) ) ;
#47098 = EDGE_CURVE ( 'NONE', #68997, #37445, #74156, .T. ) ;
#47099 = CARTESIAN_POINT ( 'NONE',  ( 118.3862315815644450, 93.55466788070661721, -6.352948492896714150 ) ) ;
#47100 = ADVANCED_FACE ( 'NONE', ( #69113 ), #69560, .F. ) ;
#47101 = CARTESIAN_POINT ( 'NONE',  ( 0.000000000000000000, 44.45000000000000284, 0.000000000000000000 ) ) ;
#47102 = CARTESIAN_POINT ( 'NONE',  ( 115.2378349030890945, -31.35427756934436871, 254.2899109901970292 ) ) ;
#47103 = FACE_OUTER_BOUND ( 'NONE', #27421, .T. ) ;
#47104 = ORIENTED_EDGE ( 'NONE', *, *, #68168, .T. ) ;
#47105 = EDGE_CURVE ( 'NONE', #1366, #37421, #23834, .T. ) ;
#47106 = CARTESIAN_POINT ( 'NONE',  ( 188.5667039024479834, -58.35344715994099829, 293.2178068554150627 ) ) ;
#47107 = DIRECTION ( 'NONE',  ( 1.000000000000000000, 0.000000000000000000, 0.000000000000000000 ) ) ;
#47108 = CARTESIAN_POINT ( 'NONE',  ( 99.78939748087903183, -33.03164401141575723, 48.77094751244892734 ) ) ;
#47109 = CIRCLE ( 'NONE', #70354, 6.571100913904384555 ) ;
#47110 = EDGE_CURVE ( 'NONE', #41326, #58613, #49934, .T. ) ;
#47111 = DIRECTION ( 'NONE',  ( 1.000000000000000000, 0.000000000000000000, 0.000000000000000000 ) ) ;
#47112 = VECTOR ( 'NONE', #54759, 1000.000000000000000 ) ;
#47113 = PLANE ( 'NONE',  #6965 ) ;
#47114 = ADVANCED_FACE ( 'NONE', ( #28203 ), #55896, .T. ) ;
#47115 = CARTESIAN_POINT ( 'NONE',  ( 104.4080392062299012, -46.45807122338121786, 193.3647126831750143 ) ) ;
#47116 = EDGE_LOOP ( 'NONE', ( #16907, #16521, #60779, #54058, #81161, #56064, #37502, #24682, #50637, #77238, #64994, #54516 ) ) ;
#47117 = FACE_OUTER_BOUND ( 'NONE', #29805, .T. ) ;
#47118 = EDGE_LOOP ( 'NONE', ( #73570, #53570, #15829, #22727 ) ) ;
#47119 = CARTESIAN_POINT ( 'NONE',  ( 98.83989573471103540, -28.19928051380002287, 115.6870538473389587 ) ) ;
#47120 = EDGE_LOOP ( 'NONE', ( #49917, #17209, #44260, #3147 ) ) ;
#47121 = CARTESIAN_POINT ( 'NONE',  ( 109.3970511370136904, -44.97690468586920787, 72.21813411379096692 ) ) ;
#47122 = FACE_OUTER_BOUND ( 'NONE', #43921, .T. ) ;
#47123 = CARTESIAN_POINT ( 'NONE',  ( 100.2558307937446074, -42.39895253252459639, 113.3101547344679574 ) ) ;
#47124 = LINE ( 'NONE', #74859, #88123 ) ;
#47125 = DIRECTION ( 'NONE',  ( 1.000000000000000000, 4.163336342344333240E-14, 0.000000000000000000 ) ) ;
#47126 = CARTESIAN_POINT ( 'NONE',  ( 112.7535375185862705, -27.22457367525289129, 50.65943479972101215 ) ) ;
#47127 = CARTESIAN_POINT ( 'NONE',  ( 104.4903241021636973, -26.97870597410075888, 181.2818875591321444 ) ) ;
#47128 = DIRECTION ( 'NONE',  ( 0.000000000000000000, 0.000000000000000000, 1.000000000000000000 ) ) ;
#47129 = VECTOR ( 'NONE', #9807, 1000.000000000000000 ) ;
#47130 = ORIENTED_EDGE ( 'NONE', *, *, #16201, .T. ) ;
#47131 = CARTESIAN_POINT ( 'NONE',  ( 77.54412859703678862, -19.82508440162619223, 2.797770139038477044 ) ) ;
#47132 = AXIS2_PLACEMENT_3D ( 'NONE', #12250, #40396, #19965 ) ;
#47133 = AXIS2_PLACEMENT_3D ( 'NONE', #12152, #41182, #68009 ) ;
#47134 = VECTOR ( 'NONE', #23719, 1000.000000000000000 ) ;
#47135 = VERTEX_POINT ( 'NONE', #12816 ) ;
#47136 = ORIENTED_EDGE ( 'NONE', *, *, #58191, .F. ) ;
#47137 = AXIS2_PLACEMENT_3D ( 'NONE', #21863, #35460, #22306 ) ;
#47138 = DIRECTION ( 'NONE',  ( 2.900000000000000265E-14, -2.000000000000000155E-15, 1.000000000000000000 ) ) ;
#47139 = ORIENTED_EDGE ( 'NONE', *, *, #23176, .T. ) ;
#47140 = CARTESIAN_POINT ( 'NONE',  ( 104.5747221139661320, -26.66317121150808944, 240.2575300378159682 ) ) ;
#47141 = CARTESIAN_POINT ( 'NONE',  ( 108.5929805111718593, -47.10003145027929605, 138.6927681330539883 ) ) ;
#47142 = DIRECTION ( 'NONE',  ( 0.000000000000000000, 1.000000000000000000, 0.000000000000000000 ) ) ;
#47143 = DIRECTION ( 'NONE',  ( -1.000000000000000078E-15, 1.000000000000000083E-30, 1.000000000000000000 ) ) ;
#47144 = CARTESIAN_POINT ( 'NONE',  ( 112.5142634568524329, -27.84101767465772070, 90.63848241876793566 ) ) ;
#47145 = PLANE ( 'NONE',  #74051 ) ;
#47146 = ORIENTED_EDGE ( 'NONE', *, *, #83576, .T. ) ;
#47147 = CIRCLE ( 'NONE', #76216, 10.04999999999999361 ) ;
#47148 = CARTESIAN_POINT ( 'NONE',  ( 97.81168895331838087, -40.51742574516882200, 287.6356252759109680 ) ) ;
#47149 = DIRECTION ( 'NONE',  ( -1.087812297297669405E-15, 1.000000000000000000, -3.100000000000000044E-14 ) ) ;
#47150 = ADVANCED_FACE ( 'NONE', ( #34126 ), #33691, .T. ) ;
#47151 = VECTOR ( 'NONE', #76039, 1000.000000000000000 ) ;
#47152 = ORIENTED_EDGE ( 'NONE', *, *, #79629, .F. ) ;
#47153 = DIRECTION ( 'NONE',  ( 0.000000000000000000, 0.000000000000000000, 1.000000000000000000 ) ) ;
#47154 = DIRECTION ( 'NONE',  ( 0.000000000000000000, 1.000000000000000000, 0.000000000000000000 ) ) ;
#47155 = CARTESIAN_POINT ( 'NONE',  ( 99.34937008002594894, -28.84845824588779095, 270.7051490854348685 ) ) ;
#47156 = CARTESIAN_POINT ( 'NONE',  ( 57.14999999999999858, 95.25000000000000000, 329.4379999999999882 ) ) ;
#47157 = CARTESIAN_POINT ( 'NONE',  ( 74.98969683741650272, 82.54999999999999716, 346.9005000000000223 ) ) ;
#47158 = CARTESIAN_POINT ( 'NONE',  ( 44.45000000000000284, 114.2999999999999972, 257.1750000000000114 ) ) ;
#47159 = CARTESIAN_POINT ( 'NONE',  ( 105.8912501276363543, -45.18964566429946217, 256.8895626852198006 ) ) ;
#47161 = CARTESIAN_POINT ( 'NONE',  ( 97.59110611908495514, -31.08311649095520934, 126.9108633711489915 ) ) ;
#47160 = CARTESIAN_POINT ( 'NONE',  ( 98.43224882071085347, -31.53101443417716254, 100.8965674670191959 ) ) ;
#47162 = CARTESIAN_POINT ( 'NONE',  ( 172.5664832912729878, -27.57844715994070484, 198.9256252759119832 ) ) ;
#47163 = CARTESIAN_POINT ( 'NONE',  ( 102.0606772939666627, -27.53441096011033906, 145.4727681330539610 ) ) ;
#47164 = EDGE_LOOP ( 'NONE', ( #5177, #32025, #18441, #11872 ) ) ;
#47165 = DIRECTION ( 'NONE',  ( 0.000000000000000000, -1.000000000000000000, 0.000000000000000000 ) ) ;
#47166 = ORIENTED_EDGE ( 'NONE', *, *, #62208, .T. ) ;
#47167 = DIRECTION ( 'NONE',  ( -1.000000000000000000, 0.000000000000000000, 0.000000000000000000 ) ) ;
#47168 = DIRECTION ( 'NONE',  ( 0.000000000000000000, 0.000000000000000000, 1.000000000000000000 ) ) ;
#47169 = CARTESIAN_POINT ( 'NONE',  ( 136.5888380630362633, -35.63381004753313164, 2.797770231024470533 ) ) ;
#47170 = ORIENTED_EDGE ( 'NONE', *, *, #6919, .F. ) ;
#47171 = CARTESIAN_POINT ( 'NONE',  ( 141.0664832912740394, -46.72944715994099596, 14.67562527591100441 ) ) ;
#47173 = VERTEX_POINT ( 'NONE', #44577 ) ;
#47172 = CARTESIAN_POINT ( 'NONE',  ( 116.8367917427482467, -32.96809911012589112, 139.1184824187679396 ) ) ;
#47174 = CARTESIAN_POINT ( 'NONE',  ( 141.0667039024479834, -50.82844715994100682, 250.9178068554160461 ) ) ;
#47175 = CARTESIAN_POINT ( 'NONE',  ( -130.1098569802758504, 89.26666702275855414, -10.78644903371280961 ) ) ;
#47176 = CARTESIAN_POINT ( 'NONE',  ( 144.8545562996768012, -1.932463243632626781, 394.9756252759100903 ) ) ;
#47177 = AXIS2_PLACEMENT_3D ( 'NONE', #34548, #62253, #21837 ) ;
#47178 = DIRECTION ( 'NONE',  ( 1.000000000000000000, 0.000000000000000000, 0.000000000000000000 ) ) ;
#47179 = VERTEX_POINT ( 'NONE', #4491 ) ;
#47180 = ADVANCED_FACE ( 'NONE', ( #19009 ), #88060, .F. ) ;
#47181 = CIRCLE ( 'NONE', #22581, 2.749999999999974687 ) ;
#47182 = DIRECTION ( 'NONE',  ( 1.000000000000000000, 0.000000000000000000, 0.000000000000000000 ) ) ;
#47183 = ORIENTED_EDGE ( 'NONE', *, *, #58581, .T. ) ;
#47184 = ORIENTED_EDGE ( 'NONE', *, *, #19220, .T. ) ;
#47185 = DIRECTION ( 'NONE',  ( 1.000000000000000078E-15, -1.000000000000000083E-30, -1.000000000000000000 ) ) ;
#47186 = CARTESIAN_POINT ( 'NONE',  ( 93.77212533081413426, 95.08644067748868167, -90.83954799657421120 ) ) ;
#47187 = CARTESIAN_POINT ( 'NONE',  ( 98.30753412437063332, -41.72887537653042500, 156.7397919321415714 ) ) ;
#47188 = DIRECTION ( 'NONE',  ( 0.9242245927363031965, 0.3818493186865917766, 0.000000000000000000 ) ) ;
#47190 = CARTESIAN_POINT ( 'NONE',  ( -2.899925867002088431, 70.17843955035350234, -118.5212385615275252 ) ) ;
#47189 = CARTESIAN_POINT ( 'NONE',  ( 116.3212776292296127, -32.94146857471318413, 287.6356252759109680 ) ) ;
#47191 = CARTESIAN_POINT ( 'NONE',  ( 112.1392728139803694, -28.01277785882846061, 179.6564653195408425 ) ) ;
#47192 = AXIS2_PLACEMENT_3D ( 'NONE', #68581, #19981, #47663 ) ;
#47193 = ORIENTED_EDGE ( 'NONE', *, *, #41072, .F. ) ;
#47194 = CIRCLE ( 'NONE', #31255, 6.349999999999994316 ) ;
#47195 = VECTOR ( 'NONE', #4675, 999.9999999999998863 ) ;
#47196 = FACE_OUTER_BOUND ( 'NONE', #14652, .T. ) ;
#47197 = VECTOR ( 'NONE', #28617, 1000.000000000000000 ) ;
#47198 = CARTESIAN_POINT ( 'NONE',  ( 181.8764988495249497, -33.54226604284360036, 117.4678068554150627 ) ) ;
#47199 = CARTESIAN_POINT ( 'NONE',  ( 108.5755967597531679, -27.06580334247545494, 185.9527681330529845 ) ) ;
#47200 = EDGE_CURVE ( 'NONE', #25576, #752, #26267, .T. ) ;
#47202 = VERTEX_POINT ( 'NONE', #67150 ) ;
#47201 = DIRECTION ( 'NONE',  ( -0.7071067812159671506, -0.7071067811571278838, -6.612322856129998538E-17 ) ) ;
#47203 = VECTOR ( 'NONE', #45069, 1000.000000000000000 ) ;
#47204 = B_SPLINE_CURVE_WITH_KNOTS ( 'NONE', 3,
 ( #44234, #9736, #2483, #72416, #10616, #57880, #10180, #79241, #43345, #79688, #85614, #45123, #15668, #17442, #72848, #38321, #37888, #16553, #37441, #58325, #8861, #66019, #36559, #65142, #2034, #29742, #23392, #65587, #43794, #3810, #57429 ),
 .UNSPECIFIED., .F., .F.,
 ( 4, 2, 2, 1, 2, 2, 2, 2, 2, 2, 2, 1, 1, 2, 2, 2, 4 ),
 ( 0.000000000000000000, 0.1249999999999738542, 0.1874999999999520384, 0.2187499999999411304, 0.2343749999999427958, 0.2499999999999444611, 0.3749999999999549805, 0.4374999999999669709, 0.4999999999999790168, 0.6250000000000159872, 0.6875000000000371925, 0.7187500000000494049, 0.7343750000000499600, 0.7421875000000518474, 0.7500000000000536238, 0.8750000000000267564, 1.000000000000000000 ),
 .UNSPECIFIED. ) ;
#47205 = CARTESIAN_POINT ( 'NONE',  ( 116.3624975636023322, -33.68846805112529808, 85.07848241876692441 ) ) ;
#47206 = ADVANCED_FACE ( 'NONE', ( #74871 ), #25824, .T. ) ;
#47207 = LINE ( 'NONE', #67674, #41429 ) ;
#47208 = EDGE_CURVE ( 'NONE', #85102, #69134, #25369, .T. ) ;
#47209 = PLANE ( 'NONE',  #74656 ) ;
#47210 = AXIS2_PLACEMENT_3D ( 'NONE', #8580, #64881, #50793 ) ;
#47211 = DIRECTION ( 'NONE',  ( 9.351236661543306751E-17, -3.725950533538267725E-29, -1.000000000000000000 ) ) ;
#47212 = ORIENTED_EDGE ( 'NONE', *, *, #82300, .F. ) ;
#47213 = LINE ( 'NONE', #89020, #53003 ) ;
#47214 = EDGE_CURVE ( 'NONE', #11683, #64730, #74423, .T. ) ;
#47215 = ORIENTED_EDGE ( 'NONE', *, *, #53476, .F. ) ;
#47216 = ORIENTED_EDGE ( 'NONE', *, *, #44313, .T. ) ;
#47217 = AXIS2_PLACEMENT_3D ( 'NONE', #62189, #21777, #89927 ) ;
#47218 = CARTESIAN_POINT ( 'NONE',  ( 102.2537836627552821, -44.20608088590525853, 218.5530118773259574 ) ) ;
#47219 = DIRECTION ( 'NONE',  ( 1.000000000000000000, 0.000000000000000000, 0.000000000000000000 ) ) ;
#47220 = CARTESIAN_POINT ( 'NONE',  ( -118.1262036371152533, 90.29828471680515634, -10.09645181158828287 ) ) ;
#47221 = CIRCLE ( 'NONE', #16781, 5.041900000000001825 ) ;
#47222 = DIRECTION ( 'NONE',  ( -0.8660254037844351549, 0.000000000000000000, -0.5000000000000061062 ) ) ;
#47223 = EDGE_CURVE ( 'NONE', #21126, #54865, #81260, .T. ) ;
#47224 = CARTESIAN_POINT ( 'NONE',  ( 82.16371341589938027, -38.51083119283502754, 2.376725019073457013 ) ) ;
#47225 = VERTEX_POINT ( 'NONE', #82154 ) ;
#47226 = CARTESIAN_POINT ( 'NONE',  ( 41.56648329127499153, -36.32844715994070839, 18.92562527591200094 ) ) ;
#47227 = LINE ( 'NONE', #74055, #8196 ) ;
#47228 = ORIENTED_EDGE ( 'NONE', *, *, #25695, .T. ) ;
#47229 = CARTESIAN_POINT ( 'NONE',  ( 116.1206117333611871, -31.56300607074027909, 289.2384824187681716 ) ) ;
#47230 = ORIENTED_EDGE ( 'NONE', *, *, #12172, .F. ) ;
#47231 = CARTESIAN_POINT ( 'NONE',  ( 99.19750579858670392, -34.55944272753168889, 248.9309475124489950 ) ) ;
#47232 = DIRECTION ( 'NONE',  ( -0.06842228117015292099, 0.06842228117823027922, 0.9953073811028629869 ) ) ;
#47233 = CARTESIAN_POINT ( 'NONE',  ( 96.69720940280899413, -36.59277893904148726, 156.3280062282929634 ) ) ;
#47234 = CARTESIAN_POINT ( 'NONE',  ( 23.49588678361623906, 79.64122941661595689, 306.6787378533616106 ) ) ;
#47235 = DIRECTION ( 'NONE',  ( 0.000000000000000000, 0.000000000000000000, 1.000000000000000000 ) ) ;
#47236 = CARTESIAN_POINT ( 'NONE',  ( 90.44969454456405344, -18.85368780205715566, 218.8274735512160589 ) ) ;
#47237 = DIRECTION ( 'NONE',  ( 0.000000000000000000, 0.000000000000000000, -1.000000000000000000 ) ) ;
#47239 = CARTESIAN_POINT ( 'NONE',  ( 96.76602677561474763, -40.86443131079876423, 247.6422919425769749 ) ) ;
#47238 = AXIS2_PLACEMENT_3D ( 'NONE', #23630, #51289, #57678 ) ;
#47240 = DIRECTION ( 'NONE',  ( 0.000000000000000000, 0.000000000000000000, -1.000000000000000000 ) ) ;
#47241 = ORIENTED_EDGE ( 'NONE', *, *, #30410, .T. ) ;
#47242 = CARTESIAN_POINT ( 'NONE',  ( 102.5393486652204160, -27.29027178147674348, 91.43276813305395478 ) ) ;
#47243 = DIRECTION ( 'NONE',  ( -0.7071067811855900054, -0.7071067811875051401, 0.000000000000000000 ) ) ;
#47244 = AXIS2_PLACEMENT_3D ( 'NONE', #18435, #67933, #59316 ) ;
#47245 = ORIENTED_EDGE ( 'NONE', *, *, #63522, .F. ) ;
#47246 = ORIENTED_EDGE ( 'NONE', *, *, #5392, .T. ) ;
#47247 = ORIENTED_EDGE ( 'NONE', *, *, #21918, .T. ) ;
#47248 = CARTESIAN_POINT ( 'NONE',  ( 112.1371669992055047, -28.01157492980603436, 159.6564172049183412 ) ) ;
#47249 = DIRECTION ( 'NONE',  ( 0.000000000000000000, 0.000000000000000000, -1.000000000000000000 ) ) ;
#47250 = DIRECTION ( 'NONE',  ( 0.7071067811865389130, 0.000000000000000000, 0.7071067811865561215 ) ) ;
#47251 = DIRECTION ( 'NONE',  ( -1.000000000000000000, 0.000000000000000000, 0.000000000000000000 ) ) ;
#47252 = CARTESIAN_POINT ( 'NONE',  ( 99.76898186052154927, -41.38212431049157658, 139.5842808457819615 ) ) ;
#47253 = CARTESIAN_POINT ( 'NONE',  ( 105.1049547281328671, -25.82818065531082041, 271.2061014663873380 ) ) ;
#47254 = DIRECTION ( 'NONE',  ( 3.999999999999999995E-14, -1.000000000000000000, 4.100000000000000342E-29 ) ) ;
#47255 = ORIENTED_EDGE ( 'NONE', *, *, #73590, .F. ) ;
#47256 = CARTESIAN_POINT ( 'NONE',  ( 129.9989688714891827, 86.64186789594792515, 12.05153810119577251 ) ) ;
#47257 = CARTESIAN_POINT ( 'NONE',  ( 99.04405175095710945, -42.84124461182535271, 41.84339552792118155 ) ) ;
#47258 = EDGE_CURVE ( 'NONE', #17863, #27883, #46692, .T. ) ;
#47259 = EDGE_LOOP ( 'NONE', ( #67995, #31044, #70607, #20462 ) ) ;
#47260 = ORIENTED_EDGE ( 'NONE', *, *, #63963, .T. ) ;
#47261 = VECTOR ( 'NONE', #29711, 1000.000000000000000 ) ;
#47262 = AXIS2_PLACEMENT_3D ( 'NONE', #27337, #13715, #69128 ) ;
#47263 = DIRECTION ( 'NONE',  ( 1.000000000000000078E-15, -1.000000000000000083E-30, -1.000000000000000000 ) ) ;
#47264 = AXIS2_PLACEMENT_3D ( 'NONE', #7359, #2792, #78212 ) ;
#47265 = EDGE_LOOP ( 'NONE', ( #65006, #44100, #71617, #30282 ) ) ;
#47266 = ORIENTED_EDGE ( 'NONE', *, *, #2061, .T. ) ;
#47267 = DIRECTION ( 'NONE',  ( 0.7071067811865295871, -0.7071067811865655584, 7.071067811865303756E-16 ) ) ;
#47268 = DIRECTION ( 'NONE',  ( -0.7071067811864691910, -0.7071067811866257324, -7.071067811864685486E-16 ) ) ;
#47269 = CIRCLE ( 'NONE', #13897, 10.00000000000000711 ) ;
#47270 = ADVANCED_FACE ( 'NONE', ( #67603 ), #30521, .F. ) ;
#47271 = LINE ( 'NONE', #58341, #55390 ) ;
#47272 = DIRECTION ( 'NONE',  ( -1.000000000000000078E-15, 1.000000000000000000, -3.100000000000000044E-14 ) ) ;
#47273 = CARTESIAN_POINT ( 'NONE',  ( 115.0466524894680731, -42.26004630958951935, 162.7667055423629847 ) ) ;
#47274 = CARTESIAN_POINT ( 'NONE',  ( 104.4797840155964082, -46.91084102236943920, 47.37848241876796607 ) ) ;
#47275 = DIRECTION ( 'NONE',  ( -0.7071067812162665778, -0.7071067811568285677, -7.071067812162971544E-16 ) ) ;
#47276 = ORIENTED_EDGE ( 'NONE', *, *, #8, .F. ) ;
#47277 = CARTESIAN_POINT ( 'NONE',  ( -91.51265874544272094, 76.91656954603719498, -75.37281393334477286 ) ) ;
#47278 = ORIENTED_EDGE ( 'NONE', *, *, #45799, .F. ) ;
#47279 = FACE_OUTER_BOUND ( 'NONE', #68106, .T. ) ;
#47280 = VERTEX_POINT ( 'NONE', #40337 ) ;
#47281 = LINE ( 'NONE', #83627, #49394 ) ;
#47282 = CARTESIAN_POINT ( 'NONE',  ( 41.56648329127499153, -36.32844715994070839, 78.92562527591199739 ) ) ;
#47283 = CARTESIAN_POINT ( 'NONE',  ( 25.56670390244748603, -48.82844715994178841, 134.7178068554150627 ) ) ;
#47284 = CIRCLE ( 'NONE', #42948, 3.250000000000002665 ) ;
#47285 = CARTESIAN_POINT ( 'NONE',  ( 38.10000000000000142, 69.84999999999999432, 292.1000000000000227 ) ) ;
#47286 = ORIENTED_EDGE ( 'NONE', *, *, #83858, .T. ) ;
#47287 = ADVANCED_FACE ( 'NONE', ( #81702 ), #88513, .F. ) ;
#47288 = CARTESIAN_POINT ( 'NONE',  ( 102.7461184130007581, -25.66741906146929253, 20.37276813305294354 ) ) ;
#47289 = CARTESIAN_POINT ( 'NONE',  ( 115.2412948192700952, -44.23743989039658686, 74.22324432352993995 ) ) ;
#47290 = SHAPE_REPRESENTATION ( 'Proximity Switch Housing', ( #50656 ), #7165 ) ;
#47291 = CIRCLE ( 'NONE', #64760, 4.500000000000003553 ) ;
#47293 = CARTESIAN_POINT ( 'NONE',  ( 113.7313622454166904, -99.85325460238200890, -19.78219314458215550 ) ) ;
#47292 = CARTESIAN_POINT ( 'NONE',  ( 177.8371591254545478, -47.82818131005477369, 129.9678068554150059 ) ) ;
#47294 = DIRECTION ( 'NONE',  ( 8.755702086949183871E-16, 1.000000000000000000, 0.000000000000000000 ) ) ;
#47295 = DIRECTION ( 'NONE',  ( 0.000000000000000000, 0.000000000000000000, -1.000000000000000000 ) ) ;
#47296 = ORIENTED_EDGE ( 'NONE', *, *, #9088, .F. ) ;
#47297 = DIRECTION ( 'NONE',  ( 0.000000000000000000, 1.000000000000000000, 0.000000000000000000 ) ) ;
#47298 = CARTESIAN_POINT ( 'NONE',  ( 147.0667039024469886, -67.87844715994090450, 245.4920193514479934 ) ) ;
#47299 = DIRECTION ( 'NONE',  ( 0.000000000000000000, 0.000000000000000000, 1.000000000000000000 ) ) ;
#47300 = VERTEX_POINT ( 'NONE', #72309 ) ;
#47301 = CARTESIAN_POINT ( 'NONE',  ( 96.67081033544403113, -37.96906397156782731, 41.42133956162496844 ) ) ;
#47302 = CARTESIAN_POINT ( 'NONE',  ( 117.1274056176845733, -39.54282605291903252, 94.60991099019693706 ) ) ;
#47304 = DIRECTION ( 'NONE',  ( 4.299999999999999979E-14, -1.000000000000000000, 4.400000000000000367E-29 ) ) ;
#47303 = CARTESIAN_POINT ( 'NONE',  ( 117.0612810359348543, -38.07772461170434752, 173.7166616957481722 ) ) ;
#47305 = DIRECTION ( 'NONE',  ( 0.0001211784769825749220, -0.7071067708032379162, 0.7071067811865431318 ) ) ;
#47306 = LINE ( 'NONE', #61832, #76721 ) ;
#47307 = EDGE_LOOP ( 'NONE', ( #31249, #1756 ) ) ;
#47308 = CARTESIAN_POINT ( 'NONE',  ( 107.9743429475490615, -26.39917242597376301, 105.9946728949579864 ) ) ;
#47310 = ORIENTED_EDGE ( 'NONE', *, *, #70009, .F. ) ;
#47309 = CARTESIAN_POINT ( 'NONE',  ( 11.02882537043472233, 88.86092628232667323, 130.0895302200946162 ) ) ;
#47311 = CARTESIAN_POINT ( 'NONE',  ( 114.5897159479185490, -29.54407062678539830, 230.4327681330539690 ) ) ;
#47312 = CARTESIAN_POINT ( 'NONE',  ( 97.81213350417895924, -40.51851190632524435, 252.6356759604615547 ) ) ;
#47313 = CARTESIAN_POINT ( 'NONE',  ( 242.3160000000000025, 40.03750000000000142, -63.94449999999999790 ) ) ;
#47314 = DIRECTION ( 'NONE',  ( 1.000000000000000000, 1.261617073437676668E-15, 9.462128050782575008E-16 ) ) ;
#47315 = EDGE_CURVE ( 'NONE', #72419, #64158, #5839, .T. ) ;
#47316 = CARTESIAN_POINT ( 'NONE',  ( 69.25757238336809962, -1.944390235229864539, 394.9756252759101471 ) ) ;
#47317 = DIRECTION ( 'NONE',  ( 0.000000000000000000, 0.000000000000000000, 1.000000000000000000 ) ) ;
#47318 = DIRECTION ( 'NONE',  ( 0.000000000000000000, 1.000000000000000000, 0.000000000000000000 ) ) ;
#47319 = AXIS2_PLACEMENT_3D ( 'NONE', #29065, #29512, #49025 ) ;
#47320 = CARTESIAN_POINT ( 'NONE',  ( 103.1701080265564485, -27.72257962874988024, 155.4013395616259743 ) ) ;
#47321 = ORIENTED_EDGE ( 'NONE', *, *, #70178, .T. ) ;
#47322 = ORIENTED_EDGE ( 'NONE', *, *, #29175, .T. ) ;
#47323 = CIRCLE ( 'NONE', #41550, 0.5000000000000004441 ) ;
#47324 = CARTESIAN_POINT ( 'NONE',  ( 98.22997538087754776, -36.06364078424440578, 142.6987261630399644 ) ) ;
#47325 = CIRCLE ( 'NONE', #40072, 0.5000000000000172085 ) ;
#47326 = DIRECTION ( 'NONE',  ( 1.000000000000000000, -2.098553464303459752E-16, 0.000000000000000000 ) ) ;
#47327 = AXIS2_PLACEMENT_3D ( 'NONE', #81125, #68814, #5702 ) ;
#47329 = CARTESIAN_POINT ( 'NONE',  ( 133.6498166246070127, 12.92155284005802507, 336.5756252759110225 ) ) ;
#47328 = CARTESIAN_POINT ( 'NONE',  ( 100.5669465097398358, -44.03830869352244548, 262.9984824187674235 ) ) ;
#47330 = AXIS2_PLACEMENT_3D ( 'NONE', #66333, #79998, #85924 ) ;
#47331 = DIRECTION ( 'NONE',  ( 0.000000000000000000, -1.000000000000000000, 0.000000000000000000 ) ) ;
#47332 = FACE_OUTER_BOUND ( 'NONE', #41950, .T. ) ;
#47333 = ADVANCED_FACE ( 'NONE', ( #54389 ), #11292, .T. ) ;
#47334 = CARTESIAN_POINT ( 'NONE',  ( 107.0664832912739968, -36.72944715994100306, 287.6356252759109680 ) ) ;
#47335 = CARTESIAN_POINT ( 'NONE',  ( 182.0667039024476708, -32.29483332967959086, 237.4678068554150059 ) ) ;
#47336 = CARTESIAN_POINT ( 'NONE',  ( 188.5667039024479834, -62.87844715994099687, 254.4678068554150343 ) ) ;
#47337 = ADVANCED_FACE ( 'NONE', ( #75320, #37335, #65040, #85952, #23723 ), #51383, .T. ) ;
#47338 = CARTESIAN_POINT ( 'NONE',  ( 97.78191787992076911, -41.50032452247409509, 196.7041967044819728 ) ) ;
#47339 = DIRECTION ( 'NONE',  ( 0.000000000000000000, 0.000000000000000000, -1.000000000000000000 ) ) ;
#47340 = ORIENTED_EDGE ( 'NONE', *, *, #25280, .T. ) ;
#47341 = EDGE_LOOP ( 'NONE', ( #29544, #58226, #22481, #61793 ) ) ;
#47342 = CARTESIAN_POINT ( 'NONE',  ( -99.17101862044600580, 74.81660785136578795, -84.91200770515642660 ) ) ;
#47343 = CARTESIAN_POINT ( 'NONE',  ( 77.85922577378461540, -17.08568546287367695, 2.471387922356760303 ) ) ;
#47344 = CARTESIAN_POINT ( 'NONE',  ( 194.0667039024473581, -24.92844715993408045, 249.9678068554149775 ) ) ;
#47345 = CARTESIAN_POINT ( 'NONE',  ( 163.0667039024466192, -32.29483332967941323, 313.9678068554149490 ) ) ;
#47346 = VECTOR ( 'NONE', #40570, 1000.000000000000000 ) ;
#47347 = CARTESIAN_POINT ( 'NONE',  ( -186.2398777604659870, 20.32000000000000028, 107.9500000000000028 ) ) ;
#47348 = ORIENTED_EDGE ( 'NONE', *, *, #39995, .T. ) ;
#47349 = DIRECTION ( 'NONE',  ( 0.000000000000000000, 1.000000000000000000, 0.000000000000000000 ) ) ;
#47350 = CARTESIAN_POINT ( 'NONE',  ( 96.67388729539801773, -35.53787041403403180, 206.2356252759109623 ) ) ;
#47351 = EDGE_LOOP ( 'NONE', ( #72871, #6332 ) ) ;
#47352 = CARTESIAN_POINT ( 'NONE',  ( -487.2989999999999782, 100.8062500000000057, 86.36305401447658880 ) ) ;
#47353 = CARTESIAN_POINT ( 'NONE',  ( 76.06670390244796920, -26.72944715994109899, 239.5838068554169809 ) ) ;
#47354 = DIRECTION ( 'NONE',  ( 1.000000000000000000, 0.000000000000000000, -9.299908063537909262E-17 ) ) ;
#47355 = CARTESIAN_POINT ( 'NONE',  ( 109.0838521367681864, -44.63893190664380484, 45.59380465530593796 ) ) ;
#47356 = CARTESIAN_POINT ( 'NONE',  ( 105.3125989252256147, -48.47411034989094958, 143.4584824187689662 ) ) ;
#47357 = DIRECTION ( 'NONE',  ( 9.351236661543306751E-17, -3.725950533538267725E-29, -1.000000000000000000 ) ) ;
#47358 = ORIENTED_EDGE ( 'NONE', *, *, #75222, .T. ) ;
#47359 = CIRCLE ( 'NONE', #58969, 0.5000000000000004441 ) ;
#47360 = DIRECTION ( 'NONE',  ( 0.000000000000000000, 1.000000000000000000, 0.000000000000000000 ) ) ;
#47361 = CARTESIAN_POINT ( 'NONE',  ( 107.9967959839596148, -46.76990057558159464, 67.65228226674308587 ) ) ;
#47362 = ORIENTED_EDGE ( 'NONE', *, *, #7247, .T. ) ;
#47363 = ORIENTED_EDGE ( 'NONE', *, *, #70425, .F. ) ;
#47364 = DIRECTION ( 'NONE',  ( 0.7071067811869279351, -0.7071067811861670993, 6.612322855863716074E-17 ) ) ;
#47365 = VERTEX_POINT ( 'NONE', #66704 ) ;
#47366 = ORIENTED_EDGE ( 'NONE', *, *, #54256, .F. ) ;
#47367 = DIRECTION ( 'NONE',  ( 0.7071067811865487940, -0.7071067811865463515, 0.000000000000000000 ) ) ;
#47368 = ADVANCED_FACE ( 'NONE', ( #32176 ), #59872, .F. ) ;
#47369 = CARTESIAN_POINT ( 'NONE',  ( 104.5191702102720939, -45.41989400652479958, 61.76003887569697781 ) ) ;
#47370 = CARTESIAN_POINT ( 'NONE',  ( 99.73754448486663193, -29.28411171159743276, 225.6956252759109702 ) ) ;
#47371 = CARTESIAN_POINT ( 'NONE',  ( 117.4047238282099102, -30.98758422922431066, 179.2299109901959753 ) ) ;
#47373 = CARTESIAN_POINT ( 'NONE',  ( 98.44183741489698036, -42.05700530801248505, 7.768006228291934434 ) ) ;
#47372 = CARTESIAN_POINT ( 'NONE',  ( 117.0412664019691391, -35.29711810607562228, 23.94033278884533544 ) ) ;
#47374 = CARTESIAN_POINT ( 'NONE',  ( 41.56648329127398966, -27.57844715994070484, 21.92562527591199739 ) ) ;
#47375 = FACE_OUTER_BOUND ( 'NONE', #42682, .T. ) ;
#47376 = ORIENTED_EDGE ( 'NONE', *, *, #59013, .T. ) ;
#47377 = AXIS2_PLACEMENT_3D ( 'NONE', #61655, #15328, #56639 ) ;
#47378 = CARTESIAN_POINT ( 'NONE',  ( 107.0664832912739399, -36.72944715994095333, 293.6369201390379544 ) ) ;
#47380 = CARTESIAN_POINT ( 'NONE',  ( 116.6462162596975389, -40.95264290462791479, 253.4956252759109532 ) ) ;
#47379 = CIRCLE ( 'NONE', #14027, 0.5000000000000197620 ) ;
#47381 = ORIENTED_EDGE ( 'NONE', *, *, #16992, .F. ) ;
#47383 = EDGE_CURVE ( 'NONE', #29231, #6135, #80371, .T. ) ;
#47382 = AXIS2_PLACEMENT_3D ( 'NONE', #12396, #60524, #33287 ) ;
#47384 = CARTESIAN_POINT ( 'NONE',  ( 108.1817894924016770, -47.09492459897622751, 202.6613395616249704 ) ) ;
#47385 = CARTESIAN_POINT ( 'NONE',  ( 97.81168895331838087, -40.51742574516882200, 287.6356252759109680 ) ) ;
#47386 =( NAMED_UNIT ( * ) SI_UNIT ( $, .STERADIAN. ) SOLID_ANGLE_UNIT ( ) );
#47387 = VECTOR ( 'NONE', #62555, 1000.000000000000000 ) ;
#47388 = CARTESIAN_POINT ( 'NONE',  ( 97.83885977234140796, -40.58323701166357012, 22.64129154176366754 ) ) ;
#47389 = CARTESIAN_POINT ( 'NONE',  ( 115.9957689480958720, -41.40556947845971081, 29.44320292253459215 ) ) ;
#47390 = EDGE_CURVE ( 'NONE', #1937, #30939, #2046, .T. ) ;
#47392 = DIRECTION ( 'NONE',  ( 1.000000000000000000, 0.000000000000000000, 0.000000000000000000 ) ) ;
#47391 = CARTESIAN_POINT ( 'NONE',  ( 115.1992151880701840, -36.11503712634230823, 277.6356252759109680 ) ) ;
#47393 = CARTESIAN_POINT ( 'NONE',  ( 115.7830542439493939, -41.80240532925106578, 174.4064499672970499 ) ) ;
#47394 = DIRECTION ( 'NONE',  ( 0.000000000000000000, 0.000000000000000000, 1.000000000000000000 ) ) ;
#47395 = CARTESIAN_POINT ( 'NONE',  ( 167.2371591254543262, -47.82818131005522844, 249.9678068554149775 ) ) ;
#47396 = ADVANCED_FACE ( 'NONE', ( #800 ), #63470, .T. ) ;
#47397 = LINE ( 'NONE', #34228, #67482 ) ;
#47398 = DIRECTION ( 'NONE',  ( -1.000000000000000000, -4.299999999999999979E-14, -1.000000000000000078E-15 ) ) ;
#47399 = EDGE_CURVE ( 'NONE', #79779, #50718, #351, .T. ) ;
#47400 = DIRECTION ( 'NONE',  ( 0.000000000000000000, 0.000000000000000000, -1.000000000000000000 ) ) ;
#47402 = EDGE_LOOP ( 'NONE', ( #66000, #37932, #57994, #41206 ) ) ;
#47401 = PLANE ( 'NONE',  #63132 ) ;
#47403 = EDGE_CURVE ( 'NONE', #1757, #20886, #12212, .T. ) ;
#47404 = CARTESIAN_POINT ( 'NONE',  ( 136.8151996730028372, -18.82419990105082519, 6.751707299520380623 ) ) ;
#47405 = CARTESIAN_POINT ( 'NONE',  ( 113.1129168750088638, -46.01039980791943407, 223.0480062282919675 ) ) ;
#47406 = CARTESIAN_POINT ( 'NONE',  ( 97.22566771925157525, -31.69632393854739760, 91.96229194257693962 ) ) ;
#47407 = CARTESIAN_POINT ( 'NONE',  ( 115.0881438103696155, -30.00293675228997614, 265.3813395616251682 ) ) ;
#47408 = LINE ( 'NONE', #26539, #29473 ) ;
#47409 = B_SPLINE_CURVE_WITH_KNOTS ( 'NONE', 3,
 ( #54689, #47883, #75625, #13392, #8371, #70143 ),
 .UNSPECIFIED., .F., .F.,
 ( 4, 2, 4 ),
 ( -0.009174681380988100945, -0.004588847231327390468, -7.778521765323606618E-06 ),
 .UNSPECIFIED. ) ;
#47410 = CARTESIAN_POINT ( 'NONE',  ( 83.06670390244796920, -58.35344715994099829, 207.5838068554149913 ) ) ;
#47411 = VECTOR ( 'NONE', #24169, 999.9999999999998863 ) ;
#47413 = DIRECTION ( 'NONE',  ( 2.900000000000000265E-14, -2.000000000000000155E-15, 1.000000000000000000 ) ) ;
#47412 = FACE_OUTER_BOUND ( 'NONE', #13906, .T. ) ;
#47414 = CARTESIAN_POINT ( 'NONE',  ( 134.0664832912740110, -46.72944715994100306, 4.925625275910997303 ) ) ;
#47415 = EDGE_CURVE ( 'NONE', #60807, #72752, #27608, .T. ) ;
#47416 = CARTESIAN_POINT ( 'NONE',  ( 131.5565945955665370, -19.85370728022636655, 2.783021134849384737 ) ) ;
#47417 = CLOSED_SHELL ( 'NONE', ( #26411, #49379, #4472, #71040, #83124, #18139, #47427 ) ) ;
#47418 = EDGE_CURVE ( 'NONE', #40854, #22057, #33979, .T. ) ;
#47419 = ORIENTED_EDGE ( 'NONE', *, *, #88928, .F. ) ;
#47420 = VERTEX_POINT ( 'NONE', #35305 ) ;
#47421 = CARTESIAN_POINT ( 'NONE',  ( 99.32441224009949110, -32.03125536261004669, 125.3028960185529570 ) ) ;
#47423 = ORIENTED_EDGE ( 'NONE', *, *, #261, .T. ) ;
#47422 = CARTESIAN_POINT ( 'NONE',  ( 0.000000000000000000, 184.0000000000000000, 90.32146847885336172 ) ) ;
#47424 = CARTESIAN_POINT ( 'NONE',  ( 108.4173643679176706, -26.73502001125028116, 89.96755253173861888 ) ) ;
#47425 = CARTESIAN_POINT ( 'NONE',  ( 117.5859182825551983, -33.41202194707546624, 125.0575300378149706 ) ) ;
#47426 = FACE_OUTER_BOUND ( 'NONE', #76142, .T. ) ;
#47427 = ADVANCED_FACE ( 'NONE', ( #35757 ), #8066, .F. ) ;
#47428 = CARTESIAN_POINT ( 'NONE',  ( -47.15545942921612266, 92.90828646061743257, 75.16624513914106842 ) ) ;
#47429 = DIRECTION ( 'NONE',  ( 1.000000000000000078E-15, -1.000000000000000000, 0.000000000000000000 ) ) ;
#47430 = CARTESIAN_POINT ( 'NONE',  ( 109.6430121354276963, -46.48008673386306100, 108.7814586096431100 ) ) ;
#47431 = CARTESIAN_POINT ( 'NONE',  ( 97.89279369561084820, -33.33727167892450183, 66.04419670448297097 ) ) ;
#47432 = EDGE_LOOP ( 'NONE', ( #72275, #41529, #77434, #19080, #13109, #4593, #48035, #20407, #37985, #49876, #86898, #69067 ) ) ;
#47433 = ORIENTED_EDGE ( 'NONE', *, *, #37987, .T. ) ;
#47434 = ORIENTED_EDGE ( 'NONE', *, *, #19149, .T. ) ;
#47435 = CARTESIAN_POINT ( 'NONE',  ( 145.3728389244185450, -136.8603515927981107, 247.4879652615099985 ) ) ;
#47437 = DIRECTION ( 'NONE',  ( 0.000000000000000000, 0.000000000000000000, -1.000000000000000000 ) ) ;
#47436 = CARTESIAN_POINT ( 'NONE',  ( 108.2029444874845723, -47.03713394308625340, 153.6518157521009584 ) ) ;
#47438 = CYLINDRICAL_SURFACE ( 'NONE', #79900, 9.999999999999998224 ) ;
#47439 = CARTESIAN_POINT ( 'NONE',  ( 132.2857443282840393, -124.7784471599409102, 55.21780685541800437 ) ) ;
#47440 = CARTESIAN_POINT ( 'NONE',  ( 163.5667039024460223, -18.82844715994111340, -5.074374724088000832 ) ) ;
#47441 = ADVANCED_FACE ( 'NONE', ( #41220 ), #1257, .T. ) ;
#47442 = CARTESIAN_POINT ( 'NONE',  ( 91.81710919847640184, 87.03046781249440755, 75.00112839233788975 ) ) ;
#47443 = CARTESIAN_POINT ( 'NONE',  ( 108.3331690636866256, -46.73489103495947461, 178.6772697487780306 ) ) ;
#47444 = CARTESIAN_POINT ( 'NONE',  ( 113.3016265961370408, -28.35762455946448668, 104.5670538473399347 ) ) ;
#47445 = ORIENTED_EDGE ( 'NONE', *, *, #32031, .F. ) ;
#47446 = VERTEX_POINT ( 'NONE', #42556 ) ;
#47447 = VERTEX_POINT ( 'NONE', #83938 ) ;
#47448 = EDGE_CURVE ( 'NONE', #49158, #28809, #75768, .T. ) ;
#47449 = CARTESIAN_POINT ( 'NONE',  ( 199.3900000000000148, 46.38749999999999574, -38.10000000000000142 ) ) ;
#47450 = AXIS2_PLACEMENT_3D ( 'NONE', #53766, #18373, #79738 ) ;
#47451 = CARTESIAN_POINT ( 'NONE',  ( 183.6524903400783444, -49.32844715993451956, 300.4678068554149490 ) ) ;
#47452 = EDGE_CURVE ( 'NONE', #42257, #34850, #6717, .T. ) ;
#47453 = VECTOR ( 'NONE', #53566, 1000.000000000000000 ) ;
#47454 = DIRECTION ( 'NONE',  ( -0.7071067811865410224, 0.000000000000000000, -0.7071067811865540120 ) ) ;
#47455 = CARTESIAN_POINT ( 'NONE',  ( 99.48373692063242402, -40.90112338471579534, 174.5328522743529618 ) ) ;
#47456 = AXIS2_PLACEMENT_3D ( 'NONE', #26428, #20067, #34576 ) ;
#47457 = AXIS2_PLACEMENT_3D ( 'NONE', #18088, #74409, #12184 ) ;
#47458 = AXIS2_PLACEMENT_3D ( 'NONE', #83806, #54257, #21580 ) ;
#47459 = LINE ( 'NONE', #13413, #79408 ) ;
#47460 = EDGE_LOOP ( 'NONE', ( #10598, #16872, #80229, #816 ) ) ;
#47462 = ORIENTED_EDGE ( 'NONE', *, *, #50284, .F. ) ;
#47461 = EDGE_LOOP ( 'NONE', ( #34298, #42411, #7249, #9814, #9752, #12603, #8664, #25088, #66014, #57791 ) ) ;
#47463 = DIRECTION ( 'NONE',  ( 0.000000000000000000, 0.000000000000000000, -1.000000000000000000 ) ) ;
#47464 = CARTESIAN_POINT ( 'NONE',  ( -20.16291403587278097, 44.76340627898822078, 32.32900225554683260 ) ) ;
#47465 = VERTEX_POINT ( 'NONE', #21707 ) ;
#47466 = ORIENTED_EDGE ( 'NONE', *, *, #72788, .F. ) ;
#47467 = CARTESIAN_POINT ( 'NONE',  ( 77.68755387134090995, -20.11069332325651615, 7.213126773501262967 ) ) ;
#47468 = CARTESIAN_POINT ( 'NONE',  ( 104.6178464025351218, -28.18156397322882967, 221.7301547344689823 ) ) ;
#47469 = AXIS2_PLACEMENT_3D ( 'NONE', #24404, #31195, #46151 ) ;
#47470 = VECTOR ( 'NONE', #57853, 1000.000000000000000 ) ;
#47471 = AXIS2_PLACEMENT_3D ( 'NONE', #33977, #6733, #33097 ) ;
#47472 = LINE ( 'NONE', #12080, #70490 ) ;
#47473 = DIRECTION ( 'NONE',  ( 0.000000000000000000, 0.000000000000000000, 1.000000000000000000 ) ) ;
#47474 = VERTEX_POINT ( 'NONE', #83048 ) ;
#47475 = ORIENTED_EDGE ( 'NONE', *, *, #36298, .F. ) ;
#47476 = PLANE ( 'NONE',  #34777 ) ;
#47477 = VERTEX_POINT ( 'NONE', #49380 ) ;
#47478 = ORIENTED_EDGE ( 'NONE', *, *, #87339, .T. ) ;
#47479 = CARTESIAN_POINT ( 'NONE',  ( 106.4678557813946043, -44.87017016969328864, 220.3366617981629645 ) ) ;
#47480 = CARTESIAN_POINT ( 'NONE',  ( 117.1850550582282580, -34.12927998004249730, 124.0270538473399426 ) ) ;
#47481 = CARTESIAN_POINT ( 'NONE',  ( 116.1047473792920357, -29.10330858331343151, 74.38419670448293175 ) ) ;
#47482 = CARTESIAN_POINT ( 'NONE',  ( 99.61185357976398791, -39.68090676418853491, 249.5838068554173503 ) ) ;
#47483 = CARTESIAN_POINT ( 'NONE',  ( 131.0667039024480118, -61.87844715994100397, 231.5838068554150198 ) ) ;
#47484 = DIRECTION ( 'NONE',  ( -3.100000000000000258E-29, 3.100000000000000044E-14, 1.000000000000000000 ) ) ;
#47485 = CARTESIAN_POINT ( 'NONE',  ( 117.9485099285917613, -34.79154191225799053, 194.9546728949589749 ) ) ;
#47486 = DIRECTION ( 'NONE',  ( 0.9963424814100680926, -0.08544974978095712381, 0.000000000000000000 ) ) ;
#47487 = ORIENTED_EDGE ( 'NONE', *, *, #71938, .T. ) ;
#47488 = CARTESIAN_POINT ( 'NONE',  ( 107.0667039024479834, -36.72944715994100306, 239.5838068554170093 ) ) ;
#47489 = ORIENTED_EDGE ( 'NONE', *, *, #42854, .T. ) ;
#47490 = ORIENTED_EDGE ( 'NONE', *, *, #19220, .F. ) ;
#47491 = CARTESIAN_POINT ( 'NONE',  ( 0.000000000000000000, 93.07500000000001705, 0.000000000000000000 ) ) ;
#47492 = VERTEX_POINT ( 'NONE', #61666 ) ;
#47493 = VECTOR ( 'NONE', #30677, 1000.000000000000000 ) ;
#47494 = CARTESIAN_POINT ( 'NONE',  ( 51.06648329127400388, 12.92155284005902516, 336.6506252759110112 ) ) ;
#47495 = DIRECTION ( 'NONE',  ( -0.8660254037844390407, 0.000000000000000000, -0.4999999999999995004 ) ) ;
#47496 = CARTESIAN_POINT ( 'NONE',  ( 106.0764471815382279, -48.53877882342441552, 112.5099109901969712 ) ) ;
#47497 = CARTESIAN_POINT ( 'NONE',  ( -11.60276384529982430, 77.38453301234325465, 130.0394192264149922 ) ) ;
#47498 = CARTESIAN_POINT ( 'NONE',  ( 136.6005499775789076, -35.66120003907548863, 7.039521718172190745 ) ) ;
#47499 = DIRECTION ( 'NONE',  ( 0.000000000000000000, 0.000000000000000000, 1.000000000000000000 ) ) ;
#47500 = ADVANCED_FACE ( 'NONE', ( #56644 ), #89404, .F. ) ;
#47503 = CARTESIAN_POINT ( 'NONE',  ( 113.2071528006339918, -45.12711609280817271, 224.0784824187679476 ) ) ;
#47502 = CARTESIAN_POINT ( 'NONE',  ( 63.03715912545644784, -24.42818131006026761, 117.4678068554150485 ) ) ;
#47501 = CARTESIAN_POINT ( 'NONE',  ( 101.9936209308341262, -45.44607153293747359, 143.1564586083297286 ) ) ;
#47504 = LINE ( 'NONE', #26630, #69855 ) ;
#47505 = DIRECTION ( 'NONE',  ( 0.000000000000000000, 0.000000000000000000, 1.000000000000000000 ) ) ;
#47506 = ORIENTED_EDGE ( 'NONE', *, *, #60455, .T. ) ;
#47507 = LINE ( 'NONE', #33449, #26650 ) ;
#47508 = ADVANCED_FACE ( 'NONE', ( #13536 ), #41662, .F. ) ;
#47509 = LINE ( 'NONE', #33450, #42771 ) ;
#47510 = FACE_OUTER_BOUND ( 'NONE', #49812, .T. ) ;
#47511 = ADVANCED_FACE ( 'NONE', ( #20799, #34866 ), #28048, .F. ) ;
#47512 = DIRECTION ( 'NONE',  ( 0.000000000000000000, -1.000000000000000000, 0.000000000000000000 ) ) ;
#47514 = ORIENTED_EDGE ( 'NONE', *, *, #3169, .T. ) ;
#47513 = CARTESIAN_POINT ( 'NONE',  ( 105.1026693892091117, -26.44596034844076371, 235.2270538473399313 ) ) ;
#47515 = ADVANCED_FACE ( 'NONE', ( #7619, #41280 ), #48092, .F. ) ;
#47516 = CARTESIAN_POINT ( 'NONE',  ( 103.7740925671131151, -27.25659402154724020, 195.3423308223554784 ) ) ;
#47517 = CARTESIAN_POINT ( 'NONE',  ( 118.1260584382194025, -36.12034675239389259, 269.8822919425776945 ) ) ;
#47518 = CARTESIAN_POINT ( 'NONE',  ( 116.8472425118689841, -43.50793233799721094, 159.3441967044829539 ) ) ;
#47519 = VECTOR ( 'NONE', #79367, 1000.000000000000000 ) ;
#47520 = DIRECTION ( 'NONE',  ( 0.000000000000000000, 0.000000000000000000, 1.000000000000000000 ) ) ;
#47521 = PLANE ( 'NONE',  #38753 ) ;
#47523 = DIRECTION ( 'NONE',  ( 3.100000000000000258E-29, -3.100000000000000044E-14, -1.000000000000000000 ) ) ;
#47522 = LINE ( 'NONE', #82091, #46332 ) ;
#47524 = CARTESIAN_POINT ( 'NONE',  ( 115.8254323939450501, -31.73001883370779552, 189.2397919421528343 ) ) ;
#47525 = DIRECTION ( 'NONE',  ( 1.000000000000000000, 0.000000000000000000, 0.000000000000000000 ) ) ;
#47526 = ORIENTED_EDGE ( 'NONE', *, *, #25131, .T. ) ;
#47527 = EDGE_CURVE ( 'NONE', #49825, #78550, #77571, .T. ) ;
#47528 = AXIS2_PLACEMENT_3D ( 'NONE', #30357, #58054, #87109 ) ;
#47529 = CIRCLE ( 'NONE', #4030, 24.63800000000000168 ) ;
#47530 = EDGE_CURVE ( 'NONE', #46470, #61847, #55353, .T. ) ;
#47531 = ORIENTED_EDGE ( 'NONE', *, *, #10486, .F. ) ;
#47532 = VERTEX_POINT ( 'NONE', #41729 ) ;
#47533 = CIRCLE ( 'NONE', #4036, 1.000000000000000888 ) ;
#47534 = ORIENTED_EDGE ( 'NONE', *, *, #7458, .F. ) ;
#47535 = CARTESIAN_POINT ( 'NONE',  ( 184.5664832912729878, 15.62155284005731204, 361.9756252759109998 ) ) ;
#47536 = CARTESIAN_POINT ( 'NONE',  ( 99.99555918775628527, -44.36035129061379934, 42.98133956162492098 ) ) ;
#47537 = CARTESIAN_POINT ( 'NONE',  ( 70.06029815369576852, -140.3870298840350870, 246.8745206071880034 ) ) ;
#47538 = EDGE_CURVE ( 'NONE', #75765, #59961, #75823, .T. ) ;
#47539 = CIRCLE ( 'NONE', #69350, 4.762500000000001066 ) ;
#47540 = CARTESIAN_POINT ( 'NONE',  ( 173.9900000000000091, 28.98850000000000193, -7.937500000000000000 ) ) ;
#47541 = CIRCLE ( 'NONE', #60570, 2.116999999999993776 ) ;
#47542 = DIRECTION ( 'NONE',  ( 0.000000000000000000, 0.000000000000000000, 1.000000000000000000 ) ) ;
#47543 = AXIS2_PLACEMENT_3D ( 'NONE', #45923, #60005, #67744 ) ;
#47544 = CARTESIAN_POINT ( 'NONE',  ( 113.7727705757230297, -31.39298644294678908, 243.7838483995059562 ) ) ;
#47545 = EDGE_LOOP ( 'NONE', ( #66808, #67458, #62999, #39638 ) ) ;
#47546 = ADVANCED_FACE ( 'NONE', ( #20861 ), #25096, .T. ) ;
#47547 = VERTEX_POINT ( 'NONE', #20422 ) ;
#47548 = ORIENTED_EDGE ( 'NONE', *, *, #57058, .T. ) ;
#47549 = DIRECTION ( 'NONE',  ( 0.000000000000000000, 5.463695987328529395E-16, -1.000000000000000000 ) ) ;
#47550 = CARTESIAN_POINT ( 'NONE',  ( 0.000000000000000000, 92.07499999999998863, 88.90000000000000568 ) ) ;
#47551 = LINE ( 'NONE', #25776, #28093 ) ;
#47552 = DIRECTION ( 'NONE',  ( 0.7071067811865779928, -0.7071067811865171526, 7.071067811865786933E-16 ) ) ;
#47553 = FACE_OUTER_BOUND ( 'NONE', #23396, .T. ) ;
#47554 = DIRECTION ( 'NONE',  ( 1.000000000000000078E-15, -1.000000000000000083E-30, -1.000000000000000000 ) ) ;
#47555 = CARTESIAN_POINT ( 'NONE',  ( 99.81116105471912192, -29.32005551970541291, 270.7051490854354938 ) ) ;
#47556 = CARTESIAN_POINT ( 'NONE',  ( 172.5664832912740110, 0.2215528400590013880, 78.92562527591199739 ) ) ;
#47557 = VERTEX_POINT ( 'NONE', #69464 ) ;
#47558 = EDGE_CURVE ( 'NONE', #36904, #28057, #49998, .T. ) ;
#47559 = DIRECTION ( 'NONE',  ( 1.000000000000000078E-15, -1.000000000000000083E-30, -1.000000000000000000 ) ) ;
#47560 = ADVANCED_FACE ( 'NONE', ( #27674 ), #87333, .F. ) ;
#47561 = CARTESIAN_POINT ( 'NONE',  ( 131.3164832912740110, -36.72944715994100306, 6.749768910606454675 ) ) ;
#47562 = CARTESIAN_POINT ( 'NONE',  ( 99.60924227704973077, -33.40991670024246218, 98.81094751244894780 ) ) ;
#47563 = PLANE ( 'NONE',  #69707 ) ;
#47564 = CARTESIAN_POINT ( 'NONE',  ( 213.7409999999999854, 52.73749999999999716, -44.45000000000000284 ) ) ;
#47565 = PLANE ( 'NONE',  #85179 ) ;
#47566 = EDGE_LOOP ( 'NONE', ( #64520, #80003 ) ) ;
#47567 = CARTESIAN_POINT ( 'NONE',  ( 77.96454488115681158, -34.94667115355367315, 7.474641677900894621 ) ) ;
#47568 = ORIENTED_EDGE ( 'NONE', *, *, #5094, .F. ) ;
#47569 = CARTESIAN_POINT ( 'NONE',  ( 108.6487477603288170, -25.79654920012707109, 149.9737205140059473 ) ) ;
#47570 = EDGE_LOOP ( 'NONE', ( #47743, #28456 ) ) ;
#47571 = CARTESIAN_POINT ( 'NONE',  ( 98.06038178923066084, -41.07745101822689548, 87.68391174719410230 ) ) ;
#47572 = CARTESIAN_POINT ( 'NONE',  ( 115.6007127221643032, -39.11591036577164004, 95.04158330589696391 ) ) ;
#47573 = PLANE ( 'NONE',  #70614 ) ;
#47574 = VECTOR ( 'NONE', #37697, 1000.000000000000000 ) ;
#47575 = CARTESIAN_POINT ( 'NONE',  ( 74.67117555236049498, -69.13001345503671757, 247.4595024958179863 ) ) ;
#47576 = CARTESIAN_POINT ( 'NONE',  ( 98.57234554589554421, -43.83823254894062416, 67.86895860924497015 ) ) ;
#47577 = EDGE_CURVE ( 'NONE', #27248, #21233, #31905, .T. ) ;
#47578 = DIRECTION ( 'NONE',  ( 0.7071067811987160612, 0.7071067811743789733, 0.000000000000000000 ) ) ;
#47579 = ORIENTED_EDGE ( 'NONE', *, *, #36522, .F. ) ;
#47580 = CIRCLE ( 'NONE', #63556, 15.69999999999999574 ) ;
#47581 = DIRECTION ( 'NONE',  ( 0.000000000000000000, 0.000000000000000000, 1.000000000000000000 ) ) ;
#47582 = EDGE_LOOP ( 'NONE', ( #41539, #3792 ) ) ;
#47583 = ORIENTED_EDGE ( 'NONE', *, *, #41558, .T. ) ;
#47584 = VECTOR ( 'NONE', #71516, 1000.000000000000000 ) ;
#47585 = DIRECTION ( 'NONE',  ( 1.000000000000000000, -3.885780586187990841E-13, 0.000000000000000000 ) ) ;
#47586 = ORIENTED_EDGE ( 'NONE', *, *, #80633, .F. ) ;
#47587 = CARTESIAN_POINT ( 'NONE',  ( 101.6507727546967175, -27.01955209951621129, 255.4813395616254468 ) ) ;
#47588 = CARTESIAN_POINT ( 'NONE',  ( 114.2549023322775383, -45.16142510923258868, 149.1508633711489722 ) ) ;
#47589 = CARTESIAN_POINT ( 'NONE',  ( 25.56670390244797275, -67.87844715994100397, 288.3428068554150059 ) ) ;
#47590 = CARTESIAN_POINT ( 'NONE',  ( 115.8254323921544682, -31.73001882933136741, 140.2397919425295356 ) ) ;
#47591 = CARTESIAN_POINT ( 'NONE',  ( 117.3387810265436144, -32.64853063025485369, 95.13943479972097350 ) ) ;
#47592 = DIRECTION ( 'NONE',  ( 0.000000000000000000, 0.000000000000000000, 1.000000000000000000 ) ) ;
#47593 = VERTEX_POINT ( 'NONE', #21311 ) ;
#47594 = AXIS2_PLACEMENT_3D ( 'NONE', #79041, #17254, #3611 ) ;
#47595 = DIRECTION ( 'NONE',  ( 3.100000000000000258E-29, -3.100000000000000044E-14, -1.000000000000000000 ) ) ;
#47596 = VECTOR ( 'NONE', #53009, 1000.000000000000000 ) ;
#47597 = VECTOR ( 'NONE', #1854, 1000.000000000000114 ) ;
#47598 = LINE ( 'NONE', #53953, #56367 ) ;
#47600 = VERTEX_POINT ( 'NONE', #89923 ) ;
#47599 = ADVANCED_FACE ( 'NONE', ( #47196 ), #68821, .T. ) ;
#47601 = DIRECTION ( 'NONE',  ( 0.000000000000000000, 0.4999999999999998890, 0.8660254037844387076 ) ) ;
#47602 = DIRECTION ( 'NONE',  ( -1.000000000000000078E-15, 1.000000000000000083E-30, 1.000000000000000000 ) ) ;
#47603 = CARTESIAN_POINT ( 'NONE',  ( 96.58568816239599641, -40.17018292043295702, 286.5908633711491120 ) ) ;
#47604 = DIRECTION ( 'NONE',  ( 1.000000000000000000, 0.000000000000000000, 0.000000000000000000 ) ) ;
#47605 = ADVANCED_FACE ( 'NONE', ( #5896 ), #61286, .F. ) ;
#47606 = FACE_OUTER_BOUND ( 'NONE', #42195, .T. ) ;
#47607 = DIRECTION ( 'NONE',  ( 1.000000000000000000, 0.000000000000000000, 2.108231265501709878E-16 ) ) ;
#47608 = ADVANCED_FACE ( 'NONE', ( #76271, #11014, #80523 ), #14048, .F. ) ;
#47609 = CARTESIAN_POINT ( 'NONE',  ( 110.8002668817294847, -46.40403677370081681, 17.85753003781598380 ) ) ;
#47611 = CARTESIAN_POINT ( 'NONE',  ( 114.0662423116485229, -44.47333502991302367, 129.1613395616249704 ) ) ;
#47610 = DIRECTION ( 'NONE',  ( 0.000000000000000000, -1.000000000000000000, 0.000000000000000000 ) ) ;
#47612 = DIRECTION ( 'NONE',  ( -8.503806984168940141E-16, 0.000000000000000000, 1.000000000000000000 ) ) ;
#47613 = CARTESIAN_POINT ( 'NONE',  ( 99.06758658495417080, -45.54097539030503583, 156.9899109901969609 ) ) ;
#47614 = CARTESIAN_POINT ( 'NONE',  ( 182.5667039024459939, -22.48495420874030515, 342.9256252759109884 ) ) ;
#47615 = EDGE_LOOP ( 'NONE', ( #54015, #359 ) ) ;
#47616 = AXIS2_PLACEMENT_3D ( 'NONE', #67265, #12314, #59544 ) ;
#47617 = CARTESIAN_POINT ( 'NONE',  ( 92.81932083335591699, -95.00417761012948858, -11.78219314458228695 ) ) ;
#47618 = EDGE_CURVE ( 'NONE', #66479, #77917, #16543, .T. ) ;
#47619 = CARTESIAN_POINT ( 'NONE',  ( 51.56670390244799762, -33.35206098992650681, 237.4678068554150059 ) ) ;
#47620 = CARTESIAN_POINT ( 'NONE',  ( 136.2777084067157887, -35.08426318374723962, 2.472582314376420953 ) ) ;
#47621 = ORIENTED_EDGE ( 'NONE', *, *, #24977, .F. ) ;
#47622 = CARTESIAN_POINT ( 'NONE',  ( 102.0686427141774999, -27.96957108712200224, 61.48992525579068058 ) ) ;
#47623 = EDGE_CURVE ( 'NONE', #21126, #3091, #83544, .T. ) ;
#47625 = EDGE_LOOP ( 'NONE', ( #76325, #53569 ) ) ;
#47624 = CARTESIAN_POINT ( 'NONE',  ( 105.7147172347987407, -24.90567422487873017, 160.1670538473389627 ) ) ;
#47626 = CARTESIAN_POINT ( 'NONE',  ( 71.25580610988301089, -82.12815647064930147, 542.9756252759101471 ) ) ;
#47627 = CARTESIAN_POINT ( 'NONE',  ( -129.9989688714893248, 86.64186789594789673, -12.05153810119486124 ) ) ;
#47628 = VECTOR ( 'NONE', #42217, 1000.000000000000000 ) ;
#47629 = CARTESIAN_POINT ( 'NONE',  ( 31.71315051186898870, -31.94127993907790852, 342.9256252759119548 ) ) ;
#47630 = AXIS2_PLACEMENT_3D ( 'NONE', #50395, #30418, #78140 ) ;
#47631 = DIRECTION ( 'NONE',  ( 0.000000000000000000, 0.000000000000000000, 1.000000000000000000 ) ) ;
#47632 = ORIENTED_EDGE ( 'NONE', *, *, #50272, .T. ) ;
#47633 = EDGE_CURVE ( 'NONE', #49139, #30320, #47650, .T. ) ;
#47634 = ORIENTED_EDGE ( 'NONE', *, *, #49877, .T. ) ;
#47635 = EDGE_CURVE ( 'NONE', #80549, #40328, #12712, .T. ) ;
#47636 = EDGE_LOOP ( 'NONE', ( #64378, #71766, #70622, #29400 ) ) ;
#47637 = ORIENTED_EDGE ( 'NONE', *, *, #59716, .T. ) ;
#47638 = FACE_OUTER_BOUND ( 'NONE', #77858, .T. ) ;
#47639 = CARTESIAN_POINT ( 'NONE',  ( 89.95770503246907879, 94.82199753261677699, -94.61838531165687982 ) ) ;
#47640 = CYLINDRICAL_SURFACE ( 'NONE', #9180, 9.999999999999998224 ) ;
#47641 = DIRECTION ( 'NONE',  ( -1.000000000000000000, -2.756263715554006823E-15, 0.000000000000000000 ) ) ;
#47642 = AXIS2_PLACEMENT_3D ( 'NONE', #48839, #35680, #7537 ) ;
#47644 = CARTESIAN_POINT ( 'NONE',  ( 213.7409999999999854, 52.73749999999999716, -51.09754249571540186 ) ) ;
#47643 = CARTESIAN_POINT ( 'NONE',  ( 97.06107716906868177, -37.99644359145901973, 106.4272944573947370 ) ) ;
#47645 = CARTESIAN_POINT ( 'NONE',  ( 97.78492648218951899, -40.45146748447449170, 181.6299604809356936 ) ) ;
#47646 = ORIENTED_EDGE ( 'NONE', *, *, #81057, .T. ) ;
#47647 = AXIS2_PLACEMENT_3D ( 'NONE', #65967, #60039, #17830 ) ;
#47649 = ORIENTED_EDGE ( 'NONE', *, *, #41401, .T. ) ;
#47648 = VECTOR ( 'NONE', #113, 1000.000000000000000 ) ;
#47650 = LINE ( 'NONE', #38719, #10842 ) ;
#47651 = DIRECTION ( 'NONE',  ( 1.000000000000000000, 4.299999999999999979E-14, 1.000000000000000078E-15 ) ) ;
#47652 = BREP_WITH_VOIDS ( 'NONE', #61879, ( #53332 ) );
#47653 = CARTESIAN_POINT ( 'NONE',  ( 115.3120223323505940, -44.18753462406601074, 229.2413395616249545 ) ) ;
#47655 = ORIENTED_EDGE ( 'NONE', *, *, #5558, .T. ) ;
#47654 = CARTESIAN_POINT ( 'NONE',  ( 107.0664832912750057, -36.72944715993903486, 4.925625275910970657 ) ) ;
#47656 = VECTOR ( 'NONE', #56746, 1000.000000000000000 ) ;
#47657 = CARTESIAN_POINT ( 'NONE',  ( 109.1197153606379828, -46.32621810461552059, 103.7441967044819791 ) ) ;
#47658 = DIRECTION ( 'NONE',  ( -3.100000000000000258E-29, 3.100000000000000044E-14, 1.000000000000000000 ) ) ;
#47659 = CARTESIAN_POINT ( 'NONE',  ( 69.95929469538076262, -138.0461895383713795, 247.6591799766680140 ) ) ;
#47660 = AXIS2_PLACEMENT_3D ( 'NONE', #2677, #43537, #71280 ) ;
#47661 = CARTESIAN_POINT ( 'NONE',  ( 97.39131739028603363, -39.27861223437267313, 22.53144478254995420 ) ) ;
#47662 = ORIENTED_EDGE ( 'NONE', *, *, #48565, .T. ) ;
#47663 = DIRECTION ( 'NONE',  ( 0.000000000000000000, 0.000000000000000000, -1.000000000000000000 ) ) ;
#47664 = VECTOR ( 'NONE', #27092, 1000.000000000000000 ) ;
#47665 = ORIENTED_EDGE ( 'NONE', *, *, #82236, .F. ) ;
#47666 = EDGE_LOOP ( 'NONE', ( #71325, #77194 ) ) ;
#47667 = EDGE_CURVE ( 'NONE', #44045, #70380, #89182, .T. ) ;
#47668 = CARTESIAN_POINT ( 'NONE',  ( 115.7948931938460362, -35.19871557519451954, 240.3958690201829427 ) ) ;
#47669 = CARTESIAN_POINT ( 'NONE',  ( 50.88849390559460062, -32.11662333284566273, 313.9678068554150059 ) ) ;
#47670 = CARTESIAN_POINT ( 'NONE',  ( -118.0058645681207281, 88.18374315479978520, 11.41243735079867250 ) ) ;
#47671 = CARTESIAN_POINT ( 'NONE',  ( 97.81170668756638520, -40.51744870325870806, 152.6352702516163902 ) ) ;
#47672 = VECTOR ( 'NONE', #33095, 1000.000000000000114 ) ;
#47673 = LINE ( 'NONE', #19086, #83615 ) ;
#47674 = ORIENTED_EDGE ( 'NONE', *, *, #20873, .T. ) ;
#47675 = CARTESIAN_POINT ( 'NONE',  ( 1.793207055312195196E-22, 69.95000000000000284, 118.5560000000000116 ) ) ;
#47676 = CARTESIAN_POINT ( 'NONE',  ( 108.3318564647012607, -46.73503994553699670, 183.6777181701287418 ) ) ;
#47677 = ORIENTED_EDGE ( 'NONE', *, *, #83027, .F. ) ;
#47678 = CARTESIAN_POINT ( 'NONE',  ( 114.8195649486642225, -43.69914982757761379, 38.24419670448192221 ) ) ;
#47679 = ORIENTED_EDGE ( 'NONE', *, *, #36211, .F. ) ;
#47680 = CARTESIAN_POINT ( 'NONE',  ( 116.1392960594047850, -38.67366927644074082, 256.4766617981626382 ) ) ;
#47681 = LINE ( 'NONE', #75416, #57593 ) ;
#47682 = CARTESIAN_POINT ( 'NONE',  ( 103.1701080265564485, -27.72257962874988024, 155.4013395616259743 ) ) ;
#47683 = CARTESIAN_POINT ( 'NONE',  ( 23.74957699733089100, 81.92546328272709388, 307.6268863596367851 ) ) ;
#47684 = CARTESIAN_POINT ( 'NONE',  ( -240.5296158183964792, 14.28750000000026077, 6.349999999999710099 ) ) ;
#47685 = CARTESIAN_POINT ( 'NONE',  ( 97.81170212845945855, -40.51743756719207568, 176.6354241348688277 ) ) ;
#47686 = CARTESIAN_POINT ( 'NONE',  ( 9.673933672768200154, 74.31810048158574489, 130.1973409905385495 ) ) ;
#47687 = CARTESIAN_POINT ( 'NONE',  ( 96.97452011921430426, -33.94641660286638540, 247.1127681330539758 ) ) ;
#47688 = DIRECTION ( 'NONE',  ( 0.000000000000000000, 1.000000000000000000, 0.000000000000000000 ) ) ;
#47689 = VERTEX_POINT ( 'NONE', #29026 ) ;
#47690 = EDGE_CURVE ( 'NONE', #5064, #82741, #43074, .T. ) ;
#47691 = CARTESIAN_POINT ( 'NONE',  ( 98.42032043187158763, -42.69450228079005427, 122.8070538473389490 ) ) ;
#47692 = CARTESIAN_POINT ( 'NONE',  ( 122.9163323945412998, 44.80836990040677392, -44.00586793101803806 ) ) ;
#47693 = VERTEX_POINT ( 'NONE', #9040 ) ;
#47694 = VERTEX_POINT ( 'NONE', #70356 ) ;
#47695 = ORIENTED_EDGE ( 'NONE', *, *, #1527, .T. ) ;
#47696 = PLANE ( 'NONE',  #41948 ) ;
#47697 = CARTESIAN_POINT ( 'NONE',  ( 51.06670390244899238, -32.29483332968430886, -5.074374724088000832 ) ) ;
#47698 = CARTESIAN_POINT ( 'NONE',  ( 164.9667039024476765, -28.27351298636832055, 193.9678068554149775 ) ) ;
#47699 = LINE ( 'NONE', #40453, #33049 ) ;
#47700 = CARTESIAN_POINT ( 'NONE',  ( 111.5401709588312116, -43.55702686802507628, 175.8566617981629463 ) ) ;
#47701 = CARTESIAN_POINT ( 'NONE',  ( 100.2339645716073164, -28.82666620644582522, 256.6441967044821695 ) ) ;
#47702 = CARTESIAN_POINT ( 'NONE',  ( 115.7817526725759336, -41.80460064089260896, 59.40624582981430279 ) ) ;
#47703 = ORIENTED_EDGE ( 'NONE', *, *, #47004, .F. ) ;
#47704 = CARTESIAN_POINT ( 'NONE',  ( 130.2060295542615904, 90.93932679091003024, 9.571439627455211152 ) ) ;
#47705 = VECTOR ( 'NONE', #51421, 1000.000000000000000 ) ;
#47706 = CARTESIAN_POINT ( 'NONE',  ( 38.10000000000000142, 69.84999999999999432, 283.4005000000000223 ) ) ;
#47707 = ORIENTED_EDGE ( 'NONE', *, *, #20989, .T. ) ;
#47708 = ORIENTED_EDGE ( 'NONE', *, *, #87304, .F. ) ;
#47709 = AXIS2_PLACEMENT_3D ( 'NONE', #76273, #36286, #57615 ) ;
#47710 = CIRCLE ( 'NONE', #79655, 0.5000000000000004441 ) ;
#47711 = DIRECTION ( 'NONE',  ( -1.000000000000000000, 0.000000000000000000, 7.043400939473319300E-33 ) ) ;
#47712 = ORIENTED_EDGE ( 'NONE', *, *, #1802, .T. ) ;
#47713 = ORIENTED_EDGE ( 'NONE', *, *, #80788, .F. ) ;
#47714 = CARTESIAN_POINT ( 'NONE',  ( 131.0667039024480118, -43.72944715994093201, 231.5838068554170093 ) ) ;
#47715 = CARTESIAN_POINT ( 'NONE',  ( 20.03715912545639100, -24.42818131006202265, 180.4678068554150911 ) ) ;
#47716 = DIRECTION ( 'NONE',  ( 1.000000000000000000, 3.999999999999999995E-14, 1.000000000000000078E-15 ) ) ;
#47717 = CYLINDRICAL_SURFACE ( 'NONE', #9811, 0.5000000000000129896 ) ;
#47718 = EDGE_CURVE ( 'NONE', #49481, #47446, #36285, .T. ) ;
#47719 = CARTESIAN_POINT ( 'NONE',  ( 99.99456525420680464, -31.07253584695887483, 195.2000388756959808 ) ) ;
#47720 = CARTESIAN_POINT ( 'NONE',  ( 115.7096504343579539, -43.69425479293489900, 43.27467289495795200 ) ) ;
#47721 = ORIENTED_EDGE ( 'NONE', *, *, #6679, .F. ) ;
#47722 = CARTESIAN_POINT ( 'NONE',  ( 173.9900000000000091, 101.5999999999999943, -131.6533725204182019 ) ) ;
#47723 = ORIENTED_EDGE ( 'NONE', *, *, #40845, .T. ) ;
#47724 = VECTOR ( 'NONE', #84155, 1000.000000000000000 ) ;
#47725 = EDGE_CURVE ( 'NONE', #593, #6607, #31137, .T. ) ;
#47726 = CARTESIAN_POINT ( 'NONE',  ( -86.13269706310892104, 70.27900073646854651, -81.46681417397479663 ) ) ;
#47727 = ADVANCED_FACE ( 'NONE', ( #56711 ), #63082, .T. ) ;
#47728 = EDGE_LOOP ( 'NONE', ( #33576, #66242 ) ) ;
#47729 = CARTESIAN_POINT ( 'NONE',  ( 19.56648329127303043, 25.62155284005700295, 361.9756252759109998 ) ) ;
#47730 = EDGE_CURVE ( 'NONE', #39083, #2908, #7680, .T. ) ;
#47731 = ORIENTED_EDGE ( 'NONE', *, *, #22014, .T. ) ;
#47732 = LINE ( 'NONE', #68647, #18948 ) ;
#47733 = CARTESIAN_POINT ( 'NONE',  ( -9.497924344318278145, 74.22888403371547383, 118.1764031952407663 ) ) ;
#47734 = DIRECTION ( 'NONE',  ( -0.7071067811865410224, 0.000000000000000000, -0.7071067811865540120 ) ) ;
#47735 = CARTESIAN_POINT ( 'NONE',  ( 158.0667039024469886, -67.87844715994090450, 155.2178068554179902 ) ) ;
#47736 = ORIENTED_EDGE ( 'NONE', *, *, #26118, .T. ) ;
#47737 = EDGE_CURVE ( 'NONE', #69807, #914, #63997, .T. ) ;
#47738 = CARTESIAN_POINT ( 'NONE',  ( 106.5169308145888607, -25.66629059357601506, 45.12800622829193742 ) ) ;
#47740 = DIRECTION ( 'NONE',  ( 0.000000000000000000, 0.000000000000000000, 1.000000000000000000 ) ) ;
#47739 = CARTESIAN_POINT ( 'NONE',  ( 172.5664832912740110, -9.303447159940999356, 256.8086252759120498 ) ) ;
#47741 = CARTESIAN_POINT ( 'NONE',  ( 97.33784347520764868, -34.07105638201832676, 147.1152944329917887 ) ) ;
#47742 = CARTESIAN_POINT ( 'NONE',  ( -4.442790029898877613, 70.75203571141577186, 118.2732005548771070 ) ) ;
#47743 = ORIENTED_EDGE ( 'NONE', *, *, #37824, .T. ) ;
#47744 = EDGE_CURVE ( 'NONE', #82504, #51804, #78084, .T. ) ;
#47745 = VECTOR ( 'NONE', #27738, 1000.000000000000000 ) ;
#47746 = DIRECTION ( 'NONE',  ( -9.073094938289460781E-13, -1.000000000000000000, 0.000000000000000000 ) ) ;
#47747 = DIRECTION ( 'NONE',  ( -0.7071067811865473507, -0.7071067811865477948, 0.000000000000000000 ) ) ;
#47748 = CARTESIAN_POINT ( 'NONE',  ( 12.61759658107631665, 80.88542946572127335, 117.8827710199055048 ) ) ;
#47749 = ORIENTED_EDGE ( 'NONE', *, *, #83046, .F. ) ;
#47750 = CARTESIAN_POINT ( 'NONE',  ( 102.5487710710870033, -27.30991770518087591, 91.43276813305395478 ) ) ;
#47752 = CYLINDRICAL_SURFACE ( 'NONE', #47073, 2.500000000000002220 ) ;
#47751 = CARTESIAN_POINT ( 'NONE',  ( 61.00843881761244347, 49.07499999999999574, -33.74458626278666884 ) ) ;
#47753 = PLANE ( 'NONE',  #75517 ) ;
#47754 = CIRCLE ( 'NONE', #56441, 3.249999999999975131 ) ;
#47755 = CARTESIAN_POINT ( 'NONE',  ( 51.23005224011641445, -33.89581943344366977, 117.4678068554150485 ) ) ;
#47756 = ORIENTED_EDGE ( 'NONE', *, *, #72500, .T. ) ;
#47757 = CARTESIAN_POINT ( 'NONE',  ( 96.70615320395842218, -37.17927570127480408, 112.3489586092439652 ) ) ;
#47759 = ORIENTED_EDGE ( 'NONE', *, *, #58191, .T. ) ;
#47758 = CARTESIAN_POINT ( 'NONE',  ( 10.54753116919433964, 89.62386675693470295, 130.1292385957734155 ) ) ;
#47760 = CARTESIAN_POINT ( 'NONE',  ( 110.9847977634195928, -46.36662828626490551, 278.8841967044824059 ) ) ;
#47761 = DIRECTION ( 'NONE',  ( 0.000000000000000000, 0.000000000000000000, 1.000000000000000000 ) ) ;
#47762 = CARTESIAN_POINT ( 'NONE',  ( 107.0664832912749915, -36.72944715993903486, 25.56312527591096995 ) ) ;
#47763 = DIRECTION ( 'NONE',  ( 0.000000000000000000, 0.000000000000000000, -1.000000000000000000 ) ) ;
#47764 = DIRECTION ( 'NONE',  ( 0.7071067811865477948, -0.7071067811865473507, 0.000000000000000000 ) ) ;
#47765 = VECTOR ( 'NONE', #17277, 1000.000000000000000 ) ;
#47766 = CARTESIAN_POINT ( 'NONE',  ( 152.4532657509292335, -72.54478064608022692, 394.9756252759102040 ) ) ;
#47767 = DIRECTION ( 'NONE',  ( -1.000000000000000078E-15, 1.000000000000000083E-30, 1.000000000000000000 ) ) ;
#47768 = CARTESIAN_POINT ( 'NONE',  ( 115.8019334949658798, -41.12891815432281817, 203.4556252759109611 ) ) ;
#47769 = EDGE_LOOP ( 'NONE', ( #44586, #5383, #5051, #58119 ) ) ;
#47770 = ORIENTED_EDGE ( 'NONE', *, *, #74708, .F. ) ;
#47771 = EDGE_CURVE ( 'NONE', #75678, #33892, #57199, .T. ) ;
#47772 = CIRCLE ( 'NONE', #39091, 2.500000000000002220 ) ;
#47773 = CARTESIAN_POINT ( 'NONE',  ( 113.5614835896806625, -43.51851901557028413, 109.6034880678019618 ) ) ;
#47774 = AXIS2_PLACEMENT_3D ( 'NONE', #19669, #12872, #67817 ) ;
#47775 = LINE ( 'NONE', #34152, #69012 ) ;
#47777 = CARTESIAN_POINT ( 'NONE',  ( 248.6659999999999968, 52.73749999999999716, -2.903194600000015502 ) ) ;
#47776 = CARTESIAN_POINT ( 'NONE',  ( 116.3159835831961857, -41.41832011455023377, 244.4651490854349731 ) ) ;
#47778 = DIRECTION ( 'NONE',  ( 0.1811243268507098381, -0.9834602067307437467, 0.000000000000000000 ) ) ;
#47779 = ADVANCED_FACE ( 'NONE', ( #23127, #50799 ), #58064, .F. ) ;
#47780 = CARTESIAN_POINT ( 'NONE',  ( 142.8679068202682458, 10.65431904611001634, 540.9756252759101471 ) ) ;
#47781 = AXIS2_PLACEMENT_3D ( 'NONE', #2037, #15217, #78358 ) ;
#47782 = LINE ( 'NONE', #11497, #11036 ) ;
#47783 = CARTESIAN_POINT ( 'NONE',  ( 97.07207205789896420, -35.37844120677264215, 107.2189586098578076 ) ) ;
#47784 = CARTESIAN_POINT ( 'NONE',  ( 20.03715912545645850, -24.95799193693202156, 129.9678068554150627 ) ) ;
#47785 = CARTESIAN_POINT ( 'NONE',  ( 114.1099639442526268, -29.07320488188160823, 199.4841967044819739 ) ) ;
#47786 = PLANE ( 'NONE',  #32964 ) ;
#47787 = VERTEX_POINT ( 'NONE', #16294 ) ;
#47788 = ORIENTED_EDGE ( 'NONE', *, *, #83162, .F. ) ;
#47789 = CARTESIAN_POINT ( 'NONE',  ( -100.5877059554739361, 79.26455342200334542, -83.22858459372935158 ) ) ;
#47790 = DIRECTION ( 'NONE',  ( 0.000000000000000000, 1.000000000000000000, 0.000000000000000000 ) ) ;
#47791 = CARTESIAN_POINT ( 'NONE',  ( 97.81151477712479902, -40.51751189930152464, 186.6359914586728337 ) ) ;
#47792 = CARTESIAN_POINT ( 'NONE',  ( -47.08824421440486674, 65.65858298468711496, 108.8036001757373299 ) ) ;
#47793 = CARTESIAN_POINT ( 'NONE',  ( 116.3212776292296127, -32.94146857471318413, 287.6356252759109680 ) ) ;
#47794 = ORIENTED_EDGE ( 'NONE', *, *, #42428, .T. ) ;
#47795 = EDGE_CURVE ( 'NONE', #54206, #51053, #28561, .T. ) ;
#47796 = CARTESIAN_POINT ( 'NONE',  ( -9.196775925256822859, 91.17253193803733780, 117.9985040796144915 ) ) ;
#47797 = VECTOR ( 'NONE', #31908, 1000.000000000000000 ) ;
#47798 = CARTESIAN_POINT ( 'NONE',  ( 96.68196755257399388, -35.80810936406337674, 231.2556252759109725 ) ) ;
#47799 = EDGE_LOOP ( 'NONE', ( #38680, #69381 ) ) ;
#47800 = AXIS2_PLACEMENT_3D ( 'NONE', #21727, #20383, #49399 ) ;
#47801 = CARTESIAN_POINT ( 'NONE',  ( 142.8698897858160706, -0.9167816978817300289, 394.9756252759102040 ) ) ;
#47802 = CARTESIAN_POINT ( 'NONE',  ( 70.56670390244700286, -67.87844715994098976, 180.4678068554179902 ) ) ;
#47803 = CARTESIAN_POINT ( 'NONE',  ( 110.8540353023265510, -45.98441608387823720, 167.8855877171093027 ) ) ;
#47804 = CARTESIAN_POINT ( 'NONE',  ( 102.2720406957515991, -30.12315877573194101, 73.39380465530592801 ) ) ;
#47805 = CARTESIAN_POINT ( 'NONE',  ( 113.6278897941700876, -45.65318799257786964, 179.0689586092439640 ) ) ;
#47806 = DIRECTION ( 'NONE',  ( 1.000000000000000078E-15, 1.000000000000000083E-30, -1.000000000000000000 ) ) ;
#47807 = ORIENTED_EDGE ( 'NONE', *, *, #78800, .F. ) ;
#47808 = CARTESIAN_POINT ( 'NONE',  ( 241.3336515812914911, 65.43750000000000000, -2.032000000000000028 ) ) ;
#47809 = VECTOR ( 'NONE', #81456, 1000.000000000000000 ) ;
#47810 = CARTESIAN_POINT ( 'NONE',  ( 98.51277055016676343, -41.91915478865436739, 66.76116378984684729 ) ) ;
#47811 = ORIENTED_EDGE ( 'NONE', *, *, #83914, .T. ) ;
#47812 = VERTEX_POINT ( 'NONE', #49442 ) ;
#47813 = CARTESIAN_POINT ( 'NONE',  ( 9.270368442002547837, 91.24032474172571483, 118.1933656790130129 ) ) ;
#47814 = ORIENTED_EDGE ( 'NONE', *, *, #67623, .F. ) ;
#47815 = ORIENTED_EDGE ( 'NONE', *, *, #18951, .T. ) ;
#47816 = LINE ( 'NONE', #55068, #3383 ) ;
#47817 = ADVANCED_FACE ( 'NONE', ( #77177 ), #11249, .F. ) ;
#47818 = CARTESIAN_POINT ( 'NONE',  ( 98.75426529987753099, -33.13504840779251737, 60.43622935188691514 ) ) ;
#47819 = CARTESIAN_POINT ( 'NONE',  ( 111.1360948925329808, -27.10735667079447353, 244.7584824187679544 ) ) ;
#47820 = AXIS2_PLACEMENT_3D ( 'NONE', #68696, #59616, #75513 ) ;
#47821 = CARTESIAN_POINT ( 'NONE',  ( 115.4997179687694882, -29.61999039777954579, 224.3718157521009573 ) ) ;
#47823 = CARTESIAN_POINT ( 'NONE',  ( 99.16013801855510224, -43.49098322490559809, 27.88991099019694175 ) ) ;
#47822 = DIRECTION ( 'NONE',  ( 0.000000000000000000, 0.000000000000000000, 1.000000000000000000 ) ) ;
#47824 = CARTESIAN_POINT ( 'NONE',  ( 71.77848634863140376, 120.6499999999999915, -77.39114642429929347 ) ) ;
#47825 = LINE ( 'NONE', #49167, #3498 ) ;
#47826 = EDGE_CURVE ( 'NONE', #41907, #17571, #65331, .T. ) ;
#47827 = DIRECTION ( 'NONE',  ( 0.000000000000000000, -1.000000000000000000, 0.000000000000000000 ) ) ;
#47828 = AXIS2_PLACEMENT_3D ( 'NONE', #13366, #54214, #41053 ) ;
#47829 = ORIENTED_EDGE ( 'NONE', *, *, #54065, .T. ) ;
#47830 = ORIENTED_EDGE ( 'NONE', *, *, #28833, .F. ) ;
#47831 = AXIS2_PLACEMENT_3D ( 'NONE', #25841, #27624, #20816 ) ;
#47832 = CARTESIAN_POINT ( 'NONE',  ( 106.8551140066829817, -47.84553036069068099, 77.56133956162591403 ) ) ;
#47833 = CARTESIAN_POINT ( 'NONE',  ( 97.22485937713641135, -31.59570365635885736, 90.93181575210196854 ) ) ;
#47834 = CARTESIAN_POINT ( 'NONE',  ( 100.8220609092773117, -45.17687181127147511, 257.0699109901966608 ) ) ;
#47835 = EDGE_LOOP ( 'NONE', ( #27927, #40921 ) ) ;
#47836 = CARTESIAN_POINT ( 'NONE',  ( 109.3369124252947557, -26.55437064873915531, 224.9013395616249511 ) ) ;
#47837 = FACE_OUTER_BOUND ( 'NONE', #28961, .T. ) ;
#47838 = CARTESIAN_POINT ( 'NONE',  ( 82.81670390244799762, -50.82844715994100682, 250.9178068554150514 ) ) ;
#47839 = DIRECTION ( 'NONE',  ( -2.999999999999999839E-15, 1.000000000000000000, -2.999999999999999900E-30 ) ) ;
#47840 = LINE ( 'NONE', #89658, #28214 ) ;
#47842 = DIRECTION ( 'NONE',  ( 9.912705577010326536E-16, 1.000000000000000000, 0.000000000000000000 ) ) ;
#47841 = CARTESIAN_POINT ( 'NONE',  ( 98.72346068757417470, -34.40322473509486656, 277.6356252759111385 ) ) ;
#47843 = CARTESIAN_POINT ( 'NONE',  ( 97.92324767642672612, -40.78073790739274074, 172.6583826592236051 ) ) ;
#47844 = DIRECTION ( 'NONE',  ( -0.2884130866282271777, 0.7071067811865476838, 0.6456143519637543848 ) ) ;
#47845 = CARTESIAN_POINT ( 'NONE',  ( 4.090931056105404195, 94.60184303864159006, -118.4878965444427621 ) ) ;
#47846 = EDGE_CURVE ( 'NONE', #66586, #56062, #3544, .T. ) ;
#47847 = CIRCLE ( 'NONE', #49278, 3.174999999999983391 ) ;
#47848 = CARTESIAN_POINT ( 'NONE',  ( 183.5150000000000148, 37.33800000000000097, 41.27499999999999858 ) ) ;
#47849 = ADVANCED_FACE ( 'NONE', ( #72601 ), #10366, .F. ) ;
#47850 = CARTESIAN_POINT ( 'NONE',  ( 0.000000000000000000, 93.07500000000001705, 0.000000000000000000 ) ) ;
#47851 = DIRECTION ( 'NONE',  ( 3.100000000000000258E-29, -3.100000000000000044E-14, -1.000000000000000000 ) ) ;
#47853 = VERTEX_POINT ( 'NONE', #44418 ) ;
#47852 = DIRECTION ( 'NONE',  ( 0.000000000000000000, 0.5000000000000007772, -0.8660254037844381525 ) ) ;
#47854 = LINE ( 'NONE', #13361, #13302 ) ;
#47855 = CARTESIAN_POINT ( 'NONE',  ( 97.14868559305091367, -40.01329441332335790, 241.5813395616249863 ) ) ;
#47856 = CARTESIAN_POINT ( 'NONE',  ( 102.3127581962668273, -26.75066580571964536, 136.4422919425779526 ) ) ;
#47857 = CARTESIAN_POINT ( 'NONE',  ( 97.57588284487002284, -41.14775938459609250, 252.6727681330536655 ) ) ;
#47858 = CIRCLE ( 'NONE', #27584, 2.500000000000002220 ) ;
#47859 = LINE ( 'NONE', #75596, #20032 ) ;
#47861 = DIRECTION ( 'NONE',  ( 0.000000000000000000, 0.000000000000000000, -1.000000000000000000 ) ) ;
#47860 = DIRECTION ( 'NONE',  ( 0.000000000000000000, 1.000000000000000000, 0.000000000000000000 ) ) ;
#47862 = CARTESIAN_POINT ( 'NONE',  ( 176.7738106835053031, -48.62134037887501137, 180.4678068554150059 ) ) ;
#47863 = DIRECTION ( 'NONE',  ( -1.000000000000000000, 1.011922027653136551E-15, 0.000000000000000000 ) ) ;
#47864 = B_SPLINE_CURVE_WITH_KNOTS ( 'NONE', 3,
 ( #46941, #88322, #6525, #26521, #26080, #47389, #53745, #33780, #12905, #40594, #61476, #68310, #89208, #34222, #43719, #56906, #14696, #48727, #42814, #28767, #21055, #43268, #15595, #84642, #83289, #57349, #16042 ),
 .UNSPECIFIED., .F., .F.,
 ( 4, 2, 2, 2, 2, 2, 2, 2, 2, 2, 1, 1, 1, 2, 4 ),
 ( 0.000000000000000000, 0.06249619433354525883, 0.1249923886670905177, 0.1874885830006357557, 0.2499847773341810353, 0.3124809716677263149, 0.3749771660012715113, 0.4374733603348168187, 0.4687214575015891116, 0.4843455060849753968, 0.4921575303766683729, 0.4960635425225149997, 0.4980165485954382576, 0.4989930516318998310, 0.4999695546683612934 ),
 .UNSPECIFIED. ) ;
#47865 = VERTEX_POINT ( 'NONE', #17187 ) ;
#47866 = ORIENTED_EDGE ( 'NONE', *, *, #58322, .T. ) ;
#47867 = VECTOR ( 'NONE', #20610, 1000.000000000000000 ) ;
#47868 = CARTESIAN_POINT ( 'NONE',  ( 115.0376279413645761, -33.66073653188622927, 138.5409912566489652 ) ) ;
#47870 = EDGE_LOOP ( 'NONE', ( #53517, #74378, #52063, #59113, #38315 ) ) ;
#47869 = DIRECTION ( 'NONE',  ( 0.000000000000000000, 1.000000000000000000, 0.000000000000000000 ) ) ;
#47871 = DIRECTION ( 'NONE',  ( 0.000000000000000000, -0.4999999999999990563, -0.8660254037844392627 ) ) ;
#47872 = CARTESIAN_POINT ( 'NONE',  ( 113.6005200848514107, -45.61596423689125146, 179.0689586092439640 ) ) ;
#47873 = CARTESIAN_POINT ( 'NONE',  ( 97.81219807385008380, -40.51719912245609123, 147.6362401243850115 ) ) ;
#47874 = DIRECTION ( 'NONE',  ( 0.000000000000000000, -1.000000000000000000, 0.000000000000000000 ) ) ;
#47875 = CARTESIAN_POINT ( 'NONE',  ( -90.66736180499643183, 74.80137413886471620, 76.38829385798661065 ) ) ;
#47876 = FACE_BOUND ( 'NONE', #40649, .T. ) ;
#47877 = CARTESIAN_POINT ( 'NONE',  ( 98.75024281215304711, -42.92452016420553917, 111.8480062282929737 ) ) ;
#47878 = VERTEX_POINT ( 'NONE', #39403 ) ;
#47879 = ORIENTED_EDGE ( 'NONE', *, *, #12669, .F. ) ;
#47880 = VERTEX_POINT ( 'NONE', #86676 ) ;
#47881 = CARTESIAN_POINT ( 'NONE',  ( 46.03715912545433753, -48.62818131006086020, 237.4678068554150059 ) ) ;
#47883 = CARTESIAN_POINT ( 'NONE',  ( 70.06670390244707392, -140.6784471599409869, 245.4568581461520012 ) ) ;
#47882 = CARTESIAN_POINT ( 'NONE',  ( 116.6769215743979800, -34.91203320259896259, 154.9756252759109714 ) ) ;
#47884 = CARTESIAN_POINT ( 'NONE',  ( 115.8259315161528775, -31.73088453253794583, 54.23961552823458021 ) ) ;
#47886 = EDGE_CURVE ( 'NONE', #5969, #46964, #64481, .T. ) ;
#47885 = FACE_OUTER_BOUND ( 'NONE', #14046, .T. ) ;
#47887 = CARTESIAN_POINT ( 'NONE',  ( 48.79742451362098166, -36.32844715994040996, -5.074374724088000832 ) ) ;
#47888 = CIRCLE ( 'NONE', #8765, 3.174999999999983391 ) ;
#47889 = CARTESIAN_POINT ( 'NONE',  ( 73.06670390244801183, -48.82844715994099971, 310.9178068554150514 ) ) ;
#47890 = CARTESIAN_POINT ( 'NONE',  ( 97.81169128372820865, -40.51741339292117772, 177.6357569005977268 ) ) ;
#47891 = CARTESIAN_POINT ( 'NONE',  ( 110.1514708964275968, -46.66481413883396812, 97.81562527591097478 ) ) ;
#47892 = EDGE_LOOP ( 'NONE', ( #21735, #57234 ) ) ;
#47893 = ORIENTED_EDGE ( 'NONE', *, *, #11350, .T. ) ;
#47894 = ORIENTED_EDGE ( 'NONE', *, *, #64470, .F. ) ;
#47895 = DIRECTION ( 'NONE',  ( 0.000000000000000000, -1.000000000000000000, 0.000000000000000000 ) ) ;
#47896 = CARTESIAN_POINT ( 'NONE',  ( -95.69832483115250454, 94.30053025434479252, -88.80956239834407029 ) ) ;
#47897 = CARTESIAN_POINT ( 'NONE',  ( 111.5401709588312116, -43.55702686802507628, 175.8566617981629463 ) ) ;
#47898 = CIRCLE ( 'NONE', #17521, 218.1859999999999786 ) ;
#47899 = ADVANCED_FACE ( 'NONE', ( #72152 ), #67108, .T. ) ;
#47900 = PLANE ( 'NONE',  #75036 ) ;
#47901 = ORIENTED_EDGE ( 'NONE', *, *, #45759, .T. ) ;
#47903 = ORIENTED_EDGE ( 'NONE', *, *, #25905, .T. ) ;
#47902 = VERTEX_POINT ( 'NONE', #52110 ) ;
#47904 = VECTOR ( 'NONE', #51279, 1000.000000000000000 ) ;
#47905 = FACE_OUTER_BOUND ( 'NONE', #25707, .T. ) ;
#47906 = CARTESIAN_POINT ( 'NONE',  ( 134.4433815842287174, -21.47944715994100306, 1.625625275910998813 ) ) ;
#47907 = ORIENTED_EDGE ( 'NONE', *, *, #66782, .F. ) ;
#47908 = ORIENTED_EDGE ( 'NONE', *, *, #72075, .F. ) ;
#47909 = CARTESIAN_POINT ( 'NONE',  ( 77.38816033347450229, -19.35482103167604251, 6.853567712192048411 ) ) ;
#47910 = EDGE_CURVE ( 'NONE', #75634, #5474, #26786, .T. ) ;
#47911 = CARTESIAN_POINT ( 'NONE',  ( 114.2010777387499587, -30.61601215110631458, 225.8339642582779447 ) ) ;
#47912 = ADVANCED_FACE ( 'NONE', ( #9928 ), #32580, .F. ) ;
#47913 = ORIENTED_EDGE ( 'NONE', *, *, #89114, .T. ) ;
#47914 = DIRECTION ( 'NONE',  ( 0.000000000000000000, 1.000000000000000000, 0.000000000000000000 ) ) ;
#47915 = CARTESIAN_POINT ( 'NONE',  ( -113.6350504498463323, 69.61314433698439075, 64.28280664495177632 ) ) ;
#47916 = ORIENTED_EDGE ( 'NONE', *, *, #40683, .F. ) ;
#47917 = VERTEX_POINT ( 'NONE', #45741 ) ;
#47918 = CARTESIAN_POINT ( 'NONE',  ( 31.85959712127300847, -23.19206098994092002, 342.9256252759109884 ) ) ;
#47919 = EDGE_LOOP ( 'NONE', ( #22038, #39387 ) ) ;
#47920 = ORIENTED_EDGE ( 'NONE', *, *, #35418, .T. ) ;
#47921 = ADVANCED_FACE ( 'NONE', ( #60282 ), #84851, .T. ) ;
#47922 = VECTOR ( 'NONE', #2254, 1000.000000000000000 ) ;
#47923 = CARTESIAN_POINT ( 'NONE',  ( 106.9677948388671069, -45.38341651713141545, 230.3976141791149814 ) ) ;
#47924 = CARTESIAN_POINT ( 'NONE',  ( 114.2552021840540846, -45.16177683379865471, 153.1508633711489722 ) ) ;
#47925 = VECTOR ( 'NONE', #86105, 999.9999999999998863 ) ;
#47926 = CARTESIAN_POINT ( 'NONE',  ( 97.95167206076190780, -31.64175201202206011, 110.9213395616259703 ) ) ;
#47927 = CARTESIAN_POINT ( 'NONE',  ( 111.1206699024608753, -28.37365878809221797, 249.5838068554168387 ) ) ;
#47928 = DIRECTION ( 'NONE',  ( 1.000000000000000000, 0.000000000000000000, 0.000000000000000000 ) ) ;
#47929 = CARTESIAN_POINT ( 'NONE',  ( 115.0396333253530230, -29.07419673827904916, 185.4232443235299570 ) ) ;
#47930 = EDGE_CURVE ( 'NONE', #37091, #52002, #66659, .T. ) ;
#47931 = CARTESIAN_POINT ( 'NONE',  ( 106.1318753153733070, -87.31936784520605954, -19.21046202161352667 ) ) ;
#47932 = ORIENTED_EDGE ( 'NONE', *, *, #14718, .T. ) ;
#47933 = FACE_OUTER_BOUND ( 'NONE', #89701, .T. ) ;
#47934 = ORIENTED_EDGE ( 'NONE', *, *, #64790, .T. ) ;
#47935 = VERTEX_POINT ( 'NONE', #78975 ) ;
#47936 = LINE ( 'NONE', #25723, #88027 ) ;
#47938 = ORIENTED_EDGE ( 'NONE', *, *, #41724, .F. ) ;
#47937 = VECTOR ( 'NONE', #71727, 1000.000000000000000 ) ;
#47939 = CARTESIAN_POINT ( 'NONE',  ( 107.0667039024470313, -104.2784471599409528, 25.71780685541800437 ) ) ;
#47940 = CARTESIAN_POINT ( 'NONE',  ( 101.7107321646854246, -27.74380102040660390, 85.50419670448295051 ) ) ;
#47941 = CARTESIAN_POINT ( 'NONE',  ( -9.688862330989991278, 74.32879814653003336, 130.1964161894449035 ) ) ;
#47942 = CARTESIAN_POINT ( 'NONE',  ( 136.6789756616809655, -35.84952872352904762, 6.945088388040495886 ) ) ;
#47943 = CARTESIAN_POINT ( 'NONE',  ( 107.0667039024479834, -36.72944715994099596, 239.5838068554170093 ) ) ;
#47946 = CARTESIAN_POINT ( 'NONE',  ( 103.7301789885933943, -26.21598454391068600, 201.3089586092439731 ) ) ;
#47945 = DIRECTION ( 'NONE',  ( -0.000000000000000000, -1.000000000000000000, -0.000000000000000000 ) ) ;
#47944 = LINE ( 'NONE', #13454, #24456 ) ;
#47947 = CARTESIAN_POINT ( 'NONE',  ( 67.06670390244701707, -79.67844715994098692, 222.2178068554179902 ) ) ;
#47948 = DIRECTION ( 'NONE',  ( -1.000000000000000078E-15, 0.000000000000000000, 1.000000000000000000 ) ) ;
#47949 = ORIENTED_EDGE ( 'NONE', *, *, #89603, .T. ) ;
#47950 = LINE ( 'NONE', #14817, #81775 ) ;
#47951 = EDGE_CURVE ( 'NONE', #75555, #55721, #38069, .T. ) ;
#47952 = CARTESIAN_POINT ( 'NONE',  ( 151.0371591254575776, -24.42818131005592264, 129.9678068554149775 ) ) ;
#47953 = ADVANCED_FACE ( 'NONE', ( #58937, #45309, #37633, #65757, #3109, #58499, #86227 ), #24005, .T. ) ;
#47954 = CARTESIAN_POINT ( 'NONE',  ( 0.000000000000000000, 92.07499999999998863, 0.000000000000000000 ) ) ;
#47955 = AXIS2_PLACEMENT_3D ( 'NONE', #7915, #7021, #70600 ) ;
#47956 = ADVANCED_FACE ( 'NONE', ( #52555 ), #32133, .T. ) ;
#47957 = VECTOR ( 'NONE', #52651, 1000.000000000000000 ) ;
#47958 = CARTESIAN_POINT ( 'NONE',  ( 141.0664832912740394, -46.72944715994099596, -4.824374724088994704 ) ) ;
#47959 = VECTOR ( 'NONE', #55254, 1000.000000000000000 ) ;
#47961 = ORIENTED_EDGE ( 'NONE', *, *, #2124, .F. ) ;
#47960 = CARTESIAN_POINT ( 'NONE',  ( 112.4772085026190354, -45.73365988577116070, 238.0070538473389377 ) ) ;
#47962 = CARTESIAN_POINT ( 'NONE',  ( 57.14999999999999858, 69.84999999999999432, 304.0379999999999541 ) ) ;
#47963 = CARTESIAN_POINT ( 'NONE',  ( 96.00433110544545912, -37.29885927265511469, 121.3794347997209684 ) ) ;
#47964 = CARTESIAN_POINT ( 'NONE',  ( 104.7356836917145699, -47.53413844247978659, 28.41943479971997988 ) ) ;
#47965 = CARTESIAN_POINT ( 'NONE',  ( 97.96923373944615321, -30.37039525599472256, 156.8289586092439549 ) ) ;
#47966 = EDGE_CURVE ( 'NONE', #7132, #59432, #88913, .T. ) ;
#47967 = DIRECTION ( 'NONE',  ( -0.9254794337955620787, -0.3787978585227822492, 0.000000000000000000 ) ) ;
#47968 = CARTESIAN_POINT ( 'NONE',  ( 28.57499999999999929, 87.13271776169258942, 310.8325000000000387 ) ) ;
#47970 = DIRECTION ( 'NONE',  ( -4.237773401492740281E-14, 1.000000000000000000, 0.000000000000000000 ) ) ;
#47969 = LINE ( 'NONE', #75705, #59379 ) ;
#47971 = CARTESIAN_POINT ( 'NONE',  ( -79.44498778673575146, 98.01532655701802810, 25.01765082793386696 ) ) ;
#47972 = DIRECTION ( 'NONE',  ( 0.000000000000000000, -1.000000000000000000, 0.000000000000000000 ) ) ;
#47973 = EDGE_LOOP ( 'NONE', ( #71857, #60244, #42003, #45329, #45686, #73234, #24910, #21484, #7279, #38065, #23487, #17670, #39886, #46315 ) ) ;
#47974 = VECTOR ( 'NONE', #388, 1000.000000000000000 ) ;
#47975 = ORIENTED_EDGE ( 'NONE', *, *, #14644, .F. ) ;
#47976 = ORIENTED_EDGE ( 'NONE', *, *, #61192, .T. ) ;
#47977 = AXIS2_PLACEMENT_3D ( 'NONE', #21257, #56654, #22167 ) ;
#47978 = ORIENTED_EDGE ( 'NONE', *, *, #50186, .T. ) ;
#47979 = CARTESIAN_POINT ( 'NONE',  ( 107.0664832912740394, -56.47944715994103149, -5.074374724089029343 ) ) ;
#47980 = CARTESIAN_POINT ( 'NONE',  ( 115.9265467165007379, -42.18176083994490000, 14.38705384733995984 ) ) ;
#47981 = DIRECTION ( 'NONE',  ( 0.000000000000000000, 1.000000000000000000, 0.000000000000000000 ) ) ;
#47982 = AXIS2_PLACEMENT_3D ( 'NONE', #89883, #13124, #61691 ) ;
#47983 = DIRECTION ( 'NONE',  ( 1.000000000000000078E-15, -1.000000000000000083E-30, -1.000000000000000000 ) ) ;
#47984 = CARTESIAN_POINT ( 'NONE',  ( 29.00000000000001421, 172.0000000000000000, 113.8826257785461280 ) ) ;
#47985 = CARTESIAN_POINT ( 'NONE',  ( 115.6071762752661130, -36.01623928086704041, 253.3152769709339793 ) ) ;
#47986 = EDGE_LOOP ( 'NONE', ( #32754, #63928, #27088, #65250 ) ) ;
#47987 = VERTEX_POINT ( 'NONE', #53448 ) ;
#47988 = ORIENTED_EDGE ( 'NONE', *, *, #77282, .F. ) ;
#47989 = DIRECTION ( 'NONE',  ( 1.000000000000000078E-15, -1.000000000000000000, 0.000000000000000000 ) ) ;
#47990 = CARTESIAN_POINT ( 'NONE',  ( 114.0075790447407087, -33.88846322102013175, -1.864374724089012947 ) ) ;
#47991 = CARTESIAN_POINT ( 'NONE',  ( 172.5664832912729878, -27.57844715994070484, 195.9256252759119832 ) ) ;
#47992 = CARTESIAN_POINT ( 'NONE',  ( 12.59999999999999964, 82.54999999999999716, 117.8845415480757595 ) ) ;
#47993 = CARTESIAN_POINT ( 'NONE',  ( -41.60202597009397607, 40.59999999999997300, 50.85338361873603219 ) ) ;
#47994 = VECTOR ( 'NONE', #73291, 1000.000000000000000 ) ;
#47995 = DIRECTION ( 'NONE',  ( -0.9659258262890690894, 0.000000000000000000, -0.2588190451025180749 ) ) ;
#47996 = VECTOR ( 'NONE', #57716, 1000.000000000000000 ) ;
#47997 = CARTESIAN_POINT ( 'NONE',  ( 6.123233995736769241E-16, 238.7999999999999829, 149.6557476874258441 ) ) ;
#47998 = CARTESIAN_POINT ( 'NONE',  ( 97.40014589274343848, -35.23768424668791965, 266.2041967044829676 ) ) ;
#47999 = DIRECTION ( 'NONE',  ( 0.000000000000000000, -1.000000000000000000, 0.000000000000000000 ) ) ;
#48000 = VERTEX_POINT ( 'NONE', #53901 ) ;
#48001 = CARTESIAN_POINT ( 'NONE',  ( 41.56648329127399677, -18.82844715994099971, 18.92562527591200094 ) ) ;
#48002 = AXIS2_PLACEMENT_3D ( 'NONE', #36911, #77811, #50531 ) ;
#48003 = CARTESIAN_POINT ( 'NONE',  ( 34.92499999999999716, 66.67499999999999716, 342.8999999999999773 ) ) ;
#48004 = CARTESIAN_POINT ( 'NONE',  ( 100.4744175226576886, -42.33708426910433076, 74.71761417911493197 ) ) ;
#48005 = VECTOR ( 'NONE', #30075, 1000.000000000000114 ) ;
#48006 = ADVANCED_FACE ( 'NONE', ( #88012 ), #39840, .T. ) ;
#48007 = ADVANCED_FACE ( 'NONE', ( #74381 ), #61625, .F. ) ;
#48008 = LINE ( 'NONE', #54816, #6437 ) ;
#48009 = CARTESIAN_POINT ( 'NONE',  ( 97.81169607051373305, -40.51742273377266912, 46.63562653399714009 ) ) ;
#48010 = ORIENTED_EDGE ( 'NONE', *, *, #57080, .F. ) ;
#48011 = EDGE_CURVE ( 'NONE', #2214, #16775, #47091, .T. ) ;
#48012 = CARTESIAN_POINT ( 'NONE',  ( 193.5667039024414464, -48.82844715994099971, 300.4678068554149490 ) ) ;
#48013 = ORIENTED_EDGE ( 'NONE', *, *, #26762, .T. ) ;
#48014 = CARTESIAN_POINT ( 'NONE',  ( 117.0233241640237338, -39.93681227152024604, 158.5784824187679476 ) ) ;
#48015 = ORIENTED_EDGE ( 'NONE', *, *, #72041, .T. ) ;
#48016 = EDGE_CURVE ( 'NONE', #48511, #83239, #76145, .T. ) ;
#48017 = AXIS2_PLACEMENT_3D ( 'NONE', #63330, #648, #83788 ) ;
#48018 = CARTESIAN_POINT ( 'NONE',  ( 145.2601077436562207, -69.52476574176742474, 247.4934834993690060 ) ) ;
#48019 = CARTESIAN_POINT ( 'NONE',  ( 97.67976800739046439, -37.13700294324897300, 112.7806309249449441 ) ) ;
#48020 = ADVANCED_FACE ( 'NONE', ( #13056 ), #26222, .F. ) ;
#48021 = B_SPLINE_CURVE_WITH_KNOTS ( 'NONE', 3,
 ( #36756, #29946, #85373, #23148, #50821, #78557, #43990, #88033, #74398, #80331, #18078, #67581, #47115, #68028, #53922, #60300, #25340, #26684 ),
 .UNSPECIFIED., .F., .F.,
 ( 4, 2, 2, 2, 2, 2, 2, 2, 4 ),
 ( 0.000000000000000000, 0.06250343988587346578, 0.1250068797717469316, 0.1875103196576203834, 0.2500137595434938631, 0.3125171994293673428, 0.3750206393152407669, 0.4375240792011142466, 0.5000275190869877262 ),
 .UNSPECIFIED. ) ;
#48022 = DIRECTION ( 'NONE',  ( 0.000000000000000000, 0.000000000000000000, -1.000000000000000000 ) ) ;
#48023 = FACE_OUTER_BOUND ( 'NONE', #52106, .T. ) ;
#48024 = CARTESIAN_POINT ( 'NONE',  ( 96.31605362642591217, -41.77429727756310740, 57.67562527591096710 ) ) ;
#48025 = CIRCLE ( 'NONE', #68416, 8.999999999999994671 ) ;
#48026 = EDGE_CURVE ( 'NONE', #18171, #2091, #75725, .T. ) ;
#48027 = CARTESIAN_POINT ( 'NONE',  ( 116.3199495083284347, -32.94194616109231077, 85.13562527591095375 ) ) ;
#48028 = ORIENTED_EDGE ( 'NONE', *, *, #11675, .T. ) ;
#48029 = DIRECTION ( 'NONE',  ( 2.900000000000000265E-14, -2.000000000000000155E-15, 1.000000000000000000 ) ) ;
#48030 = ORIENTED_EDGE ( 'NONE', *, *, #67572, .T. ) ;
#48031 = VERTEX_POINT ( 'NONE', #89361 ) ;
#48032 = EDGE_CURVE ( 'NONE', #11211, #1301, #61660, .T. ) ;
#48033 = VECTOR ( 'NONE', #42256, 1000.000000000000000 ) ;
#48034 = DIRECTION ( 'NONE',  ( 0.000000000000000000, 0.000000000000000000, -1.000000000000000000 ) ) ;
#48035 = ORIENTED_EDGE ( 'NONE', *, *, #25593, .T. ) ;
#48036 = CARTESIAN_POINT ( 'NONE',  ( 117.3624379696767335, -35.49166588079122420, 238.9337205140069500 ) ) ;
#48037 = CARTESIAN_POINT ( 'NONE',  ( 117.0439256081559165, -39.94344854842797332, 154.5784824187679476 ) ) ;
#48038 = CARTESIAN_POINT ( 'NONE',  ( 110.0324702783101571, -120.0661611444839991, -21.02845593540760305 ) ) ;
#48039 = CARTESIAN_POINT ( 'NONE',  ( 168.5667039024486087, -48.82844715993516616, 129.9678068554150059 ) ) ;
#48040 = CARTESIAN_POINT ( 'NONE',  ( 98.64735160015825954, -43.89130460420365409, 72.89943479972099283 ) ) ;
#48041 = CIRCLE ( 'NONE', #8933, 5.599999999999994316 ) ;
#48042 = ADVANCED_FACE ( 'NONE', ( #68464, #40296 ), #54345, .T. ) ;
#48043 = CARTESIAN_POINT ( 'NONE',  ( -446.0240000000000009, 53.97500000000000142, 50.79999999999999716 ) ) ;
#48044 = ORIENTED_EDGE ( 'NONE', *, *, #71641, .T. ) ;
#48045 = CARTESIAN_POINT ( 'NONE',  ( 44.45000000000000284, 66.67499999999999716, 219.0749999999999886 ) ) ;
#48046 = CARTESIAN_POINT ( 'NONE',  ( 116.3262419368496978, -32.93860311337579105, 160.1356252759109680 ) ) ;
#48047 = ORIENTED_EDGE ( 'NONE', *, *, #18499, .T. ) ;
#48048 = LINE ( 'NONE', #53506, #86669 ) ;
#48049 =( REPRESENTATION_RELATIONSHIP ('NONE','NONE', #82876, #885 ) REPRESENTATION_RELATIONSHIP_WITH_TRANSFORMATION ( #28538 )SHAPE_REPRESENTATION_RELATIONSHIP( ) );
#48050 = CARTESIAN_POINT ( 'NONE',  ( 164.7812970173289955, -35.65087443492610930, -5.074374724088000832 ) ) ;
#48051 = CARTESIAN_POINT ( 'NONE',  ( 106.8369185487093063, -47.13021470646874178, 272.5584824187680510 ) ) ;
#48052 = CARTESIAN_POINT ( 'NONE',  ( 148.0533267522752112, 0.000000000000000000, 160.2664750769284865 ) ) ;
#48053 = DIRECTION ( 'NONE',  ( 1.387778780781444492E-15, 0.000000000000000000, -1.000000000000000000 ) ) ;
#48054 = CARTESIAN_POINT ( 'NONE',  ( 104.4095340282210600, -46.45850909292975217, 92.36551864622379071 ) ) ;
#48055 = CARTESIAN_POINT ( 'NONE',  ( 116.7468388360755966, -38.12735696270561903, 28.71276813305495423 ) ) ;
#48057 = CARTESIAN_POINT ( 'NONE',  ( 103.2134869792596135, -46.43093390711685231, 113.2756252759109827 ) ) ;
#48056 = CARTESIAN_POINT ( 'NONE',  ( 111.3508018702361682, -27.66482620347798616, 99.72597377253785567 ) ) ;
#48058 = CARTESIAN_POINT ( 'NONE',  ( 31.75000000000000000, 8.255000000000000782, 3.174999999999999822 ) ) ;
#48059 = CARTESIAN_POINT ( 'NONE',  ( 97.91784736035330639, -30.44332401329681659, 165.8594347997199634 ) ) ;
#48060 = LINE ( 'NONE', #88977, #43771 ) ;
#48061 = VERTEX_POINT ( 'NONE', #6238 ) ;
#48062 = LINE ( 'NONE', #74452, #3378 ) ;
#48063 = AXIS2_PLACEMENT_3D ( 'NONE', #62060, #48407, #76140 ) ;
#48064 = CARTESIAN_POINT ( 'NONE',  ( 109.9216266489743248, 47.43999764421818099, 70.44375787698940883 ) ) ;
#48065 = FACE_OUTER_BOUND ( 'NONE', #15793, .T. ) ;
#48066 = ORIENTED_EDGE ( 'NONE', *, *, #23759, .F. ) ;
#48067 = EDGE_CURVE ( 'NONE', #8698, #21236, #33482, .T. ) ;
#48068 = LINE ( 'NONE', #75802, #31670 ) ;
#48070 = ORIENTED_EDGE ( 'NONE', *, *, #36045, .F. ) ;
#48069 = CARTESIAN_POINT ( 'NONE',  ( 97.79690410337100559, -31.86307605613059835, 135.9413395616259947 ) ) ;
#48071 = LINE ( 'NONE', #41259, #47974 ) ;
#48072 = ADVANCED_FACE ( 'NONE', ( #40738 ), #18964, .T. ) ;
#48073 = DIRECTION ( 'NONE',  ( 1.000000000000000000, 4.163336342344333240E-14, 0.000000000000000000 ) ) ;
#48074 = VECTOR ( 'NONE', #82749, 1000.000000000000000 ) ;
#48075 = FACE_OUTER_BOUND ( 'NONE', #35808, .T. ) ;
#48076 = PLANE ( 'NONE',  #27847 ) ;
#48077 = ORIENTED_EDGE ( 'NONE', *, *, #70288, .T. ) ;
#48078 = AXIS2_PLACEMENT_3D ( 'NONE', #13104, #76666, #61232 ) ;
#48079 = EDGE_LOOP ( 'NONE', ( #64118, #62584 ) ) ;
#48080 = VERTEX_POINT ( 'NONE', #67559 ) ;
#48081 = VERTEX_POINT ( 'NONE', #82563 ) ;
#48082 = LINE ( 'NONE', #34916, #43763 ) ;
#48083 = CARTESIAN_POINT ( 'NONE',  ( 92.89936586972048360, 95.23006786499112764, -91.73195104381109388 ) ) ;
#48084 = CARTESIAN_POINT ( 'NONE',  ( 47.62500000000000000, 94.53880000000000905, 221.4562499999999829 ) ) ;
#48085 = CIRCLE ( 'NONE', #84381, 3.174999999999997158 ) ;
#48087 = CARTESIAN_POINT ( 'NONE',  ( -160.2664750769294812, 0.000000000000000000, -148.0533267522755807 ) ) ;
#48086 = CARTESIAN_POINT ( 'NONE',  ( 149.4532656544377289, -72.54365454176046057, 394.9756252759100903 ) ) ;
#48088 = LINE ( 'NONE', #62180, #79157 ) ;
#48089 = ORIENTED_EDGE ( 'NONE', *, *, #88602, .T. ) ;
#48090 = AXIS2_PLACEMENT_3D ( 'NONE', #170, #21527, #63751 ) ;
#48091 = EDGE_LOOP ( 'NONE', ( #81557, #82882, #7318, #46485 ) ) ;
#48092 = PLANE ( 'NONE',  #39817 ) ;
#48093 = LINE ( 'NONE', #89924, #18742 ) ;
#48094 = CARTESIAN_POINT ( 'NONE',  ( 99.44473759953889669, -30.59981194223820467, 236.7870538473389388 ) ) ;
#48095 = AXIS2_PLACEMENT_3D ( 'NONE', #46719, #34891, #62601 ) ;
#48096 = FACE_OUTER_BOUND ( 'NONE', #58272, .T. ) ;
#48097 = CARTESIAN_POINT ( 'NONE',  ( 114.7041265136727901, -43.74408836545391921, 74.22324432352993995 ) ) ;
#48098 = DIRECTION ( 'NONE',  ( -0.9254794337955620787, -0.3787978585227822492, 0.000000000000000000 ) ) ;
#48099 = CARTESIAN_POINT ( 'NONE',  ( 106.5507326060560729, -26.72133602940400721, 21.11751855259041477 ) ) ;
#48100 = VERTEX_POINT ( 'NONE', #6677 ) ;
#48101 = FACE_OUTER_BOUND ( 'NONE', #83593, .T. ) ;
#48102 = ORIENTED_EDGE ( 'NONE', *, *, #43413, .T. ) ;
#48103 = ORIENTED_EDGE ( 'NONE', *, *, #29175, .F. ) ;
#48104 = EDGE_CURVE ( 'NONE', #80081, #89588, #34376, .T. ) ;
#48105 = CARTESIAN_POINT ( 'NONE',  ( -458.3598257906459708, 60.32499999999999574, -3.174999999999999822 ) ) ;
#48106 = CARTESIAN_POINT ( 'NONE',  ( 97.88747888210261294, -34.72385408216754143, 252.5749166392305938 ) ) ;
#48107 = DIRECTION ( 'NONE',  ( 0.000000000000000000, 0.000000000000000000, -1.000000000000000000 ) ) ;
#48108 = CARTESIAN_POINT ( 'NONE',  ( -76.20505178924449297, 120.6499999999999915, 76.20505178924310030 ) ) ;
#48109 = EDGE_CURVE ( 'NONE', #28751, #56395, #79079, .T. ) ;
#48110 = EDGE_CURVE ( 'NONE', #54206, #14514, #33036, .T. ) ;
#48111 = DIRECTION ( 'NONE',  ( -8.839355291601565315E-16, -1.000000000000000000, 0.000000000000000000 ) ) ;
#48112 = CARTESIAN_POINT ( 'NONE',  ( 89.75424775947713840, 73.28361289573331305, -77.45828646618613789 ) ) ;
#48113 = VERTEX_POINT ( 'NONE', #13943 ) ;
#48114 = CARTESIAN_POINT ( 'NONE',  ( 144.0667052733537901, -71.37844715994090450, 222.2178068554179902 ) ) ;
#48115 = ADVANCED_FACE ( 'NONE', ( #69363 ), #71809, .T. ) ;
#48116 = CARTESIAN_POINT ( 'NONE',  ( 95.64925804648841279, -35.75026674902539980, 296.0306255462182321 ) ) ;
#48117 = ORIENTED_EDGE ( 'NONE', *, *, #31412, .T. ) ;
#48118 = CARTESIAN_POINT ( 'NONE',  ( 96.19295485998075890, -38.71576710077270889, 51.48229194257797303 ) ) ;
#48119 = ORIENTED_EDGE ( 'NONE', *, *, #39616, .F. ) ;
#48120 = CARTESIAN_POINT ( 'NONE',  ( 99.11752347482735104, -34.75543446931638414, 273.9509475124486357 ) ) ;
#48121 = EDGE_CURVE ( 'NONE', #38148, #19807, #77377, .T. ) ;
#48122 = LINE ( 'NONE', #30393, #50382 ) ;
#48123 = CARTESIAN_POINT ( 'NONE',  ( 113.4245949246308243, -29.25360672088980962, 139.5156252759109634 ) ) ;
#48124 = FACE_OUTER_BOUND ( 'NONE', #71627, .T. ) ;
#48125 = DIRECTION ( 'NONE',  ( 0.000000000000000000, -1.000000000000000000, 0.000000000000000000 ) ) ;
#48126 = CARTESIAN_POINT ( 'NONE',  ( 165.2725846195387476, -35.55794170701241796, 313.9678068554149490 ) ) ;
#48127 = AXIS2_PLACEMENT_3D ( 'NONE', #41710, #74464, #13141 ) ;
#48128 = CARTESIAN_POINT ( 'NONE',  ( 5.299065574771610443, 71.00791656138970609, 130.4484248277202880 ) ) ;
#48129 = CARTESIAN_POINT ( 'NONE',  ( 116.9258602667948566, -41.82750404599077854, 239.4346728949589647 ) ) ;
#48130 = FACE_OUTER_BOUND ( 'NONE', #11177, .T. ) ;
#48131 = EDGE_CURVE ( 'NONE', #28391, #30630, #14857, .T. ) ;
#48132 = ORIENTED_EDGE ( 'NONE', *, *, #28055, .T. ) ;
#48133 = AXIS2_PLACEMENT_3D ( 'NONE', #30202, #8880, #56549 ) ;
#48134 = ORIENTED_EDGE ( 'NONE', *, *, #24575, .T. ) ;
#48135 = CARTESIAN_POINT ( 'NONE',  ( 108.3246818025246654, -47.12222909040148267, 113.6727681330539639 ) ) ;
#48136 = CARTESIAN_POINT ( 'NONE',  ( 120.7609492062753276, 46.70542043813176036, -49.61561143115795858 ) ) ;
#48137 = EDGE_LOOP ( 'NONE', ( #46312, #36148, #34747, #84846 ) ) ;
#48138 = ORIENTED_EDGE ( 'NONE', *, *, #46478, .F. ) ;
#48139 = ORIENTED_EDGE ( 'NONE', *, *, #58609, .F. ) ;
#48140 = EDGE_CURVE ( 'NONE', #35902, #22318, #22546, .T. ) ;
#48141 = CARTESIAN_POINT ( 'NONE',  ( 99.08946256649485917, -109.4614598618343138, -19.78219314458184996 ) ) ;
#48142 = CARTESIAN_POINT ( 'NONE',  ( 137.0667039024470739, -118.2784471599408960, 51.21780685541800437 ) ) ;
#48143 = DIRECTION ( 'NONE',  ( 0.000000000000000000, 0.000000000000000000, 1.000000000000000000 ) ) ;
#48144 = CARTESIAN_POINT ( 'NONE',  ( 172.5664832912740110, -36.32844715994070839, 258.9256252759120116 ) ) ;
#48145 = CARTESIAN_POINT ( 'NONE',  ( 112.1548083954980939, -43.14751820055241893, 165.9280903695909615 ) ) ;
#48146 = CARTESIAN_POINT ( 'NONE',  ( 105.0174007254451567, -25.84429900004466063, 276.2365776568634033 ) ) ;
#48148 = ADVANCED_FACE ( 'NONE', ( #8940 ), #36639, .T. ) ;
#48147 = AXIS2_PLACEMENT_3D ( 'NONE', #62100, #56165, #27586 ) ;
#48149 = CARTESIAN_POINT ( 'NONE',  ( 97.81936407165393632, -40.53612711470664465, 57.63723432799564250 ) ) ;
#48150 = ORIENTED_EDGE ( 'NONE', *, *, #39639, .T. ) ;
#48151 = CARTESIAN_POINT ( 'NONE',  ( 129.9777364973648162, 85.83513192049079521, -12.27484926614918237 ) ) ;
#48152 = CARTESIAN_POINT ( 'NONE',  ( 134.0664832912740110, -8.729447159940999512, 4.925625275911999168 ) ) ;
#48153 = EDGE_LOOP ( 'NONE', ( #39243, #64895, #56369, #30955, #76695, #26894, #64920 ) ) ;
#48155 = ORIENTED_EDGE ( 'NONE', *, *, #81484, .T. ) ;
#48154 = VECTOR ( 'NONE', #57141, 1000.000000000000000 ) ;
#48156 = AXIS2_PLACEMENT_3D ( 'NONE', #44816, #44366, #2611 ) ;
#48157 = DIRECTION ( 'NONE',  ( 0.000000000000000000, 0.000000000000000000, -1.000000000000000000 ) ) ;
#48158 = ORIENTED_EDGE ( 'NONE', *, *, #31514, .T. ) ;
#48159 = ORIENTED_EDGE ( 'NONE', *, *, #81492, .T. ) ;
#48160 = CARTESIAN_POINT ( 'NONE',  ( 196.2150000000000034, 43.68799999999999528, 57.14999999999999858 ) ) ;
#48161 = CARTESIAN_POINT ( 'NONE',  ( -3.306647731859349904, 70.28099577563533273, -130.5147235605103617 ) ) ;
#48162 = DIRECTION ( 'NONE',  ( 0.000000000000000000, 1.000000000000000000, 0.000000000000000000 ) ) ;
#48163 = CARTESIAN_POINT ( 'NONE',  ( 194.0371591254575776, -24.89890238294407254, 129.9678068554150343 ) ) ;
#48164 = CARTESIAN_POINT ( 'NONE',  ( 113.5378671157686910, -31.15474330070945541, 183.8152769709339793 ) ) ;
#48165 = AXIS2_PLACEMENT_3D ( 'NONE', #89324, #48390, #27527 ) ;
#48166 = CARTESIAN_POINT ( 'NONE',  ( 107.8717536863088640, -26.29114242999935769, 70.01562527591099183 ) ) ;
#48167 = FACE_OUTER_BOUND ( 'NONE', #258, .T. ) ;
#48168 = EDGE_LOOP ( 'NONE', ( #28923, #77002 ) ) ;
#48169 = LINE ( 'NONE', #69987, #28122 ) ;
#48170 = CIRCLE ( 'NONE', #6128, 15.84999999999999964 ) ;
#48171 = EDGE_LOOP ( 'NONE', ( #34862, #57940, #67093, #53941 ) ) ;
#48172 = CARTESIAN_POINT ( 'NONE',  ( 104.4889533838145752, -26.97908276471815370, 261.2814877649475989 ) ) ;
#48173 = ORIENTED_EDGE ( 'NONE', *, *, #61971, .T. ) ;
#48174 = DIRECTION ( 'NONE',  ( 0.000000000000000000, 0.000000000000000000, -1.000000000000000000 ) ) ;
#48175 = PLANE ( 'NONE',  #77839 ) ;
#48176 = EDGE_CURVE ( 'NONE', #68890, #89686, #73274, .T. ) ;
#48177 = DIRECTION ( 'NONE',  ( 0.000000000000000000, 0.000000000000000000, -1.000000000000000000 ) ) ;
#48178 = CARTESIAN_POINT ( 'NONE',  ( 147.9173672921288869, -72.54391775211570348, 542.9756252759101471 ) ) ;
#48179 = ORIENTED_EDGE ( 'NONE', *, *, #81713, .F. ) ;
#48180 = CARTESIAN_POINT ( 'NONE',  ( 115.6294417704117734, -28.50085323451786579, 39.43562527591099354 ) ) ;
#48181 = SURFACE_SIDE_STYLE ('',( #36380 ) ) ;
#48183 = DIRECTION ( 'NONE',  ( 0.000000000000000000, 1.000000000000000000, 0.000000000000000000 ) ) ;
#48182 = DIRECTION ( 'NONE',  ( 0.000000000000000000, -1.000000000000000000, 0.000000000000000000 ) ) ;
#48184 = CARTESIAN_POINT ( 'NONE',  ( 177.0371591254545649, -48.62818131005479927, 180.4678068554150059 ) ) ;
#48185 = CARTESIAN_POINT ( 'NONE',  ( 133.6895842087692756, -15.97944715994100839, 1.625625275910996814 ) ) ;
#48186 = ORIENTED_EDGE ( 'NONE', *, *, #24770, .T. ) ;
#48187 = AXIS2_PLACEMENT_3D ( 'NONE', #65750, #63988, #45301 ) ;
#48188 = PLANE ( 'NONE',  #2564 ) ;
#48189 = DIRECTION ( 'NONE',  ( 0.000000000000000000, -1.000000000000000000, 0.000000000000000000 ) ) ;
#48190 = CARTESIAN_POINT ( 'NONE',  ( 11.02404012120765842, 76.19011824550719325, 118.0432514857309911 ) ) ;
#48191 = ORIENTED_EDGE ( 'NONE', *, *, #8690, .F. ) ;
#48192 = EDGE_CURVE ( 'NONE', #32697, #52469, #56147, .T. ) ;
#48193 = CARTESIAN_POINT ( 'NONE',  ( 113.3555096308132022, -27.61169779702804306, 85.60800622829195561 ) ) ;
#48195 = DIRECTION ( 'NONE',  ( 0.000000000000000000, 0.000000000000000000, -1.000000000000000000 ) ) ;
#48194 = DIRECTION ( 'NONE',  ( -1.000000000000000000, 0.000000000000000000, 0.000000000000000000 ) ) ;
#48196 = CARTESIAN_POINT ( 'NONE',  ( -194.1576000000000022, 101.5999999999999943, 114.2999999999999972 ) ) ;
#48197 = AXIS2_PLACEMENT_3D ( 'NONE', #35516, #84150, #75194 ) ;
#48198 = EDGE_CURVE ( 'NONE', #78594, #7132, #35537, .T. ) ;
#48199 = CARTESIAN_POINT ( 'NONE',  ( 138.8356781741756265, -107.9363541596096212, 249.3055338466990065 ) ) ;
#48200 = VERTEX_POINT ( 'NONE', #57052 ) ;
#48201 = CARTESIAN_POINT ( 'NONE',  ( 102.3899016914588884, -28.13915478247121271, 141.4727681330539895 ) ) ;
#48203 = ORIENTED_EDGE ( 'NONE', *, *, #71001, .F. ) ;
#48202 = DIRECTION ( 'NONE',  ( 0.000000000000000000, 0.000000000000000000, 1.000000000000000000 ) ) ;
#48204 = CARTESIAN_POINT ( 'NONE',  ( 105.1131368864170526, -25.87365329830177529, 271.2061014663872243 ) ) ;
#48205 = CARTESIAN_POINT ( 'NONE',  ( 173.9900000000000091, 20.32000000000000028, -71.37400000000000944 ) ) ;
#48206 = DIRECTION ( 'NONE',  ( 0.7071067811865525687, -0.7071067811865425767, 7.071067811865533512E-16 ) ) ;
#48207 = FACE_BOUND ( 'NONE', #28358, .T. ) ;
#48208 = CARTESIAN_POINT ( 'NONE',  ( 24.79284581386643183, 184.0000000000000000, 0.000000000000000000 ) ) ;
#48209 = AXIS2_PLACEMENT_3D ( 'NONE', #86483, #79676, #9277 ) ;
#48210 = FACE_BOUND ( 'NONE', #84389, .T. ) ;
#48211 = CARTESIAN_POINT ( 'NONE',  ( -89.95524642164049567, 70.27892663483464730, 94.62072105690099022 ) ) ;
#48212 = CARTESIAN_POINT ( 'NONE',  ( 112.6540662323892263, -44.79745133516141209, 203.0584824187689605 ) ) ;
#48213 = VERTEX_POINT ( 'NONE', #69810 ) ;
#48214 = ORIENTED_EDGE ( 'NONE', *, *, #87360, .T. ) ;
#48215 = CARTESIAN_POINT ( 'NONE',  ( 112.6324721509601545, -29.83393797428842831, 160.9672975916109579 ) ) ;
#48216 = CIRCLE ( 'NONE', #1835, 7.999999999999992895 ) ;
#48217 = LINE ( 'NONE', #70488, #48688 ) ;
#48219 = DIRECTION ( 'NONE',  ( -0.000000000000000000, -0.000000000000000000, 1.000000000000000000 ) ) ;
#48218 = CARTESIAN_POINT ( 'NONE',  ( 104.7413546109693527, -27.22895552020974108, 281.2670538473389570 ) ) ;
#48220 = CARTESIAN_POINT ( 'NONE',  ( 147.0667039024470739, -137.6773508071221954, 245.4788300746780010 ) ) ;
#48221 = EDGE_CURVE ( 'NONE', #8011, #80877, #32621, .T. ) ;
#48222 = EDGE_CURVE ( 'NONE', #55564, #83557, #34113, .T. ) ;
#48223 = CARTESIAN_POINT ( 'NONE',  ( 28.57499999999999929, 77.96728223830740490, 310.8325000000000387 ) ) ;
#48224 = CARTESIAN_POINT ( 'NONE',  ( 107.0664832912739399, -36.72944715994095333, 312.6356252759112522 ) ) ;
#48225 = CARTESIAN_POINT ( 'NONE',  ( 104.4899544478337248, -26.97880758572692272, 106.2814586095817333 ) ) ;
#48226 = EDGE_CURVE ( 'NONE', #36063, #55559, #57509, .T. ) ;
#48227 = CARTESIAN_POINT ( 'NONE',  ( 79.06648329127300201, -36.72944715994189835, 342.9256252759109884 ) ) ;
#48228 = CARTESIAN_POINT ( 'NONE',  ( 99.10268845779062019, -29.98093639561593449, 215.7670538473399517 ) ) ;
#48229 = CARTESIAN_POINT ( 'NONE',  ( 115.8264358448934246, -31.73174211693571678, 169.2397684523309067 ) ) ;
#48230 = ORIENTED_EDGE ( 'NONE', *, *, #61194, .T. ) ;
#48231 = EDGE_LOOP ( 'NONE', ( #12302, #27044, #88278, #84406 ) ) ;
#48232 = EDGE_CURVE ( 'NONE', #75146, #80780, #52877, .T. ) ;
#48233 = CARTESIAN_POINT ( 'NONE',  ( 118.5256205435842958, -36.72944715994096754, 296.0306255462182321 ) ) ;
#48234 = CARTESIAN_POINT ( 'NONE',  ( 81.77795131945210017, -20.88977919473711964, 7.751962620062596621 ) ) ;
#48236 = DIRECTION ( 'NONE',  ( -0.000000000000000000, -1.000000000000000000, -0.000000000000000000 ) ) ;
#48235 = B_SPLINE_CURVE_WITH_KNOTS ( 'NONE', 3,
 ( #32114, #73907, #72129, #87099, #51209, #18041, #31673, #3090, #17168, #45289, #45722, #52973, #23546, #52091, #44850, #37611, #30786, #78952 ),
 .UNSPECIFIED., .F., .F.,
 ( 4, 2, 2, 2, 2, 2, 2, 2, 4 ),
 ( 0.000000000000000000, 0.06250044056969467077, 0.1250008811393893415, 0.1875013217090840123, 0.2500017622787786831, 0.3125022028484733538, 0.3750026434181680246, 0.4375030839878626954, 0.5000035245575573661 ),
 .UNSPECIFIED. ) ;
#48237 = DIRECTION ( 'NONE',  ( 0.000000000000000000, 0.000000000000000000, 1.000000000000000000 ) ) ;
#48238 = DIRECTION ( 'NONE',  ( -0.7071067811985214391, 0.7071067811745735954, 0.000000000000000000 ) ) ;
#48239 = VERTEX_POINT ( 'NONE', #16195 ) ;
#48240 = CARTESIAN_POINT ( 'NONE',  ( 96.61551125061282619, -32.99117460050268846, 22.06514908543494258 ) ) ;
#48241 = CARTESIAN_POINT ( 'NONE',  ( 95.29485650985192535, -38.09666651163277606, 236.4184824187679510 ) ) ;
#48242 = ORIENTED_EDGE ( 'NONE', *, *, #57070, .T. ) ;
#48243 = EDGE_CURVE ( 'NONE', #3381, #63429, #43873, .T. ) ;
#48244 = VECTOR ( 'NONE', #82885, 1000.000000000000114 ) ;
#48245 = DIRECTION ( 'NONE',  ( -0.7071067811865437980, 0.000000000000000000, -0.7071067811865512365 ) ) ;
#48246 = CARTESIAN_POINT ( 'NONE',  ( 160.2664750769289697, 0.000000000000000000, 148.0533267522752112 ) ) ;
#48247 = CARTESIAN_POINT ( 'NONE',  ( 110.8552107763470644, -45.98393496479614129, 167.8856887709574721 ) ) ;
#48248 = CARTESIAN_POINT ( 'NONE',  ( 111.5100823108406587, -29.30278217496053017, 52.47761417911495130 ) ) ;
#48249 = CARTESIAN_POINT ( 'NONE',  ( 96.62828407576300549, -37.15518013270143172, 157.3584824187679487 ) ) ;
#48250 = DIRECTION ( 'NONE',  ( 0.000000000000000000, -1.000000000000000000, 0.000000000000000000 ) ) ;
#48251 = ORIENTED_EDGE ( 'NONE', *, *, #22634, .T. ) ;
#48252 = DIRECTION ( 'NONE',  ( 0.000000000000000000, 0.000000000000000000, 1.000000000000000000 ) ) ;
#48253 = ORIENTED_EDGE ( 'NONE', *, *, #74918, .F. ) ;
#48254 = VERTEX_POINT ( 'NONE', #312 ) ;
#48255 = AXIS2_PLACEMENT_3D ( 'NONE', #33637, #32277, #38653 ) ;
#48256 = CARTESIAN_POINT ( 'NONE',  ( -33.98325472291465132, 111.1250000000000000, 3.174999999999764899 ) ) ;
#48257 = VERTEX_POINT ( 'NONE', #55684 ) ;
#48258 = EDGE_LOOP ( 'NONE', ( #74599, #46358, #61999, #15931 ) ) ;
#48259 = CARTESIAN_POINT ( 'NONE',  ( 107.0664832912748068, -36.72944715993923381, 14.92562527591097066 ) ) ;
#48260 = CARTESIAN_POINT ( 'NONE',  ( 102.5065049712838601, -29.50707016595331567, 109.9467055423629631 ) ) ;
#48261 = CARTESIAN_POINT ( 'NONE',  ( 96.10188529952328906, -35.15685947849579662, 226.2251490854349640 ) ) ;
#48262 = CARTESIAN_POINT ( 'NONE',  ( 96.87985868497418096, -34.61725761836211035, 216.1641967044819808 ) ) ;
#48263 = CARTESIAN_POINT ( 'NONE',  ( 116.4547782460826255, -32.24742764444982157, 15.18133956162492915 ) ) ;
#48264 = DIRECTION ( 'NONE',  ( -1.000000000000000000, -3.999999999999999995E-14, -1.000000000000000078E-15 ) ) ;
#48265 = LINE ( 'NONE', #21495, #77240 ) ;
#48266 = VERTEX_POINT ( 'NONE', #7583 ) ;
#48267 = EDGE_CURVE ( 'NONE', #72016, #70034, #6194, .T. ) ;
#48268 = CARTESIAN_POINT ( 'NONE',  ( 115.9482186066389602, -32.63332544795704138, 104.1699109901969535 ) ) ;
#48269 = AXIS2_PLACEMENT_3D ( 'NONE', #69430, #56678, #77143 ) ;
#48270 = CARTESIAN_POINT ( 'NONE',  ( 96.67089207319645539, -38.24056507437282448, 66.44133956162495735 ) ) ;
#48271 = CARTESIAN_POINT ( 'NONE',  ( 100.2192867603235840, -28.80968922735345927, 260.6441967044821695 ) ) ;
#48272 = ORIENTED_EDGE ( 'NONE', *, *, #83540, .F. ) ;
#48273 = CARTESIAN_POINT ( 'NONE',  ( 117.3350766552244977, -34.92860824786317409, 243.9641967044819637 ) ) ;
#48274 = LINE ( 'NONE', #6974, #23919 ) ;
#48275 = CARTESIAN_POINT ( 'NONE',  ( -22.91753934680783544, 57.39944268860868704, 30.43757021144150343 ) ) ;
#48276 = AXIS2_PLACEMENT_3D ( 'NONE', #27836, #40573, #68293 ) ;
#48277 = EDGE_CURVE ( 'NONE', #14017, #35213, #62977, .T. ) ;
#48278 = CARTESIAN_POINT ( 'NONE',  ( 27.27158787008327678, 127.0000000000000000, 90.32146847885336172 ) ) ;
#48279 = FACE_OUTER_BOUND ( 'NONE', #29862, .T. ) ;
#48281 = CARTESIAN_POINT ( 'NONE',  ( 80.06648329127399677, -8.350947159940998787, 4.925625275911999168 ) ) ;
#48280 = DIRECTION ( 'NONE',  ( 1.000000000000000000, 0.000000000000000000, 0.000000000000000000 ) ) ;
#48282 = DIRECTION ( 'NONE',  ( 0.000000000000000000, 0.000000000000000000, 1.000000000000000000 ) ) ;
#48283 = CARTESIAN_POINT ( 'NONE',  ( 92.32962665258612844, 82.54999999999999716, -74.36911441044637172 ) ) ;
#48284 = VECTOR ( 'NONE', #11761, 1000.000000000000000 ) ;
#48285 = CARTESIAN_POINT ( 'NONE',  ( 107.0664832912749915, -36.72944715993903486, 25.56312527591096995 ) ) ;
#48286 = CARTESIAN_POINT ( 'NONE',  ( 0.000000000000000000, 125.4759999999999991, -190.5000000000000000 ) ) ;
#48287 = CYLINDRICAL_SURFACE ( 'NONE', #76397, 4.750000000000004441 ) ;
#48288 = DIRECTION ( 'NONE',  ( 0.000000000000000000, 1.000000000000000000, 0.000000000000000000 ) ) ;
#48290 = EDGE_LOOP ( 'NONE', ( #64768, #36636, #20356, #54614 ) ) ;
#48289 = LINE ( 'NONE', #20621, #89273 ) ;
#48291 = CARTESIAN_POINT ( 'NONE',  ( 110.7536356736639078, -102.7271463785351528, 2.217806855417947531 ) ) ;
#48292 = CARTESIAN_POINT ( 'NONE',  ( 106.8359473341788686, -47.17421700602214685, 272.5584824187680510 ) ) ;
#48293 = CARTESIAN_POINT ( 'NONE',  ( 97.79428472817266993, -42.74653246722733257, 142.7965776568629508 ) ) ;
#48294 = CARTESIAN_POINT ( 'NONE',  ( 96.22287284433019749, -34.36014117848482385, 252.1432443235303538 ) ) ;
#48295 = PLANE ( 'NONE',  #75143 ) ;
#48297 = DIRECTION ( 'NONE',  ( 0.000000000000000000, 0.000000000000000000, -1.000000000000000000 ) ) ;
#48296 = DIRECTION ( 'NONE',  ( 4.194175870806139918E-14, -1.000000000000000000, 0.000000000000000000 ) ) ;
#48298 = FACE_OUTER_BOUND ( 'NONE', #20666, .T. ) ;
#48299 = PLANE ( 'NONE',  #15246 ) ;
#48300 = EDGE_CURVE ( 'NONE', #27646, #37791, #30702, .T. ) ;
#48301 = VECTOR ( 'NONE', #49987, 1000.000000000000000 ) ;
#48302 = ORIENTED_EDGE ( 'NONE', *, *, #16515, .F. ) ;
#48303 = CARTESIAN_POINT ( 'NONE',  ( 31.75000000000000000, 104.3431970271542042, 3.174999999999999822 ) ) ;
#48304 = VERTEX_POINT ( 'NONE', #79319 ) ;
#48305 = CARTESIAN_POINT ( 'NONE',  ( 115.5798344143896372, -39.81741137289535004, 172.9600388756959717 ) ) ;
#48307 = ORIENTED_EDGE ( 'NONE', *, *, #66895, .T. ) ;
#48306 = DIRECTION ( 'NONE',  ( 1.000000000000000078E-15, -1.000000000000000083E-30, -1.000000000000000000 ) ) ;
#48308 = VECTOR ( 'NONE', #84568, 1000.000000000000000 ) ;
#48309 = DIRECTION ( 'NONE',  ( -1.000000000000000078E-15, 1.000000000000000083E-30, 1.000000000000000000 ) ) ;
#48310 = CARTESIAN_POINT ( 'NONE',  ( 95.59354794629810215, -39.59649474372135813, 162.5213395616259788 ) ) ;
#48311 = CARTESIAN_POINT ( 'NONE',  ( 67.65734841870819594, 95.25000000000000000, 358.0130000000000337 ) ) ;
#48312 = FACE_BOUND ( 'NONE', #78535, .T. ) ;
#48313 = CARTESIAN_POINT ( 'NONE',  ( -76.80536679343852313, 74.16967745525863620, 90.31351860656819497 ) ) ;
#48314 = FACE_OUTER_BOUND ( 'NONE', #16289, .T. ) ;
#48315 = CARTESIAN_POINT ( 'NONE',  ( 113.5922197990811213, -29.44396856740769408, 114.4956252759109816 ) ) ;
#48316 = ORIENTED_EDGE ( 'NONE', *, *, #22220, .F. ) ;
#48317 = ORIENTED_EDGE ( 'NONE', *, *, #55501, .F. ) ;
#48318 = ORIENTED_EDGE ( 'NONE', *, *, #9361, .F. ) ;
#48319 = VECTOR ( 'NONE', #87452, 1000.000000000000000 ) ;
#48320 = LINE ( 'NONE', #75623, #84989 ) ;
#48322 = DIRECTION ( 'NONE',  ( 0.000000000000000000, 0.000000000000000000, 1.000000000000000000 ) ) ;
#48321 = CARTESIAN_POINT ( 'NONE',  ( 101.5632356570521324, -44.81509498605967678, 193.1013395616249682 ) ) ;
#48323 = LINE ( 'NONE', #76059, #27680 ) ;
#48324 = CARTESIAN_POINT ( 'NONE',  ( 91.91125933621954402, -111.9799080603168449, -11.78219314458175937 ) ) ;
#48325 = EDGE_CURVE ( 'NONE', #6628, #79108, #58835, .T. ) ;
#48326 = CARTESIAN_POINT ( 'NONE',  ( 44.45000000000000284, 69.84999999999999432, 288.9250000000000114 ) ) ;
#48327 = CARTESIAN_POINT ( 'NONE',  ( 53.56670390244749314, -48.82844715994058049, 129.9678068554150911 ) ) ;
#48328 = EDGE_CURVE ( 'NONE', #35448, #79680, #10259, .T. ) ;
#48329 = CARTESIAN_POINT ( 'NONE',  ( 67.66273711577628092, -68.45061131148345623, 246.9170789443036824 ) ) ;
#48330 = CARTESIAN_POINT ( 'NONE',  ( 111.7842945758856672, -25.88553347519904335, 134.7499109901969518 ) ) ;
#48331 = ORIENTED_EDGE ( 'NONE', *, *, #12473, .F. ) ;
#48332 = ADVANCED_FACE ( 'NONE', ( #44766 ), #31136, .F. ) ;
#48333 = ORIENTED_EDGE ( 'NONE', *, *, #48328, .T. ) ;
#48334 = ORIENTED_EDGE ( 'NONE', *, *, #16391, .T. ) ;
#48335 = EDGE_CURVE ( 'NONE', #62556, #67090, #2566, .T. ) ;
#48336 = DIRECTION ( 'NONE',  ( 0.000000000000000000, 5.463695987328529395E-16, -1.000000000000000000 ) ) ;
#48337 = CARTESIAN_POINT ( 'NONE',  ( -96.20559720633563927, 93.94653598907719072, -88.25806911646377273 ) ) ;
#48338 = PLANE ( 'NONE',  #70029 ) ;
#48339 = CARTESIAN_POINT ( 'NONE',  ( 108.9290709455192570, -28.27771998284391231, 177.7099951314959583 ) ) ;
#48340 = VECTOR ( 'NONE', #63398, 1000.000000000000000 ) ;
#48341 = CARTESIAN_POINT ( 'NONE',  ( 96.41083957889333078, -31.77770432788677013, 4.925625275910959999 ) ) ;
#48342 = VECTOR ( 'NONE', #60912, 1000.000000000000000 ) ;
#48343 = CARTESIAN_POINT ( 'NONE',  ( 108.4184404244437019, -26.73515679610073192, 25.96837172698450757 ) ) ;
#48344 = ORIENTED_EDGE ( 'NONE', *, *, #76346, .T. ) ;
#48346 = EDGE_LOOP ( 'NONE', ( #19182, #38649, #20561, #49657 ) ) ;
#48345 = ORIENTED_EDGE ( 'NONE', *, *, #38604, .T. ) ;
#48347 = ADVANCED_FACE ( 'NONE', ( #37959 ), #17078, .F. ) ;
#48348 = CARTESIAN_POINT ( 'NONE',  ( 144.1741131095133994, -138.0461895383712942, 247.6591799766680140 ) ) ;
#48349 = EDGE_LOOP ( 'NONE', ( #52914, #86159 ) ) ;
#48350 = VERTEX_POINT ( 'NONE', #24340 ) ;
#48351 = EDGE_CURVE ( 'NONE', #15321, #72437, #30266, .T. ) ;
#48352 = CARTESIAN_POINT ( 'NONE',  ( 248.6659999999999968, 52.73749999999999716, 10.66800000000000104 ) ) ;
#48353 = CARTESIAN_POINT ( 'NONE',  ( 97.87165577458247867, -34.79769342939158605, 257.6053928297065454 ) ) ;
#48354 = ORIENTED_EDGE ( 'NONE', *, *, #23285, .T. ) ;
#48355 = LINE ( 'NONE', #22050, #59533 ) ;
#48356 = CARTESIAN_POINT ( 'NONE',  ( -126.0395364549222137, 66.02220425850067897, 34.04284698069740500 ) ) ;
#48357 = VERTEX_POINT ( 'NONE', #65226 ) ;
#48358 = ORIENTED_EDGE ( 'NONE', *, *, #7648, .T. ) ;
#48359 = AXIS2_PLACEMENT_3D ( 'NONE', #41308, #41752, #20446 ) ;
#48360 = CARTESIAN_POINT ( 'NONE',  ( 32.25690895537073288, -33.54226604285041446, 237.4678068554150059 ) ) ;
#48361 = CIRCLE ( 'NONE', #12153, 1.500000000000001332 ) ;
#48362 = ORIENTED_EDGE ( 'NONE', *, *, #64163, .F. ) ;
#48363 = ORIENTED_EDGE ( 'NONE', *, *, #83984, .T. ) ;
#48364 = CARTESIAN_POINT ( 'NONE',  ( 110.1408960893143956, -44.29103306967431308, 280.7023760838771409 ) ) ;
#48366 = CARTESIAN_POINT ( 'NONE',  ( 116.9251198095579554, -40.18685225151752860, 133.5584824187679658 ) ) ;
#48365 = AXIS2_PLACEMENT_3D ( 'NONE', #74383, #41186, #82113 ) ;
#48367 = CARTESIAN_POINT ( 'NONE',  ( 117.0854383170106559, -39.53109055650223524, 98.60991099019594230 ) ) ;
#48368 = CARTESIAN_POINT ( 'NONE',  ( 105.2596865451559012, -44.71351967478707223, 249.5838068554171798 ) ) ;
#48369 = CARTESIAN_POINT ( 'NONE',  ( 131.5359215223106730, -17.65293368212931568, 7.043713522541953154 ) ) ;
#48370 = CARTESIAN_POINT ( 'NONE',  ( 106.4836140971313654, -24.89327890070114435, 191.1156252759109861 ) ) ;
#48371 = CARTESIAN_POINT ( 'NONE',  ( 181.9790560690580037, -31.62489322948711035, 193.9678068554150059 ) ) ;
#48372 = LINE ( 'NONE', #42023, #85763 ) ;
#48373 = VERTEX_POINT ( 'NONE', #86571 ) ;
#48374 = CYLINDRICAL_SURFACE ( 'NONE', #20691, 2.999999999999999112 ) ;
#48375 = EDGE_LOOP ( 'NONE', ( #31850, #85465, #64943, #14893 ) ) ;
#48376 = EDGE_LOOP ( 'NONE', ( #44498, #60450, #89097, #46176 ) ) ;
#48377 = DIRECTION ( 'NONE',  ( -0.000000000000000000, 1.000000000000000000, 0.000000000000000000 ) ) ;
#48378 = ADVANCED_FACE ( 'NONE', ( #23465 ), #66100, .F. ) ;
#48379 = CIRCLE ( 'NONE', #38229, 15.84999999999999964 ) ;
#48380 = CARTESIAN_POINT ( 'NONE',  ( 102.0664873402873809, -27.97083079549564033, 136.4898195177950981 ) ) ;
#48381 = CARTESIAN_POINT ( 'NONE',  ( 96.60699139826044757, -36.88735862350505101, 136.3384824187679385 ) ) ;
#48382 = CARTESIAN_POINT ( 'NONE',  ( -10.48803521384346737, 75.38805513179248408, 130.1340587520734857 ) ) ;
#48383 = EDGE_CURVE ( 'NONE', #34061, #51923, #87012, .T. ) ;
#48384 = CARTESIAN_POINT ( 'NONE',  ( 97.81670390244700286, -67.87844715994096134, 55.21780685541800437 ) ) ;
#48385 = CARTESIAN_POINT ( 'NONE',  ( 37.56670390244743629, -48.82844715994126261, 180.4678068554150911 ) ) ;
#48388 = CARTESIAN_POINT ( 'NONE',  ( 101.4165038149807572, -45.50681337102567880, 218.1213395616249784 ) ) ;
#48387 = DIRECTION ( 'NONE',  ( 0.000000000000000000, 0.000000000000000000, -1.000000000000000000 ) ) ;
#48386 = DIRECTION ( 'NONE',  ( 0.000000000000000000, 0.000000000000000000, -1.000000000000000000 ) ) ;
#48389 = CYLINDRICAL_SURFACE ( 'NONE', #40848, 3.250000000000002665 ) ;
#48390 = DIRECTION ( 'NONE',  ( 0.000000000000000000, 1.000000000000000000, 0.000000000000000000 ) ) ;
#48391 = ORIENTED_EDGE ( 'NONE', *, *, #65904, .T. ) ;
#48392 = CARTESIAN_POINT ( 'NONE',  ( 196.2150000000000034, 30.98800000000000310, 44.45000000000000284 ) ) ;
#48393 = DIRECTION ( 'NONE',  ( 0.7071067811868657627, 0.7071067811862293828, 7.071067811868650498E-16 ) ) ;
#48394 = CARTESIAN_POINT ( 'NONE',  ( 130.1657039024480298, -18.82844715994099971, 199.5838068554170093 ) ) ;
#48395 = B_SPLINE_CURVE_WITH_KNOTS ( 'NONE', 3,
 ( #9516, #64925, #2710, #49933, #16779, #65369, #30406, #77668, #3151, #86264, #24047, #51716, #10403, #79468, #17229, #53490, #17669, #60773, #4486, #19448, #24489, #38545, #5835, #47131, #39444, #81255, #52151, #11746, #88509, #74867, #10840 ),
 .UNSPECIFIED., .F., .F.,
 ( 4, 2, 2, 1, 2, 2, 2, 2, 2, 2, 2, 1, 1, 2, 2, 2, 4 ),
 ( 0.000000000000000000, 0.1250000000000227318, 0.1875000000000338618, 0.2187500000000353328, 0.2343750000000360545, 0.2500000000000367484, 0.3750000000000290323, 0.4375000000000245359, 0.5000000000000199840, 0.6250000000000124345, 0.6875000000000107692, 0.7187500000000089928, 0.7343750000000082157, 0.7421875000000077716, 0.7500000000000072164, 0.8750000000000036637, 1.000000000000000000 ),
 .UNSPECIFIED. ) ;
#48396 = DIRECTION ( 'NONE',  ( -0.7071067811734105257, 0.7071067811996846197, 0.000000000000000000 ) ) ;
#48398 = EDGE_LOOP ( 'NONE', ( #64130, #848, #31947, #13982 ) ) ;
#48397 = CARTESIAN_POINT ( 'NONE',  ( 111.4991187713021219, -26.55290587224241960, 284.7375300378155316 ) ) ;
#48399 = LINE ( 'NONE', #87985, #10379 ) ;
#48400 = CARTESIAN_POINT ( 'NONE',  ( 113.5789493677227711, -44.94383383376451491, 168.1099109901969939 ) ) ;
#48401 = CARTESIAN_POINT ( 'NONE',  ( 96.83360046493686468, -38.89957200400883863, 27.49276813305395706 ) ) ;
#48402 = CARTESIAN_POINT ( 'NONE',  ( 117.5308098062252498, -40.43017262224169883, 174.5680062282919778 ) ) ;
#48403 = CYLINDRICAL_SURFACE ( 'NONE', #59051, 2.116999999999993776 ) ;
#48404 = CARTESIAN_POINT ( 'NONE',  ( 115.8252723203762429, -31.72975044166505398, 100.2398416254468714 ) ) ;
#48406 = DIRECTION ( 'NONE',  ( -1.000000000000000078E-15, 0.000000000000000000, 1.000000000000000000 ) ) ;
#48405 = CARTESIAN_POINT ( 'NONE',  ( -72.96458098368751166, 127.0000000000000000, 72.96458098368620426 ) ) ;
#48407 = DIRECTION ( 'NONE',  ( 1.639958061481212836E-42, -4.100000000000000342E-29, -1.000000000000000000 ) ) ;
#48408 = CARTESIAN_POINT ( 'NONE',  ( 163.2449138993008262, -32.11662333284039761, 193.9678068554149775 ) ) ;
#48409 = ORIENTED_EDGE ( 'NONE', *, *, #3850, .F. ) ;
#48410 = VECTOR ( 'NONE', #63287, 1000.000000000000000 ) ;
#48411 = EDGE_CURVE ( 'NONE', #65784, #40115, #31581, .T. ) ;
#48412 = AXIS2_PLACEMENT_3D ( 'NONE', #79049, #37712, #85872 ) ;
#48413 = ORIENTED_EDGE ( 'NONE', *, *, #62533, .F. ) ;
#48414 = ORIENTED_EDGE ( 'NONE', *, *, #1084, .F. ) ;
#48415 = ORIENTED_EDGE ( 'NONE', *, *, #65325, .T. ) ;
#48416 = DIRECTION ( 'NONE',  ( -1.000000000000000000, -1.000000000000000078E-15, -1.000000000000000078E-15 ) ) ;
#48417 = CARTESIAN_POINT ( 'NONE',  ( 104.7644060343265551, -46.87484541886965417, 68.39848241876794077 ) ) ;
#48418 = PLANE ( 'NONE',  #78890 ) ;
#48419 = CARTESIAN_POINT ( 'NONE',  ( 145.3807741851185824, -139.2458688871068375, 246.2343294490942753 ) ) ;
#48420 = EDGE_CURVE ( 'NONE', #77531, #14756, #25217, .T. ) ;
#48421 = CARTESIAN_POINT ( 'NONE',  ( 114.9980252723336207, -29.89690579156949823, 180.3927681330539770 ) ) ;
#48422 = DIRECTION ( 'NONE',  ( 0.000000000000000000, -1.000000000000000000, 0.000000000000000000 ) ) ;
#48423 = CARTESIAN_POINT ( 'NONE',  ( 114.1034101198941215, -31.83723292758831747, 278.7324198280767860 ) ) ;
#48424 = ORIENTED_EDGE ( 'NONE', *, *, #53586, .F. ) ;
#48425 = ORIENTED_EDGE ( 'NONE', *, *, #15477, .T. ) ;
#48426 = ORIENTED_EDGE ( 'NONE', *, *, #80588, .T. ) ;
#48427 = VECTOR ( 'NONE', #74401, 1000.000000000000000 ) ;
#48428 = DIRECTION ( 'NONE',  ( -1.000000000000000000, -3.201858731750027727E-15, -1.000000000000000078E-15 ) ) ;
#48429 = DIRECTION ( 'NONE',  ( -0.9130365726098601531, 0.000000000000000000, -0.4078776986755214828 ) ) ;
#48430 = AXIS2_PLACEMENT_3D ( 'NONE', #20715, #47047, #53853 ) ;
#48431 = LINE ( 'NONE', #29379, #22347 ) ;
#48432 = CARTESIAN_POINT ( 'NONE',  ( 105.7964350658723163, -26.72445465374554985, 275.1771098754847458 ) ) ;
#48433 = CARTESIAN_POINT ( 'NONE',  ( 1.224646799147354440E-15, 211.0000000000000000, 144.6557476874258441 ) ) ;
#48434 = DIRECTION ( 'NONE',  ( 0.000000000000000000, 0.000000000000000000, -1.000000000000000000 ) ) ;
#48435 = DIRECTION ( 'NONE',  ( -1.000000000000000000, 0.000000000000000000, 0.000000000000000000 ) ) ;
#48436 = CARTESIAN_POINT ( 'NONE',  ( 111.4502655420255905, -27.98611277567904310, 279.7070538473400916 ) ) ;
#48437 = EDGE_CURVE ( 'NONE', #76266, #30286, #52446, .T. ) ;
#48438 = CARTESIAN_POINT ( 'NONE',  ( 107.0667039024470313, -104.2784471599420755, -19.78219314458201694 ) ) ;
#48439 = ORIENTED_EDGE ( 'NONE', *, *, #67842, .T. ) ;
#48440 = LINE ( 'NONE', #75290, #40279 ) ;
#48441 = LINE ( 'NONE', #63909, #71405 ) ;
#48442 = CARTESIAN_POINT ( 'NONE',  ( 114.8246268090051245, -34.19154740317726038, 86.89666179816296676 ) ) ;
#48443 = CARTESIAN_POINT ( 'NONE',  ( -103.1875000000000000, 127.0000000000000000, -1.080832317973422076E-12 ) ) ;
#48444 = DIRECTION ( 'NONE',  ( 0.000000000000000000, 0.000000000000000000, 1.000000000000000000 ) ) ;
#48445 = ORIENTED_EDGE ( 'NONE', *, *, #14483, .F. ) ;
#48446 = VERTEX_POINT ( 'NONE', #45634 ) ;
#48447 = ADVANCED_FACE ( 'NONE', ( #11139 ), #38844, .T. ) ;
#48448 = CARTESIAN_POINT ( 'NONE',  ( 77.67297288197789840, -35.37149612621453088, 7.198162082951554019 ) ) ;
#48449 = ORIENTED_EDGE ( 'NONE', *, *, #41293, .F. ) ;
#48450 = CARTESIAN_POINT ( 'NONE',  ( 114.2400596693416475, -45.14401474321602592, 153.1508633711489722 ) ) ;
#48451 = ORIENTED_EDGE ( 'NONE', *, *, #33785, .F. ) ;
#48452 = ADVANCED_FACE ( 'NONE', ( #80652 ), #85690, .T. ) ;
#48453 = DIRECTION ( 'NONE',  ( -4.237773401492740281E-14, 1.000000000000000000, 0.000000000000000000 ) ) ;
#48454 = CARTESIAN_POINT ( 'NONE',  ( 107.5650335644346569, -45.56823575777373492, 149.0530118773259858 ) ) ;
#48455 = CARTESIAN_POINT ( 'NONE',  ( -6.359675246477835664, 93.55082578214793898, 118.3858732848555775 ) ) ;
#48456 = CARTESIAN_POINT ( 'NONE',  ( 34.27258461953785229, -35.55794170701850732, 193.9678068554150911 ) ) ;
#48457 = CARTESIAN_POINT ( 'NONE',  ( 96.89995799317335923, -32.33320227283598314, 57.01372051400599616 ) ) ;
#48458 = VECTOR ( 'NONE', #42506, 1000.000000000000000 ) ;
#48459 = CARTESIAN_POINT ( 'NONE',  ( 168.5667039024483813, -48.82844715993517326, 249.9678068554149775 ) ) ;
#48460 = ORIENTED_EDGE ( 'NONE', *, *, #52800, .T. ) ;
#48461 = CARTESIAN_POINT ( 'NONE',  ( -118.3250318368775567, 72.22378176823141871, -7.404816947594603960 ) ) ;
#48462 = ORIENTED_EDGE ( 'NONE', *, *, #20683, .F. ) ;
#48463 = ORIENTED_EDGE ( 'NONE', *, *, #73379, .F. ) ;
#48464 = DIRECTION ( 'NONE',  ( -0.9068632946707755327, 0.4214249218767993077, 0.000000000000000000 ) ) ;
#48465 = EDGE_LOOP ( 'NONE', ( #69510, #12287 ) ) ;
#48466 = CARTESIAN_POINT ( 'NONE',  ( 112.0124476237221103, -28.73397683645135814, 289.6356252759109680 ) ) ;
#48467 = CARTESIAN_POINT ( 'NONE',  ( 108.8525730979967676, -47.02250997168171409, 163.7127681330539701 ) ) ;
#48468 = DIRECTION ( 'NONE',  ( 0.000000000000000000, 0.000000000000000000, -1.000000000000000000 ) ) ;
#48469 = CARTESIAN_POINT ( 'NONE',  ( 0.000000000000000000, 127.0000000000000000, 0.000000000000000000 ) ) ;
#48470 = CARTESIAN_POINT ( 'NONE',  ( 104.1078173601787995, -46.72588569351386667, 103.3470538473389411 ) ) ;
#48471 = CARTESIAN_POINT ( 'NONE',  ( 101.9936209708133248, -45.44607155584300529, 262.1564586119682758 ) ) ;
#48472 = ORIENTED_EDGE ( 'NONE', *, *, #15787, .F. ) ;
#48473 = CARTESIAN_POINT ( 'NONE',  ( 97.80821801276054828, -40.50893789028450698, 116.6351770529384595 ) ) ;
#48474 = PRODUCT_DEFINITION_SHAPE ( 'NONE', 'NONE',  #61649 ) ;
#48475 = CARTESIAN_POINT ( 'NONE',  ( 107.5667039024470313, -100.3098201933444926, 2.217806855417892020 ) ) ;
#48476 = ORIENTED_EDGE ( 'NONE', *, *, #75319, .T. ) ;
#48477 = VECTOR ( 'NONE', #78892, 1000.000000000000000 ) ;
#48478 = CYLINDRICAL_SURFACE ( 'NONE', #54723, 23.50000000000000711 ) ;
#48479 = VECTOR ( 'NONE', #26875, 1000.000000000000000 ) ;
#48480 = AXIS2_PLACEMENT_3D ( 'NONE', #18508, #46194, #80314 ) ;
#48481 = LINE ( 'NONE', #13998, #50781 ) ;
#48482 = CARTESIAN_POINT ( 'NONE',  ( 115.4447846419100472, -42.99283068281499709, 28.31562527591097123 ) ) ;
#48483 = CARTESIAN_POINT ( 'NONE',  ( 72.96458098368701428, 101.5999999999999943, -72.96458098368670164 ) ) ;
#48484 = AXIS2_PLACEMENT_3D ( 'NONE', #52834, #31539, #16589 ) ;
#48485 = CARTESIAN_POINT ( 'NONE',  ( 141.0235900724604790, -8.833000550534265471, 14.92562527591107369 ) ) ;
#48486 = DIRECTION ( 'NONE',  ( 0.000000000000000000, 0.000000000000000000, -1.000000000000000000 ) ) ;
#48487 = CARTESIAN_POINT ( 'NONE',  ( 114.6457050300329996, -40.66804080626008044, 287.8667055423626380 ) ) ;
#48489 = CARTESIAN_POINT ( 'NONE',  ( 117.1882713363356174, -39.28166824301211335, 119.6299109901969615 ) ) ;
#48488 = CARTESIAN_POINT ( 'NONE',  ( 103.2384247724198332, -27.39885374353689329, 100.3865915095992420 ) ) ;
#48490 = DIRECTION ( 'NONE',  ( -4.237773401492740281E-14, 1.000000000000000000, 0.000000000000000000 ) ) ;
#48491 = CARTESIAN_POINT ( 'NONE',  ( 98.05257159168807846, -42.12399974224388188, 161.7556252759109725 ) ) ;
#48492 = CARTESIAN_POINT ( 'NONE',  ( 32.56670390244700997, -22.48495420874110806, -5.074374724088000832 ) ) ;
#48493 = EDGE_LOOP ( 'NONE', ( #85958, #39226, #69476, #11160 ) ) ;
#48494 = CARTESIAN_POINT ( 'NONE',  ( 115.5439452383991892, -99.96145986183427112, -19.78219314458215550 ) ) ;
#48495 = AXIS2_PLACEMENT_3D ( 'NONE', #74124, #53190, #5544 ) ;
#48496 = AXIS2_PLACEMENT_3D ( 'NONE', #17898, #73305, #57446 ) ;
#48497 = CARTESIAN_POINT ( 'NONE',  ( 109.3101629130975709, 52.31002220769687483, 71.38747593275114411 ) ) ;
#48498 = CARTESIAN_POINT ( 'NONE',  ( 136.5763721200418672, -35.60518726037151538, 2.783021291305102896 ) ) ;
#48499 = ORIENTED_EDGE ( 'NONE', *, *, #23370, .T. ) ;
#48500 = CARTESIAN_POINT ( 'NONE',  ( 41.56648329127398966, -18.82844715994071194, 195.9256252759120684 ) ) ;
#48502 = EDGE_LOOP ( 'NONE', ( #11400, #17331 ) ) ;
#48501 = CARTESIAN_POINT ( 'NONE',  ( 117.5013794172148351, -40.51439451343497922, 173.5375300378159693 ) ) ;
#48503 = DIRECTION ( 'NONE',  ( -0.000000000000000000, 1.000000000000000000, 0.000000000000000000 ) ) ;
#48504 = CARTESIAN_POINT ( 'NONE',  ( 112.2157656529268763, -45.81911987206276393, 208.9870538473389558 ) ) ;
#48505 = CARTESIAN_POINT ( 'NONE',  ( 184.5667039024548615, -48.82844715994099971, 300.4678068554149490 ) ) ;
#48506 = DIRECTION ( 'NONE',  ( -0.000000000000000000, -0.000000000000000000, 1.000000000000000000 ) ) ;
#48507 = CARTESIAN_POINT ( 'NONE',  ( 143.0664832912740110, -8.729447159940999512, 342.9256252759119548 ) ) ;
#48508 = VERTEX_POINT ( 'NONE', #51134 ) ;
#48509 = EDGE_CURVE ( 'NONE', #81323, #22750, #78874, .T. ) ;
#48510 = EDGE_CURVE ( 'NONE', #63113, #36552, #50057, .T. ) ;
#48511 = VERTEX_POINT ( 'NONE', #60169 ) ;
#48512 = ORIENTED_EDGE ( 'NONE', *, *, #68491, .F. ) ;
#48513 = ADVANCED_FACE ( 'NONE', ( #54687 ), #4786, .F. ) ;
#48514 = ORIENTED_EDGE ( 'NONE', *, *, #22466, .F. ) ;
#48515 = CYLINDRICAL_SURFACE ( 'NONE', #74255, 34.13125000000000142 ) ;
#48516 = CARTESIAN_POINT ( 'NONE',  ( 105.1109661324377811, -26.48940614006117755, 231.2270538473399597 ) ) ;
#48517 = DIRECTION ( 'NONE',  ( 3.310531404218880154E-13, -1.000000000000000000, 3.320531404218880632E-28 ) ) ;
#48518 = CARTESIAN_POINT ( 'NONE',  ( 135.1485260852034571, -16.20116861174954082, 1.807989644433795728 ) ) ;
#48519 = ADVANCED_FACE ( 'NONE', ( #33377 ), #68355, .F. ) ;
#48520 = EDGE_CURVE ( 'NONE', #31976, #30939, #10904, .T. ) ;
#48522 = CARTESIAN_POINT ( 'NONE',  ( 52.56670390244699576, -68.37844715994100397, 180.4678068554179902 ) ) ;
#48521 = DIRECTION ( 'NONE',  ( 0.000000000000000000, 0.000000000000000000, 1.000000000000000000 ) ) ;
#48523 = PLANE ( 'NONE',  #54398 ) ;
#48524 = CARTESIAN_POINT ( 'NONE',  ( 111.4247116192842810, -46.22429891269226943, 27.91848241876792969 ) ) ;
#48525 = VERTEX_POINT ( 'NONE', #19309 ) ;
#48526 = EDGE_CURVE ( 'NONE', #69613, #75906, #46979, .T. ) ;
#48527 = EDGE_CURVE ( 'NONE', #63937, #70860, #68893, .T. ) ;
#48528 = EDGE_LOOP ( 'NONE', ( #20139, #26359 ) ) ;
#48529 = DIRECTION ( 'NONE',  ( 1.000000000000000000, 0.000000000000000000, 0.000000000000000000 ) ) ;
#48530 = CIRCLE ( 'NONE', #76183, 0.4999999999999982236 ) ;
#48532 = EDGE_CURVE ( 'NONE', #83421, #46468, #58816, .T. ) ;
#48531 = LINE ( 'NONE', #25885, #60748 ) ;
#48533 = CARTESIAN_POINT ( 'NONE',  ( 104.4938967476557821, -26.68352342390111787, 241.2880062282909535 ) ) ;
#48534 = CARTESIAN_POINT ( 'NONE',  ( 165.2725846195380086, -35.55794170701810941, -5.074374724088000832 ) ) ;
#48535 = CARTESIAN_POINT ( 'NONE',  ( 114.6661721138974315, -42.88640786233941782, 84.28419670448195689 ) ) ;
#48536 = ADVANCED_FACE ( 'NONE', ( #34267 ), #82063, .T. ) ;
#48537 = CARTESIAN_POINT ( 'NONE',  ( 50.30672865705777497, 91.74178678112681951, -72.48695520484585586 ) ) ;
#48538 = EDGE_CURVE ( 'NONE', #23155, #21324, #48320, .T. ) ;
#48539 = CARTESIAN_POINT ( 'NONE',  ( 97.81170999498195329, -40.51745678363457159, 187.6351607544849287 ) ) ;
#48540 = VERTEX_POINT ( 'NONE', #75167 ) ;
#48541 = CYLINDRICAL_SURFACE ( 'NONE', #61722, 4.750000000000004441 ) ;
#48542 = EDGE_LOOP ( 'NONE', ( #42454, #76707 ) ) ;
#48543 = ORIENTED_EDGE ( 'NONE', *, *, #80774, .F. ) ;
#48544 = DIRECTION ( 'NONE',  ( 0.000000000000000000, -0.8660254037844384856, 0.5000000000000003331 ) ) ;
#48545 = CARTESIAN_POINT ( 'NONE',  ( 115.1162204959661466, -41.57488383322457537, 274.8149166392303755 ) ) ;
#48546 = CONICAL_SURFACE ( 'NONE', #57257, 9.571100913904325935, 0.7853981633974543852 ) ;
#48547 = CARTESIAN_POINT ( 'NONE',  ( 113.1782937289016218, -44.75186862573180946, 193.0939586049964021 ) ) ;
#48548 = AXIS2_PLACEMENT_3D ( 'NONE', #48522, #43066, #7233 ) ;
#48549 = VECTOR ( 'NONE', #68910, 1000.000000000000000 ) ;
#48550 = CARTESIAN_POINT ( 'NONE',  ( 97.81169952324414396, -40.51743120087827776, 141.6355106266202313 ) ) ;
#48551 = AXIS2_PLACEMENT_3D ( 'NONE', #89060, #80023, #45455 ) ;
#48552 = CARTESIAN_POINT ( 'NONE',  ( 99.09570908776939291, -30.55043173837237092, 85.80229194108821389 ) ) ;
#48553 = CARTESIAN_POINT ( 'NONE',  ( 75.67519899969724406, 76.18740257834571139, -91.26337341211403498 ) ) ;
#48554 = AXIS2_PLACEMENT_3D ( 'NONE', #77493, #63873, #14832 ) ;
#48555 = VERTEX_POINT ( 'NONE', #12497 ) ;
#48556 = CARTESIAN_POINT ( 'NONE',  ( 141.0667039024479834, -50.82844715994100682, 310.9178068554150514 ) ) ;
#48557 = EDGE_CURVE ( 'NONE', #53716, #49237, #60945, .T. ) ;
#48558 = VECTOR ( 'NONE', #36845, 1000.000000000000000 ) ;
#48559 = CARTESIAN_POINT ( 'NONE',  ( 183.5150000000000148, 53.21300000000000097, 59.96543552338529537 ) ) ;
#48560 = EDGE_LOOP ( 'NONE', ( #42050, #5854, #6163, #40936 ) ) ;
#48561 = CARTESIAN_POINT ( 'NONE',  ( 107.6068636345326155, -48.56787927409158812, 42.61276813305398292 ) ) ;
#48562 = EDGE_LOOP ( 'NONE', ( #55709, #13218, #62420, #44817 ) ) ;
#48563 = EDGE_CURVE ( 'NONE', #85065, #71100, #26125, .T. ) ;
#48564 = CARTESIAN_POINT ( 'NONE',  ( 114.3096959184101280, -40.49343719410034481, 286.2623760838771432 ) ) ;
#48565 = EDGE_CURVE ( 'NONE', #32414, #9456, #33827, .T. ) ;
#48566 = CARTESIAN_POINT ( 'NONE',  ( 108.3347386951206204, -46.73470465874113700, 127.6774649500359828 ) ) ;
#48567 = CARTESIAN_POINT ( 'NONE',  ( 102.9676436823273917, -46.25511244710201453, 137.2651490854349561 ) ) ;
#48568 = CARTESIAN_POINT ( 'NONE',  ( 23.62126498357886462, 80.43107061863682361, 298.6185181214070212 ) ) ;
#48569 = DIRECTION ( 'NONE',  ( 0.2645893543674792125, -0.6270931345857608807, -0.7326299707975406639 ) ) ;
#48571 = EDGE_CURVE ( 'NONE', #12725, #79504, #27016, .T. ) ;
#48570 = FACE_OUTER_BOUND ( 'NONE', #85732, .T. ) ;
#48572 = CARTESIAN_POINT ( 'NONE',  ( 10.56424515663473507, 75.50111803887961059, 130.1278827369076794 ) ) ;
#48573 = AXIS2_PLACEMENT_3D ( 'NONE', #55006, #34591, #48650 ) ;
#48574 = CARTESIAN_POINT ( 'NONE',  ( 104.3994723555534989, -25.95519307775132134, 236.2575300378159682 ) ) ;
#48575 = CARTESIAN_POINT ( 'NONE',  ( 82.65294504194743297, 95.16897323824362331, -84.99816483510849707 ) ) ;
#48576 = VERTEX_POINT ( 'NONE', #47881 ) ;
#48577 = CARTESIAN_POINT ( 'NONE',  ( 63.03715912545735023, -46.82818131006016671, 180.4678068554151196 ) ) ;
#48578 = ORIENTED_EDGE ( 'NONE', *, *, #2093, .T. ) ;
#48579 = CARTESIAN_POINT ( 'NONE',  ( 95.97749374758174667, -37.21091289986100037, 112.3489586092449599 ) ) ;
#48580 = CARTESIAN_POINT ( 'NONE',  ( 123.8510197158557418, 45.44641352664827849, -41.30202659462528203 ) ) ;
#48581 = ORIENTED_EDGE ( 'NONE', *, *, #43442, .F. ) ;
#48582 = CONICAL_SURFACE ( 'NONE', #71831, 10.66799999999999748, 0.08726646259971625186 ) ;
#48583 = VERTEX_POINT ( 'NONE', #13390 ) ;
#48584 = EDGE_LOOP ( 'NONE', ( #67133, #1556, #48307 ) ) ;
#48585 = DIRECTION ( 'NONE',  ( 0.000000000000000000, 0.000000000000000000, -1.000000000000000000 ) ) ;
#48586 = DIRECTION ( 'NONE',  ( -1.000000000000000000, 0.000000000000000000, 0.000000000000000000 ) ) ;
#48587 = CARTESIAN_POINT ( 'NONE',  ( 107.0664832912739541, -20.72944715994095333, 357.5272416190308604 ) ) ;
#48588 = CARTESIAN_POINT ( 'NONE',  ( 45.76696975232698605, -48.62818131005841593, 129.9678068554150911 ) ) ;
#48589 = CARTESIAN_POINT ( 'NONE',  ( 103.7603453811189667, -44.19263536178414142, 175.0623760838769840 ) ) ;
#48590 = CARTESIAN_POINT ( 'NONE',  ( 97.19620376612084556, -33.30704266974938577, 282.0613395616252888 ) ) ;
#48591 = PLANE ( 'NONE',  #7344 ) ;
#48592 = EDGE_LOOP ( 'NONE', ( #42229, #6221 ) ) ;
#48593 = CARTESIAN_POINT ( 'NONE',  ( 10.32955618830038347, 75.14983015127609178, 118.1053723791018086 ) ) ;
#48594 = DIRECTION ( 'NONE',  ( 0.7071067811865560104, 0.000000000000000000, -0.7071067811865391350 ) ) ;
#48595 = EDGE_LOOP ( 'NONE', ( #75965, #3118, #71196, #54330 ) ) ;
#48596 = EDGE_LOOP ( 'NONE', ( #70048, #76621, #30650, #49824 ) ) ;
#48597 = VECTOR ( 'NONE', #51618, 999.9999999999998863 ) ;
#48598 = DIRECTION ( 'NONE',  ( 1.000000000000000000, 4.163336342344333240E-14, 0.000000000000000000 ) ) ;
#48599 = SHAPE_REPRESENTATION ( 'Rotary Table Central Base', ( #50656 ), #10078 ) ;
#48600 = DIRECTION ( 'NONE',  ( -1.000000000000000000, -1.000000000000000078E-15, 0.000000000000000000 ) ) ;
#48601 = VECTOR ( 'NONE', #18602, 1000.000000000000000 ) ;
#48602 = CARTESIAN_POINT ( 'NONE',  ( -11.02410282832817856, 76.19023921641802133, -130.0905510769329965 ) ) ;
#48603 = DIRECTION ( 'NONE',  ( 3.999999999999999995E-14, -1.000000000000000000, 4.100000000000000342E-29 ) ) ;
#48604 = DIRECTION ( 'NONE',  ( 0.9068632946707807507, -0.4214249218767881500, 9.068605531941956314E-16 ) ) ;
#48605 = CARTESIAN_POINT ( 'NONE',  ( 103.4754675462218927, -28.97956086136533926, 179.8438483995059869 ) ) ;
#48606 = CARTESIAN_POINT ( 'NONE',  ( 116.7859321266972330, -32.83856289285826335, 54.12991099019698282 ) ) ;
#48607 = CARTESIAN_POINT ( 'NONE',  ( 25.56670390244816815, -48.82844715994168183, 295.7178068554150059 ) ) ;
#48608 = ORIENTED_EDGE ( 'NONE', *, *, #9709, .F. ) ;
#48609 = CARTESIAN_POINT ( 'NONE',  ( -83.23139715273258332, 69.85063172184842983, -84.43201024598432980 ) ) ;
#48610 = ORIENTED_EDGE ( 'NONE', *, *, #65788, .F. ) ;
#48611 = CARTESIAN_POINT ( 'NONE',  ( 4.665904304751416087E-15, 91.07499999999996021, -38.10000000000000142 ) ) ;
#48612 = VERTEX_POINT ( 'NONE', #41079 ) ;
#48613 = CARTESIAN_POINT ( 'NONE',  ( -72.96458098368751166, 117.4749999999999943, 78.00648098368618832 ) ) ;
#48614 = LINE ( 'NONE', #21855, #60369 ) ;
#48615 = CARTESIAN_POINT ( 'NONE',  ( 116.7959471365900299, -39.38489853325881285, 274.6145815639363832 ) ) ;
#48617 = VECTOR ( 'NONE', #8474, 1000.000000000000000 ) ;
#48616 = DIRECTION ( 'NONE',  ( -0.000000000000000000, -0.000000000000000000, 1.000000000000000000 ) ) ;
#48618 = ORIENTED_EDGE ( 'NONE', *, *, #460, .F. ) ;
#48619 = CARTESIAN_POINT ( 'NONE',  ( 113.4731498177359725, -46.72887913999166898, 68.02991099019695298 ) ) ;
#48620 = CIRCLE ( 'NONE', #73347, 2.517500000000000071 ) ;
#48621 = AXIS2_PLACEMENT_3D ( 'NONE', #29702, #8829, #203 ) ;
#48622 = CIRCLE ( 'NONE', #26928, 3.250000000000002665 ) ;
#48623 = EDGE_CURVE ( 'NONE', #17788, #72087, #74776, .T. ) ;
#48625 = CARTESIAN_POINT ( 'NONE',  ( 83.41556370846545576, 78.46683822716995849, -100.4327019155581979 ) ) ;
#48624 = DIRECTION ( 'NONE',  ( 0.000000000000000000, -1.000000000000000000, 0.000000000000000000 ) ) ;
#48626 = DIRECTION ( 'NONE',  ( 0.000000000000000000, -1.000000000000000000, 0.000000000000000000 ) ) ;
#48627 = EDGE_CURVE ( 'NONE', #79347, #35754, #46542, .T. ) ;
#48628 = DIRECTION ( 'NONE',  ( 0.000000000000000000, -1.000000000000000000, 0.000000000000000000 ) ) ;
#48629 = ORIENTED_EDGE ( 'NONE', *, *, #14660, .F. ) ;
#48630 = AXIS2_PLACEMENT_3D ( 'NONE', #36157, #29353, #49766 ) ;
#48631 = EDGE_CURVE ( 'NONE', #47902, #66479, #5233, .T. ) ;
#48632 = CARTESIAN_POINT ( 'NONE',  ( 116.3212776292293995, -32.94146857471267253, 120.1356252759109537 ) ) ;
#48633 = AXIS2_PLACEMENT_3D ( 'NONE', #15400, #43067, #6329 ) ;
#48634 = DIRECTION ( 'NONE',  ( 0.000000000000000000, -1.000000000000000000, 0.000000000000000000 ) ) ;
#48635 = CARTESIAN_POINT ( 'NONE',  ( 12.27510648567648133, 79.26588701359587219, 117.9188774285743762 ) ) ;
#48636 = ADVANCED_FACE ( 'NONE', ( #7911 ), #69249, .F. ) ;
#48637 = EDGE_LOOP ( 'NONE', ( #187, #42780, #70941, #37550 ) ) ;
#48639 = ADVANCED_FACE ( 'NONE', ( #70141, #77862 ), #22010, .F. ) ;
#48638 = CARTESIAN_POINT ( 'NONE',  ( 101.6669702799278525, -27.05833217848093497, 101.4937205140059575 ) ) ;
#48641 = CARTESIAN_POINT ( 'NONE',  ( 72.06648329127402519, -46.72944715994106701, -5.074374724089063982 ) ) ;
#48640 = CARTESIAN_POINT ( 'NONE',  ( -76.20505178924278766, 120.6499999999999915, -76.20505178924469192 ) ) ;
#48642 = PLANE ( 'NONE',  #45139 ) ;
#48643 = VECTOR ( 'NONE', #88129, 1000.000000000000000 ) ;
#48644 = EDGE_CURVE ( 'NONE', #31262, #88514, #21557, .T. ) ;
#48645 = VECTOR ( 'NONE', #23762, 1000.000000000000000 ) ;
#48647 = ADVANCED_FACE ( 'NONE', ( #42859 ), #35611, .F. ) ;
#48646 = CARTESIAN_POINT ( 'NONE',  ( 145.9305329516949143, -89.25781324566730746, 247.4783998280190076 ) ) ;
#48648 = ORIENTED_EDGE ( 'NONE', *, *, #60323, .F. ) ;
#48649 = CARTESIAN_POINT ( 'NONE',  ( 102.6065612795740805, -27.36740250608086100, 136.4422919425769578 ) ) ;
#48651 = ORIENTED_EDGE ( 'NONE', *, *, #81308, .T. ) ;
#48650 = DIRECTION ( 'NONE',  ( 1.000000000000000000, 0.000000000000000000, 0.000000000000000000 ) ) ;
#48652 = CARTESIAN_POINT ( 'NONE',  ( 96.93559702949583823, -34.21358363697174099, 272.1327681330538439 ) ) ;
#48653 = CARTESIAN_POINT ( 'NONE',  ( 97.81795488547844286, -40.53270472218247278, 252.6369010203054586 ) ) ;
#48654 = DIRECTION ( 'NONE',  ( -0.000000000000000000, -0.000000000000000000, -1.000000000000000000 ) ) ;
#48655 = DIRECTION ( 'NONE',  ( -1.000000000000000078E-15, 1.000000000000000083E-30, 1.000000000000000000 ) ) ;
#48656 = AXIS2_PLACEMENT_3D ( 'NONE', #19252, #19694, #87846 ) ;
#48657 = DIRECTION ( 'NONE',  ( 1.000000000000000078E-15, -1.000000000000000083E-30, -1.000000000000000000 ) ) ;
#48658 = ADVANCED_FACE ( 'NONE', ( #71055 ), #76055, .T. ) ;
#48659 = DIRECTION ( 'NONE',  ( -1.000000000000000078E-15, 1.000000000000000083E-30, 1.000000000000000000 ) ) ;
#48660 = DIRECTION ( 'NONE',  ( -0.9659258262890686453, 0.000000000000000000, 0.2588190451025194072 ) ) ;
#48661 = CARTESIAN_POINT ( 'NONE',  ( 116.5663773505005310, -40.88766770462213884, 208.4861014663879644 ) ) ;
#48662 = ORIENTED_EDGE ( 'NONE', *, *, #40853, .F. ) ;
#48663 = VERTEX_POINT ( 'NONE', #7018 ) ;
#48664 = EDGE_CURVE ( 'NONE', #30086, #78255, #77715, .T. ) ;
#48665 = AXIS2_PLACEMENT_3D ( 'NONE', #33100, #46710, #52610 ) ;
#48666 = CARTESIAN_POINT ( 'NONE',  ( 98.83447963006204873, -41.25831470702095061, 173.1463452106589784 ) ) ;
#48667 = CARTESIAN_POINT ( 'NONE',  ( -7.205548786489490269E-13, 127.0000000000000000, 103.1875000000000000 ) ) ;
#48668 = CARTESIAN_POINT ( 'NONE',  ( 115.7455327456632403, -41.23958449135837867, 284.4441967044819535 ) ) ;
#48669 = DIRECTION ( 'NONE',  ( 0.000000000000000000, 0.000000000000000000, -1.000000000000000000 ) ) ;
#48670 = CARTESIAN_POINT ( 'NONE',  ( -17.54031676229694270, 53.97499999999997300, 43.71138335376677020 ) ) ;
#48671 = CARTESIAN_POINT ( 'NONE',  ( 148.0533267522749838, 0.000000000000000000, -160.2664750769289697 ) ) ;
#48672 = CYLINDRICAL_SURFACE ( 'NONE', #49245, 25.39999999999999858 ) ;
#48673 = DIRECTION ( 'NONE',  ( 0.000000000000000000, 0.000000000000000000, -1.000000000000000000 ) ) ;
#48674 = CARTESIAN_POINT ( 'NONE',  ( 99.76842024043810397, -29.31547782932919688, 225.6956252759109702 ) ) ;
#48675 = CARTESIAN_POINT ( 'NONE',  ( 97.06386455791596291, -37.34269636115125479, 171.3750780254042070 ) ) ;
#48676 = ORIENTED_EDGE ( 'NONE', *, *, #71034, .F. ) ;
#48677 = ORIENTED_EDGE ( 'NONE', *, *, #16595, .T. ) ;
#48678 = EDGE_CURVE ( 'NONE', #39354, #87937, #36528, .T. ) ;
#48679 = CARTESIAN_POINT ( 'NONE',  ( 143.9834832912729894, -1.929447159941392931, 342.9256252759109316 ) ) ;
#48680 = CARTESIAN_POINT ( 'NONE',  ( -92.27768215249976436, 84.21498941703525531, -74.43373480440716605 ) ) ;
#48681 = LINE ( 'NONE', #42762, #6993 ) ;
#48683 = EDGE_CURVE ( 'NONE', #50282, #39081, #63326, .T. ) ;
#48682 = CARTESIAN_POINT ( 'NONE',  ( 107.0664832912748068, -36.72944715993923381, -5.074374724089029343 ) ) ;
#48685 = DIRECTION ( 'NONE',  ( 0.9963424814100680926, -0.08544974978095698503, 0.000000000000000000 ) ) ;
#48684 = VECTOR ( 'NONE', #29481, 999.9999999999998863 ) ;
#48686 = ORIENTED_EDGE ( 'NONE', *, *, #10710, .F. ) ;
#48687 = CARTESIAN_POINT ( 'NONE',  ( 111.1459338097010914, -47.05202348217205355, 18.88800622829195319 ) ) ;
#48688 = VECTOR ( 'NONE', #8719, 1000.000000000000000 ) ;
#48689 = CIRCLE ( 'NONE', #9567, 1.000000000000000888 ) ;
#48690 = CARTESIAN_POINT ( 'NONE',  ( 115.9600293333739387, -30.16561243848903828, 259.3203871806730945 ) ) ;
#48691 = VERTEX_POINT ( 'NONE', #643 ) ;
#48692 = CARTESIAN_POINT ( 'NONE',  ( 77.49051321911612433, -37.69637952316315221, 6.988870342670268521 ) ) ;
#48693 = CARTESIAN_POINT ( 'NONE',  ( 107.2978958415778123, -24.20855449189627251, 322.4523926293242653 ) ) ;
#48694 = CARTESIAN_POINT ( 'NONE',  ( 172.5664832912740110, -27.82844715994070484, 23.67562527591200094 ) ) ;
#48695 = CARTESIAN_POINT ( 'NONE',  ( 106.8900815348805509, -46.00655951153972723, 75.37951894101996686 ) ) ;
#48696 = CARTESIAN_POINT ( 'NONE',  ( 107.9200411489893412, -47.17696527638128856, 173.6413395616249886 ) ) ;
#48697 = CARTESIAN_POINT ( 'NONE',  ( 62.03742497533652767, -23.42844715994041493, 193.9678068554150911 ) ) ;
#48698 = VERTEX_POINT ( 'NONE', #42413 ) ;
#48699 = ADVANCED_FACE ( 'NONE', ( #34719 ), #27903, .T. ) ;
#48700 = VECTOR ( 'NONE', #67386, 1000.000000000000000 ) ;
#48701 = CYLINDRICAL_SURFACE ( 'NONE', #79936, 5.562600000000000655 ) ;
#48702 = ORIENTED_EDGE ( 'NONE', *, *, #19973, .T. ) ;
#48703 = EDGE_LOOP ( 'NONE', ( #34199, #80363, #8635, #77193 ) ) ;
#48704 = EDGE_CURVE ( 'NONE', #61361, #37855, #41463, .T. ) ;
#48705 = CARTESIAN_POINT ( 'NONE',  ( 10.33011338239549737, 89.94938708489701185, 118.1053235025621433 ) ) ;
#48706 = VERTEX_POINT ( 'NONE', #1999 ) ;
#48707 = ORIENTED_EDGE ( 'NONE', *, *, #38806, .T. ) ;
#48708 = CARTESIAN_POINT ( 'NONE',  ( -57.91199999999999903, 101.5999999999999943, 178.6098374884404905 ) ) ;
#48709 = AXIS2_PLACEMENT_3D ( 'NONE', #89558, #62734, #33690 ) ;
#48710 = CARTESIAN_POINT ( 'NONE',  ( 99.88917683200891418, -30.19057113389683167, 80.16099125664798919 ) ) ;
#48711 = CARTESIAN_POINT ( 'NONE',  ( 106.3003094972131208, -47.14862859053906874, 222.5184824187679453 ) ) ;
#48712 = CARTESIAN_POINT ( 'NONE',  ( 107.6532706963292725, -47.74396045468181882, 197.6308633711489620 ) ) ;
#48713 = CARTESIAN_POINT ( 'NONE',  ( 96.94236579736397630, -32.35154040576534840, 57.01372051400599616 ) ) ;
#48714 = DIRECTION ( 'NONE',  ( 0.000000000000000000, -0.5000000000000007772, 0.8660254037844381525 ) ) ;
#48715 = DIRECTION ( 'NONE',  ( 0.000000000000000000, -1.000000000000000000, 0.000000000000000000 ) ) ;
#48716 = ORIENTED_EDGE ( 'NONE', *, *, #9178, .T. ) ;
#48717 = CARTESIAN_POINT ( 'NONE',  ( 94.87702571208353675, -93.81616114448341648, -21.02845593540959968 ) ) ;
#48718 = CARTESIAN_POINT ( 'NONE',  ( 177.0371591254545649, -48.62818131005479927, 180.4678068554150059 ) ) ;
#48719 = ADVANCED_FACE ( 'NONE', ( #50125 ), #43311, .T. ) ;
#48720 = CARTESIAN_POINT ( 'NONE',  ( 108.4470127171752125, -27.04659769318750762, 104.9641967044829869 ) ) ;
#48721 = CARTESIAN_POINT ( 'NONE',  ( 101.1158648436187235, -27.35912039304959009, 65.51467289495799662 ) ) ;
#48722 = CARTESIAN_POINT ( 'NONE',  ( 116.2574608483823226, -41.81646255891691766, 263.4241967044824833 ) ) ;
#48723 = VERTEX_POINT ( 'NONE', #45527 ) ;
#48724 = CARTESIAN_POINT ( 'NONE',  ( 95.29485650985192535, -38.09666651163277606, 236.4184824187679510 ) ) ;
#48725 = DIRECTION ( 'NONE',  ( 0.0001713722455994998422, -0.9999999853157766072, 0.000000000000000000 ) ) ;
#48726 = LINE ( 'NONE', #13348, #55116 ) ;
#48727 = CARTESIAN_POINT ( 'NONE',  ( 98.60354758604864855, -42.06789318863769012, 27.77490799794517073 ) ) ;
#48728 = EDGE_CURVE ( 'NONE', #32371, #77722, #50580, .T. ) ;
#48730 = CARTESIAN_POINT ( 'NONE',  ( 68.69170846778827411, -139.3034517252403930, 245.6607681749549386 ) ) ;
#48729 = DIRECTION ( 'NONE',  ( -0.2884130866282260119, -0.7071067811865425767, 0.6456143519637603800 ) ) ;
#48731 = CARTESIAN_POINT ( 'NONE',  ( 107.0664832912739541, -36.72944715994095333, 309.2406250056037038 ) ) ;
#48732 = ADVANCED_FACE ( 'NONE', ( #71501 ), #24231, .F. ) ;
#48733 = DIRECTION ( 'NONE',  ( 0.7071067811865614505, -0.7071067811865336949, 0.000000000000000000 ) ) ;
#48734 = DIRECTION ( 'NONE',  ( 0.9068632946707807507, -0.4214249218767881500, 1.031805784967618114E-15 ) ) ;
#48735 = EDGE_CURVE ( 'NONE', #68783, #4380, #73249, .T. ) ;
#48736 = DIRECTION ( 'NONE',  ( 0.000000000000000000, 0.000000000000000000, 1.000000000000000000 ) ) ;
#48737 = CARTESIAN_POINT ( 'NONE',  ( 104.4836948513005552, -26.98053053655335276, 40.28118682077015222 ) ) ;
#48738 = DIRECTION ( 'NONE',  ( -7.497410362015770371E-15, 0.000000000000000000, 1.000000000000000000 ) ) ;
#48740 = ORIENTED_EDGE ( 'NONE', *, *, #32663, .F. ) ;
#48739 = CARTESIAN_POINT ( 'NONE',  ( 115.0889047219105663, -30.61763667692697055, 259.3439586095311142 ) ) ;
#48741 = EDGE_CURVE ( 'NONE', #10966, #3353, #11032, .T. ) ;
#48742 = DIRECTION ( 'NONE',  ( -0.7071067811865475727, -0.7071067811865475727, -1.287852911526280419E-16 ) ) ;
#48743 = CARTESIAN_POINT ( 'NONE',  ( 115.9256476412969192, -30.08033833575881033, 264.3508633711492735 ) ) ;
#48744 = CARTESIAN_POINT ( 'NONE',  ( 98.85664311730629095, -30.30429143764317601, 151.7984824187679465 ) ) ;
#48745 = CARTESIAN_POINT ( 'NONE',  ( 110.7484172854196629, -26.25849398357808084, 250.8194347997207387 ) ) ;
#48746 = VECTOR ( 'NONE', #47578, 1000.000000000000000 ) ;
#48747 = CARTESIAN_POINT ( 'NONE',  ( 0.000000000000000000, 50.79999999999999716, 258.6990000000000123 ) ) ;
#48749 = CARTESIAN_POINT ( 'NONE',  ( 81.62727349186259573, -34.46583755400396143, 7.833212107640068034 ) ) ;
#48748 = CARTESIAN_POINT ( 'NONE',  ( 142.8821648370248170, -72.54478064608022692, 396.9756252759102040 ) ) ;
#48750 = CARTESIAN_POINT ( 'NONE',  ( 104.4079917138377454, -46.45806025294579200, 138.3647832575413190 ) ) ;
#48751 = DIRECTION ( 'NONE',  ( 0.000000000000000000, 0.000000000000000000, 1.000000000000000000 ) ) ;
#48752 = AXIS2_PLACEMENT_3D ( 'NONE', #84008, #31590, #87023 ) ;
#48753 = EDGE_CURVE ( 'NONE', #80487, #40161, #29800, .T. ) ;
#48754 = VECTOR ( 'NONE', #7764, 1000.000000000000000 ) ;
#48755 = AXIS2_PLACEMENT_3D ( 'NONE', #36974, #64684, #83345 ) ;
#48756 = CIRCLE ( 'NONE', #42985, 5.041900000000000048 ) ;
#48757 = EDGE_LOOP ( 'NONE', ( #65145, #84960 ) ) ;
#48758 = CARTESIAN_POINT ( 'NONE',  ( -141.3509999999999991, 20.32000000000000028, 141.3509999999999991 ) ) ;
#48759 = ORIENTED_EDGE ( 'NONE', *, *, #14288, .F. ) ;
#48760 = EDGE_CURVE ( 'NONE', #20871, #20676, #45095, .T. ) ;
#48761 = CARTESIAN_POINT ( 'NONE',  ( 111.5068547175069824, -28.09499701576110198, 169.1209912566479545 ) ) ;
#48763 = VERTEX_POINT ( 'NONE', #37860 ) ;
#48762 = CARTESIAN_POINT ( 'NONE',  ( 91.91125933621930244, -98.95301919085837028, -21.02845593540826741 ) ) ;
#48764 = DIRECTION ( 'NONE',  ( 0.000000000000000000, 0.000000000000000000, -1.000000000000000000 ) ) ;
#48765 = CARTESIAN_POINT ( 'NONE',  ( 98.10941331148548272, -42.08998169807667722, 157.7556252759109725 ) ) ;
#48766 = PLANE ( 'NONE',  #39574 ) ;
#48767 = CARTESIAN_POINT ( 'NONE',  ( 115.8259185139441456, -31.73085971727213916, 149.2400304187415543 ) ) ;
#48768 = LINE ( 'NONE', #50116, #33995 ) ;
#48769 = CARTESIAN_POINT ( 'NONE',  ( 36.23715912545429063, -47.82818131006125384, 249.9678068554150343 ) ) ;
#48770 = LINE ( 'NONE', #35602, #42505 ) ;
#48772 = CARTESIAN_POINT ( 'NONE',  ( 102.0841886111852261, -27.63463957783707770, 100.4632443235309580 ) ) ;
#48771 = AXIS2_PLACEMENT_3D ( 'NONE', #59548, #38230, #73186 ) ;
#48773 = VERTEX_POINT ( 'NONE', #36956 ) ;
#48774 = ORIENTED_EDGE ( 'NONE', *, *, #83445, .T. ) ;
#48775 = ORIENTED_EDGE ( 'NONE', *, *, #4986, .T. ) ;
#48776 = CARTESIAN_POINT ( 'NONE',  ( 109.2565852557048629, -45.31616550848684000, 44.20729759161095984 ) ) ;
#48777 = DIRECTION ( 'NONE',  ( -1.000000000000000000, -1.092739197465703932E-16, 0.000000000000000000 ) ) ;
#48779 = CARTESIAN_POINT ( 'NONE',  ( -487.2989999999999782, 85.41360802895360393, 11.11250000000036131 ) ) ;
#48778 = CARTESIAN_POINT ( 'NONE',  ( 113.2095242374419541, -45.08419629851108823, 179.0689586092439640 ) ) ;
#48780 = VECTOR ( 'NONE', #54440, 999.9999999999998863 ) ;
#48781 = DIRECTION ( 'NONE',  ( 0.000000000000000000, 1.000000000000000000, 0.000000000000000000 ) ) ;
#48782 = CARTESIAN_POINT ( 'NONE',  ( 90.06670390244703128, -106.9675116026789539, -9.937637710809946512 ) ) ;
#48783 = DIRECTION ( 'NONE',  ( 0.000000000000000000, 0.000000000000000000, -1.000000000000000000 ) ) ;
#48784 = CARTESIAN_POINT ( 'NONE',  ( 37.03715912545348488, -48.62818131006127942, 117.4678068554150485 ) ) ;
#48785 = CARTESIAN_POINT ( 'NONE',  ( 0.000000000000000000, 95.00619999999999266, 0.000000000000000000 ) ) ;
#48786 = CARTESIAN_POINT ( 'NONE',  ( 102.7067583520260712, -46.86140753836549777, 137.2651490854349561 ) ) ;
#48787 = ORIENTED_EDGE ( 'NONE', *, *, #4784, .F. ) ;
#48788 = ORIENTED_EDGE ( 'NONE', *, *, #71963, .F. ) ;
#48789 = VERTEX_POINT ( 'NONE', #79210 ) ;
#48790 = CARTESIAN_POINT ( 'NONE',  ( 83.06670390244796920, -58.72944715994099596, 234.8338068554150198 ) ) ;
#48791 = CARTESIAN_POINT ( 'NONE',  ( 145.7412724758569027, -69.14289728258658840, 247.3817316427832793 ) ) ;
#48793 = EDGE_CURVE ( 'NONE', #2491, #76131, #38290, .T. ) ;
#48792 = CARTESIAN_POINT ( 'NONE',  ( 92.91125933621933086, -94.95109689075250969, -21.78219314458229405 ) ) ;
#48794 = CARTESIAN_POINT ( 'NONE',  ( 107.9397346479727418, -44.84530559174715592, 200.4795189410199612 ) ) ;
#48795 = LINE ( 'NONE', #50146, #40693 ) ;
#48796 = CARTESIAN_POINT ( 'NONE',  ( 97.33791405800978680, -34.07076917306103780, 27.11454834448431939 ) ) ;
#48797 = ORIENTED_EDGE ( 'NONE', *, *, #53651, .T. ) ;
#48799 = ORIENTED_EDGE ( 'NONE', *, *, #4663, .T. ) ;
#48798 = ORIENTED_EDGE ( 'NONE', *, *, #69567, .F. ) ;
#48800 = CARTESIAN_POINT ( 'NONE',  ( 136.7280559526967920, -19.42731094489385768, 2.974216770160625689 ) ) ;
#48801 = ORIENTED_EDGE ( 'NONE', *, *, #37751, .F. ) ;
#48802 = ORIENTED_EDGE ( 'NONE', *, *, #46827, .T. ) ;
#48803 = DIRECTION ( 'NONE',  ( 0.8660254037844379305, 0.000000000000000000, -0.5000000000000011102 ) ) ;
#48804 = CARTESIAN_POINT ( 'NONE',  ( 101.6974430329241272, -44.43982537643711339, 233.5120594963729559 ) ) ;
#48805 = CARTESIAN_POINT ( 'NONE',  ( 0.000000000000000000, 101.5999999999999943, 188.9759999999999991 ) ) ;
#48806 = VERTEX_POINT ( 'NONE', #58293 ) ;
#48807 = AXIS2_PLACEMENT_3D ( 'NONE', #10289, #3476, #44347 ) ;
#48808 = FACE_OUTER_BOUND ( 'NONE', #50466, .T. ) ;
#48809 = B_SPLINE_CURVE_WITH_KNOTS ( 'NONE', 3,
 ( #81363, #12752, #11, #6369, #88614, #74067, #34060, #60422, #61764, #41321, #6816, #34519, #88169, #19104, #46787, #77662, #84034, #14988, #21810, #49927, #69502, #8629, #56751, #28602, #56290, #42657, #48575, #84940, #43111, #15443, #29062, #76309, #8170, #41767, #36323, #21349, #7277, #905, #14543, #55388, #49480, #83585, #20902, #42221, #49023, #14082, #69950, #70857, #84497 ),
 .UNSPECIFIED., .F., .F.,
 ( 4, 2, 2, 2, 2, 2, 2, 2, 2, 2, 2, 2, 2, 2, 2, 1, 2, 2, 2, 2, 2, 2, 2, 2, 4 ),
 ( 0.01987186023414421951, 0.02111356671950570182, 0.02235527320486718761, 0.02483868617559015918, 0.02608039266095162761, 0.02732209914631309605, 0.02980551211703602946, 0.03228892508775896286, 0.03353063157312041048, 0.03477233805848185116, 0.03725575102920475334, 0.03849745751456622178, 0.03973916399992768328, 0.04222257697065066873, 0.04346428345601213716, 0.04470598994137360560, 0.04594769642673506710, 0.04718940291209652860, 0.04967281588281945159, 0.05091452236818091309, 0.05215622885354237459, 0.05463964182426531146, 0.05588134830962682154, 0.05712305479498831773, 0.05960646776571126848 ),
 .UNSPECIFIED. ) ;
#48810 = CARTESIAN_POINT ( 'NONE',  ( -122.5031070146980028, 73.82525647761227106, 45.14392447952047149 ) ) ;
#48811 = ORIENTED_EDGE ( 'NONE', *, *, #9012, .F. ) ;
#48812 = ORIENTED_EDGE ( 'NONE', *, *, #28939, .T. ) ;
#48813 = ADVANCED_FACE ( 'NONE', ( #30595 ), #24668, .T. ) ;
#48814 = VECTOR ( 'NONE', #44554, 1000.000000000000000 ) ;
#48815 = DIRECTION ( 'NONE',  ( 1.000000000000000078E-15, 1.000000000000000083E-30, -1.000000000000000000 ) ) ;
#48816 = CIRCLE ( 'NONE', #15530, 11.17600000000001970 ) ;
#48817 = ORIENTED_EDGE ( 'NONE', *, *, #65605, .F. ) ;
#48818 = VERTEX_POINT ( 'NONE', #16967 ) ;
#48819 = CARTESIAN_POINT ( 'NONE',  ( 99.35431583021956214, -34.05534528112548287, 283.8795189410199100 ) ) ;
#48820 = CARTESIAN_POINT ( 'NONE',  ( 97.96720171806632038, -41.86261760143219846, 136.7356252759109623 ) ) ;
#48821 = CARTESIAN_POINT ( 'NONE',  ( 112.5028774994482035, -27.85959465031275784, 94.63848241876793566 ) ) ;
#48822 = DIRECTION ( 'NONE',  ( 1.000000000000000000, 0.000000000000000000, 0.000000000000000000 ) ) ;
#48823 =( LENGTH_UNIT ( ) NAMED_UNIT ( * ) SI_UNIT ( .MILLI., .METRE. ) );
#48824 = CARTESIAN_POINT ( 'NONE',  ( 116.5266666817545627, -41.19333145446972821, 224.4756252759109714 ) ) ;
#48825 = CYLINDRICAL_SURFACE ( 'NONE', #44304, 0.4999999999999932832 ) ;
#48826 = LINE ( 'NONE', #1617, #42204 ) ;
#48827 = ORIENTED_EDGE ( 'NONE', *, *, #40259, .T. ) ;
#48828 = CARTESIAN_POINT ( 'NONE',  ( 130.4363378768869381, 71.14122173980733521, 5.641126054321851768 ) ) ;
#48829 = VERTEX_POINT ( 'NONE', #23795 ) ;
#48830 = ORIENTED_EDGE ( 'NONE', *, *, #44221, .T. ) ;
#48831 = FACE_OUTER_BOUND ( 'NONE', #1253, .T. ) ;
#48832 = CARTESIAN_POINT ( 'NONE',  ( 107.8158413964318925, -26.73611026959684267, 136.0168363452475546 ) ) ;
#48833 = CIRCLE ( 'NONE', #3922, 88.90000000000000568 ) ;
#48834 = ORIENTED_EDGE ( 'NONE', *, *, #85066, .F. ) ;
#48835 = CARTESIAN_POINT ( 'NONE',  ( 96.67071733825032709, -35.94615501309311156, 146.2670538473399517 ) ) ;
#48836 = CARTESIAN_POINT ( 'NONE',  ( -12.62696438262051046, 80.95609589054741662, 129.9443975344997284 ) ) ;
#48837 = DIRECTION ( 'NONE',  ( 0.000000000000000000, -1.000000000000000000, 0.000000000000000000 ) ) ;
#48838 = DIRECTION ( 'NONE',  ( 0.000000000000000000, -1.000000000000000000, 0.000000000000000000 ) ) ;
#48841 = CARTESIAN_POINT ( 'NONE',  ( 115.3705510513157009, -30.46277945167186374, 215.3413395616249773 ) ) ;
#48840 = DIRECTION ( 'NONE',  ( -1.000000000000000078E-15, -1.000000000000000000, 0.000000000000000000 ) ) ;
#48839 = CARTESIAN_POINT ( 'NONE',  ( 7.661254700127833495, 95.64746158385918307, 317.6630000000000109 ) ) ;
#48842 = CARTESIAN_POINT ( 'NONE',  ( 194.0667039024482392, -40.32844715993407192, 129.9678068554150343 ) ) ;
#48843 = EDGE_CURVE ( 'NONE', #31385, #48257, #38735, .T. ) ;
#48844 = PLANE ( 'NONE',  #6177 ) ;
#48845 = ORIENTED_EDGE ( 'NONE', *, *, #67538, .T. ) ;
#48846 = CARTESIAN_POINT ( 'NONE',  ( 80.06648329127399677, -8.729447159940999512, 311.1531252759119752 ) ) ;
#48847 = EDGE_CURVE ( 'NONE', #51938, #56684, #3780, .T. ) ;
#48848 = CARTESIAN_POINT ( 'NONE',  ( 110.0667047667142953, -67.87844715994094713, 93.21780685541800437 ) ) ;
#48849 = EDGE_CURVE ( 'NONE', #62608, #6901, #31469, .T. ) ;
#48850 = FACE_OUTER_BOUND ( 'NONE', #28856, .T. ) ;
#48851 = FACE_OUTER_BOUND ( 'NONE', #6069, .T. ) ;
#48853 = VERTEX_POINT ( 'NONE', #80099 ) ;
#48852 = CARTESIAN_POINT ( 'NONE',  ( 101.0612956599395602, -45.30524461813642745, 282.0899109901967563 ) ) ;
#48854 = EDGE_CURVE ( 'NONE', #55635, #86394, #85583, .T. ) ;
#48855 = DIRECTION ( 'NONE',  ( 2.089354330573420398E-14, 0.000000000000000000, 1.000000000000000000 ) ) ;
#48856 = CARTESIAN_POINT ( 'NONE',  ( 95.65096329713743728, -33.45531905120653704, 141.1041967044829732 ) ) ;
#48857 = CARTESIAN_POINT ( 'NONE',  ( 117.4876440797474828, -37.01562065295904347, 39.80419670448193159 ) ) ;
#48858 = CARTESIAN_POINT ( 'NONE',  ( 109.4552518484143206, -25.89010755186295754, 175.8918157521009391 ) ) ;
#48859 = CARTESIAN_POINT ( 'NONE',  ( 107.0667039024470313, -104.2784471599421323, -21.78219314458201694 ) ) ;
#48860 = CARTESIAN_POINT ( 'NONE',  ( -7.941868552260229762E-13, 120.6499999999999915, 107.7702177616926065 ) ) ;
#48862 = CARTESIAN_POINT ( 'NONE',  ( 191.6375511031381222, 22.69262065192312150, 361.9756252759109998 ) ) ;
#48861 = DIRECTION ( 'NONE',  ( 1.000000000000000078E-15, 0.000000000000000000, 1.000000000000000000 ) ) ;
#48863 = CARTESIAN_POINT ( 'NONE',  ( 57.56670390244832447, -48.82844715994039575, 257.2178068554150627 ) ) ;
#48864 = LINE ( 'NONE', #69787, #84494 ) ;
#48865 = ORIENTED_EDGE ( 'NONE', *, *, #23759, .T. ) ;
#48866 = AXIS2_PLACEMENT_3D ( 'NONE', #3300, #85540, #9656 ) ;
#48867 = CARTESIAN_POINT ( 'NONE',  ( 70.14948329127297200, -1.929447159941395817, 342.9256252759109884 ) ) ;
#48868 = EDGE_LOOP ( 'NONE', ( #54885, #38714, #20678, #54896 ) ) ;
#48869 = ORIENTED_EDGE ( 'NONE', *, *, #48351, .T. ) ;
#48870 = EDGE_CURVE ( 'NONE', #32697, #88397, #86024, .T. ) ;
#48871 = ORIENTED_EDGE ( 'NONE', *, *, #42484, .F. ) ;
#48872 = CARTESIAN_POINT ( 'NONE',  ( 96.73644666290624627, -38.23103596604165233, 62.44133956162495025 ) ) ;
#48873 = LINE ( 'NONE', #76155, #58556 ) ;
#48874 = DIRECTION ( 'NONE',  ( 1.000000000000000000, 1.150535366796005147E-15, -4.666596370676151832E-30 ) ) ;
#48875 = CARTESIAN_POINT ( 'NONE',  ( 108.9530382828359052, -26.39605832486118331, 160.9327681330539690 ) ) ;
#48876 = CIRCLE ( 'NONE', #19915, 2.030000000000003801 ) ;
#48877 = CARTESIAN_POINT ( 'NONE',  ( 114.3094922386577110, -31.29331878451978355, 263.7733722090294464 ) ) ;
#48878 = ORIENTED_EDGE ( 'NONE', *, *, #1399, .F. ) ;
#48879 = ORIENTED_EDGE ( 'NONE', *, *, #46651, .F. ) ;
#48880 = ORIENTED_EDGE ( 'NONE', *, *, #257, .F. ) ;
#48881 = VECTOR ( 'NONE', #63637, 1000.000000000000114 ) ;
#48882 = VECTOR ( 'NONE', #337, 1000.000000000000000 ) ;
#48883 = CARTESIAN_POINT ( 'NONE',  ( 112.0659116249482423, -45.48839625912368945, 107.9897919428080684 ) ) ;
#48884 = DIRECTION ( 'NONE',  ( -0.7071067811865171526, -0.7071067811865779928, -7.071067811865164719E-16 ) ) ;
#48885 = AXIS2_PLACEMENT_3D ( 'NONE', #22474, #86046, #50150 ) ;
#48886 = LINE ( 'NONE', #70710, #30368 ) ;
#48887 = CARTESIAN_POINT ( 'NONE',  ( 99.09610799260327951, -30.54990352127401110, 20.80127292277482098 ) ) ;
#48888 = CARTESIAN_POINT ( 'NONE',  ( 83.40142812120517135, 86.64186789594788252, 100.4448767513726466 ) ) ;
#48889 = DIRECTION ( 'NONE',  ( 1.000000000000000078E-15, -1.000000000000000083E-30, -1.000000000000000000 ) ) ;
#48890 = DIRECTION ( 'NONE',  ( 0.7071067811865510144, 0.000000000000000000, -0.7071067811865441310 ) ) ;
#48891 = DIRECTION ( 'NONE',  ( 1.000000000000000000, 0.000000000000000000, 0.000000000000000000 ) ) ;
#48892 = CARTESIAN_POINT ( 'NONE',  ( 111.0379167980823496, -47.01981040405703993, 17.85753003781598380 ) ) ;
#48893 = DIRECTION ( 'NONE',  ( -0.9999999853157766072, -0.0001713722456133601202, 9.999999853157765648E-16 ) ) ;
#48894 = ORIENTED_EDGE ( 'NONE', *, *, #16873, .T. ) ;
#48895 = DIRECTION ( 'NONE',  ( 0.000000000000000000, 0.000000000000000000, -1.000000000000000000 ) ) ;
#48896 = AXIS2_PLACEMENT_3D ( 'NONE', #48326, #5239, #54693 ) ;
#48897 = CIRCLE ( 'NONE', #22813, 2.117000000000007987 ) ;
#48899 = ADVANCED_FACE ( 'NONE', ( #44652 ), #9705, .F. ) ;
#48898 = DIRECTION ( 'NONE',  ( 1.000000000000000000, 0.000000000000000000, 0.000000000000000000 ) ) ;
#48900 = CARTESIAN_POINT ( 'NONE',  ( 104.5412336160381273, -44.52083999592182550, 80.14523322673395000 ) ) ;
#48901 = ADVANCED_FACE ( 'NONE', ( #31033 ), #78768, .T. ) ;
#48902 = CARTESIAN_POINT ( 'NONE',  ( 3.968749999999229949, 120.6499999999999915, 100.8961411191535973 ) ) ;
#48903 = CARTESIAN_POINT ( 'NONE',  ( 176.7738106836353325, -48.62134037874481862, 300.4678068554149490 ) ) ;
#48904 = ORIENTED_EDGE ( 'NONE', *, *, #38910, .T. ) ;
#48905 = ORIENTED_EDGE ( 'NONE', *, *, #347, .T. ) ;
#48906 = DIRECTION ( 'NONE',  ( 0.9242245927363031965, 0.3818493186865917766, 0.000000000000000000 ) ) ;
#48907 = VERTEX_POINT ( 'NONE', #79656 ) ;
#48908 = ORIENTED_EDGE ( 'NONE', *, *, #27127, .T. ) ;
#48909 = CARTESIAN_POINT ( 'NONE',  ( 115.7831076793861200, -41.80230949354785253, 69.40645861076393430 ) ) ;
#48910 = CARTESIAN_POINT ( 'NONE',  ( 99.14414808984345484, -41.78050036225572228, 138.1977737820869834 ) ) ;
#48911 = CARTESIAN_POINT ( 'NONE',  ( -9.572570118836543074, 90.93799233918605296, 118.1704038715884053 ) ) ;
#48912 = CARTESIAN_POINT ( 'NONE',  ( 97.52247766716473620, -32.48101032970659219, 96.99276813305395706 ) ) ;
#48913 = VECTOR ( 'NONE', #68441, 1000.000000000000000 ) ;
#48914 = CARTESIAN_POINT ( 'NONE',  ( -492.0614999999999668, 14.28749999999982201, 90.48749999999999716 ) ) ;
#48915 = ORIENTED_EDGE ( 'NONE', *, *, #69352, .F. ) ;
#48916 = EDGE_CURVE ( 'NONE', #75012, #74274, #86902, .T. ) ;
#48917 = DIRECTION ( 'NONE',  ( 0.000000000000000000, 1.000000000000000000, 1.541976423090495239E-15 ) ) ;
#48918 = VERTEX_POINT ( 'NONE', #33722 ) ;
#48919 = ORIENTED_EDGE ( 'NONE', *, *, #7878, .T. ) ;
#48920 = CARTESIAN_POINT ( 'NONE',  ( -72.96458098368751166, 127.0000000000000000, 65.02708098368620426 ) ) ;
#48921 = EDGE_LOOP ( 'NONE', ( #83972, #14453 ) ) ;
#48922 = CARTESIAN_POINT ( 'NONE',  ( 110.6561457788925793, -27.59554888373224557, 269.7784824187687605 ) ) ;
#48923 = CARTESIAN_POINT ( 'NONE',  ( 117.3128790654603080, -34.51798396817098080, 179.9956252759109532 ) ) ;
#48924 = DIRECTION ( 'NONE',  ( 1.000000000000000078E-15, 1.000000000000000083E-30, -1.000000000000000000 ) ) ;
#48925 = DIRECTION ( 'NONE',  ( 0.000000000000000000, 0.000000000000000000, -1.000000000000000000 ) ) ;
#48926 = CARTESIAN_POINT ( 'NONE',  ( 112.8017646537355176, -47.09965271489118521, 98.97848241876793907 ) ) ;
#48927 = CARTESIAN_POINT ( 'NONE',  ( 115.7831076762087577, -41.80230949924659711, 263.4064586102478529 ) ) ;
#48928 = ORIENTED_EDGE ( 'NONE', *, *, #64657, .T. ) ;
#48929 = CARTESIAN_POINT ( 'NONE',  ( 97.39154043693341123, -39.27946349389958414, 116.5321201934415285 ) ) ;
#48930 = ADVANCED_FACE ( 'NONE', ( #60974, #68248, #32355 ), #40529, .T. ) ;
#48931 = VECTOR ( 'NONE', #19140, 1000.000000000000114 ) ;
#48932 = CARTESIAN_POINT ( 'NONE',  ( 101.9936390655985292, -45.44609458172816119, 133.1574646095896810 ) ) ;
#48933 = VERTEX_POINT ( 'NONE', #40972 ) ;
#48934 = CIRCLE ( 'NONE', #69341, 13.16666666666670160 ) ;
#48935 = LINE ( 'NONE', #14458, #70724 ) ;
#48936 = AXIS2_PLACEMENT_3D ( 'NONE', #59122, #71891, #38683 ) ;
#48937 = CARTESIAN_POINT ( 'NONE',  ( 97.49412692080079523, -39.74150246419772259, 132.5691861445521056 ) ) ;
#48938 = CARTESIAN_POINT ( 'NONE',  ( 104.6488677213912695, -47.51528149961286829, 27.38895860924395009 ) ) ;
#48939 = DIRECTION ( 'NONE',  ( 1.000000000000000078E-15, -1.000000000000000000, 0.000000000000000000 ) ) ;
#48940 = CARTESIAN_POINT ( 'NONE',  ( 107.0667039024470313, -104.2784471599420897, -20.48315503890502143 ) ) ;
#48941 = DIRECTION ( 'NONE',  ( 1.000000000000000078E-15, -1.000000000000000083E-30, -1.000000000000000000 ) ) ;
#48942 = CARTESIAN_POINT ( 'NONE',  ( 104.8797383215544556, -46.86635653470259655, 32.41943479972098174 ) ) ;
#48944 = CARTESIAN_POINT ( 'NONE',  ( 99.07096106853141748, -43.38529345585680375, 112.8784824187679732 ) ) ;
#48943 = CARTESIAN_POINT ( 'NONE',  ( 109.7246617015826331, -27.00074531322127669, 109.8648087393802086 ) ) ;
#48945 = CARTESIAN_POINT ( 'NONE',  ( 115.8254323917127664, -31.73001882825242959, 70.23979194262223302 ) ) ;
#48946 = CARTESIAN_POINT ( 'NONE',  ( 177.0371591254545649, -48.62818131005479927, 180.4678068554150059 ) ) ;
#48947 = ORIENTED_EDGE ( 'NONE', *, *, #2861, .F. ) ;
#48948 = LINE ( 'NONE', #42586, #20755 ) ;
#48949 = AXIS2_PLACEMENT_3D ( 'NONE', #32484, #23477, #9834 ) ;
#48950 = FACE_BOUND ( 'NONE', #24606, .T. ) ;
#48951 = CARTESIAN_POINT ( 'NONE',  ( 136.5970450997408534, -35.65293374834303819, 2.807537076564766920 ) ) ;
#48953 = VERTEX_POINT ( 'NONE', #26015 ) ;
#48952 = ADVANCED_FACE ( 'NONE', ( #54128 ), #75058, .F. ) ;
#48954 = VECTOR ( 'NONE', #52944, 1000.000000000000000 ) ;
#48955 = CARTESIAN_POINT ( 'NONE',  ( -27.27158787008326968, 184.0000000000000000, 106.1020876358972771 ) ) ;
#48957 = ORIENTED_EDGE ( 'NONE', *, *, #63859, .T. ) ;
#48956 = CARTESIAN_POINT ( 'NONE',  ( 101.7470617766046956, -45.74667603143129924, 162.1527681330539679 ) ) ;
#48958 = CARTESIAN_POINT ( 'NONE',  ( 91.42390633313587500, -35.38788608837992911, 293.6356252759109680 ) ) ;
#48959 = CARTESIAN_POINT ( 'NONE',  ( 96.83718905160354495, -34.60841009949970726, 212.1641967044819808 ) ) ;
#48960 = CARTESIAN_POINT ( 'NONE',  ( 105.9839165226978110, -26.31690525417204540, 46.15848241876796720 ) ) ;
#48961 = CIRCLE ( 'NONE', #66345, 11.45913725231036118 ) ;
#48962 = CARTESIAN_POINT ( 'NONE',  ( 99.08946256649485917, -109.4614598618336174, 2.217806855418169576 ) ) ;
#48963 = VECTOR ( 'NONE', #68520, 1000.000000000000000 ) ;
#48964 = LINE ( 'NONE', #19948, #77879 ) ;
#48965 = CARTESIAN_POINT ( 'NONE',  ( 117.0608945238105463, -38.08045311834111146, 78.71895860944069057 ) ) ;
#48966 = ORIENTED_EDGE ( 'NONE', *, *, #7024, .T. ) ;
#48967 = VECTOR ( 'NONE', #70477, 1000.000000000000000 ) ;
#48968 = CONTEXT_DEPENDENT_SHAPE_REPRESENTATION ( #4567, #11925 ) ;
#48969 = ORIENTED_EDGE ( 'NONE', *, *, #70347, .T. ) ;
#48970 = ORIENTED_EDGE ( 'NONE', *, *, #43001, .F. ) ;
#48971 = EDGE_CURVE ( 'NONE', #18271, #68666, #12844, .T. ) ;
#48972 = EDGE_LOOP ( 'NONE', ( #4207, #68750, #18548, #6282 ) ) ;
#48973 = CARTESIAN_POINT ( 'NONE',  ( 184.5667039024485518, -48.82844715993447693, 180.4678068554150343 ) ) ;
#48974 = CARTESIAN_POINT ( 'NONE',  ( 97.01652928432748979, -33.95800134492240119, 247.1127681330539758 ) ) ;
#48975 = CARTESIAN_POINT ( 'NONE',  ( 97.66492352869934734, -33.15663352981950140, 251.0373582895531399 ) ) ;
#48976 = EDGE_CURVE ( 'NONE', #6767, #85401, #73348, .T. ) ;
#48977 = DIRECTION ( 'NONE',  ( 0.000000000000000000, 0.000000000000000000, 1.000000000000000000 ) ) ;
#48979 = CARTESIAN_POINT ( 'NONE',  ( 168.3664380525669912, -48.62818131005477795, 180.4678068554150059 ) ) ;
#48978 = LINE ( 'NONE', #63530, #61292 ) ;
#48980 = FACE_OUTER_BOUND ( 'NONE', #61445, .T. ) ;
#48981 = CARTESIAN_POINT ( 'NONE',  ( 115.6914824993820901, -43.67961476919119690, 43.27467289495795200 ) ) ;
#48982 = ORIENTED_EDGE ( 'NONE', *, *, #36381, .F. ) ;
#48983 = B_SPLINE_CURVE_WITH_KNOTS ( 'NONE', 3,
 ( #23278, #36439, #22815, #57760, #70054, #552, #1914, #85045, #50490, #43677, #9175, #36875, #64583, #50942, #78687, #51372, #37773, #31833, #72298, #4134, #45443, #59969, #30507, #30949, #32274 ),
 .UNSPECIFIED., .F., .F.,
 ( 4, 2, 2, 1, 2, 2, 2, 2, 2, 2, 2, 2, 4 ),
 ( 0.03942124974134118831, 0.04188566783051467235, 0.04311787687510139355, 0.04435008591968810782, 0.04558229496427482902, 0.04681450400886155022, 0.04927892209803499957, 0.05051113114262172077, 0.05174334018720844891, 0.05420775827638189825, 0.05543996732096862640, 0.05667217636555535454, 0.05913659445472881082 ),
 .UNSPECIFIED. ) ;
#48984 = ORIENTED_EDGE ( 'NONE', *, *, #7630, .T. ) ;
#48985 = CARTESIAN_POINT ( 'NONE',  ( 172.5664832912729878, -27.82844715994070484, 258.9256252759120116 ) ) ;
#48986 = CARTESIAN_POINT ( 'NONE',  ( -446.0240000000000009, 53.97500000000000853, 101.5999999999999943 ) ) ;
#48987 = CARTESIAN_POINT ( 'NONE',  ( 100.0046238269857639, -29.91446987444276928, 246.7156252759109520 ) ) ;
#48988 = CARTESIAN_POINT ( 'NONE',  ( -7.301849239715819957E-13, 120.6499999999999915, 98.60478223830740774 ) ) ;
#48989 = CARTESIAN_POINT ( 'NONE',  ( 109.6029845306728134, -46.78454271877401283, 88.78514908543394313 ) ) ;
#48990 = LINE ( 'NONE', #21317, #82129 ) ;
#48991 = CARTESIAN_POINT ( 'NONE',  ( 103.2779527552481795, -27.47487875237766630, 21.38567362161598595 ) ) ;
#48992 = ORIENTED_EDGE ( 'NONE', *, *, #54781, .F. ) ;
#48993 = DIRECTION ( 'NONE',  ( -0.1315836003796857501, 0.7863649282873461654, -0.6035859140758308428 ) ) ;
#48994 = AXIS2_PLACEMENT_3D ( 'NONE', #28067, #61687, #68971 ) ;
#48995 = ORIENTED_EDGE ( 'NONE', *, *, #4332, .T. ) ;
#48996 = ORIENTED_EDGE ( 'NONE', *, *, #27552, .F. ) ;
#48997 = CARTESIAN_POINT ( 'NONE',  ( -86.67392531623309537, 94.60304557064715425, 80.89343850130832436 ) ) ;
#48998 = CARTESIAN_POINT ( 'NONE',  ( 99.03278789346684619, -40.46950289042285220, 253.1044404487540760 ) ) ;
#48999 = VECTOR ( 'NONE', #18495, 1000.000000000000000 ) ;
#49000 = CARTESIAN_POINT ( 'NONE',  ( 179.4595971212720258, -26.00627455219131789, 193.9678068554150059 ) ) ;
#49001 = VECTOR ( 'NONE', #7659, 1000.000000000000000 ) ;
#49002 = CARTESIAN_POINT ( 'NONE',  ( -118.1709372608868875, 90.93089219781630561, 9.551212252129760216 ) ) ;
#49003 = EDGE_CURVE ( 'NONE', #9196, #82603, #11490, .T. ) ;
#49004 = CARTESIAN_POINT ( 'NONE',  ( 115.8254323923647604, -31.73001882984776501, 84.23979194248457247 ) ) ;
#49005 = CARTESIAN_POINT ( 'NONE',  ( 91.11526841082624628, 75.84278307195158675, -75.85240403722320934 ) ) ;
#49006 = ORIENTED_EDGE ( 'NONE', *, *, #58998, .T. ) ;
#49007 = LINE ( 'NONE', #61750, #53635 ) ;
#49008 = CIRCLE ( 'NONE', #60630, 3.299999999999999822 ) ;
#49009 = LINE ( 'NONE', #48559, #61469 ) ;
#49010 = ORIENTED_EDGE ( 'NONE', *, *, #44435, .F. ) ;
#49011 = CARTESIAN_POINT ( 'NONE',  ( 114.0907319755898186, -46.27410096495736269, 33.08133956162495792 ) ) ;
#49012 = ORIENTED_EDGE ( 'NONE', *, *, #22276, .T. ) ;
#49013 = CARTESIAN_POINT ( 'NONE',  ( 114.3408732721816534, -41.20596775705023163, 17.80956268521999419 ) ) ;
#49014 = AXIS2_PLACEMENT_3D ( 'NONE', #54178, #32863, #87844 ) ;
#49015 = DIRECTION ( 'NONE',  ( -4.237773401492740281E-14, 1.000000000000000000, 0.000000000000000000 ) ) ;
#49016 = CARTESIAN_POINT ( 'NONE',  ( 102.2986265273211188, -45.30740241592388884, 187.1727681330549729 ) ) ;
#49017 = CARTESIAN_POINT ( 'NONE',  ( 23.35552145179432770, 78.96279258983980753, 299.7471977194603028 ) ) ;
#49018 = DIRECTION ( 'NONE',  ( -1.000000000000000000, -2.756263715554006823E-15, 0.000000000000000000 ) ) ;
#49019 = VECTOR ( 'NONE', #76742, 1000.000000000000000 ) ;
#49020 = CARTESIAN_POINT ( 'NONE',  ( 32.15435173586061524, -31.62489322948298209, 193.9678068554150911 ) ) ;
#49021 = CARTESIAN_POINT ( 'NONE',  ( 7.305616351080206350, 72.16134662172612479, 130.3514124915961645 ) ) ;
#49022 = CARTESIAN_POINT ( 'NONE',  ( 112.2081591769286177, -26.91769754996824560, 10.68038718067299087 ) ) ;
#49023 = CARTESIAN_POINT ( 'NONE',  ( 74.70172715947563802, 85.83559868056556752, -92.06080542007434531 ) ) ;
#49024 = EDGE_LOOP ( 'NONE', ( #19332, #74471, #26409, #15714 ) ) ;
#49025 = DIRECTION ( 'NONE',  ( 0.000000000000000000, 0.000000000000000000, -1.000000000000000000 ) ) ;
#49026 = ORIENTED_EDGE ( 'NONE', *, *, #36908, .F. ) ;
#49027 = CARTESIAN_POINT ( 'NONE',  ( 104.0954500313802527, -46.76767116204542418, 103.3470538473389411 ) ) ;
#49028 = EDGE_CURVE ( 'NONE', #10129, #32950, #12381, .T. ) ;
#49029 = DIRECTION ( 'NONE',  ( 0.000000000000000000, 0.000000000000000000, 1.000000000000000000 ) ) ;
#49030 = ORIENTED_EDGE ( 'NONE', *, *, #79684, .T. ) ;
#49031 = LINE ( 'NONE', #21359, #47037 ) ;
#49032 = VERTEX_POINT ( 'NONE', #81450 ) ;
#49033 = ORIENTED_EDGE ( 'NONE', *, *, #60031, .F. ) ;
#49034 = VECTOR ( 'NONE', #1380, 999.9999999999998863 ) ;
#49035 = EDGE_CURVE ( 'NONE', #77239, #11120, #40073, .T. ) ;
#49036 = DIRECTION ( 'NONE',  ( 0.000000000000000000, 0.000000000000000000, -1.000000000000000000 ) ) ;
#49037 = CARTESIAN_POINT ( 'NONE',  ( 38.10000000000000142, 69.84999999999999432, 358.0130000000000337 ) ) ;
#49038 = LINE ( 'NONE', #42674, #29801 ) ;
#49039 = CARTESIAN_POINT ( 'NONE',  ( 29.56670390244797630, -48.82844715994099971, 20.91780685541479912 ) ) ;
#49040 = DIRECTION ( 'NONE',  ( 1.000000000000000078E-15, -1.000000000000000083E-30, -1.000000000000000000 ) ) ;
#49041 = CARTESIAN_POINT ( 'NONE',  ( 112.7646070568428911, -30.84607450481293256, 172.2823760838769829 ) ) ;
#49042 = CARTESIAN_POINT ( 'NONE',  ( 115.7943364950945977, -30.98820711043258669, 250.2899109901966028 ) ) ;
#49043 = EDGE_CURVE ( 'NONE', #33687, #61833, #5118, .T. ) ;
#49044 = CARTESIAN_POINT ( 'NONE',  ( -454.6936515812919879, 53.97500000000000142, 3.174999999999999822 ) ) ;
#49045 = VERTEX_POINT ( 'NONE', #61411 ) ;
#49046 = CARTESIAN_POINT ( 'NONE',  ( 4.867662263754145791, 70.79804876089910692, 118.4578822119320023 ) ) ;
#49047 = EDGE_CURVE ( 'NONE', #63446, #48213, #6460, .T. ) ;
#49048 = CARTESIAN_POINT ( 'NONE',  ( 134.4433815842106412, -39.47944715994101017, 1.625625275910999257 ) ) ;
#49049 = ORIENTED_EDGE ( 'NONE', *, *, #14554, .F. ) ;
#49051 = EDGE_LOOP ( 'NONE', ( #2498, #42916, #75496, #60408 ) ) ;
#49050 = VECTOR ( 'NONE', #66248, 1000.000000000000000 ) ;
#49052 = EDGE_CURVE ( 'NONE', #16389, #64803, #47775, .T. ) ;
#49053 = CARTESIAN_POINT ( 'NONE',  ( 82.32434691321189746, -20.30306751045458213, 2.518077574347549419 ) ) ;
#49054 = FACE_OUTER_BOUND ( 'NONE', #53104, .T. ) ;
#49055 = CARTESIAN_POINT ( 'NONE',  ( 98.34981380874698687, -31.65666098073609191, 15.90646538746769778 ) ) ;
#49056 = EDGE_CURVE ( 'NONE', #23436, #12855, #89140, .T. ) ;
#49057 = DIRECTION ( 'NONE',  ( 0.000000000000000000, 0.000000000000000000, -1.000000000000000000 ) ) ;
#49058 = FACE_OUTER_BOUND ( 'NONE', #44537, .T. ) ;
#49059 = CARTESIAN_POINT ( 'NONE',  ( 100.0786887504289666, -31.81753722825460429, 205.2609912566479693 ) ) ;
#49060 = CARTESIAN_POINT ( 'NONE',  ( 97.18391573584769105, -31.67496972499959895, 95.96229194257799122 ) ) ;
#49061 = ORIENTED_EDGE ( 'NONE', *, *, #65373, .F. ) ;
#49062 = DIRECTION ( 'NONE',  ( -0.7071067811864634178, 0.7071067811866316166, -7.071067811864642099E-16 ) ) ;
#49063 = EDGE_LOOP ( 'NONE', ( #68351, #71266, #52444, #16124 ) ) ;
#49064 = CARTESIAN_POINT ( 'NONE',  ( 52.65249034007831597, -48.32844715994060181, 249.9678068554150343 ) ) ;
#49066 = EDGE_LOOP ( 'NONE', ( #18050, #82095, #34371 ) ) ;
#49065 = EDGE_CURVE ( 'NONE', #30543, #78177, #60512, .T. ) ;
#49067 = CIRCLE ( 'NONE', #25877, 160.4955849403809793 ) ;
#49068 = CARTESIAN_POINT ( 'NONE',  ( 74.06670390244704549, -118.2784471599409812, 45.21780685541799727 ) ) ;
#49069 = ORIENTED_EDGE ( 'NONE', *, *, #67114, .T. ) ;
#49070 = FACE_OUTER_BOUND ( 'NONE', #12244, .T. ) ;
#49071 = CARTESIAN_POINT ( 'NONE',  ( 69.26949937496601706, -71.54137415153812185, 394.9756252759101471 ) ) ;
#49072 = CARTESIAN_POINT ( 'NONE',  ( 73.17003668186728760, -8.979447159941065237, -5.074374724089063982 ) ) ;
#49074 = LINE ( 'NONE', #61815, #77092 ) ;
#49073 = VECTOR ( 'NONE', #57262, 1000.000000000000000 ) ;
#49075 = ORIENTED_EDGE ( 'NONE', *, *, #42716, .T. ) ;
#49076 = CIRCLE ( 'NONE', #50513, 0.5000000000000004441 ) ;
#49077 = CARTESIAN_POINT ( 'NONE',  ( 97.33091451745008271, -32.84266655496112008, 41.02419670448193045 ) ) ;
#49079 = CARTESIAN_POINT ( 'NONE',  ( 95.16559702356694572, 70.52006616879377532, -89.37861919290396884 ) ) ;
#49078 = DIRECTION ( 'NONE',  ( 1.000000000000000078E-15, -1.000000000000000083E-30, -1.000000000000000000 ) ) ;
#49080 = LINE ( 'NONE', #61821, #13267 ) ;
#49081 = CARTESIAN_POINT ( 'NONE',  ( 131.5185316161780804, -17.69475198630851764, 2.828485944707543442 ) ) ;
#49082 = EDGE_LOOP ( 'NONE', ( #33734, #81198, #85288, #17579, #71814 ) ) ;
#49083 = EDGE_CURVE ( 'NONE', #67881, #49139, #26898, .T. ) ;
#49084 = CARTESIAN_POINT ( 'NONE',  ( -194.1576000000000022, 20.32000000000000028, -9.525000000000000355 ) ) ;
#49085 = B_SPLINE_CURVE_WITH_KNOTS ( 'NONE', 3,
 ( #7899, #28802, #69686, #62855, #41068, #77393, #35598, #56484, #84229, #15169, #68344, #6126, #6558, #89242, #27007, #54675, #82439, #47873 ),
 .UNSPECIFIED., .F., .F.,
 ( 4, 2, 2, 2, 2, 2, 2, 2, 4 ),
 ( 0.000000000000000000, 0.06249496329388545823, 0.1249899265877709165, 0.1874848898816563747, 0.2499798531755418329, 0.3124748164694273189, 0.3749697797633127494, 0.4374647430571981799, 0.4999597063510836659 ),
 .UNSPECIFIED. ) ;
#49086 = CARTESIAN_POINT ( 'NONE',  ( 97.81170669197712186, -40.51744871389600178, 156.6352702525290681 ) ) ;
#49087 = ADVANCED_FACE ( 'NONE', ( #80537 ), #66889, .T. ) ;
#49088 = AXIS2_PLACEMENT_3D ( 'NONE', #54237, #19757, #47437 ) ;
#49089 = CARTESIAN_POINT ( 'NONE',  ( 182.2420472961719895, -31.76306994223730840, 193.9678068554150059 ) ) ;
#49090 = CARTESIAN_POINT ( 'NONE',  ( 12.03342778677654934, 78.46830267626332045, 117.9437853765525404 ) ) ;
#49091 = CARTESIAN_POINT ( 'NONE',  ( 109.2595486427728559, -46.97979643076451595, 103.7441967044829880 ) ) ;
#49092 = EDGE_CURVE ( 'NONE', #12031, #41030, #87789, .T. ) ;
#49093 = AXIS2_PLACEMENT_3D ( 'NONE', #59465, #88098, #4966 ) ;
#49095 = DIRECTION ( 'NONE',  ( 0.000000000000000000, 0.000000000000000000, 1.000000000000000000 ) ) ;
#49094 = FACE_OUTER_BOUND ( 'NONE', #30835, .T. ) ;
#49096 = CARTESIAN_POINT ( 'NONE',  ( 41.56648329127499153, -32.07844715994070839, 194.1756252759119832 ) ) ;
#49097 = EDGE_LOOP ( 'NONE', ( #84250, #88316, #4252, #501 ) ) ;
#49098 = DIRECTION ( 'NONE',  ( 0.1858654558203195195, -0.9825752044157765042, 0.000000000000000000 ) ) ;
#49099 = CARTESIAN_POINT ( 'NONE',  ( 102.9676436823274202, -46.25511244710193637, 133.2651490854339613 ) ) ;
#49100 = AXIS2_PLACEMENT_3D ( 'NONE', #28059, #83487, #63030 ) ;
#49102 = EDGE_LOOP ( 'NONE', ( #56276, #61736, #44401, #84285 ) ) ;
#49101 = CARTESIAN_POINT ( 'NONE',  ( 107.0664832912739968, -36.72944715994100306, 287.6356252759109680 ) ) ;
#49103 = CARTESIAN_POINT ( 'NONE',  ( 106.1402962346845982, -47.72062544595559785, 258.4975300378158636 ) ) ;
#49104 = DIRECTION ( 'NONE',  ( 0.000000000000000000, -1.000000000000000000, 0.000000000000000000 ) ) ;
#49105 = LINE ( 'NONE', #86, #89590 ) ;
#49106 = LINE ( 'NONE', #8247, #9564 ) ;
#49107 = CARTESIAN_POINT ( 'NONE',  ( 25.56670390244797275, -62.87844715994099687, 173.2178068554149775 ) ) ;
#49108 = PLANE ( 'NONE',  #86880 ) ;
#49109 = CARTESIAN_POINT ( 'NONE',  ( -91.13743891206615899, 69.93117631934792655, 93.48535127324173288 ) ) ;
#49110 = CARTESIAN_POINT ( 'NONE',  ( 98.91665286848242999, -30.31703347128389225, 200.8080062282919869 ) ) ;
#49111 = VERTEX_POINT ( 'NONE', #25553 ) ;
#49112 = ORIENTED_EDGE ( 'NONE', *, *, #39762, .F. ) ;
#49113 = VECTOR ( 'NONE', #53907, 1000.000000000000000 ) ;
#49114 = CARTESIAN_POINT ( 'NONE',  ( 113.1089835609813719, -43.92423027677314451, 144.5520594963729764 ) ) ;
#49115 = CARTESIAN_POINT ( 'NONE',  ( 21.03689327557706790, -23.42844715994186089, 300.4678068554150059 ) ) ;
#49116 = CARTESIAN_POINT ( 'NONE',  ( 105.5822692374337777, -27.99308443639166555, 11.64158330589692980 ) ) ;
#49117 = CARTESIAN_POINT ( 'NONE',  ( 71.24189083761808661, -0.9290567490904538817, 396.9756252759102040 ) ) ;
#49118 = CARTESIAN_POINT ( 'NONE',  ( 117.0607201049021029, -38.08168303701916813, 268.7191026460068315 ) ) ;
#49119 = CARTESIAN_POINT ( 'NONE',  ( 210.5660000000000025, 52.73749999999999716, -44.45000000000000284 ) ) ;
#49120 = DIRECTION ( 'NONE',  ( 0.000000000000000000, 0.000000000000000000, 1.000000000000000000 ) ) ;
#49121 = DIRECTION ( 'NONE',  ( 0.000000000000000000, 0.000000000000000000, -1.000000000000000000 ) ) ;
#49122 = CARTESIAN_POINT ( 'NONE',  ( 115.8368392028494185, -44.66223131803950963, 233.2413395616259493 ) ) ;
#49123 = DIRECTION ( 'NONE',  ( 1.000000000000000078E-15, 1.000000000000000083E-30, -1.000000000000000000 ) ) ;
#49124 = EDGE_LOOP ( 'NONE', ( #78012, #50676, #58169, #71982 ) ) ;
#49125 = ORIENTED_EDGE ( 'NONE', *, *, #23659, .F. ) ;
#49126 = VECTOR ( 'NONE', #83290, 1000.000000000000000 ) ;
#49127 = DIRECTION ( 'NONE',  ( 0.000000000000000000, 1.000000000000000000, 0.000000000000000000 ) ) ;
#49128 = CARTESIAN_POINT ( 'NONE',  ( 82.81648064515530905, -18.72944715939135207, 6.749772901088279653 ) ) ;
#49129 = CYLINDRICAL_SURFACE ( 'NONE', #53375, 0.9999999999999800160 ) ;
#49130 = CARTESIAN_POINT ( 'NONE',  ( 25.56670390244797275, -58.35344715994099829, 293.2178068554150627 ) ) ;
#49132 = CARTESIAN_POINT ( 'NONE',  ( 62.03742497533751532, -23.42844715994041849, 249.9678068554150343 ) ) ;
#49131 = AXIS2_PLACEMENT_3D ( 'NONE', #74382, #33037, #60730 ) ;
#49133 = AXIS2_PLACEMENT_3D ( 'NONE', #11508, #4694, #19656 ) ;
#49134 = VERTEX_POINT ( 'NONE', #53229 ) ;
#49135 = CARTESIAN_POINT ( 'NONE',  ( 100.5706289694924607, -28.47478668554837000, 11.60705384733995515 ) ) ;
#49136 = EDGE_CURVE ( 'NONE', #71373, #77225, #5140, .T. ) ;
#49137 = CARTESIAN_POINT ( 'NONE',  ( 104.4105186412307944, -25.99981812482467092, 240.2575300378159682 ) ) ;
#49138 = EDGE_CURVE ( 'NONE', #43505, #55059, #34608, .T. ) ;
#49139 = VERTEX_POINT ( 'NONE', #49115 ) ;
#49141 = ADVANCED_FACE ( 'NONE', ( #27348 ), #8256, .F. ) ;
#49140 = CIRCLE ( 'NONE', #89840, 5.799999999999998934 ) ;
#49142 = DIRECTION ( 'NONE',  ( 0.000000000000000000, 0.000000000000000000, 1.000000000000000000 ) ) ;
#49143 = LINE ( 'NONE', #75978, #74721 ) ;
#49144 = DIRECTION ( 'NONE',  ( -4.299999999999999979E-14, 1.000000000000000000, 0.000000000000000000 ) ) ;
#49145 = CARTESIAN_POINT ( 'NONE',  ( 109.6546009468767693, -44.98793201169110034, 50.62428084578196774 ) ) ;
#49147 = CARTESIAN_POINT ( 'NONE',  ( 95.88671040095643150, -32.72508343906864781, 172.0527681330539735 ) ) ;
#49146 = AXIS2_PLACEMENT_3D ( 'NONE', #65114, #58725, #85139 ) ;
#49148 = EDGE_CURVE ( 'NONE', #41996, #26777, #76398, .T. ) ;
#49149 = CARTESIAN_POINT ( 'NONE',  ( 107.0667039024470313, -104.2784471599408676, 19.21780685541799016 ) ) ;
#49150 = EDGE_LOOP ( 'NONE', ( #42133, #62010 ) ) ;
#49151 = EDGE_CURVE ( 'NONE', #61703, #75492, #70946, .T. ) ;
#49152 = AXIS2_PLACEMENT_3D ( 'NONE', #66173, #23974, #52523 ) ;
#49153 = DIRECTION ( 'NONE',  ( 0.000000000000000000, 0.000000000000000000, 1.000000000000000000 ) ) ;
#49154 = ORIENTED_EDGE ( 'NONE', *, *, #86621, .T. ) ;
#49155 = ORIENTED_EDGE ( 'NONE', *, *, #45351, .F. ) ;
#49156 = EDGE_CURVE ( 'NONE', #71659, #88009, #32753, .T. ) ;
#49157 = CARTESIAN_POINT ( 'NONE',  ( 12.70000000000000284, 83.38971874880476776, 117.8738102209307783 ) ) ;
#49158 = VERTEX_POINT ( 'NONE', #41849 ) ;
#49159 = EDGE_LOOP ( 'NONE', ( #1114, #65251, #43917, #73012 ) ) ;
#49160 = CARTESIAN_POINT ( 'NONE',  ( 51.42025729302698522, -31.94127993907710206, -5.074374724088000832 ) ) ;
#49161 = EDGE_CURVE ( 'NONE', #52237, #75709, #20551, .T. ) ;
#49162 = FACE_OUTER_BOUND ( 'NONE', #41663, .T. ) ;
#49163 = AXIS2_PLACEMENT_3D ( 'NONE', #80375, #65823, #31303 ) ;
#49164 = CARTESIAN_POINT ( 'NONE',  ( 111.5299334411454311, -29.44702005892069607, 94.06099125664896121 ) ) ;
#49165 = CARTESIAN_POINT ( 'NONE',  ( 100.6426946765138695, -44.96845825347062231, 232.0499109901969632 ) ) ;
#49166 = CARTESIAN_POINT ( 'NONE',  ( 95.43233898611173061, -38.84956357215551748, 201.4699109901969791 ) ) ;
#49167 = CARTESIAN_POINT ( 'NONE',  ( -479.3614999999999782, 10.16305401447645984, 83.34375000000000000 ) ) ;
#49168 = CARTESIAN_POINT ( 'NONE',  ( 100.8868098461901610, -44.69967630397148639, 93.05222427096256865 ) ) ;
#49169 = EDGE_CURVE ( 'NONE', #20444, #79957, #70510, .T. ) ;
#49170 = EDGE_LOOP ( 'NONE', ( #8855, #34897, #19135, #88177, #89797, #50900, #85247, #48512 ) ) ;
#49171 = DIRECTION ( 'NONE',  ( -0.000000000000000000, 1.000000000000000000, -0.000000000000000000 ) ) ;
#49172 = CARTESIAN_POINT ( 'NONE',  ( 77.39114642429960611, 127.0000000000000000, -71.77848634863110533 ) ) ;
#49173 = CARTESIAN_POINT ( 'NONE',  ( 70.77521666129561595, -139.2590457508245265, 247.4515711584743087 ) ) ;
#49174 = VECTOR ( 'NONE', #14299, 1000.000000000000000 ) ;
#49175 = CARTESIAN_POINT ( 'NONE',  ( 98.70071965984708129, -42.85747980491203180, 106.8175300378169652 ) ) ;
#49176 = CARTESIAN_POINT ( 'NONE',  ( 116.2704737988580206, -31.74013610724590961, 69.22133956162495849 ) ) ;
#49177 = CARTESIAN_POINT ( 'NONE',  ( 100.2183167550744685, -45.46532142855728864, 277.0594347997204068 ) ) ;
#49178 = VERTEX_POINT ( 'NONE', #1452 ) ;
#49179 = CARTESIAN_POINT ( 'NONE',  ( 118.7903470546216482, -38.45904373001069843, 223.7099109901969598 ) ) ;
#49180 = DIRECTION ( 'NONE',  ( 1.000000000000000078E-15, 0.000000000000000000, -1.000000000000000000 ) ) ;
#49181 = SURFACE_STYLE_FILL_AREA ( #83286 ) ;
#49182 = CARTESIAN_POINT ( 'NONE',  ( 12.69999999999999929, 82.54999999999999716, 129.9368274816650057 ) ) ;
#49183 = LINE ( 'NONE', #36482, #59040 ) ;
#49185 = CARTESIAN_POINT ( 'NONE',  ( 68.70527646626339902, -139.2915593431212358, 245.9274751462549204 ) ) ;
#49184 = LINE ( 'NONE', #22407, #7079 ) ;
#49186 = CARTESIAN_POINT ( 'NONE',  ( 105.2610101554027295, -25.41321098886781016, 321.3089972913614929 ) ) ;
#49187 = CYLINDRICAL_SURFACE ( 'NONE', #29458, 0.2500000000000002220 ) ;
#49188 = CARTESIAN_POINT ( 'NONE',  ( 7.746212673614271793, 92.64801822704204426, -118.3046725678181446 ) ) ;
#49189 = CARTESIAN_POINT ( 'NONE',  ( -1.663881452865377808, 95.14749909259209915, 130.5460625349953432 ) ) ;
#49190 = CARTESIAN_POINT ( 'NONE',  ( 97.33784129644996597, -34.07106458208137667, 12.11479194675188253 ) ) ;
#49191 = CARTESIAN_POINT ( 'NONE',  ( -15.89999999999999680, 53.97500000000000142, 50.79999999999999716 ) ) ;
#49192 = ADVANCED_FACE ( 'NONE', ( #83673 ), #20990, .F. ) ;
#49194 = ORIENTED_EDGE ( 'NONE', *, *, #88153, .T. ) ;
#49193 = DIRECTION ( 'NONE',  ( 1.000000000000000000, 0.000000000000000000, 0.000000000000000000 ) ) ;
#49195 = AXIS2_PLACEMENT_3D ( 'NONE', #62274, #49078, #61819 ) ;
#49196 = CARTESIAN_POINT ( 'NONE',  ( 124.6905118036816305, -125.4749327540681492, 250.2178068554179902 ) ) ;
#49197 = CARTESIAN_POINT ( 'NONE',  ( 104.8365363718904888, -26.48661066032647327, 260.2470538473397710 ) ) ;
#49198 = CARTESIAN_POINT ( 'NONE',  ( 102.6976273654655643, -46.88262786655960923, 133.2651490854349561 ) ) ;
#49199 = CARTESIAN_POINT ( 'NONE',  ( 115.9100415161514945, -31.16808610560197224, 30.27276813305396175 ) ) ;
#49200 = EDGE_CURVE ( 'NONE', #8807, #63506, #37113, .T. ) ;
#49201 = PLANE ( 'NONE',  #86759 ) ;
#49203 = CARTESIAN_POINT ( 'NONE',  ( 82.18073802037270070, -34.97076862298165878, 7.459445689453488626 ) ) ;
#49202 = DIRECTION ( 'NONE',  ( 0.000000000000000000, 0.000000000000000000, 1.000000000000000000 ) ) ;
#49204 = CYLINDRICAL_SURFACE ( 'NONE', #37844, 13.16666666666670160 ) ;
#49205 = CIRCLE ( 'NONE', #56403, 0.5000000000000004441 ) ;
#49206 = AXIS2_PLACEMENT_3D ( 'NONE', #7274, #75420, #61761 ) ;
#49207 = ORIENTED_EDGE ( 'NONE', *, *, #49557, .F. ) ;
#49208 = DIRECTION ( 'NONE',  ( 0.000000000000000000, 0.000000000000000000, -1.000000000000000000 ) ) ;
#49209 = ORIENTED_EDGE ( 'NONE', *, *, #15356, .T. ) ;
#49210 = CARTESIAN_POINT ( 'NONE',  ( 113.1264120695652622, -29.99967374510735141, 158.9276579233149391 ) ) ;
#49211 = AXIS2_PLACEMENT_3D ( 'NONE', #57053, #29822, #83900 ) ;
#49213 = EDGE_LOOP ( 'NONE', ( #85781, #87164 ) ) ;
#49212 = CARTESIAN_POINT ( 'NONE',  ( 94.06648329127393993, -36.72944715994095333, 294.6356252759106837 ) ) ;
#49214 = CARTESIAN_POINT ( 'NONE',  ( 188.5667039024484097, -48.82844715993431350, 259.7178068554150059 ) ) ;
#49215 = CARTESIAN_POINT ( 'NONE',  ( 112.7681627534586113, -45.43114336468919134, 174.0384824187679556 ) ) ;
#49216 = PLANE ( 'NONE',  #72962 ) ;
#49217 = MECHANICAL_DESIGN_GEOMETRIC_PRESENTATION_REPRESENTATION (  '', ( #26025 ), #57982 ) ;
#49218 = DIRECTION ( 'NONE',  ( 0.000000000000000000, 0.000000000000000000, 1.000000000000000000 ) ) ;
#49219 = CARTESIAN_POINT ( 'NONE',  ( 99.10117237422181802, -30.54315369407227720, 86.80178034974119328 ) ) ;
#49220 = LINE ( 'NONE', #70588, #88254 ) ;
#49221 = DIRECTION ( 'NONE',  ( 1.000000000000000000, 3.999999999999999995E-14, 1.000000000000000078E-15 ) ) ;
#49222 = CARTESIAN_POINT ( 'NONE',  ( 109.1197153606379970, -46.32621810461561296, 107.7441967044829880 ) ) ;
#49223 = ORIENTED_EDGE ( 'NONE', *, *, #71114, .F. ) ;
#49224 = ORIENTED_EDGE ( 'NONE', *, *, #45610, .T. ) ;
#49225 = EDGE_LOOP ( 'NONE', ( #81502, #75092, #47322, #61605, #36452 ) ) ;
#49226 = CARTESIAN_POINT ( 'NONE',  ( 114.2978770801668418, -41.85148020179265416, 49.76729759161096922 ) ) ;
#49227 = CARTESIAN_POINT ( 'NONE',  ( 107.0664832912749915, -36.72944715993903486, 25.56312527591096995 ) ) ;
#49229 = DIRECTION ( 'NONE',  ( 1.092739197465703932E-16, -1.000000000000000000, 0.000000000000000000 ) ) ;
#49228 = CARTESIAN_POINT ( 'NONE',  ( 113.3375292005773929, -44.23527279707077042, 189.1299109901959525 ) ) ;
#49230 = CARTESIAN_POINT ( 'NONE',  ( 152.4409905591762708, -0.9151414768250908383, 394.9756252759102040 ) ) ;
#49231 = DIRECTION ( 'NONE',  ( 1.000000000000000000, 0.000000000000000000, 0.000000000000000000 ) ) ;
#49232 = CIRCLE ( 'NONE', #30384, 2.029999999999997140 ) ;
#49233 = DIRECTION ( 'NONE',  ( 0.000000000000000000, 1.000000000000000000, 0.000000000000000000 ) ) ;
#49234 = CARTESIAN_POINT ( 'NONE',  ( 162.7866693523289996, -36.02818131005891189, -5.074374724088000832 ) ) ;
#49235 = CARTESIAN_POINT ( 'NONE',  ( 41.56648329127499153, -36.32844715994070839, 18.92562527591200094 ) ) ;
#49236 = CARTESIAN_POINT ( 'NONE',  ( 96.66376384204015437, -36.61947630124858932, 111.3184824187679567 ) ) ;
#49237 = VERTEX_POINT ( 'NONE', #63214 ) ;
#49238 = ORIENTED_EDGE ( 'NONE', *, *, #54366, .F. ) ;
#49239 = ORIENTED_EDGE ( 'NONE', *, *, #5940, .T. ) ;
#49240 = FILL_AREA_STYLE_COLOUR ( '', #35737 ) ;
#49241 = CARTESIAN_POINT ( 'NONE',  ( 51.34673845256598668, -36.02818131005800950, 342.9256252759119548 ) ) ;
#49242 = DIRECTION ( 'NONE',  ( 0.000000000000000000, 0.000000000000000000, -1.000000000000000000 ) ) ;
#49243 = CARTESIAN_POINT ( 'NONE',  ( 37.03715912545343514, -48.62818131006108757, 180.4678068554150911 ) ) ;
#49244 = CARTESIAN_POINT ( 'NONE',  ( 105.1059768409772062, -45.79875505096494237, 180.2252332267349857 ) ) ;
#49246 = ADVANCED_FACE ( 'NONE', ( #62760 ), #51608, .F. ) ;
#49245 = AXIS2_PLACEMENT_3D ( 'NONE', #76405, #21452, #49120 ) ;
#49247 =( REPRESENTATION_RELATIONSHIP ('NONE','NONE', #82876, #19449 ) REPRESENTATION_RELATIONSHIP_WITH_TRANSFORMATION ( #14029 )SHAPE_REPRESENTATION_RELATIONSHIP( ) );
#49248 = LINE ( 'NONE', #21122, #84236 ) ;
#49249 = EDGE_CURVE ( 'NONE', #29159, #30966, #87884, .T. ) ;
#49250 = EDGE_CURVE ( 'NONE', #5960, #849, #48217, .T. ) ;
#49251 = CARTESIAN_POINT ( 'NONE',  ( 107.0667039024470313, -104.2784471599413934, 2.217806855418003043 ) ) ;
#49252 = ORIENTED_EDGE ( 'NONE', *, *, #46092, .F. ) ;
#49254 = VERTEX_POINT ( 'NONE', #21894 ) ;
#49253 = EDGE_LOOP ( 'NONE', ( #45878, #51689, #36988, #88832 ) ) ;
#49255 = CIRCLE ( 'NONE', #52155, 2.500000000000002220 ) ;
#49256 = ADVANCED_FACE ( 'NONE', ( #35050 ), #35957, .F. ) ;
#49257 = CARTESIAN_POINT ( 'NONE',  ( 162.7131505118551047, -33.70561438051486647, 313.9678068554149490 ) ) ;
#49258 = ORIENTED_EDGE ( 'NONE', *, *, #63223, .F. ) ;
#49259 = ORIENTED_EDGE ( 'NONE', *, *, #31531, .F. ) ;
#49260 = CARTESIAN_POINT ( 'NONE',  ( 78.94219388974397589, -21.23922437001919761, 8.028287874532589186 ) ) ;
#49261 = CARTESIAN_POINT ( 'NONE',  ( 98.52374054827556904, -34.37364049580116898, 247.5444404487539600 ) ) ;
#49262 = VECTOR ( 'NONE', #35581, 999.9999999999998863 ) ;
#49263 = EDGE_CURVE ( 'NONE', #57944, #70541, #6904, .T. ) ;
#49264 = CARTESIAN_POINT ( 'NONE',  ( -487.2989999999999782, 14.28750000000026077, 15.87499999999969802 ) ) ;
#49265 = ORIENTED_EDGE ( 'NONE', *, *, #82925, .T. ) ;
#49266 = FACE_BOUND ( 'NONE', #77337, .T. ) ;
#49267 = CARTESIAN_POINT ( 'NONE',  ( -120.3273848475766954, 74.62250637307523959, 50.66261013073812336 ) ) ;
#49268 = CONICAL_SURFACE ( 'NONE', #60883, 89.90000000000000568, 0.7853981633974206344 ) ;
#49269 = VERTEX_POINT ( 'NONE', #56831 ) ;
#49271 = ORIENTED_EDGE ( 'NONE', *, *, #69116, .F. ) ;
#49270 = AXIS2_PLACEMENT_3D ( 'NONE', #25694, #62001, #25243 ) ;
#49272 = EDGE_CURVE ( 'NONE', #10481, #67680, #22338, .T. ) ;
#49273 = DIRECTION ( 'NONE',  ( 0.000000000000000000, -1.000000000000000000, 0.000000000000000000 ) ) ;
#49274 = VERTEX_POINT ( 'NONE', #50016 ) ;
#49275 = ORIENTED_EDGE ( 'NONE', *, *, #13395, .T. ) ;
#49276 = ADVANCED_FACE ( 'NONE', ( #77751, #27795 ), #41410, .T. ) ;
#49277 = CARTESIAN_POINT ( 'NONE',  ( 114.5169583807067966, -41.13300932163210177, 281.2318998934008505 ) ) ;
#49278 = AXIS2_PLACEMENT_3D ( 'NONE', #30078, #85513, #30522 ) ;
#49279 = CARTESIAN_POINT ( 'NONE',  ( 114.0011561472229289, -28.09198494482817310, 119.5261014663869474 ) ) ;
#49280 = CARTESIAN_POINT ( 'NONE',  ( 108.9808406375927063, -47.59218431635562041, 122.7032443235299723 ) ) ;
#49281 = FACE_OUTER_BOUND ( 'NONE', #58107, .T. ) ;
#49282 = CYLINDRICAL_SURFACE ( 'NONE', #87325, 0.9999999999999731326 ) ;
#49283 = CARTESIAN_POINT ( 'NONE',  ( -118.1052286201201298, 89.94786999841839759, 10.33119577496824526 ) ) ;
#49284 = CARTESIAN_POINT ( 'NONE',  ( 96.85852386828889848, -34.61283385893091236, 212.1641967044819808 ) ) ;
#49285 = DIRECTION ( 'NONE',  ( 0.000000000000000000, 1.000000000000000000, 0.000000000000000000 ) ) ;
#49286 = LINE ( 'NONE', #7074, #58237 ) ;
#49287 = VERTEX_POINT ( 'NONE', #44091 ) ;
#49288 = CARTESIAN_POINT ( 'NONE',  ( 130.4017839623309953, 71.54617234588344843, -6.354402276674679939 ) ) ;
#49289 = ORIENTED_EDGE ( 'NONE', *, *, #78891, .F. ) ;
#49290 = EDGE_CURVE ( 'NONE', #43695, #65034, #77775, .T. ) ;
#49291 = EDGE_LOOP ( 'NONE', ( #29009, #9272, #68049, #72120 ) ) ;
#49292 = AXIS2_PLACEMENT_3D ( 'NONE', #61118, #51719, #24051 ) ;
#49293 = FACE_BOUND ( 'NONE', #28192, .T. ) ;
#49294 = CARTESIAN_POINT ( 'NONE',  ( 112.7099490626184206, -28.41643172750246293, 135.6016206186066881 ) ) ;
#49295 = VERTEX_POINT ( 'NONE', #16859 ) ;
#49296 = CARTESIAN_POINT ( 'NONE',  ( 97.79409093757406879, -42.74665822538010929, 146.7965776568629508 ) ) ;
#49297 = CARTESIAN_POINT ( 'NONE',  ( 119.2637946045969954, -42.39761235918182791, 25.56312527591098416 ) ) ;
#49298 = B_SPLINE_CURVE_WITH_KNOTS ( 'NONE', 3,
 ( #63606, #49955, #24065, #79931, #65820, #86734, #31751, #39009, #32192, #17686, #73533, #52168, #45366, #79486, #66720, #16799, #4504, #23628 ),
 .UNSPECIFIED., .F., .F.,
 ( 4, 2, 2, 2, 2, 2, 2, 2, 4 ),
 ( 0.000000000000000000, 0.06249510223317854968, 0.1249902044663570994, 0.1874853066995356421, 0.2499804089327141987, 0.3124755111658927276, 0.3749706133990712842, 0.4374657156322498408, 0.4999608178654283974 ),
 .UNSPECIFIED. ) ;
#49299 = LINE ( 'NONE', #63392, #68822 ) ;
#49302 = CARTESIAN_POINT ( 'NONE',  ( 97.24442698086048154, -40.26379795196656630, 262.6013395616254797 ) ) ;
#49301 = CARTESIAN_POINT ( 'NONE',  ( 98.77692026739322273, -42.37295007796758739, 56.80169783176815912 ) ) ;
#49300 = LINE ( 'NONE', #63849, #23046 ) ;
#49303 = CARTESIAN_POINT ( 'NONE',  ( 133.5842039024480528, -43.72944715994092491, 207.5838068554170377 ) ) ;
#49304 = DIRECTION ( 'NONE',  ( 0.000000000000000000, 0.000000000000000000, -1.000000000000000000 ) ) ;
#49305 = VECTOR ( 'NONE', #63847, 999.9999999999998863 ) ;
#49306 = DIRECTION ( 'NONE',  ( 0.000000000000000000, 0.000000000000000000, 1.000000000000000000 ) ) ;
#49307 = DIRECTION ( 'NONE',  ( 9.693101022688619289E-16, 0.000000000000000000, -1.000000000000000000 ) ) ;
#49308 = CARTESIAN_POINT ( 'NONE',  ( 97.31584372507236935, -39.30597603430089748, 257.5314586121004368 ) ) ;
#49309 = CARTESIAN_POINT ( 'NONE',  ( -187.8075999999999794, 20.32000000000000028, -6.349999999999999645 ) ) ;
#49311 = EDGE_LOOP ( 'NONE', ( #33569, #7815, #83093, #60996, #87771, #12299, #37747, #54113, #50328, #25363, #53175, #67803, #5724, #60647, #30319, #4555, #38410, #62863, #82931, #6889, #75769, #54629, #66862, #32409, #42744, #27250, #43198, #20265, #86793, #35990, #52331, #8977, #30726, #75923, #25213, #6859, #19809, #87066, #85168, #16469, #10582, #34733, #61210, #82987, #133, #53667, #18846, #44893, #89777, #15113, #18908, #8649, #68178, #6458, #76768, #5808, #22965, #67911, #18682, #22444, #17345, #50956, #62107, #59209, #67439, #51071, #81238, #14726, #3822, #53601, #59955, #5068, #70838, #81019, #74206, #12003, #39317, #81243, #26829, #58063, #30404, #35220, #14303, #62946, #89305, #70732, #68660, #26780, #46115, #3470, #28960, #30051, #38014, #2080, #18591, #15449, #32068, #76517, #75606, #83897, #38854, #18650, #11764, #43407, #63551, #75782, #6319, #5670, #860, #31224, #5901, #54873, #31564, #488, #13863, #8991, #4808, #41279, #59197, #19846, #6270, #72624, #33400, #35410, #77346, #30015, #77925, #46590, #84009, #26276, #70619, #62521, #53162, #43777, #65569, #16793, #26813, #63228, #26198, #4433, #37437, #72337, #63047, #88155, #10538, #4716, #89086, #74096, #17282, #63164, #81306, #59324, #80035 ) ) ;
#49310 = CARTESIAN_POINT ( 'NONE',  ( 112.8291378599181485, -28.63395795371034680, 195.5838068554166966 ) ) ;
#49312 = DIRECTION ( 'NONE',  ( 0.000000000000000000, 0.000000000000000000, -1.000000000000000000 ) ) ;
#49313 = CARTESIAN_POINT ( 'NONE',  ( 118.9428397581607442, -36.92852597549882177, 153.8127681330539644 ) ) ;
#49314 = CARTESIAN_POINT ( 'NONE',  ( 117.3845446746782386, -38.21944606407609513, 24.71276813305395237 ) ) ;
#49315 = CARTESIAN_POINT ( 'NONE',  ( 103.5276745422693523, -26.83930826182397311, 186.3499109901969746 ) ) ;
#49316 = CARTESIAN_POINT ( 'NONE',  ( 97.07207202760696418, -35.37844142050483498, 32.21895862687611611 ) ) ;
#49317 = EDGE_CURVE ( 'NONE', #61816, #17322, #13894, .T. ) ;
#49318 = CYLINDRICAL_SURFACE ( 'NONE', #77956, 3.000000000000002665 ) ;
#49319 = AXIS2_PLACEMENT_3D ( 'NONE', #73605, #88596, #74953 ) ;
#49321 = DIRECTION ( 'NONE',  ( -4.237773401492740281E-14, 1.000000000000000000, 0.000000000000000000 ) ) ;
#49320 = LINE ( 'NONE', #43849, #50704 ) ;
#49322 = FACE_OUTER_BOUND ( 'NONE', #12334, .T. ) ;
#49323 = CARTESIAN_POINT ( 'NONE',  ( 143.5667039024469886, -68.87844715994090450, 55.21780685541800437 ) ) ;
#49324 = VERTEX_POINT ( 'NONE', #78667 ) ;
#49325 = FACE_OUTER_BOUND ( 'NONE', #65222, .T. ) ;
#49326 = ORIENTED_EDGE ( 'NONE', *, *, #556, .T. ) ;
#49327 = VERTEX_POINT ( 'NONE', #65008 ) ;
#49329 = ORIENTED_EDGE ( 'NONE', *, *, #70020, .F. ) ;
#49328 = CYLINDRICAL_SURFACE ( 'NONE', #41520, 2.517500000000005844 ) ;
#49330 = CARTESIAN_POINT ( 'NONE',  ( 112.7298150101557610, -27.26422151970083263, 50.65943479972101215 ) ) ;
#49331 = FACE_OUTER_BOUND ( 'NONE', #23578, .T. ) ;
#49333 = CARTESIAN_POINT ( 'NONE',  ( 68.06670390244701707, -86.77844715994098124, 55.21780685541800437 ) ) ;
#49332 = AXIS2_PLACEMENT_3D ( 'NONE', #83305, #29673, #21986 ) ;
#49334 = EDGE_CURVE ( 'NONE', #11985, #23552, #85478, .T. ) ;
#49335 = CARTESIAN_POINT ( 'NONE',  ( 116.7009037750506053, -40.82467873942847802, 164.5070538473399608 ) ) ;
#49336 = B_SPLINE_CURVE_WITH_KNOTS ( 'NONE', 3,
 ( #65790, #2699, #58093, #51258, #85829, #24480, #9505, #38099, #31272, #72180, #9956, #64913, #86254, #79001, #44449, #72630, #44000, #65358 ),
 .UNSPECIFIED., .F., .F.,
 ( 4, 2, 2, 2, 2, 2, 2, 2, 4 ),
 ( 0.000000000000000000, 0.06249789214766773848, 0.1249957842953354770, 0.1874936764430032154, 0.2499915685906709539, 0.3124894607383387202, 0.3749873528860064309, 0.4374852450336741416, 0.4999831371813419079 ),
 .UNSPECIFIED. ) ;
#49337 = CARTESIAN_POINT ( 'NONE',  ( 113.0872481101271205, -29.11229423309321618, 273.9667055423626039 ) ) ;
#49338 = ORIENTED_EDGE ( 'NONE', *, *, #62002, .F. ) ;
#49339 = ORIENTED_EDGE ( 'NONE', *, *, #86288, .F. ) ;
#49341 = ORIENTED_EDGE ( 'NONE', *, *, #38492, .T. ) ;
#49340 = AXIS2_PLACEMENT_3D ( 'NONE', #30096, #1505, #65507 ) ;
#49342 = ADVANCED_FACE ( 'NONE', ( #30928 ), #86796, .F. ) ;
#49343 = EDGE_LOOP ( 'NONE', ( #39682, #46427 ) ) ;
#49344 = DIRECTION ( 'NONE',  ( 0.000000000000000000, 0.000000000000000000, 1.000000000000000000 ) ) ;
#49345 = LINE ( 'NONE', #56611, #86979 ) ;
#49346 = CARTESIAN_POINT ( 'NONE',  ( 104.4895514573384077, -26.97891836813563415, 161.2814916280540558 ) ) ;
#49347 = CARTESIAN_POINT ( 'NONE',  ( 102.0670549530419606, -27.97049806322867127, 75.48979194321593411 ) ) ;
#49348 = CARTESIAN_POINT ( 'NONE',  ( 100.0339087179658577, 88.18319050751493648, 83.89391322244469507 ) ) ;
#49349 = CARTESIAN_POINT ( 'NONE',  ( 131.0667039024480403, -43.72944715994093201, 207.5838068554170377 ) ) ;
#49350 = CARTESIAN_POINT ( 'NONE',  ( 151.5667039024485518, -48.82844715993590512, 180.4678068554149775 ) ) ;
#49351 = CARTESIAN_POINT ( 'NONE',  ( -11.42323817349576309, 88.11531169846917066, 130.0554870647972905 ) ) ;
#49352 = CARTESIAN_POINT ( 'NONE',  ( 101.3960830062750063, -28.00733582429760204, 25.53562527591096654 ) ) ;
#49353 = CARTESIAN_POINT ( 'NONE',  ( 57.14999999999999858, 95.25000000000000000, 280.2255000000000109 ) ) ;
#49354 = EDGE_LOOP ( 'NONE', ( #21599, #68565, #73693, #51165 ) ) ;
#49355 = DIRECTION ( 'NONE',  ( 0.000000000000000000, 1.000000000000000000, 0.000000000000000000 ) ) ;
#49356 = VECTOR ( 'NONE', #66736, 1000.000000000000000 ) ;
#49357 = DIRECTION ( 'NONE',  ( 1.000000000000000000, 0.000000000000000000, 0.000000000000000000 ) ) ;
#49358 = CARTESIAN_POINT ( 'NONE',  ( 106.8900815348805509, -46.00655951153972723, 75.37951894101996686 ) ) ;
#49359 = EDGE_CURVE ( 'NONE', #40480, #58480, #58187, .T. ) ;
#49360 = DIRECTION ( 'NONE',  ( 3.100000000000000258E-29, -3.100000000000000044E-14, -1.000000000000000000 ) ) ;
#49361 = EDGE_CURVE ( 'NONE', #9382, #63793, #85919, .T. ) ;
#49362 = AXIS2_PLACEMENT_3D ( 'NONE', #19680, #32391, #53718 ) ;
#49363 = CARTESIAN_POINT ( 'NONE',  ( 97.31584371710860637, -39.30597600346539622, 46.53145860958892399 ) ) ;
#49364 = ORIENTED_EDGE ( 'NONE', *, *, #70300, .T. ) ;
#49365 = ORIENTED_EDGE ( 'NONE', *, *, #57784, .F. ) ;
#49366 = CARTESIAN_POINT ( 'NONE',  ( 107.0664832912739968, -36.72944715994100306, 287.6356252759109680 ) ) ;
#49367 = EDGE_CURVE ( 'NONE', #49424, #33950, #65452, .T. ) ;
#49368 = ORIENTED_EDGE ( 'NONE', *, *, #71953, .F. ) ;
#49369 = EDGE_LOOP ( 'NONE', ( #58708, #20987, #35091, #80707 ) ) ;
#49370 = CARTESIAN_POINT ( 'NONE',  ( 111.3621671965809270, -45.84085784651199447, 134.3587261630399894 ) ) ;
#49371 = ADVANCED_FACE ( 'NONE', ( #22793 ), #57739, .F. ) ;
#49372 = CARTESIAN_POINT ( 'NONE',  ( -6.715083999775230517, 93.33742752469728998, 118.3661748111209704 ) ) ;
#49373 = AXIS2_PLACEMENT_3D ( 'NONE', #71076, #57418, #8850 ) ;
#49374 = CARTESIAN_POINT ( 'NONE',  ( 96.61744970692362244, -37.56424831167382195, 97.38991099019594344 ) ) ;
#49375 = DIRECTION ( 'NONE',  ( 7.340987889507870014E-14, 0.000000000000000000, 1.000000000000000000 ) ) ;
#49376 = ORIENTED_EDGE ( 'NONE', *, *, #14063, .T. ) ;
#49377 = VERTEX_POINT ( 'NONE', #24565 ) ;
#49378 = ORIENTED_EDGE ( 'NONE', *, *, #47208, .T. ) ;
#49379 = ADVANCED_FACE ( 'NONE', ( #44539 ), #37754, .F. ) ;
#49380 = CARTESIAN_POINT ( 'NONE',  ( 177.1649999999999920, 5.112500000000000711, -7.937500000000000000 ) ) ;
#49381 = VERTEX_POINT ( 'NONE', #9595 ) ;
#49382 = CARTESIAN_POINT ( 'NONE',  ( 111.4502655420255905, -27.98611277567904310, 279.7070538473400916 ) ) ;
#49383 = CARTESIAN_POINT ( 'NONE',  ( 99.99340640592768636, -27.19037833420660277, 181.5841967044829630 ) ) ;
#49384 = CARTESIAN_POINT ( 'NONE',  ( 12.61957378781718297, 80.89607376620493540, -117.8825615626982994 ) ) ;
#49385 = CARTESIAN_POINT ( 'NONE',  ( -109.6863455812695776, 48.91650121126127715, 70.80801475970909564 ) ) ;
#49386 = CARTESIAN_POINT ( 'NONE',  ( 98.45872715028987443, -30.84820395253375125, 116.8499109901969604 ) ) ;
#49387 = CIRCLE ( 'NONE', #13164, 190.5000000000000000 ) ;
#49388 = CARTESIAN_POINT ( 'NONE',  ( 107.5667039024470313, -100.3098201933451605, -19.78219314458212708 ) ) ;
#49389 = ORIENTED_EDGE ( 'NONE', *, *, #28252, .F. ) ;
#49390 = DIRECTION ( 'NONE',  ( 0.000000000000000000, 1.000000000000000000, 0.000000000000000000 ) ) ;
#49391 = AXIS2_PLACEMENT_3D ( 'NONE', #28669, #70464, #21872 ) ;
#49392 = CARTESIAN_POINT ( 'NONE',  ( 104.4082832666847054, -46.45815023090534623, 133.3659487707936364 ) ) ;
#49393 = VERTEX_POINT ( 'NONE', #72277 ) ;
#49394 = VECTOR ( 'NONE', #76803, 1000.000000000000000 ) ;
#49395 = CARTESIAN_POINT ( 'NONE',  ( 115.5439452383992176, -108.5954344580491551, 2.217806855418142042 ) ) ;
#49396 = DIRECTION ( 'NONE',  ( -1.000000000000000000, -3.999999999999999995E-14, -1.000000000000000078E-15 ) ) ;
#49397 = CARTESIAN_POINT ( 'NONE',  ( 97.07516343140007109, -33.75277822987297327, 31.09562527591097592 ) ) ;
#49398 = CARTESIAN_POINT ( 'NONE',  ( -1.415542646969860267E-16, 70.24203434096102683, 38.10000000000000142 ) ) ;
#49399 = DIRECTION ( 'NONE',  ( 1.000000000000000000, 0.000000000000000000, 0.000000000000000000 ) ) ;
#49400 = DIRECTION ( 'NONE',  ( -1.500809167996645702E-15, 0.7071067811865391350, 0.7071067811865560104 ) ) ;
#49401 = CARTESIAN_POINT ( 'NONE',  ( 111.8051047218221896, -27.50533234054179843, 19.71086337114996567 ) ) ;
#49403 = CARTESIAN_POINT ( 'NONE',  ( 98.29923130492889527, -31.06375673945267124, 141.8699109901969564 ) ) ;
#49402 = CARTESIAN_POINT ( 'NONE',  ( 116.3212776292267989, -32.94146857470629186, 109.1356252759109680 ) ) ;
#49404 = CARTESIAN_POINT ( 'NONE',  ( -487.2989999999999782, 86.51875000000001137, 94.61194598552339130 ) ) ;
#49405 = LINE ( 'NONE', #828, #59706 ) ;
#49406 = ORIENTED_EDGE ( 'NONE', *, *, #16879, .F. ) ;
#49407 = AXIS2_PLACEMENT_3D ( 'NONE', #38224, #37786, #86830 ) ;
#49408 = DIRECTION ( 'NONE',  ( 0.000000000000000000, 0.000000000000000000, 1.000000000000000000 ) ) ;
#49409 = CARTESIAN_POINT ( 'NONE',  ( 109.5618042869657387, 49.74144395212335468, 71.00059892473528578 ) ) ;
#49410 = DIRECTION ( 'NONE',  ( -1.000000000000000000, 0.000000000000000000, 0.000000000000000000 ) ) ;
#49411 = ORIENTED_EDGE ( 'NONE', *, *, #48735, .T. ) ;
#49412 = DIRECTION ( 'NONE',  ( -1.000000000000000000, 0.000000000000000000, -1.531877379624855416E-14 ) ) ;
#49414 = ORIENTED_EDGE ( 'NONE', *, *, #86017, .T. ) ;
#49413 = CARTESIAN_POINT ( 'NONE',  ( 98.22399452165288380, -42.33453934503185678, 186.7756252759109543 ) ) ;
#49415 = CARTESIAN_POINT ( 'NONE',  ( 88.90000000000000568, 66.67499999999999716, 346.0750000000000455 ) ) ;
#49416 = CARTESIAN_POINT ( 'NONE',  ( 115.4773891788847067, -29.52237647247901009, 225.4022919425769658 ) ) ;
#49417 = CARTESIAN_POINT ( 'NONE',  ( 96.29363189909904008, -41.78481911317979325, 57.67562527591096710 ) ) ;
#49418 = DIRECTION ( 'NONE',  ( 0.000000000000000000, 0.000000000000000000, 1.000000000000000000 ) ) ;
#49419 = EDGE_CURVE ( 'NONE', #2137, #67480, #58616, .T. ) ;
#49420 = DIRECTION ( 'NONE',  ( -3.100000000000000258E-29, 3.100000000000000044E-14, 1.000000000000000000 ) ) ;
#49421 = CARTESIAN_POINT ( 'NONE',  ( 164.9667039024474491, -26.71338133338732845, 237.4678068554150059 ) ) ;
#49422 = ORIENTED_EDGE ( 'NONE', *, *, #63338, .F. ) ;
#49423 = EDGE_CURVE ( 'NONE', #60085, #14890, #44989, .T. ) ;
#49424 = VERTEX_POINT ( 'NONE', #52232 ) ;
#49426 = EDGE_LOOP ( 'NONE', ( #48966, #73392, #52999, #64831 ) ) ;
#49425 = AXIS2_PLACEMENT_3D ( 'NONE', #85956, #9195, #57774 ) ;
#49427 = AXIS2_PLACEMENT_3D ( 'NONE', #10563, #44624, #3755 ) ;
#49428 = ORIENTED_EDGE ( 'NONE', *, *, #5142, .F. ) ;
#49429 = LINE ( 'NONE', #77165, #29324 ) ;
#49430 = CARTESIAN_POINT ( 'NONE',  ( 117.4742555207853059, -36.12881027634428222, 224.8727681330539667 ) ) ;
#49431 = CARTESIAN_POINT ( 'NONE',  ( 110.2536356736639078, -101.8611209747507189, 2.217806855417919998 ) ) ;
#49432 = CARTESIAN_POINT ( 'NONE',  ( 136.4599941731241302, -17.37149686616246669, 2.653088969751947523 ) ) ;
#49434 = CARTESIAN_POINT ( 'NONE',  ( -179.6205029264235122, 101.5999999999999943, 123.8612349545196025 ) ) ;
#49433 = DIRECTION ( 'NONE',  ( 2.900000000000000265E-14, -2.000000000000000155E-15, 1.000000000000000000 ) ) ;
#49435 = CARTESIAN_POINT ( 'NONE',  ( 162.8913605087219878, -31.76306994223740432, -5.074374724088000832 ) ) ;
#49436 = AXIS2_PLACEMENT_3D ( 'NONE', #10604, #2473, #57869 ) ;
#49437 = CARTESIAN_POINT ( 'NONE',  ( 110.5626142325126153, -46.61202937628593190, 37.84705384733994293 ) ) ;
#49438 = EDGE_LOOP ( 'NONE', ( #11631, #74495, #82946 ) ) ;
#49439 = VERTEX_POINT ( 'NONE', #9155 ) ;
#49440 = AXIS2_PLACEMENT_3D ( 'NONE', #56304, #34072, #54501 ) ;
#49441 = EDGE_CURVE ( 'NONE', #73517, #87063, #10487, .T. ) ;
#49442 = CARTESIAN_POINT ( 'NONE',  ( 34.67381068360343477, -28.98061976759059988, 117.4678068554150485 ) ) ;
#49443 = DIRECTION ( 'NONE',  ( -0.7759704746411383303, 0.6307692307692303046, 0.000000000000000000 ) ) ;
#49444 = CARTESIAN_POINT ( 'NONE',  ( 114.9410966442421795, -29.98191058901456074, 225.4022919425769658 ) ) ;
#49445 = CARTESIAN_POINT ( 'NONE',  ( -179.8898777604659927, 0.000000000000000000, -123.4696824136383952 ) ) ;
#49446 = CARTESIAN_POINT ( 'NONE',  ( 96.37928053093618530, -33.66421044892481262, 137.1041967044819501 ) ) ;
#49447 = CARTESIAN_POINT ( 'NONE',  ( 179.1667039024460166, -28.27351298637280408, 342.9256252759109884 ) ) ;
#49448 = CARTESIAN_POINT ( 'NONE',  ( -76.47785380479396622, 54.92403073184157591, 30.82222824574506603 ) ) ;
#49450 = ORIENTED_EDGE ( 'NONE', *, *, #20201, .F. ) ;
#49449 = VECTOR ( 'NONE', #49687, 1000.000000000000000 ) ;
#49451 = CYLINDRICAL_SURFACE ( 'NONE', #48752, 3.000000000000002665 ) ;
#49452 = ORIENTED_EDGE ( 'NONE', *, *, #10407, .F. ) ;
#49453 = ORIENTED_EDGE ( 'NONE', *, *, #59934, .T. ) ;
#49454 = CARTESIAN_POINT ( 'NONE',  ( -487.2989999999999782, 93.66249999999999432, 98.73639197104678544 ) ) ;
#49455 = CARTESIAN_POINT ( 'NONE',  ( 111.6101215911791087, -44.95330735676063938, 249.3977737820869720 ) ) ;
#49456 = VECTOR ( 'NONE', #33120, 1000.000000000000000 ) ;
#49457 = CARTESIAN_POINT ( 'NONE',  ( 109.6430120631640079, -46.48008675372654608, 192.7814586037220295 ) ) ;
#49458 = CARTESIAN_POINT ( 'NONE',  ( 183.5150000000000148, 21.46300000000000097, 59.96543552338529537 ) ) ;
#49459 = CARTESIAN_POINT ( 'NONE',  ( 97.81375517989221180, -40.51659548082960072, 91.63516306087667829 ) ) ;
#49460 = ADVANCED_FACE ( 'NONE', ( #65882 ), #3672, .F. ) ;
#49461 = AXIS2_PLACEMENT_3D ( 'NONE', #9414, #64827, #52053 ) ;
#49462 = CARTESIAN_POINT ( 'NONE',  ( 29.56670390244797630, -67.87844715994100397, 300.9178068554150514 ) ) ;
#49463 = ORIENTED_EDGE ( 'NONE', *, *, #50194, .T. ) ;
#49464 = LINE ( 'NONE', #22692, #74031 ) ;
#49465 = CARTESIAN_POINT ( 'NONE',  ( 97.81493411881378108, -40.51644251795452334, 167.6359250042934264 ) ) ;
#49466 = ORIENTED_EDGE ( 'NONE', *, *, #57640, .F. ) ;
#49467 = CARTESIAN_POINT ( 'NONE',  ( 118.0833341887621373, -37.62838194956883342, 38.77372051400595865 ) ) ;
#49468 = EDGE_LOOP ( 'NONE', ( #4120, #10933, #23462, #28005 ) ) ;
#49469 = EDGE_CURVE ( 'NONE', #23732, #35180, #7690, .T. ) ;
#49471 = VECTOR ( 'NONE', #75564, 1000.000000000000000 ) ;
#49470 = CARTESIAN_POINT ( 'NONE',  ( 110.3949268851355328, -45.15168757608171290, 22.31051506617198754 ) ) ;
#49472 = CARTESIAN_POINT ( 'NONE',  ( 104.4091555634243349, -46.45838639981014495, 127.3648633746425105 ) ) ;
#49473 = CARTESIAN_POINT ( 'NONE',  ( 106.5196382177906855, -25.62481104856546565, 195.1156252759109861 ) ) ;
#49474 = DIRECTION ( 'NONE',  ( 0.000000000000000000, 0.000000000000000000, -1.000000000000000000 ) ) ;
#49475 = EDGE_CURVE ( 'NONE', #75348, #70994, #73599, .T. ) ;
#49476 = LINE ( 'NONE', #70851, #12438 ) ;
#49477 = CARTESIAN_POINT ( 'NONE',  ( 107.0664832912739399, -36.72944715994095333, 311.3356252759109566 ) ) ;
#49478 = CARTESIAN_POINT ( 'NONE',  ( 68.80140062917963917, -69.47028513356498536, 247.4826175141195108 ) ) ;
#49479 = CARTESIAN_POINT ( 'NONE',  ( 99.30088202768328642, -28.79894053213705973, 266.7051490854347549 ) ) ;
#49480 = CARTESIAN_POINT ( 'NONE',  ( 75.67533895324405080, 88.91291927174617626, -91.26325766987429233 ) ) ;
#49481 = VERTEX_POINT ( 'NONE', #39525 ) ;
#49482 = DIRECTION ( 'NONE',  ( -1.806816776397999960E-14, 1.000000000000000000, -1.906816776398000198E-29 ) ) ;
#49483 = ORIENTED_EDGE ( 'NONE', *, *, #46478, .T. ) ;
#49484 = CARTESIAN_POINT ( 'NONE',  ( 97.50257212865312795, -32.47214954040395440, 96.99276813305395706 ) ) ;
#49485 = CARTESIAN_POINT ( 'NONE',  ( 73.06648329127402519, -46.72944715994106701, -5.074374724089063982 ) ) ;
#49486 = ORIENTED_EDGE ( 'NONE', *, *, #2764, .T. ) ;
#49487 = ORIENTED_EDGE ( 'NONE', *, *, #39487, .F. ) ;
#49488 = ORIENTED_EDGE ( 'NONE', *, *, #8233, .F. ) ;
#49489 = EDGE_CURVE ( 'NONE', #68501, #35213, #16827, .T. ) ;
#49490 = AXIS2_PLACEMENT_3D ( 'NONE', #19509, #60835, #11354 ) ;
#49491 = CARTESIAN_POINT ( 'NONE',  ( 152.0368932755770288, -23.42844715993588522, 313.9678068554149490 ) ) ;
#49492 = LINE ( 'NONE', #55846, #17281 ) ;
#49494 = EDGE_CURVE ( 'NONE', #50110, #32624, #32255, .T. ) ;
#49493 = DIRECTION ( 'NONE',  ( 0.000000000000000000, 0.000000000000000000, 1.000000000000000000 ) ) ;
#49495 = CARTESIAN_POINT ( 'NONE',  ( 107.0664832912730020, -27.87844715994269862, 361.9756252759109998 ) ) ;
#49496 = CARTESIAN_POINT ( 'NONE',  ( 107.0664832912739968, 12.92155284005902516, 333.4006252759110112 ) ) ;
#49497 = CARTESIAN_POINT ( 'NONE',  ( 110.5551769720564863, -46.59100632561725064, 33.84705384733993583 ) ) ;
#49498 = CARTESIAN_POINT ( 'NONE',  ( 0.000000000000000000, 184.0000000000000000, 106.1020876358972771 ) ) ;
#49499 = ORIENTED_EDGE ( 'NONE', *, *, #22843, .F. ) ;
#49500 = DIRECTION ( 'NONE',  ( 1.000000000000000000, 0.000000000000000000, 0.000000000000000000 ) ) ;
#49501 = CARTESIAN_POINT ( 'NONE',  ( 51.56670390244799762, -33.35206098992650681, -5.074374724088000832 ) ) ;
#49502 = AXIS2_PLACEMENT_3D ( 'NONE', #81410, #40032, #19157 ) ;
#49503 = ORIENTED_EDGE ( 'NONE', *, *, #77024, .T. ) ;
#49504 = ORIENTED_EDGE ( 'NONE', *, *, #69822, .F. ) ;
#49505 = AXIS2_PLACEMENT_3D ( 'NONE', #16237, #2156, #43913 ) ;
#49506 = PLANE ( 'NONE',  #56094 ) ;
#49507 = LINE ( 'NONE', #64947, #45488 ) ;
#49508 = CARTESIAN_POINT ( 'NONE',  ( -5.627553765716396761, 71.15732062108085643, -130.4351721735936280 ) ) ;
#49509 = CARTESIAN_POINT ( 'NONE',  ( 0.000000000000000000, 65.60000000000000853, -33.74458626278666884 ) ) ;
#49510 = CARTESIAN_POINT ( 'NONE',  ( 50.88849390559499142, -32.11662333284530746, -5.074374724088000832 ) ) ;
#49511 = CARTESIAN_POINT ( 'NONE',  ( 103.1098180292659947, -44.29918505015107399, 211.6152769709339623 ) ) ;
#49512 = CARTESIAN_POINT ( 'NONE',  ( -465.6921742093550165, 47.62500000000000000, 3.174999999999999822 ) ) ;
#49513 = CARTESIAN_POINT ( 'NONE',  ( -71.77848634863029531, 127.0000000000000000, -77.39114642430038771 ) ) ;
#49514 = CARTESIAN_POINT ( 'NONE',  ( 106.6586145429690475, -26.26807492067915462, 85.10705384733896040 ) ) ;
#49515 = EDGE_LOOP ( 'NONE', ( #55843, #27121, #490, #76457 ) ) ;
#49516 = CYLINDRICAL_SURFACE ( 'NONE', #40781, 7.937500000000000000 ) ;
#49517 = ORIENTED_EDGE ( 'NONE', *, *, #62799, .T. ) ;
#49518 = CYLINDRICAL_SURFACE ( 'NONE', #60017, 0.5000000000000104361 ) ;
#49519 = ORIENTED_EDGE ( 'NONE', *, *, #27231, .F. ) ;
#49520 = VECTOR ( 'NONE', #75172, 1000.000000000000000 ) ;
#49521 = FACE_OUTER_BOUND ( 'NONE', #13483, .T. ) ;
#49522 = EDGE_LOOP ( 'NONE', ( #88599, #88809, #58931, #42610 ) ) ;
#49523 = DIRECTION ( 'NONE',  ( 1.000000000000000078E-15, -1.000000000000000083E-30, -1.000000000000000000 ) ) ;
#49524 = LINE ( 'NONE', #35452, #53081 ) ;
#49525 = CARTESIAN_POINT ( 'NONE',  ( 67.06683615445079738, -81.17077867087118648, 245.9554665702709997 ) ) ;
#49526 = AXIS2_PLACEMENT_3D ( 'NONE', #53762, #55104, #26093 ) ;
#49527 = DIRECTION ( 'NONE',  ( -1.000000000000000078E-15, 1.000000000000000000, 0.000000000000000000 ) ) ;
#49528 = EDGE_LOOP ( 'NONE', ( #8557, #53989, #62718, #83167 ) ) ;
#49529 = CARTESIAN_POINT ( 'NONE',  ( 104.4852212567679004, -46.88943973524933995, 47.37848241876796607 ) ) ;
#49530 = FILL_AREA_STYLE_COLOUR ( '', #20259 ) ;
#49533 = EDGE_CURVE ( 'NONE', #71638, #74855, #54514, .T. ) ;
#49532 = CARTESIAN_POINT ( 'NONE',  ( 85.52748787272849995, 73.86195533656248813, -98.64078293412647724 ) ) ;
#49531 = CARTESIAN_POINT ( 'NONE',  ( 67.06670390210777555, -137.6784471596019728, 245.4218662566959779 ) ) ;
#49534 = DIRECTION ( 'NONE',  ( -0.9999999853157766072, -0.0001713722456143218888, 0.000000000000000000 ) ) ;
#49535 = CARTESIAN_POINT ( 'NONE',  ( 57.14999999999999858, 60.86974387893089755, 326.2630000000000337 ) ) ;
#49536 = ORIENTED_EDGE ( 'NONE', *, *, #89872, .T. ) ;
#49537 = CIRCLE ( 'NONE', #64016, 3.174999999999983391 ) ;
#49538 = DIRECTION ( 'NONE',  ( -0.5610517121635795190, -0.5610517121635953952, -0.6086394273760236118 ) ) ;
#49539 = DIRECTION ( 'NONE',  ( 0.000000000000000000, 1.000000000000000000, 0.000000000000000000 ) ) ;
#49540 = FACE_OUTER_BOUND ( 'NONE', #80916, .T. ) ;
#49541 = CARTESIAN_POINT ( 'NONE',  ( 109.0764703591063522, -47.62188296335364157, 123.7337205140059666 ) ) ;
#49543 = CARTESIAN_POINT ( 'NONE',  ( 20.56670390244828184, -48.82844715994187368, 300.4678068554150059 ) ) ;
#49542 = FACE_OUTER_BOUND ( 'NONE', #69805, .T. ) ;
#49544 = DIRECTION ( 'NONE',  ( 0.000000000000000000, 0.000000000000000000, 1.000000000000000000 ) ) ;
#49545 = ORIENTED_EDGE ( 'NONE', *, *, #41906, .F. ) ;
#49546 = ADVANCED_FACE ( 'NONE', ( #25906 ), #11379, .T. ) ;
#49547 = CARTESIAN_POINT ( 'NONE',  ( -77.89700433585329620, 82.54999999999999716, -59.93649209371570663 ) ) ;
#49548 = CARTESIAN_POINT ( 'NONE',  ( 116.5825849560771417, -39.12894369053751120, 119.6299109901959525 ) ) ;
#49550 = ORIENTED_EDGE ( 'NONE', *, *, #78959, .F. ) ;
#49549 = LINE ( 'NONE', #84565, #21046 ) ;
#49551 = AXIS2_PLACEMENT_3D ( 'NONE', #2761, #51766, #79515 ) ;
#49552 = CARTESIAN_POINT ( 'NONE',  ( 118.0799254396264786, -36.12288750354066735, 269.8822919425776945 ) ) ;
#49553 = DIRECTION ( 'NONE',  ( -0.000000000000000000, 1.000000000000000000, 0.000000000000000000 ) ) ;
#49554 = DIRECTION ( 'NONE',  ( 0.000000000000000000, 0.000000000000000000, 1.000000000000000000 ) ) ;
#49555 = PLANE ( 'NONE',  #63239 ) ;
#49556 = CARTESIAN_POINT ( 'NONE',  ( 45.56670390244421753, -48.82844715994099971, 129.9678068554150911 ) ) ;
#49557 = EDGE_CURVE ( 'NONE', #13223, #16389, #80429, .T. ) ;
#49558 = CARTESIAN_POINT ( 'NONE',  ( 0.000000000000000000, 91.07499999999996021, 0.000000000000000000 ) ) ;
#49559 = CARTESIAN_POINT ( 'NONE',  ( -92.91726854070100217, 69.85063703626886422, 91.71670967180014600 ) ) ;
#49560 = CARTESIAN_POINT ( 'NONE',  ( 114.3351522754913674, -30.13549343754558407, 209.4127681330539872 ) ) ;
#49561 = VERTEX_POINT ( 'NONE', #66328 ) ;
#49562 = CIRCLE ( 'NONE', #20601, 4.762500000000002842 ) ;
#49563 = ORIENTED_EDGE ( 'NONE', *, *, #22226, .T. ) ;
#49564 = CARTESIAN_POINT ( 'NONE',  ( 115.7737780547358710, -35.08282516751891933, 155.4072975916109556 ) ) ;
#49565 = VECTOR ( 'NONE', #9757, 1000.000000000000000 ) ;
#49566 = DIRECTION ( 'NONE',  ( 0.000000000000000000, 0.000000000000000000, -1.000000000000000000 ) ) ;
#49567 = CARTESIAN_POINT ( 'NONE',  ( 115.9456366428866119, -37.20155953748186306, 15.21586902018295895 ) ) ;
#49568 = DIRECTION ( 'NONE',  ( -0.0001713722455994998422, 0.9999999853157766072, 0.000000000000000000 ) ) ;
#49569 = EDGE_CURVE ( 'NONE', #48031, #77074, #53573, .T. ) ;
#49570 = DIRECTION ( 'NONE',  ( 1.000000000000000000, 4.163336342344333240E-14, 0.000000000000000000 ) ) ;
#49571 = CARTESIAN_POINT ( 'NONE',  ( 74.38348329127296665, -71.52944715994142655, 342.9256252759110453 ) ) ;
#49572 = LINE ( 'NONE', #542, #78342 ) ;
#49573 = DIRECTION ( 'NONE',  ( -3.576143065239989638E-15, 0.000000000000000000, 1.000000000000000000 ) ) ;
#49574 = CARTESIAN_POINT ( 'NONE',  ( 107.5091008941355994, -47.12332782054438951, 237.6099109901969655 ) ) ;
#49575 = CARTESIAN_POINT ( 'NONE',  ( 10.01853287408365745, 90.23518421848368121, 117.9321046141928662 ) ) ;
#49576 = ORIENTED_EDGE ( 'NONE', *, *, #17502, .F. ) ;
#49578 = EDGE_LOOP ( 'NONE', ( #75764, #70168, #77251, #61527 ) ) ;
#49577 = EDGE_CURVE ( 'NONE', #57432, #74315, #81776, .T. ) ;
#49579 = VECTOR ( 'NONE', #72824, 1000.000000000000000 ) ;
#49580 = DIRECTION ( 'NONE',  ( -1.000000000000000078E-15, 1.000000000000000000, 0.000000000000000000 ) ) ;
#49581 = CARTESIAN_POINT ( 'NONE',  ( -76.38857008572975360, 90.29828471680511370, -90.66710916952459343 ) ) ;
#49582 = LINE ( 'NONE', #85039, #79507 ) ;
#49583 = LINE ( 'NONE', #42321, #1252 ) ;
#49584 = AXIS2_PLACEMENT_3D ( 'NONE', #89452, #69899, #82653 ) ;
#49585 = CARTESIAN_POINT ( 'NONE',  ( 100.8224265971273326, -29.20115443902030705, 36.62705384733894221 ) ) ;
#49586 = DIRECTION ( 'NONE',  ( 0.7071067811865513475, -0.7071067811865436870, 7.071067811865519707E-16 ) ) ;
#49587 = VERTEX_POINT ( 'NONE', #59950 ) ;
#49588 = VECTOR ( 'NONE', #58009, 1000.000000000000000 ) ;
#49589 = CARTESIAN_POINT ( 'NONE',  ( 111.3409431244321439, -27.17319409035083666, 20.74133956162494030 ) ) ;
#49590 = PLANE ( 'NONE',  #71451 ) ;
#49591 = CARTESIAN_POINT ( 'NONE',  ( 106.1383370350330324, -47.74387551462719159, 262.4975300378158636 ) ) ;
#49592 = ORIENTED_EDGE ( 'NONE', *, *, #60861, .T. ) ;
#49593 = VECTOR ( 'NONE', #77141, 1000.000000000000114 ) ;
#49594 = EDGE_CURVE ( 'NONE', #77147, #71100, #68133, .T. ) ;
#49595 = CARTESIAN_POINT ( 'NONE',  ( 44.45000000000000284, 66.67499999999999716, 292.1000000000000227 ) ) ;
#49597 = EDGE_CURVE ( 'NONE', #36775, #24180, #40420, .T. ) ;
#49596 = LINE ( 'NONE', #42775, #50061 ) ;
#49598 = DIRECTION ( 'NONE',  ( 0.000000000000000000, -1.000000000000000000, 0.000000000000000000 ) ) ;
#49599 = VECTOR ( 'NONE', #87755, 1000.000000000000000 ) ;
#49600 = EDGE_CURVE ( 'NONE', #77142, #3395, #80886, .T. ) ;
#49601 = CARTESIAN_POINT ( 'NONE',  ( 100.5332814249895108, -41.62301430380158962, 64.65666179816298609 ) ) ;
#49602 = CARTESIAN_POINT ( 'NONE',  ( 114.8301775850900128, -29.68641892472961175, 205.4127681330539872 ) ) ;
#49603 = LINE ( 'NONE', #87715, #44941 ) ;
#49604 = VERTEX_POINT ( 'NONE', #74048 ) ;
#49605 = CIRCLE ( 'NONE', #72834, 2.029999999999997140 ) ;
#49606 = EDGE_CURVE ( 'NONE', #16666, #47179, #60404, .T. ) ;
#49607 = CYLINDRICAL_SURFACE ( 'NONE', #24799, 0.4999999999999982236 ) ;
#49608 = VERTEX_POINT ( 'NONE', #33161 ) ;
#49609 = ORIENTED_EDGE ( 'NONE', *, *, #88052, .T. ) ;
#49610 = CARTESIAN_POINT ( 'NONE',  ( 163.0664832912739826, 22.62155284005901024, 333.4006252759110112 ) ) ;
#49611 = ORIENTED_EDGE ( 'NONE', *, *, #27620, .T. ) ;
#49612 = ORIENTED_EDGE ( 'NONE', *, *, #32195, .T. ) ;
#49613 = CARTESIAN_POINT ( 'NONE',  ( 179.4595971212723100, -26.00627455218570461, 313.9678068554149490 ) ) ;
#49614 = CARTESIAN_POINT ( 'NONE',  ( 107.9985670441620726, -25.30821118569420491, 321.5222355017487530 ) ) ;
#49615 = CARTESIAN_POINT ( 'NONE',  ( 114.9386757252747771, -33.34113070369811993, 78.57241982807700253 ) ) ;
#49616 = CARTESIAN_POINT ( 'NONE',  ( 97.53973001301494605, -43.81993288943278486, 261.8356252759109566 ) ) ;
#49617 = CARTESIAN_POINT ( 'NONE',  ( 177.0664832912730162, 12.92155284005730387, 355.9756252759109998 ) ) ;
#49618 = CARTESIAN_POINT ( 'NONE',  ( -41.60202597009397607, 40.59999999999997300, 54.55338361873603503 ) ) ;
#49619 = ORIENTED_EDGE ( 'NONE', *, *, #58033, .F. ) ;
#49620 = VERTEX_POINT ( 'NONE', #69480 ) ;
#49621 = DIRECTION ( 'NONE',  ( 1.000000000000000000, 4.163336342344333240E-14, 0.000000000000000000 ) ) ;
#49622 = VECTOR ( 'NONE', #63413, 1000.000000000000000 ) ;
#49623 = DIRECTION ( 'NONE',  ( -4.237773401492740281E-14, 1.000000000000000000, 0.000000000000000000 ) ) ;
#49624 = CARTESIAN_POINT ( 'NONE',  ( 163.0664832912739826, 12.92155284005902516, 330.1506252759110680 ) ) ;
#49625 = AXIS2_PLACEMENT_3D ( 'NONE', #32494, #73842, #66573 ) ;
#49626 = CARTESIAN_POINT ( 'NONE',  ( 99.34849973496650932, -28.72665311504486141, 115.6870538473399534 ) ) ;
#49627 = CARTESIAN_POINT ( 'NONE',  ( 116.7155050624037926, -32.57635518107161943, 79.14991099019697174 ) ) ;
#49628 = DIRECTION ( 'NONE',  ( 1.000000000000000000, 4.163336342344333240E-14, 0.000000000000000000 ) ) ;
#49629 = VERTEX_POINT ( 'NONE', #40859 ) ;
#49630 = UNCERTAINTY_MEASURE_WITH_UNIT (LENGTH_MEASURE( 1.000000000000000082E-05 ), #38593, 'distance_accuracy_value', 'NONE');
#49631 = CARTESIAN_POINT ( 'NONE',  ( 96.51793475972648650, -31.32865002300666646, 245.9499109901969689 ) ) ;
#49632 = DIRECTION ( 'NONE',  ( 2.056463827196271584E-15, -0.8571673007021100021, 0.5150380749100580413 ) ) ;
#49633 = CARTESIAN_POINT ( 'NONE',  ( 12.28931626436909497, 79.31803562664185847, 129.9766762937439069 ) ) ;
#49634 = LINE ( 'NONE', #62822, #73510 ) ;
#49636 = FACE_OUTER_BOUND ( 'NONE', #53523, .T. ) ;
#49635 = LINE ( 'NONE', #36484, #70959 ) ;
#49637 = CARTESIAN_POINT ( 'NONE',  ( 105.0850183953499197, -25.44292241093928553, 321.8714993217711822 ) ) ;
#49638 = DIRECTION ( 'NONE',  ( -3.100000000000000258E-29, 3.100000000000000044E-14, 1.000000000000000000 ) ) ;
#49639 = AXIS2_PLACEMENT_3D ( 'NONE', #34534, #21365, #26819 ) ;
#49640 = CARTESIAN_POINT ( 'NONE',  ( 11.39384497175739064, 88.17529471328433033, -118.0073914794113961 ) ) ;
#49641 = CARTESIAN_POINT ( 'NONE',  ( 0.000000000000000000, 239.0000000000000000, 154.6557476874258441 ) ) ;
#49642 = CYLINDRICAL_SURFACE ( 'NONE', #34374, 3.500000000000003109 ) ;
#49643 = DIRECTION ( 'NONE',  ( 0.000000000000000000, -1.000000000000000000, 0.000000000000000000 ) ) ;
#49644 = VECTOR ( 'NONE', #73834, 1000.000000000000000 ) ;
#49646 = ORIENTED_EDGE ( 'NONE', *, *, #59807, .T. ) ;
#49645 = CARTESIAN_POINT ( 'NONE',  ( 97.07207205388709781, -35.37844123507927918, 261.2189586121116918 ) ) ;
#49647 = DIRECTION ( 'NONE',  ( -1.821299053822143307E-16, 0.000000000000000000, 1.000000000000000000 ) ) ;
#49648 = CARTESIAN_POINT ( 'NONE',  ( 115.2691655829841579, -30.20224515277380917, 244.3613395616249875 ) ) ;
#49649 = CARTESIAN_POINT ( 'NONE',  ( 97.74639642956380214, -42.67166664343270099, 137.7661014663869992 ) ) ;
#49650 = CARTESIAN_POINT ( 'NONE',  ( 116.1774319148507573, -31.53050193741562524, 285.2384824187680579 ) ) ;
#49651 = LINE ( 'NONE', #28313, #38877 ) ;
#49653 = CARTESIAN_POINT ( 'NONE',  ( 90.44969454456413871, -50.82895651782494895, 229.5838068554169809 ) ) ;
#49652 = CARTESIAN_POINT ( 'NONE',  ( 3.063943826786759644E-15, 125.7300000000000040, 24.63800000000000168 ) ) ;
#49654 = CARTESIAN_POINT ( 'NONE',  ( 117.0608918343000653, -38.08047937793136128, 139.7189565292726172 ) ) ;
#49655 = VECTOR ( 'NONE', #65834, 1000.000000000000000 ) ;
#49656 = ADVANCED_FACE ( 'NONE', ( #55369 ), #63097, .F. ) ;
#49657 = ORIENTED_EDGE ( 'NONE', *, *, #63577, .T. ) ;
#49658 = ADVANCED_FACE ( 'NONE', ( #82679 ), #75843, .T. ) ;
#49659 = DIRECTION ( 'NONE',  ( 0.000000000000000000, 0.000000000000000000, -1.000000000000000000 ) ) ;
#49660 = ORIENTED_EDGE ( 'NONE', *, *, #66395, .T. ) ;
#49661 = AXIS2_PLACEMENT_3D ( 'NONE', #80720, #65294, #54756 ) ;
#49662 = CARTESIAN_POINT ( 'NONE',  ( 113.5378671157686910, -31.15474330070945541, 183.8152769709339793 ) ) ;
#49663 = EDGE_CURVE ( 'NONE', #29598, #55608, #42200, .T. ) ;
#49665 = VERTEX_POINT ( 'NONE', #49000 ) ;
#49664 = CARTESIAN_POINT ( 'NONE',  ( 23.27731929905161223, 53.97500000000000142, 30.16249999999999076 ) ) ;
#49666 = LINE ( 'NONE', #77848, #82376 ) ;
#49667 = CARTESIAN_POINT ( 'NONE',  ( 97.40233316251689644, -42.04621543282986096, 172.7146728949589942 ) ) ;
#49668 = DIRECTION ( 'NONE',  ( -4.299999999999999979E-14, 1.000000000000000000, -4.400000000000000367E-29 ) ) ;
#49669 = FACE_OUTER_BOUND ( 'NONE', #33018, .T. ) ;
#49670 = CARTESIAN_POINT ( 'NONE',  ( 107.0667039024470313, -104.2784471599409528, 22.21780685541800082 ) ) ;
#49671 = ADVANCED_FACE ( 'NONE', ( #34494, #7256 ), #52185, .F. ) ;
#49672 = EDGE_CURVE ( 'NONE', #10162, #52592, #83121, .T. ) ;
#49673 = DIRECTION ( 'NONE',  ( 2.900000000000000265E-14, -2.000000000000000155E-15, 1.000000000000000000 ) ) ;
#49674 = DIRECTION ( 'NONE',  ( 1.000000000000000000, 0.000000000000000000, 0.000000000000000000 ) ) ;
#49675 = CARTESIAN_POINT ( 'NONE',  ( 107.9743429475490615, -26.39917242597363867, 109.9946728949599759 ) ) ;
#49676 = ORIENTED_EDGE ( 'NONE', *, *, #51917, .T. ) ;
#49677 = ORIENTED_EDGE ( 'NONE', *, *, #56375, .F. ) ;
#49678 = ORIENTED_EDGE ( 'NONE', *, *, #63491, .T. ) ;
#49679 = ADVANCED_FACE ( 'NONE', ( #34943 ), #27238, .F. ) ;
#49680 = CARTESIAN_POINT ( 'NONE',  ( 98.44267559312871185, -33.00030968290830202, 57.44539282970595195 ) ) ;
#49681 = DIRECTION ( 'NONE',  ( 1.000000000000000078E-15, -1.000000000000000000, 0.000000000000000000 ) ) ;
#49682 =( BOUNDED_CURVE ( )  B_SPLINE_CURVE ( 3, ( #4099, #59493, #67671, #25888 ),
 .UNSPECIFIED., .F., .T. ) 
 B_SPLINE_CURVE_WITH_KNOTS ( ( 4, 4 ),
 ( 1.504499544760546481, 1.569169445332449397 ),
 .UNSPECIFIED. ) 
 CURVE ( )  GEOMETRIC_REPRESENTATION_ITEM ( )  RATIONAL_B_SPLINE_CURVE ( ( 1.000000000000000000, 0.9996515140281859724, 0.9996515140281859724, 1.000000000000000000 ) ) 
 REPRESENTATION_ITEM ( '' )  );
#49684 = DIRECTION ( 'NONE',  ( 0.000000000000000000, 0.000000000000000000, 1.000000000000000000 ) ) ;
#49683 = CARTESIAN_POINT ( 'NONE',  ( 118.1473594538625349, -37.63838399483782382, 184.7613395616249647 ) ) ;
#49685 = DIRECTION ( 'NONE',  ( 0.000000000000000000, -1.000000000000000000, 0.000000000000000000 ) ) ;
#49686 = EDGE_CURVE ( 'NONE', #82238, #19244, #34037, .T. ) ;
#49687 = DIRECTION ( 'NONE',  ( -1.000000000000000000, 0.000000000000000000, -2.108231265501709878E-16 ) ) ;
#49688 = CARTESIAN_POINT ( 'NONE',  ( 162.7131505118539962, -33.70561438052090608, 193.9678068554150059 ) ) ;
#49689 = CIRCLE ( 'NONE', #13576, 8.636000000000004562 ) ;
#49690 = DIRECTION ( 'NONE',  ( 0.000000000000000000, 0.000000000000000000, 1.000000000000000000 ) ) ;
#49691 = CARTESIAN_POINT ( 'NONE',  ( 125.0664851986225443, -56.72944715994101728, -4.824374724089012467 ) ) ;
#49692 = EDGE_CURVE ( 'NONE', #2723, #18676, #61894, .T. ) ;
#49693 = CARTESIAN_POINT ( 'NONE',  ( 113.8422018911647484, -44.62364141802228090, 108.1413395616249744 ) ) ;
#49694 = ORIENTED_EDGE ( 'NONE', *, *, #78519, .T. ) ;
#49695 = VERTEX_POINT ( 'NONE', #432 ) ;
#49697 = EDGE_LOOP ( 'NONE', ( #23896, #34762, #26207, #72754, #79602, #25355 ) ) ;
#49696 = EDGE_CURVE ( 'NONE', #69894, #23016, #42637, .T. ) ;
#49698 = CARTESIAN_POINT ( 'NONE',  ( 12.03356702080700202, 78.46872568947895843, 130.0002966128845969 ) ) ;
#49699 = CARTESIAN_POINT ( 'NONE',  ( -99.78216974382876003, 88.91243380484087311, -84.19383299529374654 ) ) ;
#49700 = DIRECTION ( 'NONE',  ( -4.237773401492740281E-14, 1.000000000000000000, 0.000000000000000000 ) ) ;
#49701 = DIRECTION ( 'NONE',  ( -0.4214249218767880945, -0.9068632946707806397, -4.214249218767889924E-16 ) ) ;
#49702 = CARTESIAN_POINT ( 'NONE',  ( 109.4710126485015280, -28.41565358443893174, 212.6585665600669870 ) ) ;
#49703 = CIRCLE ( 'NONE', #70016, 3.299999999999997158 ) ;
#49704 = CARTESIAN_POINT ( 'NONE',  ( 31.90335556477799628, -33.89581943344391135, 237.4678068554150059 ) ) ;
#49705 = CARTESIAN_POINT ( 'NONE',  ( 19.56670390244734747, -25.42844715994192129, 300.4678068554150059 ) ) ;
#49706 = ORIENTED_EDGE ( 'NONE', *, *, #17109, .F. ) ;
#49708 = ORIENTED_EDGE ( 'NONE', *, *, #45114, .F. ) ;
#49707 = ORIENTED_EDGE ( 'NONE', *, *, #11256, .F. ) ;
#49709 = EDGE_CURVE ( 'NONE', #28060, #37074, #57527, .T. ) ;
#49710 = CARTESIAN_POINT ( 'NONE',  ( 71.77848634863079269, 120.6499999999999915, 77.39114642429989033 ) ) ;
#49711 = ORIENTED_EDGE ( 'NONE', *, *, #25781, .T. ) ;
#49712 = ORIENTED_EDGE ( 'NONE', *, *, #67648, .T. ) ;
#49714 = ADVANCED_FACE ( 'NONE', ( #49908 ), #13174, .T. ) ;
#49713 = CARTESIAN_POINT ( 'NONE',  ( -34.53140813619931748, 54.97499999999996589, 35.02576496182814481 ) ) ;
#49715 = ADVANCED_FACE ( 'NONE', ( #54916 ), #11151, .T. ) ;
#49716 = CARTESIAN_POINT ( 'NONE',  ( 115.9273305379513062, -35.98950415022901694, 250.3244404487543022 ) ) ;
#49717 = CARTESIAN_POINT ( 'NONE',  ( 154.4532655810165238, -72.54279768053240218, 540.9756252759101471 ) ) ;
#49718 = ORIENTED_EDGE ( 'NONE', *, *, #17430, .F. ) ;
#49719 = ADVANCED_FACE ( 'NONE', ( #87029 ), #31152, .T. ) ;
#49720 = CARTESIAN_POINT ( 'NONE',  ( 179.1667039024460166, -26.71338133339251542, -5.074374724088000832 ) ) ;
#49721 = DIRECTION ( 'NONE',  ( 0.000000000000000000, 0.000000000000000000, 1.000000000000000000 ) ) ;
#49722 = EDGE_LOOP ( 'NONE', ( #11259, #12401 ) ) ;
#49723 = EDGE_LOOP ( 'NONE', ( #28731, #52758, #67366, #7762 ) ) ;
#49724 = AXIS2_PLACEMENT_3D ( 'NONE', #75797, #12678, #13563 ) ;
#49725 = CARTESIAN_POINT ( 'NONE',  ( -7.941868552260229762E-13, 120.6499999999999915, 107.7702177616926065 ) ) ;
#49726 = ORIENTED_EDGE ( 'NONE', *, *, #45348, .F. ) ;
#49727 = EDGE_LOOP ( 'NONE', ( #86176, #21817, #61101, #12856 ) ) ;
#49728 = AXIS2_PLACEMENT_3D ( 'NONE', #42371, #70100, #27861 ) ;
#49729 = CARTESIAN_POINT ( 'NONE',  ( 115.8942015304759252, -33.87145029861233070, 281.8938046553057575 ) ) ;
#49730 = CARTESIAN_POINT ( 'NONE',  ( 102.0403423364015509, -46.60028036886249225, 172.2137205140059564 ) ) ;
#49731 = CARTESIAN_POINT ( 'NONE',  ( 107.6020193903983824, -26.30459096080988246, 95.03562527591097364 ) ) ;
#49732 = SURFACE_SIDE_STYLE ('',( #247 ) ) ;
#49733 = FACE_OUTER_BOUND ( 'NONE', #63358, .T. ) ;
#49734 = CARTESIAN_POINT ( 'NONE',  ( 110.0520154068402263, -26.08705182471624795, 215.8708633711489711 ) ) ;
#49735 = CARTESIAN_POINT ( 'NONE',  ( -492.0614999999999668, 93.66249999999999432, 6.350000000000409983 ) ) ;
#49736 = DIRECTION ( 'NONE',  ( 0.000000000000000000, 0.000000000000000000, 1.000000000000000000 ) ) ;
#49737 = ORIENTED_EDGE ( 'NONE', *, *, #17689, .T. ) ;
#49738 = CARTESIAN_POINT ( 'NONE',  ( 130.0004344034681765, 78.46444036551649504, 12.03207709110674806 ) ) ;
#49739 = ORIENTED_EDGE ( 'NONE', *, *, #2789, .T. ) ;
#49740 = ORIENTED_EDGE ( 'NONE', *, *, #49441, .F. ) ;
#49741 = CARTESIAN_POINT ( 'NONE',  ( 21.03689327557705369, -23.42844715994186089, 313.9678068554150059 ) ) ;
#49742 = VERTEX_POINT ( 'NONE', #52462 ) ;
#49743 = CARTESIAN_POINT ( 'NONE',  ( 96.69902036285651548, -37.82614351231516281, 126.4099109901969626 ) ) ;
#49744 = CARTESIAN_POINT ( 'NONE',  ( 31.71315051185499811, -33.70561438052111214, -5.074374724088000832 ) ) ;
#49745 = CARTESIAN_POINT ( 'NONE',  ( 135.6073602527815183, -34.45223222829677212, 7.843813999039347173 ) ) ;
#49746 = FACE_OUTER_BOUND ( 'NONE', #43084, .T. ) ;
#49749 = CARTESIAN_POINT ( 'NONE',  ( 99.34937008002601999, -28.84845824588786911, 266.7051490854347549 ) ) ;
#49748 = FACE_OUTER_BOUND ( 'NONE', #81040, .T. ) ;
#49747 = LINE ( 'NONE', #57012, #53394 ) ;
#49750 = DIRECTION ( 'NONE',  ( 0.000000000000000000, 0.000000000000000000, 1.000000000000000000 ) ) ;
#49751 = CARTESIAN_POINT ( 'NONE',  ( -9.261585182541640648, 223.9999999999999716, 152.5407914452011084 ) ) ;
#49752 = DIRECTION ( 'NONE',  ( -0.000000000000000000, 1.000000000000000000, -0.000000000000000000 ) ) ;
#49753 = CIRCLE ( 'NONE', #83109, 130.5560000000000116 ) ;
#49754 = PLANE ( 'NONE',  #19577 ) ;
#49755 = CARTESIAN_POINT ( 'NONE',  ( 165.9667039024459996, -26.71338133339301635, -5.074374724088000832 ) ) ;
#49756 = CARTESIAN_POINT ( 'NONE',  ( 146.5585094824388648, -137.3868253791688687, 246.8399677638830667 ) ) ;
#49758 = ORIENTED_EDGE ( 'NONE', *, *, #87559, .T. ) ;
#49757 = CARTESIAN_POINT ( 'NONE',  ( 118.1498169324930529, -36.11903826555217023, 273.8822919425775808 ) ) ;
#49759 = CARTESIAN_POINT ( 'NONE',  ( 183.5150000000000148, 68.61249999999999716, -35.28456447661459805 ) ) ;
#49760 = CARTESIAN_POINT ( 'NONE',  ( 117.3318588842742685, -34.78817910010258174, 158.9756252759109714 ) ) ;
#49761 = CARTESIAN_POINT ( 'NONE',  ( 115.6112259330891305, -28.51835778375803798, 35.43562527591098643 ) ) ;
#49762 = CARTESIAN_POINT ( 'NONE',  ( 115.0729613760110084, -29.04219751930509119, 185.4232443235299570 ) ) ;
#49763 = DIRECTION ( 'NONE',  ( 0.000000000000000000, 0.000000000000000000, -1.000000000000000000 ) ) ;
#49764 = LINE ( 'NONE', #1650, #14133 ) ;
#49766 = DIRECTION ( 'NONE',  ( 1.000000000000000000, 8.953411488912556626E-16, 0.000000000000000000 ) ) ;
#49765 = LINE ( 'NONE', #29792, #43492 ) ;
#49767 = CARTESIAN_POINT ( 'NONE',  ( 29.56670390244797630, -67.87844715994100397, 20.91780685541479912 ) ) ;
#49768 = DIRECTION ( 'NONE',  ( 0.7071067811865441310, 0.000000000000000000, 0.7071067811865510144 ) ) ;
#49769 = EDGE_LOOP ( 'NONE', ( #73662, #66214, #27170, #52005 ) ) ;
#49770 = CIRCLE ( 'NONE', #74481, 9.524999999999998579 ) ;
#49771 = CARTESIAN_POINT ( 'NONE',  ( 51.39690000000000225, 82.54999999999999716, 335.3740053999999304 ) ) ;
#49772 = ADVANCED_FACE ( 'NONE', ( #65671 ), #72058, .F. ) ;
#49773 = ORIENTED_EDGE ( 'NONE', *, *, #19493, .F. ) ;
#49774 = EDGE_CURVE ( 'NONE', #43762, #36567, #38857, .T. ) ;
#49775 = VERTEX_POINT ( 'NONE', #66114 ) ;
#49776 = EDGE_CURVE ( 'NONE', #77006, #11339, #44417, .T. ) ;
#49778 = ORIENTED_EDGE ( 'NONE', *, *, #23144, .F. ) ;
#49777 = DIRECTION ( 'NONE',  ( 0.000000000000000000, 0.000000000000000000, 1.000000000000000000 ) ) ;
#49779 = CARTESIAN_POINT ( 'NONE',  ( 115.0059970501926330, -43.50650750775896825, 59.26419670448196086 ) ) ;
#49780 = LINE ( 'NONE', #70694, #29534 ) ;
#49781 = PLANE ( 'NONE',  #35472 ) ;
#49782 = EDGE_CURVE ( 'NONE', #12034, #61226, #19589, .T. ) ;
#49783 = CARTESIAN_POINT ( 'NONE',  ( 98.05313438099307177, -42.12366292992533801, 157.7556252759109725 ) ) ;
#49784 = CARTESIAN_POINT ( 'NONE',  ( 101.3905103160957850, -43.11219441383617124, 266.4209912566481080 ) ) ;
#49785 = ORIENTED_EDGE ( 'NONE', *, *, #82638, .T. ) ;
#49786 = ORIENTED_EDGE ( 'NONE', *, *, #35730, .F. ) ;
#49787 = ORIENTED_EDGE ( 'NONE', *, *, #79758, .T. ) ;
#49788 = EDGE_CURVE ( 'NONE', #78225, #11071, #73382, .T. ) ;
#49789 = AXIS2_PLACEMENT_3D ( 'NONE', #34338, #14367, #6643 ) ;
#49790 = EDGE_LOOP ( 'NONE', ( #50797, #27997, #26534, #89729 ) ) ;
#49791 = CARTESIAN_POINT ( 'NONE',  ( 109.6430121338576953, -46.48008673429469439, 107.7814586095166334 ) ) ;
#49792 = CARTESIAN_POINT ( 'NONE',  ( 21.03689327557711763, -23.42844715994186089, 249.9678068554150059 ) ) ;
#49794 = AXIS2_PLACEMENT_3D ( 'NONE', #37346, #30533, #65053 ) ;
#49793 = DIRECTION ( 'NONE',  ( -1.000000000000000000, 0.000000000000000000, 0.000000000000000000 ) ) ;
#49795 = DIRECTION ( 'NONE',  ( -1.000000000000000000, 0.000000000000000000, 0.000000000000000000 ) ) ;
#49796 = CARTESIAN_POINT ( 'NONE',  ( 82.97845804870276254, 84.21348395916255924, 100.7940789023230508 ) ) ;
#49797 = LINE ( 'NONE', #6682, #74176 ) ;
#49798 = ADVANCED_FACE ( 'NONE', ( #72508 ), #79271, .F. ) ;
#49799 = DIRECTION ( 'NONE',  ( 0.000000000000000000, -1.000000000000000000, 0.000000000000000000 ) ) ;
#49800 = DIRECTION ( 'NONE',  ( 0.000000000000000000, 0.000000000000000000, 1.000000000000000000 ) ) ;
#49801 = CARTESIAN_POINT ( 'NONE',  ( 95.28387218206118803, -35.72034718286344201, 36.25848241876794731 ) ) ;
#49802 = DIRECTION ( 'NONE',  ( 0.000000000000000000, -1.000000000000000000, 0.000000000000000000 ) ) ;
#49804 = EDGE_LOOP ( 'NONE', ( #71578, #42395, #2598, #56887 ) ) ;
#49803 = EDGE_CURVE ( 'NONE', #52054, #46455, #72000, .T. ) ;
#49805 = DIRECTION ( 'NONE',  ( 0.000000000000000000, 0.000000000000000000, -1.000000000000000000 ) ) ;
#49806 = CARTESIAN_POINT ( 'NONE',  ( -55.59646339173026774, 54.92078272276780382, 70.77919445882530169 ) ) ;
#49807 = CARTESIAN_POINT ( 'NONE',  ( 112.4846873277006267, -29.98081840548436006, 117.3442808457819666 ) ) ;
#49808 = ADVANCED_FACE ( 'NONE', ( #86138 ), #87915, .F. ) ;
#49809 = VECTOR ( 'NONE', #64094, 1000.000000000000000 ) ;
#49810 = DIRECTION ( 'NONE',  ( -0.7071067811865165975, -0.7071067811865784369, -7.071067811865158803E-16 ) ) ;
#49811 = DIRECTION ( 'NONE',  ( 0.8660254037844392627, 0.000000000000000000, -0.4999999999999990008 ) ) ;
#49812 = EDGE_LOOP ( 'NONE', ( #31235, #69274 ) ) ;
#49813 = ORIENTED_EDGE ( 'NONE', *, *, #22556, .T. ) ;
#49814 = CARTESIAN_POINT ( 'NONE',  ( 97.81316109541715775, -40.52102254706596796, 136.6363148235126630 ) ) ;
#49815 = AXIS2_PLACEMENT_3D ( 'NONE', #3767, #11017, #24654 ) ;
#49816 = VERTEX_POINT ( 'NONE', #79330 ) ;
#49817 = ORIENTED_EDGE ( 'NONE', *, *, #78101, .T. ) ;
#49818 = CARTESIAN_POINT ( 'NONE',  ( 99.43677639672335999, -41.29559517668970869, 158.1872975916109567 ) ) ;
#49819 = CARTESIAN_POINT ( 'NONE',  ( 80.06648329127402519, -46.72944715994105991, 4.925625275910944012 ) ) ;
#49820 = EDGE_CURVE ( 'NONE', #61816, #45134, #17094, .T. ) ;
#49821 = CARTESIAN_POINT ( 'NONE',  ( 117.3749687695755171, -38.63058443890392368, 84.68133956162593279 ) ) ;
#49822 = VECTOR ( 'NONE', #23822, 1000.000000000000000 ) ;
#49823 = CARTESIAN_POINT ( 'NONE',  ( 72.31648329127402519, -56.72944715994105991, 14.67562527591093513 ) ) ;
#49824 = ORIENTED_EDGE ( 'NONE', *, *, #16682, .F. ) ;
#49825 = VERTEX_POINT ( 'NONE', #33839 ) ;
#49826 = ORIENTED_EDGE ( 'NONE', *, *, #72057, .F. ) ;
#49827 = CARTESIAN_POINT ( 'NONE',  ( 114.1400169897070924, -40.01656155057797548, 9.125625275910977052 ) ) ;
#49828 = ORIENTED_EDGE ( 'NONE', *, *, #60209, .T. ) ;
#49829 = CARTESIAN_POINT ( 'NONE',  ( 97.12559377168363994, -39.79659400623925336, 21.56419670448195092 ) ) ;
#49830 = CARTESIAN_POINT ( 'NONE',  ( 117.4480285489056683, -30.96353277002295101, 175.2299109901969700 ) ) ;
#49831 = FACE_OUTER_BOUND ( 'NONE', #89855, .T. ) ;
#49832 = CARTESIAN_POINT ( 'NONE',  ( 51.56670390244899238, -32.29483332968450782, 237.4678068554150059 ) ) ;
#49833 = CARTESIAN_POINT ( 'NONE',  ( 95.67524734051724522, -33.46228404877688689, 137.1041967044819501 ) ) ;
#49834 = CARTESIAN_POINT ( 'NONE',  ( -27.27158787008326968, 184.0000000000000000, 106.1020876358972771 ) ) ;
#49835 = EDGE_LOOP ( 'NONE', ( #43545, #70199, #82842, #89839 ) ) ;
#49836 = CARTESIAN_POINT ( 'NONE',  ( 0.000000000000000000, 125.7300000000000040, -24.63800000000000168 ) ) ;
#49837 = EDGE_CURVE ( 'NONE', #23384, #86581, #41092, .T. ) ;
#49838 = EDGE_LOOP ( 'NONE', ( #77371, #5698, #21196, #42352 ) ) ;
#49839 = LINE ( 'NONE', #8080, #70929 ) ;
#49840 = ORIENTED_EDGE ( 'NONE', *, *, #13993, .T. ) ;
#49841 = ORIENTED_EDGE ( 'NONE', *, *, #1912, .F. ) ;
#49843 = ADVANCED_FACE ( 'NONE', ( #74733 ), #81572, .T. ) ;
#49842 = CIRCLE ( 'NONE', #64391, 12.99999999999999822 ) ;
#49844 = LINE ( 'NONE', #43473, #43136 ) ;
#49845 = CARTESIAN_POINT ( 'NONE',  ( 7.669751788741939080, 92.55534477396975035, 118.3080865832529440 ) ) ;
#49846 = CARTESIAN_POINT ( 'NONE',  ( 111.3232390708907786, -27.21277439355663219, 24.74133956162494030 ) ) ;
#49847 = CARTESIAN_POINT ( 'NONE',  ( 12.65714626781473839, 68.30105204775735217, 35.94211041470738621 ) ) ;
#49848 = VECTOR ( 'NONE', #87179, 1000.000000000000114 ) ;
#49849 = DIRECTION ( 'NONE',  ( 0.000000000000000000, 0.000000000000000000, 1.000000000000000000 ) ) ;
#49850 = CARTESIAN_POINT ( 'NONE',  ( 63.06670390244699576, -67.87844715994098976, 85.21780685541799016 ) ) ;
#49851 = CARTESIAN_POINT ( 'NONE',  ( 106.9359508110862720, -26.91635713860562973, 60.08705384733998045 ) ) ;
#49853 = CARTESIAN_POINT ( 'NONE',  ( 99.11802762103509679, -45.48540990049882282, 152.9899109901969894 ) ) ;
#49852 = DIRECTION ( 'NONE',  ( -4.237773401492740281E-14, 1.000000000000000000, 0.000000000000000000 ) ) ;
#49854 = FACE_BOUND ( 'NONE', #86199, .T. ) ;
#49855 = CARTESIAN_POINT ( 'NONE',  ( 41.56648329127399677, 0.2215528400590013880, 138.9256252759119832 ) ) ;
#49856 = ORIENTED_EDGE ( 'NONE', *, *, #67419, .T. ) ;
#49857 = CARTESIAN_POINT ( 'NONE',  ( 89.06648138392552028, -56.72944715994104570, 14.67562527591095289 ) ) ;
#49858 = CARTESIAN_POINT ( 'NONE',  ( 142.8698897858160706, -0.9167816978817300289, 394.9756252759102040 ) ) ;
#49859 = CARTESIAN_POINT ( 'NONE',  ( 107.0667039024470313, -104.2784471599413934, 2.217806855418003043 ) ) ;
#49860 = ORIENTED_EDGE ( 'NONE', *, *, #48026, .T. ) ;
#49861 = LINE ( 'NONE', #63504, #50527 ) ;
#49863 = ORIENTED_EDGE ( 'NONE', *, *, #8810, .T. ) ;
#49862 = CARTESIAN_POINT ( 'NONE',  ( 113.7790015168560558, -44.76367177190390834, 193.1299109901969757 ) ) ;
#49864 = DIRECTION ( 'NONE',  ( -1.000000000000000000, 0.000000000000000000, 0.000000000000000000 ) ) ;
#49865 = CARTESIAN_POINT ( 'NONE',  ( 113.1681127151884141, -26.54159316308081173, 200.6470538473399756 ) ) ;
#49866 = CARTESIAN_POINT ( 'NONE',  ( 103.8278507311454177, -46.72190801433284690, 78.32705384733995402 ) ) ;
#49867 = LINE ( 'NONE', #77599, #49001 ) ;
#49868 = CARTESIAN_POINT ( 'NONE',  ( 22.49541547940886588, 22.69262065192414468, 361.9756252759109998 ) ) ;
#49869 = CARTESIAN_POINT ( 'NONE',  ( 156.5667039024481255, -42.82844715993568485, 257.2178068554149490 ) ) ;
#49870 = ORIENTED_EDGE ( 'NONE', *, *, #15090, .F. ) ;
#49871 = AXIS2_PLACEMENT_3D ( 'NONE', #56275, #42208, #892 ) ;
#49872 = CONTEXT_DEPENDENT_SHAPE_REPRESENTATION ( #75929, #25692 ) ;
#49873 = CIRCLE ( 'NONE', #10709, 2.500000000000002220 ) ;
#49874 = CIRCLE ( 'NONE', #10711, 9.999999999999998224 ) ;
#49875 = ADVANCED_FACE ( 'NONE', ( #82016 ), #74288, .F. ) ;
#49876 = ORIENTED_EDGE ( 'NONE', *, *, #44221, .F. ) ;
#49877 = EDGE_CURVE ( 'NONE', #60674, #81215, #46556, .T. ) ;
#49878 = EDGE_LOOP ( 'NONE', ( #85610, #31054, #23250, #4833, #88548, #52470, #45991, #43456, #19130, #83456, #65208, #38120, #81773, #60760 ) ) ;
#49879 = ADVANCED_FACE ( 'NONE', ( #6585 ), #34280, .T. ) ;
#49880 = ORIENTED_EDGE ( 'NONE', *, *, #16411, .F. ) ;
#49881 = DIRECTION ( 'NONE',  ( 1.777766061779359009E-15, -1.000000000000000000, 3.100000000000000044E-14 ) ) ;
#49882 = CARTESIAN_POINT ( 'NONE',  ( 115.9598434605651107, -30.16574962093465828, 255.3203871806729524 ) ) ;
#49883 = DIRECTION ( 'NONE',  ( -0.7071067811865774377, 0.7071067811865175967, -7.071067811865782003E-16 ) ) ;
#49884 = CARTESIAN_POINT ( 'NONE',  ( 135.1249450788499757, -16.19118199975284611, 1.799893109327562524 ) ) ;
#49885 = EDGE_CURVE ( 'NONE', #17889, #56291, #60637, .T. ) ;
#49887 = DIRECTION ( 'NONE',  ( 0.000000000000000000, 0.000000000000000000, -1.000000000000000000 ) ) ;
#49886 = CARTESIAN_POINT ( 'NONE',  ( 41.56648329127499153, -32.07844715994070839, 23.67562527591200094 ) ) ;
#49888 = PLANE ( 'NONE',  #48633 ) ;
#49889 = CARTESIAN_POINT ( 'NONE',  ( 118.1065893711158594, -37.63027948749972751, 38.77372051400595865 ) ) ;
#49890 = ORIENTED_EDGE ( 'NONE', *, *, #60384, .F. ) ;
#49891 = ORIENTED_EDGE ( 'NONE', *, *, #242, .T. ) ;
#49892 = ADVANCED_FACE ( 'NONE', ( #54701 ), #33394, .T. ) ;
#49893 = CARTESIAN_POINT ( 'NONE',  ( 115.8264675611344359, -31.73180946705375050, 15.24044151184909168 ) ) ;
#49894 = CARTESIAN_POINT ( 'NONE',  ( 110.7503267229639476, -45.78994093226354778, 278.8841967044818375 ) ) ;
#49895 = ADVANCED_FACE ( 'NONE', ( #19770, #39748 ), #53806, .F. ) ;
#49896 = DIRECTION ( 'NONE',  ( 1.000000000000000078E-15, -1.000000000000000083E-30, -1.000000000000000000 ) ) ;
#49897 = CARTESIAN_POINT ( 'NONE',  ( 108.2018929880948548, -26.98138995270375062, 125.9841967044819597 ) ) ;
#49898 = CARTESIAN_POINT ( 'NONE',  ( -68.91674821478457602, 82.54999999999999716, 68.91674821478434865 ) ) ;
#49899 = CARTESIAN_POINT ( 'NONE',  ( 116.3289480479917017, -32.94026123176625731, 29.13562527591096085 ) ) ;
#49900 = EDGE_LOOP ( 'NONE', ( #42904, #36781, #16566, #14009, #16313 ) ) ;
#49901 = CARTESIAN_POINT ( 'NONE',  ( 188.5667039024479834, -65.37844715994100397, 293.2178068554150627 ) ) ;
#49902 = CARTESIAN_POINT ( 'NONE',  ( 97.53184938156154260, -39.74897048756918849, 57.57051766616469024 ) ) ;
#49903 = ORIENTED_EDGE ( 'NONE', *, *, #36808, .F. ) ;
#49904 = ORIENTED_EDGE ( 'NONE', *, *, #9816, .T. ) ;
#49905 = CARTESIAN_POINT ( 'NONE',  ( 255.9983484187079910, 40.03750000000000142, -2.032000000000000028 ) ) ;
#49906 = CARTESIAN_POINT ( 'NONE',  ( 111.8242684682981718, -44.20552626741085334, 259.4587261630397848 ) ) ;
#49907 = AXIS2_PLACEMENT_3D ( 'NONE', #76018, #21973, #26980 ) ;
#49908 = FACE_OUTER_BOUND ( 'NONE', #54838, .T. ) ;
#49909 = CARTESIAN_POINT ( 'NONE',  ( 103.1875000000000000, 101.5999999999999943, -5.041899999999640336 ) ) ;
#49910 = LINE ( 'NONE', #42202, #20075 ) ;
#49911 = DIRECTION ( 'NONE',  ( 0.000000000000000000, 1.000000000000000000, 0.000000000000000000 ) ) ;
#49912 = ORIENTED_EDGE ( 'NONE', *, *, #35262, .T. ) ;
#49913 = FACE_BOUND ( 'NONE', #39804, .T. ) ;
#49914 = DIRECTION ( 'NONE',  ( 0.000000000000000000, 0.000000000000000000, -1.000000000000000000 ) ) ;
#49915 = ORIENTED_EDGE ( 'NONE', *, *, #89926, .T. ) ;
#49916 = CARTESIAN_POINT ( 'NONE',  ( 106.8411850752606966, -48.57806423327891565, 77.56133956162491927 ) ) ;
#49917 = ORIENTED_EDGE ( 'NONE', *, *, #78649, .T. ) ;
#49918 = CARTESIAN_POINT ( 'NONE',  ( 99.98530978427844218, -41.10337153935440568, 11.19051506617196878 ) ) ;
#49919 = CARTESIAN_POINT ( 'NONE',  ( -446.0240000000000009, 3.174999999999999822, -1.387778780781445991E-14 ) ) ;
#49920 = CARTESIAN_POINT ( 'NONE',  ( 116.0678243078411498, -40.55558035091543445, 168.5070538473399608 ) ) ;
#49921 = DIRECTION ( 'NONE',  ( -1.000000000000000000, 0.000000000000000000, 0.000000000000000000 ) ) ;
#49922 = DIRECTION ( 'NONE',  ( -0.000000000000000000, -0.000000000000000000, 1.000000000000000000 ) ) ;
#49923 = CARTESIAN_POINT ( 'NONE',  ( 172.5664832912729878, -18.82844715994071194, 315.9256252759120684 ) ) ;
#49924 = EDGE_CURVE ( 'NONE', #49695, #12195, #66201, .T. ) ;
#49925 = CARTESIAN_POINT ( 'NONE',  ( 173.9900000000000091, 20.32000000000000028, -71.37400000000000944 ) ) ;
#49926 = CARTESIAN_POINT ( 'NONE',  ( 105.1008636489907673, -25.80544433381534475, 271.2061014663873380 ) ) ;
#49927 = CARTESIAN_POINT ( 'NONE',  ( 86.67392531623372065, 94.60304557064719688, -80.89343850130777014 ) ) ;
#49928 = ORIENTED_EDGE ( 'NONE', *, *, #4090, .T. ) ;
#49929 = DIRECTION ( 'NONE',  ( 1.000000000000000000, 1.040834085586083310E-14, 0.000000000000000000 ) ) ;
#49930 = VECTOR ( 'NONE', #70269, 999.9999999999998863 ) ;
#49931 = ORIENTED_EDGE ( 'NONE', *, *, #45348, .T. ) ;
#49932 = CARTESIAN_POINT ( 'NONE',  ( 102.5975616584704966, -46.88947854763195267, 128.2346728949589760 ) ) ;
#49933 = CARTESIAN_POINT ( 'NONE',  ( 79.41328093380936082, -21.40256188477534494, 1.689562700882486723 ) ) ;
#49934 = CIRCLE ( 'NONE', #16564, 10.66800000000000459 ) ;
#49935 = VECTOR ( 'NONE', #21728, 1000.000000000000000 ) ;
#49936 = VERTEX_POINT ( 'NONE', #27472 ) ;
#49937 = VERTEX_POINT ( 'NONE', #46995 ) ;
#49938 = ORIENTED_EDGE ( 'NONE', *, *, #51912, .F. ) ;
#49939 = CIRCLE ( 'NONE', #47009, 11.57110091390437034 ) ;
#49940 = DIRECTION ( 'NONE',  ( 0.000000000000000000, 0.000000000000000000, -1.000000000000000000 ) ) ;
#49941 = VECTOR ( 'NONE', #20203, 1000.000000000000114 ) ;
#49942 = CARTESIAN_POINT ( 'NONE',  ( 105.7995281078892873, -26.72403387351276294, 266.1772911773911119 ) ) ;
#49943 = FACE_OUTER_BOUND ( 'NONE', #45670, .T. ) ;
#49944 = DIRECTION ( 'NONE',  ( 0.000000000000000000, 1.000000000000000000, 0.000000000000000000 ) ) ;
#49945 = DIRECTION ( 'NONE',  ( 0.7071067811865483499, 0.7071067811865466846, 0.000000000000000000 ) ) ;
#49946 = CARTESIAN_POINT ( 'NONE',  ( 115.8915968718629017, -31.17968520675552924, 30.27276813305396175 ) ) ;
#49947 = CARTESIAN_POINT ( 'NONE',  ( 162.7131505118539962, -33.70561438052090608, -5.074374724088000832 ) ) ;
#49948 = EDGE_LOOP ( 'NONE', ( #18470, #20197, #12882, #67239 ) ) ;
#49949 = CARTESIAN_POINT ( 'NONE',  ( 127.0664832912738973, -54.72944906728955772, -4.970821333495670125 ) ) ;
#49950 = CARTESIAN_POINT ( 'NONE',  ( 115.7831080051488613, -41.80230922285955586, 43.40611986575648018 ) ) ;
#49951 = ORIENTED_EDGE ( 'NONE', *, *, #55902, .F. ) ;
#49952 = ORIENTED_EDGE ( 'NONE', *, *, #15251, .T. ) ;
#49953 = EDGE_CURVE ( 'NONE', #51660, #9633, #76334, .T. ) ;
#49954 = CARTESIAN_POINT ( 'NONE',  ( 82.63685198412170507, -19.70758306363565637, 2.855952960430490073 ) ) ;
#49955 = CARTESIAN_POINT ( 'NONE',  ( 116.8182998100438965, -34.15748031063536416, 115.0320983290675656 ) ) ;
#49956 = DIRECTION ( 'NONE',  ( 1.000000000000000000, 0.000000000000000000, -0.000000000000000000 ) ) ;
#49957 = B_SPLINE_CURVE_WITH_KNOTS ( 'NONE', 3,
 ( #37366, #65072, #57804, #72342, #10110, #78725, #85982, #2854, #40381, #19047, #5429, #37818, #30107, #79168, #19494, #23318, #60364, #33124 ),
 .UNSPECIFIED., .F., .F.,
 ( 4, 2, 2, 2, 2, 2, 2, 2, 4 ),
 ( 0.000000000000000000, 0.06250000002257644072, 0.1250000000451528814, 0.1875000000677293222, 0.2500000000903057629, 0.3125000001128822036, 0.3750000001354586443, 0.4375000001580350850, 0.5000000001806115257 ),
 .UNSPECIFIED. ) ;
#49958 = FACE_BOUND ( 'NONE', #11231, .T. ) ;
#49959 = DIRECTION ( 'NONE',  ( 0.000000000000000000, 0.000000000000000000, -1.000000000000000000 ) ) ;
#49960 = CARTESIAN_POINT ( 'NONE',  ( 100.5279579596103332, -31.18870816475473262, 215.1895626852199541 ) ) ;
#49961 = DIRECTION ( 'NONE',  ( -4.299999999999999979E-14, 1.000000000000000000, -4.100000000000000342E-29 ) ) ;
#49962 = CARTESIAN_POINT ( 'NONE',  ( 107.0664832912739968, -36.72944715994100306, -1.864374724089012947 ) ) ;
#49963 = CARTESIAN_POINT ( 'NONE',  ( 96.03104818302425372, -37.92613241492836806, 81.40038718067299328 ) ) ;
#49964 = ORIENTED_EDGE ( 'NONE', *, *, #7693, .T. ) ;
#49965 = DIRECTION ( 'NONE',  ( 0.000000000000000000, 0.000000000000000000, 1.000000000000000000 ) ) ;
#49966 = ORIENTED_EDGE ( 'NONE', *, *, #3749, .T. ) ;
#49967 = CARTESIAN_POINT ( 'NONE',  ( 161.4809174648185888, -48.32844715993547169, 129.9678068554149775 ) ) ;
#49968 = CARTESIAN_POINT ( 'NONE',  ( 167.2371591254543546, -47.82818131005522844, 237.4678068554150059 ) ) ;
#49969 = ORIENTED_EDGE ( 'NONE', *, *, #62898, .F. ) ;
#49970 = LINE ( 'NONE', #15488, #56287 ) ;
#49971 = ORIENTED_EDGE ( 'NONE', *, *, #78221, .F. ) ;
#49972 = CARTESIAN_POINT ( 'NONE',  ( 57.56670390244808289, -42.82844715994040286, 254.7178068554150627 ) ) ;
#49973 = CARTESIAN_POINT ( 'NONE',  ( 67.35067855263200443, -81.16520196425757661, 246.8834897342799763 ) ) ;
#49974 = AXIS2_PLACEMENT_3D ( 'NONE', #17279, #44957, #38159 ) ;
#49975 = DIRECTION ( 'NONE',  ( 0.000000000000000000, -1.000000000000000000, 0.000000000000000000 ) ) ;
#49976 = VERTEX_POINT ( 'NONE', #20669 ) ;
#49977 = CARTESIAN_POINT ( 'NONE',  ( 117.8794170024721240, -39.13275856168890243, 103.6403871806729455 ) ) ;
#49978 = CIRCLE ( 'NONE', #9352, 10.04999999999999361 ) ;
#49980 = CARTESIAN_POINT ( 'NONE',  ( 82.96304607088339367, 80.88456863959029874, -100.8068867829400688 ) ) ;
#49979 = DIRECTION ( 'NONE',  ( 0.08544974978095713769, 0.9963424814100680926, -0.000000000000000000 ) ) ;
#49981 = CARTESIAN_POINT ( 'NONE',  ( 134.0664832912740110, -41.22944715994101017, 10.42562527591099553 ) ) ;
#49982 = CARTESIAN_POINT ( 'NONE',  ( -6.309812078926137602, 71.61276833203498882, 118.1896733548958451 ) ) ;
#49983 = ORIENTED_EDGE ( 'NONE', *, *, #76241, .F. ) ;
#49984 = EDGE_CURVE ( 'NONE', #26649, #17992, #54248, .T. ) ;
#49985 = EDGE_CURVE ( 'NONE', #14599, #13052, #12963, .T. ) ;
#49986 = CARTESIAN_POINT ( 'NONE',  ( 83.06670390244796920, -61.87844715994100397, 201.9838068554149970 ) ) ;
#49987 = DIRECTION ( 'NONE',  ( 0.000000000000000000, 0.000000000000000000, 1.000000000000000000 ) ) ;
#49988 = EDGE_CURVE ( 'NONE', #50110, #23298, #61531, .T. ) ;
#49989 = DIRECTION ( 'NONE',  ( 0.000000000000000000, -1.000000000000000000, 0.000000000000000000 ) ) ;
#49990 = CARTESIAN_POINT ( 'NONE',  ( 103.1665349694895895, -27.03781871365087142, 126.3813395616259783 ) ) ;
#49991 = EDGE_CURVE ( 'NONE', #34477, #2880, #51678, .T. ) ;
#49993 = DIRECTION ( 'NONE',  ( -0.7071067811865165975, -0.7071067811865784369, -7.071067811865470403E-16 ) ) ;
#49992 = CARTESIAN_POINT ( 'NONE',  ( 29.56670390244797630, -48.82844715994099971, 300.9178068554150514 ) ) ;
#49994 = DIRECTION ( 'NONE',  ( 0.000000000000000000, -0.5000000000000087708, 0.8660254037844336006 ) ) ;
#49995 = CIRCLE ( 'NONE', #6495, 0.5000000000000004441 ) ;
#49996 = ORIENTED_EDGE ( 'NONE', *, *, #65477, .F. ) ;
#49997 = CIRCLE ( 'NONE', #5010, 218.1859999999999786 ) ;
#49998 = CIRCLE ( 'NONE', #20966, 13.00000000000000355 ) ;
#49999 = AXIS2_PLACEMENT_3D ( 'NONE', #50196, #50647, #35225 ) ;
#50000 = CARTESIAN_POINT ( 'NONE',  ( 109.2168187703260998, -26.58475186820039582, 180.9222919425769760 ) ) ;
#50001 = EDGE_CURVE ( 'NONE', #25538, #67615, #20224, .T. ) ;
#50003 = ORIENTED_EDGE ( 'NONE', *, *, #25778, .F. ) ;
#50002 = DIRECTION ( 'NONE',  ( 0.000000000000000000, 0.000000000000000000, -1.000000000000000000 ) ) ;
#50004 = AXIS2_PLACEMENT_3D ( 'NONE', #25626, #53302, #81067 ) ;
#50005 = CIRCLE ( 'NONE', #20976, 2.117000000000000881 ) ;
#50006 = CARTESIAN_POINT ( 'NONE',  ( 111.8803037788896262, -27.54327565145516488, 10.68038718067199078 ) ) ;
#50007 = CARTESIAN_POINT ( 'NONE',  ( 179.8585841295800094, -30.08671355700241179, -5.074374724088000832 ) ) ;
#50008 = LINE ( 'NONE', #66662, #72212 ) ;
#50009 = CARTESIAN_POINT ( 'NONE',  ( 126.1218394983595630, -84.35882332054457322, 250.2178068554179333 ) ) ;
#50010 = CARTESIAN_POINT ( 'NONE',  ( 29.56648329127400388, 25.62155284005901379, 328.6381252759109088 ) ) ;
#50011 = FACE_BOUND ( 'NONE', #65739, .T. ) ;
#50012 = CARTESIAN_POINT ( 'NONE',  ( 111.3277751695583078, -45.53312973143663811, 247.9356252759109509 ) ) ;
#50013 = VERTEX_POINT ( 'NONE', #62440 ) ;
#50014 = VERTEX_POINT ( 'NONE', #53358 ) ;
#50015 = CARTESIAN_POINT ( 'NONE',  ( 108.6634326348915351, -27.98234008310821608, 161.3644404487539816 ) ) ;
#50016 = CARTESIAN_POINT ( 'NONE',  ( 63.06670390244699576, -67.87844715994098976, 120.2178068554179902 ) ) ;
#50017 = CARTESIAN_POINT ( 'NONE',  ( 113.0371668699568204, -44.84250099658410704, 29.51301187732496700 ) ) ;
#50018 = DIRECTION ( 'NONE',  ( 1.000000000000000000, 0.000000000000000000, 0.000000000000000000 ) ) ;
#50019 = CARTESIAN_POINT ( 'NONE',  ( 172.5664832912740110, 0.2215528400590013880, 81.04262527591200183 ) ) ;
#50020 = FACE_OUTER_BOUND ( 'NONE', #34912, .T. ) ;
#50021 = DIRECTION ( 'NONE',  ( -2.999999999999999839E-15, 1.000000000000000000, -2.999999999999999900E-30 ) ) ;
#50022 = DIRECTION ( 'NONE',  ( -2.900000000000000265E-14, 2.000000000000000155E-15, -1.000000000000000000 ) ) ;
#50023 = CARTESIAN_POINT ( 'NONE',  ( 103.3114313307233658, -27.02747569519249993, 215.3699109901969848 ) ) ;
#50024 = CARTESIAN_POINT ( 'NONE',  ( 104.1009375265838486, -88.49073317540022288, -21.02845593540859426 ) ) ;
#50025 = ORIENTED_EDGE ( 'NONE', *, *, #56028, .T. ) ;
#50026 = ORIENTED_EDGE ( 'NONE', *, *, #88043, .T. ) ;
#50027 = DIRECTION ( 'NONE',  ( -1.000000000000000000, -1.000000000000000078E-15, 0.000000000000000000 ) ) ;
#50028 = CARTESIAN_POINT ( 'NONE',  ( -74.68844285250172277, 85.85031469618034805, -92.07164801315032321 ) ) ;
#50029 = DIRECTION ( 'NONE',  ( 0.000000000000000000, 0.000000000000000000, -1.000000000000000000 ) ) ;
#50030 = FACE_OUTER_BOUND ( 'NONE', #13816, .T. ) ;
#50031 = EDGE_CURVE ( 'NONE', #72087, #17788, #74915, .T. ) ;
#50033 = CARTESIAN_POINT ( 'NONE',  ( 101.3196941207357469, -46.24713579373438677, 48.14419670448194211 ) ) ;
#50032 = AXIS2_PLACEMENT_3D ( 'NONE', #14106, #63599, #49500 ) ;
#50034 = DIRECTION ( 'NONE',  ( -0.7071067811985215501, 0.7071067811745735954, 0.000000000000000000 ) ) ;
#50035 = VERTEX_POINT ( 'NONE', #15194 ) ;
#50036 = CARTESIAN_POINT ( 'NONE',  ( -0.8226739993993643640, 95.14999999999996305, 118.3559999999999519 ) ) ;
#50037 = DIRECTION ( 'NONE',  ( 1.000000000000000078E-15, -1.000000000000000000, 0.000000000000000000 ) ) ;
#50038 = VECTOR ( 'NONE', #75693, 1000.000000000000000 ) ;
#50039 = EDGE_CURVE ( 'NONE', #61226, #46913, #81404, .T. ) ;
#50040 = CARTESIAN_POINT ( 'NONE',  ( 98.94247553594858857, -30.19587780982054070, 240.7870538473399620 ) ) ;
#50041 = MANIFOLD_SOLID_BREP ( 'Stock-BR-Y-104-1', #24230 ) ;
#50042 = ORIENTED_EDGE ( 'NONE', *, *, #80467, .F. ) ;
#50043 = CARTESIAN_POINT ( 'NONE',  ( 78.16547420785481393, -38.71744337668656044, 7.623533105427367396 ) ) ;
#50044 = DIRECTION ( 'NONE',  ( 0.000000000000000000, 0.000000000000000000, -1.000000000000000000 ) ) ;
#50045 = DIRECTION ( 'NONE',  ( -3.999999999999999995E-14, 1.000000000000000000, -4.100000000000000342E-29 ) ) ;
#50046 = CARTESIAN_POINT ( 'NONE',  ( 100.7929862627584754, -41.95179922106267156, 114.6966617981629639 ) ) ;
#50047 = CARTESIAN_POINT ( 'NONE',  ( 98.51983665003312751, -30.72177789114069313, 201.8384824187679385 ) ) ;
#50048 = CARTESIAN_POINT ( 'NONE',  ( 142.8698897858160706, -0.9167816978817300289, 394.9756252759102040 ) ) ;
#50049 = VERTEX_POINT ( 'NONE', #62880 ) ;
#50050 = DIRECTION ( 'NONE',  ( 4.299999999999999979E-14, -1.000000000000000000, 0.000000000000000000 ) ) ;
#50051 = ORIENTED_EDGE ( 'NONE', *, *, #45794, .T. ) ;
#50052 = ORIENTED_EDGE ( 'NONE', *, *, #34101, .F. ) ;
#50053 = AXIS2_PLACEMENT_3D ( 'NONE', #60503, #87343, #66882 ) ;
#50054 = EDGE_CURVE ( 'NONE', #69712, #61365, #27917, .T. ) ;
#50055 = CONICAL_SURFACE ( 'NONE', #36981, 1.258749999999999369, 1.029744258676650093 ) ;
#50056 = CARTESIAN_POINT ( 'NONE',  ( 107.0664832912750057, -36.72944715993903486, 0.4256252759109709349 ) ) ;
#50057 = CIRCLE ( 'NONE', #57321, 6.349999999999999645 ) ;
#50058 = ORIENTED_EDGE ( 'NONE', *, *, #3123, .F. ) ;
#50059 = ORIENTED_EDGE ( 'NONE', *, *, #1906, .T. ) ;
#50060 = CARTESIAN_POINT ( 'NONE',  ( 115.0385986129619482, -42.90675649914010137, 169.3030387614307699 ) ) ;
#50061 = VECTOR ( 'NONE', #50044, 1000.000000000000000 ) ;
#50062 = CARTESIAN_POINT ( 'NONE',  ( 97.33783257808994449, -34.07109485886046230, 42.11472017254328648 ) ) ;
#50063 = CARTESIAN_POINT ( 'NONE',  ( 112.2084326156563066, -29.27471527533065299, 89.03051506617198640 ) ) ;
#50065 = CARTESIAN_POINT ( 'NONE',  ( 100.1628669375702714, -45.39175184048325917, 272.0289586092442278 ) ) ;
#50064 = CIRCLE ( 'NONE', #13840, 18.00000000000000355 ) ;
#50066 = FACE_OUTER_BOUND ( 'NONE', #5491, .T. ) ;
#50067 = DIRECTION ( 'NONE',  ( -0.4999999999999998890, 0.8660254037844387076, 0.000000000000000000 ) ) ;
#50068 = ORIENTED_EDGE ( 'NONE', *, *, #74813, .T. ) ;
#50069 = VECTOR ( 'NONE', #29022, 1000.000000000000000 ) ;
#50070 = EDGE_CURVE ( 'NONE', #52647, #1233, #14760, .T. ) ;
#50071 = ORIENTED_EDGE ( 'NONE', *, *, #87576, .T. ) ;
#50072 = DIRECTION ( 'NONE',  ( 1.000000000000000078E-15, -1.000000000000000083E-30, -1.000000000000000000 ) ) ;
#50073 = CARTESIAN_POINT ( 'NONE',  ( 156.5667039024484097, -48.82844715993568485, 175.7178068554150059 ) ) ;
#50074 = CARTESIAN_POINT ( 'NONE',  ( 70.87602654543734104, -139.0212896760968420, 247.5093344598249701 ) ) ;
#50075 = AXIS2_PLACEMENT_3D ( 'NONE', #27441, #71037, #83769 ) ;
#50076 = CARTESIAN_POINT ( 'NONE',  ( 113.4367438382844284, -44.15125393826594546, 108.1413395616259692 ) ) ;
#50077 = CARTESIAN_POINT ( 'NONE',  ( 104.9539341177782177, -25.01766106605714768, 125.2184824187689856 ) ) ;
#50078 = DIRECTION ( 'NONE',  ( 0.000000000000000000, 0.000000000000000000, 1.000000000000000000 ) ) ;
#50079 = VERTEX_POINT ( 'NONE', #22464 ) ;
#50080 = CARTESIAN_POINT ( 'NONE',  ( 109.2120108049357299, -48.38436871983039111, 277.7213395616254843 ) ) ;
#50081 = DIRECTION ( 'NONE',  ( 4.299999999999999979E-14, -1.000000000000000000, 4.400000000000000367E-29 ) ) ;
#50082 = CARTESIAN_POINT ( 'NONE',  ( 0.000000000000000000, 124.5870000000000033, 0.000000000000000000 ) ) ;
#50083 = VECTOR ( 'NONE', #83298, 1000.000000000000000 ) ;
#50085 = CARTESIAN_POINT ( 'NONE',  ( 68.71873216121885264, -139.2787739119035280, 246.0441243801330700 ) ) ;
#50084 = FACE_OUTER_BOUND ( 'NONE', #52829, .T. ) ;
#50086 = LINE ( 'NONE', #71012, #27824 ) ;
#50087 = DIRECTION ( 'NONE',  ( -1.000000000000000000, 1.011922027653136551E-15, 0.000000000000000000 ) ) ;
#50088 = CARTESIAN_POINT ( 'NONE',  ( 132.3477924061170370, -38.87777042261645732, 7.743969477062123019 ) ) ;
#50089 = CARTESIAN_POINT ( 'NONE',  ( -487.2989999999999782, 100.8062500000000057, 94.61194598552329182 ) ) ;
#50090 = DIRECTION ( 'NONE',  ( 0.000000000000000000, 0.000000000000000000, -1.000000000000000000 ) ) ;
#50091 = ADVANCED_FACE ( 'NONE', ( #29718, #57411 ), #9274, .T. ) ;
#50092 = LINE ( 'NONE', #84650, #70980 ) ;
#50094 = VERTEX_POINT ( 'NONE', #48790 ) ;
#50093 = CARTESIAN_POINT ( 'NONE',  ( 49.21437657594998427, -35.91149509761070391, -5.074374724088000832 ) ) ;
#50095 = DIRECTION ( 'NONE',  ( 0.000000000000000000, 0.000000000000000000, 1.000000000000000000 ) ) ;
#50096 = CARTESIAN_POINT ( 'NONE',  ( 104.3185787381473375, -25.99890841748068482, 245.2880062282919482 ) ) ;
#50097 = CARTESIAN_POINT ( 'NONE',  ( 109.8559662660393172, -26.68448463234438606, 170.8613395616249591 ) ) ;
#50098 = CARTESIAN_POINT ( 'NONE',  ( 116.3557873595856336, -41.55669258580370951, 284.4441967044824082 ) ) ;
#50100 = CARTESIAN_POINT ( 'NONE',  ( 82.78382032693660619, -36.30343833343673765, 6.798133076501194694 ) ) ;
#50099 = FACE_OUTER_BOUND ( 'NONE', #84093, .T. ) ;
#50101 = CARTESIAN_POINT ( 'NONE',  ( 97.86667236827629779, -40.64944809824318384, 137.6470064143673255 ) ) ;
#50102 = AXIS2_PLACEMENT_3D ( 'NONE', #46364, #17790, #3715 ) ;
#50103 = VECTOR ( 'NONE', #63288, 1000.000000000000000 ) ;
#50104 = ORIENTED_EDGE ( 'NONE', *, *, #67059, .T. ) ;
#50105 = CARTESIAN_POINT ( 'NONE',  ( -76.20505178924278766, 127.0000000000000000, -76.20505178924469192 ) ) ;
#50106 = ORIENTED_EDGE ( 'NONE', *, *, #17491, .T. ) ;
#50107 = CARTESIAN_POINT ( 'NONE',  ( 112.4896002948435410, -43.98220334580144453, 187.5219436376009696 ) ) ;
#50108 = EDGE_CURVE ( 'NONE', #29697, #42257, #656, .T. ) ;
#50110 = VERTEX_POINT ( 'NONE', #37423 ) ;
#50109 = CARTESIAN_POINT ( 'NONE',  ( 117.0599855631655544, -38.08685173747024066, 188.7190441128558120 ) ) ;
#50111 = CARTESIAN_POINT ( 'NONE',  ( 99.08946256649487339, -99.09543445804985140, -19.78219314458218392 ) ) ;
#50112 = CARTESIAN_POINT ( 'NONE',  ( 98.45302666770176359, -29.83944080489372652, 191.7775300378159784 ) ) ;
#50113 = CARTESIAN_POINT ( 'NONE',  ( 41.56648329127398966, -27.82844715994070484, 194.1756252759119832 ) ) ;
#50114 = ADVANCED_FACE ( 'NONE', ( #10164 ), #74171, .F. ) ;
#50115 = DIRECTION ( 'NONE',  ( -1.000000000000000078E-15, 1.000000000000000000, 0.000000000000000000 ) ) ;
#50116 = CARTESIAN_POINT ( 'NONE',  ( 180.2121375201600131, -29.73316016639650172, -5.074374724088000832 ) ) ;
#50117 = CARTESIAN_POINT ( 'NONE',  ( 145.9203257412752919, -138.8248129988771211, 246.0151717635989996 ) ) ;
#50118 = CARTESIAN_POINT ( 'NONE',  ( 110.8563607029707327, -45.98346426043695345, 97.88578756584530538 ) ) ;
#50119 = CARTESIAN_POINT ( 'NONE',  ( 102.6819511611810753, -27.33185899950643005, 135.4118157521019441 ) ) ;
#50120 = ORIENTED_EDGE ( 'NONE', *, *, #10848, .F. ) ;
#50121 = VERTEX_POINT ( 'NONE', #78780 ) ;
#50122 = VECTOR ( 'NONE', #33155, 1000.000000000000000 ) ;
#50123 = CARTESIAN_POINT ( 'NONE',  ( 105.1055546886446308, -45.37138199117224957, 68.83015473446796761 ) ) ;
#50124 = AXIS2_PLACEMENT_3D ( 'NONE', #22438, #50115, #42847 ) ;
#50125 = FACE_OUTER_BOUND ( 'NONE', #22172, .T. ) ;
#50126 = VECTOR ( 'NONE', #19200, 999.9999999999998863 ) ;
#50128 = DIRECTION ( 'NONE',  ( -1.000000000000000000, 0.000000000000000000, 0.000000000000000000 ) ) ;
#50127 = CARTESIAN_POINT ( 'NONE',  ( 106.9806506443342755, -46.50983917909364607, 183.5699109901959787 ) ) ;
#50129 = AXIS2_PLACEMENT_3D ( 'NONE', #69963, #34976, #917 ) ;
#50130 = LINE ( 'NONE', #55584, #43623 ) ;
#50131 = CARTESIAN_POINT ( 'NONE',  ( -148.0533267522759786, 20.32000000000000028, -160.2664750769289697 ) ) ;
#50132 = CARTESIAN_POINT ( 'NONE',  ( 107.0664832912739399, -36.72944715994095333, 302.6356252759109680 ) ) ;
#50133 = DIRECTION ( 'NONE',  ( -1.000000000000000000, 0.000000000000000000, 0.000000000000000000 ) ) ;
#50134 = CARTESIAN_POINT ( 'NONE',  ( 67.06980256514445671, -67.88054560554753891, 245.6023804759829829 ) ) ;
#50135 = CARTESIAN_POINT ( 'NONE',  ( 108.0321269276242049, -25.74166508409281917, 109.9946728949589811 ) ) ;
#50136 = ORIENTED_EDGE ( 'NONE', *, *, #17389, .T. ) ;
#50137 = EDGE_LOOP ( 'NONE', ( #19652, #32081, #57439, #46595, #74840, #38345 ) ) ;
#50138 = ORIENTED_EDGE ( 'NONE', *, *, #18826, .T. ) ;
#50139 = AXIS2_PLACEMENT_3D ( 'NONE', #16076, #76950, #42848 ) ;
#50140 = CARTESIAN_POINT ( 'NONE',  ( 6.359898342742077659, 71.54935466043629333, 130.4015153071888733 ) ) ;
#50141 = DIRECTION ( 'NONE',  ( 0.2130003897598659046, -0.000000000000000000, 0.9770521142508956647 ) ) ;
#50142 = CARTESIAN_POINT ( 'NONE',  ( 117.0608945232069971, -38.08045312423180917, 79.71895860897220132 ) ) ;
#50143 = DIRECTION ( 'NONE',  ( -1.000000000000000000, -4.299999999999999979E-14, -1.000000000000000078E-15 ) ) ;
#50145 = CARTESIAN_POINT ( 'NONE',  ( 111.0898924481313941, -43.83169361959101451, 210.8052332267339750 ) ) ;
#50144 = CIRCLE ( 'NONE', #34191, 0.5000000000000004441 ) ;
#50146 = CARTESIAN_POINT ( 'NONE',  ( 34.67381068362099228, -26.00627455219321860, -5.074374724088000832 ) ) ;
#50147 = AXIS2_PLACEMENT_3D ( 'NONE', #26430, #86873, #80066 ) ;
#50148 = ADVANCED_FACE ( 'NONE', ( #79672 ), #66002, .T. ) ;
#50149 = CARTESIAN_POINT ( 'NONE',  ( 102.0817216996469483, -27.57306688727539168, 145.4727681330539610 ) ) ;
#50150 = DIRECTION ( 'NONE',  ( 0.000000000000000000, 0.000000000000000000, -1.000000000000000000 ) ) ;
#50151 = ORIENTED_EDGE ( 'NONE', *, *, #50001, .F. ) ;
#50153 = ORIENTED_EDGE ( 'NONE', *, *, #14524, .F. ) ;
#50152 = EDGE_LOOP ( 'NONE', ( #53147, #10405 ) ) ;
#50154 = FACE_OUTER_BOUND ( 'NONE', #11655, .T. ) ;
#50155 = ORIENTED_EDGE ( 'NONE', *, *, #44441, .T. ) ;
#50156 = ORIENTED_EDGE ( 'NONE', *, *, #44259, .F. ) ;
#50157 = CARTESIAN_POINT ( 'NONE',  ( 78.64532134555092568, -21.08531275930071658, 7.905164235254865446 ) ) ;
#50158 = LINE ( 'NONE', #86494, #4906 ) ;
#50159 = CARTESIAN_POINT ( 'NONE',  ( 98.34725308318749626, -40.22966859802066608, 248.0739642582779538 ) ) ;
#50160 = CARTESIAN_POINT ( 'NONE',  ( 90.06648329127391150, -36.72944715993925513, -5.074374724089047106 ) ) ;
#50161 = EDGE_LOOP ( 'NONE', ( #55299, #14057, #33962, #64365 ) ) ;
#50162 = CARTESIAN_POINT ( 'NONE',  ( 115.6637425838761430, -40.30355366565792252, 9.635625275910941312 ) ) ;
#50163 = CARTESIAN_POINT ( 'NONE',  ( 177.0664832912740110, 12.92155284005802685, 349.2756252759111248 ) ) ;
#50164 = ORIENTED_EDGE ( 'NONE', *, *, #62518, .F. ) ;
#50165 = EDGE_LOOP ( 'NONE', ( #68537, #19665, #89739, #77650 ) ) ;
#50166 = EDGE_CURVE ( 'NONE', #81111, #2816, #45539, .T. ) ;
#50167 = CARTESIAN_POINT ( 'NONE',  ( 113.1931473032385185, -44.64809289480323429, 113.1005158354814597 ) ) ;
#50168 = ORIENTED_EDGE ( 'NONE', *, *, #52165, .F. ) ;
#50169 = ORIENTED_EDGE ( 'NONE', *, *, #14336, .T. ) ;
#50170 = CARTESIAN_POINT ( 'NONE',  ( 107.8084489643801334, -27.48037055177216104, 262.8309475124484038 ) ) ;
#50171 = EDGE_CURVE ( 'NONE', #26178, #667, #52785, .T. ) ;
#50172 = CARTESIAN_POINT ( 'NONE',  ( 114.3594209402202182, -29.19941241435835266, 174.4641967044819637 ) ) ;
#50173 = CARTESIAN_POINT ( 'NONE',  ( 105.3199149336540046, -48.42511963160334432, 147.4584824187679715 ) ) ;
#50174 = DIRECTION ( 'NONE',  ( 0.000000000000000000, 0.000000000000000000, -1.000000000000000000 ) ) ;
#50175 = DIRECTION ( 'NONE',  ( 1.000000000000000078E-15, -1.000000000000000083E-30, -1.000000000000000000 ) ) ;
#50176 = CARTESIAN_POINT ( 'NONE',  ( 97.91927484100293100, -41.73055353899491138, 217.7241967044829494 ) ) ;
#50177 = DIRECTION ( 'NONE',  ( -0.9659258262890686453, 0.000000000000000000, 0.2588190451025194072 ) ) ;
#50178 = CARTESIAN_POINT ( 'NONE',  ( 63.03715912545818156, -46.82818131006018092, 313.9678068554150059 ) ) ;
#50179 = ORIENTED_EDGE ( 'NONE', *, *, #44966, .F. ) ;
#50180 = CARTESIAN_POINT ( 'NONE',  ( 0.000000000000000000, 101.6000000000000227, 0.000000000000000000 ) ) ;
#50182 = EDGE_LOOP ( 'NONE', ( #71883, #2997, #28145, #81846 ) ) ;
#50181 = EDGE_CURVE ( 'NONE', #60890, #20236, #34306, .T. ) ;
#50183 = ADVANCED_FACE ( 'NONE', ( #79224 ), #72835, .F. ) ;
#50184 = VERTEX_POINT ( 'NONE', #44666 ) ;
#50185 = CIRCLE ( 'NONE', #47319, 4.875000000000017764 ) ;
#50186 = EDGE_CURVE ( 'NONE', #21752, #10255, #13960, .T. ) ;
#50188 = CARTESIAN_POINT ( 'NONE',  ( 108.6818361061225602, -26.38549717321916788, 189.9527681330539792 ) ) ;
#50187 = AXIS2_PLACEMENT_3D ( 'NONE', #53106, #47658, #60846 ) ;
#50189 = VERTEX_POINT ( 'NONE', #86920 ) ;
#50190 = VECTOR ( 'NONE', #66781, 1000.000000000000000 ) ;
#50191 = CARTESIAN_POINT ( 'NONE',  ( 107.3339538991774447, -26.30757161206916095, 120.0556252759109555 ) ) ;
#50192 = LINE ( 'NONE', #42035, #19555 ) ;
#50193 = AXIS2_PLACEMENT_3D ( 'NONE', #24676, #87357, #72392 ) ;
#50194 = EDGE_CURVE ( 'NONE', #13929, #5997, #11047, .T. ) ;
#50195 = CARTESIAN_POINT ( 'NONE',  ( 135.5773992616565238, -34.43204134599594113, 7.859568798196992390 ) ) ;
#50196 = CARTESIAN_POINT ( 'NONE',  ( 165.9667039024459996, -26.71338133339301635, -5.074374724088000832 ) ) ;
#50199 = CARTESIAN_POINT ( 'NONE',  ( 100.2624651760415873, -28.85963121439202794, 256.6441967044821695 ) ) ;
#50198 = CARTESIAN_POINT ( 'NONE',  ( 111.7879433275918473, -45.58683771644975025, 57.96604673916865380 ) ) ;
#50197 = DIRECTION ( 'NONE',  ( -2.999999999999999839E-15, 1.000000000000000000, -2.999999999999999900E-30 ) ) ;
#50200 = CARTESIAN_POINT ( 'NONE',  ( -1.415542646969860267E-16, 70.24203434096102683, 38.10000000000000142 ) ) ;
#50201 = DIRECTION ( 'NONE',  ( 1.000000000000000078E-15, -1.000000000000000000, 0.000000000000000000 ) ) ;
#50202 = CARTESIAN_POINT ( 'NONE',  ( 140.0667039024470455, -118.2784471599408960, 45.21780685541799727 ) ) ;
#50203 = DIRECTION ( 'NONE',  ( -1.000000000000000000, -4.299999999999999979E-14, -1.000000000000000078E-15 ) ) ;
#50204 = CARTESIAN_POINT ( 'NONE',  ( -50.35902679310718355, 64.60000000000000853, 27.95514712793348977 ) ) ;
#50205 = EDGE_CURVE ( 'NONE', #76783, #43325, #18308, .T. ) ;
#50206 = DIRECTION ( 'NONE',  ( -1.000000000000000000, 0.000000000000000000, 0.000000000000000000 ) ) ;
#50208 = ORIENTED_EDGE ( 'NONE', *, *, #36853, .T. ) ;
#50207 = CARTESIAN_POINT ( 'NONE',  ( 112.8675307907708287, -28.58609239232746546, 195.5838076129389833 ) ) ;
#50209 = CARTESIAN_POINT ( 'NONE',  ( 219.9639999999999986, 40.03750000000000142, -7.937500000000000000 ) ) ;
#50210 = CARTESIAN_POINT ( 'NONE',  ( 103.4607332334527001, -46.53479866174185986, 142.2956252759109645 ) ) ;
#50211 = CARTESIAN_POINT ( 'NONE',  ( 107.2322063299336605, -25.67745564896214816, 76.07657765686298035 ) ) ;
#50212 = CARTESIAN_POINT ( 'NONE',  ( 95.35923950155199691, -38.86288465644625489, 197.4699109901969791 ) ) ;
#50213 = CARTESIAN_POINT ( 'NONE',  ( 194.0371591254572934, -24.42818131005417825, 300.4678068554149490 ) ) ;
#50214 = FACE_OUTER_BOUND ( 'NONE', #6321, .T. ) ;
#50215 = CIRCLE ( 'NONE', #76287, 7.143750000000001599 ) ;
#50217 = LINE ( 'NONE', #77952, #15337 ) ;
#50216 = CARTESIAN_POINT ( 'NONE',  ( -3.174999999999664979, 104.3431970271541616, -31.75000000000000000 ) ) ;
#50218 = CARTESIAN_POINT ( 'NONE',  ( 97.07207206176971681, -35.37844117946191602, 71.21895860768269415 ) ) ;
#50219 = DIRECTION ( 'NONE',  ( -0.7071067811865420216, 0.000000000000000000, 0.7071067811865531239 ) ) ;
#50220 = ORIENTED_EDGE ( 'NONE', *, *, #49423, .T. ) ;
#50221 = DIRECTION ( 'NONE',  ( 3.100000000000000258E-29, -3.100000000000000044E-14, -1.000000000000000000 ) ) ;
#50222 =( BOUNDED_CURVE ( )  B_SPLINE_CURVE ( 3, ( #26610, #5736, #21488, #77340 ),
 .UNSPECIFIED., .F., .T. ) 
 B_SPLINE_CURVE_WITH_KNOTS ( ( 4, 4 ),
 ( 4.646092198350340041, 4.647722573419572178 ),
 .UNSPECIFIED. ) 
 CURVE ( )  GEOMETRIC_REPRESENTATION_ITEM ( )  RATIONAL_B_SPLINE_CURVE ( ( 1.000000000000000000, 0.9999997784897733943, 0.9999997784897733943, 1.000000000000000000 ) ) 
 REPRESENTATION_ITEM ( '' )  );
#50223 = EDGE_LOOP ( 'NONE', ( #39031, #80194, #24817, #12793 ) ) ;
#50224 = ORIENTED_EDGE ( 'NONE', *, *, #25267, .T. ) ;
#50225 = EDGE_CURVE ( 'NONE', #39116, #42164, #44211, .T. ) ;
#50227 = VERTEX_POINT ( 'NONE', #68266 ) ;
#50226 = CARTESIAN_POINT ( 'NONE',  ( 37.06648329127298780, 12.92155284005730387, 361.9756252759109998 ) ) ;
#50228 = CARTESIAN_POINT ( 'NONE',  ( 117.9019101119219357, -41.46671778014663801, 54.49848241876792088 ) ) ;
#50229 = FACE_OUTER_BOUND ( 'NONE', #21234, .T. ) ;
#50230 = EDGE_CURVE ( 'NONE', #54776, #2723, #55039, .T. ) ;
#50231 = EDGE_CURVE ( 'NONE', #23923, #77722, #70637, .T. ) ;
#50232 = DIRECTION ( 'NONE',  ( 4.299999999999999979E-14, -1.000000000000000000, 4.400000000000000367E-29 ) ) ;
#50233 = CARTESIAN_POINT ( 'NONE',  ( 96.00064313654479520, -35.86649870909684523, 187.2765776568629406 ) ) ;
#50234 = EDGE_CURVE ( 'NONE', #32410, #54956, #25570, .T. ) ;
#50235 = CARTESIAN_POINT ( 'NONE',  ( 106.3060546692423145, -45.75354925581387278, 261.9200388756959796 ) ) ;
#50236 = ORIENTED_EDGE ( 'NONE', *, *, #37803, .F. ) ;
#50237 = ORIENTED_EDGE ( 'NONE', *, *, #68135, .F. ) ;
#50238 = ORIENTED_EDGE ( 'NONE', *, *, #24921, .F. ) ;
#50239 = DIRECTION ( 'NONE',  ( 0.000000000000000000, 0.000000000000000000, -1.000000000000000000 ) ) ;
#50240 = LINE ( 'NONE', #57510, #21692 ) ;
#50241 = DIRECTION ( 'NONE',  ( 1.387778780781444492E-15, 0.000000000000000000, -1.000000000000000000 ) ) ;
#50242 = DIRECTION ( 'NONE',  ( 0.000000000000000000, 1.000000000000000000, 0.000000000000000000 ) ) ;
#50243 = CARTESIAN_POINT ( 'NONE',  ( 98.82361644294680048, 90.93081950567960803, 85.31607583734509603 ) ) ;
#50244 = DIRECTION ( 'NONE',  ( 0.000000000000000000, 0.000000000000000000, 1.000000000000000000 ) ) ;
#50245 = CARTESIAN_POINT ( 'NONE',  ( -24.79284581386642827, 127.0000000000000000, 101.0189074266571794 ) ) ;
#50246 = DIRECTION ( 'NONE',  ( -0.7071067811865794361, 0.7071067811865157093, -7.071067811865492096E-16 ) ) ;
#50247 = CARTESIAN_POINT ( 'NONE',  ( 115.5933672690474765, -28.53551910654237389, 39.43562527591099354 ) ) ;
#50248 = ORIENTED_EDGE ( 'NONE', *, *, #54100, .F. ) ;
#50249 = DIRECTION ( 'NONE',  ( -1.000000000000000000, 0.000000000000000000, 0.000000000000000000 ) ) ;
#50250 = VECTOR ( 'NONE', #791, 1000.000000000000114 ) ;
#50251 = CARTESIAN_POINT ( 'NONE',  ( -55.95243198108136085, 55.97500000000000142, 70.69974874213239957 ) ) ;
#50252 = CARTESIAN_POINT ( 'NONE',  ( 107.2759047676296120, -28.56943069780466971, 117.8738046553059462 ) ) ;
#50253 = AXIS2_PLACEMENT_3D ( 'NONE', #57289, #50022, #2351 ) ;
#50254 = VECTOR ( 'NONE', #29042, 1000.000000000000000 ) ;
#50255 = CIRCLE ( 'NONE', #35738, 2.999999999999919176 ) ;
#50256 = DIRECTION ( 'NONE',  ( 1.000000000000000078E-15, 0.000000000000000000, -1.000000000000000000 ) ) ;
#50257 = LINE ( 'NONE', #86145, #79337 ) ;
#50258 = ORIENTED_EDGE ( 'NONE', *, *, #86822, .F. ) ;
#50259 = ORIENTED_EDGE ( 'NONE', *, *, #73789, .T. ) ;
#50260 = CYLINDRICAL_SURFACE ( 'NONE', #85975, 30.99999999999998579 ) ;
#50261 = ORIENTED_EDGE ( 'NONE', *, *, #18189, .T. ) ;
#50262 = VERTEX_POINT ( 'NONE', #67804 ) ;
#50263 = CARTESIAN_POINT ( 'NONE',  ( 111.0851542815211985, -27.49251106464650007, 131.1815833058969645 ) ) ;
#50264 = DIRECTION ( 'NONE',  ( 0.000000000000000000, 1.000000000000000000, 0.000000000000000000 ) ) ;
#50265 = AXIS2_PLACEMENT_3D ( 'NONE', #572, #135, #58231 ) ;
#50266 = CARTESIAN_POINT ( 'NONE',  ( 104.1016336957795261, -46.74677842777965253, 103.3470538473389411 ) ) ;
#50267 = CARTESIAN_POINT ( 'NONE',  ( 101.9933438188864159, -45.44590076357884101, 17.15650773109305760 ) ) ;
#50268 = ORIENTED_EDGE ( 'NONE', *, *, #73155, .F. ) ;
#50269 = AXIS2_PLACEMENT_3D ( 'NONE', #51629, #71658, #24396 ) ;
#50270 = ORIENTED_EDGE ( 'NONE', *, *, #86312, .T. ) ;
#50271 = VERTEX_POINT ( 'NONE', #48233 ) ;
#50272 = EDGE_CURVE ( 'NONE', #86794, #61024, #5592, .T. ) ;
#50273 = EDGE_CURVE ( 'NONE', #88226, #63113, #66908, .T. ) ;
#50274 = CARTESIAN_POINT ( 'NONE',  ( 100.9301527464941444, -28.27416411254235840, 75.57562527591093726 ) ) ;
#50275 = EDGE_LOOP ( 'NONE', ( #42990, #22985, #36227, #15132 ) ) ;
#50276 = CARTESIAN_POINT ( 'NONE',  ( 114.8131502045276449, -44.70447909941025699, 268.1899109901970633 ) ) ;
#50277 = CARTESIAN_POINT ( 'NONE',  ( 115.0562973506820157, -29.05819712879207017, 185.4232443235299570 ) ) ;
#50278 = FACE_BOUND ( 'NONE', #59549, .T. ) ;
#50279 = CARTESIAN_POINT ( 'NONE',  ( -110.0436475921183899, 47.06665061967962060, 70.25164585318982802 ) ) ;
#50280 = CARTESIAN_POINT ( 'NONE',  ( 104.9628592394672069, -25.06714115267218546, 121.2184824187679766 ) ) ;
#50281 = LINE ( 'NONE', #2159, #30622 ) ;
#50282 = VERTEX_POINT ( 'NONE', #89605 ) ;
#50283 = FACE_OUTER_BOUND ( 'NONE', #22678, .T. ) ;
#50284 = EDGE_CURVE ( 'NONE', #2396, #76220, #15528, .T. ) ;
#50285 = ADVANCED_FACE ( 'NONE', ( #87804 ), #54142, .T. ) ;
#50286 = ORIENTED_EDGE ( 'NONE', *, *, #26504, .T. ) ;
#50287 = CARTESIAN_POINT ( 'NONE',  ( 109.6435279985285405, -46.47996157675320461, 133.7827314339946554 ) ) ;
#50288 = ORIENTED_EDGE ( 'NONE', *, *, #61025, .T. ) ;
#50289 = AXIS2_PLACEMENT_3D ( 'NONE', #73057, #58095, #16324 ) ;
#50290 = EDGE_LOOP ( 'NONE', ( #10844, #67224, #62119, #89235 ) ) ;
#50291 = VECTOR ( 'NONE', #70096, 1000.000000000000114 ) ;
#50292 = EDGE_CURVE ( 'NONE', #14878, #70474, #24900, .T. ) ;
#50293 = CARTESIAN_POINT ( 'NONE',  ( -59.93649209371543662, 82.54999999999999716, 77.89700433585352357 ) ) ;
#50294 = CARTESIAN_POINT ( 'NONE',  ( 11.93201035062058679, 86.61901526127904560, 117.9540879163301526 ) ) ;
#50295 = CARTESIAN_POINT ( 'NONE',  ( 117.3847603239957635, -38.21947720531817083, 28.71276813305395592 ) ) ;
#50296 = CARTESIAN_POINT ( 'NONE',  ( 2.759391577539827445, 70.18407359651233435, 38.02468864519824621 ) ) ;
#50297 = EDGE_CURVE ( 'NONE', #4100, #63429, #43217, .T. ) ;
#50298 = LINE ( 'NONE', #56668, #2837 ) ;
#50299 = CARTESIAN_POINT ( 'NONE',  ( 57.56670390244829605, -48.82844715994039575, 290.7178068554150627 ) ) ;
#50300 = CARTESIAN_POINT ( 'NONE',  ( 97.89279369561084820, -33.33727167892450183, 66.04419670448297097 ) ) ;
#50302 = CARTESIAN_POINT ( 'NONE',  ( 105.7232414704440941, -24.98023492732646744, 156.1670538473399574 ) ) ;
#50301 = CARTESIAN_POINT ( 'NONE',  ( 97.60806933018331222, -39.98294871649164861, 111.5901086304039751 ) ) ;
#50303 = CARTESIAN_POINT ( 'NONE',  ( 140.0667039024470455, -118.2784471599408960, 45.21780685541799727 ) ) ;
#50304 = DIRECTION ( 'NONE',  ( -2.170915417798913418E-16, 0.000000000000000000, -1.000000000000000000 ) ) ;
#50305 = ORIENTED_EDGE ( 'NONE', *, *, #19953, .T. ) ;
#50306 = CARTESIAN_POINT ( 'NONE',  ( 154.5667039024469886, -67.87844715994090450, 85.21780685541799016 ) ) ;
#50307 = CARTESIAN_POINT ( 'NONE',  ( 156.5667039024485803, -48.82844715993568485, 137.2178068554149775 ) ) ;
#50308 = CARTESIAN_POINT ( 'NONE',  ( -77.39114642429849766, 120.6499999999999915, -71.77848634863219957 ) ) ;
#50309 = ORIENTED_EDGE ( 'NONE', *, *, #67405, .F. ) ;
#50310 = EDGE_CURVE ( 'NONE', #78458, #83951, #3277, .T. ) ;
#50311 = CARTESIAN_POINT ( 'NONE',  ( 63.03715912545741418, -46.82818131006016671, 117.4678068554150485 ) ) ;
#50313 = VERTEX_POINT ( 'NONE', #55487 ) ;
#50312 = CARTESIAN_POINT ( 'NONE',  ( 98.51514891278741004, -45.00612994150532842, 191.9384824187679612 ) ) ;
#50314 = DIRECTION ( 'NONE',  ( 0.000000000000000000, 0.000000000000000000, -1.000000000000000000 ) ) ;
#50315 = CARTESIAN_POINT ( 'NONE',  ( 109.3416101119966442, -26.53331765884353644, 220.9013395616249795 ) ) ;
#50316 = CARTESIAN_POINT ( 'NONE',  ( 97.22547384517952196, -31.59602418489684084, 86.93181575210095957 ) ) ;
#50317 = VECTOR ( 'NONE', #7624, 1000.000000000000114 ) ;
#50318 = CARTESIAN_POINT ( 'NONE',  ( 85.30119219530003249, 74.16222525595215131, 98.83784439188701754 ) ) ;
#50319 = LINE ( 'NONE', #72127, #25663 ) ;
#50320 = EDGE_CURVE ( 'NONE', #28372, #59253, #86589, .T. ) ;
#50321 = DIRECTION ( 'NONE',  ( -1.000000000000000078E-15, 0.000000000000000000, 1.000000000000000000 ) ) ;
#50322 = ORIENTED_EDGE ( 'NONE', *, *, #8102, .T. ) ;
#50323 = CIRCLE ( 'NONE', #64798, 88.90000000000000568 ) ;
#50324 = AXIS2_PLACEMENT_3D ( 'NONE', #80903, #54031, #47232 ) ;
#50325 = CIRCLE ( 'NONE', #44484, 27.49999999999999645 ) ;
#50326 = ORIENTED_EDGE ( 'NONE', *, *, #76567, .T. ) ;
#50327 = ORIENTED_EDGE ( 'NONE', *, *, #55049, .T. ) ;
#50328 = ORIENTED_EDGE ( 'NONE', *, *, #8287, .F. ) ;
#50329 = CARTESIAN_POINT ( 'NONE',  ( 183.6524903400786286, -49.32844715993451956, 129.9678068554150059 ) ) ;
#50330 = CARTESIAN_POINT ( 'NONE',  ( 107.2492351517315683, -24.88034519751278850, 226.0641967044829812 ) ) ;
#50331 = CARTESIAN_POINT ( 'NONE',  ( 151.5667039024483245, -48.82844715993591223, 300.4678068554149490 ) ) ;
#50332 = CARTESIAN_POINT ( 'NONE',  ( 136.6805397534846236, -17.85322261660804699, 2.908039740961557929 ) ) ;
#50333 = EDGE_CURVE ( 'NONE', #32579, #7668, #58993, .T. ) ;
#50334 = AXIS2_PLACEMENT_3D ( 'NONE', #15642, #71063, #8834 ) ;
#50337 = EDGE_CURVE ( 'NONE', #56758, #20355, #69199, .T. ) ;
#50336 = CARTESIAN_POINT ( 'NONE',  ( 191.6375511031384633, -78.44951497180814215, 361.9756252759109998 ) ) ;
#50335 = DIRECTION ( 'NONE',  ( -1.000000000000000000, -3.999999999999999995E-14, -1.000000000000000078E-15 ) ) ;
#50338 = CARTESIAN_POINT ( 'NONE',  ( 0.000000000000000000, 101.5999999999999943, 0.000000000000000000 ) ) ;
#50339 = CONICAL_SURFACE ( 'NONE', #16962, 39.10000000000005116, 0.7853981633974587151 ) ;
#50340 = CARTESIAN_POINT ( 'NONE',  ( 96.66386919200992622, -42.45828961175909200, 26.72705384733997747 ) ) ;
#50341 = ORIENTED_EDGE ( 'NONE', *, *, #9178, .F. ) ;
#50342 = ORIENTED_EDGE ( 'NONE', *, *, #85503, .F. ) ;
#50343 = ORIENTED_EDGE ( 'NONE', *, *, #42587, .T. ) ;
#50344 = VECTOR ( 'NONE', #35966, 1000.000000000000000 ) ;
#50345 = DIRECTION ( 'NONE',  ( -1.000000000000000078E-15, 1.000000000000000083E-30, 1.000000000000000000 ) ) ;
#50346 = DIRECTION ( 'NONE',  ( 0.000000000000000000, -1.000000000000000000, 0.000000000000000000 ) ) ;
#50347 = CARTESIAN_POINT ( 'NONE',  ( 115.1619974903459251, -42.21817061296636808, 269.3527681330531891 ) ) ;
#50348 = CARTESIAN_POINT ( 'NONE',  ( 107.0664832912739968, -36.72944715994100306, 287.6356252759109680 ) ) ;
#50349 = CARTESIAN_POINT ( 'NONE',  ( 105.0928733274061813, -25.78792777683075599, 121.2184824187669818 ) ) ;
#50350 = LINE ( 'NONE', #84464, #70698 ) ;
#50351 = ORIENTED_EDGE ( 'NONE', *, *, #37362, .F. ) ;
#50352 = CARTESIAN_POINT ( 'NONE',  ( 63.03715912545643363, -24.42818131006026761, 129.9678068554150911 ) ) ;
#50353 = CARTESIAN_POINT ( 'NONE',  ( 77.45963244950118565, -35.85248396559181572, 2.902015641458088879 ) ) ;
#50354 = ORIENTED_EDGE ( 'NONE', *, *, #66094, .T. ) ;
#50355 = CARTESIAN_POINT ( 'NONE',  ( -76.80574412431003850, 90.93089219781633403, 90.31319802837631983 ) ) ;
#50356 = CARTESIAN_POINT ( 'NONE',  ( 102.6173380888347282, -29.88584920324980487, 23.35380465530695204 ) ) ;
#50357 = VECTOR ( 'NONE', #70680, 1000.000000000000000 ) ;
#50358 = EDGE_CURVE ( 'NONE', #22506, #25248, #56848, .T. ) ;
#50359 = DIRECTION ( 'NONE',  ( 1.000000000000000000, 1.261617073437676668E-15, 9.462128050782575008E-16 ) ) ;
#50360 = CARTESIAN_POINT ( 'NONE',  ( 143.0664832912740110, -18.82844715994099971, 17.92562527591199739 ) ) ;
#50361 = DIRECTION ( 'NONE',  ( -0.000000000000000000, -0.000000000000000000, -1.000000000000000000 ) ) ;
#50362 = ORIENTED_EDGE ( 'NONE', *, *, #17250, .F. ) ;
#50363 = DIRECTION ( 'NONE',  ( 0.000000000000000000, -1.000000000000000000, 0.000000000000000000 ) ) ;
#50364 = LINE ( 'NONE', #85821, #80369 ) ;
#50365 = ORIENTED_EDGE ( 'NONE', *, *, #83685, .F. ) ;
#50366 = CARTESIAN_POINT ( 'NONE',  ( 114.5675797908445475, -44.02050044317889643, 98.21276813305395592 ) ) ;
#50367 = ORIENTED_EDGE ( 'NONE', *, *, #34180, .F. ) ;
#50368 = CARTESIAN_POINT ( 'NONE',  ( 115.9627085491522536, -40.61889491704908295, 57.92099125664801562 ) ) ;
#50369 = DIRECTION ( 'NONE',  ( 0.000000000000000000, 0.000000000000000000, -1.000000000000000000 ) ) ;
#50370 = CARTESIAN_POINT ( 'NONE',  ( 98.25516505653058630, -40.97492784622586015, 171.6841967044829573 ) ) ;
#50371 = LINE ( 'NONE', #86703, #23060 ) ;
#50372 = LINE ( 'NONE', #52143, #51657 ) ;
#50373 = DIRECTION ( 'NONE',  ( 0.000000000000000000, 0.000000000000000000, -1.000000000000000000 ) ) ;
#50374 = VECTOR ( 'NONE', #39777, 1000.000000000000000 ) ;
#50375 = DIRECTION ( 'NONE',  ( 0.000000000000000000, 0.000000000000000000, -1.000000000000000000 ) ) ;
#50376 = EDGE_CURVE ( 'NONE', #56973, #65405, #7817, .T. ) ;
#50377 = CARTESIAN_POINT ( 'NONE',  ( 117.4730440113279855, -35.59081861377887179, 274.9127681330539872 ) ) ;
#50378 = ORIENTED_EDGE ( 'NONE', *, *, #75148, .F. ) ;
#50379 = CARTESIAN_POINT ( 'NONE',  ( -487.2989999999999782, 14.28750000000026077, 6.349999999999710099 ) ) ;
#50380 = ORIENTED_EDGE ( 'NONE', *, *, #3731, .F. ) ;
#50381 = CARTESIAN_POINT ( 'NONE',  ( 102.0609898346451274, -27.53498505803861107, 141.4727681330539895 ) ) ;
#50382 = VECTOR ( 'NONE', #50831, 1000.000000000000000 ) ;
#50383 = CARTESIAN_POINT ( 'NONE',  ( 173.9900000000000091, 68.61249999999999716, -35.28456447661459805 ) ) ;
#50384 = VECTOR ( 'NONE', #54709, 1000.000000000000000 ) ;
#50385 = ORIENTED_EDGE ( 'NONE', *, *, #79357, .T. ) ;
#50387 = ADVANCED_FACE ( 'NONE', ( #69152 ), #63682, .T. ) ;
#50386 = ORIENTED_EDGE ( 'NONE', *, *, #1095, .T. ) ;
#50389 = VERTEX_POINT ( 'NONE', #48679 ) ;
#50388 = EDGE_CURVE ( 'NONE', #22617, #39335, #62860, .T. ) ;
#50390 = DIRECTION ( 'NONE',  ( 0.000000000000000000, 1.000000000000000000, 0.000000000000000000 ) ) ;
#50391 = EDGE_CURVE ( 'NONE', #31265, #30966, #76411, .T. ) ;
#50392 = CYLINDRICAL_SURFACE ( 'NONE', #66589, 2.117000000000007987 ) ;
#50393 = CARTESIAN_POINT ( 'NONE',  ( 110.0667047667142953, -67.87844715994094713, 173.2178068554179902 ) ) ;
#50394 = DIRECTION ( 'NONE',  ( -0.4214249218767882055, -0.9068632946707806397, -4.214249218767890910E-16 ) ) ;
#50395 = CARTESIAN_POINT ( 'NONE',  ( 213.7409999999999854, 52.73749999999999716, -37.80245750428454699 ) ) ;
#50396 = CARTESIAN_POINT ( 'NONE',  ( 96.71473009235836571, -37.96382682441392831, 37.42133956162496844 ) ) ;
#50397 = CARTESIAN_POINT ( 'NONE',  ( 188.5667039024479834, -62.87844715994099687, 137.2178068554150059 ) ) ;
#50398 = ORIENTED_EDGE ( 'NONE', *, *, #77998, .F. ) ;
#50399 = CIRCLE ( 'NONE', #79416, 0.4999999999999933387 ) ;
#50400 = CARTESIAN_POINT ( 'NONE',  ( 12.70000000000000107, 82.54999999999999716, 117.8738102209307641 ) ) ;
#50401 = ADVANCED_FACE ( 'NONE', ( #69604 ), #24137, .T. ) ;
#50402 = CIRCLE ( 'NONE', #12692, 1.523999999999053889 ) ;
#50403 = DIRECTION ( 'NONE',  ( 0.000000000000000000, -1.000000000000000000, 0.000000000000000000 ) ) ;
#50404 = ORIENTED_EDGE ( 'NONE', *, *, #74595, .F. ) ;
#50405 = ORIENTED_EDGE ( 'NONE', *, *, #17305, .F. ) ;
#50407 = EDGE_CURVE ( 'NONE', #49254, #43486, #51811, .T. ) ;
#50406 = CIRCLE ( 'NONE', #24359, 3.968750000000020872 ) ;
#50408 = CARTESIAN_POINT ( 'NONE',  ( 82.62351725430393401, -19.74149216370279802, 2.839569540204898601 ) ) ;
#50409 = CARTESIAN_POINT ( 'NONE',  ( 173.9900000000000091, 0.000000000000000000, 131.6533725204182019 ) ) ;
#50410 = CARTESIAN_POINT ( 'NONE',  ( 103.3797721312301547, -105.8297479413482876, -19.78219314458196010 ) ) ;
#50411 = PLANE ( 'NONE',  #27461 ) ;
#50412 = CARTESIAN_POINT ( 'NONE',  ( 107.0664832912739968, -36.72944715994100306, 287.6356252759109680 ) ) ;
#50413 = EDGE_CURVE ( 'NONE', #19054, #15026, #87806, .T. ) ;
#50414 = CARTESIAN_POINT ( 'NONE',  ( 101.9513324583280962, -44.20259256747556975, 241.5333722090289825 ) ) ;
#50416 = CARTESIAN_POINT ( 'NONE',  ( 96.73636544059199593, -37.96124694896865748, 37.42133956162496844 ) ) ;
#50415 = DIRECTION ( 'NONE',  ( 0.000000000000000000, 0.000000000000000000, 1.000000000000000000 ) ) ;
#50417 = CARTESIAN_POINT ( 'NONE',  ( 126.1740464204627301, 65.29148310750557016, 33.54086098101917202 ) ) ;
#50418 = CARTESIAN_POINT ( 'NONE',  ( 98.11178232766683038, -43.28888419983005775, 106.8175300378159704 ) ) ;
#50419 = VERTEX_POINT ( 'NONE', #38640 ) ;
#50420 = CARTESIAN_POINT ( 'NONE',  ( 165.6738106836042732, -28.98061976758451053, 313.9678068554149490 ) ) ;
#50421 = ORIENTED_EDGE ( 'NONE', *, *, #59757, .T. ) ;
#50422 = CARTESIAN_POINT ( 'NONE',  ( 97.31584373184972492, -39.30597606054212179, 67.53145861423732299 ) ) ;
#50423 = DIRECTION ( 'NONE',  ( -1.000000000000000000, 0.000000000000000000, 0.000000000000000000 ) ) ;
#50424 = VERTEX_POINT ( 'NONE', #10060 ) ;
#50425 = ADVANCED_FACE ( 'NONE', ( #30058 ), #36869, .F. ) ;
#50426 = DIRECTION ( 'NONE',  ( 1.000000000000000078E-15, -1.000000000000000083E-30, -1.000000000000000000 ) ) ;
#50427 = ORIENTED_EDGE ( 'NONE', *, *, #19670, .F. ) ;
#50428 = LINE ( 'NONE', #56792, #72634 ) ;
#50429 = DIRECTION ( 'NONE',  ( 4.299999999999999979E-14, -1.000000000000000000, 4.400000000000000367E-29 ) ) ;
#50430 = CIRCLE ( 'NONE', #59171, 0.5000000000000004441 ) ;
#50431 = CARTESIAN_POINT ( 'NONE',  ( 142.8832909413445122, -79.11588146349311046, 394.9756252759100903 ) ) ;
#50432 = EDGE_LOOP ( 'NONE', ( #7759, #52986, #69503, #87887 ) ) ;
#50433 = CARTESIAN_POINT ( 'NONE',  ( 109.7758433794879664, -47.46978277150036263, 92.78514908543495210 ) ) ;
#50434 = DIRECTION ( 'NONE',  ( 0.000000000000000000, 0.000000000000000000, 1.000000000000000000 ) ) ;
#50435 = DIRECTION ( 'NONE',  ( 1.000000000000000000, 0.000000000000000000, 0.000000000000000000 ) ) ;
#50436 = FACE_OUTER_BOUND ( 'NONE', #55875, .T. ) ;
#50437 = CARTESIAN_POINT ( 'NONE',  ( -5.586631576746658112, 71.22609051415520298, 118.2265399586805472 ) ) ;
#50438 = ORIENTED_EDGE ( 'NONE', *, *, #38684, .T. ) ;
#50439 = CARTESIAN_POINT ( 'NONE',  ( 19.56670390244796920, -67.87844715994100397, 300.9178068554150514 ) ) ;
#50440 = DIRECTION ( 'NONE',  ( 3.100000000000000258E-29, -3.100000000000000044E-14, -1.000000000000000000 ) ) ;
#50441 = CARTESIAN_POINT ( 'NONE',  ( 118.5256205435843526, -36.72944715994100306, 312.6356252759112522 ) ) ;
#50442 = VECTOR ( 'NONE', #56650, 1000.000000000000000 ) ;
#50445 = ADVANCED_FACE ( 'NONE', ( #24578 ), #65020, .F. ) ;
#50444 = DIRECTION ( 'NONE',  ( 0.000000000000000000, 0.000000000000000000, 1.000000000000000000 ) ) ;
#50443 = CARTESIAN_POINT ( 'NONE',  ( 167.6524903400753885, -49.32844715993521589, 249.9678068554149775 ) ) ;
#50446 = CARTESIAN_POINT ( 'NONE',  ( 116.3212776292278363, -32.94146857470881429, 179.1356252759109395 ) ) ;
#50447 = AXIS2_PLACEMENT_3D ( 'NONE', #64978, #31787, #86322 ) ;
#50448 = ORIENTED_EDGE ( 'NONE', *, *, #51439, .F. ) ;
#50449 = VECTOR ( 'NONE', #79197, 1000.000000000000000 ) ;
#50450 = DIRECTION ( 'NONE',  ( 1.000000000000000000, 0.000000000000000000, 1.047444401652940007E-14 ) ) ;
#50451 = CARTESIAN_POINT ( 'NONE',  ( 98.80555182512732415, -41.96590078842027793, 182.7756252759109543 ) ) ;
#50453 = ORIENTED_EDGE ( 'NONE', *, *, #70576, .T. ) ;
#50452 = CARTESIAN_POINT ( 'NONE',  ( 107.0664832912750057, -36.72944715993903486, 3.024967495036150922 ) ) ;
#50454 = VECTOR ( 'NONE', #73941, 1000.000000000000000 ) ;
#50455 = CARTESIAN_POINT ( 'NONE',  ( 117.4970320020026406, -36.54623693216563396, 284.8413395616252615 ) ) ;
#50456 = DIRECTION ( 'NONE',  ( -0.4634479843259246556, 0.000000000000000000, -0.8861241255175470455 ) ) ;
#50457 = CARTESIAN_POINT ( 'NONE',  ( 134.0664832912739826, -18.72944715994100306, -5.074374724089001809 ) ) ;
#50458 = CARTESIAN_POINT ( 'NONE',  ( 121.5948191693370717, -80.85146542362632260, 250.2178068554179902 ) ) ;
#50459 = CARTESIAN_POINT ( 'NONE',  ( 100.8868523152179364, -44.69971148260871274, 12.05236635724705252 ) ) ;
#50460 = ADVANCED_FACE ( 'NONE', ( #51367, #58632, #79561, #31827, #45001 ), #57753, .T. ) ;
#50461 = DIRECTION ( 'NONE',  ( 0.000000000000000000, -1.000000000000000000, 0.000000000000000000 ) ) ;
#50462 = CIRCLE ( 'NONE', #18564, 0.5000000000000004441 ) ;
#50464 = CARTESIAN_POINT ( 'NONE',  ( 106.8648936900573005, -47.09757847023110600, 227.5489586092449485 ) ) ;
#50463 = CIRCLE ( 'NONE', #62078, 17.00000000000000000 ) ;
#50465 = ORIENTED_EDGE ( 'NONE', *, *, #4803, .T. ) ;
#50466 = EDGE_LOOP ( 'NONE', ( #48677, #84424 ) ) ;
#50467 = CARTESIAN_POINT ( 'NONE',  ( 113.6520771548495503, -30.75516201018407614, 205.8444404487539714 ) ) ;
#50468 = AXIS2_PLACEMENT_3D ( 'NONE', #26671, #74832, #13059 ) ;
#50469 = EDGE_CURVE ( 'NONE', #16654, #61996, #8257, .T. ) ;
#50470 = CARTESIAN_POINT ( 'NONE',  ( 219.9639999999999986, 40.03750000000000142, -7.937500000000000000 ) ) ;
#50471 = CARTESIAN_POINT ( 'NONE',  ( 101.4671292710339117, -29.18466352532158226, 32.02824997256392692 ) ) ;
#50472 = CARTESIAN_POINT ( 'NONE',  ( -97.63151088911699560, 92.64985122628468162, 86.68005309089153343 ) ) ;
#50473 = CARTESIAN_POINT ( 'NONE',  ( 274.0659999999999741, 36.86249999999999716, -7.937500000000000000 ) ) ;
#50474 = VECTOR ( 'NONE', #29979, 1000.000000000000000 ) ;
#50475 = CARTESIAN_POINT ( 'NONE',  ( 63.03715912545729338, -24.42818131006027826, 313.9678068554150059 ) ) ;
#50476 = EDGE_LOOP ( 'NONE', ( #27398, #37872, #56772, #39667 ) ) ;
#50477 = DIRECTION ( 'NONE',  ( 2.973811673103097665E-16, 0.000000000000000000, 1.000000000000000000 ) ) ;
#50478 = CARTESIAN_POINT ( 'NONE',  ( 97.80893753052176010, -40.51861053356429920, 37.63533870039827178 ) ) ;
#50479 = CARTESIAN_POINT ( 'NONE',  ( 96.78489722101812731, -35.14273565208913652, 266.2041967044821149 ) ) ;
#50480 = CARTESIAN_POINT ( 'NONE',  ( 92.55667057654251551, -29.98664840991042269, 0.7256252759109563799 ) ) ;
#50481 = VERTEX_POINT ( 'NONE', #38204 ) ;
#50482 = ORIENTED_EDGE ( 'NONE', *, *, #4088, .F. ) ;
#50483 = CARTESIAN_POINT ( 'NONE',  ( 104.4081006417629851, -46.45808913496205861, 87.36479194099514700 ) ) ;
#50484 = CARTESIAN_POINT ( 'NONE',  ( 172.5664832912729878, -18.82844715994071194, 135.9256252759120684 ) ) ;
#50485 = CARTESIAN_POINT ( 'NONE',  ( 51.34673845256598668, -29.62846900982231446, -5.074374724088000832 ) ) ;
#50486 = DIRECTION ( 'NONE',  ( 0.000000000000000000, -1.000000000000000000, 0.000000000000000000 ) ) ;
#50487 = VECTOR ( 'NONE', #64579, 1000.000000000000000 ) ;
#50488 = VECTOR ( 'NONE', #58285, 1000.000000000000000 ) ;
#50489 = CARTESIAN_POINT ( 'NONE',  ( 97.72045521349410535, -39.61305637792672485, 17.56419670448195092 ) ) ;
#50490 = CARTESIAN_POINT ( 'NONE',  ( 10.91960523489288093, 76.24982137887049305, 117.8513599261979721 ) ) ;
#50491 = ORIENTED_EDGE ( 'NONE', *, *, #88582, .F. ) ;
#50492 = CARTESIAN_POINT ( 'NONE',  ( 117.3094150574360128, -38.89169797369248727, 59.66133956162595098 ) ) ;
#50493 = DIRECTION ( 'NONE',  ( 3.100000000000000258E-29, -3.100000000000000044E-14, -1.000000000000000000 ) ) ;
#50494 = CARTESIAN_POINT ( 'NONE',  ( 115.0549195170180639, -30.03079676387787345, 269.3813395616251682 ) ) ;
#50495 = MANIFOLD_SOLID_BREP ( 'Stock-BR-Y-104-1', #25647 ) ;
#50497 = ORIENTED_EDGE ( 'NONE', *, *, #43447, .F. ) ;
#50496 = ADVANCED_FACE ( 'NONE', ( #73614 ), #65900, .T. ) ;
#50498 = ADVANCED_FACE ( 'NONE', ( #81790, #59963, #88606, #74512, #5480, #40873, #46781 ), #67697, .T. ) ;
#50499 = CARTESIAN_POINT ( 'NONE',  ( 99.48898161933323081, -117.4034471599418197, -11.78219314458159239 ) ) ;
#50500 = FACE_OUTER_BOUND ( 'NONE', #847, .T. ) ;
#50501 = EDGE_CURVE ( 'NONE', #64449, #56609, #13190, .T. ) ;
#50502 = CARTESIAN_POINT ( 'NONE',  ( 0.000000000000000000, 11.42999999999999972, 0.000000000000000000 ) ) ;
#50503 = CARTESIAN_POINT ( 'NONE',  ( 99.36125835269150741, -32.78858003560463175, 93.78047132197198721 ) ) ;
#50504 = CARTESIAN_POINT ( 'NONE',  ( 107.5668116379858787, -47.79447663526521239, 188.6003871806729535 ) ) ;
#50505 = LINE ( 'NONE', #36888, #46411 ) ;
#50506 = ORIENTED_EDGE ( 'NONE', *, *, #87734, .F. ) ;
#50507 = EDGE_CURVE ( 'NONE', #68541, #73425, #53131, .T. ) ;
#50508 = LINE ( 'NONE', #57315, #63977 ) ;
#50509 = ORIENTED_EDGE ( 'NONE', *, *, #64836, .T. ) ;
#50510 = ORIENTED_EDGE ( 'NONE', *, *, #76363, .F. ) ;
#50511 = AXIS2_PLACEMENT_3D ( 'NONE', #37390, #85116, #50560 ) ;
#50512 = EDGE_CURVE ( 'NONE', #65273, #22589, #3905, .T. ) ;
#50513 = AXIS2_PLACEMENT_3D ( 'NONE', #45828, #25408, #48073 ) ;
#50514 = CARTESIAN_POINT ( 'NONE',  ( 75.31670390244798341, -50.82844715994100682, 84.20080685541500998 ) ) ;
#50515 = ORIENTED_EDGE ( 'NONE', *, *, #41004, .T. ) ;
#50516 = ORIENTED_EDGE ( 'NONE', *, *, #48870, .T. ) ;
#50517 = CARTESIAN_POINT ( 'NONE',  ( 37.03715912545342093, -48.62818131006128652, 193.9678068554150911 ) ) ;
#50518 = CARTESIAN_POINT ( 'NONE',  ( 116.3216976867776964, -32.94060878512167534, 40.13562527591096796 ) ) ;
#50519 = EDGE_CURVE ( 'NONE', #6845, #7688, #28536, .T. ) ;
#50520 = CARTESIAN_POINT ( 'NONE',  ( 99.32441224009949110, -32.03125536261004669, 125.3028960185529570 ) ) ;
#50521 = CARTESIAN_POINT ( 'NONE',  ( 115.7136949400716333, -42.59221908682786761, 273.3527681330537575 ) ) ;
#50522 = LINE ( 'NONE', #43705, #35388 ) ;
#50523 = EDGE_LOOP ( 'NONE', ( #74109, #18320, #19007, #51183 ) ) ;
#50524 = AXIS2_PLACEMENT_3D ( 'NONE', #82452, #12499, #12048 ) ;
#50525 = ORIENTED_EDGE ( 'NONE', *, *, #60431, .F. ) ;
#50526 = DIRECTION ( 'NONE',  ( 0.000000000000000000, 0.000000000000000000, 1.000000000000000000 ) ) ;
#50527 = VECTOR ( 'NONE', #70328, 1000.000000000000000 ) ;
#50528 = CARTESIAN_POINT ( 'NONE',  ( 29.77381068363477112, -48.62134037875501491, 300.4678068554150059 ) ) ;
#50529 = LINE ( 'NONE', #35555, #45513 ) ;
#50530 = CARTESIAN_POINT ( 'NONE',  ( 101.6553708923145649, -27.03755641387271069, 105.4937205140069665 ) ) ;
#50531 = DIRECTION ( 'NONE',  ( 1.000000000000000000, 4.163336342344333240E-14, 0.000000000000000000 ) ) ;
#50532 = ORIENTED_EDGE ( 'NONE', *, *, #14310, .T. ) ;
#50533 = CARTESIAN_POINT ( 'NONE',  ( 117.4299418851264818, -35.59553461117717887, 278.9127681330539872 ) ) ;
#50534 = LINE ( 'NONE', #71457, #87770 ) ;
#50535 =( LENGTH_UNIT ( ) NAMED_UNIT ( * ) SI_UNIT ( .MILLI., .METRE. ) );
#50536 = LINE ( 'NONE', #9222, #50291 ) ;
#50538 = CARTESIAN_POINT ( 'NONE',  ( 179.8608231853560255, -35.55794170701751256, -5.074374724088000832 ) ) ;
#50537 = CARTESIAN_POINT ( 'NONE',  ( 134.0664832912740110, -8.729447159940999512, 7.443125275912000127 ) ) ;
#50539 = CARTESIAN_POINT ( 'NONE',  ( 88.17226027475679473, -58.72944715994100306, 239.5838068554174924 ) ) ;
#50540 = DIRECTION ( 'NONE',  ( 1.000000000000000000, 0.000000000000000000, 0.000000000000000000 ) ) ;
#50541 = CARTESIAN_POINT ( 'NONE',  ( 131.3165200636274790, -36.90534128960221238, 6.749824347015201731 ) ) ;
#50542 = AXIS2_PLACEMENT_3D ( 'NONE', #1832, #16349, #77682 ) ;
#50543 = CARTESIAN_POINT ( 'NONE',  ( 180.1667039024460166, -28.27351298637340093, -5.074374724088000832 ) ) ;
#50544 = CARTESIAN_POINT ( 'NONE',  ( 41.56648329127398966, -27.82844715994070484, 258.9256252759120116 ) ) ;
#50545 = DIRECTION ( 'NONE',  ( 3.100000000000000258E-29, -3.100000000000000044E-14, -1.000000000000000000 ) ) ;
#50547 = VERTEX_POINT ( 'NONE', #89039 ) ;
#50546 = LINE ( 'NONE', #64631, #64622 ) ;
#50548 = CARTESIAN_POINT ( 'NONE',  ( 116.3168070826688876, -32.94156582961523583, 135.1356252759109680 ) ) ;
#50549 = CARTESIAN_POINT ( 'NONE',  ( 100.5702229155400858, -28.47427015469623868, 15.60705384733995871 ) ) ;
#50550 = CARTESIAN_POINT ( 'NONE',  ( 108.9451852418780362, -26.43907245703257303, 160.9327681330539690 ) ) ;
#50551 = CARTESIAN_POINT ( 'NONE',  ( 116.4941038412854510, -32.22865339830268283, 15.18133956162492915 ) ) ;
#50552 = AXIS2_PLACEMENT_3D ( 'NONE', #6365, #89042, #82248 ) ;
#50555 = EDGE_CURVE ( 'NONE', #85489, #22788, #39086, .T. ) ;
#50554 = CARTESIAN_POINT ( 'NONE',  ( 82.59705637153234647, -35.65296049054536098, 7.043700149390168974 ) ) ;
#50553 = CARTESIAN_POINT ( 'NONE',  ( -48.02966122971775320, 65.60000000000000853, -8.747637655308301746E-15 ) ) ;
#50556 = CARTESIAN_POINT ( 'NONE',  ( 9.749037034254360634, 224.4999999999999432, 152.4294779587682740 ) ) ;
#50557 = AXIS2_PLACEMENT_3D ( 'NONE', #30695, #23460, #72038 ) ;
#50558 = EDGE_CURVE ( 'NONE', #22058, #31578, #25464, .T. ) ;
#50559 = VERTEX_POINT ( 'NONE', #11392 ) ;
#50560 = DIRECTION ( 'NONE',  ( 0.000000000000000000, 0.000000000000000000, -1.000000000000000000 ) ) ;
#50561 = ORIENTED_EDGE ( 'NONE', *, *, #6340, .T. ) ;
#50562 = CARTESIAN_POINT ( 'NONE',  ( 116.0809032858470999, -32.84949784884748425, 75.14991099019596277 ) ) ;
#50564 = VERTEX_POINT ( 'NONE', #81357 ) ;
#50563 = CARTESIAN_POINT ( 'NONE',  ( 6.579133765263863509, 93.41355262086047162, 130.3901338211574057 ) ) ;
#50565 = CARTESIAN_POINT ( 'NONE',  ( 100.8873290257058954, -44.70010636051070918, 48.05227766291039160 ) ) ;
#50566 = CARTESIAN_POINT ( 'NONE',  ( 116.7748712849171255, -40.56502120445009751, 189.5270538473389479 ) ) ;
#50567 = DIRECTION ( 'NONE',  ( 0.000000000000000000, 0.000000000000000000, 1.000000000000000000 ) ) ;
#50568 = CARTESIAN_POINT ( 'NONE',  ( 110.8561050889767472, -45.98356882364006282, 147.8857656880664422 ) ) ;
#50569 = CARTESIAN_POINT ( 'NONE',  ( -44.45000000000000284, 50.79999999999999716, 257.1750000000000114 ) ) ;
#50570 = CARTESIAN_POINT ( 'NONE',  ( 105.8095979597606373, -26.72298644015105396, 86.17751431161180165 ) ) ;
#50571 = AXIS2_PLACEMENT_3D ( 'NONE', #14811, #28418, #8439 ) ;
#50572 = CARTESIAN_POINT ( 'NONE',  ( 144.5619505544954393, -138.4421194277352924, 247.5996269027399990 ) ) ;
#50573 = CARTESIAN_POINT ( 'NONE',  ( 110.8524082669982391, -45.98508177266331387, 97.88544780039453030 ) ) ;
#50574 = CARTESIAN_POINT ( 'NONE',  ( 105.4244293397738659, -47.72525222749325735, 147.4584824187689662 ) ) ;
#50575 = ORIENTED_EDGE ( 'NONE', *, *, #20968, .F. ) ;
#50576 = ORIENTED_EDGE ( 'NONE', *, *, #89391, .T. ) ;
#50577 = VECTOR ( 'NONE', #1875, 1000.000000000000000 ) ;
#50578 = CARTESIAN_POINT ( 'NONE',  ( 97.82387236378413320, -38.41783952554947490, 47.91396425827898753 ) ) ;
#50579 = EDGE_CURVE ( 'NONE', #18807, #50606, #77902, .T. ) ;
#50580 = LINE ( 'NONE', #10586, #37057 ) ;
#50582 = LINE ( 'NONE', #31035, #17217 ) ;
#50581 = CARTESIAN_POINT ( 'NONE',  ( 101.1405520526760284, -45.23956608920054379, 233.0803871806719769 ) ) ;
#50583 = CARTESIAN_POINT ( 'NONE',  ( 31.90335556477799628, -33.89581943344391135, 342.9256252759119548 ) ) ;
#50584 = CARTESIAN_POINT ( 'NONE',  ( 97.31584962811177775, -39.30599893963958635, 112.5320257889539306 ) ) ;
#50585 = CARTESIAN_POINT ( 'NONE',  ( 112.8677825012601375, -28.59025478454122648, 249.5838084826162913 ) ) ;
#50586 = VECTOR ( 'NONE', #24036, 1000.000000000000000 ) ;
#50587 = LINE ( 'NONE', #45102, #60895 ) ;
#50588 = CARTESIAN_POINT ( 'NONE',  ( 9.473969254672010010, 74.23277938464349290, 118.1771504636201797 ) ) ;
#50589 = CARTESIAN_POINT ( 'NONE',  ( 108.0049669398584911, -26.36739623290726442, 155.0041967044819557 ) ) ;
#50590 = ORIENTED_EDGE ( 'NONE', *, *, #46817, .T. ) ;
#50591 = ORIENTED_EDGE ( 'NONE', *, *, #78325, .T. ) ;
#50592 = VERTEX_POINT ( 'NONE', #68601 ) ;
#50593 = AXIS2_PLACEMENT_3D ( 'NONE', #74164, #32357, #40974 ) ;
#50594 = ORIENTED_CLOSED_SHELL ( 'NONE', *, #73489, .F. );
#50595 = CARTESIAN_POINT ( 'NONE',  ( 9.275599959524004845, 73.86527412294591954, 130.2264118494045420 ) ) ;
#50596 = DIRECTION ( 'NONE',  ( 0.000000000000000000, 1.000000000000000000, 0.000000000000000000 ) ) ;
#50597 = AXIS2_PLACEMENT_3D ( 'NONE', #51201, #24856, #32545 ) ;
#50598 = CARTESIAN_POINT ( 'NONE',  ( 152.0368932755772562, -23.42844715993588878, 117.4678068554150485 ) ) ;
#50599 = CARTESIAN_POINT ( 'NONE',  ( 117.0719072149801434, -35.46254345245687745, 104.9272870867127665 ) ) ;
#50600 = CARTESIAN_POINT ( 'NONE',  ( 114.4736784013144586, -40.22460793573437599, 226.2938046553059621 ) ) ;
#50601 = CARTESIAN_POINT ( 'NONE',  ( 98.30752301746520061, -41.72885616756393290, 267.7397901826493580 ) ) ;
#50602 = CARTESIAN_POINT ( 'NONE',  ( 99.10121394234140269, -45.50393173043428163, 156.9899109901969609 ) ) ;
#50603 = DIRECTION ( 'NONE',  ( 0.000000000000000000, 0.000000000000000000, -1.000000000000000000 ) ) ;
#50604 = ORIENTED_EDGE ( 'NONE', *, *, #49924, .T. ) ;
#50607 = ORIENTED_EDGE ( 'NONE', *, *, #60600, .T. ) ;
#50606 = VERTEX_POINT ( 'NONE', #11844 ) ;
#50605 = ADVANCED_FACE ( 'NONE', ( #34053, #89492 ), #5025, .F. ) ;
#50608 = AXIS2_PLACEMENT_3D ( 'NONE', #31637, #59779, #44368 ) ;
#50609 = FACE_OUTER_BOUND ( 'NONE', #54397, .T. ) ;
#50610 = ORIENTED_EDGE ( 'NONE', *, *, #11656, .F. ) ;
#50611 = ORIENTED_EDGE ( 'NONE', *, *, #16381, .F. ) ;
#50612 = FACE_BOUND ( 'NONE', #26388, .T. ) ;
#50613 = DIRECTION ( 'NONE',  ( 0.7071067811865431318, -0.7071067811865517916, 7.071067811865425043E-16 ) ) ;
#50614 = CARTESIAN_POINT ( 'NONE',  ( 97.00631399252166887, -37.24296311215223909, 267.7987261630397029 ) ) ;
#50615 = FACE_OUTER_BOUND ( 'NONE', #33390, .T. ) ;
#50616 = ORIENTED_EDGE ( 'NONE', *, *, #81613, .T. ) ;
#50617 = EDGE_CURVE ( 'NONE', #11707, #73753, #34375, .T. ) ;
#50618 = CARTESIAN_POINT ( 'NONE',  ( 114.3732006581859650, -41.89629318141880532, 9.635625275910941312 ) ) ;
#50619 = CIRCLE ( 'NONE', #7059, 12.99999999999999822 ) ;
#50620 = CARTESIAN_POINT ( 'NONE',  ( 93.94797395270801132, -35.60435878782501362, 247.7440089327910755 ) ) ;
#50621 = VERTEX_POINT ( 'NONE', #20001 ) ;
#50622 = ORIENTED_EDGE ( 'NONE', *, *, #45905, .T. ) ;
#50623 = CARTESIAN_POINT ( 'NONE',  ( 104.4081753580950505, -46.45811105792077456, 112.3648722168799736 ) ) ;
#50624 = ORIENTED_EDGE ( 'NONE', *, *, #22455, .T. ) ;
#50625 = ORIENTED_EDGE ( 'NONE', *, *, #50808, .T. ) ;
#50626 = EDGE_CURVE ( 'NONE', #76956, #4611, #47681, .T. ) ;
#50627 = CARTESIAN_POINT ( 'NONE',  ( 109.9248237270229680, -44.80917438794489271, 37.26956268521996662 ) ) ;
#50628 = CARTESIAN_POINT ( 'NONE',  ( 116.8272927809998123, -43.49410631979629471, 163.3441967044829823 ) ) ;
#50629 = CARTESIAN_POINT ( 'NONE',  ( 109.1969564574039282, -26.54663071456422330, 139.9127681330539872 ) ) ;
#50630 = EDGE_CURVE ( 'NONE', #84435, #14978, #18202, .T. ) ;
#50631 = DIRECTION ( 'NONE',  ( 3.100000000000000258E-29, -3.100000000000000044E-14, -1.000000000000000000 ) ) ;
#50632 = CARTESIAN_POINT ( 'NONE',  ( 110.2558863881303779, -26.76706588525435748, 230.8299109901969643 ) ) ;
#50633 = DIRECTION ( 'NONE',  ( 1.000000000000000078E-15, -1.000000000000000083E-30, -1.000000000000000000 ) ) ;
#50634 = DIRECTION ( 'NONE',  ( 0.000000000000000000, 1.000000000000000000, 0.000000000000000000 ) ) ;
#50635 = ORIENTED_EDGE ( 'NONE', *, *, #2286, .F. ) ;
#50636 = FACE_OUTER_BOUND ( 'NONE', #12442, .T. ) ;
#50637 = ORIENTED_EDGE ( 'NONE', *, *, #12982, .T. ) ;
#50638 = VECTOR ( 'NONE', #45053, 1000.000000000000000 ) ;
#50639 = ORIENTED_EDGE ( 'NONE', *, *, #82740, .T. ) ;
#50640 = AXIS2_PLACEMENT_3D ( 'NONE', #13944, #42970, #83437 ) ;
#50641 = AXIS2_PLACEMENT_3D ( 'NONE', #27258, #89043, #69945 ) ;
#50642 = CARTESIAN_POINT ( 'NONE',  ( 107.6569944592711607, -47.81385874506208467, 197.6308633711489620 ) ) ;
#50643 = EDGE_LOOP ( 'NONE', ( #85046, #6751, #26662, #11282 ) ) ;
#50644 = CARTESIAN_POINT ( 'NONE',  ( 117.4265927121613089, -30.97543824232759135, 179.2299109901959753 ) ) ;
#50645 = CARTESIAN_POINT ( 'NONE',  ( 194.5667039024479834, -67.87844715994100397, 10.91780685541479734 ) ) ;
#50646 = CARTESIAN_POINT ( 'NONE',  ( 135.6382054840678109, -34.47341874818869201, 7.827313014938068747 ) ) ;
#50647 = DIRECTION ( 'NONE',  ( -1.000000000000000000, -4.554376769437570034E-14, 0.000000000000000000 ) ) ;
#50650 = CARTESIAN_POINT ( 'NONE',  ( 105.6350724880777534, -47.03380199863519806, 253.4670538473393719 ) ) ;
#50649 = CARTESIAN_POINT ( 'NONE',  ( 100.7545310429336354, -44.50279142785353770, 57.03342830892890447 ) ) ;
#50648 = CARTESIAN_POINT ( 'NONE',  ( 3.175000000000355094, 17.78000000000000114, 33.98325472291460159 ) ) ;
#50651 = CARTESIAN_POINT ( 'NONE',  ( 194.5667039024479834, -67.87844715994100397, 10.91780685541479734 ) ) ;
#50652 = CYLINDRICAL_SURFACE ( 'NONE', #51096, 17.33514202138210081 ) ;
#50653 = CARTESIAN_POINT ( 'NONE',  ( 97.33757460489857749, -34.07214903665069272, 272.1144460458409071 ) ) ;
#50654 = AXIS2_PLACEMENT_3D ( 'NONE', #76770, #14557, #20914 ) ;
#50655 = LINE ( 'NONE', #62940, #15250 ) ;
#50656 = AXIS2_PLACEMENT_3D ( 'NONE', #89656, #19265, #5642 ) ;
#50657 = CARTESIAN_POINT ( 'NONE',  ( 64.67079002020506096, -0.9301828534102468682, 361.9756252759101471 ) ) ;
#50658 = CYLINDRICAL_SURFACE ( 'NONE', #79674, 0.2500000000000039968 ) ;
#50660 = ORIENTED_EDGE ( 'NONE', *, *, #67706, .F. ) ;
#50659 = CARTESIAN_POINT ( 'NONE',  ( 99.16241280097113986, -32.69931702961348208, 195.5838068554172651 ) ) ;
#50661 = DIRECTION ( 'NONE',  ( 0.7071067811865473507, 0.7071067811865477948, 0.000000000000000000 ) ) ;
#50662 = CARTESIAN_POINT ( 'NONE',  ( 114.9818473740405835, -29.91084206771912690, 184.3927681330539770 ) ) ;
#50663 = CARTESIAN_POINT ( 'NONE',  ( 95.34914990350537778, -34.95780559393485731, 67.20705384733894050 ) ) ;
#50664 = CARTESIAN_POINT ( 'NONE',  ( 98.22454660805831850, -42.33418938753942484, 182.7756252759109543 ) ) ;
#50665 = DIRECTION ( 'NONE',  ( 1.000000000000000000, 0.000000000000000000, 0.000000000000000000 ) ) ;
#50666 = AXIS2_PLACEMENT_3D ( 'NONE', #10225, #80617, #37930 ) ;
#50667 = DIRECTION ( 'NONE',  ( 0.000000000000000000, -1.000000000000000000, 0.000000000000000000 ) ) ;
#50669 = DIRECTION ( 'NONE',  ( -1.000000000000000078E-15, 1.000000000000000083E-30, 1.000000000000000000 ) ) ;
#50668 = PLANE ( 'NONE',  #7269 ) ;
#50670 = CARTESIAN_POINT ( 'NONE',  ( 133.5842039024480812, -58.72944715994091780, 231.5838068554170093 ) ) ;
#50671 = CARTESIAN_POINT ( 'NONE',  ( 144.0654454572467671, -140.6784471599409017, 245.5026818079589930 ) ) ;
#50672 = ORIENTED_EDGE ( 'NONE', *, *, #33575, .T. ) ;
#50673 = LINE ( 'NONE', #72029, #61639 ) ;
#50674 = EDGE_CURVE ( 'NONE', #10101, #36821, #32269, .T. ) ;
#50675 = ORIENTED_EDGE ( 'NONE', *, *, #9694, .F. ) ;
#50676 = ORIENTED_EDGE ( 'NONE', *, *, #8871, .F. ) ;
#50677 = AXIS2_PLACEMENT_3D ( 'NONE', #80595, #4728, #33768 ) ;
#50678 = VECTOR ( 'NONE', #1389, 1000.000000000000000 ) ;
#50679 = CARTESIAN_POINT ( 'NONE',  ( 101.0184087763112757, -44.32493413285080663, 121.4638483995059630 ) ) ;
#50681 = ORIENTED_EDGE ( 'NONE', *, *, #65774, .F. ) ;
#50680 = DIRECTION ( 'NONE',  ( -2.900000000000000265E-14, 2.000000000000000155E-15, -1.000000000000000000 ) ) ;
#50682 = CARTESIAN_POINT ( 'NONE',  ( 117.8527506973082524, -39.03601561205230297, 104.6708633711489824 ) ) ;
#50683 = DIRECTION ( 'NONE',  ( -1.000000000000000000, -2.756263715554006823E-15, 0.000000000000000000 ) ) ;
#50684 = LINE ( 'NONE', #748, #71743 ) ;
#50685 = DIRECTION ( 'NONE',  ( 2.900000000000000265E-14, -2.000000000000000155E-15, 1.000000000000000000 ) ) ;
#50686 = CARTESIAN_POINT ( 'NONE',  ( 100.8863495415024119, -28.40209871822978371, 35.59657765686397113 ) ) ;
#50687 = ORIENTED_EDGE ( 'NONE', *, *, #86903, .T. ) ;
#50688 = AXIS2_PLACEMENT_3D ( 'NONE', #34274, #61976, #89714 ) ;
#50689 = ORIENTED_EDGE ( 'NONE', *, *, #13082, .T. ) ;
#50690 = VERTEX_POINT ( 'NONE', #83136 ) ;
#50691 = ADVANCED_FACE ( 'NONE', ( #20894 ), #898, .F. ) ;
#50692 = DIRECTION ( 'NONE',  ( 0.000000000000000000, 1.000000000000000000, -0.000000000000000000 ) ) ;
#50693 = DIRECTION ( 'NONE',  ( 0.7071067811864886199, 0.7071067811866064146, 7.071067811864879743E-16 ) ) ;
#50694 = CARTESIAN_POINT ( 'NONE',  ( 97.31584371326931659, -39.30597598860000375, 117.5314586083788555 ) ) ;
#50695 = CARTESIAN_POINT ( 'NONE',  ( 0.000000000000000000, 95.00619999999999266, 38.10000000000000142 ) ) ;
#50696 = DIRECTION ( 'NONE',  ( 1.000000000000000078E-15, -1.000000000000000083E-30, -1.000000000000000000 ) ) ;
#50697 = CARTESIAN_POINT ( 'NONE',  ( 97.75827217529801771, -40.38459891742106578, 52.62384772014601708 ) ) ;
#50698 = CARTESIAN_POINT ( 'NONE',  ( 145.5667039024470739, -139.1784471599409017, 228.4678068554179902 ) ) ;
#50699 = AXIS2_PLACEMENT_3D ( 'NONE', #88368, #5692, #4789 ) ;
#50700 = CARTESIAN_POINT ( 'NONE',  ( -10.61352881085396049, 89.52455520069554495, 130.1238749127236360 ) ) ;
#50701 = CARTESIAN_POINT ( 'NONE',  ( 99.99555918775621421, -44.36035129061385618, 46.98133956162592284 ) ) ;
#50702 = EDGE_CURVE ( 'NONE', #29891, #28724, #70848, .T. ) ;
#50703 = ORIENTED_EDGE ( 'NONE', *, *, #16190, .F. ) ;
#50704 = VECTOR ( 'NONE', #70227, 1000.000000000000000 ) ;
#50705 = EDGE_CURVE ( 'NONE', #66869, #52443, #36316, .T. ) ;
#50706 = DIRECTION ( 'NONE',  ( -0.000000000000000000, -0.000000000000000000, -1.000000000000000000 ) ) ;
#50707 = CARTESIAN_POINT ( 'NONE',  ( 82.78637150392543731, -91.25622735614753367, 250.2178068554179902 ) ) ;
#50708 = CARTESIAN_POINT ( 'NONE',  ( 113.0638415271824897, -42.26672268200739069, 121.0509475124479906 ) ) ;
#50709 = AXIS2_PLACEMENT_3D ( 'NONE', #21502, #1506, #76906 ) ;
#50710 = VECTOR ( 'NONE', #52797, 1000.000000000000000 ) ;
#50711 = EDGE_CURVE ( 'NONE', #84863, #61024, #6883, .T. ) ;
#50712 = CYLINDRICAL_SURFACE ( 'NONE', #36912, 2.116999999999980009 ) ;
#50713 = DIRECTION ( 'NONE',  ( 1.000000000000000000, 8.673617379883546378E-16, 9.757819552368989676E-16 ) ) ;
#50714 = EDGE_LOOP ( 'NONE', ( #1406, #6595, #43440, #73596 ) ) ;
#50715 = VERTEX_POINT ( 'NONE', #41759 ) ;
#50716 = VECTOR ( 'NONE', #77440, 1000.000000000000000 ) ;
#50717 = FACE_OUTER_BOUND ( 'NONE', #9075, .T. ) ;
#50718 = VERTEX_POINT ( 'NONE', #35853 ) ;
#50719 = VERTEX_POINT ( 'NONE', #14980 ) ;
#50720 = STYLED_ITEM ( 'NONE', ( #46835 ), #43438 ) ;
#50721 = EDGE_CURVE ( 'NONE', #29906, #58630, #19921, .T. ) ;
#50722 = CARTESIAN_POINT ( 'NONE',  ( 100.4550560919867479, -30.82882778563945791, 187.1787261630399541 ) ) ;
#50723 = DIRECTION ( 'NONE',  ( 0.000000000000000000, 0.000000000000000000, 1.000000000000000000 ) ) ;
#50724 = AXIS2_PLACEMENT_3D ( 'NONE', #15454, #56301, #35420 ) ;
#50725 = CARTESIAN_POINT ( 'NONE',  ( 96.06465719955961902, -38.01203376208108153, 82.43086337114895912 ) ) ;
#50726 = FACE_OUTER_BOUND ( 'NONE', #62921, .T. ) ;
#50727 = CARTESIAN_POINT ( 'NONE',  ( 110.8538278642257779, -45.98450097318836782, 17.88556988677979476 ) ) ;
#50728 = ORIENTED_EDGE ( 'NONE', *, *, #57603, .T. ) ;
#50729 = EDGE_LOOP ( 'NONE', ( #1659, #60375 ) ) ;
#50730 = ORIENTED_EDGE ( 'NONE', *, *, #83685, .T. ) ;
#50731 = CIRCLE ( 'NONE', #52131, 27.99999999999999645 ) ;
#50732 = ADVANCED_FACE ( 'NONE', ( #62218 ), #61991, .T. ) ;
#50733 = CARTESIAN_POINT ( 'NONE',  ( 98.88612577743202792, -36.32393613343754879, 169.1052332267339580 ) ) ;
#50734 = CARTESIAN_POINT ( 'NONE',  ( 117.4766623710874853, -37.96092365070988706, 53.73276813305394484 ) ) ;
#50735 = ORIENTED_EDGE ( 'NONE', *, *, #47795, .T. ) ;
#50736 = CARTESIAN_POINT ( 'NONE',  ( 111.4063510358307667, -46.18429848020807782, 27.91848241876792969 ) ) ;
#50737 = CARTESIAN_POINT ( 'NONE',  ( 117.4353638176713446, -35.45525114565609215, 189.9241967044829664 ) ) ;
#50738 = EDGE_CURVE ( 'NONE', #65614, #16533, #42214, .T. ) ;
#50739 = LINE ( 'NONE', #23510, #26313 ) ;
#50740 = CARTESIAN_POINT ( 'NONE',  ( -109.6785575274413418, 48.96444734860763504, 70.82007752391335487 ) ) ;
#50741 = CARTESIAN_POINT ( 'NONE',  ( 114.7074080197622976, -44.71632701241580321, 109.1718157521009687 ) ) ;
#50743 = EDGE_CURVE ( 'NONE', #42621, #5363, #69493, .T. ) ;
#50742 = DIRECTION ( 'NONE',  ( -0.7071067811865753283, 0.7071067811865197061, -7.071067811865760309E-16 ) ) ;
#50744 = VERTEX_POINT ( 'NONE', #35398 ) ;
#50745 = FACE_BOUND ( 'NONE', #12075, .T. ) ;
#50746 = EDGE_CURVE ( 'NONE', #62066, #19234, #39051, .T. ) ;
#50747 = VERTEX_POINT ( 'NONE', #49919 ) ;
#50748 = CARTESIAN_POINT ( 'NONE',  ( 116.3168070826688876, -32.94156582961523583, 135.1356252759109680 ) ) ;
#50749 = ORIENTED_EDGE ( 'NONE', *, *, #86112, .F. ) ;
#50751 = ORIENTED_EDGE ( 'NONE', *, *, #41167, .F. ) ;
#50750 = CIRCLE ( 'NONE', #76825, 0.9999999999999731326 ) ;
#50752 = B_SPLINE_CURVE_WITH_KNOTS ( 'NONE', 3,
 ( #32716, #80002, #54476, #69037, #28130, #75410, #14068, #27247, #13621, #7703, #47676, #14975, #76297, #438, #54923, #13184, #6801, #55821 ),
 .UNSPECIFIED., .F., .F.,
 ( 4, 2, 2, 2, 2, 2, 2, 2, 4 ),
 ( 0.000000000000000000, 0.06249549862835345609, 0.1249909972567069122, 0.1874864958850603613, 0.2499819945134138244, 0.3124774931417672597, 0.3749729917701207227, 0.4374684903984741857, 0.4999639890268276488 ),
 .UNSPECIFIED. ) ;
#50753 = DIRECTION ( 'NONE',  ( 0.000000000000000000, 0.000000000000000000, -1.000000000000000000 ) ) ;
#50754 =( BOUNDED_CURVE ( )  B_SPLINE_CURVE ( 3, ( #82742, #75465, #35003, #13235 ),
 .UNSPECIFIED., .F., .T. ) 
 B_SPLINE_CURVE_WITH_KNOTS ( ( 4, 4 ),
 ( 4.712388980377630432, 6.283185307174195877 ),
 .UNSPECIFIED. ) 
 CURVE ( )  GEOMETRIC_REPRESENTATION_ITEM ( )  RATIONAL_B_SPLINE_CURVE ( ( 1.000000000000000000, 0.8047378541227010462, 0.8047378541227010462, 1.000000000000000000 ) ) 
 REPRESENTATION_ITEM ( '' )  );
#50755 = CARTESIAN_POINT ( 'NONE',  ( 10.69948230274378531, 89.21725969999198469, 118.0724339613718570 ) ) ;
#50756 = CARTESIAN_POINT ( 'NONE',  ( 116.6749405801447921, -32.59381477748385691, 79.14991099019697174 ) ) ;
#50757 = DIRECTION ( 'NONE',  ( 0.000000000000000000, 0.000000000000000000, 1.000000000000000000 ) ) ;
#50758 = FACE_OUTER_BOUND ( 'NONE', #89489, .T. ) ;
#50759 = CARTESIAN_POINT ( 'NONE',  ( -34.75390121890993811, 65.59999999999998010, 71.80362806563780964 ) ) ;
#50760 = CARTESIAN_POINT ( 'NONE',  ( 99.23822674327645643, -42.59304969680529496, 66.83848241876894747 ) ) ;
#50762 = CARTESIAN_POINT ( 'NONE',  ( 117.7567108552514128, -34.01230579303181401, 165.0365776568629315 ) ) ;
#50761 = CARTESIAN_POINT ( 'NONE',  ( 97.07198648724674683, -35.37904510147855319, 111.2190064217568874 ) ) ;
#50763 = DIRECTION ( 'NONE',  ( 0.000000000000000000, 0.000000000000000000, 1.000000000000000000 ) ) ;
#50764 = DIRECTION ( 'NONE',  ( 0.7071067812152160847, -0.7071067811578790607, 0.000000000000000000 ) ) ;
#50765 = ORIENTED_EDGE ( 'NONE', *, *, #71061, .F. ) ;
#50766 = FACE_OUTER_BOUND ( 'NONE', #69415, .T. ) ;
#50767 = AXIS2_PLACEMENT_3D ( 'NONE', #81889, #82342, #40975 ) ;
#50768 = PLANE ( 'NONE',  #3560 ) ;
#50769 = ORIENTED_EDGE ( 'NONE', *, *, #24199, .T. ) ;
#50770 = AXIS2_PLACEMENT_3D ( 'NONE', #38372, #51109, #59698 ) ;
#50771 = DIRECTION ( 'NONE',  ( -0.000000000000000000, -0.000000000000000000, -1.000000000000000000 ) ) ;
#50773 = ORIENTED_EDGE ( 'NONE', *, *, #64643, .F. ) ;
#50772 = CARTESIAN_POINT ( 'NONE',  ( 103.7090067442367314, -26.14926592973559138, 205.3089586092439731 ) ) ;
#50774 = DIRECTION ( 'NONE',  ( 2.999999999999999839E-15, -1.000000000000000000, 2.999999999999999900E-30 ) ) ;
#50775 = CARTESIAN_POINT ( 'NONE',  ( 96.24544184373708333, -34.36507245719054282, 252.1432443235302969 ) ) ;
#50776 = CARTESIAN_POINT ( 'NONE',  ( 96.03173718742787912, -37.92605769912402991, 77.40038718067299328 ) ) ;
#50777 = CARTESIAN_POINT ( 'NONE',  ( 75.31670390244798341, -67.87844715994100397, 60.91780685541480267 ) ) ;
#50778 = LINE ( 'NONE', #22199, #45996 ) ;
#50779 = DIRECTION ( 'NONE',  ( 0.000000000000000000, 1.000000000000000000, 0.000000000000000000 ) ) ;
#50780 = ORIENTED_EDGE ( 'NONE', *, *, #20381, .F. ) ;
#50781 = VECTOR ( 'NONE', #41681, 1000.000000000000000 ) ;
#50782 = ORIENTED_EDGE ( 'NONE', *, *, #13085, .F. ) ;
#50783 = VERTEX_POINT ( 'NONE', #56744 ) ;
#50784 = CIRCLE ( 'NONE', #82710, 0.5000000000000004441 ) ;
#50785 = VERTEX_POINT ( 'NONE', #13628 ) ;
#50786 = LINE ( 'NONE', #63524, #78481 ) ;
#50787 = CARTESIAN_POINT ( 'NONE',  ( 96.53701874497966173, -40.09164955422465937, 277.5603871806729899 ) ) ;
#50788 = CYLINDRICAL_SURFACE ( 'NONE', #73660, 4.750000000000004441 ) ;
#50789 = DIRECTION ( 'NONE',  ( 1.907762142705490052E-15, 7.167082501179359715E-16, -1.000000000000000000 ) ) ;
#50790 = AXIS2_PLACEMENT_3D ( 'NONE', #17703, #53521, #60354 ) ;
#50792 = CARTESIAN_POINT ( 'NONE',  ( 78.17938156622449242, 72.47328848629021536, 89.12695577293618499 ) ) ;
#50791 = PLANE ( 'NONE',  #83047 ) ;
#50793 = DIRECTION ( 'NONE',  ( 0.000000000000000000, 0.000000000000000000, -1.000000000000000000 ) ) ;
#50794 = CARTESIAN_POINT ( 'NONE',  ( 102.4276729374712431, -43.93594010915269621, 221.5438483995059755 ) ) ;
#50795 = ORIENTED_EDGE ( 'NONE', *, *, #71198, .T. ) ;
#50796 = ORIENTED_EDGE ( 'NONE', *, *, #27023, .T. ) ;
#50797 = ORIENTED_EDGE ( 'NONE', *, *, #42189, .T. ) ;
#50798 = EDGE_CURVE ( 'NONE', #59868, #6360, #84488, .T. ) ;
#50799 = FACE_OUTER_BOUND ( 'NONE', #66113, .T. ) ;
#50800 = CARTESIAN_POINT ( 'NONE',  ( 100.8873721005049475, -44.70014299556108739, 182.0523503870009847 ) ) ;
#50801 = EDGE_CURVE ( 'NONE', #41861, #35904, #22855, .T. ) ;
#50802 = CARTESIAN_POINT ( 'NONE',  ( 99.18317230595245348, -39.95607890373031523, 8.067297591610955720 ) ) ;
#50803 = VECTOR ( 'NONE', #17036, 1000.000000000000000 ) ;
#50804 = FACE_OUTER_BOUND ( 'NONE', #81660, .T. ) ;
#50805 = EDGE_CURVE ( 'NONE', #31593, #50744, #57652, .T. ) ;
#50806 = CARTESIAN_POINT ( 'NONE',  ( 97.28626111821324685, -36.62605694204433604, 107.3184824187669619 ) ) ;
#50807 = DIRECTION ( 'NONE',  ( 1.000000000000000000, 0.000000000000000000, 0.000000000000000000 ) ) ;
#50808 = EDGE_CURVE ( 'NONE', #15323, #86096, #48122, .T. ) ;
#50809 = ORIENTED_EDGE ( 'NONE', *, *, #16917, .F. ) ;
#50810 = DIRECTION ( 'NONE',  ( -4.299999999999999979E-14, 1.000000000000000000, -4.400000000000000367E-29 ) ) ;
#50811 = EDGE_CURVE ( 'NONE', #73425, #76987, #52140, .T. ) ;
#50812 = FACE_OUTER_BOUND ( 'NONE', #43416, .T. ) ;
#50813 = EDGE_LOOP ( 'NONE', ( #62660, #34171, #30146, #79045, #69754, #44127 ) ) ;
#50814 = AXIS2_PLACEMENT_3D ( 'NONE', #66335, #39079, #81350 ) ;
#50815 = CARTESIAN_POINT ( 'NONE',  ( 180.2121375201596152, -29.73316016638949577, 313.9678068554149490 ) ) ;
#50816 = CARTESIAN_POINT ( 'NONE',  ( 113.9764273654521674, -32.38405892540742315, 32.09094751244895605 ) ) ;
#50817 = EDGE_CURVE ( 'NONE', #40235, #40317, #78116, .T. ) ;
#50818 = DIRECTION ( 'NONE',  ( -0.7071067811865671127, -0.7071067811865279218, -7.071067811865664660E-16 ) ) ;
#50819 = EDGE_CURVE ( 'NONE', #53871, #13694, #41680, .T. ) ;
#50820 = CARTESIAN_POINT ( 'NONE',  ( 188.5667039024483529, -48.82844715993431350, 293.2178068554150059 ) ) ;
#50821 = CARTESIAN_POINT ( 'NONE',  ( 116.7950807104413684, -39.38798874826055396, 194.6147885282144614 ) ) ;
#50822 = EDGE_LOOP ( 'NONE', ( #1476, #87264, #9923, #40008 ) ) ;
#50823 = FACE_OUTER_BOUND ( 'NONE', #15564, .T. ) ;
#50824 = CARTESIAN_POINT ( 'NONE',  ( 72.96458098368650269, 127.0000000000000000, 72.96458098368729850 ) ) ;
#50825 = ORIENTED_EDGE ( 'NONE', *, *, #33334, .T. ) ;
#50826 = CARTESIAN_POINT ( 'NONE',  ( 107.8683683300076837, -26.33502505738635691, 70.01562527591099183 ) ) ;
#50827 = ORIENTED_EDGE ( 'NONE', *, *, #42308, .T. ) ;
#50828 = CARTESIAN_POINT ( 'NONE',  ( 98.88061221520823096, -34.29066745521690507, 30.51813411379100671 ) ) ;
#50829 = ADVANCED_FACE ( 'NONE', ( #15879 ), #3138, .T. ) ;
#50830 = AXIS2_PLACEMENT_3D ( 'NONE', #79625, #64636, #73224 ) ;
#50831 = DIRECTION ( 'NONE',  ( -1.000000000000000000, -1.000000000000000078E-15, 0.000000000000000000 ) ) ;
#50832 = CARTESIAN_POINT ( 'NONE',  ( 104.4962338114797262, -45.76661171243296877, 63.79967854399193072 ) ) ;
#50833 = DIRECTION ( 'NONE',  ( 0.000000000000000000, 0.000000000000000000, -1.000000000000000000 ) ) ;
#50834 = DIRECTION ( 'NONE',  ( -0.7071067811865487940, 0.000000000000000000, 0.7071067811865463515 ) ) ;
#50835 = CARTESIAN_POINT ( 'NONE',  ( 37.03715912545427358, -48.62818131006112310, 300.4678068554150059 ) ) ;
#50836 = CARTESIAN_POINT ( 'NONE',  ( 115.0881438103696155, -30.00293675228997614, 265.3813395616251682 ) ) ;
#50837 = VECTOR ( 'NONE', #75007, 1000.000000000000000 ) ;
#50838 = CARTESIAN_POINT ( 'NONE',  ( 226.4410000000000025, 65.43750000000000000, -2.032000000000000028 ) ) ;
#50839 = ORIENTED_EDGE ( 'NONE', *, *, #23192, .F. ) ;
#50840 = LINE ( 'NONE', #65797, #66128 ) ;
#50841 = ORIENTED_EDGE ( 'NONE', *, *, #81037, .T. ) ;
#50842 = CARTESIAN_POINT ( 'NONE',  ( 108.0108636065302932, -26.30228954677034992, 151.0041967044829505 ) ) ;
#50843 = CARTESIAN_POINT ( 'NONE',  ( 125.1260334383333657, 49.36275571881125046, -37.26066279344849619 ) ) ;
#50844 = ORIENTED_EDGE ( 'NONE', *, *, #8272, .F. ) ;
#50845 = ORIENTED_EDGE ( 'NONE', *, *, #42488, .T. ) ;
#50846 = VERTEX_POINT ( 'NONE', #17218 ) ;
#50847 = CARTESIAN_POINT ( 'NONE',  ( 117.0718954882821947, -35.46248237174801687, 123.9272919413459562 ) ) ;
#50848 = CARTESIAN_POINT ( 'NONE',  ( 41.56670390244804025, -42.82844715994103524, 300.4678068554150059 ) ) ;
#50849 = CARTESIAN_POINT ( 'NONE',  ( 101.7545977962314225, -44.98157700518534341, 222.1213395616259731 ) ) ;
#50850 = DIRECTION ( 'NONE',  ( -0.9254794337955620787, -0.3787978585227822492, 0.000000000000000000 ) ) ;
#50851 = DIRECTION ( 'NONE',  ( 1.000000000000000078E-15, 9.367723249499513438E-31, -1.000000000000000000 ) ) ;
#50852 = CARTESIAN_POINT ( 'NONE',  ( -33.98325472291465132, 104.3431970271541900, 3.174999999999764899 ) ) ;
#50853 = CARTESIAN_POINT ( 'NONE',  ( 104.6489182489307552, -47.51505607846939938, 23.38895860924494841 ) ) ;
#50855 = EDGE_CURVE ( 'NONE', #19111, #84744, #10829, .T. ) ;
#50854 = FACE_OUTER_BOUND ( 'NONE', #81041, .T. ) ;
#50856 = VERTEX_POINT ( 'NONE', #43557 ) ;
#50857 = CARTESIAN_POINT ( 'NONE',  ( 103.4067605119645776, -27.42305663254103010, 171.3746256237512569 ) ) ;
#50858 = PRESENTATION_LAYER_ASSIGNMENT (  '', '', ( #24725 ) ) ;
#50859 = EDGE_CURVE ( 'NONE', #24431, #68999, #6712, .T. ) ;
#50860 = DIRECTION ( 'NONE',  ( 1.000000000000000000, -3.885780586188044357E-13, 0.000000000000000000 ) ) ;
#50861 = ORIENTED_EDGE ( 'NONE', *, *, #52896, .F. ) ;
#50862 = DIRECTION ( 'NONE',  ( -1.000000000000000000, 0.000000000000000000, 0.000000000000000000 ) ) ;
#50863 = DIRECTION ( 'NONE',  ( 0.000000000000000000, 0.000000000000000000, -1.000000000000000000 ) ) ;
#50864 = CARTESIAN_POINT ( 'NONE',  ( 103.7301789885933658, -26.21598454391059363, 205.3089586092439731 ) ) ;
#50865 = FACE_OUTER_BOUND ( 'NONE', #24819, .T. ) ;
#50866 = FACE_BOUND ( 'NONE', #11149, .T. ) ;
#50867 = DIRECTION ( 'NONE',  ( 7.340987889507870014E-14, 0.000000000000000000, 1.000000000000000000 ) ) ;
#50868 = CARTESIAN_POINT ( 'NONE',  ( 116.0578256703656308, -35.64850657512946697, 238.3562293518859576 ) ) ;
#50870 = CARTESIAN_POINT ( 'NONE',  ( 110.7866772467784955, -46.44483816919306207, 58.86705384733998159 ) ) ;
#50869 = DIRECTION ( 'NONE',  ( 1.000000000000000000, 0.000000000000000000, -2.761895400282000234E-15 ) ) ;
#50871 = CARTESIAN_POINT ( 'NONE',  ( 123.1260477991215367, 73.24606306481838658, 43.41488809734197929 ) ) ;
#50872 = CARTESIAN_POINT ( 'NONE',  ( 108.5441999379606983, -26.36493947475176114, 104.9641967044819779 ) ) ;
#50873 = EDGE_LOOP ( 'NONE', ( #29960, #1206 ) ) ;
#50874 = CARTESIAN_POINT ( 'NONE',  ( 131.6875538713323408, -20.11069332324015235, 7.213126773492521515 ) ) ;
#50875 = ORIENTED_EDGE ( 'NONE', *, *, #26937, .T. ) ;
#50876 = AXIS2_PLACEMENT_3D ( 'NONE', #56470, #22427, #43287 ) ;
#50877 = CARTESIAN_POINT ( 'NONE',  ( 134.0664832912739826, -21.47944715994100306, 1.625625275910997480 ) ) ;
#50878 = CARTESIAN_POINT ( 'NONE',  ( 105.0465253178684719, -26.92297229278132775, 276.2381595649878818 ) ) ;
#50879 = ORIENTED_EDGE ( 'NONE', *, *, #61906, .T. ) ;
#50880 = DIRECTION ( 'NONE',  ( 1.000000000000000000, 4.299999999999999979E-14, 1.000000000000000078E-15 ) ) ;
#50881 = ORIENTED_EDGE ( 'NONE', *, *, #5381, .F. ) ;
#50882 = DIRECTION ( 'NONE',  ( 0.9130365726098600421, 0.000000000000000000, 0.4078776986755216494 ) ) ;
#50883 = CARTESIAN_POINT ( 'NONE',  ( 97.81168895331838087, -40.51742574516882200, 287.6356252759109680 ) ) ;
#50884 = VECTOR ( 'NONE', #15201, 1000.000000000000000 ) ;
#50885 = DIRECTION ( 'NONE',  ( 0.000000000000000000, 0.000000000000000000, 1.000000000000000000 ) ) ;
#50886 = ORIENTED_EDGE ( 'NONE', *, *, #61878, .T. ) ;
#50887 = CARTESIAN_POINT ( 'NONE',  ( 101.6667450491003706, -27.05792876557581650, 105.4937205140069665 ) ) ;
#50888 =( NAMED_UNIT ( * ) SI_UNIT ( $, .STERADIAN. ) SOLID_ANGLE_UNIT ( ) );
#50889 = LINE ( 'NONE', #36382, #89891 ) ;
#50890 = FACE_OUTER_BOUND ( 'NONE', #3977, .T. ) ;
#50891 = DIRECTION ( 'NONE',  ( 0.000000000000000000, -1.000000000000000000, 0.000000000000000000 ) ) ;
#50892 = ORIENTED_EDGE ( 'NONE', *, *, #35417, .T. ) ;
#50893 = CARTESIAN_POINT ( 'NONE',  ( 0.000000000000000000, 2.031999999999865025, 0.000000000000000000 ) ) ;
#50894 = CARTESIAN_POINT ( 'NONE',  ( 73.06648329127401098, -46.72944715994106701, 14.67562527591093513 ) ) ;
#50895 = DIRECTION ( 'NONE',  ( 0.000000000000000000, 0.000000000000000000, -1.000000000000000000 ) ) ;
#50896 = VECTOR ( 'NONE', #86215, 1000.000000000000000 ) ;
#50898 = DIRECTION ( 'NONE',  ( 0.000000000000000000, 1.000000000000000000, 0.000000000000000000 ) ) ;
#50897 = DIRECTION ( 'NONE',  ( 3.491483361109385222E-15, 0.000000000000000000, -1.000000000000000000 ) ) ;
#50899 = CARTESIAN_POINT ( 'NONE',  ( 115.8254259877983827, -31.73000318220183047, 179.2397932879499649 ) ) ;
#50900 = ORIENTED_EDGE ( 'NONE', *, *, #5793, .T. ) ;
#50901 = EDGE_CURVE ( 'NONE', #4177, #25538, #30103, .T. ) ;
#50902 = DIRECTION ( 'NONE',  ( 0.000000000000000000, 0.000000000000000000, 1.000000000000000000 ) ) ;
#50903 = ADVANCED_FACE ( 'NONE', ( #73053 ), #84931, .F. ) ;
#50904 = CARTESIAN_POINT ( 'NONE',  ( 98.64540312569894809, -41.76920806142280185, 157.7556252759109725 ) ) ;
#50905 = VECTOR ( 'NONE', #5738, 1000.000000000000000 ) ;
#50907 = ORIENTED_EDGE ( 'NONE', *, *, #49984, .F. ) ;
#50906 = DIRECTION ( 'NONE',  ( -1.000000000000000078E-15, 1.000000000000000000, 0.000000000000000000 ) ) ;
#50908 = EDGE_CURVE ( 'NONE', #42989, #78177, #2696, .T. ) ;
#50909 = CARTESIAN_POINT ( 'NONE',  ( 116.1300133678978170, -31.69047823903422412, 25.24229194257693365 ) ) ;
#50910 = CARTESIAN_POINT ( 'NONE',  ( 107.0667039024479834, -48.82844715994099971, 160.9178068554150229 ) ) ;
#50911 = CARTESIAN_POINT ( 'NONE',  ( 127.0667052882549797, -78.66107132697005966, 55.21780685541800437 ) ) ;
#50912 = CARTESIAN_POINT ( 'NONE',  ( 112.0636370890131985, -45.48966441153708473, 12.99003379025321614 ) ) ;
#50913 = AXIS2_PLACEMENT_3D ( 'NONE', #42144, #9434, #42583 ) ;
#50914 = EDGE_CURVE ( 'NONE', #3056, #76987, #36765, .T. ) ;
#50915 = DIRECTION ( 'NONE',  ( 1.000000000000000000, 4.163336342344333240E-14, 0.000000000000000000 ) ) ;
#50916 = CARTESIAN_POINT ( 'NONE',  ( 116.3159835831962852, -41.41832011455028351, 248.4651490854349731 ) ) ;
#50917 = ORIENTED_EDGE ( 'NONE', *, *, #35217, .T. ) ;
#50918 = ORIENTED_EDGE ( 'NONE', *, *, #64811, .F. ) ;
#50919 = CARTESIAN_POINT ( 'NONE',  ( 97.70553735687687436, -35.92370728225471055, 182.6777737820879679 ) ) ;
#50920 = EDGE_CURVE ( 'NONE', #56383, #78468, #64006, .T. ) ;
#50921 = CARTESIAN_POINT ( 'NONE',  ( -12.70000000000000107, 82.54999999999999716, 97.46299999999996544 ) ) ;
#50922 = CARTESIAN_POINT ( 'NONE',  ( 111.9552019894765493, -28.70592206014574543, 46.06063092494500211 ) ) ;
#50923 = CARTESIAN_POINT ( 'NONE',  ( -93.77212533081346635, 95.08644067748863904, 90.83954799657482226 ) ) ;
#50924 = EDGE_CURVE ( 'NONE', #87762, #82436, #33514, .T. ) ;
#50925 = CARTESIAN_POINT ( 'NONE',  ( 172.5667039024478129, -36.32844715993500273, 300.4678068554149490 ) ) ;
#50926 = DIRECTION ( 'NONE',  ( 1.000000000000000000, 0.000000000000000000, 0.000000000000000000 ) ) ;
#50928 = ORIENTED_EDGE ( 'NONE', *, *, #53404, .T. ) ;
#50927 = AXIS2_PLACEMENT_3D ( 'NONE', #55000, #60948, #82317 ) ;
#50929 = DIRECTION ( 'NONE',  ( 3.999999999999999995E-14, -1.000000000000000000, 4.100000000000000342E-29 ) ) ;
#50930 = CARTESIAN_POINT ( 'NONE',  ( 194.0667039024473297, -24.92844715993408045, 300.4678068554149490 ) ) ;
#50931 = CARTESIAN_POINT ( 'NONE',  ( 100.8614382317054776, -45.12360235833661903, 257.0699109901967745 ) ) ;
#50932 = LINE ( 'NONE', #24135, #76487 ) ;
#50933 = EDGE_LOOP ( 'NONE', ( #34410, #86768, #33853, #13860, #36331 ) ) ;
#50934 = ORIENTED_EDGE ( 'NONE', *, *, #16879, .T. ) ;
#50935 = EDGE_CURVE ( 'NONE', #62791, #23038, #73958, .T. ) ;
#50936 = DIRECTION ( 'NONE',  ( 1.000000000000000078E-15, -1.000000000000000083E-30, -1.000000000000000000 ) ) ;
#50937 = CARTESIAN_POINT ( 'NONE',  ( 152.0371591254585155, -47.82818131005588214, 193.9678068554149775 ) ) ;
#50938 = CARTESIAN_POINT ( 'NONE',  ( 73.06648329127396835, -8.729447159941065237, 14.67562527591093513 ) ) ;
#50939 = FACE_BOUND ( 'NONE', #61657, .T. ) ;
#50940 = VECTOR ( 'NONE', #79607, 1000.000000000000114 ) ;
#50941 = CARTESIAN_POINT ( 'NONE',  ( 104.7983354005985888, -46.84845355258768507, 23.38895860924395009 ) ) ;
#50942 = CARTESIAN_POINT ( 'NONE',  ( 8.316536451391945306, 73.07542579002461025, 118.0638868015453795 ) ) ;
#50943 = ORIENTED_EDGE ( 'NONE', *, *, #21826, .F. ) ;
#50944 = CIRCLE ( 'NONE', #18981, 3.500000000000003109 ) ;
#50945 = CARTESIAN_POINT ( 'NONE',  ( 117.9699911065184637, -41.49648292930365301, 54.49848241876792088 ) ) ;
#50946 = LINE ( 'NONE', #17333, #88898 ) ;
#50947 = CARTESIAN_POINT ( 'NONE',  ( 99.38138666193238180, -29.68485204926252763, 275.7356252759109907 ) ) ;
#50948 = ORIENTED_EDGE ( 'NONE', *, *, #81938, .F. ) ;
#50949 = CARTESIAN_POINT ( 'NONE',  ( 82.68053975348408358, -17.85322261661534426, 2.908039740960796316 ) ) ;
#50950 = FACE_OUTER_BOUND ( 'NONE', #38431, .T. ) ;
#50951 = DIRECTION ( 'NONE',  ( -1.000000000000000078E-15, 1.000000000000000083E-30, 1.000000000000000000 ) ) ;
#50952 = CARTESIAN_POINT ( 'NONE',  ( 115.1210532203963766, -38.21490719095142197, 86.49951894101998562 ) ) ;
#50953 = CARTESIAN_POINT ( 'NONE',  ( 117.2487272683742532, -41.08916198262414099, 209.5165776568640013 ) ) ;
#50954 = AXIS2_PLACEMENT_3D ( 'NONE', #23907, #16639, #50244 ) ;
#50955 = DIRECTION ( 'NONE',  ( 0.000000000000000000, 0.000000000000000000, -1.000000000000000000 ) ) ;
#50956 = ORIENTED_EDGE ( 'NONE', *, *, #57558, .F. ) ;
#50957 = EDGE_CURVE ( 'NONE', #78504, #49604, #60489, .T. ) ;
#50958 = FACE_OUTER_BOUND ( 'NONE', #71498, .T. ) ;
#50959 = ORIENTED_EDGE ( 'NONE', *, *, #20900, .T. ) ;
#50961 = ORIENTED_EDGE ( 'NONE', *, *, #42183, .F. ) ;
#50960 = AXIS2_PLACEMENT_3D ( 'NONE', #49759, #70675, #76592 ) ;
#50962 = DIRECTION ( 'NONE',  ( 0.000000000000000000, 0.000000000000000000, -1.000000000000000000 ) ) ;
#50963 = ORIENTED_EDGE ( 'NONE', *, *, #63384, .T. ) ;
#50964 = ORIENTED_EDGE ( 'NONE', *, *, #61362, .F. ) ;
#50965 = CARTESIAN_POINT ( 'NONE',  ( 193.0374249753377001, -23.42844715993431848, 129.9678068554150343 ) ) ;
#50966 = CARTESIAN_POINT ( 'NONE',  ( 112.6855112425771210, -28.39944475707905625, 40.60397405478997968 ) ) ;
#50967 = CARTESIAN_POINT ( 'NONE',  ( 100.3264543382982907, -29.74069638407027938, 115.1095626852199558 ) ) ;
#50968 = AXIS2_PLACEMENT_3D ( 'NONE', #4959, #66272, #59007 ) ;
#50969 = CARTESIAN_POINT ( 'NONE',  ( 96.51457183773001702, -40.09881715592517537, 281.5603871806727625 ) ) ;
#50970 = CARTESIAN_POINT ( 'NONE',  ( -479.3614999999999782, 7.143750000000339995, 6.988054014476269948 ) ) ;
#50971 = VECTOR ( 'NONE', #71124, 1000.000000000000000 ) ;
#50972 = ORIENTED_EDGE ( 'NONE', *, *, #983, .T. ) ;
#50973 = EDGE_CURVE ( 'NONE', #8752, #4393, #87590, .T. ) ;
#50974 = CARTESIAN_POINT ( 'NONE',  ( 113.5732777703083229, -29.05103677887047198, 135.5174360739645181 ) ) ;
#50975 = EDGE_LOOP ( 'NONE', ( #37763, #44868, #82279, #40110 ) ) ;
#50976 = DIRECTION ( 'NONE',  ( 0.000000000000000000, 1.000000000000000000, 0.000000000000000000 ) ) ;
#50977 = DIRECTION ( 'NONE',  ( 0.000000000000000000, 0.000000000000000000, -1.000000000000000000 ) ) ;
#50978 = DIRECTION ( 'NONE',  ( 1.000000000000000000, 0.000000000000000000, 0.000000000000000000 ) ) ;
#50979 = EDGE_CURVE ( 'NONE', #48918, #66495, #75305, .T. ) ;
#50980 = FACE_OUTER_BOUND ( 'NONE', #88040, .T. ) ;
#50981 = ORIENTED_EDGE ( 'NONE', *, *, #10689, .F. ) ;
#50982 = CARTESIAN_POINT ( 'NONE',  ( 114.4151681834755294, -27.43228005255051016, 274.5441967044824878 ) ) ;
#50983 = CARTESIAN_POINT ( 'NONE',  ( 101.5861822943782755, -47.29253114347246623, 13.19562527591094891 ) ) ;
#50984 = PRESENTATION_STYLE_ASSIGNMENT (( #44605 ) ) ;
#50985 = CARTESIAN_POINT ( 'NONE',  ( 19.56648329127400032, -18.82844715994099971, -5.074374724088000832 ) ) ;
#50987 = CARTESIAN_POINT ( 'NONE',  ( 69.02879735949464646, -138.9723707447056142, 246.9664177707386159 ) ) ;
#50986 = CARTESIAN_POINT ( 'NONE',  ( 173.9900000000000091, 36.86249999999999716, -53.61543552338530105 ) ) ;
#50988 = CARTESIAN_POINT ( 'NONE',  ( 213.4642805167760002, 52.73749999999999716, -44.45000000000000284 ) ) ;
#50989 = PLANE ( 'NONE',  #71547 ) ;
#50990 = CARTESIAN_POINT ( 'NONE',  ( 131.4143329470395827, -37.45719076514804868, 6.889371645759285734 ) ) ;
#50991 = CIRCLE ( 'NONE', #7497, 9.999999999999994671 ) ;
#50992 = LINE ( 'NONE', #29665, #22792 ) ;
#50993 = DIRECTION ( 'NONE',  ( -0.6544127834855474335, -0.2678505344604094618, 0.7071067811865270336 ) ) ;
#50994 = DIRECTION ( 'NONE',  ( 4.299999999999999979E-14, -1.000000000000000000, 0.000000000000000000 ) ) ;
#50995 = CARTESIAN_POINT ( 'NONE',  ( 52.99265158129170317, 95.25000000000000000, 346.9005000000000223 ) ) ;
#50996 = CARTESIAN_POINT ( 'NONE',  ( 115.6735817710496264, -30.74561775548394849, 279.3099109901964994 ) ) ;
#50997 = CARTESIAN_POINT ( 'NONE',  ( 117.0170930581839457, -33.62013007832896960, 170.0670538473399631 ) ) ;
#50998 = CARTESIAN_POINT ( 'NONE',  ( 116.6217178149748008, -42.37701578139068204, 279.4137205140061724 ) ) ;
#50999 = CIRCLE ( 'NONE', #11849, 2.030000000001310312 ) ;
#51001 = CARTESIAN_POINT ( 'NONE',  ( -450.8499999999999659, 53.97500000000000142, -2.412999999999919876 ) ) ;
#51000 = CARTESIAN_POINT ( 'NONE',  ( 152.0371591254585724, -47.82818131005588214, 129.9678068554149775 ) ) ;
#51002 = CARTESIAN_POINT ( 'NONE',  ( 82.54618223951568723, -35.53884010535914229, 2.747932095373032180 ) ) ;
#51003 = CIRCLE ( 'NONE', #58212, 0.4999999999999989453 ) ;
#51004 = ORIENTED_EDGE ( 'NONE', *, *, #56184, .T. ) ;
#51005 = ADVANCED_FACE ( 'NONE', ( #47122 ), #81245, .T. ) ;
#51006 = CARTESIAN_POINT ( 'NONE',  ( 41.56648329127399677, 0.2215528400590013880, 198.9256252759119832 ) ) ;
#51007 = EDGE_LOOP ( 'NONE', ( #27015, #7938, #76531, #17795 ) ) ;
#51008 = EDGE_CURVE ( 'NONE', #76709, #72100, #13083, .T. ) ;
#51009 = CARTESIAN_POINT ( 'NONE',  ( 99.23822674327652749, -42.59304969680523101, 62.83848241876793850 ) ) ;
#51011 = VERTEX_POINT ( 'NONE', #74857 ) ;
#51010 = FACE_OUTER_BOUND ( 'NONE', #36990, .T. ) ;
#51012 = CARTESIAN_POINT ( 'NONE',  ( 116.7948932105152835, -39.38865681179672862, 49.61472410800634947 ) ) ;
#51013 = EDGE_CURVE ( 'NONE', #41648, #73742, #5826, .T. ) ;
#51014 = CARTESIAN_POINT ( 'NONE',  ( 99.30484619187392070, -29.80227926343066613, 186.7470538473389752 ) ) ;
#51015 = DIRECTION ( 'NONE',  ( -1.000000000000000000, -4.299999999999999979E-14, -1.000000000000000078E-15 ) ) ;
#51016 = B_SPLINE_CURVE_WITH_KNOTS ( 'NONE', 3,
 ( #49182, #70095, #42366, #35563, #49633, #29218, #77359, #56905, #14244, #16041, #64186, #1960, #42813, #29656, #28297, #599, #43718, #70552, #57348, #85089, #41920, #69651, #7420, #55989, #82698, #48572, #82250, #5487, #74965, #61322, #47686, #55832, #62223, #9, #60880, #33182, #14080, #54933, #81795, #27709, #49021, #75421, #75861, #76756, #13634, #19548, #68155, #89044, #42219, #69047, #83141, #20458, #14541, #48128, #41318, #13195, #20899, #21347, #68607, #76307, #55386, #69499, #6814, #34517, #41765 ),
 .UNSPECIFIED., .F., .F.,
 ( 4, 2, 2, 2, 1, 1, 1, 2, 2, 2, 2, 1, 1, 1, 1, 1, 2, 2, 2, 2, 2, 2, 2, 2, 2, 1, 1, 1, 1, 2, 2, 2, 2, 1, 1, 1, 2, 2, 2, 4 ),
 ( 0.000000000000000000, 0.1249999999995733135, 0.1874999999993589295, 0.2187499999992517374, 0.2343749999991982247, 0.2421874999991724120, 0.2460937499991595057, 0.2480468749991530386, 0.2499999999991465716, 0.3124999999989560573, 0.3437499999988598010, 0.3593749999988124499, 0.3671874999987889132, 0.3710937499987771448, 0.3730468749987704835, 0.3740234374987679300, 0.3745117187487666532, 0.3749999999987653210, 0.4374999999987978505, 0.4687499999988149479, 0.4843749999988227195, 0.4999999999988304911, 0.5624999999988645749, 0.5937499999988823385, 0.6093749999988912203, 0.6171874999988957722, 0.6210937499988979926, 0.6230468749988992139, 0.6240234374989007682, 0.6245117187489016564, 0.6249999999989025445, 0.6874999999990687449, 0.7187499999991523447, 0.7343749999991942001, 0.7421874999992156274, 0.7460937499992262856, 0.7480468749992316146, 0.7499999999992368327, 0.8749999999996184163, 1.000000000000000000 ),
 .UNSPECIFIED. ) ;
#51017 = CARTESIAN_POINT ( 'NONE',  ( 6.938893903907229955E-15, 50.79999999999999716, 210.4643999999999835 ) ) ;
#51018 = CARTESIAN_POINT ( 'NONE',  ( 94.12733899296569007, -42.07533762155323842, 290.1356252759106837 ) ) ;
#51019 = DIRECTION ( 'NONE',  ( 0.000000000000000000, 0.000000000000000000, 1.000000000000000000 ) ) ;
#51020 = AXIS2_PLACEMENT_3D ( 'NONE', #58074, #66216, #85366 ) ;
#51021 = DIRECTION ( 'NONE',  ( 0.000000000000000000, 0.000000000000000000, -1.000000000000000000 ) ) ;
#51022 = EDGE_CURVE ( 'NONE', #1345, #81899, #39434, .T. ) ;
#51023 = CARTESIAN_POINT ( 'NONE',  ( 113.8179087694832958, -44.13528601191151068, 98.16463148459392585 ) ) ;
#51024 = CARTESIAN_POINT ( 'NONE',  ( 103.6907823165633005, -45.90921117331532741, 142.2956252759109645 ) ) ;
#51025 = ORIENTED_EDGE ( 'NONE', *, *, #68817, .F. ) ;
#51026 = EDGE_LOOP ( 'NONE', ( #89587, #33201, #24114, #77116 ) ) ;
#51027 = VECTOR ( 'NONE', #41270, 1000.000000000000000 ) ;
#51028 = CARTESIAN_POINT ( 'NONE',  ( 99.62013013265574557, -29.94545647671011679, 77.17015473446797102 ) ) ;
#51029 = CIRCLE ( 'NONE', #16421, 13.99999999999999822 ) ;
#51030 = DIRECTION ( 'NONE',  ( -1.000000000000000000, 0.000000000000000000, 6.982966722218760189E-15 ) ) ;
#51032 = LINE ( 'NONE', #78770, #25964 ) ;
#51031 = CARTESIAN_POINT ( 'NONE',  ( 114.9950743857440756, -30.04541929558971702, 220.3718157521009573 ) ) ;
#51033 = PLANE ( 'NONE',  #59434 ) ;
#51034 = CARTESIAN_POINT ( 'NONE',  ( 97.33783612330317681, -34.07108296596891250, 112.1152844433803750 ) ) ;
#51035 = ADVANCED_FACE ( 'NONE', ( #54371 ), #46679, .T. ) ;
#51036 = AXIS2_PLACEMENT_3D ( 'NONE', #7202, #6300, #5868 ) ;
#51037 = DIRECTION ( 'NONE',  ( 0.000000000000000000, 0.000000000000000000, 1.000000000000000000 ) ) ;
#51038 = CARTESIAN_POINT ( 'NONE',  ( -7.199374239792870816E-13, 127.0000000000000000, 98.14560000000000173 ) ) ;
#51039 = CARTESIAN_POINT ( 'NONE',  ( 7.690721451477779524, 72.53503295708138410, 118.3083018788591971 ) ) ;
#51040 = CARTESIAN_POINT ( 'NONE',  ( 95.33621695423326514, -38.27597901479985865, 151.4299109901969871 ) ) ;
#51041 = ORIENTED_EDGE ( 'NONE', *, *, #26812, .T. ) ;
#51042 = CIRCLE ( 'NONE', #29341, 4.762500000000002842 ) ;
#51043 = VERTEX_POINT ( 'NONE', #39868 ) ;
#51044 = CARTESIAN_POINT ( 'NONE',  ( 107.0667039024470739, -140.6784471599409301, 55.21780685541800437 ) ) ;
#51045 = CARTESIAN_POINT ( 'NONE',  ( 77.49614765539782013, -17.75123073099876336, 2.855912073278433994 ) ) ;
#51046 = CARTESIAN_POINT ( 'NONE',  ( 50.97905606905900555, -31.62489322948711035, -5.074374724088000832 ) ) ;
#51047 = CARTESIAN_POINT ( 'NONE',  ( 0.000000000000000000, 12.26999999999999957, 0.000000000000000000 ) ) ;
#51048 = CARTESIAN_POINT ( 'NONE',  ( 113.6383730011278601, -31.09817814777808564, 227.2204713219719565 ) ) ;
#51049 = DIRECTION ( 'NONE',  ( 0.000000000000000000, 0.000000000000000000, -1.000000000000000000 ) ) ;
#51050 = CARTESIAN_POINT ( 'NONE',  ( 96.64414437497798360, -36.48068628021362514, 196.3070538473399438 ) ) ;
#51051 = CARTESIAN_POINT ( 'NONE',  ( 25.56670390244832802, -48.82844715994168183, 254.7178068554150059 ) ) ;
#51052 = VERTEX_POINT ( 'NONE', #67589 ) ;
#51054 = ORIENTED_EDGE ( 'NONE', *, *, #58686, .T. ) ;
#51053 = VERTEX_POINT ( 'NONE', #66689 ) ;
#51055 = CARTESIAN_POINT ( 'NONE',  ( 172.5667039024482960, -42.82844715993499563, 180.4678068554150059 ) ) ;
#51056 = VERTEX_POINT ( 'NONE', #31721 ) ;
#51057 = DIRECTION ( 'NONE',  ( 0.000000000000000000, 0.000000000000000000, 1.000000000000000000 ) ) ;
#51058 = CARTESIAN_POINT ( 'NONE',  ( 29.77381068363742855, -48.62134037875159720, 180.4678068554150911 ) ) ;
#51059 = CARTESIAN_POINT ( 'NONE',  ( 101.0802515965118573, -30.15484820110618358, 282.0958690201827039 ) ) ;
#51060 = CARTESIAN_POINT ( 'NONE',  ( -479.3614999999999782, 10.16305401447645984, 83.34375000000000000 ) ) ;
#51061 = ORIENTED_EDGE ( 'NONE', *, *, #31574, .T. ) ;
#51062 = VECTOR ( 'NONE', #30893, 1000.000000000000000 ) ;
#51063 = ADVANCED_FACE ( 'NONE', ( #5367 ), #59418, .T. ) ;
#51064 = CARTESIAN_POINT ( 'NONE',  ( 114.0818748889228402, -42.19149755589351969, 9.635625275910941312 ) ) ;
#51065 = DIRECTION ( 'NONE',  ( 1.907762142705490052E-15, 7.167082501179359715E-16, -1.000000000000000000 ) ) ;
#51066 = VERTEX_POINT ( 'NONE', #40319 ) ;
#51067 = ORIENTED_EDGE ( 'NONE', *, *, #25945, .F. ) ;
#51068 = CIRCLE ( 'NONE', #9021, 11.49999999999999645 ) ;
#51069 = PLANE ( 'NONE',  #22684 ) ;
#51070 = ORIENTED_EDGE ( 'NONE', *, *, #34478, .F. ) ;
#51071 = ORIENTED_EDGE ( 'NONE', *, *, #68658, .F. ) ;
#51072 = CARTESIAN_POINT ( 'NONE',  ( 116.4921678451845111, -34.41013889705870099, 13.44099125664899219 ) ) ;
#51073 = CARTESIAN_POINT ( 'NONE',  ( 112.4976487814606685, -26.16836495570049337, 169.6984824187679521 ) ) ;
#51074 = CARTESIAN_POINT ( 'NONE',  ( 109.0680860650138442, -47.57644715601883689, 127.7337205140059382 ) ) ;
#51075 = DIRECTION ( 'NONE',  ( -1.000000000000000078E-15, 1.000000000000000083E-30, 1.000000000000000000 ) ) ;
#51076 = CARTESIAN_POINT ( 'NONE',  ( 101.2940058763137330, -26.37990030743140224, 251.4813395616249920 ) ) ;
#51077 = CARTESIAN_POINT ( 'NONE',  ( 1.154229608196380665E-15, 2.269999999999994245, 9.425000000000000711 ) ) ;
#51078 = CARTESIAN_POINT ( 'NONE',  ( 79.84748767001921976, -82.36537145558867223, 249.3055308415380011 ) ) ;
#51079 = CARTESIAN_POINT ( 'NONE',  ( -130.2266331669275985, 73.86195533656248813, 9.272499861615250083 ) ) ;
#51080 = ORIENTED_EDGE ( 'NONE', *, *, #38084, .F. ) ;
#51081 = CIRCLE ( 'NONE', #29321, 7.937500000000000000 ) ;
#51082 = ORIENTED_EDGE ( 'NONE', *, *, #74527, .T. ) ;
#51083 = AXIS2_PLACEMENT_3D ( 'NONE', #15832, #57599, #43960 ) ;
#51084 = EDGE_CURVE ( 'NONE', #60648, #24397, #82318, .T. ) ;
#51085 = CARTESIAN_POINT ( 'NONE',  ( 95.35850850670631473, -38.86301786728916596, 201.4699109901969791 ) ) ;
#51086 = ORIENTED_EDGE ( 'NONE', *, *, #9684, .T. ) ;
#51087 = CARTESIAN_POINT ( 'NONE',  ( 105.7204000585623191, -24.95538135984382677, 160.1670538473389627 ) ) ;
#51088 = CARTESIAN_POINT ( 'NONE',  ( 121.2221484686747317, -94.95109689075241022, -19.26696060647628528 ) ) ;
#51089 = CARTESIAN_POINT ( 'NONE',  ( 136.0678963112995064, -34.84294903901248830, 7.549690073094341258 ) ) ;
#51090 = FACE_BOUND ( 'NONE', #16722, .T. ) ;
#51093 = CARTESIAN_POINT ( 'NONE',  ( 96.54020141486705597, -31.34005042439575561, 241.9499109901969689 ) ) ;
#51092 = DIRECTION ( 'NONE',  ( -0.000000000000000000, -1.000000000000000000, -0.000000000000000000 ) ) ;
#51091 = DIRECTION ( 'NONE',  ( 1.000000000000000000, 4.299999999999999979E-14, 1.000000000000000078E-15 ) ) ;
#51094 = DIRECTION ( 'NONE',  ( 1.000000000000000000, 0.000000000000000000, 0.000000000000000000 ) ) ;
#51095 = CARTESIAN_POINT ( 'NONE',  ( 37.56670390244720892, -48.82844715994099971, 129.9678068554150911 ) ) ;
#51096 = AXIS2_PLACEMENT_3D ( 'NONE', #57016, #28884, #49304 ) ;
#51097 = CARTESIAN_POINT ( 'NONE',  ( 102.0649443859646794, -27.97173592226305416, 271.4895552763892965 ) ) ;
#51098 = CARTESIAN_POINT ( 'NONE',  ( -254.0000000000000000, 104.7749999999999915, 50.79999999999999716 ) ) ;
#51099 = CARTESIAN_POINT ( 'NONE',  ( 101.9936209668059348, -45.44607155354699302, 258.1564586116036253 ) ) ;
#51100 = CARTESIAN_POINT ( 'NONE',  ( 194.0371591254582881, -46.82818131005407736, 249.9678068554149775 ) ) ;
#51102 = ORIENTED_EDGE ( 'NONE', *, *, #8054, .T. ) ;
#51101 = CARTESIAN_POINT ( 'NONE',  ( 112.9776102722344007, -29.11574116196578643, 195.5838068554210167 ) ) ;
#51103 = CARTESIAN_POINT ( 'NONE',  ( 135.2499210002603718, -21.21189388395679742, 8.006199623929127540 ) ) ;
#51104 = CARTESIAN_POINT ( 'NONE',  ( 107.6557532049571932, -47.79055931493532938, 197.6308633711489620 ) ) ;
#51105 = CARTESIAN_POINT ( 'NONE',  ( 118.0020517745808633, -38.33796275862062686, 69.72229194257801055 ) ) ;
#51106 = CARTESIAN_POINT ( 'NONE',  ( 101.1761829863686160, -45.38377220964024161, 193.1013395616249682 ) ) ;
#51107 = LINE ( 'NONE', #43396, #12655 ) ;
#51108 = DIRECTION ( 'NONE',  ( 1.639958061481212836E-42, -4.100000000000000342E-29, -1.000000000000000000 ) ) ;
#51110 = CARTESIAN_POINT ( 'NONE',  ( 116.8019713974398286, -34.34661232220942395, 40.01729125403449672 ) ) ;
#51109 = DIRECTION ( 'NONE',  ( 0.000000000000000000, 1.000000000000000000, 0.000000000000000000 ) ) ;
#51111 = DIRECTION ( 'NONE',  ( 0.000000000000000000, 0.000000000000000000, 1.000000000000000000 ) ) ;
#51112 = CARTESIAN_POINT ( 'NONE',  ( 118.5256205435843526, -36.72944715994100306, 294.6356252759106837 ) ) ;
#51113 = VERTEX_POINT ( 'NONE', #19890 ) ;
#51114 = CARTESIAN_POINT ( 'NONE',  ( 97.33793630998916058, -34.07062831540125813, 66.11592348782718886 ) ) ;
#51115 = ORIENTED_EDGE ( 'NONE', *, *, #19235, .F. ) ;
#51116 = EDGE_LOOP ( 'NONE', ( #44563, #83400, #84440, #51263, #32731 ) ) ;
#51117 = EDGE_CURVE ( 'NONE', #29858, #35560, #78111, .T. ) ;
#51118 = CARTESIAN_POINT ( 'NONE',  ( 104.0317209996959065, -45.26190801010356779, 101.7390864947439724 ) ) ;
#51120 = VERTEX_POINT ( 'NONE', #55276 ) ;
#51119 = CARTESIAN_POINT ( 'NONE',  ( 130.5667039024479834, -36.72944715994100306, 239.5838068554162987 ) ) ;
#51121 = VECTOR ( 'NONE', #23119, 1000.000000000000114 ) ;
#51122 = EDGE_CURVE ( 'NONE', #4991, #60356, #7609, .T. ) ;
#51123 = CARTESIAN_POINT ( 'NONE',  ( 117.3173117416416744, -32.65705981835812111, 95.13943479972097350 ) ) ;
#51124 = PLANE ( 'NONE',  #13461 ) ;
#51125 = EDGE_CURVE ( 'NONE', #64292, #46374, #41207, .T. ) ;
#51126 = CARTESIAN_POINT ( 'NONE',  ( 97.81169128372820865, -40.51741339292117772, 177.6357569005977268 ) ) ;
#51127 = CARTESIAN_POINT ( 'NONE',  ( 59.56670390244699576, -67.87844715994098976, 85.21780685541799016 ) ) ;
#51128 = ADVANCED_FACE ( 'NONE', ( #13971, #83462 ), #61650, .F. ) ;
#51129 = CARTESIAN_POINT ( 'NONE',  ( 104.7983354006062058, -46.84845355260645761, 27.38895860924495196 ) ) ;
#51130 = EDGE_LOOP ( 'NONE', ( #35624, #18314, #33718, #87527 ) ) ;
#51131 = ORIENTED_EDGE ( 'NONE', *, *, #33753, .T. ) ;
#51132 = ORIENTED_EDGE ( 'NONE', *, *, #51347, .F. ) ;
#51133 = VECTOR ( 'NONE', #72072, 1000.000000000000114 ) ;
#51134 = CARTESIAN_POINT ( 'NONE',  ( 151.0371591254575492, -24.95799193692592155, 180.4678068554149775 ) ) ;
#51135 = CARTESIAN_POINT ( 'NONE',  ( 106.5667039024470313, -100.3098201933451747, -19.78219314458212708 ) ) ;
#51136 = CARTESIAN_POINT ( 'NONE',  ( 115.0889047244793488, -30.61763668078588907, 115.3439586091690785 ) ) ;
#51137 = DIRECTION ( 'NONE',  ( 1.000000000000000000, 0.000000000000000000, 0.000000000000000000 ) ) ;
#51138 = FACE_BOUND ( 'NONE', #85961, .T. ) ;
#51139 = CARTESIAN_POINT ( 'NONE',  ( 147.0667039024469886, -67.87844715994090450, 222.2178068554179902 ) ) ;
#51140 = EDGE_CURVE ( 'NONE', #76315, #59415, #62562, .T. ) ;
#51141 = CARTESIAN_POINT ( 'NONE',  ( 67.06674172433055503, -67.87844715943892027, 245.5060123894820379 ) ) ;
#51142 = CARTESIAN_POINT ( 'NONE',  ( -5.751998507614636047, 93.87463779977233003, 130.4293086530511232 ) ) ;
#51143 = EDGE_CURVE ( 'NONE', #65875, #35035, #89389, .T. ) ;
#51144 = CARTESIAN_POINT ( 'NONE',  ( 96.94826409162251935, -39.14818769109204055, 56.51276813305394597 ) ) ;
#51146 = VERTEX_POINT ( 'NONE', #54823 ) ;
#51145 = VECTOR ( 'NONE', #39644, 1000.000000000000114 ) ;
#51147 = CARTESIAN_POINT ( 'NONE',  ( 97.81171235735017433, -40.51746255502365557, 257.6350867217079212 ) ) ;
#51148 = CARTESIAN_POINT ( 'NONE',  ( 119.5843592605237120, 52.73749999999999716, -52.38749999999991758 ) ) ;
#51149 = CARTESIAN_POINT ( 'NONE',  ( 111.0233670443594463, -45.12224181339347240, 135.7452332267339443 ) ) ;
#51150 = AXIS2_PLACEMENT_3D ( 'NONE', #79499, #51750, #39023 ) ;
#51151 = CARTESIAN_POINT ( 'NONE',  ( 100.9527330894022299, -28.70853417486769033, 95.59415746019152493 ) ) ;
#51152 = AXIS2_PLACEMENT_3D ( 'NONE', #89663, #6096, #26525 ) ;
#51153 = CARTESIAN_POINT ( 'NONE',  ( 107.0667039024470313, -104.2784471599409528, 249.2178068554179902 ) ) ;
#51154 = EDGE_LOOP ( 'NONE', ( #11135, #68732, #43698, #42327 ) ) ;
#51155 = ORIENTED_EDGE ( 'NONE', *, *, #24471, .T. ) ;
#51156 = CARTESIAN_POINT ( 'NONE',  ( 112.0661856499390012, -45.48824432087039327, 137.9874038074903240 ) ) ;
#51157 = ORIENTED_EDGE ( 'NONE', *, *, #38299, .T. ) ;
#51158 = EDGE_LOOP ( 'NONE', ( #48618, #24517 ) ) ;
#51159 = CARTESIAN_POINT ( 'NONE',  ( 102.7360552222912418, -45.06754756083040547, 163.6149166392309837 ) ) ;
#51160 = CYLINDRICAL_SURFACE ( 'NONE', #30755, 7.937500000000000000 ) ;
#51162 = EDGE_CURVE ( 'NONE', #34428, #53716, #29365, .T. ) ;
#51161 = CARTESIAN_POINT ( 'NONE',  ( 117.0539910656555094, -30.30509957368958496, 140.2813395616249750 ) ) ;
#51163 = DIRECTION ( 'NONE',  ( 1.000000000000000000, 1.000000000000000078E-15, -0.000000000000000000 ) ) ;
#51164 = CARTESIAN_POINT ( 'NONE',  ( 116.3188053082936051, -32.94429434937755019, 19.13562527591095019 ) ) ;
#51165 = ORIENTED_EDGE ( 'NONE', *, *, #7221, .F. ) ;
#51166 = VERTEX_POINT ( 'NONE', #33366 ) ;
#51167 = VERTEX_POINT ( 'NONE', #39720 ) ;
#51168 = EDGE_CURVE ( 'NONE', #39335, #11421, #4415, .T. ) ;
#51169 = CARTESIAN_POINT ( 'NONE',  ( 102.6333607924234883, -43.61639954521550067, 219.9395189410199691 ) ) ;
#51170 = CARTESIAN_POINT ( 'NONE',  ( 101.1283730419716562, -27.37881681735623829, 65.51467289495799662 ) ) ;
#51171 = VERTEX_POINT ( 'NONE', #5676 ) ;
#51172 = CARTESIAN_POINT ( 'NONE',  ( 97.09625384711483775, -33.75906160244644383, 31.09562527591097592 ) ) ;
#51173 = DIRECTION ( 'NONE',  ( 0.7071067811865507924, 0.7071067811865441310, -0.000000000000000000 ) ) ;
#51174 = PLANE ( 'NONE',  #49505 ) ;
#51175 = DIRECTION ( 'NONE',  ( 1.000000000000000078E-15, -1.000000000000000000, 0.000000000000000000 ) ) ;
#51176 = CARTESIAN_POINT ( 'NONE',  ( 114.2533759015650787, -44.28132150547345702, 154.1813395616249807 ) ) ;
#51177 = CARTESIAN_POINT ( 'NONE',  ( 116.3149231129805941, -32.94053081170188335, 174.1356252759109680 ) ) ;
#51178 = EDGE_LOOP ( 'NONE', ( #66371, #42255, #9740, #45448 ) ) ;
#51179 = CARTESIAN_POINT ( 'NONE',  ( 0.000000000000000000, 124.5870000000000033, -25.39999999999999858 ) ) ;
#51180 = VERTEX_POINT ( 'NONE', #19297 ) ;
#51181 = CARTESIAN_POINT ( 'NONE',  ( 165.9667039024459996, -28.27351298637401200, -5.074374724088000832 ) ) ;
#51182 = ORIENTED_EDGE ( 'NONE', *, *, #58454, .F. ) ;
#51183 = ORIENTED_EDGE ( 'NONE', *, *, #50721, .T. ) ;
#51184 = CARTESIAN_POINT ( 'NONE',  ( -29.99999999999996092, 172.0000000000000000, 182.8826257785461280 ) ) ;
#51185 = EDGE_CURVE ( 'NONE', #23113, #54222, #74703, .T. ) ;
#51186 = CARTESIAN_POINT ( 'NONE',  ( 115.9861642887573367, -32.12167434585060732, 130.2065129988452270 ) ) ;
#51187 = CARTESIAN_POINT ( 'NONE',  ( 117.2669906530413186, -38.88274231480306042, 63.66133956162494911 ) ) ;
#51188 = CARTESIAN_POINT ( 'NONE',  ( 20.45523698819324565, 62.82274409087659706, 32.14693258707937673 ) ) ;
#51189 = DIRECTION ( 'NONE',  ( 1.000000000000000000, 0.000000000000000000, 0.000000000000000000 ) ) ;
#51190 = CARTESIAN_POINT ( 'NONE',  ( 0.000000000000000000, 125.7300000000000040, 0.000000000000000000 ) ) ;
#51191 = CARTESIAN_POINT ( 'NONE',  ( 106.0550521757682816, -27.00111521709620277, 50.15848241876896907 ) ) ;
#51193 = CARTESIAN_POINT ( 'NONE',  ( 102.9221092647374149, -27.14930527916913050, 151.4013395616249511 ) ) ;
#51192 = CYLINDRICAL_SURFACE ( 'NONE', #2676, 9.999999999999998224 ) ;
#51194 = CARTESIAN_POINT ( 'NONE',  ( 112.1355955708808523, -28.01067529516842214, 59.65679988530178690 ) ) ;
#51195 = DIRECTION ( 'NONE',  ( 0.000000000000000000, 1.000000000000000000, 0.000000000000000000 ) ) ;
#51196 = ORIENTED_EDGE ( 'NONE', *, *, #15010, .T. ) ;
#51197 = PLANE ( 'NONE',  #51264 ) ;
#51198 = FACE_OUTER_BOUND ( 'NONE', #79237, .T. ) ;
#51199 = DIRECTION ( 'NONE',  ( 1.000000000000000000, 0.000000000000000000, 0.000000000000000000 ) ) ;
#51200 = EDGE_CURVE ( 'NONE', #18271, #44789, #26551, .T. ) ;
#51201 = CARTESIAN_POINT ( 'NONE',  ( 107.0664832912739399, -36.72944715994095333, 357.5272416190308604 ) ) ;
#51203 = ORIENTED_EDGE ( 'NONE', *, *, #29367, .F. ) ;
#51202 = CARTESIAN_POINT ( 'NONE',  ( 100.6103855434584631, -26.73206753375993827, 220.5327681330539633 ) ) ;
#51204 = CARTESIAN_POINT ( 'NONE',  ( 97.33774096734804004, -34.07142221982499564, 146.1148210333605562 ) ) ;
#51205 = CARTESIAN_POINT ( 'NONE',  ( 95.27050013873164858, -38.09949539013453546, 232.4184824187679794 ) ) ;
#51206 = CARTESIAN_POINT ( 'NONE',  ( 103.2630468498471856, -47.15688066943211254, 93.28610146638693834 ) ) ;
#51207 = CARTESIAN_POINT ( 'NONE',  ( 83.41622542100820681, 78.46444036551646661, 100.4321520267703249 ) ) ;
#51208 = DIRECTION ( 'NONE',  ( 1.000000000000000000, 0.000000000000000000, 2.108231265501709878E-16 ) ) ;
#51209 = CARTESIAN_POINT ( 'NONE',  ( 116.7948133712559127, -39.38894117706560394, 264.6149338185274473 ) ) ;
#51210 = ORIENTED_EDGE ( 'NONE', *, *, #25793, .T. ) ;
#51211 = AXIS2_PLACEMENT_3D ( 'NONE', #63720, #52183, #17701 ) ;
#51212 = VECTOR ( 'NONE', #36000, 1000.000000000000114 ) ;
#51213 = ORIENTED_EDGE ( 'NONE', *, *, #70242, .T. ) ;
#51214 = VERTEX_POINT ( 'NONE', #12035 ) ;
#51215 = VECTOR ( 'NONE', #31728, 1000.000000000000000 ) ;
#51216 = B_SPLINE_CURVE_WITH_KNOTS ( 'NONE', 3,
 ( #10488, #30492, #85921, #44542, #85027, #45427, #38188, #65885, #3673, #59060, #24566, #23691, #17751, #85480, #50472, #2794, #44094, #36422, #51355, #3236, #9157, #50923, #22797, #78214, #36856, #30930, #58619, #15976, #43656, #9597, #37305, #79100, #65010, #16862, #52673, #73145, #4115, #46320, #46768, #25451, #32710, #88591, #39074, #53117, #74499, #60860, #80889, #4569, #31814 ),
 .UNSPECIFIED., .F., .F.,
 ( 4, 2, 2, 2, 2, 2, 2, 2, 2, 2, 2, 2, 2, 2, 2, 1, 2, 2, 2, 2, 2, 2, 2, 2, 4 ),
 ( 0.01986933033599076748, 0.02111088875730818271, 0.02235244717862559446, 0.02483556402126041798, 0.02607712244257780546, 0.02731868086389519293, 0.02980179770652992971, 0.03228491454916466996, 0.03352647297048201580, 0.03476803139179936164, 0.03725114823443406720, 0.03849270665575145467, 0.03973426507706884214, 0.04221738191970363097, 0.04345894034102103232, 0.04470049876233841979, 0.04594205718365582114, 0.04718361560497322249, 0.04966673244760801131, 0.05090829086892539879, 0.05214984929024277238, 0.05463296613287750569, 0.05587452455419486541, 0.05711608297551221819, 0.05959919981814693762 ),
 .UNSPECIFIED. ) ;
#51217 = EDGE_LOOP ( 'NONE', ( #34746, #59229 ) ) ;
#51218 = CARTESIAN_POINT ( 'NONE',  ( 144.5667039024470171, -90.27844715994091018, 51.21780685541800437 ) ) ;
#51219 = CARTESIAN_POINT ( 'NONE',  ( 109.2119659639152047, -48.38412513495681111, 273.7213395616252569 ) ) ;
#51220 = LINE ( 'NONE', #38059, #70764 ) ;
#51221 = CARTESIAN_POINT ( 'NONE',  ( 131.4050152070336424, -36.03131342368293133, 2.974074870386977931 ) ) ;
#51222 = EDGE_CURVE ( 'NONE', #9402, #89894, #14156, .T. ) ;
#51224 = CARTESIAN_POINT ( 'NONE',  ( 78.43243611888021860, 72.22378176823139029, 88.90442867306012431 ) ) ;
#51223 = DIRECTION ( 'NONE',  ( -0.7071067811865420216, 0.000000000000000000, 0.7071067811865531239 ) ) ;
#51225 = CYLINDRICAL_SURFACE ( 'NONE', #71885, 218.1859999999999786 ) ;
#51226 = CARTESIAN_POINT ( 'NONE',  ( 113.4141308401190287, -30.97102092343966007, 208.8352769709339896 ) ) ;
#51227 = VERTEX_POINT ( 'NONE', #80639 ) ;
#51228 = VERTEX_POINT ( 'NONE', #46071 ) ;
#51229 = ORIENTED_EDGE ( 'NONE', *, *, #66431, .T. ) ;
#51230 = DIRECTION ( 'NONE',  ( -0.000000000000000000, 1.000000000000000000, 0.000000000000000000 ) ) ;
#51231 = VECTOR ( 'NONE', #72697, 1000.000000000000000 ) ;
#51232 = CARTESIAN_POINT ( 'NONE',  ( 111.0152562398575213, -45.91716645315732848, 182.8994882387802932 ) ) ;
#51233 = CARTESIAN_POINT ( 'NONE',  ( 97.54182784564409303, -34.36413255805981493, 272.1327681330532755 ) ) ;
#51234 = DIRECTION ( 'NONE',  ( 0.000000000000000000, -1.000000000000000000, 0.000000000000000000 ) ) ;
#51235 = EDGE_CURVE ( 'NONE', #62232, #77142, #26111, .T. ) ;
#51236 = CIRCLE ( 'NONE', #23717, 154.1697486074984909 ) ;
#51237 = PLANE ( 'NONE',  #89815 ) ;
#51238 = EDGE_CURVE ( 'NONE', #43116, #48706, #32940, .T. ) ;
#51239 = DIRECTION ( 'NONE',  ( 0.000000000000000000, 0.000000000000000000, 1.000000000000000000 ) ) ;
#51240 = ORIENTED_EDGE ( 'NONE', *, *, #44569, .F. ) ;
#51241 = CARTESIAN_POINT ( 'NONE',  ( 78.92334784196830810, -34.22821065591988798, 1.829869330583619558 ) ) ;
#51242 = ORIENTED_EDGE ( 'NONE', *, *, #40558, .F. ) ;
#51243 = DIRECTION ( 'NONE',  ( 0.000000000000000000, -1.000000000000000000, 0.000000000000000000 ) ) ;
#51244 = CARTESIAN_POINT ( 'NONE',  ( 115.1453852183930593, -37.89609606526670404, 26.53094751244894312 ) ) ;
#51245 = VECTOR ( 'NONE', #47581, 1000.000000000000000 ) ;
#51246 = PLANE ( 'NONE',  #43546 ) ;
#51247 = CARTESIAN_POINT ( 'NONE',  ( 131.3179999999999836, 53.97500000000000142, 71.43750000000000000 ) ) ;
#51248 = CARTESIAN_POINT ( 'NONE',  ( 57.56670390244747892, -48.82844715994040286, 134.7178068554150911 ) ) ;
#51249 = EDGE_LOOP ( 'NONE', ( #82877, #69969, #5914, #8990, #35505, #87548, #989 ) ) ;
#51250 = PLANE ( 'NONE',  #26177 ) ;
#51251 = FACE_BOUND ( 'NONE', #72833, .T. ) ;
#51252 = VERTEX_POINT ( 'NONE', #68342 ) ;
#51253 = CARTESIAN_POINT ( 'NONE',  ( 114.3532617768494504, -44.18530993788802874, 73.19276813305397411 ) ) ;
#51254 = ORIENTED_EDGE ( 'NONE', *, *, #71311, .F. ) ;
#51255 = CARTESIAN_POINT ( 'NONE',  ( 104.9561144943094035, -45.03597746244296474, 46.80099125664899162 ) ) ;
#51256 = CARTESIAN_POINT ( 'NONE',  ( 3.174999999999879918, 24.56180297284579694, -33.98325472291465132 ) ) ;
#51257 = CARTESIAN_POINT ( 'NONE',  ( 112.4631721614844651, -29.03839555594388955, 81.00920235351600240 ) ) ;
#51258 = CARTESIAN_POINT ( 'NONE',  ( 117.0606442662038091, -38.08221774826209582, 14.71881810016104275 ) ) ;
#51259 = CARTESIAN_POINT ( 'NONE',  ( 151.0371591254572934, -24.42818131005592974, 300.4678068554149490 ) ) ;
#51260 = CARTESIAN_POINT ( 'NONE',  ( -215.9000000000000057, 101.5999999999999943, -45.33899999999999864 ) ) ;
#51261 = CARTESIAN_POINT ( 'NONE',  ( 105.9861696881796860, -26.33857706295247070, 46.15848241876796720 ) ) ;
#51262 = DIRECTION ( 'NONE',  ( 0.7071067811865101582, 0.7071067811865849873, 0.000000000000000000 ) ) ;
#51263 = ORIENTED_EDGE ( 'NONE', *, *, #14113, .T. ) ;
#51264 = AXIS2_PLACEMENT_3D ( 'NONE', #31657, #29892, #43487 ) ;
#51265 = DIRECTION ( 'NONE',  ( -1.000000000000000000, -8.953411488912552682E-16, 0.000000000000000000 ) ) ;
#51266 = ORIENTED_EDGE ( 'NONE', *, *, #81886, .T. ) ;
#51267 = CARTESIAN_POINT ( 'NONE',  ( 97.75552660847078812, -42.77168409777202385, 142.7965776568629508 ) ) ;
#51268 = DIRECTION ( 'NONE',  ( 1.147230458779309805E-16, 0.000000000000000000, 1.000000000000000000 ) ) ;
#51269 = CIRCLE ( 'NONE', #75930, 5.599999999999994316 ) ;
#51270 = ORIENTED_EDGE ( 'NONE', *, *, #84663, .F. ) ;
#51271 = EDGE_LOOP ( 'NONE', ( #19257, #12575 ) ) ;
#51272 = CYLINDRICAL_SURFACE ( 'NONE', #62330, 13.44999999999999396 ) ;
#51273 = LINE ( 'NONE', #44017, #28948 ) ;
#51274 = CARTESIAN_POINT ( 'NONE',  ( 102.5357197525641766, -45.39752751535337438, 212.1927681330539599 ) ) ;
#51275 = CARTESIAN_POINT ( 'NONE',  ( 69.72411017812960665, 120.6499999999999915, 69.72411017813040246 ) ) ;
#51276 = LINE ( 'NONE', #1373, #62621 ) ;
#51277 = PLANE ( 'NONE',  #80931 ) ;
#51278 = CARTESIAN_POINT ( 'NONE',  ( 96.68599849774213340, -42.44610274171655817, 22.72705384733997391 ) ) ;
#51279 = DIRECTION ( 'NONE',  ( 0.000000000000000000, 0.000000000000000000, 1.000000000000000000 ) ) ;
#51280 = ORIENTED_EDGE ( 'NONE', *, *, #30029, .T. ) ;
#51281 = CARTESIAN_POINT ( 'NONE',  ( 116.0758788059830096, -32.34242916441947813, 170.1871404008558670 ) ) ;
#51282 = FACE_OUTER_BOUND ( 'NONE', #38987, .T. ) ;
#51283 = VERTEX_POINT ( 'NONE', #66989 ) ;
#51284 = CARTESIAN_POINT ( 'NONE',  ( 172.5664832912740110, -9.303447159940999356, 321.0426252759119734 ) ) ;
#51285 = EDGE_CURVE ( 'NONE', #7646, #79779, #6123, .T. ) ;
#51286 = AXIS2_PLACEMENT_3D ( 'NONE', #35812, #63527, #89913 ) ;
#51287 = CARTESIAN_POINT ( 'NONE',  ( 0.000000000000000000, 95.00619999999999266, 0.000000000000000000 ) ) ;
#51288 = CARTESIAN_POINT ( 'NONE',  ( 115.9412561796928429, -30.17946786548967353, 259.3203871806730945 ) ) ;
#51289 = DIRECTION ( 'NONE',  ( -1.000000000000000078E-15, 0.000000000000000000, -1.000000000000000000 ) ) ;
#51290 = EDGE_CURVE ( 'NONE', #80402, #87454, #67886, .T. ) ;
#51291 = FACE_BOUND ( 'NONE', #86047, .T. ) ;
#51292 = CARTESIAN_POINT ( 'NONE',  ( 106.0039306387646860, -11.55185827894094786, 322.0356252759110021 ) ) ;
#51293 = CARTESIAN_POINT ( 'NONE',  ( 99.20650695390740736, -40.14600596985821568, 231.0752769709339418 ) ) ;
#51295 = CARTESIAN_POINT ( 'NONE',  ( 106.5192459994187715, -25.71289806663804711, 41.12800622829193742 ) ) ;
#51294 = CARTESIAN_POINT ( 'NONE',  ( 107.0664832912739399, -36.72944715994095333, 294.6356252759106837 ) ) ;
#51296 = CARTESIAN_POINT ( 'NONE',  ( 111.6857113302616824, 65.94691145059840665, 67.61047547054599249 ) ) ;
#51297 = CARTESIAN_POINT ( 'NONE',  ( 96.59774800590200527, -36.61877842429220209, 111.3184824187679567 ) ) ;
#51298 = ORIENTED_EDGE ( 'NONE', *, *, #62048, .F. ) ;
#51299 = DIRECTION ( 'NONE',  ( 1.000000000000000000, 4.163336342344333240E-14, 0.000000000000000000 ) ) ;
#51300 = ORIENTED_EDGE ( 'NONE', *, *, #2533, .T. ) ;
#51301 = EDGE_CURVE ( 'NONE', #16063, #48612, #89240, .T. ) ;
#51302 = VECTOR ( 'NONE', #67110, 1000.000000000000000 ) ;
#51303 = CARTESIAN_POINT ( 'NONE',  ( 123.0664832912750057, -36.72944715993921960, 9.125625275910985934 ) ) ;
#51304 = CARTESIAN_POINT ( 'NONE',  ( 103.2913588842583721, -27.46939931803447976, 276.3845213361897777 ) ) ;
#51305 = VERTEX_POINT ( 'NONE', #13379 ) ;
#51306 = EDGE_CURVE ( 'NONE', #72479, #52459, #41065, .T. ) ;
#51307 = EDGE_CURVE ( 'NONE', #32868, #62133, #9749, .T. ) ;
#51308 = DIRECTION ( 'NONE',  ( 0.7071067708032375831, 0.0001211784769776684463, -0.7071067811865434649 ) ) ;
#51309 = VERTEX_POINT ( 'NONE', #32911 ) ;
#51310 = DIRECTION ( 'NONE',  ( 1.387778780781444492E-15, 0.000000000000000000, -1.000000000000000000 ) ) ;
#51311 = DIRECTION ( 'NONE',  ( 1.000000000000000000, 4.299999999999999979E-14, 1.000000000000000078E-15 ) ) ;
#51312 = ADVANCED_FACE ( 'NONE', ( #59711 ), #87445, .F. ) ;
#51313 = DIRECTION ( 'NONE',  ( 0.000000000000000000, 1.000000000000000000, 0.000000000000000000 ) ) ;
#51314 = EDGE_CURVE ( 'NONE', #66470, #50313, #28608, .T. ) ;
#51315 = EDGE_LOOP ( 'NONE', ( #36793, #68870, #4328, #9152 ) ) ;
#51316 = CARTESIAN_POINT ( 'NONE',  ( 100.9301527464941444, -28.27416411254235840, 75.57562527591093726 ) ) ;
#51317 = DIRECTION ( 'NONE',  ( 1.000000000000000000, 0.000000000000000000, 0.000000000000000000 ) ) ;
#51318 = EDGE_CURVE ( 'NONE', #67326, #16018, #82883, .T. ) ;
#51319 = CARTESIAN_POINT ( 'NONE',  ( 116.3265979651016409, -32.94445627519164077, 14.13562527591094664 ) ) ;
#51320 = CARTESIAN_POINT ( 'NONE',  ( 50.56670390244699576, -22.48495420874030515, -5.074374724088000832 ) ) ;
#51321 = CARTESIAN_POINT ( 'NONE',  ( 99.04406183884522363, -42.84125761427707602, 141.8439586067010509 ) ) ;
#51322 = VERTEX_POINT ( 'NONE', #1088 ) ;
#51323 = EDGE_CURVE ( 'NONE', #53584, #70167, #24272, .T. ) ;
#51324 = CARTESIAN_POINT ( 'NONE',  ( 83.06670390244806867, -58.72944715994108122, 231.5838068554169524 ) ) ;
#51325 = CARTESIAN_POINT ( 'NONE',  ( 142.0664832912740394, -45.72944715994099596, -5.074374724088994704 ) ) ;
#51326 = ADVANCED_FACE ( 'NONE', ( #83316 ), #76494, .T. ) ;
#51327 = DIRECTION ( 'NONE',  ( 0.000000000000000000, 1.000000000000000000, 0.000000000000000000 ) ) ;
#51329 = DIRECTION ( 'NONE',  ( 0.000000000000000000, 1.000000000000000000, 0.000000000000000000 ) ) ;
#51328 = DIRECTION ( 'NONE',  ( 0.7071067811865460184, 0.000000000000000000, 0.7071067811865487940 ) ) ;
#51330 = DIRECTION ( 'NONE',  ( 6.745093096447288888E-17, 1.000000000000000000, 0.000000000000000000 ) ) ;
#51331 = AXIS2_PLACEMENT_3D ( 'NONE', #81070, #46501, #74237 ) ;
#51332 = ORIENTED_EDGE ( 'NONE', *, *, #43553, .F. ) ;
#51333 = VECTOR ( 'NONE', #21850, 1000.000000000000000 ) ;
#51334 = DIRECTION ( 'NONE',  ( 0.000000000000000000, 0.000000000000000000, 1.000000000000000000 ) ) ;
#51335 = CARTESIAN_POINT ( 'NONE',  ( 116.4500618263485592, -39.48841239489304655, 179.5984824187679294 ) ) ;
#51337 = VERTEX_POINT ( 'NONE', #28800 ) ;
#51336 = DIRECTION ( 'NONE',  ( -0.9068632946707807507, 0.4214249218767881500, -9.028300618466658994E-16 ) ) ;
#51338 = EDGE_CURVE ( 'NONE', #51651, #48080, #19988, .T. ) ;
#51339 = CARTESIAN_POINT ( 'NONE',  ( 105.5226833586260966, -46.38761039419742360, 33.44991099019595282 ) ) ;
#51340 = FACE_OUTER_BOUND ( 'NONE', #36719, .T. ) ;
#51342 = ADVANCED_FACE ( 'NONE', ( #7005 ), #56482, .T. ) ;
#51341 = DIRECTION ( 'NONE',  ( 1.000000000000000000, 0.000000000000000000, 0.000000000000000000 ) ) ;
#51343 = DIRECTION ( 'NONE',  ( -0.7071067811865171526, -0.7071067811865779928, -7.071067811865164719E-16 ) ) ;
#51344 = EDGE_CURVE ( 'NONE', #73928, #69134, #77391, .T. ) ;
#51345 = VERTEX_POINT ( 'NONE', #36052 ) ;
#51346 = CARTESIAN_POINT ( 'NONE',  ( 31.71315051186713418, -31.94127993907761009, 117.4678068554150485 ) ) ;
#51347 = EDGE_CURVE ( 'NONE', #65933, #62770, #41505, .T. ) ;
#51348 = CARTESIAN_POINT ( 'NONE',  ( 109.1965444620390571, -27.18343884754219886, 224.9013395616259459 ) ) ;
#51349 = ORIENTED_EDGE ( 'NONE', *, *, #9694, .T. ) ;
#51350 = ORIENTED_EDGE ( 'NONE', *, *, #20271, .F. ) ;
#51351 = CARTESIAN_POINT ( 'NONE',  ( 108.4337774161041921, -27.97394686652187090, 186.3844404487539634 ) ) ;
#51352 = AXIS2_PLACEMENT_3D ( 'NONE', #21920, #42323, #63236 ) ;
#51353 = DIRECTION ( 'NONE',  ( -0.9834602067153815907, -0.1811243269341220596, 0.000000000000000000 ) ) ;
#51354 = CARTESIAN_POINT ( 'NONE',  ( 114.2978770801668418, -41.85148020179265416, 49.76729759161096922 ) ) ;
#51355 = CARTESIAN_POINT ( 'NONE',  ( -95.94886839522581568, 94.12569442554139698, 88.53717826876649610 ) ) ;
#51356 = VECTOR ( 'NONE', #74781, 1000.000000000000000 ) ;
#51357 = CARTESIAN_POINT ( 'NONE',  ( 188.5667039024479834, -62.87844715994099687, 257.2178068554150059 ) ) ;
#51358 = PLANE ( 'NONE',  #2370 ) ;
#51359 = AXIS2_PLACEMENT_3D ( 'NONE', #70665, #63850, #48840 ) ;
#51360 = ORIENTED_EDGE ( 'NONE', *, *, #43886, .T. ) ;
#51361 = CARTESIAN_POINT ( 'NONE',  ( 97.80791547859365664, -40.51903635482080546, 112.6360621818907077 ) ) ;
#51362 = DIRECTION ( 'NONE',  ( 0.000000000000000000, 1.000000000000000000, 0.000000000000000000 ) ) ;
#51363 = ORIENTED_EDGE ( 'NONE', *, *, #9115, .T. ) ;
#51364 = CARTESIAN_POINT ( 'NONE',  ( 110.8846227072672121, -27.01418920731891404, 269.7784824187681920 ) ) ;
#51365 = DIRECTION ( 'NONE',  ( 0.000000000000000000, 1.000000000000000000, 0.000000000000000000 ) ) ;
#51366 = VERTEX_POINT ( 'NONE', #41951 ) ;
#51367 = FACE_BOUND ( 'NONE', #58819, .T. ) ;
#51368 = DIRECTION ( 'NONE',  ( 0.000000000000000000, 0.000000000000000000, 1.000000000000000000 ) ) ;
#51369 = DIRECTION ( 'NONE',  ( 0.000000000000000000, -1.000000000000000000, 0.000000000000000000 ) ) ;
#51370 = CARTESIAN_POINT ( 'NONE',  ( 112.7927988201233944, -69.16395658370818467, 247.7076816059330042 ) ) ;
#51371 = CARTESIAN_POINT ( 'NONE',  ( 97.30224646444959546, -33.23681714887386818, 22.06514908543394426 ) ) ;
#51372 = CARTESIAN_POINT ( 'NONE',  ( 7.341135922521115909, 72.30123413915578112, 118.1286081293353760 ) ) ;
#51373 = ORIENTED_EDGE ( 'NONE', *, *, #26453, .F. ) ;
#51374 = CARTESIAN_POINT ( 'NONE',  ( 99.11046098610404442, -43.53346720896296773, 27.88991099019694175 ) ) ;
#51375 = CARTESIAN_POINT ( 'NONE',  ( 125.0664851986225159, -56.72944715994101728, 14.67562527591098842 ) ) ;
#51376 = CARTESIAN_POINT ( 'NONE',  ( 111.7737306318703361, -46.73355046572731908, 287.9146728949587555 ) ) ;
#51377 = VERTEX_POINT ( 'NONE', #69684 ) ;
#51378 = CARTESIAN_POINT ( 'NONE',  ( 82.80042800423676397, -18.38432671279261754, 3.076561810303517497 ) ) ;
#51379 = FACE_OUTER_BOUND ( 'NONE', #12881, .T. ) ;
#51380 = FACE_BOUND ( 'NONE', #86307, .T. ) ;
#51381 = CARTESIAN_POINT ( 'NONE',  ( 114.9276189159122907, -38.92769025571944042, 96.42809036959192781 ) ) ;
#51382 = CARTESIAN_POINT ( 'NONE',  ( 101.1884425732228436, -45.36575980889334403, 193.1013395616249682 ) ) ;
#51383 = PLANE ( 'NONE',  #47002 ) ;
#51384 = CARTESIAN_POINT ( 'NONE',  ( 134.0664832912740110, -46.72944715994100306, 8.225625275910998013 ) ) ;
#51385 = ORIENTED_EDGE ( 'NONE', *, *, #71358, .F. ) ;
#51386 = DIRECTION ( 'NONE',  ( 0.000000000000000000, 1.000000000000000000, 0.000000000000000000 ) ) ;
#51387 = VERTEX_POINT ( 'NONE', #42844 ) ;
#51388 = ORIENTED_EDGE ( 'NONE', *, *, #26937, .F. ) ;
#51389 = AXIS2_PLACEMENT_3D ( 'NONE', #3744, #59133, #24630 ) ;
#51390 = CARTESIAN_POINT ( 'NONE',  ( 183.5150000000000148, 14.63749999999999929, -14.28749999999999964 ) ) ;
#51391 = ORIENTED_EDGE ( 'NONE', *, *, #63660, .T. ) ;
#51392 = EDGE_LOOP ( 'NONE', ( #55471, #64501, #67569, #16098 ) ) ;
#51393 = LINE ( 'NONE', #50517, #77358 ) ;
#51394 = TOROIDAL_SURFACE ( 'NONE', #67351, 15.69999999999999929, 0.2999999999999999889 ) ;
#51395 = EDGE_CURVE ( 'NONE', #66654, #58230, #83771, .T. ) ;
#51396 = EDGE_CURVE ( 'NONE', #65745, #75765, #49666, .T. ) ;
#51397 = CARTESIAN_POINT ( 'NONE',  ( 103.2789150993301774, -27.47448485603423407, 41.38559085328053300 ) ) ;
#51398 = CARTESIAN_POINT ( 'NONE',  ( 112.6791402994794709, -29.62235551608389628, 123.9790864947439815 ) ) ;
#51399 = CARTESIAN_POINT ( 'NONE',  ( 96.22633597390384352, -34.45202597047101278, 261.1737205140064475 ) ) ;
#51400 = EDGE_CURVE ( 'NONE', #47935, #65138, #70583, .T. ) ;
#51401 = CYLINDRICAL_SURFACE ( 'NONE', #83268, 15.99999999999999822 ) ;
#51402 = ORIENTED_EDGE ( 'NONE', *, *, #86310, .F. ) ;
#51403 = EDGE_CURVE ( 'NONE', #50559, #26343, #76946, .T. ) ;
#51404 = EDGE_CURVE ( 'NONE', #80549, #17803, #14727, .T. ) ;
#51405 = CARTESIAN_POINT ( 'NONE',  ( 110.9938485345201258, -27.48116441456390646, 135.7571480591466582 ) ) ;
#51406 = ORIENTED_EDGE ( 'NONE', *, *, #37503, .F. ) ;
#51407 = DIRECTION ( 'NONE',  ( 0.000000000000000000, 1.000000000000000000, 0.000000000000000000 ) ) ;
#51408 = CARTESIAN_POINT ( 'NONE',  ( 116.3219235766278672, -32.94275373074044211, 34.13562527591096085 ) ) ;
#51409 = CARTESIAN_POINT ( 'NONE',  ( 30.48091746481831166, -48.32844715994148999, 249.9678068554150059 ) ) ;
#51410 = EDGE_CURVE ( 'NONE', #88510, #37203, #7897, .T. ) ;
#51412 = VECTOR ( 'NONE', #14394, 1000.000000000000000 ) ;
#51411 = CARTESIAN_POINT ( 'NONE',  ( 97.17500156396280886, -33.29969143728342829, 286.0613395616251751 ) ) ;
#51413 = ORIENTED_EDGE ( 'NONE', *, *, #80457, .F. ) ;
#51414 = CARTESIAN_POINT ( 'NONE',  ( 97.61519122654028990, -41.12945951998310790, 256.6727681330537507 ) ) ;
#51415 = VECTOR ( 'NONE', #10467, 1000.000000000000000 ) ;
#51416 = CARTESIAN_POINT ( 'NONE',  ( 99.73159624296292236, -44.24858557630691536, 17.96133956162493206 ) ) ;
#51417 = SURFACE_STYLE_FILL_AREA ( #85088 ) ;
#51418 = VECTOR ( 'NONE', #54194, 1000.000000000000000 ) ;
#51419 = DIRECTION ( 'NONE',  ( 0.8660254037844392627, -0.4999999999999990008, 1.549999999999999706E-14 ) ) ;
#51420 = EDGE_CURVE ( 'NONE', #52361, #73456, #34495, .T. ) ;
#51422 = CARTESIAN_POINT ( 'NONE',  ( 69.24472453127575022, -138.7583646271384055, 247.2489375779490501 ) ) ;
#51421 = DIRECTION ( 'NONE',  ( -1.000000000000000078E-15, 1.000000000000000083E-30, 1.000000000000000000 ) ) ;
#51423 = CARTESIAN_POINT ( 'NONE',  ( 106.1313900203587366, -25.30815840704239150, 323.4690612957397775 ) ) ;
#51424 = CYLINDRICAL_SURFACE ( 'NONE', #75875, 25.39999999999999858 ) ;
#51425 = DIRECTION ( 'NONE',  ( 0.000000000000000000, 0.000000000000000000, -1.000000000000000000 ) ) ;
#51426 = AXIS2_PLACEMENT_3D ( 'NONE', #48281, #57352, #63738 ) ;
#51427 = CIRCLE ( 'NONE', #57268, 1.000000000000000888 ) ;
#51428 = DIRECTION ( 'NONE',  ( -0.7071067811607679721, 0.7071067812123270624, 0.000000000000000000 ) ) ;
#51429 = CARTESIAN_POINT ( 'NONE',  ( -487.2989999999999782, 89.53805401447711176, 3.968750000000410338 ) ) ;
#51430 = EDGE_CURVE ( 'NONE', #51167, #76957, #43183, .T. ) ;
#51431 = DIRECTION ( 'NONE',  ( 0.000000000000000000, -1.000000000000000000, -7.536132396315209176E-17 ) ) ;
#51432 = CARTESIAN_POINT ( 'NONE',  ( 134.0664832912740110, -46.72944715994100306, 1.625625275910997480 ) ) ;
#51433 = CARTESIAN_POINT ( 'NONE',  ( 96.29878009220107060, -39.42515072222565209, 16.53372051400597798 ) ) ;
#51434 = CARTESIAN_POINT ( 'NONE',  ( 117.4872506282070503, -40.41476785070875621, 174.5680062282919778 ) ) ;
#51435 = CARTESIAN_POINT ( 'NONE',  ( 106.9270610292626742, -26.24804662171751346, 56.08705384733997334 ) ) ;
#51437 = CARTESIAN_POINT ( 'NONE',  ( 115.7831076706773388, -41.80230950916739374, 48.40645860934917977 ) ) ;
#51436 = CYLINDRICAL_SURFACE ( 'NONE', #71156, 4.762500000000002842 ) ;
#51438 = DIRECTION ( 'NONE',  ( 0.000000000000000000, 0.000000000000000000, 1.000000000000000000 ) ) ;
#51439 = EDGE_CURVE ( 'NONE', #28273, #16229, #43296, .T. ) ;
#51440 = ORIENTED_EDGE ( 'NONE', *, *, #68548, .F. ) ;
#51441 = DIRECTION ( 'NONE',  ( 1.000000000000000000, 0.000000000000000000, 0.000000000000000000 ) ) ;
#51442 = ORIENTED_EDGE ( 'NONE', *, *, #74407, .F. ) ;
#51443 = CARTESIAN_POINT ( 'NONE',  ( 116.8124865092210456, -37.88235468918157522, 49.73276813305294297 ) ) ;
#51445 = ORIENTED_EDGE ( 'NONE', *, *, #72767, .T. ) ;
#51444 = PLANE ( 'NONE',  #750 ) ;
#51446 = DIRECTION ( 'NONE',  ( -8.953411488912552682E-16, 1.000000000000000000, 0.000000000000000000 ) ) ;
#51447 = CARTESIAN_POINT ( 'NONE',  ( 117.2062538965839309, -41.07097622818925942, 209.5165776568640013 ) ) ;
#51448 = CARTESIAN_POINT ( 'NONE',  ( 162.8913605087219878, -31.76306994223740432, -5.074374724088000832 ) ) ;
#51449 = CARTESIAN_POINT ( 'NONE',  ( 97.81556513139278763, -40.52688310217321543, 146.6364384312551294 ) ) ;
#51450 = DIRECTION ( 'NONE',  ( -3.100000000000000258E-29, 3.100000000000000044E-14, 1.000000000000000000 ) ) ;
#51451 = DIRECTION ( 'NONE',  ( 1.777766061779359009E-15, -1.000000000000000000, 3.100000000000000044E-14 ) ) ;
#51452 = EDGE_CURVE ( 'NONE', #26493, #38746, #63487, .T. ) ;
#51453 = CARTESIAN_POINT ( 'NONE',  ( 146.3532711110487980, -136.6656657599555160, 247.3338320286590033 ) ) ;
#51454 = CARTESIAN_POINT ( 'NONE',  ( 41.56648329127499153, -32.07844715994070839, 18.92562527591200094 ) ) ;
#51455 = EDGE_CURVE ( 'NONE', #59609, #27384, #1986, .T. ) ;
#51456 = CARTESIAN_POINT ( 'NONE',  ( 113.4935171807054246, -28.59114140144088623, 124.5565776568639507 ) ) ;
#51457 = ORIENTED_EDGE ( 'NONE', *, *, #77128, .F. ) ;
#51458 = VERTEX_POINT ( 'NONE', #58709 ) ;
#51459 = VECTOR ( 'NONE', #82874, 1000.000000000000000 ) ;
#51460 = CARTESIAN_POINT ( 'NONE',  ( 112.3776303481765950, -29.59825886299321951, 100.9987261630399757 ) ) ;
#51461 = CARTESIAN_POINT ( 'NONE',  ( -33.98325472291465132, 24.56180297284579694, -3.174999999999764899 ) ) ;
#51463 = DIRECTION ( 'NONE',  ( 5.512527431108029424E-15, -1.000000000000000000, 0.000000000000000000 ) ) ;
#51462 = CARTESIAN_POINT ( 'NONE',  ( 114.8736367985562623, -30.83777597042988106, 215.3413395616249773 ) ) ;
#51464 = VECTOR ( 'NONE', #89779, 1000.000000000000114 ) ;
#51465 = DIRECTION ( 'NONE',  ( 1.000000000000000000, -8.545435842250265406E-15, 0.000000000000000000 ) ) ;
#51466 = CARTESIAN_POINT ( 'NONE',  ( 70.06670390244707392, -137.6784471599409869, 55.21780685541800437 ) ) ;
#51467 = CARTESIAN_POINT ( 'NONE',  ( 118.5108917117887160, 70.27763793881258891, 3.294392537550968392 ) ) ;
#51468 = LINE ( 'NONE', #11041, #63243 ) ;
#51469 = DIRECTION ( 'NONE',  ( 1.000000000000000000, 6.493183223601999383E-14, 9.351236661543306751E-17 ) ) ;
#51470 = CARTESIAN_POINT ( 'NONE',  ( 1.793207055312195196E-22, 69.95000000000000284, 118.5560000000000116 ) ) ;
#51471 = CARTESIAN_POINT ( 'NONE',  ( 117.2167691715783064, -39.01263929987995027, 148.6499109901969859 ) ) ;
#51472 = ORIENTED_EDGE ( 'NONE', *, *, #67116, .T. ) ;
#51473 = ORIENTED_EDGE ( 'NONE', *, *, #61511, .T. ) ;
#51474 = DIRECTION ( 'NONE',  ( 1.000000000000000000, 0.000000000000000000, 0.000000000000000000 ) ) ;
#51475 = CARTESIAN_POINT ( 'NONE',  ( 134.0664832912740110, -8.350947159940998787, 291.1181252759119502 ) ) ;
#51476 = DIRECTION ( 'NONE',  ( -1.000000000000000000, 0.000000000000000000, 0.000000000000000000 ) ) ;
#51477 = CYLINDRICAL_SURFACE ( 'NONE', #383, 3.000000000000002665 ) ;
#51478 = EDGE_CURVE ( 'NONE', #42555, #59958, #29685, .T. ) ;
#51479 = AXIS2_PLACEMENT_3D ( 'NONE', #51454, #43759, #71495 ) ;
#51480 = VECTOR ( 'NONE', #21766, 1000.000000000000000 ) ;
#51481 = CARTESIAN_POINT ( 'NONE',  ( 116.3115597373110290, -32.94279827685361539, 270.1356252759109680 ) ) ;
#51482 = AXIS2_PLACEMENT_3D ( 'NONE', #18398, #73820, #37077 ) ;
#51483 = VECTOR ( 'NONE', #85509, 1000.000000000000000 ) ;
#51484 = CARTESIAN_POINT ( 'NONE',  ( 113.5652313304969567, -44.92653082429684730, 168.1099109901969939 ) ) ;
#51485 = CARTESIAN_POINT ( 'NONE',  ( 83.73314995793998605, 12.92155284005730387, 355.9756252759109998 ) ) ;
#51486 = ORIENTED_EDGE ( 'NONE', *, *, #76098, .T. ) ;
#51488 = ORIENTED_EDGE ( 'NONE', *, *, #29676, .F. ) ;
#51487 = ORIENTED_EDGE ( 'NONE', *, *, #73563, .F. ) ;
#51489 = CARTESIAN_POINT ( 'NONE',  ( 115.4190912951222288, -42.26680109789320028, 64.36133032379248675 ) ) ;
#51490 = DIRECTION ( 'NONE',  ( -1.000000000000000000, 0.000000000000000000, -2.108231265501709878E-16 ) ) ;
#51491 = PLANE ( 'NONE',  #9260 ) ;
#51492 = CARTESIAN_POINT ( 'NONE',  ( 105.6993345102559942, -28.68213381844667609, 13.02809036959096112 ) ) ;
#51493 = CARTESIAN_POINT ( 'NONE',  ( 104.4080996569733770, -46.45808887385236829, 272.3647918606883991 ) ) ;
#51494 = ORIENTED_EDGE ( 'NONE', *, *, #50935, .T. ) ;
#51495 = AXIS2_PLACEMENT_3D ( 'NONE', #45077, #10571, #73233 ) ;
#51496 = CARTESIAN_POINT ( 'NONE',  ( 115.1675060414467993, -40.96806874415090505, 9.635625275910943088 ) ) ;
#51497 = EDGE_CURVE ( 'NONE', #58643, #57294, #53036, .T. ) ;
#51498 = CARTESIAN_POINT ( 'NONE',  ( -126.4537727773635254, 63.48808950043785870, 32.47212463199235088 ) ) ;
#51499 = VERTEX_POINT ( 'NONE', #72368 ) ;
#51500 = VERTEX_POINT ( 'NONE', #37395 ) ;
#51501 = FACE_BOUND ( 'NONE', #55218, .T. ) ;
#51502 = ORIENTED_EDGE ( 'NONE', *, *, #83670, .F. ) ;
#51503 = ORIENTED_EDGE ( 'NONE', *, *, #39436, .F. ) ;
#51504 = AXIS2_PLACEMENT_3D ( 'NONE', #85549, #2864, #3748 ) ;
#51505 = ADVANCED_FACE ( 'NONE', ( #65098 ), #59159, .T. ) ;
#51506 = ADVANCED_FACE ( 'NONE', ( #36944 ), #41745, .T. ) ;
#51507 = CARTESIAN_POINT ( 'NONE',  ( 100.5751258508236674, -42.28088033547287949, 31.31241982807697610 ) ) ;
#51508 = CARTESIAN_POINT ( 'NONE',  ( 117.0443417989465758, -39.94358261462815562, 158.5784824187679476 ) ) ;
#51509 = EDGE_CURVE ( 'NONE', #34951, #73279, #24652, .T. ) ;
#51510 = CARTESIAN_POINT ( 'NONE',  ( 118.8928063919343998, -36.92768728534039724, 153.8127681330539644 ) ) ;
#51511 = FACE_OUTER_BOUND ( 'NONE', #74032, .T. ) ;
#51512 = CARTESIAN_POINT ( 'NONE',  ( 103.0905057572046672, -47.89305850247227880, 248.3041967044829619 ) ) ;
#51513 = CARTESIAN_POINT ( 'NONE',  ( 41.56670390244689628, -36.32844715994109208, 180.4678068554150911 ) ) ;
#51514 = LINE ( 'NONE', #58344, #10382 ) ;
#51515 = CARTESIAN_POINT ( 'NONE',  ( -57.91199999999999903, 0.000000000000000000, 191.3008000794699797 ) ) ;
#51516 = ORIENTED_EDGE ( 'NONE', *, *, #72118, .T. ) ;
#51517 = EDGE_CURVE ( 'NONE', #43446, #52666, #80082, .T. ) ;
#51518 = ORIENTED_EDGE ( 'NONE', *, *, #18409, .F. ) ;
#51519 = AXIS2_PLACEMENT_3D ( 'NONE', #76788, #5971, #54518 ) ;
#51520 = EDGE_CURVE ( 'NONE', #41931, #43342, #47529, .T. ) ;
#51521 = CARTESIAN_POINT ( 'NONE',  ( 115.0734612967709722, -29.04171753102041365, 189.4232443235299570 ) ) ;
#51522 = ORIENTED_EDGE ( 'NONE', *, *, #57996, .T. ) ;
#51523 = CARTESIAN_POINT ( 'NONE',  ( 113.6143417880574020, -45.63476223351307226, 183.0689586092439640 ) ) ;
#51524 = DIRECTION ( 'NONE',  ( 0.7071067811869279351, -0.7071067811861670993, 6.612322855863716074E-17 ) ) ;
#51525 = AXIS2_PLACEMENT_3D ( 'NONE', #18152, #31337, #87211 ) ;
#51526 = DIRECTION ( 'NONE',  ( 1.000000000000000000, 0.000000000000000000, -9.299908063537909262E-17 ) ) ;
#51527 = CARTESIAN_POINT ( 'NONE',  ( 143.7940362993692531, -140.2217314834169315, 246.8063787849100095 ) ) ;
#51530 = CARTESIAN_POINT ( 'NONE',  ( 104.5933598291445605, -26.62426044571802208, 281.2670538473395823 ) ) ;
#51529 = DIRECTION ( 'NONE',  ( 0.000000000000000000, 0.000000000000000000, -1.000000000000000000 ) ) ;
#51528 = CARTESIAN_POINT ( 'NONE',  ( 123.6837132603318707, -20.11243780205705534, 219.5838068554170093 ) ) ;
#51531 = DIRECTION ( 'NONE',  ( 1.000000000000000000, 0.000000000000000000, 0.000000000000000000 ) ) ;
#51533 = ADVANCED_FACE ( 'NONE', ( #2437 ), #38278, .T. ) ;
#51532 = CARTESIAN_POINT ( 'NONE',  ( 130.0664832912740110, -18.82844715994099971, 226.9256252759120116 ) ) ;
#51534 = CARTESIAN_POINT ( 'NONE',  ( 105.7964350658774180, -26.72445465374488549, 271.1771098916634628 ) ) ;
#51535 = CARTESIAN_POINT ( 'NONE',  ( 67.56422611121462296, -137.3915314758240811, 246.8274931754388604 ) ) ;
#51536 = PLANE ( 'NONE',  #12605 ) ;
#51537 = DIRECTION ( 'NONE',  ( 0.000000000000000000, 0.000000000000000000, -1.000000000000000000 ) ) ;
#51539 = VERTEX_POINT ( 'NONE', #57831 ) ;
#51538 = CARTESIAN_POINT ( 'NONE',  ( 99.65405756092035006, -40.29016652223857164, 195.5838068554173219 ) ) ;
#51540 = CYLINDRICAL_SURFACE ( 'NONE', #52424, 0.9999999999999731326 ) ;
#51541 = CARTESIAN_POINT ( 'NONE',  ( 97.36144725414590084, -42.06870896796115034, 176.7146728949589658 ) ) ;
#51542 = CARTESIAN_POINT ( 'NONE',  ( 103.8413319783160489, -46.68031304110885316, 78.32705384733995402 ) ) ;
#51543 = CARTESIAN_POINT ( 'NONE',  ( 118.0865697951701350, -35.40461063965730659, 234.9337205140059552 ) ) ;
#51544 = CARTESIAN_POINT ( 'NONE',  ( 0.000000000000000000, 215.0000000000000000, 154.6557476874258441 ) ) ;
#51545 = CARTESIAN_POINT ( 'NONE',  ( 19.56670390244648416, -25.42844715994203852, 129.9678068554150627 ) ) ;
#51547 = CARTESIAN_POINT ( 'NONE',  ( 117.0736645660960988, -36.55483027940629626, 39.84004045961177809 ) ) ;
#51546 = FACE_OUTER_BOUND ( 'NONE', #79990, .T. ) ;
#51548 = CYLINDRICAL_SURFACE ( 'NONE', #14637, 6.349999999999999645 ) ;
#51549 = CARTESIAN_POINT ( 'NONE',  ( 223.2659999999999911, 52.73749999999999716, -33.78199999999999648 ) ) ;
#51550 = EDGE_LOOP ( 'NONE', ( #5498, #57307, #43239, #68394 ) ) ;
#51551 = CARTESIAN_POINT ( 'NONE',  ( 100.9557301351062932, -28.70619097067474002, 65.59534030220335410 ) ) ;
#51552 = CIRCLE ( 'NONE', #19657, 5.562599999999973122 ) ;
#51553 = VECTOR ( 'NONE', #62300, 1000.000000000000000 ) ;
#51554 = VECTOR ( 'NONE', #23359, 1000.000000000000114 ) ;
#51555 = AXIS2_PLACEMENT_3D ( 'NONE', #47556, #14867, #56159 ) ;
#51556 = ORIENTED_EDGE ( 'NONE', *, *, #55362, .T. ) ;
#51557 = ORIENTED_EDGE ( 'NONE', *, *, #10248, .F. ) ;
#51558 = VECTOR ( 'NONE', #77380, 1000.000000000000000 ) ;
#51559 = CARTESIAN_POINT ( 'NONE',  ( 114.8760577754623569, -30.96046336120327069, 108.7552769709339771 ) ) ;
#51561 = ORIENTED_EDGE ( 'NONE', *, *, #79471, .T. ) ;
#51560 = CARTESIAN_POINT ( 'NONE',  ( 140.0667039024470455, -118.2784471599408960, 51.21780685541800437 ) ) ;
#51562 = CARTESIAN_POINT ( 'NONE',  ( 101.6894933626720245, -27.09867346898214180, 101.4937205140059575 ) ) ;
#51563 = CARTESIAN_POINT ( 'NONE',  ( 71.25529199314597406, -79.12815651470191369, 361.9756252759101471 ) ) ;
#51564 = CARTESIAN_POINT ( 'NONE',  ( 79.05226586200201666, -16.17316201338597637, 8.065992442479700486 ) ) ;
#51565 = LINE ( 'NONE', #15739, #65026 ) ;
#51566 = EDGE_CURVE ( 'NONE', #8767, #67043, #44187, .T. ) ;
#51568 = CARTESIAN_POINT ( 'NONE',  ( 104.8797383215544556, -46.86635653470259655, 32.41943479972098174 ) ) ;
#51567 = VECTOR ( 'NONE', #86782, 1000.000000000000000 ) ;
#51569 = ORIENTED_EDGE ( 'NONE', *, *, #39725, .F. ) ;
#51570 = VERTEX_POINT ( 'NONE', #65542 ) ;
#51571 = VERTEX_POINT ( 'NONE', #3325 ) ;
#51572 = CARTESIAN_POINT ( 'NONE',  ( 125.0664851986225159, -56.72944715994084675, -4.970821333495647920 ) ) ;
#51573 = CARTESIAN_POINT ( 'NONE',  ( 34.27482367531361973, -30.08671355700341010, 193.9678068554150911 ) ) ;
#51574 = DIRECTION ( 'NONE',  ( 1.000000000000000000, 0.000000000000000000, 0.000000000000000000 ) ) ;
#51575 = DIRECTION ( 'NONE',  ( 1.000000000000000000, 1.000000000000000078E-15, 0.000000000000000000 ) ) ;
#51576 = AXIS2_PLACEMENT_3D ( 'NONE', #45403, #73121, #18158 ) ;
#51577 = CARTESIAN_POINT ( 'NONE',  ( 47.62500000000000000, 66.67499999999999716, 288.9250000000000114 ) ) ;
#51578 = DIRECTION ( 'NONE',  ( 0.000000000000000000, 1.000000000000000000, 0.000000000000000000 ) ) ;
#51579 = CARTESIAN_POINT ( 'NONE',  ( -462.0260000000000105, 41.27499999999999858, 3.174999999999999822 ) ) ;
#51580 = CARTESIAN_POINT ( 'NONE',  ( 3.944304526105059924E-28, 95.25000000000000000, 130.5560000000000116 ) ) ;
#51581 = CARTESIAN_POINT ( 'NONE',  ( 107.6057229598026339, -48.54288983744056907, 42.61276813305398292 ) ) ;
#51583 = ORIENTED_EDGE ( 'NONE', *, *, #9680, .T. ) ;
#51582 = VECTOR ( 'NONE', #4815, 1000.000000000000000 ) ;
#51584 = ORIENTED_EDGE ( 'NONE', *, *, #72483, .T. ) ;
#51585 = DIRECTION ( 'NONE',  ( 0.000000000000000000, 1.000000000000000000, 0.000000000000000000 ) ) ;
#51586 = LINE ( 'NONE', #52892, #24543 ) ;
#51587 = B_SPLINE_CURVE_WITH_KNOTS ( 'NONE', 3,
 ( #64685, #73266, #86481, #66451, #3357, #31047, #51914, #58737, #25125, #72402, #11048, #4240, #45109, #10601, #37875, #59186, #79673, #38307 ),
 .UNSPECIFIED., .F., .F.,
 ( 4, 2, 2, 2, 2, 2, 2, 2, 4 ),
 ( 0.5000000022694898183, 0.5625000019858036326, 0.6250000017021173360, 0.6875000014184311503, 0.7500000011347449647, 0.8125000008510586680, 0.8750000005673724823, 0.9375000002836861857, 1.000000000000000000 ),
 .UNSPECIFIED. ) ;
#51588 = PLANE ( 'NONE',  #43817 ) ;
#51589 = CARTESIAN_POINT ( 'NONE',  ( 113.0992926495536182, -42.93477843977468922, 116.0204713219719679 ) ) ;
#51590 =( GEOMETRIC_REPRESENTATION_CONTEXT ( 3 ) GLOBAL_UNCERTAINTY_ASSIGNED_CONTEXT ( ( #16926 ) ) GLOBAL_UNIT_ASSIGNED_CONTEXT ( ( #37244, #44034, #42686 ) ) REPRESENTATION_CONTEXT ( 'NONE', 'WORKASPACE' ) );
#51591 = ADVANCED_FACE ( 'NONE', ( #10573 ), #45514, .T. ) ;
#51592 = AXIS2_PLACEMENT_3D ( 'NONE', #67373, #5164, #46021 ) ;
#51593 = LINE ( 'NONE', #66914, #4945 ) ;
#51594 = FACE_OUTER_BOUND ( 'NONE', #28245, .T. ) ;
#51595 = ORIENTED_EDGE ( 'NONE', *, *, #75119, .T. ) ;
#51596 = ORIENTED_EDGE ( 'NONE', *, *, #9367, .F. ) ;
#51597 = DIRECTION ( 'NONE',  ( 1.000000000000000000, 1.000000000000000078E-15, 0.000000000000000000 ) ) ;
#51598 = EDGE_LOOP ( 'NONE', ( #70620, #46705 ) ) ;
#51599 = ORIENTED_EDGE ( 'NONE', *, *, #48032, .F. ) ;
#51600 = CARTESIAN_POINT ( 'NONE',  ( 104.2961655698287302, -28.31198801876947613, 161.7615833058969486 ) ) ;
#51601 = CARTESIAN_POINT ( 'NONE',  ( 106.1656040943334460, -121.2545485715094316, -21.78219314458149114 ) ) ;
#51602 = CARTESIAN_POINT ( 'NONE',  ( 96.58534993179142703, -36.88768535406505578, 132.3384824187679669 ) ) ;
#51603 = DIRECTION ( 'NONE',  ( -0.7071067811865270336, 0.7071067811865680008, -7.071067811865277132E-16 ) ) ;
#51604 = CARTESIAN_POINT ( 'NONE',  ( 108.3328101825627385, -46.73493184262017763, 17.67728433966769686 ) ) ;
#51605 = AXIS2_PLACEMENT_3D ( 'NONE', #46096, #5241, #75176 ) ;
#51606 = ORIENTED_EDGE ( 'NONE', *, *, #54427, .T. ) ;
#51607 = CIRCLE ( 'NONE', #87883, 1.000000000000000888 ) ;
#51608 = CONICAL_SURFACE ( 'NONE', #61791, 1.258750000000002922, 1.029744258676650093 ) ;
#51609 = AXIS2_PLACEMENT_3D ( 'NONE', #27800, #55480, #15078 ) ;
#51610 = EDGE_LOOP ( 'NONE', ( #5264, #82151, #85639, #54715 ) ) ;
#51611 = ORIENTED_EDGE ( 'NONE', *, *, #79771, .T. ) ;
#51612 = EDGE_CURVE ( 'NONE', #67030, #2296, #44602, .T. ) ;
#51613 = CARTESIAN_POINT ( 'NONE',  ( 98.90610402553750191, -36.53467484046868208, 194.1252332267349630 ) ) ;
#51614 = CARTESIAN_POINT ( 'NONE',  ( 104.0363141061766186, -47.38371934748259662, 67.36800622829191809 ) ) ;
#51615 = ORIENTED_EDGE ( 'NONE', *, *, #56459, .T. ) ;
#51616 = EDGE_CURVE ( 'NONE', #752, #34034, #6948, .T. ) ;
#51617 = CARTESIAN_POINT ( 'NONE',  ( 100.9539191370901960, -46.85292318231938680, 52.14419670448194921 ) ) ;
#51618 = DIRECTION ( 'NONE',  ( 0.7071067811869841124, -0.7071067811861110330, 0.000000000000000000 ) ) ;
#51619 = CARTESIAN_POINT ( 'NONE',  ( 103.2030832344709381, -107.0864598618342995, -19.78219314458193168 ) ) ;
#51620 = CARTESIAN_POINT ( 'NONE',  ( 107.3661318999371161, -25.27282818541385367, 323.3302093749328492 ) ) ;
#51621 = EDGE_CURVE ( 'NONE', #26492, #85897, #57719, .T. ) ;
#51622 = CARTESIAN_POINT ( 'NONE',  ( 97.67470816545109358, -41.25460433215529577, 167.6841967044829573 ) ) ;
#51623 = CARTESIAN_POINT ( 'NONE',  ( 162.7131505118549057, -33.70561438051511516, 237.4678068554150059 ) ) ;
#51624 = ORIENTED_EDGE ( 'NONE', *, *, #85077, .F. ) ;
#51625 = CARTESIAN_POINT ( 'NONE',  ( -254.0000000000000000, 104.7749999999999915, -41.27499999999999858 ) ) ;
#51626 = ADVANCED_FACE ( 'NONE', ( #45046 ), #30984, .T. ) ;
#51627 = ORIENTED_EDGE ( 'NONE', *, *, #19558, .F. ) ;
#51628 = DIRECTION ( 'NONE',  ( 0.000000000000000000, 0.000000000000000000, 1.000000000000000000 ) ) ;
#51629 = CARTESIAN_POINT ( 'NONE',  ( 138.8167039024479834, -50.82844715994100682, 35.51780685541480409 ) ) ;
#51630 = AXIS2_PLACEMENT_3D ( 'NONE', #60573, #24726, #86965 ) ;
#51631 = ORIENTED_EDGE ( 'NONE', *, *, #23264, .F. ) ;
#51632 = LINE ( 'NONE', #79377, #25767 ) ;
#51633 = PLANE ( 'NONE',  #44988 ) ;
#51634 = CARTESIAN_POINT ( 'NONE',  ( 117.9889986865933196, -38.42583888725547325, 68.69181575210198787 ) ) ;
#51635 = CARTESIAN_POINT ( 'NONE',  ( 32.06670390244800473, -33.35206098992711077, -5.074374724088000832 ) ) ;
#51636 = AXIS2_PLACEMENT_3D ( 'NONE', #36626, #15733, #26758 ) ;
#51637 = CARTESIAN_POINT ( 'NONE',  ( 100.1253875378088338, -39.57043109886122778, 9.125625275910969947 ) ) ;
#51638 = DIRECTION ( 'NONE',  ( 1.000000000000000000, 1.000000000000000078E-15, 0.000000000000000000 ) ) ;
#51639 = CARTESIAN_POINT ( 'NONE',  ( 117.4022237771662276, -37.57280582802028590, 38.77372051400595865 ) ) ;
#51641 = CARTESIAN_POINT ( 'NONE',  ( 112.7681627534586113, -45.43114336468919134, 174.0384824187679556 ) ) ;
#51640 = CARTESIAN_POINT ( 'NONE',  ( 126.8164832912740394, -54.72944906728950798, -5.074374724089010691 ) ) ;
#51642 = LINE ( 'NONE', #82962, #16117 ) ;
#51644 = EDGE_CURVE ( 'NONE', #74639, #53210, #59566, .T. ) ;
#51643 = CARTESIAN_POINT ( 'NONE',  ( 0.000000000000000000, 61.59999999999999432, 0.000000000000000000 ) ) ;
#51645 = ORIENTED_EDGE ( 'NONE', *, *, #75928, .T. ) ;
#51646 = CARTESIAN_POINT ( 'NONE',  ( 83.06670390244796920, -67.87844715994100397, 225.9838068554150254 ) ) ;
#51647 = DIRECTION ( 'NONE',  ( 1.000000000000000000, 4.299999999999999979E-14, 1.000000000000000078E-15 ) ) ;
#51648 = CARTESIAN_POINT ( 'NONE',  ( 74.85599922111907745, -133.5313194959603607, 248.4142799812389910 ) ) ;
#51649 = DIRECTION ( 'NONE',  ( 0.000000000000000000, 0.000000000000000000, -1.000000000000000000 ) ) ;
#51651 = VERTEX_POINT ( 'NONE', #17363 ) ;
#51650 = CARTESIAN_POINT ( 'NONE',  ( 113.0507064547910829, -46.07834852625790489, 218.0175300378159591 ) ) ;
#51652 = DIRECTION ( 'NONE',  ( -4.237773401492740281E-14, 1.000000000000000000, 0.000000000000000000 ) ) ;
#51653 = CARTESIAN_POINT ( 'NONE',  ( 116.9459113946819286, -41.73765103896904805, 244.4651490854349731 ) ) ;
#51654 = CARTESIAN_POINT ( 'NONE',  ( 99.47006920962783738, -43.93274313109116491, 77.92991099019597812 ) ) ;
#51655 = DIRECTION ( 'NONE',  ( 0.000000000000000000, 0.000000000000000000, 1.000000000000000000 ) ) ;
#51656 = CARTESIAN_POINT ( 'NONE',  ( 98.34933868204893770, -31.65751815772215849, 191.9063711284184706 ) ) ;
#51657 = VECTOR ( 'NONE', #31273, 1000.000000000000000 ) ;
#51658 = CARTESIAN_POINT ( 'NONE',  ( 172.5667039024480118, -36.32844715993499563, 180.4678068554150059 ) ) ;
#51659 = CARTESIAN_POINT ( 'NONE',  ( 25.56670390244832447, -48.82844715994168183, 257.2178068554150059 ) ) ;
#51660 = VERTEX_POINT ( 'NONE', #72777 ) ;
#51661 = ORIENTED_EDGE ( 'NONE', *, *, #85632, .T. ) ;
#51662 = ORIENTED_EDGE ( 'NONE', *, *, #54163, .F. ) ;
#51663 = VERTEX_POINT ( 'NONE', #37811 ) ;
#51664 = CARTESIAN_POINT ( 'NONE',  ( 167.2371591254544967, -47.82818131005522133, 180.4678068554150059 ) ) ;
#51665 = CARTESIAN_POINT ( 'NONE',  ( 116.2186307022408727, -41.79497087860992366, 259.4241967044825969 ) ) ;
#51666 = CARTESIAN_POINT ( 'NONE',  ( 0.000000000000000000, 44.45000000000000284, 0.000000000000000000 ) ) ;
#51667 = CARTESIAN_POINT ( 'NONE',  ( 69.56670390244701707, -85.27844715994098124, 55.21780685541800437 ) ) ;
#51669 = CARTESIAN_POINT ( 'NONE',  ( 80.88853703239254855, 70.52018178143200089, 86.67600044576384732 ) ) ;
#51668 = FACE_BOUND ( 'NONE', #32843, .T. ) ;
#51670 = AXIS2_PLACEMENT_3D ( 'NONE', #6267, #40326, #82148 ) ;
#51671 = CARTESIAN_POINT ( 'NONE',  ( 27.27158787008327678, 184.0000000000000000, 85.23828826961327820 ) ) ;
#51672 = EDGE_CURVE ( 'NONE', #20334, #10389, #23312, .T. ) ;
#51673 = CARTESIAN_POINT ( 'NONE',  ( 115.3666750469823938, -34.71377145672549602, 208.4381341137909658 ) ) ;
#51674 = EDGE_LOOP ( 'NONE', ( #57103, #1513 ) ) ;
#51675 = ORIENTED_EDGE ( 'NONE', *, *, #87176, .T. ) ;
#51676 = AXIS2_PLACEMENT_3D ( 'NONE', #1001, #42311, #6467 ) ;
#51677 = ORIENTED_EDGE ( 'NONE', *, *, #22142, .F. ) ;
#51678 = CIRCLE ( 'NONE', #12532, 3.249999999999975131 ) ;
#51679 = CARTESIAN_POINT ( 'NONE',  ( 107.0667039024479834, -48.82844715994099971, 160.9178068554150229 ) ) ;
#51680 = CIRCLE ( 'NONE', #61857, 2.500000000000002220 ) ;
#51681 = CARTESIAN_POINT ( 'NONE',  ( 98.15099777509990986, -41.26165302448119121, 181.7007408304860689 ) ) ;
#51682 = EDGE_CURVE ( 'NONE', #29480, #67802, #31421, .T. ) ;
#51683 = CARTESIAN_POINT ( 'NONE',  ( 114.8131502045275880, -44.70447909941016462, 264.1899109901960401 ) ) ;
#51684 = CARTESIAN_POINT ( 'NONE',  ( 176.7669697523286061, -48.62818131005462163, 300.4678068554149490 ) ) ;
#51685 = DIRECTION ( 'NONE',  ( 0.000000000000000000, 0.000000000000000000, 1.000000000000000000 ) ) ;
#51686 = CARTESIAN_POINT ( 'NONE',  ( 97.81170495107971874, -40.51745053935989915, 26.63526479160227112 ) ) ;
#51687 = ORIENTED_EDGE ( 'NONE', *, *, #74397, .F. ) ;
#51688 = CARTESIAN_POINT ( 'NONE',  ( 103.2843211798393241, -27.47227357675608772, 56.38512623260010770 ) ) ;
#51689 = ORIENTED_EDGE ( 'NONE', *, *, #27667, .F. ) ;
#51690 = AXIS2_PLACEMENT_3D ( 'NONE', #9200, #85521, #50962 ) ;
#51691 = DIRECTION ( 'NONE',  ( -0.7071067811865475727, -0.000000000000000000, -0.7071067811865475727 ) ) ;
#51692 = CARTESIAN_POINT ( 'NONE',  ( 98.94126815719160106, -33.74921318831734851, 18.85285227435401367 ) ) ;
#51693 = EDGE_CURVE ( 'NONE', #228, #10278, #86860, .T. ) ;
#51694 = CARTESIAN_POINT ( 'NONE',  ( 36.65249034007526063, -48.32844715994123419, 300.4678068554150059 ) ) ;
#51695 = CARTESIAN_POINT ( 'NONE',  ( 20.03715912545735023, -46.82818131006202123, 180.4678068554150911 ) ) ;
#51696 = CARTESIAN_POINT ( 'NONE',  ( 186.6899999999999977, 59.08750000000000568, -50.79999999999999716 ) ) ;
#51697 = ORIENTED_EDGE ( 'NONE', *, *, #2200, .T. ) ;
#51698 = DIRECTION ( 'NONE',  ( 0.000000000000000000, 0.000000000000000000, -1.000000000000000000 ) ) ;
#51699 = DIRECTION ( 'NONE',  ( 0.000000000000000000, 1.000000000000000000, 0.000000000000000000 ) ) ;
#51700 = VERTEX_POINT ( 'NONE', #24185 ) ;
#51701 = CARTESIAN_POINT ( 'NONE',  ( 99.50153220775246155, -43.90290835836871253, 81.92991099019597812 ) ) ;
#51702 = ORIENTED_EDGE ( 'NONE', *, *, #82809, .F. ) ;
#51703 = CARTESIAN_POINT ( 'NONE',  ( 115.5775591941339542, -37.73626844564258676, 53.15527697093397563 ) ) ;
#51704 = CARTESIAN_POINT ( 'NONE',  ( 105.2997058862832347, -46.60644133428081659, 88.43476079292317138 ) ) ;
#51705 = CARTESIAN_POINT ( 'NONE',  ( 104.3250142303409831, -45.18796221723782480, 78.75872616303996665 ) ) ;
#51706 = FACE_BOUND ( 'NONE', #68144, .T. ) ;
#51707 = DIRECTION ( 'NONE',  ( -2.913971193241881161E-15, 0.000000000000000000, 1.000000000000000000 ) ) ;
#51708 = CARTESIAN_POINT ( 'NONE',  ( 91.91125933621951560, -96.57698625956682292, -11.78219314458225853 ) ) ;
#51709 = CIRCLE ( 'NONE', #67682, 5.599999999999994316 ) ;
#51710 = CARTESIAN_POINT ( 'NONE',  ( 111.0545523236672807, -47.06291463499678684, 13.85753003781498016 ) ) ;
#51711 = DIRECTION ( 'NONE',  ( 0.7071067811866377228, -0.7071067811864573116, 0.000000000000000000 ) ) ;
#51712 = ORIENTED_EDGE ( 'NONE', *, *, #76659, .F. ) ;
#51713 = DIRECTION ( 'NONE',  ( 0.0001713722456133526934, -0.9999999853157766072, 0.000000000000000000 ) ) ;
#51714 = ORIENTED_EDGE ( 'NONE', *, *, #85853, .F. ) ;
#51715 = CARTESIAN_POINT ( 'NONE',  ( 96.62748084391311920, -35.94289726309906996, 142.2670538473399517 ) ) ;
#51716 = CARTESIAN_POINT ( 'NONE',  ( 78.64593636901959428, -21.09121833381964706, 1.942446336658495643 ) ) ;
#51717 = ORIENTED_EDGE ( 'NONE', *, *, #8569, .T. ) ;
#51718 = ORIENTED_EDGE ( 'NONE', *, *, #977, .F. ) ;
#51719 = DIRECTION ( 'NONE',  ( -1.000000000000000078E-15, 1.000000000000000000, 0.000000000000000000 ) ) ;
#51720 = CARTESIAN_POINT ( 'NONE',  ( 91.91441891875214765, -111.9861225405541632, -21.78219314458176825 ) ) ;
#51721 = CARTESIAN_POINT ( 'NONE',  ( 109.8674951572811551, -26.74480306206631397, 219.8708633711499658 ) ) ;
#51722 = CARTESIAN_POINT ( 'NONE',  ( 115.5869760628213214, -31.41147761708738173, 124.2698573529066977 ) ) ;
#51723 = CARTESIAN_POINT ( 'NONE',  ( 71.25614885437424562, -84.12815644128085069, 396.9756252759102040 ) ) ;
#51724 = EDGE_CURVE ( 'NONE', #34970, #79915, #30168, .T. ) ;
#51725 = CARTESIAN_POINT ( 'NONE',  ( 96.95674990518240577, -32.26097187787489418, 51.98324432352996638 ) ) ;
#51726 = CARTESIAN_POINT ( 'NONE',  ( 72.06648329127399677, -8.729447159941065237, -4.824374724089063982 ) ) ;
#51727 = ORIENTED_EDGE ( 'NONE', *, *, #82413, .T. ) ;
#51728 = CARTESIAN_POINT ( 'NONE',  ( 107.8824949288598987, -26.74133428231821696, 171.0115286325450654 ) ) ;
#51729 = CIRCLE ( 'NONE', #77834, 4.875000000000017764 ) ;
#51730 = DIRECTION ( 'NONE',  ( 0.7071067811865475727, -0.7071067811865475727, 0.000000000000000000 ) ) ;
#51731 = EDGE_LOOP ( 'NONE', ( #25095, #74508, #62894, #76125, #63210, #85474, #6274, #64724, #72261, #43573, #89526, #5675 ) ) ;
#51732 = VECTOR ( 'NONE', #80173, 1000.000000000000000 ) ;
#51733 = PLANE ( 'NONE',  #79351 ) ;
#51734 = VECTOR ( 'NONE', #33624, 1000.000000000000000 ) ;
#51735 = CARTESIAN_POINT ( 'NONE',  ( 83.06670390244796920, -58.72944715994093201, 204.3338068554149913 ) ) ;
#51736 = CARTESIAN_POINT ( 'NONE',  ( 96.14807755961376756, -35.16348456217429685, 226.2251490854349640 ) ) ;
#51737 = LINE ( 'NONE', #67166, #9536 ) ;
#51738 = AXIS2_PLACEMENT_3D ( 'NONE', #22146, #49811, #23921 ) ;
#51739 = FACE_OUTER_BOUND ( 'NONE', #10505, .T. ) ;
#51740 = CARTESIAN_POINT ( 'NONE',  ( 107.9747653995834753, -121.2541776101292186, -11.78219314458148226 ) ) ;
#51741 = CARTESIAN_POINT ( 'NONE',  ( 104.8904560483511545, -27.93868065388478428, 239.6800388756959705 ) ) ;
#51743 = CARTESIAN_POINT ( 'NONE',  ( 117.0329088946582630, -32.00354160957723337, 60.19086337114898555 ) ) ;
#51742 = DIRECTION ( 'NONE',  ( 0.000000000000000000, -1.000000000000000000, 0.000000000000000000 ) ) ;
#51744 = CARTESIAN_POINT ( 'NONE',  ( 109.8326081572954251, 59.86973552847310742, 70.58103716012563211 ) ) ;
#51745 = CARTESIAN_POINT ( 'NONE',  ( 96.65525155030036331, -37.83077348759547220, 126.4099109901969626 ) ) ;
#51746 = ORIENTED_EDGE ( 'NONE', *, *, #55610, .F. ) ;
#51748 = ADVANCED_FACE ( 'NONE', ( #38246 ), #78719, .F. ) ;
#51747 = CARTESIAN_POINT ( 'NONE',  ( 46.03715912545348488, -48.62818131006090283, 129.9678068554150911 ) ) ;
#51749 = ORIENTED_EDGE ( 'NONE', *, *, #25368, .F. ) ;
#51750 = DIRECTION ( 'NONE',  ( 1.000000000000000078E-15, -1.000000000000000083E-30, -1.000000000000000000 ) ) ;
#51751 = LINE ( 'NONE', #64517, #1467 ) ;
#51752 = EDGE_CURVE ( 'NONE', #19525, #20491, #24621, .T. ) ;
#51753 = CARTESIAN_POINT ( 'NONE',  ( 134.0664832912740110, -33.97944715994100306, 1.625625275910997480 ) ) ;
#51754 = EDGE_LOOP ( 'NONE', ( #1708, #30942, #34088, #28639, #68378, #76245 ) ) ;
#51755 = CARTESIAN_POINT ( 'NONE',  ( 97.39139531738810263, -39.27891137106568920, 51.53149185393750287 ) ) ;
#51756 = EDGE_LOOP ( 'NONE', ( #18330, #11801 ) ) ;
#51757 = CARTESIAN_POINT ( 'NONE',  ( -465.6921742093539933, 60.32499999999999574, 3.174999999999999822 ) ) ;
#51758 = CARTESIAN_POINT ( 'NONE',  ( 0.000000000000000000, 8.255000000000000782, 0.000000000000000000 ) ) ;
#51759 = AXIS2_PLACEMENT_3D ( 'NONE', #6844, #75890, #13660 ) ;
#51760 = DIRECTION ( 'NONE',  ( 3.100000000000000258E-29, -3.100000000000000044E-14, -1.000000000000000000 ) ) ;
#51761 = ORIENTED_EDGE ( 'NONE', *, *, #33896, .F. ) ;
#51762 = AXIS2_PLACEMENT_3D ( 'NONE', #2615, #86624, #72098 ) ;
#51763 = CARTESIAN_POINT ( 'NONE',  ( 99.48556355041279176, -43.91805062995148745, 81.92991099019597812 ) ) ;
#51764 = DIRECTION ( 'NONE',  ( -2.544367396927093358E-16, 0.000000000000000000, 1.000000000000000000 ) ) ;
#51765 = DIRECTION ( 'NONE',  ( 0.7071067811739204512, -0.7071067811991745833, 0.000000000000000000 ) ) ;
#51766 = DIRECTION ( 'NONE',  ( 0.000000000000000000, 0.000000000000000000, 1.000000000000000000 ) ) ;
#51767 = CARTESIAN_POINT ( 'NONE',  ( 96.67439905703393777, -115.7784471599421323, -21.78219314458165812 ) ) ;
#51768 = ORIENTED_EDGE ( 'NONE', *, *, #70371, .F. ) ;
#51769 = DIRECTION ( 'NONE',  ( -2.999999999999999839E-15, 1.000000000000000000, -2.999999999999999900E-30 ) ) ;
#51770 = DIRECTION ( 'NONE',  ( -2.505701470911820065E-15, 0.000000000000000000, -1.000000000000000000 ) ) ;
#51771 = CARTESIAN_POINT ( 'NONE',  ( 141.9629299006807059, -45.68655394112752077, 14.92562527591105415 ) ) ;
#51773 = CARTESIAN_POINT ( 'NONE',  ( 184.5667039024480118, -67.87844715994100397, 310.9178068554150514 ) ) ;
#51772 = CARTESIAN_POINT ( 'NONE',  ( 90.44969454456405344, -20.11243780205715481, 219.5838068554169809 ) ) ;
#51774 = CARTESIAN_POINT ( 'NONE',  ( 107.0664832912739399, -36.72944715994095333, 312.1356252759112522 ) ) ;
#51775 = AXIS2_PLACEMENT_3D ( 'NONE', #8111, #51208, #37159 ) ;
#51776 = ORIENTED_EDGE ( 'NONE', *, *, #16463, .T. ) ;
#51777 = CARTESIAN_POINT ( 'NONE',  ( 164.9212702847350158, -29.73316016639540749, 193.9678068554150059 ) ) ;
#51778 = EDGE_CURVE ( 'NONE', #79496, #11556, #86713, .T. ) ;
#51779 = CARTESIAN_POINT ( 'NONE',  ( 108.7386892141029335, -46.36620816325528693, 163.7127681330539701 ) ) ;
#51781 = ORIENTED_EDGE ( 'NONE', *, *, #40637, .T. ) ;
#51780 = DIRECTION ( 'NONE',  ( 0.2588190451025154659, 0.000000000000000000, 0.9659258262890696445 ) ) ;
#51782 = CARTESIAN_POINT ( 'NONE',  ( 104.7983354005985888, -46.84845355258768507, 23.38895860924395009 ) ) ;
#51783 = CARTESIAN_POINT ( 'NONE',  ( 72.96458098368650269, 101.5999999999999943, 67.92268098368730023 ) ) ;
#51784 = CARTESIAN_POINT ( 'NONE',  ( 182.3467384525650061, -36.02818131005800950, -5.074374724088000832 ) ) ;
#51785 = PLANE ( 'NONE',  #86272 ) ;
#51786 = EDGE_LOOP ( 'NONE', ( #86407, #59516 ) ) ;
#51787 = CARTESIAN_POINT ( 'NONE',  ( 107.0664832912739968, -36.72944715994100306, 293.2242906452868851 ) ) ;
#51788 = AXIS2_PLACEMENT_3D ( 'NONE', #42946, #57484, #85223 ) ;
#51789 = CIRCLE ( 'NONE', #8312, 5.041900000000001825 ) ;
#51790 = EDGE_LOOP ( 'NONE', ( #15620, #70756, #108, #10725 ) ) ;
#51791 = ORIENTED_EDGE ( 'NONE', *, *, #15338, .F. ) ;
#51792 = CARTESIAN_POINT ( 'NONE',  ( 97.69936372639945432, -35.99897019620807725, 187.7082499725639764 ) ) ;
#51793 = VECTOR ( 'NONE', #29564, 1000.000000000000000 ) ;
#51794 = CARTESIAN_POINT ( 'NONE',  ( 51.06648329127330044, -0.7548456658612000547, 335.0256252759120343 ) ) ;
#51796 = EDGE_CURVE ( 'NONE', #30264, #88540, #76606, .T. ) ;
#51795 = AXIS2_PLACEMENT_3D ( 'NONE', #17657, #24478, #37658 ) ;
#51797 = CARTESIAN_POINT ( 'NONE',  ( 109.8762032759827321, -45.69504804023497968, 49.23777378208799149 ) ) ;
#51798 = CARTESIAN_POINT ( 'NONE',  ( 23.44978778479566728, 85.69659655706036006, 306.4834544166336059 ) ) ;
#51799 = CARTESIAN_POINT ( 'NONE',  ( 100.9546728179205815, -28.70702572233378191, 80.59395860859407890 ) ) ;
#51800 = CARTESIAN_POINT ( 'NONE',  ( 63.03715912545825262, -46.82818131006018092, 249.9678068554150343 ) ) ;
#51801 = EDGE_LOOP ( 'NONE', ( #37899, #23805, #81135, #6664 ) ) ;
#51802 = CYLINDRICAL_SURFACE ( 'NONE', #26122, 2.000000000000007550 ) ;
#51803 = DIRECTION ( 'NONE',  ( 0.000000000000000000, 0.000000000000000000, 1.000000000000000000 ) ) ;
#51804 = VERTEX_POINT ( 'NONE', #64615 ) ;
#51805 = CARTESIAN_POINT ( 'NONE',  ( 100.1919508713739049, -45.35525880799018239, 272.0289586092443415 ) ) ;
#51806 = CARTESIAN_POINT ( 'NONE',  ( 7.730661649919364997, 92.63472181420671347, 118.3041290865632220 ) ) ;
#51807 = VERTEX_POINT ( 'NONE', #79606 ) ;
#51808 = EDGE_CURVE ( 'NONE', #79084, #25402, #80051, .T. ) ;
#51809 = CIRCLE ( 'NONE', #72142, 5.041900000000001825 ) ;
#51810 = EDGE_CURVE ( 'NONE', #29308, #7172, #85974, .T. ) ;
#51811 = LINE ( 'NONE', #65465, #48814 ) ;
#51812 = PLANE ( 'NONE',  #2634 ) ;
#51813 = FACE_OUTER_BOUND ( 'NONE', #27719, .T. ) ;
#51814 = VECTOR ( 'NONE', #62873, 1000.000000000000000 ) ;
#51815 = LINE ( 'NONE', #16877, #63626 ) ;
#51816 = CARTESIAN_POINT ( 'NONE',  ( 116.5662105847193999, -41.21199064955116143, 224.4756252759109714 ) ) ;
#51817 = CARTESIAN_POINT ( 'NONE',  ( 75.61066417432020614, 101.5999999999999943, 189.7379999999999995 ) ) ;
#51818 = ORIENTED_EDGE ( 'NONE', *, *, #59807, .F. ) ;
#51819 = CARTESIAN_POINT ( 'NONE',  ( 117.4979393226723516, -37.96344061660173708, 49.73276813305393773 ) ) ;
#51820 = DIRECTION ( 'NONE',  ( -0.7071067811865434649, -0.7071067811865516806, -7.071067811865440820E-16 ) ) ;
#51821 = EDGE_CURVE ( 'NONE', #64957, #8036, #68213, .T. ) ;
#51822 = CARTESIAN_POINT ( 'NONE',  ( 112.3383795496262820, -28.20708685789894687, 289.6356252759109680 ) ) ;
#51823 = VERTEX_POINT ( 'NONE', #47283 ) ;
#51824 = CARTESIAN_POINT ( 'NONE',  ( 78.82227874342571283, -39.18254450372162978, 7.982620440113867843 ) ) ;
#51825 = CARTESIAN_POINT ( 'NONE',  ( 70.06670390244707392, -140.6784471599409869, 228.4678068554179902 ) ) ;
#51826 = PLANE ( 'NONE',  #33501 ) ;
#51827 = EDGE_CURVE ( 'NONE', #49032, #47693, #40275, .T. ) ;
#51828 = CARTESIAN_POINT ( 'NONE',  ( 114.4788834064733862, -33.31096057238692509, 101.9880903695909780 ) ) ;
#51829 = CARTESIAN_POINT ( 'NONE',  ( 104.4050232528787774, -25.97761772452189888, 236.2575300378159682 ) ) ;
#51830 = CARTESIAN_POINT ( 'NONE',  ( 50.88849390559499142, -32.11662333284530746, -5.074374724088000832 ) ) ;
#51831 = ORIENTED_EDGE ( 'NONE', *, *, #76003, .T. ) ;
#51832 = CARTESIAN_POINT ( 'NONE',  ( 136.4640758026458229, -38.08864647353156130, 2.654395117668909343 ) ) ;
#51833 = ORIENTED_EDGE ( 'NONE', *, *, #86343, .F. ) ;
#51835 = ORIENTED_EDGE ( 'NONE', *, *, #47886, .T. ) ;
#51834 = AXIS2_PLACEMENT_3D ( 'NONE', #21648, #36155, #63870 ) ;
#51836 = LINE ( 'NONE', #12319, #67722 ) ;
#51837 = ORIENTED_EDGE ( 'NONE', *, *, #83008, .T. ) ;
#51838 = ORIENTED_EDGE ( 'NONE', *, *, #63740, .T. ) ;
#51839 = DIRECTION ( 'NONE',  ( -0.7071067811865671127, -0.7071067811865279218, -7.071067811865664660E-16 ) ) ;
#51840 = CARTESIAN_POINT ( 'NONE',  ( 103.2785405023565346, -27.47463817066477532, 41.38562306036225635 ) ) ;
#51841 = CARTESIAN_POINT ( 'NONE',  ( 111.9909297607753160, -29.75048171432638355, 129.0095626852189525 ) ) ;
#51842 = CARTESIAN_POINT ( 'NONE',  ( 117.5565198162756104, -37.28721152219886648, 18.78419670448294809 ) ) ;
#51843 = EDGE_CURVE ( 'NONE', #68139, #4100, #19156, .T. ) ;
#51844 = ADVANCED_FACE ( 'NONE', ( #5985 ), #89094, .F. ) ;
#51845 = CARTESIAN_POINT ( 'NONE',  ( -12.03144885753538595, 78.46257116061715919, 130.0004926519013111 ) ) ;
#51846 = ORIENTED_EDGE ( 'NONE', *, *, #35315, .T. ) ;
#51847 = EDGE_CURVE ( 'NONE', #54367, #5023, #32312, .T. ) ;
#51848 = CARTESIAN_POINT ( 'NONE',  ( 164.9667039024459996, -28.27351298637401200, -5.074374724088000832 ) ) ;
#51849 = ORIENTED_EDGE ( 'NONE', *, *, #60873, .F. ) ;
#51850 = PLANE ( 'NONE',  #29131 ) ;
#51851 = ADVANCED_FACE ( 'NONE', ( #75469 ), #89546, .T. ) ;
#51852 = DIRECTION ( 'NONE',  ( -0.04216478779797398074, 0.9991106698809455455, 0.000000000000000000 ) ) ;
#51853 = DIRECTION ( 'NONE',  ( 0.000000000000000000, 0.000000000000000000, -1.000000000000000000 ) ) ;
#51854 = PLANE ( 'NONE',  #43675 ) ;
#51855 = ORIENTED_EDGE ( 'NONE', *, *, #50512, .F. ) ;
#51856 = VECTOR ( 'NONE', #66388, 1000.000000000000000 ) ;
#51857 = CARTESIAN_POINT ( 'NONE',  ( 118.3411383306134468, -33.07924694129162901, 284.0756252759109657 ) ) ;
#51858 = CARTESIAN_POINT ( 'NONE',  ( 115.9284861604400731, -31.15648700444841879, 30.27276813305396175 ) ) ;
#51859 =( LENGTH_UNIT ( ) NAMED_UNIT ( * ) SI_UNIT ( .MILLI., .METRE. ) );
#51861 = CARTESIAN_POINT ( 'NONE',  ( 68.92834633064059346, -139.0720971569717221, 246.7691504559092550 ) ) ;
#51860 = DIRECTION ( 'NONE',  ( -0.000000000000000000, -0.000000000000000000, 1.000000000000000000 ) ) ;
#51862 = CARTESIAN_POINT ( 'NONE',  ( 172.5664832912729878, -18.82844715994071194, 318.9256252759120116 ) ) ;
#51863 = DIRECTION ( 'NONE',  ( 0.000000000000000000, 0.000000000000000000, -1.000000000000000000 ) ) ;
#51864 = CARTESIAN_POINT ( 'NONE',  ( 139.7494832912729805, -71.52944715994142655, 352.4506252759077825 ) ) ;
#51865 = CARTESIAN_POINT ( 'NONE',  ( 107.0958534276316527, -25.26768445413491904, 322.6018878585615539 ) ) ;
#51866 = CARTESIAN_POINT ( 'NONE',  ( 108.3338011049130785, -46.73481928183232270, 162.6771430053029519 ) ) ;
#51867 = AXIS2_PLACEMENT_3D ( 'NONE', #80828, #39469, #44934 ) ;
#51868 = CARTESIAN_POINT ( 'NONE',  ( 193.0371591254585724, -47.82818131005411999, 129.9678068554150343 ) ) ;
#51869 = CARTESIAN_POINT ( 'NONE',  ( 111.3412100197261765, -27.17259740239810739, 24.74133956162494030 ) ) ;
#51870 = CARTESIAN_POINT ( 'NONE',  ( 111.4172602844868862, -47.75239391268459599, 168.8756252759109486 ) ) ;
#51871 = CARTESIAN_POINT ( 'NONE',  ( 117.5094244910773114, -37.01621876064744754, 39.80419670448193159 ) ) ;
#51872 = VECTOR ( 'NONE', #88261, 1000.000000000000000 ) ;
#51874 = CARTESIAN_POINT ( 'NONE',  ( 116.7951252716678425, -39.38782978912111332, 48.61479194265253057 ) ) ;
#51873 = FACE_OUTER_BOUND ( 'NONE', #51271, .T. ) ;
#51875 = CARTESIAN_POINT ( 'NONE',  ( 82.60038231476902126, -35.66080131299400335, 2.811527311783414973 ) ) ;
#51876 = VECTOR ( 'NONE', #18511, 1000.000000000000000 ) ;
#51877 = ORIENTED_EDGE ( 'NONE', *, *, #80695, .T. ) ;
#51878 = CARTESIAN_POINT ( 'NONE',  ( 134.0664832912739826, -9.029447159941003775, 4.925625275910997303 ) ) ;
#51879 = EDGE_LOOP ( 'NONE', ( #69986, #3693, #40332, #68788 ) ) ;
#51880 = CARTESIAN_POINT ( 'NONE',  ( 101.4370486012140589, -28.02035706366318379, 66.54514908543396245 ) ) ;
#51882 = ORIENTED_EDGE ( 'NONE', *, *, #88673, .T. ) ;
#51881 = CARTESIAN_POINT ( 'NONE',  ( 4.354213876134587657, 94.48073875936546528, 130.4833586261829055 ) ) ;
#51883 = CARTESIAN_POINT ( 'NONE',  ( 96.21411768969888101, -32.03111041547180804, 207.0013395616249738 ) ) ;
#51884 = DIRECTION ( 'NONE',  ( 0.000000000000000000, -1.000000000000000000, 0.000000000000000000 ) ) ;
#51885 = FACE_OUTER_BOUND ( 'NONE', #88837, .T. ) ;
#51886 = CARTESIAN_POINT ( 'NONE',  ( 107.0667039024470313, -104.2784471599420755, -19.78219314458201694 ) ) ;
#51887 = DIRECTION ( 'NONE',  ( 0.000000000000000000, 1.000000000000000000, 0.000000000000000000 ) ) ;
#51888 = CARTESIAN_POINT ( 'NONE',  ( 146.3607517370862752, -137.9410632998380208, 246.8967281812609826 ) ) ;
#51889 = CARTESIAN_POINT ( 'NONE',  ( 97.86670531118147665, -40.64952528798283993, 96.64701509883359165 ) ) ;
#51890 = CARTESIAN_POINT ( 'NONE',  ( 116.9310496459150244, -33.53114825773879915, 134.0880062282919880 ) ) ;
#51891 = AXIS2_PLACEMENT_3D ( 'NONE', #82805, #18762, #39643 ) ;
#51892 = VERTEX_POINT ( 'NONE', #74115 ) ;
#51893 = EDGE_LOOP ( 'NONE', ( #36333, #86207 ) ) ;
#51894 = CIRCLE ( 'NONE', #44648, 2.750000000000002665 ) ;
#51895 = CARTESIAN_POINT ( 'NONE',  ( 99.44206372185087162, -32.21319818083724584, 82.33301187732594428 ) ) ;
#51896 = DIRECTION ( 'NONE',  ( -1.000000000000000000, -3.360405532702990443E-14, 0.000000000000000000 ) ) ;
#51897 = ADVANCED_FACE ( 'NONE', ( #11897 ), #66901, .F. ) ;
#51899 = FACE_OUTER_BOUND ( 'NONE', #21755, .T. ) ;
#51898 = CARTESIAN_POINT ( 'NONE',  ( 112.1213531720969883, -45.14146623880446185, 234.0070538473389377 ) ) ;
#51900 = CARTESIAN_POINT ( 'NONE',  ( -103.1875000000000000, 127.0000000000000000, -7.937500000001080913 ) ) ;
#51901 = FACE_OUTER_BOUND ( 'NONE', #32496, .T. ) ;
#51902 = EDGE_CURVE ( 'NONE', #81089, #49254, #11286, .T. ) ;
#51903 = CARTESIAN_POINT ( 'NONE',  ( 118.5469577077832497, 69.93366089391886931, 1.674277437723032502 ) ) ;
#51904 = EDGE_CURVE ( 'NONE', #62846, #78275, #62269, .T. ) ;
#51905 = CARTESIAN_POINT ( 'NONE',  ( -5.625308623692421683, 71.15616178428264504, 118.4230398497201122 ) ) ;
#51906 = DIRECTION ( 'NONE',  ( 0.000000000000000000, 1.000000000000000000, 0.000000000000000000 ) ) ;
#51907 = DIRECTION ( 'NONE',  ( -0.7071067708032388044, -0.0001211784769776682566, -0.7071067811865423547 ) ) ;
#51908 = CARTESIAN_POINT ( 'NONE',  ( 96.69266148864264210, -35.94780844399461017, 146.2670538473399517 ) ) ;
#51909 = ORIENTED_EDGE ( 'NONE', *, *, #63824, .F. ) ;
#51910 = ORIENTED_EDGE ( 'NONE', *, *, #27765, .F. ) ;
#51911 = EDGE_CURVE ( 'NONE', #54222, #48446, #77260, .T. ) ;
#51912 = EDGE_CURVE ( 'NONE', #5603, #34522, #15116, .T. ) ;
#51913 = CARTESIAN_POINT ( 'NONE',  ( 127.4144167604540030, -85.80981773760922238, 250.2201230397200220 ) ) ;
#51914 = CARTESIAN_POINT ( 'NONE',  ( 99.09570913538954073, -30.55043167795444248, 151.8022919350126756 ) ) ;
#51915 = CARTESIAN_POINT ( 'NONE',  ( 0.000000000000000000, 11.42999999999999972, 0.000000000000000000 ) ) ;
#51916 = CARTESIAN_POINT ( 'NONE',  ( 101.9931138818980259, -45.44578100715379776, 103.1564127035998695 ) ) ;
#51917 = EDGE_CURVE ( 'NONE', #39822, #6347, #43161, .T. ) ;
#51918 = AXIS2_PLACEMENT_3D ( 'NONE', #43609, #52193, #73111 ) ;
#51919 = FACE_OUTER_BOUND ( 'NONE', #39331, .T. ) ;
#51920 = EDGE_CURVE ( 'NONE', #5997, #55129, #57238, .T. ) ;
#51921 = CARTESIAN_POINT ( 'NONE',  ( 101.9844316336549070, -45.87267731258258152, 187.1727681330539781 ) ) ;
#51922 = CARTESIAN_POINT ( 'NONE',  ( 135.7779513194176957, -38.88977919476615597, 7.751962620083525657 ) ) ;
#51923 = VERTEX_POINT ( 'NONE', #55878 ) ;
#51925 = ORIENTED_EDGE ( 'NONE', *, *, #65282, .F. ) ;
#51924 = ORIENTED_EDGE ( 'NONE', *, *, #6749, .F. ) ;
#51926 = CARTESIAN_POINT ( 'NONE',  ( 100.9418374907563276, -44.69577378954579672, 63.05520604563989906 ) ) ;
#51927 = LINE ( 'NONE', #71971, #14488 ) ;
#51928 = LINE ( 'NONE', #64261, #49822 ) ;
#51929 = EDGE_CURVE ( 'NONE', #41258, #75328, #16016, .T. ) ;
#51930 = CARTESIAN_POINT ( 'NONE',  ( 111.0677264286952521, -45.23305914580045339, 284.3463452106589102 ) ) ;
#51931 = AXIS2_PLACEMENT_3D ( 'NONE', #41966, #76961, #48322 ) ;
#51932 = DIRECTION ( 'NONE',  ( 0.000000000000000000, 0.000000000000000000, -1.000000000000000000 ) ) ;
#51933 = ORIENTED_EDGE ( 'NONE', *, *, #39232, .T. ) ;
#51934 = CIRCLE ( 'NONE', #66409, 3.999999999999992895 ) ;
#51935 = CONICAL_SURFACE ( 'NONE', #73745, 88.90000000000000568, 0.7853981633974621568 ) ;
#51936 = CARTESIAN_POINT ( 'NONE',  ( 116.1871362286084235, -39.57816415692806089, 9.635625275910941312 ) ) ;
#51937 = CARTESIAN_POINT ( 'NONE',  ( 82.79786375350293781, -18.40984252624906858, 6.777538624683209889 ) ) ;
#51938 = VERTEX_POINT ( 'NONE', #13677 ) ;
#51939 = EDGE_LOOP ( 'NONE', ( #9366, #16114, #36092, #40541 ) ) ;
#51940 = PLANE ( 'NONE',  #44428 ) ;
#51941 = ORIENTED_EDGE ( 'NONE', *, *, #88960, .T. ) ;
#51942 = ORIENTED_EDGE ( 'NONE', *, *, #68524, .T. ) ;
#51943 = DIRECTION ( 'NONE',  ( 1.000000000000000078E-15, -1.000000000000000083E-30, -1.000000000000000000 ) ) ;
#51944 = CIRCLE ( 'NONE', #54866, 13.16666666666670160 ) ;
#51945 = CARTESIAN_POINT ( 'NONE',  ( 101.6581149080599573, -43.36298066831790265, 11.45527697093296027 ) ) ;
#51946 = CARTESIAN_POINT ( 'NONE',  ( 116.8159443494545826, -40.58124828358739222, 193.5270538473389479 ) ) ;
#51947 = CARTESIAN_POINT ( 'NONE',  ( 96.62907006607237292, -36.88702529232764249, 136.3384824187679385 ) ) ;
#51948 = DIRECTION ( 'NONE',  ( 0.000000000000000000, 0.000000000000000000, -1.000000000000000000 ) ) ;
#51949 = CARTESIAN_POINT ( 'NONE',  ( 110.8167803534805813, -26.33188723323253910, 245.7889586092439629 ) ) ;
#51950 = CYLINDRICAL_SURFACE ( 'NONE', #54263, 2.117000000000007987 ) ;
#51951 = DIRECTION ( 'NONE',  ( -1.000000000000000000, 0.000000000000000000, -3.491483361109380094E-15 ) ) ;
#51952 = ORIENTED_EDGE ( 'NONE', *, *, #55152, .T. ) ;
#51953 = EDGE_CURVE ( 'NONE', #51387, #29395, #10448, .T. ) ;
#51954 = VERTEX_POINT ( 'NONE', #4074 ) ;
#51955 = EDGE_CURVE ( 'NONE', #17979, #52932, #10006, .T. ) ;
#51956 = VECTOR ( 'NONE', #53133, 1000.000000000000000 ) ;
#51957 = CIRCLE ( 'NONE', #17184, 29.00000000000000000 ) ;
#51958 = CARTESIAN_POINT ( 'NONE',  ( 110.7116931949060614, -48.05822654157750407, 207.8241967044819489 ) ) ;
#51959 = VERTEX_POINT ( 'NONE', #31775 ) ;
#51960 = CARTESIAN_POINT ( 'NONE',  ( 102.0509295376110117, -46.57948817496540528, 172.2137205140059564 ) ) ;
#51961 = CARTESIAN_POINT ( 'NONE',  ( 113.2442291481513053, -28.75770190615245170, 264.5523025444954897 ) ) ;
#51962 = LINE ( 'NONE', #9005, #56623 ) ;
#51963 = DIRECTION ( 'NONE',  ( 3.100000000000000258E-29, -3.100000000000000044E-14, -1.000000000000000000 ) ) ;
#51964 = CARTESIAN_POINT ( 'NONE',  ( 144.0637245237351749, -140.6784087391956746, 245.5331728883010101 ) ) ;
#51967 = CARTESIAN_POINT ( 'NONE',  ( 111.4711666614668673, -26.61707918639095993, 280.7375300378156453 ) ) ;
#51966 = CARTESIAN_POINT ( 'NONE',  ( 25.56670390244797275, -62.87844715994099687, 173.2178068554149775 ) ) ;
#51965 = DIRECTION ( 'NONE',  ( 1.000000000000000000, 0.000000000000000000, 0.000000000000000000 ) ) ;
#51968 = DIRECTION ( 'NONE',  ( 0.000000000000000000, 0.000000000000000000, 1.000000000000000000 ) ) ;
#51969 = CARTESIAN_POINT ( 'NONE',  ( 226.4410000000000025, 40.03750000000000142, -63.94449999999999790 ) ) ;
#51970 = PLANE ( 'NONE',  #6350 ) ;
#51971 = DIRECTION ( 'NONE',  ( -0.7071067811855900054, -0.7071067811875051401, 0.000000000000000000 ) ) ;
#51972 = CARTESIAN_POINT ( 'NONE',  ( 162.8595971212720031, -23.19206098994090581, -5.074374724088000832 ) ) ;
#51973 = CARTESIAN_POINT ( 'NONE',  ( 127.0664832912738405, -46.72944715994102438, -4.970821333495669236 ) ) ;
#51975 = ORIENTED_EDGE ( 'NONE', *, *, #71848, .F. ) ;
#51974 = CARTESIAN_POINT ( 'NONE',  ( 108.0557358071366423, -44.68002202782491139, 195.5838068554168103 ) ) ;
#51976 = AXIS2_PLACEMENT_3D ( 'NONE', #40249, #60687, #33443 ) ;
#51977 = CARTESIAN_POINT ( 'NONE',  ( 135.5597725514459171, -21.04085022828651930, 7.869587501222441439 ) ) ;
#51978 = CARTESIAN_POINT ( 'NONE',  ( 117.0895389762686136, -39.67643183956238317, 183.5984824187679578 ) ) ;
#51979 = CARTESIAN_POINT ( 'NONE',  ( 96.08760325403525826, -38.00935872415581684, 82.43086337114895912 ) ) ;
#51980 = CARTESIAN_POINT ( 'NONE',  ( 96.09249528944252461, -35.06539016137039511, 217.1946728949589840 ) ) ;
#51981 = PLANE ( 'NONE',  #47450 ) ;
#51982 = FACE_OUTER_BOUND ( 'NONE', #62170, .T. ) ;
#51984 = CARTESIAN_POINT ( 'NONE',  ( 117.0243171429062556, -35.72162122982938826, 39.90646649224381548 ) ) ;
#51983 = FACE_OUTER_BOUND ( 'NONE', #86625, .T. ) ;
#51985 = DIRECTION ( 'NONE',  ( 0.000000000000000000, 0.000000000000000000, 1.000000000000000000 ) ) ;
#51986 = CARTESIAN_POINT ( 'NONE',  ( 0.000000000000000000, 65.60000000000000853, 0.000000000000000000 ) ) ;
#51987 = CARTESIAN_POINT ( 'NONE',  ( 116.3283240494693160, -32.94276334974209419, 64.13562527591099638 ) ) ;
#51988 = VECTOR ( 'NONE', #42763, 1000.000000000000000 ) ;
#51989 = VERTEX_POINT ( 'NONE', #64524 ) ;
#51990 = ORIENTED_EDGE ( 'NONE', *, *, #17537, .F. ) ;
#51991 = CARTESIAN_POINT ( 'NONE',  ( 115.3391490808644875, -34.60362203641794565, 123.4495626852199734 ) ) ;
#51992 = VECTOR ( 'NONE', #84716, 1000.000000000000000 ) ;
#51994 = VERTEX_POINT ( 'NONE', #38151 ) ;
#51993 = CARTESIAN_POINT ( 'NONE',  ( -10.33024153997673089, 89.94921403597288645, -130.1468737228267685 ) ) ;
#51995 = CARTESIAN_POINT ( 'NONE',  ( 117.3497117099303892, -32.73958051198275854, 90.10895860924395606 ) ) ;
#51996 = CARTESIAN_POINT ( 'NONE',  ( 62.03742497533659872, -23.42844715994041493, 129.9678068554150911 ) ) ;
#51997 = AXIS2_PLACEMENT_3D ( 'NONE', #81001, #25556, #88258 ) ;
#51998 = CARTESIAN_POINT ( 'NONE',  ( 77.58678459498788982, -17.53883969337279680, 7.103318745423876202 ) ) ;
#51999 = LINE ( 'NONE', #31130, #5576 ) ;
#52000 = VECTOR ( 'NONE', #50771, 1000.000000000000000 ) ;
#52001 = CARTESIAN_POINT ( 'NONE',  ( 116.8666057829012033, -37.25052826422871277, 18.78419670448294809 ) ) ;
#52002 = VERTEX_POINT ( 'NONE', #24087 ) ;
#52003 = ADVANCED_FACE ( 'NONE', ( #85441 ), #57699, .F. ) ;
#52004 = ORIENTED_EDGE ( 'NONE', *, *, #10710, .T. ) ;
#52005 = ORIENTED_EDGE ( 'NONE', *, *, #62910, .F. ) ;
#52006 = DIRECTION ( 'NONE',  ( 0.000000000000000000, -0.8660254037844427044, 0.4999999999999928391 ) ) ;
#52007 = CARTESIAN_POINT ( 'NONE',  ( 78.56670390244701707, -90.27844715994098124, 45.21780685541799727 ) ) ;
#52008 = CARTESIAN_POINT ( 'NONE',  ( 105.7995184923274792, -26.72403496536887246, 116.1772919422014070 ) ) ;
#52009 = LINE ( 'NONE', #58401, #42609 ) ;
#52010 = LINE ( 'NONE', #79770, #55008 ) ;
#52011 = EDGE_CURVE ( 'NONE', #26172, #31238, #54832, .T. ) ;
#52012 = CARTESIAN_POINT ( 'NONE',  ( 100.9550256842345703, -28.70674946826466467, 51.59535640286041058 ) ) ;
#52013 = ADVANCED_FACE ( 'NONE', ( #10886 ), #79055, .T. ) ;
#52014 = AXIS2_PLACEMENT_3D ( 'NONE', #68962, #5395, #7187 ) ;
#52015 = LINE ( 'NONE', #4792, #53222 ) ;
#52016 = ADVANCED_FACE ( 'NONE', ( #71789 ), #45390, .F. ) ;
#52017 = CARTESIAN_POINT ( 'NONE',  ( 78.17826422383464546, 92.64969027323469675, 89.13001032377241017 ) ) ;
#52018 = CARTESIAN_POINT ( 'NONE',  ( 101.9712125536870957, -27.65933791914790874, 60.48419670448296159 ) ) ;
#52019 = EDGE_LOOP ( 'NONE', ( #84079, #79411 ) ) ;
#52020 = VERTEX_POINT ( 'NONE', #72682 ) ;
#52021 = EDGE_CURVE ( 'NONE', #39595, #73742, #1200, .T. ) ;
#52022 = DIRECTION ( 'NONE',  ( 0.000000000000000000, 0.000000000000000000, -1.000000000000000000 ) ) ;
#52023 = CARTESIAN_POINT ( 'NONE',  ( -24.79284581386642827, 127.0000000000000000, 0.000000000000000000 ) ) ;
#52024 = DIRECTION ( 'NONE',  ( 0.000000000000000000, 1.000000000000000000, 0.000000000000000000 ) ) ;
#52025 = CARTESIAN_POINT ( 'NONE',  ( 115.4543170047500098, -34.59750657913997429, 166.8547570362579506 ) ) ;
#52026 = CIRCLE ( 'NONE', #56384, 5.041900000000001825 ) ;
#52027 = EDGE_CURVE ( 'NONE', #79315, #50547, #66456, .T. ) ;
#52028 = ADVANCED_FACE ( 'NONE', ( #30007 ), #23218, .T. ) ;
#52029 = CARTESIAN_POINT ( 'NONE',  ( 87.06648329127403940, -54.72944906728955061, -4.824374724089049771 ) ) ;
#52030 = ORIENTED_EDGE ( 'NONE', *, *, #35, .T. ) ;
#52031 = ORIENTED_EDGE ( 'NONE', *, *, #43886, .F. ) ;
#52032 = DIRECTION ( 'NONE',  ( 1.000000000000000000, 4.299999999999999979E-14, 1.000000000000000078E-15 ) ) ;
#52033 = EDGE_LOOP ( 'NONE', ( #72028, #76432, #28337, #66149 ) ) ;
#52034 = ORIENTED_EDGE ( 'NONE', *, *, #39717, .F. ) ;
#52035 = CARTESIAN_POINT ( 'NONE',  ( 107.0664832912739968, -36.72944715994100306, 287.6356252759109680 ) ) ;
#52036 = EDGE_CURVE ( 'NONE', #8519, #3245, #3626, .T. ) ;
#52037 = CARTESIAN_POINT ( 'NONE',  ( 97.58318307924886881, -33.33272491023742390, 172.4844404487539578 ) ) ;
#52038 = AXIS2_PLACEMENT_3D ( 'NONE', #55091, #82852, #76014 ) ;
#52039 = DIRECTION ( 'NONE',  ( 0.000000000000000000, 0.000000000000000000, -1.000000000000000000 ) ) ;
#52040 = CARTESIAN_POINT ( 'NONE',  ( 32.06670390244800473, -33.35206098992711077, 342.9256252759119548 ) ) ;
#52041 = FACE_OUTER_BOUND ( 'NONE', #42668, .T. ) ;
#52042 = EDGE_LOOP ( 'NONE', ( #14350, #82025, #61116 ) ) ;
#52043 = ORIENTED_EDGE ( 'NONE', *, *, #44642, .T. ) ;
#52044 = VERTEX_POINT ( 'NONE', #17269 ) ;
#52045 = CARTESIAN_POINT ( 'NONE',  ( 109.4710126485015280, -28.41565358443893174, 212.6585665600669870 ) ) ;
#52046 = VECTOR ( 'NONE', #12761, 1000.000000000000000 ) ;
#52047 = CARTESIAN_POINT ( 'NONE',  ( 117.3857798876165788, -38.35993227889734669, 113.7013395616249767 ) ) ;
#52048 = CARTESIAN_POINT ( 'NONE',  ( 115.7104945841387718, -43.58108136993647719, 48.30514908543492680 ) ) ;
#52049 = CARTESIAN_POINT ( 'NONE',  ( 100.8867414696376272, -44.69961926644128170, 252.0525101340111860 ) ) ;
#52050 = DIRECTION ( 'NONE',  ( 0.9068632946707755327, -0.4214249218767993077, 0.000000000000000000 ) ) ;
#52051 = CARTESIAN_POINT ( 'NONE',  ( 131.0667039024480971, -58.72944715994092491, 207.5838068554170377 ) ) ;
#52052 = CARTESIAN_POINT ( 'NONE',  ( 117.7791004155048853, -34.00661502546044801, 165.0365776568629315 ) ) ;
#52053 = DIRECTION ( 'NONE',  ( 0.000000000000000000, 0.000000000000000000, 1.000000000000000000 ) ) ;
#52054 = VERTEX_POINT ( 'NONE', #2304 ) ;
#52055 = AXIS2_PLACEMENT_3D ( 'NONE', #34844, #5810, #88481 ) ;
#52056 = LINE ( 'NONE', #17570, #71414 ) ;
#52057 = ORIENTED_EDGE ( 'NONE', *, *, #51452, .T. ) ;
#52058 = ORIENTED_EDGE ( 'NONE', *, *, #85735, .F. ) ;
#52059 = AXIS2_PLACEMENT_3D ( 'NONE', #18823, #74240, #39699 ) ;
#52060 = LINE ( 'NONE', #11192, #60715 ) ;
#52061 = CARTESIAN_POINT ( 'NONE',  ( 22.49541547940750519, -78.44951497180814215, 342.9256252759109884 ) ) ;
#52062 = EDGE_CURVE ( 'NONE', #74183, #70165, #69396, .T. ) ;
#52063 = ORIENTED_EDGE ( 'NONE', *, *, #87734, .T. ) ;
#52064 = DIRECTION ( 'NONE',  ( 0.000000000000000000, 1.000000000000000000, 0.000000000000000000 ) ) ;
#52065 = ORIENTED_EDGE ( 'NONE', *, *, #51955, .F. ) ;
#52066 = CARTESIAN_POINT ( 'NONE',  ( 99.04406183770223038, -42.84125761279484124, 176.8439586068464280 ) ) ;
#52067 = CARTESIAN_POINT ( 'NONE',  ( 112.7599586733956727, -27.95389904326713904, 69.61848241876793963 ) ) ;
#52068 = DIRECTION ( 'NONE',  ( 0.000000000000000000, 0.000000000000000000, 1.000000000000000000 ) ) ;
#52069 = DIRECTION ( 'NONE',  ( 0.7071067811865171526, 0.7071067811865779928, 7.071067811865164719E-16 ) ) ;
#52070 = CARTESIAN_POINT ( 'NONE',  ( -479.3614999999999782, 86.51875000000001137, 86.36305401447658880 ) ) ;
#52071 = CARTESIAN_POINT ( 'NONE',  ( 107.5699729851651938, -26.92841289699908458, 95.03562527591097364 ) ) ;
#52073 = CARTESIAN_POINT ( 'NONE',  ( 98.39792771585426578, -29.90889243069713288, 196.8080062282919869 ) ) ;
#52072 = CARTESIAN_POINT ( 'NONE',  ( 70.98999999999998067, 52.73749999999999716, -44.45000000000002416 ) ) ;
#52074 = DIRECTION ( 'NONE',  ( 0.000000000000000000, 0.000000000000000000, -1.000000000000000000 ) ) ;
#52075 = CARTESIAN_POINT ( 'NONE',  ( 86.72755763596096301, -122.7870702624433648, 250.2178068554179902 ) ) ;
#52076 = ORIENTED_EDGE ( 'NONE', *, *, #76553, .F. ) ;
#52077 = AXIS2_PLACEMENT_3D ( 'NONE', #29537, #15915, #24069 ) ;
#52078 = DIRECTION ( 'NONE',  ( 0.000000000000000000, 0.000000000000000000, -1.000000000000000000 ) ) ;
#52079 = CARTESIAN_POINT ( 'NONE',  ( 116.0667039024470739, -137.6784471599409301, 222.2178068554179902 ) ) ;
#52080 = CARTESIAN_POINT ( 'NONE',  ( 97.79672674250161890, -40.48067604376981166, 136.6328479018905284 ) ) ;
#52081 = CARTESIAN_POINT ( 'NONE',  ( 107.0664832912739968, -36.72944715994100306, 277.6356252759110248 ) ) ;
#52082 = EDGE_CURVE ( 'NONE', #13607, #88437, #79955, .T. ) ;
#52084 = EDGE_LOOP ( 'NONE', ( #81377, #37547 ) ) ;
#52083 = CARTESIAN_POINT ( 'NONE',  ( 97.99847537351134008, -44.43658864837386346, 226.8870538473399563 ) ) ;
#52085 = CARTESIAN_POINT ( 'NONE',  ( -179.8898777604655095, 20.32000000000000028, -12.69999999999999929 ) ) ;
#52086 = CARTESIAN_POINT ( 'NONE',  ( 110.7407540106703010, -26.28028736477551419, 250.8194347997206819 ) ) ;
#52087 = CARTESIAN_POINT ( 'NONE',  ( 109.2103426150987104, -26.48265019188898606, 135.9127681330539872 ) ) ;
#52088 = CARTESIAN_POINT ( 'NONE',  ( 108.4212757395327174, -26.73551752249970548, 250.9740451590128316 ) ) ;
#52089 = CARTESIAN_POINT ( 'NONE',  ( 81.20964327716589537, -39.23067567606557304, 8.021372095561080329 ) ) ;
#52090 = DIRECTION ( 'NONE',  ( 9.073094938289460781E-13, 1.000000000000000000, 0.000000000000000000 ) ) ;
#52091 = CARTESIAN_POINT ( 'NONE',  ( 101.9933639039164035, -45.44591285733346098, 263.1565428173477130 ) ) ;
#52092 = ORIENTED_EDGE ( 'NONE', *, *, #80203, .F. ) ;
#52093 = ADVANCED_FACE ( 'NONE', ( #30453 ), #16378, .F. ) ;
#52094 = ORIENTED_EDGE ( 'NONE', *, *, #12315, .F. ) ;
#52095 = ORIENTED_EDGE ( 'NONE', *, *, #33789, .F. ) ;
#52096 = ORIENTED_EDGE ( 'NONE', *, *, #74640, .T. ) ;
#52097 = PLANE ( 'NONE',  #77042 ) ;
#52098 = CARTESIAN_POINT ( 'NONE',  ( 96.88896422860915436, -30.65880273170215276, 276.8984824187680829 ) ) ;
#52099 = DIRECTION ( 'NONE',  ( 0.000000000000000000, 0.000000000000000000, 1.000000000000000000 ) ) ;
#52100 = CARTESIAN_POINT ( 'NONE',  ( 51.06670390244899238, -32.29483332968430886, -5.074374724088000832 ) ) ;
#52101 = VECTOR ( 'NONE', #48624, 1000.000000000000000 ) ;
#52103 = CARTESIAN_POINT ( 'NONE',  ( 88.44575049335495009, 71.76236341258000095, 78.94931995840828165 ) ) ;
#52102 = FACE_OUTER_BOUND ( 'NONE', #20841, .T. ) ;
#52104 = CARTESIAN_POINT ( 'NONE',  ( 99.14828105993673546, -39.93229045078558670, 206.0552769709339884 ) ) ;
#52105 = ORIENTED_EDGE ( 'NONE', *, *, #17799, .F. ) ;
#52106 = EDGE_LOOP ( 'NONE', ( #13618, #80648, #19422, #77906 ) ) ;
#52107 = AXIS2_PLACEMENT_3D ( 'NONE', #38397, #79768, #72046 ) ;
#52109 = ORIENTED_EDGE ( 'NONE', *, *, #10521, .T. ) ;
#52108 = CIRCLE ( 'NONE', #17388, 11.57110091390437034 ) ;
#52110 = CARTESIAN_POINT ( 'NONE',  ( 87.31648329127402519, -54.62589567669624557, 14.92562527591095112 ) ) ;
#52111 = PLANE ( 'NONE',  #75294 ) ;
#52112 = CARTESIAN_POINT ( 'NONE',  ( 63.31670390244797630, -58.72944715994110254, 310.9178068554150514 ) ) ;
#52113 = EDGE_CURVE ( 'NONE', #20491, #60190, #58577, .T. ) ;
#52114 = CARTESIAN_POINT ( 'NONE',  ( 101.4092135025303776, -29.90862777007100703, 37.05872616303995670 ) ) ;
#52115 = EDGE_CURVE ( 'NONE', #48663, #4991, #67898, .T. ) ;
#52116 = CARTESIAN_POINT ( 'NONE',  ( 118.0645351272586510, 89.26692529358290074, 10.78628659036793813 ) ) ;
#52117 = CIRCLE ( 'NONE', #1398, 9.999999999999994671 ) ;
#52118 = EDGE_CURVE ( 'NONE', #64715, #1134, #9876, .T. ) ;
#52119 = LINE ( 'NONE', #72607, #85416 ) ;
#52120 = COLOUR_RGB ( '', 0.66274510, 0.83137255, 0.94901961) ;
#52121 = DIRECTION ( 'NONE',  ( -1.000200923085726652E-15, -1.000000000000000000, 0.000000000000000000 ) ) ;
#52122 = EDGE_LOOP ( 'NONE', ( #43467, #36737, #64975, #20954 ) ) ;
#52123 = ADVANCED_FACE ( 'NONE', ( #18145 ), #80845, .F. ) ;
#52124 = CARTESIAN_POINT ( 'NONE',  ( 196.2150000000000034, 37.33800000000000097, 60.32499999999999574 ) ) ;
#52125 = ORIENTED_EDGE ( 'NONE', *, *, #44685, .T. ) ;
#52126 = FACE_OUTER_BOUND ( 'NONE', #64103, .T. ) ;
#52127 = CARTESIAN_POINT ( 'NONE',  ( 115.6864120445923163, -37.50259225211298286, 31.56142370292397459 ) ) ;
#52128 = CYLINDRICAL_SURFACE ( 'NONE', #63882, 12.70000000000000107 ) ;
#52129 = CARTESIAN_POINT ( 'NONE',  ( -487.2989999999999782, 14.28750000000023945, 19.36139197104649767 ) ) ;
#52130 = EDGE_CURVE ( 'NONE', #21819, #32172, #47580, .T. ) ;
#52131 = AXIS2_PLACEMENT_3D ( 'NONE', #5298, #4847, #25730 ) ;
#52132 = CARTESIAN_POINT ( 'NONE',  ( 92.05992619857352111, 79.25941250729452747, -74.70281015415415027 ) ) ;
#52133 = ORIENTED_EDGE ( 'NONE', *, *, #22841, .T. ) ;
#52134 = DIRECTION ( 'NONE',  ( -0.7071067811865431318, 0.7071067811865517916, -7.071067811865425043E-16 ) ) ;
#52135 = CARTESIAN_POINT ( 'NONE',  ( 120.5286047550879260, 58.23918486294396502, -50.17733349311141211 ) ) ;
#52136 = ORIENTED_EDGE ( 'NONE', *, *, #23831, .T. ) ;
#52137 = CARTESIAN_POINT ( 'NONE',  ( 101.6781192058861762, -27.07830111727894362, 105.4937205140069665 ) ) ;
#52138 = ORIENTED_EDGE ( 'NONE', *, *, #85798, .F. ) ;
#52139 = CARTESIAN_POINT ( 'NONE',  ( 101.7280645633873775, -29.41412380334073973, 29.98861030426797214 ) ) ;
#52140 = LINE ( 'NONE', #31270, #59058 ) ;
#52141 = CARTESIAN_POINT ( 'NONE',  ( 112.5007446479794453, -45.21116328700192355, 64.46158330589696561 ) ) ;
#52142 = PLANE ( 'NONE',  #70913 ) ;
#52143 = CARTESIAN_POINT ( 'NONE',  ( 71.06648329127399677, -8.729447159940999512, 323.8756252759120002 ) ) ;
#52144 = CARTESIAN_POINT ( 'NONE',  ( 131.8431396993165947, -68.25097877586425454, 247.0389312302800136 ) ) ;
#52145 = AXIS2_PLACEMENT_3D ( 'NONE', #30155, #23802, #51906 ) ;
#52146 = CARTESIAN_POINT ( 'NONE',  ( 111.1374431767090414, -47.03053892029802796, 18.88800622829195319 ) ) ;
#52147 = CARTESIAN_POINT ( 'NONE',  ( 162.5667039024460223, -19.82844715994111340, -5.074374724088000832 ) ) ;
#52148 = ORIENTED_EDGE ( 'NONE', *, *, #10913, .T. ) ;
#52149 = CARTESIAN_POINT ( 'NONE',  ( 19.56648329127400032, -18.82844715994099971, -5.074374724088000832 ) ) ;
#52150 = ORIENTED_EDGE ( 'NONE', *, *, #82033, .F. ) ;
#52151 = CARTESIAN_POINT ( 'NONE',  ( 77.45242755740704865, -19.60567372264617703, 2.908038864009607316 ) ) ;
#52152 = ORIENTED_EDGE ( 'NONE', *, *, #28129, .T. ) ;
#52153 = ORIENTED_EDGE ( 'NONE', *, *, #27231, .T. ) ;
#52155 = AXIS2_PLACEMENT_3D ( 'NONE', #12847, #80541, #60977 ) ;
#52154 = LINE ( 'NONE', #58979, #10146 ) ;
#52156 = CARTESIAN_POINT ( 'NONE',  ( 97.99937763885726838, -40.39701179870337455, 206.6327681330539860 ) ) ;
#52157 = LINE ( 'NONE', #25372, #11795 ) ;
#52158 = CARTESIAN_POINT ( 'NONE',  ( 147.0665874381622018, -67.87844715994090450, 245.5130140176639770 ) ) ;
#52159 = CARTESIAN_POINT ( 'NONE',  ( 110.7944688027788658, -46.46518603654068613, 58.86705384733998159 ) ) ;
#52160 = LINE ( 'NONE', #23622, #47904 ) ;
#52161 = EDGE_LOOP ( 'NONE', ( #87733, #35653, #66378, #31898 ) ) ;
#52162 = DIRECTION ( 'NONE',  ( 1.000000000000000000, 4.163336342344333240E-14, 0.000000000000000000 ) ) ;
#52163 = VECTOR ( 'NONE', #4317, 1000.000000000000000 ) ;
#52164 = LINE ( 'NONE', #39458, #79618 ) ;
#52165 = EDGE_CURVE ( 'NONE', #82562, #8401, #17205, .T. ) ;
#52166 = EDGE_LOOP ( 'NONE', ( #80856, #67056, #29176, #76204, #13389, #79156 ) ) ;
#52167 = LINE ( 'NONE', #51284, #38729 ) ;
#52168 = CARTESIAN_POINT ( 'NONE',  ( 105.7138707427173898, -46.72361436802630408, 113.4695631962065505 ) ) ;
#52169 = CARTESIAN_POINT ( 'NONE',  ( 115.8368392028494185, -44.66223131803950963, 233.2413395616259493 ) ) ;
#52170 = DIRECTION ( 'NONE',  ( 0.000000000000000000, 0.000000000000000000, 1.000000000000000000 ) ) ;
#52171 = EDGE_CURVE ( 'NONE', #35753, #834, #88279, .T. ) ;
#52172 = LINE ( 'NONE', #33101, #7121 ) ;
#52173 = CARTESIAN_POINT ( 'NONE',  ( 77.67297288197859473, -38.08739819366309121, 2.653088468869586602 ) ) ;
#52174 = CARTESIAN_POINT ( 'NONE',  ( 110.9972015515846238, -44.34532242709460093, 272.3781341137911909 ) ) ;
#52176 = CARTESIAN_POINT ( 'NONE',  ( 117.3173117416416744, -32.65705981835812111, 95.13943479972097350 ) ) ;
#52175 = DIRECTION ( 'NONE',  ( 4.194175870806139918E-14, -1.000000000000000000, 0.000000000000000000 ) ) ;
#52177 = CARTESIAN_POINT ( 'NONE',  ( 117.7358725014768481, 73.84217107435090099, 56.42336322934903592 ) ) ;
#52178 = CARTESIAN_POINT ( 'NONE',  ( 102.5972826210866060, -46.89011293525640411, 132.2346728949579528 ) ) ;
#52179 = EDGE_LOOP ( 'NONE', ( #32714, #11969, #30697, #88480, #4432, #64848, #26809, #60910, #25059, #5882, #19363, #3153, #10824, #32507, #7208, #80918, #52805, #5780, #15781, #74623, #21633, #59282, #51363, #28652, #85777, #81732, #43869, #19980, #88909, #83936, #26595, #25915, #78981, #65093, #17768, #50051, #24832, #46630, #32603, #61713, #66823, #68341, #60202, #25599, #38324, #637, #49890, #80422, #66291, #66186, #23028, #46244, #57451, #69236, #39681, #41845, #22462, #80332, #5163, #3776, #10980, #20223, #84019, #32342, #48159, #29633, #29107, #39563, #6028, #34716, #33596, #67729, #31604, #41024, #85380, #15105, #1878, #68091, #36432, #5982, #28964, #18716, #76698, #43586, #56296, #9979, #46329, #51157, #60441, #33859, #59856, #56262, #88298, #3705, #25548, #89560 ) ) ;
#52180 = CARTESIAN_POINT ( 'NONE',  ( 132.7628207310606854, -21.15113447712359473, 7.957506268076239841 ) ) ;
#52181 = ORIENTED_EDGE ( 'NONE', *, *, #60777, .F. ) ;
#52182 = CONICAL_SURFACE ( 'NONE', #34837, 16.33514202138213633, 0.7853981633974430610 ) ;
#52183 = DIRECTION ( 'NONE',  ( 0.000000000000000000, -1.000000000000000000, 0.000000000000000000 ) ) ;
#52184 = CARTESIAN_POINT ( 'NONE',  ( 131.3179999999999836, 37.33800000000000097, 50.79999999999999716 ) ) ;
#52185 = PLANE ( 'NONE',  #41431 ) ;
#52186 = DIRECTION ( 'NONE',  ( -1.000000000000000000, 0.000000000000000000, 0.000000000000000000 ) ) ;
#52187 = ORIENTED_EDGE ( 'NONE', *, *, #46406, .F. ) ;
#52188 = CARTESIAN_POINT ( 'NONE',  ( 99.09552584949113907, -30.55066422794973136, 50.80231514688692585 ) ) ;
#52190 = ORIENTED_EDGE ( 'NONE', *, *, #10511, .F. ) ;
#52189 = CARTESIAN_POINT ( 'NONE',  ( 99.02022134730059122, -43.42753157066677261, 116.8784824187679732 ) ) ;
#52191 = CARTESIAN_POINT ( 'NONE',  ( 25.56670390244797275, -65.37844715994100397, 293.2178068554150627 ) ) ;
#52192 = AXIS2_PLACEMENT_3D ( 'NONE', #71782, #15926, #72674 ) ;
#52193 = DIRECTION ( 'NONE',  ( 0.000000000000000000, 1.809101308280369915E-15, -1.000000000000000000 ) ) ;
#52194 = LINE ( 'NONE', #72236, #6082 ) ;
#52195 = ORIENTED_EDGE ( 'NONE', *, *, #44355, .T. ) ;
#52196 = EDGE_CURVE ( 'NONE', #78219, #11954, #49076, .T. ) ;
#52197 = CARTESIAN_POINT ( 'NONE',  ( 113.8708677755033847, -44.65703921284106315, 108.1413395616249744 ) ) ;
#52198 = CARTESIAN_POINT ( 'NONE',  ( -2.170823869927923866, 1.527609608640607000E-59, -1.047975677455812069E-12 ) ) ;
#52199 = LINE ( 'NONE', #37270, #66649 ) ;
#52200 = CARTESIAN_POINT ( 'NONE',  ( 167.2371591254545535, -47.82818131005522133, 129.9678068554149775 ) ) ;
#52201 = DIRECTION ( 'NONE',  ( -1.000000000000000078E-15, 0.000000000000000000, -1.000000000000000000 ) ) ;
#52202 = ORIENTED_EDGE ( 'NONE', *, *, #69170, .T. ) ;
#52203 = VECTOR ( 'NONE', #45157, 1000.000000000000000 ) ;
#52204 = EDGE_LOOP ( 'NONE', ( #46689, #16995 ) ) ;
#52205 = CARTESIAN_POINT ( 'NONE',  ( 172.5664832912729878, -27.57844715994070484, 318.9256252759120116 ) ) ;
#52206 = DIRECTION ( 'NONE',  ( 0.000000000000000000, 0.000000000000000000, 1.000000000000000000 ) ) ;
#52207 = CARTESIAN_POINT ( 'NONE',  ( 2.323620343766204915E-14, 127.0000000000000000, 188.9759999999999991 ) ) ;
#52209 = FACE_OUTER_BOUND ( 'NONE', #51756, .T. ) ;
#52208 = CARTESIAN_POINT ( 'NONE',  ( 142.8838050580813785, -82.11588141944041297, 542.9756252759101471 ) ) ;
#52210 = LINE ( 'NONE', #65432, #47996 ) ;
#52211 = AXIS2_PLACEMENT_3D ( 'NONE', #66788, #59956, #39974 ) ;
#52212 = ORIENTED_EDGE ( 'NONE', *, *, #74885, .F. ) ;
#52213 = FACE_OUTER_BOUND ( 'NONE', #69694, .T. ) ;
#52214 = CARTESIAN_POINT ( 'NONE',  ( 106.3491918589965763, -46.48387837312645132, 218.5184824187679453 ) ) ;
#52215 = EDGE_CURVE ( 'NONE', #33892, #75678, #9941, .T. ) ;
#52217 = ORIENTED_EDGE ( 'NONE', *, *, #64878, .T. ) ;
#52216 = LINE ( 'NONE', #24996, #57416 ) ;
#52218 = CIRCLE ( 'NONE', #36308, 2.517500000000005844 ) ;
#52219 = CARTESIAN_POINT ( 'NONE',  ( 116.4365193811696457, -32.28633913640747011, 60.19086337114898555 ) ) ;
#52220 = EDGE_CURVE ( 'NONE', #51113, #86385, #14482, .T. ) ;
#52221 = CARTESIAN_POINT ( 'NONE',  ( 97.83900272812365984, -40.58357929434716738, 51.64132164664623303 ) ) ;
#52222 = EDGE_CURVE ( 'NONE', #57775, #76254, #56268, .T. ) ;
#52223 = DIRECTION ( 'NONE',  ( 0.000000000000000000, 1.000000000000000000, -0.000000000000000000 ) ) ;
#52224 = VECTOR ( 'NONE', #85108, 1000.000000000000000 ) ;
#52225 = ORIENTED_EDGE ( 'NONE', *, *, #41669, .T. ) ;
#52226 = CARTESIAN_POINT ( 'NONE',  ( 208.9149999999999920, 28.98850000000000193, -7.937500000000000000 ) ) ;
#52227 = EDGE_CURVE ( 'NONE', #63620, #11064, #22198, .T. ) ;
#52228 = ORIENTED_EDGE ( 'NONE', *, *, #14533, .T. ) ;
#52229 = ORIENTED_EDGE ( 'NONE', *, *, #20863, .F. ) ;
#52230 = CARTESIAN_POINT ( 'NONE',  ( 98.55918112442081735, -40.71722039560211925, 208.0949166392299787 ) ) ;
#52231 = AXIS2_PLACEMENT_3D ( 'NONE', #81840, #60925, #62719 ) ;
#52232 = CARTESIAN_POINT ( 'NONE',  ( 91.91441891875203396, -96.57077177933005885, -19.18411693322927292 ) ) ;
#52233 = CARTESIAN_POINT ( 'NONE',  ( 23.03812769098065161, 87.31235724081935246, 302.5802168940534216 ) ) ;
#52234 = DIRECTION ( 'NONE',  ( 0.7071067811874257591, -0.7071067811856692753, 2.899137802861360256E-29 ) ) ;
#52235 = EDGE_CURVE ( 'NONE', #88986, #56291, #55769, .T. ) ;
#52236 = CYLINDRICAL_SURFACE ( 'NONE', #47330, 7.937500000000000000 ) ;
#52237 = VERTEX_POINT ( 'NONE', #15382 ) ;
#52238 = CARTESIAN_POINT ( 'NONE',  ( 134.0664832912739826, -33.97944715994100306, 8.225625275910998013 ) ) ;
#52239 = DIRECTION ( 'NONE',  ( 1.000000000000000000, 0.000000000000000000, 0.000000000000000000 ) ) ;
#52240 = EDGE_CURVE ( 'NONE', #74190, #68597, #72388, .T. ) ;
#52241 = ORIENTED_EDGE ( 'NONE', *, *, #60023, .F. ) ;
#52242 = CARTESIAN_POINT ( 'NONE',  ( 101.3840881871039272, -27.98888560156178329, 25.53562527591096654 ) ) ;
#52243 = CARTESIAN_POINT ( 'NONE',  ( 1.664568416404320850, 95.16759698565884662, 118.5470925690480755 ) ) ;
#52244 = ORIENTED_EDGE ( 'NONE', *, *, #61301, .T. ) ;
#52245 = CARTESIAN_POINT ( 'NONE',  ( 107.0667039024470171, -79.67844715994094429, 138.7178068554180186 ) ) ;
#52246 = CARTESIAN_POINT ( 'NONE',  ( -23.75871628398702384, 82.54999999999999716, 275.4630000000000223 ) ) ;
#52247 = PLANE ( 'NONE',  #40380 ) ;
#52248 = DIRECTION ( 'NONE',  ( -2.981567257902526681E-15, 0.8571673007021100021, 0.5150380749100580413 ) ) ;
#52249 = CARTESIAN_POINT ( 'NONE',  ( 103.6242938494280423, -26.17725164406494542, 206.3394347997209763 ) ) ;
#52250 = DIRECTION ( 'NONE',  ( 0.000000000000000000, 0.000000000000000000, 1.000000000000000000 ) ) ;
#52251 = VERTEX_POINT ( 'NONE', #48505 ) ;
#52252 = CARTESIAN_POINT ( 'NONE',  ( 99.26130681012091372, -43.75918647830361863, 52.90991099019698396 ) ) ;
#52253 = DIRECTION ( 'NONE',  ( -0.7071067812160284349, 0.7071067811570665995, -7.071067812160292375E-16 ) ) ;
#52254 = ORIENTED_EDGE ( 'NONE', *, *, #13297, .T. ) ;
#52255 = EDGE_LOOP ( 'NONE', ( #7614, #52310 ) ) ;
#52256 = AXIS2_PLACEMENT_3D ( 'NONE', #28848, #34754, #76545 ) ;
#52257 = CARTESIAN_POINT ( 'NONE',  ( 81.91153210826661279, -16.68812259376749907, 2.188418746631556999 ) ) ;
#52258 = CARTESIAN_POINT ( 'NONE',  ( 90.44969454456416713, -53.34645651782494724, 219.5838068554169809 ) ) ;
#52259 = CARTESIAN_POINT ( 'NONE',  ( 41.56670390244783420, -36.32844715994104234, 249.9678068554150343 ) ) ;
#52260 = CARTESIAN_POINT ( 'NONE',  ( 98.22859028455410169, -39.55567757615634861, 129.3909475124479798 ) ) ;
#52261 = CARTESIAN_POINT ( 'NONE',  ( 113.2328747769256410, -45.16229216617723097, 224.0784824187679476 ) ) ;
#52262 = CARTESIAN_POINT ( 'NONE',  ( -3.174999999999644995, 24.56180297284579694, 33.98325472291465132 ) ) ;
#52263 = ORIENTED_EDGE ( 'NONE', *, *, #50738, .F. ) ;
#52264 = CARTESIAN_POINT ( 'NONE',  ( 136.8165183345649041, -36.90056224777460159, 3.101534470964323553 ) ) ;
#52265 = VECTOR ( 'NONE', #45768, 1000.000000000000000 ) ;
#52266 = EDGE_CURVE ( 'NONE', #28614, #84277, #49867, .T. ) ;
#52267 = ORIENTED_EDGE ( 'NONE', *, *, #32866, .F. ) ;
#52268 = VERTEX_POINT ( 'NONE', #1297 ) ;
#52269 = FACE_OUTER_BOUND ( 'NONE', #4394, .T. ) ;
#52270 = ORIENTED_EDGE ( 'NONE', *, *, #75210, .F. ) ;
#52271 = ORIENTED_EDGE ( 'NONE', *, *, #11484, .F. ) ;
#52272 = LINE ( 'NONE', #73189, #39604 ) ;
#52273 = CARTESIAN_POINT ( 'NONE',  ( -12.70000000000000107, 82.54999999999999716, -129.9368274816650910 ) ) ;
#52274 = EDGE_CURVE ( 'NONE', #1981, #9843, #73491, .T. ) ;
#52275 = DIRECTION ( 'NONE',  ( -1.000000000000000078E-15, -9.367723249499513438E-31, 1.000000000000000000 ) ) ;
#52276 = CARTESIAN_POINT ( 'NONE',  ( 115.3767887321059789, -38.82490071601502990, 123.0524198280769639 ) ) ;
#52277 = CARTESIAN_POINT ( 'NONE',  ( 115.9290394997688480, -31.15613903141374763, 34.27276813305396530 ) ) ;
#52278 = ORIENTED_EDGE ( 'NONE', *, *, #1006, .T. ) ;
#52279 = DIRECTION ( 'NONE',  ( -3.100000000000000258E-29, 3.100000000000000044E-14, 1.000000000000000000 ) ) ;
#52280 = VECTOR ( 'NONE', #65663, 1000.000000000000000 ) ;
#52281 = ORIENTED_EDGE ( 'NONE', *, *, #69624, .T. ) ;
#52282 = VECTOR ( 'NONE', #38606, 1000.000000000000114 ) ;
#52283 = DIRECTION ( 'NONE',  ( 0.7071067811575828532, -0.7071067812155121812, 0.000000000000000000 ) ) ;
#52284 = ORIENTED_EDGE ( 'NONE', *, *, #36276, .T. ) ;
#52285 = CARTESIAN_POINT ( 'NONE',  ( 97.80162807463898389, -40.49275734879226718, 167.6337774318473350 ) ) ;
#52286 = CARTESIAN_POINT ( 'NONE',  ( -1.650252395058525057, 70.05163022878409151, 118.5452349891252339 ) ) ;
#52287 = DIRECTION ( 'NONE',  ( 1.000000000000000000, 0.000000000000000000, 0.000000000000000000 ) ) ;
#52288 = CONICAL_SURFACE ( 'NONE', #81408, 1.258750000000002922, 1.029744258676650093 ) ;
#52289 = CARTESIAN_POINT ( 'NONE',  ( 89.33314995793998037, 12.92155284005730387, 355.9756252759109998 ) ) ;
#52290 = EDGE_LOOP ( 'NONE', ( #75873, #48869, #47548, #82059, #59705, #56655, #19006, #43776 ) ) ;
#52291 = EDGE_CURVE ( 'NONE', #65644, #18741, #78950, .T. ) ;
#52292 = CARTESIAN_POINT ( 'NONE',  ( 111.7737306318703361, -46.73355046572731908, 287.9146728949587555 ) ) ;
#52293 = CARTESIAN_POINT ( 'NONE',  ( 117.4276745381585556, -38.22567431247780689, 24.71276813305395237 ) ) ;
#52294 = CARTESIAN_POINT ( 'NONE',  ( 107.0664832912739399, -36.72944715994095333, 302.4856252759109907 ) ) ;
#52295 = DIRECTION ( 'NONE',  ( 0.000000000000000000, 0.000000000000000000, -1.000000000000000000 ) ) ;
#52296 = DIRECTION ( 'NONE',  ( 4.299999999999999979E-14, -1.000000000000000000, 0.000000000000000000 ) ) ;
#52297 = CARTESIAN_POINT ( 'NONE',  ( 132.8827458516741160, -39.21170328187210430, 8.006085407568425794 ) ) ;
#52298 = AXIS2_PLACEMENT_3D ( 'NONE', #88410, #32515, #47486 ) ;
#52299 = CARTESIAN_POINT ( 'NONE',  ( 116.3212776292296127, -32.94146857471318413, 287.6356252759109680 ) ) ;
#52300 = FACE_OUTER_BOUND ( 'NONE', #4657, .T. ) ;
#52301 = PLANE ( 'NONE',  #50147 ) ;
#52302 = EDGE_CURVE ( 'NONE', #23986, #19042, #64860, .T. ) ;
#52303 = CARTESIAN_POINT ( 'NONE',  ( 101.3600985487617692, -27.95198515609010315, 25.53562527591096654 ) ) ;
#52304 = CARTESIAN_POINT ( 'NONE',  ( 102.2372498927960720, -45.96854842739928415, 208.1927681330539599 ) ) ;
#52305 = CARTESIAN_POINT ( 'NONE',  ( 98.70509129169590778, -42.99238438483101987, 62.83848241876793850 ) ) ;
#52307 = CARTESIAN_POINT ( 'NONE',  ( 107.0664832912730020, -36.72944715994189835, 342.9256252759119548 ) ) ;
#52306 = DIRECTION ( 'NONE',  ( 1.000000000000000078E-15, -1.000000000000000083E-30, -1.000000000000000000 ) ) ;
#52308 = FACE_OUTER_BOUND ( 'NONE', #30637, .T. ) ;
#52309 = EDGE_CURVE ( 'NONE', #17548, #5232, #29448, .T. ) ;
#52310 = ORIENTED_EDGE ( 'NONE', *, *, #1334, .T. ) ;
#52311 = CARTESIAN_POINT ( 'NONE',  ( 90.44969454456405344, -22.62993780205708916, 219.5838068554169809 ) ) ;
#52312 = ORIENTED_EDGE ( 'NONE', *, *, #973, .F. ) ;
#52313 = AXIS2_PLACEMENT_3D ( 'NONE', #1485, #58227, #64599 ) ;
#52314 = CARTESIAN_POINT ( 'NONE',  ( 113.1080853710607528, -29.03773216254920797, 75.54705384733895812 ) ) ;
#52316 = VERTEX_POINT ( 'NONE', #9899 ) ;
#52315 = CARTESIAN_POINT ( 'NONE',  ( -31.75000000000000000, 124.5870000000000033, -3.175000000000219647 ) ) ;
#52317 = VECTOR ( 'NONE', #16839, 999.9999999999998863 ) ;
#52318 = CARTESIAN_POINT ( 'NONE',  ( 172.5667039024480687, -36.32844715993499563, 129.9678068554150059 ) ) ;
#52319 = CARTESIAN_POINT ( 'NONE',  ( 100.6510976905702393, -26.79511100149722935, 216.5327681330539633 ) ) ;
#52320 = CARTESIAN_POINT ( 'NONE',  ( 41.56648329127499153, -36.32844715994070839, 318.9256252759120116 ) ) ;
#52321 = CARTESIAN_POINT ( 'NONE',  ( 97.81218034145919660, -40.51862630628952644, 146.6357281275130902 ) ) ;
#52322 = DIRECTION ( 'NONE',  ( -1.000000000000000000, -4.299999999999999979E-14, -1.000000000000000078E-15 ) ) ;
#52324 = EDGE_CURVE ( 'NONE', #19093, #24119, #9016, .T. ) ;
#52323 = CIRCLE ( 'NONE', #63987, 3.000000000000002665 ) ;
#52325 = LINE ( 'NONE', #58714, #54460 ) ;
#52326 = CARTESIAN_POINT ( 'NONE',  ( 132.6459363690134978, -39.09121833381820466, 1.942446336661487027 ) ) ;
#52327 = CARTESIAN_POINT ( 'NONE',  ( -82.96304607088271155, 80.88456863959031296, 100.8068867829406514 ) ) ;
#52328 = CARTESIAN_POINT ( 'NONE',  ( 107.6167445103326230, -46.48501816386551866, 152.6213395616259731 ) ) ;
#52329 = VERTEX_POINT ( 'NONE', #78063 ) ;
#52330 = VECTOR ( 'NONE', #32839, 1000.000000000000000 ) ;
#52331 = ORIENTED_EDGE ( 'NONE', *, *, #18209, .F. ) ;
#52332 = CARTESIAN_POINT ( 'NONE',  ( 117.0765951205083439, -35.60322954364740156, 80.34729759161096752 ) ) ;
#52333 = AXIS2_PLACEMENT_3D ( 'NONE', #16445, #85510, #56866 ) ;
#52334 = CARTESIAN_POINT ( 'NONE',  ( -458.3598257906459708, 47.62500000000000000, 3.174999999999999822 ) ) ;
#52336 = DIRECTION ( 'NONE',  ( -1.000000000000000078E-15, 1.000000000000000000, 0.000000000000000000 ) ) ;
#52335 = CARTESIAN_POINT ( 'NONE',  ( 112.8396959964675972, -44.62460075896464673, 224.0784824187679476 ) ) ;
#52337 = DIRECTION ( 'NONE',  ( 0.000000000000000000, -0.000000000000000000, -1.000000000000000000 ) ) ;
#52338 = FACE_OUTER_BOUND ( 'NONE', #38140, .T. ) ;
#52339 = CARTESIAN_POINT ( 'NONE',  ( 118.5107509192928887, 70.27900073646854651, -3.299277431128419202 ) ) ;
#52340 = EDGE_CURVE ( 'NONE', #11616, #21936, #3517, .T. ) ;
#52341 = CARTESIAN_POINT ( 'NONE',  ( 34.96670390244699433, -28.27351298637401200, -5.074374724088000832 ) ) ;
#52342 = CARTESIAN_POINT ( 'NONE',  ( 60.32499999999999574, 82.54999999999999716, 358.0130000000000337 ) ) ;
#52343 = DIRECTION ( 'NONE',  ( 1.000000000000000000, 0.000000000000000000, 0.000000000000000000 ) ) ;
#52344 = EDGE_CURVE ( 'NONE', #29169, #73752, #70833, .T. ) ;
#52345 = CARTESIAN_POINT ( 'NONE',  ( 96.67182511810079859, -37.15340426533111895, 161.3584824187679487 ) ) ;
#52346 = ORIENTED_EDGE ( 'NONE', *, *, #34011, .F. ) ;
#52347 = ORIENTED_EDGE ( 'NONE', *, *, #52721, .F. ) ;
#52348 = EDGE_CURVE ( 'NONE', #62712, #73560, #43949, .T. ) ;
#52349 = AXIS2_PLACEMENT_3D ( 'NONE', #1226, #14409, #77081 ) ;
#52350 = CARTESIAN_POINT ( 'NONE',  ( 139.3215235511330263, -74.97943253980591294, 248.4067532124560103 ) ) ;
#52351 = CARTESIAN_POINT ( 'NONE',  ( 147.0528210869385077, -67.88961359424753539, 245.7502281596648288 ) ) ;
#52352 = ADVANCED_FACE ( 'NONE', ( #86650 ), #17606, .T. ) ;
#52353 = CARTESIAN_POINT ( 'NONE',  ( 51.03742451361238608, -23.42844715994066362, 313.9678068554150059 ) ) ;
#52354 = DIRECTION ( 'NONE',  ( -1.000000000000000078E-15, 1.000000000000000000, 0.000000000000000000 ) ) ;
#52355 = AXIS2_PLACEMENT_3D ( 'NONE', #38473, #17160, #79845 ) ;
#52356 = FACE_OUTER_BOUND ( 'NONE', #79047, .T. ) ;
#52357 = CARTESIAN_POINT ( 'NONE',  ( 109.4453579932576872, -25.93500217162640453, 179.8918157521019339 ) ) ;
#52358 = LINE ( 'NONE', #38314, #926 ) ;
#52359 = EDGE_LOOP ( 'NONE', ( #33948, #62437, #67438, #6478, #77647 ) ) ;
#52361 = VERTEX_POINT ( 'NONE', #15824 ) ;
#52360 = VERTEX_POINT ( 'NONE', #57129 ) ;
#52362 = AXIS2_PLACEMENT_3D ( 'NONE', #5526, #61801, #34998 ) ;
#52363 = CARTESIAN_POINT ( 'NONE',  ( -7.736705052999859333, 72.46990138899384704, 118.3037342042693325 ) ) ;
#52364 = DIRECTION ( 'NONE',  ( 0.08544974978095713769, 0.9963424814100680926, -0.000000000000000000 ) ) ;
#52365 = CARTESIAN_POINT ( 'NONE',  ( 108.3327054655748469, -46.73494365500790337, 163.6772328748223231 ) ) ;
#52366 = VECTOR ( 'NONE', #79834, 1000.000000000000000 ) ;
#52367 = CARTESIAN_POINT ( 'NONE',  ( 99.81817287040931319, -30.93652672145504567, 43.60809036959195595 ) ) ;
#52368 = DIRECTION ( 'NONE',  ( 1.000000000000000000, 4.163336342344333240E-14, 0.000000000000000000 ) ) ;
#52369 = ORIENTED_EDGE ( 'NONE', *, *, #73667, .F. ) ;
#52370 = CARTESIAN_POINT ( 'NONE',  ( 194.0371591254572650, -24.42818131005417825, 313.9678068554149490 ) ) ;
#52371 = CARTESIAN_POINT ( 'NONE',  ( 82.60054997757899287, -17.66120003907535363, 7.039521718172035314 ) ) ;
#52372 = ORIENTED_EDGE ( 'NONE', *, *, #7597, .T. ) ;
#52373 = EDGE_LOOP ( 'NONE', ( #70320, #62966, #6175 ) ) ;
#52374 = CARTESIAN_POINT ( 'NONE',  ( 44.45000000000000284, 69.84999999999999432, 292.1000000000000227 ) ) ;
#52375 = ORIENTED_EDGE ( 'NONE', *, *, #24377, .T. ) ;
#52376 = ORIENTED_EDGE ( 'NONE', *, *, #77339, .F. ) ;
#52377 = DIRECTION ( 'NONE',  ( 0.000000000000000000, 1.000000000000000000, 0.000000000000000000 ) ) ;
#52378 = EDGE_CURVE ( 'NONE', #11503, #20018, #22646, .T. ) ;
#52379 = CARTESIAN_POINT ( 'NONE',  ( 114.9815630121539272, -32.32897180620768296, 28.66480078045796631 ) ) ;
#52380 = CARTESIAN_POINT ( 'NONE',  ( 114.8305014334234642, -29.68612513766509053, 209.4127681330539872 ) ) ;
#52381 = CIRCLE ( 'NONE', #88746, 8.636000000000004562 ) ;
#52382 = CARTESIAN_POINT ( 'NONE',  ( 103.5497706991576905, -26.90106182813401503, 190.3499109901969746 ) ) ;
#52383 = DIRECTION ( 'NONE',  ( 0.7071067811865171526, 0.7071067811865779928, 7.071067811865164719E-16 ) ) ;
#52384 = CARTESIAN_POINT ( 'NONE',  ( 103.9393079366161032, -26.78443525705497663, 246.3184824187679567 ) ) ;
#52385 = CYLINDRICAL_SURFACE ( 'NONE', #48496, 7.937500000000000000 ) ;
#52386 = CARTESIAN_POINT ( 'NONE',  ( -487.2989999999999782, 86.51875000000001137, 86.36305401447658880 ) ) ;
#52387 = ORIENTED_EDGE ( 'NONE', *, *, #298, .F. ) ;
#52388 = ORIENTED_EDGE ( 'NONE', *, *, #26504, .F. ) ;
#52389 = CARTESIAN_POINT ( 'NONE',  ( 0.000000000000000000, 125.7300000000000040, -24.63800000000000168 ) ) ;
#52390 = CARTESIAN_POINT ( 'NONE',  ( 97.88046564956832185, -41.75177191353013484, 221.7241967044819546 ) ) ;
#52391 = ORIENTED_EDGE ( 'NONE', *, *, #32299, .F. ) ;
#52392 = EDGE_CURVE ( 'NONE', #6148, #84235, #16090, .T. ) ;
#52393 = CARTESIAN_POINT ( 'NONE',  ( 108.9452245070828411, -26.43885738637160543, 164.9327681330529742 ) ) ;
#52394 = CARTESIAN_POINT ( 'NONE',  ( 99.09532346180453999, -30.55094594714533329, 265.8023343502491684 ) ) ;
#52395 = DIRECTION ( 'NONE',  ( 0.9068632946707755327, -0.4214249218767993077, 0.000000000000000000 ) ) ;
#52396 = CARTESIAN_POINT ( 'NONE',  ( 188.5667039024484097, -48.82844715993431350, 254.7178068554150059 ) ) ;
#52397 = CARTESIAN_POINT ( 'NONE',  ( 144.0179926818975673, -140.6397677690979151, 245.9888717887127427 ) ) ;
#52398 = ADVANCED_FACE ( 'NONE', ( #64414 ), #25747, .T. ) ;
#52401 = CARTESIAN_POINT ( 'NONE',  ( 96.99990081654259200, -39.35482002063352525, 272.5299109901966972 ) ) ;
#52400 = DIRECTION ( 'NONE',  ( 0.000000000000000000, 0.000000000000000000, -1.000000000000000000 ) ) ;
#52399 = LINE ( 'NONE', #45159, #57837 ) ;
#52402 = LINE ( 'NONE', #30224, #80045 ) ;
#52403 = LINE ( 'NONE', #78394, #61331 ) ;
#52404 = DIRECTION ( 'NONE',  ( 0.7071067811865604513, 0.000000000000000000, -0.7071067811865345831 ) ) ;
#52405 = ADVANCED_FACE ( 'NONE', ( #59366 ), #57778, .T. ) ;
#52406 = PLANE ( 'NONE',  #64587 ) ;
#52407 = LINE ( 'NONE', #17922, #51732 ) ;
#52408 = ADVANCED_FACE ( 'NONE', ( #19388 ), #73903, .T. ) ;
#52409 = CARTESIAN_POINT ( 'NONE',  ( 97.33784131552974372, -34.07106451407344139, 77.11479194128529002 ) ) ;
#52410 = CIRCLE ( 'NONE', #13296, 1.000000000000000888 ) ;
#52412 = VERTEX_POINT ( 'NONE', #46172 ) ;
#52411 = CARTESIAN_POINT ( 'NONE',  ( 115.5168658168125830, -36.45974858580882483, 195.5838068554167819 ) ) ;
#52413 = ADVANCED_FACE ( 'NONE', ( #26202 ), #47064, .F. ) ;
#52414 = LINE ( 'NONE', #31105, #42266 ) ;
#52415 = CARTESIAN_POINT ( 'NONE',  ( 98.51948014227190242, -30.72152729218522538, 205.8384824187679669 ) ) ;
#52416 = CARTESIAN_POINT ( 'NONE',  ( 118.9036788419121962, -36.16782713317093112, 114.8641967044819694 ) ) ;
#52417 = CARTESIAN_POINT ( 'NONE',  ( 115.4949314580552624, -29.50734498268579387, 225.4022919425769658 ) ) ;
#52418 = FACE_OUTER_BOUND ( 'NONE', #38421, .T. ) ;
#52419 = CARTESIAN_POINT ( 'NONE',  ( 31.89136050872298966, -31.76306994223740432, -5.074374724088000832 ) ) ;
#52421 = CARTESIAN_POINT ( 'NONE',  ( 98.52126951539199240, -41.93296859720368985, 37.76142964116910861 ) ) ;
#52420 = CARTESIAN_POINT ( 'NONE',  ( 162.5667039024470171, -32.29483332968611364, -5.074374724088000832 ) ) ;
#52422 = LINE ( 'NONE', #78852, #47925 ) ;
#52423 = DIRECTION ( 'NONE',  ( -1.000000000000000000, -4.237773401492740281E-14, 0.000000000000000000 ) ) ;
#52424 = AXIS2_PLACEMENT_3D ( 'NONE', #86545, #80178, #85659 ) ;
#52425 = ADVANCED_FACE ( 'NONE', ( #12126 ), #67086, .F. ) ;
#52426 = CARTESIAN_POINT ( 'NONE',  ( 172.5664832912740110, -36.32844715994070839, 258.9256252759120116 ) ) ;
#52427 = ADVANCED_FACE ( 'NONE', ( #80731 ), #67659, .T. ) ;
#52428 = ADVANCED_FACE ( 'NONE', ( #59805 ), #87539, .T. ) ;
#52429 = VERTEX_POINT ( 'NONE', #31669 ) ;
#52430 = VERTEX_POINT ( 'NONE', #12580 ) ;
#52431 = CARTESIAN_POINT ( 'NONE',  ( 116.7648798213666623, -36.26930322673007367, 118.2867055423629807 ) ) ;
#52433 = EDGE_LOOP ( 'NONE', ( #85793, #74666, #44728, #51061 ) ) ;
#52432 = CARTESIAN_POINT ( 'NONE',  ( 1.387778780781445676E-14, 239.0000000000000000, 97.27542076772557778 ) ) ;
#52434 = CARTESIAN_POINT ( 'NONE',  ( 116.5783909117431136, -29.70293872869714846, 105.3327681330539463 ) ) ;
#52435 = EDGE_CURVE ( 'NONE', #85180, #21659, #33009, .T. ) ;
#52436 = DIRECTION ( 'NONE',  ( 1.000000000000000000, 0.000000000000000000, 2.108231265501709878E-16 ) ) ;
#52437 = AXIS2_PLACEMENT_3D ( 'NONE', #50651, #2073, #84314 ) ;
#52438 = EDGE_CURVE ( 'NONE', #65413, #57074, #53876, .T. ) ;
#52439 = CARTESIAN_POINT ( 'NONE',  ( 79.18623681048846663, -16.12360705087681367, 8.106403045240202943 ) ) ;
#52440 = CARTESIAN_POINT ( 'NONE',  ( 76.06670390244796920, -26.72944715994109899, 239.5838068554169809 ) ) ;
#52441 = CARTESIAN_POINT ( 'NONE',  ( 99.04406186382159660, -42.84125764666617897, 107.8439586099191700 ) ) ;
#52442 = CARTESIAN_POINT ( 'NONE',  ( 99.63325261332695959, -43.08637385293071986, 31.88991099019694531 ) ) ;
#52443 = VERTEX_POINT ( 'NONE', #5768 ) ;
#52444 = ORIENTED_EDGE ( 'NONE', *, *, #80998, .T. ) ;
#52445 = ORIENTED_EDGE ( 'NONE', *, *, #31013, .T. ) ;
#52446 = LINE ( 'NONE', #80209, #74718 ) ;
#52448 = CARTESIAN_POINT ( 'NONE',  ( 63.56670390244824631, -47.82844715994016127, 300.4678068554150627 ) ) ;
#52447 = CARTESIAN_POINT ( 'NONE',  ( 108.8662857618680846, -46.94215964495589333, 118.7032443235299723 ) ) ;
#52449 = CARTESIAN_POINT ( 'NONE',  ( 31.56670390244720892, -33.35206098992784263, 193.9678068554150911 ) ) ;
#52450 = PLANE ( 'NONE',  #16161 ) ;
#52451 = DIRECTION ( 'NONE',  ( 1.000000000000000000, 0.000000000000000000, -0.000000000000000000 ) ) ;
#52452 = VECTOR ( 'NONE', #3424, 1000.000000000000000 ) ;
#52453 = ADVANCED_FACE ( 'NONE', ( #40267, #25299 ), #33459, .T. ) ;
#52454 = LINE ( 'NONE', #17961, #44847 ) ;
#52455 = FACE_OUTER_BOUND ( 'NONE', #5710, .T. ) ;
#52456 = B_SPLINE_CURVE_WITH_KNOTS ( 'NONE', 3,
 ( #87168, #10853, #51722, #66247, #88063, #73975, #80807, #59875, #72646, #18557, #10412, #39890, #5386, #11295, #3595, #58981, #11754, #4039, #38115, #59437, #87608, #39452, #46240, #67153, #31740, #25828, #86275, #4935, #38998, #24934, #24054, #52598, #4494, #53497, #65807, #80359 ),
 .UNSPECIFIED., .F., .F.,
 ( 4, 2, 2, 2, 2, 2, 2, 2, 2, 2, 2, 2, 2, 2, 1, 1, 1, 1, 2, 4 ),
 ( 0.000000000000000000, 0.06249359649563903524, 0.1249871929912780705, 0.1874807894869170988, 0.2499743859825561410, 0.2812211842303752873, 0.3124679824781944060, 0.3437147807260135246, 0.3749615789738326432, 0.4062083772216517619, 0.4374551754694708805, 0.4687019737172900546, 0.4843253728411998082, 0.4921370724031547961, 0.4960429221841324288, 0.4979958470746210786, 0.4989723095198653202, 0.4994605407424874133, 0.4997046563537985708, 0.4999487719651097284 ),
 .UNSPECIFIED. ) ;
#52457 = EDGE_CURVE ( 'NONE', #42555, #40469, #82088, .T. ) ;
#52458 = CARTESIAN_POINT ( 'NONE',  ( 103.6060256796756534, -46.54035428658124118, 57.30705384733997221 ) ) ;
#52459 = VERTEX_POINT ( 'NONE', #75256 ) ;
#52460 = ORIENTED_EDGE ( 'NONE', *, *, #68923, .T. ) ;
#52461 = EDGE_CURVE ( 'NONE', #24254, #45930, #38476, .T. ) ;
#52462 = CARTESIAN_POINT ( 'NONE',  ( 97.95250717983367394, -32.49412669507731266, 6.826283056785781511 ) ) ;
#52463 = CARTESIAN_POINT ( 'NONE',  ( 126.8161134320454977, 48.06767884207233976, 31.02493203361878926 ) ) ;
#52464 = EDGE_CURVE ( 'NONE', #21130, #28780, #34366, .T. ) ;
#52465 = CARTESIAN_POINT ( 'NONE',  ( 80.34435516212752759, -110.9887994459054994, 250.2178068554180470 ) ) ;
#52466 = CARTESIAN_POINT ( 'NONE',  ( 112.3727512366848487, -30.49036002617200936, 137.3338046553059826 ) ) ;
#52467 = VECTOR ( 'NONE', #43361, 1000.000000000000000 ) ;
#52468 = LINE ( 'NONE', #41990, #18489 ) ;
#52469 = VERTEX_POINT ( 'NONE', #73448 ) ;
#52470 = ORIENTED_EDGE ( 'NONE', *, *, #70006, .F. ) ;
#52471 = LINE ( 'NONE', #79792, #25008 ) ;
#52472 = ORIENTED_EDGE ( 'NONE', *, *, #84726, .F. ) ;
#52473 = ORIENTED_EDGE ( 'NONE', *, *, #58850, .F. ) ;
#52474 = CYLINDRICAL_SURFACE ( 'NONE', #89836, 9.999999999999998224 ) ;
#52475 = AXIS2_PLACEMENT_3D ( 'NONE', #773, #42538, #83449 ) ;
#52476 = CARTESIAN_POINT ( 'NONE',  ( 104.0709181822855243, -28.35754658334662182, 186.7815833058969872 ) ) ;
#52477 = CYLINDRICAL_SURFACE ( 'NONE', #39979, 0.4999999999999933387 ) ;
#52478 = CARTESIAN_POINT ( 'NONE',  ( 274.0659999999999741, 36.86249999999999716, -7.937500000000000000 ) ) ;
#52479 = AXIS2_PLACEMENT_3D ( 'NONE', #35359, #41717, #54888 ) ;
#52480 = CARTESIAN_POINT ( 'NONE',  ( 27.27158787008328389, 184.0000000000000000, 111.9860621927989683 ) ) ;
#52481 = ORIENTED_EDGE ( 'NONE', *, *, #61804, .F. ) ;
#52482 = VERTEX_POINT ( 'NONE', #11223 ) ;
#52483 = VECTOR ( 'NONE', #30313, 1000.000000000000000 ) ;
#52484 = VERTEX_POINT ( 'NONE', #38927 ) ;
#52485 = VERTEX_POINT ( 'NONE', #66634 ) ;
#52486 = CARTESIAN_POINT ( 'NONE',  ( 115.0224139972512063, -40.13592505470528238, 211.3347570362579404 ) ) ;
#52487 = CARTESIAN_POINT ( 'NONE',  ( 99.03713458771083822, -43.41345219906346387, 116.8784824187679732 ) ) ;
#52488 = CARTESIAN_POINT ( 'NONE',  ( 116.2124334422530865, -31.77159869865914388, 69.22133956162495849 ) ) ;
#52489 = LINE ( 'NONE', #45245, #80534 ) ;
#52490 = DIRECTION ( 'NONE',  ( 0.9068632946707808618, -0.4214249218767877059, 0.000000000000000000 ) ) ;
#52491 = DIRECTION ( 'NONE',  ( 1.000000000000000000, 1.000000000000000078E-15, 0.000000000000000000 ) ) ;
#52492 = CARTESIAN_POINT ( 'NONE',  ( 102.9134293080737450, -27.12924067693381502, 151.4013395616249511 ) ) ;
#52493 = CIRCLE ( 'NONE', #74266, 2.999999999999947153 ) ;
#52494 = FACE_BOUND ( 'NONE', #41556, .T. ) ;
#52495 = ORIENTED_EDGE ( 'NONE', *, *, #1328, .F. ) ;
#52496 = CARTESIAN_POINT ( 'NONE',  ( 129.9368274816652331, 82.54999999999999716, -12.69999999999864038 ) ) ;
#52497 = ORIENTED_EDGE ( 'NONE', *, *, #3565, .T. ) ;
#52498 = ORIENTED_EDGE ( 'NONE', *, *, #87045, .F. ) ;
#52499 = CARTESIAN_POINT ( 'NONE',  ( 147.0667039024470171, -101.1152277505316164, 245.7200377504910023 ) ) ;
#52500 = CARTESIAN_POINT ( 'NONE',  ( 91.91441891875203396, -96.57077177933005885, -19.18411693322927292 ) ) ;
#52501 = ORIENTED_EDGE ( 'NONE', *, *, #11642, .T. ) ;
#52502 = CARTESIAN_POINT ( 'NONE',  ( 49.21437657594911741, -35.91149509761154945, 193.9678068554150911 ) ) ;
#52503 = ORIENTED_EDGE ( 'NONE', *, *, #14953, .T. ) ;
#52504 = CARTESIAN_POINT ( 'NONE',  ( 99.82429199452421642, -29.71057280230317232, 131.7142967403817124 ) ) ;
#52505 = CARTESIAN_POINT ( 'NONE',  ( 116.2317802277880787, -31.76111116818806224, 69.22133956162495849 ) ) ;
#52506 = DIRECTION ( 'NONE',  ( 1.000000000000000000, 0.000000000000000000, 0.000000000000000000 ) ) ;
#52507 = EDGE_CURVE ( 'NONE', #72426, #8076, #70225, .T. ) ;
#52508 = CARTESIAN_POINT ( 'NONE',  ( 165.9667039024475059, -28.27351298636806831, 237.4678068554150059 ) ) ;
#52509 = FACE_OUTER_BOUND ( 'NONE', #57448, .T. ) ;
#52510 = EDGE_CURVE ( 'NONE', #27981, #57293, #24757, .T. ) ;
#52511 = CARTESIAN_POINT ( 'NONE',  ( 112.9545114599701918, -28.19305977888944525, 89.60800622829296458 ) ) ;
#52513 = CARTESIAN_POINT ( 'NONE',  ( 112.4747680694540293, -26.21285726233897506, 165.6984824187679521 ) ) ;
#52512 = CARTESIAN_POINT ( 'NONE',  ( -72.96458098368600531, 127.0000000000000000, -72.96458098368781009 ) ) ;
#52514 = LINE ( 'NONE', #80719, #52366 ) ;
#52515 = DIRECTION ( 'NONE',  ( -1.000000000000000078E-15, 0.000000000000000000, 1.000000000000000000 ) ) ;
#52516 = ORIENTED_EDGE ( 'NONE', *, *, #20254, .F. ) ;
#52517 = CARTESIAN_POINT ( 'NONE',  ( 116.0667039024470313, -104.2784471599411091, 2.217806855418003043 ) ) ;
#52518 = ADVANCED_FACE ( 'NONE', ( #75703 ), #7558, .F. ) ;
#52519 = AXIS2_PLACEMENT_3D ( 'NONE', #73019, #52547, #10789 ) ;
#52520 = CARTESIAN_POINT ( 'NONE',  ( 75.31670390244798341, -57.40094715994099772, 84.20080685541500998 ) ) ;
#52521 = CARTESIAN_POINT ( 'NONE',  ( 143.0664832912740110, -18.82844715994099971, 246.4006252759120059 ) ) ;
#52522 = EDGE_CURVE ( 'NONE', #11886, #70782, #45945, .T. ) ;
#52523 = DIRECTION ( 'NONE',  ( 1.387778780781444492E-15, 0.000000000000000000, -1.000000000000000000 ) ) ;
#52525 = VERTEX_POINT ( 'NONE', #28900 ) ;
#52524 = CARTESIAN_POINT ( 'NONE',  ( 113.2461215947159161, -45.18040784396236376, 228.0784824187679760 ) ) ;
#52526 = LINE ( 'NONE', #18034, #85750 ) ;
#52527 = CARTESIAN_POINT ( 'NONE',  ( 112.4656099449901916, -45.71435824391657832, 234.0070538473389377 ) ) ;
#52528 = CARTESIAN_POINT ( 'NONE',  ( 113.1020477030913582, -28.17579636167772605, 125.5870538473399591 ) ) ;
#52529 = CARTESIAN_POINT ( 'NONE',  ( 51.23005224011598102, -33.89581943344511217, -5.074374724088000832 ) ) ;
#52530 = CIRCLE ( 'NONE', #14849, 1.571100913904416307 ) ;
#52531 = CARTESIAN_POINT ( 'NONE',  ( 82.45326694837886805, -38.09809895854016304, 7.205238605739220148 ) ) ;
#52532 = LINE ( 'NONE', #18483, #19606 ) ;
#52533 = DIRECTION ( 'NONE',  ( -1.000000000000000078E-15, 1.000000000000000000, 0.000000000000000000 ) ) ;
#52534 = VERTEX_POINT ( 'NONE', #13033 ) ;
#52535 = EDGE_CURVE ( 'NONE', #77006, #26329, #82538, .T. ) ;
#52536 = CONICAL_SURFACE ( 'NONE', #35104, 81.91591158490091118, 0.7853981633974760346 ) ;
#52537 = B_SPLINE_CURVE_WITH_KNOTS ( 'NONE', 3,
 ( #45967, #57836, #2886, #30585, #86015, #72374, #10143, #65547, #25543, #33261, #32348, #39177, #46861, #89133, #67322, #40961, #60051, #75048 ),
 .UNSPECIFIED., .F., .F.,
 ( 4, 2, 2, 2, 2, 2, 2, 2, 4 ),
 ( 0.4999914309044427019, 0.5624925020413873433, 0.6249935731783320403, 0.6874946443152767372, 0.7499957154522214342, 0.8124967865891661312, 0.8749978577261107171, 0.9374989288630553030, 1.000000000000000000 ),
 .UNSPECIFIED. ) ;
#52538 = VERTEX_POINT ( 'NONE', #13471 ) ;
#52539 = ORIENTED_EDGE ( 'NONE', *, *, #32258, .F. ) ;
#52540 = ORIENTED_EDGE ( 'NONE', *, *, #54810, .T. ) ;
#52541 = CARTESIAN_POINT ( 'NONE',  ( 116.8171228669039721, -34.15291832155635632, 74.03145860916620791 ) ) ;
#52542 = CARTESIAN_POINT ( 'NONE',  ( 100.4791399132689236, -44.80881982087480964, 8.032768133053981074 ) ) ;
#52543 = CARTESIAN_POINT ( 'NONE',  ( 49.35031423293201414, -29.99615139349890569, -5.074374724088000832 ) ) ;
#52544 = CARTESIAN_POINT ( 'NONE',  ( 131.3325396840767212, -36.38436945697923619, 3.076560175367943906 ) ) ;
#52546 = EDGE_CURVE ( 'NONE', #28680, #22667, #72121, .T. ) ;
#52545 = CIRCLE ( 'NONE', #1828, 7.937500000000000000 ) ;
#52548 = CARTESIAN_POINT ( 'NONE',  ( 109.7255615593723377, -27.00098969710095886, 149.8651129182388217 ) ) ;
#52547 = DIRECTION ( 'NONE',  ( 0.000000000000000000, -1.000000000000000000, 0.000000000000000000 ) ) ;
#52549 = CARTESIAN_POINT ( 'NONE',  ( 100.5279579596103332, -31.18870816475473262, 215.1895626852199541 ) ) ;
#52550 = ORIENTED_EDGE ( 'NONE', *, *, #67080, .T. ) ;
#52551 = ADVANCED_FACE ( 'NONE', ( #42497 ), #27987, .T. ) ;
#52552 = ORIENTED_EDGE ( 'NONE', *, *, #86485, .T. ) ;
#52553 = ORIENTED_EDGE ( 'NONE', *, *, #77372, .F. ) ;
#52554 = CIRCLE ( 'NONE', #9097, 7.937500000000000000 ) ;
#52555 = FACE_OUTER_BOUND ( 'NONE', #83145, .T. ) ;
#52556 = CARTESIAN_POINT ( 'NONE',  ( 110.8745347144050015, -45.97600918556555882, 182.8873507977141628 ) ) ;
#52557 = DIRECTION ( 'NONE',  ( 0.000000000000000000, 0.000000000000000000, -1.000000000000000000 ) ) ;
#52558 = CARTESIAN_POINT ( 'NONE',  ( 97.02995690277612084, -35.86988738539728416, 32.69015473446795994 ) ) ;
#52559 = AXIS2_PLACEMENT_3D ( 'NONE', #86089, #43832, #23861 ) ;
#52560 = CARTESIAN_POINT ( 'NONE',  ( 117.8848147242575237, 84.21376545118702950, 12.59751181725513014 ) ) ;
#52561 = DIRECTION ( 'NONE',  ( 1.000000000000000078E-15, -1.000000000000000083E-30, -1.000000000000000000 ) ) ;
#52562 = DIRECTION ( 'NONE',  ( 0.000000000000000000, 0.000000000000000000, -1.000000000000000000 ) ) ;
#52563 = EDGE_LOOP ( 'NONE', ( #64407, #44384, #50796, #309 ) ) ;
#52564 = EDGE_CURVE ( 'NONE', #35850, #6945, #17005, .T. ) ;
#52565 = CARTESIAN_POINT ( 'NONE',  ( 108.7002376003399178, -26.83066989546479775, 55.94644779129590972 ) ) ;
#52566 = ORIENTED_EDGE ( 'NONE', *, *, #35655, .F. ) ;
#52567 = ADVANCED_FACE ( 'NONE', ( #27100 ), #13920, .F. ) ;
#52568 = DIRECTION ( 'NONE',  ( 1.000000000000000078E-15, 1.000000000000000083E-30, -1.000000000000000000 ) ) ;
#52569 = CARTESIAN_POINT ( 'NONE',  ( 104.6989491262461769, -45.05385146434951338, 65.18618560768597092 ) ) ;
#52570 = CARTESIAN_POINT ( 'NONE',  ( 136.5970563715337391, -17.65296049054856553, 7.043700149388504528 ) ) ;
#52571 = CARTESIAN_POINT ( 'NONE',  ( -215.9000000000000057, 53.97500000000000142, 70.79999999999999716 ) ) ;
#52572 = CARTESIAN_POINT ( 'NONE',  ( -12.37528545905534649, 85.43392152113592886, 117.9083718356618817 ) ) ;
#52573 = EDGE_LOOP ( 'NONE', ( #69725, #33604 ) ) ;
#52574 = CARTESIAN_POINT ( 'NONE',  ( 142.8821648370248170, -72.54478064608022692, 394.9756252759100903 ) ) ;
#52575 = CARTESIAN_POINT ( 'NONE',  ( 124.2933722748468028, 59.28198175267112191, -39.95096659757145829 ) ) ;
#52576 = VECTOR ( 'NONE', #2439, 1000.000000000000000 ) ;
#52577 = ORIENTED_EDGE ( 'NONE', *, *, #59034, .F. ) ;
#52578 = CARTESIAN_POINT ( 'NONE',  ( 117.2096823498778662, -39.28706705594211712, 123.6299109901969615 ) ) ;
#52579 = ORIENTED_EDGE ( 'NONE', *, *, #57404, .F. ) ;
#52580 = CARTESIAN_POINT ( 'NONE',  ( 98.06318007301436523, -37.70576754076741821, 80.82289601855296723 ) ) ;
#52581 = DIRECTION ( 'NONE',  ( 0.000000000000000000, 0.000000000000000000, 1.000000000000000000 ) ) ;
#52582 = CARTESIAN_POINT ( 'NONE',  ( 115.7370193921850898, -38.55977017368898174, 60.09301187732596361 ) ) ;
#52583 = EDGE_CURVE ( 'NONE', #79680, #60387, #44533, .T. ) ;
#52584 = LINE ( 'NONE', #60310, #40107 ) ;
#52585 = DIRECTION ( 'NONE',  ( 0.000000000000000000, -1.000000000000000000, 0.000000000000000000 ) ) ;
#52586 = CARTESIAN_POINT ( 'NONE',  ( 96.63726304471626349, -32.99895513370901057, 22.06514908543494258 ) ) ;
#52587 = PLANE ( 'NONE',  #7529 ) ;
#52588 = ORIENTED_EDGE ( 'NONE', *, *, #48627, .F. ) ;
#52589 = VECTOR ( 'NONE', #59084, 1000.000000000000000 ) ;
#52590 = EDGE_CURVE ( 'NONE', #17172, #84388, #79395, .T. ) ;
#52591 = LINE ( 'NONE', #61222, #60362 ) ;
#52592 = VERTEX_POINT ( 'NONE', #56118 ) ;
#52593 = CARTESIAN_POINT ( 'NONE',  ( -118.2598914205052409, 72.98405218941672956, 8.394510633990522663 ) ) ;
#52594 = VERTEX_POINT ( 'NONE', #62952 ) ;
#52595 = ORIENTED_EDGE ( 'NONE', *, *, #73105, .T. ) ;
#52596 = ORIENTED_EDGE ( 'NONE', *, *, #52717, .F. ) ;
#52597 = CARTESIAN_POINT ( 'NONE',  ( 106.8648936900573005, -47.09757847023110600, 227.5489586092449485 ) ) ;
#52598 = CARTESIAN_POINT ( 'NONE',  ( 97.79342564157622064, -40.47254066486753743, 126.6313135746393357 ) ) ;
#52599 = CARTESIAN_POINT ( 'NONE',  ( 67.06681736700808472, -67.87844715931913697, 245.5130139978070076 ) ) ;
#52600 = CARTESIAN_POINT ( 'NONE',  ( 117.0537825276303749, -31.99364369613817161, 60.19086337114898555 ) ) ;
#52601 = CARTESIAN_POINT ( 'NONE',  ( 116.7950950855014156, -39.38795255544770413, 44.61478202052061448 ) ) ;
#52602 = ORIENTED_EDGE ( 'NONE', *, *, #75316, .F. ) ;
#52603 = LINE ( 'NONE', #47148, #42391 ) ;
#52604 = CARTESIAN_POINT ( 'NONE',  ( 51.42025729302567072, -31.94127993907664020, 193.9678068554150911 ) ) ;
#52605 = ORIENTED_EDGE ( 'NONE', *, *, #6176, .F. ) ;
#52606 = AXIS2_PLACEMENT_3D ( 'NONE', #5416, #26736, #81733 ) ;
#52607 = FACE_OUTER_BOUND ( 'NONE', #89402, .T. ) ;
#52608 = DIRECTION ( 'NONE',  ( -1.000000000000000000, -1.000000000000000078E-15, 0.000000000000000000 ) ) ;
#52609 = CARTESIAN_POINT ( 'NONE',  ( 117.3134009501235795, -34.93240959161192194, 243.9641967044819637 ) ) ;
#52610 = DIRECTION ( 'NONE',  ( -1.000000000000000000, 0.000000000000000000, 0.000000000000000000 ) ) ;
#52611 = AXIS2_PLACEMENT_3D ( 'NONE', #49160, #21032, #138 ) ;
#52612 = EDGE_CURVE ( 'NONE', #25238, #30354, #19914, .T. ) ;
#52613 = DIRECTION ( 'NONE',  ( 1.000000000000000000, 0.000000000000000000, -0.000000000000000000 ) ) ;
#52614 = CARTESIAN_POINT ( 'NONE',  ( 79.18623681048256913, -39.33528726900532746, 1.744847506583331098 ) ) ;
#52615 = ADVANCED_FACE ( 'NONE', ( #20733 ), #48403, .F. ) ;
#52616 = CARTESIAN_POINT ( 'NONE',  ( 116.0913394378304702, -33.14858145062638073, 248.5495626852199678 ) ) ;
#52619 = CARTESIAN_POINT ( 'NONE',  ( 109.9050689397999605, -46.77468768478695438, 68.79562527591099297 ) ) ;
#52618 = CARTESIAN_POINT ( 'NONE',  ( 194.5664832912729878, -71.37844715994266664, 342.9256252759109884 ) ) ;
#52617 = VECTOR ( 'NONE', #80345, 1000.000000000000000 ) ;
#52620 = CARTESIAN_POINT ( 'NONE',  ( 110.4077240393726527, 62.31375596498891412, 69.67785885149439196 ) ) ;
#52621 = CARTESIAN_POINT ( 'NONE',  ( 117.6526747975261458, -33.39096950974673916, 129.0575300378159795 ) ) ;
#52622 = ORIENTED_EDGE ( 'NONE', *, *, #4895, .T. ) ;
#52623 = CARTESIAN_POINT ( 'NONE',  ( 132.2449836194477655, -20.78962918509812496, 7.677444906557659543 ) ) ;
#52624 = ORIENTED_EDGE ( 'NONE', *, *, #70185, .T. ) ;
#52625 = DIRECTION ( 'NONE',  ( 0.000000000000000000, -0.9995520592605569021, -0.02992792722492374630 ) ) ;
#52626 = ADVANCED_FACE ( 'NONE', ( #72465 ), #78406, .F. ) ;
#52627 = DIRECTION ( 'NONE',  ( 0.000000000000000000, 0.000000000000000000, -1.000000000000000000 ) ) ;
#52628 = DIRECTION ( 'NONE',  ( 4.299999999999999979E-14, -1.000000000000000000, 4.400000000000000367E-29 ) ) ;
#52629 = ORIENTED_EDGE ( 'NONE', *, *, #37801, .T. ) ;
#52630 = CARTESIAN_POINT ( 'NONE',  ( 103.1875000000000000, 127.0000000000000000, 3.602774393244745134E-13 ) ) ;
#52631 = ADVANCED_FACE ( 'NONE', ( #71583 ), #65198, .T. ) ;
#52633 = VERTEX_POINT ( 'NONE', #57028 ) ;
#52632 = CARTESIAN_POINT ( 'NONE',  ( 117.3823636748946058, -32.63121637840519895, 99.13943479972098771 ) ) ;
#52634 = DIRECTION ( 'NONE',  ( 0.000000000000000000, -1.000000000000000000, 0.000000000000000000 ) ) ;
#52635 = CARTESIAN_POINT ( 'NONE',  ( 107.0664832912739968, -36.72944715994100306, 394.9756252759102040 ) ) ;
#52636 = DIRECTION ( 'NONE',  ( -1.000000000000000078E-15, 1.000000000000000083E-30, 1.000000000000000000 ) ) ;
#52637 = ORIENTED_EDGE ( 'NONE', *, *, #64643, .T. ) ;
#52638 = EDGE_CURVE ( 'NONE', #54865, #38542, #9342, .T. ) ;
#52639 = CARTESIAN_POINT ( 'NONE',  ( 114.0369391955824483, -28.94747385925965943, 114.4956252759109816 ) ) ;
#52640 = DIRECTION ( 'NONE',  ( 7.237399417378975455E-15, 0.000000000000000000, -1.000000000000000000 ) ) ;
#52641 = AXIS2_PLACEMENT_3D ( 'NONE', #4757, #19284, #60141 ) ;
#52642 = CARTESIAN_POINT ( 'NONE',  ( 7.661254700127822836, 98.64746158385918307, 317.6630000000000109 ) ) ;
#52643 = CARTESIAN_POINT ( 'NONE',  ( 91.91441891875204817, -111.9861225405540637, -19.18411693322877198 ) ) ;
#52644 = ORIENTED_EDGE ( 'NONE', *, *, #51410, .T. ) ;
#52645 = EDGE_CURVE ( 'NONE', #20262, #74824, #64315, .T. ) ;
#52646 = CONICAL_SURFACE ( 'NONE', #46878, 10.66800000000000459, 0.02993239667170383839 ) ;
#52647 = VERTEX_POINT ( 'NONE', #16168 ) ;
#52648 = CARTESIAN_POINT ( 'NONE',  ( 100.7545871043110424, 84.62817240485476589, -83.02643542997968495 ) ) ;
#52649 = DIRECTION ( 'NONE',  ( 0.000000000000000000, 1.000000000000000000, 0.000000000000000000 ) ) ;
#52650 = PLANE ( 'NONE',  #35634 ) ;
#52652 = CARTESIAN_POINT ( 'NONE',  ( 33.96670390244654669, -26.71338133339342136, 117.4678068554150485 ) ) ;
#52651 = DIRECTION ( 'NONE',  ( 0.000000000000000000, -1.000000000000000000, 0.000000000000000000 ) ) ;
#52653 = CARTESIAN_POINT ( 'NONE',  ( 97.39138678773666413, -39.27887895447691591, 181.5314891877281127 ) ) ;
#52654 = AXIS2_PLACEMENT_3D ( 'NONE', #80202, #67436, #81990 ) ;
#52655 = ORIENTED_EDGE ( 'NONE', *, *, #8074, .F. ) ;
#52656 = DIRECTION ( 'NONE',  ( 1.000000000000000000, 3.999999999999999995E-14, 1.000000000000000078E-15 ) ) ;
#52657 = CARTESIAN_POINT ( 'NONE',  ( 108.1128363339379490, -46.45408497333508535, 198.6613395616249989 ) ) ;
#52659 = VERTEX_POINT ( 'NONE', #9788 ) ;
#52658 = DIRECTION ( 'NONE',  ( 0.9068632946707805287, -0.4214249218767882055, 8.896017825522093530E-16 ) ) ;
#52660 = CARTESIAN_POINT ( 'NONE',  ( 101.3196941207357469, -46.24713579373438677, 48.14419670448194211 ) ) ;
#52661 = CARTESIAN_POINT ( 'NONE',  ( 110.8553855737280003, -45.98386346395795243, 52.88570380872458543 ) ) ;
#52662 = CARTESIAN_POINT ( 'NONE',  ( 107.0664832912739968, -8.979447159941031487, -4.824374724089029343 ) ) ;
#52663 = DIRECTION ( 'NONE',  ( -4.012088370409549976E-14, 1.000000000000000000, 0.000000000000000000 ) ) ;
#52664 = ORIENTED_EDGE ( 'NONE', *, *, #57558, .T. ) ;
#52665 = CARTESIAN_POINT ( 'NONE',  ( 130.5667039024480118, -39.24694715994093741, 229.5838068554170093 ) ) ;
#52666 = VERTEX_POINT ( 'NONE', #8916 ) ;
#52667 = ORIENTED_EDGE ( 'NONE', *, *, #69463, .T. ) ;
#52668 = EDGE_CURVE ( 'NONE', #76240, #74866, #69190, .T. ) ;
#52669 = CARTESIAN_POINT ( 'NONE',  ( 117.0318879909729048, -38.19962202173364574, 220.1415833058969724 ) ) ;
#52670 = CIRCLE ( 'NONE', #29511, 1.000000000000000888 ) ;
#52671 =( REPRESENTATION_RELATIONSHIP ('NONE','NONE', #82876, #64293 ) REPRESENTATION_RELATIONSHIP_WITH_TRANSFORMATION ( #54881 )SHAPE_REPRESENTATION_RELATIONSHIP( ) );
#52672 = DIRECTION ( 'NONE',  ( 0.000000000000000000, 0.000000000000000000, 1.000000000000000000 ) ) ;
#52673 = CARTESIAN_POINT ( 'NONE',  ( -86.67213519546623957, 92.64237678566782108, 97.63858630140191508 ) ) ;
#52674 = VECTOR ( 'NONE', #47602, 1000.000000000000000 ) ;
#52675 = CARTESIAN_POINT ( 'NONE',  ( 41.56648329127399677, -18.82844715994099971, 78.92562527591199739 ) ) ;
#52676 = CARTESIAN_POINT ( 'NONE',  ( 81.19087023417370119, -39.23918067504817486, 1.822998012175015559 ) ) ;
#52677 = EDGE_LOOP ( 'NONE', ( #22389, #65137, #52387, #9531 ) ) ;
#52678 = DIRECTION ( 'NONE',  ( 0.000000000000000000, 1.000000000000000000, 0.000000000000000000 ) ) ;
#52679 = CARTESIAN_POINT ( 'NONE',  ( 97.39144547896158599, -39.27908535653673994, 37.53121822511904782 ) ) ;
#52680 = ORIENTED_EDGE ( 'NONE', *, *, #17514, .T. ) ;
#52681 = CARTESIAN_POINT ( 'NONE',  ( 104.6488677213912695, -47.51528149961286829, 27.38895860924395009 ) ) ;
#52682 = CARTESIAN_POINT ( 'NONE',  ( 9.562607838165547491, 90.94827852097223797, 118.1711730385347607 ) ) ;
#52683 = ORIENTED_EDGE ( 'NONE', *, *, #2706, .T. ) ;
#52684 = CARTESIAN_POINT ( 'NONE',  ( 104.9869425053901892, -28.32846893322983917, 238.0757094172099642 ) ) ;
#52685 = CARTESIAN_POINT ( 'NONE',  ( 194.0667039024475287, -24.92844715993407334, 180.4678068554150343 ) ) ;
#52686 = CARTESIAN_POINT ( 'NONE',  ( 0.000000000000000000, 50.79999999999999716, 265.5569999999999595 ) ) ;
#52687 = LINE ( 'NONE', #54485, #43284 ) ;
#52688 = LINE ( 'NONE', #18205, #65171 ) ;
#52689 = CARTESIAN_POINT ( 'NONE',  ( 96.63066398506619237, -35.53291458860860530, 202.2356252759109623 ) ) ;
#52690 = CARTESIAN_POINT ( 'NONE',  ( 0.000000000000000000, 95.00619999999999266, 0.000000000000000000 ) ) ;
#52691 = EDGE_LOOP ( 'NONE', ( #66607, #62848, #59155, #82351, #57086, #59218, #2921, #30215, #14610, #34466 ) ) ;
#52692 = ADVANCED_FACE ( 'NONE', ( #24314 ), #2975, .T. ) ;
#52693 = CARTESIAN_POINT ( 'NONE',  ( 102.9539626486510713, -46.35650038051790744, 88.25562527591095829 ) ) ;
#52694 = FACE_OUTER_BOUND ( 'NONE', #17732, .T. ) ;
#52695 = AXIS2_PLACEMENT_3D ( 'NONE', #78865, #43865, #10681 ) ;
#52696 = ORIENTED_EDGE ( 'NONE', *, *, #18183, .T. ) ;
#52697 = ORIENTED_EDGE ( 'NONE', *, *, #22653, .F. ) ;
#52698 = ORIENTED_EDGE ( 'NONE', *, *, #16186, .F. ) ;
#52699 = AXIS2_PLACEMENT_3D ( 'NONE', #44317, #37529, #72047 ) ;
#52700 = CARTESIAN_POINT ( 'NONE',  ( 63.56670390244708813, -40.82844715994014706, 180.4678068554151196 ) ) ;
#52701 = CARTESIAN_POINT ( 'NONE',  ( 181.8764988495240118, -33.54226604284930602, -5.074374724088000832 ) ) ;
#52702 = DIRECTION ( 'NONE',  ( 1.000000000000000000, 0.000000000000000000, 0.000000000000000000 ) ) ;
#52703 = CARTESIAN_POINT ( 'NONE',  ( 114.8702562078425160, -31.70976148532177064, 142.0995189410209605 ) ) ;
#52704 = CARTESIAN_POINT ( 'NONE',  ( 100.6429626219512983, -44.96811459249982335, 228.0499109901969348 ) ) ;
#52705 = CARTESIAN_POINT ( 'NONE',  ( 116.3279290549545806, -32.94269076977911226, 60.13562527591098927 ) ) ;
#52706 = ORIENTED_EDGE ( 'NONE', *, *, #51200, .F. ) ;
#52707 = DIRECTION ( 'NONE',  ( 0.000000000000000000, 0.000000000000000000, -1.000000000000000000 ) ) ;
#52708 = ORIENTED_EDGE ( 'NONE', *, *, #7042, .F. ) ;
#52709 = VERTEX_POINT ( 'NONE', #43847 ) ;
#52710 = CIRCLE ( 'NONE', #1997, 0.5000000000000004441 ) ;
#52711 = CARTESIAN_POINT ( 'NONE',  ( 90.44969454456405344, -20.11243780205715481, 218.8274735512160589 ) ) ;
#52712 = VERTEX_POINT ( 'NONE', #3420 ) ;
#52713 = ORIENTED_EDGE ( 'NONE', *, *, #70922, .T. ) ;
#52714 = CARTESIAN_POINT ( 'NONE',  ( 113.1798478553082248, -44.75070311407051094, 169.0948016189585417 ) ) ;
#52715 = CARTESIAN_POINT ( 'NONE',  ( 184.5667039024480118, -67.87844715994100397, 20.91780685541479912 ) ) ;
#52716 = CARTESIAN_POINT ( 'NONE',  ( 97.81170495107971874, -40.51745053935989915, 26.63526479160227112 ) ) ;
#52717 = EDGE_CURVE ( 'NONE', #22746, #12675, #70697, .T. ) ;
#52718 = CARTESIAN_POINT ( 'NONE',  ( 102.9572487778789878, -44.79956872283601399, 171.6362293518859587 ) ) ;
#52719 = CARTESIAN_POINT ( 'NONE',  ( 111.1461885285858671, -47.05266801877174032, 22.88800622829195675 ) ) ;
#52720 = ORIENTED_EDGE ( 'NONE', *, *, #8866, .F. ) ;
#52721 = EDGE_CURVE ( 'NONE', #82989, #5511, #51107, .T. ) ;
#52722 = DIRECTION ( 'NONE',  ( -2.671820169801660301E-13, 0.000000000000000000, 1.000000000000000000 ) ) ;
#52723 = ADVANCED_FACE ( 'NONE', ( #22990 ), #15270, .F. ) ;
#52724 = VERTEX_POINT ( 'NONE', #23874 ) ;
#52725 = CARTESIAN_POINT ( 'NONE',  ( 167.2371591254544967, -47.82818131005522133, 180.4678068554150059 ) ) ;
#52726 = EDGE_CURVE ( 'NONE', #9140, #42594, #63426, .T. ) ;
#52727 = VERTEX_POINT ( 'NONE', #79293 ) ;
#52728 = CYLINDRICAL_SURFACE ( 'NONE', #8774, 3.249999999999975131 ) ;
#52729 = DIRECTION ( 'NONE',  ( 1.000000000000000000, 0.000000000000000000, 0.000000000000000000 ) ) ;
#52730 = DIRECTION ( 'NONE',  ( -1.000000000000000078E-15, 1.000000000000000083E-30, 1.000000000000000000 ) ) ;
#52731 = CARTESIAN_POINT ( 'NONE',  ( 107.5667039024470313, -108.2470741265389620, -19.78219314458190681 ) ) ;
#52732 = ORIENTED_EDGE ( 'NONE', *, *, #7917, .T. ) ;
#52733 = CARTESIAN_POINT ( 'NONE',  ( 100.4512775726424820, -44.84301714363712676, 12.03276813305398463 ) ) ;
#52734 = CARTESIAN_POINT ( 'NONE',  ( 106.5158076061070460, -25.64367904723916780, 41.12800622829193742 ) ) ;
#52735 = VECTOR ( 'NONE', #77703, 999.9999999999998863 ) ;
#52737 = DIRECTION ( 'NONE',  ( 0.9068632946707806397, -0.4214249218767879279, 9.068632946707804446E-16 ) ) ;
#52736 = FACE_OUTER_BOUND ( 'NONE', #87399, .T. ) ;
#52738 = CARTESIAN_POINT ( 'NONE',  ( 107.0667039024470313, -104.2784471599418197, -11.78219314458200984 ) ) ;
#52739 = LINE ( 'NONE', #87756, #78625 ) ;
#52740 = DIRECTION ( 'NONE',  ( 1.000000000000000000, 4.163336342344333240E-14, 0.000000000000000000 ) ) ;
#52741 = EDGE_CURVE ( 'NONE', #28724, #58384, #17053, .T. ) ;
#52742 = CARTESIAN_POINT ( 'NONE',  ( 106.6019379103756535, -25.27972995136449441, 322.9014499992877631 ) ) ;
#52743 = DIRECTION ( 'NONE',  ( 0.08544974978095713769, 0.9963424814100680926, -0.000000000000000000 ) ) ;
#52744 = CARTESIAN_POINT ( 'NONE',  ( 99.09377177006922466, -44.45270778143659385, 41.95086337114900488 ) ) ;
#52745 = CARTESIAN_POINT ( 'NONE',  ( 100.6376613383881704, -26.77430457650146423, 216.5327681330539633 ) ) ;
#52746 = CARTESIAN_POINT ( 'NONE',  ( 113.4728825864854116, -46.72846204934055692, 64.02991099019695298 ) ) ;
#52748 = CARTESIAN_POINT ( 'NONE',  ( 116.8171228664610766, -34.15291832047437026, 49.03145860925929611 ) ) ;
#52747 = DIRECTION ( 'NONE',  ( 0.000000000000000000, 0.000000000000000000, 1.000000000000000000 ) ) ;
#52749 = CARTESIAN_POINT ( 'NONE',  ( 81.77561474850375589, -34.57277681850425211, 2.101554741571703744 ) ) ;
#52750 = AXIS2_PLACEMENT_3D ( 'NONE', #30830, #23152, #37205 ) ;
#52751 = CIRCLE ( 'NONE', #28151, 1.000000000000000888 ) ;
#52752 = VECTOR ( 'NONE', #69315, 1000.000000000000000 ) ;
#52753 = EDGE_LOOP ( 'NONE', ( #55824, #52217, #76394, #8414 ) ) ;
#52754 = CARTESIAN_POINT ( 'NONE',  ( -254.0000000000000000, 3.174999999999999822, -41.27499999999999858 ) ) ;
#52755 = EDGE_LOOP ( 'NONE', ( #78564, #38417, #23686, #4139 ) ) ;
#52756 = CARTESIAN_POINT ( 'NONE',  ( 114.2351621074132026, -44.22269940884944361, 109.1718157521009687 ) ) ;
#52758 = ORIENTED_EDGE ( 'NONE', *, *, #3650, .T. ) ;
#52757 = CARTESIAN_POINT ( 'NONE',  ( -34.75390121890993100, 53.97499999999997300, 71.80362806563778122 ) ) ;
#52759 = VECTOR ( 'NONE', #72495, 1000.000000000000000 ) ;
#52760 = CARTESIAN_POINT ( 'NONE',  ( 115.3705510513157009, -30.46277945167186374, 215.3413395616249773 ) ) ;
#52761 = CARTESIAN_POINT ( 'NONE',  ( 107.0667039024470313, -104.2784471599420471, -19.18411693322902423 ) ) ;
#52762 = CARTESIAN_POINT ( 'NONE',  ( 110.9557970953006247, -45.94221351776628381, 147.8943543333864739 ) ) ;
#52763 = CARTESIAN_POINT ( 'NONE',  ( 161.0667039024470171, -78.67844715994088745, 96.96780685541800437 ) ) ;
#52764 = DIRECTION ( 'NONE',  ( 1.017460296392624983E-15, 1.000000000000000000, 0.000000000000000000 ) ) ;
#52765 = CARTESIAN_POINT ( 'NONE',  ( 131.5325842222575830, -37.79809288067819040, 2.811527366592918575 ) ) ;
#52766 = CARTESIAN_POINT ( 'NONE',  ( 172.5664832912740110, -18.82844715994099971, 78.92562527591199739 ) ) ;
#52767 = CARTESIAN_POINT ( 'NONE',  ( 96.69720940280899413, -36.59277893904148726, 156.3280062282929634 ) ) ;
#52768 = ORIENTED_EDGE ( 'NONE', *, *, #27130, .F. ) ;
#52769 = ORIENTED_EDGE ( 'NONE', *, *, #28557, .T. ) ;
#52770 = ADVANCED_FACE ( 'NONE', ( #77949 ), #86549, .F. ) ;
#52771 = CARTESIAN_POINT ( 'NONE',  ( 115.4437480007128443, -33.74891607059462473, 110.5301547344689794 ) ) ;
#52772 = CARTESIAN_POINT ( 'NONE',  ( 111.3555650440039528, -119.3022720253470226, -11.78219314458153733 ) ) ;
#52774 = DIRECTION ( 'NONE',  ( 0.000000000000000000, -1.000000000000000000, 0.000000000000000000 ) ) ;
#52773 = CARTESIAN_POINT ( 'NONE',  ( 97.83217745605955429, -40.05230289513912822, 262.6013395616248545 ) ) ;
#52775 = DIRECTION ( 'NONE',  ( 0.000000000000000000, 1.000000000000000000, 0.000000000000000000 ) ) ;
#52777 = EDGE_CURVE ( 'NONE', #54390, #42703, #1649, .T. ) ;
#52776 = DIRECTION ( 'NONE',  ( 0.000000000000000000, -1.000000000000000000, 0.000000000000000000 ) ) ;
#52778 = CARTESIAN_POINT ( 'NONE',  ( 117.9582931081851029, 78.06989712577870932, -11.89083204515574721 ) ) ;
#52779 = DIRECTION ( 'NONE',  ( 1.639958061481212836E-42, -4.100000000000000342E-29, -1.000000000000000000 ) ) ;
#52780 = LINE ( 'NONE', #5125, #23235 ) ;
#52781 = DIRECTION ( 'NONE',  ( -1.000000000000000000, 0.000000000000000000, 0.000000000000000000 ) ) ;
#52782 = CARTESIAN_POINT ( 'NONE',  ( 97.42226921825827901, -40.63044708855872500, 206.6327681330539860 ) ) ;
#52783 = ORIENTED_EDGE ( 'NONE', *, *, #45745, .T. ) ;
#52784 = VERTEX_POINT ( 'NONE', #71137 ) ;
#52785 = LINE ( 'NONE', #23807, #73472 ) ;
#52786 = LINE ( 'NONE', #51475, #30251 ) ;
#52787 = FACE_OUTER_BOUND ( 'NONE', #64258, .T. ) ;
#52788 = CARTESIAN_POINT ( 'NONE',  ( 116.1804594027163517, -40.96476762480074996, 0.4256252759109800388 ) ) ;
#52789 = ORIENTED_EDGE ( 'NONE', *, *, #77880, .F. ) ;
#52790 = EDGE_CURVE ( 'NONE', #70380, #78000, #36615, .T. ) ;
#52791 = CARTESIAN_POINT ( 'NONE',  ( 115.0356604027599587, -42.91048835123673655, 63.30208818923281910 ) ) ;
#52792 = CARTESIAN_POINT ( 'NONE',  ( 116.7954078171858896, -40.57313474401875197, 193.5270538473389479 ) ) ;
#52793 = CARTESIAN_POINT ( 'NONE',  ( 135.9139897988364112, -38.77444411304905714, 7.664507283842826979 ) ) ;
#52794 = ORIENTED_EDGE ( 'NONE', *, *, #9622, .T. ) ;
#52795 = ORIENTED_EDGE ( 'NONE', *, *, #68415, .T. ) ;
#52796 = CARTESIAN_POINT ( 'NONE',  ( -12.03133265694088294, 78.46222587235902779, 117.9439990761035943 ) ) ;
#52797 = DIRECTION ( 'NONE',  ( 0.000000000000000000, 0.000000000000000000, 1.000000000000000000 ) ) ;
#52798 = CARTESIAN_POINT ( 'NONE',  ( 116.7947413403456522, -39.38919790731562642, 164.6146797249617748 ) ) ;
#52799 = CARTESIAN_POINT ( 'NONE',  ( 98.54061126669880366, -38.21619907818254802, 44.26999513149598897 ) ) ;
#52800 = EDGE_CURVE ( 'NONE', #36112, #44764, #75029, .T. ) ;
#52801 = FACE_OUTER_BOUND ( 'NONE', #78766, .T. ) ;
#52802 = ORIENTED_EDGE ( 'NONE', *, *, #33163, .T. ) ;
#52803 = LINE ( 'NONE', #18328, #16130 ) ;
#52804 = CARTESIAN_POINT ( 'NONE',  ( 82.06789631129603890, -16.84294903901377793, 7.549690073096890330 ) ) ;
#52805 = ORIENTED_EDGE ( 'NONE', *, *, #1943, .T. ) ;
#52806 = VERTEX_POINT ( 'NONE', #73338 ) ;
#52807 = AXIS2_PLACEMENT_3D ( 'NONE', #75075, #40548, #89157 ) ;
#52808 = AXIS2_PLACEMENT_3D ( 'NONE', #7782, #29569, #36396 ) ;
#52809 = LINE ( 'NONE', #66030, #77855 ) ;
#52810 = VECTOR ( 'NONE', #64439, 1000.000000000000000 ) ;
#52811 = ORIENTED_EDGE ( 'NONE', *, *, #54264, .T. ) ;
#52812 = VERTEX_POINT ( 'NONE', #25639 ) ;
#52813 = CARTESIAN_POINT ( 'NONE',  ( 97.06112134132963831, -37.99667316087620605, 157.4271097502474390 ) ) ;
#52814 = AXIS2_PLACEMENT_3D ( 'NONE', #21169, #34783, #33885 ) ;
#52815 = CARTESIAN_POINT ( 'NONE',  ( 101.2610328325635010, -42.99465878394229179, 46.40384839950495177 ) ) ;
#52817 = CARTESIAN_POINT ( 'NONE',  ( 103.6313148537710305, -26.19877486694289459, 210.3394347997209763 ) ) ;
#52816 = AXIS2_PLACEMENT_3D ( 'NONE', #2521, #58359, #25174 ) ;
#52818 = CONICAL_SURFACE ( 'NONE', #60108, 24.50000000000000711, 0.7419472680059182590 ) ;
#52819 = CARTESIAN_POINT ( 'NONE',  ( 103.8142050530422438, -26.84757730287814326, 165.3299109901969643 ) ) ;
#52821 = CARTESIAN_POINT ( 'NONE',  ( 97.55999611477783162, -43.80484941858547643, 257.8356252759109566 ) ) ;
#52820 = CARTESIAN_POINT ( 'NONE',  ( 98.05739576140550184, -41.07564549115163288, 21.68389642371685255 ) ) ;
#52822 = LINE ( 'NONE', #26960, #39058 ) ;
#52823 = ADVANCED_FACE ( 'NONE', ( #11580 ), #51981, .T. ) ;
#52824 = DIRECTION ( 'NONE',  ( 0.000000000000000000, 1.000000000000000000, 0.000000000000000000 ) ) ;
#52825 = VERTEX_POINT ( 'NONE', #80182 ) ;
#52826 = VERTEX_POINT ( 'NONE', #52852 ) ;
#52827 = LINE ( 'NONE', #60118, #25513 ) ;
#52828 = CARTESIAN_POINT ( 'NONE',  ( 115.4232488078209258, -30.42301107085752321, 219.3413395616249773 ) ) ;
#52829 = EDGE_LOOP ( 'NONE', ( #86502, #10083, #27244, #24455 ) ) ;
#52830 = CARTESIAN_POINT ( 'NONE',  ( 113.6857051329922683, -45.58184738042410800, 188.0994347997199725 ) ) ;
#52831 = CARTESIAN_POINT ( 'NONE',  ( 115.8245126124504907, -31.72842839644106405, 264.2397945930570700 ) ) ;
#52832 = CARTESIAN_POINT ( 'NONE',  ( -17.75984020069129343, 65.55676468737539153, 33.71262514113522712 ) ) ;
#52833 = FACE_OUTER_BOUND ( 'NONE', #42629, .T. ) ;
#52834 = CARTESIAN_POINT ( 'NONE',  ( 74.06670390244704549, -118.2784471599409812, 51.21780685541800437 ) ) ;
#52837 = CARTESIAN_POINT ( 'NONE',  ( 105.4283309587863613, -27.08694620864308789, 11.20991099019597037 ) ) ;
#52836 = DIRECTION ( 'NONE',  ( 0.000000000000000000, 0.000000000000000000, 1.000000000000000000 ) ) ;
#52835 = LINE ( 'NONE', #11096, #76649 ) ;
#52838 = DIRECTION ( 'NONE',  ( -1.639958061481212836E-42, 4.100000000000000342E-29, 1.000000000000000000 ) ) ;
#52839 = FACE_OUTER_BOUND ( 'NONE', #23640, .T. ) ;
#52840 = CARTESIAN_POINT ( 'NONE',  ( 180.3521107875639871, -35.65087443492551245, -5.074374724088000832 ) ) ;
#52841 = EDGE_CURVE ( 'NONE', #56941, #82390, #66070, .T. ) ;
#52842 = CARTESIAN_POINT ( 'NONE',  ( 73.06670390244801183, -48.82844715994099971, 198.9178068554149945 ) ) ;
#52843 = ADVANCED_FACE ( 'NONE', ( #59259 ), #24749, .F. ) ;
#52844 = DIRECTION ( 'NONE',  ( -1.000000000000000000, -1.206764157201257538E-15, 0.000000000000000000 ) ) ;
#52845 = CARTESIAN_POINT ( 'NONE',  ( -48.02966122971777452, 100.5999999999999659, 106.4272185163641780 ) ) ;
#52847 = ORIENTED_EDGE ( 'NONE', *, *, #85741, .T. ) ;
#52846 = CARTESIAN_POINT ( 'NONE',  ( -9.270368442002537179, 91.24032474172570062, -118.1933656790129987 ) ) ;
#52848 = CARTESIAN_POINT ( 'NONE',  ( 136.5663465660592806, -19.87725565066165956, 7.080220459962397683 ) ) ;
#52849 = CARTESIAN_POINT ( 'NONE',  ( 99.73754448486663193, -29.28411171159743276, 225.6956252759109702 ) ) ;
#52850 = CARTESIAN_POINT ( 'NONE',  ( 117.3712488531672165, -32.73122415481606851, 90.10895860924395606 ) ) ;
#52851 = CARTESIAN_POINT ( 'NONE',  ( 116.5662105847193999, -41.21199064955116143, 224.4756252759109714 ) ) ;
#52852 = CARTESIAN_POINT ( 'NONE',  ( 172.5664832912740110, -18.82844715994099971, 256.8086252759120498 ) ) ;
#52853 = B_SPLINE_CURVE_WITH_KNOTS ( 'NONE', 3,
 ( #18796, #4726, #12431, #25607, #5169, #66489, #52820, #32405, #81941, #60563, #80593, #46480, #73759, #18339, #74217, #11542, #39237, #26064, #53732, #81498, #19250, #46923, #40120, #19692, #47372, #40579, #75103 ),
 .UNSPECIFIED., .F., .F.,
 ( 4, 2, 1, 1, 1, 2, 2, 2, 2, 2, 2, 2, 2, 2, 4 ),
 ( 0.4999367561938997673, 0.5009134422169587708, 0.5018901282400176633, 0.5038435002861353373, 0.5077502443783706854, 0.5155637325628411594, 0.5311907089317821073, 0.5624446616696634482, 0.6249525671454257969, 0.6874604726211881456, 0.7499683780969504943, 0.8124762835727128429, 0.8749841890484753026, 0.9374920945242376513, 1.000000000000000000 ),
 .UNSPECIFIED. ) ;
#52854 = PLANE ( 'NONE',  #60529 ) ;
#52856 = CARTESIAN_POINT ( 'NONE',  ( 107.0664832912739968, 19.62155284005901024, 333.4006252759110112 ) ) ;
#52855 = CARTESIAN_POINT ( 'NONE',  ( -47.18030668273772221, 93.07500000000001705, 75.34738655934135920 ) ) ;
#52857 = PLANE ( 'NONE',  #75712 ) ;
#52858 = CYLINDRICAL_SURFACE ( 'NONE', #54358, 7.937500000000000000 ) ;
#52859 = AXIS2_PLACEMENT_3D ( 'NONE', #28522, #14922, #35788 ) ;
#52860 = EDGE_LOOP ( 'NONE', ( #70457, #24927, #8005, #24216 ) ) ;
#52861 = ORIENTED_EDGE ( 'NONE', *, *, #28563, .F. ) ;
#52862 = CARTESIAN_POINT ( 'NONE',  ( 103.6638222329471262, -28.86385020797125733, 154.8238483995059767 ) ) ;
#52864 = ORIENTED_EDGE ( 'NONE', *, *, #48843, .T. ) ;
#52863 = CARTESIAN_POINT ( 'NONE',  ( 21.03689327557619748, -23.42844715994197813, 129.9678068554150627 ) ) ;
#52865 = CARTESIAN_POINT ( 'NONE',  ( 109.7247368277677424, -27.00077089589298751, 89.86349248373032594 ) ) ;
#52866 = CARTESIAN_POINT ( 'NONE',  ( 114.4965984691700953, -29.44205611023144087, 145.4441967044819819 ) ) ;
#52867 = DIRECTION ( 'NONE',  ( 0.000000000000000000, 0.000000000000000000, -1.000000000000000000 ) ) ;
#52868 = CARTESIAN_POINT ( 'NONE',  ( 77.61460381940085540, -17.48272374588778533, 7.134497377255414108 ) ) ;
#52869 = CARTESIAN_POINT ( 'NONE',  ( 106.5667039024470455, -113.7784471599420613, -19.78219314458171141 ) ) ;
#52870 = PLANE ( 'NONE',  #61371 ) ;
#52871 = CARTESIAN_POINT ( 'NONE',  ( 101.4370486012140020, -28.02035706366309853, 70.54514908543596619 ) ) ;
#52872 = ORIENTED_EDGE ( 'NONE', *, *, #50320, .T. ) ;
#52873 = VERTEX_POINT ( 'NONE', #18831 ) ;
#52874 = ORIENTED_EDGE ( 'NONE', *, *, #37476, .T. ) ;
#52875 = CIRCLE ( 'NONE', #55742, 10.66800000000000992 ) ;
#52876 = DIRECTION ( 'NONE',  ( 0.000000000000000000, 0.000000000000000000, 1.000000000000000000 ) ) ;
#52877 = CIRCLE ( 'NONE', #58743, 82.41591158490091118 ) ;
#52879 = CARTESIAN_POINT ( 'NONE',  ( 83.06670390244796920, -58.35344715994099829, 228.3338068554150198 ) ) ;
#52878 = CARTESIAN_POINT ( 'NONE',  ( 97.29384000864243376, -37.12803473146956890, 157.3584824187679487 ) ) ;
#52880 = CIRCLE ( 'NONE', #48551, 118.5560000000000116 ) ;
#52881 = DIRECTION ( 'NONE',  ( -0.04216478779797398074, 0.9991106698809455455, 0.000000000000000000 ) ) ;
#52882 = LINE ( 'NONE', #87462, #3115 ) ;
#52884 = CARTESIAN_POINT ( 'NONE',  ( 34.92499999999999716, 82.54999999999999716, 302.8950000000000387 ) ) ;
#52883 = AXIS2_PLACEMENT_3D ( 'NONE', #39255, #66963, #4743 ) ;
#52885 = AXIS2_PLACEMENT_3D ( 'NONE', #60395, #61296, #89017 ) ;
#52886 = CARTESIAN_POINT ( 'NONE',  ( 91.90730674524625954, 86.63388195152282378, 74.89049941105180608 ) ) ;
#52887 = CARTESIAN_POINT ( 'NONE',  ( 0.000000000000000000, 223.9999999999999716, 164.6557476874258441 ) ) ;
#52888 = CARTESIAN_POINT ( 'NONE',  ( 98.32466564902610173, -28.76522518762216052, 80.73848241876795839 ) ) ;
#52889 = ORIENTED_EDGE ( 'NONE', *, *, #17313, .T. ) ;
#52890 = ORIENTED_EDGE ( 'NONE', *, *, #69690, .T. ) ;
#52891 = CARTESIAN_POINT ( 'NONE',  ( 0.8293186434173880350, 95.25000000000001421, 130.5560000000000116 ) ) ;
#52892 = CARTESIAN_POINT ( 'NONE',  ( 142.0664832912740394, -46.72944715994099596, 14.67562527591100441 ) ) ;
#52893 = LINE ( 'NONE', #88825, #84446 ) ;
#52895 = CARTESIAN_POINT ( 'NONE',  ( 99.71285092336476907, -40.27258376677666263, 169.5023760838769817 ) ) ;
#52894 = AXIS2_PLACEMENT_3D ( 'NONE', #63311, #27888, #63767 ) ;
#52896 = EDGE_CURVE ( 'NONE', #68461, #38148, #32898, .T. ) ;
#52897 = CIRCLE ( 'NONE', #77605, 3.968749999999992895 ) ;
#52898 = DIRECTION ( 'NONE',  ( -4.237773401492740281E-14, 1.000000000000000000, 0.000000000000000000 ) ) ;
#52899 = ORIENTED_EDGE ( 'NONE', *, *, #82614, .T. ) ;
#52900 = ORIENTED_EDGE ( 'NONE', *, *, #26841, .F. ) ;
#52901 = EDGE_CURVE ( 'NONE', #57610, #83459, #21556, .T. ) ;
#52902 = DIRECTION ( 'NONE',  ( 1.000000000000000078E-15, -1.000000000000000083E-30, -1.000000000000000000 ) ) ;
#52903 = ORIENTED_EDGE ( 'NONE', *, *, #37415, .F. ) ;
#52904 = ORIENTED_EDGE ( 'NONE', *, *, #48104, .T. ) ;
#52905 = PLANE ( 'NONE',  #4287 ) ;
#52906 = EDGE_CURVE ( 'NONE', #8522, #44708, #87493, .T. ) ;
#52907 = CARTESIAN_POINT ( 'NONE',  ( 113.6520771548495503, -30.75516201018407614, 205.8444404487539714 ) ) ;
#52908 = EDGE_CURVE ( 'NONE', #6901, #85061, #81081, .T. ) ;
#52909 = DIRECTION ( 'NONE',  ( 0.000000000000000000, 0.000000000000000000, -1.000000000000000000 ) ) ;
#52910 = CARTESIAN_POINT ( 'NONE',  ( -7.661254700127833495, 66.45253841614081125, 320.6630000000000109 ) ) ;
#52911 = EDGE_CURVE ( 'NONE', #11918, #86172, #39706, .T. ) ;
#52912 =( GEOMETRIC_REPRESENTATION_CONTEXT ( 3 ) GLOBAL_UNCERTAINTY_ASSIGNED_CONTEXT ( ( #30550 ) ) GLOBAL_UNIT_ASSIGNED_CONTEXT ( ( #31626, #10732, #24386 ) ) REPRESENTATION_CONTEXT ( 'NONE', 'WORKASPACE' ) );
#52913 = CARTESIAN_POINT ( 'NONE',  ( -110.5312426757802626, 62.76878794380225202, 69.48247424316639353 ) ) ;
#52914 = ORIENTED_EDGE ( 'NONE', *, *, #62048, .T. ) ;
#52915 = VERTEX_POINT ( 'NONE', #86989 ) ;
#52916 = VECTOR ( 'NONE', #25180, 1000.000000000000000 ) ;
#52917 = EDGE_LOOP ( 'NONE', ( #22585, #3289, #65553, #48102, #84010, #26704 ) ) ;
#52918 = EDGE_LOOP ( 'NONE', ( #63368, #15108, #60400, #13777 ) ) ;
#52919 = ADVANCED_FACE ( 'NONE', ( #52418 ), #46513, .F. ) ;
#52920 = B_SPLINE_CURVE_WITH_KNOTS ( 'NONE', 3,
 ( #82523, #85653, #22978, #3409, #50653, #64304, #3852, #72452, #51097, #16157, #51534, #30226, #2964, #8902, #43834, #57917, #58364, #37925 ),
 .UNSPECIFIED., .F., .F.,
 ( 4, 2, 2, 2, 2, 2, 2, 2, 4 ),
 ( 0.5000723104273193664, 0.5625632716239044040, 0.6250542328204895526, 0.6875451940170745901, 0.7500361552136596277, 0.8125271164102447763, 0.8750180776068298139, 0.9375090388034148514, 1.000000000000000000 ),
 .UNSPECIFIED. ) ;
#52921 = CARTESIAN_POINT ( 'NONE',  ( 114.9986391697397607, -34.80314782265816831, 206.8338046553059826 ) ) ;
#52922 = CARTESIAN_POINT ( 'NONE',  ( 117.3606796971436523, -32.63983085838949449, 99.13943479972098771 ) ) ;
#52923 = CARTESIAN_POINT ( 'NONE',  ( 116.6546583390153131, -32.60254457568996855, 79.14991099019697174 ) ) ;
#52924 = CARTESIAN_POINT ( 'NONE',  ( 112.8677825012601375, -28.59025478454122648, 249.5838084826162913 ) ) ;
#52925 = FACE_BOUND ( 'NONE', #15769, .T. ) ;
#52926 = CARTESIAN_POINT ( 'NONE',  ( 103.8797721312301547, -106.6957733451327215, -19.78219314458193168 ) ) ;
#52927 = CARTESIAN_POINT ( 'NONE',  ( 100.8865061632069882, -45.89117093204367137, 148.0918157521009562 ) ) ;
#52928 = EDGE_CURVE ( 'NONE', #42715, #64265, #17852, .T. ) ;
#52929 = CARTESIAN_POINT ( 'NONE',  ( 115.0667039024470313, -104.2784471599420897, -19.78219314458201694 ) ) ;
#52930 = ORIENTED_EDGE ( 'NONE', *, *, #76554, .T. ) ;
#52931 = DIRECTION ( 'NONE',  ( -1.000000000000000000, 0.000000000000000000, 0.000000000000000000 ) ) ;
#52932 = VERTEX_POINT ( 'NONE', #12024 ) ;
#52933 = ORIENTED_EDGE ( 'NONE', *, *, #86409, .T. ) ;
#52934 = PLANE ( 'NONE',  #62154 ) ;
#52935 = DIRECTION ( 'NONE',  ( 1.000000000000000000, 0.000000000000000000, 0.000000000000000000 ) ) ;
#52936 = ORIENTED_EDGE ( 'NONE', *, *, #5499, .T. ) ;
#52937 = VECTOR ( 'NONE', #47767, 1000.000000000000000 ) ;
#52938 = DIRECTION ( 'NONE',  ( 0.000000000000000000, 1.000000000000000000, 1.598363122120870523E-15 ) ) ;
#52939 = VERTEX_POINT ( 'NONE', #33352 ) ;
#52940 = VECTOR ( 'NONE', #12371, 1000.000000000000000 ) ;
#52941 = AXIS2_PLACEMENT_3D ( 'NONE', #73712, #45979, #6032 ) ;
#52942 = DIRECTION ( 'NONE',  ( 1.000000000000000000, 0.000000000000000000, 0.000000000000000000 ) ) ;
#52943 = CARTESIAN_POINT ( 'NONE',  ( 115.1669806615814622, -43.29214270484202132, 88.28419670448195689 ) ) ;
#52944 = DIRECTION ( 'NONE',  ( 0.000000000000000000, -1.000000000000000000, 0.000000000000000000 ) ) ;
#52945 = VECTOR ( 'NONE', #10804, 1000.000000000000000 ) ;
#52946 = CARTESIAN_POINT ( 'NONE',  ( 48.16670390244701139, -28.27351298637280408, -5.074374724088000832 ) ) ;
#52947 = DIRECTION ( 'NONE',  ( 0.000000000000000000, -0.000000000000000000, -1.000000000000000000 ) ) ;
#52948 = CARTESIAN_POINT ( 'NONE',  ( 116.7039036015866031, -32.90075090702271865, 99.13943479972198247 ) ) ;
#52950 = CARTESIAN_POINT ( 'NONE',  ( 96.64068249873270133, -36.21262657180042766, 167.2870538473399620 ) ) ;
#52949 = DIRECTION ( 'NONE',  ( -0.000000000000000000, 1.000000000000000000, -0.000000000000000000 ) ) ;
#52951 = CARTESIAN_POINT ( 'NONE',  ( 38.10000000000000142, 69.84999999999999432, 358.0130000000000337 ) ) ;
#52952 = DIRECTION ( 'NONE',  ( 3.340531404218880531E-13, -1.000000000000000000, 3.350531404218880242E-28 ) ) ;
#52953 = ORIENTED_EDGE ( 'NONE', *, *, #26850, .F. ) ;
#52954 = CARTESIAN_POINT ( 'NONE',  ( 49.21213752016101495, -29.73316016639650172, -5.074374724088000832 ) ) ;
#52955 = AXIS2_PLACEMENT_3D ( 'NONE', #26863, #47740, #75475 ) ;
#52956 = EDGE_CURVE ( 'NONE', #15070, #12137, #66525, .T. ) ;
#52957 = FACE_OUTER_BOUND ( 'NONE', #21261, .T. ) ;
#52958 = EDGE_CURVE ( 'NONE', #17260, #65590, #88993, .T. ) ;
#52959 = DIRECTION ( 'NONE',  ( 0.000000000000000000, 1.000000000000000000, 1.914177628664063178E-15 ) ) ;
#52960 = ADVANCED_FACE ( 'NONE', ( #66976 ), #1918, .T. ) ;
#52961 = VECTOR ( 'NONE', #56705, 1000.000000000000000 ) ;
#52962 = DIRECTION ( 'NONE',  ( 1.000000000000000000, 0.000000000000000000, -2.973811673103097665E-16 ) ) ;
#52964 = ORIENTED_EDGE ( 'NONE', *, *, #73583, .F. ) ;
#52963 = CARTESIAN_POINT ( 'NONE',  ( 116.9264758816979537, -41.82782236628663242, 243.4346728949589647 ) ) ;
#52965 = CARTESIAN_POINT ( 'NONE',  ( 97.07201709675129564, -35.37882905153811208, 146.2189892174000363 ) ) ;
#52966 = CARTESIAN_POINT ( 'NONE',  ( 96.86769303131731590, -30.64611497598638579, 276.8984824187680829 ) ) ;
#52967 = CARTESIAN_POINT ( 'NONE',  ( 114.7580948764747291, -43.83100269166961027, 119.2327681330539804 ) ) ;
#52968 = EDGE_CURVE ( 'NONE', #84350, #17132, #39271, .T. ) ;
#52969 = DIRECTION ( 'NONE',  ( -0.7071067811865671127, -0.7071067811865279218, -7.071067811865664660E-16 ) ) ;
#52970 = CARTESIAN_POINT ( 'NONE',  ( 12.69999999999999929, 82.96435431876524547, -129.9368274816650626 ) ) ;
#52971 = AXIS2_PLACEMENT_3D ( 'NONE', #11359, #88576, #39061 ) ;
#52972 = CYLINDRICAL_SURFACE ( 'NONE', #10912, 2.117000000000000881 ) ;
#52973 = CARTESIAN_POINT ( 'NONE',  ( 105.7149977036519459, -46.72378562122258927, 263.4690551747434597 ) ) ;
#52974 = ORIENTED_EDGE ( 'NONE', *, *, #72767, .F. ) ;
#52975 = CIRCLE ( 'NONE', #13856, 7.937500000000000000 ) ;
#52976 = VERTEX_POINT ( 'NONE', #88338 ) ;
#52977 = VERTEX_POINT ( 'NONE', #88782 ) ;
#52978 = VERTEX_POINT ( 'NONE', #17496 ) ;
#52979 = CYLINDRICAL_SURFACE ( 'NONE', #26252, 32.50000000000001421 ) ;
#52980 = CARTESIAN_POINT ( 'NONE',  ( 100.4250012405661607, -28.72198927997979823, 36.62705384733894221 ) ) ;
#52981 = DIRECTION ( 'NONE',  ( -2.279500465453769633E-16, 3.512896218562319948E-31, 1.000000000000000000 ) ) ;
#52982 = CARTESIAN_POINT ( 'NONE',  ( 77.11671781838086304, -140.6784471615123664, 245.5822703020409961 ) ) ;
#52984 = DIRECTION ( 'NONE',  ( 0.000000000000000000, 0.000000000000000000, 1.000000000000000000 ) ) ;
#52983 = CARTESIAN_POINT ( 'NONE',  ( -492.0614999999999668, 93.66249999999999432, 90.48749999999999716 ) ) ;
#52985 = CARTESIAN_POINT ( 'NONE',  ( 97.42200983434074146, -37.84960760947268454, 235.8409912566479818 ) ) ;
#52986 = ORIENTED_EDGE ( 'NONE', *, *, #40841, .F. ) ;
#52987 = VERTEX_POINT ( 'NONE', #56806 ) ;
#52988 = AXIS2_PLACEMENT_3D ( 'NONE', #2731, #24067, #65393 ) ;
#52989 = ORIENTED_EDGE ( 'NONE', *, *, #77080, .F. ) ;
#52990 = DIRECTION ( 'NONE',  ( -0.7071067811864671926, -0.7071067811866279529, -7.071067811864976379E-16 ) ) ;
#52991 = CIRCLE ( 'NONE', #13874, 3.300000000000000711 ) ;
#52992 = CARTESIAN_POINT ( 'NONE',  ( 116.3216177720312317, -32.94249360885015676, 184.1356252759109680 ) ) ;
#52993 = CARTESIAN_POINT ( 'NONE',  ( 34.33598329127499227, -36.32844715994100682, -5.074374724088000832 ) ) ;
#52994 = CARTESIAN_POINT ( 'NONE',  ( 109.8015415646094226, -45.15840846867854452, 9.258726163039964874 ) ) ;
#52995 = CARTESIAN_POINT ( 'NONE',  ( 122.2189888861420286, -96.57077177933004464, -19.18411693322927292 ) ) ;
#52996 = DIRECTION ( 'NONE',  ( 4.299999999999999979E-14, -1.000000000000000000, 0.000000000000000000 ) ) ;
#52997 = CARTESIAN_POINT ( 'NONE',  ( 104.4938967476557536, -26.68352342390101128, 245.2880062282919482 ) ) ;
#52998 = DIRECTION ( 'NONE',  ( -1.000000000000000000, -1.206764157201257538E-15, 0.000000000000000000 ) ) ;
#52999 = ORIENTED_EDGE ( 'NONE', *, *, #37668, .T. ) ;
#53000 = DIRECTION ( 'NONE',  ( 0.000000000000000000, 1.000000000000000000, 0.000000000000000000 ) ) ;
#53001 = DIRECTION ( 'NONE',  ( 1.000000000000000078E-15, -1.000000000000000083E-30, -1.000000000000000000 ) ) ;
#53002 = CARTESIAN_POINT ( 'NONE',  ( 115.5682441604615178, -40.44643428488449644, 56.31666179816296847 ) ) ;
#53003 = VECTOR ( 'NONE', #82672, 1000.000000000000114 ) ;
#53004 = AXIS2_PLACEMENT_3D ( 'NONE', #19519, #39516, #12718 ) ;
#53005 = AXIS2_PLACEMENT_3D ( 'NONE', #14521, #1340, #6351 ) ;
#53006 = FACE_OUTER_BOUND ( 'NONE', #48703, .T. ) ;
#53007 = AXIS2_PLACEMENT_3D ( 'NONE', #68919, #20768, #7145 ) ;
#53008 = EDGE_CURVE ( 'NONE', #67672, #16139, #37796, .T. ) ;
#53009 = DIRECTION ( 'NONE',  ( 1.000000000000000000, 4.299999999999999979E-14, 1.000000000000000078E-15 ) ) ;
#53010 = DIRECTION ( 'NONE',  ( 0.000000000000000000, 0.000000000000000000, -1.000000000000000000 ) ) ;
#53011 = EDGE_LOOP ( 'NONE', ( #6072, #13756, #80412, #55737 ) ) ;
#53012 = CARTESIAN_POINT ( 'NONE',  ( 33.78129701732998313, -35.65087443492610930, -5.074374724088000832 ) ) ;
#53013 = EDGE_CURVE ( 'NONE', #54044, #19525, #67194, .T. ) ;
#53014 = CARTESIAN_POINT ( 'NONE',  ( 122.6405678466407352, 60.67261296635635404, -44.76865280868378250 ) ) ;
#53015 = ORIENTED_EDGE ( 'NONE', *, *, #22019, .F. ) ;
#53016 = CARTESIAN_POINT ( 'NONE',  ( 116.5335121716806981, -32.36339692672488155, 104.1699109901969535 ) ) ;
#53017 = VERTEX_POINT ( 'NONE', #28663 ) ;
#53018 = CARTESIAN_POINT ( 'NONE',  ( 97.46629167631436985, -35.27791395320982559, 70.62956268521996606 ) ) ;
#53019 = EDGE_CURVE ( 'NONE', #88126, #33837, #47408, .T. ) ;
#53020 = DIRECTION ( 'NONE',  ( 1.000000000000000078E-15, 0.000000000000000000, 1.000000000000000000 ) ) ;
#53021 = CARTESIAN_POINT ( 'NONE',  ( 99.74759560186635099, -41.77880479991928553, 123.2387261630399564 ) ) ;
#53022 = EDGE_CURVE ( 'NONE', #87703, #48933, #56355, .T. ) ;
#53023 = LINE ( 'NONE', #25350, #31485 ) ;
#53024 = CARTESIAN_POINT ( 'NONE',  ( 1.474728703520907694E-14, 239.0000000000000000, 104.2754207677255920 ) ) ;
#53025 = CARTESIAN_POINT ( 'NONE',  ( 117.5094244910773114, -37.01621876064744754, 39.80419670448193159 ) ) ;
#53027 = EDGE_CURVE ( 'NONE', #81179, #60711, #21868, .T. ) ;
#53026 = DIRECTION ( 'NONE',  ( 0.000000000000000000, 0.000000000000000000, 1.000000000000000000 ) ) ;
#53028 = ORIENTED_EDGE ( 'NONE', *, *, #74295, .T. ) ;
#53029 = CARTESIAN_POINT ( 'NONE',  ( 115.0370918404214393, -42.90867283834190715, 258.3021863231967927 ) ) ;
#53030 = EDGE_LOOP ( 'NONE', ( #80738, #56079, #78921, #58026 ) ) ;
#53031 = CARTESIAN_POINT ( 'NONE',  ( -118.5560669097358897, 69.84937538953988678, 0.8299548590975466267 ) ) ;
#53032 = ORIENTED_EDGE ( 'NONE', *, *, #34069, .F. ) ;
#53033 = AXIS2_PLACEMENT_3D ( 'NONE', #30021, #29566, #29124 ) ;
#53034 = ORIENTED_EDGE ( 'NONE', *, *, #87828, .T. ) ;
#53035 = ADVANCED_FACE ( 'NONE', ( #77272 ), #42718, .F. ) ;
#53036 = B_SPLINE_CURVE_WITH_KNOTS ( 'NONE', 3,
 ( #43750, #16509, #86450, #71487, #51012, #72806, #85568, #57379, #23782, #9687, #85122, #79638, #9249, #22889, #50565, #2881, #86009, #30580 ),
 .UNSPECIFIED., .F., .F.,
 ( 4, 2, 2, 2, 2, 2, 2, 2, 4 ),
 ( 0.000000000000000000, 0.06249892886305533773, 0.1249978577261106755, 0.1874967865891660201, 0.2499957154522213509, 0.3124946443152766817, 0.3749935731783320403, 0.4374925020413873433, 0.4999914309044427019 ),
 .UNSPECIFIED. ) ;
#53037 = CARTESIAN_POINT ( 'NONE',  ( 107.0667039024469886, -67.87844715994094713, 173.2178068554179902 ) ) ;
#53038 = VERTEX_POINT ( 'NONE', #15045 ) ;
#53039 = CARTESIAN_POINT ( 'NONE',  ( 112.3177584634463244, -44.98096486020163098, 263.0270538473400279 ) ) ;
#53040 = DIRECTION ( 'NONE',  ( 0.000000000000000000, 0.000000000000000000, -1.000000000000000000 ) ) ;
#53041 = CARTESIAN_POINT ( 'NONE',  ( 6.349999999999999645, 82.54999999999999716, 302.8950000000000387 ) ) ;
#53042 = CARTESIAN_POINT ( 'NONE',  ( 109.6429888323185224, -46.83113546657025950, 43.77562527591094721 ) ) ;
#53043 = EDGE_CURVE ( 'NONE', #48663, #36108, #40611, .T. ) ;
#53044 = CARTESIAN_POINT ( 'NONE',  ( 97.92315705725079056, -40.78053340632050094, 42.65836484899426040 ) ) ;
#53045 = VERTEX_POINT ( 'NONE', #68328 ) ;
#53046 = CARTESIAN_POINT ( 'NONE',  ( 105.7993578692051244, -26.72404692965724848, 115.1793930805829547 ) ) ;
#53047 = DIRECTION ( 'NONE',  ( 0.000000000000000000, 1.000000000000000000, 0.000000000000000000 ) ) ;
#53048 = VECTOR ( 'NONE', #27707, 1000.000000000000000 ) ;
#53050 = ORIENTED_EDGE ( 'NONE', *, *, #5508, .T. ) ;
#53049 = ADVANCED_FACE ( 'NONE', ( #22311 ), #54656, .F. ) ;
#53051 = DIRECTION ( 'NONE',  ( -1.000000000000000078E-15, 1.000000000000000000, 0.000000000000000000 ) ) ;
#53052 = LINE ( 'NONE', #73987, #30991 ) ;
#53053 = CARTESIAN_POINT ( 'NONE',  ( 118.0177608886754967, -35.41288285714057338, 238.9337205140059552 ) ) ;
#53054 = CARTESIAN_POINT ( 'NONE',  ( 48.79742451362098166, -36.32844715994040996, -5.074374724088000832 ) ) ;
#53055 = CARTESIAN_POINT ( 'NONE',  ( -479.3614999999999782, 85.41360802895360393, 11.11250000000036131 ) ) ;
#53056 = CARTESIAN_POINT ( 'NONE',  ( 79.87807227642889529, -39.47944715994105280, 1.625625275910943301 ) ) ;
#53057 = CARTESIAN_POINT ( 'NONE',  ( 101.3905103160957850, -43.11219441383617124, 266.4209912566481080 ) ) ;
#53059 = CARTESIAN_POINT ( 'NONE',  ( 116.9541756933414263, -33.49491404195861577, 85.07848241876791917 ) ) ;
#53058 = DIRECTION ( 'NONE',  ( 0.000000000000000000, -1.000000000000000000, 0.000000000000000000 ) ) ;
#53060 = CARTESIAN_POINT ( 'NONE',  ( 114.1934708208216307, 70.42029666602465454, 63.28548749111810423 ) ) ;
#53061 = CARTESIAN_POINT ( 'NONE',  ( 103.1581569894456294, -27.01699888143334860, 130.3813395616259925 ) ) ;
#53062 = VERTEX_POINT ( 'NONE', #71366 ) ;
#53063 = FACE_OUTER_BOUND ( 'NONE', #57132, .T. ) ;
#53064 = ORIENTED_EDGE ( 'NONE', *, *, #922, .F. ) ;
#53065 = DIRECTION ( 'NONE',  ( 1.000000000000000000, 4.163336342344333240E-14, 0.000000000000000000 ) ) ;
#53066 = PLANE ( 'NONE',  #75445 ) ;
#53067 = CARTESIAN_POINT ( 'NONE',  ( 20.03715912545730760, -24.42818131006189830, 300.4678068554150059 ) ) ;
#53068 = ORIENTED_EDGE ( 'NONE', *, *, #6337, .F. ) ;
#53069 = ADVANCED_FACE ( 'NONE', ( #35465 ), #35921, .F. ) ;
#53070 = CARTESIAN_POINT ( 'NONE',  ( 97.60797852784317286, -39.98268459812312869, 51.59008640786052524 ) ) ;
#53072 = ORIENTED_EDGE ( 'NONE', *, *, #81519, .F. ) ;
#53071 = CARTESIAN_POINT ( 'NONE',  ( 108.3247603638532865, -47.12287801086134920, 117.6727681330539639 ) ) ;
#53073 = DIRECTION ( 'NONE',  ( 0.000000000000000000, 0.000000000000000000, 1.000000000000000000 ) ) ;
#53074 = EDGE_CURVE ( 'NONE', #79111, #39595, #14602, .T. ) ;
#53075 = VECTOR ( 'NONE', #3148, 1000.000000000000000 ) ;
#53076 = CARTESIAN_POINT ( 'NONE',  ( -130.4018701889608565, 93.55484823631827851, 6.352633250518059604 ) ) ;
#53078 = CIRCLE ( 'NONE', #31327, 9.525000000000000355 ) ;
#53077 = DIRECTION ( 'NONE',  ( -1.000000000000000000, -1.000000000000000078E-15, -1.000000000000000078E-15 ) ) ;
#53079 = EDGE_LOOP ( 'NONE', ( #67667, #15582, #66175, #20142 ) ) ;
#53080 = CARTESIAN_POINT ( 'NONE',  ( 97.81638875629413121, -31.87330516686267501, 135.9413395616259947 ) ) ;
#53081 = VECTOR ( 'NONE', #86195, 1000.000000000000000 ) ;
#53082 = APPLICATION_PROTOCOL_DEFINITION ( 'draft international standard', 'automotive_design', 1998, #71799 ) ;
#53083 = CIRCLE ( 'NONE', #74917, 34.13125000000000142 ) ;
#53084 = DIRECTION ( 'NONE',  ( 0.9963424814100680926, -0.08544974978095691565, 0.000000000000000000 ) ) ;
#53085 = DIRECTION ( 'NONE',  ( -1.424786214935630051E-15, 0.000000000000000000, 1.000000000000000000 ) ) ;
#53086 = VERTEX_POINT ( 'NONE', #1867 ) ;
#53087 = ORIENTED_EDGE ( 'NONE', *, *, #4672, .T. ) ;
#53088 = CARTESIAN_POINT ( 'NONE',  ( 74.06670390244704549, -118.2784471599409812, 222.2178068554179902 ) ) ;
#53089 = B_SPLINE_SURFACE_WITH_KNOTS ( 'NONE', 3, 3, ( 
 ( #16286, #21089, #80745, #34707 ),
 ( #53894, #83319, #76497, #73464 ),
 ( #88461, #45734, #18502, #12598 ),
 ( #74821, #4882, #66651, #66193 ),
 ( #4439, #32127, #11702, #32574 ) ),
 .UNSPECIFIED., .F., .F., .F.,
 ( 4, 1, 4 ),
 ( 4, 4 ),
 ( 0.000000000000000000, 0.5714285714285709528, 1.000000000000000000 ),
 ( 0.1481392554759810021, 0.3635576785635249997 ),
 .UNSPECIFIED. ) ;
#53090 = CARTESIAN_POINT ( 'NONE',  ( 83.52531662946692848, 87.03008507238372715, -100.3414980266870913 ) ) ;
#53091 = DIRECTION ( 'NONE',  ( -2.106816776397999944E-14, 1.000000000000000000, -2.206816776398000223E-29 ) ) ;
#53092 = DIRECTION ( 'NONE',  ( 0.000000000000000000, 1.000000000000000000, 0.000000000000000000 ) ) ;
#53094 = CARTESIAN_POINT ( 'NONE',  ( -10.08473622792051039, 74.81935728795534146, -118.1266015380916912 ) ) ;
#53093 = CARTESIAN_POINT ( 'NONE',  ( 109.7246038384062246, -27.00073569414776387, 104.8648133147524391 ) ) ;
#53095 = DIRECTION ( 'NONE',  ( 0.000000000000000000, 0.000000000000000000, 1.000000000000000000 ) ) ;
#53096 = AXIS2_PLACEMENT_3D ( 'NONE', #42901, #23833, #85624 ) ;
#53097 = EDGE_CURVE ( 'NONE', #58575, #38868, #36739, .T. ) ;
#53098 = ORIENTED_EDGE ( 'NONE', *, *, #86717, .F. ) ;
#53099 =( BOUNDED_CURVE ( )  B_SPLINE_CURVE ( 3, ( #54051, #74978, #45900, #4145 ),
 .UNSPECIFIED., .F., .F. ) 
 B_SPLINE_CURVE_WITH_KNOTS ( ( 4, 4 ),
 ( 1.570796326781801477, 3.141592653579262873 ),
 .UNSPECIFIED. ) 
 CURVE ( )  GEOMETRIC_REPRESENTATION_ITEM ( )  RATIONAL_B_SPLINE_CURVE ( ( 1.000000000000000000, 0.8047378541237604210, 0.8047378541237604210, 1.000000000000000000 ) ) 
 REPRESENTATION_ITEM ( '' )  );
#53100 = VECTOR ( 'NONE', #46069, 1000.000000000000000 ) ;
#53101 = DIRECTION ( 'NONE',  ( -1.000000000000000078E-15, 0.000000000000000000, -1.000000000000000000 ) ) ;
#53102 = CARTESIAN_POINT ( 'NONE',  ( 107.5349099188610893, -47.08895302312297559, 188.6003871806719587 ) ) ;
#53104 = EDGE_LOOP ( 'NONE', ( #42026, #34649, #27333, #2294, #83025, #3228, #19775, #26029 ) ) ;
#53103 = PLANE ( 'NONE',  #52971 ) ;
#53105 = CARTESIAN_POINT ( 'NONE',  ( 104.9021620152489476, -46.26774620671717031, 68.39848241876694601 ) ) ;
#53106 = CARTESIAN_POINT ( 'NONE',  ( 107.0667039024470313, -104.2784471599413934, 2.217806855418003043 ) ) ;
#53107 = DIRECTION ( 'NONE',  ( -1.000000000000000000, 0.000000000000000000, 0.000000000000000000 ) ) ;
#53108 = DIRECTION ( 'NONE',  ( 0.000000000000000000, 0.000000000000000000, -1.000000000000000000 ) ) ;
#53109 = ORIENTED_EDGE ( 'NONE', *, *, #3146, .F. ) ;
#53110 = DIRECTION ( 'NONE',  ( 1.000000000000000000, 0.000000000000000000, 1.472650733923983947E-14 ) ) ;
#53111 = ORIENTED_EDGE ( 'NONE', *, *, #51301, .F. ) ;
#53112 = ORIENTED_EDGE ( 'NONE', *, *, #42484, .T. ) ;
#53113 = VECTOR ( 'NONE', #57642, 1000.000000000000000 ) ;
#53114 = EDGE_CURVE ( 'NONE', #63918, #46374, #57251, .T. ) ;
#53115 = CARTESIAN_POINT ( 'NONE',  ( 103.8678987209337947, -28.46522696937008945, 211.8015833058969690 ) ) ;
#53116 = CARTESIAN_POINT ( 'NONE',  ( 104.4090465223629707, -46.45838000546697089, 53.36450883979372151 ) ) ;
#53117 = CARTESIAN_POINT ( 'NONE',  ( -83.41565754067454463, 86.63355734047004830, 100.4326241145872984 ) ) ;
#53118 = ADVANCED_FACE ( 'NONE', ( #70008 ), #86323, .F. ) ;
#53119 = EDGE_CURVE ( 'NONE', #17979, #53213, #23662, .T. ) ;
#53120 = DIRECTION ( 'NONE',  ( -1.000000000000000000, 0.000000000000000000, 0.000000000000000000 ) ) ;
#53121 = DIRECTION ( 'NONE',  ( -0.7071067812159671506, -0.7071067811571278838, -6.612322856129998538E-17 ) ) ;
#53122 = ORIENTED_EDGE ( 'NONE', *, *, #60114, .T. ) ;
#53123 = DIRECTION ( 'NONE',  ( 0.000000000000000000, 0.000000000000000000, -1.000000000000000000 ) ) ;
#53124 = ADVANCED_FACE ( 'NONE', ( #24102 ), #19347, .T. ) ;
#53125 = DIRECTION ( 'NONE',  ( -1.000000000000000000, 0.000000000000000000, 0.000000000000000000 ) ) ;
#53126 = VERTEX_POINT ( 'NONE', #10462 ) ;
#53127 = CARTESIAN_POINT ( 'NONE',  ( 115.9452887564414851, -42.19329433630747417, 18.38705384733896153 ) ) ;
#53128 = ORIENTED_EDGE ( 'NONE', *, *, #24256, .F. ) ;
#53129 = ORIENTED_EDGE ( 'NONE', *, *, #11783, .T. ) ;
#53130 = CARTESIAN_POINT ( 'NONE',  ( 99.03493788190004921, -39.95360648959476180, 249.4604713219719656 ) ) ;
#53131 = LINE ( 'NONE', #19096, #60426 ) ;
#53132 = CYLINDRICAL_SURFACE ( 'NONE', #25823, 5.562599999999973122 ) ;
#53133 = DIRECTION ( 'NONE',  ( -1.000000000000000078E-15, 1.000000000000000083E-30, 1.000000000000000000 ) ) ;
#53134 = CARTESIAN_POINT ( 'NONE',  ( 49.16670390244661348, -28.27351298637376686, 117.4678068554150485 ) ) ;
#53135 = VECTOR ( 'NONE', #37449, 1000.000000000000000 ) ;
#53136 = CARTESIAN_POINT ( 'NONE',  ( 104.4428039971878803, -26.59488813107328653, 196.2784824187679362 ) ) ;
#53138 = LINE ( 'NONE', #58638, #65944 ) ;
#53137 = CIRCLE ( 'NONE', #25614, 218.1859999999999786 ) ;
#53139 = ADVANCED_FACE ( 'NONE', ( #37275 ), #85453, .F. ) ;
#53140 = ORIENTED_EDGE ( 'NONE', *, *, #29281, .T. ) ;
#53141 = AXIS2_PLACEMENT_3D ( 'NONE', #50204, #37485, #36144 ) ;
#53142 = CARTESIAN_POINT ( 'NONE',  ( 98.05938055883913762, -31.39417958322244218, 81.90133956162493689 ) ) ;
#53143 = MECHANICAL_DESIGN_GEOMETRIC_PRESENTATION_REPRESENTATION (  '', ( #83612 ), #77840 ) ;
#53144 = DIRECTION ( 'NONE',  ( -1.042183321081676705E-15, -1.000000000000000000, 0.000000000000000000 ) ) ;
#53145 = CIRCLE ( 'NONE', #32879, 0.5000000000000004441 ) ;
#53146 = ORIENTED_EDGE ( 'NONE', *, *, #17093, .F. ) ;
#53147 = ORIENTED_EDGE ( 'NONE', *, *, #45253, .T. ) ;
#53148 = VERTEX_POINT ( 'NONE', #50894 ) ;
#53149 = EDGE_CURVE ( 'NONE', #83508, #68103, #17726, .T. ) ;
#53150 = CARTESIAN_POINT ( 'NONE',  ( 97.31589304778262317, -39.30609602821370174, 161.5312681493450668 ) ) ;
#53151 = LINE ( 'NONE', #46348, #73211 ) ;
#53152 = CARTESIAN_POINT ( 'NONE',  ( 97.81219835445369881, -40.51719899421586746, 151.6362400511890769 ) ) ;
#53153 = CARTESIAN_POINT ( 'NONE',  ( 100.3267271402381624, -32.12451360540737255, 118.6680903695919653 ) ) ;
#53154 = CARTESIAN_POINT ( 'NONE',  ( 116.9053397700284478, -41.81689336946376301, 239.4346728949589647 ) ) ;
#53155 = EDGE_CURVE ( 'NONE', #86605, #58432, #45402, .T. ) ;
#53156 = CARTESIAN_POINT ( 'NONE',  ( 71.06648329127399677, -18.82844715994099971, 17.92562527591199739 ) ) ;
#53157 = ORIENTED_EDGE ( 'NONE', *, *, #6065, .T. ) ;
#53158 = CARTESIAN_POINT ( 'NONE',  ( 129.9368274816652331, 82.54999999999999716, -12.69999999999864038 ) ) ;
#53159 = AXIS2_PLACEMENT_3D ( 'NONE', #59217, #86947, #87836 ) ;
#53160 = CARTESIAN_POINT ( 'NONE',  ( 0.000000000000000000, 65.60000000000000853, 0.000000000000000000 ) ) ;
#53161 = VERTEX_POINT ( 'NONE', #78637 ) ;
#53162 = ORIENTED_EDGE ( 'NONE', *, *, #64251, .F. ) ;
#53163 = AXIS2_PLACEMENT_3D ( 'NONE', #85302, #79374, #23078 ) ;
#53164 = FACE_OUTER_BOUND ( 'NONE', #24586, .T. ) ;
#53165 = EDGE_LOOP ( 'NONE', ( #32874, #39899, #48827, #59638, #44209, #61823 ) ) ;
#53166 = EDGE_LOOP ( 'NONE', ( #68688, #801, #48334, #16014 ) ) ;
#53167 = CARTESIAN_POINT ( 'NONE',  ( 180.1667039024460166, -28.27351298637340093, -5.074374724088000832 ) ) ;
#53168 = DIRECTION ( 'NONE',  ( 3.100000000000000258E-29, -3.100000000000000044E-14, -1.000000000000000000 ) ) ;
#53169 = DIRECTION ( 'NONE',  ( 1.000000000000000000, 0.000000000000000000, 0.000000000000000000 ) ) ;
#53170 = CARTESIAN_POINT ( 'NONE',  ( 107.8370078009992028, -28.22187835749811313, 154.4267055423619581 ) ) ;
#53171 = CARTESIAN_POINT ( 'NONE',  ( 106.2486884972880432, -26.25648168547507311, 25.13848241876792855 ) ) ;
#53172 = CARTESIAN_POINT ( 'NONE',  ( 112.1373864550455153, -28.01170058494273718, 125.6566369152155005 ) ) ;
#53173 = ORIENTED_EDGE ( 'NONE', *, *, #34620, .T. ) ;
#53174 = CARTESIAN_POINT ( 'NONE',  ( 0.000000000000000000, 239.0000000000000000, 154.6557476874258441 ) ) ;
#53175 = ORIENTED_EDGE ( 'NONE', *, *, #42801, .F. ) ;
#53176 = DIRECTION ( 'NONE',  ( -1.000000000000000078E-15, 1.000000000000000000, 0.000000000000000000 ) ) ;
#53177 = VERTEX_POINT ( 'NONE', #38165 ) ;
#53178 = LINE ( 'NONE', #31873, #76982 ) ;
#53179 = CARTESIAN_POINT ( 'NONE',  ( -6.309997437435098888, 71.63602457591818506, 118.3885225546303133 ) ) ;
#53180 = EDGE_CURVE ( 'NONE', #86096, #69445, #45841, .T. ) ;
#53181 = CARTESIAN_POINT ( 'NONE',  ( -68.53801554307339927, 127.0000000000000000, -74.15067561874339219 ) ) ;
#53182 = VECTOR ( 'NONE', #71300, 1000.000000000000000 ) ;
#53183 = VECTOR ( 'NONE', #25864, 1000.000000000000000 ) ;
#53184 = CARTESIAN_POINT ( 'NONE',  ( 83.06670390244804025, -51.22944715994108122, 231.5838068554169524 ) ) ;
#53185 = ORIENTED_EDGE ( 'NONE', *, *, #55044, .T. ) ;
#53186 = CARTESIAN_POINT ( 'NONE',  ( 109.6173639926175269, -25.13086864565549661, 29.90419670448196854 ) ) ;
#53187 = CARTESIAN_POINT ( 'NONE',  ( 98.68765228159747949, -43.00544673443933874, 62.83848241876793850 ) ) ;
#53188 =( NAMED_UNIT ( * ) SI_UNIT ( $, .STERADIAN. ) SOLID_ANGLE_UNIT ( ) );
#53190 = DIRECTION ( 'NONE',  ( 0.000000000000000000, 0.000000000000000000, 1.000000000000000000 ) ) ;
#53189 = DIRECTION ( 'NONE',  ( 0.000000000000000000, -1.000000000000000000, 0.000000000000000000 ) ) ;
#53191 = LINE ( 'NONE', #32783, #55430 ) ;
#53192 = CARTESIAN_POINT ( 'NONE',  ( 134.0664832912740110, -46.72944715994100306, 1.625625275910997480 ) ) ;
#53193 = DIRECTION ( 'NONE',  ( 1.000000000000000000, 0.000000000000000000, 0.000000000000000000 ) ) ;
#53194 = LINE ( 'NONE', #24196, #73598 ) ;
#53195 = CARTESIAN_POINT ( 'NONE',  ( 146.6849323694283669, -124.3898625509450966, 247.0153898053430055 ) ) ;
#53196 = ORIENTED_EDGE ( 'NONE', *, *, #86918, .T. ) ;
#53197 = EDGE_CURVE ( 'NONE', #59106, #50747, #66301, .T. ) ;
#53198 = CARTESIAN_POINT ( 'NONE',  ( 100.3828542815028015, -28.67117381486349004, 40.62705384733894221 ) ) ;
#53199 = CARTESIAN_POINT ( 'NONE',  ( 113.1553867986010857, -26.56284154956258092, 200.6470538473399756 ) ) ;
#53200 = CARTESIAN_POINT ( 'NONE',  ( 104.4853289249099362, -46.88901594738546663, 43.37848241876896083 ) ) ;
#53201 = AXIS2_PLACEMENT_3D ( 'NONE', #51544, #31109, #70679 ) ;
#53202 = AXIS2_PLACEMENT_3D ( 'NONE', #40412, #88583, #74491 ) ;
#53204 = DIRECTION ( 'NONE',  ( 0.000000000000000000, 0.000000000000000000, 1.000000000000000000 ) ) ;
#53203 = CARTESIAN_POINT ( 'NONE',  ( 100.8878723336333536, -44.70055754049414531, 172.0502159399892150 ) ) ;
#53205 = CARTESIAN_POINT ( 'NONE',  ( 144.5245849510534697, -140.2205661113345911, 245.5201220521130097 ) ) ;
#53206 = EDGE_CURVE ( 'NONE', #79502, #51066, #10021, .T. ) ;
#53207 = AXIS2_PLACEMENT_3D ( 'NONE', #12813, #40499, #61382 ) ;
#53208 = AXIS2_PLACEMENT_3D ( 'NONE', #32723, #82245, #88161 ) ;
#53209 = CARTESIAN_POINT ( 'NONE',  ( 115.0889047302471369, -30.61763668945012995, 185.3439586083565871 ) ) ;
#53210 = VERTEX_POINT ( 'NONE', #80405 ) ;
#53211 = CARTESIAN_POINT ( 'NONE',  ( 108.4470127171751983, -27.04659769318761775, 100.9641967044819779 ) ) ;
#53213 = VERTEX_POINT ( 'NONE', #2767 ) ;
#53212 = CARTESIAN_POINT ( 'NONE',  ( 10.18556280471778486, 90.13775373083149134, 130.1582303542269017 ) ) ;
#53214 = CARTESIAN_POINT ( 'NONE',  ( 97.19046783542286505, -39.99946004141659017, 237.5813395616249579 ) ) ;
#53215 = CARTESIAN_POINT ( 'NONE',  ( 172.5664832912740110, -32.07844715994070839, 203.6756252759119832 ) ) ;
#53216 = PRODUCT_DEFINITION_SHAPE ( 'NONE', 'NONE',  #89937 ) ;
#53217 = CARTESIAN_POINT ( 'NONE',  ( 116.7487619956327052, -34.15501469173477744, 149.0333341547117527 ) ) ;
#53218 = CARTESIAN_POINT ( 'NONE',  ( 134.0664832912739826, -18.72944715994100306, -5.074374724089001809 ) ) ;
#53219 = CARTESIAN_POINT ( 'NONE',  ( 107.0667039024479834, -48.82844715994099971, 160.9178068554150229 ) ) ;
#53220 = CARTESIAN_POINT ( 'NONE',  ( 133.0080215814357700, -39.26771232012913515, 1.799893082726756965 ) ) ;
#53221 = CARTESIAN_POINT ( 'NONE',  ( 0.000000000000000000, 61.59999999999999432, 0.000000000000000000 ) ) ;
#53222 = VECTOR ( 'NONE', #86577, 1000.000000000000000 ) ;
#53224 = CARTESIAN_POINT ( 'NONE',  ( 105.8036208730406003, -25.68330614323999228, 160.1670538473399574 ) ) ;
#53223 = VECTOR ( 'NONE', #47711, 1000.000000000000000 ) ;
#53225 = ORIENTED_EDGE ( 'NONE', *, *, #37600, .T. ) ;
#53226 = ORIENTED_EDGE ( 'NONE', *, *, #26398, .T. ) ;
#53227 = CARTESIAN_POINT ( 'NONE',  ( 108.3613424580152724, -45.52634895430261253, 139.1244404487539725 ) ) ;
#53228 = CIRCLE ( 'NONE', #34392, 5.599999999999994316 ) ;
#53229 = CARTESIAN_POINT ( 'NONE',  ( 100.1253875378072848, -39.57043109886186727, -1.864374724089012947 ) ) ;
#53231 = PLANE ( 'NONE',  #50593 ) ;
#53230 = CARTESIAN_POINT ( 'NONE',  ( 96.91794407517411969, -34.59732685048010126, 257.1737205140059928 ) ) ;
#53232 = LINE ( 'NONE', #18748, #24631 ) ;
#53233 = PLANE ( 'NONE',  #88774 ) ;
#53234 = EDGE_CURVE ( 'NONE', #27248, #58422, #30953, .T. ) ;
#53235 = CARTESIAN_POINT ( 'NONE',  ( 0.000000000000000000, 65.60000000000000853, 0.000000000000000000 ) ) ;
#53236 = FACE_OUTER_BOUND ( 'NONE', #24590, .T. ) ;
#53237 = CARTESIAN_POINT ( 'NONE',  ( 32.15435173583699680, -31.62489322948790971, -5.074374724088000832 ) ) ;
#53238 = ADVANCED_FACE ( 'NONE', ( #86770 ), #44514, .T. ) ;
#53239 = CARTESIAN_POINT ( 'NONE',  ( 151.0371591254585155, -46.82818131005592477, 129.9678068554149775 ) ) ;
#53240 = CARTESIAN_POINT ( 'NONE',  ( 99.30484619187383544, -29.80227926343058797, 190.7470538473399415 ) ) ;
#53241 = DIRECTION ( 'NONE',  ( 1.000000000000000078E-15, 1.000000000000000083E-30, -1.000000000000000000 ) ) ;
#53242 = EDGE_LOOP ( 'NONE', ( #77332, #51837, #43355, #12776, #37075 ) ) ;
#53243 = EDGE_LOOP ( 'NONE', ( #37808, #37329, #78863 ) ) ;
#53244 = EDGE_CURVE ( 'NONE', #61695, #47090, #3209, .T. ) ;
#53245 = CARTESIAN_POINT ( 'NONE',  ( -100.8068867829403956, 80.88456863959032717, -82.96304607088309524 ) ) ;
#53246 = CARTESIAN_POINT ( 'NONE',  ( 82.51464772712792239, -19.98222059079053636, 7.138441653514920660 ) ) ;
#53247 = CARTESIAN_POINT ( 'NONE',  ( 48.16670390244738797, -26.71338133339277476, 313.9678068554150059 ) ) ;
#53248 = DIRECTION ( 'NONE',  ( 1.000000000000000000, 4.163336342344333240E-14, 0.000000000000000000 ) ) ;
#53249 = CIRCLE ( 'NONE', #25725, 3.299999999999999822 ) ;
#53250 = CARTESIAN_POINT ( 'NONE',  ( 113.2420556116021260, -28.75603552117033956, 94.55263669061166354 ) ) ;
#53252 = ORIENTED_EDGE ( 'NONE', *, *, #70817, .F. ) ;
#53251 = EDGE_CURVE ( 'NONE', #18458, #48525, #73572, .T. ) ;
#53253 = CARTESIAN_POINT ( 'NONE',  ( -12.27767284950918203, 85.41138372342587104, 117.7174922484384467 ) ) ;
#53254 = CARTESIAN_POINT ( 'NONE',  ( 118.0511761103140316, -35.49834556997346624, 233.9032443235299752 ) ) ;
#53255 = LINE ( 'NONE', #86930, #74908 ) ;
#53256 = ORIENTED_EDGE ( 'NONE', *, *, #73835, .T. ) ;
#53257 = ORIENTED_EDGE ( 'NONE', *, *, #17723, .T. ) ;
#53258 = EDGE_CURVE ( 'NONE', #73498, #686, #24542, .T. ) ;
#53259 = DIRECTION ( 'NONE',  ( 0.000000000000000000, 0.000000000000000000, -1.000000000000000000 ) ) ;
#53260 = CARTESIAN_POINT ( 'NONE',  ( 50.79999999999999716, 73.02500000000000568, 219.0749999999999886 ) ) ;
#53261 = CARTESIAN_POINT ( 'NONE',  ( 99.08974868363957000, -42.79574995047337183, 166.8439877233610105 ) ) ;
#53262 = CARTESIAN_POINT ( 'NONE',  ( 102.6173380888347282, -29.88584920324980487, 23.35380465530695204 ) ) ;
#53263 = CARTESIAN_POINT ( 'NONE',  ( 97.96758126215280527, -41.86240348953004542, 132.7356252759109623 ) ) ;
#53264 = CARTESIAN_POINT ( 'NONE',  ( 63.56670390244745050, -47.82844715994014706, 129.9678068554150911 ) ) ;
#53265 = VERTEX_POINT ( 'NONE', #38602 ) ;
#53266 = VECTOR ( 'NONE', #88407, 1000.000000000000000 ) ;
#53267 = CARTESIAN_POINT ( 'NONE',  ( 188.5667039024479834, -62.87844715994099687, 262.0928068554150059 ) ) ;
#53268 = DIRECTION ( 'NONE',  ( 0.7071067811864676367, 0.7071067811866273978, 7.071067811864669709E-16 ) ) ;
#53269 = ORIENTED_EDGE ( 'NONE', *, *, #67092, .T. ) ;
#53270 = ORIENTED_EDGE ( 'NONE', *, *, #72773, .T. ) ;
#53271 = CIRCLE ( 'NONE', #12660, 29.00000000000000000 ) ;
#53272 = AXIS2_PLACEMENT_3D ( 'NONE', #59858, #52581, #26253 ) ;
#53273 = DIRECTION ( 'NONE',  ( 0.000000000000000000, 0.000000000000000000, 1.000000000000000000 ) ) ;
#53274 = AXIS2_PLACEMENT_3D ( 'NONE', #58746, #5144, #26039 ) ;
#53275 = ORIENTED_EDGE ( 'NONE', *, *, #2106, .F. ) ;
#53276 = ORIENTED_EDGE ( 'NONE', *, *, #16672, .F. ) ;
#53277 = PLANE ( 'NONE',  #19506 ) ;
#53278 = CARTESIAN_POINT ( 'NONE',  ( 98.15782025887804707, -38.35683565110198145, 50.90480078045794698 ) ) ;
#53279 = CARTESIAN_POINT ( 'NONE',  ( 113.1683672335202431, -26.54116819535108363, 204.6470538473399756 ) ) ;
#53280 = CARTESIAN_POINT ( 'NONE',  ( 102.8528367378537496, -46.24122135049443472, 177.2441967044819648 ) ) ;
#53282 = CARTESIAN_POINT ( 'NONE',  ( 114.0759046727995241, -46.25395340493271590, 29.08133956162595268 ) ) ;
#53281 = LINE ( 'NONE', #60110, #8406 ) ;
#53283 = DIRECTION ( 'NONE',  ( 0.000000000000000000, 0.8660254037844387076, 0.4999999999999998890 ) ) ;
#53284 = FACE_BOUND ( 'NONE', #41672, .T. ) ;
#53285 = ORIENTED_EDGE ( 'NONE', *, *, #57793, .F. ) ;
#53286 = AXIS2_PLACEMENT_3D ( 'NONE', #38564, #59449, #18123 ) ;
#53287 = ORIENTED_EDGE ( 'NONE', *, *, #85969, .F. ) ;
#53288 = AXIS2_PLACEMENT_3D ( 'NONE', #10489, #16863, #25011 ) ;
#53289 = VECTOR ( 'NONE', #22618, 1000.000000000000000 ) ;
#53290 = EDGE_CURVE ( 'NONE', #60678, #25804, #4087, .T. ) ;
#53291 = AXIS2_PLACEMENT_3D ( 'NONE', #86679, #24450, #81219 ) ;
#53292 = DIRECTION ( 'NONE',  ( -0.8571673007021110013, 1.917331853055865018E-16, 0.5150380749100563760 ) ) ;
#53293 = CARTESIAN_POINT ( 'NONE',  ( 98.86425576617398292, -29.25038657358478744, 230.7261014663869503 ) ) ;
#53294 = ORIENTED_EDGE ( 'NONE', *, *, #35821, .F. ) ;
#53295 = CARTESIAN_POINT ( 'NONE',  ( 96.64414437497798360, -36.48068628021362514, 196.3070538473399438 ) ) ;
#53296 = DIRECTION ( 'NONE',  ( 4.299999999999999979E-14, -1.000000000000000000, 4.400000000000000367E-29 ) ) ;
#53297 = CYLINDRICAL_SURFACE ( 'NONE', #74063, 2.117000000000007987 ) ;
#53298 = EDGE_CURVE ( 'NONE', #72757, #43367, #83170, .T. ) ;
#53299 = DIRECTION ( 'NONE',  ( 0.000000000000000000, 0.000000000000000000, 1.000000000000000000 ) ) ;
#53300 = CARTESIAN_POINT ( 'NONE',  ( 72.96458098368650269, 117.4749999999999943, 80.10833098368729566 ) ) ;
#53302 = DIRECTION ( 'NONE',  ( 1.000000000000000000, 0.000000000000000000, 0.000000000000000000 ) ) ;
#53301 = CARTESIAN_POINT ( 'NONE',  ( 107.0280868098776210, -28.61744286730494125, 277.6356252759110816 ) ) ;
#53303 = DIRECTION ( 'NONE',  ( -0.7071067812123270624, -0.7071067811607679721, 0.000000000000000000 ) ) ;
#53304 = DIRECTION ( 'NONE',  ( -0.7071067811865739960, 0.000000000000000000, -0.7071067811865210384 ) ) ;
#53305 = DIRECTION ( 'NONE',  ( 0.000000000000000000, 0.000000000000000000, 1.000000000000000000 ) ) ;
#53306 = DIRECTION ( 'NONE',  ( 2.900000000000000265E-14, -2.000000000000000155E-15, 1.000000000000000000 ) ) ;
#53307 = DIRECTION ( 'NONE',  ( 0.000000000000000000, 0.000000000000000000, 1.000000000000000000 ) ) ;
#53308 = CYLINDRICAL_SURFACE ( 'NONE', #41958, 4.762500000000000178 ) ;
#53310 = ORIENTED_EDGE ( 'NONE', *, *, #55005, .F. ) ;
#53309 = CARTESIAN_POINT ( 'NONE',  ( -12.69999999999999929, 83.38971874880475355, -117.8738102209307641 ) ) ;
#53311 = CARTESIAN_POINT ( 'NONE',  ( 62.03715912545726496, -23.42818131006022142, 300.4678068554150627 ) ) ;
#53312 = CARTESIAN_POINT ( 'NONE',  ( 109.3417050147583041, -26.53289234591626311, 224.9013395616249511 ) ) ;
#53313 = CARTESIAN_POINT ( 'NONE',  ( 113.9864041344766861, -28.11035927269328738, 115.5261014663869474 ) ) ;
#53314 = CARTESIAN_POINT ( 'NONE',  ( 111.1444126100616927, -27.08769046218140986, 240.7584824187679544 ) ) ;
#53315 = DIRECTION ( 'NONE',  ( -1.000000000000000000, 6.036837696399408848E-13, 0.000000000000000000 ) ) ;
#53316 = CARTESIAN_POINT ( 'NONE',  ( 156.5667039024482676, -48.82844715993569196, 259.7178068554149490 ) ) ;
#53318 = PLANE ( 'NONE',  #21109 ) ;
#53317 = CARTESIAN_POINT ( 'NONE',  ( -72.96458098368751166, 117.4749999999999943, 72.96458098368620426 ) ) ;
#53319 = CARTESIAN_POINT ( 'NONE',  ( 70.06670390244707392, -137.6784471599409869, 55.21780685541800437 ) ) ;
#53320 = AXIS2_PLACEMENT_3D ( 'NONE', #43128, #1374, #29526 ) ;
#53321 = CARTESIAN_POINT ( 'NONE',  ( 59.56670390244699576, -67.87844715994098976, 190.2178068554179902 ) ) ;
#53322 = EDGE_CURVE ( 'NONE', #21597, #89871, #11349, .T. ) ;
#53323 = ORIENTED_EDGE ( 'NONE', *, *, #53022, .F. ) ;
#53324 = ORIENTED_EDGE ( 'NONE', *, *, #81206, .F. ) ;
#53325 = CARTESIAN_POINT ( 'NONE',  ( 98.49703967840136443, -36.85882374884989332, 135.7609912566479409 ) ) ;
#53327 = VERTEX_POINT ( 'NONE', #48084 ) ;
#53326 = LINE ( 'NONE', #75608, #57494 ) ;
#53328 = CARTESIAN_POINT ( 'NONE',  ( -465.6921742093539933, 60.32499999999999574, 3.174999999999999822 ) ) ;
#53329 = CARTESIAN_POINT ( 'NONE',  ( 117.6568287320715882, -39.81301747186223139, 134.5889586092439743 ) ) ;
#53330 = CARTESIAN_POINT ( 'NONE',  ( 116.3214453605167478, -32.94026287388232532, 159.1356252759109680 ) ) ;
#53331 = DIRECTION ( 'NONE',  ( 1.000000000000000000, 1.261617073437676668E-15, 1.261617073437676668E-15 ) ) ;
#53332 = ORIENTED_CLOSED_SHELL ( 'NONE', *, #27142, .F. );
#53333 = LINE ( 'NONE', #40172, #66497 ) ;
#53334 = LINE ( 'NONE', #73814, #88943 ) ;
#53335 = AXIS2_PLACEMENT_3D ( 'NONE', #43146, #64951, #78605 ) ;
#53336 = CARTESIAN_POINT ( 'NONE',  ( 107.8187922529720026, -26.97765417004747945, 70.01562527591099183 ) ) ;
#53337 = ORIENTED_EDGE ( 'NONE', *, *, #88036, .F. ) ;
#53338 = EDGE_LOOP ( 'NONE', ( #73380, #9647, #73764, #40523 ) ) ;
#53339 = ORIENTED_EDGE ( 'NONE', *, *, #27021, .F. ) ;
#53340 = AXIS2_PLACEMENT_3D ( 'NONE', #56238, #76259, #14037 ) ;
#53341 = VECTOR ( 'NONE', #2849, 1000.000000000000000 ) ;
#53342 = DIRECTION ( 'NONE',  ( 0.000000000000000000, 0.000000000000000000, -1.000000000000000000 ) ) ;
#53344 = CARTESIAN_POINT ( 'NONE',  ( 50.97905606905900555, -31.62489322948711035, 313.9678068554150059 ) ) ;
#53343 = CARTESIAN_POINT ( 'NONE',  ( 114.0519814166326995, -29.87813257090978070, 145.4441967044819819 ) ) ;
#53345 = DIRECTION ( 'NONE',  ( 0.000000000000000000, 1.000000000000000000, 0.000000000000000000 ) ) ;
#53346 = CARTESIAN_POINT ( 'NONE',  ( 172.5667039024482960, -42.82844715993499563, 180.4678068554150059 ) ) ;
#53347 = ADVANCED_FACE ( 'NONE', ( #88118, #12705 ), #87660, .T. ) ;
#53348 = CARTESIAN_POINT ( 'NONE',  ( 154.4409905298078058, -0.9147987323338667709, 540.9756252759101471 ) ) ;
#53349 = CIRCLE ( 'NONE', #31658, 6.571100913904396101 ) ;
#53350 = CARTESIAN_POINT ( 'NONE',  ( 82.35292268805442006, 95.08639429146515454, 85.28591416242430512 ) ) ;
#53351 = DIRECTION ( 'NONE',  ( -1.000000000000000078E-15, 1.000000000000000000, 0.000000000000000000 ) ) ;
#53352 = CARTESIAN_POINT ( 'NONE',  ( 103.2867953297129588, -47.09177226061144239, 97.28610146638693834 ) ) ;
#53353 = VERTEX_POINT ( 'NONE', #54890 ) ;
#53354 = ADVANCED_FACE ( 'NONE', ( #25422 ), #4984, .T. ) ;
#53355 = ORIENTED_EDGE ( 'NONE', *, *, #86499, .F. ) ;
#53356 = AXIS2_PLACEMENT_3D ( 'NONE', #18128, #72220, #44488 ) ;
#53357 = EDGE_CURVE ( 'NONE', #74086, #29576, #62845, .T. ) ;
#53358 = CARTESIAN_POINT ( 'NONE',  ( 33.78129701732998313, -35.65087443492610930, -5.074374724088000832 ) ) ;
#53359 = CARTESIAN_POINT ( 'NONE',  ( -83.90854149456433220, 88.17609398443094904, -100.0213216842702906 ) ) ;
#53360 = AXIS2_PLACEMENT_3D ( 'NONE', #434, #42640, #63558 ) ;
#53361 = DIRECTION ( 'NONE',  ( -0.7071067812160284349, 0.7071067811570665995, -7.071067812159980775E-16 ) ) ;
#53362 = CARTESIAN_POINT ( 'NONE',  ( 104.2492358271959603, -44.39057208814350020, 140.1138046553059837 ) ) ;
#53363 = CARTESIAN_POINT ( 'NONE',  ( -48.26476610531311451, 53.97499999999997300, 65.76796570303405076 ) ) ;
#53364 = VERTEX_POINT ( 'NONE', #33135 ) ;
#53365 = ORIENTED_EDGE ( 'NONE', *, *, #63519, .F. ) ;
#53366 = ADVANCED_FACE ( 'NONE', ( #27212 ), #20413, .T. ) ;
#53367 = AXIS2_PLACEMENT_3D ( 'NONE', #43137, #36345, #85415 ) ;
#53368 = DIRECTION ( 'NONE',  ( 1.000000000000000000, 0.000000000000000000, 0.000000000000000000 ) ) ;
#53369 = EDGE_LOOP ( 'NONE', ( #16747, #51624, #65313, #49773 ) ) ;
#53370 = EDGE_LOOP ( 'NONE', ( #27700, #70082, #51388 ) ) ;
#53371 = EDGE_CURVE ( 'NONE', #47011, #50271, #26321, .T. ) ;
#53372 = DIRECTION ( 'NONE',  ( 0.000000000000000000, 0.000000000000000000, 1.000000000000000000 ) ) ;
#53373 = CARTESIAN_POINT ( 'NONE',  ( 107.2166699364993292, -45.61986748510933865, 209.0215833058969963 ) ) ;
#53374 = CARTESIAN_POINT ( 'NONE',  ( 172.5664832912729878, -18.82844715994071194, 198.9256252759119832 ) ) ;
#53375 = AXIS2_PLACEMENT_3D ( 'NONE', #35063, #76867, #7376 ) ;
#53376 = FACE_BOUND ( 'NONE', #42078, .T. ) ;
#53377 = AXIS2_PLACEMENT_3D ( 'NONE', #62415, #49673, #77397 ) ;
#53378 = CARTESIAN_POINT ( 'NONE',  ( -110.7180744603615352, 63.37589224994205495, 69.18472289323493385 ) ) ;
#53379 = ORIENTED_EDGE ( 'NONE', *, *, #34809, .F. ) ;
#53380 = VERTEX_POINT ( 'NONE', #53547 ) ;
#53381 = ORIENTED_EDGE ( 'NONE', *, *, #65763, .F. ) ;
#53382 = ORIENTED_EDGE ( 'NONE', *, *, #20870, .T. ) ;
#53383 = CARTESIAN_POINT ( 'NONE',  ( 113.8860208566381544, -32.24350986527421981, 252.1080903695913662 ) ) ;
#53384 = CARTESIAN_POINT ( 'NONE',  ( 97.20468889015201341, -31.68559423518837193, 95.96229194257799122 ) ) ;
#53385 = CARTESIAN_POINT ( 'NONE',  ( 115.2499566122393588, -44.12502604085376134, 83.25372051400698581 ) ) ;
#53386 = CARTESIAN_POINT ( 'NONE',  ( 107.1343666215160937, -28.01736584179905876, 249.5838068554171230 ) ) ;
#53387 = DIRECTION ( 'NONE',  ( -0.0001713722456120069274, 0.9999999853157766072, 0.000000000000000000 ) ) ;
#53388 = CARTESIAN_POINT ( 'NONE',  ( 181.5667039024459939, -18.82844715994031048, 342.9256252759119548 ) ) ;
#53389 = CARTESIAN_POINT ( 'NONE',  ( 113.6142049395107421, -45.63457611473454989, 179.0689586092439640 ) ) ;
#53390 = CARTESIAN_POINT ( 'NONE',  ( 0.000000000000000000, 184.0000000000000000, 106.1020876358972771 ) ) ;
#53391 = EDGE_LOOP ( 'NONE', ( #57620, #6419, #77402, #22694, #25867 ) ) ;
#53392 = CARTESIAN_POINT ( 'NONE',  ( 91.06648329127500574, -36.72944715993925513, 0.7256252759109548256 ) ) ;
#53393 = ORIENTED_EDGE ( 'NONE', *, *, #37162, .F. ) ;
#53394 = VECTOR ( 'NONE', #50197, 1000.000000000000000 ) ;
#53395 = VERTEX_POINT ( 'NONE', #75817 ) ;
#53396 = DIRECTION ( 'NONE',  ( 1.000000000000000078E-15, -1.000000000000000083E-30, -1.000000000000000000 ) ) ;
#53397 = CARTESIAN_POINT ( 'NONE',  ( 139.7494832912729805, -1.929447159941395817, 352.4506252759079530 ) ) ;
#53398 = EDGE_LOOP ( 'NONE', ( #88649, #46726, #81026, #36160 ) ) ;
#53399 = CARTESIAN_POINT ( 'NONE',  ( 152.0371591254585155, -47.82818131005588214, 180.4678068554149775 ) ) ;
#53400 = AXIS2_PLACEMENT_3D ( 'NONE', #86309, #26307, #13139 ) ;
#53401 = CARTESIAN_POINT ( 'NONE',  ( 116.3228127852087113, -32.93589129790882453, 90.13562527591095375 ) ) ;
#53402 = CARTESIAN_POINT ( 'NONE',  ( 116.5335121716806981, -32.36339692672488155, 104.1699109901969535 ) ) ;
#53403 = FACE_OUTER_BOUND ( 'NONE', #55965, .T. ) ;
#53404 = EDGE_CURVE ( 'NONE', #35189, #40115, #10170, .T. ) ;
#53405 = PLANE ( 'NONE',  #56502 ) ;
#53406 = CARTESIAN_POINT ( 'NONE',  ( 83.73314995793998605, 12.92155284005730387, 355.9756252759109998 ) ) ;
#53409 = CARTESIAN_POINT ( 'NONE',  ( 114.9485010938853122, -29.93956786141553295, 180.3927681330539770 ) ) ;
#53408 = CARTESIAN_POINT ( 'NONE',  ( 97.81577456866601494, -40.52739464819840265, 56.63606675467388385 ) ) ;
#53407 = CYLINDRICAL_SURFACE ( 'NONE', #36058, 6.349999999999997868 ) ;
#53410 = FACE_OUTER_BOUND ( 'NONE', #18527, .T. ) ;
#53411 = CARTESIAN_POINT ( 'NONE',  ( 179.1667039024460166, -26.71338133339251542, 342.9256252759119548 ) ) ;
#53412 = ORIENTED_EDGE ( 'NONE', *, *, #67007, .F. ) ;
#53413 = DIRECTION ( 'NONE',  ( 0.000000000000000000, 0.000000000000000000, 1.000000000000000000 ) ) ;
#53414 = AXIS2_PLACEMENT_3D ( 'NONE', #54265, #55158, #54714 ) ;
#53415 = PLANE ( 'NONE',  #45615 ) ;
#53416 = CARTESIAN_POINT ( 'NONE',  ( 99.09586653601625983, -30.55018848384835550, 135.8022601447096633 ) ) ;
#53417 = LINE ( 'NONE', #68434, #82539 ) ;
#53419 = ORIENTED_EDGE ( 'NONE', *, *, #65287, .F. ) ;
#53418 = CARTESIAN_POINT ( 'NONE',  ( 117.5348925983358583, -35.85526142194976273, 253.8927681330537780 ) ) ;
#53420 = CARTESIAN_POINT ( 'NONE',  ( 108.2708916590322019, -26.77333427660188292, 194.9803191584221622 ) ) ;
#53421 = CARTESIAN_POINT ( 'NONE',  ( 102.3694487442499934, -47.63304195565743981, 283.2527681330539053 ) ) ;
#53422 = CARTESIAN_POINT ( 'NONE',  ( 96.62748084391311920, -35.94289726309906996, 142.2670538473399517 ) ) ;
#53423 = DIRECTION ( 'NONE',  ( 1.000000000000000000, 4.299999999999999979E-14, 1.000000000000000078E-15 ) ) ;
#53424 = VECTOR ( 'NONE', #83081, 1000.000000000000000 ) ;
#53425 = FACE_OUTER_BOUND ( 'NONE', #17231, .T. ) ;
#53426 = CARTESIAN_POINT ( 'NONE',  ( 100.2530235599239887, 77.68489675156567387, -83.63178471058850505 ) ) ;
#53427 = DIRECTION ( 'NONE',  ( 1.000000000000000000, 1.000000000000000078E-15, 0.000000000000000000 ) ) ;
#53428 = LINE ( 'NONE', #82094, #61239 ) ;
#53429 = ORIENTED_EDGE ( 'NONE', *, *, #34876, .F. ) ;
#53430 = EDGE_CURVE ( 'NONE', #16139, #54231, #65523, .T. ) ;
#53431 = ORIENTED_EDGE ( 'NONE', *, *, #28757, .T. ) ;
#53432 = ORIENTED_EDGE ( 'NONE', *, *, #59277, .T. ) ;
#53433 = VECTOR ( 'NONE', #62586, 1000.000000000000000 ) ;
#53434 = ORIENTED_EDGE ( 'NONE', *, *, #12068, .T. ) ;
#53435 = LINE ( 'NONE', #81202, #4671 ) ;
#53436 = CARTESIAN_POINT ( 'NONE',  ( 115.7104945841387007, -43.58108136993639903, 44.30514908543492680 ) ) ;
#53437 = DIRECTION ( 'NONE',  ( 0.000000000000000000, 0.000000000000000000, -1.000000000000000000 ) ) ;
#53438 = DIRECTION ( 'NONE',  ( 1.000000000000000078E-15, -1.000000000000000000, 0.000000000000000000 ) ) ;
#53439 = ADVANCED_FACE ( 'NONE', ( #6324 ), #33579, .T. ) ;
#53440 = ADVANCED_FACE ( 'NONE', ( #80859 ), #47640, .T. ) ;
#53442 = DIRECTION ( 'NONE',  ( 0.000000000000000000, 1.000000000000000000, 0.000000000000000000 ) ) ;
#53441 = CARTESIAN_POINT ( 'NONE',  ( 0.000000000000000000, 215.0000000000000000, 154.6557476874258441 ) ) ;
#53443 = CARTESIAN_POINT ( 'NONE',  ( 99.66831329903114067, -43.01734891331329891, 226.3095626852189639 ) ) ;
#53444 = ORIENTED_EDGE ( 'NONE', *, *, #67423, .T. ) ;
#53445 = AXIS2_PLACEMENT_3D ( 'NONE', #42296, #75944, #68241 ) ;
#53446 = VERTEX_POINT ( 'NONE', #34016 ) ;
#53447 = ORIENTED_EDGE ( 'NONE', *, *, #83652, .F. ) ;
#53448 = CARTESIAN_POINT ( 'NONE',  ( 77.31648329127399677, -18.72944715994106346, 3.101481641215480867 ) ) ;
#53450 = EDGE_CURVE ( 'NONE', #52784, #2982, #4821, .T. ) ;
#53449 = DIRECTION ( 'NONE',  ( 0.000000000000000000, 1.000000000000000000, 0.000000000000000000 ) ) ;
#53451 = DIRECTION ( 'NONE',  ( 4.299999999999999979E-14, -1.000000000000000000, 0.000000000000000000 ) ) ;
#53452 = CARTESIAN_POINT ( 'NONE',  ( 112.1356898331015657, -28.01072921633452850, 274.6563675756979137 ) ) ;
#53453 = CARTESIAN_POINT ( 'NONE',  ( 101.5678104218880549, -29.74196420480149072, 12.03872616303996956 ) ) ;
#53454 = CARTESIAN_POINT ( 'NONE',  ( 118.1705221151482164, 90.93965867633431799, 9.571124722858908029 ) ) ;
#53455 = CARTESIAN_POINT ( 'NONE',  ( 112.1370916094985546, -28.01153175057062228, 174.6566637475011419 ) ) ;
#53456 = CARTESIAN_POINT ( 'NONE',  ( 117.4208826026019779, -36.15918394850536544, 273.8822919425783198 ) ) ;
#53457 = EDGE_CURVE ( 'NONE', #14490, #58962, #33807, .T. ) ;
#53458 = CARTESIAN_POINT ( 'NONE',  ( 134.0664832912740110, -8.729447159940999512, 293.6356252759119911 ) ) ;
#53459 = ORIENTED_EDGE ( 'NONE', *, *, #73126, .F. ) ;
#53460 = CARTESIAN_POINT ( 'NONE',  ( 103.2774713272750233, -27.47507576204077040, 56.38571505098142467 ) ) ;
#53461 = DIRECTION ( 'NONE',  ( -3.100000000000000258E-29, 3.100000000000000044E-14, 1.000000000000000000 ) ) ;
#53462 = CARTESIAN_POINT ( 'NONE',  ( 104.2561231690431782, -27.88649476002280636, 53.13951894101997908 ) ) ;
#53463 = VECTOR ( 'NONE', #44078, 1000.000000000000000 ) ;
#53464 = VECTOR ( 'NONE', #31938, 1000.000000000000000 ) ;
#53465 = CARTESIAN_POINT ( 'NONE',  ( 136.6789756616833813, -17.84952872354597275, 6.945088388037557792 ) ) ;
#53466 = CARTESIAN_POINT ( 'NONE',  ( 158.0667039024470171, -79.67844715994088745, 85.21780685541799016 ) ) ;
#53467 = CARTESIAN_POINT ( 'NONE',  ( 152.0371591254583450, -47.82818131005587503, 237.4678068554150059 ) ) ;
#53468 = VERTEX_POINT ( 'NONE', #35362 ) ;
#53469 = LINE ( 'NONE', #45326, #72613 ) ;
#53470 = EDGE_CURVE ( 'NONE', #37134, #30354, #48361, .T. ) ;
#53471 = VECTOR ( 'NONE', #78571, 1000.000000000000000 ) ;
#53472 = CARTESIAN_POINT ( 'NONE',  ( 123.0934642905847198, 60.63545122801047427, -43.51030618446090870 ) ) ;
#53473 = ORIENTED_EDGE ( 'NONE', *, *, #70745, .T. ) ;
#53474 = CARTESIAN_POINT ( 'NONE',  ( 96.02763272632168423, -37.29765984735794859, 121.3794347997209684 ) ) ;
#53475 = ORIENTED_EDGE ( 'NONE', *, *, #35769, .F. ) ;
#53476 = EDGE_CURVE ( 'NONE', #45997, #33402, #54191, .T. ) ;
#53477 = CARTESIAN_POINT ( 'NONE',  ( 102.6785256587874926, -29.36752282311925200, 84.92670554236298130 ) ) ;
#53478 = ADVANCED_FACE ( 'NONE', ( #8121 ), #84890, .F. ) ;
#53479 = CARTESIAN_POINT ( 'NONE',  ( 98.34084657651359862, -41.62045863392593503, 87.73252430093928922 ) ) ;
#53480 = CARTESIAN_POINT ( 'NONE',  ( 115.6990777838195186, -41.92069145011852527, 124.8272975916109573 ) ) ;
#53481 = CARTESIAN_POINT ( 'NONE',  ( 0.000000000000000000, 127.0000000000000000, -103.1875000000000000 ) ) ;
#53482 = EDGE_CURVE ( 'NONE', #73971, #3897, #34919, .T. ) ;
#53483 = AXIS2_PLACEMENT_3D ( 'NONE', #75250, #39802, #89782 ) ;
#53484 = CARTESIAN_POINT ( 'NONE',  ( 131.8479104382178946, -69.08669111203026603, 247.4970909970599848 ) ) ;
#53485 = CARTESIAN_POINT ( 'NONE',  ( 99.27755186283980038, -43.74455535675208040, 52.90991099019698396 ) ) ;
#53486 = LINE ( 'NONE', #74415, #64277 ) ;
#53487 = ORIENTED_EDGE ( 'NONE', *, *, #35928, .F. ) ;
#53488 = FACE_OUTER_BOUND ( 'NONE', #55019, .T. ) ;
#53489 = ORIENTED_EDGE ( 'NONE', *, *, #6176, .T. ) ;
#53490 = CARTESIAN_POINT ( 'NONE',  ( 78.15700282949087807, -20.71057579843893492, 2.232988688762077345 ) ) ;
#53491 = EDGE_LOOP ( 'NONE', ( #22854, #65802 ) ) ;
#53492 = EDGE_LOOP ( 'NONE', ( #49517, #22461, #6727, #67148 ) ) ;
#53493 = CIRCLE ( 'NONE', #25979, 2.517500000000005844 ) ;
#53494 = DIRECTION ( 'NONE',  ( -0.8660254037844392627, 0.4999999999999990008, -1.549999999999999706E-14 ) ) ;
#53495 = ORIENTED_EDGE ( 'NONE', *, *, #35418, .F. ) ;
#53496 = CARTESIAN_POINT ( 'NONE',  ( 105.7207279102414077, -46.41719084699269615, 257.4670538473400825 ) ) ;
#53497 = CARTESIAN_POINT ( 'NONE',  ( 97.80667890149351251, -40.50516858506785667, 126.6341183413926217 ) ) ;
#53498 = CARTESIAN_POINT ( 'NONE',  ( 117.0718954874529345, -35.46248236743199556, 189.9272919416899015 ) ) ;
#53499 = CARTESIAN_POINT ( 'NONE',  ( 116.3875994391314634, -31.98201348113981268, 40.20133956162496958 ) ) ;
#53500 = FACE_OUTER_BOUND ( 'NONE', #83474, .T. ) ;
#53501 = ORIENTED_EDGE ( 'NONE', *, *, #4941, .T. ) ;
#53502 = CARTESIAN_POINT ( 'NONE',  ( 168.3595971213390499, -48.62134037882588444, 300.4678068554149490 ) ) ;
#53503 = DIRECTION ( 'NONE',  ( 0.000000000000000000, 0.000000000000000000, -1.000000000000000000 ) ) ;
#53505 = ORIENTED_EDGE ( 'NONE', *, *, #76526, .T. ) ;
#53504 = AXIS2_PLACEMENT_3D ( 'NONE', #46549, #87910, #25672 ) ;
#53506 = CARTESIAN_POINT ( 'NONE',  ( 45.76696975232824371, -48.62818131006036992, 300.4678068554150059 ) ) ;
#53507 = DIRECTION ( 'NONE',  ( 1.000000000000000078E-15, -1.000000000000000000, 0.000000000000000000 ) ) ;
#53508 = CARTESIAN_POINT ( 'NONE',  ( 118.3173389373707920, -33.08695204176926552, 284.0756252759109657 ) ) ;
#53509 = CARTESIAN_POINT ( 'NONE',  ( 3.968750000000000000, 120.6499999999999915, -105.4788588808464027 ) ) ;
#53510 = CARTESIAN_POINT ( 'NONE',  ( 72.96458098368650269, 117.4749999999999943, 67.92268098368730023 ) ) ;
#53511 = CARTESIAN_POINT ( 'NONE',  ( 78.64593636900363549, -39.09121833381438904, 1.942446336666123985 ) ) ;
#53512 = CARTESIAN_POINT ( 'NONE',  ( 113.8315610999352714, -43.69395359880221719, 267.6124198280766677 ) ) ;
#53514 = CARTESIAN_POINT ( 'NONE',  ( 113.3292761056178648, -27.64973082387879444, 85.60800622829195561 ) ) ;
#53513 = CARTESIAN_POINT ( 'NONE',  ( 152.4409905591762993, -0.9151414768251351362, 394.9756252759102040 ) ) ;
#53515 = DIRECTION ( 'NONE',  ( 0.8660254037844392627, -0.4999999999999990008, 1.549999999999999706E-14 ) ) ;
#53516 = CARTESIAN_POINT ( 'NONE',  ( 108.3716159000525039, -47.75258262280652843, 162.6822919425769669 ) ) ;
#53517 = ORIENTED_EDGE ( 'NONE', *, *, #76452, .F. ) ;
#53518 = CARTESIAN_POINT ( 'NONE',  ( 173.9900000000000091, 37.33800000000000097, 50.79999999999999716 ) ) ;
#53519 = VERTEX_POINT ( 'NONE', #63074 ) ;
#53520 = CARTESIAN_POINT ( 'NONE',  ( 29.56670390244789459, -48.82844715994099971, 129.9678068554150627 ) ) ;
#53521 = DIRECTION ( 'NONE',  ( -4.237773401492740281E-14, 1.000000000000000000, 0.000000000000000000 ) ) ;
#53522 = DIRECTION ( 'NONE',  ( 0.000000000000000000, 0.000000000000000000, -1.000000000000000000 ) ) ;
#53523 = EDGE_LOOP ( 'NONE', ( #35746, #30342, #57375, #79355 ) ) ;
#53524 = VECTOR ( 'NONE', #16170, 1000.000000000000000 ) ;
#53525 = DIRECTION ( 'NONE',  ( -4.237773401492740281E-14, 1.000000000000000000, 0.000000000000000000 ) ) ;
#53527 = ORIENTED_EDGE ( 'NONE', *, *, #71441, .T. ) ;
#53526 = CARTESIAN_POINT ( 'NONE',  ( 114.4941961175866254, -28.48069933791915531, 159.5051490854349652 ) ) ;
#53529 = DIRECTION ( 'NONE',  ( 1.000000000000000000, -7.570719237730591757E-15, 0.000000000000000000 ) ) ;
#53528 = UNCERTAINTY_MEASURE_WITH_UNIT (LENGTH_MEASURE( 1.000000000000000082E-05 ), #22403, 'distance_accuracy_value', 'NONE');
#53530 = CARTESIAN_POINT ( 'NONE',  ( -130.1658227983198515, 90.29814575435200652, -10.09656535537057209 ) ) ;
#53531 = CARTESIAN_POINT ( 'NONE',  ( 32.56670390244700997, -22.48495420874110806, -5.074374724088000832 ) ) ;
#53533 = CYLINDRICAL_SURFACE ( 'NONE', #87321, 0.2500000000000002220 ) ;
#53532 = VECTOR ( 'NONE', #53556, 1000.000000000000000 ) ;
#53534 = ORIENTED_EDGE ( 'NONE', *, *, #42294, .F. ) ;
#53535 = VECTOR ( 'NONE', #62672, 1000.000000000000000 ) ;
#53536 = EDGE_CURVE ( 'NONE', #40328, #43983, #405, .T. ) ;
#53537 = CARTESIAN_POINT ( 'NONE',  ( 295.6978641014171671, 7.710689432856530360E-60, 1.032368090408195659E-12 ) ) ;
#53538 = CARTESIAN_POINT ( 'NONE',  ( 172.5667039024480118, -36.32844715993499563, 180.4678068554150059 ) ) ;
#53539 = EDGE_CURVE ( 'NONE', #78479, #59669, #87564, .T. ) ;
#53540 = CARTESIAN_POINT ( 'NONE',  ( 37.03715912545342093, -48.62818131006128652, 193.9678068554150911 ) ) ;
#53541 = ORIENTED_EDGE ( 'NONE', *, *, #58975, .T. ) ;
#53543 = EDGE_CURVE ( 'NONE', #86794, #83222, #75955, .T. ) ;
#53542 = VECTOR ( 'NONE', #70974, 1000.000000000000000 ) ;
#53544 = ORIENTED_EDGE ( 'NONE', *, *, #87438, .F. ) ;
#53545 = DIRECTION ( 'NONE',  ( 0.000000000000000000, 0.000000000000000000, 1.000000000000000000 ) ) ;
#53546 = CARTESIAN_POINT ( 'NONE',  ( 91.13883569058506851, 95.16896684734909684, -93.48397507443779375 ) ) ;
#53547 = CARTESIAN_POINT ( 'NONE',  ( 158.0667039024470171, -79.67844715994088745, 120.2178068554179902 ) ) ;
#53548 = DIRECTION ( 'NONE',  ( 0.000000000000000000, 1.000000000000000000, 0.000000000000000000 ) ) ;
#53549 = EDGE_CURVE ( 'NONE', #72641, #13444, #14532, .T. ) ;
#53550 = EDGE_CURVE ( 'NONE', #79692, #14032, #46938, .T. ) ;
#53552 = CARTESIAN_POINT ( 'NONE',  ( -10.33363185139394957, 75.15554654547490543, -118.1050150300115007 ) ) ;
#53551 = CARTESIAN_POINT ( 'NONE',  ( 99.09563243660048215, -30.55053396421687850, 105.8023020003378178 ) ) ;
#53553 = CARTESIAN_POINT ( 'NONE',  ( 97.06384305289986969, -37.34228284162757205, 181.3752372158707828 ) ) ;
#53554 = EDGE_CURVE ( 'NONE', #62031, #41740, #21301, .T. ) ;
#53555 = ORIENTED_EDGE ( 'NONE', *, *, #39326, .T. ) ;
#53557 = EDGE_CURVE ( 'NONE', #89203, #16001, #10354, .T. ) ;
#53556 = DIRECTION ( 'NONE',  ( -1.000000000000000000, 0.000000000000000000, 2.544367396927093851E-16 ) ) ;
#53558 = CARTESIAN_POINT ( 'NONE',  ( 116.2522929705882859, -40.08866370952546987, 214.5470538473389581 ) ) ;
#53559 = AXIS2_PLACEMENT_3D ( 'NONE', #70770, #23960, #16253 ) ;
#53561 = VERTEX_POINT ( 'NONE', #9030 ) ;
#53560 = DIRECTION ( 'NONE',  ( -1.000000000000000078E-15, 1.000000000000000000, 0.000000000000000000 ) ) ;
#53562 = CARTESIAN_POINT ( 'NONE',  ( 107.5734549334945314, -47.83597508069280480, 38.61276813305297395 ) ) ;
#53563 = CARTESIAN_POINT ( 'NONE',  ( 113.6628025804010775, -44.27377612063442314, 53.14812363029078313 ) ) ;
#53564 = CARTESIAN_POINT ( 'NONE',  ( 147.0667039024469886, -67.87844716047348470, 245.4920193514540188 ) ) ;
#53565 = EDGE_CURVE ( 'NONE', #72320, #34580, #31008, .T. ) ;
#53566 = DIRECTION ( 'NONE',  ( 0.000000000000000000, 0.000000000000000000, 1.000000000000000000 ) ) ;
#53567 = ORIENTED_EDGE ( 'NONE', *, *, #55400, .F. ) ;
#53568 = CARTESIAN_POINT ( 'NONE',  ( 173.9900000000000091, 101.5999999999999943, -71.37400000000000944 ) ) ;
#53569 = ORIENTED_EDGE ( 'NONE', *, *, #14720, .F. ) ;
#53570 = ORIENTED_EDGE ( 'NONE', *, *, #22428, .T. ) ;
#53571 = AXIS2_PLACEMENT_3D ( 'NONE', #86033, #37417, #78775 ) ;
#53572 = CARTESIAN_POINT ( 'NONE',  ( 104.8088860400571463, -27.60915219823615985, 236.6892023535159808 ) ) ;
#53573 = LINE ( 'NONE', #39073, #50190 ) ;
#53574 = CARTESIAN_POINT ( 'NONE',  ( 72.96458098368650269, 127.0000000000000000, 80.90208098368729850 ) ) ;
#53575 = CARTESIAN_POINT ( 'NONE',  ( 98.34985891762011079, -31.65658480093746974, 80.90645860845471304 ) ) ;
#53576 = FACE_OUTER_BOUND ( 'NONE', #34843, .T. ) ;
#53577 = EDGE_LOOP ( 'NONE', ( #74045, #76352, #47749, #67775 ) ) ;
#53578 = VECTOR ( 'NONE', #86471, 1000.000000000000114 ) ;
#53579 = DIRECTION ( 'NONE',  ( -4.237773401492740281E-14, 1.000000000000000000, 0.000000000000000000 ) ) ;
#53580 = CARTESIAN_POINT ( 'NONE',  ( 69.63919639214307722, 92.07499999999998863, -53.63573739454432854 ) ) ;
#53581 = VERTEX_POINT ( 'NONE', #10788 ) ;
#53582 = CARTESIAN_POINT ( 'NONE',  ( 117.3847603239957635, -38.21947720531817083, 28.71276813305395592 ) ) ;
#53583 = ORIENTED_EDGE ( 'NONE', *, *, #2014, .T. ) ;
#53584 = VERTEX_POINT ( 'NONE', #36729 ) ;
#53585 = CARTESIAN_POINT ( 'NONE',  ( 99.35983957736841887, -39.50259174935074213, 264.4195189410201579 ) ) ;
#53586 = EDGE_CURVE ( 'NONE', #72918, #52237, #59974, .T. ) ;
#53587 = VECTOR ( 'NONE', #83873, 1000.000000000000000 ) ;
#53588 = DIRECTION ( 'NONE',  ( -0.000000000000000000, 1.000000000000000000, 0.000000000000000000 ) ) ;
#53589 = CARTESIAN_POINT ( 'NONE',  ( 102.0969121991172557, -45.15362633196983211, 162.1527681330539679 ) ) ;
#53590 = DIRECTION ( 'NONE',  ( 1.000000000000000000, 8.953411488912556626E-16, 0.000000000000000000 ) ) ;
#53591 = CARTESIAN_POINT ( 'NONE',  ( 63.56670390244796920, -40.82844715994016127, 300.4678068554150627 ) ) ;
#53593 = EDGE_CURVE ( 'NONE', #62569, #24379, #37169, .T. ) ;
#53592 = DIRECTION ( 'NONE',  ( 0.000000000000000000, 0.000000000000000000, 1.000000000000000000 ) ) ;
#53594 = CARTESIAN_POINT ( 'NONE',  ( 117.9780035659441495, -34.69567636304840619, 199.9851490854349549 ) ) ;
#53596 = FACE_OUTER_BOUND ( 'NONE', #77336, .T. ) ;
#53595 = VECTOR ( 'NONE', #22183, 1000.000000000000000 ) ;
#53597 = CIRCLE ( 'NONE', #2873, 6.571100913904396990 ) ;
#53598 = EDGE_LOOP ( 'NONE', ( #78652, #83921, #72163, #40005, #53128, #13688, #74431, #13041, #81386, #84717, #16413, #82532 ) ) ;
#53599 = CARTESIAN_POINT ( 'NONE',  ( 95.30017103329034001, -34.95040006919153086, 67.20705384733894050 ) ) ;
#53600 = CYLINDRICAL_SURFACE ( 'NONE', #7632, 50.79999999999999716 ) ;
#53601 = ORIENTED_EDGE ( 'NONE', *, *, #37722, .F. ) ;
#53602 = EDGE_LOOP ( 'NONE', ( #64871, #23123, #55967, #73137 ) ) ;
#53603 = ORIENTED_EDGE ( 'NONE', *, *, #56785, .T. ) ;
#53604 = CIRCLE ( 'NONE', #37707, 1.000000000000000888 ) ;
#53605 = CARTESIAN_POINT ( 'NONE',  ( -487.2989999999999782, 21.43125000000035030, 6.988054014476359654 ) ) ;
#53606 = DIRECTION ( 'NONE',  ( 7.076552332833900719E-16, -1.000000000000000000, 3.100000000000000044E-14 ) ) ;
#53607 = DIRECTION ( 'NONE',  ( 0.000000000000000000, 0.000000000000000000, 1.000000000000000000 ) ) ;
#53608 = CARTESIAN_POINT ( 'NONE',  ( 112.9083776113003665, -30.34675141079074834, 152.2928522743529527 ) ) ;
#53609 = CARTESIAN_POINT ( 'NONE',  ( 96.10234264863321130, -35.15692507338371087, 222.2251490854349640 ) ) ;
#53610 = LINE ( 'NONE', #19123, #21820 ) ;
#53611 = ORIENTED_EDGE ( 'NONE', *, *, #30720, .F. ) ;
#53612 = CARTESIAN_POINT ( 'NONE',  ( 130.4354318373310946, 93.94566094357732311, 5.621620364687625937 ) ) ;
#53613 = VECTOR ( 'NONE', #48815, 1000.000000000000000 ) ;
#53614 = CARTESIAN_POINT ( 'NONE',  ( 136.8164832912740110, -36.72944715994100306, 3.101481641215515950 ) ) ;
#53615 = ORIENTED_EDGE ( 'NONE', *, *, #74212, .T. ) ;
#53616 = ORIENTED_EDGE ( 'NONE', *, *, #83235, .F. ) ;
#53617 = DIRECTION ( 'NONE',  ( 0.000000000000000000, -1.000000000000000000, 0.000000000000000000 ) ) ;
#53618 = VERTEX_POINT ( 'NONE', #15835 ) ;
#53619 = ORIENTED_EDGE ( 'NONE', *, *, #67211, .T. ) ;
#53620 = CARTESIAN_POINT ( 'NONE',  ( 127.0664832912740394, -54.72944906728950798, -4.824374724089008915 ) ) ;
#53621 = DIRECTION ( 'NONE',  ( 0.000000000000000000, 1.000000000000000000, 0.000000000000000000 ) ) ;
#53622 = FACE_OUTER_BOUND ( 'NONE', #60101, .T. ) ;
#53623 = VECTOR ( 'NONE', #8437, 1000.000000000000000 ) ;
#53624 = CARTESIAN_POINT ( 'NONE',  ( 108.6057327191364976, -28.29838476132584191, 164.3552769709339714 ) ) ;
#53625 = CARTESIAN_POINT ( 'NONE',  ( 103.4619715496438630, -25.38765309446003116, 55.32133956162594046 ) ) ;
#53626 = CARTESIAN_POINT ( 'NONE',  ( 107.0667039024470029, -74.77844715994095282, 25.71780685541800437 ) ) ;
#53627 = ORIENTED_EDGE ( 'NONE', *, *, #642, .F. ) ;
#53628 = LINE ( 'NONE', #81835, #81849 ) ;
#53629 = VERTEX_POINT ( 'NONE', #66190 ) ;
#53630 = DIRECTION ( 'NONE',  ( 1.000000000000000000, -9.104347601086962483E-12, 0.000000000000000000 ) ) ;
#53631 = ORIENTED_EDGE ( 'NONE', *, *, #36586, .T. ) ;
#53632 = CARTESIAN_POINT ( 'NONE',  ( 104.4230182660072472, -27.06115666640247852, 166.2882327781027527 ) ) ;
#53633 = CARTESIAN_POINT ( 'NONE',  ( -11.48301544705986998, 77.34703915398208096, 117.9986893718514409 ) ) ;
#53634 = CARTESIAN_POINT ( 'NONE',  ( 111.5308273356922797, -45.68399439548272056, 132.9444956965449194 ) ) ;
#53635 = VECTOR ( 'NONE', #41306, 1000.000000000000000 ) ;
#53636 = DIRECTION ( 'NONE',  ( -1.000000000000000000, -2.756263715554006823E-15, 0.000000000000000000 ) ) ;
#53637 = ORIENTED_EDGE ( 'NONE', *, *, #20357, .F. ) ;
#53638 = CARTESIAN_POINT ( 'NONE',  ( 97.05407301568530443, -33.74649485729950271, 31.09562527591097592 ) ) ;
#53639 = CARTESIAN_POINT ( 'NONE',  ( 118.7813114821712901, -34.63805691389952557, 44.96705384733895272 ) ) ;
#53640 =( BOUNDED_CURVE ( )  B_SPLINE_CURVE ( 3, ( #73273, #72840, #23381, #24248 ),
 .UNSPECIFIED., .F., .F. ) 
 B_SPLINE_CURVE_WITH_KNOTS ( ( 4, 4 ),
 ( 1.570796326806955134, 3.141592653599507123 ),
 .UNSPECIFIED. ) 
 CURVE ( )  GEOMETRIC_REPRESENTATION_ITEM ( )  RATIONAL_B_SPLINE_CURVE ( ( 1.000000000000000000, 0.8047378541249177175, 0.8047378541249177175, 1.000000000000000000 ) ) 
 REPRESENTATION_ITEM ( '' )  );
#53641 = EDGE_CURVE ( 'NONE', #33706, #48061, #57602, .T. ) ;
#53643 = CARTESIAN_POINT ( 'NONE',  ( 183.5150000000000148, 21.46300000000000097, 41.63456447661474868 ) ) ;
#53642 = DIRECTION ( 'NONE',  ( -1.000000000000000000, -4.299999999999999979E-14, -1.000000000000000078E-15 ) ) ;
#53644 = DIRECTION ( 'NONE',  ( -1.000000000000000000, -8.163404592832032979E-16, 0.000000000000000000 ) ) ;
#53645 = ADVANCED_FACE ( 'NONE', ( #86218 ), #9461, .T. ) ;
#53646 = FACE_OUTER_BOUND ( 'NONE', #15390, .T. ) ;
#53647 = VECTOR ( 'NONE', #64013, 1000.000000000000000 ) ;
#53648 = EDGE_CURVE ( 'NONE', #65744, #53086, #44405, .T. ) ;
#53649 = CARTESIAN_POINT ( 'NONE',  ( 103.5958499319329036, -27.24642460418891687, 121.3544414785948788 ) ) ;
#53650 = CARTESIAN_POINT ( 'NONE',  ( 145.7688716652828873, -137.6858083443213161, 247.4233469738189797 ) ) ;
#53651 = EDGE_CURVE ( 'NONE', #5415, #8910, #3985, .T. ) ;
#53652 = ORIENTED_EDGE ( 'NONE', *, *, #54670, .T. ) ;
#53653 = CARTESIAN_POINT ( 'NONE',  ( 115.9290394997688480, -31.15613903141374763, 34.27276813305396530 ) ) ;
#53654 = CARTESIAN_POINT ( 'NONE',  ( 96.19138854833354912, -32.02127024200479610, 207.0013395616249738 ) ) ;
#53655 = CARTESIAN_POINT ( 'NONE',  ( 99.48587976144928291, -43.91775078298940116, 77.92991099019597812 ) ) ;
#53657 = CARTESIAN_POINT ( 'NONE',  ( -215.9000000000000057, 53.97500000000000142, 30.79999999999999361 ) ) ;
#53656 = DIRECTION ( 'NONE',  ( 0.000000000000000000, 1.000000000000000000, 0.000000000000000000 ) ) ;
#53658 = DIRECTION ( 'NONE',  ( 0.000000000000000000, 1.000000000000000000, 0.000000000000000000 ) ) ;
#53659 = AXIS2_PLACEMENT_3D ( 'NONE', #19021, #12213, #39902 ) ;
#53660 = EDGE_CURVE ( 'NONE', #21597, #16304, #30796, .T. ) ;
#53661 = DIRECTION ( 'NONE',  ( 1.000000000000000000, 0.000000000000000000, 0.000000000000000000 ) ) ;
#53662 = ORIENTED_EDGE ( 'NONE', *, *, #18937, .F. ) ;
#53663 = EDGE_CURVE ( 'NONE', #30378, #67268, #77437, .T. ) ;
#53664 = CARTESIAN_POINT ( 'NONE',  ( 114.1038288540492687, -43.56973530630599356, 94.21276813305296116 ) ) ;
#53665 = AXIS2_PLACEMENT_3D ( 'NONE', #77329, #70065, #71426 ) ;
#53667 = ORIENTED_EDGE ( 'NONE', *, *, #50388, .F. ) ;
#53666 = DIRECTION ( 'NONE',  ( 0.000000000000000000, -1.000000000000000000, -6.982966722218760189E-15 ) ) ;
#53668 = CARTESIAN_POINT ( 'NONE',  ( 99.55514648348079731, -29.48070623161996551, 246.7156252759109520 ) ) ;
#53669 = CARTESIAN_POINT ( 'NONE',  ( 115.0368136288728067, -42.90904383531166388, 254.3042057836352114 ) ) ;
#53670 = CARTESIAN_POINT ( 'NONE',  ( 116.3173461584868278, -32.93718857426866720, 59.13562527591098217 ) ) ;
#53671 = AXIS2_PLACEMENT_3D ( 'NONE', #53537, #39929, #66294 ) ;
#53672 = PLANE ( 'NONE',  #2235 ) ;
#53673 = CYLINDRICAL_SURFACE ( 'NONE', #16642, 11.45913725231036118 ) ;
#53674 = EDGE_CURVE ( 'NONE', #19968, #36283, #4890, .T. ) ;
#53675 = CARTESIAN_POINT ( 'NONE',  ( 0.000000000000000000, 117.4749999999999943, -103.1875000000000000 ) ) ;
#53676 = CYLINDRICAL_SURFACE ( 'NONE', #21098, 3.999999999999992895 ) ;
#53677 = VECTOR ( 'NONE', #85871, 1000.000000000000000 ) ;
#53678 = CARTESIAN_POINT ( 'NONE',  ( 108.2857792741417882, -47.02760743735412063, 162.6822919425779617 ) ) ;
#53679 = ORIENTED_EDGE ( 'NONE', *, *, #87208, .T. ) ;
#53680 = EDGE_LOOP ( 'NONE', ( #18241, #14584, #4026, #45723 ) ) ;
#53681 = CARTESIAN_POINT ( 'NONE',  ( 105.2783438540041061, -26.81616000048136428, 121.6501547344689698 ) ) ;
#53682 = CARTESIAN_POINT ( 'NONE',  ( 8.398627748552550652E-16, 50.79999999999999716, 272.4150000000000205 ) ) ;
#53684 = CARTESIAN_POINT ( 'NONE',  ( 172.5664832912740110, -9.303447159940999356, 258.9256252759120116 ) ) ;
#53683 = CARTESIAN_POINT ( 'NONE',  ( 103.3362402991319584, -47.20309360805207177, 248.3041967044819387 ) ) ;
#53685 = LINE ( 'NONE', #33725, #1435 ) ;
#53686 = CONICAL_SURFACE ( 'NONE', #72605, 1.258749999999999369, 1.029744258676650093 ) ;
#53687 = CARTESIAN_POINT ( 'NONE',  ( 37.03715912545347777, -48.62818131006128652, 129.9678068554150911 ) ) ;
#53688 = CARTESIAN_POINT ( 'NONE',  ( 55.48342271751659638, 20.32000000000000028, 171.1197181046785261 ) ) ;
#53689 = LINE ( 'NONE', #19207, #5770 ) ;
#53690 = DIRECTION ( 'NONE',  ( -3.100000000000000258E-29, 3.100000000000000044E-14, 1.000000000000000000 ) ) ;
#53691 = CARTESIAN_POINT ( 'NONE',  ( 100.0229104548316172, -27.23016881827663127, 185.5841967044829630 ) ) ;
#53692 = CARTESIAN_POINT ( 'NONE',  ( 3.968749999999215294, 120.6499999999999915, 105.4788588808464027 ) ) ;
#53693 = ORIENTED_EDGE ( 'NONE', *, *, #73320, .T. ) ;
#53694 = VERTEX_POINT ( 'NONE', #68000 ) ;
#53695 = B_SPLINE_CURVE_WITH_KNOTS ( 'NONE', 3,
 ( #83590, #7283, #56295, #54940, #56756, #8176, #456, #14549, #75427, #62683, #35869, #63586, #48136, #69507, #68613, #13201, #20907, #910, #13641, #1365, #6374, #27717, #47692, #34969, #42226, #75870, #62231, #48580, #76314, #28150, #76764, #69956, #28609, #34065, #29069, #84040, #21816, #30850, #15448, #85838, #50843, #43119, #57653, #58105, #36777, #44011 ),
 .UNSPECIFIED., .F., .F.,
 ( 4, 2, 2, 2, 2, 2, 2, 2, 2, 2, 2, 2, 2, 2, 2, 2, 2, 2, 2, 2, 2, 2, 4 ),
 ( 1.387778780781445676E-17, 0.001601640810786372163, 0.003203281621572730449, 0.004804922432359089168, 0.005605742837752265492, 0.006406563243145441816, 0.007207383648538618140, 0.008008204053931794464, 0.009609844864718143642, 0.01121148567550449282, 0.01281312648629084373, 0.01361394689168402700, 0.01441476729707721373, 0.01601640810786359934, 0.01681722851325679127, 0.01761804891864998668, 0.01921968972943637402, 0.02002051013482955902, 0.02082133054022275095, 0.02162215094561594289, 0.02242297135100913136, 0.02402461216179551870, 0.02562625297258190604 ),
 .UNSPECIFIED. ) ;
#53696 = CARTESIAN_POINT ( 'NONE',  ( -87.70409100286360626, 71.53177522571070313, -96.71266027437734181 ) ) ;
#53697 = CARTESIAN_POINT ( 'NONE',  ( 41.56648329127399677, 0.2215528400590013880, 81.04262527591200183 ) ) ;
#53698 = CARTESIAN_POINT ( 'NONE',  ( 194.0371591254582313, -46.82818131005407736, 313.9678068554149490 ) ) ;
#53700 = EDGE_CURVE ( 'NONE', #86147, #74870, #16501, .T. ) ;
#53699 = DIRECTION ( 'NONE',  ( 4.194175870806139918E-14, -1.000000000000000000, 0.000000000000000000 ) ) ;
#53701 = AXIS2_PLACEMENT_3D ( 'NONE', #56057, #7932, #62446 ) ;
#53702 = FACE_OUTER_BOUND ( 'NONE', #11057, .T. ) ;
#53703 = ORIENTED_EDGE ( 'NONE', *, *, #30229, .F. ) ;
#53704 = CARTESIAN_POINT ( 'NONE',  ( -10.93444747363166769, 88.86474737026325954, 117.8507171435055483 ) ) ;
#53705 = CARTESIAN_POINT ( 'NONE',  ( 97.09604340039788895, -41.50117806558871791, 216.6937205140059461 ) ) ;
#53706 = DIRECTION ( 'NONE',  ( -0.9254794337955620787, -0.3787978585227822492, 0.000000000000000000 ) ) ;
#53707 = EDGE_LOOP ( 'NONE', ( #21859, #20244, #36270, #67705 ) ) ;
#53708 = VECTOR ( 'NONE', #86923, 1000.000000000000000 ) ;
#53709 = CARTESIAN_POINT ( 'NONE',  ( 121.3140869715381456, -113.5527167097541508, -11.78219314458173272 ) ) ;
#53710 = FACE_OUTER_BOUND ( 'NONE', #51154, .T. ) ;
#53711 = LINE ( 'NONE', #59204, #16522 ) ;
#53712 = CARTESIAN_POINT ( 'NONE',  ( 114.4327864602578870, -33.21273682179715792, 16.99951894101997496 ) ) ;
#53713 = CARTESIAN_POINT ( 'NONE',  ( 98.44073678691454177, -30.83591204966533894, 116.8499109901969604 ) ) ;
#53714 = VECTOR ( 'NONE', #46746, 1000.000000000000000 ) ;
#53715 = DIRECTION ( 'NONE',  ( -0.8660254037844389297, 0.4999999999999993894, -1.550000000000000968E-14 ) ) ;
#53716 = VERTEX_POINT ( 'NONE', #39830 ) ;
#53717 = EDGE_CURVE ( 'NONE', #45547, #63478, #33920, .T. ) ;
#53718 = DIRECTION ( 'NONE',  ( 0.000000000000000000, 0.000000000000000000, -1.000000000000000000 ) ) ;
#53719 = CARTESIAN_POINT ( 'NONE',  ( 82.81181082189912956, -18.54506369575707225, 6.756870620000345440 ) ) ;
#53720 = ORIENTED_EDGE ( 'NONE', *, *, #11642, .F. ) ;
#53722 = ORIENTED_EDGE ( 'NONE', *, *, #24527, .T. ) ;
#53721 = CIRCLE ( 'NONE', #14609, 15.50000000000000000 ) ;
#53723 = EDGE_CURVE ( 'NONE', #15453, #65492, #33024, .T. ) ;
#53724 = CARTESIAN_POINT ( 'NONE',  ( 167.6524903400755875, -48.32844715993520879, 129.9678068554150059 ) ) ;
#53725 = ORIENTED_EDGE ( 'NONE', *, *, #78526, .F. ) ;
#53726 = ORIENTED_EDGE ( 'NONE', *, *, #55739, .F. ) ;
#53727 = CARTESIAN_POINT ( 'NONE',  ( 97.81136857581559241, -40.51756142658395987, 157.6353372204761456 ) ) ;
#53728 = CARTESIAN_POINT ( 'NONE',  ( 116.6246688045503248, -35.02307164793359107, 48.38956268521998538 ) ) ;
#53729 = AXIS2_PLACEMENT_3D ( 'NONE', #30862, #87611, #2722 ) ;
#53730 = CARTESIAN_POINT ( 'NONE',  ( 117.2491520020922451, -41.08934384016853869, 213.5165776568629781 ) ) ;
#53731 = CARTESIAN_POINT ( 'NONE',  ( 107.9164806882189396, -47.13338536194959971, 177.6413395616249886 ) ) ;
#53733 = CARTESIAN_POINT ( 'NONE',  ( 102.7643194828038702, -25.71402177940534983, 16.37276813305293999 ) ) ;
#53732 = CARTESIAN_POINT ( 'NONE',  ( 112.5159765079568928, -45.21572303546594895, 23.03180688963041689 ) ) ;
#53734 = DIRECTION ( 'NONE',  ( 4.299999999999999979E-14, -1.000000000000000000, 4.400000000000000367E-29 ) ) ;
#53735 = CARTESIAN_POINT ( 'NONE',  ( 181.9694315774339941, -34.03355364505720360, -5.074374724088000832 ) ) ;
#53736 = ORIENTED_EDGE ( 'NONE', *, *, #56985, .T. ) ;
#53737 = ORIENTED_EDGE ( 'NONE', *, *, #52638, .T. ) ;
#53738 = CARTESIAN_POINT ( 'NONE',  ( 0.000000000000000000, 124.9679999999999893, 0.000000000000000000 ) ) ;
#53739 = CARTESIAN_POINT ( 'NONE',  ( 116.0932472193867966, -42.03267250216092776, 238.4041967044829562 ) ) ;
#53740 = ORIENTED_EDGE ( 'NONE', *, *, #73261, .F. ) ;
#53741 = CARTESIAN_POINT ( 'NONE',  ( 98.55109871784688380, -44.97133477160940629, 191.9384824187679612 ) ) ;
#53742 = DIRECTION ( 'NONE',  ( -4.237773401492740281E-14, 1.000000000000000000, 0.000000000000000000 ) ) ;
#53743 = CARTESIAN_POINT ( 'NONE',  ( 0.000000000000000000, 61.59999999999999432, 118.5560000000000116 ) ) ;
#53744 = CARTESIAN_POINT ( 'NONE',  ( 112.0650724570131018, -45.48886861298491624, 23.98971456471283048 ) ) ;
#53745 = CARTESIAN_POINT ( 'NONE',  ( 115.3228590304952519, -42.51629437446412396, 29.34178388814013516 ) ) ;
#53746 = EDGE_CURVE ( 'NONE', #38959, #71019, #62961, .T. ) ;
#53748 = FACE_OUTER_BOUND ( 'NONE', #23747, .T. ) ;
#53747 = CARTESIAN_POINT ( 'NONE',  ( 98.00444231558566344, -38.77556477352123920, 277.6356252759110248 ) ) ;
#53749 = CARTESIAN_POINT ( 'NONE',  ( 104.4078422938526387, -46.45802063222308931, 173.3647710761513281 ) ) ;
#53750 = EDGE_CURVE ( 'NONE', #52976, #52525, #18496, .T. ) ;
#53751 = CARTESIAN_POINT ( 'NONE',  ( -34.53140813619931748, 64.60000000000000853, 35.02576496182815191 ) ) ;
#53752 = AXIS2_PLACEMENT_3D ( 'NONE', #81038, #59212, #11066 ) ;
#53753 = LINE ( 'NONE', #39259, #83263 ) ;
#53754 = CIRCLE ( 'NONE', #62469, 2.517500000000005844 ) ;
#53755 = EDGE_CURVE ( 'NONE', #27930, #12659, #26213, .T. ) ;
#53756 = LINE ( 'NONE', #54647, #70428 ) ;
#53757 = LINE ( 'NONE', #89217, #80819 ) ;
#53758 = DIRECTION ( 'NONE',  ( -0.8660254037844381525, -0.5000000000000007772, 1.549999999999999706E-14 ) ) ;
#53760 = ORIENTED_EDGE ( 'NONE', *, *, #55194, .F. ) ;
#53759 = CARTESIAN_POINT ( 'NONE',  ( 101.1484327817356927, -28.92773574981692164, 195.5838068554168672 ) ) ;
#53761 = EDGE_CURVE ( 'NONE', #47300, #87803, #53891, .T. ) ;
#53762 = CARTESIAN_POINT ( 'NONE',  ( 83.06670390244796920, -67.87844715994100397, 207.5838068554149913 ) ) ;
#53763 = CARTESIAN_POINT ( 'NONE',  ( 115.8739437555936718, -44.69579237430344421, 233.2413395616259493 ) ) ;
#53764 = CARTESIAN_POINT ( 'NONE',  ( 117.1635299909640082, -34.13481127188234865, 120.0270538473389479 ) ) ;
#53765 = CARTESIAN_POINT ( 'NONE',  ( 109.2209341577003698, -48.43284210327079364, 273.7213395616253706 ) ) ;
#53766 = CARTESIAN_POINT ( 'NONE',  ( 21.03715912545744615, -47.82818131006197149, 129.9678068554150627 ) ) ;
#53767 = DIRECTION ( 'NONE',  ( 0.000000000000000000, -1.000000000000000000, 0.000000000000000000 ) ) ;
#53768 = AXIS2_PLACEMENT_3D ( 'NONE', #11052, #17433, #23813 ) ;
#53770 = PLANE ( 'NONE',  #89119 ) ;
#53769 = FACE_OUTER_BOUND ( 'NONE', #83910, .T. ) ;
#53771 = DIRECTION ( 'NONE',  ( 1.000000000000000000, -4.238735976179846264E-15, 0.000000000000000000 ) ) ;
#53772 = CARTESIAN_POINT ( 'NONE',  ( 133.1862368104746110, -21.33528726900525641, 1.744847506585589292 ) ) ;
#53773 = EDGE_CURVE ( 'NONE', #14469, #33687, #25168, .T. ) ;
#53774 = VECTOR ( 'NONE', #26379, 1000.000000000000000 ) ;
#53775 = ORIENTED_EDGE ( 'NONE', *, *, #17599, .T. ) ;
#53776 = VERTEX_POINT ( 'NONE', #39393 ) ;
#53777 = ADVANCED_FACE ( 'NONE', ( #73919 ), #12541, .F. ) ;
#53778 = CARTESIAN_POINT ( 'NONE',  ( 98.54925023078828872, -36.08769725913535353, 145.6895626852199541 ) ) ;
#53780 = ORIENTED_EDGE ( 'NONE', *, *, #30139, .T. ) ;
#53779 = CARTESIAN_POINT ( 'NONE',  ( 22.90438369314431100, 50.44815651554718983, 30.44723272559076221 ) ) ;
#53781 = CARTESIAN_POINT ( 'NONE',  ( 97.07206807804939785, -35.37847778407284949, 91.21778693248904801 ) ) ;
#53782 = CARTESIAN_POINT ( 'NONE',  ( 117.1424269838422987, -34.14023410701943817, 120.0270538473389479 ) ) ;
#53783 = CARTESIAN_POINT ( 'NONE',  ( 64.68306507141296890, -72.55818180160879649, 361.9756252759101471 ) ) ;
#53784 = CARTESIAN_POINT ( 'NONE',  ( 90.44969454456405344, -17.59493780205721691, 219.5838068554169809 ) ) ;
#53785 = AXIS2_PLACEMENT_3D ( 'NONE', #27557, #39827, #67544 ) ;
#53786 = DIRECTION ( 'NONE',  ( 0.000000000000000000, 0.000000000000000000, 1.000000000000000000 ) ) ;
#53787 = CARTESIAN_POINT ( 'NONE',  ( 107.0667039024470313, -104.2784471599413934, 2.217806855418003043 ) ) ;
#53788 = CARTESIAN_POINT ( 'NONE',  ( 111.6283393632454448, -28.07768985461828848, 59.68991099019693536 ) ) ;
#53789 = ORIENTED_EDGE ( 'NONE', *, *, #67919, .F. ) ;
#53790 = ORIENTED_EDGE ( 'NONE', *, *, #6225, .T. ) ;
#53792 = ORIENTED_EDGE ( 'NONE', *, *, #54280, .T. ) ;
#53791 = VECTOR ( 'NONE', #24966, 1000.000000000000000 ) ;
#53793 = CARTESIAN_POINT ( 'NONE',  ( 145.3595637443018234, -69.45303146431501773, 247.4784022495120155 ) ) ;
#53795 = DIRECTION ( 'NONE',  ( -3.100000000000000258E-29, 3.100000000000000044E-14, 1.000000000000000000 ) ) ;
#53794 = CARTESIAN_POINT ( 'NONE',  ( 98.82386243697619932, -31.40279086140556331, 141.8699109901959616 ) ) ;
#53796 = DIRECTION ( 'NONE',  ( -0.9254794337955620787, -0.3787978585227822492, 0.000000000000000000 ) ) ;
#53797 = CARTESIAN_POINT ( 'NONE',  ( -57.68704571023340577, 88.97500000000002274, 67.38312395177700864 ) ) ;
#53798 = CIRCLE ( 'NONE', #13179, 7.837499999999996803 ) ;
#53799 = DIRECTION ( 'NONE',  ( 1.000000000000000000, 4.299999999999999979E-14, 1.000000000000000078E-15 ) ) ;
#53800 = DIRECTION ( 'NONE',  ( 1.000000000000000078E-15, -1.000000000000000083E-30, -1.000000000000000000 ) ) ;
#53801 = CARTESIAN_POINT ( 'NONE',  ( 67.06723304023354615, -67.87844715994098976, 245.5215440408323104 ) ) ;
#53802 = CARTESIAN_POINT ( 'NONE',  ( 96.05879824974435621, -41.05137697672059716, 96.62419670448197451 ) ) ;
#53803 = VERTEX_POINT ( 'NONE', #20312 ) ;
#53804 = CIRCLE ( 'NONE', #55240, 0.5000000000000004441 ) ;
#53805 = ORIENTED_EDGE ( 'NONE', *, *, #63562, .F. ) ;
#53806 = PLANE ( 'NONE',  #80753 ) ;
#53807 = CARTESIAN_POINT ( 'NONE',  ( -7.205548786489490269E-13, 117.4749999999999943, 103.1875000000000000 ) ) ;
#53809 = EDGE_CURVE ( 'NONE', #73841, #58184, #28090, .T. ) ;
#53808 = CARTESIAN_POINT ( 'NONE',  ( -68.53801554307339927, 120.6499999999999915, -74.15067561874339219 ) ) ;
#53810 = CARTESIAN_POINT ( 'NONE',  ( 115.3951208896509399, -39.08203659613434411, 141.4376141791150019 ) ) ;
#53811 = FACE_OUTER_BOUND ( 'NONE', #22119, .T. ) ;
#53812 = ORIENTED_EDGE ( 'NONE', *, *, #70518, .F. ) ;
#53813 = ORIENTED_EDGE ( 'NONE', *, *, #77936, .T. ) ;
#53814 = CARTESIAN_POINT ( 'NONE',  ( 3.175000000000334666, 17.78000000000000114, 31.75000000000000000 ) ) ;
#53815 = AXIS2_PLACEMENT_3D ( 'NONE', #68670, #61831, #74578 ) ;
#53816 = CARTESIAN_POINT ( 'NONE',  ( 135.4847699230876117, -21.08750326149013077, 1.944748881540630858 ) ) ;
#53817 = EDGE_LOOP ( 'NONE', ( #22844, #72860, #74976, #39336 ) ) ;
#53818 = ORIENTED_EDGE ( 'NONE', *, *, #80261, .F. ) ;
#53819 = CYLINDRICAL_SURFACE ( 'NONE', #82647, 7.937500000000000000 ) ;
#53820 = CARTESIAN_POINT ( 'NONE',  ( 101.6018043438793796, -28.26729678577900273, 216.9644404487539475 ) ) ;
#53821 = DIRECTION ( 'NONE',  ( 0.000000000000000000, 1.000000000000000000, 0.000000000000000000 ) ) ;
#53822 = VECTOR ( 'NONE', #8675, 1000.000000000000000 ) ;
#53823 = DIRECTION ( 'NONE',  ( -0.000000000000000000, -1.000000000000000000, 0.000000000000000000 ) ) ;
#53824 = DIRECTION ( 'NONE',  ( 0.000000000000000000, 0.000000000000000000, -1.000000000000000000 ) ) ;
#53825 = ORIENTED_EDGE ( 'NONE', *, *, #15451, .F. ) ;
#53826 = ORIENTED_EDGE ( 'NONE', *, *, #8261, .T. ) ;
#53827 = VECTOR ( 'NONE', #30417, 1000.000000000000000 ) ;
#53828 = ADVANCED_FACE ( 'NONE', ( #28916 ), #48418, .T. ) ;
#53829 = DIRECTION ( 'NONE',  ( -1.000000000000000000, -4.163336342344275811E-14, 0.000000000000000000 ) ) ;
#53830 = VERTEX_POINT ( 'NONE', #28449 ) ;
#53831 = ORIENTED_EDGE ( 'NONE', *, *, #31285, .F. ) ;
#53832 = CARTESIAN_POINT ( 'NONE',  ( 102.0474437309886184, -43.16675777147634108, 229.8680903695919540 ) ) ;
#53833 = CARTESIAN_POINT ( 'NONE',  ( 108.0362122550155135, -25.69517931502184993, 109.9946728949589811 ) ) ;
#53834 = CARTESIAN_POINT ( 'NONE',  ( 117.9659426345832713, -38.42225801833666310, 68.69181575210198787 ) ) ;
#53835 = CARTESIAN_POINT ( 'NONE',  ( 99.04747455419412461, -37.07517787504866646, 249.5838068554172651 ) ) ;
#53836 = CARTESIAN_POINT ( 'NONE',  ( 132.4277392773762472, -16.51875925607410167, 7.791169830161673637 ) ) ;
#53837 = CARTESIAN_POINT ( 'NONE',  ( 97.81168895331838087, -40.51742574516882200, 287.6356252759109680 ) ) ;
#53838 = CARTESIAN_POINT ( 'NONE',  ( 116.3502490628398647, -44.09465650233049416, 194.2927681330539542 ) ) ;
#53839 = CARTESIAN_POINT ( 'NONE',  ( 97.81252181335722184, -40.51708140359354360, 276.6353344664656220 ) ) ;
#53840 = ORIENTED_EDGE ( 'NONE', *, *, #30986, .F. ) ;
#53841 = DIRECTION ( 'NONE',  ( 2.900000000000000265E-14, -2.000000000000000155E-15, 1.000000000000000000 ) ) ;
#53842 = ORIENTED_EDGE ( 'NONE', *, *, #34908, .F. ) ;
#53843 = CIRCLE ( 'NONE', #68347, 0.5000000000000079936 ) ;
#53844 = ORIENTED_EDGE ( 'NONE', *, *, #28959, .T. ) ;
#53845 = FACE_OUTER_BOUND ( 'NONE', #22951, .T. ) ;
#53846 = EDGE_LOOP ( 'NONE', ( #24042, #46289, #32455, #24957 ) ) ;
#53847 = AXIS2_PLACEMENT_3D ( 'NONE', #10661, #2534, #72896 ) ;
#53848 = DIRECTION ( 'NONE',  ( 8.755702086949183871E-16, 1.000000000000000000, 0.000000000000000000 ) ) ;
#53849 = CARTESIAN_POINT ( 'NONE',  ( 99.09478958797689074, -30.55165821669924497, 91.80241262291944793 ) ) ;
#53850 = CARTESIAN_POINT ( 'NONE',  ( 98.33613682261365341, -42.42752411612296015, 101.7870538473399620 ) ) ;
#53851 = CARTESIAN_POINT ( 'NONE',  ( -12.69999999999999929, 82.54999999999999716, 129.9368274816650057 ) ) ;
#53852 = CARTESIAN_POINT ( 'NONE',  ( 172.5664832912729878, -27.82844715994070484, 74.17562527591199739 ) ) ;
#53853 = DIRECTION ( 'NONE',  ( -2.127927463864879951E-15, 0.000000000000000000, -1.000000000000000000 ) ) ;
#53856 = CARTESIAN_POINT ( 'NONE',  ( 100.6510976905702393, -26.79511100149722935, 216.5327681330539633 ) ) ;
#53855 = CARTESIAN_POINT ( 'NONE',  ( 199.3900000000000148, 59.08750000000000568, -38.10000000000000142 ) ) ;
#53854 = CARTESIAN_POINT ( 'NONE',  ( 116.3212776292299253, -32.94146857471393730, 145.1356252759109680 ) ) ;
#53857 = DIRECTION ( 'NONE',  ( 0.000000000000000000, 1.000000000000000000, 0.000000000000000000 ) ) ;
#53858 = ADVANCED_FACE ( 'NONE', ( #35258 ), #8472, .T. ) ;
#53859 = FACE_OUTER_BOUND ( 'NONE', #1849, .T. ) ;
#53860 = VERTEX_POINT ( 'NONE', #20747 ) ;
#53861 = VECTOR ( 'NONE', #16367, 1000.000000000000000 ) ;
#53862 = DIRECTION ( 'NONE',  ( -2.108538789381372925E-16, 0.5150380749100580413, 0.8571673007021100021 ) ) ;
#53863 = EDGE_CURVE ( 'NONE', #26572, #81096, #69349, .T. ) ;
#53864 = LINE ( 'NONE', #55210, #16665 ) ;
#53865 = EDGE_CURVE ( 'NONE', #55247, #61174, #23773, .T. ) ;
#53866 = FACE_OUTER_BOUND ( 'NONE', #23586, .T. ) ;
#53867 = B_SPLINE_CURVE_WITH_KNOTS ( 'NONE', 3,
 ( #38658, #79575, #59536, #45017, #10514, #38219, #65912, #80460, #3699, #87271, #25037, #31392, #59089, #86824, #52257, #80022, #17776, #10952, #72304, #45454, #18219, #45899, #2373, #9623, #30073, #57767, #50949, #65035, #51378, #23718, #79127 ),
 .UNSPECIFIED., .F., .F.,
 ( 4, 2, 2, 1, 2, 2, 2, 2, 2, 2, 2, 1, 1, 2, 2, 2, 4 ),
 ( 0.000000000000000000, 0.06250000000002874090, 0.09375000000004299339, 0.1093750000000480727, 0.1171875000000508066, 0.1250000000000535405, 0.1875000000000552891, 0.2187500000000547895, 0.2500000000000542899, 0.3125000000000500711, 0.3437500000000475175, 0.3593750000000461853, 0.3671875000000460187, 0.3710937500000459077, 0.3750000000000457967, 0.4375000000000229261, 0.5000000000000000000 ),
 .UNSPECIFIED. ) ;
#53868 = AXIS2_PLACEMENT_3D ( 'NONE', #5303, #19823, #20719 ) ;
#53869 = CARTESIAN_POINT ( 'NONE',  ( 98.58946256649487339, -99.96145986183429955, -19.78219314458215550 ) ) ;
#53871 = VERTEX_POINT ( 'NONE', #42513 ) ;
#53870 = CARTESIAN_POINT ( 'NONE',  ( 111.6277637875740538, -46.15289590646231943, 247.9356252759109509 ) ) ;
#53872 = EDGE_CURVE ( 'NONE', #72947, #47135, #54788, .T. ) ;
#53873 = CARTESIAN_POINT ( 'NONE',  ( 113.1467068653160908, -28.75413120684047996, 194.5579722171665082 ) ) ;
#53874 = CARTESIAN_POINT ( 'NONE',  ( 112.3492874949901932, -28.18945346073204306, 285.6356252759109680 ) ) ;
#53875 = CARTESIAN_POINT ( 'NONE',  ( 118.9531587402301511, -36.16547954148851574, 114.8641967044819694 ) ) ;
#53876 = LINE ( 'NONE', #60257, #17139 ) ;
#53877 = CARTESIAN_POINT ( 'NONE',  ( 82.53070037946083914, -37.95069274173288676, 7.120636252906606956 ) ) ;
#53879 = CARTESIAN_POINT ( 'NONE',  ( 25.56670390244748248, -48.82844715994178841, 137.2178068554150627 ) ) ;
#53878 = CARTESIAN_POINT ( 'NONE',  ( 33.98325472291465132, 124.5870000000000033, 3.174999999999999822 ) ) ;
#53880 = CARTESIAN_POINT ( 'NONE',  ( 97.81170999939396893, -40.51745679428447744, 191.6351607553995393 ) ) ;
#53881 = CARTESIAN_POINT ( 'NONE',  ( 73.06648329127401098, -8.729447159940974643, 14.82207188531764608 ) ) ;
#53882 = ORIENTED_EDGE ( 'NONE', *, *, #71780, .F. ) ;
#53883 = ORIENTED_EDGE ( 'NONE', *, *, #11342, .T. ) ;
#53884 = EDGE_LOOP ( 'NONE', ( #69957, #68064, #35380, #35391 ) ) ;
#53885 = EDGE_CURVE ( 'NONE', #76504, #6713, #48873, .T. ) ;
#53886 = VECTOR ( 'NONE', #27991, 1000.000000000000114 ) ;
#53887 = EDGE_LOOP ( 'NONE', ( #74698, #24623, #50153, #66971 ) ) ;
#53888 = CARTESIAN_POINT ( 'NONE',  ( -126.7857788319987407, 47.45011355129853570, 31.15124566716904653 ) ) ;
#53889 = CARTESIAN_POINT ( 'NONE',  ( 111.4063510358307241, -46.18429848020799255, 23.91848241876792969 ) ) ;
#53890 = EDGE_CURVE ( 'NONE', #46794, #69984, #77065, .T. ) ;
#53891 = LINE ( 'NONE', #19402, #80315 ) ;
#53892 = CARTESIAN_POINT ( 'NONE',  ( 145.4284892259529727, -139.2918928890854886, 245.9245030021744753 ) ) ;
#53894 = CARTESIAN_POINT ( 'NONE',  ( 71.07979490493546848, -139.9914422477621656, 247.3423811826519909 ) ) ;
#53893 = DIRECTION ( 'NONE',  ( 0.000000000000000000, 0.000000000000000000, -1.000000000000000000 ) ) ;
#53895 = AXIS2_PLACEMENT_3D ( 'NONE', #1300, #84434, #2198 ) ;
#53896 = CARTESIAN_POINT ( 'NONE',  ( 98.83240126976802742, -34.45875894154226415, 250.5352769709339782 ) ) ;
#53897 = ORIENTED_EDGE ( 'NONE', *, *, #17001, .T. ) ;
#53898 = ORIENTED_EDGE ( 'NONE', *, *, #27108, .T. ) ;
#53899 = ORIENTED_EDGE ( 'NONE', *, *, #20668, .T. ) ;
#53900 = AXIS2_PLACEMENT_3D ( 'NONE', #88642, #26399, #66038 ) ;
#53901 = CARTESIAN_POINT ( 'NONE',  ( 3.968750000000050182, 120.6499999999999915, -100.8961411191535973 ) ) ;
#53902 = FACE_OUTER_BOUND ( 'NONE', #43053, .T. ) ;
#53903 = CYLINDRICAL_SURFACE ( 'NONE', #68765, 5.041900000000001825 ) ;
#53904 = CARTESIAN_POINT ( 'NONE',  ( 36.23715912545344509, -47.82818131006131779, 129.9678068554150911 ) ) ;
#53905 = CARTESIAN_POINT ( 'NONE',  ( 98.57375871705461634, -34.19924797442281772, 27.52729759161093170 ) ) ;
#53906 = CARTESIAN_POINT ( 'NONE',  ( 118.5538584119706798, 95.23005795263746620, 0.8256312046399985061 ) ) ;
#53907 = DIRECTION ( 'NONE',  ( 0.000000000000000000, 1.000000000000000000, 0.000000000000000000 ) ) ;
#53908 = CARTESIAN_POINT ( 'NONE',  ( 99.87094702832891358, -29.26198151734318742, 265.6746728949591443 ) ) ;
#53909 = CARTESIAN_POINT ( 'NONE',  ( 177.8371591254545194, -47.82818131005477369, 180.4678068554150343 ) ) ;
#53911 = VERTEX_POINT ( 'NONE', #35711 ) ;
#53910 = AXIS2_PLACEMENT_3D ( 'NONE', #10810, #51691, #31252 ) ;
#53912 = LINE ( 'NONE', #40753, #21429 ) ;
#53914 = EDGE_CURVE ( 'NONE', #36668, #75973, #15288, .T. ) ;
#53913 = LINE ( 'NONE', #84812, #30797 ) ;
#53915 = CARTESIAN_POINT ( 'NONE',  ( 102.4274780401303531, -29.97946060242000144, 48.37380465530593909 ) ) ;
#53916 = AXIS2_PLACEMENT_3D ( 'NONE', #85992, #39937, #33133 ) ;
#53917 = VECTOR ( 'NONE', #40795, 1000.000000000000000 ) ;
#53918 = CARTESIAN_POINT ( 'NONE',  ( 57.14999999999999858, 95.25000000000000000, 326.2630000000000337 ) ) ;
#53919 = EDGE_CURVE ( 'NONE', #24368, #6819, #34817, .T. ) ;
#53920 = DIRECTION ( 'NONE',  ( 0.000000000000000000, 0.000000000000000000, 1.000000000000000000 ) ) ;
#53921 = VECTOR ( 'NONE', #33553, 1000.000000000000000 ) ;
#53922 = CARTESIAN_POINT ( 'NONE',  ( 100.8874379353258064, -44.70019678655637563, 193.0521937219151312 ) ) ;
#53923 = ORIENTED_EDGE ( 'NONE', *, *, #37728, .T. ) ;
#53924 = CARTESIAN_POINT ( 'NONE',  ( 1.387778780781445676E-14, 238.5000000000000000, 82.27542076772557778 ) ) ;
#53925 = CARTESIAN_POINT ( 'NONE',  ( 125.3463460965256786, 53.27927791669488755, -36.51250000000000284 ) ) ;
#53926 = EDGE_LOOP ( 'NONE', ( #8813, #40635, #51627, #679 ) ) ;
#53927 = CARTESIAN_POINT ( 'NONE',  ( 114.7075677164476986, -44.71649393962480445, 113.1718157521009687 ) ) ;
#53928 = EDGE_LOOP ( 'NONE', ( #5849, #32764, #75443, #42522 ) ) ;
#53930 = AXIS2_PLACEMENT_3D ( 'NONE', #46497, #81960, #12011 ) ;
#53929 = CARTESIAN_POINT ( 'NONE',  ( 100.2301541646454552, -41.85006585248910937, 66.26099125664796929 ) ) ;
#53931 = CARTESIAN_POINT ( 'NONE',  ( 97.83394025066695576, -40.57137221588841669, 87.63980401892214900 ) ) ;
#53932 = CARTESIAN_POINT ( 'NONE',  ( 99.64559906019141522, -41.57287113897975672, 98.21872616303994619 ) ) ;
#53933 = CARTESIAN_POINT ( 'NONE',  ( 6.000769315822015949E-16, 239.0000000000000000, 159.4557476874258271 ) ) ;
#53934 = DIRECTION ( 'NONE',  ( -0.9254794337955620787, -0.3787978585227822492, 0.000000000000000000 ) ) ;
#53935 = CARTESIAN_POINT ( 'NONE',  ( 116.6948211927369812, -32.58525784656897883, 75.14991099019697174 ) ) ;
#53936 = CARTESIAN_POINT ( 'NONE',  ( 97.33787651319606482, -34.07092125289876350, 182.1152721348323666 ) ) ;
#53937 = CARTESIAN_POINT ( 'NONE',  ( 104.4079846621045107, -46.45805526528280183, 257.3646764449513853 ) ) ;
#53938 = EDGE_LOOP ( 'NONE', ( #33620, #53270, #52706, #27616, #43893, #60319, #56186, #10269, #78208, #8703, #32721, #59017, #45319, #57182, #3170, #64162, #89521, #33157, #61424, #41267, #24723, #34097, #66571, #33119, #18382, #44400, #21210, #546, #61721, #35197, #11089, #79091, #49238, #28294, #3806, #12948, #86881, #37632, #69231, #14257, #81869, #6158, #56900, #60521, #75868, #61803, #50561, #41594 ) ) ;
#53939 = EDGE_CURVE ( 'NONE', #58383, #49742, #42605, .T. ) ;
#53940 = CARTESIAN_POINT ( 'NONE',  ( -117.9438495704237795, 78.46643079253874475, 12.03279974799046848 ) ) ;
#53941 = ORIENTED_EDGE ( 'NONE', *, *, #57358, .F. ) ;
#53942 = EDGE_LOOP ( 'NONE', ( #7203, #73452, #29072, #34110 ) ) ;
#53943 = CARTESIAN_POINT ( 'NONE',  ( 194.0371591254572650, -24.42818131005417825, 313.9678068554149490 ) ) ;
#53944 = ORIENTED_EDGE ( 'NONE', *, *, #62706, .T. ) ;
#53945 = CARTESIAN_POINT ( 'NONE',  ( 117.9377692877172450, -39.05906590213767515, 258.6584824187686422 ) ) ;
#53946 = CARTESIAN_POINT ( 'NONE',  ( 100.8735899011331014, -45.91031909761725416, 148.0918157521009562 ) ) ;
#53947 = CARTESIAN_POINT ( 'NONE',  ( 11.39816346244706580, 76.93354734096725167, -118.0069729841872146 ) ) ;
#53948 = CARTESIAN_POINT ( 'NONE',  ( 107.0667039024470313, -104.2784471599420755, -19.78219314458201694 ) ) ;
#53949 = CARTESIAN_POINT ( 'NONE',  ( 113.8563929230154912, -44.64017497981368621, 104.1413395616249744 ) ) ;
#53950 = DIRECTION ( 'NONE',  ( 1.000000000000000000, 0.000000000000000000, 0.000000000000000000 ) ) ;
#53951 = ORIENTED_EDGE ( 'NONE', *, *, #56980, .T. ) ;
#53952 = CARTESIAN_POINT ( 'NONE',  ( -254.0000000000000000, 53.97500000000000142, 50.79999999999999716 ) ) ;
#53953 = CARTESIAN_POINT ( 'NONE',  ( -240.5296158183964792, 93.66249999999999432, 85.72499999999999432 ) ) ;
#53954 = AXIS2_PLACEMENT_3D ( 'NONE', #40824, #61707, #89442 ) ;
#53955 = ORIENTED_EDGE ( 'NONE', *, *, #53097, .T. ) ;
#53956 = AXIS2_PLACEMENT_3D ( 'NONE', #8961, #16655, #36660 ) ;
#53957 = DIRECTION ( 'NONE',  ( -0.000000000000000000, -0.000000000000000000, -1.000000000000000000 ) ) ;
#53958 = LINE ( 'NONE', #5857, #61452 ) ;
#53959 = CARTESIAN_POINT ( 'NONE',  ( 106.1402962346845982, -47.72062544595571154, 262.4975300378158636 ) ) ;
#53960 = DIRECTION ( 'NONE',  ( 0.000000000000000000, -1.000000000000000000, 0.000000000000000000 ) ) ;
#53961 = B_SPLINE_CURVE_WITH_KNOTS ( 'NONE', 3,
 ( #62193, #48537, #69019, #70819 ),
 .UNSPECIFIED., .F., .F.,
 ( 4, 4 ),
 ( 0.000000000000000000, 0.001493295663798172414 ),
 .UNSPECIFIED. ) ;
#53962 = CARTESIAN_POINT ( 'NONE',  ( 95.60734603896362671, -36.72944715994100306, 293.2242906452868851 ) ) ;
#53963 = CARTESIAN_POINT ( 'NONE',  ( 151.0371591254573218, -24.95799193692592866, 300.4678068554149490 ) ) ;
#53964 = CARTESIAN_POINT ( 'NONE',  ( 114.3094922386577110, -31.29331878451978355, 263.7733722090294464 ) ) ;
#53966 = CARTESIAN_POINT ( 'NONE',  ( 108.0321269276242049, -25.74166508409292220, 105.9946728949589811 ) ) ;
#53965 = CARTESIAN_POINT ( 'NONE',  ( 179.1667039024460166, -28.27351298637280408, -5.074374724088000832 ) ) ;
#53967 = PLANE ( 'NONE',  #20451 ) ;
#53968 = CARTESIAN_POINT ( 'NONE',  ( 96.57452018799374116, -36.20934681947932177, 171.2870538473399620 ) ) ;
#53969 = ORIENTED_EDGE ( 'NONE', *, *, #52062, .T. ) ;
#53970 = LINE ( 'NONE', #6744, #53921 ) ;
#53971 = ORIENTED_EDGE ( 'NONE', *, *, #57123, .F. ) ;
#53972 = B_SPLINE_CURVE_WITH_KNOTS ( 'NONE', 3,
 ( #6381, #11861, #19559, #54945, #47248, #82711, #74977, #5041, #59980, #87710, #68170, #25479, #5951, #33641, #61332, #89059, #53150, #80919 ),
 .UNSPECIFIED., .F., .F.,
 ( 4, 2, 2, 2, 2, 2, 2, 2, 4 ),
 ( 0.000000000000000000, 0.06249602157272145242, 0.1249920431454429048, 0.1874880647181643711, 0.2499840862908858097, 0.3124801078636072482, 0.3749761294363287423, 0.4374721510090504584, 0.4999681725817722855 ),
 .UNSPECIFIED. ) ;
#53973 = DIRECTION ( 'NONE',  ( -4.237773401492740281E-14, 1.000000000000000000, 0.000000000000000000 ) ) ;
#53974 = CARTESIAN_POINT ( 'NONE',  ( 116.3201542697790529, -32.94256427661516540, 65.13562527591099638 ) ) ;
#53975 = DIRECTION ( 'NONE',  ( -3.100000000000000258E-29, 3.100000000000000044E-14, 1.000000000000000000 ) ) ;
#53977 = EDGE_LOOP ( 'NONE', ( #48919, #56862, #13432, #12417 ) ) ;
#53976 = EDGE_CURVE ( 'NONE', #85218, #60508, #7572, .T. ) ;
#53978 = CARTESIAN_POINT ( 'NONE',  ( 25.56670390244797275, -67.87844715994100397, 252.3428068554150059 ) ) ;
#53980 = ORIENTED_EDGE ( 'NONE', *, *, #17918, .T. ) ;
#53979 = CARTESIAN_POINT ( 'NONE',  ( 109.0807882705640139, -47.64528240413121551, 127.7337205140059382 ) ) ;
#53981 = DIRECTION ( 'NONE',  ( 0.000000000000000000, 0.000000000000000000, 1.000000000000000000 ) ) ;
#53982 = CARTESIAN_POINT ( 'NONE',  ( -130.5150051272322571, 94.82199753261677699, 3.295598630356760150 ) ) ;
#53983 = CARTESIAN_POINT ( 'NONE',  ( -3.968750000000770051, 120.6499999999999915, 105.4788588808462038 ) ) ;
#53984 = FACE_OUTER_BOUND ( 'NONE', #70629, .T. ) ;
#53985 = ORIENTED_EDGE ( 'NONE', *, *, #41478, .T. ) ;
#53986 = CIRCLE ( 'NONE', #58350, 1.000000000000000888 ) ;
#53987 = DIRECTION ( 'NONE',  ( -5.551115123125783935E-17, 0.000000000000000000, -1.000000000000000000 ) ) ;
#53988 = CARTESIAN_POINT ( 'NONE',  ( 172.5664832912728457, -18.82844715994071194, 321.9256252759119548 ) ) ;
#53989 = ORIENTED_EDGE ( 'NONE', *, *, #1203, .T. ) ;
#53990 = CIRCLE ( 'NONE', #26463, 11.45913725231036118 ) ;
#53991 = ADVANCED_FACE ( 'NONE', ( #49331 ), #28000, .T. ) ;
#53992 = ORIENTED_EDGE ( 'NONE', *, *, #15855, .F. ) ;
#53993 = LINE ( 'NONE', #13149, #11873 ) ;
#53994 = CARTESIAN_POINT ( 'NONE',  ( 82.96293804092860569, 84.21449860606320215, -100.8069756963038657 ) ) ;
#53995 = EDGE_CURVE ( 'NONE', #14566, #15500, #49780, .T. ) ;
#53996 = CARTESIAN_POINT ( 'NONE',  ( 99.04406178140811789, -42.84125753979320450, 156.8439585992620096 ) ) ;
#53997 = DIRECTION ( 'NONE',  ( 0.000000000000000000, 1.000000000000000000, 0.000000000000000000 ) ) ;
#53999 = CARTESIAN_POINT ( 'NONE',  ( -12.61759658107631665, 80.88542946572127335, -117.8827710199055048 ) ) ;
#53998 = CARTESIAN_POINT ( 'NONE',  ( 97.33782221849729410, -34.07114218142883288, 106.1147982288662774 ) ) ;
#54000 = CARTESIAN_POINT ( 'NONE',  ( 177.1649999999999920, 5.112500000000000711, -7.937500000000000000 ) ) ;
#54001 = B_SPLINE_CURVE_WITH_KNOTS ( 'NONE', 3,
 ( #83308, #35133, #41056, #62844, #621, #6389, #47256, #74985, #40006, #61340, #26386, #19568, #47704, #19125, #40458, #89068, #82270, #53612, #54507, #67721, #12769, #87717, #26826, #11870, #46804, #74537, #27278, #32289, #34079, #66820, #59987, #25943, #82720, #20028, #75885, #40900, #68625, #5507, #20481, #61783, #33202, #5961, #60903, #88631, #48151, #89522, #25486, #5048, #53158 ),
 .UNSPECIFIED., .F., .F.,
 ( 4, 2, 2, 2, 2, 2, 2, 2, 2, 2, 2, 2, 2, 2, 2, 1, 2, 2, 2, 2, 2, 2, 2, 2, 4 ),
 ( 0.01986933033599076401, 0.02111088875730814801, 0.02235244717862552855, 0.02483556402126029655, 0.02607712244257766321, 0.02731868086389502639, 0.02980179770652975624, 0.03228491454916448261, 0.03352647297048184927, 0.03476803139179920898, 0.03725114823443395617, 0.03849270665575132977, 0.03973426507706870336, 0.04221738191970343668, 0.04345894034102081721, 0.04470049876233818387, 0.04594205718365555746, 0.04718361560497292412, 0.04966673244760769212, 0.05090829086892509348, 0.05214984929024249483, 0.05463296613287729753, 0.05587452455419468500, 0.05711608297551208635, 0.05959919981814688905 ),
 .UNSPECIFIED. ) ;
#54002 = ORIENTED_EDGE ( 'NONE', *, *, #38346, .F. ) ;
#54003 = DIRECTION ( 'NONE',  ( 1.000000000000000078E-15, 1.000000000000000083E-30, -1.000000000000000000 ) ) ;
#54004 = CARTESIAN_POINT ( 'NONE',  ( 98.48461633480667388, -41.42146110206439147, 217.7241967044819546 ) ) ;
#54006 = ORIENTED_EDGE ( 'NONE', *, *, #26762, .F. ) ;
#54005 = FACE_BOUND ( 'NONE', #67712, .T. ) ;
#54007 = AXIS2_PLACEMENT_3D ( 'NONE', #73921, #11701, #53893 ) ;
#54008 = CARTESIAN_POINT ( 'NONE',  ( 112.3909220325769382, -27.83061929752864572, 50.65943479972001739 ) ) ;
#54009 = DIRECTION ( 'NONE',  ( 0.000000000000000000, 0.000000000000000000, -1.000000000000000000 ) ) ;
#54010 = LINE ( 'NONE', #19520, #23910 ) ;
#54011 = CARTESIAN_POINT ( 'NONE',  ( 210.5660000000000025, 52.73749999999999716, -39.68750000000000000 ) ) ;
#54012 = ORIENTED_EDGE ( 'NONE', *, *, #31173, .F. ) ;
#54013 = PLANE ( 'NONE',  #76267 ) ;
#54014 = ORIENTED_EDGE ( 'NONE', *, *, #80119, .T. ) ;
#54015 = ORIENTED_EDGE ( 'NONE', *, *, #43112, .T. ) ;
#54016 = CARTESIAN_POINT ( 'NONE',  ( 109.7775653660112596, -28.26114369521987868, 231.2615833058969770 ) ) ;
#54017 = VECTOR ( 'NONE', #9967, 1000.000000000000114 ) ;
#54018 = DIRECTION ( 'NONE',  ( 0.000000000000000000, 0.000000000000000000, -1.000000000000000000 ) ) ;
#54019 = DIRECTION ( 'NONE',  ( -1.000000000000000078E-15, 1.000000000000000000, 0.000000000000000000 ) ) ;
#54020 = EDGE_CURVE ( 'NONE', #48304, #31161, #41171, .T. ) ;
#54021 = CARTESIAN_POINT ( 'NONE',  ( 34.96670390244699433, -26.71338133339301635, 313.9678068554150059 ) ) ;
#54022 = CARTESIAN_POINT ( 'NONE',  ( 82.60909586547556671, -37.77717416134770190, 2.822018739140996324 ) ) ;
#54023 = ORIENTED_EDGE ( 'NONE', *, *, #84999, .T. ) ;
#54024 = CARTESIAN_POINT ( 'NONE',  ( 74.06670390244704549, -118.2784471599409812, 230.7030882296565721 ) ) ;
#54025 = CARTESIAN_POINT ( 'NONE',  ( 112.1310759968675654, -28.00808910187714673, 35.65652423099695056 ) ) ;
#54026 = ORIENTED_EDGE ( 'NONE', *, *, #87288, .F. ) ;
#54027 = CARTESIAN_POINT ( 'NONE',  ( 105.3203727031265373, -26.45150370518939198, 15.20991099019697401 ) ) ;
#54028 = VERTEX_POINT ( 'NONE', #68902 ) ;
#54029 = CARTESIAN_POINT ( 'NONE',  ( 98.61142602524013512, -34.88203500400037882, 253.9614237029248613 ) ) ;
#54030 = AXIS2_PLACEMENT_3D ( 'NONE', #51047, #66005, #36977 ) ;
#54031 = DIRECTION ( 'NONE',  ( 0.7071067811869833353, 0.7071067811861116992, -5.678536605557180514E-12 ) ) ;
#54032 = CARTESIAN_POINT ( 'NONE',  ( 109.3575602964533431, -46.23809593081423941, 132.7641967044829698 ) ) ;
#54033 = CARTESIAN_POINT ( 'NONE',  ( 23.35562885956705514, 78.96316603869469475, 306.0434217894609787 ) ) ;
#54034 = DIRECTION ( 'NONE',  ( -0.9254794337955620787, -0.3787978585227822492, 0.000000000000000000 ) ) ;
#54035 = CARTESIAN_POINT ( 'NONE',  ( -194.1576000000000022, 20.32000000000000028, -213.9117947927954901 ) ) ;
#54036 = LINE ( 'NONE', #12750, #55174 ) ;
#54037 = CARTESIAN_POINT ( 'NONE',  ( 111.6274790011277247, -46.15230754745154940, 243.9356252759109509 ) ) ;
#54038 = DIRECTION ( 'NONE',  ( 8.659560562355022838E-17, 0.7071067811865401342, -0.7071067811865549002 ) ) ;
#54039 = ORIENTED_EDGE ( 'NONE', *, *, #63736, .F. ) ;
#54040 = VECTOR ( 'NONE', #47827, 1000.000000000000000 ) ;
#54041 = CARTESIAN_POINT ( 'NONE',  ( 109.9229042994399492, -46.83780379245977343, 68.79562527591099297 ) ) ;
#54042 = EDGE_CURVE ( 'NONE', #63582, #83770, #49873, .T. ) ;
#54043 = DIRECTION ( 'NONE',  ( 0.000000000000000000, -1.000000000000000000, 0.000000000000000000 ) ) ;
#54044 = VERTEX_POINT ( 'NONE', #27559 ) ;
#54046 = EDGE_CURVE ( 'NONE', #35135, #27298, #55238, .T. ) ;
#54045 = ORIENTED_EDGE ( 'NONE', *, *, #25584, .F. ) ;
#54047 = ORIENTED_EDGE ( 'NONE', *, *, #27740, .F. ) ;
#54048 = CIRCLE ( 'NONE', #1842, 8.636000000000004562 ) ;
#54049 = EDGE_CURVE ( 'NONE', #69845, #88931, #79755, .T. ) ;
#54050 = CARTESIAN_POINT ( 'NONE',  ( 182.5667039024480118, -32.29483332968450782, 193.9678068554150059 ) ) ;
#54051 = CARTESIAN_POINT ( 'NONE',  ( 140.9629299006806775, -8.979447159940995959, -5.074374724088994704 ) ) ;
#54052 = LINE ( 'NONE', #45456, #45094 ) ;
#54053 = PLANE ( 'NONE',  #11265 ) ;
#54054 = CARTESIAN_POINT ( 'NONE',  ( 105.4193742293517460, -27.59801994936882252, 123.0366617981629673 ) ) ;
#54055 = CARTESIAN_POINT ( 'NONE',  ( 117.5131067102741582, -36.80237174509009179, 259.8213395616249386 ) ) ;
#54056 = EDGE_CURVE ( 'NONE', #15222, #5926, #44303, .T. ) ;
#54057 = CARTESIAN_POINT ( 'NONE',  ( 152.0371591254582881, -47.82818131005588214, 313.9678068554149490 ) ) ;
#54058 = ORIENTED_EDGE ( 'NONE', *, *, #86324, .F. ) ;
#54059 = SURFACE_STYLE_FILL_AREA ( #32747 ) ;
#54060 = ADVANCED_FACE ( 'NONE', ( #16185 ), #72482, .F. ) ;
#54061 = CARTESIAN_POINT ( 'NONE',  ( 82.56670390244703128, -104.2784471599409670, 22.21780685541800082 ) ) ;
#54062 = ORIENTED_EDGE ( 'NONE', *, *, #7251, .F. ) ;
#54063 = ORIENTED_EDGE ( 'NONE', *, *, #18, .T. ) ;
#54064 = ADVANCED_FACE ( 'NONE', ( #10247 ), #16622, .F. ) ;
#54065 = EDGE_CURVE ( 'NONE', #37203, #34061, #72036, .T. ) ;
#54066 = DIRECTION ( 'NONE',  ( 0.000000000000000000, 1.000000000000000000, 0.000000000000000000 ) ) ;
#54067 = ORIENTED_EDGE ( 'NONE', *, *, #5816, .F. ) ;
#54068 = ORIENTED_EDGE ( 'NONE', *, *, #77614, .F. ) ;
#54069 = LINE ( 'NONE', #54517, #86129 ) ;
#54070 = CARTESIAN_POINT ( 'NONE',  ( -11.89174298505462524, 78.07232539501590907, -130.0133884065672589 ) ) ;
#54071 = EDGE_CURVE ( 'NONE', #43245, #65614, #62782, .T. ) ;
#54072 = CARTESIAN_POINT ( 'NONE',  ( 71.24076473329807868, 5.642044068322332961, 361.9756252759101471 ) ) ;
#54073 = CARTESIAN_POINT ( 'NONE',  ( 102.8311628264132906, -45.84342327138038087, 9.425625275910965328 ) ) ;
#54074 = CARTESIAN_POINT ( 'NONE',  ( 99.71244791179715605, -41.13061414147755812, 161.1781341137909465 ) ) ;
#54075 = CARTESIAN_POINT ( 'NONE',  ( 114.3840247170090407, -44.21678670926648635, 73.19276813305397411 ) ) ;
#54076 = ORIENTED_EDGE ( 'NONE', *, *, #35303, .F. ) ;
#54077 = DIRECTION ( 'NONE',  ( 0.8660254037844387076, -0.4999999999999998890, 0.000000000000000000 ) ) ;
#54078 = ORIENTED_EDGE ( 'NONE', *, *, #89595, .F. ) ;
#54079 = AXIS2_PLACEMENT_3D ( 'NONE', #41507, #89693, #27892 ) ;
#54080 = CARTESIAN_POINT ( 'NONE',  ( -91.90737012895647240, 78.46643079253875896, -74.89042153202906604 ) ) ;
#54082 = EDGE_LOOP ( 'NONE', ( #69191, #53129 ) ) ;
#54081 = EDGE_CURVE ( 'NONE', #6564, #52316, #49753, .T. ) ;
#54083 = CARTESIAN_POINT ( 'NONE',  ( 102.0662944402450876, -27.97094399344484117, 261.4898263993179626 ) ) ;
#54084 = ORIENTED_EDGE ( 'NONE', *, *, #31297, .T. ) ;
#54085 = CARTESIAN_POINT ( 'NONE',  ( -30.86579703273523734, 65.59999999999998010, 73.54054752236282866 ) ) ;
#54086 = CARTESIAN_POINT ( 'NONE',  ( -11.95696095735741160, 78.49132214204263391, 117.9519267565928118 ) ) ;
#54087 = CARTESIAN_POINT ( 'NONE',  ( 113.7395804989182579, -44.20594635639993442, 133.1562568519375418 ) ) ;
#54088 = VECTOR ( 'NONE', #55722, 1000.000000000000000 ) ;
#54089 = LINE ( 'NONE', #54534, #45149 ) ;
#54090 = EDGE_LOOP ( 'NONE', ( #40636, #50972, #62835, #38712 ) ) ;
#54091 = CARTESIAN_POINT ( 'NONE',  ( 104.6437644399306635, -47.53804903515802494, 27.38895860924395009 ) ) ;
#54092 = CARTESIAN_POINT ( 'NONE',  ( 96.61310803562074057, -37.29506674262550803, 72.36991099019596163 ) ) ;
#54094 = DIRECTION ( 'NONE',  ( 1.000000000000000000, 0.000000000000000000, 0.000000000000000000 ) ) ;
#54093 = LINE ( 'NONE', #81850, #66578 ) ;
#54095 = LINE ( 'NONE', #40495, #43838 ) ;
#54096 = CARTESIAN_POINT ( 'NONE',  ( 36.65249034007531037, -48.32844715994123419, 249.9678068554150343 ) ) ;
#54097 = EDGE_CURVE ( 'NONE', #25485, #8128, #71507, .T. ) ;
#54098 = DIRECTION ( 'NONE',  ( 0.000000000000000000, 1.000000000000000000, 0.000000000000000000 ) ) ;
#54099 = EDGE_CURVE ( 'NONE', #76315, #22883, #32305, .T. ) ;
#54100 = EDGE_CURVE ( 'NONE', #53086, #55800, #23457, .T. ) ;
#54101 = CARTESIAN_POINT ( 'NONE',  ( 147.0667039024470455, -124.3811837900075972, 245.5761017658709875 ) ) ;
#54102 = DIRECTION ( 'NONE',  ( 0.000000000000000000, 0.000000000000000000, -1.000000000000000000 ) ) ;
#54103 = VERTEX_POINT ( 'NONE', #37516 ) ;
#54104 = CARTESIAN_POINT ( 'NONE',  ( 110.3859512856231788, -47.32161482583386913, 52.80610146638697699 ) ) ;
#54105 = CARTESIAN_POINT ( 'NONE',  ( 115.2842354651272814, -44.15600456922878436, 79.25372051400697160 ) ) ;
#54106 = ADVANCED_FACE ( 'NONE', ( #38386 ), #84787, .T. ) ;
#54108 = DIRECTION ( 'NONE',  ( 0.000000000000000000, -1.000000000000000000, 0.000000000000000000 ) ) ;
#54107 = CARTESIAN_POINT ( 'NONE',  ( 182.4202572930259976, -31.94127993907710206, -5.074374724088000832 ) ) ;
#54109 = CARTESIAN_POINT ( 'NONE',  ( 44.45000000000000284, 66.67499999999999716, 260.3500000000000227 ) ) ;
#54110 = CIRCLE ( 'NONE', #14990, 2.500000000000002220 ) ;
#54111 = AXIS2_PLACEMENT_3D ( 'NONE', #36897, #29197, #7843 ) ;
#54112 = DIRECTION ( 'NONE',  ( 1.000000000000000078E-15, -1.000000000000000083E-30, -1.000000000000000000 ) ) ;
#54113 = ORIENTED_EDGE ( 'NONE', *, *, #63194, .F. ) ;
#54114 = CARTESIAN_POINT ( 'NONE',  ( 97.87212830949614784, -31.93334231290201330, 86.93181575210095957 ) ) ;
#54116 = ORIENTED_EDGE ( 'NONE', *, *, #78228, .F. ) ;
#54115 = DIRECTION ( 'NONE',  ( -4.237773401492740281E-14, 1.000000000000000000, 0.000000000000000000 ) ) ;
#54117 = CARTESIAN_POINT ( 'NONE',  ( 106.8520627977276973, -47.75749532952657006, 223.5489586092439538 ) ) ;
#54118 = CARTESIAN_POINT ( 'NONE',  ( 101.9925926974754731, -45.44547922718067667, 253.1577994238472513 ) ) ;
#54119 = CARTESIAN_POINT ( 'NONE',  ( 113.2118005416166682, -44.63368877937661239, 148.1023887368787086 ) ) ;
#54120 = DIRECTION ( 'NONE',  ( 0.000000000000000000, 0.000000000000000000, -1.000000000000000000 ) ) ;
#54121 = CARTESIAN_POINT ( 'NONE',  ( 141.8664832912729992, -1.929447159941394263, 361.9756252759109998 ) ) ;
#54122 = LINE ( 'NONE', #81879, #2726 ) ;
#54123 = LINE ( 'NONE', #88249, #13831 ) ;
#54124 = CARTESIAN_POINT ( 'NONE',  ( 98.02110346605346081, -41.80092515478916937, 181.7451490854359974 ) ) ;
#54125 = VERTEX_POINT ( 'NONE', #15736 ) ;
#54126 = VERTEX_POINT ( 'NONE', #43411 ) ;
#54127 = CARTESIAN_POINT ( 'NONE',  ( 117.1284314671335665, -36.25205438732766083, 115.2958690201829626 ) ) ;
#54128 = FACE_OUTER_BOUND ( 'NONE', #27403, .T. ) ;
#54130 = DIRECTION ( 'NONE',  ( 1.639958061481212836E-42, -4.100000000000000342E-29, -1.000000000000000000 ) ) ;
#54129 = CARTESIAN_POINT ( 'NONE',  ( 105.2300248619054344, -26.52326248388681051, 271.2061014663865990 ) ) ;
#54131 = AXIS2_PLACEMENT_3D ( 'NONE', #82655, #53091, #25875 ) ;
#54132 = DIRECTION ( 'NONE',  ( 1.000000000000000000, 1.000000000000000078E-15, 0.000000000000000000 ) ) ;
#54133 = DIRECTION ( 'NONE',  ( -0.0001713722456133526934, 0.9999999853157766072, 0.000000000000000000 ) ) ;
#54134 = DIRECTION ( 'NONE',  ( 1.000000000000000000, 1.276118419109374860E-15, 0.000000000000000000 ) ) ;
#54135 = CIRCLE ( 'NONE', #58505, 10.66799999999999748 ) ;
#54136 = DIRECTION ( 'NONE',  ( 1.000000000000000078E-15, 1.000000000000000083E-30, -1.000000000000000000 ) ) ;
#54137 = CARTESIAN_POINT ( 'NONE',  ( 177.4809174648216299, -49.32844715993478246, 129.9678068554150059 ) ) ;
#54138 = CARTESIAN_POINT ( 'NONE',  ( 113.6717327907684165, -45.56316108038149082, 188.0994347997199725 ) ) ;
#54139 = CARTESIAN_POINT ( 'NONE',  ( 108.4185240248554720, -26.73515827628457231, 169.9680643324088862 ) ) ;
#54140 = ORIENTED_EDGE ( 'NONE', *, *, #69446, .F. ) ;
#54141 = ORIENTED_EDGE ( 'NONE', *, *, #23869, .F. ) ;
#54142 = CYLINDRICAL_SURFACE ( 'NONE', #35802, 9.999999999999998224 ) ;
#54143 = CARTESIAN_POINT ( 'NONE',  ( 143.5667039024469886, -67.87844715994090450, 55.21780685541800437 ) ) ;
#54144 = CARTESIAN_POINT ( 'NONE',  ( 98.35001644836999901, -31.65630223862054393, 185.9069172308759335 ) ) ;
#54145 = CARTESIAN_POINT ( 'NONE',  ( -72.96458098368751166, 117.4749999999999943, 72.96458098368620426 ) ) ;
#54146 = CIRCLE ( 'NONE', #78904, 4.750000000000004441 ) ;
#54147 = DIRECTION ( 'NONE',  ( 0.000000000000000000, 0.000000000000000000, 1.000000000000000000 ) ) ;
#54148 = VERTEX_POINT ( 'NONE', #23007 ) ;
#54149 = CARTESIAN_POINT ( 'NONE',  ( 116.8180511536208712, -34.15651531693190179, 64.03116570955137377 ) ) ;
#54150 = ADVANCED_FACE ( 'NONE', ( #9359 ), #86118, .F. ) ;
#54151 = CARTESIAN_POINT ( 'NONE',  ( 109.3369124252947557, -26.55437064873915531, 224.9013395616249511 ) ) ;
#54152 = ADVANCED_FACE ( 'NONE', ( #22555 ), #51124, .F. ) ;
#54153 = ORIENTED_EDGE ( 'NONE', *, *, #68982, .T. ) ;
#54154 = EDGE_CURVE ( 'NONE', #65985, #976, #29410, .T. ) ;
#54155 = CARTESIAN_POINT ( 'NONE',  ( -8.316535683762193543, 92.02457483822063011, 118.2643808479089671 ) ) ;
#54156 = DIRECTION ( 'NONE',  ( 0.000000000000000000, 1.000000000000000000, 0.000000000000000000 ) ) ;
#54157 = DIRECTION ( 'NONE',  ( 0.000000000000000000, 0.000000000000000000, -1.000000000000000000 ) ) ;
#54158 = CARTESIAN_POINT ( 'NONE',  ( 113.8053744393198485, -42.15975756917345763, 41.09285227435299959 ) ) ;
#54159 = CARTESIAN_POINT ( 'NONE',  ( 108.7467188015556729, -25.78131109771034701, 140.9432443235299672 ) ) ;
#54160 = ADVANCED_FACE ( 'NONE', ( #50229 ), #71154, .F. ) ;
#54161 = DIRECTION ( 'NONE',  ( 0.7071067811873675835, 0.7071067811857274510, 7.071067811873980240E-16 ) ) ;
#54162 = ORIENTED_EDGE ( 'NONE', *, *, #5297, .F. ) ;
#54163 = EDGE_CURVE ( 'NONE', #37451, #61450, #14959, .T. ) ;
#54164 = CARTESIAN_POINT ( 'NONE',  ( 28.57499999999999929, 73.38456447661469895, 302.8950000000000387 ) ) ;
#54165 = CARTESIAN_POINT ( 'NONE',  ( 98.03114200176756299, -41.01962003592631589, 66.67980080132694809 ) ) ;
#54166 = VERTEX_POINT ( 'NONE', #11128 ) ;
#54167 = ORIENTED_EDGE ( 'NONE', *, *, #50171, .F. ) ;
#54168 = EDGE_CURVE ( 'NONE', #64389, #32858, #31570, .T. ) ;
#54169 = CARTESIAN_POINT ( 'NONE',  ( 7.752335291937837880, 92.64399975678504973, 118.3043120271755413 ) ) ;
#54170 = EDGE_LOOP ( 'NONE', ( #5788, #240 ) ) ;
#54171 = ORIENTED_EDGE ( 'NONE', *, *, #20971, .F. ) ;
#54172 = DIRECTION ( 'NONE',  ( -1.000000000000000078E-15, -1.000000000000000083E-30, 1.000000000000000000 ) ) ;
#54173 = VECTOR ( 'NONE', #39463, 1000.000000000000000 ) ;
#54174 = EDGE_CURVE ( 'NONE', #39224, #66807, #46970, .T. ) ;
#54175 = CARTESIAN_POINT ( 'NONE',  ( 98.75910798445569583, -38.71530899645634349, 55.93527697093397677 ) ) ;
#54176 = CARTESIAN_POINT ( 'NONE',  ( 103.0820296961932456, -47.91685729158425744, 252.3041967044823366 ) ) ;
#54177 = CARTESIAN_POINT ( 'NONE',  ( 98.18688568738947708, -31.30898482519904036, 170.8899109901960003 ) ) ;
#54179 = CARTESIAN_POINT ( 'NONE',  ( 97.21679027376985971, -33.31418093018012172, 282.0613395616252888 ) ) ;
#54178 = CARTESIAN_POINT ( 'NONE',  ( 41.56648329127398966, -27.57844715994070484, 198.9256252759119832 ) ) ;
#54180 = LINE ( 'NONE', #11993, #89856 ) ;
#54181 = CARTESIAN_POINT ( 'NONE',  ( 115.7812481455904390, -41.80544854195400717, 94.40617102049091613 ) ) ;
#54182 = ADVANCED_FACE ( 'NONE', ( #32913 ), #25205, .T. ) ;
#54183 = VERTEX_POINT ( 'NONE', #74265 ) ;
#54184 = ADVANCED_FACE ( 'NONE', ( #32459 ), #74705, .T. ) ;
#54185 = CARTESIAN_POINT ( 'NONE',  ( 97.92339830869723016, -40.78107783808657416, 111.6584168148213223 ) ) ;
#54187 = VECTOR ( 'NONE', #4467, 1000.000000000000000 ) ;
#54186 = CARTESIAN_POINT ( 'NONE',  ( 100.6291634319263864, -44.98581313249158598, 232.0499109901969632 ) ) ;
#54188 = VERTEX_POINT ( 'NONE', #12037 ) ;
#54189 = CARTESIAN_POINT ( 'NONE',  ( 101.9844316336549070, -45.87267731258258152, 187.1727681330539781 ) ) ;
#54190 = CARTESIAN_POINT ( 'NONE',  ( 116.3219235766278672, -32.94275373074044211, 34.13562527591096085 ) ) ;
#54191 = CIRCLE ( 'NONE', #35354, 0.5000000000000004441 ) ;
#54192 = SURFACE_STYLE_USAGE ( .BOTH. , #26519 ) ;
#54193 = CARTESIAN_POINT ( 'NONE',  ( 105.7147421359655795, -46.72375322334213621, 23.46889897272690106 ) ) ;
#54194 = DIRECTION ( 'NONE',  ( -1.821299053822143307E-16, 0.000000000000000000, 1.000000000000000000 ) ) ;
#54196 = LINE ( 'NONE', #46943, #79017 ) ;
#54195 = CARTESIAN_POINT ( 'NONE',  ( 100.9356538695852663, -31.07395776800294485, 277.6356252759110248 ) ) ;
#54197 = CARTESIAN_POINT ( 'NONE',  ( 0.000000000000000000, 0.000000000000000000, 0.000000000000000000 ) ) ;
#54198 = LINE ( 'NONE', #53751, #74386 ) ;
#54199 = LINE ( 'NONE', #87418, #2021 ) ;
#54200 = VECTOR ( 'NONE', #39405, 1000.000000000000000 ) ;
#54201 = CARTESIAN_POINT ( 'NONE',  ( 41.56648329127399677, -18.82844715994099971, 196.8086252759119645 ) ) ;
#54202 = CARTESIAN_POINT ( 'NONE',  ( 97.06125986173157116, -37.99738863349521978, 41.42674836562936491 ) ) ;
#54203 = DIRECTION ( 'NONE',  ( 0.000000000000000000, 1.000000000000000000, 0.000000000000000000 ) ) ;
#54204 = EDGE_CURVE ( 'NONE', #41893, #46749, #80641, .T. ) ;
#54206 = VERTEX_POINT ( 'NONE', #12487 ) ;
#54205 = CARTESIAN_POINT ( 'NONE',  ( 160.7738106836385441, -48.62134037874550074, 180.4678068554150059 ) ) ;
#54207 = DIRECTION ( 'NONE',  ( 9.351236661543306751E-17, -3.725950533538267725E-29, -1.000000000000000000 ) ) ;
#54208 = CARTESIAN_POINT ( 'NONE',  ( 96.83676235526975518, -34.60832162431106696, 216.1641967044819808 ) ) ;
#54209 = CARTESIAN_POINT ( 'NONE',  ( 116.5983126044778402, -29.68822244385183140, 105.3327681330539463 ) ) ;
#54210 = CARTESIAN_POINT ( 'NONE',  ( 112.4341072229889136, -46.44469865882210513, 248.9661014663869878 ) ) ;
#54211 = CARTESIAN_POINT ( 'NONE',  ( 100.9546728758785150, -28.70702567901418689, 155.5939586028919450 ) ) ;
#54212 = ADVANCED_FACE ( 'NONE', ( #19299 ), #26114, .F. ) ;
#54213 = LINE ( 'NONE', #19721, #8432 ) ;
#54215 = DIRECTION ( 'NONE',  ( -3.360405532702990443E-14, 1.000000000000000000, 0.000000000000000000 ) ) ;
#54214 = DIRECTION ( 'NONE',  ( 0.7071067811865171526, 0.7071067811865779928, 7.071067811865164719E-16 ) ) ;
#54216 = CARTESIAN_POINT ( 'NONE',  ( 123.6837132603319418, -50.82895651782485658, 239.5838068554170377 ) ) ;
#54217 = CARTESIAN_POINT ( 'NONE',  ( 131.6729728819825311, -20.08739819367843182, 2.653088468865466787 ) ) ;
#54218 = VERTEX_POINT ( 'NONE', #40628 ) ;
#54219 = VERTEX_POINT ( 'NONE', #18389 ) ;
#54220 = CARTESIAN_POINT ( 'NONE',  ( 100.5405518937255209, -43.91836718856000488, 156.4124198280769917 ) ) ;
#54222 = VERTEX_POINT ( 'NONE', #66991 ) ;
#54221 = CYLINDRICAL_SURFACE ( 'NONE', #28290, 9.425000000000000711 ) ;
#54223 = CARTESIAN_POINT ( 'NONE',  ( 183.6524903400783160, -48.32844715993452667, 300.4678068554149490 ) ) ;
#54224 = CARTESIAN_POINT ( 'NONE',  ( 112.1095002620001253, -47.42599740258504681, 133.9270538473399768 ) ) ;
#54225 = DIRECTION ( 'NONE',  ( 0.000000000000000000, 0.000000000000000000, -1.000000000000000000 ) ) ;
#54226 = CARTESIAN_POINT ( 'NONE',  ( 164.7830935719630361, -29.99615139349950965, -5.074374724088000832 ) ) ;
#54227 = DIRECTION ( 'NONE',  ( 1.000000000000000078E-15, -1.000000000000000083E-30, -1.000000000000000000 ) ) ;
#54228 = CARTESIAN_POINT ( 'NONE',  ( 107.0664832912748068, -36.72944715993923381, 14.92562527591097066 ) ) ;
#54229 = CARTESIAN_POINT ( 'NONE',  ( 116.8124865092211451, -37.88235468918158944, 53.73276813305394484 ) ) ;
#54230 = ORIENTED_EDGE ( 'NONE', *, *, #64663, .F. ) ;
#54231 = VERTEX_POINT ( 'NONE', #53330 ) ;
#54232 = ORIENTED_EDGE ( 'NONE', *, *, #619, .F. ) ;
#54234 = EDGE_CURVE ( 'NONE', #41446, #42554, #66541, .T. ) ;
#54233 = AXIS2_PLACEMENT_3D ( 'NONE', #66513, #46946, #12455 ) ;
#54235 = CARTESIAN_POINT ( 'NONE',  ( 145.4167568336388001, -78.89489531512775500, 247.5190035850939125 ) ) ;
#54237 = CARTESIAN_POINT ( 'NONE',  ( 41.56648329127398966, -27.82844715994070484, 318.9256252759120116 ) ) ;
#54236 = CARTESIAN_POINT ( 'NONE',  ( 116.4171719250472137, -30.71472603919677624, 140.2813395616249750 ) ) ;
#54238 = AXIS2_PLACEMENT_3D ( 'NONE', #85530, #16464, #2394 ) ;
#54239 = CARTESIAN_POINT ( 'NONE',  ( 191.6375511031384633, -78.44951497180814215, 342.9256252759109884 ) ) ;
#54240 = CARTESIAN_POINT ( 'NONE',  ( 7.736432051520609754, 72.46968852267782779, -130.3269799747974957 ) ) ;
#54241 = CARTESIAN_POINT ( 'NONE',  ( 127.0664832912740110, -46.72944715994101017, 14.67562527591099197 ) ) ;
#54242 = CARTESIAN_POINT ( 'NONE',  ( 84.42134122279030350, 95.24969287062864964, 83.24211534968756609 ) ) ;
#54243 = CARTESIAN_POINT ( 'NONE',  ( 100.8873815386462809, -44.70014985875308611, 178.0522830632788214 ) ) ;
#54244 = CARTESIAN_POINT ( 'NONE',  ( 104.2200364793041274, -25.25138339198301907, 90.26991099019693365 ) ) ;
#54245 = ORIENTED_EDGE ( 'NONE', *, *, #31735, .T. ) ;
#54246 = ORIENTED_EDGE ( 'NONE', *, *, #57164, .T. ) ;
#54247 = ORIENTED_EDGE ( 'NONE', *, *, #45957, .F. ) ;
#54248 = LINE ( 'NONE', #47449, #3838 ) ;
#54249 = DIRECTION ( 'NONE',  ( 0.000000000000000000, 0.000000000000000000, -1.000000000000000000 ) ) ;
#54250 = CARTESIAN_POINT ( 'NONE',  ( -12.60000000000000142, 82.54999999999999716, 117.6834004267381744 ) ) ;
#54251 = CARTESIAN_POINT ( 'NONE',  ( 115.1781387256201725, -32.22423048609648788, 177.0480903695909660 ) ) ;
#54252 = EDGE_CURVE ( 'NONE', #4156, #43071, #39722, .T. ) ;
#54253 = AXIS2_PLACEMENT_3D ( 'NONE', #9387, #79339, #18766 ) ;
#54254 = CIRCLE ( 'NONE', #84736, 3.250000000000002665 ) ;
#54255 = EDGE_CURVE ( 'NONE', #61899, #18226, #58434, .T. ) ;
#54256 = EDGE_CURVE ( 'NONE', #6148, #22550, #46074, .T. ) ;
#54257 = DIRECTION ( 'NONE',  ( -1.000000000000000078E-15, 0.000000000000000000, -1.000000000000000000 ) ) ;
#54258 = ORIENTED_EDGE ( 'NONE', *, *, #69796, .T. ) ;
#54260 = ORIENTED_EDGE ( 'NONE', *, *, #26450, .T. ) ;
#54259 = ORIENTED_EDGE ( 'NONE', *, *, #39048, .T. ) ;
#54261 = DIRECTION ( 'NONE',  ( 0.000000000000000000, -1.000000000000000000, 0.000000000000000000 ) ) ;
#54262 = AXIS2_PLACEMENT_3D ( 'NONE', #46607, #75686, #26187 ) ;
#54264 = EDGE_CURVE ( 'NONE', #770, #58384, #87003, .T. ) ;
#54263 = AXIS2_PLACEMENT_3D ( 'NONE', #3389, #45143, #2505 ) ;
#54265 = CARTESIAN_POINT ( 'NONE',  ( 107.3678158256761179, -26.30747296201684549, 321.5865679059475610 ) ) ;
#54266 = VERTEX_POINT ( 'NONE', #87893 ) ;
#54267 = ORIENTED_EDGE ( 'NONE', *, *, #18026, .T. ) ;
#54268 = CARTESIAN_POINT ( 'NONE',  ( 77.31648329127399677, -18.72944715994106346, 6.749768910606400496 ) ) ;
#54269 = CARTESIAN_POINT ( 'NONE',  ( 102.0804048320179618, -44.05524405925518039, 193.5330118773259755 ) ) ;
#54270 = ADVANCED_FACE ( 'NONE', ( #25656 ), #73811, .F. ) ;
#54271 = DIRECTION ( 'NONE',  ( 0.000000000000000000, 0.000000000000000000, 1.000000000000000000 ) ) ;
#54272 = B_SPLINE_CURVE_WITH_KNOTS ( 'NONE', 3,
 ( #26215, #55676, #5785, #53892, #55242, #33921, #20748, #75273, #33475, #81653, #82994, #61179, #74818, #76157, #27115, #48419, #46639, #61618, #13936, #41614, #33026, #69351, #89354, #12596, #34819, #28001, #62529, #74372, #12144, #39831 ),
 .UNSPECIFIED., .F., .F.,
 ( 4, 2, 2, 2, 1, 1, 1, 1, 1, 2, 2, 2, 2, 1, 1, 1, 2, 2, 4 ),
 ( 0.000000000000000000, 0.1250000000002037537, 0.1406250000002256251, 0.1484375000002365330, 0.1562500000002474687, 0.1875000000002649825, 0.2187500000002825240, 0.2343750000002711997, 0.2421875000002656209, 0.2460937500002628453, 0.2500000000002600142, 0.3749999999996757039, 0.4374999999993836042, 0.4687499999992374988, 0.4843749999991791566, 0.4921874999991500133, 0.4960937499991504018, 0.4999999999991508459, 1.000000000000000000 ),
 .UNSPECIFIED. ) ;
#54273 = CARTESIAN_POINT ( 'NONE',  ( -109.3008916335299716, 55.38362039756903954, 71.40162167859008946 ) ) ;
#54274 = ORIENTED_EDGE ( 'NONE', *, *, #89818, .T. ) ;
#54275 = ORIENTED_EDGE ( 'NONE', *, *, #11328, .F. ) ;
#54276 = ADVANCED_FACE ( 'NONE', ( #47426 ), #12939, .T. ) ;
#54277 = FACE_OUTER_BOUND ( 'NONE', #39294, .T. ) ;
#54278 = ORIENTED_EDGE ( 'NONE', *, *, #36542, .F. ) ;
#54279 = ORIENTED_EDGE ( 'NONE', *, *, #70938, .F. ) ;
#54280 = EDGE_CURVE ( 'NONE', #72232, #77895, #80197, .T. ) ;
#54281 = CARTESIAN_POINT ( 'NONE',  ( 115.6591437269271694, -35.69643618062379176, 236.7518998934009460 ) ) ;
#54282 = CARTESIAN_POINT ( 'NONE',  ( 113.9315101381565682, -28.03652776953382286, 124.5565776568629559 ) ) ;
#54283 = CARTESIAN_POINT ( 'NONE',  ( 111.9186950350130303, -27.52701776748434170, 59.68991099019693536 ) ) ;
#54284 = CARTESIAN_POINT ( 'NONE',  ( 99.40430160516557123, -34.20253528913899999, 249.5838068554174356 ) ) ;
#54285 = CARTESIAN_POINT ( 'NONE',  ( 162.9033555647770015, -33.89581943344391135, 342.9256252759119548 ) ) ;
#54286 = CARTESIAN_POINT ( 'NONE',  ( 107.3114696520656395, -25.27148101547330228, 320.7096034169829863 ) ) ;
#54287 = CARTESIAN_POINT ( 'NONE',  ( 108.6750115452441747, -26.42919841034747819, 185.9527681330539792 ) ) ;
#54288 = DIRECTION ( 'NONE',  ( 4.299999999999999979E-14, -1.000000000000000000, 4.400000000000000367E-29 ) ) ;
#54289 = ORIENTED_EDGE ( 'NONE', *, *, #53357, .T. ) ;
#54290 = CARTESIAN_POINT ( 'NONE',  ( 72.26949937496598864, -71.54137415153812185, 361.9756252759101471 ) ) ;
#54291 = ORIENTED_EDGE ( 'NONE', *, *, #68598, .F. ) ;
#54292 = ORIENTED_EDGE ( 'NONE', *, *, #37388, .F. ) ;
#54293 = DIRECTION ( 'NONE',  ( 0.000000000000000000, 0.000000000000000000, 1.000000000000000000 ) ) ;
#54294 = VERTEX_POINT ( 'NONE', #73357 ) ;
#54295 = CIRCLE ( 'NONE', #6417, 8.636000000000004562 ) ;
#54296 = CARTESIAN_POINT ( 'NONE',  ( 116.3192736897089645, -32.94707975126958388, 130.1356252759109680 ) ) ;
#54297 = CARTESIAN_POINT ( 'NONE',  ( 0.000000000000000000, 0.000000000000000000, -161.5439999999999827 ) ) ;
#54298 = CARTESIAN_POINT ( 'NONE',  ( 98.20221454234541625, -43.33276655250838871, 111.8480062282919647 ) ) ;
#54299 = CARTESIAN_POINT ( 'NONE',  ( 105.8028369410636316, -26.72358438641067124, 255.1772342916230798 ) ) ;
#54300 = VECTOR ( 'NONE', #79948, 1000.000000000000000 ) ;
#54301 = CARTESIAN_POINT ( 'NONE',  ( 136.7727304466901899, -36.23917853418728185, 6.814128304792808066 ) ) ;
#54302 = DIRECTION ( 'NONE',  ( -1.000000000000000078E-15, 1.000000000000000083E-30, 1.000000000000000000 ) ) ;
#54305 = CARTESIAN_POINT ( 'NONE',  ( 110.2492204789523100, -26.78788743924354065, 230.8299109901969643 ) ) ;
#54304 = CARTESIAN_POINT ( 'NONE',  ( 194.5667039024485234, -47.82844715993405060, 180.4678068554150343 ) ) ;
#54303 = CARTESIAN_POINT ( 'NONE',  ( 117.0718954855416172, -35.46248235747613364, 144.9272919424813892 ) ) ;
#54306 = DIRECTION ( 'NONE',  ( -4.237773401492740281E-14, 1.000000000000000000, 0.000000000000000000 ) ) ;
#54307 = CARTESIAN_POINT ( 'NONE',  ( 90.44969454456416713, -54.60520651782495349, 218.8274735512160589 ) ) ;
#54308 = ORIENTED_EDGE ( 'NONE', *, *, #81184, .F. ) ;
#54309 = DIRECTION ( 'NONE',  ( -1.000200923085726652E-15, -1.000000000000000000, 0.000000000000000000 ) ) ;
#54310 = DIRECTION ( 'NONE',  ( 0.000000000000000000, -1.000000000000000000, 0.000000000000000000 ) ) ;
#54311 = CARTESIAN_POINT ( 'NONE',  ( 106.1586424053105873, -87.30271670975442078, -11.78219314458253741 ) ) ;
#54312 = DIRECTION ( 'NONE',  ( -1.821299053822143307E-16, 0.000000000000000000, 1.000000000000000000 ) ) ;
#54314 = VERTEX_POINT ( 'NONE', #32016 ) ;
#54313 = CARTESIAN_POINT ( 'NONE',  ( 97.57529025620152652, -41.14803526195210992, 256.6727681330537507 ) ) ;
#54315 = DIRECTION ( 'NONE',  ( -0.9254794337955620787, -0.3787978585227822492, 0.000000000000000000 ) ) ;
#54316 = CARTESIAN_POINT ( 'NONE',  ( 97.10477362122047396, -39.80301782323012105, 17.56419670448195092 ) ) ;
#54317 = CARTESIAN_POINT ( 'NONE',  ( 114.2834173682332732, -44.31288860877327807, 154.1813395616249807 ) ) ;
#54318 = DIRECTION ( 'NONE',  ( 1.000000000000000000, 2.999999999999999839E-15, 1.000000000000000078E-15 ) ) ;
#54319 = EDGE_CURVE ( 'NONE', #54218, #69445, #42485, .T. ) ;
#54320 = CARTESIAN_POINT ( 'NONE',  ( 97.33785231244870317, -34.07101398346973298, 102.1147137487239718 ) ) ;
#54322 = PLANE ( 'NONE',  #54388 ) ;
#54321 = CARTESIAN_POINT ( 'NONE',  ( 107.0664832912739541, -23.41337547937445862, 305.7141315223800007 ) ) ;
#54323 = DIRECTION ( 'NONE',  ( 0.000000000000000000, 0.000000000000000000, -1.000000000000000000 ) ) ;
#54324 = DIRECTION ( 'NONE',  ( -1.000000000000000000, -0.000000000000000000, -0.000000000000000000 ) ) ;
#54325 = EDGE_LOOP ( 'NONE', ( #81229, #65471, #16520, #52795 ) ) ;
#54326 = AXIS2_PLACEMENT_3D ( 'NONE', #59526, #24584, #10944 ) ;
#54327 = AXIS2_PLACEMENT_3D ( 'NONE', #23667, #51329, #38168 ) ;
#54328 = VECTOR ( 'NONE', #23569, 1000.000000000000000 ) ;
#54329 = VECTOR ( 'NONE', #62037, 1000.000000000000000 ) ;
#54330 = ORIENTED_EDGE ( 'NONE', *, *, #21220, .T. ) ;
#54331 = EDGE_LOOP ( 'NONE', ( #13132, #12772, #14976, #78364 ) ) ;
#54332 = CIRCLE ( 'NONE', #47078, 4.875000000000017764 ) ;
#54333 = AXIS2_PLACEMENT_3D ( 'NONE', #7795, #48657, #43193 ) ;
#54334 = VERTEX_POINT ( 'NONE', #55123 ) ;
#54335 = CARTESIAN_POINT ( 'NONE',  ( -126.9767693855287405, 51.08807848479448666, 30.36069443887403096 ) ) ;
#54336 = CARTESIAN_POINT ( 'NONE',  ( 115.6551466294303054, -43.65033472170370032, 39.27467289495895386 ) ) ;
#54337 = CARTESIAN_POINT ( 'NONE',  ( 70.05650175495836152, -139.5326789363696776, 247.4193337233699879 ) ) ;
#54338 = DIRECTION ( 'NONE',  ( 1.000000000000000078E-15, 0.000000000000000000, 1.000000000000000000 ) ) ;
#54339 = FACE_OUTER_BOUND ( 'NONE', #49838, .T. ) ;
#54340 = CARTESIAN_POINT ( 'NONE',  ( 116.5602560931381220, -38.76387722282552062, 258.0809912566484741 ) ) ;
#54341 = VERTEX_POINT ( 'NONE', #20200 ) ;
#54342 = ORIENTED_EDGE ( 'NONE', *, *, #406, .T. ) ;
#54343 = EDGE_LOOP ( 'NONE', ( #56520, #73898, #88150, #61893 ) ) ;
#54344 = EDGE_CURVE ( 'NONE', #34033, #70235, #1091, .T. ) ;
#54345 = PLANE ( 'NONE',  #47133 ) ;
#54346 = LINE ( 'NONE', #40297, #15843 ) ;
#54347 = DIRECTION ( 'NONE',  ( 0.000000000000000000, 1.000000000000000000, 0.000000000000000000 ) ) ;
#54348 = AXIS2_PLACEMENT_3D ( 'NONE', #9770, #4738, #25167 ) ;
#54349 = LINE ( 'NONE', #27126, #69290 ) ;
#54350 = CARTESIAN_POINT ( 'NONE',  ( 142.8821648370248170, -72.54478064608022692, 540.9756252759101471 ) ) ;
#54351 = CARTESIAN_POINT ( 'NONE',  ( -12.70000000000000107, 82.54999999999999716, 117.8738102209307641 ) ) ;
#54352 = CARTESIAN_POINT ( 'NONE',  ( 98.14754276252327259, -43.36755551587079083, 261.8356252759109566 ) ) ;
#54353 = CARTESIAN_POINT ( 'NONE',  ( 188.5667039024479834, -62.87844715994099687, 168.3428068554150059 ) ) ;
#54354 = EDGE_LOOP ( 'NONE', ( #56791, #19171, #32278, #77683 ) ) ;
#54355 = CYLINDRICAL_SURFACE ( 'NONE', #24347, 12.70000000000000107 ) ;
#54356 = CARTESIAN_POINT ( 'NONE',  ( 107.0664832912749915, -36.72944715993903486, 25.56312527591096995 ) ) ;
#54357 = CARTESIAN_POINT ( 'NONE',  ( 110.2109830224615052, -27.99972479296931382, 97.61951894101994753 ) ) ;
#54358 = AXIS2_PLACEMENT_3D ( 'NONE', #59702, #80629, #73344 ) ;
#54359 = DIRECTION ( 'NONE',  ( 0.000000000000000000, 1.000000000000000000, 0.000000000000000000 ) ) ;
#54360 = AXIS2_PLACEMENT_3D ( 'NONE', #1639, #57019, #21636 ) ;
#54361 = CARTESIAN_POINT ( 'NONE',  ( 49.35211078756498893, -35.65087443492551245, 313.9678068554150059 ) ) ;
#54362 = ADVANCED_FACE ( 'NONE', ( #21088 ), #38161, .T. ) ;
#54363 = DIRECTION ( 'NONE',  ( -1.000000000000000078E-15, 0.000000000000000000, -1.000000000000000000 ) ) ;
#54364 = ORIENTED_EDGE ( 'NONE', *, *, #11171, .T. ) ;
#54365 = CARTESIAN_POINT ( 'NONE',  ( 0.000000000000000000, 1.270000000000000018, 0.000000000000000000 ) ) ;
#54366 = EDGE_CURVE ( 'NONE', #70797, #64389, #33817, .T. ) ;
#54367 = VERTEX_POINT ( 'NONE', #20646 ) ;
#54368 = CARTESIAN_POINT ( 'NONE',  ( 98.09046607155295305, -42.10132104613245474, 161.7556252759109725 ) ) ;
#54369 = VERTEX_POINT ( 'NONE', #48311 ) ;
#54370 = EDGE_CURVE ( 'NONE', #75722, #26617, #13381, .T. ) ;
#54371 = FACE_OUTER_BOUND ( 'NONE', #84498, .T. ) ;
#54372 = CARTESIAN_POINT ( 'NONE',  ( 115.6492561437540445, -34.52393389210755004, 120.4587261630399837 ) ) ;
#54373 = ADVANCED_FACE ( 'NONE', ( #68791 ), #48766, .T. ) ;
#54374 = DIRECTION ( 'NONE',  ( 0.000000000000000000, 0.000000000000000000, -1.000000000000000000 ) ) ;
#54375 = CARTESIAN_POINT ( 'NONE',  ( 44.45000000000000284, 66.67499999999999716, 288.9250000000000114 ) ) ;
#54376 = CARTESIAN_POINT ( 'NONE',  ( 101.0536616762676374, -27.42723333900414318, 66.54514908543495721 ) ) ;
#54377 = DIRECTION ( 'NONE',  ( -1.000000000000000000, -9.999999999999862726E-16, 4.440892098500630106E-16 ) ) ;
#54378 = DIRECTION ( 'NONE',  ( 0.000000000000000000, 1.000000000000000000, 0.000000000000000000 ) ) ;
#54379 = CIRCLE ( 'NONE', #22544, 38.10000000000000142 ) ;
#54380 = ORIENTED_EDGE ( 'NONE', *, *, #46555, .T. ) ;
#54381 = CARTESIAN_POINT ( 'NONE',  ( 130.5667039024479834, -36.72944715994100306, 239.5838068554162987 ) ) ;
#54382 = VECTOR ( 'NONE', #2210, 1000.000000000000000 ) ;
#54383 = AXIS2_PLACEMENT_3D ( 'NONE', #58398, #10690, #23900 ) ;
#54384 = VECTOR ( 'NONE', #84156, 1000.000000000000000 ) ;
#54385 = ORIENTED_EDGE ( 'NONE', *, *, #35366, .T. ) ;
#54386 = ORIENTED_EDGE ( 'NONE', *, *, #64159, .F. ) ;
#54387 = ADVANCED_FACE ( 'NONE', ( #7007 ), #49216, .T. ) ;
#54388 = AXIS2_PLACEMENT_3D ( 'NONE', #47067, #33462, #82092 ) ;
#54389 = FACE_OUTER_BOUND ( 'NONE', #66819, .T. ) ;
#54390 = VERTEX_POINT ( 'NONE', #76948 ) ;
#54391 = CARTESIAN_POINT ( 'NONE',  ( 110.8764511561472546, -27.72125199330407241, 244.7584824187689492 ) ) ;
#54392 = CARTESIAN_POINT ( 'NONE',  ( 117.7257289732168744, -39.74036323029751117, 139.6194347997199827 ) ) ;
#54393 = CARTESIAN_POINT ( 'NONE',  ( 49.35031423293199282, -29.99615139349890924, 342.9256252759109884 ) ) ;
#54394 = CARTESIAN_POINT ( 'NONE',  ( 112.1393456442706196, -28.01282278279440519, 140.6564586090036357 ) ) ;
#54395 = CARTESIAN_POINT ( 'NONE',  ( 114.5674230198705317, -44.02034806205370643, 94.21276813305395592 ) ) ;
#54396 = CARTESIAN_POINT ( 'NONE',  ( 0.000000000000000000, 82.54999999999999716, 92.46299999999996544 ) ) ;
#54397 = EDGE_LOOP ( 'NONE', ( #59595, #86282, #33054, #38758, #44365, #13965 ) ) ;
#54398 = AXIS2_PLACEMENT_3D ( 'NONE', #69907, #42618, #41723 ) ;
#54399 = LINE ( 'NONE', #82163, #53917 ) ;
#54400 = DIRECTION ( 'NONE',  ( 4.194175870806139918E-14, -1.000000000000000000, 0.000000000000000000 ) ) ;
#54401 = VECTOR ( 'NONE', #88241, 1000.000000000000114 ) ;
#54402 = VERTEX_POINT ( 'NONE', #13823 ) ;
#54403 = CARTESIAN_POINT ( 'NONE',  ( 107.0664832912739399, -36.72944715994095333, 311.6356252759109680 ) ) ;
#54404 = CARTESIAN_POINT ( 'NONE',  ( 154.5667039024469886, -67.87844715994090450, 155.2178068554179902 ) ) ;
#54405 = CARTESIAN_POINT ( 'NONE',  ( 115.0380569359702463, -30.04493676975920380, 269.3813395616251682 ) ) ;
#54406 = CARTESIAN_POINT ( 'NONE',  ( 85.72499999999999432, 66.67499999999999716, 342.8999999999999773 ) ) ;
#54407 = TOROIDAL_SURFACE ( 'NONE', #87840, 15.84999999999999964, 0.1499999999999999944 ) ;
#54408 = CARTESIAN_POINT ( 'NONE',  ( 131.3164832912739826, -18.72944715994100662, -5.074374724089004474 ) ) ;
#54409 = CARTESIAN_POINT ( 'NONE',  ( 165.6738106836199904, -26.00627455219321860, -5.074374724088000832 ) ) ;
#54410 = CARTESIAN_POINT ( 'NONE',  ( 99.63325261332695959, -43.08637385293071986, 31.88991099019694531 ) ) ;
#54412 = CARTESIAN_POINT ( 'NONE',  ( 113.9719413768824126, -28.12837331961977938, 115.5261014663869474 ) ) ;
#54411 = CARTESIAN_POINT ( 'NONE',  ( 114.3025730761101357, -29.78814224338164962, 99.43545738674667689 ) ) ;
#54413 = DIRECTION ( 'NONE',  ( 0.0001211784769804374580, -0.7071067708032349186, 0.7071067811865462405 ) ) ;
#54414 = CARTESIAN_POINT ( 'NONE',  ( 97.96866571142417968, -30.36999819975766357, 160.8289586092449497 ) ) ;
#54415 = EDGE_LOOP ( 'NONE', ( #80689, #11779 ) ) ;
#54416 = CYLINDRICAL_SURFACE ( 'NONE', #275, 7.837499999999996803 ) ;
#54417 = VERTEX_POINT ( 'NONE', #61507 ) ;
#54418 = CARTESIAN_POINT ( 'NONE',  ( 130.5667039024480118, -36.72944715994093912, 219.5838068554170093 ) ) ;
#54419 = DIRECTION ( 'NONE',  ( 1.000000000000000078E-15, -1.000000000000000083E-30, -1.000000000000000000 ) ) ;
#54420 = CARTESIAN_POINT ( 'NONE',  ( 136.8004280042375740, -36.38432671277701758, 3.076561810304699218 ) ) ;
#54421 = VERTEX_POINT ( 'NONE', #70129 ) ;
#54422 = CARTESIAN_POINT ( 'NONE',  ( 164.9190312289439930, -35.91149509761220315, -5.074374724088000832 ) ) ;
#54424 = ORIENTED_EDGE ( 'NONE', *, *, #36217, .F. ) ;
#54423 = CARTESIAN_POINT ( 'NONE',  ( 118.9678564412739092, -36.92894532057803758, 153.8127681330539644 ) ) ;
#54425 = CARTESIAN_POINT ( 'NONE',  ( 116.3183049785035195, -32.94379174720932468, 54.13562527591098217 ) ) ;
#54426 = CARTESIAN_POINT ( 'NONE',  ( -130.3273610158207134, 92.64237678566782108, 7.754451942557587074 ) ) ;
#54427 = EDGE_CURVE ( 'NONE', #41221, #85162, #80249, .T. ) ;
#54428 = DIRECTION ( 'NONE',  ( 0.000000000000000000, 0.000000000000000000, 1.000000000000000000 ) ) ;
#54429 = CARTESIAN_POINT ( 'NONE',  ( 101.9936209511393486, -45.44607154457114007, 77.15645861017721074 ) ) ;
#54430 = ORIENTED_EDGE ( 'NONE', *, *, #17403, .F. ) ;
#54431 = SHAPE_DEFINITION_REPRESENTATION ( #46997, #48599 ) ;
#54432 = VECTOR ( 'NONE', #59477, 1000.000000000000000 ) ;
#54433 = ADVANCED_FACE ( 'NONE', ( #75612 ), #76496, .T. ) ;
#54434 = ORIENTED_EDGE ( 'NONE', *, *, #78635, .T. ) ;
#54435 = VERTEX_POINT ( 'NONE', #35145 ) ;
#54436 = EDGE_LOOP ( 'NONE', ( #28544, #77540, #42840, #83794 ) ) ;
#54437 = CARTESIAN_POINT ( 'NONE',  ( 123.6837132603318992, -53.34645651782490461, 239.5838068554164693 ) ) ;
#54438 = CARTESIAN_POINT ( 'NONE',  ( 98.83759631548541336, 90.93932679091000182, -85.30153658290333851 ) ) ;
#54439 = DIRECTION ( 'NONE',  ( -2.900000000000000265E-14, 2.000000000000000155E-15, -1.000000000000000000 ) ) ;
#54440 = DIRECTION ( 'NONE',  ( 0.6537961156249192385, 0.7071067811865345831, 0.2693522585644786416 ) ) ;
#54442 = CARTESIAN_POINT ( 'NONE',  ( 50.24780502318014896, 92.07499999999998863, -72.12189744004568581 ) ) ;
#54441 = LINE ( 'NONE', #33138, #24768 ) ;
#54443 = CARTESIAN_POINT ( 'NONE',  ( 97.33775388477235424, -34.07137617144550035, 181.1148172561750869 ) ) ;
#54444 = VERTEX_POINT ( 'NONE', #42402 ) ;
#54445 = CIRCLE ( 'NONE', #12399, 7.937500000000000000 ) ;
#54446 = VERTEX_POINT ( 'NONE', #14278 ) ;
#54447 = EDGE_CURVE ( 'NONE', #17557, #89449, #49085, .T. ) ;
#54448 = CIRCLE ( 'NONE', #29799, 3.299999999999997158 ) ;
#54449 = VECTOR ( 'NONE', #20211, 1000.000000000000000 ) ;
#54450 = CARTESIAN_POINT ( 'NONE',  ( 188.5667039024479834, -65.37844715994100397, 262.0928068554150059 ) ) ;
#54451 = CIRCLE ( 'NONE', #15333, 17.33514202138209370 ) ;
#54452 = FACE_OUTER_BOUND ( 'NONE', #25549, .T. ) ;
#54453 = CARTESIAN_POINT ( 'NONE',  ( 110.5849939505706487, -26.97450646431661880, 245.7889586092439629 ) ) ;
#54455 = ORIENTED_EDGE ( 'NONE', *, *, #24447, .T. ) ;
#54454 = CARTESIAN_POINT ( 'NONE',  ( 162.5667039024460223, -22.48495420874110806, 342.9256252759119548 ) ) ;
#54456 = AXIS2_PLACEMENT_3D ( 'NONE', #37049, #64755, #59699 ) ;
#54457 = CARTESIAN_POINT ( 'NONE',  ( 113.1080853710607528, -29.03773216254920797, 75.54705384733895812 ) ) ;
#54458 = CARTESIAN_POINT ( 'NONE',  ( 115.9438631943473723, -41.40486966552543890, 53.44085822901627125 ) ) ;
#54459 = DIRECTION ( 'NONE',  ( 1.000000000000000000, 0.000000000000000000, 1.047444401652940007E-14 ) ) ;
#54460 = VECTOR ( 'NONE', #80089, 1000.000000000000000 ) ;
#54461 = CARTESIAN_POINT ( 'NONE',  ( 103.2784135495991222, -27.47469012475126604, 21.38563400800847347 ) ) ;
#54462 = ORIENTED_EDGE ( 'NONE', *, *, #50501, .T. ) ;
#54463 = DIRECTION ( 'NONE',  ( -1.000000000000000078E-15, 1.000000000000000083E-30, 1.000000000000000000 ) ) ;
#54464 = ORIENTED_EDGE ( 'NONE', *, *, #70161, .F. ) ;
#54465 = ORIENTED_EDGE ( 'NONE', *, *, #66487, .F. ) ;
#54466 = AXIS2_PLACEMENT_3D ( 'NONE', #65438, #36403, #50002 ) ;
#54467 = CARTESIAN_POINT ( 'NONE',  ( 104.3066903214637620, -46.41728735870637479, 213.7872975916119458 ) ) ;
#54468 = CARTESIAN_POINT ( 'NONE',  ( 112.0680535738694488, -45.48720938564293448, 53.98962239635005034 ) ) ;
#54469 = CARTESIAN_POINT ( 'NONE',  ( -118.5559670995752697, 95.24969287062862122, 0.8338386114225508905 ) ) ;
#54470 = AXIS2_PLACEMENT_3D ( 'NONE', #64538, #35922, #84555 ) ;
#54471 = FACE_OUTER_BOUND ( 'NONE', #22807, .T. ) ;
#54472 = EDGE_CURVE ( 'NONE', #59655, #66001, #65100, .T. ) ;
#54473 = CARTESIAN_POINT ( 'NONE',  ( 82.10314251156871990, -38.57949487819261236, 2.327894807235353802 ) ) ;
#54474 = VERTEX_POINT ( 'NONE', #8358 ) ;
#54475 = DIRECTION ( 'NONE',  ( 1.387778780781444492E-15, 0.000000000000000000, -1.000000000000000000 ) ) ;
#54476 = CARTESIAN_POINT ( 'NONE',  ( 117.0723176125373044, -35.46598533043084700, 184.9276149807092509 ) ) ;
#54477 = ORIENTED_EDGE ( 'NONE', *, *, #29283, .T. ) ;
#54478 = CARTESIAN_POINT ( 'NONE',  ( 100.4109522542116650, -28.70505079160765760, 40.62705384733894221 ) ) ;
#54479 = ORIENTED_EDGE ( 'NONE', *, *, #53809, .F. ) ;
#54480 = EDGE_CURVE ( 'NONE', #50419, #37237, #63771, .T. ) ;
#54481 = CARTESIAN_POINT ( 'NONE',  ( 113.3211896355758057, -31.48460449655562954, 267.1995189410199600 ) ) ;
#54482 = DIRECTION ( 'NONE',  ( 0.7071067811865460184, 0.000000000000000000, 0.7071067811865487940 ) ) ;
#54483 = CARTESIAN_POINT ( 'NONE',  ( 116.4171719250473984, -30.71472603919669098, 144.2813395616259697 ) ) ;
#54484 = DIRECTION ( 'NONE',  ( 0.000000000000000000, 0.000000000000000000, -1.000000000000000000 ) ) ;
#54485 = CARTESIAN_POINT ( 'NONE',  ( -7.195828152521259823E-13, 127.0000000000000000, 95.25000000000000000 ) ) ;
#54486 = CARTESIAN_POINT ( 'NONE',  ( 172.5664832912729878, -27.57844715994070484, 255.9256252759120116 ) ) ;
#54487 = CARTESIAN_POINT ( 'NONE',  ( 120.0056275895821898, -31.38355669832866468, 293.6369201390379544 ) ) ;
#54488 = CARTESIAN_POINT ( 'NONE',  ( 118.0865697951701350, -35.40461063965730659, 234.9337205140059552 ) ) ;
#54489 = DIRECTION ( 'NONE',  ( 0.000000000000000000, 0.000000000000000000, 1.000000000000000000 ) ) ;
#54490 = EDGE_LOOP ( 'NONE', ( #13157, #53969 ) ) ;
#54491 = CARTESIAN_POINT ( 'NONE',  ( 96.03173718742787912, -37.92605769912402991, 77.40038718067299328 ) ) ;
#54492 = CYLINDRICAL_SURFACE ( 'NONE', #68586, 0.4999999999999982236 ) ;
#54493 = CIRCLE ( 'NONE', #58853, 7.199999999999998401 ) ;
#54494 = EDGE_LOOP ( 'NONE', ( #77295, #28171, #63149, #12644, #14439, #21848, #39912, #32026 ) ) ;
#54495 = ORIENTED_EDGE ( 'NONE', *, *, #61280, .T. ) ;
#54496 = VERTEX_POINT ( 'NONE', #65544 ) ;
#54497 = EDGE_CURVE ( 'NONE', #64498, #29605, #77323, .T. ) ;
#54498 = CARTESIAN_POINT ( 'NONE',  ( -72.96458098368600531, 127.0000000000000000, -72.96458098368781009 ) ) ;
#54500 = EDGE_CURVE ( 'NONE', #38055, #19567, #40996, .T. ) ;
#54499 = CARTESIAN_POINT ( 'NONE',  ( 32.06670390244800473, -32.29483332968611364, -5.074374724088000832 ) ) ;
#54501 = DIRECTION ( 'NONE',  ( 0.000000000000000000, 0.000000000000000000, -1.000000000000000000 ) ) ;
#54502 = CARTESIAN_POINT ( 'NONE',  ( 21.03715912545823130, -47.82818131006186491, 313.9678068554150059 ) ) ;
#54503 = CARTESIAN_POINT ( 'NONE',  ( 107.7334136049453406, -44.89265071023657327, 175.4595189410199509 ) ) ;
#54504 = CARTESIAN_POINT ( 'NONE',  ( 118.6781471654015689, -39.21772221756580734, 254.6584824187681022 ) ) ;
#54505 = CARTESIAN_POINT ( 'NONE',  ( 116.7943317353957440, -39.39066265141695311, 59.61455726299030999 ) ) ;
#54506 = VERTEX_POINT ( 'NONE', #50113 ) ;
#54507 = CARTESIAN_POINT ( 'NONE',  ( 130.4513346304067340, 94.12569442554139698, 5.240856348473897697 ) ) ;
#54508 = DIRECTION ( 'NONE',  ( 1.000000000000000000, 6.208581945447490230E-14, 1.000000000000000078E-15 ) ) ;
#54509 = ORIENTED_EDGE ( 'NONE', *, *, #1907, .T. ) ;
#54510 = VERTEX_POINT ( 'NONE', #42846 ) ;
#54511 = CIRCLE ( 'NONE', #29923, 38.10000000000000853 ) ;
#54512 = CIRCLE ( 'NONE', #26998, 11.57110091390434192 ) ;
#54513 = CARTESIAN_POINT ( 'NONE',  ( 74.06670390244704549, -118.2784471599409812, 51.21780685541800437 ) ) ;
#54514 = CIRCLE ( 'NONE', #89378, 1.000000000002049694 ) ;
#54515 = VERTEX_POINT ( 'NONE', #64652 ) ;
#54516 = ORIENTED_EDGE ( 'NONE', *, *, #59388, .T. ) ;
#54517 = CARTESIAN_POINT ( 'NONE',  ( 54.06670390244700997, -79.67844715994098692, 180.4678068554179902 ) ) ;
#54518 = DIRECTION ( 'NONE',  ( 0.000000000000000000, 0.000000000000000000, 1.000000000000000000 ) ) ;
#54519 = VECTOR ( 'NONE', #12388, 1000.000000000000000 ) ;
#54520 = DIRECTION ( 'NONE',  ( 9.351236661543306751E-17, -3.725950533538267725E-29, -1.000000000000000000 ) ) ;
#54521 = CARTESIAN_POINT ( 'NONE',  ( 219.9639999999999986, 40.03750000000000142, -58.73749999999999716 ) ) ;
#54522 = CARTESIAN_POINT ( 'NONE',  ( 112.9437820074331569, -43.62348782359368471, 152.5733722090289746 ) ) ;
#54523 = CARTESIAN_POINT ( 'NONE',  ( 117.9706719164645250, -41.49678058079525300, 58.49848241876792798 ) ) ;
#54524 = CARTESIAN_POINT ( 'NONE',  ( 107.0664832912739968, -36.72944715994100306, 293.2242906452868851 ) ) ;
#54525 = ORIENTED_EDGE ( 'NONE', *, *, #33688, .T. ) ;
#54526 = CARTESIAN_POINT ( 'NONE',  ( -75.85240403722346514, 75.84278307195158675, -91.11526841082596206 ) ) ;
#54527 = ORIENTED_EDGE ( 'NONE', *, *, #59736, .F. ) ;
#54528 = CARTESIAN_POINT ( 'NONE',  ( 108.4162223138228285, -26.73487509133866524, 260.9689798133920249 ) ) ;
#54529 = ORIENTED_EDGE ( 'NONE', *, *, #57709, .F. ) ;
#54530 = CARTESIAN_POINT ( 'NONE',  ( 25.56670390244797275, -65.37844715994100397, 168.3428068554150059 ) ) ;
#54531 = CARTESIAN_POINT ( 'NONE',  ( 133.5122728224967830, -134.8238870115027055, 248.4142799812389910 ) ) ;
#54532 = CARTESIAN_POINT ( 'NONE',  ( 116.3197976069899795, -32.94561274469138112, 134.1356252759109680 ) ) ;
#54533 = VECTOR ( 'NONE', #53292, 1000.000000000000000 ) ;
#54534 = CARTESIAN_POINT ( 'NONE',  ( 19.56648329127400032, 0.2215528400590013880, -5.074374724088000832 ) ) ;
#54535 = ORIENTED_EDGE ( 'NONE', *, *, #15294, .F. ) ;
#54536 = CARTESIAN_POINT ( 'NONE',  ( 105.9861246248700439, -26.33814362677674836, 50.15848241876796720 ) ) ;
#54537 =( NAMED_UNIT ( * ) SI_UNIT ( $, .STERADIAN. ) SOLID_ANGLE_UNIT ( ) );
#54538 = AXIS2_PLACEMENT_3D ( 'NONE', #4543, #10464, #67203 ) ;
#54541 = EDGE_CURVE ( 'NONE', #25005, #47477, #71924, .T. ) ;
#54540 = CARTESIAN_POINT ( 'NONE',  ( 90.06670420047028358, -137.6784471599409585, 55.21780685541800437 ) ) ;
#54539 = CARTESIAN_POINT ( 'NONE',  ( -29.99999999999996092, 127.0000000000000000, 183.8826257785461280 ) ) ;
#54542 = DIRECTION ( 'NONE',  ( 0.9963424814100679816, -0.08544974978095716545, 0.000000000000000000 ) ) ;
#54543 = CARTESIAN_POINT ( 'NONE',  ( -3.258242219038141485, 70.37154502160744585, 118.3118053218331767 ) ) ;
#54544 = ORIENTED_EDGE ( 'NONE', *, *, #77754, .F. ) ;
#54545 = DIRECTION ( 'NONE',  ( 0.000000000000000000, 0.000000000000000000, 1.000000000000000000 ) ) ;
#54546 = CARTESIAN_POINT ( 'NONE',  ( 123.6837132603318565, -22.62993780205705718, 239.5838068554170377 ) ) ;
#54547 = CARTESIAN_POINT ( 'NONE',  ( 3.306873253463332496, 70.28105300984509540, 118.5105382607468130 ) ) ;
#54548 = EDGE_LOOP ( 'NONE', ( #51488, #25090, #17800, #58974 ) ) ;
#54549 = CARTESIAN_POINT ( 'NONE',  ( 114.3683386633632324, -44.20073667237542026, 69.19276813305397411 ) ) ;
#54551 = DIRECTION ( 'NONE',  ( 0.000000000000000000, -1.000000000000000000, 0.000000000000000000 ) ) ;
#54550 = CARTESIAN_POINT ( 'NONE',  ( 99.08999158803118235, -42.79608037983736324, 171.8429505068361891 ) ) ;
#54552 = DIRECTION ( 'NONE',  ( 1.000000000000000000, 0.000000000000000000, -9.299908063537909262E-17 ) ) ;
#54553 = ADVANCED_FACE ( 'NONE', ( #1988 ), #30137, .T. ) ;
#54554 = DIRECTION ( 'NONE',  ( 1.000000000000000078E-15, -1.000000000000000083E-30, -1.000000000000000000 ) ) ;
#54555 = VERTEX_POINT ( 'NONE', #57833 ) ;
#54556 = CARTESIAN_POINT ( 'NONE',  ( 112.4472966703648780, -46.45872411559670212, 98.97848241876694431 ) ) ;
#54558 = VERTEX_POINT ( 'NONE', #56935 ) ;
#54557 = CARTESIAN_POINT ( 'NONE',  ( -33.98325472291465132, 24.56180297284579694, -3.174999999999764899 ) ) ;
#54559 = CARTESIAN_POINT ( 'NONE',  ( 105.7790678824445223, -26.40611305247087870, 266.1756252759109884 ) ) ;
#54560 = DIRECTION ( 'NONE',  ( 0.000000000000000000, 1.000000000000000000, 0.000000000000000000 ) ) ;
#54561 = CARTESIAN_POINT ( 'NONE',  ( 113.6616400493835357, -44.27479244131740899, 148.1480010436838768 ) ) ;
#54562 = DIRECTION ( 'NONE',  ( 1.000000000000000000, 0.000000000000000000, 0.000000000000000000 ) ) ;
#54563 = LINE ( 'NONE', #32805, #71816 ) ;
#54564 = ADVANCED_FACE ( 'NONE', ( #86012 ), #59853, .T. ) ;
#54565 = EDGE_CURVE ( 'NONE', #57694, #53468, #9129, .T. ) ;
#54566 = DIRECTION ( 'NONE',  ( 0.000000000000000000, 0.000000000000000000, -1.000000000000000000 ) ) ;
#54567 = CARTESIAN_POINT ( 'NONE',  ( -97.40459591070860768, 72.22361908171434663, 86.93292302958646189 ) ) ;
#54568 = CARTESIAN_POINT ( 'NONE',  ( 113.3375292005774639, -44.23527279707086279, 193.1299109901969757 ) ) ;
#54569 = ORIENTED_EDGE ( 'NONE', *, *, #64888, .T. ) ;
#54570 = ORIENTED_EDGE ( 'NONE', *, *, #30789, .F. ) ;
#54571 = CARTESIAN_POINT ( 'NONE',  ( 115.6990777838195186, -41.92069145011852527, 124.8272975916109573 ) ) ;
#54572 = VECTOR ( 'NONE', #71890, 1000.000000000000000 ) ;
#54573 = CARTESIAN_POINT ( 'NONE',  ( 162.5667039024460223, -19.82844715994111340, -5.074374724088000832 ) ) ;
#54574 = VECTOR ( 'NONE', #47895, 1000.000000000000000 ) ;
#54576 = FACE_OUTER_BOUND ( 'NONE', #54494, .T. ) ;
#54575 = CARTESIAN_POINT ( 'NONE',  ( 106.5981863181247604, -46.53222597210204725, 243.5384824187679556 ) ) ;
#54577 = CIRCLE ( 'NONE', #87940, 16.33514202138210791 ) ;
#54578 = CARTESIAN_POINT ( 'NONE',  ( 188.5667039024483529, -42.82844715993430640, 137.2178068554150059 ) ) ;
#54579 = EDGE_CURVE ( 'NONE', #57891, #68568, #37397, .T. ) ;
#54580 = B_SPLINE_CURVE_WITH_KNOTS ( 'NONE', 3,
 ( #65332, #24007, #37634, #17631, #45310, #9474, #16295, #65758, #11250, #59833, #51681, #3110, #58501, #31693, #38502, #50800, #17188, #3994, #3545, #86228, #78539, #43974, #23570, #66204, #79876, #59390, #24890, #2671, #30371, #72602, #52556, #80316, #18062, #51232, #78976, #81217, #61626, #18965, #32581, #62085, #40739, #12154, #88014, #6678, #67561, #34377, #25775, #19414, #25325, #68911, #52992 ),
 .UNSPECIFIED., .F., .F.,
 ( 4, 2, 1, 1, 1, 1, 1, 1, 2, 2, 2, 2, 2, 2, 2, 1, 1, 1, 1, 1, 1, 1, 2, 2, 2, 2, 2, 2, 2, 2, 2, 4 ),
 ( 0.5000148990659494252, 0.5001369657410288383, 0.5002590324161083624, 0.5005031657662670774, 0.5009914324665847296, 0.5019679658672203670, 0.5039210326684915309, 0.5078271662710340806, 0.5156394334761188469, 0.5312639678862881576, 0.5625130367066264458, 0.6250111743473033554, 0.6875093119879802650, 0.7500074496286570636, 0.7500684829661968811, 0.7501295163037366986, 0.7502515829787583801, 0.7504957163287344635, 0.7509839830286886286, 0.7519605164285885213, 0.7539135832283616612, 0.7578197168279081630, 0.7656319840270084942, 0.7812565184252078243, 0.8125055872216067065, 0.8437546560180054778, 0.8750037248144043600, 0.9062527936108031312, 0.9375018624072020135, 0.9687509312036008957, 0.9843754656018004479, 1.000000000000000000 ),
 .UNSPECIFIED. ) ;
#54581 = LINE ( 'NONE', #60516, #85265 ) ;
#54582 = B_SPLINE_CURVE_WITH_KNOTS ( 'NONE', 3,
 ( #20214, #47884, #13393, #41082, #27458, #43314, #69252, #56500, #29706, #20659, #71059, #36072, #1107, #21560, #56041, #69703, #83787, #14295 ),
 .UNSPECIFIED., .F., .F.,
 ( 4, 2, 2, 2, 2, 2, 2, 2, 4 ),
 ( 0.000000000000000000, 0.06249194833952455286, 0.1249838966790491057, 0.1874758450185736725, 0.2499677933580982114, 0.3124597416976227504, 0.3749516900371473449, 0.4374436383766718839, 0.4999355867161964229 ),
 .UNSPECIFIED. ) ;
#54583 = DIRECTION ( 'NONE',  ( -0.8660254037844394848, 0.000000000000000000, 0.4999999999999985567 ) ) ;
#54584 = CARTESIAN_POINT ( 'NONE',  ( 182.0374245136174522, -23.42844715993458848, 117.4678068554150627 ) ) ;
#54585 = DIRECTION ( 'NONE',  ( -0.7071067811865101582, -0.7071067811865849873, 0.000000000000000000 ) ) ;
#54586 = CARTESIAN_POINT ( 'NONE',  ( 98.55548742614587354, -30.74683778668241985, 205.8384824187679669 ) ) ;
#54587 = DIRECTION ( 'NONE',  ( -2.900000000000000265E-14, 2.000000000000000155E-15, -1.000000000000000000 ) ) ;
#54588 = ORIENTED_EDGE ( 'NONE', *, *, #35960, .F. ) ;
#54590 = VERTEX_POINT ( 'NONE', #29250 ) ;
#54589 = EDGE_CURVE ( 'NONE', #33523, #57034, #23348, .T. ) ;
#54591 = CARTESIAN_POINT ( 'NONE',  ( -94.33976020835963539, 70.17656663518266669, -90.24991642302057926 ) ) ;
#54592 = CARTESIAN_POINT ( 'NONE',  ( 82.16007929298940837, -20.51483178663177398, 7.477467810856416541 ) ) ;
#54593 = CARTESIAN_POINT ( 'NONE',  ( 100.1253875378072848, -39.57043109886186727, 9.635625275910941312 ) ) ;
#54594 = CARTESIAN_POINT ( 'NONE',  ( 41.56648329127398966, -27.57844715994070484, 141.9256252759119832 ) ) ;
#54595 = CARTESIAN_POINT ( 'NONE',  ( 182.4202572930269923, -31.94127993907680718, -5.074374724088000832 ) ) ;
#54596 = ORIENTED_EDGE ( 'NONE', *, *, #81395, .T. ) ;
#54597 = DIRECTION ( 'NONE',  ( 0.000000000000000000, 0.000000000000000000, -1.000000000000000000 ) ) ;
#54598 = CARTESIAN_POINT ( 'NONE',  ( 117.4744730450754560, -36.12879772292662039, 228.8727681330539667 ) ) ;
#54599 = ORIENTED_EDGE ( 'NONE', *, *, #44628, .T. ) ;
#54600 = EDGE_CURVE ( 'NONE', #2833, #60027, #77850, .T. ) ;
#54601 = PLANE ( 'NONE',  #60756 ) ;
#54603 = EDGE_CURVE ( 'NONE', #34812, #8195, #23784, .T. ) ;
#54602 = LINE ( 'NONE', #20128, #23195 ) ;
#54604 = CARTESIAN_POINT ( 'NONE',  ( -72.96458098368751166, 101.5999999999999943, 72.96458098368620426 ) ) ;
#54605 = ADVANCED_FACE ( 'NONE', ( #57381 ), #58711, .T. ) ;
#54606 = CARTESIAN_POINT ( 'NONE',  ( 104.5412336160381273, -44.52083999592182550, 80.14523322673395000 ) ) ;
#54607 = CARTESIAN_POINT ( 'NONE',  ( 117.4480285489056683, -30.96353277002295101, 175.2299109901969700 ) ) ;
#54608 = LINE ( 'NONE', #48697, #71103 ) ;
#54609 = ORIENTED_EDGE ( 'NONE', *, *, #69091, .F. ) ;
#54610 = B_SPLINE_CURVE_WITH_KNOTS ( 'NONE', 3,
 ( #73950, #31711, #66680, #52572, #45324, #60753, #73043, #11727, #38521, #32155, #5359, #66221, #4010, #26244, #45766, #81237, #88488, #4464, #59849, #25797, #59408, #87582, #39423, #67128, #87140 ),
 .UNSPECIFIED., .F., .F.,
 ( 4, 2, 2, 1, 2, 2, 2, 2, 2, 2, 2, 2, 4 ),
 ( 0.03973447012869897599, 0.04221846688269337983, 0.04346046525969059909, 0.04470246363668782530, 0.04594446201368504457, 0.04718646039068226383, 0.04967045714467674400, 0.05091245552167399102, 0.05215445389867124498, 0.05463845065266575290, 0.05588044902966299993, 0.05712244740666024001, 0.05960644416065473405 ),
 .UNSPECIFIED. ) ;
#54611 = ADVANCED_FACE ( 'NONE', ( #16956 ), #85124, .F. ) ;
#54612 = CYLINDRICAL_SURFACE ( 'NONE', #21899, 14.00000000000000888 ) ;
#54613 = CARTESIAN_POINT ( 'NONE',  ( 117.0906974882439755, -35.57082847448015883, 68.91926238958696160 ) ) ;
#54614 = ORIENTED_EDGE ( 'NONE', *, *, #30631, .F. ) ;
#54616 = VERTEX_POINT ( 'NONE', #10138 ) ;
#54615 = VECTOR ( 'NONE', #84877, 1000.000000000000000 ) ;
#54617 = CARTESIAN_POINT ( 'NONE',  ( 2.883928177975687124, 94.92528396209716846, 118.5216277020858229 ) ) ;
#54618 = ORIENTED_EDGE ( 'NONE', *, *, #63536, .F. ) ;
#54619 = EDGE_LOOP ( 'NONE', ( #44593, #15320, #9497, #10004, #11191 ) ) ;
#54620 = DIRECTION ( 'NONE',  ( 0.000000000000000000, 0.000000000000000000, -1.000000000000000000 ) ) ;
#54621 = CARTESIAN_POINT ( 'NONE',  ( 102.1503607674210343, -29.12389592045764530, 69.96765792331494538 ) ) ;
#54622 = CARTESIAN_POINT ( 'NONE',  ( 110.2626856154920603, -26.74582790018529366, 234.8299109901969643 ) ) ;
#54623 = CARTESIAN_POINT ( 'NONE',  ( 114.1099639442526268, -29.07320488188160823, 199.4841967044819739 ) ) ;
#54625 = CARTESIAN_POINT ( 'NONE',  ( 117.5188882057536830, -36.54585972124053939, 284.8413395616252615 ) ) ;
#54624 = LINE ( 'NONE', #88306, #59140 ) ;
#54626 = CYLINDRICAL_SURFACE ( 'NONE', #50677, 6.349999999999994316 ) ;
#54627 = DIRECTION ( 'NONE',  ( 0.000000000000000000, 0.000000000000000000, -1.000000000000000000 ) ) ;
#54628 = ORIENTED_EDGE ( 'NONE', *, *, #46475, .F. ) ;
#54629 = ORIENTED_EDGE ( 'NONE', *, *, #4689, .F. ) ;
#54630 = AXIS2_PLACEMENT_3D ( 'NONE', #3375, #9300, #56986 ) ;
#54631 = CARTESIAN_POINT ( 'NONE',  ( 97.30000116515907393, -37.25789978020652882, 76.36991099019796536 ) ) ;
#54632 = CARTESIAN_POINT ( 'NONE',  ( 104.2019728789896078, -25.17854340234507760, 90.26991099019693365 ) ) ;
#54634 = CARTESIAN_POINT ( 'NONE',  ( 117.4736937924436688, -35.59074751853778196, 278.9127681330539872 ) ) ;
#54633 = AXIS2_PLACEMENT_3D ( 'NONE', #67404, #59687, #5195 ) ;
#54635 = ORIENTED_EDGE ( 'NONE', *, *, #6504, .F. ) ;
#54636 = VECTOR ( 'NONE', #59628, 1000.000000000000000 ) ;
#54637 = CARTESIAN_POINT ( 'NONE',  ( 118.8775732333442647, -37.69828162312832376, 188.7613395616259595 ) ) ;
#54638 = CARTESIAN_POINT ( 'NONE',  ( 108.4174892093325440, -26.73503592116915684, 34.96895861265306138 ) ) ;
#54639 = VECTOR ( 'NONE', #37980, 1000.000000000000000 ) ;
#54640 = LINE ( 'NONE', #89207, #8745 ) ;
#54641 = DIRECTION ( 'NONE',  ( 0.000000000000000000, 1.000000000000000000, 0.000000000000000000 ) ) ;
#54643 = CARTESIAN_POINT ( 'NONE',  ( 131.0667039024480118, -64.87844715994098976, 201.9838068554149970 ) ) ;
#54642 = CARTESIAN_POINT ( 'NONE',  ( 98.57600492221074262, -34.82225168922051495, 277.6356252759111953 ) ) ;
#54644 = DIRECTION ( 'NONE',  ( 1.000000000000000000, 8.953411488912556626E-16, 0.000000000000000000 ) ) ;
#54645 = PLANE ( 'NONE',  #399 ) ;
#54646 = CARTESIAN_POINT ( 'NONE',  ( 10.09762896578686941, 90.29673011329585108, -118.1261022283270705 ) ) ;
#54647 = CARTESIAN_POINT ( 'NONE',  ( 3.968750000000050182, 127.0000000000000000, -100.8961411191535973 ) ) ;
#54648 = CARTESIAN_POINT ( 'NONE',  ( 75.31670390244798341, -50.82844715994100682, 86.31780685541500020 ) ) ;
#54649 = CARTESIAN_POINT ( 'NONE',  ( 99.09570908462971772, -30.55043174235573034, 76.80229194148932947 ) ) ;
#54651 = ORIENTED_EDGE ( 'NONE', *, *, #27816, .F. ) ;
#54650 = CARTESIAN_POINT ( 'NONE',  ( -8.391666350164323163, 92.11848141222131403, -118.2600956121756610 ) ) ;
#54652 = DIRECTION ( 'NONE',  ( 0.000000000000000000, 0.000000000000000000, 1.000000000000000000 ) ) ;
#54653 = CARTESIAN_POINT ( 'NONE',  ( 98.01753632367962155, -44.42038823906860756, 226.8870538473399563 ) ) ;
#54654 = CARTESIAN_POINT ( 'NONE',  ( 117.2221417514105610, -42.83659189374058940, 124.3956252759109731 ) ) ;
#54655 = CARTESIAN_POINT ( 'NONE',  ( 100.1487569102796300, -45.40945638099971404, 268.0289586092443415 ) ) ;
#54656 = PLANE ( 'NONE',  #42540 ) ;
#54657 = AXIS2_PLACEMENT_3D ( 'NONE', #30708, #11145, #79773 ) ;
#54658 = CYLINDRICAL_SURFACE ( 'NONE', #73639, 3.250000000000002665 ) ;
#54659 = VECTOR ( 'NONE', #28172, 1000.000000000000000 ) ;
#54661 = CARTESIAN_POINT ( 'NONE',  ( 57.14999999999999858, 60.86974387893089755, 304.0379999999999541 ) ) ;
#54660 = CARTESIAN_POINT ( 'NONE',  ( 188.5667039024479834, -48.82844715994099971, 290.4678068554150627 ) ) ;
#54662 = FACE_OUTER_BOUND ( 'NONE', #41623, .T. ) ;
#54663 = CARTESIAN_POINT ( 'NONE',  ( 131.5359215223111278, -19.80596063775375626, 2.807537029279443708 ) ) ;
#54664 = VECTOR ( 'NONE', #32521, 1000.000000000000000 ) ;
#54665 = EDGE_CURVE ( 'NONE', #43971, #21656, #83179, .T. ) ;
#54666 = EDGE_LOOP ( 'NONE', ( #86378, #65314, #2563, #54943 ) ) ;
#54667 = EDGE_CURVE ( 'NONE', #5006, #75208, #78309, .T. ) ;
#54668 = ORIENTED_EDGE ( 'NONE', *, *, #53155, .T. ) ;
#54669 = CARTESIAN_POINT ( 'NONE',  ( 107.5470202762386549, -45.24887850357546171, 152.0438483995049523 ) ) ;
#54670 = EDGE_CURVE ( 'NONE', #10572, #12659, #78836, .T. ) ;
#54672 = VERTEX_POINT ( 'NONE', #12369 ) ;
#54671 = FACE_OUTER_BOUND ( 'NONE', #21955, .T. ) ;
#54673 = CARTESIAN_POINT ( 'NONE',  ( 98.34983002861665113, -31.65663634061341369, 90.90496632418863499 ) ) ;
#54674 = CARTESIAN_POINT ( 'NONE',  ( 102.4028819069269645, -26.73371583578780886, 131.4118157521009778 ) ) ;
#54675 = CARTESIAN_POINT ( 'NONE',  ( 99.04382043865727780, -42.84089565470306837, 147.8445008508561216 ) ) ;
#54676 = CARTESIAN_POINT ( 'NONE',  ( -47.13037117915683893, 92.74157015026722206, 74.98513935456327317 ) ) ;
#54677 = EDGE_CURVE ( 'NONE', #24616, #49620, #80525, .T. ) ;
#54678 = EDGE_CURVE ( 'NONE', #67341, #58630, #18278, .T. ) ;
#54679 = CARTESIAN_POINT ( 'NONE',  ( 34.96670390244699433, -28.27351298637401200, -5.074374724088000832 ) ) ;
#54680 = FACE_OUTER_BOUND ( 'NONE', #15929, .T. ) ;
#54681 = CARTESIAN_POINT ( 'NONE',  ( 103.8130989789263197, -45.95327097697902730, 57.30705384734097407 ) ) ;
#54682 = ORIENTED_EDGE ( 'NONE', *, *, #2580, .F. ) ;
#54683 = ORIENTED_EDGE ( 'NONE', *, *, #77095, .F. ) ;
#54685 = EDGE_LOOP ( 'NONE', ( #63768, #13324, #50385, #39070, #51473, #79710 ) ) ;
#54684 = AXIS2_PLACEMENT_3D ( 'NONE', #35348, #76249, #63063 ) ;
#54686 = EDGE_CURVE ( 'NONE', #17571, #58627, #19187, .T. ) ;
#54687 = FACE_OUTER_BOUND ( 'NONE', #52563, .T. ) ;
#54689 = CARTESIAN_POINT ( 'NONE',  ( 70.06670390441306040, -140.6784471619069734, 245.4415720117440003 ) ) ;
#54688 = CARTESIAN_POINT ( 'NONE',  ( 96.03815445040697796, -38.18343476501374312, 147.4299109901959923 ) ) ;
#54690 = CARTESIAN_POINT ( 'NONE',  ( 125.0664832912740110, -18.82844715994099971, 284.9256252759119548 ) ) ;
#54691 = ADVANCED_FACE ( 'NONE', ( #39174 ), #60961, .F. ) ;
#54692 = CARTESIAN_POINT ( 'NONE',  ( 116.0667039024470313, -104.2784471599411091, 19.21780685541799016 ) ) ;
#54693 = DIRECTION ( 'NONE',  ( 0.000000000000000000, 0.000000000000000000, -1.000000000000000000 ) ) ;
#54694 = CARTESIAN_POINT ( 'NONE',  ( 152.5667039024471592, -23.42844715993585325, 180.4678068554149775 ) ) ;
#54695 = CARTESIAN_POINT ( 'NONE',  ( 113.1779779702134903, -44.75210462311810744, 179.0939275391108936 ) ) ;
#54696 = CARTESIAN_POINT ( 'NONE',  ( 102.5676158828201352, -27.34920955258903419, 95.43276813305395478 ) ) ;
#54697 = ORIENTED_EDGE ( 'NONE', *, *, #16751, .T. ) ;
#54698 = ORIENTED_EDGE ( 'NONE', *, *, #45028, .T. ) ;
#54700 = VERTEX_POINT ( 'NONE', #45081 ) ;
#54699 = EDGE_CURVE ( 'NONE', #62015, #67197, #86889, .T. ) ;
#54701 = FACE_OUTER_BOUND ( 'NONE', #75650, .T. ) ;
#54702 = CARTESIAN_POINT ( 'NONE',  ( 142.8821648370248170, -72.54478064608022692, 540.9756252759101471 ) ) ;
#54703 = AXIS2_PLACEMENT_3D ( 'NONE', #9934, #1781, #44423 ) ;
#54704 = PLANE ( 'NONE',  #33712 ) ;
#54705 = CARTESIAN_POINT ( 'NONE',  ( 98.33113000137380766, -33.60062404821446336, 173.8709475124489359 ) ) ;
#54706 = CIRCLE ( 'NONE', #86655, 12.69999999999998863 ) ;
#54707 = VECTOR ( 'NONE', #71297, 1000.000000000000000 ) ;
#54708 = CIRCLE ( 'NONE', #43120, 5.599999999999994316 ) ;
#54709 = DIRECTION ( 'NONE',  ( 0.000000000000000000, 0.000000000000000000, 1.000000000000000000 ) ) ;
#54710 = VERTEX_POINT ( 'NONE', #32802 ) ;
#54712 = VERTEX_POINT ( 'NONE', #73237 ) ;
#54711 = ORIENTED_EDGE ( 'NONE', *, *, #50579, .T. ) ;
#54713 = FACE_OUTER_BOUND ( 'NONE', #39954, .T. ) ;
#54714 = DIRECTION ( 'NONE',  ( -0.04216478779797398074, 0.9991106698809455455, 0.000000000000000000 ) ) ;
#54715 = ORIENTED_EDGE ( 'NONE', *, *, #57133, .F. ) ;
#54716 = ORIENTED_EDGE ( 'NONE', *, *, #365, .T. ) ;
#54717 = CARTESIAN_POINT ( 'NONE',  ( 131.3179999999999836, 37.33800000000000097, 58.73749999999999716 ) ) ;
#54718 = EDGE_CURVE ( 'NONE', #27069, #21321, #1922, .T. ) ;
#54719 = CARTESIAN_POINT ( 'NONE',  ( 104.1527054293246550, -27.79712248444839773, 206.7711071154209606 ) ) ;
#54720 = CIRCLE ( 'NONE', #35883, 3.174999999999983391 ) ;
#54721 = AXIS2_PLACEMENT_3D ( 'NONE', #66896, #40978, #6037 ) ;
#54722 = ADVANCED_FACE ( 'NONE', ( #66424 ), #39612, .F. ) ;
#54723 = AXIS2_PLACEMENT_3D ( 'NONE', #68069, #47153, #25840 ) ;
#54724 = DIRECTION ( 'NONE',  ( 4.299999999999999979E-14, -1.000000000000000000, 4.400000000000000367E-29 ) ) ;
#54725 = CARTESIAN_POINT ( 'NONE',  ( -125.5854312618940867, 68.04355014475468977, 35.68462287192087956 ) ) ;
#54726 = ORIENTED_EDGE ( 'NONE', *, *, #20174, .F. ) ;
#54727 = ORIENTED_EDGE ( 'NONE', *, *, #65756, .F. ) ;
#54728 = AXIS2_PLACEMENT_3D ( 'NONE', #70656, #48377, #27960 ) ;
#54729 = DIRECTION ( 'NONE',  ( 1.000000000000000000, 0.000000000000000000, 8.465970413060558704E-17 ) ) ;
#54730 = ORIENTED_EDGE ( 'NONE', *, *, #9088, .T. ) ;
#54731 = ORIENTED_EDGE ( 'NONE', *, *, #76149, .F. ) ;
#54732 = CARTESIAN_POINT ( 'NONE',  ( 100.6247221172615127, -30.94977259965520844, 233.5747570362579495 ) ) ;
#54733 = CARTESIAN_POINT ( 'NONE',  ( 107.6542440074338458, -47.14984605634950299, 152.6213395616249500 ) ) ;
#54734 = CARTESIAN_POINT ( 'NONE',  ( 117.8527506973083518, -39.03601561205234560, 108.6708633711489824 ) ) ;
#54735 = CARTESIAN_POINT ( 'NONE',  ( 99.32188085270527722, -38.83570505065259937, 249.5838068554172935 ) ) ;
#54736 = DIRECTION ( 'NONE',  ( -0.7349399772593249169, -0.6687953793059874252, 0.1121426343770439288 ) ) ;
#54737 = CARTESIAN_POINT ( 'NONE',  ( 114.9650091533680722, -29.92534717146685708, 180.3927681330539770 ) ) ;
#54738 = CARTESIAN_POINT ( 'NONE',  ( 98.75905348231658820, -42.39375861569092052, 276.8019443637107884 ) ) ;
#54739 = VERTEX_POINT ( 'NONE', #80084 ) ;
#54740 = CARTESIAN_POINT ( 'NONE',  ( -130.0134586223093436, 78.07027470200928576, 11.89097723361267178 ) ) ;
#54741 = ORIENTED_EDGE ( 'NONE', *, *, #70243, .T. ) ;
#54742 = ORIENTED_EDGE ( 'NONE', *, *, #70246, .T. ) ;
#54743 = DIRECTION ( 'NONE',  ( 0.000000000000000000, 0.000000000000000000, 1.000000000000000000 ) ) ;
#54744 = VECTOR ( 'NONE', #33953, 1000.000000000000000 ) ;
#54745 = ORIENTED_EDGE ( 'NONE', *, *, #77992, .F. ) ;
#54746 = AXIS2_PLACEMENT_3D ( 'NONE', #28435, #74800, #728 ) ;
#54747 = DIRECTION ( 'NONE',  ( -1.000000000000000000, 0.000000000000000000, 0.000000000000000000 ) ) ;
#54748 = CARTESIAN_POINT ( 'NONE',  ( 101.5007711604877159, -27.91412646590841362, 110.5241967044819944 ) ) ;
#54749 = CARTESIAN_POINT ( 'NONE',  ( -8.063121854991559090, 72.73576936706652418, 130.3067131650634565 ) ) ;
#54750 = DIRECTION ( 'NONE',  ( -0.7071067811865516806, 0.7071067811865433539, -7.071067811865510832E-16 ) ) ;
#54751 = CYLINDRICAL_SURFACE ( 'NONE', #71690, 2.517499999999998739 ) ;
#54754 = CARTESIAN_POINT ( 'NONE',  ( 113.1426608820137716, -26.58408993604434301, 200.6470538473399756 ) ) ;
#54753 = DIRECTION ( 'NONE',  ( -0.000000000000000000, 1.000000000000000000, -0.000000000000000000 ) ) ;
#54752 = DIRECTION ( 'NONE',  ( 0.000000000000000000, 0.000000000000000000, -1.000000000000000000 ) ) ;
#54755 = DIRECTION ( 'NONE',  ( -1.000000000000000000, 0.000000000000000000, 0.000000000000000000 ) ) ;
#54756 = DIRECTION ( 'NONE',  ( 1.000000000000000000, 4.299999999999999979E-14, 1.000000000000000078E-15 ) ) ;
#54757 = ORIENTED_EDGE ( 'NONE', *, *, #83553, .F. ) ;
#54758 = LINE ( 'NONE', #25738, #517 ) ;
#54759 = DIRECTION ( 'NONE',  ( -1.000000000000000078E-15, 1.000000000000000083E-30, 1.000000000000000000 ) ) ;
#54760 = LINE ( 'NONE', #75694, #13959 ) ;
#54761 = CARTESIAN_POINT ( 'NONE',  ( 0.000000000000000000, 223.9999999999999716, 154.6557476874258441 ) ) ;
#54763 = ORIENTED_EDGE ( 'NONE', *, *, #64465, .F. ) ;
#54762 = CARTESIAN_POINT ( 'NONE',  ( 106.1344186357298867, -47.79037565197016590, 262.4975300378158067 ) ) ;
#54764 = DIRECTION ( 'NONE',  ( -0.9659258262890663138, 0.000000000000000000, -0.2588190451025281225 ) ) ;
#54765 = CARTESIAN_POINT ( 'NONE',  ( 112.1308356434906273, -47.47125106351535351, 137.9270538473389820 ) ) ;
#54766 = CARTESIAN_POINT ( 'NONE',  ( 96.71473009235836571, -37.96382682441392831, 37.42133956162496844 ) ) ;
#54767 = CARTESIAN_POINT ( 'NONE',  ( 99.06808600115306263, -45.54042523694053557, 152.9899109901969894 ) ) ;
#54768 = AXIS2_PLACEMENT_3D ( 'NONE', #17126, #72091, #45680 ) ;
#54769 = CARTESIAN_POINT ( 'NONE',  ( 242.3160000000000025, 65.43750000000000000, -63.94449999999999790 ) ) ;
#54770 = DIRECTION ( 'NONE',  ( -1.000000000000000000, 0.000000000000000000, -2.108231265501709878E-16 ) ) ;
#54771 = ADVANCED_FACE ( 'NONE', ( #60047 ), #52646, .F. ) ;
#54773 = CARTESIAN_POINT ( 'NONE',  ( 51.56670390244699576, -19.82844715994031048, -5.074374724088000832 ) ) ;
#54772 = CARTESIAN_POINT ( 'NONE',  ( -254.0000000000000000, 3.174999999999999822, -41.27499999999999858 ) ) ;
#54774 = FACE_OUTER_BOUND ( 'NONE', #82226, .T. ) ;
#54775 = DIRECTION ( 'NONE',  ( 1.000000000000000078E-15, -1.000000000000000083E-30, -1.000000000000000000 ) ) ;
#54776 = VERTEX_POINT ( 'NONE', #38280 ) ;
#54777 = AXIS2_PLACEMENT_3D ( 'NONE', #31681, #85784, #23116 ) ;
#54778 = AXIS2_PLACEMENT_3D ( 'NONE', #40926, #68649, #48177 ) ;
#54779 = EDGE_CURVE ( 'NONE', #2705, #54188, #59599, .T. ) ;
#54780 = VERTEX_POINT ( 'NONE', #46415 ) ;
#54781 = EDGE_CURVE ( 'NONE', #9096, #56828, #25117, .T. ) ;
#54782 = VERTEX_POINT ( 'NONE', #87778 ) ;
#54784 = EDGE_CURVE ( 'NONE', #30635, #6148, #88041, .T. ) ;
#54783 = AXIS2_PLACEMENT_3D ( 'NONE', #47106, #12618, #41197 ) ;
#54785 = EDGE_LOOP ( 'NONE', ( #63840, #89021, #55804, #70742 ) ) ;
#54786 = CARTESIAN_POINT ( 'NONE',  ( -127.0239848601435995, 53.97500000000000142, 30.16249999999999787 ) ) ;
#54787 = CARTESIAN_POINT ( 'NONE',  ( 100.5643946202652756, -27.81952766013699119, 26.56610146638793779 ) ) ;
#54788 = LINE ( 'NONE', #77508, #64354 ) ;
#54789 = VECTOR ( 'NONE', #7127, 1000.000000000000000 ) ;
#54790 = CARTESIAN_POINT ( 'NONE',  ( 115.3189361407783480, -42.43561143203083930, 118.3469642877515327 ) ) ;
#54791 = EDGE_CURVE ( 'NONE', #47032, #84299, #54135, .T. ) ;
#54792 = AXIS2_PLACEMENT_3D ( 'NONE', #46668, #60299, #33052 ) ;
#54793 = CARTESIAN_POINT ( 'NONE',  ( 162.5667039024460223, -22.48495420874110806, -5.074374724088000832 ) ) ;
#54794 = VECTOR ( 'NONE', #32308, 1000.000000000000000 ) ;
#54795 = CARTESIAN_POINT ( 'NONE',  ( 100.4104977919876802, -31.37650509455747283, 240.2095626852199928 ) ) ;
#54796 = VERTEX_POINT ( 'NONE', #34141 ) ;
#54797 = ORIENTED_EDGE ( 'NONE', *, *, #48383, .F. ) ;
#54798 = ORIENTED_EDGE ( 'NONE', *, *, #16895, .F. ) ;
#54800 = EDGE_CURVE ( 'NONE', #23215, #7800, #55565, .T. ) ;
#54799 = CIRCLE ( 'NONE', #56231, 3.700000000000001954 ) ;
#54801 = CARTESIAN_POINT ( 'NONE',  ( 186.6899999999999977, 46.38749999999999574, -38.10000000000000142 ) ) ;
#54802 = CARTESIAN_POINT ( 'NONE',  ( 116.7952057194422224, -39.38754349606188754, 103.6145979094304721 ) ) ;
#54803 = CARTESIAN_POINT ( 'NONE',  ( 3.017284783739249916E-15, 125.7300000000000040, 24.63800000000000168 ) ) ;
#54804 = CARTESIAN_POINT ( 'NONE',  ( 63.56670390244739366, -47.82844715994014706, 180.4678068554151196 ) ) ;
#54805 = EDGE_CURVE ( 'NONE', #31184, #78791, #82777, .T. ) ;
#54806 = LINE ( 'NONE', #34836, #5228 ) ;
#54807 = FACE_OUTER_BOUND ( 'NONE', #48091, .T. ) ;
#54808 = CARTESIAN_POINT ( 'NONE',  ( 101.2327472597881552, -44.62129728587218835, 257.0699109901973998 ) ) ;
#54809 = CARTESIAN_POINT ( 'NONE',  ( 72.96458098368701428, 117.4749999999999943, -72.96458098368670164 ) ) ;
#54811 = EDGE_LOOP ( 'NONE', ( #22941, #64335, #24029, #30698, #67787 ) ) ;
#54810 = EDGE_CURVE ( 'NONE', #68056, #79637, #80320, .T. ) ;
#54812 = DIRECTION ( 'NONE',  ( 0.000000000000000000, 1.000000000000000000, 0.000000000000000000 ) ) ;
#54813 = LINE ( 'NONE', #80771, #8964 ) ;
#54814 = CARTESIAN_POINT ( 'NONE',  ( 115.5148531418241191, -38.60720430987922214, 101.4585665600679647 ) ) ;
#54815 = VECTOR ( 'NONE', #55849, 1000.000000000000000 ) ;
#54816 = CARTESIAN_POINT ( 'NONE',  ( 183.5150000000000148, 14.63749999999999929, -57.14999999999999858 ) ) ;
#54817 = CARTESIAN_POINT ( 'NONE',  ( 25.56670390244797275, -48.82844715994099971, 175.9678068554150059 ) ) ;
#54818 = ORIENTED_EDGE ( 'NONE', *, *, #809, .T. ) ;
#54819 = DIRECTION ( 'NONE',  ( 0.000000000000000000, -1.000000000000000000, 0.000000000000000000 ) ) ;
#54820 = ORIENTED_EDGE ( 'NONE', *, *, #86404, .T. ) ;
#54821 = CARTESIAN_POINT ( 'NONE',  ( 96.64983689172015602, -37.15430107835312157, 161.3584824187679487 ) ) ;
#54822 = EDGE_LOOP ( 'NONE', ( #71558, #89746, #41202 ) ) ;
#54823 = CARTESIAN_POINT ( 'NONE',  ( 184.5664832912729878, -81.37844715994266664, 342.9256252759109884 ) ) ;
#54824 = CARTESIAN_POINT ( 'NONE',  ( 112.9789619575112596, -30.12862337550717484, 110.9272975916109658 ) ) ;
#54825 = CARTESIAN_POINT ( 'NONE',  ( -47.02966122971777452, 101.5999999999999943, 107.7386843274874053 ) ) ;
#54826 = ADVANCED_FACE ( 'NONE', ( #61839 ), #64305, .T. ) ;
#54827 = CARTESIAN_POINT ( 'NONE',  ( 80.06648329127401098, -41.22944715994105280, 4.925625275910944012 ) ) ;
#54828 = CARTESIAN_POINT ( 'NONE',  ( 111.9390199320367145, -27.48847072138506320, 55.68991099019693536 ) ) ;
#54829 = CARTESIAN_POINT ( 'NONE',  ( 117.0608945229798081, -38.08045312644978964, 84.71895860879563145 ) ) ;
#54830 = CONICAL_SURFACE ( 'NONE', #60621, 16.25000000000000000, 0.5235987755982992597 ) ;
#54831 = ORIENTED_EDGE ( 'NONE', *, *, #5335, .T. ) ;
#54832 = CIRCLE ( 'NONE', #30246, 11.45913725231036118 ) ;
#54833 = FACE_OUTER_BOUND ( 'NONE', #55365, .T. ) ;
#54834 = ORIENTED_EDGE ( 'NONE', *, *, #33393, .T. ) ;
#54835 = VERTEX_POINT ( 'NONE', #89130 ) ;
#54836 = AXIS2_PLACEMENT_3D ( 'NONE', #15195, #50141, #57412 ) ;
#54837 = CARTESIAN_POINT ( 'NONE',  ( 71.77848634863140376, 120.6499999999999915, -77.39114642429929347 ) ) ;
#54838 = EDGE_LOOP ( 'NONE', ( #30890, #7077, #37254, #63976 ) ) ;
#54839 = CARTESIAN_POINT ( 'NONE',  ( 98.19951187208806687, -40.85743130997450834, 256.6727681330542623 ) ) ;
#54840 = CARTESIAN_POINT ( 'NONE',  ( 117.8230732226064532, -34.08729308082334342, 160.0061014663869798 ) ) ;
#54841 = CARTESIAN_POINT ( 'NONE',  ( 107.0664832912739968, -36.72944715994100306, 287.6356252759109680 ) ) ;
#54842 = CARTESIAN_POINT ( 'NONE',  ( 20.56670390244828184, -48.82844715994187368, 300.4678068554150059 ) ) ;
#54843 = CARTESIAN_POINT ( 'NONE',  ( 98.30635682897023742, -28.74854496012902771, 76.73848241876795839 ) ) ;
#54844 = DIRECTION ( 'NONE',  ( -1.000000000000000078E-15, 1.000000000000000083E-30, 1.000000000000000000 ) ) ;
#54845 = EDGE_LOOP ( 'NONE', ( #673, #28999 ) ) ;
#54846 = VECTOR ( 'NONE', #30267, 1000.000000000000000 ) ;
#54847 = CARTESIAN_POINT ( 'NONE',  ( 99.09536660752770842, -30.55085998965113347, 115.8042979613130399 ) ) ;
#54848 = EDGE_CURVE ( 'NONE', #82011, #36180, #51236, .T. ) ;
#54849 = VECTOR ( 'NONE', #74282, 1000.000000000000000 ) ;
#54850 = LINE ( 'NONE', #41676, #8550 ) ;
#54851 = ORIENTED_EDGE ( 'NONE', *, *, #73105, .F. ) ;
#54852 = ADVANCED_FACE ( 'NONE', ( #40515 ), #34594, .T. ) ;
#54853 = CARTESIAN_POINT ( 'NONE',  ( 111.8298436232616240, -89.52844715994213232, -21.78219314458246103 ) ) ;
#54854 = CARTESIAN_POINT ( 'NONE',  ( 105.4788588808462038, 120.6499999999999915, -3.968749999999580336 ) ) ;
#54855 = CARTESIAN_POINT ( 'NONE',  ( 96.78489722101812731, -35.14273565208913652, 266.2041967044821149 ) ) ;
#54856 = FACE_OUTER_BOUND ( 'NONE', #37670, .T. ) ;
#54857 = DIRECTION ( 'NONE',  ( -1.087812297297669405E-15, 1.000000000000000000, -3.100000000000000044E-14 ) ) ;
#54858 = DIRECTION ( 'NONE',  ( 4.299999999999999979E-14, -1.000000000000000000, 0.000000000000000000 ) ) ;
#54859 = CARTESIAN_POINT ( 'NONE',  ( 100.8732324256648951, -44.32512360075851632, 12.03276813305398463 ) ) ;
#54861 = CARTESIAN_POINT ( 'NONE',  ( 101.6894933626720245, -27.09867346898214180, 101.4937205140059575 ) ) ;
#54860 = DIRECTION ( 'NONE',  ( 0.000000000000000000, 0.000000000000000000, 1.000000000000000000 ) ) ;
#54862 = CARTESIAN_POINT ( 'NONE',  ( 116.6018603435394141, -39.73108032723776972, 249.5838075904518121 ) ) ;
#54863 = CARTESIAN_POINT ( 'NONE',  ( 95.26177648276406273, -38.28579333248966776, 151.4299109901969871 ) ) ;
#54864 = CARTESIAN_POINT ( 'NONE',  ( 161.4809174648183898, -48.32844715993547879, 249.9678068554149490 ) ) ;
#54865 = VERTEX_POINT ( 'NONE', #979 ) ;
#54866 = AXIS2_PLACEMENT_3D ( 'NONE', #75887, #13657, #26387 ) ;
#54867 = CARTESIAN_POINT ( 'NONE',  ( 41.56648329127398966, -27.82844715994070484, 18.92562527591200094 ) ) ;
#54868 = CARTESIAN_POINT ( 'NONE',  ( 150.5667039024475571, -25.42844715993593852, 180.4678068554149775 ) ) ;
#54869 = DIRECTION ( 'NONE',  ( 0.1250000000000000278, 0.9921567416492215186, -3.035766082959410522E-14 ) ) ;
#54870 = ORIENTED_EDGE ( 'NONE', *, *, #89868, .T. ) ;
#54871 = CARTESIAN_POINT ( 'NONE',  ( 45.56670390244743629, -48.82844715994092866, 180.4678068554150911 ) ) ;
#54873 = ORIENTED_EDGE ( 'NONE', *, *, #26669, .F. ) ;
#54872 = CARTESIAN_POINT ( 'NONE',  ( 113.1024245609201984, -28.17526227570857955, 129.5870538473399449 ) ) ;
#54874 = DIRECTION ( 'NONE',  ( 0.000000000000000000, 0.000000000000000000, -1.000000000000000000 ) ) ;
#54875 = CARTESIAN_POINT ( 'NONE',  ( 89.95878776288157042, 70.27756284692560484, 94.61736061587697577 ) ) ;
#54876 = AXIS2_PLACEMENT_3D ( 'NONE', #20004, #34056, #80447 ) ;
#54877 = DIRECTION ( 'NONE',  ( -0.000000000000000000, -1.000000000000000000, -0.000000000000000000 ) ) ;
#54878 = AXIS2_PLACEMENT_3D ( 'NONE', #52440, #12942, #67890 ) ;
#54879 = DIRECTION ( 'NONE',  ( 0.000000000000000000, 0.000000000000000000, -1.000000000000000000 ) ) ;
#54880 = ORIENTED_EDGE ( 'NONE', *, *, #34190, .T. ) ;
#54881 = ITEM_DEFINED_TRANSFORMATION ( 'NONE', 'NONE', #7291,  #50656 ) ;
#54882 = EDGE_CURVE ( 'NONE', #88430, #2245, #62298, .T. ) ;
#54883 = ORIENTED_EDGE ( 'NONE', *, *, #3639, .T. ) ;
#54884 = ADVANCED_FACE ( 'NONE', ( #7348 ), #27782, .F. ) ;
#54885 = ORIENTED_EDGE ( 'NONE', *, *, #72075, .T. ) ;
#54886 = ADVANCED_FACE ( 'NONE', ( #523 ), #12088, .T. ) ;
#54887 = ORIENTED_EDGE ( 'NONE', *, *, #71521, .F. ) ;
#54888 = DIRECTION ( 'NONE',  ( 1.000000000000000000, 4.163336342344333240E-14, 0.000000000000000000 ) ) ;
#54889 = CARTESIAN_POINT ( 'NONE',  ( 96.20686424029936745, 93.94566094357729469, -88.25669247804565032 ) ) ;
#54890 = CARTESIAN_POINT ( 'NONE',  ( 167.2371591254542693, -47.82818131005522844, 300.4678068554149490 ) ) ;
#54891 = VECTOR ( 'NONE', #63393, 1000.000000000000000 ) ;
#54892 = EDGE_CURVE ( 'NONE', #36690, #2932, #10655, .T. ) ;
#54894 = CARTESIAN_POINT ( 'NONE',  ( 36.74138383868169910, -48.33240602328862678, 249.9678068554150343 ) ) ;
#54893 = PLANE ( 'NONE',  #33745 ) ;
#54895 = CARTESIAN_POINT ( 'NONE',  ( 64.67079002020506096, -0.9301828534102468682, 361.9756252759101471 ) ) ;
#54896 = ORIENTED_EDGE ( 'NONE', *, *, #24591, .T. ) ;
#54897 = VECTOR ( 'NONE', #59491, 1000.000000000000000 ) ;
#54899 = EDGE_LOOP ( 'NONE', ( #61212, #63604 ) ) ;
#54898 = CIRCLE ( 'NONE', #83932, 2.030000000002086580 ) ;
#54900 = DIRECTION ( 'NONE',  ( 1.387778780781444492E-15, 0.000000000000000000, -1.000000000000000000 ) ) ;
#54901 = DIRECTION ( 'NONE',  ( 0.000000000000000000, 1.000000000000000000, 0.000000000000000000 ) ) ;
#54902 = CARTESIAN_POINT ( 'NONE',  ( 106.8648936900573148, -47.09757847023101363, 223.5489586092439538 ) ) ;
#54903 = EDGE_CURVE ( 'NONE', #41003, #59850, #67198, .T. ) ;
#54904 = DIRECTION ( 'NONE',  ( 0.000000000000000000, 3.785359618865284342E-16, 1.000000000000000000 ) ) ;
#54905 = CARTESIAN_POINT ( 'NONE',  ( 98.70071965984716655, -42.85747980491196074, 102.8175300378149899 ) ) ;
#54906 = CARTESIAN_POINT ( 'NONE',  ( 165.3359832912740046, -36.32844715994100682, -5.074374724088000832 ) ) ;
#54907 = AXIS2_PLACEMENT_3D ( 'NONE', #80539, #45981, #73714 ) ;
#54908 = CARTESIAN_POINT ( 'NONE',  ( 179.4595971212889935, -28.98061976758940617, 193.9678068554150059 ) ) ;
#54909 = VERTEX_POINT ( 'NONE', #21431 ) ;
#54910 = DIRECTION ( 'NONE',  ( 0.000000000000000000, 1.000000000000000000, 1.914177628664063178E-15 ) ) ;
#54911 = CIRCLE ( 'NONE', #14379, 16.00000000000000000 ) ;
#54912 = EDGE_LOOP ( 'NONE', ( #2984, #63995 ) ) ;
#54913 = EDGE_LOOP ( 'NONE', ( #86834, #57166, #86360, #56146, #42033 ) ) ;
#54914 = DIRECTION ( 'NONE',  ( 0.4999999999999915623, -0.8660254037844433705, 0.000000000000000000 ) ) ;
#54915 = CARTESIAN_POINT ( 'NONE',  ( 105.3283384058428851, -27.49606390364131414, 276.6682499725636717 ) ) ;
#54916 = FACE_OUTER_BOUND ( 'NONE', #9169, .T. ) ;
#54917 = LINE ( 'NONE', #48108, #71149 ) ;
#54918 = CARTESIAN_POINT ( 'NONE',  ( 97.33784131412605234, -34.07106451907700517, 81.11479194169517370 ) ) ;
#54919 = AXIS2_PLACEMENT_3D ( 'NONE', #43470, #69860, #58011 ) ;
#54920 = CARTESIAN_POINT ( 'NONE',  ( 74.43377912862210621, 80.88465057165900873, -92.27764637677437065 ) ) ;
#54921 = ORIENTED_EDGE ( 'NONE', *, *, #79066, .T. ) ;
#54922 = CARTESIAN_POINT ( 'NONE',  ( -67.92268098368749918, 117.4749999999999943, 72.96458098368620426 ) ) ;
#54923 = CARTESIAN_POINT ( 'NONE',  ( 100.8869759769006578, -44.69981387740176615, 183.0527697648384731 ) ) ;
#54924 = ORIENTED_EDGE ( 'NONE', *, *, #23416, .F. ) ;
#54925 = CARTESIAN_POINT ( 'NONE',  ( 99.12728904495253346, -44.42023919799950704, 41.95086337114900488 ) ) ;
#54926 = ORIENTED_EDGE ( 'NONE', *, *, #57344, .F. ) ;
#54927 = CARTESIAN_POINT ( 'NONE',  ( 110.0622958990556839, -29.10660024649327227, 267.5966617981628701 ) ) ;
#54928 = CARTESIAN_POINT ( 'NONE',  ( 6.938893903907229955E-15, 50.79999999999999716, 216.0269999999999868 ) ) ;
#54929 = CARTESIAN_POINT ( 'NONE',  ( 113.7965574739370993, -44.62378898692907825, 153.1508633711499670 ) ) ;
#54930 = DIRECTION ( 'NONE',  ( 0.000000000000000000, -1.000000000000000000, 0.000000000000000000 ) ) ;
#54931 = FACE_OUTER_BOUND ( 'NONE', #9556, .T. ) ;
#54932 = FACE_OUTER_BOUND ( 'NONE', #39914, .T. ) ;
#54933 = CARTESIAN_POINT ( 'NONE',  ( 7.736379116599698236, 72.47620246569817937, 130.3265317108386512 ) ) ;
#54934 = VECTOR ( 'NONE', #55016, 1000.000000000000000 ) ;
#54935 = CARTESIAN_POINT ( 'NONE',  ( 106.9399153568602259, -47.82816235210678002, 228.5794347997199907 ) ) ;
#54936 = LINE ( 'NONE', #61324, #15199 ) ;
#54937 = EDGE_LOOP ( 'NONE', ( #36687, #61884, #81252, #23968 ) ) ;
#54938 = EDGE_LOOP ( 'NONE', ( #83541, #50590, #5777, #38544 ) ) ;
#54939 = CARTESIAN_POINT ( 'NONE',  ( 116.5728860035299164, -32.34523831224304047, 100.1699109901969535 ) ) ;
#54940 = CARTESIAN_POINT ( 'NONE',  ( 119.7018510303924756, 50.62094380000917937, -52.11861110539391717 ) ) ;
#54941 = ADVANCED_FACE ( 'NONE', ( #7792 ), #40958, .T. ) ;
#54942 = ORIENTED_EDGE ( 'NONE', *, *, #47930, .T. ) ;
#54943 = ORIENTED_EDGE ( 'NONE', *, *, #38610, .T. ) ;
#54944 = EDGE_LOOP ( 'NONE', ( #79270, #67000, #84352, #17628 ) ) ;
#54945 = CARTESIAN_POINT ( 'NONE',  ( 113.2433956935260113, -28.75706466399002537, 159.5522588191168154 ) ) ;
#54946 = DIRECTION ( 'NONE',  ( 0.000000000000000000, 0.000000000000000000, 1.000000000000000000 ) ) ;
#54947 = DIRECTION ( 'NONE',  ( 0.000000000000000000, 1.000000000000000000, 0.000000000000000000 ) ) ;
#54948 = PLANE ( 'NONE',  #34476 ) ;
#54949 = CARTESIAN_POINT ( 'NONE',  ( 115.0870346033256055, -35.21269407640084381, 156.7938046553059905 ) ) ;
#54950 = CARTESIAN_POINT ( 'NONE',  ( 112.5006845157638651, -46.38111348219169372, 253.9965776568635647 ) ) ;
#54951 = CYLINDRICAL_SURFACE ( 'NONE', #66785, 2.750000000000002665 ) ;
#54952 = EDGE_LOOP ( 'NONE', ( #22108, #58307 ) ) ;
#54953 = CYLINDRICAL_SURFACE ( 'NONE', #6476, 4.762500000000002842 ) ;
#54954 = CARTESIAN_POINT ( 'NONE',  ( 76.20505178924339873, 127.0000000000000000, 76.20505178924419454 ) ) ;
#54955 = ORIENTED_EDGE ( 'NONE', *, *, #16374, .F. ) ;
#54956 = VERTEX_POINT ( 'NONE', #77741 ) ;
#54957 = CIRCLE ( 'NONE', #62249, 32.50000000000000711 ) ;
#54958 = VECTOR ( 'NONE', #74304, 1000.000000000000000 ) ;
#54959 = ADVANCED_FACE ( 'NONE', ( #29578, #85467 ), #15515, .T. ) ;
#54960 = DIRECTION ( 'NONE',  ( 0.000000000000000000, 0.000000000000000000, -1.000000000000000000 ) ) ;
#54961 = ORIENTED_EDGE ( 'NONE', *, *, #11778, .T. ) ;
#54962 = ORIENTED_EDGE ( 'NONE', *, *, #29187, .T. ) ;
#54963 = CARTESIAN_POINT ( 'NONE',  ( 63.03715912545637678, -24.42818131006026761, 193.9678068554150911 ) ) ;
#54964 = CARTESIAN_POINT ( 'NONE',  ( 97.39131799614082752, -39.27861749894243815, 16.53146768276753420 ) ) ;
#54965 = DIRECTION ( 'NONE',  ( 0.000000000000000000, 1.000000000000000000, -0.000000000000000000 ) ) ;
#54966 = CARTESIAN_POINT ( 'NONE',  ( 125.0235919798090833, -56.62589376934762697, 14.92562527591091204 ) ) ;
#54967 = CARTESIAN_POINT ( 'NONE',  ( 102.9027671602101037, -44.22047980607887752, 186.5952769709339805 ) ) ;
#54968 = CARTESIAN_POINT ( 'NONE',  ( 105.9838489277333480, -26.31625509990853828, 50.15848241876796720 ) ) ;
#54969 = LINE ( 'NONE', #41799, #55288 ) ;
#54970 = ORIENTED_EDGE ( 'NONE', *, *, #10817, .F. ) ;
#54971 = AXIS2_PLACEMENT_3D ( 'NONE', #61924, #68754, #12447 ) ;
#54972 = CARTESIAN_POINT ( 'NONE',  ( -78.43243611888087230, 72.22378176823139029, -88.90442867305952745 ) ) ;
#54973 = ORIENTED_EDGE ( 'NONE', *, *, #449, .T. ) ;
#54974 = CARTESIAN_POINT ( 'NONE',  ( 127.0667052882549797, -71.37844715994091871, 222.2178068554179902 ) ) ;
#54975 = EDGE_LOOP ( 'NONE', ( #16534, #35640, #43651, #83939 ) ) ;
#54976 = LINE ( 'NONE', #28186, #50837 ) ;
#54977 = DIRECTION ( 'NONE',  ( 0.000000000000000000, 0.000000000000000000, -1.000000000000000000 ) ) ;
#54978 = CARTESIAN_POINT ( 'NONE',  ( 115.9858208431400044, -41.32354544834976906, 133.4481121647361306 ) ) ;
#54979 = LINE ( 'NONE', #83189, #13277 ) ;
#54980 = ORIENTED_EDGE ( 'NONE', *, *, #7536, .T. ) ;
#54981 = CARTESIAN_POINT ( 'NONE',  ( 97.26762016986505444, -33.10609988230974920, 66.04419670448297097 ) ) ;
#54982 = FILL_AREA_STYLE_COLOUR ( '', #8667 ) ;
#54984 = CARTESIAN_POINT ( 'NONE',  ( 83.15068351451354545, 79.66695435136418268, -100.6520717229715842 ) ) ;
#54983 = CARTESIAN_POINT ( 'NONE',  ( 115.8250108040429467, -31.72928582533900865, 164.2398587763299531 ) ) ;
#54985 = PLANE ( 'NONE',  #81495 ) ;
#54986 = DIRECTION ( 'NONE',  ( 1.000000000000000078E-15, -1.000000000000000000, 0.000000000000000000 ) ) ;
#54987 = VERTEX_POINT ( 'NONE', #8245 ) ;
#54988 = ADVANCED_FACE ( 'NONE', ( #23244 ), #43642, .T. ) ;
#54989 = CIRCLE ( 'NONE', #66624, 1.000000000000000888 ) ;
#54990 = ADVANCED_FACE ( 'NONE', ( #77286 ), #70476, .T. ) ;
#54991 = DIRECTION ( 'NONE',  ( 0.000000000000000000, 0.000000000000000000, 1.000000000000000000 ) ) ;
#54992 = ADVANCED_FACE ( 'NONE', ( #51340 ), #43190, .T. ) ;
#54993 = LINE ( 'NONE', #82761, #9580 ) ;
#54994 = CARTESIAN_POINT ( 'NONE',  ( 6.720192613126054759, 71.76561204655834558, 118.3658933525135524 ) ) ;
#54995 = ORIENTED_EDGE ( 'NONE', *, *, #37415, .T. ) ;
#54996 = CARTESIAN_POINT ( 'NONE',  ( 96.01268936646508223, -41.06948063400285776, 92.62419670448296927 ) ) ;
#54997 = EDGE_CURVE ( 'NONE', #33634, #61676, #30477, .T. ) ;
#54999 = CYLINDRICAL_SURFACE ( 'NONE', #7931, 25.39999999999999858 ) ;
#54998 = DIRECTION ( 'NONE',  ( 1.000000000000000078E-15, -1.000000000000000000, 0.000000000000000000 ) ) ;
#55000 = CARTESIAN_POINT ( 'NONE',  ( 163.0667039024470171, -33.35206098992711077, -5.074374724088000832 ) ) ;
#55001 = AXIS2_PLACEMENT_3D ( 'NONE', #49234, #29268, #84694 ) ;
#55002 = CYLINDRICAL_SURFACE ( 'NONE', #4158, 1.000000000000000888 ) ;
#55003 = ORIENTED_EDGE ( 'NONE', *, *, #42514, .F. ) ;
#55004 = CARTESIAN_POINT ( 'NONE',  ( 116.5944731948637809, -42.45914096480943556, 124.3956252759109731 ) ) ;
#55005 = EDGE_CURVE ( 'NONE', #79094, #35450, #35942, .T. ) ;
#55007 = VERTEX_POINT ( 'NONE', #84112 ) ;
#55006 = CARTESIAN_POINT ( 'NONE',  ( 130.3998166246059895, 12.92155284005730387, 355.9756252759109998 ) ) ;
#55008 = VECTOR ( 'NONE', #80212, 1000.000000000000000 ) ;
#55009 = CARTESIAN_POINT ( 'NONE',  ( 106.8369185487093063, -47.13021470646864941, 268.5584824187679374 ) ) ;
#55010 = CARTESIAN_POINT ( 'NONE',  ( 97.83847648579691736, -40.58231914350135838, 252.6411887015405000 ) ) ;
#55011 = CARTESIAN_POINT ( 'NONE',  ( 1.387778780781445676E-14, 238.5000000000000000, 97.27542076772557778 ) ) ;
#55012 = ADVANCED_FACE ( 'NONE', ( #56819, #71818, #42736, #1438 ), #63656, .F. ) ;
#55013 = DIRECTION ( 'NONE',  ( -2.900000000000000265E-14, 2.000000000000000155E-15, -1.000000000000000000 ) ) ;
#55014 = CARTESIAN_POINT ( 'NONE',  ( 97.06107109349493101, -37.99641193259417093, 82.42729194011009497 ) ) ;
#55015 = AXIS2_PLACEMENT_3D ( 'NONE', #73668, #11451, #32320 ) ;
#55016 = DIRECTION ( 'NONE',  ( -0.000000000000000000, -0.000000000000000000, -1.000000000000000000 ) ) ;
#55017 = CARTESIAN_POINT ( 'NONE',  ( 1.166476076187854022E-15, 95.00619999999999266, 9.525000000000000355 ) ) ;
#55018 = CARTESIAN_POINT ( 'NONE',  ( 101.7740290765682403, -45.64733444449330335, 207.1622919425779514 ) ) ;
#55019 = EDGE_LOOP ( 'NONE', ( #33033, #36431, #70353, #62602 ) ) ;
#55020 = ORIENTED_EDGE ( 'NONE', *, *, #29907, .T. ) ;
#55021 = AXIS2_PLACEMENT_3D ( 'NONE', #5863, #83069, #61250 ) ;
#55022 = CARTESIAN_POINT ( 'NONE',  ( 107.5650335644346569, -45.56823575777373492, 149.0530118773259858 ) ) ;
#55023 = VECTOR ( 'NONE', #27486, 1000.000000000000000 ) ;
#55024 = DIRECTION ( 'NONE',  ( -4.237773401492740281E-14, 1.000000000000000000, 0.000000000000000000 ) ) ;
#55026 = CARTESIAN_POINT ( 'NONE',  ( 97.80782663584228942, -40.50797902753792101, 57.63481331718827505 ) ) ;
#55025 = CARTESIAN_POINT ( 'NONE',  ( 111.3597915011938539, -28.37217101237177985, 16.14253568684992501 ) ) ;
#55027 = DIRECTION ( 'NONE',  ( -0.7071067811865753283, 0.7071067811865197061, -7.071067811865760309E-16 ) ) ;
#55028 = B_SPLINE_CURVE_WITH_KNOTS ( 'NONE', 3,
 ( #72243, #15040, #51321, #21865, #42714, #2762, #3205, #30459, #30899, #84092, #70456, #8228, #35918, #63633, #84550, #11344, #87654, #3637 ),
 .UNSPECIFIED., .F., .F.,
 ( 4, 2, 2, 2, 2, 2, 2, 2, 4 ),
 ( 0.4999949742048476198, 0.5624956024292416812, 0.6249962306536357426, 0.6874968588780296930, 0.7499974871024237544, 0.8124981153268178158, 0.8749987435512118772, 0.9374993717756059386, 1.000000000000000000 ),
 .UNSPECIFIED. ) ;
#55029 = CARTESIAN_POINT ( 'NONE',  ( -26.31381232569119533, 175.6861876743088260, 113.8826257785461280 ) ) ;
#55030 = AXIS2_PLACEMENT_3D ( 'NONE', #83436, #48884, #76623 ) ;
#55031 = DIRECTION ( 'NONE',  ( 0.000000000000000000, 0.000000000000000000, -1.000000000000000000 ) ) ;
#55032 = CARTESIAN_POINT ( 'NONE',  ( 97.33784130911575971, -34.07106453693553760, 107.1147919431604834 ) ) ;
#55033 = DIRECTION ( 'NONE',  ( 3.100000000000000258E-29, -3.100000000000000044E-14, -1.000000000000000000 ) ) ;
#55035 = CARTESIAN_POINT ( 'NONE',  ( 96.21411768969875311, -32.03111041547175120, 211.0013395616249738 ) ) ;
#55034 = STYLED_ITEM ( 'NONE', ( #29559 ), #56477 ) ;
#55036 = CARTESIAN_POINT ( 'NONE',  ( 51.56670390244699576, -19.82844715994031048, 342.9256252759119548 ) ) ;
#55037 = ORIENTED_EDGE ( 'NONE', *, *, #64656, .T. ) ;
#55038 = VERTEX_POINT ( 'NONE', #36843 ) ;
#55039 = LINE ( 'NONE', #20564, #64866 ) ;
#55040 = CARTESIAN_POINT ( 'NONE',  ( 78.21890182792367341, -16.68450975841368233, 2.186797062523622159 ) ) ;
#55041 = AXIS2_PLACEMENT_3D ( 'NONE', #16338, #49940, #8181 ) ;
#55042 = FACE_OUTER_BOUND ( 'NONE', #70828, .T. ) ;
#55043 = CARTESIAN_POINT ( 'NONE',  ( -47.05895527891580343, 65.62929404919808007, 108.8162712210547056 ) ) ;
#55044 = EDGE_CURVE ( 'NONE', #8645, #21680, #8706, .T. ) ;
#55045 = CARTESIAN_POINT ( 'NONE',  ( 107.0664832912739399, -36.72944715994095333, 293.9356252759109793 ) ) ;
#55046 = EDGE_LOOP ( 'NONE', ( #5252, #64423, #20786, #69477 ) ) ;
#55047 = DIRECTION ( 'NONE',  ( -0.000000000000000000, 1.000000000000000000, -0.000000000000000000 ) ) ;
#55048 = VECTOR ( 'NONE', #38723, 1000.000000000000114 ) ;
#55049 = EDGE_CURVE ( 'NONE', #66156, #46554, #16406, .T. ) ;
#55050 = CARTESIAN_POINT ( 'NONE',  ( 99.39677155223240845, -28.76988628678374837, 265.6746728949588032 ) ) ;
#55051 = ORIENTED_EDGE ( 'NONE', *, *, #13213, .F. ) ;
#55052 = VECTOR ( 'NONE', #17143, 1000.000000000000000 ) ;
#55053 = CARTESIAN_POINT ( 'NONE',  ( -4.052637573187175768, 94.48764834648464728, 118.4873761436849691 ) ) ;
#55054 = PLANE ( 'NONE',  #66010 ) ;
#55055 = CARTESIAN_POINT ( 'NONE',  ( 110.8627678800837657, -45.98083881433460363, 167.8863385848088399 ) ) ;
#55056 = CARTESIAN_POINT ( 'NONE',  ( 100.0434009169665757, -32.56939427797095021, 83.71951894101997027 ) ) ;
#55057 = CARTESIAN_POINT ( 'NONE',  ( 104.5573670441197720, -48.33662538491821437, 178.4070538473399665 ) ) ;
#55058 = CARTESIAN_POINT ( 'NONE',  ( 173.8164832912740394, 12.92155284005802685, 336.5756252759111362 ) ) ;
#55059 = VERTEX_POINT ( 'NONE', #36407 ) ;
#55060 = CARTESIAN_POINT ( 'NONE',  ( 6.938893903907229955E-15, 50.79999999999999716, 216.0269999999999868 ) ) ;
#55061 = AXIS2_PLACEMENT_3D ( 'NONE', #89598, #82797, #35501 ) ;
#55062 = ORIENTED_EDGE ( 'NONE', *, *, #67127, .F. ) ;
#55063 = ORIENTED_EDGE ( 'NONE', *, *, #5444, .T. ) ;
#55064 = EDGE_CURVE ( 'NONE', #38655, #41295, #2333, .T. ) ;
#55065 = LINE ( 'NONE', #48256, #70590 ) ;
#55066 = ORIENTED_EDGE ( 'NONE', *, *, #79635, .T. ) ;
#55067 = ORIENTED_EDGE ( 'NONE', *, *, #41464, .T. ) ;
#55068 = CARTESIAN_POINT ( 'NONE',  ( 73.06670390244801183, -58.35344715994099829, 310.9178068554150514 ) ) ;
#55069 = CARTESIAN_POINT ( 'NONE',  ( 112.6295607727957133, -43.21082823627408231, 107.5638483995059715 ) ) ;
#55070 = CARTESIAN_POINT ( 'NONE',  ( 113.1129168750088638, -46.01039980791943407, 223.0480062282919675 ) ) ;
#55071 = VECTOR ( 'NONE', #32359, 1000.000000000000000 ) ;
#55072 = CARTESIAN_POINT ( 'NONE',  ( 117.1759530674219860, -34.27439392744687296, 209.0156252759109634 ) ) ;
#55074 = CARTESIAN_POINT ( 'NONE',  ( 97.50674219252222485, -32.62548708300533207, 12.00419670448293985 ) ) ;
#55073 = DIRECTION ( 'NONE',  ( -0.4999999999999941158, 0.8660254037844420383, 0.000000000000000000 ) ) ;
#55075 = DIRECTION ( 'NONE',  ( 1.000000000000000078E-15, 1.000000000000000083E-30, -1.000000000000000000 ) ) ;
#55076 = CYLINDRICAL_SURFACE ( 'NONE', #88845, 8.928100000000000591 ) ;
#55077 = ADVANCED_FACE ( 'NONE', ( #44083, #37289 ), #64110, .T. ) ;
#55078 = ORIENTED_EDGE ( 'NONE', *, *, #16864, .F. ) ;
#55079 = AXIS2_PLACEMENT_3D ( 'NONE', #43709, #15583, #70997 ) ;
#55080 = CARTESIAN_POINT ( 'NONE',  ( 114.6661721138975025, -42.88640786233948887, 88.28419670448295165 ) ) ;
#55081 = CARTESIAN_POINT ( 'NONE',  ( 101.0407447616467351, -27.40725005837418138, 70.54514908543497143 ) ) ;
#55082 = CARTESIAN_POINT ( 'NONE',  ( 96.97388998173752839, -33.94624283173551049, 251.1127681330538337 ) ) ;
#55083 = VERTEX_POINT ( 'NONE', #64997 ) ;
#55084 = CARTESIAN_POINT ( 'NONE',  ( 98.94247553594858857, -30.19587780982054070, 240.7870538473399620 ) ) ;
#55085 = DIRECTION ( 'NONE',  ( 1.000000000000000000, 0.000000000000000000, 0.000000000000000000 ) ) ;
#55086 = SURFACE_STYLE_FILL_AREA ( #33778 ) ;
#55087 = EDGE_CURVE ( 'NONE', #83503, #81882, #72264, .T. ) ;
#55088 = DIRECTION ( 'NONE',  ( 0.000000000000000000, 0.000000000000000000, 1.000000000000000000 ) ) ;
#55089 = LINE ( 'NONE', #76013, #23904 ) ;
#55090 = B_SPLINE_CURVE_WITH_KNOTS ( 'NONE', 3,
 ( #62749, #50009, #29580, #50458, #36409, #42738, #525, #63658, #22783, #83216, #981, #63204, #8708, #56374, #20981, #7794, #84114, #14165 ),
 .UNSPECIFIED., .F., .F.,
 ( 4, 2, 2, 2, 2, 2, 2, 2, 4 ),
 ( 0.000000000000000000, 0.1250000000000000000, 0.2500000000000000000, 0.3750000000000000000, 0.5000000000000000000, 0.6250000000000000000, 0.7500000000000000000, 0.8750000000000000000, 1.000000000000000000 ),
 .UNSPECIFIED. ) ;
#55092 = DIRECTION ( 'NONE',  ( 0.000000000000000000, 0.000000000000000000, -1.000000000000000000 ) ) ;
#55091 = CARTESIAN_POINT ( 'NONE',  ( 181.8884939055940038, -32.11662333284530746, -5.074374724088000832 ) ) ;
#55093 = FACE_OUTER_BOUND ( 'NONE', #53079, .T. ) ;
#55094 = CYLINDRICAL_SURFACE ( 'NONE', #88917, 218.1859999999999786 ) ;
#55095 = CARTESIAN_POINT ( 'NONE',  ( 107.0664832912739399, -36.72944715994095333, 293.6356252759106837 ) ) ;
#55096 = AXIS2_PLACEMENT_3D ( 'NONE', #56871, #35989, #15563 ) ;
#55097 = LINE ( 'NONE', #39697, #39930 ) ;
#55098 = CARTESIAN_POINT ( 'NONE',  ( 98.41530666024773666, -31.56922914487509502, 277.3301547344686355 ) ) ;
#55099 = CARTESIAN_POINT ( 'NONE',  ( 97.07187113119439914, -35.38041075382983536, 41.21846444838222823 ) ) ;
#55100 = EDGE_CURVE ( 'NONE', #61174, #52592, #78202, .T. ) ;
#55101 = DIRECTION ( 'NONE',  ( -0.5000000000000008882, 0.8660254037844382635, -2.684678751731760294E-14 ) ) ;
#55103 = ORIENTED_EDGE ( 'NONE', *, *, #87131, .T. ) ;
#55102 = CARTESIAN_POINT ( 'NONE',  ( 107.0667039024469886, -67.87844715994094713, 93.21780685541800437 ) ) ;
#55104 = DIRECTION ( 'NONE',  ( 0.000000000000000000, 1.000000000000000000, 0.000000000000000000 ) ) ;
#55105 = CARTESIAN_POINT ( 'NONE',  ( 106.2251211966456879, -47.77424462129209815, 267.5280062282920994 ) ) ;
#55106 = CARTESIAN_POINT ( 'NONE',  ( 95.67524734051724522, -33.46228404877688689, 137.1041967044819501 ) ) ;
#55107 = CARTESIAN_POINT ( 'NONE',  ( 103.9262362324350590, -26.74286475366834281, 246.3184824187679567 ) ) ;
#55108 = AXIS2_PLACEMENT_3D ( 'NONE', #52184, #19485, #47168 ) ;
#55109 = DIRECTION ( 'NONE',  ( 0.000000000000000000, 0.000000000000000000, -1.000000000000000000 ) ) ;
#55110 = DIRECTION ( 'NONE',  ( 0.000000000000000000, 0.000000000000000000, 1.000000000000000000 ) ) ;
#55111 = CARTESIAN_POINT ( 'NONE',  ( -110.7653435595065901, 44.45000000000000284, 69.10794311903988785 ) ) ;
#55112 = CARTESIAN_POINT ( 'NONE',  ( -105.4788588808464027, 127.0000000000000000, 3.968749999998844924 ) ) ;
#55113 = ORIENTED_EDGE ( 'NONE', *, *, #43647, .T. ) ;
#55114 = LINE ( 'NONE', #28322, #82448 ) ;
#55115 = ORIENTED_EDGE ( 'NONE', *, *, #13693, .T. ) ;
#55116 = VECTOR ( 'NONE', #81955, 1000.000000000000000 ) ;
#55117 = CARTESIAN_POINT ( 'NONE',  ( 99.37165735872611094, -40.43697808898449608, 171.1067055423629597 ) ) ;
#55118 = EDGE_CURVE ( 'NONE', #68275, #63748, #44527, .T. ) ;
#55120 = ORIENTED_EDGE ( 'NONE', *, *, #34231, .T. ) ;
#55119 = LINE ( 'NONE', #1544, #79096 ) ;
#55121 = DIRECTION ( 'NONE',  ( -0.0001713722456133601202, 0.9999999853157766072, 1.713722456133601401E-19 ) ) ;
#55122 = CARTESIAN_POINT ( 'NONE',  ( 102.6926969729870507, -27.29023857175978662, 176.4213395616249898 ) ) ;
#55123 = CARTESIAN_POINT ( 'NONE',  ( 63.03715912545740707, -46.82818131006016671, 129.9678068554150911 ) ) ;
#55124 = EDGE_CURVE ( 'NONE', #40542, #77354, #75282, .T. ) ;
#55125 = CARTESIAN_POINT ( 'NONE',  ( 182.0667039024477276, -33.35206098992059509, 237.4678068554150059 ) ) ;
#55126 = CARTESIAN_POINT ( 'NONE',  ( 112.8675307907708287, -28.58609239232746546, 195.5838076129389833 ) ) ;
#55127 = CARTESIAN_POINT ( 'NONE',  ( -44.45000000000000284, 101.5999999999999943, 206.3750000000000000 ) ) ;
#55128 = CARTESIAN_POINT ( 'NONE',  ( 114.2351621074132879, -44.22269940884951467, 113.1718157521019776 ) ) ;
#55129 = VERTEX_POINT ( 'NONE', #33485 ) ;
#55130 = AXIS2_PLACEMENT_3D ( 'NONE', #22348, #17316, #15982 ) ;
#55131 = VERTEX_POINT ( 'NONE', #12155 ) ;
#55132 = ORIENTED_EDGE ( 'NONE', *, *, #38990, .T. ) ;
#55133 = DIRECTION ( 'NONE',  ( 1.000000000000000000, 0.000000000000000000, 0.000000000000000000 ) ) ;
#55135 = CARTESIAN_POINT ( 'NONE',  ( 138.8167039024479834, -57.40094715994099772, 86.31780685541500020 ) ) ;
#55134 = CARTESIAN_POINT ( 'NONE',  ( 99.18511857479145988, -30.88155312011797804, 176.8184824187669619 ) ) ;
#55136 = FACE_OUTER_BOUND ( 'NONE', #41214, .T. ) ;
#55137 = DIRECTION ( 'NONE',  ( -4.237773401492740281E-14, 1.000000000000000000, 0.000000000000000000 ) ) ;
#55138 = DIRECTION ( 'NONE',  ( 0.000000000000000000, 1.000000000000000000, -0.000000000000000000 ) ) ;
#55139 = AXIS2_PLACEMENT_3D ( 'NONE', #31709, #4907, #47111 ) ;
#55140 = CARTESIAN_POINT ( 'NONE',  ( 144.0667039024470739, -140.6784471599409017, 55.21780685541800437 ) ) ;
#55141 = CARTESIAN_POINT ( 'NONE',  ( 67.06928294555038406, -67.88014341905780213, 245.5936337082227681 ) ) ;
#55142 = CARTESIAN_POINT ( 'NONE',  ( 109.5033840998384136, -46.84330794493983774, 132.7641967044819751 ) ) ;
#55143 = ORIENTED_EDGE ( 'NONE', *, *, #31574, .F. ) ;
#55144 = ORIENTED_EDGE ( 'NONE', *, *, #35121, .F. ) ;
#55145 = EDGE_LOOP ( 'NONE', ( #38077, #85561, #58051, #10141, #57162, #73069 ) ) ;
#55146 = AXIS2_PLACEMENT_3D ( 'NONE', #71912, #9672, #17384 ) ;
#55147 = DIRECTION ( 'NONE',  ( 1.000000000000000078E-15, 0.000000000000000000, -1.000000000000000000 ) ) ;
#55148 = CARTESIAN_POINT ( 'NONE',  ( -82.91466710319176059, 83.38002811471483255, -100.8465607796068184 ) ) ;
#55149 = CARTESIAN_POINT ( 'NONE',  ( 86.06670390244804025, -16.72944715994094622, 239.5838068554176346 ) ) ;
#55150 = CARTESIAN_POINT ( 'NONE',  ( 115.2023469127646820, -39.68048904007974897, 171.3557094172109885 ) ) ;
#55151 = AXIS2_PLACEMENT_3D ( 'NONE', #30451, #77708, #15490 ) ;
#55152 = EDGE_CURVE ( 'NONE', #17076, #43582, #59922, .T. ) ;
#55153 = CARTESIAN_POINT ( 'NONE',  ( 99.09599905102065520, -30.55004517099500561, 26.80180474063285345 ) ) ;
#55154 = EDGE_LOOP ( 'NONE', ( #44713, #52445, #59473, #42518 ) ) ;
#55156 = ORIENTED_EDGE ( 'NONE', *, *, #26310, .F. ) ;
#55155 = VERTEX_POINT ( 'NONE', #88915 ) ;
#55157 = VECTOR ( 'NONE', #64051, 1000.000000000000000 ) ;
#55158 = DIRECTION ( 'NONE',  ( 0.4808135048159887792, 0.02029144519433677407, -0.8765880622267739897 ) ) ;
#55159 = ORIENTED_EDGE ( 'NONE', *, *, #17970, .T. ) ;
#55160 = ORIENTED_EDGE ( 'NONE', *, *, #82620, .F. ) ;
#55161 = LINE ( 'NONE', #21131, #34758 ) ;
#55162 = CARTESIAN_POINT ( 'NONE',  ( 116.3948728625927060, -35.60798670905003860, 235.3653928297059679 ) ) ;
#55163 = EDGE_LOOP ( 'NONE', ( #83221, #36993, #75389, #81711, #79992 ) ) ;
#55164 = B_SPLINE_CURVE_WITH_KNOTS ( 'NONE', 3,
 ( #89244, #80201, #59718, #87451, #18391, #81104, #46534, #39726, #5225, #32915, #60614, #48313, #76046, #62858, #75615, #63775, #82442, #35601, #83776, #634, #27896, #63318, #56488, #34711, #76951, #1094, #42849, #41071, #56027, #20204, #14735, #28333, #61960, #13825, #14282, #42406, #22002, #47875, #21091, #41509, #6560, #70133, #13384, #68793, #7902, #34259, #89697, #28806 ),
 .UNSPECIFIED., .F., .F.,
 ( 4, 2, 2, 2, 2, 2, 2, 2, 2, 1, 2, 2, 2, 2, 2, 2, 2, 2, 2, 2, 2, 1, 2, 2, 4 ),
 ( 0.05960646776571128236, 0.06208927922045071740, 0.06333068494782043145, 0.06457209067519015244, 0.06705490212992962218, 0.06829630785729937092, 0.06953771358466910579, 0.07202052503940861716, 0.07326193076677835203, 0.07450333649414807302, 0.07574474222151779401, 0.07698614794888751500, 0.07946895940362699862, 0.08195177085836648223, 0.08319317658573623098, 0.08443458231310599360, 0.08691739376784550497, 0.08815879949521525372, 0.08940020522258501634, 0.09188301667732445832, 0.09312442240469415156, 0.09436582813206384479, 0.09560723385943353803, 0.09684863958680323126, 0.09933145104154257610 ),
 .UNSPECIFIED. ) ;
#55165 = DIRECTION ( 'NONE',  ( 1.000000000000000000, -9.073094938289460781E-13, 0.000000000000000000 ) ) ;
#55166 = CARTESIAN_POINT ( 'NONE',  ( -119.0649508995676626, 74.44429733102370506, 53.56549206838347743 ) ) ;
#55167 = ORIENTED_EDGE ( 'NONE', *, *, #40278, .F. ) ;
#55168 = ORIENTED_EDGE ( 'NONE', *, *, #19166, .F. ) ;
#55169 = EDGE_CURVE ( 'NONE', #78995, #4807, #60285, .T. ) ;
#55170 = DIRECTION ( 'NONE',  ( -1.000000000000000078E-15, 1.000000000000000083E-30, 1.000000000000000000 ) ) ;
#55171 = ORIENTED_EDGE ( 'NONE', *, *, #20397, .T. ) ;
#55172 = ORIENTED_EDGE ( 'NONE', *, *, #15660, .F. ) ;
#55173 = EDGE_CURVE ( 'NONE', #22477, #2950, #7810, .T. ) ;
#55174 = VECTOR ( 'NONE', #40879, 1000.000000000000000 ) ;
#55175 = CARTESIAN_POINT ( 'NONE',  ( 101.6421866332951396, -42.82917926744636361, 264.8166617981626700 ) ) ;
#55176 = EDGE_CURVE ( 'NONE', #73698, #82549, #58570, .T. ) ;
#55177 = CARTESIAN_POINT ( 'NONE',  ( 107.3345184958865275, -26.28557234761613159, 120.0556252759109555 ) ) ;
#55178 = AXIS2_PLACEMENT_3D ( 'NONE', #89231, #5207, #53771 ) ;
#55179 = CARTESIAN_POINT ( 'NONE',  ( 108.0321269276242049, -25.74166508409281917, 109.9946728949589811 ) ) ;
#55180 = CARTESIAN_POINT ( 'NONE',  ( 103.0103351263445859, -43.74012547698517750, 249.5838068554171514 ) ) ;
#55181 = CARTESIAN_POINT ( 'NONE',  ( 132.2214349158033713, -16.68812225916125058, 7.662832107305504792 ) ) ;
#55182 = CARTESIAN_POINT ( 'NONE',  ( 97.42522746746806206, -42.13501527293522742, 177.7451490854349743 ) ) ;
#55183 = DIRECTION ( 'NONE',  ( -1.000000000000000000, 0.000000000000000000, 0.000000000000000000 ) ) ;
#55184 = CARTESIAN_POINT ( 'NONE',  ( 142.8687636814963184, 5.654319119531167281, 394.9756252759100903 ) ) ;
#55185 = ORIENTED_EDGE ( 'NONE', *, *, #68062, .F. ) ;
#55186 = CARTESIAN_POINT ( 'NONE',  ( 130.0575199856853885, 76.93632333215538210, 11.39952500586094253 ) ) ;
#55188 = ORIENTED_EDGE ( 'NONE', *, *, #873, .F. ) ;
#55187 = EDGE_CURVE ( 'NONE', #66271, #27158, #68912, .T. ) ;
#55189 = EDGE_CURVE ( 'NONE', #25661, #47060, #88015, .T. ) ;
#55190 = VERTEX_POINT ( 'NONE', #68011 ) ;
#55191 = LINE ( 'NONE', #49741, #43141 ) ;
#55193 = ORIENTED_EDGE ( 'NONE', *, *, #34695, .T. ) ;
#55192 = VECTOR ( 'NONE', #8155, 999.9999999999998863 ) ;
#55194 = EDGE_CURVE ( 'NONE', #75223, #32339, #74528, .T. ) ;
#55195 = EDGE_CURVE ( 'NONE', #82764, #14401, #47551, .T. ) ;
#55196 = DIRECTION ( 'NONE',  ( -1.000000000000000078E-15, 1.000000000000000083E-30, 1.000000000000000000 ) ) ;
#55197 = CARTESIAN_POINT ( 'NONE',  ( 116.7957173713512873, -32.98391181527420457, 139.1184824187679396 ) ) ;
#55198 = CARTESIAN_POINT ( 'NONE',  ( -5.566352093571659942, 71.12725780905140027, 130.4377547077455688 ) ) ;
#55199 = EDGE_CURVE ( 'NONE', #48508, #71603, #60731, .T. ) ;
#55200 = CARTESIAN_POINT ( 'NONE',  ( 136.8118108218990869, -36.54506369575593538, 6.756870620000529293 ) ) ;
#55201 = FACE_OUTER_BOUND ( 'NONE', #30210, .T. ) ;
#55204 = CARTESIAN_POINT ( 'NONE',  ( 114.7977927517517855, -29.71579763117551565, 205.4127681330539872 ) ) ;
#55203 = DIRECTION ( 'NONE',  ( -3.100000000000000258E-29, 3.100000000000000044E-14, 1.000000000000000000 ) ) ;
#55202 = DIRECTION ( 'NONE',  ( 0.000000000000000000, 0.000000000000000000, -1.000000000000000000 ) ) ;
#55205 = CARTESIAN_POINT ( 'NONE',  ( 194.5667039024479834, -48.82844715994099971, 20.91780685541479912 ) ) ;
#55206 = CYLINDRICAL_SURFACE ( 'NONE', #39499, 5.600000000000000533 ) ;
#55207 = ORIENTED_EDGE ( 'NONE', *, *, #61295, .F. ) ;
#55208 = LINE ( 'NONE', #13907, #45424 ) ;
#55209 = EDGE_CURVE ( 'NONE', #16685, #89473, #3468, .T. ) ;
#55210 = CARTESIAN_POINT ( 'NONE',  ( 177.4809174648215162, -48.32844715993478246, 180.4678068554150059 ) ) ;
#55211 = DIRECTION ( 'NONE',  ( 0.9068632946707805287, -0.4214249218767880389, 9.068632946707802473E-16 ) ) ;
#55212 = AXIS2_PLACEMENT_3D ( 'NONE', #74722, #6573, #67004 ) ;
#55213 = EDGE_CURVE ( 'NONE', #27806, #71309, #30917, .T. ) ;
#55214 = VECTOR ( 'NONE', #64539, 1000.000000000000000 ) ;
#55215 = CARTESIAN_POINT ( 'NONE',  ( 49.16670390244701139, -26.71338133339240528, 342.9256252759119548 ) ) ;
#55216 = CIRCLE ( 'NONE', #18995, 3.250000000000002665 ) ;
#55218 = EDGE_LOOP ( 'NONE', ( #83365, #87719 ) ) ;
#55217 = CARTESIAN_POINT ( 'NONE',  ( 111.0096634661633885, -46.42778601040829045, 282.8841967044824628 ) ) ;
#55219 = PLANE ( 'NONE',  #27755 ) ;
#55220 = CARTESIAN_POINT ( 'NONE',  ( 107.3345184958865275, -26.28557234761613159, 120.0556252759109555 ) ) ;
#55221 = CARTESIAN_POINT ( 'NONE',  ( 96.92707254288593788, -39.15325348941441064, 52.51276813305394597 ) ) ;
#55222 = CARTESIAN_POINT ( 'NONE',  ( 105.3089409210114269, -48.49860570903479129, 143.4584824187689662 ) ) ;
#55223 = CARTESIAN_POINT ( 'NONE',  ( 107.0664832912739968, -36.72944715994100306, 9.635625275910941312 ) ) ;
#55224 = LINE ( 'NONE', #19390, #41655 ) ;
#55226 = DIRECTION ( 'NONE',  ( 0.000000000000000000, 0.000000000000000000, -1.000000000000000000 ) ) ;
#55225 = LINE ( 'NONE', #12128, #79711 ) ;
#55227 = CARTESIAN_POINT ( 'NONE',  ( 113.2454987145582663, -28.75867295845091576, 189.5522919408784333 ) ) ;
#55228 = CARTESIAN_POINT ( 'NONE',  ( 131.0667039024480118, -67.87844715994100397, 201.9838068554149970 ) ) ;
#55229 = VERTEX_POINT ( 'NONE', #58606 ) ;
#55230 = VECTOR ( 'NONE', #38149, 1000.000000000000000 ) ;
#55231 = ORIENTED_EDGE ( 'NONE', *, *, #76098, .F. ) ;
#55232 = EDGE_LOOP ( 'NONE', ( #51131, #7542 ) ) ;
#55233 = VECTOR ( 'NONE', #89304, 1000.000000000000000 ) ;
#55234 = ADVANCED_FACE ( 'NONE', ( #17299 ), #53903, .F. ) ;
#55235 = ORIENTED_EDGE ( 'NONE', *, *, #11947, .T. ) ;
#55236 = CARTESIAN_POINT ( 'NONE',  ( 164.7830935719583181, -29.99615139351723769, 313.9678068554149490 ) ) ;
#55237 = CARTESIAN_POINT ( 'NONE',  ( 98.32466564902617279, -28.76522518762223157, 76.73848241876795839 ) ) ;
#55238 = LINE ( 'NONE', #82993, #61473 ) ;
#55239 = EDGE_CURVE ( 'NONE', #50389, #10149, #80387, .T. ) ;
#55240 = AXIS2_PLACEMENT_3D ( 'NONE', #39910, #88536, #19479 ) ;
#55241 = EDGE_CURVE ( 'NONE', #12149, #23464, #33931, .T. ) ;
#55242 = CARTESIAN_POINT ( 'NONE',  ( 145.4263377285063257, -139.2898755805769326, 245.9459212860521404 ) ) ;
#55243 = CARTESIAN_POINT ( 'NONE',  ( 117.4569897637122011, -35.45259360763351708, 189.9241967044829664 ) ) ;
#55245 = EDGE_CURVE ( 'NONE', #2317, #62004, #89364, .T. ) ;
#55244 = DIRECTION ( 'NONE',  ( 1.000000000000000000, 0.000000000000000000, 0.000000000000000000 ) ) ;
#55246 = CARTESIAN_POINT ( 'NONE',  ( 113.8315610999352714, -43.69395359880221719, 267.6124198280766677 ) ) ;
#55247 = VERTEX_POINT ( 'NONE', #74831 ) ;
#55248 = EDGE_LOOP ( 'NONE', ( #49863, #63434, #75991, #9291 ) ) ;
#55249 = ORIENTED_EDGE ( 'NONE', *, *, #28247, .T. ) ;
#55250 = CARTESIAN_POINT ( 'NONE',  ( 76.06670390244805446, -58.72944715994109544, 239.5838068554169809 ) ) ;
#55251 = FACE_OUTER_BOUND ( 'NONE', #46718, .T. ) ;
#55252 = DIRECTION ( 'NONE',  ( 0.000000000000000000, 0.000000000000000000, -1.000000000000000000 ) ) ;
#55253 = CARTESIAN_POINT ( 'NONE',  ( 28.57499999999999929, 91.71543552338529537, 302.8950000000000387 ) ) ;
#55254 = DIRECTION ( 'NONE',  ( 0.000000000000000000, 0.000000000000000000, -1.000000000000000000 ) ) ;
#55255 = CIRCLE ( 'NONE', #40742, 5.599999999999994316 ) ;
#55256 = DIRECTION ( 'NONE',  ( 1.000000000000000000, 0.000000000000000000, 0.000000000000000000 ) ) ;
#55257 = AXIS2_PLACEMENT_3D ( 'NONE', #51774, #72252, #3648 ) ;
#55258 = LINE ( 'NONE', #76174, #39071 ) ;
#55259 = CARTESIAN_POINT ( 'NONE',  ( 105.8561066403587176, -27.02385992090109568, 270.1756252759109884 ) ) ;
#55260 = FACE_OUTER_BOUND ( 'NONE', #27956, .T. ) ;
#55261 = ORIENTED_EDGE ( 'NONE', *, *, #76862, .F. ) ;
#55262 = DIRECTION ( 'NONE',  ( -0.7071067811874389708, 0.7071067811856560636, 0.000000000000000000 ) ) ;
#55263 = AXIS2_PLACEMENT_3D ( 'NONE', #71961, #65578, #38755 ) ;
#55264 = FACE_OUTER_BOUND ( 'NONE', #38573, .T. ) ;
#55265 = CARTESIAN_POINT ( 'NONE',  ( 100.0434009169665757, -32.56939427797095021, 83.71951894101997027 ) ) ;
#55266 = VECTOR ( 'NONE', #59539, 1000.000000000000000 ) ;
#55267 = DIRECTION ( 'NONE',  ( -0.5000000000000015543, 0.8660254037844377084, -2.602085213965216006E-14 ) ) ;
#55268 = DIRECTION ( 'NONE',  ( 1.000000000000000000, 0.000000000000000000, 0.000000000000000000 ) ) ;
#55269 = ORIENTED_EDGE ( 'NONE', *, *, #55917, .F. ) ;
#55270 = ORIENTED_EDGE ( 'NONE', *, *, #64204, .F. ) ;
#55271 = CARTESIAN_POINT ( 'NONE',  ( 77.31651901074903321, -36.55810522839829702, 6.749822759741121558 ) ) ;
#55272 = ORIENTED_EDGE ( 'NONE', *, *, #20945, .F. ) ;
#55273 = CARTESIAN_POINT ( 'NONE',  ( 108.0069521509713297, -26.34547698190780451, 155.0041967044819557 ) ) ;
#55274 = VERTEX_POINT ( 'NONE', #51783 ) ;
#55275 = VECTOR ( 'NONE', #36532, 1000.000000000000114 ) ;
#55276 = CARTESIAN_POINT ( 'NONE',  ( 149.4430470701762488, -12.91565541735124256, 361.9756252759100335 ) ) ;
#55277 = CARTESIAN_POINT ( 'NONE',  ( 112.3917779585437131, -43.81249117439911345, 139.5215833058969679 ) ) ;
#55278 = CARTESIAN_POINT ( 'NONE',  ( -12.53573128184445373, 84.62794568765839642, 117.8914214560859790 ) ) ;
#55279 = CARTESIAN_POINT ( 'NONE',  ( 83.06670390244796920, -61.87844715994100397, 225.9838068554150254 ) ) ;
#55280 = CARTESIAN_POINT ( 'NONE',  ( 116.2507439086588761, -31.75083131158774918, 65.22133956162595325 ) ) ;
#55281 = CARTESIAN_POINT ( 'NONE',  ( 116.8171228670677806, -34.15291832195875799, 85.03145860913214449 ) ) ;
#55282 = EDGE_LOOP ( 'NONE', ( #6432, #61754, #2779, #33877, #57773 ) ) ;
#55283 = CARTESIAN_POINT ( 'NONE',  ( -41.60202597009397607, 65.59999999999998010, 34.51824159735389230 ) ) ;
#55284 = EDGE_LOOP ( 'NONE', ( #32679, #79470 ) ) ;
#55286 = EDGE_CURVE ( 'NONE', #75364, #31678, #27125, .T. ) ;
#55285 = ORIENTED_EDGE ( 'NONE', *, *, #10308, .F. ) ;
#55287 = EDGE_CURVE ( 'NONE', #1937, #44152, #38277, .T. ) ;
#55288 = VECTOR ( 'NONE', #49062, 1000.000000000000000 ) ;
#55289 = ADVANCED_FACE ( 'NONE', ( #69365 ), #89058, .T. ) ;
#55290 = CARTESIAN_POINT ( 'NONE',  ( -465.6921742093539933, 60.32499999999999574, -3.174999999999999822 ) ) ;
#55291 = ORIENTED_EDGE ( 'NONE', *, *, #75557, .T. ) ;
#55292 = CARTESIAN_POINT ( 'NONE',  ( 115.5786047259628759, -31.87203575477177964, 289.2384824187686263 ) ) ;
#55293 = CARTESIAN_POINT ( 'NONE',  ( 97.81677459100555438, -31.87350772351088679, 131.9413395616259947 ) ) ;
#55294 = CARTESIAN_POINT ( 'NONE',  ( 111.8298436232616240, -119.0284471599421181, -21.78219314458157285 ) ) ;
#55295 = CARTESIAN_POINT ( 'NONE',  ( 108.3316104892186189, -46.73506784959683102, 128.6771457822665354 ) ) ;
#55296 = CARTESIAN_POINT ( 'NONE',  ( 117.8564148307409596, -39.12764603782969886, 99.64038718067195077 ) ) ;
#55297 = AXIS2_PLACEMENT_3D ( 'NONE', #86088, #86536, #17041 ) ;
#55298 = LINE ( 'NONE', #88520, #66858 ) ;
#55299 = ORIENTED_EDGE ( 'NONE', *, *, #53298, .T. ) ;
#55300 = CARTESIAN_POINT ( 'NONE',  ( 100.9543326502937504, -28.70727443998947592, 115.5961036648878775 ) ) ;
#55301 = ADVANCED_FACE ( 'NONE', ( #36184 ), #83005, .T. ) ;
#55302 = CARTESIAN_POINT ( 'NONE',  ( 172.5664832912740110, -32.07844715994070839, 23.67562527591200094 ) ) ;
#55303 = ORIENTED_EDGE ( 'NONE', *, *, #68926, .T. ) ;
#55304 = EDGE_CURVE ( 'NONE', #55351, #9306, #55689, .T. ) ;
#55305 = CARTESIAN_POINT ( 'NONE',  ( 41.56648329127399677, -18.82844715994099971, 258.9256252759120116 ) ) ;
#55306 = LINE ( 'NONE', #48050, #41164 ) ;
#55307 = CARTESIAN_POINT ( 'NONE',  ( 105.4209491665783105, -47.02406944081578644, 37.44991099019695469 ) ) ;
#55308 = DIRECTION ( 'NONE',  ( -6.524622321627019585E-16, -4.013151879589939944E-16, -1.000000000000000000 ) ) ;
#55309 = EDGE_CURVE ( 'NONE', #26574, #89290, #56151, .T. ) ;
#55310 = CARTESIAN_POINT ( 'NONE',  ( 140.9629299006806491, -8.979447159940995959, 14.92562527591100618 ) ) ;
#55311 = CARTESIAN_POINT ( 'NONE',  ( 117.0713329378632039, -35.45783045783232978, 93.92760797587766319 ) ) ;
#55312 = CARTESIAN_POINT ( 'NONE',  ( 98.99648076951073961, -33.93126856627920773, 285.4838483995053480 ) ) ;
#55314 = CARTESIAN_POINT ( 'NONE',  ( 107.9437834512411314, -25.73425880284256095, 111.0251490854349754 ) ) ;
#55313 = LINE ( 'NONE', #60801, #66656 ) ;
#55315 = CARTESIAN_POINT ( 'NONE',  ( 62.03715912545824551, -47.82818131006021645, 300.4678068554150627 ) ) ;
#55316 = CARTESIAN_POINT ( 'NONE',  ( 96.62682903746573970, -35.94284815129010013, 146.2670538473399517 ) ) ;
#55317 = DIRECTION ( 'NONE',  ( 4.299999999999999979E-14, -1.000000000000000000, 4.400000000000000367E-29 ) ) ;
#55318 = VERTEX_POINT ( 'NONE', #34832 ) ;
#55319 = DIRECTION ( 'NONE',  ( 1.000000000000000000, 0.000000000000000000, 0.000000000000000000 ) ) ;
#55320 = AXIS2_PLACEMENT_3D ( 'NONE', #6870, #21864, #70001 ) ;
#55321 = FACE_BOUND ( 'NONE', #11602, .T. ) ;
#55322 = DIRECTION ( 'NONE',  ( 0.000000000000000000, -3.491483361109380094E-15, 1.000000000000000000 ) ) ;
#55323 = ORIENTED_EDGE ( 'NONE', *, *, #60881, .T. ) ;
#55324 = EDGE_CURVE ( 'NONE', #77063, #48698, #6380, .T. ) ;
#55325 = DIRECTION ( 'NONE',  ( 0.000000000000000000, 0.000000000000000000, 1.000000000000000000 ) ) ;
#55327 = EDGE_LOOP ( 'NONE', ( #54763, #15225, #8211 ) ) ;
#55326 = CARTESIAN_POINT ( 'NONE',  ( 100.8602861511969024, -45.93004170815812159, 152.0918157521009562 ) ) ;
#55328 = DIRECTION ( 'NONE',  ( 1.000000000000000000, 0.000000000000000000, 0.000000000000000000 ) ) ;
#55329 = CARTESIAN_POINT ( 'NONE',  ( 110.5060411634814557, -26.86503128786541694, 205.8099109901969541 ) ) ;
#55330 = CARTESIAN_POINT ( 'NONE',  ( 87.93968657577623560, -139.1807631652558825, 247.6215491605419174 ) ) ;
#55331 = VECTOR ( 'NONE', #10888, 1000.000000000000000 ) ;
#55332 = LINE ( 'NONE', #68544, #6793 ) ;
#55333 = EDGE_CURVE ( 'NONE', #84665, #40315, #83438, .T. ) ;
#55334 = DIRECTION ( 'NONE',  ( -1.000000000000000000, -1.206764157201257538E-15, 0.000000000000000000 ) ) ;
#55335 = VERTEX_POINT ( 'NONE', #1676 ) ;
#55336 = AXIS2_PLACEMENT_3D ( 'NONE', #78020, #81155, #52050 ) ;
#55337 = ORIENTED_EDGE ( 'NONE', *, *, #88777, .T. ) ;
#55338 = EDGE_LOOP ( 'NONE', ( #22247, #3128 ) ) ;
#55339 = EDGE_LOOP ( 'NONE', ( #80154, #86313, #82824, #32809 ) ) ;
#55340 = DIRECTION ( 'NONE',  ( 0.000000000000000000, -1.000000000000000000, 0.000000000000000000 ) ) ;
#55341 = CARTESIAN_POINT ( 'NONE',  ( 117.4137378716304738, -35.45790868367866722, 189.9241967044829664 ) ) ;
#55342 = CARTESIAN_POINT ( 'NONE',  ( 151.5667039024483813, -48.82844715993591223, 249.9678068554149490 ) ) ;
#55343 = CARTESIAN_POINT ( 'NONE',  ( 74.06670390244704549, -118.2784471599409812, 45.21780685541799727 ) ) ;
#55344 = VECTOR ( 'NONE', #11943, 1000.000000000000000 ) ;
#55345 = EDGE_CURVE ( 'NONE', #18243, #39332, #48431, .T. ) ;
#55348 = EDGE_CURVE ( 'NONE', #68797, #2099, #37037, .T. ) ;
#55347 = CARTESIAN_POINT ( 'NONE',  ( 94.86917197795301604, -31.06128196069623471, 6.826283056785777958 ) ) ;
#55346 = CARTESIAN_POINT ( 'NONE',  ( -240.5296158183964792, 93.66249999999999432, 6.350000000000409983 ) ) ;
#55349 = DIRECTION ( 'NONE',  ( 1.000000000000000000, 0.000000000000000000, -1.224646799147355919E-16 ) ) ;
#55350 = ORIENTED_EDGE ( 'NONE', *, *, #77303, .T. ) ;
#55351 = VERTEX_POINT ( 'NONE', #69813 ) ;
#55352 = AXIS2_PLACEMENT_3D ( 'NONE', #44611, #52296, #86868 ) ;
#55353 = LINE ( 'NONE', #4211, #12275 ) ;
#55354 = CARTESIAN_POINT ( 'NONE',  ( 162.5667039024460223, -22.48495420874110806, -5.074374724088000832 ) ) ;
#55355 = CARTESIAN_POINT ( 'NONE',  ( 107.4826147187165333, -46.50135945624614209, 233.6099109901959707 ) ) ;
#55356 = CARTESIAN_POINT ( 'NONE',  ( 134.0664832912739826, -9.029447159941003775, 4.925625275910997303 ) ) ;
#55357 = CARTESIAN_POINT ( 'NONE',  ( 116.8058161338297509, -37.62879752186919546, 74.75276813305298163 ) ) ;
#55358 = DIRECTION ( 'NONE',  ( 0.000000000000000000, 0.000000000000000000, -1.000000000000000000 ) ) ;
#55359 = AXIS2_PLACEMENT_3D ( 'NONE', #36486, #76466, #76920 ) ;
#55360 = LINE ( 'NONE', #21320, #89498 ) ;
#55361 = EDGE_LOOP ( 'NONE', ( #83558, #72668, #89022, #78662, #35414, #88601 ) ) ;
#55362 = EDGE_CURVE ( 'NONE', #49327, #44506, #33818, .T. ) ;
#55363 = DIRECTION ( 'NONE',  ( 1.000000000000000000, 0.000000000000000000, 0.000000000000000000 ) ) ;
#55364 = VERTEX_POINT ( 'NONE', #50695 ) ;
#55365 = EDGE_LOOP ( 'NONE', ( #53339, #6946, #10566, #6255 ) ) ;
#55366 = LINE ( 'NONE', #89476, #23493 ) ;
#55367 = CARTESIAN_POINT ( 'NONE',  ( 98.11614316284976667, -39.58741349592436620, 277.9920594963732015 ) ) ;
#55368 = EDGE_CURVE ( 'NONE', #13876, #54219, #78436, .T. ) ;
#55369 = FACE_OUTER_BOUND ( 'NONE', #64821, .T. ) ;
#55370 = CARTESIAN_POINT ( 'NONE',  ( 104.4896222497930864, -26.97889890500220034, 140.2814858277504015 ) ) ;
#55371 = CARTESIAN_POINT ( 'NONE',  ( -72.96458098368751166, 127.0000000000000000, 72.96458098368620426 ) ) ;
#55372 = CARTESIAN_POINT ( 'NONE',  ( 110.0667047667142953, -70.87844715994094713, 93.21780685541800437 ) ) ;
#55373 = ORIENTED_EDGE ( 'NONE', *, *, #52021, .T. ) ;
#55374 = LINE ( 'NONE', #83568, #68204 ) ;
#55375 = CARTESIAN_POINT ( 'NONE',  ( 116.3268456006857718, -32.93825467094161752, 164.1356252759109680 ) ) ;
#55376 = VERTEX_POINT ( 'NONE', #17081 ) ;
#55377 = CARTESIAN_POINT ( 'NONE',  ( 118.0757533234433083, -37.71689883586016379, 33.74324432352998571 ) ) ;
#55378 = VERTEX_POINT ( 'NONE', #3447 ) ;
#55379 = CARTESIAN_POINT ( 'NONE',  ( 101.5523784292199991, -30.67338203694697185, 283.4823760838770568 ) ) ;
#55380 = CARTESIAN_POINT ( 'NONE',  ( 117.0716382134925340, -35.46038279169101060, 128.9272686535105379 ) ) ;
#55381 = CARTESIAN_POINT ( 'NONE',  ( 113.7357275853186991, -44.67049210939298831, 148.1203871806729353 ) ) ;
#55382 = CARTESIAN_POINT ( 'NONE',  ( 23.68703819316727888, 81.00531446394714408, 298.3792380957531236 ) ) ;
#55383 = LINE ( 'NONE', #83139, #32795 ) ;
#55384 = CARTESIAN_POINT ( 'NONE',  ( 164.9190312289449878, -35.91149509761320502, 342.9256252759109884 ) ) ;
#55385 = AXIS2_PLACEMENT_3D ( 'NONE', #63514, #84878, #9452 ) ;
#55386 = CARTESIAN_POINT ( 'NONE',  ( 4.049920669541869245, 70.48119388710848909, 130.4956849816146871 ) ) ;
#55387 = CARTESIAN_POINT ( 'NONE',  ( 97.52025866034094292, -43.83442485161933178, 257.8356252759109566 ) ) ;
#55388 = CARTESIAN_POINT ( 'NONE',  ( 76.20774946062907418, 89.94786999841842601, -90.81826664111991931 ) ) ;
#55389 = ORIENTED_EDGE ( 'NONE', *, *, #72659, .F. ) ;
#55390 = VECTOR ( 'NONE', #86070, 1000.000000000000000 ) ;
#55391 = DIRECTION ( 'NONE',  ( 0.000000000000000000, 1.000000000000000000, 0.000000000000000000 ) ) ;
#55392 = ORIENTED_EDGE ( 'NONE', *, *, #64625, .T. ) ;
#55393 = CARTESIAN_POINT ( 'NONE',  ( 98.16534761909046836, -43.36023007783336425, 107.8480062282919647 ) ) ;
#55394 = CARTESIAN_POINT ( 'NONE',  ( 48.16670390244701139, -28.27351298637280408, -5.074374724088000832 ) ) ;
#55395 = ORIENTED_EDGE ( 'NONE', *, *, #51693, .T. ) ;
#55397 = ADVANCED_FACE ( 'NONE', ( #2116 ), #79322, .T. ) ;
#55396 = VERTEX_POINT ( 'NONE', #86130 ) ;
#55399 = EDGE_LOOP ( 'NONE', ( #47934, #51254, #62242, #82391 ) ) ;
#55398 = ADVANCED_FACE ( 'NONE', ( #10262 ), #64344, .T. ) ;
#55400 = EDGE_CURVE ( 'NONE', #11922, #89416, #62912, .T. ) ;
#55401 = DIRECTION ( 'NONE',  ( 4.299999999999999979E-14, -1.000000000000000000, 0.000000000000000000 ) ) ;
#55402 = CARTESIAN_POINT ( 'NONE',  ( 165.2725846195390602, -35.55794170701241086, 117.4678068554150485 ) ) ;
#55403 = DIRECTION ( 'NONE',  ( 0.000000000000000000, -1.000000000000000000, 0.000000000000000000 ) ) ;
#55404 = CARTESIAN_POINT ( 'NONE',  ( 25.56670390244797275, -62.87844715994099687, 173.2178068554149775 ) ) ;
#55405 = CARTESIAN_POINT ( 'NONE',  ( 101.5399107887468944, -29.27606352979315574, 183.4023760838769590 ) ) ;
#55406 = CARTESIAN_POINT ( 'NONE',  ( 115.9784307414374780, -30.15203137637957909, 255.3203871806729524 ) ) ;
#55407 = VECTOR ( 'NONE', #39750, 1000.000000000000000 ) ;
#55408 = CARTESIAN_POINT ( 'NONE',  ( -72.96458098368751166, 127.0000000000000000, 65.02708098368620426 ) ) ;
#55409 = ORIENTED_EDGE ( 'NONE', *, *, #19328, .F. ) ;
#55410 = LINE ( 'NONE', #83165, #73247 ) ;
#55411 = EDGE_CURVE ( 'NONE', #75550, #79764, #12161, .T. ) ;
#55412 = DIRECTION ( 'NONE',  ( 0.000000000000000000, 1.000000000000000000, 0.000000000000000000 ) ) ;
#55413 = EDGE_LOOP ( 'NONE', ( #20208, #68271, #76662, #48203 ) ) ;
#55415 = ORIENTED_EDGE ( 'NONE', *, *, #76983, .T. ) ;
#55414 = VECTOR ( 'NONE', #88903, 1000.000000000000000 ) ;
#55416 = ADVANCED_FACE ( 'NONE', ( #8943 ), #58838, .F. ) ;
#55417 = CIRCLE ( 'NONE', #27882, 29.00000000000000000 ) ;
#55418 = DIRECTION ( 'NONE',  ( -1.000000000000000000, -3.360405532702990443E-14, 0.000000000000000000 ) ) ;
#55419 = FACE_OUTER_BOUND ( 'NONE', #59008, .T. ) ;
#55420 = CARTESIAN_POINT ( 'NONE',  ( 97.60787735695338085, -39.98239029230723673, 16.59006164541757755 ) ) ;
#55421 = LINE ( 'NONE', #29092, #33239 ) ;
#55422 = DIRECTION ( 'NONE',  ( 0.000000000000000000, 0.000000000000000000, 1.000000000000000000 ) ) ;
#55423 = ADVANCED_FACE ( 'NONE', ( #10694 ), #86149, .T. ) ;
#55424 = CARTESIAN_POINT ( 'NONE',  ( 104.9258105463076873, -28.46061097091046577, 199.7009912566479386 ) ) ;
#55425 = CIRCLE ( 'NONE', #40915, 179.8898777604655095 ) ;
#55426 = CARTESIAN_POINT ( 'NONE',  ( 100.9172270114722494, -28.25635367234391992, 75.57562527591093726 ) ) ;
#55427 = CARTESIAN_POINT ( 'NONE',  ( 182.2300522401149863, -33.89581943344511217, 342.9256252759109884 ) ) ;
#55428 = ORIENTED_EDGE ( 'NONE', *, *, #74250, .T. ) ;
#55429 = FACE_OUTER_BOUND ( 'NONE', #54975, .T. ) ;
#55430 = VECTOR ( 'NONE', #62276, 1000.000000000000000 ) ;
#55431 = ORIENTED_EDGE ( 'NONE', *, *, #48664, .T. ) ;
#55432 = DIRECTION ( 'NONE',  ( -1.000000000000000000, 0.000000000000000000, 0.000000000000000000 ) ) ;
#55433 = VERTEX_POINT ( 'NONE', #30269 ) ;
#55434 = DIRECTION ( 'NONE',  ( -0.9834602067153815907, -0.1811243269341220596, 0.000000000000000000 ) ) ;
#55435 = CARTESIAN_POINT ( 'NONE',  ( 37.56670390244814683, -48.82844715994099971, 249.9678068554150343 ) ) ;
#55436 = CARTESIAN_POINT ( 'NONE',  ( 116.8161993950274535, -34.14934549342144976, 275.0312959239825545 ) ) ;
#55437 = DIRECTION ( 'NONE',  ( 0.000000000000000000, -0.5000000000000087708, 0.8660254037844336006 ) ) ;
#55438 = ORIENTED_EDGE ( 'NONE', *, *, #33164, .F. ) ;
#55439 = CARTESIAN_POINT ( 'NONE',  ( 117.2885226371813872, -38.88728764921428649, 63.66133956162494911 ) ) ;
#55441 = LINE ( 'NONE', #27311, #80567 ) ;
#55440 = CARTESIAN_POINT ( 'NONE',  ( 97.81186544543886896, -40.51730612966257183, 271.6361395295153898 ) ) ;
#55442 = LINE ( 'NONE', #76366, #37967 ) ;
#55443 = DIRECTION ( 'NONE',  ( 3.999999999999999995E-14, -1.000000000000000000, 4.100000000000000342E-29 ) ) ;
#55444 = VERTEX_POINT ( 'NONE', #37962 ) ;
#55445 = AXIS2_PLACEMENT_3D ( 'NONE', #84447, #49433, #14947 ) ;
#55446 = DIRECTION ( 'NONE',  ( 2.900000000000000265E-14, -2.000000000000000155E-15, 1.000000000000000000 ) ) ;
#55447 = DIRECTION ( 'NONE',  ( 1.000000000000000000, 0.000000000000000000, -6.982966722218760189E-15 ) ) ;
#55448 = CARTESIAN_POINT ( 'NONE',  ( 4.101352651117800896, 70.52330563318118095, 118.4857037620892726 ) ) ;
#55449 = ORIENTED_EDGE ( 'NONE', *, *, #50391, .T. ) ;
#55450 = CARTESIAN_POINT ( 'NONE',  ( 106.6594888599963298, -26.29050016388675104, 81.10705384733896040 ) ) ;
#55453 = ADVANCED_FACE ( 'NONE', ( #57512 ), #65229, .F. ) ;
#55452 = CARTESIAN_POINT ( 'NONE',  ( -487.2989999999999782, 18.41194598552320016, 97.63125000000000853 ) ) ;
#55451 = DIRECTION ( 'NONE',  ( 0.000000000000000000, 0.000000000000000000, 1.000000000000000000 ) ) ;
#55454 = DIRECTION ( 'NONE',  ( 1.000000000000000000, 0.000000000000000000, 0.000000000000000000 ) ) ;
#55455 = AXIS2_PLACEMENT_3D ( 'NONE', #26587, #77320, #82028 ) ;
#55456 = CARTESIAN_POINT ( 'NONE',  ( 133.9812285940911067, -95.46118927874373128, 250.2191008560389776 ) ) ;
#55457 = EDGE_LOOP ( 'NONE', ( #85272, #76972 ) ) ;
#55458 = CARTESIAN_POINT ( 'NONE',  ( 113.7965574739370140, -44.62378898692899298, 149.1508633711479774 ) ) ;
#55460 = ORIENTED_EDGE ( 'NONE', *, *, #46365, .T. ) ;
#55459 = LINE ( 'NONE', #14160, #2255 ) ;
#55461 = CARTESIAN_POINT ( 'NONE',  ( 115.3062145713271747, -45.21207857638179917, 264.1899109901965517 ) ) ;
#55462 = DIRECTION ( 'NONE',  ( 1.000000000000000000, 0.000000000000000000, 1.472650733923983947E-14 ) ) ;
#55463 = CARTESIAN_POINT ( 'NONE',  ( 107.0664832912739541, -20.87944715994095546, 302.6356252759109680 ) ) ;
#55464 = LINE ( 'NONE', #69576, #13893 ) ;
#55465 = DIRECTION ( 'NONE',  ( 0.000000000000000000, 0.000000000000000000, -1.000000000000000000 ) ) ;
#55466 = VECTOR ( 'NONE', #38861, 1000.000000000000000 ) ;
#55467 = CARTESIAN_POINT ( 'NONE',  ( 68.83135239564657581, -139.4430956531405172, 245.6798494796449859 ) ) ;
#55468 = CARTESIAN_POINT ( 'NONE',  ( -95.43663006862796294, 70.66229531820913223, 89.08909376920047407 ) ) ;
#55469 = CARTESIAN_POINT ( 'NONE',  ( 110.4719531740380347, -47.31314961125950447, 207.8241967044829721 ) ) ;
#55470 = ORIENTED_EDGE ( 'NONE', *, *, #49200, .T. ) ;
#55471 = ORIENTED_EDGE ( 'NONE', *, *, #48683, .F. ) ;
#55472 = CARTESIAN_POINT ( 'NONE',  ( 112.5904859203986206, -43.69705252635404236, 164.5415833058969781 ) ) ;
#55474 = EDGE_CURVE ( 'NONE', #38746, #76506, #52009, .T. ) ;
#55473 = VECTOR ( 'NONE', #25158, 1000.000000000000000 ) ;
#55475 = CARTESIAN_POINT ( 'NONE',  ( 52.38749999999999574, 94.53880000000000905, 246.8562499999999886 ) ) ;
#55476 = CARTESIAN_POINT ( 'NONE',  ( 98.21984324360056462, -33.56503799257626497, 22.49682140113501561 ) ) ;
#55477 = DIRECTION ( 'NONE',  ( 0.000000000000000000, 1.000000000000000000, 0.000000000000000000 ) ) ;
#55478 = AXIS2_PLACEMENT_3D ( 'NONE', #71013, #8329, #36487 ) ;
#55479 = CARTESIAN_POINT ( 'NONE',  ( 101.9933586085964805, -45.44590959077525127, 267.1565423270654378 ) ) ;
#55480 = DIRECTION ( 'NONE',  ( 0.000000000000000000, 1.000000000000000000, 0.000000000000000000 ) ) ;
#55481 = CARTESIAN_POINT ( 'NONE',  ( 97.81169789812091153, -40.51742632959496859, 107.6355761348045519 ) ) ;
#55482 = CARTESIAN_POINT ( 'NONE',  ( 86.98314995794061133, 12.92155284005802507, 336.5756252759109657 ) ) ;
#55483 = CARTESIAN_POINT ( 'NONE',  ( 100.7633749303630850, -45.78122309449486949, 237.0803871806729717 ) ) ;
#55484 = FACE_BOUND ( 'NONE', #55728, .T. ) ;
#55485 = ORIENTED_EDGE ( 'NONE', *, *, #60344, .T. ) ;
#55486 = ORIENTED_EDGE ( 'NONE', *, *, #49600, .F. ) ;
#55487 = CARTESIAN_POINT ( 'NONE',  ( -472.4400000000000546, 53.97500000000000142, -3.174999999999999822 ) ) ;
#55488 = CARTESIAN_POINT ( 'NONE',  ( -92.12450916458696781, 85.43299024555682308, -74.62309654709174822 ) ) ;
#55489 = CARTESIAN_POINT ( 'NONE',  ( 176.5667039024483245, -48.82844715993483220, 300.4678068554149490 ) ) ;
#55490 = DIRECTION ( 'NONE',  ( 0.000000000000000000, -1.000000000000000000, 0.000000000000000000 ) ) ;
#55491 = CARTESIAN_POINT ( 'NONE',  ( 60.32499999999999574, 82.54999999999999716, 335.3740053999999304 ) ) ;
#55492 = ORIENTED_EDGE ( 'NONE', *, *, #28792, .T. ) ;
#55493 = CARTESIAN_POINT ( 'NONE',  ( 105.3131098409624542, -26.40875552125079295, 11.20991099019697046 ) ) ;
#55494 = CARTESIAN_POINT ( 'NONE',  ( 97.22365000156210613, -40.27127430222545001, 266.6013395616254797 ) ) ;
#55496 = ORIENTED_EDGE ( 'NONE', *, *, #254, .T. ) ;
#55495 = EDGE_CURVE ( 'NONE', #81124, #70274, #46947, .T. ) ;
#55497 = AXIS2_PLACEMENT_3D ( 'NONE', #16511, #24219, #70585 ) ;
#55498 = EDGE_CURVE ( 'NONE', #2162, #1004, #23020, .T. ) ;
#55499 = CARTESIAN_POINT ( 'NONE',  ( 77.43081253121034990, -37.51428458727112769, 6.911392308671570284 ) ) ;
#55500 = LINE ( 'NONE', #14659, #36984 ) ;
#55501 = EDGE_CURVE ( 'NONE', #61365, #23550, #17526, .T. ) ;
#55502 = CARTESIAN_POINT ( 'NONE',  ( 116.3170820643562564, -32.94538914428453324, 169.1356252759109680 ) ) ;
#55503 = CARTESIAN_POINT ( 'NONE',  ( 114.2426363300227763, -32.83938885940727204, 67.03951894101994924 ) ) ;
#55504 = CARTESIAN_POINT ( 'NONE',  ( 117.4790109288255309, -40.50628101140208770, 169.5375300378159693 ) ) ;
#55505 = CARTESIAN_POINT ( 'NONE',  ( 118.5256205435843526, -36.72944715994100306, 293.2242906452868851 ) ) ;
#55506 = VERTEX_POINT ( 'NONE', #36642 ) ;
#55507 = EDGE_CURVE ( 'NONE', #89573, #73333, #10716, .T. ) ;
#55508 = LINE ( 'NONE', #7393, #32050 ) ;
#55509 = VERTEX_POINT ( 'NONE', #28289 ) ;
#55510 = ORIENTED_EDGE ( 'NONE', *, *, #54020, .F. ) ;
#55511 = AXIS2_PLACEMENT_3D ( 'NONE', #46342, #40443, #39097 ) ;
#55512 = CARTESIAN_POINT ( 'NONE',  ( 10.08084112162954682, 90.28574336371693221, 118.1269349842563088 ) ) ;
#55513 = ORIENTED_EDGE ( 'NONE', *, *, #63979, .T. ) ;
#55514 = ORIENTED_EDGE ( 'NONE', *, *, #1403, .T. ) ;
#55515 = LINE ( 'NONE', #575, #23692 ) ;
#55516 = ADVANCED_FACE ( 'NONE', ( #76907 ), #78271, .T. ) ;
#55517 = CARTESIAN_POINT ( 'NONE',  ( 110.3568814055478242, -27.59468345507334064, 99.22384839950498758 ) ) ;
#55518 = CARTESIAN_POINT ( 'NONE',  ( 116.0742729640735007, -42.02152512393894312, 238.4041967044829562 ) ) ;
#55519 = CARTESIAN_POINT ( 'NONE',  ( 102.2473430764596714, -45.94923854148477460, 212.1927681330539599 ) ) ;
#55520 = CARTESIAN_POINT ( 'NONE',  ( 96.94826409162261882, -39.14818769109201213, 52.51276813305394597 ) ) ;
#55521 = CARTESIAN_POINT ( 'NONE',  ( 162.7131505118683208, -31.94127993907824958, 342.9256252759109884 ) ) ;
#55522 = CARTESIAN_POINT ( 'NONE',  ( 104.4066637080126867, -46.45766777219723309, 93.36467352085369953 ) ) ;
#55523 = VERTEX_POINT ( 'NONE', #83277 ) ;
#55524 = DIRECTION ( 'NONE',  ( 0.000000000000000000, 0.000000000000000000, -1.000000000000000000 ) ) ;
#55525 = CARTESIAN_POINT ( 'NONE',  ( 31.90335556477799628, -33.89581943344391135, -5.074374724088000832 ) ) ;
#55526 = CARTESIAN_POINT ( 'NONE',  ( 98.49710108934563380, -31.94619897774420636, 110.9213395616259703 ) ) ;
#55527 = CIRCLE ( 'NONE', #23688, 2.500000000000002220 ) ;
#55528 = CARTESIAN_POINT ( 'NONE',  ( 96.03104818302425372, -37.92613241492836806, 81.40038718067299328 ) ) ;
#55529 = CARTESIAN_POINT ( 'NONE',  ( 111.6277637875740538, -46.15289590646231943, 247.9356252759109509 ) ) ;
#55530 = ORIENTED_EDGE ( 'NONE', *, *, #65769, .T. ) ;
#55531 = CARTESIAN_POINT ( 'NONE',  ( 96.13794759894150843, -35.07228238994858316, 221.1946728949589840 ) ) ;
#55532 = DIRECTION ( 'NONE',  ( 0.000000000000000000, 0.000000000000000000, -1.000000000000000000 ) ) ;
#55533 = AXIS2_PLACEMENT_3D ( 'NONE', #67273, #32756, #86841 ) ;
#55534 = CARTESIAN_POINT ( 'NONE',  ( 104.4074300115074294, -46.45789994007284918, 23.36473591763067503 ) ) ;
#55535 = FACE_OUTER_BOUND ( 'NONE', #12840, .T. ) ;
#55537 = CARTESIAN_POINT ( 'NONE',  ( 69.56670390244701707, -90.27844715994098124, 45.21780685541799727 ) ) ;
#55536 = CARTESIAN_POINT ( 'NONE',  ( -105.4788588808462038, 120.6499999999999915, -3.968750000001139977 ) ) ;
#55538 = CARTESIAN_POINT ( 'NONE',  ( 106.1642028280447363, -25.30548797942247674, 320.5922460209141605 ) ) ;
#55539 = DIRECTION ( 'NONE',  ( 0.000000000000000000, -1.000000000000000000, 0.000000000000000000 ) ) ;
#55540 = CONICAL_SURFACE ( 'NONE', #43765, 10.41399999999997839, 0.7853981633974744803 ) ;
#55541 = CARTESIAN_POINT ( 'NONE',  ( 1.451892247740217613E-14, 95.25000000000000000, -118.5560000000000116 ) ) ;
#55542 = FACE_OUTER_BOUND ( 'NONE', #72410, .T. ) ;
#55543 = CARTESIAN_POINT ( 'NONE',  ( 168.3664380525667639, -48.62818131005518296, 300.4678068554149490 ) ) ;
#55544 = CYLINDRICAL_SURFACE ( 'NONE', #73872, 20.00000000000000355 ) ;
#55546 = EDGE_LOOP ( 'NONE', ( #49880, #51975, #56695, #15355 ) ) ;
#55545 = CARTESIAN_POINT ( 'NONE',  ( 115.8254323912423303, -31.73001882710328658, 259.2397919427208990 ) ) ;
#55547 = FACE_OUTER_BOUND ( 'NONE', #66934, .T. ) ;
#55548 = CARTESIAN_POINT ( 'NONE',  ( 99.31672145811513985, -28.81511631862888123, 270.7051490854347549 ) ) ;
#55549 = CARTESIAN_POINT ( 'NONE',  ( 102.9134293080737450, -27.12924067693381502, 151.4013395616249511 ) ) ;
#55550 = CARTESIAN_POINT ( 'NONE',  ( 115.3579863298411254, -45.26537652146382840, 264.1899109901965517 ) ) ;
#55551 = DIRECTION ( 'NONE',  ( -9.073094938289460781E-13, -1.000000000000000000, 0.000000000000000000 ) ) ;
#55554 = ADVANCED_FACE ( 'NONE', ( #16031 ), #85081, .F. ) ;
#55553 = CARTESIAN_POINT ( 'NONE',  ( 82.51738923908165191, -35.48112160757226263, 7.135585143033805977 ) ) ;
#55552 = DIRECTION ( 'NONE',  ( -0.8660254037844387076, 0.000000000000000000, -0.4999999999999998890 ) ) ;
#55555 = CARTESIAN_POINT ( 'NONE',  ( 121.9571836895285486, -124.7784471599409386, 222.2178068554179902 ) ) ;
#55556 = DIRECTION ( 'NONE',  ( 0.000000000000000000, 0.000000000000000000, 1.000000000000000000 ) ) ;
#55557 = AXIS2_PLACEMENT_3D ( 'NONE', #26097, #38820, #31556 ) ;
#55558 = EDGE_CURVE ( 'NONE', #10820, #32414, #50529, .T. ) ;
#55559 = VERTEX_POINT ( 'NONE', #70085 ) ;
#55560 = DIRECTION ( 'NONE',  ( 0.000000000000000000, 1.000000000000000000, 0.000000000000000000 ) ) ;
#55561 = EDGE_LOOP ( 'NONE', ( #89886, #55066 ) ) ;
#55562 = CARTESIAN_POINT ( 'NONE',  ( 98.03781028509631312, -36.02536330594374192, 190.6990864947429998 ) ) ;
#55564 = VERTEX_POINT ( 'NONE', #15586 ) ;
#55563 = CARTESIAN_POINT ( 'NONE',  ( 113.1746683643167728, -44.75457706286819359, 188.0941723682731208 ) ) ;
#55565 = CIRCLE ( 'NONE', #491, 0.2999999999999943823 ) ;
#55566 = DIRECTION ( 'NONE',  ( -0.7071067812152160847, 0.7071067811578790607, 0.000000000000000000 ) ) ;
#55567 = CARTESIAN_POINT ( 'NONE',  ( 101.9826776100855881, -46.51815199768660847, 163.1832443235299763 ) ) ;
#55568 = CARTESIAN_POINT ( 'NONE',  ( 107.0667039024470313, -104.2784471599413934, 2.217806855418003043 ) ) ;
#55569 = CARTESIAN_POINT ( 'NONE',  ( 116.3221839001005264, -32.94216875276463696, 149.1356252759109680 ) ) ;
#55570 = CARTESIAN_POINT ( 'NONE',  ( 109.3845169419079042, -26.99633185450459649, 85.89096953987156269 ) ) ;
#55571 = DIRECTION ( 'NONE',  ( -1.094868876412250136E-15, -2.588449845256440170E-31, -1.000000000000000000 ) ) ;
#55572 = LINE ( 'NONE', #21093, #80267 ) ;
#55573 = CARTESIAN_POINT ( 'NONE',  ( 99.34849973496650932, -28.72665311504486141, 115.6870538473399534 ) ) ;
#55574 = ORIENTED_EDGE ( 'NONE', *, *, #87943, .F. ) ;
#55575 = ORIENTED_EDGE ( 'NONE', *, *, #69162, .F. ) ;
#55576 = EDGE_LOOP ( 'NONE', ( #4981, #53831, #299 ) ) ;
#55577 = AXIS2_PLACEMENT_3D ( 'NONE', #33524, #26698, #76656 ) ;
#55578 = B_SPLINE_CURVE_WITH_KNOTS ( 'NONE', 3,
 ( #101, #27799, #57284, #85028, #55479, #22799, #83231, #20994, #7363, #76403, #14180, #83677, #56389, #21450, #49118, #76851, #14635, #65888 ),
 .UNSPECIFIED., .F., .F.,
 ( 4, 2, 2, 2, 2, 2, 2, 2, 4 ),
 ( 0.4999967102254601614, 0.5624971214472775927, 0.6249975326690950794, 0.6874979438909125662, 0.7499983551127300530, 0.8124987663345475397, 0.8749991775563650265, 0.9374995887781825132, 1.000000000000000000 ),
 .UNSPECIFIED. ) ;
#55579 = CARTESIAN_POINT ( 'NONE',  ( 115.5559677222042154, -32.70388140663459353, 60.62253568684894134 ) ) ;
#55580 = EDGE_CURVE ( 'NONE', #30145, #86172, #29211, .T. ) ;
#55581 = DIRECTION ( 'NONE',  ( 0.7071067811865516806, -0.7071067811865434649, 7.071067811865510832E-16 ) ) ;
#55583 = DIRECTION ( 'NONE',  ( -1.000000000000000000, 0.000000000000000000, 0.000000000000000000 ) ) ;
#55582 = CARTESIAN_POINT ( 'NONE',  ( 107.8656169629272341, -46.51081515578102454, 173.6413395616249886 ) ) ;
#55584 = CARTESIAN_POINT ( 'NONE',  ( 138.8167039024479834, -57.40094715994099772, 84.20080685541500998 ) ) ;
#55585 = CARTESIAN_POINT ( 'NONE',  ( 90.06670390244703128, -104.2784471599417770, -9.937637710810031777 ) ) ;
#55586 = CARTESIAN_POINT ( 'NONE',  ( 0.000000000000000000, 111.1250000000000000, 0.000000000000000000 ) ) ;
#55587 = CARTESIAN_POINT ( 'NONE',  ( 3.063943826786764771E-15, 1.270000000000000018, -24.63800000000000168 ) ) ;
#55588 = LINE ( 'NONE', #63791, #2363 ) ;
#55589 = CARTESIAN_POINT ( 'NONE',  ( 109.0680860650138442, -47.57644715601883689, 127.7337205140059382 ) ) ;
#55590 = EDGE_LOOP ( 'NONE', ( #26779, #69683 ) ) ;
#55591 = EDGE_LOOP ( 'NONE', ( #52057, #85880 ) ) ;
#55592 = VERTEX_POINT ( 'NONE', #22850 ) ;
#55593 = EDGE_CURVE ( 'NONE', #68597, #67104, #44571, .T. ) ;
#55594 = CARTESIAN_POINT ( 'NONE',  ( 12.69999999999999929, 81.71142461540233626, 129.9368274816650626 ) ) ;
#55595 = DIRECTION ( 'NONE',  ( 4.299999999999999979E-14, -1.000000000000000000, 4.400000000000000367E-29 ) ) ;
#55596 = LINE ( 'NONE', #1577, #20684 ) ;
#55597 = CARTESIAN_POINT ( 'NONE',  ( 114.8576755932693487, -34.29489411463138282, 171.8852332267339591 ) ) ;
#55598 = VECTOR ( 'NONE', #22087, 1000.000000000000114 ) ;
#55599 =( REPRESENTATION_RELATIONSHIP ('NONE','NONE', #82876, #42769 ) REPRESENTATION_RELATIONSHIP_WITH_TRANSFORMATION ( #42604 )SHAPE_REPRESENTATION_RELATIONSHIP( ) );
#55600 = DIRECTION ( 'NONE',  ( 1.000000000000000000, 3.999999999999999995E-14, 1.000000000000000078E-15 ) ) ;
#55601 = VECTOR ( 'NONE', #84064, 1000.000000000000000 ) ;
#55602 = CARTESIAN_POINT ( 'NONE',  ( 116.3274949261486881, -32.94048995676258329, 25.13562527591095375 ) ) ;
#55603 = EDGE_LOOP ( 'NONE', ( #39838, #37946, #42889, #66642 ) ) ;
#55605 = VERTEX_POINT ( 'NONE', #48718 ) ;
#55604 = VERTEX_POINT ( 'NONE', #55525 ) ;
#55606 = CARTESIAN_POINT ( 'NONE',  ( 136.1031425115596392, -20.57949487819923462, 2.327894807228624074 ) ) ;
#55607 = ORIENTED_EDGE ( 'NONE', *, *, #5297, .T. ) ;
#55608 = VERTEX_POINT ( 'NONE', #76451 ) ;
#55609 = CARTESIAN_POINT ( 'NONE',  ( 77.86687873446965114, -20.38871026388561347, 7.389079501618835089 ) ) ;
#55610 = EDGE_CURVE ( 'NONE', #56124, #53803, #14235, .T. ) ;
#55611 = CARTESIAN_POINT ( 'NONE',  ( 102.4628740603001233, -44.30143901548009211, 243.5730118773259676 ) ) ;
#55612 = ORIENTED_EDGE ( 'NONE', *, *, #69602, .F. ) ;
#55613 = CARTESIAN_POINT ( 'NONE',  ( 106.5667039024470313, -106.2627606432404974, -19.78219314458196010 ) ) ;
#55614 = CARTESIAN_POINT ( 'NONE',  ( -125.8688597900877397, 66.85668029895285258, 34.66965736785963514 ) ) ;
#55615 = EDGE_LOOP ( 'NONE', ( #43980, #25821, #59105, #15431, #7013 ) ) ;
#55616 = EDGE_LOOP ( 'NONE', ( #4016, #63587, #24491, #68165 ) ) ;
#55617 = CIRCLE ( 'NONE', #71622, 2.116999999999980009 ) ;
#55618 = CARTESIAN_POINT ( 'NONE',  ( 193.5667039024416738, -48.82844715994099971, 129.9678068554150343 ) ) ;
#55619 = VECTOR ( 'NONE', #64430, 1000.000000000000000 ) ;
#55620 = ORIENTED_EDGE ( 'NONE', *, *, #53043, .F. ) ;
#55621 = ORIENTED_EDGE ( 'NONE', *, *, #41987, .T. ) ;
#55622 = EDGE_CURVE ( 'NONE', #33210, #5885, #88426, .T. ) ;
#55623 = CARTESIAN_POINT ( 'NONE',  ( 101.5523784292199991, -30.67338203694697185, 283.4823760838770568 ) ) ;
#55625 = CARTESIAN_POINT ( 'NONE',  ( 102.0711994968067984, -27.55373892369285826, 145.4727681330539610 ) ) ;
#55624 = AXIS2_PLACEMENT_3D ( 'NONE', #70999, #77349, #35103 ) ;
#55626 = CARTESIAN_POINT ( 'NONE',  ( 98.35456548258453324, -42.41549619454043096, 101.7870538473399620 ) ) ;
#55627 = FILL_AREA_STYLE_COLOUR ( '', #83451 ) ;
#55628 = EDGE_CURVE ( 'NONE', #87146, #16628, #20847, .T. ) ;
#55629 = CARTESIAN_POINT ( 'NONE',  ( 132.9844404253383630, -16.20116865955289143, 8.043260881866483913 ) ) ;
#55630 = CARTESIAN_POINT ( 'NONE',  ( 116.8848192732620390, -41.80628269293674748, 239.4346728949589647 ) ) ;
#55631 = DIRECTION ( 'NONE',  ( 1.000000000000000000, 3.999999999999999995E-14, 1.000000000000000078E-15 ) ) ;
#55632 = CARTESIAN_POINT ( 'NONE',  ( 4.163101094985349692E-14, 120.6499999999999915, -107.7702177616926065 ) ) ;
#55633 = ORIENTED_EDGE ( 'NONE', *, *, #78516, .T. ) ;
#55634 = CARTESIAN_POINT ( 'NONE',  ( 130.4354319819074419, 71.15434825076366110, -5.621545387652600922 ) ) ;
#55635 = VERTEX_POINT ( 'NONE', #87971 ) ;
#55636 = ORIENTED_EDGE ( 'NONE', *, *, #87795, .F. ) ;
#55637 = CYLINDRICAL_SURFACE ( 'NONE', #59080, 2.030000000001872529 ) ;
#55638 = AXIS2_PLACEMENT_3D ( 'NONE', #30181, #24259, #86052 ) ;
#55639 = CARTESIAN_POINT ( 'NONE',  ( 103.9236440166535687, -27.23036313016521248, 136.3307465375340541 ) ) ;
#55640 = CARTESIAN_POINT ( 'NONE',  ( 116.9043533071046568, -40.17956947857189220, 133.5584824187679658 ) ) ;
#55641 = CARTESIAN_POINT ( 'NONE',  ( -10.81204423530230585, 75.87175144098965518, 130.1077780123643208 ) ) ;
#55642 = DIRECTION ( 'NONE',  ( -4.237773401492740281E-14, 1.000000000000000000, 0.000000000000000000 ) ) ;
#55643 = PLANE ( 'NONE',  #12277 ) ;
#55646 = CARTESIAN_POINT ( 'NONE',  ( 110.0457755916377494, -26.10929462018219382, 215.8708633711489711 ) ) ;
#55645 = CARTESIAN_POINT ( 'NONE',  ( 114.0300661836957090, -43.96678976627357827, 58.18600423541299449 ) ) ;
#55644 = PLANE ( 'NONE',  #78169 ) ;
#55647 = LINE ( 'NONE', #48842, #58240 ) ;
#55648 = CARTESIAN_POINT ( 'NONE',  ( 0.000000000000000000, 127.0000000000000000, 106.1020876358972771 ) ) ;
#55649 = ORIENTED_EDGE ( 'NONE', *, *, #46269, .T. ) ;
#55650 = DIRECTION ( 'NONE',  ( 0.000000000000000000, 0.000000000000000000, -1.000000000000000000 ) ) ;
#55651 = LINE ( 'NONE', #67975, #51464 ) ;
#55652 = DIRECTION ( 'NONE',  ( 0.000000000000000000, 0.000000000000000000, -1.000000000000000000 ) ) ;
#55653 = CARTESIAN_POINT ( 'NONE',  ( 146.4162810824392125, -137.3184838880133611, 246.9859360010804039 ) ) ;
#55655 = VERTEX_POINT ( 'NONE', #47502 ) ;
#55654 = CARTESIAN_POINT ( 'NONE',  ( 117.4736937924436688, -35.59074751853778196, 278.9127681330539872 ) ) ;
#55656 = DIRECTION ( 'NONE',  ( 1.000000000000000000, 0.000000000000000000, -2.089354330573420398E-14 ) ) ;
#55657 = CARTESIAN_POINT ( 'NONE',  ( 98.83914123113804351, -30.29059417415423638, 155.7984824187679465 ) ) ;
#55658 = CARTESIAN_POINT ( 'NONE',  ( 105.4209835578153189, -47.02385428587647453, 33.44991099019695469 ) ) ;
#55659 = CARTESIAN_POINT ( 'NONE',  ( 107.9218213793745633, -47.19875523359718983, 173.6413395616249886 ) ) ;
#55660 = CARTESIAN_POINT ( 'NONE',  ( 34.92499999999999716, 66.67499999999999716, 342.8999999999999773 ) ) ;
#55661 = PLANE ( 'NONE',  #59100 ) ;
#55663 = FACE_OUTER_BOUND ( 'NONE', #28922, .T. ) ;
#55662 = FACE_OUTER_BOUND ( 'NONE', #29981, .T. ) ;
#55664 = CARTESIAN_POINT ( 'NONE',  ( 74.06670390244701707, -90.27844715994098124, 45.21780685541799727 ) ) ;
#55665 = FACE_OUTER_BOUND ( 'NONE', #20420, .T. ) ;
#55666 = ORIENTED_EDGE ( 'NONE', *, *, #85297, .T. ) ;
#55667 = AXIS2_PLACEMENT_3D ( 'NONE', #85545, #10114, #37823 ) ;
#55668 = DIRECTION ( 'NONE',  ( -1.000000000000000078E-15, 1.000000000000000000, 0.000000000000000000 ) ) ;
#55669 = AXIS2_PLACEMENT_3D ( 'NONE', #31413, #40024, #60921 ) ;
#55670 = EDGE_CURVE ( 'NONE', #61557, #59994, #83233, .T. ) ;
#55671 = ORIENTED_EDGE ( 'NONE', *, *, #21948, .T. ) ;
#55672 = ORIENTED_EDGE ( 'NONE', *, *, #66498, .T. ) ;
#55673 = ORIENTED_EDGE ( 'NONE', *, *, #70207, .T. ) ;
#55674 = CARTESIAN_POINT ( 'NONE',  ( 106.9276426037745011, -26.29176787048590214, 56.08705384733997334 ) ) ;
#55675 = DIRECTION ( 'NONE',  ( 1.000000000000000000, 3.999999999999999995E-14, 1.000000000000000078E-15 ) ) ;
#55676 = CARTESIAN_POINT ( 'NONE',  ( 145.4417903158968670, -139.3033607457884102, 245.6608632105124173 ) ) ;
#55677 = CARTESIAN_POINT ( 'NONE',  ( 98.13109353019112291, -31.27492705589930821, 166.8899109901969950 ) ) ;
#55678 = CARTESIAN_POINT ( 'NONE',  ( 105.3911398957759076, -27.82967838469355115, 279.6590864947435762 ) ) ;
#55679 = ORIENTED_EDGE ( 'NONE', *, *, #20314, .F. ) ;
#55680 = ORIENTED_EDGE ( 'NONE', *, *, #14229, .T. ) ;
#55681 = ORIENTED_EDGE ( 'NONE', *, *, #47886, .F. ) ;
#55682 = AXIS2_PLACEMENT_3D ( 'NONE', #61430, #26476, #82358 ) ;
#55683 = ADVANCED_FACE ( 'NONE', ( #61584 ), #75239, .T. ) ;
#55684 = CARTESIAN_POINT ( 'NONE',  ( 87.06670390244778446, -15.72944715994119669, 239.5838068554169809 ) ) ;
#55685 = VECTOR ( 'NONE', #39885, 1000.000000000000000 ) ;
#55686 = FACE_OUTER_BOUND ( 'NONE', #85084, .T. ) ;
#55687 = CARTESIAN_POINT ( 'NONE',  ( 80.06648329127402519, -46.42944715994105565, -0.5743747240890559880 ) ) ;
#55688 = AXIS2_PLACEMENT_3D ( 'NONE', #76578, #68863, #41581 ) ;
#55689 = LINE ( 'NONE', #8487, #65835 ) ;
#55690 = CARTESIAN_POINT ( 'NONE',  ( 92.02731164704593425, 95.25015599858943460, 92.60677566276864070 ) ) ;
#55691 = DIRECTION ( 'NONE',  ( -0.7071067811865175967, -0.7071067811865774377, -7.071067811865480264E-16 ) ) ;
#55692 = CARTESIAN_POINT ( 'NONE',  ( 0.000000000000000000, 239.0000000000000000, 154.6557476874258441 ) ) ;
#55693 = ADVANCED_FACE ( 'NONE', ( #13014 ), #61147, .F. ) ;
#55694 = VECTOR ( 'NONE', #74783, 1000.000000000000000 ) ;
#55695 = CARTESIAN_POINT ( 'NONE',  ( -12.69999999999999929, 83.33535579944408767, 129.9368274816650057 ) ) ;
#55696 = CARTESIAN_POINT ( 'NONE',  ( 115.5786047259628759, -31.87203575477177964, 289.2384824187686263 ) ) ;
#55697 = PLANE ( 'NONE',  #69014 ) ;
#55698 = EDGE_CURVE ( 'NONE', #69445, #85102, #76019, .T. ) ;
#55699 = VERTEX_POINT ( 'NONE', #53855 ) ;
#55700 = ADVANCED_FACE ( 'NONE', ( #74340 ), #82960, .T. ) ;
#55701 = DIRECTION ( 'NONE',  ( 0.000000000000000000, 0.000000000000000000, 1.000000000000000000 ) ) ;
#55702 = CARTESIAN_POINT ( 'NONE',  ( 74.98969683741650272, 82.54999999999999716, 358.0130000000000337 ) ) ;
#55703 = CARTESIAN_POINT ( 'NONE',  ( 107.4866789999374390, -28.54983079893278486, 92.85380465530596439 ) ) ;
#55704 = ADVANCED_FACE ( 'NONE', ( #76121 ), #88872, .T. ) ;
#55705 = B_SPLINE_CURVE_WITH_KNOTS ( 'NONE', 3,
 ( #59120, #18696, #60007, #52285, #73200, #60464, #4178, #11440, #80049, #80488, #10981, #87299, #25063, #17361, #18247, #39139, #45044, #66844, #4626, #5532, #88207, #80948, #72775, #25967, #53632, #19154, #12335, #40028, #67747, #69095, #83184, #89092, #75467, #20508, #76353 ),
 .UNSPECIFIED., .F., .F.,
 ( 4, 2, 1, 1, 1, 1, 1, 2, 2, 2, 2, 2, 2, 2, 2, 2, 2, 2, 2, 4 ),
 ( 0.4999644244176295604, 0.5002085824135195091, 0.5004527404094094578, 0.5009410564011892442, 0.5019176883847487058, 0.5038709523518675182, 0.5077774802861049208, 0.5155905361545793930, 0.5312166478915285595, 0.5624688713654264482, 0.5937210948393243370, 0.6249733183132222258, 0.6562255417871201146, 0.6874777652610181145, 0.7187299887349160032, 0.7499822122088140031, 0.8124866591566104468, 0.8749911061044071126, 0.9374955530522035563, 1.000000000000000000 ),
 .UNSPECIFIED. ) ;
#55706 = EDGE_CURVE ( 'NONE', #18234, #2491, #47049, .T. ) ;
#55707 = DIRECTION ( 'NONE',  ( 0.000000000000000000, 0.000000000000000000, 1.000000000000000000 ) ) ;
#55708 = CARTESIAN_POINT ( 'NONE',  ( 115.8254323918504696, -31.73001882859116662, 44.23979194259261760 ) ) ;
#55709 = ORIENTED_EDGE ( 'NONE', *, *, #87127, .F. ) ;
#55710 = ORIENTED_EDGE ( 'NONE', *, *, #8100, .F. ) ;
#55711 = CARTESIAN_POINT ( 'NONE',  ( 41.56648329127398966, -27.57844715994070484, 138.9256252759119832 ) ) ;
#55712 = EDGE_LOOP ( 'NONE', ( #83029, #6626, #53122, #46464 ) ) ;
#55713 = ORIENTED_EDGE ( 'NONE', *, *, #12679, .F. ) ;
#55714 = EDGE_CURVE ( 'NONE', #3629, #21597, #89321, .T. ) ;
#55715 = CARTESIAN_POINT ( 'NONE',  ( 117.0608945246740973, -38.08045310990723920, 69.71895861011263662 ) ) ;
#55716 = CARTESIAN_POINT ( 'NONE',  ( 108.4114243528872095, -27.43637152299345061, 146.4053928297069547 ) ) ;
#55717 = CARTESIAN_POINT ( 'NONE',  ( -5.624880194777449383, 93.94404932077412695, 118.4230601929072435 ) ) ;
#55718 = CARTESIAN_POINT ( 'NONE',  ( 115.1837411929738977, -43.30572140991047547, 84.28419670448195689 ) ) ;
#55719 = AXIS2_PLACEMENT_3D ( 'NONE', #734, #50221, #62519 ) ;
#55720 = CARTESIAN_POINT ( 'NONE',  ( 53.56670390244743629, -48.82844715994058049, 180.4678068554151196 ) ) ;
#55721 = VERTEX_POINT ( 'NONE', #68424 ) ;
#55722 = DIRECTION ( 'NONE',  ( 0.000000000000000000, -1.682382052829014912E-15, -1.000000000000000000 ) ) ;
#55723 = VECTOR ( 'NONE', #52628, 1000.000000000000000 ) ;
#55724 = ORIENTED_EDGE ( 'NONE', *, *, #64766, .F. ) ;
#55725 = EDGE_LOOP ( 'NONE', ( #20532, #18452, #35785 ) ) ;
#55726 = EDGE_CURVE ( 'NONE', #11190, #58495, #6200, .T. ) ;
#55727 = DIRECTION ( 'NONE',  ( 1.000000000000000078E-15, 0.000000000000000000, -1.000000000000000000 ) ) ;
#55728 = EDGE_LOOP ( 'NONE', ( #81636, #17683 ) ) ;
#55729 = CARTESIAN_POINT ( 'NONE',  ( 95.96284676697203508, -37.29622633765243478, 271.3670538473399461 ) ) ;
#55730 = CARTESIAN_POINT ( 'NONE',  ( 116.8158478801051530, -32.97616202413719577, 135.1184824187679396 ) ) ;
#55731 = EDGE_CURVE ( 'NONE', #65405, #85819, #42670, .T. ) ;
#55732 = CARTESIAN_POINT ( 'NONE',  ( 4.085245964383497075, 70.51776014978250373, -118.4862668242151358 ) ) ;
#55733 = CARTESIAN_POINT ( 'NONE',  ( 72.96458098368650269, 127.0000000000000000, 80.90208098368729850 ) ) ;
#55734 = CARTESIAN_POINT ( 'NONE',  ( 109.2549746569086437, -46.95841770046993702, 103.7441967044829880 ) ) ;
#55736 = EDGE_CURVE ( 'NONE', #4142, #78790, #68865, .T. ) ;
#55735 = DIRECTION ( 'NONE',  ( 0.000000000000000000, 0.000000000000000000, -1.000000000000000000 ) ) ;
#55737 = ORIENTED_EDGE ( 'NONE', *, *, #54667, .F. ) ;
#55738 = CARTESIAN_POINT ( 'NONE',  ( 97.06387421237998581, -37.34281635329717375, 116.3762687914366722 ) ) ;
#55739 = EDGE_CURVE ( 'NONE', #25814, #960, #22412, .T. ) ;
#55740 = LINE ( 'NONE', #62138, #36095 ) ;
#55741 = ORIENTED_EDGE ( 'NONE', *, *, #63545, .F. ) ;
#55742 = AXIS2_PLACEMENT_3D ( 'NONE', #87263, #52250, #86372 ) ;
#55743 = CARTESIAN_POINT ( 'NONE',  ( 57.14999999999999858, 95.25000000000000000, 300.8629999999999995 ) ) ;
#55744 = AXIS2_PLACEMENT_3D ( 'NONE', #49543, #1871, #75926 ) ;
#55745 = COLOUR_RGB ( '', 0.31764706, 0.68627451, 0.89019608) ;
#55746 = DIRECTION ( 'NONE',  ( 9.351236661543306751E-17, -3.725950533538267725E-29, -1.000000000000000000 ) ) ;
#55747 = CARTESIAN_POINT ( 'NONE',  ( 96.17734138947662359, -38.62830894954290528, 46.45181575210094138 ) ) ;
#55748 = DIRECTION ( 'NONE',  ( 1.000000000000000078E-15, -1.000000000000000000, 0.000000000000000000 ) ) ;
#55749 = DIRECTION ( 'NONE',  ( -3.100000000000000258E-29, 3.100000000000000044E-14, 1.000000000000000000 ) ) ;
#55750 = CARTESIAN_POINT ( 'NONE',  ( 112.0683309827296767, -45.48704644034171451, 92.99083554691495124 ) ) ;
#55751 = CARTESIAN_POINT ( 'NONE',  ( 97.46604185887800043, -38.76544784714115366, 31.49276813305495892 ) ) ;
#55753 = CARTESIAN_POINT ( 'NONE',  ( 102.3122812202564802, -27.43633205498518635, 116.4527681330539650 ) ) ;
#55752 = CARTESIAN_POINT ( 'NONE',  ( 112.1392154949572841, -28.01274250318494197, 109.6564706139660075 ) ) ;
#55754 = DIRECTION ( 'NONE',  ( -0.7071067811578587436, 0.7071067812152364018, 0.000000000000000000 ) ) ;
#55755 = FACE_OUTER_BOUND ( 'NONE', #38288, .T. ) ;
#55756 = ORIENTED_EDGE ( 'NONE', *, *, #5669, .T. ) ;
#55757 = DIRECTION ( 'NONE',  ( 0.000000000000000000, 0.000000000000000000, 1.000000000000000000 ) ) ;
#55758 = AXIS2_PLACEMENT_3D ( 'NONE', #70098, #27859, #41475 ) ;
#55759 = VECTOR ( 'NONE', #47764, 999.9999999999998863 ) ;
#55760 = DIRECTION ( 'NONE',  ( 0.000000000000000000, 0.000000000000000000, -1.000000000000000000 ) ) ;
#55761 = LINE ( 'NONE', #5873, #84829 ) ;
#55762 = ORIENTED_EDGE ( 'NONE', *, *, #10019, .F. ) ;
#55763 = CARTESIAN_POINT ( 'NONE',  ( 0.000000000000000000, 93.07500000000001705, 0.000000000000000000 ) ) ;
#55765 = ORIENTED_EDGE ( 'NONE', *, *, #47200, .F. ) ;
#55764 = CARTESIAN_POINT ( 'NONE',  ( 108.9531560784502915, -26.39541311287850434, 164.9327681330529742 ) ) ;
#55766 = CARTESIAN_POINT ( 'NONE',  ( 165.9667039024459996, -26.71338133339301635, -5.074374724088000832 ) ) ;
#55767 = CARTESIAN_POINT ( 'NONE',  ( 98.01791376823749147, -44.42006743888428133, 222.8870538473399563 ) ) ;
#55768 = CARTESIAN_POINT ( 'NONE',  ( 110.3678327243794541, -25.29650332976257943, 60.85276813305395649 ) ) ;
#55769 = LINE ( 'NONE', #56226, #33075 ) ;
#55770 = DIRECTION ( 'NONE',  ( 0.000000000000000000, 1.000000000000000000, 0.000000000000000000 ) ) ;
#55771 = FACE_OUTER_BOUND ( 'NONE', #41825, .T. ) ;
#55772 = ORIENTED_EDGE ( 'NONE', *, *, #20432, .T. ) ;
#55773 = CONTEXT_DEPENDENT_SHAPE_REPRESENTATION ( #83490, #53216 ) ;
#55774 = VECTOR ( 'NONE', #84751, 1000.000000000000000 ) ;
#55775 = ORIENTED_EDGE ( 'NONE', *, *, #32299, .T. ) ;
#55776 = ORIENTED_EDGE ( 'NONE', *, *, #51752, .T. ) ;
#55777 = ORIENTED_EDGE ( 'NONE', *, *, #25255, .F. ) ;
#55778 = CARTESIAN_POINT ( 'NONE',  ( 107.0664832912739399, -48.18858441225130917, 305.0306255462182321 ) ) ;
#55779 = CARTESIAN_POINT ( 'NONE',  ( 96.80890382254112581, -40.84721887859184619, 247.6422919425769749 ) ) ;
#55780 = CARTESIAN_POINT ( 'NONE',  ( 97.81085527707094229, -40.51777768585955641, 251.6359959587111064 ) ) ;
#55781 = CARTESIAN_POINT ( 'NONE',  ( 136.5888380630391339, -17.63381004753921033, 2.797770231027887800 ) ) ;
#55783 = LINE ( 'NONE', #1313, #77640 ) ;
#55782 = DIRECTION ( 'NONE',  ( -1.000000000000000000, -4.163336342344275811E-14, 0.000000000000000000 ) ) ;
#55784 = CARTESIAN_POINT ( 'NONE',  ( 181.9694315774203233, -34.03355364505981129, 342.9256252759109884 ) ) ;
#55785 = CARTESIAN_POINT ( 'NONE',  ( 100.4651824673786393, -27.83460210401261747, 35.59657765686397113 ) ) ;
#55786 = EDGE_LOOP ( 'NONE', ( #19066, #81340, #57636, #19984 ) ) ;
#55787 = ORIENTED_EDGE ( 'NONE', *, *, #43160, .F. ) ;
#55788 = EDGE_CURVE ( 'NONE', #55509, #4752, #38164, .T. ) ;
#55789 = CARTESIAN_POINT ( 'NONE',  ( 89.06648138392552028, -56.72944715994104570, 14.67562527591095289 ) ) ;
#55790 = CIRCLE ( 'NONE', #21011, 5.599999999999994316 ) ;
#55791 = CARTESIAN_POINT ( 'NONE',  ( 32.06670390244800473, -32.29483332968611364, -5.074374724088000832 ) ) ;
#55792 = EDGE_CURVE ( 'NONE', #53468, #14978, #35227, .T. ) ;
#55793 = CARTESIAN_POINT ( 'NONE',  ( 104.1325824198641783, -27.39908484284276469, 246.3184824187669619 ) ) ;
#55794 = DIRECTION ( 'NONE',  ( 0.000000000000000000, 0.000000000000000000, 1.000000000000000000 ) ) ;
#55795 = ADVANCED_FACE ( 'NONE', ( #49748 ), #15705, .T. ) ;
#55796 = CARTESIAN_POINT ( 'NONE',  ( 98.87588542518402335, -42.07524381596787322, 97.78705384733893879 ) ) ;
#55797 = CARTESIAN_POINT ( 'NONE',  ( 73.06648329127396835, -8.979447159941065237, 14.92562527591093691 ) ) ;
#55798 = CARTESIAN_POINT ( 'NONE',  ( 112.7336434204684252, -28.43300400972322350, 20.59933406696459457 ) ) ;
#55799 = EDGE_CURVE ( 'NONE', #11998, #29962, #87636, .T. ) ;
#55800 = VERTEX_POINT ( 'NONE', #1633 ) ;
#55801 = DIRECTION ( 'NONE',  ( 0.000000000000000000, 0.000000000000000000, -1.000000000000000000 ) ) ;
#55802 = ADVANCED_FACE ( 'NONE', ( #1175 ), #28157, .T. ) ;
#55803 = ORIENTED_EDGE ( 'NONE', *, *, #54020, .T. ) ;
#55804 = ORIENTED_EDGE ( 'NONE', *, *, #50166, .F. ) ;
#55805 = CARTESIAN_POINT ( 'NONE',  ( -88.20661029664569242, 93.55239623846826191, 79.21650378603861498 ) ) ;
#55806 = CARTESIAN_POINT ( 'NONE',  ( 115.1751221500829701, -40.30411560180680652, 249.9272975916113637 ) ) ;
#55807 = EDGE_CURVE ( 'NONE', #70994, #61646, #77034, .T. ) ;
#55808 = CIRCLE ( 'NONE', #87809, 2.500000000000002220 ) ;
#55809 = CARTESIAN_POINT ( 'NONE',  ( 98.30753412859742468, -41.72887538384050288, 191.7397919328074636 ) ) ;
#55810 = AXIS2_PLACEMENT_3D ( 'NONE', #35365, #69906, #855 ) ;
#55811 = VECTOR ( 'NONE', #71607, 1000.000000000000000 ) ;
#55812 = CARTESIAN_POINT ( 'NONE',  ( -118.5215310810514495, 94.92435932957491218, 2.887881501069120116 ) ) ;
#55813 = VECTOR ( 'NONE', #35523, 1000.000000000000000 ) ;
#55814 = ADVANCED_FACE ( 'NONE', ( #28880, #15255 ), #42928, .T. ) ;
#55815 = CARTESIAN_POINT ( 'NONE',  ( 91.06648329127393993, -36.72944715994093912, 311.6356252759109680 ) ) ;
#55816 = CARTESIAN_POINT ( 'NONE',  ( 76.80536679343914841, 74.16967745525862199, -90.31351860656764075 ) ) ;
#55817 = VECTOR ( 'NONE', #11689, 1000.000000000000000 ) ;
#55818 = ORIENTED_EDGE ( 'NONE', *, *, #69897, .T. ) ;
#55819 = LINE ( 'NONE', #48556, #39202 ) ;
#55820 = AXIS2_PLACEMENT_3D ( 'NONE', #49350, #85259, #16641 ) ;
#55821 = CARTESIAN_POINT ( 'NONE',  ( 97.81151460250711693, -40.51751193867107759, 182.6359910548048333 ) ) ;
#55822 = ORIENTED_EDGE ( 'NONE', *, *, #41883, .T. ) ;
#55823 = CARTESIAN_POINT ( 'NONE',  ( 117.9248307134361937, -41.47673871369620002, 58.49848241876792798 ) ) ;
#55824 = ORIENTED_EDGE ( 'NONE', *, *, #887, .F. ) ;
#55825 = CARTESIAN_POINT ( 'NONE',  ( 101.6581149080599573, -43.36298066831790265, 11.45527697093296027 ) ) ;
#55826 = EDGE_CURVE ( 'NONE', #15646, #4014, #9311, .T. ) ;
#55827 = DIRECTION ( 'NONE',  ( -4.237773401492740281E-14, 1.000000000000000000, 0.000000000000000000 ) ) ;
#55828 = CARTESIAN_POINT ( 'NONE',  ( 115.7764676695378512, -43.63945112744040955, 198.2927681330539542 ) ) ;
#55829 = CARTESIAN_POINT ( 'NONE',  ( 165.3359832912740046, -36.32844715994100682, -5.074374724088000832 ) ) ;
#55830 = FACE_OUTER_BOUND ( 'NONE', #50714, .T. ) ;
#55831 = DIRECTION ( 'NONE',  ( -0.7071067811578587436, 0.7071067812152364018, 0.000000000000000000 ) ) ;
#55832 = CARTESIAN_POINT ( 'NONE',  ( 9.432210905596992490, 74.04481405089026680, 130.2149380284310212 ) ) ;
#55833 = AXIS2_PLACEMENT_3D ( 'NONE', #55908, #21427, #69123 ) ;
#55834 = CARTESIAN_POINT ( 'NONE',  ( 110.2692182064865420, -26.72542277727598403, 230.8299109901969643 ) ) ;
#55835 = CARTESIAN_POINT ( 'NONE',  ( 107.7544711540019478, -46.72718120385261642, 117.6331727250829715 ) ) ;
#55836 = ORIENTED_EDGE ( 'NONE', *, *, #25941, .T. ) ;
#55837 = DIRECTION ( 'NONE',  ( 0.000000000000000000, 0.000000000000000000, -1.000000000000000000 ) ) ;
#55838 = EDGE_LOOP ( 'NONE', ( #56298, #67106, #77873, #698 ) ) ;
#55839 = CARTESIAN_POINT ( 'NONE',  ( 114.7580948764747291, -43.83100269166961027, 119.2327681330539804 ) ) ;
#55840 = LINE ( 'NONE', #27266, #62793 ) ;
#55841 = ORIENTED_EDGE ( 'NONE', *, *, #49138, .F. ) ;
#55842 = CIRCLE ( 'NONE', #3674, 2.116999999999980009 ) ;
#55843 = ORIENTED_EDGE ( 'NONE', *, *, #50376, .F. ) ;
#55844 = ORIENTED_EDGE ( 'NONE', *, *, #14435, .T. ) ;
#55845 = DIRECTION ( 'NONE',  ( -2.734539469520093702E-14, -1.000000000000000000, 0.000000000000000000 ) ) ;
#55846 = CARTESIAN_POINT ( 'NONE',  ( 255.9983484187079910, 40.03750000000000142, 10.66800000000000104 ) ) ;
#55847 = LINE ( 'NONE', #27271, #6572 ) ;
#55848 = LINE ( 'NONE', #40452, #72687 ) ;
#55849 = DIRECTION ( 'NONE',  ( 0.000000000000000000, 0.000000000000000000, 1.000000000000000000 ) ) ;
#55850 = CARTESIAN_POINT ( 'NONE',  ( 111.3099657731024337, -28.47785412639777647, 167.5166617981629713 ) ) ;
#55851 = CARTESIAN_POINT ( 'NONE',  ( 102.3694487442499934, -47.63304195565743981, 283.2527681330539053 ) ) ;
#55853 = EDGE_CURVE ( 'NONE', #58766, #54444, #12228, .T. ) ;
#55852 = DIRECTION ( 'NONE',  ( 0.000000000000000000, 0.000000000000000000, -1.000000000000000000 ) ) ;
#55854 = ORIENTED_EDGE ( 'NONE', *, *, #78527, .T. ) ;
#55855 = CARTESIAN_POINT ( 'NONE',  ( 4.087783556564577481, 70.51867047662535981, 118.4861746650021104 ) ) ;
#55856 = EDGE_CURVE ( 'NONE', #48806, #241, #20913, .T. ) ;
#55857 = LINE ( 'NONE', #69971, #82478 ) ;
#55858 = VERTEX_POINT ( 'NONE', #73324 ) ;
#55859 = VERTEX_POINT ( 'NONE', #30222 ) ;
#55860 = CIRCLE ( 'NONE', #38498, 4.762500000000002842 ) ;
#55861 = CARTESIAN_POINT ( 'NONE',  ( -446.0240000000000009, 93.66249999999999432, 11.11250000000040217 ) ) ;
#55862 = CARTESIAN_POINT ( 'NONE',  ( -3.968750000000754508, 120.6499999999999915, 100.8961411191535973 ) ) ;
#55863 = AXIS2_PLACEMENT_3D ( 'NONE', #21062, #29664, #21521 ) ;
#55864 = CARTESIAN_POINT ( 'NONE',  ( 105.7994668797627185, -26.72404082623033972, 15.17729597880891390 ) ) ;
#55865 = FACE_OUTER_BOUND ( 'NONE', #22744, .T. ) ;
#55866 = DIRECTION ( 'NONE',  ( -1.000000000000000000, -3.999999999999999995E-14, -1.000000000000000078E-15 ) ) ;
#55867 = CARTESIAN_POINT ( 'NONE',  ( 115.2610577610831655, -39.13882072599808026, 183.0209912566479602 ) ) ;
#55868 = CARTESIAN_POINT ( 'NONE',  ( 116.7155050624037926, -32.57635518107161943, 79.14991099019697174 ) ) ;
#55869 = ORIENTED_EDGE ( 'NONE', *, *, #30837, .F. ) ;
#55870 = DIRECTION ( 'NONE',  ( 0.000000000000000000, 1.000000000000000000, 0.000000000000000000 ) ) ;
#55871 = ORIENTED_EDGE ( 'NONE', *, *, #87642, .T. ) ;
#55872 = DIRECTION ( 'NONE',  ( 0.000000000000000000, -1.000000000000000000, 0.000000000000000000 ) ) ;
#55873 = ORIENTED_EDGE ( 'NONE', *, *, #67275, .T. ) ;
#55874 = FACE_OUTER_BOUND ( 'NONE', #45864, .T. ) ;
#55875 = EDGE_LOOP ( 'NONE', ( #37910, #57734, #9286, #30820 ) ) ;
#55876 = LINE ( 'NONE', #54530, #63893 ) ;
#55877 = DIRECTION ( 'NONE',  ( -1.000000000000000000, -8.163404592832032979E-16, 0.000000000000000000 ) ) ;
#55878 = CARTESIAN_POINT ( 'NONE',  ( 147.0667039027857470, -137.6784471596013191, 245.4218662566959779 ) ) ;
#55880 = AXIS2_PLACEMENT_3D ( 'NONE', #3667, #86790, #45862 ) ;
#55879 = CARTESIAN_POINT ( 'NONE',  ( -46.60773131249376888, 65.60000000000000853, -44.42500552774628630 ) ) ;
#55881 = VERTEX_POINT ( 'NONE', #45160 ) ;
#55882 = CARTESIAN_POINT ( 'NONE',  ( 112.7719768816358936, -27.93537496831996592, 69.61848241876793963 ) ) ;
#55883 = AXIS2_PLACEMENT_3D ( 'NONE', #26889, #40960, #54562 ) ;
#55884 = AXIS2_PLACEMENT_3D ( 'NONE', #68800, #27455, #18858 ) ;
#55885 =( NAMED_UNIT ( * ) SI_UNIT ( $, .STERADIAN. ) SOLID_ANGLE_UNIT ( ) );
#55886 = VECTOR ( 'NONE', #11718, 1000.000000000000000 ) ;
#55888 = DIRECTION ( 'NONE',  ( 1.000000000000000000, 0.000000000000000000, 0.000000000000000000 ) ) ;
#55887 = CARTESIAN_POINT ( 'NONE',  ( 144.5667039024470171, -85.27844715994089597, 55.21780685541800437 ) ) ;
#55889 = CARTESIAN_POINT ( 'NONE',  ( 241.3336515812914911, 40.03750000000000142, -2.032000000000000028 ) ) ;
#55890 = LINE ( 'NONE', #14598, #23881 ) ;
#55891 = ORIENTED_EDGE ( 'NONE', *, *, #46034, .F. ) ;
#55892 = VECTOR ( 'NONE', #84772, 1000.000000000000000 ) ;
#55893 = CARTESIAN_POINT ( 'NONE',  ( 29.56670390244864777, -48.82844715994099971, 249.9678068554150059 ) ) ;
#55894 = CIRCLE ( 'NONE', #58755, 17.00000000000000000 ) ;
#55895 = CARTESIAN_POINT ( 'NONE',  ( -129.9368274816650626, 82.54999999999999716, -12.70000000000045404 ) ) ;
#55896 = CYLINDRICAL_SURFACE ( 'NONE', #10776, 0.4999999999999989453 ) ;
#55897 = CARTESIAN_POINT ( 'NONE',  ( 99.66919142226757344, -46.01935155626545537, 118.0413395616259606 ) ) ;
#55899 = CARTESIAN_POINT ( 'NONE',  ( 21.03715912545739641, -47.82818131006197149, 180.4678068554150911 ) ) ;
#55898 = CARTESIAN_POINT ( 'NONE',  ( 193.5667039024415033, -48.82844715994099971, 249.9678068554149775 ) ) ;
#55900 = FACE_OUTER_BOUND ( 'NONE', #52573, .T. ) ;
#55901 = CIRCLE ( 'NONE', #44308, 118.5560000000000116 ) ;
#55902 = EDGE_CURVE ( 'NONE', #10820, #64140, #49939, .T. ) ;
#55903 = CONICAL_SURFACE ( 'NONE', #29825, 1.219499999999975159, 1.047197551196598297 ) ;
#55904 = EDGE_CURVE ( 'NONE', #18647, #30283, #62985, .T. ) ;
#55905 = CARTESIAN_POINT ( 'NONE',  ( 172.5664832912740110, 0.2215528400590013880, 321.0426252759119734 ) ) ;
#55906 = EDGE_CURVE ( 'NONE', #39283, #70136, #23839, .T. ) ;
#55907 = CARTESIAN_POINT ( 'NONE',  ( 113.4245949246307532, -29.25360672088989489, 135.5156252759109634 ) ) ;
#55909 = ORIENTED_EDGE ( 'NONE', *, *, #84881, .F. ) ;
#55908 = CARTESIAN_POINT ( 'NONE',  ( 107.0667039024470313, -104.2784471599420755, -19.78219314458201694 ) ) ;
#55910 = ADVANCED_FACE ( 'NONE', ( #86086 ), #31095, .F. ) ;
#55911 = CARTESIAN_POINT ( 'NONE',  ( 97.23737678141888807, -33.32131919061086478, 282.0613395616252888 ) ) ;
#55912 = CARTESIAN_POINT ( 'NONE',  ( 0.000000000000000000, 17.78000000000000114, 0.000000000000000000 ) ) ;
#55913 = DIRECTION ( 'NONE',  ( -1.000000000000000000, -5.782411586589351722E-16, 5.782411586589351722E-16 ) ) ;
#55914 = DIRECTION ( 'NONE',  ( 1.000000000000000078E-15, 1.000000000000000083E-30, -1.000000000000000000 ) ) ;
#55915 = CIRCLE ( 'NONE', #28380, 10.00000000000002665 ) ;
#55916 = CARTESIAN_POINT ( 'NONE',  ( 210.5660000000000025, 52.73749999999999716, -37.80245750428454699 ) ) ;
#55917 = EDGE_CURVE ( 'NONE', #57180, #19136, #67316, .T. ) ;
#55918 = CARTESIAN_POINT ( 'NONE',  ( 68.16498115913746858, -136.2709715552406635, 247.3967431772409782 ) ) ;
#55919 = CARTESIAN_POINT ( 'NONE',  ( -99.18073718829342056, 74.80151635532867260, 84.90151352399695384 ) ) ;
#55920 = B_SPLINE_CURVE_WITH_KNOTS ( 'NONE', 3,
 ( #82017, #27473, #55148, #40193, #46996, #89268, #74734, #12964, #53359, #74289, #67914, #41093, #18872, #41532, #34735, #88380, #13850, #33395, #46557, #5703, #61096, #61984, #75639, #40653, #6151, #82468, #20225, #76070, #89723, #39749, #47896, #48337, #69262, #1118, #657, #84255, #14307, #41983, #29276, #22029, #49699, #84703, #64242, #85149, #71071, #77421, #35170, #28363, #8386 ),
 .UNSPECIFIED., .F., .F.,
 ( 4, 2, 2, 2, 2, 2, 2, 2, 2, 2, 2, 2, 2, 2, 2, 1, 2, 2, 2, 2, 2, 2, 2, 2, 4 ),
 ( 0.01986933033599077442, 0.02111088875730818271, 0.02235244717862559100, 0.02483556402126041451, 0.02607712244257780546, 0.02731868086389519640, 0.02980179770652996440, 0.03228491454916473241, 0.03352647297048211295, 0.03476803139179950042, 0.03725114823443430312, 0.03849270665575170447, 0.03973426507706910582, 0.04221738191970388077, 0.04345894034102125436, 0.04470049876233862796, 0.04594205718365600155, 0.04718361560497337515, 0.04966673244760812234, 0.05090829086892548205, 0.05214984929024284871, 0.05463296613287755427, 0.05587452455419490011, 0.05711608297551223901, 0.05959919981814693069 ),
 .UNSPECIFIED. ) ;
#55921 = CARTESIAN_POINT ( 'NONE',  ( 97.71246005893821973, -41.20616857227592789, 216.6937205140069409 ) ) ;
#55922 = ORIENTED_EDGE ( 'NONE', *, *, #84891, .T. ) ;
#55923 = ORIENTED_EDGE ( 'NONE', *, *, #83201, .T. ) ;
#55924 = AXIS2_PLACEMENT_3D ( 'NONE', #17688, #73088, #81277 ) ;
#55925 = CARTESIAN_POINT ( 'NONE',  ( 113.3535730310440215, -29.74740315656111989, 155.9368214011359726 ) ) ;
#55926 = EDGE_CURVE ( 'NONE', #20086, #1937, #86213, .T. ) ;
#55927 = DIRECTION ( 'NONE',  ( 0.000000000000000000, 1.000000000000000000, 0.000000000000000000 ) ) ;
#55928 = CARTESIAN_POINT ( 'NONE',  ( 116.5375268006221319, -40.16019621794498562, 19.98158330589694387 ) ) ;
#55929 = CIRCLE ( 'NONE', #7904, 6.557978799109520196 ) ;
#55930 = CARTESIAN_POINT ( 'NONE',  ( 151.0371591254573502, -24.42818131005592974, 249.9678068554149490 ) ) ;
#55931 = EDGE_CURVE ( 'NONE', #73188, #48100, #9774, .T. ) ;
#55932 = CARTESIAN_POINT ( 'NONE',  ( 7.620115932400929327E-15, 50.79999999999999716, 221.5895999999999901 ) ) ;
#55933 = DIRECTION ( 'NONE',  ( 0.000000000000000000, 0.000000000000000000, 1.000000000000000000 ) ) ;
#55934 = DIRECTION ( 'NONE',  ( 1.000000000000000000, 0.000000000000000000, 0.000000000000000000 ) ) ;
#55935 = LINE ( 'NONE', #105, #67646 ) ;
#55936 = CARTESIAN_POINT ( 'NONE',  ( 107.2488531970940073, -24.90511003128400347, 230.0641967044819580 ) ) ;
#55937 = CARTESIAN_POINT ( 'NONE',  ( 0.8234126494891776948, 95.12992737732547255, 118.3538578355079522 ) ) ;
#55938 = ORIENTED_EDGE ( 'NONE', *, *, #45132, .F. ) ;
#55939 = ORIENTED_EDGE ( 'NONE', *, *, #27432, .T. ) ;
#55940 = EDGE_CURVE ( 'NONE', #43695, #29186, #58789, .T. ) ;
#55941 = CARTESIAN_POINT ( 'NONE',  ( -83.22961976134699569, 79.25971567868506895, -100.5868491334645825 ) ) ;
#55942 = CARTESIAN_POINT ( 'NONE',  ( -92.06080542007461531, 85.83559868056556752, -74.70172715947531117 ) ) ;
#55943 = CARTESIAN_POINT ( 'NONE',  ( 107.0664832912739968, -36.72944715994100306, 287.6356252759109680 ) ) ;
#55944 = DIRECTION ( 'NONE',  ( 0.000000000000000000, 0.000000000000000000, 1.000000000000000000 ) ) ;
#55946 = DIRECTION ( 'NONE',  ( 0.000000000000000000, 0.000000000000000000, -1.000000000000000000 ) ) ;
#55945 = AXIS2_PLACEMENT_3D ( 'NONE', #78776, #79220, #57856 ) ;
#55947 = ORIENTED_EDGE ( 'NONE', *, *, #9589, .T. ) ;
#55948 = AXIS2_PLACEMENT_3D ( 'NONE', #7350, #55914, #21433 ) ;
#55949 = DIRECTION ( 'NONE',  ( 0.000000000000000000, 0.000000000000000000, -1.000000000000000000 ) ) ;
#55950 = AXIS2_PLACEMENT_3D ( 'NONE', #61196, #6248, #41195 ) ;
#55951 = CARTESIAN_POINT ( 'NONE',  ( 111.6085881668573450, -46.11327973307566452, 247.9356252759109509 ) ) ;
#55952 = ORIENTED_EDGE ( 'NONE', *, *, #82525, .T. ) ;
#55953 = CARTESIAN_POINT ( 'NONE',  ( 77.46225723383157913, -37.61690131752746424, 6.952852217891951625 ) ) ;
#55954 = B_SPLINE_CURVE_WITH_KNOTS ( 'NONE', 3,
 ( #51753, #19037, #88095, #25857, #59463, #46725, #24961, #67635, #5418, #79501, #80389, #45821, #73551, #13565, #20831, #88981, #75351, #47620, #13131, #26741, #89889, #12681, #48498, #47169, #48951, #69878, #75799, #33558, #54420, #41698, #82183 ),
 .UNSPECIFIED., .F., .F.,
 ( 4, 2, 2, 1, 2, 2, 2, 2, 2, 2, 2, 1, 1, 2, 2, 2, 4 ),
 ( 0.000000000000000000, 0.06249999999996883049, 0.09374999999995763111, 0.1093749999999479305, 0.1171874999999430872, 0.1249999999999382161, 0.1874999999999378275, 0.2187499999999375777, 0.2499999999999373834, 0.3124999999999420464, 0.3437499999999465428, 0.3593749999999497624, 0.3671874999999486522, 0.3710937499999490963, 0.3749999999999495404, 0.4374999999999747424, 0.5000000000000000000 ),
 .UNSPECIFIED. ) ;
#55955 = DIRECTION ( 'NONE',  ( 0.000000000000000000, -1.000000000000000000, 4.100000000000000342E-29 ) ) ;
#55956 = DIRECTION ( 'NONE',  ( 0.000000000000000000, 5.300584669389750404E-15, -1.000000000000000000 ) ) ;
#55957 = CARTESIAN_POINT ( 'NONE',  ( 113.4874516948114547, -42.53221286317273098, 81.07189989340096758 ) ) ;
#55958 = CARTESIAN_POINT ( 'NONE',  ( 108.8525730979967676, -47.02250997168171409, 163.7127681330539701 ) ) ;
#55959 = DIRECTION ( 'NONE',  ( 0.000000000000000000, 0.000000000000000000, -1.000000000000000000 ) ) ;
#55960 = ORIENTED_EDGE ( 'NONE', *, *, #4813, .F. ) ;
#55961 = EDGE_CURVE ( 'NONE', #15070, #28045, #4297, .T. ) ;
#55962 = VECTOR ( 'NONE', #64000, 1000.000000000000114 ) ;
#55963 = FACE_OUTER_BOUND ( 'NONE', #67014, .T. ) ;
#55964 = ORIENTED_EDGE ( 'NONE', *, *, #14348, .F. ) ;
#55965 = EDGE_LOOP ( 'NONE', ( #76252, #69548, #59319, #53269 ) ) ;
#55966 = DIRECTION ( 'NONE',  ( 0.000000000000000000, 0.000000000000000000, 1.000000000000000000 ) ) ;
#55967 = ORIENTED_EDGE ( 'NONE', *, *, #67009, .F. ) ;
#55968 = EDGE_LOOP ( 'NONE', ( #32352, #54171 ) ) ;
#55969 = DIRECTION ( 'NONE',  ( 0.000000000000000000, 0.000000000000000000, 1.000000000000000000 ) ) ;
#55970 = AXIS2_PLACEMENT_3D ( 'NONE', #61384, #48634, #82309 ) ;
#55971 = CYLINDRICAL_SURFACE ( 'NONE', #1119, 1.999999999999995781 ) ;
#55972 = CARTESIAN_POINT ( 'NONE',  ( 115.1845888671227556, -34.07379402343466523, 88.50099125664800681 ) ) ;
#55973 = CARTESIAN_POINT ( 'NONE',  ( 106.9401735163927611, -47.80552439772274909, 232.5794347997199907 ) ) ;
#55974 = CARTESIAN_POINT ( 'NONE',  ( 97.11708974113231818, -41.49110554365062598, 216.6937205140059461 ) ) ;
#55975 = DIRECTION ( 'NONE',  ( 1.000000000000000000, 0.000000000000000000, 2.283216351027200160E-14 ) ) ;
#55976 = CYLINDRICAL_SURFACE ( 'NONE', #64208, 12.70000000000000107 ) ;
#55977 = EDGE_CURVE ( 'NONE', #80780, #11707, #37478, .T. ) ;
#55978 = EDGE_LOOP ( 'NONE', ( #69024, #59305 ) ) ;
#55979 = CARTESIAN_POINT ( 'NONE',  ( 115.8232288109526991, -31.72620974502509483, 90.24013890756648948 ) ) ;
#55980 = DIRECTION ( 'NONE',  ( 0.000000000000000000, -1.000000000000000000, 0.000000000000000000 ) ) ;
#55981 = CARTESIAN_POINT ( 'NONE',  ( 70.60763308006013972, -139.6429023009440016, 247.2863130087092429 ) ) ;
#55982 = CARTESIAN_POINT ( 'NONE',  ( 103.4440497394145808, -45.85039829771051245, 117.2756252759109543 ) ) ;
#55983 = ADVANCED_FACE ( 'NONE', ( #2959 ), #44270, .T. ) ;
#55984 = CARTESIAN_POINT ( 'NONE',  ( 108.9933628702935238, -47.01991853554855538, 82.72419670448194040 ) ) ;
#55985 = CARTESIAN_POINT ( 'NONE',  ( 111.8844023637430638, -46.06429852124467317, 272.9556252759110180 ) ) ;
#55986 = ORIENTED_EDGE ( 'NONE', *, *, #65777, .T. ) ;
#55987 = CARTESIAN_POINT ( 'NONE',  ( 116.8850244782298091, -41.80638879970206290, 243.4346728949589647 ) ) ;
#55988 = CARTESIAN_POINT ( 'NONE',  ( 74.06670390244704549, -118.2784471599409812, 222.2178068554179902 ) ) ;
#55989 = CARTESIAN_POINT ( 'NONE',  ( 10.57409824832103418, 75.51590200896762894, 130.1270826008356778 ) ) ;
#55990 = FACE_OUTER_BOUND ( 'NONE', #18440, .T. ) ;
#55992 = DIRECTION ( 'NONE',  ( 0.9659258262890693114, 0.000000000000000000, 0.2588190451025170757 ) ) ;
#55991 = DIRECTION ( 'NONE',  ( 0.000000000000000000, 1.000000000000000000, 0.000000000000000000 ) ) ;
#55993 = CARTESIAN_POINT ( 'NONE',  ( 105.8056005331014688, -25.33960583424948965, 320.7503373063622689 ) ) ;
#55994 = DIRECTION ( 'NONE',  ( 1.000000000000000000, 1.000000000000000078E-15, 1.000000000000000078E-15 ) ) ;
#55995 = DIRECTION ( 'NONE',  ( 1.248844797103662002E-15, 0.000000000000000000, -1.000000000000000000 ) ) ;
#55996 = CARTESIAN_POINT ( 'NONE',  ( -3.298961202091059697, 94.84210650921832553, 130.5168528568578097 ) ) ;
#55997 = FACE_OUTER_BOUND ( 'NONE', #20905, .T. ) ;
#55998 = DIRECTION ( 'NONE',  ( -1.000000000000000000, -0.000000000000000000, -0.000000000000000000 ) ) ;
#56000 = ORIENTED_EDGE ( 'NONE', *, *, #80365, .T. ) ;
#55999 = CARTESIAN_POINT ( 'NONE',  ( 120.1849926298398685, -37.85453553205689303, 247.7440089327910755 ) ) ;
#56001 = CARTESIAN_POINT ( 'NONE',  ( 108.9744791726667756, -131.7784471599409244, 250.2178068554180470 ) ) ;
#56002 = CARTESIAN_POINT ( 'NONE',  ( 110.7409072761653306, -26.27985149715145496, 254.8194347997204545 ) ) ;
#56003 = CARTESIAN_POINT ( 'NONE',  ( 108.2778103265350893, -47.71616603169876214, 153.6518157521009584 ) ) ;
#56004 = CARTESIAN_POINT ( 'NONE',  ( 109.6172575917244529, -25.13135243900233817, 25.90419670448196143 ) ) ;
#56005 = AXIS2_PLACEMENT_3D ( 'NONE', #45343, #78578, #72187 ) ;
#56006 = CARTESIAN_POINT ( 'NONE',  ( 107.0664832912739968, -18.82844715994099971, 168.9256252759119832 ) ) ;
#56008 = DIRECTION ( 'NONE',  ( 0.000000000000000000, 1.000000000000000000, 0.000000000000000000 ) ) ;
#56007 = LINE ( 'NONE', #70570, #49262 ) ;
#56009 = CARTESIAN_POINT ( 'NONE',  ( 98.04148634841929777, -41.04178939192217968, 137.6811862625705487 ) ) ;
#56010 = DIRECTION ( 'NONE',  ( 1.000000000000000000, 4.299999999999999979E-14, 1.000000000000000078E-15 ) ) ;
#56011 = VECTOR ( 'NONE', #53690, 1000.000000000000000 ) ;
#56012 = AXIS2_PLACEMENT_3D ( 'NONE', #87531, #25291, #52959 ) ;
#56013 = VECTOR ( 'NONE', #26576, 1000.000000000000000 ) ;
#56014 = ORIENTED_EDGE ( 'NONE', *, *, #26606, .F. ) ;
#56015 = DIRECTION ( 'NONE',  ( 0.000000000000000000, -1.000000000000000000, 0.000000000000000000 ) ) ;
#56016 = EDGE_LOOP ( 'NONE', ( #65052, #10826, #73545, #9273 ) ) ;
#56017 = EDGE_CURVE ( 'NONE', #55800, #46111, #16591, .T. ) ;
#56018 = CARTESIAN_POINT ( 'NONE',  ( 113.0289883941274525, -30.57309799635150682, 173.8867055423629608 ) ) ;
#56020 = ORIENTED_EDGE ( 'NONE', *, *, #30619, .T. ) ;
#56019 = CARTESIAN_POINT ( 'NONE',  ( 142.0664832912740394, -45.72944715994099596, 14.67562527591100441 ) ) ;
#56021 = DIRECTION ( 'NONE',  ( 0.000000000000000000, 1.000000000000000000, 0.000000000000000000 ) ) ;
#56022 = EDGE_CURVE ( 'NONE', #28034, #34082, #73151, .T. ) ;
#56023 = CARTESIAN_POINT ( 'NONE',  ( 102.8528367378537922, -46.24122135049434235, 173.2441967044829596 ) ) ;
#56024 = DIRECTION ( 'NONE',  ( -3.100000000000000258E-29, 3.100000000000000044E-14, 1.000000000000000000 ) ) ;
#56025 = DIRECTION ( 'NONE',  ( 0.000000000000000000, 0.000000000000000000, -1.000000000000000000 ) ) ;
#56026 = CARTESIAN_POINT ( 'NONE',  ( -254.0000000000000000, 14.28749999999982201, 90.48749999999999716 ) ) ;
#56027 = CARTESIAN_POINT ( 'NONE',  ( -86.67600044576296625, 70.52018178143200089, 80.88853703239344384 ) ) ;
#56028 = EDGE_CURVE ( 'NONE', #55859, #14474, #72007, .T. ) ;
#56029 = CARTESIAN_POINT ( 'NONE',  ( -76.20505178924278766, 127.0000000000000000, -76.20505178924469192 ) ) ;
#56031 = CARTESIAN_POINT ( 'NONE',  ( 117.1895451461017643, -38.97942580829906944, 103.6403871806739545 ) ) ;
#56030 = AXIS2_PLACEMENT_3D ( 'NONE', #56876, #21940, #64603 ) ;
#56032 = VERTEX_POINT ( 'NONE', #24300 ) ;
#56033 = ORIENTED_EDGE ( 'NONE', *, *, #16581, .F. ) ;
#56034 = EDGE_LOOP ( 'NONE', ( #23463, #16277, #26440, #12320 ) ) ;
#56035 = CARTESIAN_POINT ( 'NONE',  ( 113.8294273123088374, -42.50220367264088139, 59.69586902018298247 ) ) ;
#56036 = CARTESIAN_POINT ( 'NONE',  ( 134.5667039024469886, -102.5864808479222319, 250.2178068554180470 ) ) ;
#56037 =( BOUNDED_CURVE ( )  B_SPLINE_CURVE ( 3, ( #5945, #67710, #18212, #73170 ),
 .UNSPECIFIED., .F., .T. ) 
 B_SPLINE_CURVE_WITH_KNOTS ( ( 4, 4 ),
 ( 6.634086817347963434E-13, 1.570796326796151110 ),
 .UNSPECIFIED. ) 
 CURVE ( )  GEOMETRIC_REPRESENTATION_ITEM ( )  RATIONAL_B_SPLINE_CURVE ( ( 1.000000000000000000, 0.8047378541242256045, 0.8047378541242256045, 1.000000000000000000 ) ) 
 REPRESENTATION_ITEM ( '' )  );
#56039 = CARTESIAN_POINT ( 'NONE',  ( 113.1782938136983603, -44.75186855938550679, 38.09395861350527213 ) ) ;
#56038 = CARTESIAN_POINT ( 'NONE',  ( 117.2759483237919085, -34.91131378075003511, 194.9546728949579517 ) ) ;
#56040 = CIRCLE ( 'NONE', #70533, 117.5559999999999974 ) ;
#56041 = CARTESIAN_POINT ( 'NONE',  ( 97.07211459577071366, -35.37809379564900070, 56.21790486657103258 ) ) ;
#56042 = CARTESIAN_POINT ( 'NONE',  ( 41.56648329127399677, -18.82844715994099971, 258.9256252759120116 ) ) ;
#56043 = EDGE_CURVE ( 'NONE', #2932, #36690, #45573, .T. ) ;
#56044 = CARTESIAN_POINT ( 'NONE',  ( -487.2989999999999782, 6.038608028953049711, 90.48749999999999716 ) ) ;
#56045 = CARTESIAN_POINT ( 'NONE',  ( 117.4590087478601390, -115.7784471599421181, -21.78219314458165812 ) ) ;
#56046 = CARTESIAN_POINT ( 'NONE',  ( 67.07271190493912627, -67.88299602618702977, 245.6488590705319268 ) ) ;
#56047 = CARTESIAN_POINT ( 'NONE',  ( 102.3703197837810279, -46.01248081495484854, 127.2041967044829960 ) ) ;
#56048 = ORIENTED_EDGE ( 'NONE', *, *, #24940, .T. ) ;
#56049 = ORIENTED_EDGE ( 'NONE', *, *, #70026, .T. ) ;
#56050 = ORIENTED_EDGE ( 'NONE', *, *, #62547, .T. ) ;
#56051 = CARTESIAN_POINT ( 'NONE',  ( 12.27515439545620701, 79.26608163778621474, 129.9777074703579842 ) ) ;
#56052 = CARTESIAN_POINT ( 'NONE',  ( -492.0614999999999668, 93.66249999999999432, 15.87500000000039968 ) ) ;
#56053 = CARTESIAN_POINT ( 'NONE',  ( 117.0718954856374552, -35.46248235797460779, 79.92729194244158464 ) ) ;
#56054 = DIRECTION ( 'NONE',  ( 0.000000000000000000, -1.000000000000000000, 0.000000000000000000 ) ) ;
#56055 = CARTESIAN_POINT ( 'NONE',  ( 107.4574165340472263, -45.37514529517124373, 190.4185665600669779 ) ) ;
#56056 = VECTOR ( 'NONE', #18091, 1000.000000000000000 ) ;
#56057 = CARTESIAN_POINT ( 'NONE',  ( 72.06648329127396835, -9.729447159941065237, 14.92562527591093691 ) ) ;
#56058 = B_SPLINE_CURVE_WITH_KNOTS ( 'NONE', 3,
 ( #1968, #71466, #9228, #36928, #49190, #76926, #64629, #85547, #21522, #14704, #42375, #70104, #7879, #30561, #4193, #10554, #85988, #25077 ),
 .UNSPECIFIED., .F., .F.,
 ( 4, 2, 2, 2, 2, 2, 2, 2, 4 ),
 ( 0.4999831371813419079, 0.5624852450336741416, 0.6249873528860063754, 0.6874894607383387202, 0.7499915685906709539, 0.8124936764430031877, 0.8749957842953355325, 0.9374978921476677662, 1.000000000000000000 ),
 .UNSPECIFIED. ) ;
#56059 = CARTESIAN_POINT ( 'NONE',  ( 112.1403329462429639, -28.01338855262134686, 25.65604057059988108 ) ) ;
#56060 = ORIENTED_EDGE ( 'NONE', *, *, #66928, .F. ) ;
#56062 = VERTEX_POINT ( 'NONE', #80166 ) ;
#56061 = ORIENTED_EDGE ( 'NONE', *, *, #65783, .F. ) ;
#56063 = DIRECTION ( 'NONE',  ( 0.4999999999999998890, 0.000000000000000000, -0.8660254037844387076 ) ) ;
#56064 = ORIENTED_EDGE ( 'NONE', *, *, #52227, .F. ) ;
#56065 = VERTEX_POINT ( 'NONE', #17913 ) ;
#56066 = CARTESIAN_POINT ( 'NONE',  ( 79.68962695804320617, -21.47945062089174684, 8.225625248534930378 ) ) ;
#56067 = CARTESIAN_POINT ( 'NONE',  ( 106.9593448401346620, -46.12439510495315886, 229.0111071154209696 ) ) ;
#56068 = CARTESIAN_POINT ( 'NONE',  ( 204.2160000000000082, 52.73749999999999716, -44.45000000000000284 ) ) ;
#56069 = ORIENTED_EDGE ( 'NONE', *, *, #67431, .T. ) ;
#56070 = ADVANCED_FACE ( 'NONE', ( #45592 ), #64487, .F. ) ;
#56071 = LINE ( 'NONE', #49720, #1542 ) ;
#56072 = CARTESIAN_POINT ( 'NONE',  ( -124.4872849904342189, 71.15633340822272146, 39.34666567088954992 ) ) ;
#56073 = ORIENTED_EDGE ( 'NONE', *, *, #55931, .T. ) ;
#56074 = ORIENTED_EDGE ( 'NONE', *, *, #78887, .T. ) ;
#56075 = VECTOR ( 'NONE', #84761, 1000.000000000000000 ) ;
#56076 = VECTOR ( 'NONE', #50027, 1000.000000000000000 ) ;
#56077 = CARTESIAN_POINT ( 'NONE',  ( 21.03715912545739641, -47.82818131006197149, 180.4678068554150911 ) ) ;
#56078 = ORIENTED_EDGE ( 'NONE', *, *, #64316, .T. ) ;
#56079 = ORIENTED_EDGE ( 'NONE', *, *, #63491, .F. ) ;
#56080 = ADVANCED_FACE ( 'NONE', ( #31987 ), #44099, .F. ) ;
#56081 = CARTESIAN_POINT ( 'NONE',  ( 111.4490224358278994, -43.61588866942526721, 260.8452332267341376 ) ) ;
#56082 = CARTESIAN_POINT ( 'NONE',  ( 103.4607332334527001, -46.53479866174185986, 142.2956252759109645 ) ) ;
#56083 = CARTESIAN_POINT ( 'NONE',  ( 97.28692064948100438, -31.62807703868913833, 90.93181575210196854 ) ) ;
#56084 = CARTESIAN_POINT ( 'NONE',  ( 194.0371591254575492, -24.42818131005417115, 129.9678068554150343 ) ) ;
#56085 = DIRECTION ( 'NONE',  ( 3.999999999999999995E-14, -1.000000000000000000, 4.100000000000000342E-29 ) ) ;
#56086 = CARTESIAN_POINT ( 'NONE',  ( 97.09625178000921153, -41.50107833764869980, 212.6937205140059461 ) ) ;
#56087 = DIRECTION ( 'NONE',  ( 0.000000000000000000, 1.000000000000000000, 0.000000000000000000 ) ) ;
#56088 = DIRECTION ( 'NONE',  ( 0.000000000000000000, 0.000000000000000000, 1.000000000000000000 ) ) ;
#56089 = ORIENTED_EDGE ( 'NONE', *, *, #88236, .T. ) ;
#56090 = LINE ( 'NONE', #20263, #26458 ) ;
#56091 = ORIENTED_EDGE ( 'NONE', *, *, #68276, .F. ) ;
#56092 = EDGE_LOOP ( 'NONE', ( #81394, #87229, #67469, #7691 ) ) ;
#56093 = DIRECTION ( 'NONE',  ( 0.000000000000000000, 0.000000000000000000, -1.000000000000000000 ) ) ;
#56094 = AXIS2_PLACEMENT_3D ( 'NONE', #29985, #58124, #21378 ) ;
#56095 = CARTESIAN_POINT ( 'NONE',  ( 97.70649186885867721, -40.25113332959050183, 137.6128355545769466 ) ) ;
#56096 = ADVANCED_FACE ( 'NONE', ( #53748 ), #33338, .T. ) ;
#56097 = EDGE_LOOP ( 'NONE', ( #73769, #44591, #65731, #11899 ) ) ;
#56098 = CARTESIAN_POINT ( 'NONE',  ( 108.9848901524495801, -47.61516268848960465, 122.7032443235299723 ) ) ;
#56099 = CARTESIAN_POINT ( 'NONE',  ( 167.7413838386819691, -48.33240602328260849, 129.9678068554150059 ) ) ;
#56100 = PLANE ( 'NONE',  #39190 ) ;
#56101 = LINE ( 'NONE', #2518, #60104 ) ;
#56104 = CARTESIAN_POINT ( 'NONE',  ( 117.3134009501234658, -34.93240959161192905, 239.9641967044819637 ) ) ;
#56103 = CARTESIAN_POINT ( 'NONE',  ( 116.7787425647057091, -34.05740579004297075, 59.03918106495919460 ) ) ;
#56102 = FACE_OUTER_BOUND ( 'NONE', #28113, .T. ) ;
#56105 = CARTESIAN_POINT ( 'NONE',  ( 106.5667039024470313, -108.2470741265389620, -19.78219314458190681 ) ) ;
#56106 = FACE_OUTER_BOUND ( 'NONE', #79916, .T. ) ;
#56107 = ORIENTED_EDGE ( 'NONE', *, *, #87529, .T. ) ;
#56108 = DIRECTION ( 'NONE',  ( -6.245004513516504751E-15, 0.000000000000000000, -1.000000000000000000 ) ) ;
#56109 = DIRECTION ( 'NONE',  ( 0.000000000000000000, 0.000000000000000000, -1.000000000000000000 ) ) ;
#56110 = LINE ( 'NONE', #82527, #45891 ) ;
#56111 = CARTESIAN_POINT ( 'NONE',  ( 146.5617523730059872, -137.3883890306192939, 246.8362840236234490 ) ) ;
#56113 = ORIENTED_EDGE ( 'NONE', *, *, #37660, .T. ) ;
#56112 = DIRECTION ( 'NONE',  ( -0.04216478779797398074, 0.9991106698809455455, 0.000000000000000000 ) ) ;
#56114 = CARTESIAN_POINT ( 'NONE',  ( 107.0667039024479834, -36.72944715994099596, 239.5838068554170093 ) ) ;
#56115 = CARTESIAN_POINT ( 'NONE',  ( 113.6284486023480724, -28.60005753680112761, 164.5356252759109736 ) ) ;
#56116 = CARTESIAN_POINT ( 'NONE',  ( 112.8177273059790764, -27.29031728650405597, 45.62895860924398761 ) ) ;
#56117 = CARTESIAN_POINT ( 'NONE',  ( 114.1542194384027908, -29.02509929289194801, 195.4841967044819739 ) ) ;
#56118 = CARTESIAN_POINT ( 'NONE',  ( 51.42025729304101844, -33.70561438051982606, 342.9256252759109884 ) ) ;
#56119 = LINE ( 'NONE', #83872, #27156 ) ;
#56121 = DIRECTION ( 'NONE',  ( 0.000000000000000000, 0.000000000000000000, 1.000000000000000000 ) ) ;
#56120 = CARTESIAN_POINT ( 'NONE',  ( 25.56670390244797275, -65.37844715994100397, 257.2178068554150059 ) ) ;
#56122 = CARTESIAN_POINT ( 'NONE',  ( -215.9000000000000057, 101.5999999999999943, -45.33899999999999864 ) ) ;
#56123 = CARTESIAN_POINT ( 'NONE',  ( 37.03715912545433042, -48.62818131006122258, 249.9678068554150343 ) ) ;
#56124 = VERTEX_POINT ( 'NONE', #19707 ) ;
#56125 = AXIS2_PLACEMENT_3D ( 'NONE', #1298, #43950, #78513 ) ;
#56126 = FACE_BOUND ( 'NONE', #69094, .T. ) ;
#56127 = ORIENTED_EDGE ( 'NONE', *, *, #36493, .F. ) ;
#56128 = VERTEX_POINT ( 'NONE', #60582 ) ;
#56129 = EDGE_CURVE ( 'NONE', #39780, #28327, #74674, .T. ) ;
#56131 = ORIENTED_EDGE ( 'NONE', *, *, #71944, .F. ) ;
#56130 = CARTESIAN_POINT ( 'NONE',  ( 184.5667039024480118, -67.87844715994100397, 20.91780685541479912 ) ) ;
#56132 = CARTESIAN_POINT ( 'NONE',  ( 110.3650187231686601, -47.25482062520513438, 48.80610146638797175 ) ) ;
#56133 = DIRECTION ( 'NONE',  ( 0.4214249218767882055, 0.9068632946707806397, 4.214249218767890910E-16 ) ) ;
#56134 = EDGE_CURVE ( 'NONE', #78126, #69728, #68760, .T. ) ;
#56135 = CARTESIAN_POINT ( 'NONE',  ( 107.5667039024470455, -113.7784471599420613, -19.78219314458171141 ) ) ;
#56136 = CARTESIAN_POINT ( 'NONE',  ( 117.1100247017212723, -39.68245506451066262, 179.5984824187679294 ) ) ;
#56137 = EDGE_CURVE ( 'NONE', #60854, #69462, #7939, .T. ) ;
#56138 = AXIS2_PLACEMENT_3D ( 'NONE', #55223, #76136, #89789 ) ;
#56139 = VECTOR ( 'NONE', #68060, 1000.000000000000000 ) ;
#56140 = CARTESIAN_POINT ( 'NONE',  ( 106.8780034376490278, -45.26880352128168283, 271.9809912566482808 ) ) ;
#56141 = VERTEX_POINT ( 'NONE', #39693 ) ;
#56142 = ORIENTED_EDGE ( 'NONE', *, *, #32195, .F. ) ;
#56143 = ORIENTED_EDGE ( 'NONE', *, *, #80691, .T. ) ;
#56144 = VECTOR ( 'NONE', #32325, 1000.000000000000000 ) ;
#56145 = AXIS2_PLACEMENT_3D ( 'NONE', #24917, #88499, #82141 ) ;
#56146 = ORIENTED_EDGE ( 'NONE', *, *, #15955, .F. ) ;
#56147 = LINE ( 'NONE', #70253, #42787 ) ;
#56148 = LINE ( 'NONE', #70708, #65248 ) ;
#56149 = VECTOR ( 'NONE', #66570, 999.9999999999998863 ) ;
#56150 = DIRECTION ( 'NONE',  ( -1.000000000000000078E-15, 0.000000000000000000, -1.000000000000000000 ) ) ;
#56151 = LINE ( 'NONE', #35723, #29597 ) ;
#56152 = CARTESIAN_POINT ( 'NONE',  ( 91.13664476550619042, 95.14808745951974345, 93.48344774443376082 ) ) ;
#56153 = CARTESIAN_POINT ( 'NONE',  ( 177.0371591254545933, -48.62818131005479927, 129.9678068554150059 ) ) ;
#56154 = ADVANCED_FACE ( 'NONE', ( #26082 ), #33783, .F. ) ;
#56155 = CARTESIAN_POINT ( 'NONE',  ( 48.16670390244647137, -26.71338133339281029, 193.9678068554150911 ) ) ;
#56156 = CARTESIAN_POINT ( 'NONE',  ( -11.73779877120047743, 87.39914602784801900, 130.0272786502210067 ) ) ;
#56157 = EDGE_CURVE ( 'NONE', #36065, #73817, #54196, .T. ) ;
#56158 = CARTESIAN_POINT ( 'NONE',  ( 100.6111884388666766, -28.52632756463403751, 15.60705384733995871 ) ) ;
#56159 = DIRECTION ( 'NONE',  ( 0.000000000000000000, 0.000000000000000000, -1.000000000000000000 ) ) ;
#56160 = VERTEX_POINT ( 'NONE', #61929 ) ;
#56161 = AXIS2_PLACEMENT_3D ( 'NONE', #29882, #78929, #2622 ) ;
#56162 = CARTESIAN_POINT ( 'NONE',  ( 97.07207223047387856, -35.37843998912999410, 271.2189585129040097 ) ) ;
#56163 = CIRCLE ( 'NONE', #22811, 8.999999999999994671 ) ;
#56164 = AXIS2_PLACEMENT_3D ( 'NONE', #8537, #77130, #29879 ) ;
#56165 = DIRECTION ( 'NONE',  ( -3.999999999999999995E-14, 1.000000000000000000, -4.100000000000000342E-29 ) ) ;
#56166 = CARTESIAN_POINT ( 'NONE',  ( 99.36125835269150741, -32.78858003560463175, 93.78047132197198721 ) ) ;
#56167 = CONICAL_SURFACE ( 'NONE', #80850, 188.9759999999999991, 0.7853981633974758125 ) ;
#56168 = CARTESIAN_POINT ( 'NONE',  ( 182.4202572930406916, -33.70561438051399961, 313.9678068554149490 ) ) ;
#56169 = CARTESIAN_POINT ( 'NONE',  ( 112.1393456408476510, -28.01282278068320508, 44.65645860931923750 ) ) ;
#56170 = ORIENTED_EDGE ( 'NONE', *, *, #37826, .T. ) ;
#56171 = ORIENTED_EDGE ( 'NONE', *, *, #4171, .T. ) ;
#56172 = CARTESIAN_POINT ( 'NONE',  ( 97.81553679132888135, -40.52681664444901344, 136.6368110416782145 ) ) ;
#56173 = ORIENTED_EDGE ( 'NONE', *, *, #40737, .F. ) ;
#56174 = ORIENTED_EDGE ( 'NONE', *, *, #277, .T. ) ;
#56175 = CARTESIAN_POINT ( 'NONE',  ( 99.22037001696983793, -32.61037140242165577, 132.3730118773259790 ) ) ;
#56176 = DIRECTION ( 'NONE',  ( 0.000000000000000000, -0.000000000000000000, -1.000000000000000000 ) ) ;
#56177 = CONICAL_SURFACE ( 'NONE', #25788, 5.799999999999998934, 0.7853981633974369547 ) ;
#56178 = CARTESIAN_POINT ( 'NONE',  ( 114.0366484478682310, -28.94779845652852757, 110.4956252759109816 ) ) ;
#56179 = AXIS2_PLACEMENT_3D ( 'NONE', #2086, #70226, #8000 ) ;
#56180 = DIRECTION ( 'NONE',  ( 0.000000000000000000, 0.000000000000000000, 1.000000000000000000 ) ) ;
#56181 = ORIENTED_EDGE ( 'NONE', *, *, #69384, .T. ) ;
#56182 = ORIENTED_EDGE ( 'NONE', *, *, #85526, .F. ) ;
#56183 = ORIENTED_EDGE ( 'NONE', *, *, #6513, .T. ) ;
#56184 = EDGE_CURVE ( 'NONE', #46552, #69245, #87861, .T. ) ;
#56185 = DIRECTION ( 'NONE',  ( 6.745093096447288888E-17, 1.000000000000000000, 0.000000000000000000 ) ) ;
#56186 = ORIENTED_EDGE ( 'NONE', *, *, #68222, .T. ) ;
#56187 = CARTESIAN_POINT ( 'NONE',  ( 117.4903696573864522, -37.28369426754697002, 18.78419670448294809 ) ) ;
#56188 = CARTESIAN_POINT ( 'NONE',  ( 98.64836624540230048, -30.48328824330908660, 176.8184824187679567 ) ) ;
#56189 = CYLINDRICAL_SURFACE ( 'NONE', #80016, 16.00000000000090239 ) ;
#56190 = CARTESIAN_POINT ( 'NONE',  ( 83.56670390244801183, -37.98819715994108037, 218.8274735512160589 ) ) ;
#56191 = CARTESIAN_POINT ( 'NONE',  ( 116.9041476981693677, -40.17949737190902937, 129.5584824187679658 ) ) ;
#56192 = PLANE ( 'NONE',  #61086 ) ;
#56193 = ORIENTED_EDGE ( 'NONE', *, *, #51022, .T. ) ;
#56194 = PLANE ( 'NONE',  #1772 ) ;
#56195 = CONICAL_SURFACE ( 'NONE', #24332, 10.00000000000000888, 0.7853981633974691512 ) ;
#56196 = DIRECTION ( 'NONE',  ( -1.000000000000000000, -3.999999999999999995E-14, 4.193851878741028267E-47 ) ) ;
#56197 = ORIENTED_EDGE ( 'NONE', *, *, #32658, .T. ) ;
#56198 = AXIS2_PLACEMENT_3D ( 'NONE', #35811, #8573, #63526 ) ;
#56199 = CARTESIAN_POINT ( 'NONE',  ( 97.06670390244703128, -104.2784471599412228, 7.717806855417980394 ) ) ;
#56201 = EDGE_CURVE ( 'NONE', #33687, #14469, #39823, .T. ) ;
#56200 = VECTOR ( 'NONE', #16954, 1000.000000000000000 ) ;
#56202 = CARTESIAN_POINT ( 'NONE',  ( 1.651468531095106718, 95.06824417558520679, 118.5472321064814452 ) ) ;
#56203 = CARTESIAN_POINT ( 'NONE',  ( 96.34404753607181249, -39.41381804822120216, 16.53372051400597798 ) ) ;
#56204 = CARTESIAN_POINT ( 'NONE',  ( 19.18896583590734650, 64.29237593614118396, 32.91936650831844702 ) ) ;
#56205 = LINE ( 'NONE', #34436, #24611 ) ;
#56206 = DIRECTION ( 'NONE',  ( 1.000000000000000000, 0.000000000000000000, 0.000000000000000000 ) ) ;
#56207 = CARTESIAN_POINT ( 'NONE',  ( 110.2835424219824034, -44.64187515646635518, 282.3067055423625789 ) ) ;
#56209 = CARTESIAN_POINT ( 'NONE',  ( 95.33621695423336462, -38.27597901479983733, 147.4299109901969871 ) ) ;
#56208 = DIRECTION ( 'NONE',  ( -1.000000000000000078E-15, 1.000000000000000083E-30, 1.000000000000000000 ) ) ;
#56210 = CARTESIAN_POINT ( 'NONE',  ( 105.7995184819918535, -26.72403496654249011, 71.17729194302346230 ) ) ;
#56211 = DIRECTION ( 'NONE',  ( 0.000000000000000000, 1.000000000000000000, 0.000000000000000000 ) ) ;
#56212 = ORIENTED_EDGE ( 'NONE', *, *, #73056, .F. ) ;
#56213 = CYLINDRICAL_SURFACE ( 'NONE', #62813, 3.000000000000002665 ) ;
#56214 = CARTESIAN_POINT ( 'NONE',  ( 75.31670390244798341, -57.40094715994099772, 35.51780685541480409 ) ) ;
#56215 = LINE ( 'NONE', #37149, #16615 ) ;
#56216 = ORIENTED_EDGE ( 'NONE', *, *, #36217, .T. ) ;
#56217 = CIRCLE ( 'NONE', #15670, 6.349999999999994316 ) ;
#56218 = EDGE_CURVE ( 'NONE', #71147, #18287, #54332, .T. ) ;
#56219 = LINE ( 'NONE', #83970, #7110 ) ;
#56221 = ORIENTED_EDGE ( 'NONE', *, *, #81708, .T. ) ;
#56220 = CARTESIAN_POINT ( 'NONE',  ( 102.8260968645185045, -46.30158323273214904, 177.2441967044819648 ) ) ;
#56222 = FACE_OUTER_BOUND ( 'NONE', #45822, .T. ) ;
#56223 = CARTESIAN_POINT ( 'NONE',  ( 113.0346028865331363, -45.34691455509256031, 199.0584824187679374 ) ) ;
#56224 = CARTESIAN_POINT ( 'NONE',  ( 96.13205292066136565, -38.63620640773733328, 42.45181575210199298 ) ) ;
#56225 = AXIS2_PLACEMENT_3D ( 'NONE', #41414, #19644, #67796 ) ;
#56226 = CARTESIAN_POINT ( 'NONE',  ( 63.06670390244736524, -24.92844715994017690, 249.9678068554150343 ) ) ;
#56227 = AXIS2_PLACEMENT_3D ( 'NONE', #87738, #74553, #60462 ) ;
#56228 = LINE ( 'NONE', #77156, #54615 ) ;
#56229 = DIRECTION ( 'NONE',  ( -6.524622321627019585E-16, -4.013151879589939944E-16, -1.000000000000000000 ) ) ;
#56230 = ORIENTED_EDGE ( 'NONE', *, *, #68472, .T. ) ;
#56231 = AXIS2_PLACEMENT_3D ( 'NONE', #89365, #75728, #88472 ) ;
#56232 = EDGE_CURVE ( 'NONE', #21135, #17509, #89189, .T. ) ;
#56233 = VERTEX_POINT ( 'NONE', #81959 ) ;
#56234 = ORIENTED_EDGE ( 'NONE', *, *, #41461, .T. ) ;
#56235 = VERTEX_POINT ( 'NONE', #41038 ) ;
#56236 = DIRECTION ( 'NONE',  ( 0.7071067809773464719, -0.7071067813957485626, 7.071067809773160819E-16 ) ) ;
#56237 = CARTESIAN_POINT ( 'NONE',  ( 101.2940058763137330, -26.37990030743140224, 251.4813395616249920 ) ) ;
#56238 = CARTESIAN_POINT ( 'NONE',  ( -71.09939861440099662, 101.5999999999999943, 177.8662485265279827 ) ) ;
#56239 = DIRECTION ( 'NONE',  ( 0.000000000000000000, -1.000000000000000000, 0.000000000000000000 ) ) ;
#56240 = EDGE_CURVE ( 'NONE', #44500, #59691, #75123, .T. ) ;
#56242 = CARTESIAN_POINT ( 'NONE',  ( 182.4202572930259976, -31.94127993907710206, -5.074374724088000832 ) ) ;
#56241 = LINE ( 'NONE', #14040, #87376 ) ;
#56243 = CARTESIAN_POINT ( 'NONE',  ( 210.5660000000000025, 52.73749999999999716, -49.21249999999999858 ) ) ;
#56244 = CARTESIAN_POINT ( 'NONE',  ( 111.3322245453084918, -27.19268589797737334, 24.74133956162494030 ) ) ;
#56245 = ORIENTED_EDGE ( 'NONE', *, *, #59230, .F. ) ;
#56246 = CIRCLE ( 'NONE', #15697, 10.00000000000000355 ) ;
#56247 = ORIENTED_EDGE ( 'NONE', *, *, #37709, .F. ) ;
#56248 = CARTESIAN_POINT ( 'NONE',  ( 151.0371591254575776, -24.42818131005592264, 129.9678068554149775 ) ) ;
#56249 = CARTESIAN_POINT ( 'NONE',  ( 97.53179058352803565, -39.74878676319904969, 17.57055365400502822 ) ) ;
#56250 = CARTESIAN_POINT ( 'NONE',  ( 115.4995704134666141, -41.68388727776409297, 234.4041967044819899 ) ) ;
#56251 = CARTESIAN_POINT ( 'NONE',  ( -48.26476610531312872, 65.59999999999998010, 65.76796570303407918 ) ) ;
#56252 = EDGE_CURVE ( 'NONE', #26653, #32576, #12907, .T. ) ;
#56253 = CARTESIAN_POINT ( 'NONE',  ( 116.0809032858470999, -32.84949784884748425, 75.14991099019596277 ) ) ;
#56255 = EDGE_CURVE ( 'NONE', #7616, #19968, #40596, .T. ) ;
#56254 = LINE ( 'NONE', #14961, #57393 ) ;
#56256 = ADVANCED_FACE ( 'NONE', ( #20168, #75580, #13351 ), #46044, .F. ) ;
#56257 = DIRECTION ( 'NONE',  ( 0.000000000000000000, 0.000000000000000000, -1.000000000000000000 ) ) ;
#56258 = ORIENTED_EDGE ( 'NONE', *, *, #68560, .F. ) ;
#56259 = LINE ( 'NONE', #73376, #5135 ) ;
#56260 = ADVANCED_FACE ( 'NONE', ( #32424 ), #60127, .F. ) ;
#56261 = CIRCLE ( 'NONE', #62055, 5.599999999999994316 ) ;
#56262 = ORIENTED_EDGE ( 'NONE', *, *, #56951, .F. ) ;
#56263 = EDGE_LOOP ( 'NONE', ( #8189, #67844, #27071, #58174 ) ) ;
#56264 = CARTESIAN_POINT ( 'NONE',  ( -78.95047879920342382, 93.33860577356860233, 88.44471653959794821 ) ) ;
#56265 = CARTESIAN_POINT ( 'NONE',  ( 106.3528233092926740, -46.09786297945525035, 263.9596785439923678 ) ) ;
#56266 = AXIS2_PLACEMENT_3D ( 'NONE', #4206, #25089, #87328 ) ;
#56267 = CARTESIAN_POINT ( 'NONE',  ( 140.0667039024470455, -118.2784471599408960, 230.7030882296565721 ) ) ;
#56268 = CIRCLE ( 'NONE', #8464, 188.9759999999999991 ) ;
#56269 = CARTESIAN_POINT ( 'NONE',  ( -117.9583070260532764, 87.03046781249437913, 11.89069406032439247 ) ) ;
#56270 = DIRECTION ( 'NONE',  ( -0.7071067812164788524, 0.7071067811566160710, 0.000000000000000000 ) ) ;
#56271 = FACE_OUTER_BOUND ( 'NONE', #53817, .T. ) ;
#56272 = VERTEX_POINT ( 'NONE', #74234 ) ;
#56273 = CARTESIAN_POINT ( 'NONE',  ( 121.3178890780284434, -113.5468731908971165, -11.78219314458173272 ) ) ;
#56274 = AXIS2_PLACEMENT_3D ( 'NONE', #28829, #55595, #56512 ) ;
#56275 = CARTESIAN_POINT ( 'NONE',  ( 3.174999999999879918, 104.3431970271541900, 33.98325472291465132 ) ) ;
#56276 = ORIENTED_EDGE ( 'NONE', *, *, #15758, .T. ) ;
#56277 = CARTESIAN_POINT ( 'NONE',  ( 96.92686062739846875, -39.15330414739766240, 56.51276813305394597 ) ) ;
#56278 = ORIENTED_EDGE ( 'NONE', *, *, #69074, .F. ) ;
#56279 = CARTESIAN_POINT ( 'NONE',  ( 105.6358988306284346, -28.30874812457275524, 14.63241982807694797 ) ) ;
#56280 = CIRCLE ( 'NONE', #5611, 2.030000000000003801 ) ;
#56281 = CARTESIAN_POINT ( 'NONE',  ( -3.174999999999664979, 17.78000000000000114, 31.75000000000000000 ) ) ;
#56282 = CARTESIAN_POINT ( 'NONE',  ( 96.28008679191512442, -39.42493101749853679, 166.5213395616259788 ) ) ;
#56283 = DIRECTION ( 'NONE',  ( 1.607304094387810152E-29, -0.7071067811865555663, 0.7071067811865394681 ) ) ;
#56284 = CARTESIAN_POINT ( 'NONE',  ( 168.3664380525666218, -48.62818131005518296, 249.9678068554149775 ) ) ;
#56285 = VECTOR ( 'NONE', #36755, 1000.000000000000000 ) ;
#56286 = PLANE ( 'NONE',  #36128 ) ;
#56287 = VECTOR ( 'NONE', #70899, 1000.000000000000000 ) ;
#56288 = DIRECTION ( 'NONE',  ( -1.000000000000000078E-15, 1.000000000000000083E-30, 1.000000000000000000 ) ) ;
#56289 = CARTESIAN_POINT ( 'NONE',  ( 112.3603056216204550, -28.17164194844215430, 285.6356252759109680 ) ) ;
#56290 = CARTESIAN_POINT ( 'NONE',  ( 84.12159398442716451, 95.25015226514366873, -83.54193218351822736 ) ) ;
#56291 = VERTEX_POINT ( 'NONE', #36025 ) ;
#56292 = CARTESIAN_POINT ( 'NONE',  ( 136.8151996730033204, -36.82419990104954621, 6.751707299519810412 ) ) ;
#56293 = ORIENTED_EDGE ( 'NONE', *, *, #77938, .F. ) ;
#56294 = CARTESIAN_POINT ( 'NONE',  ( 103.1892778894433320, -46.49189014610453086, 113.2756252759109827 ) ) ;
#56295 = CARTESIAN_POINT ( 'NONE',  ( 119.6084552581333469, 51.66411822165594003, -52.33259208581855404 ) ) ;
#56296 = ORIENTED_EDGE ( 'NONE', *, *, #36764, .T. ) ;
#56297 = CARTESIAN_POINT ( 'NONE',  ( 115.8254323948531095, -31.73001883592735339, 119.2397919419617551 ) ) ;
#56298 = ORIENTED_EDGE ( 'NONE', *, *, #19109, .F. ) ;
#56299 = ORIENTED_EDGE ( 'NONE', *, *, #29743, .T. ) ;
#56300 = VECTOR ( 'NONE', #54508, 1000.000000000000000 ) ;
#56301 = DIRECTION ( 'NONE',  ( 1.000000000000000078E-15, 0.000000000000000000, 1.000000000000000000 ) ) ;
#56302 = CARTESIAN_POINT ( 'NONE',  ( 108.4174969398134323, -26.73503709278844198, 265.9689579970951172 ) ) ;
#56303 = FACE_BOUND ( 'NONE', #66562, .T. ) ;
#56304 = CARTESIAN_POINT ( 'NONE',  ( 179.7974245136200011, -36.32844715994040996, -5.074374724088000832 ) ) ;
#56305 = CARTESIAN_POINT ( 'NONE',  ( 194.0371591254584587, -46.82818131005407736, 193.9678068554150343 ) ) ;
#56306 = CARTESIAN_POINT ( 'NONE',  ( 105.4209835578153189, -47.02385428587647453, 33.44991099019695469 ) ) ;
#56307 = DIRECTION ( 'NONE',  ( 1.000000000000000000, -0.000000000000000000, 0.000000000000000000 ) ) ;
#56308 = ORIENTED_EDGE ( 'NONE', *, *, #84455, .F. ) ;
#56309 = CARTESIAN_POINT ( 'NONE',  ( 11.41159535906576217, 76.91451165865561279, 118.0059465515839747 ) ) ;
#56310 = AXIS2_PLACEMENT_3D ( 'NONE', #88609, #61320, #60419 ) ;
#56311 = DIRECTION ( 'NONE',  ( 0.000000000000000000, -1.000000000000000000, 0.000000000000000000 ) ) ;
#56312 = ORIENTED_EDGE ( 'NONE', *, *, #17367, .T. ) ;
#56314 = ORIENTED_EDGE ( 'NONE', *, *, #49200, .F. ) ;
#56313 = CIRCLE ( 'NONE', #30212, 0.5000000000000073275 ) ;
#56315 = DIRECTION ( 'NONE',  ( 0.000000000000000000, -1.000000000000000000, 0.000000000000000000 ) ) ;
#56316 = ADVANCED_FACE ( 'NONE', ( #8785 ), #21058, .F. ) ;
#56317 = DIRECTION ( 'NONE',  ( -1.000000000000000000, -8.540177112501204385E-16, 0.000000000000000000 ) ) ;
#56318 = CARTESIAN_POINT ( 'NONE',  ( -6.359898342742077659, 71.54935466043629333, -130.4015153071888733 ) ) ;
#56319 = EDGE_CURVE ( 'NONE', #1129, #68410, #14698, .T. ) ;
#56320 = DIRECTION ( 'NONE',  ( -2.981567257902526681E-15, 0.8571673007021100021, 0.5150380749100580413 ) ) ;
#56321 = LINE ( 'NONE', #62705, #76523 ) ;
#56322 = CARTESIAN_POINT ( 'NONE',  ( 97.51448592794399417, -38.47012922887837760, 200.8924198280769815 ) ) ;
#56323 = DIRECTION ( 'NONE',  ( -0.7071067811865165975, -0.7071067811865784369, -7.071067811865158803E-16 ) ) ;
#56324 = CARTESIAN_POINT ( 'NONE',  ( 113.4422559937560777, -27.64306140573813408, 84.57753003781698453 ) ) ;
#56325 = ORIENTED_EDGE ( 'NONE', *, *, #14940, .F. ) ;
#56326 = CARTESIAN_POINT ( 'NONE',  ( 162.5667039024460223, -19.82844715994111340, -5.074374724088000832 ) ) ;
#56327 = ORIENTED_EDGE ( 'NONE', *, *, #54234, .F. ) ;
#56328 = ADVANCED_FACE ( 'NONE', ( #21970 ), #62378, .T. ) ;
#56329 = CARTESIAN_POINT ( 'NONE',  ( -80.59807192910929530, 70.66242608954388515, -86.94609723791364786 ) ) ;
#56330 = ORIENTED_EDGE ( 'NONE', *, *, #45193, .T. ) ;
#56331 = EDGE_CURVE ( 'NONE', #74022, #7823, #81936, .T. ) ;
#56332 = CIRCLE ( 'NONE', #17197, 0.5000000000000004441 ) ;
#56333 = EDGE_CURVE ( 'NONE', #1134, #85218, #3591, .T. ) ;
#56334 = CARTESIAN_POINT ( 'NONE',  ( 112.1392665423922210, -28.01277399031326709, 49.65646589883106543 ) ) ;
#56335 = ORIENTED_EDGE ( 'NONE', *, *, #34811, .T. ) ;
#56336 = DIRECTION ( 'NONE',  ( -0.7071067811865274777, 0.7071067811865675568, -7.071067811865283048E-16 ) ) ;
#56337 = CARTESIAN_POINT ( 'NONE',  ( 241.3336515812914911, 40.03750000000000142, 10.66800000000000104 ) ) ;
#56338 = CARTESIAN_POINT ( 'NONE',  ( 112.0677311185675649, -45.48738121332133488, 273.9895100238672399 ) ) ;
#56339 = EDGE_CURVE ( 'NONE', #10437, #33219, #6978, .T. ) ;
#56341 = FACE_BOUND ( 'NONE', #34702, .T. ) ;
#56340 = VECTOR ( 'NONE', #89464, 1000.000000000000000 ) ;
#56342 = ORIENTED_EDGE ( 'NONE', *, *, #86310, .T. ) ;
#56343 = VECTOR ( 'NONE', #74620, 1000.000000000000000 ) ;
#56344 = CARTESIAN_POINT ( 'NONE',  ( 104.7546666864753320, -46.91776733316893200, 72.39848241876795498 ) ) ;
#56345 = FILL_AREA_STYLE ('',( #54982 ) ) ;
#56346 = ADVANCED_FACE ( 'NONE', ( #49636 ), #28300, .F. ) ;
#56348 = FACE_OUTER_BOUND ( 'NONE', #52122, .T. ) ;
#56347 = DIRECTION ( 'NONE',  ( 0.000000000000000000, 0.000000000000000000, -1.000000000000000000 ) ) ;
#56349 = LINE ( 'NONE', #27762, #14770 ) ;
#56350 = CARTESIAN_POINT ( 'NONE',  ( 80.06648329127402519, -46.72944715994105991, 4.925625275910944012 ) ) ;
#56351 = ORIENTED_EDGE ( 'NONE', *, *, #69793, .F. ) ;
#56352 = AXIS2_PLACEMENT_3D ( 'NONE', #4020, #89282, #88835 ) ;
#56353 = ADVANCED_FACE ( 'NONE', ( #56451 ), #13791, .T. ) ;
#56354 = DIRECTION ( 'NONE',  ( 0.000000000000000000, -1.000000000000000000, 0.000000000000000000 ) ) ;
#56355 = LINE ( 'NONE', #78187, #20776 ) ;
#56356 = EDGE_CURVE ( 'NONE', #51043, #18192, #61612, .T. ) ;
#56357 = VECTOR ( 'NONE', #17955, 999.9999999999998863 ) ;
#56358 = DIRECTION ( 'NONE',  ( -1.000000000000000000, -4.299999999999999979E-14, -1.000000000000000078E-15 ) ) ;
#56359 = CARTESIAN_POINT ( 'NONE',  ( 108.0361718062294614, -25.69563957016125855, 105.9946728949589811 ) ) ;
#56360 = VECTOR ( 'NONE', #5762, 1000.000000000000000 ) ;
#56362 = LINE ( 'NONE', #70014, #89180 ) ;
#56361 = DIRECTION ( 'NONE',  ( 0.000000000000000000, 0.000000000000000000, 1.000000000000000000 ) ) ;
#56363 = LINE ( 'NONE', #35927, #71253 ) ;
#56364 = ORIENTED_EDGE ( 'NONE', *, *, #41027, .F. ) ;
#56365 = DIRECTION ( 'NONE',  ( -1.000000000000000000, 0.000000000000000000, 0.000000000000000000 ) ) ;
#56366 = CARTESIAN_POINT ( 'NONE',  ( 108.9483104351207174, -46.92736419409149562, 123.7337205140059666 ) ) ;
#56367 = VECTOR ( 'NONE', #88961, 1000.000000000000000 ) ;
#56369 = ORIENTED_EDGE ( 'NONE', *, *, #36602, .T. ) ;
#56368 = CARTESIAN_POINT ( 'NONE',  ( 130.3998166246059895, 12.92155284005730387, 361.9756252759109998 ) ) ;
#56370 = ADVANCED_FACE ( 'NONE', ( #64189 ), #15141, .F. ) ;
#56371 = CARTESIAN_POINT ( 'NONE',  ( 118.0844448206163833, -36.21142561920247971, 264.8518157521014587 ) ) ;
#56372 = DIRECTION ( 'NONE',  ( 0.000000000000000000, 0.000000000000000000, -1.000000000000000000 ) ) ;
#56373 = CARTESIAN_POINT ( 'NONE',  ( 95.60734603896362671, -36.72944715994100306, 394.9756252759102040 ) ) ;
#56375 = EDGE_CURVE ( 'NONE', #3973, #960, #8327, .T. ) ;
#56374 = CARTESIAN_POINT ( 'NONE',  ( 94.20285697596281693, -79.89790063748488080, 250.2178068554180470 ) ) ;
#56376 = DIRECTION ( 'NONE',  ( 0.000000000000000000, 1.000000000000000000, 0.000000000000000000 ) ) ;
#56377 = EDGE_CURVE ( 'NONE', #58908, #80081, #83291, .T. ) ;
#56378 = FACE_OUTER_BOUND ( 'NONE', #13320, .T. ) ;
#56379 = CARTESIAN_POINT ( 'NONE',  ( 173.9900000000000091, 21.46300000000000097, 41.63456447661474868 ) ) ;
#56380 = EDGE_CURVE ( 'NONE', #22589, #84959, #2390, .T. ) ;
#56381 = CARTESIAN_POINT ( 'NONE',  ( 114.4768422515204946, -30.34587328852055066, 184.3927681330539770 ) ) ;
#56382 = ORIENTED_EDGE ( 'NONE', *, *, #60636, .F. ) ;
#56383 = VERTEX_POINT ( 'NONE', #44162 ) ;
#56384 = AXIS2_PLACEMENT_3D ( 'NONE', #53675, #4666, #47317 ) ;
#56385 = CARTESIAN_POINT ( 'NONE',  ( 113.4085779730985166, -29.80024602262787425, 150.9063452106589693 ) ) ;
#56386 = DIRECTION ( 'NONE',  ( 0.000000000000000000, 0.8660254037844428154, -0.4999999999999928946 ) ) ;
#56387 = CARTESIAN_POINT ( 'NONE',  ( 115.5794671477453761, -31.87256924526127477, 285.2384824187676600 ) ) ;
#56388 = CARTESIAN_POINT ( 'NONE',  ( 147.0667039024470739, -137.6782278159828934, 245.4503596475569793 ) ) ;
#56389 = CARTESIAN_POINT ( 'NONE',  ( 115.7825698381208213, -41.80321761809266690, 268.4065905822184845 ) ) ;
#56390 = LINE ( 'NONE', #84132, #80632 ) ;
#56391 = CARTESIAN_POINT ( 'NONE',  ( 168.0371591254546217, -48.62818131005519007, 129.9678068554150059 ) ) ;
#56392 = CARTESIAN_POINT ( 'NONE',  ( 176.7669697523285208, -48.62818131005431610, 180.4678068554150059 ) ) ;
#56393 = CARTESIAN_POINT ( 'NONE',  ( 116.5068947302722222, -41.18400185692905069, 228.4756252759109714 ) ) ;
#56394 = CARTESIAN_POINT ( 'NONE',  ( 97.80437445726883539, -40.49951938081226643, 171.6343582250473787 ) ) ;
#56395 = VERTEX_POINT ( 'NONE', #31883 ) ;
#56396 = ORIENTED_EDGE ( 'NONE', *, *, #35430, .F. ) ;
#56397 = VECTOR ( 'NONE', #80165, 1000.000000000000000 ) ;
#56398 = DIRECTION ( 'NONE',  ( 1.000000000000000000, 0.000000000000000000, 0.000000000000000000 ) ) ;
#56399 = CARTESIAN_POINT ( 'NONE',  ( 270.8910000000000196, 65.43750000000000000, 10.66800000000000104 ) ) ;
#56400 = CARTESIAN_POINT ( 'NONE',  ( 98.54754732716219223, -41.97681284361367204, 122.7650852229510576 ) ) ;
#56401 = DIRECTION ( 'NONE',  ( -4.237773401492740281E-14, 1.000000000000000000, 0.000000000000000000 ) ) ;
#56402 = CARTESIAN_POINT ( 'NONE',  ( 95.98894198207693762, -35.78073158428682632, 32.25848241876694544 ) ) ;
#56404 = FACE_OUTER_BOUND ( 'NONE', #49804, .T. ) ;
#56403 = AXIS2_PLACEMENT_3D ( 'NONE', #87565, #45743, #24449 ) ;
#56405 = VERTEX_POINT ( 'NONE', #30109 ) ;
#56406 = CARTESIAN_POINT ( 'NONE',  ( -1.790903581468949841E-22, 95.14999999999999147, 118.3560000000000088 ) ) ;
#56407 = CARTESIAN_POINT ( 'NONE',  ( 37.03715912545427358, -48.62818131006101652, 300.4678068554150059 ) ) ;
#56408 = CARTESIAN_POINT ( 'NONE',  ( 96.24916995763402383, -34.45682319295006124, 261.1737205140064475 ) ) ;
#56409 = ORIENTED_EDGE ( 'NONE', *, *, #19630, .T. ) ;
#56410 = AXIS2_PLACEMENT_3D ( 'NONE', #83253, #15099, #49142 ) ;
#56411 = LINE ( 'NONE', #77324, #47724 ) ;
#56412 = CARTESIAN_POINT ( 'NONE',  ( 172.5664832912729878, -27.82844715994070484, 75.92562527591199739 ) ) ;
#56413 = PLANE ( 'NONE',  #29555 ) ;
#56414 = CARTESIAN_POINT ( 'NONE',  ( 102.4269143325283835, -29.42360532460997291, 63.33285227435298026 ) ) ;
#56416 = CARTESIAN_POINT ( 'NONE',  ( 96.59701100649584760, -36.21046171878319342, 167.2870538473399620 ) ) ;
#56415 = CIRCLE ( 'NONE', #54907, 3.500000000000003109 ) ;
#56417 = CARTESIAN_POINT ( 'NONE',  ( 102.7030832344709523, -102.3364598618342853, -19.78219314458207378 ) ) ;
#56418 = ORIENTED_EDGE ( 'NONE', *, *, #73056, .T. ) ;
#56419 = VECTOR ( 'NONE', #77827, 1000.000000000000114 ) ;
#56420 = CARTESIAN_POINT ( 'NONE',  ( 46.48091746482131015, -48.32844715994084339, 249.9678068554150343 ) ) ;
#56421 = ORIENTED_EDGE ( 'NONE', *, *, #20414, .F. ) ;
#56422 = EDGE_LOOP ( 'NONE', ( #65693, #47433, #64165, #1035, #10524, #44548, #29496, #17004, #89137, #13079 ) ) ;
#56423 = DIRECTION ( 'NONE',  ( 1.000000000000000078E-15, 1.000000000000000083E-30, -1.000000000000000000 ) ) ;
#56424 = ORIENTED_EDGE ( 'NONE', *, *, #19432, .T. ) ;
#56425 = ORIENTED_EDGE ( 'NONE', *, *, #31463, .T. ) ;
#56426 = LINE ( 'NONE', #71875, #68673 ) ;
#56427 = ADVANCED_FACE ( 'NONE', ( #30994 ), #78280, .F. ) ;
#56428 = EDGE_CURVE ( 'NONE', #18305, #63160, #85093, .T. ) ;
#56429 = CARTESIAN_POINT ( 'NONE',  ( 97.81170003938157720, -40.51743348276853851, 42.63567940883270069 ) ) ;
#56430 = CIRCLE ( 'NONE', #24552, 10.00000000000000888 ) ;
#56431 = CARTESIAN_POINT ( 'NONE',  ( 99.76075522406560481, -42.08098971643298825, 106.2400388756959728 ) ) ;
#56432 = CARTESIAN_POINT ( 'NONE',  ( 111.4898014013570560, -26.57429697695857129, 284.7375300378155316 ) ) ;
#56433 = ADVANCED_FACE ( 'NONE', ( #9658 ), #22478, .F. ) ;
#56434 = LINE ( 'NONE', #21950, #23814 ) ;
#56435 = CARTESIAN_POINT ( 'NONE',  ( 7.661254700127844153, 66.45253841614081125, 320.6630000000000109 ) ) ;
#56436 = ADVANCED_FACE ( 'NONE', ( #72784 ), #37368, .T. ) ;
#56437 = ORIENTED_EDGE ( 'NONE', *, *, #41289, .T. ) ;
#56438 = DIRECTION ( 'NONE',  ( 1.000000000000000000, 0.000000000000000000, 0.000000000000000000 ) ) ;
#56439 = FACE_OUTER_BOUND ( 'NONE', #14788, .T. ) ;
#56440 = CARTESIAN_POINT ( 'NONE',  ( 70.74592677485811976, -139.3271945191473833, 247.4287440493089605 ) ) ;
#56441 = AXIS2_PLACEMENT_3D ( 'NONE', #28017, #57063, #28932 ) ;
#56442 = ADVANCED_FACE ( 'NONE', ( #30556 ), #85542, .F. ) ;
#56443 = CARTESIAN_POINT ( 'NONE',  ( 98.75024281215304711, -42.92452016420553917, 111.8480062282929737 ) ) ;
#56444 = CARTESIAN_POINT ( 'NONE',  ( 98.55409819730274990, -43.85350384415066571, 71.86895860924397539 ) ) ;
#56445 = DIRECTION ( 'NONE',  ( 0.000000000000000000, 1.000000000000000000, 0.000000000000000000 ) ) ;
#56446 = ORIENTED_EDGE ( 'NONE', *, *, #68135, .T. ) ;
#56447 = CARTESIAN_POINT ( 'NONE',  ( 116.9255123305063222, -41.72731008894000837, 248.4651490854349731 ) ) ;
#56448 = DIRECTION ( 'NONE',  ( 0.000000000000000000, 0.000000000000000000, -1.000000000000000000 ) ) ;
#56449 = DIRECTION ( 'NONE',  ( 0.000000000000000000, 1.000000000000000000, 0.000000000000000000 ) ) ;
#56451 = FACE_OUTER_BOUND ( 'NONE', #14105, .T. ) ;
#56450 = CARTESIAN_POINT ( 'NONE',  ( 125.5177273812784762, -137.6784471599409301, 55.21780685541800437 ) ) ;
#56452 = CARTESIAN_POINT ( 'NONE',  ( 106.0697754944390994, -25.31338314874918538, 320.6231843933491064 ) ) ;
#56454 = EDGE_CURVE ( 'NONE', #17490, #2213, #24627, .T. ) ;
#56453 = CARTESIAN_POINT ( 'NONE',  ( 125.8897075496517317, -55.55267141831851774, -4.824374724089010691 ) ) ;
#56455 = CARTESIAN_POINT ( 'NONE',  ( 0.000000000000000000, 238.7999999999999829, 159.6557476874258441 ) ) ;
#56456 = DIRECTION ( 'NONE',  ( -1.000000000000000000, 6.036837696399451257E-13, 0.000000000000000000 ) ) ;
#56457 = DIRECTION ( 'NONE',  ( -1.000000000000000000, 0.000000000000000000, 0.000000000000000000 ) ) ;
#56458 = CARTESIAN_POINT ( 'NONE',  ( 29.56648329127400388, 15.62155284005900491, 323.8756252759109202 ) ) ;
#56459 = EDGE_CURVE ( 'NONE', #57152, #48829, #18106, .T. ) ;
#56461 = ORIENTED_EDGE ( 'NONE', *, *, #49161, .T. ) ;
#56460 = CARTESIAN_POINT ( 'NONE',  ( 33.92127028473601769, -29.73316016639540749, -5.074374724088000832 ) ) ;
#56462 = VECTOR ( 'NONE', #3633, 1000.000000000000000 ) ;
#56463 = CARTESIAN_POINT ( 'NONE',  ( 94.20285697596305852, -128.6589936823971527, 250.2178068554179902 ) ) ;
#56464 = CARTESIAN_POINT ( 'NONE',  ( 115.7136949400716333, -42.59221908682786761, 273.3527681330537575 ) ) ;
#56465 = CARTESIAN_POINT ( 'NONE',  ( 117.6790090996954632, -39.81947568642139856, 134.5889586092439743 ) ) ;
#56466 = CARTESIAN_POINT ( 'NONE',  ( 102.7462986198438273, -25.66788047019655394, 16.37276813305293999 ) ) ;
#56467 = DIRECTION ( 'NONE',  ( 1.000000000000000000, 0.000000000000000000, 0.000000000000000000 ) ) ;
#56469 = CARTESIAN_POINT ( 'NONE',  ( 82.67897566168164758, -35.84952872354146791, 6.945088388039701854 ) ) ;
#56468 = FACE_OUTER_BOUND ( 'NONE', #68941, .T. ) ;
#56470 = CARTESIAN_POINT ( 'NONE',  ( -64.50026246089650783, 64.60000000000000853, 59.61038444174924678 ) ) ;
#56471 = ADVANCED_FACE ( 'NONE', ( #59130 ), #76150, .T. ) ;
#56472 = VECTOR ( 'NONE', #30768, 1000.000000000000000 ) ;
#56473 = AXIS2_PLACEMENT_3D ( 'NONE', #31495, #37440, #59203 ) ;
#56474 = ORIENTED_EDGE ( 'NONE', *, *, #79233, .F. ) ;
#56475 = CARTESIAN_POINT ( 'NONE',  ( -487.2989999999999782, 89.53805401447711176, 3.968750000000410338 ) ) ;
#56476 = ORIENTED_EDGE ( 'NONE', *, *, #60790, .F. ) ;
#56477 = ADVANCED_BREP_SHAPE_REPRESENTATION ( '', ( #18841, #50656 ), #27505 ) ;
#56478 = CARTESIAN_POINT ( 'NONE',  ( 115.4440039095595409, -34.92134030032634939, 183.4181341137909556 ) ) ;
#56479 = AXIS2_PLACEMENT_3D ( 'NONE', #84799, #70255, #77974 ) ;
#56481 = EDGE_LOOP ( 'NONE', ( #84713, #50238, #39297, #12601 ) ) ;
#56480 = FACE_BOUND ( 'NONE', #67253, .T. ) ;
#56482 = PLANE ( 'NONE',  #70766 ) ;
#56483 = CARTESIAN_POINT ( 'NONE',  ( 116.6407469026008243, -40.79910830432089597, 164.5070538473399608 ) ) ;
#56484 = CARTESIAN_POINT ( 'NONE',  ( 113.1759050958252004, -44.75365348611187244, 149.0944250870025769 ) ) ;
#56485 = B_SPLINE_CURVE_WITH_KNOTS ( 'NONE', 3,
 ( #12559, #40247, #55200, #67964, #88869, #26625, #82514, #54301, #82068, #47942, #47498, #40698, #33884, #61581, #56566, #2517, #23423, #9325, #15702, #70662, #72004, #29773, #42475, #9771, #51089, #1630, #14809, #50646, #71564, #49745, #50195, #77469, #78827, #37028, #36595, #22971, #28877 ),
 .UNSPECIFIED., .F., .F.,
 ( 4, 2, 2, 1, 2, 2, 2, 1, 1, 2, 2, 2, 2, 1, 2, 2, 2, 1, 1, 1, 2, 4 ),
 ( 0.6666501603260894804, 0.6874845253057108030, 0.6926931165506157173, 0.6979017077955206316, 0.7083188902853314595, 0.7499876202445696638, 0.7525919158670218989, 0.7551962114894742450, 0.7604048027343788263, 0.7708219852241890990, 0.7916563502038072020, 0.8124907151834253050, 0.8176993064283285539, 0.8229078976732318029, 0.8333250801630380789, 0.8749938101222534126, 0.8775981057447067579, 0.8802024013671601033, 0.8854109926120669050, 0.8958281751018802863, 0.9166625400815033853, 1.000000000000000000 ),
 .UNSPECIFIED. ) ;
#56486 = CARTESIAN_POINT ( 'NONE',  ( 97.33789316567710159, -34.07085429710922142, 151.1152779172331861 ) ) ;
#56487 = LINE ( 'NONE', #84675, #31269 ) ;
#56488 = CARTESIAN_POINT ( 'NONE',  ( -82.65143893653566920, 69.93120980984942037, 84.99964240976949270 ) ) ;
#56489 = DIRECTION ( 'NONE',  ( 0.000000000000000000, 0.000000000000000000, -1.000000000000000000 ) ) ;
#56490 = AXIS2_PLACEMENT_3D ( 'NONE', #71017, #8794, #49643 ) ;
#56491 = EDGE_CURVE ( 'NONE', #83766, #59751, #80057, .T. ) ;
#56492 = CARTESIAN_POINT ( 'NONE',  ( 115.9482186066389602, -32.63332544795704138, 104.1699109901969535 ) ) ;
#56493 = ORIENTED_EDGE ( 'NONE', *, *, #79874, .F. ) ;
#56494 = ORIENTED_EDGE ( 'NONE', *, *, #82123, .T. ) ;
#56495 = ORIENTED_EDGE ( 'NONE', *, *, #22542, .F. ) ;
#56496 = CARTESIAN_POINT ( 'NONE',  ( 107.7480938161759951, -27.89408153625565845, 66.44729759161194238 ) ) ;
#56497 = CARTESIAN_POINT ( 'NONE',  ( 133.7890526427665634, -110.9887994459054710, 250.2178068554179902 ) ) ;
#56499 = FACE_OUTER_BOUND ( 'NONE', #67312, .T. ) ;
#56498 = CARTESIAN_POINT ( 'NONE',  ( 98.33750497493211640, -41.21483588869658377, 192.7041967044819728 ) ) ;
#56500 = CARTESIAN_POINT ( 'NONE',  ( 105.8002047024404106, -26.72394367052961428, 55.17592173170812231 ) ) ;
#56501 = CARTESIAN_POINT ( 'NONE',  ( 199.3900000000000148, 52.73749999999999716, -53.97500000000000142 ) ) ;
#56502 = AXIS2_PLACEMENT_3D ( 'NONE', #46604, #52069, #38457 ) ;
#56503 = CARTESIAN_POINT ( 'NONE',  ( 63.56670390244714497, -40.82844715994014706, 129.9678068554150911 ) ) ;
#56504 = PLANE ( 'NONE',  #50688 ) ;
#56505 = CARTESIAN_POINT ( 'NONE',  ( -40.89999999999999858, 53.97500000000000142, 70.79999999999999716 ) ) ;
#56506 = CARTESIAN_POINT ( 'NONE',  ( 108.9808406375927063, -47.59218431635562041, 122.7032443235299723 ) ) ;
#56507 = ORIENTED_EDGE ( 'NONE', *, *, #9405, .F. ) ;
#56508 = EDGE_LOOP ( 'NONE', ( #24867, #47104, #87284, #87740 ) ) ;
#56509 = ORIENTED_EDGE ( 'NONE', *, *, #26914, .T. ) ;
#56510 = ADVANCED_FACE ( 'NONE', ( #4634 ), #73669, .T. ) ;
#56511 = CARTESIAN_POINT ( 'NONE',  ( 12.37565694608801437, 79.66829940370548968, 129.9681453810340770 ) ) ;
#56512 = DIRECTION ( 'NONE',  ( 1.000000000000000000, 4.299999999999999979E-14, 1.000000000000000078E-15 ) ) ;
#56513 = CARTESIAN_POINT ( 'NONE',  ( 99.09507197483526397, -30.55126955676270839, 130.8023766919142474 ) ) ;
#56514 = CYLINDRICAL_SURFACE ( 'NONE', #87400, 20.63750000000000284 ) ;
#56515 = CARTESIAN_POINT ( 'NONE',  ( 98.49961498605385657, -35.50075171889626091, 224.0433284648299548 ) ) ;
#56516 = VECTOR ( 'NONE', #57855, 1000.000000000000000 ) ;
#56517 = EDGE_CURVE ( 'NONE', #41269, #11232, #36926, .T. ) ;
#56518 = CARTESIAN_POINT ( 'NONE',  ( -254.0000000000000000, 93.66249999999999432, 90.48749999999999716 ) ) ;
#56519 = DIRECTION ( 'NONE',  ( 0.000000000000000000, 0.000000000000000000, 1.000000000000000000 ) ) ;
#56520 = ORIENTED_EDGE ( 'NONE', *, *, #50272, .F. ) ;
#56522 = VERTEX_POINT ( 'NONE', #33683 ) ;
#56521 = EDGE_LOOP ( 'NONE', ( #69959, #9063 ) ) ;
#56523 = AXIS2_PLACEMENT_3D ( 'NONE', #3341, #72823, #44203 ) ;
#56524 = CARTESIAN_POINT ( 'NONE',  ( -546.0365000000000464, 53.97500000000000142, 50.79999999999999716 ) ) ;
#56525 = VERTEX_POINT ( 'NONE', #47293 ) ;
#56526 = VERTEX_POINT ( 'NONE', #87754 ) ;
#56527 = CARTESIAN_POINT ( 'NONE',  ( 72.96458098368701428, 127.0000000000000000, -65.82083098368670449 ) ) ;
#56528 = CARTESIAN_POINT ( 'NONE',  ( 101.6176986403717279, -43.71793944654686470, 228.4815833058969758 ) ) ;
#56529 = VECTOR ( 'NONE', #6110, 1000.000000000000000 ) ;
#56530 = PLANE ( 'NONE',  #66665 ) ;
#56531 = ORIENTED_EDGE ( 'NONE', *, *, #55474, .F. ) ;
#56532 = FACE_OUTER_BOUND ( 'NONE', #22503, .T. ) ;
#56533 = CARTESIAN_POINT ( 'NONE',  ( -119.5597780469935145, 74.55132283206019395, 52.44562168052537743 ) ) ;
#56534 = AXIS2_PLACEMENT_3D ( 'NONE', #67510, #55202, #70210 ) ;
#56535 = ORIENTED_EDGE ( 'NONE', *, *, #89360, .T. ) ;
#56537 = ORIENTED_EDGE ( 'NONE', *, *, #19737, .T. ) ;
#56536 = CIRCLE ( 'NONE', #78298, 7.143749999999999822 ) ;
#56538 = CARTESIAN_POINT ( 'NONE',  ( 180.1667039024477504, -28.27351298636767041, 117.4678068554150627 ) ) ;
#56539 = ORIENTED_EDGE ( 'NONE', *, *, #474, .T. ) ;
#56540 = ORIENTED_EDGE ( 'NONE', *, *, #72739, .T. ) ;
#56541 = EDGE_CURVE ( 'NONE', #48789, #43538, #87688, .T. ) ;
#56542 = EDGE_CURVE ( 'NONE', #12790, #55335, #11903, .T. ) ;
#56543 = CARTESIAN_POINT ( 'NONE',  ( 108.7463670854851756, -45.85490172528324138, 275.5395189410199919 ) ) ;
#56544 = AXIS2_PLACEMENT_3D ( 'NONE', #53156, #72751, #30962 ) ;
#56545 = CARTESIAN_POINT ( 'NONE',  ( 97.36144725414590084, -42.06870896796115034, 176.7146728949589658 ) ) ;
#56546 = EDGE_CURVE ( 'NONE', #70798, #77857, #60106, .T. ) ;
#56547 = CARTESIAN_POINT ( 'NONE',  ( 99.70004787478420383, -45.98060041612311721, 122.0413395616249659 ) ) ;
#56548 = DIRECTION ( 'NONE',  ( 0.000000000000000000, 0.000000000000000000, 1.000000000000000000 ) ) ;
#56549 = DIRECTION ( 'NONE',  ( 0.000000000000000000, 0.000000000000000000, -1.000000000000000000 ) ) ;
#56550 = DIRECTION ( 'NONE',  ( 1.000000000000000000, 1.000000000000000078E-15, 0.000000000000000000 ) ) ;
#56551 = CARTESIAN_POINT ( 'NONE',  ( 109.3368649739139187, -26.55458330520283994, 220.9013395616249795 ) ) ;
#56552 = LINE ( 'NONE', #89756, #8017 ) ;
#56553 = CARTESIAN_POINT ( 'NONE',  ( 88.17226027475679473, -14.72944715994100484, 239.5838068554175777 ) ) ;
#56554 = VERTEX_POINT ( 'NONE', #46837 ) ;
#56555 = DIRECTION ( 'NONE',  ( -4.237773401492740281E-14, 1.000000000000000000, 0.000000000000000000 ) ) ;
#56556 = VERTEX_POINT ( 'NONE', #54540 ) ;
#56557 = ADVANCED_FACE ( 'NONE', ( #67755 ), #81416, .F. ) ;
#56558 = ORIENTED_EDGE ( 'NONE', *, *, #87576, .F. ) ;
#56559 = AXIS2_PLACEMENT_3D ( 'NONE', #63137, #84046, #42671 ) ;
#56560 = DIRECTION ( 'NONE',  ( 0.000000000000000000, 0.000000000000000000, -1.000000000000000000 ) ) ;
#56561 = CARTESIAN_POINT ( 'NONE',  ( 103.3256077877525030, -27.45548614628576445, 136.3815795745832133 ) ) ;
#56562 = ADVANCED_FACE ( 'NONE', ( #66855 ), #81851, .F. ) ;
#56563 = ORIENTED_EDGE ( 'NONE', *, *, #69276, .F. ) ;
#56564 = CARTESIAN_POINT ( 'NONE',  ( 96.02763272632168423, -37.29765984735794859, 121.3794347997209684 ) ) ;
#56565 = DIRECTION ( 'NONE',  ( 0.000000000000000000, 0.000000000000000000, 1.000000000000000000 ) ) ;
#56566 = CARTESIAN_POINT ( 'NONE',  ( 136.5456844410060455, -35.53793914063654569, 7.103892432653868383 ) ) ;
#56567 = CYLINDRICAL_SURFACE ( 'NONE', #81934, 1.000000000000000888 ) ;
#56570 = CARTESIAN_POINT ( 'NONE',  ( 116.9047011640239759, -41.71676023082950735, 244.4651490854349731 ) ) ;
#56569 = CARTESIAN_POINT ( 'NONE',  ( 99.75293322724810707, -43.56396968085568489, 56.92422635920629403 ) ) ;
#56568 = CARTESIAN_POINT ( 'NONE',  ( 0.000000000000000000, 124.5870000000000033, 0.000000000000000000 ) ) ;
#56571 = CARTESIAN_POINT ( 'NONE',  ( 140.0667039024470171, -90.27844715994091018, 51.21780685541800437 ) ) ;
#56573 = ADVANCED_FACE ( 'NONE', ( #40494 ), #12807, .F. ) ;
#56572 = CARTESIAN_POINT ( 'NONE',  ( 182.0667039024478413, -32.29483332967958376, 193.9678068554150059 ) ) ;
#56574 = DIRECTION ( 'NONE',  ( 0.000000000000000000, 0.000000000000000000, -1.000000000000000000 ) ) ;
#56575 = LINE ( 'NONE', #43386, #7977 ) ;
#56576 = LINE ( 'NONE', #84318, #44478 ) ;
#56577 = DIRECTION ( 'NONE',  ( 1.000000000000000000, 4.299999999999999979E-14, 1.000000000000000078E-15 ) ) ;
#56579 = ORIENTED_EDGE ( 'NONE', *, *, #76047, .T. ) ;
#56578 = CARTESIAN_POINT ( 'NONE',  ( 115.3585040474263508, -45.26590950091470233, 268.1899109901965517 ) ) ;
#56580 = CARTESIAN_POINT ( 'NONE',  ( 134.0664832912740110, 0.2215528400590013880, 293.6356252759119911 ) ) ;
#56581 = CARTESIAN_POINT ( 'NONE',  ( 114.1902268275144507, -45.21166270573645107, 148.1203871806719405 ) ) ;
#56582 = CARTESIAN_POINT ( 'NONE',  ( 109.6119375470732109, -25.15554210634138954, 25.90419670448196143 ) ) ;
#56583 = CARTESIAN_POINT ( 'NONE',  ( 117.8211145215647946, -31.63542911875440211, 210.1784824187679703 ) ) ;
#56584 = CARTESIAN_POINT ( 'NONE',  ( 108.4174891635765619, -26.73503591423436276, 30.96895861629700519 ) ) ;
#56585 = DIRECTION ( 'NONE',  ( -1.000000000000000078E-15, 1.000000000000000083E-30, 1.000000000000000000 ) ) ;
#56586 = CIRCLE ( 'NONE', #30469, 4.750000000000000888 ) ;
#56588 = DIRECTION ( 'NONE',  ( -0.7071067811865444641, 0.000000000000000000, 0.7071067811865505703 ) ) ;
#56587 = DIRECTION ( 'NONE',  ( 0.1811243268507098381, -0.9834602067307437467, 0.000000000000000000 ) ) ;
#56589 = CARTESIAN_POINT ( 'NONE',  ( 41.56648329127398966, -18.82844715994071194, 258.9256252759120116 ) ) ;
#56590 = CARTESIAN_POINT ( 'NONE',  ( 144.0637245237351749, -140.6784087391956746, 245.5331728883010101 ) ) ;
#56591 = ORIENTED_EDGE ( 'NONE', *, *, #8757, .F. ) ;
#56592 = CARTESIAN_POINT ( 'NONE',  ( 165.3359832912740046, -36.32844715994100682, -5.074374724088000832 ) ) ;
#56593 =( BOUNDED_CURVE ( )  B_SPLINE_CURVE ( 3, ( #68190, #54966, #14576, #484 ),
 .UNSPECIFIED., .F., .T. ) 
 B_SPLINE_CURVE_WITH_KNOTS ( ( 4, 4 ),
 ( 1.570796326790817377, 3.141592653586014805 ),
 .UNSPECIFIED. ) 
 CURVE ( )  GEOMETRIC_REPRESENTATION_ITEM ( )  RATIONAL_B_SPLINE_CURVE ( ( 1.000000000000000000, 0.8047378541242942163, 0.8047378541242942163, 1.000000000000000000 ) ) 
 REPRESENTATION_ITEM ( '' )  );
#56594 = VERTEX_POINT ( 'NONE', #61378 ) ;
#56595 = ORIENTED_EDGE ( 'NONE', *, *, #59929, .F. ) ;
#56596 = AXIS2_PLACEMENT_3D ( 'NONE', #29043, #61745, #83122 ) ;
#56598 = ORIENTED_EDGE ( 'NONE', *, *, #5809, .T. ) ;
#56597 = CARTESIAN_POINT ( 'NONE',  ( 107.0664832912739399, -36.72944715994095333, 290.1356252759106837 ) ) ;
#56599 = CARTESIAN_POINT ( 'NONE',  ( 110.7866772467784955, -46.44483816919306207, 58.86705384733998159 ) ) ;
#56600 = DIRECTION ( 'NONE',  ( 1.000000000000000000, 4.299999999999999979E-14, 1.000000000000000078E-15 ) ) ;
#56602 = CARTESIAN_POINT ( 'NONE',  ( 121.3042370176062548, -43.34581843340460239, 0.7256252759109850237 ) ) ;
#56601 = VECTOR ( 'NONE', #83758, 1000.000000000000000 ) ;
#56603 = CARTESIAN_POINT ( 'NONE',  ( 108.6817352505430705, -26.38614300430984372, 185.9527681330539792 ) ) ;
#56604 = ADVANCED_FACE ( 'NONE', ( #67295 ), #19163, .T. ) ;
#56605 = CARTESIAN_POINT ( 'NONE',  ( 111.6523633261645188, -43.93540552976629243, 262.4495626852196892 ) ) ;
#56606 = VERTEX_POINT ( 'NONE', #53643 ) ;
#56607 = EDGE_LOOP ( 'NONE', ( #23935, #30900, #46883, #83354 ) ) ;
#56608 = VERTEX_POINT ( 'NONE', #74566 ) ;
#56609 = VERTEX_POINT ( 'NONE', #89102 ) ;
#56610 = DIRECTION ( 'NONE',  ( -0.0001713722456129692653, 0.9999999853157764962, 0.000000000000000000 ) ) ;
#56611 = CARTESIAN_POINT ( 'NONE',  ( 48.16670390244701139, -26.71338133339251542, -5.074374724088000832 ) ) ;
#56612 = CARTESIAN_POINT ( 'NONE',  ( 70.06670417066791856, -83.77844715994098124, 222.2178068554179902 ) ) ;
#56613 = CARTESIAN_POINT ( 'NONE',  ( 113.2466443085970553, -28.75955056167441271, 19.55182030042092478 ) ) ;
#56614 = CARTESIAN_POINT ( 'NONE',  ( 83.76986456925334323, 87.79544278253753475, 100.1374281256150169 ) ) ;
#56615 = CARTESIAN_POINT ( 'NONE',  ( 135.2444258376730204, 20.32000000000000028, -147.4575741623271767 ) ) ;
#56616 = AXIS2_PLACEMENT_3D ( 'NONE', #38662, #66362, #87276 ) ;
#56617 = DIRECTION ( 'NONE',  ( 0.000000000000000000, -1.000000000000000000, 0.000000000000000000 ) ) ;
#56618 = CARTESIAN_POINT ( 'NONE',  ( -24.20305689751608824, 53.97499999999997300, 58.62596543806478877 ) ) ;
#56619 = CARTESIAN_POINT ( 'NONE',  ( 96.68076663292303863, -33.01451620012163346, 26.06514908543494613 ) ) ;
#56620 = CARTESIAN_POINT ( 'NONE',  ( -12.67976079355167052, 81.71985538306350350, 117.8759963413547212 ) ) ;
#56621 = ORIENTED_EDGE ( 'NONE', *, *, #61535, .T. ) ;
#56622 = PLANE ( 'NONE',  #43188 ) ;
#56623 = VECTOR ( 'NONE', #59677, 1000.000000000000000 ) ;
#56624 = DIRECTION ( 'NONE',  ( -0.000000000000000000, -0.000000000000000000, 1.000000000000000000 ) ) ;
#56625 = CARTESIAN_POINT ( 'NONE',  ( 112.5126453671185942, -30.64922967528412556, 112.3138046553059723 ) ) ;
#56626 = EDGE_CURVE ( 'NONE', #810, #15908, #12349, .T. ) ;
#56627 = FACE_OUTER_BOUND ( 'NONE', #20210, .T. ) ;
#56628 = DIRECTION ( 'NONE',  ( 0.000000000000000000, 0.000000000000000000, -1.000000000000000000 ) ) ;
#56629 = ORIENTED_EDGE ( 'NONE', *, *, #25475, .T. ) ;
#56630 = VERTEX_POINT ( 'NONE', #60935 ) ;
#56631 = CARTESIAN_POINT ( 'NONE',  ( 115.7833298848688344, -41.80193538969286493, 138.4043975589790705 ) ) ;
#56632 = AXIS2_PLACEMENT_3D ( 'NONE', #59151, #86879, #24641 ) ;
#56633 = EDGE_LOOP ( 'NONE', ( #56987, #40441, #493, #73925 ) ) ;
#56634 = VERTEX_POINT ( 'NONE', #88663 ) ;
#56635 = CARTESIAN_POINT ( 'NONE',  ( 105.9222987080832752, -26.72137021301569959, 156.5987261630399701 ) ) ;
#56636 = CARTESIAN_POINT ( 'NONE',  ( -12.67976775996874572, 83.37995484863287743, 117.8759955821573158 ) ) ;
#56637 = AXIS2_PLACEMENT_3D ( 'NONE', #56518, #36090, #63346 ) ;
#56638 = CARTESIAN_POINT ( 'NONE',  ( 117.3853494549534844, -38.35986426902426416, 109.7013395616249767 ) ) ;
#56639 = DIRECTION ( 'NONE',  ( 0.9834602067019604377, 0.1811243270069963496, 0.000000000000000000 ) ) ;
#56640 = ORIENTED_EDGE ( 'NONE', *, *, #13742, .F. ) ;
#56641 = EDGE_LOOP ( 'NONE', ( #62808, #52964, #7954, #72074 ) ) ;
#56642 = ORIENTED_EDGE ( 'NONE', *, *, #42381, .T. ) ;
#56643 = ADVANCED_FACE ( 'NONE', ( #5994 ), #6424, .F. ) ;
#56644 = FACE_OUTER_BOUND ( 'NONE', #37436, .T. ) ;
#56645 = ORIENTED_EDGE ( 'NONE', *, *, #9303, .F. ) ;
#56646 = EDGE_CURVE ( 'NONE', #33311, #76266, #40933, .T. ) ;
#56647 = CARTESIAN_POINT ( 'NONE',  ( 116.4547782460827250, -32.24742764444978604, 19.18133956162493092 ) ) ;
#56648 = CARTESIAN_POINT ( 'NONE',  ( 98.14969091592392658, -31.28627964566590336, 166.8899109901969950 ) ) ;
#56649 = PLANE ( 'NONE',  #3108 ) ;
#56650 = DIRECTION ( 'NONE',  ( 0.000000000000000000, -1.000000000000000000, 0.000000000000000000 ) ) ;
#56651 = EDGE_CURVE ( 'NONE', #48373, #47090, #59573, .T. ) ;
#56652 = CARTESIAN_POINT ( 'NONE',  ( 117.6079501356808947, -33.40507394795707796, 125.0575300378149706 ) ) ;
#56653 = VECTOR ( 'NONE', #26566, 1000.000000000000000 ) ;
#56654 = DIRECTION ( 'NONE',  ( 1.000000000000000078E-15, 1.000000000000000083E-30, -1.000000000000000000 ) ) ;
#56655 = ORIENTED_EDGE ( 'NONE', *, *, #14348, .T. ) ;
#56656 = CARTESIAN_POINT ( 'NONE',  ( 97.70685139758691662, -40.25208905359860267, 116.6132694511275218 ) ) ;
#56657 = AXIS2_PLACEMENT_3D ( 'NONE', #86326, #64984, #17288 ) ;
#56658 = ADVANCED_FACE ( 'NONE', ( #56348 ), #14595, .F. ) ;
#56659 = ORIENTED_EDGE ( 'NONE', *, *, #66675, .F. ) ;
#56660 = CARTESIAN_POINT ( 'NONE',  ( 99.08970696490817431, -42.79570318340363855, 132.8446165289294356 ) ) ;
#56661 = EDGE_LOOP ( 'NONE', ( #68035, #7178, #58777, #88674 ) ) ;
#56662 = ORIENTED_EDGE ( 'NONE', *, *, #15878, .T. ) ;
#56663 = VECTOR ( 'NONE', #8672, 1000.000000000000000 ) ;
#56664 = FACE_OUTER_BOUND ( 'NONE', #17267, .T. ) ;
#56665 = CARTESIAN_POINT ( 'NONE',  ( 97.25147018216796369, -38.86936842998233033, 132.4977133313580850 ) ) ;
#56666 = CARTESIAN_POINT ( 'NONE',  ( 107.6068636345326155, -48.56787927409158812, 42.61276813305398292 ) ) ;
#56667 = CARTESIAN_POINT ( 'NONE',  ( 19.63602930441068750, 63.82048847602042940, 32.65376468583215086 ) ) ;
#56668 = CARTESIAN_POINT ( 'NONE',  ( 22.49563609058249725, -67.87844715994100397, 13.84673904354931651 ) ) ;
#56669 = LINE ( 'NONE', #83957, #23837 ) ;
#56670 = CARTESIAN_POINT ( 'NONE',  ( 110.5640613610538168, -45.86347053068967483, 62.86705384733992474 ) ) ;
#56672 = CARTESIAN_POINT ( 'NONE',  ( 98.02603654163385727, -30.41010087969375775, 156.8289586092439549 ) ) ;
#56671 = CARTESIAN_POINT ( 'NONE',  ( 97.06386015463802153, -37.34256901384676297, 111.3752599851678298 ) ) ;
#56673 = CARTESIAN_POINT ( 'NONE',  ( 109.7248659175985779, -27.00080517866619800, 70.86479194288972394 ) ) ;
#56675 = EDGE_CURVE ( 'NONE', #1395, #39002, #42272, .T. ) ;
#56674 = DIRECTION ( 'NONE',  ( 1.000000000000000078E-15, 0.000000000000000000, -1.000000000000000000 ) ) ;
#56676 = EDGE_LOOP ( 'NONE', ( #72423, #7837, #23913, #4155 ) ) ;
#56677 = AXIS2_PLACEMENT_3D ( 'NONE', #41126, #6185, #34317 ) ;
#56678 = DIRECTION ( 'NONE',  ( -0.000000000000000000, 1.000000000000000000, 0.000000000000000000 ) ) ;
#56679 = DIRECTION ( 'NONE',  ( 0.000000000000000000, 0.000000000000000000, -1.000000000000000000 ) ) ;
#56680 = FACE_OUTER_BOUND ( 'NONE', #66299, .T. ) ;
#56681 = EDGE_LOOP ( 'NONE', ( #77174, #53567 ) ) ;
#56682 = DIRECTION ( 'NONE',  ( 1.387778780781444492E-15, 0.000000000000000000, -1.000000000000000000 ) ) ;
#56684 = VERTEX_POINT ( 'NONE', #69104 ) ;
#56683 = CARTESIAN_POINT ( 'NONE',  ( 97.91784736035330639, -30.44332401329681659, 165.8594347997199634 ) ) ;
#56685 = DIRECTION ( 'NONE',  ( 1.000000000000000078E-15, -1.000000000000000083E-30, -1.000000000000000000 ) ) ;
#56686 = CARTESIAN_POINT ( 'NONE',  ( 96.16865940696823145, -32.01143006853777706, 207.0013395616249738 ) ) ;
#56687 = CARTESIAN_POINT ( 'NONE',  ( 95.43962894333766656, -34.19422119854147013, 102.1556252759109640 ) ) ;
#56688 = CARTESIAN_POINT ( 'NONE',  ( 129.4373059489699926, -139.1238275029716362, 247.5908586209667988 ) ) ;
#56689 = LINE ( 'NONE', #36262, #44582 ) ;
#56690 = DIRECTION ( 'NONE',  ( 0.7071067811868696484, 0.7071067811862253860, 7.071067811868689941E-16 ) ) ;
#56691 = ORIENTED_EDGE ( 'NONE', *, *, #2915, .T. ) ;
#56692 = ITEM_DEFINED_TRANSFORMATION ( 'NONE', 'NONE', #14560,  #50656 ) ;
#56693 = ORIENTED_EDGE ( 'NONE', *, *, #13872, .F. ) ;
#56695 = ORIENTED_EDGE ( 'NONE', *, *, #55124, .T. ) ;
#56694 = VECTOR ( 'NONE', #23726, 1000.000000000000000 ) ;
#56696 = CONICAL_SURFACE ( 'NONE', #69818, 1.624999999999987566, 1.029744258676650093 ) ;
#56697 = VERTEX_POINT ( 'NONE', #83193 ) ;
#56698 = CARTESIAN_POINT ( 'NONE',  ( 188.5667039024479834, -62.87844715994099687, 288.3428068554150059 ) ) ;
#56699 = CARTESIAN_POINT ( 'NONE',  ( 110.7330907359209107, -26.30208074597294754, 250.8194347997206819 ) ) ;
#56700 = DIRECTION ( 'NONE',  ( 1.000000000000000000, -1.581013800890250371E-15, 0.000000000000000000 ) ) ;
#56701 = CARTESIAN_POINT ( 'NONE',  ( 134.2548946453563303, -15.97944715994100484, 1.625625275910998147 ) ) ;
#56702 = VECTOR ( 'NONE', #87994, 1000.000000000000000 ) ;
#56704 = DIRECTION ( 'NONE',  ( 0.000000000000000000, -1.000000000000000000, 0.000000000000000000 ) ) ;
#56703 = DIRECTION ( 'NONE',  ( -1.000000000000000078E-15, 1.000000000000000083E-30, 1.000000000000000000 ) ) ;
#56705 = DIRECTION ( 'NONE',  ( 0.000000000000000000, 0.000000000000000000, 1.000000000000000000 ) ) ;
#56706 = VECTOR ( 'NONE', #80954, 1000.000000000000000 ) ;
#56707 = ADVANCED_FACE ( 'NONE', ( #27761 ), #21408, .T. ) ;
#56708 = CARTESIAN_POINT ( 'NONE',  ( 114.8359307259106856, -43.71386199060815869, 38.24419670448192221 ) ) ;
#56709 = VERTEX_POINT ( 'NONE', #56800 ) ;
#56710 = VERTEX_POINT ( 'NONE', #20951 ) ;
#56711 = FACE_OUTER_BOUND ( 'NONE', #58462, .T. ) ;
#56712 = CARTESIAN_POINT ( 'NONE',  ( 112.1408248370476741, -28.01367038444149316, 15.65874614011077881 ) ) ;
#56713 = EDGE_CURVE ( 'NONE', #56395, #31400, #8226, .T. ) ;
#56714 = CARTESIAN_POINT ( 'NONE',  ( 116.7892270756567967, -35.66563809766837778, 274.9127681330532482 ) ) ;
#56715 = CARTESIAN_POINT ( 'NONE',  ( 181.8764988495246655, -33.54226604284360747, 313.9678068554149490 ) ) ;
#56716 = CARTESIAN_POINT ( 'NONE',  ( 103.6907823165633289, -45.90921117331522083, 138.2956252759109645 ) ) ;
#56717 = CYLINDRICAL_SURFACE ( 'NONE', #19729, 12.70000000000000462 ) ;
#56718 = DIRECTION ( 'NONE',  ( 1.000000000000000078E-15, 1.000000000000000083E-30, -1.000000000000000000 ) ) ;
#56720 = VERTEX_POINT ( 'NONE', #7328 ) ;
#56719 = VECTOR ( 'NONE', #17084, 1000.000000000000114 ) ;
#56721 = CARTESIAN_POINT ( 'NONE',  ( 62.03715912545732181, -23.42818131006021432, 237.4678068554150059 ) ) ;
#56722 = CARTESIAN_POINT ( 'NONE',  ( 97.81168895331838087, -40.51742574516882200, 287.6356252759109680 ) ) ;
#56723 = ORIENTED_EDGE ( 'NONE', *, *, #50555, .T. ) ;
#56724 = ORIENTED_EDGE ( 'NONE', *, *, #15951, .T. ) ;
#56725 = CARTESIAN_POINT ( 'NONE',  ( -91.24829632406202506, 88.91144712388911842, 75.69222284415488389 ) ) ;
#56726 = CARTESIAN_POINT ( 'NONE',  ( 98.69997382787508400, -39.74003663468293013, 263.0330118773257482 ) ) ;
#56727 = CIRCLE ( 'NONE', #17577, 17.00000000000000000 ) ;
#56728 = CARTESIAN_POINT ( 'NONE',  ( 57.14999999999999858, 69.84999999999999432, 300.8629999999999995 ) ) ;
#56729 = EDGE_CURVE ( 'NONE', #66807, #83508, #55441, .T. ) ;
#56730 = CARTESIAN_POINT ( 'NONE',  ( 98.34976866985373078, -31.65674666536116888, 140.9064732640824502 ) ) ;
#56731 = B_SPLINE_CURVE_WITH_KNOTS ( 'NONE', 3,
 ( #11313, #39014, #66265, #25845 ),
 .UNSPECIFIED., .F., .F.,
 ( 4, 4 ),
 ( -0.6035999334370459879, -0.5903216970416090836 ),
 .UNSPECIFIED. ) ;
#56732 = CARTESIAN_POINT ( 'NONE',  ( 105.7995184992940381, -26.72403496457788563, 85.17729194164677153 ) ) ;
#56733 = CIRCLE ( 'NONE', #19069, 9.425000000000000711 ) ;
#56734 = CARTESIAN_POINT ( 'NONE',  ( 85.85219768521609751, 70.17671898886894155, -81.76240029069555248 ) ) ;
#56735 = ORIENTED_EDGE ( 'NONE', *, *, #34190, .F. ) ;
#56736 = DIRECTION ( 'NONE',  ( 1.000000000000000000, 4.299999999999999979E-14, 1.000000000000000078E-15 ) ) ;
#56737 = LINE ( 'NONE', #64906, #36851 ) ;
#56738 = ORIENTED_EDGE ( 'NONE', *, *, #42269, .F. ) ;
#56739 = CARTESIAN_POINT ( 'NONE',  ( 109.7701363090614990, -47.44715903388583200, 92.78514908543495210 ) ) ;
#56740 = ORIENTED_EDGE ( 'NONE', *, *, #24898, .T. ) ;
#56742 = AXIS2_PLACEMENT_3D ( 'NONE', #38462, #44832, #52074 ) ;
#56741 = CARTESIAN_POINT ( 'NONE',  ( 115.0166753900997065, -32.39272993814809354, 23.63432458998199337 ) ) ;
#56743 = EDGE_CURVE ( 'NONE', #9318, #32614, #68505, .T. ) ;
#56744 = CARTESIAN_POINT ( 'NONE',  ( 123.0664832912750057, -36.72944715993921960, 0.7256252759109869110 ) ) ;
#56745 = CARTESIAN_POINT ( 'NONE',  ( 102.9544237342423969, -27.85507949283293527, 180.4213395616259845 ) ) ;
#56746 = DIRECTION ( 'NONE',  ( 3.999999999999999995E-14, -1.000000000000000000, 4.100000000000000342E-29 ) ) ;
#56747 = CARTESIAN_POINT ( 'NONE',  ( 107.0664832912739968, -36.72944715994100306, 293.2242906452868851 ) ) ;
#56748 = PLANE ( 'NONE',  #10068 ) ;
#56749 = CARTESIAN_POINT ( 'NONE',  ( 1.387778780781445676E-14, 184.0000000000000000, 97.27542076772557778 ) ) ;
#56750 = CARTESIAN_POINT ( 'NONE',  ( 105.7709788128635182, -26.34124963128569163, 266.1756252759109884 ) ) ;
#56751 = CARTESIAN_POINT ( 'NONE',  ( 84.99753727674156778, 95.14807216649714405, -82.65057572782293960 ) ) ;
#56752 = ORIENTED_EDGE ( 'NONE', *, *, #11030, .T. ) ;
#56753 = LINE ( 'NONE', #21351, #61784 ) ;
#56754 = ORIENTED_EDGE ( 'NONE', *, *, #44244, .T. ) ;
#56755 = CARTESIAN_POINT ( 'NONE',  ( 104.9540660161283370, -25.01839229886434524, 121.2184824187679766 ) ) ;
#56756 = CARTESIAN_POINT ( 'NONE',  ( 119.7724476469521449, 50.10406306454358827, -51.95653040766548258 ) ) ;
#56757 = ORIENTED_EDGE ( 'NONE', *, *, #25900, .T. ) ;
#56758 = VERTEX_POINT ( 'NONE', #37610 ) ;
#56759 = VERTEX_POINT ( 'NONE', #87098 ) ;
#56760 = DIRECTION ( 'NONE',  ( 0.000000000000000000, 0.000000000000000000, -1.000000000000000000 ) ) ;
#56761 = FACE_OUTER_BOUND ( 'NONE', #14870, .T. ) ;
#56762 = FACE_OUTER_BOUND ( 'NONE', #79304, .T. ) ;
#56763 = CARTESIAN_POINT ( 'NONE',  ( 177.4809174648213741, -48.32844715993478957, 249.9678068554149775 ) ) ;
#56764 = DIRECTION ( 'NONE',  ( -0.7071067811607679721, 0.7071067812123270624, 0.000000000000000000 ) ) ;
#56765 = ADVANCED_FACE ( 'NONE', ( #24865 ), #38050, .F. ) ;
#56766 = CARTESIAN_POINT ( 'NONE',  ( 116.1584918543541960, -31.54133664852386332, 285.2384824187680579 ) ) ;
#56767 = DIRECTION ( 'NONE',  ( -0.7071067811862239427, -0.7071067811868709807, 0.000000000000000000 ) ) ;
#56768 = ORIENTED_EDGE ( 'NONE', *, *, #54589, .T. ) ;
#56769 = CARTESIAN_POINT ( 'NONE',  ( -179.8898777604655095, 101.5999999999999943, 114.2999999999999972 ) ) ;
#56770 = DIRECTION ( 'NONE',  ( 0.7071067811865779928, -0.7071067811865171526, 7.071067811865786933E-16 ) ) ;
#56771 = VERTEX_POINT ( 'NONE', #23984 ) ;
#56772 = ORIENTED_EDGE ( 'NONE', *, *, #60762, .T. ) ;
#56773 = AXIS2_PLACEMENT_3D ( 'NONE', #78590, #2719, #77676 ) ;
#56774 = CARTESIAN_POINT ( 'NONE',  ( -30.89999999999999858, 53.97500000000000142, 50.79999999999999716 ) ) ;
#56775 = LINE ( 'NONE', #22732, #78877 ) ;
#56776 = DIRECTION ( 'NONE',  ( 0.000000000000000000, 1.000000000000000000, 0.000000000000000000 ) ) ;
#56777 = FACE_BOUND ( 'NONE', #13596, .T. ) ;
#56778 = CARTESIAN_POINT ( 'NONE',  ( 68.76053423562146349, -136.8603496727827746, 247.4879725229279757 ) ) ;
#56779 = CARTESIAN_POINT ( 'NONE',  ( 107.4298862253102698, -45.26314917194000742, 237.0324198280769679 ) ) ;
#56780 = CARTESIAN_POINT ( 'NONE',  ( -74.56320856954198462, 53.97500000000000142, 30.79999999999999361 ) ) ;
#56781 = CARTESIAN_POINT ( 'NONE',  ( 177.0371591254543375, -48.62818131005480637, 300.4678068554149490 ) ) ;
#56782 = CARTESIAN_POINT ( 'NONE',  ( 101.7334424669833339, -26.99437863453528408, 100.4632443235299633 ) ) ;
#56783 = EDGE_LOOP ( 'NONE', ( #47506, #10792, #15874, #47278 ) ) ;
#56785 = EDGE_CURVE ( 'NONE', #23292, #17303, #52532, .T. ) ;
#56784 = CARTESIAN_POINT ( 'NONE',  ( 131.3881603334746160, -19.35482103166650703, 6.853567712192263350 ) ) ;
#56786 = EDGE_LOOP ( 'NONE', ( #24130, #53489 ) ) ;
#56787 = ADVANCED_FACE ( 'NONE', ( #4427 ), #87541, .F. ) ;
#56788 = CARTESIAN_POINT ( 'NONE',  ( 103.4155122767169388, -27.41960725263014709, 276.3738772456573543 ) ) ;
#56789 = ORIENTED_EDGE ( 'NONE', *, *, #25792, .T. ) ;
#56790 = CARTESIAN_POINT ( 'NONE',  ( 83.06670390244796920, -64.87844715994098976, 213.1838068554149856 ) ) ;
#56791 = ORIENTED_EDGE ( 'NONE', *, *, #75206, .F. ) ;
#56792 = CARTESIAN_POINT ( 'NONE',  ( 151.5667039024486087, -48.82844715993590512, 129.9678068554149775 ) ) ;
#56793 = DIRECTION ( 'NONE',  ( 0.000000000000000000, -1.000000000000000000, 0.000000000000000000 ) ) ;
#56794 = AXIS2_PLACEMENT_3D ( 'NONE', #61490, #74245, #75591 ) ;
#56795 = DIRECTION ( 'NONE',  ( 0.000000000000000000, 0.000000000000000000, -1.000000000000000000 ) ) ;
#56796 = ORIENTED_EDGE ( 'NONE', *, *, #41781, .T. ) ;
#56797 = CARTESIAN_POINT ( 'NONE',  ( 117.3932167392688655, -32.72270067050601483, 94.10895860924395606 ) ) ;
#56798 = PRESENTATION_STYLE_ASSIGNMENT (( #43166 ) ) ;
#56800 = CARTESIAN_POINT ( 'NONE',  ( -479.3614999999999782, 14.28750000000036025, 2.863608028952929985 ) ) ;
#56799 = CARTESIAN_POINT ( 'NONE',  ( 116.3268456006857718, -32.93825467094161752, 164.1356252759109680 ) ) ;
#56801 = DIRECTION ( 'NONE',  ( -0.000000000000000000, 1.000000000000000000, -0.000000000000000000 ) ) ;
#56802 = DIRECTION ( 'NONE',  ( 0.000000000000000000, 0.000000000000000000, -1.000000000000000000 ) ) ;
#56803 = ORIENTED_EDGE ( 'NONE', *, *, #37268, .F. ) ;
#56804 = CIRCLE ( 'NONE', #10459, 0.5000000000000004441 ) ;
#56805 = DIRECTION ( 'NONE',  ( 1.000000000000000078E-15, -1.000000000000000083E-30, -1.000000000000000000 ) ) ;
#56806 = CARTESIAN_POINT ( 'NONE',  ( 80.06648329127399677, -8.729447159940999512, 291.1181252759119502 ) ) ;
#56807 = DIRECTION ( 'NONE',  ( -0.7071067811865460184, 0.000000000000000000, 0.7071067811865489050 ) ) ;
#56808 = CARTESIAN_POINT ( 'NONE',  ( 117.3853494549534844, -38.35986426902426416, 109.7013395616249767 ) ) ;
#56810 = CARTESIAN_POINT ( 'NONE',  ( 0.000000000000000000, 20.32000000000000028, 0.000000000000000000 ) ) ;
#56809 = DIRECTION ( 'NONE',  ( 0.000000000000000000, -1.000000000000000000, 0.000000000000000000 ) ) ;
#56811 = LINE ( 'NONE', #8696, #16133 ) ;
#56812 = ORIENTED_EDGE ( 'NONE', *, *, #35756, .T. ) ;
#56813 = CYLINDRICAL_SURFACE ( 'NONE', #2754, 0.4999999999999994449 ) ;
#56814 = CARTESIAN_POINT ( 'NONE',  ( 99.89458030379221043, -28.23347241844150091, 146.6356252759109395 ) ) ;
#56816 = ORIENTED_EDGE ( 'NONE', *, *, #12050, .T. ) ;
#56815 = DIRECTION ( 'NONE',  ( -0.9254794337955620787, -0.3787978585227822492, 0.000000000000000000 ) ) ;
#56817 = AXIS2_PLACEMENT_3D ( 'NONE', #35461, #40934, #958 ) ;
#56818 = CARTESIAN_POINT ( 'NONE',  ( 111.7637953458031745, -46.71243375810358600, 283.9146728949585849 ) ) ;
#56819 = FACE_BOUND ( 'NONE', #78854, .T. ) ;
#56820 = DIRECTION ( 'NONE',  ( 1.000000000000000078E-15, -1.000000000000000000, 0.000000000000000000 ) ) ;
#56821 = DIRECTION ( 'NONE',  ( 0.000000000000000000, 0.000000000000000000, 1.000000000000000000 ) ) ;
#56822 = DIRECTION ( 'NONE',  ( -1.000000000000000000, 0.000000000000000000, 1.046082768126375896E-16 ) ) ;
#56823 = CARTESIAN_POINT ( 'NONE',  ( -33.98325472291465132, 17.78000000000000114, -3.174999999999764899 ) ) ;
#56824 = LINE ( 'NONE', #57730, #18163 ) ;
#56825 = CARTESIAN_POINT ( 'NONE',  ( 109.8674951572811551, -26.74480306206631397, 219.8708633711499658 ) ) ;
#56826 = ORIENTED_EDGE ( 'NONE', *, *, #69689, .T. ) ;
#56827 = AXIS2_PLACEMENT_3D ( 'NONE', #12238, #20840, #7218 ) ;
#56828 = VERTEX_POINT ( 'NONE', #32113 ) ;
#56829 = CARTESIAN_POINT ( 'NONE',  ( 97.07454461617307118, -38.04679588918885713, 147.8615833058969713 ) ) ;
#56830 = AXIS2_PLACEMENT_3D ( 'NONE', #24282, #37460, #73303 ) ;
#56831 = CARTESIAN_POINT ( 'NONE',  ( 162.9033555647770015, -33.89581943344391135, 193.9678068554150059 ) ) ;
#56832 = ADVANCED_FACE ( 'NONE', ( #18040 ), #58915, .F. ) ;
#56833 = CARTESIAN_POINT ( 'NONE',  ( 111.4502655538902758, -27.98611278301861560, 275.7070538473389547 ) ) ;
#56834 = FACE_OUTER_BOUND ( 'NONE', #16108, .T. ) ;
#56835 = EDGE_CURVE ( 'NONE', #78594, #628, #44849, .T. ) ;
#56836 = LINE ( 'NONE', #55932, #6898 ) ;
#56837 = EDGE_CURVE ( 'NONE', #944, #32467, #63106, .T. ) ;
#56838 = CARTESIAN_POINT ( 'NONE',  ( 107.3428450438784694, -25.27364292152175551, 322.4523926293242653 ) ) ;
#56839 = CARTESIAN_POINT ( 'NONE',  ( -72.96458098368600531, 101.5999999999999943, -72.96458098368781009 ) ) ;
#56840 = CARTESIAN_POINT ( 'NONE',  ( 97.78482738069629931, -40.45122027033047374, 37.62964898729292429 ) ) ;
#56841 = CARTESIAN_POINT ( 'NONE',  ( 110.1310368924891350, -26.13358316477604504, 214.8403871806729342 ) ) ;
#56842 = CARTESIAN_POINT ( 'NONE',  ( 10.70251037890477797, 89.21217201404442676, 117.8713340830158955 ) ) ;
#56843 = VERTEX_POINT ( 'NONE', #67088 ) ;
#56844 = ORIENTED_EDGE ( 'NONE', *, *, #73147, .T. ) ;
#56845 = ADVANCED_FACE ( 'NONE', ( #45721, #73450 ), #38479, .F. ) ;
#56846 = VECTOR ( 'NONE', #10273, 1000.000000000000000 ) ;
#56847 = EDGE_CURVE ( 'NONE', #65495, #74787, #38930, .T. ) ;
#56848 = LINE ( 'NONE', #83242, #37241 ) ;
#56849 = CARTESIAN_POINT ( 'NONE',  ( -91.51255889651575615, 88.18374315479977099, -75.37293521528332008 ) ) ;
#56850 = LINE ( 'NONE', #62774, #67875 ) ;
#56851 = DIRECTION ( 'NONE',  ( 0.000000000000000000, 0.000000000000000000, -1.000000000000000000 ) ) ;
#56852 = AXIS2_PLACEMENT_3D ( 'NONE', #36726, #23114, #21759 ) ;
#56853 = ADVANCED_FACE ( 'NONE', ( #4866 ), #52972, .F. ) ;
#56854 = CARTESIAN_POINT ( 'NONE',  ( 116.1702204287673794, -31.76348745224625958, 20.21181575210096071 ) ) ;
#56855 = LINE ( 'NONE', #49132, #71688 ) ;
#56856 = ORIENTED_EDGE ( 'NONE', *, *, #38915, .F. ) ;
#56857 = VECTOR ( 'NONE', #26173, 1000.000000000000000 ) ;
#56858 = CARTESIAN_POINT ( 'NONE',  ( 112.2188834189205409, -26.89723471487287654, 10.68038718067299087 ) ) ;
#56859 = CARTESIAN_POINT ( 'NONE',  ( 0.000000000000000000, 101.5999999999999943, 118.5560000000000116 ) ) ;
#56860 = EDGE_CURVE ( 'NONE', #1971, #38989, #32554, .T. ) ;
#56861 = CARTESIAN_POINT ( 'NONE',  ( 100.7500417190893245, -45.80037066963202363, 237.0803871806729717 ) ) ;
#56862 = ORIENTED_EDGE ( 'NONE', *, *, #35417, .F. ) ;
#56863 = CIRCLE ( 'NONE', #62708, 9.525000000000000355 ) ;
#56864 = CARTESIAN_POINT ( 'NONE',  ( 77.42411991178801145, -37.49143581486279686, 6.902478035881912000 ) ) ;
#56865 = DIRECTION ( 'NONE',  ( -0.000000000000000000, 1.000000000000000000, -0.000000000000000000 ) ) ;
#56866 = DIRECTION ( 'NONE',  ( 0.000000000000000000, 0.000000000000000000, -1.000000000000000000 ) ) ;
#56867 = CIRCLE ( 'NONE', #78638, 5.599999999999994316 ) ;
#56868 = ADVANCED_FACE ( 'NONE', ( #3089 ), #58474, .T. ) ;
#56869 = CARTESIAN_POINT ( 'NONE',  ( 115.3104451506078192, -40.98773602117310588, 91.26523322673496352 ) ) ;
#56870 = CARTESIAN_POINT ( 'NONE',  ( 117.2182995153958132, -34.26411022451439692, 205.0156252759109634 ) ) ;
#56871 = CARTESIAN_POINT ( 'NONE',  ( 107.0620278373210255, -36.73691869758540207, 361.9756252759100903 ) ) ;
#56872 = VERTEX_POINT ( 'NONE', #10771 ) ;
#56873 = DIRECTION ( 'NONE',  ( 0.9242245927363033076, 0.3818493186865917766, 0.000000000000000000 ) ) ;
#56874 = ORIENTED_EDGE ( 'NONE', *, *, #12315, .T. ) ;
#56875 = ORIENTED_EDGE ( 'NONE', *, *, #76242, .F. ) ;
#56876 = CARTESIAN_POINT ( 'NONE',  ( 51.34673845256598668, -36.02818131005800950, -5.074374724088000832 ) ) ;
#56877 = ORIENTED_EDGE ( 'NONE', *, *, #75353, .T. ) ;
#56878 = ORIENTED_EDGE ( 'NONE', *, *, #63650, .T. ) ;
#56879 = CARTESIAN_POINT ( 'NONE',  ( 116.8163745243374194, -34.15002972185388330, 170.0315280845597670 ) ) ;
#56880 = CARTESIAN_POINT ( 'NONE',  ( 103.2785698053728396, -27.47462617712415422, 41.38562054109723221 ) ) ;
#56881 = CARTESIAN_POINT ( 'NONE',  ( 113.2121186763659040, -42.70299450126940144, 97.63527697093398672 ) ) ;
#56882 = CARTESIAN_POINT ( 'NONE',  ( 111.0013748985821422, -46.40740010236051916, 282.8841967044824628 ) ) ;
#56883 = ADVANCED_FACE ( 'NONE', ( #86205 ), #31672, .F. ) ;
#56884 = EDGE_CURVE ( 'NONE', #51252, #45127, #61602, .T. ) ;
#56885 = LINE ( 'NONE', #70993, #13681 ) ;
#56886 = CARTESIAN_POINT ( 'NONE',  ( 38.10000000000000142, 95.25000000000000000, 346.9005000000000223 ) ) ;
#56887 = ORIENTED_EDGE ( 'NONE', *, *, #44249, .T. ) ;
#56888 = EDGE_CURVE ( 'NONE', #39002, #12424, #21035, .T. ) ;
#56889 = ORIENTED_EDGE ( 'NONE', *, *, #58090, .T. ) ;
#56890 = CARTESIAN_POINT ( 'NONE',  ( 183.5150000000000148, 14.63749999999999929, -52.38749999999999574 ) ) ;
#56891 = ADVANCED_FACE ( 'NONE', ( #55663 ), #88894, .T. ) ;
#56892 = AXIS2_PLACEMENT_3D ( 'NONE', #6660, #82986, #47525 ) ;
#56893 = CARTESIAN_POINT ( 'NONE',  ( 107.0667039024470171, -73.27844715994095282, 25.71780685541800437 ) ) ;
#56894 = CARTESIAN_POINT ( 'NONE',  ( 70.36104920614575065, -140.1771413417756094, 246.8581798060137942 ) ) ;
#56895 = AXIS2_PLACEMENT_3D ( 'NONE', #63693, #1017, #47463 ) ;
#56896 = CARTESIAN_POINT ( 'NONE',  ( 108.9483104351207317, -46.92736419409159510, 127.7337205140069472 ) ) ;
#56897 = B_SPLINE_CURVE_WITH_KNOTS ( 'NONE', 3,
 ( #80528, #44640, #18281, #30141 ),
 .UNSPECIFIED., .F., .F.,
 ( 4, 4 ),
 ( -0.6035999334370309999, -0.5903216970415989806 ),
 .UNSPECIFIED. ) ;
#56898 = CARTESIAN_POINT ( 'NONE',  ( 96.59774800590200527, -36.61877842429220209, 111.3184824187679567 ) ) ;
#56899 = CARTESIAN_POINT ( 'NONE',  ( 6.938893903907229955E-15, 67.86880000000000734, 216.0269999999999868 ) ) ;
#56900 = ORIENTED_EDGE ( 'NONE', *, *, #74749, .F. ) ;
#56901 = UNCERTAINTY_MEASURE_WITH_UNIT (LENGTH_MEASURE( 1.000000000000000082E-05 ), #69550, 'distance_accuracy_value', 'NONE');
#56902 = CARTESIAN_POINT ( 'NONE',  ( 115.9600293333739387, -30.16561243848903828, 259.3203871806730945 ) ) ;
#56903 = DIRECTION ( 'NONE',  ( -1.000000000000000000, -5.512527431108013646E-15, 0.000000000000000000 ) ) ;
#56904 = SURFACE_SIDE_STYLE ('',( #49181 ) ) ;
#56905 = CARTESIAN_POINT ( 'NONE',  ( 11.92955753101793626, 78.19254692348476965, 130.0098836371429627 ) ) ;
#56906 = CARTESIAN_POINT ( 'NONE',  ( 99.63728152159639251, -43.45851683074288019, 27.91285964145581033 ) ) ;
#56908 = CARTESIAN_POINT ( 'NONE',  ( 68.70480626725813522, -139.2920007788289070, 245.9226302269273106 ) ) ;
#56907 = DIRECTION ( 'NONE',  ( 1.000000000000000078E-15, -1.000000000000000000, 0.000000000000000000 ) ) ;
#56909 = CARTESIAN_POINT ( 'NONE',  ( 105.1452543958526178, -25.43249337517275066, 322.4561491387724459 ) ) ;
#56910 = DIRECTION ( 'NONE',  ( 0.000000000000000000, 0.000000000000000000, -1.000000000000000000 ) ) ;
#56911 = CARTESIAN_POINT ( 'NONE',  ( 132.2601441849014918, -38.80290789369895066, 7.687431601935594827 ) ) ;
#56912 = CARTESIAN_POINT ( 'NONE',  ( -0.4144590284063416896, 95.25000000000001421, 130.5560000000000400 ) ) ;
#56913 = CARTESIAN_POINT ( 'NONE',  ( 163.2569089553700223, -33.54226604285010893, -5.074374724088000832 ) ) ;
#56914 = DIRECTION ( 'NONE',  ( -0.9254794337955620787, -0.3787978585227822492, 0.000000000000000000 ) ) ;
#56915 = AXIS2_PLACEMENT_3D ( 'NONE', #47345, #12861, #75073 ) ;
#56917 = ORIENTED_EDGE ( 'NONE', *, *, #72694, .T. ) ;
#56916 = CARTESIAN_POINT ( 'NONE',  ( 41.56648329127399677, -18.82844715994099971, 318.9256252759120116 ) ) ;
#56918 = CARTESIAN_POINT ( 'NONE',  ( 183.5150000000000148, 36.86249999999999716, -35.28456447661465489 ) ) ;
#56919 = CARTESIAN_POINT ( 'NONE',  ( 118.6786315247609167, -39.21782601141705271, 258.6584824187679033 ) ) ;
#56920 = CARTESIAN_POINT ( 'NONE',  ( 98.55127668717894096, -44.97116251829300637, 187.9384824187679612 ) ) ;
#56921 = CARTESIAN_POINT ( 'NONE',  ( 111.7933198282062364, -46.77516514641244783, 283.9146728949586418 ) ) ;
#56923 = CARTESIAN_POINT ( 'NONE',  ( 100.8874678875339583, -44.70022137742768109, 47.05229194287733208 ) ) ;
#56922 = PLANE ( 'NONE',  #81269 ) ;
#56924 = DIRECTION ( 'NONE',  ( 0.000000000000000000, 0.000000000000000000, 1.000000000000000000 ) ) ;
#56925 = VECTOR ( 'NONE', #22388, 1000.000000000000000 ) ;
#56926 = EDGE_LOOP ( 'NONE', ( #34031, #82201 ) ) ;
#56927 = FACE_BOUND ( 'NONE', #3989, .T. ) ;
#56928 = ORIENTED_EDGE ( 'NONE', *, *, #1714, .F. ) ;
#56929 = VECTOR ( 'NONE', #67970, 1000.000000000000000 ) ;
#56930 = CARTESIAN_POINT ( 'NONE',  ( 115.8611420101186269, -34.56920459637935750, 163.4286103042669822 ) ) ;
#56932 = ORIENTED_EDGE ( 'NONE', *, *, #23863, .F. ) ;
#56931 = PLANE ( 'NONE',  #50075 ) ;
#56933 = CARTESIAN_POINT ( 'NONE',  ( 177.0664832912730162, 12.92155284005730387, 355.9756252759109998 ) ) ;
#56934 = CARTESIAN_POINT ( 'NONE',  ( 117.7782040715256926, -34.09831434418946827, 160.0061014663869798 ) ) ;
#56935 = CARTESIAN_POINT ( 'NONE',  ( 31.90335556477799628, -33.89581943344391135, 313.9678068554150059 ) ) ;
#56936 = DIRECTION ( 'NONE',  ( -1.000000000000000000, 0.000000000000000000, 0.000000000000000000 ) ) ;
#56937 = CARTESIAN_POINT ( 'NONE',  ( 110.9162716161081477, -27.50018748410121106, 85.76213040958664635 ) ) ;
#56938 = DIRECTION ( 'NONE',  ( 0.000000000000000000, -1.000000000000000000, 0.000000000000000000 ) ) ;
#56939 = DIRECTION ( 'NONE',  ( -0.9254794337955620787, -0.3787978585227822492, 0.000000000000000000 ) ) ;
#56940 = CARTESIAN_POINT ( 'NONE',  ( 103.2241971045484092, -45.72390501747114655, 92.25562527591097250 ) ) ;
#56941 = VERTEX_POINT ( 'NONE', #40270 ) ;
#56942 = ORIENTED_EDGE ( 'NONE', *, *, #32889, .F. ) ;
#56943 = CARTESIAN_POINT ( 'NONE',  ( 97.10642131522254772, -35.22350214559244819, 67.63872616303994789 ) ) ;
#56944 = CARTESIAN_POINT ( 'NONE',  ( 131.3470363009685684, -91.25622735614739156, 250.2178068554180470 ) ) ;
#56946 = CARTESIAN_POINT ( 'NONE',  ( 116.7951252779109552, -39.38782976372972655, 38.61479194470811649 ) ) ;
#56945 = CARTESIAN_POINT ( 'NONE',  ( 103.9298229712114363, -26.84510867568836545, 201.3089586092439731 ) ) ;
#56947 = PLANE ( 'NONE',  #4275 ) ;
#56948 = CARTESIAN_POINT ( 'NONE',  ( 112.1393427418982611, -28.01282092607783625, 110.6566897338729234 ) ) ;
#56949 = ADVANCED_FACE ( 'NONE', ( #68887 ), #83414, .F. ) ;
#56950 = DIRECTION ( 'NONE',  ( 1.000000000000000000, 7.076552332833900719E-16, 9.062687768214910535E-30 ) ) ;
#56951 = EDGE_CURVE ( 'NONE', #51146, #1529, #86338, .T. ) ;
#56952 = VECTOR ( 'NONE', #24880, 1000.000000000000000 ) ;
#56953 = CARTESIAN_POINT ( 'NONE',  ( 89.60916260784479448, 239.0000000000000000, 134.1927865330827103 ) ) ;
#56954 = LINE ( 'NONE', #49691, #60366 ) ;
#56955 = CARTESIAN_POINT ( 'NONE',  ( 103.1828028919049558, -27.07824557232541807, 130.3813395616259925 ) ) ;
#56956 = EDGE_LOOP ( 'NONE', ( #14275, #33115, #6258, #9457, #16733 ) ) ;
#56957 = VERTEX_POINT ( 'NONE', #69337 ) ;
#56958 = ORIENTED_EDGE ( 'NONE', *, *, #19225, .F. ) ;
#56959 = ADVANCED_FACE ( 'NONE', ( #74359 ), #6218, .F. ) ;
#56960 = ADVANCED_FACE ( 'NONE', ( #40719 ), #54322, .F. ) ;
#56961 = DIRECTION ( 'NONE',  ( 1.000000000000000078E-15, -1.000000000000000083E-30, -1.000000000000000000 ) ) ;
#56962 = CARTESIAN_POINT ( 'NONE',  ( 62.03742497533659872, -23.42844715994041493, 129.9678068554150911 ) ) ;
#56963 = CARTESIAN_POINT ( 'NONE',  ( 112.0659116142514762, -45.48839626539587755, 78.98979194182945207 ) ) ;
#56964 = CARTESIAN_POINT ( 'NONE',  ( 77.39114642429899504, 120.6499999999999915, 71.77848634863160271 ) ) ;
#56965 = CARTESIAN_POINT ( 'NONE',  ( 111.7322531227442681, -44.01858407219413039, 215.8357094172109782 ) ) ;
#56966 = EDGE_CURVE ( 'NONE', #28336, #23638, #19392, .T. ) ;
#56967 = AXIS2_PLACEMENT_3D ( 'NONE', #23610, #36329, #65799 ) ;
#56968 = DIRECTION ( 'NONE',  ( 1.000000000000000078E-15, -1.000000000000000083E-30, -1.000000000000000000 ) ) ;
#56969 = ADVANCED_FACE ( 'NONE', ( #27103 ), #82542, .F. ) ;
#56970 = CARTESIAN_POINT ( 'NONE',  ( 112.1201679527454047, -47.44862423305024635, 137.9270538473389820 ) ) ;
#56971 = CARTESIAN_POINT ( 'NONE',  ( 20.03715912545826328, -46.82818131006190043, 237.4678068554150059 ) ) ;
#56972 = ORIENTED_EDGE ( 'NONE', *, *, #87739, .T. ) ;
#56974 = ORIENTED_EDGE ( 'NONE', *, *, #25265, .F. ) ;
#56973 = VERTEX_POINT ( 'NONE', #75706 ) ;
#56975 = CARTESIAN_POINT ( 'NONE',  ( 71.77848634863079269, 120.6499999999999915, 77.39114642429989033 ) ) ;
#56976 = ORIENTED_EDGE ( 'NONE', *, *, #61406, .T. ) ;
#56977 = VERTEX_POINT ( 'NONE', #6658 ) ;
#56978 = DIRECTION ( 'NONE',  ( 1.000000000000000078E-15, 0.000000000000000000, 1.000000000000000000 ) ) ;
#56979 = DIRECTION ( 'NONE',  ( -1.000000000000000000, 0.000000000000000000, 1.046082768126375896E-16 ) ) ;
#56980 = EDGE_CURVE ( 'NONE', #61833, #51166, #66016, .T. ) ;
#56981 = CARTESIAN_POINT ( 'NONE',  ( 98.23953817868523686, -35.94630056370082372, 227.6872975916109567 ) ) ;
#56982 = CARTESIAN_POINT ( 'NONE',  ( 117.0718955085710746, -35.46248247742748561, 273.9272919329436036 ) ) ;
#56983 = ORIENTED_EDGE ( 'NONE', *, *, #9182, .T. ) ;
#56984 = CARTESIAN_POINT ( 'NONE',  ( 114.1129555325863549, -42.16089393588610079, 9.635625275910941312 ) ) ;
#56985 = EDGE_CURVE ( 'NONE', #27806, #43612, #89794, .T. ) ;
#56986 = DIRECTION ( 'NONE',  ( 0.000000000000000000, 0.000000000000000000, 1.000000000000000000 ) ) ;
#56987 = ORIENTED_EDGE ( 'NONE', *, *, #62520, .F. ) ;
#56988 = ORIENTED_EDGE ( 'NONE', *, *, #52590, .T. ) ;
#56989 = VECTOR ( 'NONE', #86193, 1000.000000000000000 ) ;
#56990 = CARTESIAN_POINT ( 'NONE',  ( 110.8545929532096608, -45.98418784724056252, 112.8856356861517725 ) ) ;
#56991 = ORIENTED_EDGE ( 'NONE', *, *, #29044, .F. ) ;
#56992 = ORIENTED_EDGE ( 'NONE', *, *, #71048, .F. ) ;
#56993 = CONICAL_SURFACE ( 'NONE', #3321, 13.31607168056649115, 0.1047197551196538678 ) ;
#56994 = CARTESIAN_POINT ( 'NONE',  ( 101.0114332956932088, -30.54581597779692359, 268.5233284648295466 ) ) ;
#56995 = CARTESIAN_POINT ( 'NONE',  ( 95.54500964991285628, -39.60862429916534211, 166.5213395616259788 ) ) ;
#56996 = CARTESIAN_POINT ( 'NONE',  ( 112.1095002620001821, -47.42599740258513208, 137.9270538473389820 ) ) ;
#56997 = FACE_OUTER_BOUND ( 'NONE', #41058, .T. ) ;
#56998 = CARTESIAN_POINT ( 'NONE',  ( 102.2372498927960720, -45.96854842739928415, 208.1927681330539599 ) ) ;
#56999 = DIRECTION ( 'NONE',  ( 1.000000000000000000, 4.299999999999999979E-14, 1.000000000000000078E-15 ) ) ;
#57000 = ORIENTED_EDGE ( 'NONE', *, *, #10253, .F. ) ;
#57001 = DIRECTION ( 'NONE',  ( 1.000000000000000000, -6.745093096447288888E-17, 0.000000000000000000 ) ) ;
#57002 = ORIENTED_EDGE ( 'NONE', *, *, #41664, .T. ) ;
#57003 = EDGE_CURVE ( 'NONE', #69055, #68920, #50064, .T. ) ;
#57004 = ORIENTED_EDGE ( 'NONE', *, *, #41401, .F. ) ;
#57005 = EDGE_CURVE ( 'NONE', #38670, #48540, #9438, .T. ) ;
#57006 = CARTESIAN_POINT ( 'NONE',  ( 108.1864980337677764, -47.13868502929719284, 202.6613395616249704 ) ) ;
#57007 = ORIENTED_EDGE ( 'NONE', *, *, #47448, .F. ) ;
#57008 = CARTESIAN_POINT ( 'NONE',  ( 113.0770494671172628, -28.21122406429266150, 129.5870538473399449 ) ) ;
#57009 = LINE ( 'NONE', #28413, #76169 ) ;
#57010 = DIRECTION ( 'NONE',  ( 0.7071067811865330288, 0.000000000000000000, 0.7071067811865621167 ) ) ;
#57011 = DIRECTION ( 'NONE',  ( 1.000000000000000078E-15, -1.000000000000000083E-30, -1.000000000000000000 ) ) ;
#57014 = CARTESIAN_POINT ( 'NONE',  ( 111.5990003564989479, -46.09347164638224825, 243.9356252759109509 ) ) ;
#57013 = CARTESIAN_POINT ( 'NONE',  ( 103.6783103676969233, -46.16071442410667913, 57.30167220430897856 ) ) ;
#57012 = CARTESIAN_POINT ( 'NONE',  ( 85.58420390244806697, -51.22944715994107412, 207.5838068554169809 ) ) ;
#57015 = DIRECTION ( 'NONE',  ( -1.000000000000000000, -1.541976423090496028E-15, 0.000000000000000000 ) ) ;
#57016 = CARTESIAN_POINT ( 'NONE',  ( -41.60202597009397607, 65.59999999999998010, 50.85338361873603219 ) ) ;
#57017 = DIRECTION ( 'NONE',  ( 0.000000000000000000, -1.000000000000000000, 0.000000000000000000 ) ) ;
#57018 = AXIS2_PLACEMENT_3D ( 'NONE', #59275, #54225, #40168 ) ;
#57019 = DIRECTION ( 'NONE',  ( 0.000000000000000000, 1.000000000000000000, 0.000000000000000000 ) ) ;
#57020 = DIRECTION ( 'NONE',  ( 0.000000000000000000, 0.000000000000000000, 1.000000000000000000 ) ) ;
#57021 = PLANE ( 'NONE',  #79604 ) ;
#57023 = VERTEX_POINT ( 'NONE', #21190 ) ;
#57022 = CARTESIAN_POINT ( 'NONE',  ( 111.7936012040045597, -46.77578388097458628, 287.9146728949587555 ) ) ;
#57024 = CARTESIAN_POINT ( 'NONE',  ( 122.2221484686747459, -111.8737466215625602, -11.78219314458178779 ) ) ;
#57025 = CARTESIAN_POINT ( 'NONE',  ( 108.0089373620841826, -26.32355773090834816, 155.0041967044819557 ) ) ;
#57026 = CARTESIAN_POINT ( 'NONE',  ( 104.2140748950419464, -25.22734379144252870, 86.26991099019699050 ) ) ;
#57027 = CARTESIAN_POINT ( 'NONE',  ( 106.4811776831737262, -24.84380329649774666, 191.1156252759109861 ) ) ;
#57028 = CARTESIAN_POINT ( 'NONE',  ( -194.1576000000000022, 0.000000000000000000, 114.2999999999999972 ) ) ;
#57029 = FACE_OUTER_BOUND ( 'NONE', #88560, .T. ) ;
#57031 = CARTESIAN_POINT ( 'NONE',  ( 44.45000000000000284, 50.79999999999999716, 275.4630000000000223 ) ) ;
#57030 = DIRECTION ( 'NONE',  ( 0.000000000000000000, 0.000000000000000000, -1.000000000000000000 ) ) ;
#57032 = CARTESIAN_POINT ( 'NONE',  ( 98.34985892109634165, -31.65658479506688039, 70.90645860791694588 ) ) ;
#57033 = CARTESIAN_POINT ( 'NONE',  ( 1.387778780781445676E-14, 239.0000000000000000, 82.77542076772560620 ) ) ;
#57034 = VERTEX_POINT ( 'NONE', #12129 ) ;
#57035 = CIRCLE ( 'NONE', #71590, 8.999999999999994671 ) ;
#57036 = EDGE_CURVE ( 'NONE', #9719, #20160, #67534, .T. ) ;
#57037 = CARTESIAN_POINT ( 'NONE',  ( 0.000000000000000000, 60.82030000000000314, 265.5569999999999595 ) ) ;
#57038 = ORIENTED_EDGE ( 'NONE', *, *, #43712, .F. ) ;
#57039 = ORIENTED_EDGE ( 'NONE', *, *, #66498, .F. ) ;
#57041 = ORIENTED_EDGE ( 'NONE', *, *, #45559, .T. ) ;
#57040 = LINE ( 'NONE', #68559, #48780 ) ;
#57042 = CARTESIAN_POINT ( 'NONE',  ( 112.8057071037347185, -27.31004523576153886, 45.62895860924398761 ) ) ;
#57043 = DIRECTION ( 'NONE',  ( -1.000000000000000078E-15, 0.000000000000000000, 1.000000000000000000 ) ) ;
#57044 = CARTESIAN_POINT ( 'NONE',  ( 76.06670390244796920, -26.72944715994109899, 239.5838068554169809 ) ) ;
#57045 = CARTESIAN_POINT ( 'NONE',  ( 103.0329776526464087, -26.38883157761164000, 166.3603871806729444 ) ) ;
#57046 = CARTESIAN_POINT ( 'NONE',  ( 116.1125752699382048, -36.30413522796790460, 268.2743245899816884 ) ) ;
#57047 = EDGE_LOOP ( 'NONE', ( #80767, #47949 ) ) ;
#57048 = ADVANCED_FACE ( 'NONE', ( #88445 ), #26205, .F. ) ;
#57049 = ORIENTED_EDGE ( 'NONE', *, *, #69893, .T. ) ;
#57050 = ORIENTED_EDGE ( 'NONE', *, *, #81421, .F. ) ;
#57051 = CIRCLE ( 'NONE', #25146, 16.72999999999999332 ) ;
#57052 = CARTESIAN_POINT ( 'NONE',  ( 158.0667039024469886, -67.87844715994090450, 190.2178068554179902 ) ) ;
#57053 = CARTESIAN_POINT ( 'NONE',  ( 51.42025729302698522, -31.94127993907710206, -5.074374724088000832 ) ) ;
#57055 = CIRCLE ( 'NONE', #29454, 2.999999999999975131 ) ;
#57054 = DIRECTION ( 'NONE',  ( 4.299999999999999979E-14, -1.000000000000000000, 4.400000000000000367E-29 ) ) ;
#57056 = CARTESIAN_POINT ( 'NONE',  ( 102.0677952829802706, -27.97006589295626711, 20.48873420085072539 ) ) ;
#57057 = CARTESIAN_POINT ( 'NONE',  ( 100.4326241145864032, 86.63355734047006251, 83.41565754067561045 ) ) ;
#57058 = EDGE_CURVE ( 'NONE', #72437, #25185, #8458, .T. ) ;
#57059 = CARTESIAN_POINT ( 'NONE',  ( 115.8259566582697175, -31.73092551245608561, 50.24009526075410292 ) ) ;
#57060 = ADVANCED_FACE ( 'NONE', ( #42950 ), #63411, .T. ) ;
#57061 = CARTESIAN_POINT ( 'NONE',  ( 72.26949937496601706, -71.54137415153812185, 394.9756252759101471 ) ) ;
#57062 = EDGE_CURVE ( 'NONE', #43158, #16965, #41378, .T. ) ;
#57063 = DIRECTION ( 'NONE',  ( 0.000000000000000000, -1.000000000000000000, 0.000000000000000000 ) ) ;
#57064 = CARTESIAN_POINT ( 'NONE',  ( 111.4063510358307667, -46.18429848020807782, 27.91848241876792969 ) ) ;
#57065 = ORIENTED_EDGE ( 'NONE', *, *, #80976, .T. ) ;
#57066 = EDGE_CURVE ( 'NONE', #87632, #43121, #61665, .T. ) ;
#57067 = CARTESIAN_POINT ( 'NONE',  ( 125.9611475301391721, -58.72944715994100306, 239.5838068554164124 ) ) ;
#57068 = CARTESIAN_POINT ( 'NONE',  ( -54.98109326260873786, 54.34217962558955861, 70.79744912815033331 ) ) ;
#57069 = CARTESIAN_POINT ( 'NONE',  ( 99.63185314732805864, -32.29918761127225224, 128.7290427505439823 ) ) ;
#57070 = EDGE_CURVE ( 'NONE', #43122, #17548, #2541, .T. ) ;
#57071 = CARTESIAN_POINT ( 'NONE',  ( 112.1357519924663819, -28.01076024733613679, 94.65678908386330193 ) ) ;
#57072 = ADVANCED_FACE ( 'NONE', ( #30240 ), #69785, .T. ) ;
#57073 = DIRECTION ( 'NONE',  ( 1.387778780781444492E-15, 0.000000000000000000, -1.000000000000000000 ) ) ;
#57074 = VERTEX_POINT ( 'NONE', #14383 ) ;
#57075 = EDGE_LOOP ( 'NONE', ( #82187, #34539, #41099, #72930 ) ) ;
#57076 = DIRECTION ( 'NONE',  ( 0.000000000000000000, 0.000000000000000000, -1.000000000000000000 ) ) ;
#57077 = VECTOR ( 'NONE', #25540, 1000.000000000000000 ) ;
#57078 = ORIENTED_EDGE ( 'NONE', *, *, #5497, .T. ) ;
#57079 = VERTEX_POINT ( 'NONE', #57934 ) ;
#57080 = EDGE_CURVE ( 'NONE', #41873, #83946, #84922, .T. ) ;
#57081 = CARTESIAN_POINT ( 'NONE',  ( 102.8293847037436421, -28.94642981657014147, 141.9044404487549684 ) ) ;
#57082 = DIRECTION ( 'NONE',  ( 0.000000000000000000, 1.000000000000000000, 0.000000000000000000 ) ) ;
#57083 = CARTESIAN_POINT ( 'NONE',  ( 116.5531001583795216, -32.35436324414348519, 100.1699109901969535 ) ) ;
#57084 = AXIS2_PLACEMENT_3D ( 'NONE', #22484, #46904, #80128 ) ;
#57085 = CARTESIAN_POINT ( 'NONE',  ( 110.9644701411503718, -45.93855847050220120, 17.89510309453403991 ) ) ;
#57086 = ORIENTED_EDGE ( 'NONE', *, *, #30132, .F. ) ;
#57087 = ORIENTED_EDGE ( 'NONE', *, *, #24559, .T. ) ;
#57088 = ORIENTED_EDGE ( 'NONE', *, *, #25920, .T. ) ;
#57089 = CARTESIAN_POINT ( 'NONE',  ( 99.48556355041279176, -43.91805062995148745, 81.92991099019597812 ) ) ;
#57090 = ORIENTED_EDGE ( 'NONE', *, *, #41850, .F. ) ;
#57091 = CARTESIAN_POINT ( 'NONE',  ( 97.54182784580959265, -34.36413255816223966, 276.1327681330543555 ) ) ;
#57092 = CARTESIAN_POINT ( 'NONE',  ( 109.4502800619034417, -25.91266766229690433, 175.8918157521009391 ) ) ;
#57093 = FACE_BOUND ( 'NONE', #1947, .T. ) ;
#57094 = FACE_OUTER_BOUND ( 'NONE', #16292, .T. ) ;
#57095 = CARTESIAN_POINT ( 'NONE',  ( 107.9456208643995012, -25.71123053419755422, 111.0251490854349754 ) ) ;
#57096 = CARTESIAN_POINT ( 'NONE',  ( -487.2989999999999782, 86.51875000000001137, 86.36305401447658880 ) ) ;
#57097 = ORIENTED_EDGE ( 'NONE', *, *, #58920, .F. ) ;
#57098 = CARTESIAN_POINT ( 'NONE',  ( 70.06670390244707392, -140.6784471599409869, 55.21780685541800437 ) ) ;
#57099 = EDGE_LOOP ( 'NONE', ( #50611, #73206, #25271, #53475 ) ) ;
#57100 = CARTESIAN_POINT ( 'NONE',  ( 97.83885989710027786, -40.58323732884709045, 132.6416815133410694 ) ) ;
#57101 = ORIENTED_EDGE ( 'NONE', *, *, #66652, .T. ) ;
#57102 = EDGE_CURVE ( 'NONE', #69894, #51700, #44228, .T. ) ;
#57103 = ORIENTED_EDGE ( 'NONE', *, *, #61886, .T. ) ;
#57104 = AXIS2_PLACEMENT_3D ( 'NONE', #3305, #1966, #84647 ) ;
#57105 = FACE_OUTER_BOUND ( 'NONE', #59444, .T. ) ;
#57106 = CARTESIAN_POINT ( 'NONE',  ( 4.442782598225926805, 94.34796714030134979, 118.4733406123303610 ) ) ;
#57107 = CARTESIAN_POINT ( 'NONE',  ( 115.9452887564414851, -42.19329433630747417, 18.38705384733896153 ) ) ;
#57108 = CARTESIAN_POINT ( 'NONE',  ( 30.00000000000003553, 171.0000000000000000, 183.8826257785461280 ) ) ;
#57109 = AXIS2_PLACEMENT_3D ( 'NONE', #54404, #53507, #60339 ) ;
#57110 = CARTESIAN_POINT ( 'NONE',  ( 172.5667039024478413, -36.32844715993500273, 249.9678068554149775 ) ) ;
#57111 = DIRECTION ( 'NONE',  ( -0.000000000000000000, -1.000000000000000000, 0.000000000000000000 ) ) ;
#57112 = CARTESIAN_POINT ( 'NONE',  ( 115.1932381579440943, -43.17108053757048935, 48.30514908543492680 ) ) ;
#57114 = CARTESIAN_POINT ( 'NONE',  ( 108.3633857348901159, -47.68307073960293963, 158.6822919425779617 ) ) ;
#57113 = CARTESIAN_POINT ( 'NONE',  ( 97.31316628587843809, -38.96101710005021346, 111.5054712859669053 ) ) ;
#57115 = DIRECTION ( 'NONE',  ( -1.000000000000000000, 0.000000000000000000, 0.000000000000000000 ) ) ;
#57116 = CARTESIAN_POINT ( 'NONE',  ( -72.96458098368751166, 127.0000000000000000, 78.00648098368618832 ) ) ;
#57117 = ORIENTED_EDGE ( 'NONE', *, *, #27037, .F. ) ;
#57118 = CARTESIAN_POINT ( 'NONE',  ( 44.45000000000000284, 66.67499999999999716, 257.1750000000000114 ) ) ;
#57119 = DIRECTION ( 'NONE',  ( 1.000000000000000078E-15, -1.000000000000000083E-30, -1.000000000000000000 ) ) ;
#57120 = DIRECTION ( 'NONE',  ( -3.100000000000000258E-29, 3.100000000000000044E-14, 1.000000000000000000 ) ) ;
#57121 = ORIENTED_EDGE ( 'NONE', *, *, #84378, .T. ) ;
#57122 = CYLINDRICAL_SURFACE ( 'NONE', #44818, 5.041900000000001825 ) ;
#57123 = EDGE_CURVE ( 'NONE', #46574, #75933, #85667, .T. ) ;
#57125 = VERTEX_POINT ( 'NONE', #22538 ) ;
#57124 = CARTESIAN_POINT ( 'NONE',  ( 117.4703304800641206, -30.95114626853415984, 179.2299109901959753 ) ) ;
#57126 = CARTESIAN_POINT ( 'NONE',  ( 25.56670390244797275, -48.82844715994099971, 254.4678068554150343 ) ) ;
#57127 = CARTESIAN_POINT ( 'NONE',  ( 117.2487272683742532, -41.08916198262414099, 209.5165776568640013 ) ) ;
#57128 = CARTESIAN_POINT ( 'NONE',  ( 113.3686263934108780, -27.59268128360266914, 85.60800622829195561 ) ) ;
#57129 = CARTESIAN_POINT ( 'NONE',  ( 34.33598329127389093, -36.32844715994141893, 117.4678068554150485 ) ) ;
#57130 = CARTESIAN_POINT ( 'NONE',  ( 108.4150567101785896, -26.73472737019633172, 190.9689174417968616 ) ) ;
#57131 = CARTESIAN_POINT ( 'NONE',  ( 0.000000000000000000, 152.3879256507328250, 0.000000000000000000 ) ) ;
#57132 = EDGE_LOOP ( 'NONE', ( #14571, #52473, #36019, #52278 ) ) ;
#57133 = EDGE_CURVE ( 'NONE', #78225, #23885, #50217, .T. ) ;
#57134 = VECTOR ( 'NONE', #64460, 1000.000000000000000 ) ;
#57135 = AXIS2_PLACEMENT_3D ( 'NONE', #68506, #7177, #62125 ) ;
#57136 = VECTOR ( 'NONE', #64398, 1000.000000000000000 ) ;
#57137 = ORIENTED_EDGE ( 'NONE', *, *, #84722, .F. ) ;
#57138 = EDGE_LOOP ( 'NONE', ( #4796, #14992, #82230, #3910 ) ) ;
#57139 = AXIS2_PLACEMENT_3D ( 'NONE', #4892, #61188, #20326 ) ;
#57140 = ORIENTED_EDGE ( 'NONE', *, *, #14847, .F. ) ;
#57141 = DIRECTION ( 'NONE',  ( -3.100000000000000258E-29, 3.100000000000000044E-14, 1.000000000000000000 ) ) ;
#57142 = CARTESIAN_POINT ( 'NONE',  ( 112.4117637605556297, -46.40425760712833636, 248.9661014663869878 ) ) ;
#57143 = DIRECTION ( 'NONE',  ( -0.000000000000000000, -0.000000000000000000, -1.000000000000000000 ) ) ;
#57144 = DIRECTION ( 'NONE',  ( 0.000000000000000000, -1.000000000000000000, 0.000000000000000000 ) ) ;
#57145 = PRODUCT_DEFINITION ( 'UNKNOWN', '', #5804, #62612 ) ;
#57147 = CARTESIAN_POINT ( 'NONE',  ( 97.81193015299326987, -40.51731617131004271, 31.63594527021773573 ) ) ;
#57146 = LINE ( 'NONE', #16285, #16316 ) ;
#57148 = FACE_OUTER_BOUND ( 'NONE', #5154, .T. ) ;
#57149 = CARTESIAN_POINT ( 'NONE',  ( 99.11053040751089327, -44.43647348971805400, 41.95086337114900488 ) ) ;
#57150 = ORIENTED_EDGE ( 'NONE', *, *, #65706, .F. ) ;
#57151 = VERTEX_POINT ( 'NONE', #48862 ) ;
#57152 = VERTEX_POINT ( 'NONE', #35246 ) ;
#57153 = FILL_AREA_STYLE_COLOUR ( '', #55745 ) ;
#57154 = CARTESIAN_POINT ( 'NONE',  ( 97.70647924652797656, -40.25110015705713096, 17.61264076450902039 ) ) ;
#57155 = CARTESIAN_POINT ( 'NONE',  ( 111.5675350091814266, -45.45035926415653194, 268.9556252759110180 ) ) ;
#57156 = ADVANCED_FACE ( 'NONE', ( #36618 ), #84331, .F. ) ;
#57157 = DIRECTION ( 'NONE',  ( -3.999999999999999995E-14, 1.000000000000000000, -4.100000000000000342E-29 ) ) ;
#57158 = CARTESIAN_POINT ( 'NONE',  ( 113.5922197990810645, -29.44396856740777224, 110.4956252759109816 ) ) ;
#57159 = EDGE_CURVE ( 'NONE', #35999, #87914, #71141, .T. ) ;
#57160 = ADVANCED_FACE ( 'NONE', ( #21650 ), #22601, .T. ) ;
#57161 = CARTESIAN_POINT ( 'NONE',  ( 100.8872389986638041, -44.70003178514691911, 27.05226840473932626 ) ) ;
#57162 = ORIENTED_EDGE ( 'NONE', *, *, #53651, .F. ) ;
#57163 = FACE_OUTER_BOUND ( 'NONE', #32944, .T. ) ;
#57164 = EDGE_CURVE ( 'NONE', #61470, #63620, #64319, .T. ) ;
#57165 = CARTESIAN_POINT ( 'NONE',  ( 77.48363092588479617, -35.78502016655541951, 2.871594975604034872 ) ) ;
#57166 = ORIENTED_EDGE ( 'NONE', *, *, #59195, .T. ) ;
#57167 = VERTEX_POINT ( 'NONE', #35699 ) ;
#57168 = CARTESIAN_POINT ( 'NONE',  ( -91.91945768840186304, 86.64222086580515736, 74.87617104506270493 ) ) ;
#57169 = CARTESIAN_POINT ( 'NONE',  ( 99.26659991834783625, -39.13601125124746716, 19.38237608387593980 ) ) ;
#57170 = CIRCLE ( 'NONE', #68799, 5.562599999999973122 ) ;
#57171 = EDGE_CURVE ( 'NONE', #36108, #60356, #5146, .T. ) ;
#57172 = FACE_OUTER_BOUND ( 'NONE', #29047, .T. ) ;
#57173 = CIRCLE ( 'NONE', #68804, 34.13125000000000142 ) ;
#57174 = DIRECTION ( 'NONE',  ( 0.7071067811864656383, 0.7071067811866295072, 7.071067811864962574E-16 ) ) ;
#57175 = ADVANCED_FACE ( 'NONE', ( #71586 ), #9346, .T. ) ;
#57176 = DIRECTION ( 'NONE',  ( 0.9834602067019598826, 0.1811243270069988198, 0.000000000000000000 ) ) ;
#57177 = ORIENTED_EDGE ( 'NONE', *, *, #38964, .T. ) ;
#57178 = CARTESIAN_POINT ( 'NONE',  ( 163.0959832912770082, -23.42844715993521021, 313.9678068554149490 ) ) ;
#57179 = CARTESIAN_POINT ( 'NONE',  ( 25.56670390244797275, -62.87844715994099687, 257.2178068554150059 ) ) ;
#57180 = VERTEX_POINT ( 'NONE', #66528 ) ;
#57181 = CARTESIAN_POINT ( 'NONE',  ( 98.72235591169328472, -42.97945265871884857, 66.83848241876793850 ) ) ;
#57182 = ORIENTED_EDGE ( 'NONE', *, *, #15852, .F. ) ;
#57183 = CARTESIAN_POINT ( 'NONE',  ( 106.6898958108015307, -27.68119582636871456, 39.52003887569599527 ) ) ;
#57184 = CARTESIAN_POINT ( 'NONE',  ( 106.1586424053106299, -121.2541776101292186, -11.78219314458148226 ) ) ;
#57185 = CARTESIAN_POINT ( 'NONE',  ( 116.6595528204499601, -34.65899032542078118, 183.9956252759109532 ) ) ;
#57186 = CARTESIAN_POINT ( 'NONE',  ( -23.27731929905162289, 53.97500000000000142, 30.16249999999999076 ) ) ;
#57187 = CARTESIAN_POINT ( 'NONE',  ( 62.03715912545828814, -47.82818131006021645, 237.4678068554150059 ) ) ;
#57188 = FACE_OUTER_BOUND ( 'NONE', #60902, .T. ) ;
#57189 = CARTESIAN_POINT ( 'NONE',  ( 68.89605193404321426, -69.54336780055659517, 247.4970672530039053 ) ) ;
#57190 = CARTESIAN_POINT ( 'NONE',  ( 118.1491249375158645, -36.11907637682050165, 269.8822919425776945 ) ) ;
#57191 = CARTESIAN_POINT ( 'NONE',  ( 112.4702123878613804, -45.17926194093625014, 118.0310380580964420 ) ) ;
#57192 = ORIENTED_EDGE ( 'NONE', *, *, #41135, .T. ) ;
#57193 = CARTESIAN_POINT ( 'NONE',  ( 116.3212776292296127, -32.94146857471318413, 287.6356252759109680 ) ) ;
#57194 = AXIS2_PLACEMENT_3D ( 'NONE', #83918, #49360, #75746 ) ;
#57195 = ORIENTED_EDGE ( 'NONE', *, *, #7117, .F. ) ;
#57196 = CARTESIAN_POINT ( 'NONE',  ( 108.5961642634028692, -47.12166094979025388, 138.6927681330539883 ) ) ;
#57197 = DIRECTION ( 'NONE',  ( 0.000000000000000000, -1.000000000000000000, 0.000000000000000000 ) ) ;
#57198 = VECTOR ( 'NONE', #49993, 1000.000000000000000 ) ;
#57199 = CIRCLE ( 'NONE', #47074, 2.999999999999975131 ) ;
#57200 = CIRCLE ( 'NONE', #20967, 7.143749999999999822 ) ;
#57201 = VERTEX_POINT ( 'NONE', #87434 ) ;
#57202 = ORIENTED_EDGE ( 'NONE', *, *, #12257, .T. ) ;
#57203 = ORIENTED_EDGE ( 'NONE', *, *, #30644, .F. ) ;
#57204 = AXIS2_PLACEMENT_3D ( 'NONE', #43380, #27967, #35681 ) ;
#57205 = FACE_BOUND ( 'NONE', #35800, .T. ) ;
#57206 = DIRECTION ( 'NONE',  ( 0.000000000000000000, 0.000000000000000000, 1.000000000000000000 ) ) ;
#57207 = DIRECTION ( 'NONE',  ( 0.000000000000000000, 1.000000000000000000, 0.000000000000000000 ) ) ;
#57208 = CARTESIAN_POINT ( 'NONE',  ( 145.2600001062945978, -139.0446694607154257, 247.0600440238950171 ) ) ;
#57209 = CARTESIAN_POINT ( 'NONE',  ( 107.0664832912739399, -36.72944715994095333, 311.6343304127839815 ) ) ;
#57210 = CARTESIAN_POINT ( 'NONE',  ( 100.5507766775973835, -27.80086676837388637, 26.56610146638793779 ) ) ;
#57211 = CYLINDRICAL_SURFACE ( 'NONE', #24716, 3.000000000000002665 ) ;
#57212 = VERTEX_POINT ( 'NONE', #59263 ) ;
#57213 = CARTESIAN_POINT ( 'NONE',  ( 9.269761168585562316, 73.85903009410975528, 118.1934132596428668 ) ) ;
#57214 = PLANE ( 'NONE',  #25854 ) ;
#57215 = EDGE_CURVE ( 'NONE', #81490, #78010, #80245, .T. ) ;
#57216 = ORIENTED_EDGE ( 'NONE', *, *, #19222, .F. ) ;
#57217 = ORIENTED_EDGE ( 'NONE', *, *, #11600, .F. ) ;
#57218 = FACE_OUTER_BOUND ( 'NONE', #31225, .T. ) ;
#57219 = DIRECTION ( 'NONE',  ( 0.000000000000000000, 0.000000000000000000, -1.000000000000000000 ) ) ;
#57220 = LINE ( 'NONE', #78603, #29838 ) ;
#57221 = EDGE_CURVE ( 'NONE', #6370, #18422, #31112, .T. ) ;
#57222 = FACE_BOUND ( 'NONE', #64926, .T. ) ;
#57223 = FACE_OUTER_BOUND ( 'NONE', #35378, .T. ) ;
#57224 = CARTESIAN_POINT ( 'NONE',  ( 106.9632158956753756, -45.78494306966059924, 232.0019436376009594 ) ) ;
#57226 = CARTESIAN_POINT ( 'NONE',  ( 110.3650187231686601, -47.25482062520513438, 48.80610146638797175 ) ) ;
#57225 = DIRECTION ( 'NONE',  ( 0.000000000000000000, 0.000000000000000000, 1.000000000000000000 ) ) ;
#57227 = DIRECTION ( 'NONE',  ( 0.000000000000000000, 1.000000000000000000, 0.000000000000000000 ) ) ;
#57228 = CARTESIAN_POINT ( 'NONE',  ( 117.3971137516355014, -38.63466851614541753, 88.68133956162493803 ) ) ;
#57229 = EDGE_LOOP ( 'NONE', ( #6866, #78778 ) ) ;
#57230 = DIRECTION ( 'NONE',  ( -0.000000000000000000, -0.000000000000000000, -1.000000000000000000 ) ) ;
#57231 = ORIENTED_EDGE ( 'NONE', *, *, #23601, .F. ) ;
#57232 = CARTESIAN_POINT ( 'NONE',  ( 99.09570904887901577, -30.55043178771423129, 66.80229194605105647 ) ) ;
#57233 = LINE ( 'NONE', #84978, #58660 ) ;
#57234 = ORIENTED_EDGE ( 'NONE', *, *, #65361, .T. ) ;
#57235 = DIRECTION ( 'NONE',  ( 7.980413499659429724E-32, 1.000000000000000000, -3.785359618865284342E-16 ) ) ;
#57236 = ORIENTED_EDGE ( 'NONE', *, *, #21202, .T. ) ;
#57237 = CARTESIAN_POINT ( 'NONE',  ( -34.75390121890993811, 65.59999999999998010, 71.80362806563780964 ) ) ;
#57238 = LINE ( 'NONE', #84983, #78097 ) ;
#57239 = CIRCLE ( 'NONE', #50032, 5.599999999999994316 ) ;
#57240 = DIRECTION ( 'NONE',  ( -1.000000000000000078E-15, 1.000000000000000083E-30, 1.000000000000000000 ) ) ;
#57241 = ORIENTED_EDGE ( 'NONE', *, *, #33598, .T. ) ;
#57242 = EDGE_CURVE ( 'NONE', #70634, #6412, #82077, .T. ) ;
#57243 = CARTESIAN_POINT ( 'NONE',  ( 96.63442969565970486, -37.29391305320381633, 76.36991099019697060 ) ) ;
#57244 = CARTESIAN_POINT ( 'NONE',  ( 0.000000000000000000, 0.000000000000000000, 0.000000000000000000 ) ) ;
#57245 = CIRCLE ( 'NONE', #64454, 3.250000000000002665 ) ;
#57246 = CARTESIAN_POINT ( 'NONE',  ( 97.81168895331838087, -40.51742574516882200, 287.6356252759109680 ) ) ;
#57247 = CARTESIAN_POINT ( 'NONE',  ( 173.9899999999999807, 52.73749999999999716, -44.45000000000000284 ) ) ;
#57248 = DIRECTION ( 'NONE',  ( -1.000000000000000000, 0.000000000000000000, 0.000000000000000000 ) ) ;
#57249 = EDGE_LOOP ( 'NONE', ( #51831, #84591, #85537, #42606, #82597 ) ) ;
#57250 = DIRECTION ( 'NONE',  ( 1.000000000000000078E-15, -1.000000000000000000, 0.000000000000000000 ) ) ;
#57251 = LINE ( 'NONE', #84998, #77382 ) ;
#57252 = CARTESIAN_POINT ( 'NONE',  ( 110.2536356736639220, -106.6957733451327215, -19.78219314458193168 ) ) ;
#57253 = CARTESIAN_POINT ( 'NONE',  ( 98.43831584450654759, -42.68208710540699258, 122.8070538473389490 ) ) ;
#57255 = DIRECTION ( 'NONE',  ( -1.000000000000000078E-15, 1.000000000000000083E-30, 1.000000000000000000 ) ) ;
#57254 = CYLINDRICAL_SURFACE ( 'NONE', #17515, 8.636000000000004562 ) ;
#57256 = CARTESIAN_POINT ( 'NONE',  ( 151.0371591254582597, -46.82818131005593187, 300.4678068554149490 ) ) ;
#57257 = AXIS2_PLACEMENT_3D ( 'NONE', #77510, #35712, #83890 ) ;
#57258 = ORIENTED_EDGE ( 'NONE', *, *, #63680, .T. ) ;
#57259 = CIRCLE ( 'NONE', #35535, 2.517500000000005844 ) ;
#57260 = AXIS2_PLACEMENT_3D ( 'NONE', #40638, #87902, #61517 ) ;
#57261 = VECTOR ( 'NONE', #11520, 1000.000000000000000 ) ;
#57262 = DIRECTION ( 'NONE',  ( 1.821299053822143307E-16, 0.000000000000000000, -1.000000000000000000 ) ) ;
#57263 = CARTESIAN_POINT ( 'NONE',  ( 116.6595528204498464, -34.65899032542080960, 179.9956252759109532 ) ) ;
#57264 = ADVANCED_FACE ( 'NONE', ( #32006 ), #10236, .F. ) ;
#57266 = EDGE_LOOP ( 'NONE', ( #8380, #35806, #52094, #89151 ) ) ;
#57265 = CARTESIAN_POINT ( 'NONE',  ( 71.24076473329810710, 5.642044068322332961, 394.9756252759101471 ) ) ;
#57267 = VECTOR ( 'NONE', #79613, 1000.000000000000000 ) ;
#57268 = AXIS2_PLACEMENT_3D ( 'NONE', #44085, #38179, #16408 ) ;
#57269 = CARTESIAN_POINT ( 'NONE',  ( 115.8929840288991642, -32.51563116083749350, 15.18133956162492915 ) ) ;
#57270 = CARTESIAN_POINT ( 'NONE',  ( 172.5664832912740110, -9.303447159940999356, 136.8086252759119645 ) ) ;
#57271 = LINE ( 'NONE', #52112, #31601 ) ;
#57272 = PLANE ( 'NONE',  #2310 ) ;
#57273 = ADVANCED_FACE ( 'NONE', ( #24318 ), #16609, .T. ) ;
#57274 = DIRECTION ( 'NONE',  ( 0.000000000000000000, 0.000000000000000000, -1.000000000000000000 ) ) ;
#57275 = DIRECTION ( 'NONE',  ( 5.512527431108029424E-15, -1.000000000000000000, 0.000000000000000000 ) ) ;
#57276 = EDGE_CURVE ( 'NONE', #22553, #50424, #65639, .T. ) ;
#57277 = CARTESIAN_POINT ( 'NONE',  ( 100.0046238269856929, -29.91446987444270178, 250.7156252759109520 ) ) ;
#57278 = VERTEX_POINT ( 'NONE', #86553 ) ;
#57279 = ORIENTED_EDGE ( 'NONE', *, *, #36483, .T. ) ;
#57280 = CARTESIAN_POINT ( 'NONE',  ( 98.85146132857330770, -40.05235142642286661, 203.0644404487539703 ) ) ;
#57281 = DIRECTION ( 'NONE',  ( -0.9834602067153815907, -0.1811243269341220596, 0.000000000000000000 ) ) ;
#57282 = CARTESIAN_POINT ( 'NONE',  ( 111.1996377132626748, -28.89074107182586815, 56.12158330589694799 ) ) ;
#57283 = CARTESIAN_POINT ( 'NONE',  ( 23.75871628398702384, 82.70597876660713155, 307.6575000000001410 ) ) ;
#57284 = CARTESIAN_POINT ( 'NONE',  ( 99.04399467038047078, -42.84115622384206290, 266.8440302632771477 ) ) ;
#57285 = EDGE_CURVE ( 'NONE', #58867, #30864, #89678, .T. ) ;
#57286 = CARTESIAN_POINT ( 'NONE',  ( 103.8797721312301405, -101.8611209747507189, 2.217806855417919998 ) ) ;
#57287 = ORIENTED_EDGE ( 'NONE', *, *, #32327, .T. ) ;
#57288 = DIRECTION ( 'NONE',  ( 1.000000000000000000, 3.999999999999999995E-14, 1.000000000000000078E-15 ) ) ;
#57289 = CARTESIAN_POINT ( 'NONE',  ( 123.6837132603321692, -53.34645651782491882, 249.5838068554164693 ) ) ;
#57290 = EDGE_CURVE ( 'NONE', #64042, #17117, #25275, .T. ) ;
#57291 = CARTESIAN_POINT ( 'NONE',  ( 96.54020141486694229, -31.34005042439572009, 245.9499109901969689 ) ) ;
#57292 = CARTESIAN_POINT ( 'NONE',  ( 91.06648329127389729, -36.72944715993924802, 13.92562527591095467 ) ) ;
#57293 = VERTEX_POINT ( 'NONE', #74690 ) ;
#57294 = VERTEX_POINT ( 'NONE', #39709 ) ;
#57295 = CARTESIAN_POINT ( 'NONE',  ( 115.0372575007767466, -42.90846257426783694, 88.30229194183291952 ) ) ;
#57296 = CARTESIAN_POINT ( 'NONE',  ( -86.67541640318120244, 94.58006533271586136, -80.88915705228883724 ) ) ;
#57297 = CARTESIAN_POINT ( 'NONE',  ( 98.38028489613425620, -41.69503615009242736, 122.7390885072009468 ) ) ;
#57298 = CARTESIAN_POINT ( 'NONE',  ( 177.8371591254545478, -47.82818131005477369, 129.9678068554150059 ) ) ;
#57299 = CARTESIAN_POINT ( 'NONE',  ( 111.1466539572837320, -45.61852150024213870, 23.91848241876692782 ) ) ;
#57300 = CARTESIAN_POINT ( 'NONE',  ( 44.45000000000000284, 66.67499999999999716, 257.1750000000000114 ) ) ;
#57301 = ORIENTED_EDGE ( 'NONE', *, *, #47071, .F. ) ;
#57302 = CARTESIAN_POINT ( 'NONE',  ( 115.0558824863888390, -43.54908903376227158, 59.26419670448196086 ) ) ;
#57303 = DIRECTION ( 'NONE',  ( -1.000000000000000078E-15, 1.000000000000000000, 0.000000000000000000 ) ) ;
#57304 = B_SPLINE_CURVE_WITH_KNOTS ( 'NONE', 3,
 ( #1236, #89833, #29387, #22579, #57068, #71179, #49806, #62992, #70267, #69825, #62551, #50251 ),
 .UNSPECIFIED., .F., .F.,
 ( 4, 2, 2, 2, 2, 4 ),
 ( 0.000000000000000000, 0.0008380503122013481217, 0.001676100624402696243, 0.002514150936604044474, 0.002933176092704727154, 0.003352201248805410268 ),
 .UNSPECIFIED. ) ;
#57305 = AXIS2_PLACEMENT_3D ( 'NONE', #37036, #57920, #64742 ) ;
#57306 = CARTESIAN_POINT ( 'NONE',  ( 110.2909773106953111, -46.66674596437654543, 12.82705384733995402 ) ) ;
#57307 = ORIENTED_EDGE ( 'NONE', *, *, #44117, .F. ) ;
#57308 = DIRECTION ( 'NONE',  ( 0.7071067811989762975, -0.7071067811741188480, 7.071067811989771216E-16 ) ) ;
#57309 = CARTESIAN_POINT ( 'NONE',  ( 194.5667039024479834, -48.82844715994099971, 310.9178068554150514 ) ) ;
#57310 = LINE ( 'NONE', #72306, #87207 ) ;
#57311 = CARTESIAN_POINT ( 'NONE',  ( 98.42009728606723229, -37.10485906011713553, 114.1671379886389559 ) ) ;
#57312 = CARTESIAN_POINT ( 'NONE',  ( 113.6994007951720107, -45.60016365472323230, 184.0994347997199725 ) ) ;
#57313 = FACE_OUTER_BOUND ( 'NONE', #49769, .T. ) ;
#57314 = VERTEX_POINT ( 'NONE', #40156 ) ;
#57315 = CARTESIAN_POINT ( 'NONE',  ( 48.45959712127301344, -26.00627455219131789, -5.074374724088000832 ) ) ;
#57316 = ORIENTED_EDGE ( 'NONE', *, *, #88370, .T. ) ;
#57317 = EDGE_LOOP ( 'NONE', ( #57090, #31914, #17091, #35183 ) ) ;
#57318 = VECTOR ( 'NONE', #70939, 1000.000000000000000 ) ;
#57319 = AXIS2_PLACEMENT_3D ( 'NONE', #8819, #632, #56025 ) ;
#57320 = DIRECTION ( 'NONE',  ( 0.000000000000000000, 0.7071067811865600072, 0.7071067811865350272 ) ) ;
#57321 = AXIS2_PLACEMENT_3D ( 'NONE', #61080, #88365, #82895 ) ;
#57322 = ORIENTED_EDGE ( 'NONE', *, *, #37105, .F. ) ;
#57323 = ORIENTED_EDGE ( 'NONE', *, *, #45006, .T. ) ;
#57324 = DIRECTION ( 'NONE',  ( 0.000000000000000000, -1.000000000000000000, 0.000000000000000000 ) ) ;
#57325 = CIRCLE ( 'NONE', #70452, 4.750000000000004441 ) ;
#57326 = ADVANCED_FACE ( 'NONE', ( #40615 ), #53770, .T. ) ;
#57327 = CARTESIAN_POINT ( 'NONE',  ( 103.4331722345071682, -27.41248267999953114, 41.37236127975815236 ) ) ;
#57328 = CARTESIAN_POINT ( 'NONE',  ( 102.9824767429641525, -29.22764064321736299, 144.8952769709339634 ) ) ;
#57330 = CARTESIAN_POINT ( 'NONE',  ( 105.7736212422599777, -26.36243834887274673, 270.1756252759109884 ) ) ;
#57329 = AXIS2_PLACEMENT_3D ( 'NONE', #89343, #33908, #34804 ) ;
#57331 = CARTESIAN_POINT ( 'NONE',  ( 172.5667039024478129, -36.32844715993500273, 300.4678068554149490 ) ) ;
#57332 = ORIENTED_EDGE ( 'NONE', *, *, #18188, .F. ) ;
#57333 = AXIS2_PLACEMENT_3D ( 'NONE', #16730, #78078, #29919 ) ;
#57334 = ORIENTED_EDGE ( 'NONE', *, *, #48176, .T. ) ;
#57335 = CARTESIAN_POINT ( 'NONE',  ( 45.76696975232824371, -48.62818131006036992, 300.4678068554150059 ) ) ;
#57336 = DIRECTION ( 'NONE',  ( -0.2588190451025219607, 0.000000000000000000, -0.9659258262890678681 ) ) ;
#57337 = CARTESIAN_POINT ( 'NONE',  ( 70.74975129634796644, -139.3183301492457247, 247.4318526551172113 ) ) ;
#57338 = VECTOR ( 'NONE', #30030, 1000.000000000000000 ) ;
#57339 = B_SPLINE_CURVE_WITH_KNOTS ( 'NONE', 3,
 ( #8141, #29035, #67908, #32930, #60179, #66559, #82009, #54695, #19764, #33386, #47443, #32478, #46550, #5696, #54243, #74284, #12056, #47890 ),
 .UNSPECIFIED., .F., .F.,
 ( 4, 2, 2, 2, 2, 2, 2, 2, 4 ),
 ( 0.000000000000000000, 0.06249933430492867620, 0.1249986686098573524, 0.1874980029147860217, 0.2499973372197147048, 0.3124966715246433879, 0.3749960058295720433, 0.4374953401345007542, 0.4999946744394294096 ),
 .UNSPECIFIED. ) ;
#57340 = CARTESIAN_POINT ( 'NONE',  ( 98.29927950267186532, -42.45157995928803984, 101.7870538473399620 ) ) ;
#57341 = CARTESIAN_POINT ( 'NONE',  ( 101.0612956599395602, -45.30524461813642745, 282.0899109901967563 ) ) ;
#57342 = ORIENTED_EDGE ( 'NONE', *, *, #74397, .T. ) ;
#57343 =( REPRESENTATION_RELATIONSHIP ('NONE','NONE', #82876, #19449 ) REPRESENTATION_RELATIONSHIP_WITH_TRANSFORMATION ( #63518 )SHAPE_REPRESENTATION_RELATIONSHIP( ) );
#57344 = EDGE_CURVE ( 'NONE', #47547, #43903, #798, .T. ) ;
#57345 = CARTESIAN_POINT ( 'NONE',  ( 96.91416677013903325, -34.20826173260762459, 276.1327681330537871 ) ) ;
#57346 = CARTESIAN_POINT ( 'NONE',  ( 83.06670390244796920, -58.72944715994098175, 228.3338068554150198 ) ) ;
#57347 =( NAMED_UNIT ( * ) PLANE_ANGLE_UNIT ( ) SI_UNIT ( $, .RADIAN. ) );
#57348 = CARTESIAN_POINT ( 'NONE',  ( 10.86079732252673580, 75.96631587555827991, 130.1035022676263679 ) ) ;
#57349 = CARTESIAN_POINT ( 'NONE',  ( 97.81943421394399252, -40.53634900077776848, 27.63767384540028971 ) ) ;
#57350 = CIRCLE ( 'NONE', #83494, 1.219499999999975159 ) ;
#57352 = DIRECTION ( 'NONE',  ( 0.000000000000000000, 1.000000000000000000, 0.000000000000000000 ) ) ;
#57351 = LINE ( 'NONE', #16930, #37553 ) ;
#57353 = FACE_BOUND ( 'NONE', #48465, .T. ) ;
#57354 = DIRECTION ( 'NONE',  ( 1.000000000000000000, 0.000000000000000000, -0.000000000000000000 ) ) ;
#57355 = CARTESIAN_POINT ( 'NONE',  ( 0.000000000000000000, 92.07499999999998863, 0.000000000000000000 ) ) ;
#57356 = DIRECTION ( 'NONE',  ( 0.000000000000000000, 1.000000000000000000, 0.000000000000000000 ) ) ;
#57357 = DIRECTION ( 'NONE',  ( 0.000000000000000000, 0.000000000000000000, 1.000000000000000000 ) ) ;
#57358 = EDGE_CURVE ( 'NONE', #85897, #59253, #68332, .T. ) ;
#57359 = DIRECTION ( 'NONE',  ( -0.9130365726098601531, 0.000000000000000000, -0.4078776986755214828 ) ) ;
#57361 = EDGE_LOOP ( 'NONE', ( #15909, #41228, #13845, #27493 ) ) ;
#57360 = CARTESIAN_POINT ( 'NONE',  ( 71.06670390244701707, -83.77844715994098124, 45.21780685541799727 ) ) ;
#57362 = ADVANCED_FACE ( 'NONE', ( #46960 ), #67877, .T. ) ;
#57363 = DIRECTION ( 'NONE',  ( 1.000000000000000078E-15, 1.000000000000000083E-30, -1.000000000000000000 ) ) ;
#57364 = CARTESIAN_POINT ( 'NONE',  ( 112.1386966202503430, -26.85596833298010111, 19.71086337114896736 ) ) ;
#57365 = CARTESIAN_POINT ( 'NONE',  ( 102.8440116971490852, -46.26114276377411016, 173.2441967044829596 ) ) ;
#57366 = CARTESIAN_POINT ( 'NONE',  ( 112.2081591769286177, -26.91769754996824560, 10.68038718067299087 ) ) ;
#57368 = CARTESIAN_POINT ( 'NONE',  ( 81.60736025277958561, -34.45223222829589815, 7.843813999040315288 ) ) ;
#57367 = DIRECTION ( 'NONE',  ( -6.524622321627019585E-16, -3.741823817616790462E-31, -1.000000000000000000 ) ) ;
#57369 = FACE_OUTER_BOUND ( 'NONE', #31159, .T. ) ;
#57370 = CIRCLE ( 'NONE', #18206, 2.117000000000000881 ) ;
#57371 = CIRCLE ( 'NONE', #68995, 2.517499999999998739 ) ;
#57372 = ADVANCED_FACE ( 'NONE', ( #26994 ), #60599, .F. ) ;
#57373 = VERTEX_POINT ( 'NONE', #89230 ) ;
#57374 = CARTESIAN_POINT ( 'NONE',  ( 0.000000000000000000, 65.60000000000000853, 0.000000000000000000 ) ) ;
#57375 = ORIENTED_EDGE ( 'NONE', *, *, #71259, .F. ) ;
#57376 = CARTESIAN_POINT ( 'NONE',  ( 104.9021620152489476, -46.26774620671717031, 68.39848241876694601 ) ) ;
#57378 = EDGE_LOOP ( 'NONE', ( #7969, #62247 ) ) ;
#57377 = CYLINDRICAL_SURFACE ( 'NONE', #39898, 4.750000000000004441 ) ;
#57379 = CARTESIAN_POINT ( 'NONE',  ( 113.1777857331995847, -44.75224829125603776, 49.09390862630768737 ) ) ;
#57380 = CARTESIAN_POINT ( 'NONE',  ( 113.6717327907683597, -45.56316108038139845, 184.0994347997199725 ) ) ;
#57381 = FACE_OUTER_BOUND ( 'NONE', #36539, .T. ) ;
#57382 = DIRECTION ( 'NONE',  ( 0.000000000000000000, 1.000000000000000000, 0.000000000000000000 ) ) ;
#57383 = CARTESIAN_POINT ( 'NONE',  ( 118.5256205435843526, -36.72944715994100306, 293.2242906452868851 ) ) ;
#57384 = EDGE_CURVE ( 'NONE', #6767, #83511, #20629, .T. ) ;
#57385 = CARTESIAN_POINT ( 'NONE',  ( 111.9582691220362847, -27.98680779792547213, 85.67040919175906311 ) ) ;
#57386 = FACE_OUTER_BOUND ( 'NONE', #65042, .T. ) ;
#57387 = CARTESIAN_POINT ( 'NONE',  ( 97.81846061703993200, -40.53393429449062069, 96.63704516963355218 ) ) ;
#57388 = CARTESIAN_POINT ( 'NONE',  ( 100.1408543393098682, -45.42701269980184975, 122.0413395616259606 ) ) ;
#57389 = ORIENTED_EDGE ( 'NONE', *, *, #21042, .F. ) ;
#57390 = EDGE_LOOP ( 'NONE', ( #40294, #25853, #77886, #20461, #19650, #51373, #32218, #57438, #47583, #19292, #13446, #15606, #28613, #29680, #50341, #80839, #33360, #423, #75368, #6011, #78973, #64695, #57590, #53173, #8729, #70175, #45861, #71004, #48915, #55873, #86059, #35983, #63523, #78521, #84621, #46634, #40099, #131, #55681, #76024, #31448, #72531, #82212, #22600, #50765, #81805, #33657, #25028 ) ) ;
#57391 = AXIS2_PLACEMENT_3D ( 'NONE', #72270, #30922, #15067 ) ;
#57392 = CARTESIAN_POINT ( 'NONE',  ( 110.2353755222631833, -45.00509823041481638, 59.29872616303999422 ) ) ;
#57393 = VECTOR ( 'NONE', #34484, 1000.000000000000000 ) ;
#57394 = CARTESIAN_POINT ( 'NONE',  ( 126.8164832912740110, -36.72944715994101017, -4.824374724089010691 ) ) ;
#57395 = AXIS2_PLACEMENT_3D ( 'NONE', #3338, #51896, #59173 ) ;
#57397 = CARTESIAN_POINT ( 'NONE',  ( 181.9790560690337031, -31.62489322947608628, 313.9678068554149490 ) ) ;
#57396 = CARTESIAN_POINT ( 'NONE',  ( 96.02263050233435138, -38.01213896886783061, 232.4184824187679794 ) ) ;
#57398 = DIRECTION ( 'NONE',  ( -1.000000000000000000, 0.000000000000000000, 0.000000000000000000 ) ) ;
#57399 = DIRECTION ( 'NONE',  ( 0.000000000000000000, 0.000000000000000000, 1.000000000000000000 ) ) ;
#57400 = CARTESIAN_POINT ( 'NONE',  ( 107.0664832912739257, -50.72944715994095333, 311.6343304127839815 ) ) ;
#57401 = EDGE_CURVE ( 'NONE', #28060, #46472, #25643, .T. ) ;
#57402 = DIRECTION ( 'NONE',  ( -0.7071067811874389708, 0.7071067811856560636, 0.000000000000000000 ) ) ;
#57403 = CARTESIAN_POINT ( 'NONE',  ( 5.572218945471783869, 71.24158085953891373, 118.4255381658035020 ) ) ;
#57404 = EDGE_CURVE ( 'NONE', #80932, #88430, #82426, .T. ) ;
#57405 = CARTESIAN_POINT ( 'NONE',  ( 98.29923130492881000, -31.06375673945261440, 145.8699109901969848 ) ) ;
#57406 = EDGE_LOOP ( 'NONE', ( #74975, #5365 ) ) ;
#57407 = ORIENTED_EDGE ( 'NONE', *, *, #52348, .T. ) ;
#57408 = ORIENTED_EDGE ( 'NONE', *, *, #65264, .T. ) ;
#57409 = ADVANCED_FACE ( 'NONE', ( #88341 ), #77724, .F. ) ;
#57410 = VECTOR ( 'NONE', #87340, 1000.000000000000000 ) ;
#57411 = FACE_OUTER_BOUND ( 'NONE', #33529, .T. ) ;
#57412 = DIRECTION ( 'NONE',  ( -0.000000000000000000, -1.000000000000000000, -0.000000000000000000 ) ) ;
#57413 = EDGE_CURVE ( 'NONE', #26158, #75304, #31069, .T. ) ;
#57414 = CARTESIAN_POINT ( 'NONE',  ( 113.2439442825823761, -28.75748049084303659, 129.5524476564171437 ) ) ;
#57415 = CARTESIAN_POINT ( 'NONE',  ( 116.7950883839698690, -39.38797980936810461, 104.6147798141180942 ) ) ;
#57417 = CARTESIAN_POINT ( 'NONE',  ( 107.2095755159442376, -27.45176125347251173, 227.8823760838769488 ) ) ;
#57416 = VECTOR ( 'NONE', #6336, 1000.000000000000114 ) ;
#57418 = DIRECTION ( 'NONE',  ( 1.000000000000000000, 0.000000000000000000, 0.000000000000000000 ) ) ;
#57419 = AXIS2_PLACEMENT_3D ( 'NONE', #64097, #36830, #85455 ) ;
#57420 = CARTESIAN_POINT ( 'NONE',  ( 117.3102356154742836, -34.79226824040635790, 158.9756252759109714 ) ) ;
#57421 = CARTESIAN_POINT ( 'NONE',  ( 152.5667039024474718, -23.42844715993585325, 117.4678068554150485 ) ) ;
#57422 = ORIENTED_EDGE ( 'NONE', *, *, #71493, .T. ) ;
#57424 = ORIENTED_EDGE ( 'NONE', *, *, #62807, .F. ) ;
#57423 = ORIENTED_EDGE ( 'NONE', *, *, #22345, .T. ) ;
#57425 = LINE ( 'NONE', #30177, #9947 ) ;
#57426 = ORIENTED_EDGE ( 'NONE', *, *, #45753, .F. ) ;
#57427 = ORIENTED_EDGE ( 'NONE', *, *, #60861, .F. ) ;
#57428 = DIRECTION ( 'NONE',  ( 0.000000000000000000, 1.000000000000000000, 0.000000000000000000 ) ) ;
#57429 = CARTESIAN_POINT ( 'NONE',  ( 131.3164832912740110, -36.72944715994100306, 6.749768910606454675 ) ) ;
#57430 = CARTESIAN_POINT ( 'NONE',  ( 114.0183221777719638, -41.00747610084435024, 16.20523322673395228 ) ) ;
#57431 = DIRECTION ( 'NONE',  ( 0.000000000000000000, 0.000000000000000000, -1.000000000000000000 ) ) ;
#57432 = VERTEX_POINT ( 'NONE', #69225 ) ;
#57433 = CARTESIAN_POINT ( 'NONE',  ( 112.2391605817208529, -43.63979212946189534, 9.635625275910943088 ) ) ;
#57434 = DIRECTION ( 'NONE',  ( 1.000000000000000000, 4.299999999999999979E-14, 1.000000000000000078E-15 ) ) ;
#57435 = ORIENTED_EDGE ( 'NONE', *, *, #83826, .T. ) ;
#57436 = ORIENTED_EDGE ( 'NONE', *, *, #26180, .F. ) ;
#57437 = CARTESIAN_POINT ( 'NONE',  ( 110.9492230250103830, -45.94497800772926155, 112.8937869644549750 ) ) ;
#57438 = ORIENTED_EDGE ( 'NONE', *, *, #51509, .F. ) ;
#57439 = ORIENTED_EDGE ( 'NONE', *, *, #50297, .F. ) ;
#57440 = EDGE_CURVE ( 'NONE', #80299, #13859, #60246, .T. ) ;
#57441 = CARTESIAN_POINT ( 'NONE',  ( 100.5619151801845419, -43.03049977154007166, 41.37337220902998070 ) ) ;
#57442 = CARTESIAN_POINT ( 'NONE',  ( 96.72113125116129595, -35.27340624960861959, 181.2156252759109805 ) ) ;
#57443 = CARTESIAN_POINT ( 'NONE',  ( 98.47430666977638225, -42.65725675464092603, 126.8070538473389490 ) ) ;
#57444 = CARTESIAN_POINT ( 'NONE',  ( 107.0664832912739968, -36.72944715994100306, -2.114374724089040924 ) ) ;
#57445 = CARTESIAN_POINT ( 'NONE',  ( 98.83931482081872844, -29.34787013040062931, 231.7565776568629587 ) ) ;
#57446 = DIRECTION ( 'NONE',  ( 0.000000000000000000, 0.000000000000000000, 1.000000000000000000 ) ) ;
#57447 = CARTESIAN_POINT ( 'NONE',  ( 77.44088674023640806, -88.80595668214708382, 249.3055308415380011 ) ) ;
#57448 = EDGE_LOOP ( 'NONE', ( #13970, #507, #12270, #45684 ) ) ;
#57449 = CARTESIAN_POINT ( 'NONE',  ( -130.3463096697863079, 72.22361908171431821, -7.404590904609003488 ) ) ;
#57450 = VERTEX_POINT ( 'NONE', #34688 ) ;
#57451 = ORIENTED_EDGE ( 'NONE', *, *, #18355, .T. ) ;
#57452 = CONICAL_SURFACE ( 'NONE', #24141, 1.625000000000001332, 1.029744258676650093 ) ;
#57453 = B_SPLINE_CURVE_WITH_KNOTS ( 'NONE', 3,
 ( #79432, #24010, #80321, #73480, #53455, #82119, #68917, #73936, #75732, #46656, #80763, #74388, #61193, #41192, #6684, #61632, #26231, #12613 ),
 .UNSPECIFIED., .F., .F.,
 ( 4, 2, 2, 2, 2, 2, 2, 2, 4 ),
 ( 0.000000000000000000, 0.06249676073301599355, 0.1249935214660319871, 0.1874902821990479806, 0.2499870429320639742, 0.3124838036650799955, 0.3749805643980959613, 0.4374773251311119271, 0.4999740858641279484 ),
 .UNSPECIFIED. ) ;
#57454 = VECTOR ( 'NONE', #67455, 1000.000000000000000 ) ;
#57456 = CARTESIAN_POINT ( 'NONE',  ( 104.4426401758756100, -26.59425533393106633, 200.2784824187679362 ) ) ;
#57455 = CIRCLE ( 'NONE', #79209, 13.50000000000000533 ) ;
#57457 = EDGE_LOOP ( 'NONE', ( #1034, #66739, #16452, #75530 ) ) ;
#57459 = ADVANCED_FACE ( 'NONE', ( #87879 ), #53318, .F. ) ;
#57458 = VECTOR ( 'NONE', #23254, 1000.000000000000000 ) ;
#57460 = CARTESIAN_POINT ( 'NONE',  ( 98.16810232779933187, -31.29751870953477422, 170.8899109901960003 ) ) ;
#57461 = DIRECTION ( 'NONE',  ( 1.000000000000000000, 4.163336342344333240E-14, 0.000000000000000000 ) ) ;
#57462 = CIRCLE ( 'NONE', #58870, 21.75000000000000711 ) ;
#57463 = DIRECTION ( 'NONE',  ( 0.000000000000000000, 0.000000000000000000, 1.000000000000000000 ) ) ;
#57464 = CARTESIAN_POINT ( 'NONE',  ( 173.9900000000000091, 37.33800000000000097, 32.46912895322940074 ) ) ;
#57465 = EDGE_CURVE ( 'NONE', #67672, #74946, #74253, .T. ) ;
#57468 = CARTESIAN_POINT ( 'NONE',  ( 96.29057984255084079, -34.37493501460200207, 252.1432443235302969 ) ) ;
#57467 = CARTESIAN_POINT ( 'NONE',  ( 101.5871053484441120, -45.11049957908544172, 57.11545923762081856 ) ) ;
#57466 = FACE_OUTER_BOUND ( 'NONE', #51026, .T. ) ;
#57469 = LINE ( 'NONE', #56105, #26340 ) ;
#57470 = DIRECTION ( 'NONE',  ( 0.000000000000000000, 0.000000000000000000, -1.000000000000000000 ) ) ;
#57471 = DIRECTION ( 'NONE',  ( 0.000000000000000000, 0.000000000000000000, 1.000000000000000000 ) ) ;
#57472 = ADVANCED_FACE ( 'NONE', ( #5206 ), #12409, .T. ) ;
#57473 = FACE_OUTER_BOUND ( 'NONE', #47986, .T. ) ;
#57474 = FACE_OUTER_BOUND ( 'NONE', #58061, .T. ) ;
#57475 = EDGE_CURVE ( 'NONE', #241, #8294, #177, .T. ) ;
#57476 = DIRECTION ( 'NONE',  ( 4.299999999999999979E-14, -1.000000000000000000, 4.400000000000000367E-29 ) ) ;
#57478 = ORIENTED_EDGE ( 'NONE', *, *, #75444, .F. ) ;
#57477 = CARTESIAN_POINT ( 'NONE',  ( 99.76431239122888428, -40.48807882857454388, 195.5838068554172935 ) ) ;
#57479 = EDGE_CURVE ( 'NONE', #75220, #74301, #47001, .T. ) ;
#57480 = FACE_OUTER_BOUND ( 'NONE', #15, .T. ) ;
#57481 = CARTESIAN_POINT ( 'NONE',  ( 107.6542440074338458, -47.14984605634950299, 152.6213395616249500 ) ) ;
#57482 = CARTESIAN_POINT ( 'NONE',  ( 113.3423928682155406, -27.63071431045342763, 85.60800622829195561 ) ) ;
#57483 = CARTESIAN_POINT ( 'NONE',  ( 101.4018018619443922, -46.27454447023805528, 203.1622919425779514 ) ) ;
#57484 = DIRECTION ( 'NONE',  ( 9.351236661543306751E-17, -3.725950533538267725E-29, -1.000000000000000000 ) ) ;
#57485 = DIRECTION ( 'NONE',  ( 1.000000000000000078E-15, -1.000000000000000083E-30, -1.000000000000000000 ) ) ;
#57486 = AXIS2_PLACEMENT_3D ( 'NONE', #75284, #69368, #42087 ) ;
#57488 = DIRECTION ( 'NONE',  ( 0.000000000000000000, 0.000000000000000000, 1.000000000000000000 ) ) ;
#57487 = DIRECTION ( 'NONE',  ( 0.000000000000000000, -1.000000000000000000, 0.000000000000000000 ) ) ;
#57489 = CARTESIAN_POINT ( 'NONE',  ( 83.56670390244798341, -34.21194715994108293, 239.5838068554169809 ) ) ;
#57490 = CARTESIAN_POINT ( 'NONE',  ( -71.77848634863190114, 120.6499999999999915, 77.39114642429879609 ) ) ;
#57491 = ORIENTED_EDGE ( 'NONE', *, *, #74827, .T. ) ;
#57492 = EDGE_CURVE ( 'NONE', #15894, #79308, #83306, .T. ) ;
#57493 = DIRECTION ( 'NONE',  ( 0.000000000000000000, 0.000000000000000000, 1.000000000000000000 ) ) ;
#57494 = VECTOR ( 'NONE', #81544, 1000.000000000000114 ) ;
#57495 = EDGE_CURVE ( 'NONE', #74639, #41728, #62398, .T. ) ;
#57496 = ORIENTED_EDGE ( 'NONE', *, *, #1386, .T. ) ;
#57497 = ORIENTED_EDGE ( 'NONE', *, *, #40901, .T. ) ;
#57499 = ORIENTED_EDGE ( 'NONE', *, *, #83230, .T. ) ;
#57498 = DIRECTION ( 'NONE',  ( 1.000000000000000000, 0.000000000000000000, 0.000000000000000000 ) ) ;
#57500 = CARTESIAN_POINT ( 'NONE',  ( 98.85726102317303798, -28.21728661942041683, 111.6870538473389587 ) ) ;
#57501 = DIRECTION ( 'NONE',  ( 0.000000000000000000, 0.000000000000000000, 1.000000000000000000 ) ) ;
#57502 = EDGE_CURVE ( 'NONE', #86684, #58845, #3343, .T. ) ;
#57503 = FACE_OUTER_BOUND ( 'NONE', #69648, .T. ) ;
#57504 = DIRECTION ( 'NONE',  ( -0.6537961156249243455, 0.7071067811865289210, -0.2693522585644811951 ) ) ;
#57505 = CARTESIAN_POINT ( 'NONE',  ( 113.6564618781686704, -45.68400828401192371, 33.08133956162595268 ) ) ;
#57506 = EDGE_LOOP ( 'NONE', ( #10987, #67424 ) ) ;
#57507 = ORIENTED_EDGE ( 'NONE', *, *, #58631, .F. ) ;
#57508 = ORIENTED_EDGE ( 'NONE', *, *, #44797, .F. ) ;
#57509 = LINE ( 'NONE', #85252, #39879 ) ;
#57510 = CARTESIAN_POINT ( 'NONE',  ( 150.5667039024473866, -25.42844715993594562, 249.9678068554149490 ) ) ;
#57511 = CYLINDRICAL_SURFACE ( 'NONE', #40464, 9.999999999999998224 ) ;
#57512 = FACE_OUTER_BOUND ( 'NONE', #78799, .T. ) ;
#57513 = CARTESIAN_POINT ( 'NONE',  ( 83.21537498883908768, 85.85000629251467785, 100.5986936721449467 ) ) ;
#57514 = LINE ( 'NONE', #51139, #27748 ) ;
#57515 = CARTESIAN_POINT ( 'NONE',  ( 151.0371591254573502, -24.42818131005592974, 237.4678068554150059 ) ) ;
#57516 = CARTESIAN_POINT ( 'NONE',  ( -8.224930598656271741, 92.23576600848676321, 130.2969003264876449 ) ) ;
#57517 = CARTESIAN_POINT ( 'NONE',  ( 105.4244226815142156, -47.00233879195506148, 37.44991099019695469 ) ) ;
#57518 = ORIENTED_EDGE ( 'NONE', *, *, #49290, .F. ) ;
#57519 = EDGE_CURVE ( 'NONE', #8309, #23727, #34179, .T. ) ;
#57520 = CARTESIAN_POINT ( 'NONE',  ( 97.33784162416169750, -34.07106341398686311, 271.1147918510543491 ) ) ;
#57521 = EDGE_CURVE ( 'NONE', #45437, #59268, #36042, .T. ) ;
#57522 = AXIS2_PLACEMENT_3D ( 'NONE', #39875, #18097, #88054 ) ;
#57523 = DIRECTION ( 'NONE',  ( -1.000000000000000000, 0.000000000000000000, 0.000000000000000000 ) ) ;
#57524 = CARTESIAN_POINT ( 'NONE',  ( 104.0192455041231767, -29.15686055524244935, 128.1995189410199600 ) ) ;
#57525 = CONICAL_SURFACE ( 'NONE', #85111, 1.258750000000002922, 1.029744258676650093 ) ;
#57526 = CIRCLE ( 'NONE', #64728, 2.029999999999997140 ) ;
#57527 = CIRCLE ( 'NONE', #89446, 3.174999999999983391 ) ;
#57528 = CONICAL_SURFACE ( 'NONE', #5267, 1.624999999999987566, 1.029744258676650093 ) ;
#57529 = CARTESIAN_POINT ( 'NONE',  ( 97.80997330134053414, -40.51323221472250680, 96.63526432594667881 ) ) ;
#57530 = CARTESIAN_POINT ( 'NONE',  ( 107.0664832912748068, -36.72944715993923381, -4.074374724089028454 ) ) ;
#57531 = VERTEX_POINT ( 'NONE', #21534 ) ;
#57532 = EDGE_LOOP ( 'NONE', ( #86174, #15107, #8887, #61330 ) ) ;
#57533 = CARTESIAN_POINT ( 'NONE',  ( 98.38056611065501045, -41.69552606520213800, 136.7397481390533756 ) ) ;
#57534 = ORIENTED_EDGE ( 'NONE', *, *, #64096, .T. ) ;
#57535 = ORIENTED_EDGE ( 'NONE', *, *, #55368, .F. ) ;
#57536 = CARTESIAN_POINT ( 'NONE',  ( 115.8726827828676704, -31.83848043880258061, 175.6615833058969827 ) ) ;
#57537 = DIRECTION ( 'NONE',  ( 1.000000000000000000, 0.000000000000000000, 0.000000000000000000 ) ) ;
#57538 = VECTOR ( 'NONE', #10089, 1000.000000000000000 ) ;
#57539 = CARTESIAN_POINT ( 'NONE',  ( 113.8705839548662908, -44.65670854160515546, 104.1413395616249744 ) ) ;
#57540 = CARTESIAN_POINT ( 'NONE',  ( 115.9563521928378691, -41.38085296308364036, 18.44300400888693758 ) ) ;
#57541 = ORIENTED_EDGE ( 'NONE', *, *, #30428, .T. ) ;
#57542 = ORIENTED_EDGE ( 'NONE', *, *, #21081, .T. ) ;
#57543 = EDGE_LOOP ( 'NONE', ( #28127, #52550, #88897, #44367, #53720, #87550, #66097, #26615 ) ) ;
#57544 = CARTESIAN_POINT ( 'NONE',  ( 112.2491357751623582, -43.66061143999345262, 185.9176141791149917 ) ) ;
#57545 = CARTESIAN_POINT ( 'NONE',  ( 106.6594718829666704, -26.29006472227095870, 85.10705384733896040 ) ) ;
#57546 = ORIENTED_EDGE ( 'NONE', *, *, #23387, .T. ) ;
#57547 = CARTESIAN_POINT ( 'NONE',  ( 99.14404768239418786, -44.40400490628097430, 41.95086337114900488 ) ) ;
#57548 = CARTESIAN_POINT ( 'NONE',  ( 108.6783733978936226, -26.40767070732865562, 185.9527681330539792 ) ) ;
#57549 = DIRECTION ( 'NONE',  ( 1.000000000000000000, 0.000000000000000000, 0.000000000000000000 ) ) ;
#57550 = DIRECTION ( 'NONE',  ( 0.000000000000000000, 0.000000000000000000, -1.000000000000000000 ) ) ;
#57551 = CARTESIAN_POINT ( 'NONE',  ( 97.57126093554219892, -31.07129084365559279, 126.9108633711489915 ) ) ;
#57552 = CARTESIAN_POINT ( 'NONE',  ( 99.04406188299498126, -42.84125767153000908, 261.8439586123985237 ) ) ;
#57553 = ORIENTED_EDGE ( 'NONE', *, *, #71436, .T. ) ;
#57554 = LINE ( 'NONE', #22612, #14805 ) ;
#57555 = ORIENTED_EDGE ( 'NONE', *, *, #78720, .F. ) ;
#57556 = CARTESIAN_POINT ( 'NONE',  ( 46.03715912545432332, -48.62818131006086020, 237.4678068554150059 ) ) ;
#57557 = FACE_OUTER_BOUND ( 'NONE', #17280, .T. ) ;
#57559 = VERTEX_POINT ( 'NONE', #78743 ) ;
#57558 = EDGE_CURVE ( 'NONE', #87995, #76720, #75895, .T. ) ;
#57560 = CIRCLE ( 'NONE', #15508, 8.636000000000004562 ) ;
#57561 = DIRECTION ( 'NONE',  ( -0.000000000000000000, 1.000000000000000000, -0.000000000000000000 ) ) ;
#57562 = CARTESIAN_POINT ( 'NONE',  ( 12.17234669811228720, 85.83081271406847179, 117.9295285458294273 ) ) ;
#57563 = CARTESIAN_POINT ( 'NONE',  ( 117.4476241407275978, -37.68806341539836069, 78.75276813305399060 ) ) ;
#57564 = CARTESIAN_POINT ( 'NONE',  ( -98.60478223830740774, 120.6499999999999915, -1.074461880482445986E-12 ) ) ;
#57565 = ADVANCED_FACE ( 'NONE', ( #58699 ), #59585, .F. ) ;
#57566 = CARTESIAN_POINT ( 'NONE',  ( -47.02966122971771767, 65.60000000000000853, -44.00307561052230199 ) ) ;
#57567 = LINE ( 'NONE', #22625, #4950 ) ;
#57568 = EDGE_CURVE ( 'NONE', #74209, #60920, #25084, .T. ) ;
#57569 = CARTESIAN_POINT ( 'NONE',  ( 99.56037394151441333, -43.88466257697688633, 36.92038718067297509 ) ) ;
#57571 = CARTESIAN_POINT ( 'NONE',  ( 117.6568287320715882, -39.81301747186223139, 134.5889586092439743 ) ) ;
#57570 = DIRECTION ( 'NONE',  ( 0.000000000000000000, 1.000000000000000000, 0.000000000000000000 ) ) ;
#57572 = CARTESIAN_POINT ( 'NONE',  ( 71.06648329127399677, -18.82844715994099971, -5.074374724088000832 ) ) ;
#57573 = LINE ( 'NONE', #71672, #61206 ) ;
#57574 = VERTEX_POINT ( 'NONE', #11003 ) ;
#57575 = DIRECTION ( 'NONE',  ( -1.000000000000000000, -4.299999999999999979E-14, 1.230419385187874527E-43 ) ) ;
#57576 = ADVANCED_FACE ( 'NONE', ( #80512 ), #65531, .T. ) ;
#57577 = FACE_OUTER_BOUND ( 'NONE', #28572, .T. ) ;
#57578 = ORIENTED_EDGE ( 'NONE', *, *, #13625, .T. ) ;
#57579 = EDGE_CURVE ( 'NONE', #16547, #78479, #37385, .T. ) ;
#57580 = CARTESIAN_POINT ( 'NONE',  ( 164.9212702847350158, -29.73316016639540749, 342.9256252759119548 ) ) ;
#57582 = ORIENTED_EDGE ( 'NONE', *, *, #51955, .T. ) ;
#57581 = CARTESIAN_POINT ( 'NONE',  ( 117.4565820116822010, -35.18101482210430930, 218.9441967044829482 ) ) ;
#57583 = AXIS2_PLACEMENT_3D ( 'NONE', #30237, #16606, #22535 ) ;
#57584 = CYLINDRICAL_SURFACE ( 'NONE', #10315, 2.750000000000002665 ) ;
#57585 = CARTESIAN_POINT ( 'NONE',  ( 104.8366293861751330, -26.48703790372925937, 256.2470538473397710 ) ) ;
#57586 = CARTESIAN_POINT ( 'NONE',  ( 113.8847749867171046, -44.67324210339663182, 104.1413395616249744 ) ) ;
#57587 = CARTESIAN_POINT ( 'NONE',  ( 84.90151352399593065, 74.80151635532864418, 99.18073718829431584 ) ) ;
#57588 = DIRECTION ( 'NONE',  ( 0.000000000000000000, 1.000000000000000000, 0.000000000000000000 ) ) ;
#57589 = DIRECTION ( 'NONE',  ( 1.000000000000000000, 0.000000000000000000, 0.000000000000000000 ) ) ;
#57590 = ORIENTED_EDGE ( 'NONE', *, *, #23176, .F. ) ;
#57591 = ADVANCED_FACE ( 'NONE', ( #3754 ), #3314, .T. ) ;
#57592 = AXIS2_PLACEMENT_3D ( 'NONE', #56913, #84649, #84204 ) ;
#57593 = VECTOR ( 'NONE', #66797, 1000.000000000000000 ) ;
#57594 = VECTOR ( 'NONE', #31260, 1000.000000000000000 ) ;
#57595 = ORIENTED_EDGE ( 'NONE', *, *, #7364, .T. ) ;
#57596 = ADVANCED_FACE ( 'NONE', ( #57822 ), #10775, .T. ) ;
#57597 = EDGE_LOOP ( 'NONE', ( #41703, #59990, #46248, #88495, #75448 ) ) ;
#57598 = ORIENTED_EDGE ( 'NONE', *, *, #57568, .F. ) ;
#57599 = DIRECTION ( 'NONE',  ( -0.000000000000000000, 1.000000000000000000, 0.000000000000000000 ) ) ;
#57600 = CARTESIAN_POINT ( 'NONE',  ( 116.1393041698827346, -43.00708073170991952, 9.356577656862985037 ) ) ;
#57601 = DIRECTION ( 'NONE',  ( 1.000000000000000078E-15, -1.000000000000000000, 0.000000000000000000 ) ) ;
#57602 = LINE ( 'NONE', #16727, #39689 ) ;
#57603 = EDGE_CURVE ( 'NONE', #67926, #27744, #65883, .T. ) ;
#57604 = CIRCLE ( 'NONE', #66286, 4.874999999999990230 ) ;
#57606 = CARTESIAN_POINT ( 'NONE',  ( 81.76240029069523985, 70.17671898886891313, 85.85219768521638173 ) ) ;
#57605 = DIRECTION ( 'NONE',  ( 1.000000000000000000, 6.831565154159360295E-14, 0.000000000000000000 ) ) ;
#57607 = CARTESIAN_POINT ( 'NONE',  ( 141.8164832912740110, -9.833000550534297446, -5.074374724088994704 ) ) ;
#57608 = CIRCLE ( 'NONE', #12620, 2.749999999999974687 ) ;
#57609 = CARTESIAN_POINT ( 'NONE',  ( 104.4852212567679004, -46.88943973524933995, 47.37848241876796607 ) ) ;
#57610 = VERTEX_POINT ( 'NONE', #72358 ) ;
#57611 = EDGE_LOOP ( 'NONE', ( #32519, #60924, #73609, #75205 ) ) ;
#57612 = EDGE_LOOP ( 'NONE', ( #74399, #3569, #83477, #38328 ) ) ;
#57613 = VECTOR ( 'NONE', #81459, 1000.000000000000000 ) ;
#57614 = DIRECTION ( 'NONE',  ( 0.000000000000000000, 0.000000000000000000, -1.000000000000000000 ) ) ;
#57615 = DIRECTION ( 'NONE',  ( 0.000000000000000000, 0.000000000000000000, 1.000000000000000000 ) ) ;
#57616 = CARTESIAN_POINT ( 'NONE',  ( 115.7455327456632403, -41.23958449135837867, 284.4441967044819535 ) ) ;
#57617 = LINE ( 'NONE', #29030, #82090 ) ;
#57618 = CARTESIAN_POINT ( 'NONE',  ( 113.6473777113567820, -44.00994186338851932, 129.1613395616249704 ) ) ;
#57619 = CARTESIAN_POINT ( 'NONE',  ( 115.0365192675815820, -42.90939908788407564, 28.30219775253060632 ) ) ;
#57620 = ORIENTED_EDGE ( 'NONE', *, *, #24160, .F. ) ;
#57621 = CARTESIAN_POINT ( 'NONE',  ( 168.0371591254543944, -48.62818131005519717, 249.9678068554149775 ) ) ;
#57622 = CARTESIAN_POINT ( 'NONE',  ( 77.85922577376808817, -35.08568546290069179, 2.471387922371498735 ) ) ;
#57623 = VERTEX_POINT ( 'NONE', #24640 ) ;
#57624 = EDGE_CURVE ( 'NONE', #10976, #16372, #61537, .T. ) ;
#57625 = CARTESIAN_POINT ( 'NONE',  ( -74.36911441044730964, 82.54999999999999716, 92.32962665258534685 ) ) ;
#57626 = CARTESIAN_POINT ( 'NONE',  ( 101.8980524138101345, -43.06915566006364315, 9.850947512448971821 ) ) ;
#57627 = CONICAL_SURFACE ( 'NONE', #18456, 1.258750000000002922, 1.029744258676650093 ) ;
#57628 = CARTESIAN_POINT ( 'NONE',  ( 168.5667039024483529, -48.82844715993517326, 300.4678068554149490 ) ) ;
#57629 = LINE ( 'NONE', #66220, #59210 ) ;
#57630 = DIRECTION ( 'NONE',  ( 0.000000000000000000, 0.000000000000000000, -1.000000000000000000 ) ) ;
#57631 = ORIENTED_EDGE ( 'NONE', *, *, #86324, .T. ) ;
#57632 = CARTESIAN_POINT ( 'NONE',  ( 45.56670390244626390, -48.82844715994099971, 180.4678068554150911 ) ) ;
#57633 = PLANE ( 'NONE',  #22337 ) ;
#57634 = VERTEX_POINT ( 'NONE', #73225 ) ;
#57635 = CARTESIAN_POINT ( 'NONE',  ( 117.9889986865933196, -38.42583888725547325, 68.69181575210198787 ) ) ;
#57636 = ORIENTED_EDGE ( 'NONE', *, *, #5959, .F. ) ;
#57637 = CARTESIAN_POINT ( 'NONE',  ( 111.7785660440950011, -28.99582275371927764, 49.05146744712496343 ) ) ;
#57638 = CARTESIAN_POINT ( 'NONE',  ( 113.1984054845878092, -44.65944206278228279, 89.09955263830856609 ) ) ;
#57639 = CARTESIAN_POINT ( 'NONE',  ( 103.2204921605863888, -27.09891563476508836, 175.3908633711489813 ) ) ;
#57640 = EDGE_CURVE ( 'NONE', #45127, #28392, #66412, .T. ) ;
#57641 = DIRECTION ( 'NONE',  ( 1.000000000000000000, 0.000000000000000000, -0.000000000000000000 ) ) ;
#57642 = DIRECTION ( 'NONE',  ( 0.7071067811864661934, 0.7071067811866289521, 7.071067811864654918E-16 ) ) ;
#57643 = AXIS2_PLACEMENT_3D ( 'NONE', #81607, #60669, #87950 ) ;
#57644 = CARTESIAN_POINT ( 'NONE',  ( 131.5667039024470455, -104.2784471599409244, 24.21780685541800082 ) ) ;
#57645 = CARTESIAN_POINT ( 'NONE',  ( 100.1098231460999841, -44.55235322945014076, 262.9984824187678782 ) ) ;
#57646 = PLANE ( 'NONE',  #81539 ) ;
#57647 = VERTEX_POINT ( 'NONE', #44178 ) ;
#57648 = EDGE_CURVE ( 'NONE', #76973, #82153, #26785, .T. ) ;
#57649 = CARTESIAN_POINT ( 'NONE',  ( -48.02966122971777452, 65.60000000000000853, 106.4272185163641780 ) ) ;
#57650 = VERTEX_POINT ( 'NONE', #23335 ) ;
#57651 = CARTESIAN_POINT ( 'NONE',  ( 114.2698949211017663, -45.17901133753223064, 149.1508633711489722 ) ) ;
#57652 = CIRCLE ( 'NONE', #35868, 6.858000000000003205 ) ;
#57653 = CARTESIAN_POINT ( 'NONE',  ( 125.2667151975434479, 50.60771645571414723, -36.78494105014318194 ) ) ;
#57654 = AXIS2_PLACEMENT_3D ( 'NONE', #87920, #45656, #73387 ) ;
#57655 = ORIENTED_EDGE ( 'NONE', *, *, #41669, .F. ) ;
#57656 = ORIENTED_EDGE ( 'NONE', *, *, #84779, .T. ) ;
#57657 = ORIENTED_EDGE ( 'NONE', *, *, #14107, .F. ) ;
#57658 = B_SPLINE_CURVE_WITH_KNOTS ( 'NONE', 3,
 ( #76979, #19882, #43780, #57414, #16102, #75296, #14762, #78339, #29720, #658, #85150, #56513, #64243, #15651, #8388, #43331, #36544, #15196, #71517, #71072, #70155, #2017, #7927, #22918, #26682, #9276, #61204, #88927, #8845 ),
 .UNSPECIFIED., .F., .F.,
 ( 4, 2, 2, 2, 2, 2, 2, 2, 2, 2, 1, 1, 1, 1, 1, 2, 4 ),
 ( 0.000000000000000000, 0.06250188046431207067, 0.1250037609286241413, 0.1875056413929362398, 0.2500075218572482827, 0.3125094023215603256, 0.3750112827858724796, 0.4375131632501845225, 0.4687641034823402664, 0.4843895735984181661, 0.4922023086564571992, 0.4961086761854766602, 0.4980618599499865295, 0.4990384518322412699, 0.4995267477733687511, 0.4997708957439324085, 0.5000150437144960103 ),
 .UNSPECIFIED. ) ;
#57659 = CARTESIAN_POINT ( 'NONE',  ( 142.8821648370248170, -72.54478064608022692, 540.9756252759101471 ) ) ;
#57660 = FACE_OUTER_BOUND ( 'NONE', #26471, .T. ) ;
#57661 = CARTESIAN_POINT ( 'NONE',  ( 110.2867295656602664, -27.49400189596543242, 209.8099109901969541 ) ) ;
#57662 = DIRECTION ( 'NONE',  ( 0.000000000000000000, 0.000000000000000000, -1.000000000000000000 ) ) ;
#57663 = CARTESIAN_POINT ( 'NONE',  ( 80.06648329127399677, -8.350947159940998787, 2.408125275911999097 ) ) ;
#57664 = DIRECTION ( 'NONE',  ( 1.000000000000000000, 1.261617073437676668E-15, 9.462128050782575008E-16 ) ) ;
#57665 = CARTESIAN_POINT ( 'NONE',  ( 101.3842069476886394, -27.98906827703155642, 21.53562527591096298 ) ) ;
#57666 = CARTESIAN_POINT ( 'NONE',  ( 34.33598329127384829, -36.32844715994141893, 193.9678068554150911 ) ) ;
#57667 = VERTEX_POINT ( 'NONE', #51001 ) ;
#57668 = AXIS2_PLACEMENT_3D ( 'NONE', #3063, #11667, #24842 ) ;
#57669 = SURFACE_SIDE_STYLE ('',( #64499 ) ) ;
#57670 = CIRCLE ( 'NONE', #59145, 2.030000000002079918 ) ;
#57671 = AXIS2_PLACEMENT_3D ( 'NONE', #76221, #12661, #33541 ) ;
#57672 = DIRECTION ( 'NONE',  ( 0.000000000000000000, 0.000000000000000000, 1.000000000000000000 ) ) ;
#57673 = EDGE_LOOP ( 'NONE', ( #13187, #63200 ) ) ;
#57674 = VECTOR ( 'NONE', #19416, 1000.000000000000000 ) ;
#57675 = CARTESIAN_POINT ( 'NONE',  ( 130.3998166246059895, 12.92155284005730387, 355.9756252759109998 ) ) ;
#57676 = DIRECTION ( 'NONE',  ( -1.000000000000000000, 0.000000000000000000, -0.000000000000000000 ) ) ;
#57677 = CARTESIAN_POINT ( 'NONE',  ( 103.6457867198658107, -26.24313906103844474, 210.3394347997209763 ) ) ;
#57678 = DIRECTION ( 'NONE',  ( -1.000000000000000000, 1.011922027653136551E-15, 0.000000000000000000 ) ) ;
#57679 = EDGE_CURVE ( 'NONE', #47547, #79573, #16498, .T. ) ;
#57680 = DIRECTION ( 'NONE',  ( 0.000000000000000000, 1.000000000000000000, 0.000000000000000000 ) ) ;
#57681 = DIRECTION ( 'NONE',  ( 0.000000000000000000, 1.000000000000000000, 0.000000000000000000 ) ) ;
#57682 = EDGE_CURVE ( 'NONE', #73752, #29169, #58677, .T. ) ;
#57683 = CARTESIAN_POINT ( 'NONE',  ( 112.0098809771561577, -44.31729861111978153, 222.4705150661719983 ) ) ;
#57685 = CARTESIAN_POINT ( 'NONE',  ( 110.4495079430909357, -47.22796928374258130, 53.83657765686300678 ) ) ;
#57684 = FACE_OUTER_BOUND ( 'NONE', #69849, .T. ) ;
#57686 = CARTESIAN_POINT ( 'NONE',  ( 125.4480236541915019, 68.52740834580446005, 36.16247866844641123 ) ) ;
#57687 = CARTESIAN_POINT ( 'NONE',  ( 101.6881215347969345, -27.70586588967184483, 85.50419670448295051 ) ) ;
#57688 = EDGE_LOOP ( 'NONE', ( #59624, #72425 ) ) ;
#57689 = CARTESIAN_POINT ( 'NONE',  ( 131.4905132191145753, -19.69637952316714546, 6.988870342668328739 ) ) ;
#57690 = ORIENTED_EDGE ( 'NONE', *, *, #51752, .F. ) ;
#57691 = EDGE_CURVE ( 'NONE', #54341, #64435, #77570, .T. ) ;
#57692 = CARTESIAN_POINT ( 'NONE',  ( 0.000000000000000000, 111.1250000000000000, 42.54500000000000171 ) ) ;
#57693 = CARTESIAN_POINT ( 'NONE',  ( 97.07170145856559884, -35.38119765756442092, 277.2191086048737247 ) ) ;
#57694 = VERTEX_POINT ( 'NONE', #67767 ) ;
#57695 = DIRECTION ( 'NONE',  ( -1.000000000000000000, 0.000000000000000000, 0.000000000000000000 ) ) ;
#57696 = EDGE_CURVE ( 'NONE', #53395, #38195, #67307, .T. ) ;
#57697 = ORIENTED_EDGE ( 'NONE', *, *, #26734, .T. ) ;
#57698 = CARTESIAN_POINT ( 'NONE',  ( 46.03715912545349909, -48.62818131006090283, 117.4678068554150485 ) ) ;
#57699 = PLANE ( 'NONE',  #51918 ) ;
#57700 = AXIS2_PLACEMENT_3D ( 'NONE', #83464, #68936, #14436 ) ;
#57701 = CARTESIAN_POINT ( 'NONE',  ( 184.5664832912740110, 15.62155284005900491, 328.6381252759109088 ) ) ;
#57702 = ORIENTED_EDGE ( 'NONE', *, *, #51808, .T. ) ;
#57703 = CARTESIAN_POINT ( 'NONE',  ( 113.4288541212755348, -27.66216098611360152, 84.57753003781698453 ) ) ;
#57704 = DIRECTION ( 'NONE',  ( 1.000000000000000000, 0.000000000000000000, 0.000000000000000000 ) ) ;
#57705 = LINE ( 'NONE', #79513, #47765 ) ;
#57706 = DIRECTION ( 'NONE',  ( -0.7071067811865614505, -0.7071067811865336949, 0.000000000000000000 ) ) ;
#57707 = DIRECTION ( 'NONE',  ( 1.907762142705490052E-15, 7.167082501179359715E-16, -1.000000000000000000 ) ) ;
#57708 = ORIENTED_EDGE ( 'NONE', *, *, #26106, .F. ) ;
#57709 = EDGE_CURVE ( 'NONE', #87604, #86462, #41234, .T. ) ;
#57710 = CARTESIAN_POINT ( 'NONE',  ( 107.8226678445051192, -26.73166616839828791, 121.0146427918937206 ) ) ;
#57711 = CARTESIAN_POINT ( 'NONE',  ( 163.0664832912739826, 22.62155284005901024, 333.4006252759110112 ) ) ;
#57712 = DIRECTION ( 'NONE',  ( -1.000000000000000000, 0.000000000000000000, 0.000000000000000000 ) ) ;
#57713 = AXIS2_PLACEMENT_3D ( 'NONE', #22737, #15016, #84968 ) ;
#57715 = LINE ( 'NONE', #23233, #8008 ) ;
#57714 = PLANE ( 'NONE',  #61003 ) ;
#57716 = DIRECTION ( 'NONE',  ( 0.000000000000000000, 1.000000000000000000, 0.000000000000000000 ) ) ;
#57717 = VECTOR ( 'NONE', #45297, 1000.000000000000000 ) ;
#57718 = ORIENTED_EDGE ( 'NONE', *, *, #29878, .T. ) ;
#57719 = CIRCLE ( 'NONE', #14216, 3.299999999999997158 ) ;
#57720 = CARTESIAN_POINT ( 'NONE',  ( 152.5667039024471592, -23.42844715993585325, 180.4678068554149775 ) ) ;
#57721 = CARTESIAN_POINT ( 'NONE',  ( 108.2029444874845723, -47.03713394308625340, 153.6518157521009584 ) ) ;
#57723 = ORIENTED_EDGE ( 'NONE', *, *, #41069, .F. ) ;
#57722 = DIRECTION ( 'NONE',  ( 0.000000000000000000, 1.000000000000000000, 0.000000000000000000 ) ) ;
#57724 = VECTOR ( 'NONE', #20335, 1000.000000000000000 ) ;
#57725 = CARTESIAN_POINT ( 'NONE',  ( 97.00695478131298444, -39.24785563725447446, 12.53372051400597442 ) ) ;
#57726 = CARTESIAN_POINT ( 'NONE',  ( 49.35211078756498893, -35.65087443492551245, -5.074374724088000832 ) ) ;
#57727 = CARTESIAN_POINT ( 'NONE',  ( 97.81847533801933992, -40.53397008005389779, 51.63704823906684993 ) ) ;
#57728 = CARTESIAN_POINT ( 'NONE',  ( 113.1760415728007558, -44.75355146995899247, 13.09421906058726748 ) ) ;
#57729 = CIRCLE ( 'NONE', #66404, 82.41591158490096802 ) ;
#57730 = CARTESIAN_POINT ( 'NONE',  ( 73.06670390244801183, -58.72944715994110254, 250.9178068554160461 ) ) ;
#57731 = CIRCLE ( 'NONE', #11302, 17.00000000000000000 ) ;
#57733 = CARTESIAN_POINT ( 'NONE',  ( 114.9410966442422648, -29.98191058901448969, 229.4022919425779605 ) ) ;
#57732 = AXIS2_PLACEMENT_3D ( 'NONE', #69541, #26847, #7317 ) ;
#57734 = ORIENTED_EDGE ( 'NONE', *, *, #64673, .F. ) ;
#57735 = ORIENTED_EDGE ( 'NONE', *, *, #8156, .T. ) ;
#57736 = ADVANCED_FACE ( 'NONE', ( #25987 ), #54999, .T. ) ;
#57737 = CARTESIAN_POINT ( 'NONE',  ( 99.58187507909633496, -41.47380365182278439, 183.2072975916109385 ) ) ;
#57738 = CIRCLE ( 'NONE', #18568, 2.517500000000000071 ) ;
#57739 = PLANE ( 'NONE',  #74846 ) ;
#57740 = CARTESIAN_POINT ( 'NONE',  ( 98.80858115845356338, -33.43260291865056644, 37.45586902018299469 ) ) ;
#57741 = CARTESIAN_POINT ( 'NONE',  ( 23.08500427215554751, 87.15872157593996405, 304.1353934756002104 ) ) ;
#57742 = EDGE_CURVE ( 'NONE', #23552, #51283, #20965, .T. ) ;
#57743 = LINE ( 'NONE', #31369, #77987 ) ;
#57744 = AXIS2_PLACEMENT_3D ( 'NONE', #17344, #87718, #52707 ) ;
#57745 = DIRECTION ( 'NONE',  ( 0.7071067811865417996, 0.7071067811865532349, 0.000000000000000000 ) ) ;
#57746 = EDGE_LOOP ( 'NONE', ( #32227, #67692 ) ) ;
#57747 = FACE_OUTER_BOUND ( 'NONE', #49063, .T. ) ;
#57748 = LINE ( 'NONE', #50930, #80750 ) ;
#57749 = CARTESIAN_POINT ( 'NONE',  ( 118.0799254396265923, -36.12288750354066735, 273.8822919425776945 ) ) ;
#57750 = CARTESIAN_POINT ( 'NONE',  ( 176.7669697523288335, -48.62818131005461453, 180.4678068554150059 ) ) ;
#57751 = VERTEX_POINT ( 'NONE', #5557 ) ;
#57752 = ORIENTED_EDGE ( 'NONE', *, *, #11007, .T. ) ;
#57753 = PLANE ( 'NONE',  #66258 ) ;
#57754 = DIRECTION ( 'NONE',  ( 0.000000000000000000, 0.000000000000000000, 1.000000000000000000 ) ) ;
#57755 = DIRECTION ( 'NONE',  ( 0.000000000000000000, 1.000000000000000000, 0.000000000000000000 ) ) ;
#57756 = FACE_BOUND ( 'NONE', #82433, .T. ) ;
#57757 = AXIS2_PLACEMENT_3D ( 'NONE', #70962, #8735, #79563 ) ;
#57758 = VECTOR ( 'NONE', #43414, 1000.000000000000000 ) ;
#57759 = CARTESIAN_POINT ( 'NONE',  ( 116.1300133678978170, -31.69047823903422412, 25.24229194257693365 ) ) ;
#57760 = CARTESIAN_POINT ( 'NONE',  ( 12.27784944810749401, 79.68881837611452568, 117.7174742578267370 ) ) ;
#57761 = ORIENTED_EDGE ( 'NONE', *, *, #28481, .F. ) ;
#57762 = ADVANCED_FACE ( 'NONE', ( #12822 ), #60033, .F. ) ;
#57763 = CARTESIAN_POINT ( 'NONE',  ( 99.95113126132085313, -44.40829767532816419, 42.98133956162492098 ) ) ;
#57764 = LINE ( 'NONE', #72741, #52589 ) ;
#57765 = CARTESIAN_POINT ( 'NONE',  ( 101.0865414634836696, -45.26919196907830667, 282.0899109901967563 ) ) ;
#57766 = ORIENTED_EDGE ( 'NONE', *, *, #46305, .F. ) ;
#57767 = CARTESIAN_POINT ( 'NONE',  ( 82.60038231476900705, -17.66080131299329281, 2.811527311783403427 ) ) ;
#57768 = LINE ( 'NONE', #30517, #51483 ) ;
#57769 = CARTESIAN_POINT ( 'NONE',  ( 117.0667039024470455, -109.9573555057410630, 19.21780685541815714 ) ) ;
#57770 = CARTESIAN_POINT ( 'NONE',  ( 98.47016933319702048, -37.73160053143655546, 84.24904275054394986 ) ) ;
#57771 = CARTESIAN_POINT ( 'NONE',  ( 97.07541381888600540, -41.51105113164680915, 212.6937205140059461 ) ) ;
#57772 = FACE_OUTER_BOUND ( 'NONE', #17938, .T. ) ;
#57773 = ORIENTED_EDGE ( 'NONE', *, *, #53371, .F. ) ;
#57774 = DIRECTION ( 'NONE',  ( -1.000000000000000000, 0.000000000000000000, 0.000000000000000000 ) ) ;
#57775 = VERTEX_POINT ( 'NONE', #33248 ) ;
#57776 = ORIENTED_EDGE ( 'NONE', *, *, #31318, .F. ) ;
#57777 = AXIS2_PLACEMENT_3D ( 'NONE', #81204, #55560, #39829 ) ;
#57778 = TOROIDAL_SURFACE ( 'NONE', #18620, 15.69999999999999929, 0.2999999999999999889 ) ;
#57779 = FACE_BOUND ( 'NONE', #63823, .T. ) ;
#57780 = EDGE_LOOP ( 'NONE', ( #75432, #16824, #81645, #28387 ) ) ;
#57781 = ORIENTED_EDGE ( 'NONE', *, *, #34638, .F. ) ;
#57782 = CARTESIAN_POINT ( 'NONE',  ( 130.3998166246059895, 12.92155284005730387, 355.9756252759109998 ) ) ;
#57783 = CARTESIAN_POINT ( 'NONE',  ( 97.53181966783076007, -39.74887802330798792, 42.57051035864261479 ) ) ;
#57784 = EDGE_CURVE ( 'NONE', #35999, #88384, #82767, .T. ) ;
#57785 = CARTESIAN_POINT ( 'NONE',  ( 108.7098619460078481, -45.63517435782368636, 127.1562293518869780 ) ) ;
#57786 = CARTESIAN_POINT ( 'NONE',  ( 114.4306803301698778, -27.41265490572180141, 274.5441967044824878 ) ) ;
#57787 = VECTOR ( 'NONE', #2358, 1000.000000000000114 ) ;
#57788 = EDGE_CURVE ( 'NONE', #58668, #64292, #81861, .T. ) ;
#57789 = CARTESIAN_POINT ( 'NONE',  ( -7.736432051520609754, 72.46968852267782779, 130.3269799747974957 ) ) ;
#57790 = EDGE_CURVE ( 'NONE', #67149, #70138, #32793, .T. ) ;
#57791 = ORIENTED_EDGE ( 'NONE', *, *, #60031, .T. ) ;
#57792 = AXIS2_PLACEMENT_3D ( 'NONE', #55135, #6139, #68803 ) ;
#57793 = EDGE_CURVE ( 'NONE', #73698, #15487, #34131, .T. ) ;
#57794 = ORIENTED_EDGE ( 'NONE', *, *, #65981, .T. ) ;
#57795 = DIRECTION ( 'NONE',  ( 0.000000000000000000, 0.000000000000000000, 1.000000000000000000 ) ) ;
#57796 = VECTOR ( 'NONE', #57695, 1000.000000000000000 ) ;
#57797 = CARTESIAN_POINT ( 'NONE',  ( 113.1770345814885701, -44.75280961174332361, 33.09405132221606749 ) ) ;
#57798 = CARTESIAN_POINT ( 'NONE',  ( 97.83900096657649215, -40.58357506337067377, 131.6413213018817601 ) ) ;
#57799 = CARTESIAN_POINT ( 'NONE',  ( 179.7974245136200011, -36.32844715994040996, -5.074374724088000832 ) ) ;
#57800 = ORIENTED_EDGE ( 'NONE', *, *, #28258, .T. ) ;
#57801 = CARTESIAN_POINT ( 'NONE',  ( 97.22365000156210613, -40.27127430222545001, 266.6013395616254797 ) ) ;
#57802 = CARTESIAN_POINT ( 'NONE',  ( 117.5558648759066926, -37.28717672647940873, 14.78419670448294454 ) ) ;
#57803 =( NAMED_UNIT ( * ) SI_UNIT ( $, .STERADIAN. ) SOLID_ANGLE_UNIT ( ) );
#57804 = CARTESIAN_POINT ( 'NONE',  ( 117.0718954854907139, -35.46248235721044750, 119.9272919425023787 ) ) ;
#57806 = DIRECTION ( 'NONE',  ( 0.000000000000000000, 0.000000000000000000, 1.000000000000000000 ) ) ;
#57805 = LINE ( 'NONE', #10992, #89831 ) ;
#57807 = CYLINDRICAL_SURFACE ( 'NONE', #58308, 5.599999999999994316 ) ;
#57808 = LINE ( 'NONE', #85544, #78811 ) ;
#57809 = LINE ( 'NONE', #44165, #73063 ) ;
#57810 = EDGE_CURVE ( 'NONE', #43486, #16565, #75032, .T. ) ;
#57811 = CIRCLE ( 'NONE', #2714, 38.10000000000000142 ) ;
#57812 = EDGE_CURVE ( 'NONE', #63160, #85945, #68225, .T. ) ;
#57813 = DIRECTION ( 'NONE',  ( -1.000000000000000078E-15, 1.000000000000000083E-30, 1.000000000000000000 ) ) ;
#57814 = FACE_BOUND ( 'NONE', #76671, .T. ) ;
#57815 = LINE ( 'NONE', #65525, #76226 ) ;
#57816 = DIRECTION ( 'NONE',  ( -0.8571673007021084478, -0.5150380749100604838, -8.571673007021083688E-16 ) ) ;
#57817 = CARTESIAN_POINT ( 'NONE',  ( 100.4373464023292826, -44.86011580501824625, 12.03276813305398463 ) ) ;
#57818 = CARTESIAN_POINT ( 'NONE',  ( 99.28859025714638165, -29.78777103691475858, 186.7470538473389752 ) ) ;
#57819 = CARTESIAN_POINT ( 'NONE',  ( 117.4061096064183971, -38.22256018827695101, 24.71276813305395237 ) ) ;
#57820 = AXIS2_PLACEMENT_3D ( 'NONE', #19099, #67244, #5483 ) ;
#57822 = FACE_OUTER_BOUND ( 'NONE', #31619, .T. ) ;
#57821 = CARTESIAN_POINT ( 'NONE',  ( -160.2664750769284865, 20.32000000000000028, 148.0533267522753818 ) ) ;
#57823 = DIRECTION ( 'NONE',  ( 1.000000000000000078E-15, 1.000000000000000083E-30, -1.000000000000000000 ) ) ;
#57824 = AXIS2_PLACEMENT_3D ( 'NONE', #81225, #6245, #18972 ) ;
#57825 = ORIENTED_EDGE ( 'NONE', *, *, #46582, .T. ) ;
#57826 = PLANE ( 'NONE',  #34563 ) ;
#57827 = ORIENTED_EDGE ( 'NONE', *, *, #83865, .T. ) ;
#57828 = CARTESIAN_POINT ( 'NONE',  ( 117.2535196871929770, -41.18324016912737306, 54.49848241876692612 ) ) ;
#57830 = VERTEX_POINT ( 'NONE', #88234 ) ;
#57829 = CARTESIAN_POINT ( 'NONE',  ( -72.96458098368600531, 117.4749999999999943, -65.02708098368781009 ) ) ;
#57831 = CARTESIAN_POINT ( 'NONE',  ( 33.78129701732998313, -35.65087443492610930, 237.4678068554150059 ) ) ;
#57832 = CARTESIAN_POINT ( 'NONE',  ( 115.0229693000240303, -29.09019634776603169, 185.4232443235299570 ) ) ;
#57833 = CARTESIAN_POINT ( 'NONE',  ( 71.09939861440099662, 0.000000000000000000, 177.8662485265279827 ) ) ;
#57834 = CYLINDRICAL_SURFACE ( 'NONE', #83507, 18.00000000000000000 ) ;
#57835 = CARTESIAN_POINT ( 'NONE',  ( 97.81219835445369881, -40.51719899421586746, 151.6362400511890769 ) ) ;
#57836 = CARTESIAN_POINT ( 'NONE',  ( 97.31584372111100834, -39.30597601896262461, 47.53145861081645762 ) ) ;
#57837 = VECTOR ( 'NONE', #51091, 1000.000000000000000 ) ;
#57838 = PLANE ( 'NONE',  #1299 ) ;
#57839 = CARTESIAN_POINT ( 'NONE',  ( 110.8526248007088952, -45.98499320073891994, 97.88546641285240923 ) ) ;
#57840 = CARTESIAN_POINT ( 'NONE',  ( 102.8912152862169762, -46.22186109533351583, 132.2346728949589760 ) ) ;
#57841 = ORIENTED_EDGE ( 'NONE', *, *, #12479, .F. ) ;
#57842 = ORIENTED_EDGE ( 'NONE', *, *, #1624, .T. ) ;
#57843 = EDGE_CURVE ( 'NONE', #71161, #78791, #87682, .T. ) ;
#57844 = VECTOR ( 'NONE', #78196, 999.9999999999998863 ) ;
#57845 = CARTESIAN_POINT ( 'NONE',  ( 104.6418561626188364, -26.95233673609813962, 86.70158330589694629 ) ) ;
#57846 = VECTOR ( 'NONE', #58206, 1000.000000000000000 ) ;
#57847 = DIRECTION ( 'NONE',  ( 0.000000000000000000, 0.000000000000000000, -1.000000000000000000 ) ) ;
#57849 = FACE_OUTER_BOUND ( 'NONE', #84714, .T. ) ;
#57848 = CARTESIAN_POINT ( 'NONE',  ( 96.80143343076643703, -35.25719154489702589, 222.2251490854339693 ) ) ;
#57850 = DIRECTION ( 'NONE',  ( 0.000000000000000000, 0.000000000000000000, -1.000000000000000000 ) ) ;
#57852 = EDGE_CURVE ( 'NONE', #82260, #73068, #68669, .T. ) ;
#57851 = FACE_OUTER_BOUND ( 'NONE', #1367, .T. ) ;
#57853 = DIRECTION ( 'NONE',  ( -1.000000000000000078E-15, 1.000000000000000083E-30, 1.000000000000000000 ) ) ;
#57854 = AXIS2_PLACEMENT_3D ( 'NONE', #61106, #6597, #27928 ) ;
#57855 = DIRECTION ( 'NONE',  ( 1.000000000000000078E-15, -1.000000000000000083E-30, -1.000000000000000000 ) ) ;
#57856 = DIRECTION ( 'NONE',  ( 0.000000000000000000, 0.000000000000000000, -1.000000000000000000 ) ) ;
#57857 = CARTESIAN_POINT ( 'NONE',  ( 102.9221092647373865, -27.14930527916904168, 155.4013395616249795 ) ) ;
#57858 = ORIENTED_EDGE ( 'NONE', *, *, #80368, .T. ) ;
#57859 = ORIENTED_EDGE ( 'NONE', *, *, #19630, .F. ) ;
#57860 = EDGE_LOOP ( 'NONE', ( #44919, #29731, #43022, #6804 ) ) ;
#57861 = AXIS2_PLACEMENT_3D ( 'NONE', #10375, #4457, #45754 ) ;
#57862 = CARTESIAN_POINT ( 'NONE',  ( 92.74792143564410196, -71.69957577635202028, 248.4067532124560103 ) ) ;
#57863 = CARTESIAN_POINT ( 'NONE',  ( 51.42025729304100423, -33.70561438051981185, -5.074374724088000832 ) ) ;
#57864 = AXIS2_PLACEMENT_3D ( 'NONE', #31211, #3080, #79842 ) ;
#57865 = LINE ( 'NONE', #64686, #2987 ) ;
#57866 = CARTESIAN_POINT ( 'NONE',  ( 127.0239848601435995, 53.97500000000000142, 30.16249999999999787 ) ) ;
#57867 = CARTESIAN_POINT ( 'NONE',  ( 100.8178804068425904, -31.43438811971037339, 213.5852332267339762 ) ) ;
#57868 = ADVANCED_FACE ( 'NONE', ( #20078 ), #47752, .F. ) ;
#57869 = DIRECTION ( 'NONE',  ( 1.000000000000000000, 0.000000000000000000, 0.000000000000000000 ) ) ;
#57870 = CARTESIAN_POINT ( 'NONE',  ( 106.4836019150615840, -24.89303152268002606, 195.1156252759109861 ) ) ;
#57871 = PLANE ( 'NONE',  #27181 ) ;
#57872 = ORIENTED_EDGE ( 'NONE', *, *, #15452, .T. ) ;
#57874 = VERTEX_POINT ( 'NONE', #27326 ) ;
#57873 = ORIENTED_EDGE ( 'NONE', *, *, #7221, .T. ) ;
#57875 = AXIS2_PLACEMENT_3D ( 'NONE', #63155, #48162, #937 ) ;
#57876 = DIRECTION ( 'NONE',  ( 1.000000000000000000, 0.000000000000000000, 0.000000000000000000 ) ) ;
#57877 = ORIENTED_EDGE ( 'NONE', *, *, #74021, .T. ) ;
#57878 = ORIENTED_EDGE ( 'NONE', *, *, #2329, .F. ) ;
#57879 = CARTESIAN_POINT ( 'NONE',  ( 120.0664832912739399, -36.72944715994095333, 294.6356252759106837 ) ) ;
#57880 = CARTESIAN_POINT ( 'NONE',  ( 133.1862368104903567, -34.12360705087674262, 8.106403045240790917 ) ) ;
#57881 = CARTESIAN_POINT ( 'NONE',  ( 100.5471494818408189, -29.96373860736636274, 262.1063452106591853 ) ) ;
#57882 = ADVANCED_FACE ( 'NONE', ( #87767 ), #9369, .T. ) ;
#57883 = CARTESIAN_POINT ( 'NONE',  ( 41.56648329127398966, -27.82844715994070484, 138.9256252759119832 ) ) ;
#57884 = ORIENTED_EDGE ( 'NONE', *, *, #7154, .T. ) ;
#57885 = CARTESIAN_POINT ( 'NONE',  ( 116.0151837961063563, -39.81228804796826637, 9.635625275910943088 ) ) ;
#57886 = CONICAL_SURFACE ( 'NONE', #69500, 16.33514202138210791, 0.7853981633974552734 ) ;
#57887 = CARTESIAN_POINT ( 'NONE',  ( -126.9019698816670711, 58.54574603448291725, 30.67188900999152423 ) ) ;
#57888 = ORIENTED_EDGE ( 'NONE', *, *, #49317, .T. ) ;
#57889 = ORIENTED_EDGE ( 'NONE', *, *, #51644, .F. ) ;
#57890 = CARTESIAN_POINT ( 'NONE',  ( 110.8556403160020238, -45.98375910300359948, 112.8857257452675071 ) ) ;
#57891 = VERTEX_POINT ( 'NONE', #18721 ) ;
#57892 = VERTEX_POINT ( 'NONE', #53657 ) ;
#57893 = CARTESIAN_POINT ( 'NONE',  ( 99.10695020771697727, -33.55172231072156563, 40.44670554236296312 ) ) ;
#57894 = CARTESIAN_POINT ( 'NONE',  ( 97.65468660891812647, -41.26425114427870255, 171.6841967044819626 ) ) ;
#57895 = CARTESIAN_POINT ( 'NONE',  ( 113.3182355088851381, -45.04474967211709924, 143.0899109901969553 ) ) ;
#57896 = CARTESIAN_POINT ( 'NONE',  ( 82.81648329127399677, -36.72944715994106701, 3.101481641215461327 ) ) ;
#57897 = CARTESIAN_POINT ( 'NONE',  ( 101.6506511131177461, -45.63737897744897509, 243.1413395616249886 ) ) ;
#57898 = CARTESIAN_POINT ( 'NONE',  ( 7.661254700127822836, 95.64746158385918307, 320.6630000000000109 ) ) ;
#57899 = EDGE_CURVE ( 'NONE', #22872, #20321, #34568, .T. ) ;
#57900 = CARTESIAN_POINT ( 'NONE',  ( -29.99999999999998224, 172.0000000000000000, 113.8826257785461280 ) ) ;
#57901 = CARTESIAN_POINT ( 'NONE',  ( 188.5667039024479834, -67.87844715994100397, 168.3428068554150059 ) ) ;
#57902 = ORIENTED_EDGE ( 'NONE', *, *, #32952, .F. ) ;
#57903 = AXIS2_PLACEMENT_3D ( 'NONE', #76599, #85225, #71585 ) ;
#57904 = EDGE_LOOP ( 'NONE', ( #46539, #700, #60942, #20362 ) ) ;
#57905 = VECTOR ( 'NONE', #52248, 1000.000000000000000 ) ;
#57906 = CARTESIAN_POINT ( 'NONE',  ( 106.4811411369643679, -24.84306116243460139, 195.1156252759109861 ) ) ;
#57907 = ORIENTED_EDGE ( 'NONE', *, *, #39725, .T. ) ;
#57908 = CARTESIAN_POINT ( 'NONE',  ( 117.3102356154742836, -34.79226824040635790, 158.9756252759109714 ) ) ;
#57909 = CARTESIAN_POINT ( 'NONE',  ( 51.06670390244676128, -33.35206098992668444, 193.9678068554150911 ) ) ;
#57910 = CARTESIAN_POINT ( 'NONE',  ( 158.0667039024470171, -79.67844715994088745, 155.2178068554179902 ) ) ;
#57911 = DIRECTION ( 'NONE',  ( -1.058811598242755461E-16, 0.5150380749100580413, -0.8571673007021100021 ) ) ;
#57914 = CARTESIAN_POINT ( 'NONE',  ( 104.8459308146384785, -26.52976224399709082, 256.2470538473397141 ) ) ;
#57913 = DIRECTION ( 'NONE',  ( 0.000000000000000000, 0.000000000000000000, -1.000000000000000000 ) ) ;
#57912 = DIRECTION ( 'NONE',  ( 1.000000000000000000, 3.999999999999999995E-14, 1.000000000000000078E-15 ) ) ;
#57915 = CARTESIAN_POINT ( 'NONE',  ( 107.0664832912739541, -22.72944715994095688, 311.6343304127839815 ) ) ;
#57916 = CARTESIAN_POINT ( 'NONE',  ( 73.06648329127399677, -8.729447159941065237, -4.824374724089063982 ) ) ;
#57917 = CARTESIAN_POINT ( 'NONE',  ( 115.0859250807855574, -30.61377459443286142, 270.3439221990611827 ) ) ;
#57918 = EDGE_CURVE ( 'NONE', #83511, #43446, #84797, .T. ) ;
#57919 = CIRCLE ( 'NONE', #56410, 3.249999999999975131 ) ;
#57920 = DIRECTION ( 'NONE',  ( -0.7071067811875586528, 0.7071067811855363816, -1.379597263674634046E-11 ) ) ;
#57921 = ADVANCED_FACE ( 'NONE', ( #69564 ), #29129, .T. ) ;
#57922 = CARTESIAN_POINT ( 'NONE',  ( 144.0667039024470739, -140.6784471599409017, 228.4678068554179902 ) ) ;
#57923 = DIRECTION ( 'NONE',  ( 1.000000000000000078E-15, -1.000000000000000083E-30, -1.000000000000000000 ) ) ;
#57925 = ORIENTED_EDGE ( 'NONE', *, *, #78560, .F. ) ;
#57924 = CARTESIAN_POINT ( 'NONE',  ( 113.2699234598519524, -29.59411848847293669, 195.5838068554167535 ) ) ;
#57926 = CARTESIAN_POINT ( 'NONE',  ( 32.15435173586076445, -31.62489322948364290, 117.4678068554150485 ) ) ;
#57927 = CARTESIAN_POINT ( 'NONE',  ( 101.1881973814857076, -45.36612005690837890, 197.1013395616249966 ) ) ;
#57928 = CARTESIAN_POINT ( 'NONE',  ( 113.4153195569882087, -27.68144967124534261, 80.57753003781597556 ) ) ;
#57929 = CARTESIAN_POINT ( 'NONE',  ( 106.9746138897780696, -47.19771061482636298, 183.5699109901969734 ) ) ;
#57930 = DIRECTION ( 'NONE',  ( -6.524622321627019585E-16, -4.013151879589939944E-16, -1.000000000000000000 ) ) ;
#57931 = AXIS2_PLACEMENT_3D ( 'NONE', #63290, #35122, #69661 ) ;
#57932 = LINE ( 'NONE', #77491, #50357 ) ;
#57934 = CARTESIAN_POINT ( 'NONE',  ( 180.2143765759489895, -35.91149509761070391, 193.9678068554150059 ) ) ;
#57933 = FACE_OUTER_BOUND ( 'NONE', #64464, .T. ) ;
#57935 = CARTESIAN_POINT ( 'NONE',  ( 156.5667039024483245, -42.82844715993568485, 173.2178068554149775 ) ) ;
#57936 = CARTESIAN_POINT ( 'NONE',  ( 179.7974245136200011, -36.32844715994040996, -5.074374724088000832 ) ) ;
#57937 = ORIENTED_EDGE ( 'NONE', *, *, #6672, .T. ) ;
#57938 = FACE_OUTER_BOUND ( 'NONE', #35292, .T. ) ;
#57939 = EDGE_LOOP ( 'NONE', ( #33863, #52503, #89278, #39980 ) ) ;
#57940 = ORIENTED_EDGE ( 'NONE', *, *, #85801, .T. ) ;
#57941 = VECTOR ( 'NONE', #81172, 1000.000000000000000 ) ;
#57942 = CARTESIAN_POINT ( 'NONE',  ( 107.8593070027901746, -27.70813345913228076, 109.4171817328389551 ) ) ;
#57944 = VERTEX_POINT ( 'NONE', #1427 ) ;
#57943 = DIRECTION ( 'NONE',  ( 0.000000000000000000, 0.000000000000000000, 1.000000000000000000 ) ) ;
#57945 = CARTESIAN_POINT ( 'NONE',  ( 109.7644292386349889, -47.42453529627113085, 88.78514908543493789 ) ) ;
#57946 = DIRECTION ( 'NONE',  ( 0.000000000000000000, 0.000000000000000000, -1.000000000000000000 ) ) ;
#57947 = DIRECTION ( 'NONE',  ( -0.9254794337955620787, -0.3787978585227822492, 0.000000000000000000 ) ) ;
#57948 = CARTESIAN_POINT ( 'NONE',  ( 139.7494832912729805, -1.929447159941395817, 361.9756252759109998 ) ) ;
#57949 = CARTESIAN_POINT ( 'NONE',  ( 98.38136461969642710, -29.78821554292430207, 45.78991099019597044 ) ) ;
#57950 = EDGE_LOOP ( 'NONE', ( #4483, #37206 ) ) ;
#57951 = VECTOR ( 'NONE', #16530, 999.9999999999998863 ) ;
#57952 = ORIENTED_EDGE ( 'NONE', *, *, #76241, .T. ) ;
#57953 = EDGE_LOOP ( 'NONE', ( #84322, #69107, #50106, #17939 ) ) ;
#57954 = DIRECTION ( 'NONE',  ( 0.000000000000000000, 0.000000000000000000, 1.000000000000000000 ) ) ;
#57955 = CARTESIAN_POINT ( 'NONE',  ( 12.59999999999999964, 82.54999999999999716, 206.3750000000000000 ) ) ;
#57956 = FACE_OUTER_BOUND ( 'NONE', #51801, .T. ) ;
#57957 = DIRECTION ( 'NONE',  ( 0.000000000000000000, 0.000000000000000000, -1.000000000000000000 ) ) ;
#57958 = CARTESIAN_POINT ( 'NONE',  ( -97.46300000000000807, 82.54999999999999716, 12.69999999999966178 ) ) ;
#57959 = CARTESIAN_POINT ( 'NONE',  ( 104.4905195348742240, -26.97865216368831653, 51.28294879281423846 ) ) ;
#57960 = FACE_OUTER_BOUND ( 'NONE', #85523, .T. ) ;
#57961 = AXIS2_PLACEMENT_3D ( 'NONE', #28234, #14179, #61858 ) ;
#57962 = CARTESIAN_POINT ( 'NONE',  ( 74.36911441044605908, 82.96450994655477018, 92.32962665258638424 ) ) ;
#57963 = CARTESIAN_POINT ( 'NONE',  ( 96.21590750668994474, -38.71157422997263353, 51.48229194257797303 ) ) ;
#57964 = ORIENTED_EDGE ( 'NONE', *, *, #69173, .T. ) ;
#57965 = CIRCLE ( 'NONE', #62303, 2.117000000000007987 ) ;
#57966 = CARTESIAN_POINT ( 'NONE',  ( 162.0667039024469886, -67.87844715994089029, 55.21780685541800437 ) ) ;
#57967 = DIRECTION ( 'NONE',  ( 0.000000000000000000, 0.000000000000000000, 1.000000000000000000 ) ) ;
#57968 = CARTESIAN_POINT ( 'NONE',  ( 102.7086973628091187, -29.82731503872160417, 108.3423760838769851 ) ) ;
#57969 = VECTOR ( 'NONE', #55980, 1000.000000000000000 ) ;
#57970 = VECTOR ( 'NONE', #48803, 1000.000000000000114 ) ;
#57971 = EDGE_CURVE ( 'NONE', #46578, #6827, #33978, .T. ) ;
#57972 = EDGE_CURVE ( 'NONE', #70165, #74183, #67368, .T. ) ;
#57973 = FACE_OUTER_BOUND ( 'NONE', #56092, .T. ) ;
#57974 = DIRECTION ( 'NONE',  ( 1.000000000000000000, 8.843517682682131024E-16, 1.000000000000000078E-15 ) ) ;
#57975 = ORIENTED_EDGE ( 'NONE', *, *, #61345, .T. ) ;
#57976 = ORIENTED_EDGE ( 'NONE', *, *, #7027, .F. ) ;
#57978 = ADVANCED_FACE ( 'NONE', ( #28670 ), #14153, .F. ) ;
#57977 = AXIS2_PLACEMENT_3D ( 'NONE', #36640, #64341, #8026 ) ;
#57979 = CARTESIAN_POINT ( 'NONE',  ( 97.92336871694494960, -40.78101110081310310, 136.6586925773791563 ) ) ;
#57980 = ORIENTED_EDGE ( 'NONE', *, *, #80244, .F. ) ;
#57981 = ORIENTED_EDGE ( 'NONE', *, *, #64456, .T. ) ;
#57982 =( GEOMETRIC_REPRESENTATION_CONTEXT ( 3 ) GLOBAL_UNCERTAINTY_ASSIGNED_CONTEXT ( ( #84191 ) ) GLOBAL_UNIT_ASSIGNED_CONTEXT ( ( #19161, #33680, #54537 ) ) REPRESENTATION_CONTEXT ( 'NONE', 'WORKASPACE' ) );
#57983 = EDGE_CURVE ( 'NONE', #76720, #58643, #22772, .T. ) ;
#57984 = CARTESIAN_POINT ( 'NONE',  ( 107.7905181614329564, -45.59160847044328335, 174.0730118773249728 ) ) ;
#57985 = EDGE_CURVE ( 'NONE', #75709, #33402, #56362, .T. ) ;
#57986 = PLANE ( 'NONE',  #19152 ) ;
#57987 = CIRCLE ( 'NONE', #84142, 1.000000000000000888 ) ;
#57988 = CARTESIAN_POINT ( 'NONE',  ( 118.9284187910711665, -36.16665333732972698, 114.8641967044819694 ) ) ;
#57989 = DIRECTION ( 'NONE',  ( 0.8571673007021115565, -0.5150380749100554878, 7.521945815882500121E-16 ) ) ;
#57990 = EDGE_CURVE ( 'NONE', #12239, #89203, #49997, .T. ) ;
#57991 = CARTESIAN_POINT ( 'NONE',  ( 116.9889466309420527, -35.34522876095464738, 18.93671031070073951 ) ) ;
#57992 = ORIENTED_EDGE ( 'NONE', *, *, #26526, .F. ) ;
#57993 = EDGE_CURVE ( 'NONE', #21337, #41991, #64101, .T. ) ;
#57994 = ORIENTED_EDGE ( 'NONE', *, *, #29229, .T. ) ;
#57995 = ORIENTED_EDGE ( 'NONE', *, *, #58202, .F. ) ;
#57996 = EDGE_CURVE ( 'NONE', #30195, #43969, #35469, .T. ) ;
#57997 = CARTESIAN_POINT ( 'NONE',  ( 113.2609745038455742, -30.68550774403005121, 192.2718998934009562 ) ) ;
#57998 = CARTESIAN_POINT ( 'NONE',  ( 101.0534108623914591, -27.42684531413746285, 70.54514908543497143 ) ) ;
#57999 = VERTEX_POINT ( 'NONE', #76823 ) ;
#58000 = CARTESIAN_POINT ( 'NONE',  ( 109.6376038899290677, -46.81002275840761939, 47.77562527591094721 ) ) ;
#58001 = CARTESIAN_POINT ( 'NONE',  ( 117.5090302172161500, -40.42247023647522752, 174.5680062282919778 ) ) ;
#58002 = EDGE_CURVE ( 'NONE', #10270, #34697, #63191, .T. ) ;
#58003 = CARTESIAN_POINT ( 'NONE',  ( 188.5667039024479834, -62.87844715994099687, 173.2178068554149775 ) ) ;
#58004 = CARTESIAN_POINT ( 'NONE',  ( 0.000000000000000000, 92.07499999999998863, 0.000000000000000000 ) ) ;
#58005 = CARTESIAN_POINT ( 'NONE',  ( 108.3194443806174405, -47.07896772641721839, 113.6727681330539639 ) ) ;
#58006 = ADVANCED_FACE ( 'NONE', ( #42282 ), #85005, .T. ) ;
#58007 = DIRECTION ( 'NONE',  ( -0.9254794337955620787, -0.3787978585227822492, 0.000000000000000000 ) ) ;
#58008 = ORIENTED_EDGE ( 'NONE', *, *, #26106, .T. ) ;
#58009 = DIRECTION ( 'NONE',  ( -1.000000000000000000, 0.000000000000000000, -2.108231265501709878E-16 ) ) ;
#58010 = VERTEX_POINT ( 'NONE', #69118 ) ;
#58011 = DIRECTION ( 'NONE',  ( 0.000000000000000000, 0.000000000000000000, 1.000000000000000000 ) ) ;
#58012 = PLANE ( 'NONE',  #53163 ) ;
#58014 = EDGE_LOOP ( 'NONE', ( #55168, #28645, #25376, #40870 ) ) ;
#58013 = AXIS2_PLACEMENT_3D ( 'NONE', #54922, #27245, #82685 ) ;
#58015 = CARTESIAN_POINT ( 'NONE',  ( 110.0324702783111661, -88.49073317540081973, -21.02845593540976310 ) ) ;
#58016 = CARTESIAN_POINT ( 'NONE',  ( 99.00936352106049299, -30.68773460668057851, 131.8138018080218217 ) ) ;
#58017 = CARTESIAN_POINT ( 'NONE',  ( 99.29363446503140267, -43.73007054641615809, 56.90991099019593236 ) ) ;
#58018 = DIRECTION ( 'NONE',  ( 0.000000000000000000, 0.000000000000000000, 1.000000000000000000 ) ) ;
#58019 = CARTESIAN_POINT ( 'NONE',  ( 52.38749999999999574, 94.53880000000000905, 250.8250000000000171 ) ) ;
#58020 = CARTESIAN_POINT ( 'NONE',  ( 142.0664832912740110, -9.729447159940995959, -4.824374724088994704 ) ) ;
#58021 = CARTESIAN_POINT ( 'NONE',  ( 105.5226833586260682, -46.38761039419750176, 37.44991099019695469 ) ) ;
#58023 = CARTESIAN_POINT ( 'NONE',  ( 102.4028819069269645, -26.73371583578780886, 131.4118157521009778 ) ) ;
#58022 = CARTESIAN_POINT ( 'NONE',  ( 72.17003668186733023, -45.68655394112764156, -5.074374724089090627 ) ) ;
#58024 = DIRECTION ( 'NONE',  ( 1.000000000000000000, 0.000000000000000000, 0.000000000000000000 ) ) ;
#58025 = FACE_OUTER_BOUND ( 'NONE', #87835, .T. ) ;
#58026 = ORIENTED_EDGE ( 'NONE', *, *, #57971, .F. ) ;
#58027 = DIRECTION ( 'NONE',  ( 1.000000000000000078E-15, -1.000000000000000083E-30, -1.000000000000000000 ) ) ;
#58028 = AXIS2_PLACEMENT_3D ( 'NONE', #8260, #42306, #70039 ) ;
#58029 = ADVANCED_FACE ( 'NONE', ( #77276, #15051 ), #13697, .F. ) ;
#58030 = DIRECTION ( 'NONE',  ( 0.000000000000000000, 0.000000000000000000, 1.000000000000000000 ) ) ;
#58031 = EDGE_CURVE ( 'NONE', #53830, #29616, #70465, .T. ) ;
#58032 = LINE ( 'NONE', #71677, #38650 ) ;
#58033 = EDGE_CURVE ( 'NONE', #44371, #23155, #18044, .T. ) ;
#58034 = AXIS2_PLACEMENT_3D ( 'NONE', #11583, #39274, #4759 ) ;
#58035 = DIRECTION ( 'NONE',  ( -0.7071067812158990940, -0.7071067811571960515, 0.000000000000000000 ) ) ;
#58037 = ORIENTED_EDGE ( 'NONE', *, *, #4665, .T. ) ;
#58036 = CARTESIAN_POINT ( 'NONE',  ( 103.6240789207236475, -26.17659276989511596, 210.3394347997209763 ) ) ;
#58038 = FACE_OUTER_BOUND ( 'NONE', #82056, .T. ) ;
#58039 = CARTESIAN_POINT ( 'NONE',  ( 101.2819412958853320, -26.35826957050098329, 251.4813395616249920 ) ) ;
#58040 = CARTESIAN_POINT ( 'NONE',  ( 98.05938055883913762, -31.39417958322244218, 81.90133956162493689 ) ) ;
#58041 = B_SPLINE_CURVE_WITH_KNOTS ( 'NONE', 3,
 ( #57186, #29503, #64469, #73055, #64028, #84933, #78118, #15881, #43559, #9067, #47464, #20679 ),
 .UNSPECIFIED., .F., .F.,
 ( 4, 2, 2, 2, 2, 4 ),
 ( 0.08510440135476479706, 0.08774507987650315144, 0.09038575839824151970, 0.09302643691997988795, 0.09434677618084906514, 0.09566711544171824233 ),
 .UNSPECIFIED. ) ;
#58042 = ADVANCED_FACE ( 'NONE', ( #34584 ), #62288, .F. ) ;
#58043 = CARTESIAN_POINT ( 'NONE',  ( 83.15048135366386362, 79.66749569656609253, 100.6522392491107922 ) ) ;
#58044 = FACE_OUTER_BOUND ( 'NONE', #15876, .T. ) ;
#58045 = FACE_OUTER_BOUND ( 'NONE', #29531, .T. ) ;
#58046 = ORIENTED_EDGE ( 'NONE', *, *, #47826, .T. ) ;
#58047 = VECTOR ( 'NONE', #85307, 1000.000000000000000 ) ;
#58048 = B_SPLINE_CURVE_WITH_KNOTS ( 'NONE', 3,
 ( #89629, #34193, #13319, #20137, #88736, #54165, #41006, #68726, #47810, #81925, #6492, #26491, #19681, #33755, #75549, #47361, #75090, #12880, #26945, #40567, #6067, #61444, #89175, #54613, #82372, #73136 ),
 .UNSPECIFIED., .F., .F.,
 ( 4, 2, 1, 1, 2, 2, 2, 2, 2, 2, 2, 2, 2, 4 ),
 ( 0.5000914289992475226, 0.5020441968547191269, 0.5039969647101907313, 0.5079025004211340510, 0.5157135718430211346, 0.5313357146867948577, 0.5625800003743418598, 0.6250685717494358640, 0.6875571431245298681, 0.7500457144996239833, 0.8125342858747179875, 0.8750228572498119917, 0.9375114286249059958, 1.000000000000000000 ),
 .UNSPECIFIED. ) ;
#58049 = EDGE_LOOP ( 'NONE', ( #4485, #73393, #39308, #33108 ) ) ;
#58050 = ORIENTED_EDGE ( 'NONE', *, *, #62778, .F. ) ;
#58051 = ORIENTED_EDGE ( 'NONE', *, *, #15614, .F. ) ;
#58052 = DIRECTION ( 'NONE',  ( 0.000000000000000000, 1.000000000000000000, 0.000000000000000000 ) ) ;
#58053 = CARTESIAN_POINT ( 'NONE',  ( 105.8935855965125938, -47.12395608077676457, 278.4870538473395527 ) ) ;
#58054 = DIRECTION ( 'NONE',  ( -3.100000000000000258E-29, 3.100000000000000044E-14, 1.000000000000000000 ) ) ;
#58055 = CARTESIAN_POINT ( 'NONE',  ( 131.8086190314097337, -35.15582774929892196, 2.518078172612455479 ) ) ;
#58056 = PRODUCT_DEFINITION_FORMATION_WITH_SPECIFIED_SOURCE ( 'ANY', '', #19058, .NOT_KNOWN. ) ;
#58058 = CARTESIAN_POINT ( 'NONE',  ( 74.36911441044604487, 81.72118090664555723, 92.32962665258637003 ) ) ;
#58057 = DIRECTION ( 'NONE',  ( 4.299999999999999979E-14, -1.000000000000000000, 4.400000000000000367E-29 ) ) ;
#58059 = DIRECTION ( 'NONE',  ( 4.299999999999999979E-14, -1.000000000000000000, 4.400000000000000367E-29 ) ) ;
#58060 = CARTESIAN_POINT ( 'NONE',  ( 114.6728154972408475, -42.76387655025251888, 197.7152769709339566 ) ) ;
#58061 = EDGE_LOOP ( 'NONE', ( #82464, #45736, #51712, #8481 ) ) ;
#58062 = VERTEX_POINT ( 'NONE', #3647 ) ;
#58063 = ORIENTED_EDGE ( 'NONE', *, *, #60849, .F. ) ;
#58064 = PLANE ( 'NONE',  #18045 ) ;
#58065 = CYLINDRICAL_SURFACE ( 'NONE', #31776, 3.814291549405317117 ) ;
#58066 = CARTESIAN_POINT ( 'NONE',  ( 114.5610390845466071, -30.44493693613353358, 265.3813395616247135 ) ) ;
#58067 = AXIS2_PLACEMENT_3D ( 'NONE', #42448, #47914, #34300 ) ;
#58068 = DIRECTION ( 'NONE',  ( 0.000000000000000000, 0.000000000000000000, -1.000000000000000000 ) ) ;
#58069 = CARTESIAN_POINT ( 'NONE',  ( 110.0667047667142953, -70.87844715994094713, 173.2178068554179902 ) ) ;
#58070 = ORIENTED_EDGE ( 'NONE', *, *, #1605, .T. ) ;
#58071 = DIRECTION ( 'NONE',  ( -1.000000000000000000, 0.000000000000000000, 0.000000000000000000 ) ) ;
#58072 = ORIENTED_EDGE ( 'NONE', *, *, #54892, .F. ) ;
#58073 = CIRCLE ( 'NONE', #4458, 7.499999999999992895 ) ;
#58074 = CARTESIAN_POINT ( 'NONE',  ( 0.000000000000000000, 125.7300000000000040, 0.000000000000000000 ) ) ;
#58075 = CARTESIAN_POINT ( 'NONE',  ( 102.7933444172945769, -44.96577155458380304, 15.01380465530593966 ) ) ;
#58076 = CARTESIAN_POINT ( 'NONE',  ( 136.8118108219001101, -18.54506369576942149, 6.756870619998893268 ) ) ;
#58077 = EDGE_CURVE ( 'NONE', #9110, #61450, #45405, .T. ) ;
#58078 = EDGE_CURVE ( 'NONE', #89290, #74189, #39816, .T. ) ;
#58079 = LINE ( 'NONE', #3561, #56285 ) ;
#58080 = CARTESIAN_POINT ( 'NONE',  ( 138.0667039024470171, -104.2784471599409244, 45.21780685541799727 ) ) ;
#58081 = ORIENTED_EDGE ( 'NONE', *, *, #28833, .T. ) ;
#58082 = VECTOR ( 'NONE', #16538, 1000.000000000000000 ) ;
#58083 = DIRECTION ( 'NONE',  ( 0.000000000000000000, 0.000000000000000000, 1.000000000000000000 ) ) ;
#58084 = EDGE_CURVE ( 'NONE', #19430, #55378, #86327, .T. ) ;
#58085 = CARTESIAN_POINT ( 'NONE',  ( 172.5667039024478413, -36.32844715993500273, 249.9678068554149775 ) ) ;
#58086 = EDGE_LOOP ( 'NONE', ( #76548, #12682, #11524, #26432 ) ) ;
#58087 = CARTESIAN_POINT ( 'NONE',  ( 100.2985985360463843, -46.45756217656626319, 87.09276813305393716 ) ) ;
#58088 = ORIENTED_EDGE ( 'NONE', *, *, #13077, .F. ) ;
#58089 = CARTESIAN_POINT ( 'NONE',  ( 101.6694414210978294, -29.45726664942652917, 35.01908649474394508 ) ) ;
#58090 = EDGE_CURVE ( 'NONE', #17303, #68744, #71804, .T. ) ;
#58091 = CARTESIAN_POINT ( 'NONE',  ( 106.9373099352470007, -46.76238444484523171, 88.56563845889516529 ) ) ;
#58092 = CARTESIAN_POINT ( 'NONE',  ( 111.6972492074939396, -29.17403283370891032, 91.07015473446894305 ) ) ;
#58093 = CARTESIAN_POINT ( 'NONE',  ( 117.0721298179341829, -35.46442564195397296, 14.92713738205877583 ) ) ;
#58094 = EDGE_CURVE ( 'NONE', #51807, #20018, #65947, .T. ) ;
#58095 = DIRECTION ( 'NONE',  ( 0.000000000000000000, 1.000000000000000000, 0.000000000000000000 ) ) ;
#58096 = DIRECTION ( 'NONE',  ( 0.000000000000000000, 0.000000000000000000, 1.000000000000000000 ) ) ;
#58097 = CARTESIAN_POINT ( 'NONE',  ( 96.84642183402544902, -30.63342722027062592, 276.8984824187680829 ) ) ;
#58098 = AXIS2_PLACEMENT_3D ( 'NONE', #38681, #58669, #73655 ) ;
#58100 = EDGE_CURVE ( 'NONE', #77207, #11788, #15948, .T. ) ;
#58099 = CARTESIAN_POINT ( 'NONE',  ( 188.5667039024479834, -65.37844715994100397, 178.0928068554149775 ) ) ;
#58101 = ORIENTED_EDGE ( 'NONE', *, *, #13098, .T. ) ;
#58102 = CARTESIAN_POINT ( 'NONE',  ( 162.7131505118539962, -33.70561438052090608, -5.074374724088000832 ) ) ;
#58103 = EDGE_LOOP ( 'NONE', ( #15942, #6320 ) ) ;
#58104 = CARTESIAN_POINT ( 'NONE',  ( 116.9452694852055998, -40.19391870447465465, 129.5584824187679658 ) ) ;
#58105 = CARTESIAN_POINT ( 'NONE',  ( 125.3300043389053684, 51.65368650150782770, -36.56872758047426686 ) ) ;
#58106 = EDGE_LOOP ( 'NONE', ( #32023, #23518, #14014, #26633, #89906, #18975, #51924, #24664, #44312, #23015 ) ) ;
#58107 = EDGE_LOOP ( 'NONE', ( #35265, #87327, #8113, #14335 ) ) ;
#58108 = EDGE_CURVE ( 'NONE', #29962, #31120, #73208, .T. ) ;
#58109 = VECTOR ( 'NONE', #28, 1000.000000000000000 ) ;
#58110 = DIRECTION ( 'NONE',  ( -1.000000000000000000, 0.000000000000000000, 0.000000000000000000 ) ) ;
#58111 = FACE_OUTER_BOUND ( 'NONE', #2784, .T. ) ;
#58112 = CARTESIAN_POINT ( 'NONE',  ( 97.67678136301120162, -41.13084272647608941, 211.6632443235309893 ) ) ;
#58113 = DIRECTION ( 'NONE',  ( -4.237773401492740281E-14, 1.000000000000000000, 0.000000000000000000 ) ) ;
#58114 = CARTESIAN_POINT ( 'NONE',  ( 144.0667038965492566, -140.6784471658387190, 245.4415720115519832 ) ) ;
#58115 = LINE ( 'NONE', #50852, #30147 ) ;
#58116 = CARTESIAN_POINT ( 'NONE',  ( 101.6089948421187898, -47.24856100052405594, 13.19562527591094891 ) ) ;
#58117 = EDGE_CURVE ( 'NONE', #753, #49629, #21027, .T. ) ;
#58118 = CARTESIAN_POINT ( 'NONE',  ( 72.06648329127396835, -9.729447159941065237, 14.67562527591093513 ) ) ;
#58119 = ORIENTED_EDGE ( 'NONE', *, *, #26929, .F. ) ;
#58120 = DIRECTION ( 'NONE',  ( 1.000000000000000078E-15, -1.000000000000000083E-30, -1.000000000000000000 ) ) ;
#58121 = DIRECTION ( 'NONE',  ( 1.000000000000000000, 8.326672684688666480E-14, 0.000000000000000000 ) ) ;
#58123 = ORIENTED_EDGE ( 'NONE', *, *, #35021, .F. ) ;
#58122 = EDGE_CURVE ( 'NONE', #62435, #65273, #11859, .T. ) ;
#58124 = DIRECTION ( 'NONE',  ( -0.7071067811865171526, -0.7071067811865779928, -7.071067811865164719E-16 ) ) ;
#58125 = PLANE ( 'NONE',  #65800 ) ;
#58126 = CARTESIAN_POINT ( 'NONE',  ( 103.0988156209413233, -47.86972635628425365, 252.3041967044823366 ) ) ;
#58127 = FILL_AREA_STYLE ('',( #43144 ) ) ;
#58128 = CARTESIAN_POINT ( 'NONE',  ( 172.5664832912729878, -27.82844715994070484, 78.92562527591199739 ) ) ;
#58129 = CYLINDRICAL_SURFACE ( 'NONE', #5533, 4.749999999999976907 ) ;
#58130 = AXIS2_PLACEMENT_3D ( 'NONE', #21967, #77816, #7868 ) ;
#58131 = CARTESIAN_POINT ( 'NONE',  ( 115.5432862745613676, -35.46615253551063063, 218.3667055423629790 ) ) ;
#58133 = CARTESIAN_POINT ( 'NONE',  ( 116.3681181406586518, -31.99193570193499525, 40.20133956162496958 ) ) ;
#58132 = CARTESIAN_POINT ( 'NONE',  ( 151.0371591254582597, -46.82818131005583240, 300.4678068554149490 ) ) ;
#58134 = CARTESIAN_POINT ( 'NONE',  ( 73.06670390244801183, -50.82844715994100682, 310.9178068554150514 ) ) ;
#58135 = CARTESIAN_POINT ( 'NONE',  ( 108.5962597759698127, -47.12230983477568458, 142.6927681330539883 ) ) ;
#58136 = EDGE_LOOP ( 'NONE', ( #31857, #28004, #7056, #24885 ) ) ;
#58137 = CARTESIAN_POINT ( 'NONE',  ( 131.9720459101981760, -20.52018918696424166, 7.480061334662067019 ) ) ;
#58138 = VERTEX_POINT ( 'NONE', #37734 ) ;
#58139 = VECTOR ( 'NONE', #7890, 999.9999999999998863 ) ;
#58140 = DIRECTION ( 'NONE',  ( -1.000000000000000000, -4.299999999999999979E-14, -1.000000000000000078E-15 ) ) ;
#58141 = CARTESIAN_POINT ( 'NONE',  ( 97.31637614840812489, -39.30795178117394073, 277.5316211441031555 ) ) ;
#58142 = VERTEX_POINT ( 'NONE', #30905 ) ;
#58143 = EDGE_CURVE ( 'NONE', #23113, #25704, #79524, .T. ) ;
#58144 = DIRECTION ( 'NONE',  ( 1.000000000000000000, 0.000000000000000000, 0.000000000000000000 ) ) ;
#58145 = ORIENTED_EDGE ( 'NONE', *, *, #76874, .T. ) ;
#58146 = DIRECTION ( 'NONE',  ( -3.100000000000000258E-29, 3.100000000000000044E-14, 1.000000000000000000 ) ) ;
#58147 = EDGE_CURVE ( 'NONE', #19337, #1704, #9423, .T. ) ;
#58148 = DIRECTION ( 'NONE',  ( 0.8660254037844382635, 0.5000000000000008882, -1.550000000000000022E-14 ) ) ;
#58149 = VECTOR ( 'NONE', #58518, 1000.000000000000000 ) ;
#58150 = CARTESIAN_POINT ( 'NONE',  ( 49.16670390244701139, -28.27351298637340093, 342.9256252759119548 ) ) ;
#58151 = ORIENTED_EDGE ( 'NONE', *, *, #9659, .T. ) ;
#58152 = VECTOR ( 'NONE', #29180, 1000.000000000000000 ) ;
#58153 = CARTESIAN_POINT ( 'NONE',  ( 115.2845782536562353, -44.15631435451261666, 83.25372051400698581 ) ) ;
#58154 = SHAPE_REPRESENTATION_RELATIONSHIP ( 'NONE' , 'NONE' ,  #64293, #56477 ) ;
#58155 = CARTESIAN_POINT ( 'NONE',  ( 33.98325472291465132, 111.1250000000000000, -3.174999999999999822 ) ) ;
#58156 = CYLINDRICAL_SURFACE ( 'NONE', #66942, 1.000000000000003775 ) ;
#58157 = CARTESIAN_POINT ( 'NONE',  ( -12.17234564962928012, 79.26918314695168988, 117.7284643969750135 ) ) ;
#58158 = ORIENTED_EDGE ( 'NONE', *, *, #35842, .T. ) ;
#58159 = LINE ( 'NONE', #79067, #14155 ) ;
#58160 = DIRECTION ( 'NONE',  ( 0.000000000000000000, 0.000000000000000000, 1.000000000000000000 ) ) ;
#58161 = CARTESIAN_POINT ( 'NONE',  ( 20.56670390244643443, -48.82844715994099971, 180.4678068554150911 ) ) ;
#58162 = VECTOR ( 'NONE', #13502, 1000.000000000000000 ) ;
#58163 = ADVANCED_FACE ( 'NONE', ( #24546, #52209 ), #3214, .F. ) ;
#58165 = CARTESIAN_POINT ( 'NONE',  ( 67.06670390210777555, -137.6784471596019728, 245.4218662566959779 ) ) ;
#58164 = DIRECTION ( 'NONE',  ( -1.000000000000000078E-15, 1.000000000000000083E-30, 1.000000000000000000 ) ) ;
#58166 = CARTESIAN_POINT ( 'NONE',  ( 31.78666935232898894, -29.62846900982320264, -5.074374724088000832 ) ) ;
#58167 = VECTOR ( 'NONE', #63058, 1000.000000000000000 ) ;
#58168 = ADVANCED_FACE ( 'NONE', ( #58594 ), #16689, .T. ) ;
#58169 = ORIENTED_EDGE ( 'NONE', *, *, #21401, .F. ) ;
#58170 = CARTESIAN_POINT ( 'NONE',  ( -3.175000000000120171, 8.255000000000000782, -33.98325472291460159 ) ) ;
#58171 = CARTESIAN_POINT ( 'NONE',  ( 116.0678243078410787, -40.55558035091540603, 164.5070538473389661 ) ) ;
#58172 = AXIS2_PLACEMENT_3D ( 'NONE', #31631, #68407, #19806 ) ;
#58174 = ORIENTED_EDGE ( 'NONE', *, *, #74700, .T. ) ;
#58173 = CARTESIAN_POINT ( 'NONE',  ( 80.06648329127399677, -36.72944715994107412, 14.92562527591094224 ) ) ;
#58175 = CARTESIAN_POINT ( 'NONE',  ( 97.30224646444959546, -33.23681714887386818, 22.06514908543394426 ) ) ;
#58176 = DIRECTION ( 'NONE',  ( -1.000000000000000078E-15, 1.000000000000000000, 0.000000000000000000 ) ) ;
#58177 = DIRECTION ( 'NONE',  ( 0.000000000000000000, 0.000000000000000000, 1.000000000000000000 ) ) ;
#58178 = CARTESIAN_POINT ( 'NONE',  ( 105.7138873538276727, -46.72361729074350478, 12.46910743858308379 ) ) ;
#58179 = AXIS2_PLACEMENT_3D ( 'NONE', #47162, #12222, #26730 ) ;
#58180 = VERTEX_POINT ( 'NONE', #51773 ) ;
#58181 = CARTESIAN_POINT ( 'NONE',  ( 115.0899025498120807, -30.61893087844507733, 29.34406161155381199 ) ) ;
#58182 = CARTESIAN_POINT ( 'NONE',  ( 106.9482321581270270, -47.09886382165569785, 232.5794347997209854 ) ) ;
#58183 = EDGE_LOOP ( 'NONE', ( #38444, #60692, #66696, #85971 ) ) ;
#58184 = VERTEX_POINT ( 'NONE', #59486 ) ;
#58185 = EDGE_CURVE ( 'NONE', #42451, #12839, #9577, .T. ) ;
#58186 = CARTESIAN_POINT ( 'NONE',  ( 113.7913652599847438, -30.16800768036728542, 190.8853928297069444 ) ) ;
#58187 = LINE ( 'NONE', #50921, #71937 ) ;
#58188 = CARTESIAN_POINT ( 'NONE',  ( 101.0434111811767224, -43.22951492638978266, 43.41301187732599232 ) ) ;
#58189 = CARTESIAN_POINT ( 'NONE',  ( 23.03803956593629465, 87.31264177286587369, 303.2054484439112798 ) ) ;
#58190 = ADVANCED_FACE ( 'NONE', ( #64540 ), #2322, .T. ) ;
#58191 = EDGE_CURVE ( 'NONE', #78957, #50094, #57715, .T. ) ;
#58192 = CARTESIAN_POINT ( 'NONE',  ( 115.8254323921426874, -31.73001882930526207, 79.23979194253121250 ) ) ;
#58193 = DIRECTION ( 'NONE',  ( 4.194175870806139918E-14, -1.000000000000000000, 0.000000000000000000 ) ) ;
#58194 = ORIENTED_EDGE ( 'NONE', *, *, #85298, .T. ) ;
#58195 = CARTESIAN_POINT ( 'NONE',  ( 177.1649999999999920, 25.81350000000000477, -7.937500000000000000 ) ) ;
#58196 = EDGE_CURVE ( 'NONE', #68666, #65898, #78643, .T. ) ;
#58197 = CARTESIAN_POINT ( 'NONE',  ( 0.000000000000000000, 20.32000000000000028, 0.000000000000000000 ) ) ;
#58198 = ORIENTED_EDGE ( 'NONE', *, *, #28144, .T. ) ;
#58199 = CARTESIAN_POINT ( 'NONE',  ( 109.9831304889623027, -26.74336511273919115, 259.8499109901965767 ) ) ;
#58200 = FACE_OUTER_BOUND ( 'NONE', #35995, .T. ) ;
#58201 = ORIENTED_EDGE ( 'NONE', *, *, #30911, .F. ) ;
#58202 = EDGE_CURVE ( 'NONE', #87802, #64292, #44217, .T. ) ;
#58203 = DIRECTION ( 'NONE',  ( 0.000000000000000000, 0.000000000000000000, 1.000000000000000000 ) ) ;
#58204 = LINE ( 'NONE', #59521, #12812 ) ;
#58205 = DIRECTION ( 'NONE',  ( -0.7071067811864671926, -0.7071067811866279529, -7.071067811864664779E-16 ) ) ;
#58206 = DIRECTION ( 'NONE',  ( -1.058811598242755461E-16, 0.5150380749100580413, -0.8571673007021100021 ) ) ;
#58207 = AXIS2_PLACEMENT_3D ( 'NONE', #83695, #21010, #15551 ) ;
#58208 = CARTESIAN_POINT ( 'NONE',  ( 107.5734549334945314, -47.83597508069280480, 38.61276813305297395 ) ) ;
#58209 = CARTESIAN_POINT ( 'NONE',  ( -7.301849239715819957E-13, 120.6499999999999915, 98.60478223830740774 ) ) ;
#58210 = EDGE_CURVE ( 'NONE', #58962, #4111, #74029, .T. ) ;
#58211 = ORIENTED_EDGE ( 'NONE', *, *, #8791, .F. ) ;
#58212 = AXIS2_PLACEMENT_3D ( 'NONE', #82606, #68510, #68954 ) ;
#58213 = CARTESIAN_POINT ( 'NONE',  ( 115.7091107927249283, -43.69381994074442588, 39.27467289495895386 ) ) ;
#58214 = CARTESIAN_POINT ( 'NONE',  ( -75.61066417432020614, 20.32000000000000028, 177.0380000000000109 ) ) ;
#58215 = CARTESIAN_POINT ( 'NONE',  ( 105.1090048964814940, -25.85068961359000284, 275.2061014663871674 ) ) ;
#58216 = ORIENTED_EDGE ( 'NONE', *, *, #34693, .T. ) ;
#58217 = EDGE_CURVE ( 'NONE', #73485, #8177, #66007, .T. ) ;
#58218 = DIRECTION ( 'NONE',  ( 0.000000000000000000, 0.000000000000000000, -1.000000000000000000 ) ) ;
#58219 = CARTESIAN_POINT ( 'NONE',  ( 180.2121375201600131, -29.73316016639650172, -5.074374724088000832 ) ) ;
#58220 = CARTESIAN_POINT ( 'NONE',  ( 57.56670390244804736, -42.82844715994040286, 293.2178068554150627 ) ) ;
#58221 = CARTESIAN_POINT ( 'NONE',  ( 100.0846959373945566, -41.84369885408329992, 104.6357094172109470 ) ) ;
#58222 = CARTESIAN_POINT ( 'NONE',  ( 110.5060411634814557, -26.86503128786541694, 205.8099109901969541 ) ) ;
#58223 = DIRECTION ( 'NONE',  ( 1.000000000000000078E-15, -1.000000000000000083E-30, -1.000000000000000000 ) ) ;
#58224 = CIRCLE ( 'NONE', #65485, 12.60000000000000142 ) ;
#58225 = DIRECTION ( 'NONE',  ( 0.8660254037844392627, -0.4999999999999990008, 1.549999999999999706E-14 ) ) ;
#58226 = ORIENTED_EDGE ( 'NONE', *, *, #64289, .T. ) ;
#58227 = DIRECTION ( 'NONE',  ( 1.907762142705490052E-15, 7.167082501179359715E-16, -1.000000000000000000 ) ) ;
#58228 = EDGE_LOOP ( 'NONE', ( #74404, #63841, #2448, #33480 ) ) ;
#58230 = VERTEX_POINT ( 'NONE', #81320 ) ;
#58229 = VECTOR ( 'NONE', #84323, 1000.000000000000000 ) ;
#58231 = DIRECTION ( 'NONE',  ( 0.000000000000000000, 0.000000000000000000, 1.000000000000000000 ) ) ;
#58232 = ORIENTED_EDGE ( 'NONE', *, *, #43016, .T. ) ;
#58233 = ORIENTED_EDGE ( 'NONE', *, *, #22019, .T. ) ;
#58234 = CARTESIAN_POINT ( 'NONE',  ( 116.7958028337206855, -39.38540548342588465, 169.6153133619191067 ) ) ;
#58235 = CARTESIAN_POINT ( 'NONE',  ( 103.2785305379161969, -27.47464224906687491, 41.38562391700290988 ) ) ;
#58236 = CARTESIAN_POINT ( 'NONE',  ( 104.1185212827848545, -44.74603268130591971, 141.7181341137909669 ) ) ;
#58237 = VECTOR ( 'NONE', #77916, 1000.000000000000000 ) ;
#58238 = CARTESIAN_POINT ( 'NONE',  ( 100.2336795655629089, -28.82633655636628589, 260.6441967044821695 ) ) ;
#58239 = CARTESIAN_POINT ( 'NONE',  ( -8.383129030752360933, 73.00074830044857777, 130.2869803084437592 ) ) ;
#58240 = VECTOR ( 'NONE', #42481, 1000.000000000000000 ) ;
#58241 = ORIENTED_EDGE ( 'NONE', *, *, #75886, .T. ) ;
#58242 = CARTESIAN_POINT ( 'NONE',  ( 99.09542022332205136, -30.55081675378443862, 136.8022615499500603 ) ) ;
#58243 = ORIENTED_EDGE ( 'NONE', *, *, #89197, .F. ) ;
#58244 = CARTESIAN_POINT ( 'NONE',  ( 76.20505178924339873, 127.0000000000000000, 76.20505178924419454 ) ) ;
#58245 = DIRECTION ( 'NONE',  ( 1.000000000000000000, 8.141040168700802252E-12, 0.000000000000000000 ) ) ;
#58246 = ADVANCED_FACE ( 'NONE', ( #80862 ), #88568, .T. ) ;
#58247 = DIRECTION ( 'NONE',  ( 1.000000000000000000, 4.163336342344333240E-14, 0.000000000000000000 ) ) ;
#58248 = CARTESIAN_POINT ( 'NONE',  ( 113.7843247631140571, -29.05179538500707892, 289.5032443235299979 ) ) ;
#58249 = ORIENTED_EDGE ( 'NONE', *, *, #12476, .T. ) ;
#58250 = CARTESIAN_POINT ( 'NONE',  ( 118.6541713771196527, -39.21258442193070692, 258.6584824187679033 ) ) ;
#58251 = CARTESIAN_POINT ( 'NONE',  ( 96.29945253806019423, -39.42498279898523350, 12.53372051400597442 ) ) ;
#58252 = CYLINDRICAL_SURFACE ( 'NONE', #3941, 2.750000000000002665 ) ;
#58254 = CARTESIAN_POINT ( 'NONE',  ( 79.56670390244796920, -50.82844715994100682, 280.9178068554149945 ) ) ;
#58253 = DIRECTION ( 'NONE',  ( -1.000000000000000000, 0.000000000000000000, 0.000000000000000000 ) ) ;
#58255 = DIRECTION ( 'NONE',  ( 1.000000000000000000, 0.000000000000000000, 0.000000000000000000 ) ) ;
#58256 = DIRECTION ( 'NONE',  ( 0.7071067811989784069, -0.7071067811741166276, 6.612322855976402389E-17 ) ) ;
#58257 = CARTESIAN_POINT ( 'NONE',  ( 131.5922609085481838, -37.93375462386097752, 7.110117206094888509 ) ) ;
#58258 = AXIS2_PLACEMENT_3D ( 'NONE', #71796, #30013, #15940 ) ;
#58259 = DIRECTION ( 'NONE',  ( 0.000000000000000000, 0.000000000000000000, 1.000000000000000000 ) ) ;
#58260 = CARTESIAN_POINT ( 'NONE',  ( 116.8169175499061936, -34.15212344989235760, 164.0313744165063667 ) ) ;
#58261 = CARTESIAN_POINT ( 'NONE',  ( 107.0664832912739968, -36.72944715994100306, 287.6356252759109680 ) ) ;
#58262 = CARTESIAN_POINT ( 'NONE',  ( 123.6837132603320413, -23.41243780205710578, 239.5838068554165545 ) ) ;
#58263 = CARTESIAN_POINT ( 'NONE',  ( 116.6022279875747216, -42.36549642380604297, 283.4137205140060018 ) ) ;
#58264 = CARTESIAN_POINT ( 'NONE',  ( 95.56951908670150431, -39.60249947413915805, 162.5213395616259788 ) ) ;
#58265 = CARTESIAN_POINT ( 'NONE',  ( 117.0746561606024869, -31.98374578269911339, 60.19086337114898555 ) ) ;
#58266 = AXIS2_PLACEMENT_3D ( 'NONE', #43163, #56795, #36820 ) ;
#58268 = DIRECTION ( 'NONE',  ( 0.000000000000000000, 0.000000000000000000, -1.000000000000000000 ) ) ;
#58267 = CARTESIAN_POINT ( 'NONE',  ( 116.3274949261486881, -32.94048995676258329, 25.13562527591095375 ) ) ;
#58269 = CARTESIAN_POINT ( 'NONE',  ( 82.81648329127399677, -36.72944715994106701, 3.101481641215461327 ) ) ;
#58270 = AXIS2_PLACEMENT_3D ( 'NONE', #3048, #67049, #37569 ) ;
#58271 = EDGE_CURVE ( 'NONE', #25851, #2950, #61718, .T. ) ;
#58272 = EDGE_LOOP ( 'NONE', ( #83361, #48362, #10643, #50380 ) ) ;
#58273 = CARTESIAN_POINT ( 'NONE',  ( 41.56648329127398966, -27.82844715994070484, 318.9256252759120116 ) ) ;
#58274 = ORIENTED_EDGE ( 'NONE', *, *, #71382, .F. ) ;
#58275 = CARTESIAN_POINT ( 'NONE',  ( 113.9027609268605659, -43.72435554967452731, 69.19276813305297935 ) ) ;
#58277 = EDGE_LOOP ( 'NONE', ( #34633, #3638, #81254, #21612 ) ) ;
#58276 = DIRECTION ( 'NONE',  ( -4.237773401492740281E-14, 1.000000000000000000, 0.000000000000000000 ) ) ;
#58278 = DIRECTION ( 'NONE',  ( 1.000000000000000078E-15, -1.000000000000000083E-30, -1.000000000000000000 ) ) ;
#58279 = CARTESIAN_POINT ( 'NONE',  ( 103.5497706991577189, -26.90106182813410740, 186.3499109901969746 ) ) ;
#58280 = CARTESIAN_POINT ( 'NONE',  ( 163.0664832912739826, 19.62155284005901024, 333.4006252759110112 ) ) ;
#58281 = DIRECTION ( 'NONE',  ( 0.7071067811865046071, 0.7071067811865904273, 7.071067811865351088E-16 ) ) ;
#58282 = DIRECTION ( 'NONE',  ( 0.7071067811865496822, -0.7071067811865453523, 0.000000000000000000 ) ) ;
#58283 = CARTESIAN_POINT ( 'NONE',  ( 154.5667039024470171, -79.67844715994088745, 85.21780685541799016 ) ) ;
#58284 = CIRCLE ( 'NONE', #80027, 0.5000000000000104361 ) ;
#58285 = DIRECTION ( 'NONE',  ( 1.000000000000000000, 0.000000000000000000, 0.000000000000000000 ) ) ;
#58286 = CARTESIAN_POINT ( 'NONE',  ( 98.04149280439727931, -41.04180111718832791, 96.68119745713256918 ) ) ;
#58287 = CARTESIAN_POINT ( 'NONE',  ( 113.4245949246308243, -29.25360672088980962, 139.5156252759109634 ) ) ;
#58288 = EDGE_LOOP ( 'NONE', ( #41894, #86752, #1753, #19010 ) ) ;
#58289 = ORIENTED_EDGE ( 'NONE', *, *, #73126, .T. ) ;
#58290 = AXIS2_PLACEMENT_3D ( 'NONE', #12703, #27662, #55340 ) ;
#58291 = CARTESIAN_POINT ( 'NONE',  ( 102.5140397859015877, -29.09155558458053292, 81.93586902018296314 ) ) ;
#58292 = AXIS2_PLACEMENT_3D ( 'NONE', #44905, #59426, #51711 ) ;
#58293 = CARTESIAN_POINT ( 'NONE',  ( 90.44969454456415292, -55.86395651782494554, 239.5838068554169809 ) ) ;
#58295 = FACE_OUTER_BOUND ( 'NONE', #52677, .T. ) ;
#58294 = CARTESIAN_POINT ( 'NONE',  ( 101.0525363619397581, -44.44280425155404401, 228.0499109901959400 ) ) ;
#58296 = DIRECTION ( 'NONE',  ( 0.000000000000000000, 1.000000000000000000, 0.000000000000000000 ) ) ;
#58297 = DIRECTION ( 'NONE',  ( -0.000000000000000000, 1.000000000000000000, 0.000000000000000000 ) ) ;
#58298 = ADVANCED_FACE ( 'NONE', ( #32234 ), #50055, .F. ) ;
#58299 = AXIS2_PLACEMENT_3D ( 'NONE', #77584, #56211, #63046 ) ;
#58300 = CARTESIAN_POINT ( 'NONE',  ( 118.5560669097358470, 69.84937538953987257, -0.8299548590967218420 ) ) ;
#58301 = CARTESIAN_POINT ( 'NONE',  ( -544.5124999999999318, 53.97500000000000142, 87.37599999999999056 ) ) ;
#58302 = LINE ( 'NONE', #86475, #56516 ) ;
#58303 = EDGE_CURVE ( 'NONE', #11327, #35298, #66054, .T. ) ;
#58304 = DIRECTION ( 'NONE',  ( 0.000000000000000000, 0.000000000000000000, 1.000000000000000000 ) ) ;
#58305 = CARTESIAN_POINT ( 'NONE',  ( 99.43809884604145566, -27.69271567064627604, 150.6356252759109680 ) ) ;
#58306 = EDGE_CURVE ( 'NONE', #76939, #54739, #5892, .T. ) ;
#58307 = ORIENTED_EDGE ( 'NONE', *, *, #18617, .F. ) ;
#58308 = AXIS2_PLACEMENT_3D ( 'NONE', #85543, #85985, #23322 ) ;
#58309 = ORIENTED_EDGE ( 'NONE', *, *, #46314, .T. ) ;
#58310 = EDGE_CURVE ( 'NONE', #7448, #57293, #61283, .T. ) ;
#58311 = DIRECTION ( 'NONE',  ( -0.000000000000000000, -0.000000000000000000, 1.000000000000000000 ) ) ;
#58312 = DIRECTION ( 'NONE',  ( 1.000000000000000078E-15, 0.000000000000000000, 1.000000000000000000 ) ) ;
#58313 = CARTESIAN_POINT ( 'NONE',  ( 98.30753418069124905, -41.72887547393442986, 77.73979194101322321 ) ) ;
#58314 = CARTESIAN_POINT ( 'NONE',  ( 97.82501843714776157, -40.54985425570063029, 102.6384157449830923 ) ) ;
#58315 = CARTESIAN_POINT ( 'NONE',  ( 113.6834210241909346, -31.15118039646248249, 222.1899951314959480 ) ) ;
#58316 = PLANE ( 'NONE',  #53768 ) ;
#58317 = CARTESIAN_POINT ( 'NONE',  ( 117.4265927121613089, -30.97543824232759135, 179.2299109901959753 ) ) ;
#58318 = FACE_OUTER_BOUND ( 'NONE', #76800, .T. ) ;
#58319 = VERTEX_POINT ( 'NONE', #54442 ) ;
#58321 = ORIENTED_EDGE ( 'NONE', *, *, #77664, .F. ) ;
#58320 = ORIENTED_EDGE ( 'NONE', *, *, #77237, .F. ) ;
#58322 = EDGE_CURVE ( 'NONE', #89263, #20045, #24988, .T. ) ;
#58323 = CARTESIAN_POINT ( 'NONE',  ( -4.085245964383497075, 70.51776014978250373, 118.4862668242151358 ) ) ;
#58324 = DIRECTION ( 'NONE',  ( -2.900000000000000265E-14, 2.000000000000000155E-15, -1.000000000000000000 ) ) ;
#58325 = CARTESIAN_POINT ( 'NONE',  ( 131.6729728819624370, -35.37149612623981909, 7.198162082935252393 ) ) ;
#58326 = CARTESIAN_POINT ( 'NONE',  ( 98.67113652751868358, -38.83122756767168227, 14.35189989340096517 ) ) ;
#58327 = CARTESIAN_POINT ( 'NONE',  ( 63.06670390244699576, -67.87844715994098976, 155.2178068554179902 ) ) ;
#58328 = ORIENTED_EDGE ( 'NONE', *, *, #30229, .T. ) ;
#58329 = CIRCLE ( 'NONE', #22049, 1.000000000000000888 ) ;
#58330 = CARTESIAN_POINT ( 'NONE',  ( 116.7260014990201284, -39.09146540103774470, 9.635625275910941312 ) ) ;
#58331 = CARTESIAN_POINT ( 'NONE',  ( -126.6753767262755446, 61.56490666960836222, 31.59592044441793135 ) ) ;
#58332 = ORIENTED_EDGE ( 'NONE', *, *, #12279, .F. ) ;
#58333 = ORIENTED_EDGE ( 'NONE', *, *, #50924, .T. ) ;
#58334 = VECTOR ( 'NONE', #28722, 1000.000000000000000 ) ;
#58335 = CARTESIAN_POINT ( 'NONE',  ( 107.0664832912739968, -36.72944715994100306, 287.6356252759109680 ) ) ;
#58336 = ORIENTED_EDGE ( 'NONE', *, *, #87246, .T. ) ;
#58337 = ORIENTED_EDGE ( 'NONE', *, *, #49776, .T. ) ;
#58338 = CARTESIAN_POINT ( 'NONE',  ( 105.6358988306284346, -28.30874812457275524, 14.63241982807694797 ) ) ;
#58339 = CARTESIAN_POINT ( 'NONE',  ( 105.7175586466805157, -24.93052779236126781, 160.1670538473389627 ) ) ;
#58340 = CARTESIAN_POINT ( 'NONE',  ( 114.1602155298370036, -45.17592836263241196, 148.1203871806719405 ) ) ;
#58341 = CARTESIAN_POINT ( 'NONE',  ( -33.98325472291465132, 8.255000000000000782, -3.174999999999764899 ) ) ;
#58342 = CARTESIAN_POINT ( 'NONE',  ( 96.26801084314395496, -34.37000373589627600, 252.1432443235302969 ) ) ;
#58343 = CARTESIAN_POINT ( 'NONE',  ( 177.4809174648215162, -48.32844715993478246, 180.4678068554150059 ) ) ;
#58344 = CARTESIAN_POINT ( 'NONE',  ( 29.77381068363482441, -48.62134037875501491, 249.9678068554150059 ) ) ;
#58345 = CARTESIAN_POINT ( 'NONE',  ( -129.9368274816650626, 82.54999999999999716, -12.70000000000045404 ) ) ;
#58346 = ORIENTED_EDGE ( 'NONE', *, *, #76280, .F. ) ;
#58347 = AXIS2_PLACEMENT_3D ( 'NONE', #20773, #325, #28022 ) ;
#58348 = ORIENTED_EDGE ( 'NONE', *, *, #74697, .F. ) ;
#58349 = EDGE_CURVE ( 'NONE', #16953, #34506, #67442, .T. ) ;
#58350 = AXIS2_PLACEMENT_3D ( 'NONE', #68065, #39895, #39457 ) ;
#58351 = CARTESIAN_POINT ( 'NONE',  ( 98.39836552415940218, -29.79571670633027836, 195.7775300378159784 ) ) ;
#58352 = VERTEX_POINT ( 'NONE', #32687 ) ;
#58353 = CARTESIAN_POINT ( 'NONE',  ( 112.7802237386950992, -45.44955040250216172, 178.0384824187679556 ) ) ;
#58354 = DIRECTION ( 'NONE',  ( 0.000000000000000000, 0.000000000000000000, -1.000000000000000000 ) ) ;
#58355 = EDGE_CURVE ( 'NONE', #52044, #31278, #25879, .T. ) ;
#58356 = CYLINDRICAL_SURFACE ( 'NONE', #66753, 0.5000000000000007772 ) ;
#58357 = DIRECTION ( 'NONE',  ( 1.000000000000000078E-15, 1.000000000000000083E-30, -1.000000000000000000 ) ) ;
#58360 = CARTESIAN_POINT ( 'NONE',  ( 101.0991643652557599, -45.25116564454916102, 278.0899109901965858 ) ) ;
#58359 = DIRECTION ( 'NONE',  ( 1.000000000000000078E-15, 0.000000000000000000, -1.000000000000000000 ) ) ;
#58358 = CARTESIAN_POINT ( 'NONE',  ( 129.8079539024480198, -42.97311385574000298, 231.5838068554170093 ) ) ;
#58361 = LINE ( 'NONE', #58791, #61156 ) ;
#58362 = CYLINDRICAL_SURFACE ( 'NONE', #52559, 14.00000000000000888 ) ;
#58363 = VECTOR ( 'NONE', #8443, 1000.000000000000000 ) ;
#58364 = CARTESIAN_POINT ( 'NONE',  ( 115.8228748906924750, -31.72559827118475440, 270.2397737374858480 ) ) ;
#58365 = DIRECTION ( 'NONE',  ( 0.000000000000000000, 1.000000000000000000, 1.809101308280369915E-15 ) ) ;
#58366 = FACE_OUTER_BOUND ( 'NONE', #53398, .T. ) ;
#58367 = LINE ( 'NONE', #11104, #59339 ) ;
#58369 = EDGE_LOOP ( 'NONE', ( #13378, #14400, #61386, #7399, #69714 ) ) ;
#58368 = CARTESIAN_POINT ( 'NONE',  ( 112.9239127876531938, -29.01757442955986477, 195.5838068554168387 ) ) ;
#58370 = DIRECTION ( 'NONE',  ( 0.000000000000000000, -1.000000000000000000, 0.000000000000000000 ) ) ;
#58371 = CARTESIAN_POINT ( 'NONE',  ( 98.64801509901850807, -30.48302769619336416, 180.8184824187679567 ) ) ;
#58372 = CARTESIAN_POINT ( 'NONE',  ( 115.0226255289246922, -43.52070134976005988, 59.26419670448196086 ) ) ;
#58373 = CARTESIAN_POINT ( 'NONE',  ( 101.6280127420326522, -45.67461444920139257, 243.1413395616249886 ) ) ;
#58374 = DIRECTION ( 'NONE',  ( -0.7071067811567173234, 0.7071067812163779331, 0.000000000000000000 ) ) ;
#58375 = LINE ( 'NONE', #4758, #28650 ) ;
#58377 = CARTESIAN_POINT ( 'NONE',  ( 97.83668494123075732, -40.57802212005890397, 37.64055050525384161 ) ) ;
#58376 = DIRECTION ( 'NONE',  ( 0.000000000000000000, 0.000000000000000000, -1.000000000000000000 ) ) ;
#58378 = DIRECTION ( 'NONE',  ( 1.000000000000000000, 0.000000000000000000, 0.000000000000000000 ) ) ;
#58379 = CARTESIAN_POINT ( 'NONE',  ( 25.56670390244797275, -58.35344715994099829, 137.2178068554150059 ) ) ;
#58380 = ORIENTED_EDGE ( 'NONE', *, *, #16815, .T. ) ;
#58381 = DIRECTION ( 'NONE',  ( 1.000000000000000000, 0.000000000000000000, -0.000000000000000000 ) ) ;
#58382 = EDGE_CURVE ( 'NONE', #83503, #56235, #64545, .T. ) ;
#58383 = VERTEX_POINT ( 'NONE', #55347 ) ;
#58384 = VERTEX_POINT ( 'NONE', #48979 ) ;
#58385 = CARTESIAN_POINT ( 'NONE',  ( 111.5299334411454311, -29.44702005892069607, 94.06099125664896121 ) ) ;
#58387 = ORIENTED_EDGE ( 'NONE', *, *, #30619, .F. ) ;
#58386 = CARTESIAN_POINT ( 'NONE',  ( 30.48091746481741637, -48.32844715994156815, 180.4678068554150911 ) ) ;
#58388 = VECTOR ( 'NONE', #87555, 1000.000000000000000 ) ;
#58389 = CARTESIAN_POINT ( 'NONE',  ( 106.6611865629619160, -26.33404432545466634, 81.10705384733896040 ) ) ;
#58390 = DIRECTION ( 'NONE',  ( 1.000000000000000000, 3.999999999999999995E-14, 1.000000000000000078E-15 ) ) ;
#58391 = CARTESIAN_POINT ( 'NONE',  ( 162.7131505118549342, -33.70561438051439040, 117.4678068554150485 ) ) ;
#58392 = CARTESIAN_POINT ( 'NONE',  ( 113.2454987028225730, -28.75867294873037494, 175.5522919420834853 ) ) ;
#58393 = CARTESIAN_POINT ( 'NONE',  ( 100.2135729635196242, -43.75450166755856429, 21.96133956162593748 ) ) ;
#58394 = ORIENTED_EDGE ( 'NONE', *, *, #50901, .F. ) ;
#58395 = VERTEX_POINT ( 'NONE', #27669 ) ;
#58396 = VERTEX_POINT ( 'NONE', #77171 ) ;
#58397 = CIRCLE ( 'NONE', #55511, 30.99999999999998579 ) ;
#58398 = CARTESIAN_POINT ( 'NONE',  ( 172.5667039024478129, -36.32844715993500273, 313.9678068554149490 ) ) ;
#58399 = LINE ( 'NONE', #66553, #15737 ) ;
#58400 = DIRECTION ( 'NONE',  ( 0.000000000000000000, 0.000000000000000000, 1.000000000000000000 ) ) ;
#58401 = CARTESIAN_POINT ( 'NONE',  ( 135.0664832912729878, -36.72944715994189835, 361.9756252759079871 ) ) ;
#58402 = CARTESIAN_POINT ( 'NONE',  ( 32.09598329127609873, -23.42844715994129956, 193.9678068554150911 ) ) ;
#58403 = CARTESIAN_POINT ( 'NONE',  ( 97.12551982384144367, -37.99658701952105133, 52.42742285273963887 ) ) ;
#58404 = PLANE ( 'NONE',  #11169 ) ;
#58405 = CARTESIAN_POINT ( 'NONE',  ( 75.24778849303555717, 87.79588542099537563, 91.61507027739615694 ) ) ;
#58406 = CARTESIAN_POINT ( 'NONE',  ( 116.3681181406587370, -31.99193570193495262, 44.20133956162491984 ) ) ;
#58407 = EDGE_CURVE ( 'NONE', #45672, #19975, #82659, .T. ) ;
#58409 = ORIENTED_EDGE ( 'NONE', *, *, #80391, .T. ) ;
#58408 = AXIS2_PLACEMENT_3D ( 'NONE', #66911, #68269, #39201 ) ;
#58410 = CARTESIAN_POINT ( 'NONE',  ( 6.349842397765909752, 93.55646220832403515, 130.4020064843513467 ) ) ;
#58411 = CARTESIAN_POINT ( 'NONE',  ( 126.8302186627767725, 48.26449426118261243, 30.96720769570602627 ) ) ;
#58412 = CARTESIAN_POINT ( 'NONE',  ( 80.80881079632696640, -112.6232539059703726, 250.2178068554180470 ) ) ;
#58413 = CARTESIAN_POINT ( 'NONE',  ( 111.7725766154891431, -30.05993356141850015, 127.4052332267339693 ) ) ;
#58414 = VECTOR ( 'NONE', #699, 1000.000000000000000 ) ;
#58415 = CARTESIAN_POINT ( 'NONE',  ( 97.39148490005503334, -39.27924475881587085, 96.53152011028632273 ) ) ;
#58416 = AXIS2_PLACEMENT_3D ( 'NONE', #161, #49638, #29223 ) ;
#58417 = DIRECTION ( 'NONE',  ( 0.000000000000000000, 0.000000000000000000, 1.000000000000000000 ) ) ;
#58418 = ORIENTED_EDGE ( 'NONE', *, *, #50292, .T. ) ;
#58419 = ORIENTED_EDGE ( 'NONE', *, *, #58147, .F. ) ;
#58420 = ADVANCED_FACE ( 'NONE', ( #20416 ), #14948, .F. ) ;
#58421 = LINE ( 'NONE', #80230, #19180 ) ;
#58422 = VERTEX_POINT ( 'NONE', #89918 ) ;
#58423 = ORIENTED_EDGE ( 'NONE', *, *, #85310, .F. ) ;
#58424 = EDGE_CURVE ( 'NONE', #56522, #65097, #55783, .T. ) ;
#58425 = CARTESIAN_POINT ( 'NONE',  ( 115.8619398590553260, -35.64860379657582712, 190.3558690201829506 ) ) ;
#58426 = LINE ( 'NONE', #51601, #10465 ) ;
#58427 = CARTESIAN_POINT ( 'NONE',  ( 114.5277216628477248, -29.41153075798395733, 145.4441967044819819 ) ) ;
#58428 = CARTESIAN_POINT ( 'NONE',  ( 69.63919639214307722, 92.07499999999998863, -53.63573739454432854 ) ) ;
#58429 = CARTESIAN_POINT ( 'NONE',  ( 110.8617057341842695, -45.98127435360438398, 17.88624725593324882 ) ) ;
#58430 = ORIENTED_EDGE ( 'NONE', *, *, #21504, .T. ) ;
#58431 = ORIENTED_EDGE ( 'NONE', *, *, #66709, .T. ) ;
#58432 = VERTEX_POINT ( 'NONE', #48087 ) ;
#58433 = CARTESIAN_POINT ( 'NONE',  ( 100.2649065926023297, -31.37786052998579223, 198.6261856076869776 ) ) ;
#58435 = CARTESIAN_POINT ( 'NONE',  ( 103.4695482323410118, -25.41149354249025549, 55.32133956162594046 ) ) ;
#58434 = CIRCLE ( 'NONE', #57018, 2.030000000001807248 ) ;
#58436 = EDGE_LOOP ( 'NONE', ( #50365, #78962, #53109, #83694, #17272, #62479 ) ) ;
#58437 = CARTESIAN_POINT ( 'NONE',  ( 96.21590750668994474, -38.71157422997263353, 51.48229194257797303 ) ) ;
#58438 = LINE ( 'NONE', #87500, #84898 ) ;
#58439 = DIRECTION ( 'NONE',  ( 1.000000000000000000, -6.745093096447288888E-17, 0.000000000000000000 ) ) ;
#58440 = DIRECTION ( 'NONE',  ( -4.299999999999999979E-14, 1.000000000000000000, 0.000000000000000000 ) ) ;
#58441 = CARTESIAN_POINT ( 'NONE',  ( 108.6487146914112287, -25.79677769486274386, 145.9737205140069420 ) ) ;
#58442 = CARTESIAN_POINT ( 'NONE',  ( 0.000000000000000000, 61.59999999999999432, 0.000000000000000000 ) ) ;
#58443 = ORIENTED_EDGE ( 'NONE', *, *, #1142, .T. ) ;
#58444 = DIRECTION ( 'NONE',  ( 1.000000000000000078E-15, -1.000000000000000000, 0.000000000000000000 ) ) ;
#58445 = VERTEX_POINT ( 'NONE', #54894 ) ;
#58446 = CARTESIAN_POINT ( 'NONE',  ( 97.81085527707094229, -40.51777768585955641, 251.6359959587111064 ) ) ;
#58447 = EDGE_LOOP ( 'NONE', ( #57718, #37273 ) ) ;
#58448 = ORIENTED_EDGE ( 'NONE', *, *, #5898, .F. ) ;
#58449 = AXIS2_PLACEMENT_3D ( 'NONE', #54381, #48029, #75763 ) ;
#58450 = CARTESIAN_POINT ( 'NONE',  ( 70.63919639214310564, 49.07499999999999574, -33.74458626278666884 ) ) ;
#58451 = DIRECTION ( 'NONE',  ( 0.000000000000000000, 1.000000000000000000, 0.000000000000000000 ) ) ;
#58452 = CARTESIAN_POINT ( 'NONE',  ( 103.5987056385471448, -46.56110768157568458, 57.30705384733997221 ) ) ;
#58453 = DIRECTION ( 'NONE',  ( 1.000000000000000078E-15, 9.367723249499513438E-31, -1.000000000000000000 ) ) ;
#58454 = EDGE_CURVE ( 'NONE', #59703, #71348, #28552, .T. ) ;
#58455 = DIRECTION ( 'NONE',  ( 1.000000000000000078E-15, -1.000000000000000083E-30, -1.000000000000000000 ) ) ;
#58456 = CARTESIAN_POINT ( 'NONE',  ( 73.06670390244801183, -48.82844715994099971, 10.91780685541510110 ) ) ;
#58457 = CARTESIAN_POINT ( 'NONE',  ( 115.0479362680066515, -42.38275094372912122, 53.33562527591095659 ) ) ;
#58459 = CARTESIAN_POINT ( 'NONE',  ( 104.4591861284130232, -26.65816784528765382, 196.2784824187679362 ) ) ;
#58458 = DIRECTION ( 'NONE',  ( 0.000000000000000000, 0.000000000000000000, -1.000000000000000000 ) ) ;
#58460 = CARTESIAN_POINT ( 'NONE',  ( 106.5207973735215319, -24.24134984979954410, 321.1698005525342978 ) ) ;
#58461 = DIRECTION ( 'NONE',  ( 0.000000000000000000, 0.000000000000000000, -1.000000000000000000 ) ) ;
#58462 = EDGE_LOOP ( 'NONE', ( #36330, #56723, #57752, #42898, #63016, #51877 ) ) ;
#58463 = DIRECTION ( 'NONE',  ( -1.000000000000000000, -3.999999999999999995E-14, -1.000000000000000078E-15 ) ) ;
#58464 = DIRECTION ( 'NONE',  ( 1.000000000000000000, 0.000000000000000000, -1.821231995776179916E-16 ) ) ;
#58465 = CYLINDRICAL_SURFACE ( 'NONE', #71997, 3.000000000000002665 ) ;
#58466 = CARTESIAN_POINT ( 'NONE',  ( 29.56670390244797630, -48.82844715994099971, 10.91780685541479734 ) ) ;
#58468 = ORIENTED_EDGE ( 'NONE', *, *, #52645, .F. ) ;
#58467 = CARTESIAN_POINT ( 'NONE',  ( 98.34291691341793751, -29.86560907334282788, 200.8080062282919869 ) ) ;
#58469 = LINE ( 'NONE', #45715, #13173 ) ;
#58470 = CARTESIAN_POINT ( 'NONE',  ( 118.1305967499472160, -36.20925573564677791, 264.8518157521014587 ) ) ;
#58471 = CARTESIAN_POINT ( 'NONE',  ( 98.16534761909046836, -43.36023007783336425, 107.8480062282919647 ) ) ;
#58472 = CARTESIAN_POINT ( 'NONE',  ( 97.07216957362197718, -35.37749098132034931, 252.2221255759655207 ) ) ;
#58473 = CARTESIAN_POINT ( 'NONE',  ( 100.9534681770906275, -28.70796848357117881, 191.5938865662113244 ) ) ;
#58474 = PLANE ( 'NONE',  #35545 ) ;
#58475 = CARTESIAN_POINT ( 'NONE',  ( 147.0667039024469886, -67.87844715994090450, 222.2178068554179902 ) ) ;
#58476 = ORIENTED_EDGE ( 'NONE', *, *, #63334, .T. ) ;
#58477 = CIRCLE ( 'NONE', #75867, 2.116999999999993776 ) ;
#58478 = EDGE_CURVE ( 'NONE', #69697, #80300, #42617, .T. ) ;
#58479 = VECTOR ( 'NONE', #34089, 1000.000000000000000 ) ;
#58480 = VERTEX_POINT ( 'NONE', #7675 ) ;
#58481 = ORIENTED_EDGE ( 'NONE', *, *, #29183, .F. ) ;
#58482 = AXIS2_PLACEMENT_3D ( 'NONE', #12189, #5832, #60314 ) ;
#58483 = ADVANCED_FACE ( 'NONE', ( #28100 ), #20854, .T. ) ;
#58484 = ORIENTED_EDGE ( 'NONE', *, *, #53482, .F. ) ;
#58485 = DIRECTION ( 'NONE',  ( 0.7759704746411385523, -0.6307692307692301936, 0.000000000000000000 ) ) ;
#58486 = CARTESIAN_POINT ( 'NONE',  ( 111.7390528236686436, -27.41013440965690862, 275.7070538473395800 ) ) ;
#58487 = CARTESIAN_POINT ( 'NONE',  ( 118.7735074478422348, -37.73348171986721411, 298.1356252759109680 ) ) ;
#58488 = DIRECTION ( 'NONE',  ( 3.386875084296745512E-15, 0.000000000000000000, -1.000000000000000000 ) ) ;
#58489 = EDGE_CURVE ( 'NONE', #48583, #76359, #42785, .T. ) ;
#58490 = ADVANCED_FACE ( 'NONE', ( #14500 ), #83101, .T. ) ;
#58492 = CARTESIAN_POINT ( 'NONE',  ( 75.85240403722289670, 75.84278307195161517, 91.11526841082653050 ) ) ;
#58491 = CARTESIAN_POINT ( 'NONE',  ( 141.0664832912740394, -46.72944715994099596, 14.67562527591100441 ) ) ;
#58493 = DIRECTION ( 'NONE',  ( 0.000000000000000000, 0.000000000000000000, 1.000000000000000000 ) ) ;
#58494 = CARTESIAN_POINT ( 'NONE',  ( 113.8843833678302389, -31.58431642611541434, 218.7638483995049796 ) ) ;
#58495 = VERTEX_POINT ( 'NONE', #70804 ) ;
#58496 = EDGE_CURVE ( 'NONE', #78823, #71994, #26857, .T. ) ;
#58497 = EDGE_LOOP ( 'NONE', ( #54245, #52031, #55270, #70731, #86151 ) ) ;
#58498 = VERTEX_POINT ( 'NONE', #83993 ) ;
#58499 = FACE_BOUND ( 'NONE', #4502, .T. ) ;
#58500 = AXIS2_PLACEMENT_3D ( 'NONE', #45606, #11111, #46058 ) ;
#58502 = EDGE_CURVE ( 'NONE', #39116, #5214, #70349, .T. ) ;
#58501 = CARTESIAN_POINT ( 'NONE',  ( 98.54782206469626260, -41.97725611773798704, 181.7658570118601915 ) ) ;
#58503 = CARTESIAN_POINT ( 'NONE',  ( 117.4251315444614789, -36.24242395571268816, 264.8518157521010608 ) ) ;
#58504 = CARTESIAN_POINT ( 'NONE',  ( 117.8738102209306362, 82.54999999999999716, 12.70000000000123386 ) ) ;
#58505 = AXIS2_PLACEMENT_3D ( 'NONE', #27335, #20538, #62747 ) ;
#58506 = FACE_OUTER_BOUND ( 'NONE', #8949, .T. ) ;
#58507 = ADVANCED_FACE ( 'NONE', ( #36279 ), #83535, .F. ) ;
#58508 = DIRECTION ( 'NONE',  ( 1.000000000000000000, -0.000000000000000000, 0.000000000000000000 ) ) ;
#58509 = ORIENTED_EDGE ( 'NONE', *, *, #77805, .F. ) ;
#58510 = CARTESIAN_POINT ( 'NONE',  ( 105.0948228932018083, -26.91303006142818077, 56.23424190894431973 ) ) ;
#58511 = ORIENTED_EDGE ( 'NONE', *, *, #4579, .F. ) ;
#58512 = DIRECTION ( 'NONE',  ( 0.000000000000000000, 1.000000000000000000, 0.000000000000000000 ) ) ;
#58513 = CARTESIAN_POINT ( 'NONE',  ( 99.24357903948710202, -34.39880452655780374, 28.91380465530596311 ) ) ;
#58514 = DIRECTION ( 'NONE',  ( 0.000000000000000000, 0.000000000000000000, -1.000000000000000000 ) ) ;
#58515 = CARTESIAN_POINT ( 'NONE',  ( 162.9033555647770015, -33.89581943344391135, -5.074374724088000832 ) ) ;
#58516 = CYLINDRICAL_SURFACE ( 'NONE', #60428, 0.5000000000000104361 ) ;
#58517 = ORIENTED_EDGE ( 'NONE', *, *, #65788, .T. ) ;
#58518 = DIRECTION ( 'NONE',  ( -0.8660254037844392627, 0.4999999999999990008, -1.549999999999999706E-14 ) ) ;
#58519 = EDGE_CURVE ( 'NONE', #35863, #15323, #27214, .T. ) ;
#58520 = LINE ( 'NONE', #86247, #6371 ) ;
#58521 = ORIENTED_EDGE ( 'NONE', *, *, #12811, .T. ) ;
#58522 = CARTESIAN_POINT ( 'NONE',  ( 115.2672674329477900, -44.14067019768319966, 83.25372051400698581 ) ) ;
#58523 = ORIENTED_EDGE ( 'NONE', *, *, #37615, .F. ) ;
#58524 = EDGE_CURVE ( 'NONE', #12394, #62096, #81220, .T. ) ;
#58525 = CARTESIAN_POINT ( 'NONE',  ( 106.6171843113225606, -27.68451483556421522, 44.55051506617196821 ) ) ;
#58526 = ADVANCED_FACE ( 'NONE', ( #85787 ), #16729, .T. ) ;
#58527 = CARTESIAN_POINT ( 'NONE',  ( 130.5667039024480118, -37.98819715994094537, 218.8274735512161158 ) ) ;
#58528 = CARTESIAN_POINT ( 'NONE',  ( 115.2337707449818680, -33.21411712777100433, 75.58158330589692753 ) ) ;
#58529 = CARTESIAN_POINT ( 'NONE',  ( 23.75871628398702384, 82.54999999999999716, 298.1325000000000500 ) ) ;
#58530 = CARTESIAN_POINT ( 'NONE',  ( 41.56648329127381203, -27.82844715994070484, 21.92562527591199739 ) ) ;
#58531 = EDGE_CURVE ( 'NONE', #34986, #33347, #74716, .T. ) ;
#58532 = CARTESIAN_POINT ( 'NONE',  ( 99.96594057013267332, -44.39231554709003547, 42.98133956162492098 ) ) ;
#58533 = LINE ( 'NONE', #9511, #74257 ) ;
#58534 = VERTEX_POINT ( 'NONE', #79869 ) ;
#58535 = CIRCLE ( 'NONE', #41163, 4.500000000000003553 ) ;
#58536 = LINE ( 'NONE', #64476, #31382 ) ;
#58537 = ORIENTED_EDGE ( 'NONE', *, *, #35830, .T. ) ;
#58538 = CARTESIAN_POINT ( 'NONE',  ( 102.6793653923444651, -46.92506852294805952, 133.2651490854349561 ) ) ;
#58539 = DIRECTION ( 'NONE',  ( 0.000000000000000000, 0.000000000000000000, -1.000000000000000000 ) ) ;
#58540 = CIRCLE ( 'NONE', #4870, 2.517500000000005844 ) ;
#58541 = VERTEX_POINT ( 'NONE', #29465 ) ;
#58542 = EDGE_LOOP ( 'NONE', ( #71097, #35529, #23566, #57598 ) ) ;
#58543 = CYLINDRICAL_SURFACE ( 'NONE', #39114, 5.041900000000000048 ) ;
#58544 = DIRECTION ( 'NONE',  ( 1.000000000000000000, 3.999999999999999995E-14, 1.000000000000000078E-15 ) ) ;
#58545 = CARTESIAN_POINT ( 'NONE',  ( 116.8310051202518309, -36.16593252570070405, 228.8727681330539667 ) ) ;
#58546 = CARTESIAN_POINT ( 'NONE',  ( 145.0753911212546825, -139.6697599411332078, 245.6076672521240027 ) ) ;
#58547 = CYLINDRICAL_SURFACE ( 'NONE', #37468, 1.000000000000000888 ) ;
#58548 = CARTESIAN_POINT ( 'NONE',  ( 117.9887704088505274, -38.42580343310776669, 64.69181575210097890 ) ) ;
#58549 = CARTESIAN_POINT ( 'NONE',  ( -48.02966122971776741, 93.07500000000001705, 75.53254848357481421 ) ) ;
#58550 = VERTEX_POINT ( 'NONE', #57147 ) ;
#58551 = CARTESIAN_POINT ( 'NONE',  ( 112.7461304981565036, -28.44177779729672295, 170.5981271715937169 ) ) ;
#58552 = LINE ( 'NONE', #65387, #21584 ) ;
#58553 = EDGE_LOOP ( 'NONE', ( #13415, #76912, #54278, #17951 ) ) ;
#58554 = AXIS2_PLACEMENT_3D ( 'NONE', #81682, #6699, #334 ) ;
#58555 = PLANE ( 'NONE',  #2510 ) ;
#58556 = VECTOR ( 'NONE', #47981, 1000.000000000000000 ) ;
#58557 = LINE ( 'NONE', #59447, #49848 ) ;
#58558 = CARTESIAN_POINT ( 'NONE',  ( 96.70388795518319114, -35.81005419191407668, 231.2556252759109725 ) ) ;
#58559 = DIRECTION ( 'NONE',  ( 0.6757246285173468259, 6.757246285173467929E-16, 0.7371541402007408816 ) ) ;
#58560 = CYLINDRICAL_SURFACE ( 'NONE', #2612, 9.999999999999998224 ) ;
#58561 = CARTESIAN_POINT ( 'NONE',  ( 115.4795240695424923, -35.25402295475319647, 243.3867055423619661 ) ) ;
#58563 = CARTESIAN_POINT ( 'NONE',  ( 101.1541078795468707, -28.12664281037979208, 46.55562527591094835 ) ) ;
#58562 = CARTESIAN_POINT ( 'NONE',  ( -7.205548786489490269E-13, 101.5999999999999943, 103.1875000000000000 ) ) ;
#58564 = CARTESIAN_POINT ( 'NONE',  ( 110.5173296318792069, 62.69970716989340076, 69.50396515567824451 ) ) ;
#58565 = CARTESIAN_POINT ( 'NONE',  ( 102.2925893952339749, -26.70832846991215703, 140.4422919425769578 ) ) ;
#58566 = ORIENTED_EDGE ( 'NONE', *, *, #53557, .T. ) ;
#58567 = FACE_OUTER_BOUND ( 'NONE', #26498, .T. ) ;
#58568 = VERTEX_POINT ( 'NONE', #22662 ) ;
#58569 = CARTESIAN_POINT ( 'NONE',  ( 63.56670390244714497, -40.82844715994014706, 129.9678068554150911 ) ) ;
#58570 = CIRCLE ( 'NONE', #48365, 2.500000000000002220 ) ;
#58571 = CARTESIAN_POINT ( 'NONE',  ( 160.7738106836350482, -48.62134037874900372, 180.4678068554150059 ) ) ;
#58572 = FACE_OUTER_BOUND ( 'NONE', #2826, .T. ) ;
#58573 = ORIENTED_EDGE ( 'NONE', *, *, #83854, .F. ) ;
#58574 = CARTESIAN_POINT ( 'NONE',  ( 76.20505178924389611, 127.0000000000000000, -76.20505178924359768 ) ) ;
#58575 = VERTEX_POINT ( 'NONE', #50336 ) ;
#58576 = CARTESIAN_POINT ( 'NONE',  ( 164.9212702847350158, -29.73316016639540749, -5.074374724088000832 ) ) ;
#58577 = LINE ( 'NONE', #44950, #62120 ) ;
#58578 = CARTESIAN_POINT ( 'NONE',  ( 120.2221484686747317, -96.68314769832106492, -11.78219314458223188 ) ) ;
#58579 = ORIENTED_EDGE ( 'NONE', *, *, #56966, .T. ) ;
#58580 = CARTESIAN_POINT ( 'NONE',  ( 97.52207955639441650, -32.48083311392049666, 100.9927681330539713 ) ) ;
#58581 = EDGE_CURVE ( 'NONE', #43342, #19136, #78077, .T. ) ;
#58582 = DIRECTION ( 'NONE',  ( 0.000000000000000000, 0.000000000000000000, -1.000000000000000000 ) ) ;
#58583 = PLANE ( 'NONE',  #49551 ) ;
#58584 = EDGE_CURVE ( 'NONE', #18085, #37957, #9463, .T. ) ;
#58585 = CARTESIAN_POINT ( 'NONE',  ( -100.8961411191535973, 120.6499999999999915, -3.968750000001104894 ) ) ;
#58586 = ORIENTED_EDGE ( 'NONE', *, *, #44504, .F. ) ;
#58587 = ADVANCED_FACE ( 'NONE', ( #78529 ), #53089, .F. ) ;
#58588 = LINE ( 'NONE', #45840, #63485 ) ;
#58589 = DIRECTION ( 'NONE',  ( 0.9963424814100680926, -0.08544974978095730422, 0.000000000000000000 ) ) ;
#58590 = CARTESIAN_POINT ( 'NONE',  ( 97.81170668756638520, -40.51744870325870806, 152.6352702516163902 ) ) ;
#58591 = EDGE_CURVE ( 'NONE', #52987, #46735, #57259, .T. ) ;
#58592 = EDGE_CURVE ( 'NONE', #85819, #65405, #38450, .T. ) ;
#58594 = FACE_OUTER_BOUND ( 'NONE', #88068, .T. ) ;
#58593 = CARTESIAN_POINT ( 'NONE',  ( 107.0664832912739399, -36.72944715994095333, 294.6356252759106837 ) ) ;
#58595 = DIRECTION ( 'NONE',  ( 0.000000000000000000, 0.000000000000000000, 1.000000000000000000 ) ) ;
#58596 = EDGE_CURVE ( 'NONE', #22318, #78255, #38944, .T. ) ;
#58597 = ORIENTED_EDGE ( 'NONE', *, *, #44822, .T. ) ;
#58598 = B_SPLINE_CURVE_WITH_KNOTS ( 'NONE', 3,
 ( #54786, #13484, #40281, #54335, #68452, #34360, #60717, #53888, #47081, #82991 ),
 .UNSPECIFIED., .F., .F.,
 ( 4, 2, 2, 2, 4 ),
 ( 0.000000000000000000, 0.2500000000000008327, 0.3750000000000011102, 0.5000000000000014433, 1.000000000000000000 ),
 .UNSPECIFIED. ) ;
#58599 = AXIS2_PLACEMENT_3D ( 'NONE', #27842, #48264, #53396 ) ;
#58601 = ADVANCED_FACE ( 'NONE', ( #81655 ), #60722, .T. ) ;
#58600 = CARTESIAN_POINT ( 'NONE',  ( 97.81168736999980240, -40.51740164104307240, 32.63591986563997693 ) ) ;
#58602 = CARTESIAN_POINT ( 'NONE',  ( 98.71823956546970180, -31.63334453281608916, 166.8899109901959719 ) ) ;
#58604 = ORIENTED_EDGE ( 'NONE', *, *, #76253, .T. ) ;
#58603 = DIRECTION ( 'NONE',  ( 1.000000000000000078E-15, 1.000000000000000083E-30, -1.000000000000000000 ) ) ;
#58605 = CARTESIAN_POINT ( 'NONE',  ( 100.8224265971273326, -29.20115443902030705, 36.62705384733894221 ) ) ;
#58606 = CARTESIAN_POINT ( 'NONE',  ( 192.5667039024474434, -23.42844715993433624, 180.4678068554150343 ) ) ;
#58607 = CARTESIAN_POINT ( 'NONE',  ( 110.7653435595065901, 44.45000000000000284, 69.10794311903988785 ) ) ;
#58608 = DIRECTION ( 'NONE',  ( 0.000000000000000000, 0.000000000000000000, -1.000000000000000000 ) ) ;
#58609 = EDGE_CURVE ( 'NONE', #40086, #63483, #39395, .T. ) ;
#58610 = EDGE_LOOP ( 'NONE', ( #3698, #29796 ) ) ;
#58611 = DIRECTION ( 'NONE',  ( 0.000000000000000000, 0.000000000000000000, -1.000000000000000000 ) ) ;
#58612 = ORIENTED_EDGE ( 'NONE', *, *, #63237, .T. ) ;
#58613 = VERTEX_POINT ( 'NONE', #39834 ) ;
#58614 = CARTESIAN_POINT ( 'NONE',  ( 98.87114546532168902, -41.32433164768560374, 178.1768214011349585 ) ) ;
#58615 = VECTOR ( 'NONE', #8957, 1000.000000000000000 ) ;
#58616 = LINE ( 'NONE', #24124, #57458 ) ;
#58617 = CARTESIAN_POINT ( 'NONE',  ( 114.5680773229086782, -32.01199386431652272, 30.70444044875397793 ) ) ;
#58618 = VECTOR ( 'NONE', #76661, 1000.000000000000000 ) ;
#58619 = CARTESIAN_POINT ( 'NONE',  ( -91.13883569058442902, 95.16896684734908263, 93.48397507443846166 ) ) ;
#58620 = CIRCLE ( 'NONE', #61474, 4.750000000000004441 ) ;
#58621 = CARTESIAN_POINT ( 'NONE',  ( 102.0670549667728579, -27.97049805557078983, 80.48979194197387699 ) ) ;
#58622 = DIRECTION ( 'NONE',  ( 0.7071067811866258435, -0.7071067811864693020, 7.071067811866266166E-16 ) ) ;
#58623 = VECTOR ( 'NONE', #23857, 1000.000000000000000 ) ;
#58624 = ORIENTED_EDGE ( 'NONE', *, *, #53863, .T. ) ;
#58625 = LINE ( 'NONE', #43209, #33308 ) ;
#58626 = FACE_OUTER_BOUND ( 'NONE', #1100, .T. ) ;
#58627 = VERTEX_POINT ( 'NONE', #88004 ) ;
#58628 = CARTESIAN_POINT ( 'NONE',  ( 116.1995025514324169, -41.78438384397603045, 263.4241967044824833 ) ) ;
#58629 = CARTESIAN_POINT ( 'NONE',  ( 12.02669652733116123, 86.65134610876239663, 117.9444722473752307 ) ) ;
#58630 = VERTEX_POINT ( 'NONE', #81209 ) ;
#58631 = EDGE_CURVE ( 'NONE', #48907, #9592, #6496, .T. ) ;
#58632 = FACE_BOUND ( 'NONE', #47835, .T. ) ;
#58633 = CARTESIAN_POINT ( 'NONE',  ( 29.56648329127298069, -71.37844715994266664, 342.9256252759109884 ) ) ;
#58634 = DIRECTION ( 'NONE',  ( 0.000000000000000000, 0.000000000000000000, -1.000000000000000000 ) ) ;
#58636 = EDGE_CURVE ( 'NONE', #34120, #77564, #25360, .T. ) ;
#58635 = PLANE ( 'NONE',  #25950 ) ;
#58637 = CARTESIAN_POINT ( 'NONE',  ( 96.07947519314286922, -35.15364532898842498, 222.2251490854349640 ) ) ;
#58638 = CARTESIAN_POINT ( 'NONE',  ( 199.3900000000000148, 46.38749999999999574, -50.79999999999999716 ) ) ;
#58639 = ORIENTED_EDGE ( 'NONE', *, *, #45855, .F. ) ;
#58640 = CARTESIAN_POINT ( 'NONE',  ( 106.5158076061070460, -25.64367904723916780, 41.12800622829193742 ) ) ;
#58641 = CARTESIAN_POINT ( 'NONE',  ( 97.81170669197712186, -40.51744871389600178, 156.6352702525290681 ) ) ;
#58642 = CARTESIAN_POINT ( 'NONE',  ( 95.23113311243525914, -37.33357626913954164, 271.3670538473393776 ) ) ;
#58643 = VERTEX_POINT ( 'NONE', #73922 ) ;
#58644 = CARTESIAN_POINT ( 'NONE',  ( 78.88274585166558950, -39.21170328186890686, 8.006085407565089795 ) ) ;
#58645 = CARTESIAN_POINT ( 'NONE',  ( 97.84282136733131097, -40.59266849988905079, 17.64178760023652970 ) ) ;
#58646 = LINE ( 'NONE', #1925, #43679 ) ;
#58647 = CARTESIAN_POINT ( 'NONE',  ( 108.7800423072870046, -44.73859216708707720, 105.5623760838769698 ) ) ;
#58648 = CARTESIAN_POINT ( 'NONE',  ( 116.8778831976698882, -40.31743973661899361, 214.5470538473389581 ) ) ;
#58649 = CYLINDRICAL_SURFACE ( 'NONE', #5801, 0.5000000000000129896 ) ;
#58650 = EDGE_LOOP ( 'NONE', ( #67473, #58072 ) ) ;
#58651 = AXIS2_PLACEMENT_3D ( 'NONE', #73754, #39672, #17891 ) ;
#58652 = LINE ( 'NONE', #16450, #56694 ) ;
#58653 = VERTEX_POINT ( 'NONE', #62412 ) ;
#58654 = EDGE_LOOP ( 'NONE', ( #13637, #53355 ) ) ;
#58655 = AXIS2_PLACEMENT_3D ( 'NONE', #1418, #37726, #57248 ) ;
#58656 = DIRECTION ( 'NONE',  ( 0.000000000000000000, 0.000000000000000000, 1.000000000000000000 ) ) ;
#58657 = VERTEX_POINT ( 'NONE', #47086 ) ;
#58658 = EDGE_LOOP ( 'NONE', ( #50326, #52065, #40416, #4033, #71404, #16424, #56558 ) ) ;
#58659 = FACE_OUTER_BOUND ( 'NONE', #22434, .T. ) ;
#58660 = VECTOR ( 'NONE', #50423, 1000.000000000000000 ) ;
#58661 = CARTESIAN_POINT ( 'NONE',  ( 46.83715912545424231, -47.82818131006082751, 300.4678068554150059 ) ) ;
#58662 = CARTESIAN_POINT ( 'NONE',  ( 103.8954607204944693, -27.23986633091804777, 41.33311113083999544 ) ) ;
#58663 = CARTESIAN_POINT ( 'NONE',  ( 103.9030524752275397, -44.69467205304180624, 116.6981341137909567 ) ) ;
#58664 = CARTESIAN_POINT ( 'NONE',  ( 112.2192032947272509, -26.89661630634724432, 14.68038718067299442 ) ) ;
#58665 = PLANE ( 'NONE',  #54238 ) ;
#58666 = VERTEX_POINT ( 'NONE', #74374 ) ;
#58667 = CARTESIAN_POINT ( 'NONE',  ( 103.2783699128477934, -27.47470799093264660, 136.3856377475192687 ) ) ;
#58668 = VERTEX_POINT ( 'NONE', #67552 ) ;
#58669 = DIRECTION ( 'NONE',  ( -2.999999999999999839E-15, 1.000000000000000000, -2.999999999999999900E-30 ) ) ;
#58670 = CARTESIAN_POINT ( 'NONE',  ( 117.0721904964497355, -35.46492929623623525, 33.92731048517197934 ) ) ;
#58671 = CARTESIAN_POINT ( 'NONE',  ( 188.5667039024485518, -48.82844715993430640, 170.7178068554150059 ) ) ;
#58672 = EDGE_CURVE ( 'NONE', #72716, #38840, #12146, .T. ) ;
#58674 = VECTOR ( 'NONE', #68158, 1000.000000000000000 ) ;
#58673 = CARTESIAN_POINT ( 'NONE',  ( 107.0664832912739399, -36.72944715994095333, 294.6356252759106837 ) ) ;
#58675 = VERTEX_POINT ( 'NONE', #68003 ) ;
#58676 = CARTESIAN_POINT ( 'NONE',  ( 105.8935610739654010, -47.12417332243212087, 282.4870538473394390 ) ) ;
#58677 = CIRCLE ( 'NONE', #23899, 2.117000000000000881 ) ;
#58678 = CARTESIAN_POINT ( 'NONE',  ( 118.6189051447874903, -33.88680481589229743, 10.01848241876795953 ) ) ;
#58679 = AXIS2_PLACEMENT_3D ( 'NONE', #73025, #51230, #3993 ) ;
#58680 = AXIS2_PLACEMENT_3D ( 'NONE', #5188, #68757, #32881 ) ;
#58681 = DIRECTION ( 'NONE',  ( -0.000000000000000000, 0.000000000000000000, 1.000000000000000000 ) ) ;
#58682 = EDGE_CURVE ( 'NONE', #36659, #27646, #7008, .T. ) ;
#58684 = CARTESIAN_POINT ( 'NONE',  ( 69.94616667561825807, -138.0587426493221699, 247.6570821721479945 ) ) ;
#58683 = CARTESIAN_POINT ( 'NONE',  ( -27.27158787008326968, 127.0000000000000000, -0.000000000000000000 ) ) ;
#58685 = DIRECTION ( 'NONE',  ( 0.7071067811865489050, -0.7071067811865462405, 0.000000000000000000 ) ) ;
#58686 = EDGE_CURVE ( 'NONE', #49816, #14401, #68166, .T. ) ;
#58687 = FACE_OUTER_BOUND ( 'NONE', #26405, .T. ) ;
#58688 = PLANE ( 'NONE',  #44075 ) ;
#58689 = AXIS2_PLACEMENT_3D ( 'NONE', #67398, #6094, #47392 ) ;
#58690 = EDGE_CURVE ( 'NONE', #28371, #54294, #69687, .T. ) ;
#58691 = CYLINDRICAL_SURFACE ( 'NONE', #17011, 2.500000000000002220 ) ;
#58692 = DIRECTION ( 'NONE',  ( 0.000000000000000000, 0.000000000000000000, 1.000000000000000000 ) ) ;
#58693 = DIRECTION ( 'NONE',  ( 0.000000000000000000, 0.000000000000000000, -1.000000000000000000 ) ) ;
#58694 = ADVANCED_FACE ( 'NONE', ( #14730 ), #77394, .F. ) ;
#58695 = CARTESIAN_POINT ( 'NONE',  ( 97.44607596320715004, -32.59944340835617282, 16.00419670448194154 ) ) ;
#58696 = CARTESIAN_POINT ( 'NONE',  ( 115.0396333253530230, -29.07419673827904916, 185.4232443235299570 ) ) ;
#58697 = CARTESIAN_POINT ( 'NONE',  ( 117.4762281475856724, -37.96087228405902181, 49.73276813305393773 ) ) ;
#58699 = FACE_OUTER_BOUND ( 'NONE', #31085, .T. ) ;
#58698 = CARTESIAN_POINT ( 'NONE',  ( 78.13314995793999174, 12.92155284005730387, 361.9756252759109998 ) ) ;
#58700 = CARTESIAN_POINT ( 'NONE',  ( 80.71968614772352169, -34.05633243510678909, 1.689562801603114339 ) ) ;
#58701 = EDGE_CURVE ( 'NONE', #6676, #32654, #89313, .T. ) ;
#58702 = ORIENTED_EDGE ( 'NONE', *, *, #83917, .T. ) ;
#58703 = CARTESIAN_POINT ( 'NONE',  ( 115.8254323940393107, -31.73001883393573053, 185.2397919421337633 ) ) ;
#58704 = VERTEX_POINT ( 'NONE', #7457 ) ;
#58705 = EDGE_CURVE ( 'NONE', #36809, #57891, #68944, .T. ) ;
#58706 = CARTESIAN_POINT ( 'NONE',  ( 99.16769444712207360, -43.44866735504064081, 72.89943479971999807 ) ) ;
#58708 = ORIENTED_EDGE ( 'NONE', *, *, #11323, .F. ) ;
#58707 = CARTESIAN_POINT ( 'NONE',  ( 4.506942778454146037, 94.42426803962317194, 130.4782289187788251 ) ) ;
#58709 = CARTESIAN_POINT ( 'NONE',  ( 193.0374249753375011, -23.42844715993432558, 249.9678068554149775 ) ) ;
#58710 = CARTESIAN_POINT ( 'NONE',  ( 110.1310368924891208, -26.13358316477614451, 210.8403871806729626 ) ) ;
#58711 = PLANE ( 'NONE',  #87497 ) ;
#58712 = LINE ( 'NONE', #44190, #833 ) ;
#58713 = DIRECTION ( 'NONE',  ( 0.000000000000000000, 0.000000000000000000, 1.000000000000000000 ) ) ;
#58714 = CARTESIAN_POINT ( 'NONE',  ( 33.78309357196401663, -29.99615139349950965, -5.074374724088000832 ) ) ;
#58715 = EDGE_CURVE ( 'NONE', #82109, #58666, #64220, .T. ) ;
#58716 = FACE_OUTER_BOUND ( 'NONE', #37309, .T. ) ;
#58717 = CARTESIAN_POINT ( 'NONE',  ( 116.8035579096021337, -34.12169190864647561, 99.03416637764169650 ) ) ;
#58718 = CARTESIAN_POINT ( 'NONE',  ( 117.0460787713799817, -39.54838250520750620, 143.6194347997209775 ) ) ;
#58719 = ORIENTED_EDGE ( 'NONE', *, *, #21911, .F. ) ;
#58720 = EDGE_LOOP ( 'NONE', ( #75573, #57322 ) ) ;
#58721 = COLOUR_RGB ( '', 0.08235294, 0.09019608, 0.10196078) ;
#58722 = CARTESIAN_POINT ( 'NONE',  ( 100.6361971157895283, -42.82696290926312344, 78.36158330589692866 ) ) ;
#58723 = DIRECTION ( 'NONE',  ( 0.000000000000000000, 0.000000000000000000, -1.000000000000000000 ) ) ;
#58725 = DIRECTION ( 'NONE',  ( 1.000000000000000000, 0.000000000000000000, 0.000000000000000000 ) ) ;
#58724 = CARTESIAN_POINT ( 'NONE',  ( 116.7002268312855051, -35.03994406823841246, 239.9641967044819637 ) ) ;
#58726 = VECTOR ( 'NONE', #66626, 1000.000000000000000 ) ;
#58727 = LINE ( 'NONE', #10154, #71082 ) ;
#58728 = PLANE ( 'NONE',  #26383 ) ;
#58729 = CARTESIAN_POINT ( 'NONE',  ( 118.0068565116052497, 76.93600387762167259, 11.39936611905845076 ) ) ;
#58730 = CYLINDRICAL_SURFACE ( 'NONE', #12478, 9.999999999999998224 ) ;
#58731 = CYLINDRICAL_SURFACE ( 'NONE', #62350, 8.928100000000000591 ) ;
#58732 = CARTESIAN_POINT ( 'NONE',  ( 1.473504056721760595E-14, 239.0000000000000000, 104.2754207677255920 ) ) ;
#58733 = CARTESIAN_POINT ( 'NONE',  ( 114.3286968523004248, -29.23113535793732254, 174.4641967044819637 ) ) ;
#58734 = VERTEX_POINT ( 'NONE', #35147 ) ;
#58735 = ORIENTED_EDGE ( 'NONE', *, *, #79577, .T. ) ;
#58736 = DIRECTION ( 'NONE',  ( 3.100000000000000258E-29, -3.100000000000000044E-14, -1.000000000000000000 ) ) ;
#58737 = CARTESIAN_POINT ( 'NONE',  ( 100.9546728785971794, -28.70702567698208085, 151.5939586026250083 ) ) ;
#58738 = CARTESIAN_POINT ( 'NONE',  ( 143.0667039024470171, -90.27844715994091018, 51.21780685541800437 ) ) ;
#58740 = EDGE_CURVE ( 'NONE', #20535, #43140, #43754, .T. ) ;
#58739 = DIRECTION ( 'NONE',  ( 0.000000000000000000, 0.000000000000000000, 1.000000000000000000 ) ) ;
#58741 = VECTOR ( 'NONE', #59166, 1000.000000000000000 ) ;
#58742 = CARTESIAN_POINT ( 'NONE',  ( 127.0664832912740394, -46.72944715994101017, -5.074374724089008915 ) ) ;
#58743 = AXIS2_PLACEMENT_3D ( 'NONE', #14404, #50692, #78433 ) ;
#58744 = VECTOR ( 'NONE', #87272, 1000.000000000000000 ) ;
#58745 = CARTESIAN_POINT ( 'NONE',  ( 114.9651742339629976, -29.92520496456729262, 184.3927681330539770 ) ) ;
#58746 = CARTESIAN_POINT ( 'NONE',  ( 107.0664832912739968, -36.72944715994100306, 287.6356252759109680 ) ) ;
#58747 = ORIENTED_EDGE ( 'NONE', *, *, #6340, .F. ) ;
#58749 = ORIENTED_EDGE ( 'NONE', *, *, #6429, .F. ) ;
#58748 = ORIENTED_EDGE ( 'NONE', *, *, #81004, .T. ) ;
#58750 = AXIS2_PLACEMENT_3D ( 'NONE', #46174, #66181, #65737 ) ;
#58751 = CARTESIAN_POINT ( 'NONE',  ( 97.81475986870147210, -40.52492237179531287, 62.63673496744226554 ) ) ;
#58752 = CARTESIAN_POINT ( 'NONE',  ( 135.2444258376725941, 101.5999999999999943, 147.4575741623265799 ) ) ;
#58753 = CARTESIAN_POINT ( 'NONE',  ( 131.0667039024480118, -61.87844715994100397, 204.3338068554149913 ) ) ;
#58754 = CARTESIAN_POINT ( 'NONE',  ( 115.1548909598205057, -41.51005587062507374, 279.8453928297065545 ) ) ;
#58755 = AXIS2_PLACEMENT_3D ( 'NONE', #20704, #63836, #35208 ) ;
#58756 = CARTESIAN_POINT ( 'NONE',  ( 41.56648329127399677, -18.82844715994099971, 138.9256252759119832 ) ) ;
#58757 = ORIENTED_EDGE ( 'NONE', *, *, #46185, .T. ) ;
#58758 = ADVANCED_FACE ( 'NONE', ( #84230 ), #41954, .T. ) ;
#58759 = AXIS2_PLACEMENT_3D ( 'NONE', #78651, #50906, #43639 ) ;
#58760 = CARTESIAN_POINT ( 'NONE',  ( 115.0845091798801008, -41.07331283931524268, 9.635625275910939536 ) ) ;
#58761 = CARTESIAN_POINT ( 'NONE',  ( 106.5667039024470313, -108.2470741265382799, 2.217806855418114065 ) ) ;
#58762 = EDGE_LOOP ( 'NONE', ( #79445, #23991, #29936, #38242 ) ) ;
#58763 = ORIENTED_EDGE ( 'NONE', *, *, #67740, .F. ) ;
#58764 = ADVANCED_FACE ( 'NONE', ( #1550, #49669 ), #70586, .T. ) ;
#58765 = FACE_BOUND ( 'NONE', #50729, .T. ) ;
#58766 = VERTEX_POINT ( 'NONE', #51018 ) ;
#58767 = ORIENTED_EDGE ( 'NONE', *, *, #41970, .F. ) ;
#58768 = CARTESIAN_POINT ( 'NONE',  ( 113.2433956935301467, -28.75706466399318373, 155.5522588166994069 ) ) ;
#58769 = CIRCLE ( 'NONE', #25452, 3.600000000000000089 ) ;
#58770 = CARTESIAN_POINT ( 'NONE',  ( 98.58513254605244924, -37.74079342042374918, 40.84384839950494239 ) ) ;
#58771 = CARTESIAN_POINT ( 'NONE',  ( 106.9748012750099946, -47.17635858745483546, 187.5699109901969734 ) ) ;
#58772 = CARTESIAN_POINT ( 'NONE',  ( 98.87380182923577365, -30.31772012733808808, 155.7984824187679465 ) ) ;
#58773 = DIRECTION ( 'NONE',  ( -0.5180656453708486486, -0.02186357193551463976, -0.8550613845266940016 ) ) ;
#58774 = CARTESIAN_POINT ( 'NONE',  ( 96.80890382254112581, -40.84721887859184619, 247.6422919425769749 ) ) ;
#58775 = CARTESIAN_POINT ( 'NONE',  ( 104.4081952550981214, -46.45811700621415241, 98.36623602494283602 ) ) ;
#58776 = CARTESIAN_POINT ( 'NONE',  ( 3.174999999999889688, 124.5870000000000033, 31.75000000000000000 ) ) ;
#58777 = ORIENTED_EDGE ( 'NONE', *, *, #29398, .T. ) ;
#58778 = ORIENTED_EDGE ( 'NONE', *, *, #7852, .T. ) ;
#58779 = MECHANICAL_DESIGN_GEOMETRIC_PRESENTATION_REPRESENTATION (  '', ( #3690 ), #51590 ) ;
#58780 = CARTESIAN_POINT ( 'NONE',  ( 114.1546619933443480, -29.02461823700197741, 199.4841967044819739 ) ) ;
#58781 = ORIENTED_EDGE ( 'NONE', *, *, #71159, .T. ) ;
#58782 = CARTESIAN_POINT ( 'NONE',  ( 102.8439234467419965, -46.26134197790700853, 177.2441967044819648 ) ) ;
#58783 = CARTESIAN_POINT ( 'NONE',  ( 1.166476076187854022E-15, 2.269999999999994245, 9.525000000000000355 ) ) ;
#58784 = CARTESIAN_POINT ( 'NONE',  ( 73.10937651008745775, -46.62589376934776908, 14.92562527591095645 ) ) ;
#58785 = DIRECTION ( 'NONE',  ( 1.000000000000000000, 0.000000000000000000, 0.000000000000000000 ) ) ;
#58786 = PLANE ( 'NONE',  #71749 ) ;
#58787 = EDGE_CURVE ( 'NONE', #6408, #74884, #63316, .T. ) ;
#58790 = CARTESIAN_POINT ( 'NONE',  ( 100.0388059118473052, -29.01104360887439526, 281.6641967044822650 ) ) ;
#58789 = LINE ( 'NONE', #72883, #41249 ) ;
#58788 = DIRECTION ( 'NONE',  ( 0.000000000000000000, 0.000000000000000000, 1.000000000000000000 ) ) ;
#58791 = CARTESIAN_POINT ( 'NONE',  ( 143.0667039024470171, -83.77844715994091018, 55.21780685541800437 ) ) ;
#58792 = EDGE_CURVE ( 'NONE', #27930, #37713, #71045, .T. ) ;
#58793 = DIRECTION ( 'NONE',  ( 1.000000000000000078E-15, 0.000000000000000000, 1.000000000000000000 ) ) ;
#58794 = LINE ( 'NONE', #10654, #7784 ) ;
#58795 = EDGE_CURVE ( 'NONE', #19810, #46234, #74775, .T. ) ;
#58796 = CARTESIAN_POINT ( 'NONE',  ( 68.10560579175795226, -137.1428242527968564, 247.2610778050800491 ) ) ;
#58797 = CARTESIAN_POINT ( 'NONE',  ( -31.75000000000000000, 104.3431970271541900, 3.174999999999779998 ) ) ;
#58798 = DIRECTION ( 'NONE',  ( 0.000000000000000000, 0.000000000000000000, -1.000000000000000000 ) ) ;
#58800 = ORIENTED_EDGE ( 'NONE', *, *, #79136, .F. ) ;
#58799 = CARTESIAN_POINT ( 'NONE',  ( 107.6136016015418448, -44.72672411580607132, 195.5838068554169524 ) ) ;
#58801 = ADVANCED_FACE ( 'NONE', ( #78311 ), #87813, .F. ) ;
#58802 = CARTESIAN_POINT ( 'NONE',  ( 135.2096432771652701, -21.23067567606553752, 8.021372095561345006 ) ) ;
#58803 = CARTESIAN_POINT ( 'NONE',  ( 113.0348518357461955, -45.34727401701223926, 203.0584824187679374 ) ) ;
#58804 = CARTESIAN_POINT ( 'NONE',  ( 108.9852221676114539, -46.97644323546262513, 78.72419670448194040 ) ) ;
#58805 = CARTESIAN_POINT ( 'NONE',  ( 118.1276453766531915, -32.34061975111649190, 245.1270538473389706 ) ) ;
#58806 = CARTESIAN_POINT ( 'NONE',  ( 168.5667039024483529, -48.82844715993496720, 180.4678068554150059 ) ) ;
#58807 = DIRECTION ( 'NONE',  ( 1.000000000000000078E-15, -1.000000000000000000, 0.000000000000000000 ) ) ;
#58808 = B_SPLINE_CURVE_WITH_KNOTS ( 'NONE', 3,
 ( #52995, #87125, #18513, #46655 ),
 .UNSPECIFIED., .F., .F.,
 ( 4, 4 ),
 ( -0.3974825557268170106, -0.3842043193313839922 ),
 .UNSPECIFIED. ) ;
#58810 = DIRECTION ( 'NONE',  ( 0.7071067811869283792, -0.7071067811861665442, 7.071067811869291448E-16 ) ) ;
#58809 = CARTESIAN_POINT ( 'NONE',  ( 132.2857443282840393, -124.7784471599409102, 45.21780685541799727 ) ) ;
#58811 = CYLINDRICAL_SURFACE ( 'NONE', #43602, 0.5000000000000031086 ) ;
#58812 = FACE_OUTER_BOUND ( 'NONE', #69861, .T. ) ;
#58813 = DIRECTION ( 'NONE',  ( -1.000000000000000078E-15, 1.000000000000000000, 0.000000000000000000 ) ) ;
#58814 = AXIS2_PLACEMENT_3D ( 'NONE', #39520, #87238, #88585 ) ;
#58815 = AXIS2_PLACEMENT_3D ( 'NONE', #29251, #56936, #49218 ) ;
#58816 = CIRCLE ( 'NONE', #24019, 0.5000000000000004441 ) ;
#58817 = AXIS2_PLACEMENT_3D ( 'NONE', #2269, #84510, #22717 ) ;
#58818 = VERTEX_POINT ( 'NONE', #77851 ) ;
#58819 = EDGE_LOOP ( 'NONE', ( #53034, #35755 ) ) ;
#58820 = EDGE_CURVE ( 'NONE', #36325, #53045, #25430, .T. ) ;
#58821 = AXIS2_PLACEMENT_3D ( 'NONE', #32902, #1977, #29674 ) ;
#58822 = CARTESIAN_POINT ( 'NONE',  ( 115.1410662219050067, -33.85660664540706222, 113.5209912566479744 ) ) ;
#58824 = ORIENTED_EDGE ( 'NONE', *, *, #13399, .T. ) ;
#58823 = CARTESIAN_POINT ( 'NONE',  ( 97.81168895331838087, -40.51742574516882200, 287.6356252759109680 ) ) ;
#58825 = CARTESIAN_POINT ( 'NONE',  ( 112.5028774994481466, -27.85959465031284310, 90.63848241876793566 ) ) ;
#58826 = DIRECTION ( 'NONE',  ( -0.7071067811865480168, -2.262741699796950529E-14, -0.7071067811865470176 ) ) ;
#58827 = AXIS2_PLACEMENT_3D ( 'NONE', #61959, #19300, #39723 ) ;
#58828 = DIRECTION ( 'NONE',  ( 1.000000000000000000, 0.000000000000000000, 0.000000000000000000 ) ) ;
#58829 = CARTESIAN_POINT ( 'NONE',  ( 105.4788588808462038, 127.0000000000000000, -3.968749999999580336 ) ) ;
#58831 = CARTESIAN_POINT ( 'NONE',  ( 116.7468388360755966, -38.12735696270561903, 28.71276813305495423 ) ) ;
#58830 = AXIS2_PLACEMENT_3D ( 'NONE', #6783, #75827, #34932 ) ;
#58832 = ORIENTED_EDGE ( 'NONE', *, *, #53234, .T. ) ;
#58833 = ORIENTED_EDGE ( 'NONE', *, *, #5227, .T. ) ;
#58834 = ORIENTED_EDGE ( 'NONE', *, *, #62872, .T. ) ;
#58835 = LINE ( 'NONE', #72044, #3654 ) ;
#58836 = CARTESIAN_POINT ( 'NONE',  ( 73.06648329127396835, -46.72944715994108122, -4.970821333495798022 ) ) ;
#58837 = CARTESIAN_POINT ( 'NONE',  ( 115.8254323921038491, -31.73001882920818773, 115.2397919425400232 ) ) ;
#58838 = PLANE ( 'NONE',  #36810 ) ;
#58839 = CIRCLE ( 'NONE', #19688, 2.124999999999994227 ) ;
#58840 = DIRECTION ( 'NONE',  ( -0.02150753337723538411, -0.0009076677972193728959, -0.9997682742251812194 ) ) ;
#58841 = LINE ( 'NONE', #16200, #42260 ) ;
#58842 = DIRECTION ( 'NONE',  ( 1.000000000000000078E-15, 1.000000000000000083E-30, -1.000000000000000000 ) ) ;
#58843 = CARTESIAN_POINT ( 'NONE',  ( -7.370840183531916168, 92.89254840543441105, 130.3477230843911059 ) ) ;
#58844 = CARTESIAN_POINT ( 'NONE',  ( 117.0705705820184477, -32.08379757587633208, 59.16038718067295576 ) ) ;
#58845 = VERTEX_POINT ( 'NONE', #83774 ) ;
#58846 = EDGE_LOOP ( 'NONE', ( #75904, #4034, #31617, #15683 ) ) ;
#58847 = DIRECTION ( 'NONE',  ( 4.299999999999999979E-14, -1.000000000000000000, 4.400000000000000367E-29 ) ) ;
#58848 = DIRECTION ( 'NONE',  ( 0.000000000000000000, 0.000000000000000000, 1.000000000000000000 ) ) ;
#58850 = EDGE_CURVE ( 'NONE', #54417, #72244, #21545, .T. ) ;
#58849 = CARTESIAN_POINT ( 'NONE',  ( 79.56670390244701707, -102.5864808479223456, 250.2178068554179902 ) ) ;
#58851 = CARTESIAN_POINT ( 'NONE',  ( 112.1548083954980939, -43.14751820055241893, 165.9280903695909615 ) ) ;
#58852 = VECTOR ( 'NONE', #27256, 1000.000000000000114 ) ;
#58853 = AXIS2_PLACEMENT_3D ( 'NONE', #87933, #53823, #38876 ) ;
#58854 = ADVANCED_FACE ( 'NONE', ( #65546 ), #38282, .F. ) ;
#58855 = CARTESIAN_POINT ( 'NONE',  ( 245.4909999999999854, 65.43750000000000000, -67.11950000000000216 ) ) ;
#58856 = EDGE_LOOP ( 'NONE', ( #54798, #77417, #56060, #14516 ) ) ;
#58857 = ORIENTED_EDGE ( 'NONE', *, *, #10737, .F. ) ;
#58858 = CARTESIAN_POINT ( 'NONE',  ( 131.3164832912739826, -18.72944715994100662, 6.749768910606465333 ) ) ;
#58859 = ORIENTED_EDGE ( 'NONE', *, *, #83344, .F. ) ;
#58860 = ORIENTED_EDGE ( 'NONE', *, *, #24163, .F. ) ;
#58861 = CARTESIAN_POINT ( 'NONE',  ( 270.8910000000000196, 65.43750000000000000, 10.66800000000000104 ) ) ;
#58862 = CARTESIAN_POINT ( 'NONE',  ( 101.0667092185316989, -28.63788266170726260, 182.0158690201829756 ) ) ;
#58863 = DIRECTION ( 'NONE',  ( 0.000000000000000000, 0.000000000000000000, 1.000000000000000000 ) ) ;
#58864 = CARTESIAN_POINT ( 'NONE',  ( 100.9546728989441533, -28.70702566177422455, 120.5939586006224431 ) ) ;
#58865 = CARTESIAN_POINT ( 'NONE',  ( 110.8538822462197970, -45.98447871898064676, 17.88557456161885639 ) ) ;
#58866 = AXIS2_PLACEMENT_3D ( 'NONE', #25563, #6040, #61420 ) ;
#58867 = VERTEX_POINT ( 'NONE', #39176 ) ;
#58868 = ADVANCED_FACE ( 'NONE', ( #24221, #18280 ), #59163, .F. ) ;
#58869 = AXIS2_PLACEMENT_3D ( 'NONE', #29589, #36852, #3234 ) ;
#58870 = AXIS2_PLACEMENT_3D ( 'NONE', #33728, #46877, #54134 ) ;
#58871 = ORIENTED_EDGE ( 'NONE', *, *, #67456, .T. ) ;
#58872 = ORIENTED_EDGE ( 'NONE', *, *, #18026, .F. ) ;
#58873 = CARTESIAN_POINT ( 'NONE',  ( 104.3825147926133354, -28.50161402210781603, 208.1576141791150008 ) ) ;
#58874 = CARTESIAN_POINT ( 'NONE',  ( 117.1128946550982732, -32.06414332788899912, 59.16038718067295576 ) ) ;
#58875 = CARTESIAN_POINT ( 'NONE',  ( 99.16013801855501697, -43.49098322490566204, 31.88991099019594699 ) ) ;
#58876 = DIRECTION ( 'NONE',  ( 0.000000000000000000, -1.000000000000000000, 0.000000000000000000 ) ) ;
#58877 = LINE ( 'NONE', #80696, #45150 ) ;
#58878 = DIRECTION ( 'NONE',  ( 0.000000000000000000, 2.135044278125299371E-15, -1.000000000000000000 ) ) ;
#58879 = CARTESIAN_POINT ( 'NONE',  ( 117.2380278806138278, -39.01742120631563893, 144.6499109901969859 ) ) ;
#58880 = DIRECTION ( 'NONE',  ( 0.000000000000000000, 0.000000000000000000, -1.000000000000000000 ) ) ;
#58881 = VERTEX_POINT ( 'NONE', #9691 ) ;
#58882 = CARTESIAN_POINT ( 'NONE',  ( 226.4410000000000025, 65.43750000000000000, -2.032000000000000028 ) ) ;
#58883 = ORIENTED_EDGE ( 'NONE', *, *, #78299, .T. ) ;
#58884 = ORIENTED_EDGE ( 'NONE', *, *, #69808, .T. ) ;
#58885 = DIRECTION ( 'NONE',  ( -1.000000000000000078E-15, 1.000000000000000083E-30, 1.000000000000000000 ) ) ;
#58886 = DIRECTION ( 'NONE',  ( 1.000000000000000078E-15, -1.000000000000000000, 0.000000000000000000 ) ) ;
#58887 = ORIENTED_EDGE ( 'NONE', *, *, #3979, .T. ) ;
#58888 = CARTESIAN_POINT ( 'NONE',  ( 19.56670390244824631, -47.82844715994191631, 300.4678068554150059 ) ) ;
#58889 = CARTESIAN_POINT ( 'NONE',  ( 97.81541071992751313, -32.74985850689276390, 132.0034678584867436 ) ) ;
#58890 = CARTESIAN_POINT ( 'NONE',  ( 97.77227622453175115, -32.00665715170008951, 50.95276813305294183 ) ) ;
#58891 = CARTESIAN_POINT ( 'NONE',  ( 91.91125933621933086, -96.68314769832132072, -19.26696060647622843 ) ) ;
#58892 = AXIS2_PLACEMENT_3D ( 'NONE', #74927, #12706, #40393 ) ;
#58893 = LINE ( 'NONE', #39791, #26041 ) ;
#58894 = DIRECTION ( 'NONE',  ( 1.000000000000000000, -5.337610695313248426E-16, 0.000000000000000000 ) ) ;
#58895 = CARTESIAN_POINT ( 'NONE',  ( 116.3624975636024317, -33.68846805112525544, 89.07848241876791917 ) ) ;
#58897 = CARTESIAN_POINT ( 'NONE',  ( 97.44537786355549258, -42.12371753947135744, 177.7451490854349743 ) ) ;
#58896 = DIRECTION ( 'NONE',  ( 0.000000000000000000, 1.000000000000000000, 0.000000000000000000 ) ) ;
#58898 = CARTESIAN_POINT ( 'NONE',  ( 97.07197965290352215, -35.37934377285892396, 61.21903046452214880 ) ) ;
#58899 = EDGE_CURVE ( 'NONE', #37650, #65590, #73702, .T. ) ;
#58900 = FACE_OUTER_BOUND ( 'NONE', #63975, .T. ) ;
#58901 = EDGE_LOOP ( 'NONE', ( #69879, #28185, #20690, #5686 ) ) ;
#58902 = CARTESIAN_POINT ( 'NONE',  ( 97.80893753052176010, -40.51861053356429920, 37.63533870039827178 ) ) ;
#58903 = LINE ( 'NONE', #52520, #60147 ) ;
#58904 = EDGE_CURVE ( 'NONE', #49439, #8126, #48620, .T. ) ;
#58905 = CARTESIAN_POINT ( 'NONE',  ( 100.9551865876383090, -28.70660340941259037, 135.5938645509268383 ) ) ;
#58906 = CARTESIAN_POINT ( 'NONE',  ( 188.5667039024483529, -48.82844715993431350, 295.7178068554150059 ) ) ;
#58908 = VERTEX_POINT ( 'NONE', #38724 ) ;
#58907 = CARTESIAN_POINT ( 'NONE',  ( 97.72299786849482928, -41.53060059208619492, 196.7041967044819728 ) ) ;
#58909 = EDGE_CURVE ( 'NONE', #63964, #63276, #45084, .T. ) ;
#58910 = CARTESIAN_POINT ( 'NONE',  ( 97.60798650947359079, -39.98270781540073671, 146.5900883612529810 ) ) ;
#58911 = CARTESIAN_POINT ( 'NONE',  ( 110.8246185410185944, -26.31015614812341141, 245.7889586092439629 ) ) ;
#58912 = CARTESIAN_POINT ( 'NONE',  ( 97.79748285543813324, -31.86337989110288405, 131.9413395616259947 ) ) ;
#58913 = CARTESIAN_POINT ( 'NONE',  ( 82.96136257729986596, 80.89704698943971550, 100.8082743238010011 ) ) ;
#58914 = CARTESIAN_POINT ( 'NONE',  ( 82.59390026530674334, -37.81452881268462107, 7.047625865511941257 ) ) ;
#58915 = PLANE ( 'NONE',  #73282 ) ;
#58916 = CARTESIAN_POINT ( 'NONE',  ( 3.174999999999889688, 8.255000000000000782, -31.75000000000000000 ) ) ;
#58917 = ORIENTED_EDGE ( 'NONE', *, *, #68136, .T. ) ;
#58918 = ORIENTED_EDGE ( 'NONE', *, *, #54174, .T. ) ;
#58919 = ORIENTED_EDGE ( 'NONE', *, *, #11842, .T. ) ;
#58920 = EDGE_CURVE ( 'NONE', #54314, #63468, #25542, .T. ) ;
#58921 = ORIENTED_EDGE ( 'NONE', *, *, #47390, .T. ) ;
#58922 = CARTESIAN_POINT ( 'NONE',  ( 108.3334480812130352, -46.73485935584395889, 72.67729194148455463 ) ) ;
#58923 = CARTESIAN_POINT ( 'NONE',  ( 102.3792474187797694, -47.61030217832540501, 283.2527681330539053 ) ) ;
#58924 = CARTESIAN_POINT ( 'NONE',  ( 172.5664832912740110, -32.07844715994070839, 198.9256252759119832 ) ) ;
#58925 = ADVANCED_FACE ( 'NONE', ( #79201 ), #65978, .F. ) ;
#58926 = CARTESIAN_POINT ( 'NONE',  ( 132.2189018279138679, -34.68450975841484052, 2.186797062530981162 ) ) ;
#58928 = CARTESIAN_POINT ( 'NONE',  ( 88.20503424218220800, 71.54629894495529641, 79.21825297796496557 ) ) ;
#58927 = DIRECTION ( 'NONE',  ( 1.000000000000000078E-15, -1.000000000000000083E-30, -1.000000000000000000 ) ) ;
#58929 = VECTOR ( 'NONE', #31279, 1000.000000000000000 ) ;
#58930 = CARTESIAN_POINT ( 'NONE',  ( 100.0786887504289666, -31.81753722825460429, 205.2609912566479693 ) ) ;
#58931 = ORIENTED_EDGE ( 'NONE', *, *, #72390, .T. ) ;
#58932 = EDGE_LOOP ( 'NONE', ( #17396, #2150, #40176, #13759, #22137, #59014 ) ) ;
#58933 = VECTOR ( 'NONE', #15536, 1000.000000000000000 ) ;
#58934 = ORIENTED_EDGE ( 'NONE', *, *, #8509, .T. ) ;
#58935 = CIRCLE ( 'NONE', #82196, 4.750000000000004441 ) ;
#58936 = VECTOR ( 'NONE', #43329, 1000.000000000000000 ) ;
#58937 = FACE_BOUND ( 'NONE', #36551, .T. ) ;
#58938 = AXIS2_PLACEMENT_3D ( 'NONE', #38194, #71835, #9599 ) ;
#58939 = B_SPLINE_CURVE_WITH_KNOTS ( 'NONE', 3,
 ( #28063, #48937, #56665, #84409, #30762, #72103, #58889, #58016, #52504, #43925, #80270, #23523, #80710, #32089, #72981, #59785, #71662, #9425, #73426, #4401, #85752, #31645, #64838, #10748, #51186, #59345 ),
 .UNSPECIFIED., .F., .F.,
 ( 4, 2, 2, 2, 2, 2, 2, 2, 2, 2, 2, 2, 4 ),
 ( 0.4999451768748383040, 0.5624520297654835854, 0.6249588826561287558, 0.6874657355467740372, 0.7499725884374193186, 0.7812260148827419037, 0.8124794413280644889, 0.8437328677733870741, 0.8749862942187095483, 0.9062397206640322445, 0.9374931471093547186, 0.9687465735546774148, 1.000000000000000000 ),
 .UNSPECIFIED. ) ;
#58940 = DIRECTION ( 'NONE',  ( 1.000000000000000000, 4.237773401492740281E-14, 0.000000000000000000 ) ) ;
#58941 = CYLINDRICAL_SURFACE ( 'NONE', #53291, 4.875000000000017764 ) ;
#58942 = CARTESIAN_POINT ( 'NONE',  ( 102.4274648318396146, -45.67098835673295554, 13.62729759161196341 ) ) ;
#58943 = CARTESIAN_POINT ( 'NONE',  ( 118.5472366675172537, 95.16897323824359489, -1.658320819116884781 ) ) ;
#58944 = CARTESIAN_POINT ( 'NONE',  ( 62.56670390244743629, -48.82844715994018969, 180.4678068554151196 ) ) ;
#58945 = FACE_BOUND ( 'NONE', #47892, .T. ) ;
#58946 = ORIENTED_EDGE ( 'NONE', *, *, #6012, .F. ) ;
#58947 = CARTESIAN_POINT ( 'NONE',  ( 97.06385931607105988, -37.34243354152794581, 57.37519869820856400 ) ) ;
#58948 = ORIENTED_EDGE ( 'NONE', *, *, #45551, .T. ) ;
#58949 = VECTOR ( 'NONE', #35088, 1000.000000000000000 ) ;
#58950 = FACE_OUTER_BOUND ( 'NONE', #50822, .T. ) ;
#58951 = CARTESIAN_POINT ( 'NONE',  ( 100.2991084500796575, -40.90897653417852098, 9.586185607686982024 ) ) ;
#58952 =( BOUNDED_CURVE ( )  B_SPLINE_CURVE ( 2, ( #37135, #58015, #79824 ),
 .UNSPECIFIED., .F., .T. ) 
 B_SPLINE_CURVE_WITH_KNOTS ( ( 3, 3 ),
 ( 0.01169420784673960018, 0.5170228498526568961 ),
 .UNSPECIFIED. ) 
 CURVE ( )  GEOMETRIC_REPRESENTATION_ITEM ( )  RATIONAL_B_SPLINE_CURVE ( ( 1.000420656333759872, 1.009299002520659849, 1.000000000000000000 ) ) 
 REPRESENTATION_ITEM ( '' )  );
#58953 = CARTESIAN_POINT ( 'NONE',  ( 176.7669697523286061, -48.62818131005482059, 300.4678068554149490 ) ) ;
#58954 = EDGE_CURVE ( 'NONE', #89309, #26329, #66879, .T. ) ;
#58955 = CARTESIAN_POINT ( 'NONE',  ( 152.0371591254585724, -47.82818131005588214, 117.4678068554150485 ) ) ;
#58956 = LINE ( 'NONE', #64903, #19864 ) ;
#58957 = ORIENTED_EDGE ( 'NONE', *, *, #85804, .T. ) ;
#58958 = FACE_OUTER_BOUND ( 'NONE', #71362, .T. ) ;
#58959 = CARTESIAN_POINT ( 'NONE',  ( 121.4418839049407097, 59.87844259738950825, -47.92489995295673566 ) ) ;
#58960 = ORIENTED_EDGE ( 'NONE', *, *, #70932, .F. ) ;
#58961 = CARTESIAN_POINT ( 'NONE',  ( 102.3603858057123972, -46.03211757857948783, 127.2041967044829960 ) ) ;
#58962 = VERTEX_POINT ( 'NONE', #23786 ) ;
#58963 = CARTESIAN_POINT ( 'NONE',  ( 102.2122376447956213, -29.66627497393060509, 49.97813411379098625 ) ) ;
#58964 = CARTESIAN_POINT ( 'NONE',  ( 95.83872823098280946, -118.1912118068161703, -9.274842254010202680 ) ) ;
#58965 = CARTESIAN_POINT ( 'NONE',  ( 101.8615262650677522, -29.55750872133152640, 72.00729759161094989 ) ) ;
#58966 = LINE ( 'NONE', #23599, #78185 ) ;
#58967 = CARTESIAN_POINT ( 'NONE',  ( -240.5296158183964792, 93.66249999999999432, 90.48749999999999716 ) ) ;
#58968 = CARTESIAN_POINT ( 'NONE',  ( 89.91697734863309677, -67.87849423282905548, 246.2109530912199773 ) ) ;
#58969 = AXIS2_PLACEMENT_3D ( 'NONE', #65791, #79905, #43560 ) ;
#58970 = CARTESIAN_POINT ( 'NONE',  ( 106.2504415414193488, -26.27893178022805998, 21.13848241876792144 ) ) ;
#58971 = CARTESIAN_POINT ( 'NONE',  ( 184.5667039024550888, -48.82844715994099971, 180.4678068554150343 ) ) ;
#58972 = ORIENTED_EDGE ( 'NONE', *, *, #7476, .T. ) ;
#58973 = CARTESIAN_POINT ( 'NONE',  ( 107.0667039024470313, -104.2784471599421323, -21.78219314458201694 ) ) ;
#58974 = ORIENTED_EDGE ( 'NONE', *, *, #82972, .F. ) ;
#58975 = EDGE_CURVE ( 'NONE', #18397, #12987, #60050, .T. ) ;
#58976 = CARTESIAN_POINT ( 'NONE',  ( 62.03715912545634836, -23.42818131006021787, 180.4678068554151196 ) ) ;
#58977 = ORIENTED_EDGE ( 'NONE', *, *, #51912, .T. ) ;
#58978 = ORIENTED_EDGE ( 'NONE', *, *, #87529, .F. ) ;
#58979 = CARTESIAN_POINT ( 'NONE',  ( 82.54999999999999716, 95.25000000000000000, 346.9005000000000223 ) ) ;
#58980 = CARTESIAN_POINT ( 'NONE',  ( 97.48942487598446860, -34.74365074496812156, 216.1641967044829755 ) ) ;
#58981 = CARTESIAN_POINT ( 'NONE',  ( 99.89301282343141963, -29.72232929382336053, 125.7099027331620960 ) ) ;
#58982 = CARTESIAN_POINT ( 'NONE',  ( 162.0667039024470171, -79.67844715994088745, 222.2178068554179902 ) ) ;
#58983 = CARTESIAN_POINT ( 'NONE',  ( 97.77247047105220190, -32.00675585678803969, 46.95276813305393659 ) ) ;
#58984 = FACE_OUTER_BOUND ( 'NONE', #53707, .T. ) ;
#58985 = EDGE_LOOP ( 'NONE', ( #35743, #21114 ) ) ;
#58986 = CARTESIAN_POINT ( 'NONE',  ( 110.1977257015883822, -27.19759275805366627, 170.8237533411364382 ) ) ;
#58987 = EDGE_CURVE ( 'NONE', #61997, #56720, #32691, .T. ) ;
#58988 = VECTOR ( 'NONE', #70741, 1000.000000000000000 ) ;
#58989 = DIRECTION ( 'NONE',  ( 0.000000000000000000, 1.000000000000000000, 0.000000000000000000 ) ) ;
#58990 = ORIENTED_EDGE ( 'NONE', *, *, #56542, .T. ) ;
#58991 = VECTOR ( 'NONE', #35120, 1000.000000000000000 ) ;
#58992 = DIRECTION ( 'NONE',  ( 0.000000000000000000, 0.000000000000000000, 1.000000000000000000 ) ) ;
#58993 = CIRCLE ( 'NONE', #9676, 3.174999999999983391 ) ;
#58994 = CARTESIAN_POINT ( 'NONE',  ( 67.06670390244701707, -79.67844715994098692, 222.2178068554179902 ) ) ;
#58995 = CARTESIAN_POINT ( 'NONE',  ( 96.54020141486694229, -31.34005042439572009, 245.9499109901969689 ) ) ;
#58996 = CARTESIAN_POINT ( 'NONE',  ( 163.5667039024460223, -22.48495420874110806, 342.9256252759119548 ) ) ;
#58997 = AXIS2_PLACEMENT_3D ( 'NONE', #61643, #42542, #28945 ) ;
#58998 = EDGE_CURVE ( 'NONE', #18060, #38962, #31909, .T. ) ;
#58999 = CARTESIAN_POINT ( 'NONE',  ( 83.06670390244796920, -64.87844715994098976, 225.9838068554150254 ) ) ;
#59000 = DIRECTION ( 'NONE',  ( 4.299999999999999979E-14, -1.000000000000000000, 0.000000000000000000 ) ) ;
#59001 = CARTESIAN_POINT ( 'NONE',  ( 115.5572469886287479, -35.80043457063792545, 278.3352769709341032 ) ) ;
#59003 = CARTESIAN_POINT ( 'NONE',  ( 117.0854383170105564, -39.53109055650221393, 94.60991099019693706 ) ) ;
#59002 = PLANE ( 'NONE',  #60697 ) ;
#59004 = CARTESIAN_POINT ( 'NONE',  ( 109.5833183008944474, 58.35583844470681214, 70.96735860772342619 ) ) ;
#59005 = CARTESIAN_POINT ( 'NONE',  ( 98.80516515778722919, -28.16326830255935221, 115.6870538473389587 ) ) ;
#59006 = VERTEX_POINT ( 'NONE', #37849 ) ;
#59007 = DIRECTION ( 'NONE',  ( 0.000000000000000000, 0.000000000000000000, 1.000000000000000000 ) ) ;
#59008 = EDGE_LOOP ( 'NONE', ( #76860, #43409, #36940, #9453, #75002 ) ) ;
#59009 = FACE_OUTER_BOUND ( 'NONE', #17846, .T. ) ;
#59010 = CYLINDRICAL_SURFACE ( 'NONE', #68243, 9.999999999999998224 ) ;
#59011 = B_SPLINE_CURVE_WITH_KNOTS ( 'NONE', 3,
 ( #59107, #31859, #87285, #59551, #11879, #45469 ),
 .UNSPECIFIED., .F., .F.,
 ( 4, 2, 4 ),
 ( 0.000000000000000000, 0.5000000000000000000, 1.000000000000000000 ),
 .UNSPECIFIED. ) ;
#59012 = CARTESIAN_POINT ( 'NONE',  ( -31.27367473141074683, 64.60000000000000853, 74.45358409497265484 ) ) ;
#59014 = ORIENTED_EDGE ( 'NONE', *, *, #29123, .T. ) ;
#59013 = EDGE_CURVE ( 'NONE', #32410, #74769, #83470, .T. ) ;
#59015 = CARTESIAN_POINT ( 'NONE',  ( 34.92499999999999716, 69.84999999999999432, 342.8999999999999773 ) ) ;
#59017 = ORIENTED_EDGE ( 'NONE', *, *, #85815, .F. ) ;
#59016 = CARTESIAN_POINT ( 'NONE',  ( 110.1710482807090585, -46.72786414817543488, 97.81562527591097478 ) ) ;
#59018 = LINE ( 'NONE', #87202, #3060 ) ;
#59019 = DIRECTION ( 'NONE',  ( -0.000000000000000000, -0.000000000000000000, 1.000000000000000000 ) ) ;
#59020 = AXIS2_PLACEMENT_3D ( 'NONE', #84063, #43588, #9098 ) ;
#59021 = FACE_OUTER_BOUND ( 'NONE', #72766, .T. ) ;
#59022 = ORIENTED_EDGE ( 'NONE', *, *, #32811, .T. ) ;
#59023 = CARTESIAN_POINT ( 'NONE',  ( 118.9289135900544494, -36.16662986141290048, 118.8641967044819836 ) ) ;
#59024 = SURFACE_SIDE_STYLE ('',( #10891 ) ) ;
#59025 = DIRECTION ( 'NONE',  ( -4.299999999999999979E-14, 1.000000000000000000, 0.000000000000000000 ) ) ;
#59026 = DIRECTION ( 'NONE',  ( 1.075267683398002218E-15, -1.000000000000000000, 3.100000000000000044E-14 ) ) ;
#59027 = CARTESIAN_POINT ( 'NONE',  ( -462.0260000000000105, 53.97500000000000142, -3.174999999999999822 ) ) ;
#59028 = ORIENTED_EDGE ( 'NONE', *, *, #63567, .T. ) ;
#59029 = EDGE_CURVE ( 'NONE', #49695, #62712, #86390, .T. ) ;
#59030 = ORIENTED_EDGE ( 'NONE', *, *, #71995, .T. ) ;
#59031 = CYLINDRICAL_SURFACE ( 'NONE', #79465, 2.999999999999999112 ) ;
#59032 = EDGE_CURVE ( 'NONE', #84350, #26697, #31458, .T. ) ;
#59033 = CARTESIAN_POINT ( 'NONE',  ( 188.5667039024479834, -67.87844715994100397, 257.2178068554150059 ) ) ;
#59034 = EDGE_CURVE ( 'NONE', #82293, #68666, #44191, .T. ) ;
#59035 = FACE_OUTER_BOUND ( 'NONE', #76568, .T. ) ;
#59036 = ADVANCED_FACE ( 'NONE', ( #73239 ), #25101, .T. ) ;
#59038 = DIRECTION ( 'NONE',  ( -0.4999999999999985567, -0.8660254037844395958, 2.688821387764040899E-14 ) ) ;
#59037 = DIRECTION ( 'NONE',  ( 0.000000000000000000, 0.000000000000000000, -1.000000000000000000 ) ) ;
#59039 = FACE_OUTER_BOUND ( 'NONE', #78895, .T. ) ;
#59040 = VECTOR ( 'NONE', #64187, 1000.000000000000000 ) ;
#59041 = ORIENTED_EDGE ( 'NONE', *, *, #23105, .T. ) ;
#59042 = CARTESIAN_POINT ( 'NONE',  ( 165.2748236753140247, -30.08671355700301575, -5.074374724088000832 ) ) ;
#59043 = CARTESIAN_POINT ( 'NONE',  ( 113.2095242374419541, -45.08419629851108823, 179.0689586092439640 ) ) ;
#59045 = ORIENTED_EDGE ( 'NONE', *, *, #9194, .F. ) ;
#59044 = CYLINDRICAL_SURFACE ( 'NONE', #73362, 3.250000000000002665 ) ;
#59046 = CARTESIAN_POINT ( 'NONE',  ( 115.1412022171004281, -43.23618977845870148, 39.27467289495795200 ) ) ;
#59047 = DIRECTION ( 'NONE',  ( 0.000000000000000000, 0.000000000000000000, -1.000000000000000000 ) ) ;
#59048 = CARTESIAN_POINT ( 'NONE',  ( 1.387778780781445676E-14, 223.9999999999999716, 97.27542076772557778 ) ) ;
#59049 = ORIENTED_EDGE ( 'NONE', *, *, #85322, .F. ) ;
#59050 = CARTESIAN_POINT ( 'NONE',  ( 0.000000000000000000, 103.1240000000000236, 0.000000000000000000 ) ) ;
#59051 = AXIS2_PLACEMENT_3D ( 'NONE', #64751, #57930, #50665 ) ;
#59052 = VECTOR ( 'NONE', #88134, 1000.000000000000000 ) ;
#59053 = ORIENTED_EDGE ( 'NONE', *, *, #16668, .T. ) ;
#59054 = ORIENTED_EDGE ( 'NONE', *, *, #34124, .F. ) ;
#59055 = CARTESIAN_POINT ( 'NONE',  ( 99.81674604704261355, -31.63341061165540680, 202.2701547344679796 ) ) ;
#59056 = AXIS2_PLACEMENT_3D ( 'NONE', #59136, #86871, #79619 ) ;
#59057 = CARTESIAN_POINT ( 'NONE',  ( 116.1804594027163375, -40.96476762480074996, 25.56312527591098060 ) ) ;
#59058 = VECTOR ( 'NONE', #79902, 1000.000000000000000 ) ;
#59059 = VECTOR ( 'NONE', #8852, 1000.000000000000000 ) ;
#59060 = CARTESIAN_POINT ( 'NONE',  ( -99.76704648669993958, 88.91113633199481114, 84.21071524772808914 ) ) ;
#59061 = EDGE_CURVE ( 'NONE', #23464, #71527, #47194, .T. ) ;
#59062 = CARTESIAN_POINT ( 'NONE',  ( 51.56670390244799762, -33.35206098992650681, -5.074374724088000832 ) ) ;
#59063 = CARTESIAN_POINT ( 'NONE',  ( 41.56648329127398966, -18.82844715994071194, 198.9256252759119832 ) ) ;
#59064 = ORIENTED_EDGE ( 'NONE', *, *, #62097, .F. ) ;
#59065 = DIRECTION ( 'NONE',  ( 0.000000000000000000, -1.000000000000000000, 0.000000000000000000 ) ) ;
#59066 = CARTESIAN_POINT ( 'NONE',  ( 115.8196560889659139, -31.72004084542335534, 35.23981128565909415 ) ) ;
#59067 = ORIENTED_EDGE ( 'NONE', *, *, #15977, .T. ) ;
#59068 = CARTESIAN_POINT ( 'NONE',  ( 115.8883252675857847, -30.10835006627621269, 264.3508633711492735 ) ) ;
#59069 = CARTESIAN_POINT ( 'NONE',  ( 248.6659999999999968, 52.73749999999999716, -2.903194600000015502 ) ) ;
#59070 = VERTEX_POINT ( 'NONE', #82328 ) ;
#59071 = AXIS2_PLACEMENT_3D ( 'NONE', #4403, #58453, #86183 ) ;
#59072 = DIRECTION ( 'NONE',  ( 1.000000000000000000, 4.299999999999999979E-14, 1.000000000000000078E-15 ) ) ;
#59073 = DIRECTION ( 'NONE',  ( 0.000000000000000000, 0.000000000000000000, -1.000000000000000000 ) ) ;
#59074 = CARTESIAN_POINT ( 'NONE',  ( 72.96458098368701428, 127.0000000000000000, -80.90208098368670164 ) ) ;
#59075 = CIRCLE ( 'NONE', #67783, 3.299999999999997158 ) ;
#59076 = FACE_OUTER_BOUND ( 'NONE', #30914, .T. ) ;
#59077 = AXIS2_PLACEMENT_3D ( 'NONE', #77569, #62589, #29426 ) ;
#59078 = CARTESIAN_POINT ( 'NONE',  ( 116.4163124136858443, -41.43834035574819552, 199.4556252759109611 ) ) ;
#59079 = LINE ( 'NONE', #4588, #58674 ) ;
#59080 = AXIS2_PLACEMENT_3D ( 'NONE', #76111, #77023, #13890 ) ;
#59081 = ORIENTED_EDGE ( 'NONE', *, *, #80079, .F. ) ;
#59082 = CARTESIAN_POINT ( 'NONE',  ( 100.3832715781272356, -28.67167693828054453, 36.62705384733894221 ) ) ;
#59083 = EDGE_CURVE ( 'NONE', #29939, #49937, #54448, .T. ) ;
#59084 = DIRECTION ( 'NONE',  ( 0.000000000000000000, 0.000000000000000000, -1.000000000000000000 ) ) ;
#59085 = CARTESIAN_POINT ( 'NONE',  ( 97.21658504226680009, -33.31410993950169086, 286.0613395616252888 ) ) ;
#59086 = EDGE_CURVE ( 'NONE', #88388, #121, #45760, .T. ) ;
#59087 = ORIENTED_EDGE ( 'NONE', *, *, #29402, .T. ) ;
#59088 = EDGE_CURVE ( 'NONE', #65725, #45672, #28341, .T. ) ;
#59089 = CARTESIAN_POINT ( 'NONE',  ( 81.70522810116327150, -16.51875982968476109, 2.060081176871058517 ) ) ;
#59090 = CARTESIAN_POINT ( 'NONE',  ( 97.92325040394680968, -40.78074430601089517, 17.65808851064360141 ) ) ;
#59091 = CARTESIAN_POINT ( 'NONE',  ( 115.0352805544412718, -42.91097007997968404, 153.3027619676027484 ) ) ;
#59092 = CARTESIAN_POINT ( 'NONE',  ( 99.95702547362903090, -40.74009991652987139, 134.5538046553059530 ) ) ;
#59093 = CARTESIAN_POINT ( 'NONE',  ( 101.6393319275751992, -45.65599671332518028, 243.1413395616249886 ) ) ;
#59094 = ADVANCED_FACE ( 'NONE', ( #40517 ), #60500, .F. ) ;
#59095 = CARTESIAN_POINT ( 'NONE',  ( 0.000000000000000000, 210.0000000000000000, 154.6557476874258441 ) ) ;
#59096 = ORIENTED_EDGE ( 'NONE', *, *, #47725, .F. ) ;
#59097 = ADVANCED_FACE ( 'NONE', ( #41399 ), #53672, .T. ) ;
#59098 = CARTESIAN_POINT ( 'NONE',  ( 136.1637134158967513, -38.51083119283578071, 2.376725019071385336 ) ) ;
#59099 = ORIENTED_EDGE ( 'NONE', *, *, #14538, .T. ) ;
#59101 = ORIENTED_EDGE ( 'NONE', *, *, #69384, .F. ) ;
#59100 = AXIS2_PLACEMENT_3D ( 'NONE', #48860, #89791, #21188 ) ;
#59102 = ADVANCED_FACE ( 'NONE', ( #61401 ), #11927, .F. ) ;
#59103 = EDGE_CURVE ( 'NONE', #2140, #42491, #34143, .T. ) ;
#59104 = DIRECTION ( 'NONE',  ( 2.098553464303459752E-16, 1.000000000000000000, 0.000000000000000000 ) ) ;
#59105 = ORIENTED_EDGE ( 'NONE', *, *, #20140, .F. ) ;
#59106 = VERTEX_POINT ( 'NONE', #61841 ) ;
#59107 = CARTESIAN_POINT ( 'NONE',  ( 116.3212776292296127, -32.94146857471318413, 10.13562527591094309 ) ) ;
#59108 = LINE ( 'NONE', #59552, #15316 ) ;
#59109 = ADVANCED_FACE ( 'NONE', ( #6021 ), #12833, .F. ) ;
#59110 = CARTESIAN_POINT ( 'NONE',  ( 49.21213752015856358, -29.73316016639572368, 193.9678068554150911 ) ) ;
#59111 = CARTESIAN_POINT ( 'NONE',  ( 108.8156685800011303, -28.36903548837926792, 139.3352769709339896 ) ) ;
#59112 = CARTESIAN_POINT ( 'NONE',  ( 96.64195684025510502, -42.47035700268206426, 26.72705384733997747 ) ) ;
#59113 = ORIENTED_EDGE ( 'NONE', *, *, #73381, .T. ) ;
#59114 = ADVANCED_FACE ( 'NONE', ( #48207, #6893 ), #74152, .F. ) ;
#59115 = CARTESIAN_POINT ( 'NONE',  ( -90.31351860656789654, 74.16967745525859357, -76.80536679343883577 ) ) ;
#59117 = ORIENTED_EDGE ( 'NONE', *, *, #56137, .F. ) ;
#59116 = EDGE_CURVE ( 'NONE', #28057, #36904, #5138, .T. ) ;
#59118 = DIRECTION ( 'NONE',  ( 0.000000000000000000, 1.000000000000000000, 0.000000000000000000 ) ) ;
#59119 = EDGE_LOOP ( 'NONE', ( #41100, #51557, #41231, #5495 ) ) ;
#59120 = CARTESIAN_POINT ( 'NONE',  ( 97.81493411881378108, -40.51644251795452334, 167.6359250042934264 ) ) ;
#59121 = DIRECTION ( 'NONE',  ( 2.900000000000000265E-14, -2.000000000000000155E-15, 1.000000000000000000 ) ) ;
#59122 = CARTESIAN_POINT ( 'NONE',  ( 80.06648329127401098, -41.22944715994105280, 4.925625275910944012 ) ) ;
#59124 = CARTESIAN_POINT ( 'NONE',  ( -17.13243906362141900, 54.97499999999996589, 42.79834678115690849 ) ) ;
#59123 = CIRCLE ( 'NONE', #9817, 38.10000000000000142 ) ;
#59125 = ORIENTED_EDGE ( 'NONE', *, *, #18270, .F. ) ;
#59126 = CARTESIAN_POINT ( 'NONE',  ( 102.3791524630845799, -47.61053145109372764, 287.2527681330536780 ) ) ;
#59127 = CARTESIAN_POINT ( 'NONE',  ( 106.2487395568334421, -26.25713557174866253, 21.13848241876792144 ) ) ;
#59128 = SURFACE_SIDE_STYLE ('',( #51417 ) ) ;
#59130 = FACE_OUTER_BOUND ( 'NONE', #77435, .T. ) ;
#59129 = DIRECTION ( 'NONE',  ( -1.000000000000000000, 0.000000000000000000, 0.000000000000000000 ) ) ;
#59131 = CARTESIAN_POINT ( 'NONE',  ( -23.75871628398702384, 82.54999999999999716, 320.6630000000000109 ) ) ;
#59132 = CARTESIAN_POINT ( 'NONE',  ( 193.0374249753375011, -23.42844715993432558, 249.9678068554149775 ) ) ;
#59133 = DIRECTION ( 'NONE',  ( 0.000000000000000000, 1.000000000000000000, 0.000000000000000000 ) ) ;
#59134 = ADVANCED_FACE ( 'NONE', ( #6450, #81877 ), #89132, .T. ) ;
#59135 = AXIS2_PLACEMENT_3D ( 'NONE', #12062, #27034, #81126 ) ;
#59136 = CARTESIAN_POINT ( 'NONE',  ( 154.5667039024469886, -67.87844715994090450, 120.2178068554179902 ) ) ;
#59137 = ADVANCED_FACE ( 'NONE', ( #20091 ), #89577, .T. ) ;
#59138 = FACE_BOUND ( 'NONE', #9535, .T. ) ;
#59139 = EDGE_CURVE ( 'NONE', #45628, #84598, #34597, .T. ) ;
#59140 = VECTOR ( 'NONE', #67839, 1000.000000000000000 ) ;
#59141 = CARTESIAN_POINT ( 'NONE',  ( 146.6727020897380100, -77.84109957281390280, 247.0017837352540084 ) ) ;
#59142 = CARTESIAN_POINT ( 'NONE',  ( 98.38709084977145380, -42.09077886617859576, 11.76800622829193799 ) ) ;
#59143 = CARTESIAN_POINT ( 'NONE',  ( 96.85852386828889848, -34.61283385893091236, 212.1641967044819808 ) ) ;
#59144 = CARTESIAN_POINT ( 'NONE',  ( 115.0392540076567656, -43.53489519176116573, 59.26419670448196086 ) ) ;
#59145 = AXIS2_PLACEMENT_3D ( 'NONE', #2795, #38630, #37306 ) ;
#59146 = B_SPLINE_CURVE_WITH_KNOTS ( 'NONE', 3,
 ( #62773, #22356, #42319, #14189, #13739, #50028, #84141, #15542, #70050, #7818, #21914, #49581, #36434, #21459, #43218, #70961, #77313, #42761, #76865, #8274, #70501, #69153, #62329, #35062, #1466, #6922, #29607, #22809, #83243, #57296, #35971, #75969, #29163, #8733, #85038, #34624, #64134, #63683, #84593, #21004, #28249, #56849, #111, #27809, #55942, #55488, #48680, #76412, #83687 ),
 .UNSPECIFIED., .F., .F.,
 ( 4, 2, 2, 2, 2, 2, 2, 2, 2, 2, 2, 2, 2, 2, 2, 1, 2, 2, 2, 2, 2, 2, 2, 2, 4 ),
 ( 0.01987186023414422645, 0.02111356671950572958, 0.02235527320486722924, 0.02483868617559022510, 0.02608039266095170394, 0.02732209914631318279, 0.02980551211703615089, 0.03228892508775912246, 0.03353063157312059783, 0.03477233805848208015, 0.03725575102920501008, 0.03849745751456647852, 0.03973916399992794002, 0.04222257697065086302, 0.04346428345601233145, 0.04470598994137378601, 0.04594769642673525445, 0.04718940291209671595, 0.04967281588281963894, 0.05091452236818108656, 0.05215622885354252725, 0.05463964182426545024, 0.05588134830962691868, 0.05712305479498837324, 0.05960646776571126848 ),
 .UNSPECIFIED. ) ;
#59147 = EDGE_CURVE ( 'NONE', #37193, #79159, #74845, .T. ) ;
#59148 = VECTOR ( 'NONE', #6192, 1000.000000000000000 ) ;
#59150 = CARTESIAN_POINT ( 'NONE',  ( 116.3212776292270973, -32.94146857470704504, 49.13562527591097506 ) ) ;
#59149 = DIRECTION ( 'NONE',  ( 1.000000000000000000, 4.299999999999999979E-14, 1.000000000000000078E-15 ) ) ;
#59151 = CARTESIAN_POINT ( 'NONE',  ( 33.91903122894498779, -35.91149509761220315, -5.074374724088000832 ) ) ;
#59152 = AXIS2_PLACEMENT_3D ( 'NONE', #50457, #22327, #72603 ) ;
#59153 = ORIENTED_EDGE ( 'NONE', *, *, #46582, .F. ) ;
#59154 = DIRECTION ( 'NONE',  ( 0.000000000000000000, 0.000000000000000000, -1.000000000000000000 ) ) ;
#59155 = ORIENTED_EDGE ( 'NONE', *, *, #58496, .F. ) ;
#59156 = CARTESIAN_POINT ( 'NONE',  ( 115.5638989210037124, -29.55965564860111527, 70.38419670448092802 ) ) ;
#59158 = ORIENTED_EDGE ( 'NONE', *, *, #42702, .F. ) ;
#59157 = DIRECTION ( 'NONE',  ( 1.000000000000000000, 4.299999999999999979E-14, 1.000000000000000078E-15 ) ) ;
#59159 = PLANE ( 'NONE',  #85306 ) ;
#59160 = CARTESIAN_POINT ( 'NONE',  ( 115.4423046205436094, -29.55243945206544609, 225.4022919425769658 ) ) ;
#59161 = CARTESIAN_POINT ( 'NONE',  ( 98.54715120129765182, -41.97616799658815268, 252.7661222402538499 ) ) ;
#59162 = CARTESIAN_POINT ( 'NONE',  ( 107.0667039024479834, -36.72944715994100306, 239.5838068554170093 ) ) ;
#59163 = PLANE ( 'NONE',  #16752 ) ;
#59164 = CARTESIAN_POINT ( 'NONE',  ( 80.06648329127398256, -15.97944715994105813, 8.225625275910942946 ) ) ;
#59165 = DIRECTION ( 'NONE',  ( -1.000000000000000078E-15, 1.000000000000000083E-30, 1.000000000000000000 ) ) ;
#59166 = DIRECTION ( 'NONE',  ( -1.000000000000000000, -3.999999999999999995E-14, -1.000000000000000078E-15 ) ) ;
#59167 = CARTESIAN_POINT ( 'NONE',  ( 96.71010325458811963, -37.26253042779857338, 121.3794347997209684 ) ) ;
#59168 = AXIS2_PLACEMENT_3D ( 'NONE', #65467, #38642, #58205 ) ;
#59169 = ORIENTED_EDGE ( 'NONE', *, *, #69116, .T. ) ;
#59170 = VERTEX_POINT ( 'NONE', #32804 ) ;
#59171 = AXIS2_PLACEMENT_3D ( 'NONE', #468, #49040, #21366 ) ;
#59172 = CARTESIAN_POINT ( 'NONE',  ( 107.8890265924388814, -27.36996276949999185, 106.4263452106589654 ) ) ;
#59173 = DIRECTION ( 'NONE',  ( -3.360405532702990443E-14, 1.000000000000000000, 0.000000000000000000 ) ) ;
#59175 = DIRECTION ( 'NONE',  ( 1.000000000000000000, 3.999999999999999995E-14, 1.000000000000000078E-15 ) ) ;
#59174 = CARTESIAN_POINT ( 'NONE',  ( 116.2522929705882859, -40.08866370952546987, 214.5470538473389581 ) ) ;
#59176 = FACE_BOUND ( 'NONE', #66599, .T. ) ;
#59177 = CARTESIAN_POINT ( 'NONE',  ( 2.332952152375709937E-14, 127.0000000000000000, 190.5000000000000000 ) ) ;
#59178 = CARTESIAN_POINT ( 'NONE',  ( 118.1261869548600600, 74.80137413886471620, 10.09682577435512840 ) ) ;
#59179 = FACE_OUTER_BOUND ( 'NONE', #44291, .T. ) ;
#59180 = LINE ( 'NONE', #23366, #57951 ) ;
#59181 = CARTESIAN_POINT ( 'NONE',  ( 61.68306511546570903, -72.55869591834559174, 542.9756252759101471 ) ) ;
#59182 = CARTESIAN_POINT ( 'NONE',  ( 114.4965984691701664, -29.44205611023136626, 149.4441967044819819 ) ) ;
#59183 = EDGE_LOOP ( 'NONE', ( #54385, #66752, #69344, #8417 ) ) ;
#59184 = ORIENTED_EDGE ( 'NONE', *, *, #36164, .T. ) ;
#59185 = CARTESIAN_POINT ( 'NONE',  ( 0.000000000000000000, 114.2999999999999972, 0.000000000000000000 ) ) ;
#59186 = CARTESIAN_POINT ( 'NONE',  ( 115.0889047306568074, -30.61763669006579747, 150.3439586082987205 ) ) ;
#59187 = VECTOR ( 'NONE', #36800, 1000.000000000000000 ) ;
#59188 = DIRECTION ( 'NONE',  ( 0.000000000000000000, 0.000000000000000000, -1.000000000000000000 ) ) ;
#59189 = CARTESIAN_POINT ( 'NONE',  ( 146.0667039024470455, -121.7784471599409102, 55.21780685541800437 ) ) ;
#59190 = AXIS2_PLACEMENT_3D ( 'NONE', #48758, #56015, #87553 ) ;
#59191 = VECTOR ( 'NONE', #69886, 1000.000000000000000 ) ;
#59192 = CYLINDRICAL_SURFACE ( 'NONE', #34985, 0.2500000000000039968 ) ;
#59193 = EDGE_CURVE ( 'NONE', #89263, #24990, #15064, .T. ) ;
#59194 = CARTESIAN_POINT ( 'NONE',  ( 98.16810232779933187, -31.29751870953477422, 170.8899109901960003 ) ) ;
#59195 = EDGE_CURVE ( 'NONE', #40033, #80239, #15517, .T. ) ;
#59196 = DIRECTION ( 'NONE',  ( 0.000000000000000000, 1.000000000000000000, 0.000000000000000000 ) ) ;
#59197 = ORIENTED_EDGE ( 'NONE', *, *, #16874, .F. ) ;
#59199 = ORIENTED_EDGE ( 'NONE', *, *, #76976, .T. ) ;
#59198 = EDGE_LOOP ( 'NONE', ( #6624, #59158, #332, #39056 ) ) ;
#59201 = EDGE_CURVE ( 'NONE', #37855, #47447, #55090, .T. ) ;
#59200 = AXIS2_PLACEMENT_3D ( 'NONE', #10061, #37768, #65021 ) ;
#59202 = CARTESIAN_POINT ( 'NONE',  ( 117.0649963017320090, -35.84647789964886755, 64.89715894876896130 ) ) ;
#59203 = DIRECTION ( 'NONE',  ( 0.000000000000000000, 0.000000000000000000, 1.000000000000000000 ) ) ;
#59204 = CARTESIAN_POINT ( 'NONE',  ( -21.42842094847162926, 53.97499999999997300, 41.97446389704172987 ) ) ;
#59205 = CARTESIAN_POINT ( 'NONE',  ( 101.2699428795238106, -44.12381293138377458, 273.4911071154209594 ) ) ;
#59206 = CIRCLE ( 'NONE', #62134, 4.874999999999990230 ) ;
#59207 = EDGE_CURVE ( 'NONE', #77463, #69696, #27784, .T. ) ;
#59208 = CARTESIAN_POINT ( 'NONE',  ( 118.5256205435842958, -36.72944715994100306, 300.2406250056037038 ) ) ;
#59209 = ORIENTED_EDGE ( 'NONE', *, *, #21925, .F. ) ;
#59210 = VECTOR ( 'NONE', #31710, 1000.000000000000000 ) ;
#59211 = CIRCLE ( 'NONE', #20076, 11.17600000000001970 ) ;
#59212 = DIRECTION ( 'NONE',  ( -0.7017307308175085856, -0.7121747104283100427, -0.01952340269210590604 ) ) ;
#59213 = CARTESIAN_POINT ( 'NONE',  ( 81.63820548406826560, -16.47341874818874174, 7.827313014937786306 ) ) ;
#59214 = VERTEX_POINT ( 'NONE', #70478 ) ;
#59215 = VERTEX_POINT ( 'NONE', #21886 ) ;
#59216 = EDGE_CURVE ( 'NONE', #23298, #71348, #49106, .T. ) ;
#59217 = CARTESIAN_POINT ( 'NONE',  ( 0.000000000000000000, 1.270000000000000018, 0.000000000000000000 ) ) ;
#59218 = ORIENTED_EDGE ( 'NONE', *, *, #36053, .F. ) ;
#59219 = VERTEX_POINT ( 'NONE', #76835 ) ;
#59220 = CARTESIAN_POINT ( 'NONE',  ( 115.8239080365019902, -31.72738345397822002, 155.2397836611081061 ) ) ;
#59221 = CIRCLE ( 'NONE', #27331, 2.517500000000000071 ) ;
#59222 = CARTESIAN_POINT ( 'NONE',  ( 105.5073833390055853, -45.15143093073633196, 11.85241982807799843 ) ) ;
#59223 = CARTESIAN_POINT ( 'NONE',  ( 108.6784406349466110, -26.40724015326817664, 189.9527681330539792 ) ) ;
#59224 = CARTESIAN_POINT ( 'NONE',  ( 101.9951592035502017, -45.85337710724439830, 187.1727681330539781 ) ) ;
#59225 = DIRECTION ( 'NONE',  ( 1.000000000000000000, 3.999999999999999995E-14, 1.000000000000000078E-15 ) ) ;
#59226 = CARTESIAN_POINT ( 'NONE',  ( 109.2119659639152047, -48.38412513495681111, 273.7213395616252569 ) ) ;
#59227 = CARTESIAN_POINT ( 'NONE',  ( 100.8875087413080678, -44.70025551109045381, 98.05342680442112169 ) ) ;
#59228 = LINE ( 'NONE', #80149, #42452 ) ;
#59229 = ORIENTED_EDGE ( 'NONE', *, *, #49249, .F. ) ;
#59230 = EDGE_CURVE ( 'NONE', #61133, #75751, #76386, .T. ) ;
#59231 = ORIENTED_EDGE ( 'NONE', *, *, #63667, .F. ) ;
#59232 = CIRCLE ( 'NONE', #82485, 38.10000000000000142 ) ;
#59234 = ADVANCED_FACE ( 'NONE', ( #78204 ), #49555, .F. ) ;
#59233 = CIRCLE ( 'NONE', #73710, 3.968750000000520473 ) ;
#59235 = CARTESIAN_POINT ( 'NONE',  ( -41.60202597009397607, 65.59999999999998010, 50.85338361873603219 ) ) ;
#59236 = CARTESIAN_POINT ( 'NONE',  ( 112.4772085026190354, -45.73365988577116070, 238.0070538473389377 ) ) ;
#59237 = ORIENTED_EDGE ( 'NONE', *, *, #29177, .T. ) ;
#59238 = CARTESIAN_POINT ( 'NONE',  ( 97.42502596350711030, -42.13512825026991493, 181.7451490854349743 ) ) ;
#59239 = DIRECTION ( 'NONE',  ( 0.000000000000000000, 0.000000000000000000, -1.000000000000000000 ) ) ;
#59240 = CARTESIAN_POINT ( 'NONE',  ( -14.47561641184040226, 67.58393596072598086, 35.26458586194669920 ) ) ;
#59241 = DIRECTION ( 'NONE',  ( 0.000000000000000000, 0.000000000000000000, -1.000000000000000000 ) ) ;
#59242 = DIRECTION ( 'NONE',  ( -0.9963424814100679816, 0.08544974978095724871, 0.000000000000000000 ) ) ;
#59245 = CARTESIAN_POINT ( 'NONE',  ( 112.3272512417296554, -28.22507648531182056, 285.6356252759109680 ) ) ;
#59244 = DIRECTION ( 'NONE',  ( -0.5000000000000129896, -0.8660254037844311581, 0.000000000000000000 ) ) ;
#59243 = CARTESIAN_POINT ( 'NONE',  ( 2.849336855536075284E-14, 184.0000000000000000, 111.9860621927989683 ) ) ;
#59246 = CYLINDRICAL_SURFACE ( 'NONE', #29273, 4.875000000000017764 ) ;
#59247 = DIRECTION ( 'NONE',  ( 0.000000000000000000, 0.000000000000000000, -1.000000000000000000 ) ) ;
#59248 = DIRECTION ( 'NONE',  ( 0.000000000000000000, 0.000000000000000000, -1.000000000000000000 ) ) ;
#59249 = CARTESIAN_POINT ( 'NONE',  ( 67.41169775273984044, -137.4659453879007742, 246.6330592172282081 ) ) ;
#59250 = FACE_OUTER_BOUND ( 'NONE', #26700, .T. ) ;
#59251 = DIRECTION ( 'NONE',  ( 0.000000000000000000, 0.000000000000000000, -1.000000000000000000 ) ) ;
#59253 = VERTEX_POINT ( 'NONE', #35944 ) ;
#59252 = CARTESIAN_POINT ( 'NONE',  ( 99.02250180400051249, -33.12202411512905798, 195.5838068554173788 ) ) ;
#59254 = AXIS2_PLACEMENT_3D ( 'NONE', #81174, #33886, #12562 ) ;
#59255 = DIRECTION ( 'NONE',  ( -1.000000000000000078E-15, 0.000000000000000000, -1.000000000000000000 ) ) ;
#59256 = CARTESIAN_POINT ( 'NONE',  ( 96.65194983638532733, -35.53535514585328059, 206.2356252759109623 ) ) ;
#59257 = CARTESIAN_POINT ( 'NONE',  ( 103.2054172826541816, -46.45125265344608323, 113.2756252759109827 ) ) ;
#59258 = CARTESIAN_POINT ( 'NONE',  ( 109.3463552500793554, -26.51205201248422583, 220.9013395616249795 ) ) ;
#59259 = FACE_OUTER_BOUND ( 'NONE', #43045, .T. ) ;
#59260 = EDGE_CURVE ( 'NONE', #29962, #32906, #29141, .T. ) ;
#59261 = LINE ( 'NONE', #45177, #72166 ) ;
#59263 = CARTESIAN_POINT ( 'NONE',  ( 51.42025729304100423, -33.70561438051981185, 237.4678068554150059 ) ) ;
#59262 = CARTESIAN_POINT ( 'NONE',  ( 172.5664832912729878, -27.82844715994070484, 198.9256252759119832 ) ) ;
#59264 = FACE_OUTER_BOUND ( 'NONE', #10794, .T. ) ;
#59265 = CARTESIAN_POINT ( 'NONE',  ( 126.0667039024479266, -14.72944715994094977, 239.5838068554170377 ) ) ;
#59266 = CARTESIAN_POINT ( 'NONE',  ( 97.78115606164335816, -40.44200917047258770, 66.62962555244023122 ) ) ;
#59267 = AXIS2_PLACEMENT_3D ( 'NONE', #71811, #9581, #62742 ) ;
#59268 = VERTEX_POINT ( 'NONE', #14621 ) ;
#59269 = ORIENTED_EDGE ( 'NONE', *, *, #60158, .F. ) ;
#59270 = CARTESIAN_POINT ( 'NONE',  ( 103.3727720482000620, -29.02797788616916108, 94.85527697093499455 ) ) ;
#59271 = VECTOR ( 'NONE', #63118, 1000.000000000000000 ) ;
#59273 = ORIENTED_EDGE ( 'NONE', *, *, #88043, .F. ) ;
#59272 = LINE ( 'NONE', #30252, #76362 ) ;
#59274 = CARTESIAN_POINT ( 'NONE',  ( 109.2504006710444173, -46.93703897017532967, 103.7441967044829880 ) ) ;
#59275 = CARTESIAN_POINT ( 'NONE',  ( 51.34673845256598668, -29.62846900982231446, 342.9256252759119548 ) ) ;
#59276 = CARTESIAN_POINT ( 'NONE',  ( 32.24491389929978169, -32.11662333284649407, 117.4678068554150485 ) ) ;
#59277 = EDGE_CURVE ( 'NONE', #41907, #74757, #55464, .T. ) ;
#59278 = CARTESIAN_POINT ( 'NONE',  ( 112.1393456483219921, -28.01282278529340530, 175.6564586086265933 ) ) ;
#59279 = VECTOR ( 'NONE', #78943, 1000.000000000000000 ) ;
#59280 = CARTESIAN_POINT ( 'NONE',  ( 100.9974734301594310, -29.01720366022859565, 15.60705384733995871 ) ) ;
#59281 = EDGE_LOOP ( 'NONE', ( #65046, #73044, #62126, #31618, #81570, #57702, #32736, #3440, #84379, #70033, #17454, #19634 ) ) ;
#59282 = ORIENTED_EDGE ( 'NONE', *, *, #51439, .T. ) ;
#59283 = ORIENTED_EDGE ( 'NONE', *, *, #79689, .T. ) ;
#59284 = ADVANCED_FACE ( 'NONE', ( #22328 ), #43192, .F. ) ;
#59285 = DIRECTION ( 'NONE',  ( 0.000000000000000000, -0.4999999999999928946, -0.8660254037844428154 ) ) ;
#59287 = DIRECTION ( 'NONE',  ( 1.000000000000000078E-15, -1.000000000000000083E-30, -1.000000000000000000 ) ) ;
#59286 = CARTESIAN_POINT ( 'NONE',  ( 102.8912152862170188, -46.22186109533342346, 128.2346728949579528 ) ) ;
#59288 = CARTESIAN_POINT ( 'NONE',  ( -27.27158787008326968, 184.0000000000000000, 85.23828826961327820 ) ) ;
#59289 = DIRECTION ( 'NONE',  ( 0.000000000000000000, 0.000000000000000000, -1.000000000000000000 ) ) ;
#59290 = AXIS2_PLACEMENT_3D ( 'NONE', #2163, #42567, #70761 ) ;
#59291 = CARTESIAN_POINT ( 'NONE',  ( 107.0664832912739968, 22.62155284005901024, 327.8006252759110453 ) ) ;
#59292 = CARTESIAN_POINT ( 'NONE',  ( -9.373716445341450765, 91.13655357722605288, 130.2196449801177209 ) ) ;
#59293 = CARTESIAN_POINT ( 'NONE',  ( -33.98325472291465132, 8.255000000000000782, -3.174999999999764899 ) ) ;
#59294 = CARTESIAN_POINT ( 'NONE',  ( 117.9019101119220068, -41.46671778014666643, 58.49848241876792798 ) ) ;
#59295 = ORIENTED_EDGE ( 'NONE', *, *, #769, .T. ) ;
#59296 = ORIENTED_EDGE ( 'NONE', *, *, #69189, .F. ) ;
#59297 = CARTESIAN_POINT ( 'NONE',  ( 12.61760061281885825, 84.21489741558210085, 129.9449561063389922 ) ) ;
#59298 = CARTESIAN_POINT ( 'NONE',  ( 186.6899999999999977, 46.38749999999999574, -38.10000000000000142 ) ) ;
#59299 = CARTESIAN_POINT ( 'NONE',  ( 79.72329571771361145, -107.6623471058699835, 250.2178068554180470 ) ) ;
#59300 = CARTESIAN_POINT ( 'NONE',  ( 102.9190449779222405, -43.75998617602524376, 159.9709475124489586 ) ) ;
#59301 = CIRCLE ( 'NONE', #53445, 0.5000000000000004441 ) ;
#59302 = ADVANCED_FACE ( 'NONE', ( #70936, #28224 ), #57272, .F. ) ;
#59303 = EDGE_CURVE ( 'NONE', #30460, #9382, #60297, .T. ) ;
#59304 = CARTESIAN_POINT ( 'NONE',  ( 68.86456684384336313, 93.07500000000001705, 56.22171674193015889 ) ) ;
#59305 = ORIENTED_EDGE ( 'NONE', *, *, #14117, .T. ) ;
#59306 = VERTEX_POINT ( 'NONE', #70027 ) ;
#59307 = CARTESIAN_POINT ( 'NONE',  ( 141.0664832912739826, -8.729447159940995959, 14.92562527591100618 ) ) ;
#59308 = EDGE_CURVE ( 'NONE', #24560, #14127, #28409, .T. ) ;
#59309 = EDGE_LOOP ( 'NONE', ( #3925, #13185, #78583, #7394 ) ) ;
#59310 = ORIENTED_EDGE ( 'NONE', *, *, #81525, .F. ) ;
#59311 = LINE ( 'NONE', #31609, #75295 ) ;
#59312 = CARTESIAN_POINT ( 'NONE',  ( 109.0885512386393259, -27.55405797182273631, 176.3234880678019465 ) ) ;
#59313 = VECTOR ( 'NONE', #25975, 1000.000000000000000 ) ;
#59314 = EDGE_CURVE ( 'NONE', #89556, #43538, #85468, .T. ) ;
#59315 = CARTESIAN_POINT ( 'NONE',  ( 194.5667039024482108, -40.82844715993405060, 180.4678068554150343 ) ) ;
#59316 = DIRECTION ( 'NONE',  ( 1.000000000000000000, 0.000000000000000000, 0.000000000000000000 ) ) ;
#59317 = LINE ( 'NONE', #25702, #14020 ) ;
#59318 = VECTOR ( 'NONE', #2219, 1000.000000000000000 ) ;
#59319 = ORIENTED_EDGE ( 'NONE', *, *, #43210, .F. ) ;
#59321 = ORIENTED_EDGE ( 'NONE', *, *, #34529, .F. ) ;
#59320 = AXIS2_PLACEMENT_3D ( 'NONE', #72948, #43561, #32058 ) ;
#59322 = EDGE_CURVE ( 'NONE', #24293, #48080, #85907, .T. ) ;
#59323 = ORIENTED_EDGE ( 'NONE', *, *, #86029, .T. ) ;
#59324 = ORIENTED_EDGE ( 'NONE', *, *, #40651, .F. ) ;
#59325 = EDGE_CURVE ( 'NONE', #970, #87454, #72265, .T. ) ;
#59326 = CARTESIAN_POINT ( 'NONE',  ( 99.25992742994408502, -40.46556956555936324, 214.5118998934009653 ) ) ;
#59327 = VECTOR ( 'NONE', #465, 1000.000000000000000 ) ;
#59328 = CARTESIAN_POINT ( 'NONE',  ( 107.9474950258210413, -25.68774170017952940, 115.0251490854349612 ) ) ;
#59329 = CARTESIAN_POINT ( 'NONE',  ( 104.2468583329775669, -46.74335657891444384, 22.35848241876792031 ) ) ;
#59330 = DIRECTION ( 'NONE',  ( 6.745093096447288888E-17, 1.000000000000000000, -3.328006943901140051E-31 ) ) ;
#59331 = CARTESIAN_POINT ( 'NONE',  ( 106.6155744189988326, -25.27918481551454732, 323.5352776872487652 ) ) ;
#59332 = PRESENTATION_LAYER_ASSIGNMENT (  '', '', ( #8802 ) ) ;
#59333 = CARTESIAN_POINT ( 'NONE',  ( 113.6144894440835031, -28.61735105040022376, 160.5356252759109736 ) ) ;
#59334 = FACE_OUTER_BOUND ( 'NONE', #49468, .T. ) ;
#59335 = ORIENTED_EDGE ( 'NONE', *, *, #44551, .T. ) ;
#59336 = LINE ( 'NONE', #26614, #56857 ) ;
#59337 = VERTEX_POINT ( 'NONE', #71819 ) ;
#59338 = VERTEX_POINT ( 'NONE', #24117 ) ;
#59339 = VECTOR ( 'NONE', #57923, 1000.000000000000000 ) ;
#59340 = DIRECTION ( 'NONE',  ( 0.000000000000000000, 0.000000000000000000, -1.000000000000000000 ) ) ;
#59341 = VERTEX_POINT ( 'NONE', #44980 ) ;
#59342 = ORIENTED_EDGE ( 'NONE', *, *, #77478, .F. ) ;
#59343 = CARTESIAN_POINT ( 'NONE',  ( 19.56648329127400032, -18.82844715994099971, -5.074374724088000832 ) ) ;
#59344 = ORIENTED_EDGE ( 'NONE', *, *, #82134, .T. ) ;
#59345 = CARTESIAN_POINT ( 'NONE',  ( 116.3192736897089645, -32.94707975126958388, 130.1356252759109680 ) ) ;
#59346 = CARTESIAN_POINT ( 'NONE',  ( 100.9430784815160251, -28.29197455274081463, 75.57562527591093726 ) ) ;
#59347 = PLANE ( 'NONE',  #70720 ) ;
#59348 = CARTESIAN_POINT ( 'NONE',  ( 87.31648329127403940, -46.47944715994105280, -5.074374724089048883 ) ) ;
#59349 = LINE ( 'NONE', #3501, #81866 ) ;
#59350 = CARTESIAN_POINT ( 'NONE',  ( 104.0406618471960201, -46.06530165129709076, 82.32705384733995402 ) ) ;
#59352 = CARTESIAN_POINT ( 'NONE',  ( 98.56907362037671305, -44.95393718666134930, 187.9384824187679612 ) ) ;
#59351 = DIRECTION ( 'NONE',  ( -1.110223024625155531E-13, -1.000000000000000000, 0.000000000000000000 ) ) ;
#59353 = CARTESIAN_POINT ( 'NONE',  ( 102.0648915419311606, -27.97176698159946184, 60.48998952755263758 ) ) ;
#59354 = CARTESIAN_POINT ( 'NONE',  ( 103.1875000000000000, 101.5999999999999943, 3.602774393244745134E-13 ) ) ;
#59355 = ORIENTED_EDGE ( 'NONE', *, *, #48109, .T. ) ;
#59356 = VECTOR ( 'NONE', #58559, 1000.000000000000114 ) ;
#59357 = CARTESIAN_POINT ( 'NONE',  ( 48.45959712127301344, -26.00627455219131789, -5.074374724088000832 ) ) ;
#59358 = LINE ( 'NONE', #80283, #28255 ) ;
#59359 = DIRECTION ( 'NONE',  ( 0.000000000000000000, 0.000000000000000000, 1.000000000000000000 ) ) ;
#59360 = DIRECTION ( 'NONE',  ( 0.000000000000000000, 0.000000000000000000, -1.000000000000000000 ) ) ;
#59362 = ORIENTED_EDGE ( 'NONE', *, *, #23594, .T. ) ;
#59361 = CARTESIAN_POINT ( 'NONE',  ( 109.3464976042218524, -26.51141404309336735, 224.9013395616249511 ) ) ;
#59363 = CARTESIAN_POINT ( 'NONE',  ( -75.61066417432020614, 0.000000000000000000, 177.0380000000000109 ) ) ;
#59364 = CARTESIAN_POINT ( 'NONE',  ( 106.2251562910655309, -47.77378392694726017, 263.5280062282920994 ) ) ;
#59365 = CARTESIAN_POINT ( 'NONE',  ( 102.3735796352302714, -26.67091080359734434, 131.4118157521009778 ) ) ;
#59366 = FACE_OUTER_BOUND ( 'NONE', #56641, .T. ) ;
#59367 = EDGE_CURVE ( 'NONE', #70652, #66586, #38178, .T. ) ;
#59368 = CARTESIAN_POINT ( 'NONE',  ( 12.70000000000000107, 82.54999999999999716, -129.9368274816650910 ) ) ;
#59369 = CARTESIAN_POINT ( 'NONE',  ( 100.5868491334648382, 79.25971567868508316, -83.22961976134665463 ) ) ;
#59370 = CARTESIAN_POINT ( 'NONE',  ( 115.0667039024470313, -104.2784471599421181, -21.78219314458201694 ) ) ;
#59371 = ORIENTED_EDGE ( 'NONE', *, *, #61563, .F. ) ;
#59372 = ORIENTED_EDGE ( 'NONE', *, *, #20290, .T. ) ;
#59373 = VERTEX_POINT ( 'NONE', #86786 ) ;
#59374 = ORIENTED_EDGE ( 'NONE', *, *, #50801, .F. ) ;
#59375 = CARTESIAN_POINT ( 'NONE',  ( 116.7951252702546441, -39.38782979486860825, 73.61479194218726718 ) ) ;
#59376 = CARTESIAN_POINT ( 'NONE',  ( 99.39693184722126773, -28.77005263954443492, 261.6746728949588032 ) ) ;
#59377 = PLANE ( 'NONE',  #76605 ) ;
#59378 = CARTESIAN_POINT ( 'NONE',  ( 131.6688901780889864, -35.37024878623139301, 2.654395752964708866 ) ) ;
#59379 = VECTOR ( 'NONE', #13473, 1000.000000000000000 ) ;
#59381 = DIRECTION ( 'NONE',  ( 0.000000000000000000, 1.000000000000000000, 0.000000000000000000 ) ) ;
#59380 = CARTESIAN_POINT ( 'NONE',  ( 210.5660000000000025, 52.73749999999999716, -44.45000000000000284 ) ) ;
#59382 = CARTESIAN_POINT ( 'NONE',  ( 112.0552156641497703, -28.39979068407086515, 204.0695626852199496 ) ) ;
#59383 = ORIENTED_EDGE ( 'NONE', *, *, #43001, .T. ) ;
#59384 = VERTEX_POINT ( 'NONE', #79089 ) ;
#59385 = AXIS2_PLACEMENT_3D ( 'NONE', #36473, #2398, #55524 ) ;
#59387 = ORIENTED_EDGE ( 'NONE', *, *, #82675, .T. ) ;
#59386 = AXIS2_PLACEMENT_3D ( 'NONE', #72847, #58324, #3369 ) ;
#59388 = EDGE_CURVE ( 'NONE', #89037, #60619, #44084, .T. ) ;
#59389 = DIRECTION ( 'NONE',  ( 0.000000000000000000, 0.000000000000000000, 1.000000000000000000 ) ) ;
#59390 = CARTESIAN_POINT ( 'NONE',  ( 110.8543111526358018, -45.98430318780785342, 182.8856114468024145 ) ) ;
#59391 = LINE ( 'NONE', #87120, #78068 ) ;
#59392 = CARTESIAN_POINT ( 'NONE',  ( 99.72008180067200556, -41.26785689822659009, 8.199678543991950619 ) ) ;
#59393 = CARTESIAN_POINT ( 'NONE',  ( 118.4232890149587405, 93.94641470820114648, -5.620000134942411130 ) ) ;
#59394 = AXIS2_PLACEMENT_3D ( 'NONE', #64706, #23395, #15671 ) ;
#59395 = DIRECTION ( 'NONE',  ( -1.000000000000000000, -4.299999999999999979E-14, -1.000000000000000078E-15 ) ) ;
#59396 = CARTESIAN_POINT ( 'NONE',  ( 142.8838050580813501, -82.11588141944041297, 542.9756252759101471 ) ) ;
#59397 = VERTEX_POINT ( 'NONE', #58607 ) ;
#59398 = CARTESIAN_POINT ( 'NONE',  ( 103.2800637878028454, -27.47401470249857880, 56.38549218839290234 ) ) ;
#59399 = VECTOR ( 'NONE', #27496, 1000.000000000000000 ) ;
#59400 = VERTEX_POINT ( 'NONE', #50911 ) ;
#59401 = CARTESIAN_POINT ( 'NONE',  ( 107.0664832912750057, -36.72944715993903486, 9.125625275910969947 ) ) ;
#59402 = CARTESIAN_POINT ( 'NONE',  ( 115.6923476351215641, -37.43328618085965331, 36.59189989340094940 ) ) ;
#59403 = VECTOR ( 'NONE', #32407, 1000.000000000000000 ) ;
#59404 = DIRECTION ( 'NONE',  ( 0.000000000000000000, 0.000000000000000000, 1.000000000000000000 ) ) ;
#59405 = CARTESIAN_POINT ( 'NONE',  ( 106.0667039024470455, -121.2010968907524529, -19.26696060647547881 ) ) ;
#59406 = ADVANCED_FACE ( 'NONE', ( #45415 ), #72711, .F. ) ;
#59407 = AXIS2_PLACEMENT_3D ( 'NONE', #57110, #58455, #29430 ) ;
#59408 = CARTESIAN_POINT ( 'NONE',  ( -3.286364562888697272, 94.82452044211723319, 118.5111154470731520 ) ) ;
#59409 = ORIENTED_EDGE ( 'NONE', *, *, #16411, .T. ) ;
#59410 = DIRECTION ( 'NONE',  ( -4.299999999999999979E-14, 1.000000000000000000, -4.128053709984630540E-29 ) ) ;
#59411 = CARTESIAN_POINT ( 'NONE',  ( 119.9073604651600249, 56.10210383135144241, -51.64404161576485564 ) ) ;
#59412 = ADVANCED_FACE ( 'NONE', ( #25000 ), #44528, .F. ) ;
#59413 = ORIENTED_EDGE ( 'NONE', *, *, #4173, .F. ) ;
#59414 = CARTESIAN_POINT ( 'NONE',  ( 116.5985118214053813, -29.68807528100325044, 109.3327681330539605 ) ) ;
#59415 = VERTEX_POINT ( 'NONE', #23679 ) ;
#59416 = EDGE_CURVE ( 'NONE', #87084, #27718, #20382, .T. ) ;
#59417 = CARTESIAN_POINT ( 'NONE',  ( 99.32879058785749748, -33.04431300321336806, 75.39527697093394920 ) ) ;
#59418 = PLANE ( 'NONE',  #31508 ) ;
#59419 = CARTESIAN_POINT ( 'NONE',  ( 109.8610415383596148, -27.05157811987473337, 61.28444044875497099 ) ) ;
#59420 = CARTESIAN_POINT ( 'NONE',  ( 61.67079006425787924, -0.9306969701470987344, 394.9756252759102040 ) ) ;
#59421 = EDGE_CURVE ( 'NONE', #15206, #66455, #47207, .T. ) ;
#59422 = DIRECTION ( 'NONE',  ( 0.000000000000000000, -1.000000000000000000, 0.000000000000000000 ) ) ;
#59423 = CYLINDRICAL_SURFACE ( 'NONE', #30968, 3.500000000000003109 ) ;
#59424 = VECTOR ( 'NONE', #81894, 1000.000000000000000 ) ;
#59425 = CARTESIAN_POINT ( 'NONE',  ( 96.69309474412473548, -37.96640669985919914, 37.42133956162496844 ) ) ;
#59426 = DIRECTION ( 'NONE',  ( 0.000000000000000000, 0.000000000000000000, 1.000000000000000000 ) ) ;
#59427 = ORIENTED_EDGE ( 'NONE', *, *, #50805, .T. ) ;
#59428 = DIRECTION ( 'NONE',  ( 0.000000000000000000, 0.000000000000000000, 1.000000000000000000 ) ) ;
#59429 = ORIENTED_EDGE ( 'NONE', *, *, #48557, .F. ) ;
#59430 = CARTESIAN_POINT ( 'NONE',  ( -118.3661894536416099, 71.76236341257998674, 6.714990428328777128 ) ) ;
#59431 = ORIENTED_EDGE ( 'NONE', *, *, #25426, .T. ) ;
#59432 = VERTEX_POINT ( 'NONE', #88580 ) ;
#59433 = ADVANCED_FACE ( 'NONE', ( #32244 ), #75392, .T. ) ;
#59434 = AXIS2_PLACEMENT_3D ( 'NONE', #66441, #4228, #71504 ) ;
#59435 = ORIENTED_EDGE ( 'NONE', *, *, #7824, .F. ) ;
#59436 = CARTESIAN_POINT ( 'NONE',  ( 103.8504807240352790, -26.87063827031080621, 210.3394347997209763 ) ) ;
#59437 = CARTESIAN_POINT ( 'NONE',  ( 97.48373141833911859, -33.75867255000157741, 126.0865479483587990 ) ) ;
#59438 = DIRECTION ( 'NONE',  ( 1.000000000000000000, 0.000000000000000000, -1.821231995776174986E-16 ) ) ;
#59439 = CARTESIAN_POINT ( 'NONE',  ( 97.80922128671791427, -29.33095300656633597, 41.78991099019596334 ) ) ;
#59440 = CARTESIAN_POINT ( 'NONE',  ( 105.7150778794604662, -46.72380765957736060, 43.46892697967506081 ) ) ;
#59441 = ORIENTED_EDGE ( 'NONE', *, *, #19785, .F. ) ;
#59442 = CARTESIAN_POINT ( 'NONE',  ( 103.2783743724242811, -27.47470615678986761, 171.3856373841866514 ) ) ;
#59443 = CARTESIAN_POINT ( 'NONE',  ( 138.8167039024479834, -50.82844715994100682, 37.63480685541480852 ) ) ;
#59444 = EDGE_LOOP ( 'NONE', ( #82276, #71201, #24651, #85931, #15388, #7924 ) ) ;
#59445 = AXIS2_PLACEMENT_3D ( 'NONE', #81618, #19368, #21499 ) ;
#59446 = CARTESIAN_POINT ( 'NONE',  ( 106.5667039024470171, -94.77844715994137914, 2.217806855417697953 ) ) ;
#59447 = CARTESIAN_POINT ( 'NONE',  ( -71.09939861440099662, 20.32000000000000028, 177.8662485265279827 ) ) ;
#59448 = CARTESIAN_POINT ( 'NONE',  ( 116.9047011640240754, -41.71676023082953577, 248.4651490854349731 ) ) ;
#59449 = DIRECTION ( 'NONE',  ( 1.000000000000000078E-15, -1.000000000000000083E-30, -1.000000000000000000 ) ) ;
#59450 = CARTESIAN_POINT ( 'NONE',  ( 152.0371591254582881, -47.82818131005588214, 313.9678068554149490 ) ) ;
#59451 = LINE ( 'NONE', #87184, #9868 ) ;
#59452 = CARTESIAN_POINT ( 'NONE',  ( 98.43953089107090193, -39.48415132980177589, 280.9828960185531059 ) ) ;
#59454 = CARTESIAN_POINT ( 'NONE',  ( 111.0741232671659020, -25.60348521778456288, 95.80133956162495679 ) ) ;
#59453 = DIRECTION ( 'NONE',  ( -0.5000000000000015543, 0.8660254037844377084, -2.688821387764056676E-14 ) ) ;
#59455 = CARTESIAN_POINT ( 'NONE',  ( 120.1783960690039095, 74.61161073219626871, 51.01009929557958600 ) ) ;
#59456 = CARTESIAN_POINT ( 'NONE',  ( 96.56283406263658264, -36.88802528585984675, 136.3384824187679385 ) ) ;
#59457 = ORIENTED_EDGE ( 'NONE', *, *, #72937, .T. ) ;
#59458 = LINE ( 'NONE', #24956, #32099 ) ;
#59459 = ORIENTED_EDGE ( 'NONE', *, *, #9677, .F. ) ;
#59460 = AXIS2_PLACEMENT_3D ( 'NONE', #16008, #84161, #21935 ) ;
#59461 = CARTESIAN_POINT ( 'NONE',  ( 2.036081061455522238E-14, 127.0000000000000000, 80.02307622376218887 ) ) ;
#59462 = CARTESIAN_POINT ( 'NONE',  ( 63.03715912545737865, -24.42818131006027826, 236.4678068554150343 ) ) ;
#59463 = CARTESIAN_POINT ( 'NONE',  ( 134.8111839727902748, -34.08035908359602217, 1.709393751551410823 ) ) ;
#59464 = ORIENTED_EDGE ( 'NONE', *, *, #485, .F. ) ;
#59465 = CARTESIAN_POINT ( 'NONE',  ( 251.6756888531239156, -13.32818131005263140, 117.4678068554150627 ) ) ;
#59467 = EDGE_LOOP ( 'NONE', ( #41130, #30450, #23062, #82099 ) ) ;
#59466 = CARTESIAN_POINT ( 'NONE',  ( 107.6054179116733707, -26.23843464447702090, 95.03562527591097364 ) ) ;
#59468 = CARTESIAN_POINT ( 'NONE',  ( 95.60734603896362671, -36.72944715994100306, 294.6356252759106837 ) ) ;
#59469 = AXIS2_PLACEMENT_3D ( 'NONE', #38351, #24731, #78049 ) ;
#59470 = CARTESIAN_POINT ( 'NONE',  ( 62.03715912545744260, -47.82818131006020934, 129.9678068554150911 ) ) ;
#59471 = EDGE_CURVE ( 'NONE', #12734, #23174, #61789, .T. ) ;
#59472 = DIRECTION ( 'NONE',  ( 0.000000000000000000, -1.000000000000000000, 0.000000000000000000 ) ) ;
#59473 = ORIENTED_EDGE ( 'NONE', *, *, #22747, .F. ) ;
#59474 = CARTESIAN_POINT ( 'NONE',  ( 96.67713595657845360, -37.82845849995531040, 126.4099109901969626 ) ) ;
#59475 = APPLICATION_PROTOCOL_DEFINITION ( 'draft international standard', 'automotive_design', 1998, #13854 ) ;
#59476 = ADVANCED_FACE ( 'NONE', ( #46757 ), #5000, .T. ) ;
#59477 = DIRECTION ( 'NONE',  ( -1.000000000000000000, -4.299999999999999979E-14, -1.000000000000000078E-15 ) ) ;
#59478 = FACE_OUTER_BOUND ( 'NONE', #20665, .T. ) ;
#59479 = ORIENTED_EDGE ( 'NONE', *, *, #75078, .T. ) ;
#59480 = VECTOR ( 'NONE', #6524, 1000.000000000000000 ) ;
#59481 = ORIENTED_EDGE ( 'NONE', *, *, #11458, .T. ) ;
#59482 = CARTESIAN_POINT ( 'NONE',  ( 100.8594679592218171, 82.54999999999999716, -82.89895571708191824 ) ) ;
#59483 = DIRECTION ( 'NONE',  ( -4.237773401492740281E-14, 1.000000000000000000, 0.000000000000000000 ) ) ;
#59484 = DIRECTION ( 'NONE',  ( 0.9659258262890666469, 0.000000000000000000, 0.2588190451025269012 ) ) ;
#59486 = CARTESIAN_POINT ( 'NONE',  ( 75.61066417432020614, 20.32000000000000028, 177.0380000000000109 ) ) ;
#59485 = CARTESIAN_POINT ( 'NONE',  ( 134.0664832912740110, -8.729447159940999512, 291.1181252759119502 ) ) ;
#59487 = FACE_OUTER_BOUND ( 'NONE', #65353, .T. ) ;
#59488 = VERTEX_POINT ( 'NONE', #32700 ) ;
#59489 = EDGE_CURVE ( 'NONE', #35904, #41861, #57455, .T. ) ;
#59490 =( BOUNDED_CURVE ( )  B_SPLINE_CURVE ( 3, ( #26919, #47792, #55043, #20116 ),
 .UNSPECIFIED., .F., .T. ) 
 B_SPLINE_CURVE_WITH_KNOTS ( ( 4, 4 ),
 ( 1.162083553109172218, 1.162891078689471280 ),
 .UNSPECIFIED. ) 
 CURVE ( )  GEOMETRIC_REPRESENTATION_ITEM ( )  RATIONAL_B_SPLINE_CURVE ( ( 1.000000000000000000, 0.9999999456585371149, 0.9999999456585371149, 1.000000000000000000 ) ) 
 REPRESENTATION_ITEM ( '' )  );
#59491 = DIRECTION ( 'NONE',  ( -4.237773401492740281E-14, 1.000000000000000000, 0.000000000000000000 ) ) ;
#59492 = CARTESIAN_POINT ( 'NONE',  ( 107.2322476904470108, -46.54200526979089858, 208.5899109901959605 ) ) ;
#59494 = ORIENTED_EDGE ( 'NONE', *, *, #1826, .F. ) ;
#59493 = CARTESIAN_POINT ( 'NONE',  ( 106.0715115987692201, -25.31091405536793459, 321.4693626932605071 ) ) ;
#59495 = CIRCLE ( 'NONE', #82759, 5.041900000000001825 ) ;
#59496 = CARTESIAN_POINT ( 'NONE',  ( 96.85055626654755656, -38.51091292166574220, 42.45181575209999636 ) ) ;
#59497 = CARTESIAN_POINT ( 'NONE',  ( 109.6427594141682675, -46.48015053188884593, 52.78146225493246391 ) ) ;
#59498 = DIRECTION ( 'NONE',  ( 0.000000000000000000, 0.000000000000000000, -1.000000000000000000 ) ) ;
#59499 = LINE ( 'NONE', #26776, #40194 ) ;
#59500 = VECTOR ( 'NONE', #15504, 1000.000000000000114 ) ;
#59501 = EDGE_CURVE ( 'NONE', #24430, #49775, #5453, .T. ) ;
#59502 = ORIENTED_EDGE ( 'NONE', *, *, #46250, .T. ) ;
#59503 = DIRECTION ( 'NONE',  ( 0.7071067811865510144, 0.000000000000000000, -0.7071067811865441310 ) ) ;
#59504 = ORIENTED_EDGE ( 'NONE', *, *, #53155, .F. ) ;
#59505 = ORIENTED_EDGE ( 'NONE', *, *, #82217, .F. ) ;
#59506 = CARTESIAN_POINT ( 'NONE',  ( 112.1317502087781293, -44.64270164792750961, 214.4492023535159717 ) ) ;
#59507 = AXIS2_PLACEMENT_3D ( 'NONE', #45480, #65939, #31419 ) ;
#59508 = CARTESIAN_POINT ( 'NONE',  ( 98.15076410364456194, -41.26119453264894332, 52.70027500851303159 ) ) ;
#59509 = CARTESIAN_POINT ( 'NONE',  ( 107.0664832912739968, -36.72944715994100306, 293.2242906452868851 ) ) ;
#59510 = FACE_OUTER_BOUND ( 'NONE', #81055, .T. ) ;
#59511 = CIRCLE ( 'NONE', #82773, 5.041900000000000048 ) ;
#59512 = CARTESIAN_POINT ( 'NONE',  ( 81.77804793993006172, -38.88970947304841275, 2.099345637340709114 ) ) ;
#59513 = ORIENTED_EDGE ( 'NONE', *, *, #71650, .F. ) ;
#59514 = DIRECTION ( 'NONE',  ( -4.237773401492740281E-14, 1.000000000000000000, 0.000000000000000000 ) ) ;
#59515 = CARTESIAN_POINT ( 'NONE',  ( 108.4095123903694713, -26.73402528341915030, 35.96903173305258150 ) ) ;
#59516 = ORIENTED_EDGE ( 'NONE', *, *, #82620, .T. ) ;
#59517 = CARTESIAN_POINT ( 'NONE',  ( 112.1173730388400287, -26.89747643418222722, 19.71086337114896736 ) ) ;
#59518 = CARTESIAN_POINT ( 'NONE',  ( 12.19523432446486666, 85.82332710845591350, 117.7261451817823001 ) ) ;
#59520 = ORIENTED_EDGE ( 'NONE', *, *, #21263, .T. ) ;
#59519 = EDGE_CURVE ( 'NONE', #77969, #34986, #76269, .T. ) ;
#59521 = CARTESIAN_POINT ( 'NONE',  ( -479.3614999999999782, 14.28750000000036025, 2.863608028952925100 ) ) ;
#59522 = COLOUR_RGB ( '', 0.09019608, 0.27058824, 0.51372549) ;
#59523 = CARTESIAN_POINT ( 'NONE',  ( 177.4809174648213173, -48.32844715993478957, 300.4678068554149490 ) ) ;
#59524 = DIRECTION ( 'NONE',  ( 0.9825752044328148749, 0.1858654557302456822, 0.000000000000000000 ) ) ;
#59525 = CARTESIAN_POINT ( 'NONE',  ( 100.6107886340239901, -26.73269172650989489, 216.5327681330539633 ) ) ;
#59526 = CARTESIAN_POINT ( 'NONE',  ( 245.4909999999999854, 65.43750000000000000, -67.11950000000000216 ) ) ;
#59527 = EDGE_LOOP ( 'NONE', ( #82708, #75710, #70606, #40659 ) ) ;
#59528 = CARTESIAN_POINT ( 'NONE',  ( 98.61215933031529346, -43.92124142298762735, 72.89943479972099283 ) ) ;
#59529 = LINE ( 'NONE', #74971, #32313 ) ;
#59530 = VERTEX_POINT ( 'NONE', #80873 ) ;
#59531 = ORIENTED_EDGE ( 'NONE', *, *, #2141, .F. ) ;
#59532 = ORIENTED_EDGE ( 'NONE', *, *, #19760, .T. ) ;
#59533 = VECTOR ( 'NONE', #14783, 1000.000000000000000 ) ;
#59534 = EDGE_CURVE ( 'NONE', #41030, #55155, #71935, .T. ) ;
#59535 = CIRCLE ( 'NONE', #40680, 2.500000000000002220 ) ;
#59536 = CARTESIAN_POINT ( 'NONE',  ( 80.44276116895755990, -15.99866847873249931, 1.641799428525830828 ) ) ;
#59538 = ADVANCED_FACE ( 'NONE', ( #18628 ), #6339, .F. ) ;
#59537 = FACE_OUTER_BOUND ( 'NONE', #25583, .T. ) ;
#59539 = DIRECTION ( 'NONE',  ( 0.000000000000000000, 1.365923996832131856E-16, -1.000000000000000000 ) ) ;
#59540 = CARTESIAN_POINT ( 'NONE',  ( 115.3951208896509399, -39.08203659613434411, 141.4376141791150019 ) ) ;
#59541 = CARTESIAN_POINT ( 'NONE',  ( 106.8511646352646380, -47.80368950967726249, 223.5489586092439538 ) ) ;
#59542 = CARTESIAN_POINT ( 'NONE',  ( 208.9149999999999920, 43.68799999999999528, 44.45000000000000284 ) ) ;
#59543 = ORIENTED_EDGE ( 'NONE', *, *, #29187, .F. ) ;
#59544 = DIRECTION ( 'NONE',  ( 1.000000000000000000, 0.000000000000000000, 0.000000000000000000 ) ) ;
#59545 = AXIS2_PLACEMENT_3D ( 'NONE', #44891, #24468, #87142 ) ;
#59546 = ORIENTED_EDGE ( 'NONE', *, *, #70408, .F. ) ;
#59547 = EDGE_LOOP ( 'NONE', ( #10961, #67233, #65610, #9307 ) ) ;
#59548 = CARTESIAN_POINT ( 'NONE',  ( 37.03715912545343514, -48.62818131006128652, 180.4678068554150911 ) ) ;
#59549 = EDGE_LOOP ( 'NONE', ( #24829, #39996 ) ) ;
#59550 = ORIENTED_EDGE ( 'NONE', *, *, #73899, .F. ) ;
#59551 = CARTESIAN_POINT ( 'NONE',  ( 117.1166401382700002, -37.03105959670597258, 9.802291942577573636 ) ) ;
#59552 = CARTESIAN_POINT ( 'NONE',  ( 49.21437657594998427, -35.91149509761070391, -5.074374724088000832 ) ) ;
#59553 = CARTESIAN_POINT ( 'NONE',  ( 97.33767582200576385, -34.07173766446835117, 26.11484643626505786 ) ) ;
#59554 = CARTESIAN_POINT ( 'NONE',  ( 108.0589421777836492, -45.73103505524393597, 157.0743245899819556 ) ) ;
#59555 = CARTESIAN_POINT ( 'NONE',  ( 116.1589316287842735, -31.54115767207924748, 289.2384824187681716 ) ) ;
#59556 = ORIENTED_EDGE ( 'NONE', *, *, #46752, .T. ) ;
#59557 = CARTESIAN_POINT ( 'NONE',  ( 22.62762465138245460, 171.9999999999999716, 113.8826257785461280 ) ) ;
#59558 = VECTOR ( 'NONE', #22452, 1000.000000000000000 ) ;
#59559 = VERTEX_POINT ( 'NONE', #5904 ) ;
#59560 = VECTOR ( 'NONE', #69905, 1000.000000000000000 ) ;
#59561 = CIRCLE ( 'NONE', #78685, 7.143750000000004263 ) ;
#59562 = CARTESIAN_POINT ( 'NONE',  ( 135.5667039024470455, -118.2784471599408960, 45.21780685541799727 ) ) ;
#59563 = ORIENTED_EDGE ( 'NONE', *, *, #12507, .F. ) ;
#59564 = LINE ( 'NONE', #10541, #2998 ) ;
#59565 = CARTESIAN_POINT ( 'NONE',  ( 176.7669697523285208, -48.62818131005431610, 180.4678068554150059 ) ) ;
#59566 = LINE ( 'NONE', #36910, #69342 ) ;
#59567 = CIRCLE ( 'NONE', #68353, 4.799999999999970512 ) ;
#59568 = FACE_OUTER_BOUND ( 'NONE', #31729, .T. ) ;
#59569 = ORIENTED_EDGE ( 'NONE', *, *, #72161, .F. ) ;
#59570 = CARTESIAN_POINT ( 'NONE',  ( 104.5881283732255156, -26.60288457357396652, 285.2670538473396391 ) ) ;
#59571 = CARTESIAN_POINT ( 'NONE',  ( 107.1959371850970086, -26.26158102413311468, 31.06705384733893283 ) ) ;
#59574 = EDGE_CURVE ( 'NONE', #16891, #67680, #83542, .T. ) ;
#59573 = LINE ( 'NONE', #87309, #77646 ) ;
#59572 = DIRECTION ( 'NONE',  ( 0.000000000000000000, 0.000000000000000000, -1.000000000000000000 ) ) ;
#59575 = CARTESIAN_POINT ( 'NONE',  ( 115.8254407911606734, -31.73003342290389028, 145.2401058703679837 ) ) ;
#59576 = CARTESIAN_POINT ( 'NONE',  ( 44.45000000000000284, 114.2999999999999972, 275.4630000000000223 ) ) ;
#59577 = PLANE ( 'NONE',  #12190 ) ;
#59578 = VECTOR ( 'NONE', #31181, 1000.000000000000000 ) ;
#59579 = CYLINDRICAL_SURFACE ( 'NONE', #24271, 0.2499999999999941991 ) ;
#59580 = CARTESIAN_POINT ( 'NONE',  ( 145.4065785358296239, -77.83818511938963525, 247.5132519919489766 ) ) ;
#59581 = CARTESIAN_POINT ( 'NONE',  ( 117.4985906579250354, -37.96351766657803495, 53.73276813305394484 ) ) ;
#59582 = CARTESIAN_POINT ( 'NONE',  ( 117.2274905824790778, -41.08006910540670731, 209.5165776568640013 ) ) ;
#59583 = CARTESIAN_POINT ( 'NONE',  ( 110.4636787236150184, -47.27194539037950705, 53.83657765686300678 ) ) ;
#59585 = PLANE ( 'NONE',  #86402 ) ;
#59584 = LINE ( 'NONE', #10560, #63887 ) ;
#59586 = CARTESIAN_POINT ( 'NONE',  ( 57.14999999999999858, 69.84999999999999432, 329.4379999999999882 ) ) ;
#59587 = EDGE_CURVE ( 'NONE', #58319, #12332, #53961, .T. ) ;
#59588 = EDGE_LOOP ( 'NONE', ( #74540, #37470 ) ) ;
#59589 = CYLINDRICAL_SURFACE ( 'NONE', #56266, 4.749999999999976907 ) ;
#59590 = VERTEX_POINT ( 'NONE', #54906 ) ;
#59591 = AXIS2_PLACEMENT_3D ( 'NONE', #11979, #26489, #5156 ) ;
#59592 = CARTESIAN_POINT ( 'NONE',  ( 116.7176835877704093, -38.50936494796416554, 84.68133956162493803 ) ) ;
#59593 = ADVANCED_FACE ( 'NONE', ( #63088 ), #77185, .T. ) ;
#59595 = ORIENTED_EDGE ( 'NONE', *, *, #65936, .T. ) ;
#59594 = FACE_OUTER_BOUND ( 'NONE', #55399, .T. ) ;
#59596 = VECTOR ( 'NONE', #44969, 1000.000000000000000 ) ;
#59597 = DIRECTION ( 'NONE',  ( -1.000000000000000078E-15, 1.000000000000000083E-30, 1.000000000000000000 ) ) ;
#59598 = CARTESIAN_POINT ( 'NONE',  ( 103.0988156209413518, -47.86972635628415418, 248.3041967044829619 ) ) ;
#59599 = LINE ( 'NONE', #25098, #32364 ) ;
#59600 = CARTESIAN_POINT ( 'NONE',  ( 1.088711004441995877E-14, 92.07499999999998863, -88.90000000000000568 ) ) ;
#59601 = DIRECTION ( 'NONE',  ( 0.000000000000000000, 0.000000000000000000, 1.000000000000000000 ) ) ;
#59602 = DIRECTION ( 'NONE',  ( -0.1811243269279065315, 0.9834602067165264527, 0.000000000000000000 ) ) ;
#59603 = EDGE_CURVE ( 'NONE', #14767, #17736, #51607, .T. ) ;
#59604 = ADVANCED_FACE ( 'NONE', ( #15413 ), #14053, .T. ) ;
#59605 = CARTESIAN_POINT ( 'NONE',  ( 133.6902059199477435, -39.46022584114956544, 1.641799370504869238 ) ) ;
#59606 = CARTESIAN_POINT ( 'NONE',  ( -85.31568053864886281, 74.16976894168006140, 98.82395782888174551 ) ) ;
#59607 = CARTESIAN_POINT ( 'NONE',  ( 116.4500618263486444, -39.48841239489308919, 183.5984824187689526 ) ) ;
#59608 = ORIENTED_EDGE ( 'NONE', *, *, #14839, .F. ) ;
#59609 = VERTEX_POINT ( 'NONE', #7246 ) ;
#59610 = EDGE_CURVE ( 'NONE', #81285, #23386, #83552, .T. ) ;
#59611 = CARTESIAN_POINT ( 'NONE',  ( 98.20536012454746810, -36.63577306554869750, 107.7501547344689783 ) ) ;
#59612 = VECTOR ( 'NONE', #55403, 1000.000000000000000 ) ;
#59613 = CARTESIAN_POINT ( 'NONE',  ( 152.0368932755772562, -23.42844715993587812, 180.4678068554149775 ) ) ;
#59615 = CARTESIAN_POINT ( 'NONE',  ( 152.0371591254582881, -47.82818131005588214, 300.4678068554149490 ) ) ;
#59614 = CARTESIAN_POINT ( 'NONE',  ( 107.9555263298577188, -25.64695713395855137, 261.0127681330532710 ) ) ;
#59616 = DIRECTION ( 'NONE',  ( 0.000000000000000000, 0.000000000000000000, -1.000000000000000000 ) ) ;
#59617 = EDGE_CURVE ( 'NONE', #22947, #54103, #56254, .T. ) ;
#59618 = LINE ( 'NONE', #80542, #55344 ) ;
#59619 = CARTESIAN_POINT ( 'NONE',  ( 117.9438495704238505, 78.46643079253873054, -12.03279974798964247 ) ) ;
#59620 = CARTESIAN_POINT ( 'NONE',  ( 33.96670390244752014, -28.27351298637434240, 237.4678068554150059 ) ) ;
#59621 = FACE_OUTER_BOUND ( 'NONE', #74945, .T. ) ;
#59622 = DIRECTION ( 'NONE',  ( -1.346944695195362088E-15, 1.000000000000000000, -3.469446951953620425E-31 ) ) ;
#59623 = CARTESIAN_POINT ( 'NONE',  ( 101.4371718687637838, -46.21494532752030437, 207.1622919425779514 ) ) ;
#59624 = ORIENTED_EDGE ( 'NONE', *, *, #74411, .T. ) ;
#59626 = ORIENTED_EDGE ( 'NONE', *, *, #10510, .F. ) ;
#59625 = ADVANCED_FACE ( 'NONE', ( #41287 ), #42627, .F. ) ;
#59627 = AXIS2_PLACEMENT_3D ( 'NONE', #1108, #28348, #28819 ) ;
#59628 = DIRECTION ( 'NONE',  ( 4.299999999999999979E-14, -1.000000000000000000, 4.400000000000000367E-29 ) ) ;
#59629 = CARTESIAN_POINT ( 'NONE',  ( 146.8914679696725329, -68.04425955369198675, 246.3066688845383965 ) ) ;
#59630 = CARTESIAN_POINT ( 'NONE',  ( 183.5150000000000148, 14.63749999999999929, -47.62500000000000000 ) ) ;
#59631 = FACE_OUTER_BOUND ( 'NONE', #74614, .T. ) ;
#59632 = AXIS2_PLACEMENT_3D ( 'NONE', #36149, #34797, #43843 ) ;
#59633 = ORIENTED_EDGE ( 'NONE', *, *, #58954, .F. ) ;
#59634 = CARTESIAN_POINT ( 'NONE',  ( 97.81170051792484799, -40.51743816602341752, 61.63542871443850402 ) ) ;
#59635 = CARTESIAN_POINT ( 'NONE',  ( 113.6857051329922683, -45.58184738042410800, 188.0994347997199725 ) ) ;
#59636 = CARTESIAN_POINT ( 'NONE',  ( 103.1875000000000000, 127.0000000000000000, 3.602774393244745134E-13 ) ) ;
#59637 = ORIENTED_EDGE ( 'NONE', *, *, #26345, .F. ) ;
#59639 = ORIENTED_EDGE ( 'NONE', *, *, #33998, .T. ) ;
#59638 = ORIENTED_EDGE ( 'NONE', *, *, #37983, .T. ) ;
#59640 = VECTOR ( 'NONE', #79497, 1000.000000000000000 ) ;
#59641 = ADVANCED_FACE ( 'NONE', ( #27679 ), #56717, .F. ) ;
#59642 = CARTESIAN_POINT ( 'NONE',  ( -11.39816346244706580, 76.93354734096725167, 118.0069729841872146 ) ) ;
#59644 = EDGE_CURVE ( 'NONE', #17950, #31900, #84004, .T. ) ;
#59643 = DIRECTION ( 'NONE',  ( 0.000000000000000000, 1.000000000000000000, 0.000000000000000000 ) ) ;
#59645 = CARTESIAN_POINT ( 'NONE',  ( 167.6524903400753601, -49.32844715993521589, 300.4678068554149490 ) ) ;
#59646 = AXIS2_PLACEMENT_3D ( 'NONE', #62041, #87973, #19376 ) ;
#59647 = ADVANCED_FACE ( 'NONE', ( #62646, #22225 ), #14512, .T. ) ;
#59648 = CARTESIAN_POINT ( 'NONE',  ( 99.78939748087903183, -33.03164401141575723, 48.77094751244892734 ) ) ;
#59649 = CARTESIAN_POINT ( 'NONE',  ( -41.60202597009397607, 65.59999999999998010, 47.03909206933071374 ) ) ;
#59650 = ORIENTED_EDGE ( 'NONE', *, *, #71092, .T. ) ;
#59651 = EDGE_CURVE ( 'NONE', #10845, #56771, #48990, .T. ) ;
#59652 = CARTESIAN_POINT ( 'NONE',  ( 57.91199999999999903, 101.5999999999999943, 191.3008000794699797 ) ) ;
#59653 = CARTESIAN_POINT ( 'NONE',  ( 82.80005790026137902, -18.42904715602866972, 6.774297104451808771 ) ) ;
#59654 = ORIENTED_EDGE ( 'NONE', *, *, #20164, .F. ) ;
#59655 = VERTEX_POINT ( 'NONE', #28567 ) ;
#59656 = CARTESIAN_POINT ( 'NONE',  ( 31.75000000000000000, 69.84999999999999432, 292.1000000000000227 ) ) ;
#59657 = VERTEX_POINT ( 'NONE', #83111 ) ;
#59658 = EDGE_LOOP ( 'NONE', ( #14286, #25381, #46065, #88088 ) ) ;
#59659 = CARTESIAN_POINT ( 'NONE',  ( -487.2989999999999782, 18.41194598552324990, 83.34375000000000000 ) ) ;
#59660 = CARTESIAN_POINT ( 'NONE',  ( 114.1634876701351402, -42.35485373834646339, 47.72765792331495760 ) ) ;
#59661 = CARTESIAN_POINT ( 'NONE',  ( 103.7160641590222809, -26.17150546779393494, 205.3089586092439731 ) ) ;
#59662 = AXIS2_PLACEMENT_3D ( 'NONE', #81643, #75707, #12584 ) ;
#59663 = CARTESIAN_POINT ( 'NONE',  ( 109.3536845750984412, -25.93905639472648872, 184.9222919425779708 ) ) ;
#59665 = CARTESIAN_POINT ( 'NONE',  ( 99.53941477645811631, -29.46552450412116997, 246.7156252759109520 ) ) ;
#59664 = FACE_BOUND ( 'NONE', #41132, .T. ) ;
#59666 = CARTESIAN_POINT ( 'NONE',  ( 103.1875000000000000, 117.4749999999999943, 3.602774393244745134E-13 ) ) ;
#59667 = CARTESIAN_POINT ( 'NONE',  ( 183.6524903400783160, -48.32844715993452667, 300.4678068554149490 ) ) ;
#59668 = ORIENTED_EDGE ( 'NONE', *, *, #69816, .T. ) ;
#59669 = VERTEX_POINT ( 'NONE', #49447 ) ;
#59670 = VECTOR ( 'NONE', #57240, 1000.000000000000000 ) ;
#59671 = CIRCLE ( 'NONE', #56773, 3.249999999999975131 ) ;
#59672 = CARTESIAN_POINT ( 'NONE',  ( 186.6899999999999977, 59.08750000000000568, -38.10000000000000142 ) ) ;
#59673 = CARTESIAN_POINT ( 'NONE',  ( 98.80440911621268185, -29.31655204712020080, 235.7565776568629872 ) ) ;
#59674 = ORIENTED_EDGE ( 'NONE', *, *, #33588, .F. ) ;
#59675 = CARTESIAN_POINT ( 'NONE',  ( 107.5657785589506688, -47.77162953885341778, 192.6003871806729535 ) ) ;
#59676 = CARTESIAN_POINT ( 'NONE',  ( 108.4162223138522307, -26.73487509134323048, 264.9689798130800682 ) ) ;
#59677 = DIRECTION ( 'NONE',  ( 0.000000000000000000, -1.000000000000000000, 0.000000000000000000 ) ) ;
#59678 = DIRECTION ( 'NONE',  ( 1.000000000000000078E-15, -1.000000000000000083E-30, -1.000000000000000000 ) ) ;
#59679 = CARTESIAN_POINT ( 'NONE',  ( 103.1875000000000000, 117.4749999999999943, 3.602774393244745134E-13 ) ) ;
#59682 = CARTESIAN_POINT ( 'NONE',  ( 111.7637953458031745, -46.71243375810358600, 283.9146728949585849 ) ) ;
#59681 = CARTESIAN_POINT ( 'NONE',  ( -186.2398777604655038, 20.32000000000000028, -12.69999999999999929 ) ) ;
#59680 = CARTESIAN_POINT ( 'NONE',  ( -34.53140813619931748, 148.4450814996825443, 35.02576496182814481 ) ) ;
#59683 = DIRECTION ( 'NONE',  ( 0.000000000000000000, 0.000000000000000000, 1.000000000000000000 ) ) ;
#59684 = FACE_OUTER_BOUND ( 'NONE', #71694, .T. ) ;
#59685 = LINE ( 'NONE', #86978, #4925 ) ;
#59686 = CARTESIAN_POINT ( 'NONE',  ( 67.06673837846007302, -137.6758525980020806, 245.5072637273240161 ) ) ;
#59687 = DIRECTION ( 'NONE',  ( 1.000000000000000078E-15, -1.000000000000000083E-30, -1.000000000000000000 ) ) ;
#59688 = CYLINDRICAL_SURFACE ( 'NONE', #34713, 5.599999999999994316 ) ;
#59689 = VECTOR ( 'NONE', #64898, 1000.000000000000114 ) ;
#59691 = VERTEX_POINT ( 'NONE', #20868 ) ;
#59690 = CARTESIAN_POINT ( 'NONE',  ( 100.1309283041910874, -30.67620045321505273, 195.5838068554170661 ) ) ;
#59692 = CARTESIAN_POINT ( 'NONE',  ( 127.0664832912740110, -54.72944906728950798, 14.67562527591099197 ) ) ;
#59693 = CARTESIAN_POINT ( 'NONE',  ( 117.4347420270075730, -35.18426962645584410, 218.9441967044829482 ) ) ;
#59694 = CARTESIAN_POINT ( 'NONE',  ( 112.5142634568524329, -27.84101767465772070, 90.63848241876793566 ) ) ;
#59695 = CARTESIAN_POINT ( 'NONE',  ( 97.88103918441719031, -41.75145834149261503, 217.7241967044829494 ) ) ;
#59696 = DIRECTION ( 'NONE',  ( -1.000000000000000000, 0.000000000000000000, 0.000000000000000000 ) ) ;
#59697 = FACE_OUTER_BOUND ( 'NONE', #87293, .T. ) ;
#59699 = DIRECTION ( 'NONE',  ( 0.000000000000000000, 0.000000000000000000, -1.000000000000000000 ) ) ;
#59698 = DIRECTION ( 'NONE',  ( 0.000000000000000000, 0.000000000000000000, 1.000000000000000000 ) ) ;
#59700 = CARTESIAN_POINT ( 'NONE',  ( -107.7702177616926065, 127.0000000000000000, -1.170504665415349981E-12 ) ) ;
#59701 = AXIS2_PLACEMENT_3D ( 'NONE', #1972, #70109, #7883 ) ;
#59702 = CARTESIAN_POINT ( 'NONE',  ( -72.96458098368600531, 127.0000000000000000, -72.96458098368781009 ) ) ;
#59703 = VERTEX_POINT ( 'NONE', #76278 ) ;
#59704 = EDGE_CURVE ( 'NONE', #58550, #9949, #5249, .T. ) ;
#59705 = ORIENTED_EDGE ( 'NONE', *, *, #22634, .F. ) ;
#59706 = VECTOR ( 'NONE', #8094, 1000.000000000000000 ) ;
#59707 = CARTESIAN_POINT ( 'NONE',  ( 109.2815815313881558, -45.51044995646627456, 92.20765792331498290 ) ) ;
#59708 = ADVANCED_FACE ( 'NONE', ( #4180 ), #72334, .T. ) ;
#59710 = ORIENTED_EDGE ( 'NONE', *, *, #39871, .F. ) ;
#59709 = DIRECTION ( 'NONE',  ( -1.000000000000000000, -4.510281037539694659E-14, 0.000000000000000000 ) ) ;
#59711 = FACE_OUTER_BOUND ( 'NONE', #1284, .T. ) ;
#59712 = CARTESIAN_POINT ( 'NONE',  ( 102.3122812202564802, -27.43633205498518635, 116.4527681330539650 ) ) ;
#59713 = CARTESIAN_POINT ( 'NONE',  ( 107.0667039024470313, -104.2784471599418197, -11.78219314458200984 ) ) ;
#59714 = AXIS2_PLACEMENT_3D ( 'NONE', #1964, #86867, #24628 ) ;
#59715 = LINE ( 'NONE', #24769, #44216 ) ;
#59716 = EDGE_CURVE ( 'NONE', #62685, #35953, #54512, .T. ) ;
#59717 = EDGE_CURVE ( 'NONE', #84162, #52633, #18248, .T. ) ;
#59718 = CARTESIAN_POINT ( 'NONE',  ( -74.43377912862143830, 80.88465057165899452, 92.27764637677488224 ) ) ;
#59719 = CARTESIAN_POINT ( 'NONE',  ( 104.4081006675575054, -46.45808914180122429, 108.3647919430991351 ) ) ;
#59720 = CARTESIAN_POINT ( 'NONE',  ( 101.5072281473882043, -27.97539281467247108, 65.51467289495899138 ) ) ;
#59721 = ORIENTED_EDGE ( 'NONE', *, *, #55558, .F. ) ;
#59722 = ORIENTED_EDGE ( 'NONE', *, *, #32955, .F. ) ;
#59723 = ORIENTED_EDGE ( 'NONE', *, *, #71330, .F. ) ;
#59724 = EDGE_CURVE ( 'NONE', #78458, #51305, #16471, .T. ) ;
#59725 = DIRECTION ( 'NONE',  ( 0.000000000000000000, 0.000000000000000000, 1.000000000000000000 ) ) ;
#59727 = LINE ( 'NONE', #2567, #54846 ) ;
#59726 = CARTESIAN_POINT ( 'NONE',  ( 102.6513375509277779, -45.45698538002849176, 123.2041967044819870 ) ) ;
#59728 = DIRECTION ( 'NONE',  ( 0.000000000000000000, 1.000000000000000000, 0.000000000000000000 ) ) ;
#59729 = EDGE_CURVE ( 'NONE', #12518, #49937, #65066, .T. ) ;
#59730 = CARTESIAN_POINT ( 'NONE',  ( 94.86917197795301604, -31.06128196069622760, 3.024967495036138931 ) ) ;
#59731 = CARTESIAN_POINT ( 'NONE',  ( 154.4532657509292051, -72.54478064608022692, 396.9756252759102040 ) ) ;
#59732 = CARTESIAN_POINT ( 'NONE',  ( 90.65736737572362358, 90.28416741362497078, 76.39920031718118310 ) ) ;
#59733 = DIRECTION ( 'NONE',  ( 0.08464269478575328631, -0.06148930273953279180, 0.9945122824118421967 ) ) ;
#59734 = CARTESIAN_POINT ( 'NONE',  ( 101.0787430638808928, -27.46603582566399027, 70.54514908543497143 ) ) ;
#59735 = VERTEX_POINT ( 'NONE', #45926 ) ;
#59737 = ORIENTED_EDGE ( 'NONE', *, *, #78860, .T. ) ;
#59736 = EDGE_CURVE ( 'NONE', #54672, #46304, #74914, .T. ) ;
#59738 = CARTESIAN_POINT ( 'NONE',  ( 5.616699032889737708, 93.94804372660794911, 130.4356411629704837 ) ) ;
#59739 = CARTESIAN_POINT ( 'NONE',  ( 107.0664832912739968, -36.72944715994100306, 287.6356252759109680 ) ) ;
#59740 = AXIS2_PLACEMENT_3D ( 'NONE', #35350, #50321, #14486 ) ;
#59741 = DIRECTION ( 'NONE',  ( 0.9825752044328147639, 0.1858654557302462929, 0.000000000000000000 ) ) ;
#59742 = CARTESIAN_POINT ( 'NONE',  ( 99.80647774793122551, -41.44074323372286273, 144.6147570362579415 ) ) ;
#59743 = EDGE_CURVE ( 'NONE', #770, #29891, #37810, .T. ) ;
#59744 = VECTOR ( 'NONE', #694, 1000.000000000000000 ) ;
#59745 = CARTESIAN_POINT ( 'NONE',  ( 109.0351697880554696, -103.7193031201850744, -19.78219314458204536 ) ) ;
#59746 = VERTEX_POINT ( 'NONE', #72776 ) ;
#59747 = ORIENTED_EDGE ( 'NONE', *, *, #20701, .T. ) ;
#59748 = DIRECTION ( 'NONE',  ( 0.000000000000000000, -1.000000000000000000, 0.000000000000000000 ) ) ;
#59749 = ORIENTED_EDGE ( 'NONE', *, *, #6625, .T. ) ;
#59750 = PRODUCT_DEFINITION_SHAPE ( 'NONE', 'NONE',  #89935 ) ;
#59751 = VERTEX_POINT ( 'NONE', #23742 ) ;
#59752 = CARTESIAN_POINT ( 'NONE',  ( -24.20305689751608824, 65.59999999999998010, 58.62596543806478877 ) ) ;
#59753 = AXIS2_PLACEMENT_3D ( 'NONE', #27139, #5354, #26239 ) ;
#59754 = ADVANCED_FACE ( 'NONE', ( #44148 ), #37356, .T. ) ;
#59755 = CARTESIAN_POINT ( 'NONE',  ( 103.8678987209337947, -28.46522696937008945, 211.8015833058969690 ) ) ;
#59756 = DIRECTION ( 'NONE',  ( -1.054009200593500181E-15, -1.000000000000000000, 0.000000000000000000 ) ) ;
#59757 = EDGE_CURVE ( 'NONE', #63968, #78226, #79161, .T. ) ;
#59758 = DIRECTION ( 'NONE',  ( 1.000000000000000078E-15, -1.000000000000000083E-30, -1.000000000000000000 ) ) ;
#59759 = AXIS2_PLACEMENT_3D ( 'NONE', #8571, #35809, #15391 ) ;
#59760 = CARTESIAN_POINT ( 'NONE',  ( 116.3212776292271258, -32.94146857470711609, 44.13562527591097506 ) ) ;
#59761 = VERTEX_POINT ( 'NONE', #31420 ) ;
#59762 = ORIENTED_EDGE ( 'NONE', *, *, #56980, .F. ) ;
#59763 = VECTOR ( 'NONE', #49390, 1000.000000000000000 ) ;
#59764 = ORIENTED_EDGE ( 'NONE', *, *, #78299, .F. ) ;
#59765 = ORIENTED_EDGE ( 'NONE', *, *, #10421, .F. ) ;
#59766 = CARTESIAN_POINT ( 'NONE',  ( 99.78156907347540994, -40.47280301881529851, 194.5223760838769920 ) ) ;
#59767 = CARTESIAN_POINT ( 'NONE',  ( 118.9289135900544494, -36.16662986141290048, 118.8641967044819836 ) ) ;
#59768 = CARTESIAN_POINT ( 'NONE',  ( 106.6611865629619018, -26.33404432545455265, 85.10705384733896040 ) ) ;
#59769 = LINE ( 'NONE', #11183, #48597 ) ;
#59770 = CARTESIAN_POINT ( 'NONE',  ( 99.08946256649485917, -109.4614598618343138, -19.78219314458184996 ) ) ;
#59771 = CARTESIAN_POINT ( 'NONE',  ( 51.56670390244699576, -22.48495420874030515, -5.074374724088000832 ) ) ;
#59772 = CARTESIAN_POINT ( 'NONE',  ( 108.9451852418780362, -26.43907245703257303, 160.9327681330539690 ) ) ;
#59773 = CIRCLE ( 'NONE', #16302, 13.16666666666669627 ) ;
#59774 = LINE ( 'NONE', #66146, #82833 ) ;
#59775 = ORIENTED_EDGE ( 'NONE', *, *, #72403, .F. ) ;
#59776 = CARTESIAN_POINT ( 'NONE',  ( -48.02966122971777452, 100.5999999999999659, 106.4272185163641780 ) ) ;
#59777 = EDGE_LOOP ( 'NONE', ( #40690, #2508 ) ) ;
#59778 = ORIENTED_EDGE ( 'NONE', *, *, #61882, .T. ) ;
#59779 = DIRECTION ( 'NONE',  ( 0.000000000000000000, 1.000000000000000000, 0.000000000000000000 ) ) ;
#59780 = DIRECTION ( 'NONE',  ( 0.000000000000000000, -1.000000000000000000, 0.000000000000000000 ) ) ;
#59781 = VERTEX_POINT ( 'NONE', #80489 ) ;
#59782 = EDGE_CURVE ( 'NONE', #36122, #18229, #86859, .T. ) ;
#59783 = CARTESIAN_POINT ( 'NONE',  ( 184.5667039024480118, -48.82844715994099971, 20.91780685541479912 ) ) ;
#59784 = EDGE_LOOP ( 'NONE', ( #50948, #26318 ) ) ;
#59785 = CARTESIAN_POINT ( 'NONE',  ( 107.3887696601165374, -26.70707029421490120, 131.0506897302312836 ) ) ;
#59786 = CARTESIAN_POINT ( 'NONE',  ( 106.6603292229642790, -26.31205452386275212, 85.10705384733896040 ) ) ;
#59787 = FACE_OUTER_BOUND ( 'NONE', #76888, .T. ) ;
#59788 = CARTESIAN_POINT ( 'NONE',  ( 30.00000000000003553, 171.0000000000000000, 182.8826257785461280 ) ) ;
#59789 = CARTESIAN_POINT ( 'NONE',  ( 1.387778780781445676E-14, 223.9999999999999716, 97.27542076772557778 ) ) ;
#59790 = CARTESIAN_POINT ( 'NONE',  ( 106.6854394624702707, -26.95610377642487165, 85.10705384733996937 ) ) ;
#59792 = CARTESIAN_POINT ( 'NONE',  ( 101.3611157396114635, -46.16939438856402944, 198.1318157521009482 ) ) ;
#59791 = CARTESIAN_POINT ( 'NONE',  ( 72.06648329127401098, -45.72944715994111675, -4.970821333495738514 ) ) ;
#59793 = CARTESIAN_POINT ( 'NONE',  ( 147.4575741623265799, 0.000000000000000000, 135.2444258376725941 ) ) ;
#59794 = PLANE ( 'NONE',  #29266 ) ;
#59795 = ORIENTED_EDGE ( 'NONE', *, *, #17109, .T. ) ;
#59796 = DIRECTION ( 'NONE',  ( -4.554376769437570034E-14, 1.000000000000000000, 0.000000000000000000 ) ) ;
#59797 = DIRECTION ( 'NONE',  ( 0.000000000000000000, 0.000000000000000000, 1.000000000000000000 ) ) ;
#59798 = CARTESIAN_POINT ( 'NONE',  ( 49.16670390244701139, -28.27351298637340093, -5.074374724088000832 ) ) ;
#59799 = PLANE ( 'NONE',  #5616 ) ;
#59801 = ORIENTED_EDGE ( 'NONE', *, *, #40947, .T. ) ;
#59800 = CARTESIAN_POINT ( 'NONE',  ( 118.0975507117283883, -35.49314816969329200, 233.9032443235299752 ) ) ;
#59802 = CARTESIAN_POINT ( 'NONE',  ( 108.4173341213413835, -26.73501241750527413, 144.9689709186055779 ) ) ;
#59803 = CARTESIAN_POINT ( 'NONE',  ( 102.7553090513238487, -25.69095112480093945, 16.37276813305293999 ) ) ;
#59804 = CARTESIAN_POINT ( 'NONE',  ( 114.0153296496652615, -28.07433117884028206, 115.5261014663869474 ) ) ;
#59805 = FACE_OUTER_BOUND ( 'NONE', #27779, .T. ) ;
#59806 = CARTESIAN_POINT ( 'NONE',  ( 81.55977255144560445, -39.04085022828763840, 7.869587501222556014 ) ) ;
#59807 = EDGE_CURVE ( 'NONE', #71751, #62756, #9649, .T. ) ;
#59808 = DIRECTION ( 'NONE',  ( -1.000000000000000078E-15, 1.000000000000000083E-30, 1.000000000000000000 ) ) ;
#59809 = CARTESIAN_POINT ( 'NONE',  ( -28.99999999999997513, 172.0000000000000000, 183.8826257785461280 ) ) ;
#59810 = VERTEX_POINT ( 'NONE', #10982 ) ;
#59811 = AXIS2_PLACEMENT_3D ( 'NONE', #74299, #59748, #72520 ) ;
#59812 = EDGE_CURVE ( 'NONE', #44353, #69843, #34527, .T. ) ;
#59813 = ORIENTED_EDGE ( 'NONE', *, *, #83914, .F. ) ;
#59814 = EDGE_CURVE ( 'NONE', #31265, #43132, #58935, .T. ) ;
#59815 = ORIENTED_EDGE ( 'NONE', *, *, #20372, .F. ) ;
#59816 = EDGE_CURVE ( 'NONE', #32634, #79978, #41363, .T. ) ;
#59817 = VERTEX_POINT ( 'NONE', #46380 ) ;
#59818 = CARTESIAN_POINT ( 'NONE',  ( 105.7154773147163098, -46.72385839023237253, 72.46895860799507716 ) ) ;
#59819 = CARTESIAN_POINT ( 'NONE',  ( 106.2538455105912050, -26.32252419718687619, 21.13848241876792144 ) ) ;
#59820 = CARTESIAN_POINT ( 'NONE',  ( 149.4409906032288404, -0.9156555935619370423, 361.9756252759100335 ) ) ;
#59821 = CARTESIAN_POINT ( 'NONE',  ( 87.68691565637547569, -140.6784471605521674, 245.6812520957089987 ) ) ;
#59822 = VECTOR ( 'NONE', #15197, 1000.000000000000000 ) ;
#59823 = ADVANCED_FACE ( 'NONE', ( #32773, #67748 ), #74114, .F. ) ;
#59825 = DIRECTION ( 'NONE',  ( 1.000000000000000000, 0.000000000000000000, 8.465970413060558704E-17 ) ) ;
#59824 = CARTESIAN_POINT ( 'NONE',  ( 151.0371591254585155, -46.82818131005592477, 117.4678068554150485 ) ) ;
#59826 = CARTESIAN_POINT ( 'NONE',  ( 109.4373255760682611, -46.14484595950412427, 242.1952769709339464 ) ) ;
#59827 = EDGE_LOOP ( 'NONE', ( #49422, #55261 ) ) ;
#59828 = ORIENTED_EDGE ( 'NONE', *, *, #27687, .T. ) ;
#59829 = EDGE_LOOP ( 'NONE', ( #44678, #42146, #54797, #29894, #39398, #69175, #77704 ) ) ;
#59830 = ADVANCED_FACE ( 'NONE', ( #40486 ), #25511, .T. ) ;
#59831 = VECTOR ( 'NONE', #57001, 1000.000000000000000 ) ;
#59832 = CARTESIAN_POINT ( 'NONE',  ( 150.5667039024475571, -25.42844715993593852, 180.4678068554149775 ) ) ;
#59833 = CARTESIAN_POINT ( 'NONE',  ( 98.04153869695548451, -41.04189868359566873, 181.6812057122477597 ) ) ;
#59834 = CARTESIAN_POINT ( 'NONE',  ( 41.56648329127398966, -27.82844715994070484, 318.9256252759120116 ) ) ;
#59835 = CARTESIAN_POINT ( 'NONE',  ( 115.9247622085524085, -36.97270265434710979, 40.23586902018294609 ) ) ;
#59836 = ADVANCED_FACE ( 'NONE', ( #20052 ), #48175, .F. ) ;
#59837 = CIRCLE ( 'NONE', #64212, 10.00000000000000178 ) ;
#59838 = CARTESIAN_POINT ( 'NONE',  ( 118.2599598282757114, 92.11680164986009345, -8.393562877890433427 ) ) ;
#59839 = CARTESIAN_POINT ( 'NONE',  ( 44.45000000000000284, 111.1250000000000000, 257.1750000000000114 ) ) ;
#59840 = CARTESIAN_POINT ( 'NONE',  ( 115.4995704134666994, -41.68388727776413560, 238.4041967044829562 ) ) ;
#59841 = CARTESIAN_POINT ( 'NONE',  ( 107.0664832912730020, -27.87844715994269862, 342.9256252759109884 ) ) ;
#59843 = ORIENTED_EDGE ( 'NONE', *, *, #34732, .T. ) ;
#59842 = ADVANCED_FACE ( 'NONE', ( #11896 ), #19802, .F. ) ;
#59844 = FACE_OUTER_BOUND ( 'NONE', #29967, .T. ) ;
#59845 = CARTESIAN_POINT ( 'NONE',  ( 80.06670390244696023, -40.87844715994097555, 222.2178068554179902 ) ) ;
#59846 = CARTESIAN_POINT ( 'NONE',  ( 114.8864029495430685, -33.02137736771143750, 62.00904275054391945 ) ) ;
#59847 = DIRECTION ( 'NONE',  ( -1.000000000000000000, -2.756263715554006823E-15, 0.000000000000000000 ) ) ;
#59848 = CARTESIAN_POINT ( 'NONE',  ( 152.0371591254583450, -47.82818131005588214, 249.9678068554149490 ) ) ;
#59849 = CARTESIAN_POINT ( 'NONE',  ( -4.481496500578191267, 94.44030975666426286, 118.4718929279777200 ) ) ;
#59850 = VERTEX_POINT ( 'NONE', #17154 ) ;
#59851 = CARTESIAN_POINT ( 'NONE',  ( 141.0664832912740110, -8.729447159940995959, -4.824374724088994704 ) ) ;
#59852 = CARTESIAN_POINT ( 'NONE',  ( 125.2636845449844287, 54.85408740538772321, -36.79518296114878240 ) ) ;
#59853 = CONICAL_SURFACE ( 'NONE', #20723, 9.499999999999980460, 0.7853981633974743692 ) ;
#59854 = ORIENTED_EDGE ( 'NONE', *, *, #24771, .F. ) ;
#59855 = CARTESIAN_POINT ( 'NONE',  ( 96.64175856332744274, -36.61924367559645788, 111.3184824187679567 ) ) ;
#59856 = ORIENTED_EDGE ( 'NONE', *, *, #33276, .F. ) ;
#59857 = CARTESIAN_POINT ( 'NONE',  ( 109.7600704110825802, -27.40125247274746556, 64.27527697093398729 ) ) ;
#59858 = CARTESIAN_POINT ( 'NONE',  ( 165.2748236753140247, -30.08671355700301575, 342.9256252759119548 ) ) ;
#59859 = CARTESIAN_POINT ( 'NONE',  ( 113.2603198993755882, -43.06700715444978300, 69.62444044875392990 ) ) ;
#59860 = DIRECTION ( 'NONE',  ( 1.000000000000000000, 1.092739197465703932E-16, 0.000000000000000000 ) ) ;
#59861 = ADVANCED_FACE ( 'NONE', ( #42264 ), #37599, .F. ) ;
#59862 = DIRECTION ( 'NONE',  ( 0.000000000000000000, 0.000000000000000000, 1.000000000000000000 ) ) ;
#59863 = CARTESIAN_POINT ( 'NONE',  ( 106.6058858729755201, -25.66269263286424263, 36.09753003781596448 ) ) ;
#59864 = CARTESIAN_POINT ( 'NONE',  ( 142.8821648370248170, -72.54478064608022692, 540.9756252759101471 ) ) ;
#59865 = ORIENTED_EDGE ( 'NONE', *, *, #46651, .T. ) ;
#59866 = CIRCLE ( 'NONE', #87457, 3.499999999999996003 ) ;
#59867 = CARTESIAN_POINT ( 'NONE',  ( 30.48091746481745901, -49.32844715994156815, 180.4678068554150911 ) ) ;
#59868 = VERTEX_POINT ( 'NONE', #56337 ) ;
#59869 = CARTESIAN_POINT ( 'NONE',  ( 180.2121375201600131, -29.73316016639649462, 342.9256252759109884 ) ) ;
#59870 = ORIENTED_EDGE ( 'NONE', *, *, #35304, .F. ) ;
#59871 = ORIENTED_EDGE ( 'NONE', *, *, #84045, .T. ) ;
#59872 = PLANE ( 'NONE',  #61538 ) ;
#59873 = ORIENTED_EDGE ( 'NONE', *, *, #9500, .T. ) ;
#59874 = CARTESIAN_POINT ( 'NONE',  ( 97.41213207386795148, -40.51524797426110069, 246.6118157521019896 ) ) ;
#59875 = CARTESIAN_POINT ( 'NONE',  ( 108.7144426859271391, -26.79521004361802028, 124.9450481620639408 ) ) ;
#59876 = DIRECTION ( 'NONE',  ( -6.524622321627019585E-16, -3.741823817616790462E-31, -1.000000000000000000 ) ) ;
#59877 = CARTESIAN_POINT ( 'NONE',  ( 98.59006141831567049, -43.82340604873675716, 67.86895860924497015 ) ) ;
#59878 = CARTESIAN_POINT ( 'NONE',  ( 113.1780956839291150, -44.75202357551225418, 44.09393879976367003 ) ) ;
#59879 = ORIENTED_EDGE ( 'NONE', *, *, #51644, .T. ) ;
#59880 = DIRECTION ( 'NONE',  ( 1.000000000000000000, 0.000000000000000000, 0.000000000000000000 ) ) ;
#59881 = EDGE_CURVE ( 'NONE', #8532, #51252, #28647, .T. ) ;
#59882 = DIRECTION ( 'NONE',  ( 0.000000000000000000, 1.000000000000000000, 0.000000000000000000 ) ) ;
#59883 = VERTEX_POINT ( 'NONE', #950 ) ;
#59885 = EDGE_CURVE ( 'NONE', #54474, #63459, #27753, .T. ) ;
#59884 = VECTOR ( 'NONE', #55757, 1000.000000000000000 ) ;
#59886 = CARTESIAN_POINT ( 'NONE',  ( 194.5667039024482676, -40.82844715993405060, 129.9678068554150343 ) ) ;
#59887 = CARTESIAN_POINT ( 'NONE',  ( 107.0664832912739683, -25.27030990763060103, 309.2406250056037038 ) ) ;
#59888 = CARTESIAN_POINT ( 'NONE',  ( 115.2346088729120339, -30.22974330756297690, 244.3613395616249875 ) ) ;
#59889 = DIRECTION ( 'NONE',  ( 0.7071067811861589947, -0.7071067811869361508, 0.000000000000000000 ) ) ;
#59890 = B_SPLINE_CURVE_WITH_KNOTS ( 'NONE', 3,
 ( #62051, #20729, #40713, #74352, #33004, #53873, #19832, #5765, #26640, #61596, #53420, #89334, #6650, #26199, #47516, #75253, #47061, #27539 ),
 .UNSPECIFIED., .F., .F.,
 ( 4, 2, 2, 2, 2, 2, 2, 2, 4 ),
 ( 0.000000000000000000, 0.03620097733914664356, 0.07240195467829316223, 0.1086029320174396740, 0.1448039093565861857, 0.1810048866957326974, 0.2172058640348792369, 0.2534068413740257486, 0.2896078187131722603 ),
 .UNSPECIFIED. ) ;
#59891 = CIRCLE ( 'NONE', #46850, 2.750000000000002665 ) ;
#59892 = LINE ( 'NONE', #32646, #34654 ) ;
#59893 = CARTESIAN_POINT ( 'NONE',  ( -3.174999999999664979, 124.5870000000000033, -31.75000000000000000 ) ) ;
#59894 = CARTESIAN_POINT ( 'NONE',  ( 104.5043403851385904, -28.58134581971437882, 249.7409912566480727 ) ) ;
#59897 = CARTESIAN_POINT ( 'NONE',  ( 106.6611865629619160, -26.33404432545466634, 81.10705384733896040 ) ) ;
#59896 = DIRECTION ( 'NONE',  ( 1.000000000000000000, 4.272717921125132861E-14, 0.000000000000000000 ) ) ;
#59895 = VECTOR ( 'NONE', #3145, 1000.000000000000114 ) ;
#59898 = CARTESIAN_POINT ( 'NONE',  ( 120.0727942879283745, 74.60757107455795278, 51.25817907159669318 ) ) ;
#59899 = CARTESIAN_POINT ( 'NONE',  ( 99.02022134730059122, -43.42753157066677261, 116.8784824187679732 ) ) ;
#59900 = VERTEX_POINT ( 'NONE', #69993 ) ;
#59901 = CARTESIAN_POINT ( 'NONE',  ( 132.1654742078716538, -20.71744337670341451, 7.623533105439178392 ) ) ;
#59902 = EDGE_LOOP ( 'NONE', ( #32738, #26294, #43678, #31948 ) ) ;
#59903 = B_SPLINE_CURVE_WITH_KNOTS ( 'NONE', 3,
 ( #67228, #33610, #60405, #59951, #88145, #87684, #18640, #73601, #25907, #25010, #19083, #47220, #45868, #12276, #67685, #61307, #5467, #74949, #19989, #12731, #40421, #68134, #38629, #89026, #26787, #54469, #66331, #55812, #76291, #34496, #82680, #21330, #62206, #89480, #77198, #28121, #75844, #49002, #63557, #49283, #886, #47670, #56269, #7257, #34040, #69931, #1341, #28579, #83563 ),
 .UNSPECIFIED., .F., .F.,
 ( 4, 2, 2, 2, 2, 2, 2, 2, 2, 2, 2, 2, 2, 2, 2, 1, 2, 2, 2, 2, 2, 2, 2, 2, 4 ),
 ( 0.01987186023414422298, 0.02111356671950572264, 0.02235527320486722577, 0.02483868617559022510, 0.02608039266095170741, 0.02732209914631318973, 0.02980551211703611619, 0.03228892508775904613, 0.03353063157312050069, 0.03477233805848195525, 0.03725575102920487131, 0.03849745751456633280, 0.03973916399992778736, 0.04222257697065069648, 0.04346428345601215798, 0.04470598994137361254, 0.04594769642673507404, 0.04718940291209652860, 0.04967281588281947241, 0.05091452236818093391, 0.05215622885354238847, 0.05463964182426533228, 0.05588134830962680766, 0.05712305479498828303, 0.05960646776571126848 ),
 .UNSPECIFIED. ) ;
#59904 = DIRECTION ( 'NONE',  ( -4.299999999999999979E-14, 1.000000000000000000, -4.400000000000000367E-29 ) ) ;
#59905 = CARTESIAN_POINT ( 'NONE',  ( 97.80969226196111777, -40.51824922604903634, 262.6357212258262166 ) ) ;
#59906 = DIRECTION ( 'NONE',  ( 0.000000000000000000, 0.000000000000000000, -1.000000000000000000 ) ) ;
#59907 = ORIENTED_EDGE ( 'NONE', *, *, #78657, .F. ) ;
#59908 = DIRECTION ( 'NONE',  ( 1.000000000000000000, -0.000000000000000000, 0.000000000000000000 ) ) ;
#59910 = ORIENTED_EDGE ( 'NONE', *, *, #16751, .F. ) ;
#59909 = CARTESIAN_POINT ( 'NONE',  ( 116.6387536407295329, -29.65834838561569242, 109.3327681330539605 ) ) ;
#59911 = CARTESIAN_POINT ( 'NONE',  ( 69.63919639214310564, 101.5999999999999943, 94.70900412239863897 ) ) ;
#59912 = CARTESIAN_POINT ( 'NONE',  ( -130.5480414536684179, 95.16896684734908263, 1.658263961150568067 ) ) ;
#59913 = DIRECTION ( 'NONE',  ( 0.000000000000000000, 1.000000000000000000, 0.000000000000000000 ) ) ;
#59914 = VERTEX_POINT ( 'NONE', #14131 ) ;
#59915 = CARTESIAN_POINT ( 'NONE',  ( 116.9251198095579554, -40.18685225151752860, 133.5584824187679658 ) ) ;
#59916 = APPLICATION_PROTOCOL_DEFINITION ( 'draft international standard', 'automotive_design', 1998, #30700 ) ;
#59917 = AXIS2_PLACEMENT_3D ( 'NONE', #15502, #50440, #81972 ) ;
#59918 = LINE ( 'NONE', #24536, #48601 ) ;
#59919 = CARTESIAN_POINT ( 'NONE',  ( 162.5667039024488361, -33.35206098992174617, 117.4678068554150485 ) ) ;
#59920 = ORIENTED_EDGE ( 'NONE', *, *, #16568, .F. ) ;
#59921 = ADVANCED_FACE ( 'NONE', ( #9441 ), #30338, .T. ) ;
#59922 = CIRCLE ( 'NONE', #57139, 7.000000000000006217 ) ;
#59923 = ADVANCED_FACE ( 'NONE', ( #76354 ), #58465, .F. ) ;
#59924 = ORIENTED_EDGE ( 'NONE', *, *, #19918, .T. ) ;
#59925 = CARTESIAN_POINT ( 'NONE',  ( 21.56670390244696733, -23.42844715994183957, 300.4678068554150059 ) ) ;
#59926 = FACE_OUTER_BOUND ( 'NONE', #70272, .T. ) ;
#59927 = DIRECTION ( 'NONE',  ( 1.000000000000000078E-15, 0.000000000000000000, -1.000000000000000000 ) ) ;
#59928 = FACE_OUTER_BOUND ( 'NONE', #76876, .T. ) ;
#59929 = EDGE_CURVE ( 'NONE', #25704, #67615, #49524, .T. ) ;
#59931 = CARTESIAN_POINT ( 'NONE',  ( -8.398302923777746898, 72.98741371662136146, -118.2596197875572415 ) ) ;
#59930 = LINE ( 'NONE', #67663, #63939 ) ;
#59932 = CARTESIAN_POINT ( 'NONE',  ( 97.75841769537090897, -40.38496945966961960, 181.6242637945837259 ) ) ;
#59933 = ORIENTED_EDGE ( 'NONE', *, *, #49774, .T. ) ;
#59934 = EDGE_CURVE ( 'NONE', #20871, #53911, #48614, .T. ) ;
#59935 = CARTESIAN_POINT ( 'NONE',  ( 117.0718954810517261, -35.46248233408972084, 34.92729194434081563 ) ) ;
#59936 = CARTESIAN_POINT ( 'NONE',  ( 97.67678136301130110, -41.13084272647604678, 207.6632443235299661 ) ) ;
#59937 = ADVANCED_FACE ( 'NONE', ( #77259 ), #43941, .F. ) ;
#59939 = EDGE_LOOP ( 'NONE', ( #797, #49519 ) ) ;
#59938 = DIRECTION ( 'NONE',  ( -1.000000000000000000, -0.000000000000000000, -0.000000000000000000 ) ) ;
#59940 = CARTESIAN_POINT ( 'NONE',  ( 101.4370486012140589, -28.02035706366318379, 66.54514908543396245 ) ) ;
#59941 = CARTESIAN_POINT ( 'NONE',  ( 107.0664832912739399, -36.72944715994095333, 289.6356252759107406 ) ) ;
#59942 = CARTESIAN_POINT ( 'NONE',  ( 69.94616667561825807, -138.0587426493221699, 247.6570821721479945 ) ) ;
#59943 = PLANE ( 'NONE',  #35859 ) ;
#59944 = ORIENTED_EDGE ( 'NONE', *, *, #70287, .T. ) ;
#59945 = DIRECTION ( 'NONE',  ( 0.000000000000000000, 2.135044278125299371E-15, -1.000000000000000000 ) ) ;
#59946 = ORIENTED_EDGE ( 'NONE', *, *, #5381, .T. ) ;
#59947 = EDGE_LOOP ( 'NONE', ( #87677, #44081, #13745, #60911 ) ) ;
#59948 = CARTESIAN_POINT ( 'NONE',  ( 109.6042693146342515, -27.68311267370638618, 216.3025356868499500 ) ) ;
#59949 = CIRCLE ( 'NONE', #10625, 5.499999999999999112 ) ;
#59950 = CARTESIAN_POINT ( 'NONE',  ( -34.53140813619931748, 64.60000000000000853, 35.02576496182814481 ) ) ;
#59951 = CARTESIAN_POINT ( 'NONE',  ( -117.8848147242576374, 84.21376545118702950, -12.59751181725430946 ) ) ;
#59952 = CIRCLE ( 'NONE', #26651, 13.00000000000000355 ) ;
#59953 = CARTESIAN_POINT ( 'NONE',  ( 36.65249034007445772, -49.32844715994130524, 180.4678068554150911 ) ) ;
#59954 = CARTESIAN_POINT ( 'NONE',  ( 82.54112294217885903, -37.94037323192714695, 2.740176903238848993 ) ) ;
#59955 = ORIENTED_EDGE ( 'NONE', *, *, #38378, .F. ) ;
#59956 = DIRECTION ( 'NONE',  ( 0.000000000000000000, 0.000000000000000000, 1.000000000000000000 ) ) ;
#59957 = LINE ( 'NONE', #74505, #68749 ) ;
#59958 = VERTEX_POINT ( 'NONE', #23537 ) ;
#59959 = CARTESIAN_POINT ( 'NONE',  ( 105.8960369669305805, -47.10223136823075407, 282.4870538473394390 ) ) ;
#59960 = ORIENTED_EDGE ( 'NONE', *, *, #71445, .F. ) ;
#59961 = VERTEX_POINT ( 'NONE', #55435 ) ;
#59962 = CARTESIAN_POINT ( 'NONE',  ( 110.8229109585819003, -44.00762958608321895, 270.7738046553057529 ) ) ;
#59963 = FACE_BOUND ( 'NONE', #85397, .T. ) ;
#59964 = LINE ( 'NONE', #26803, #72262 ) ;
#59965 = DIRECTION ( 'NONE',  ( 0.7071067811865460184, 0.000000000000000000, 0.7071067811865487940 ) ) ;
#59966 = FACE_OUTER_BOUND ( 'NONE', #13991, .T. ) ;
#59967 = EDGE_CURVE ( 'NONE', #38484, #63081, #58032, .T. ) ;
#59968 = CARTESIAN_POINT ( 'NONE',  ( 107.6569575903311318, -47.81316668278100224, 193.6308633711489620 ) ) ;
#59969 = CARTESIAN_POINT ( 'NONE',  ( 2.860923566319202305, 70.27222073148661252, 118.3221038006948902 ) ) ;
#59970 = EDGE_LOOP ( 'NONE', ( #67440, #21127, #55776, #63894, #89852, #80517 ) ) ;
#59971 = AXIS2_PLACEMENT_3D ( 'NONE', #75750, #69383, #48906 ) ;
#59972 = CARTESIAN_POINT ( 'NONE',  ( 97.24759266268939939, -33.09869426670887549, 62.04419670448196911 ) ) ;
#59973 = CARTESIAN_POINT ( 'NONE',  ( -72.96458098368600531, 101.5999999999999943, -72.96458098368781009 ) ) ;
#59974 = CIRCLE ( 'NONE', #32418, 0.5000000000000073275 ) ;
#59975 = EDGE_CURVE ( 'NONE', #70808, #16796, #11087, .T. ) ;
#59976 = ORIENTED_EDGE ( 'NONE', *, *, #24105, .F. ) ;
#59977 = ORIENTED_EDGE ( 'NONE', *, *, #20318, .T. ) ;
#59978 = VERTEX_POINT ( 'NONE', #49071 ) ;
#59979 = VECTOR ( 'NONE', #82518, 1000.000000000000000 ) ;
#59980 = CARTESIAN_POINT ( 'NONE',  ( 104.4882991616608905, -26.97926274729260854, 160.2813675197272403 ) ) ;
#59981 = FACE_OUTER_BOUND ( 'NONE', #19780, .T. ) ;
#59982 = CARTESIAN_POINT ( 'NONE',  ( 116.7941005169256385, -39.39147994404237352, 153.6152460865006617 ) ) ;
#59983 = CARTESIAN_POINT ( 'NONE',  ( 112.5586783213544066, -42.80550525696455821, 130.9795189410199612 ) ) ;
#59984 = CARTESIAN_POINT ( 'NONE',  ( 96.66048121734328902, -35.80620304765527351, 227.2556252759109725 ) ) ;
#59985 = DIRECTION ( 'NONE',  ( 0.000000000000000000, 0.000000000000000000, -1.000000000000000000 ) ) ;
#59986 = ORIENTED_EDGE ( 'NONE', *, *, #280, .T. ) ;
#59987 = CARTESIAN_POINT ( 'NONE',  ( 130.4667775723041814, 94.30053010088478516, -4.871090541622842274 ) ) ;
#59988 = CARTESIAN_POINT ( 'NONE',  ( 31.89136050872128791, -31.76306994223899238, 117.4678068554150485 ) ) ;
#59989 = ORIENTED_EDGE ( 'NONE', *, *, #32967, .F. ) ;
#59990 = ORIENTED_EDGE ( 'NONE', *, *, #83008, .F. ) ;
#59991 = AXIS2_PLACEMENT_3D ( 'NONE', #36996, #64703, #31496 ) ;
#59992 = ADVANCED_FACE ( 'NONE', ( #76805, #37150 ), #9891, .F. ) ;
#59993 = DIRECTION ( 'NONE',  ( 0.000000000000000000, 0.000000000000000000, 1.000000000000000000 ) ) ;
#59994 = VERTEX_POINT ( 'NONE', #78942 ) ;
#59995 = VERTEX_POINT ( 'NONE', #6862 ) ;
#59996 = DIRECTION ( 'NONE',  ( 0.000000000000000000, 0.000000000000000000, 1.000000000000000000 ) ) ;
#59997 = CARTESIAN_POINT ( 'NONE',  ( 107.0667039024470313, -104.2784471599420471, -19.18411693322902423 ) ) ;
#59998 = CARTESIAN_POINT ( 'NONE',  ( 44.45000000000000284, 66.67499999999999716, 219.0749999999999886 ) ) ;
#59999 = CARTESIAN_POINT ( 'NONE',  ( 98.01111206384085506, -36.61009632703314765, 155.7505150661719995 ) ) ;
#60000 = CARTESIAN_POINT ( 'NONE',  ( 110.5699785786504918, -46.63284631861461804, 37.84705384733994293 ) ) ;
#60001 = CARTESIAN_POINT ( 'NONE',  ( 162.5667039024470171, -33.35206098992711077, 342.9256252759119548 ) ) ;
#60002 = VERTEX_POINT ( 'NONE', #83185 ) ;
#60003 = CARTESIAN_POINT ( 'NONE',  ( 172.5664832912740110, -27.82844715994070484, 323.6756252759119548 ) ) ;
#60004 = VERTEX_POINT ( 'NONE', #20942 ) ;
#60005 = DIRECTION ( 'NONE',  ( 0.000000000000000000, 0.000000000000000000, -1.000000000000000000 ) ) ;
#60006 = ORIENTED_EDGE ( 'NONE', *, *, #23035, .T. ) ;
#60007 = CARTESIAN_POINT ( 'NONE',  ( 97.80672817134072261, -40.50528890471652943, 167.6348551699710185 ) ) ;
#60008 = CARTESIAN_POINT ( 'NONE',  ( 88.24325903289650341, -55.55267141831875222, 14.67562527591095112 ) ) ;
#60009 = CARTESIAN_POINT ( 'NONE',  ( 117.0486299590089203, -35.90762754657916389, 133.8918835446932007 ) ) ;
#60010 = AXIS2_PLACEMENT_3D ( 'NONE', #6097, #62381, #162 ) ;
#60011 = DIRECTION ( 'NONE',  ( -1.000000000000000000, 0.000000000000000000, 0.000000000000000000 ) ) ;
#60012 = VERTEX_POINT ( 'NONE', #67078 ) ;
#60013 = CARTESIAN_POINT ( 'NONE',  ( 110.2909773106953111, -46.66674596437654543, 12.82705384733995402 ) ) ;
#60014 = CARTESIAN_POINT ( 'NONE',  ( 99.95113126132085313, -44.40829767532816419, 42.98133956162492098 ) ) ;
#60015 =( BOUNDED_CURVE ( )  B_SPLINE_CURVE ( 3, ( #63961, #24296, #58784, #84867 ),
 .UNSPECIFIED., .F., .T. ) 
 B_SPLINE_CURVE_WITH_KNOTS ( ( 4, 4 ),
 ( 2.824060085324058217E-12, 1.570796326798421738 ),
 .UNSPECIFIED. ) 
 CURVE ( )  GEOMETRIC_REPRESENTATION_ITEM ( )  RATIONAL_B_SPLINE_CURVE ( ( 1.000000000000000000, 0.8047378541241997363, 0.8047378541241997363, 1.000000000000000000 ) ) 
 REPRESENTATION_ITEM ( '' )  );
#60016 = SURFACE_SIDE_STYLE ('',( #26860 ) ) ;
#60017 = AXIS2_PLACEMENT_3D ( 'NONE', #7758, #12788, #89540 ) ;
#60019 = DIRECTION ( 'NONE',  ( 0.5000000000000008882, -0.8660254037844382635, 2.684678751731760294E-14 ) ) ;
#60018 = CARTESIAN_POINT ( 'NONE',  ( 141.8545562996767444, -1.932463243632623229, 361.9756252759100335 ) ) ;
#60020 = DIRECTION ( 'NONE',  ( 0.000000000000000000, 0.000000000000000000, -1.000000000000000000 ) ) ;
#60021 = DIRECTION ( 'NONE',  ( -1.000000000000000078E-15, 1.000000000000000000, 0.000000000000000000 ) ) ;
#60022 = DIRECTION ( 'NONE',  ( -0.000000000000000000, -0.000000000000000000, 1.000000000000000000 ) ) ;
#60023 = EDGE_CURVE ( 'NONE', #61816, #56160, #47325, .T. ) ;
#60024 = LINE ( 'NONE', #87760, #22852 ) ;
#60025 = EDGE_CURVE ( 'NONE', #77712, #46235, #73441, .T. ) ;
#60026 = LINE ( 'NONE', #33242, #35565 ) ;
#60027 = VERTEX_POINT ( 'NONE', #11214 ) ;
#60028 = CARTESIAN_POINT ( 'NONE',  ( 99.10996421577944204, -43.53389204880360097, 31.88991099019594699 ) ) ;
#60029 = CARTESIAN_POINT ( 'NONE',  ( 96.12521010412353917, -35.16020481777900386, 222.2251490854349640 ) ) ;
#60030 = CARTESIAN_POINT ( 'NONE',  ( 109.6483737747080198, -46.85224817473300618, 43.77562527591094721 ) ) ;
#60031 = EDGE_CURVE ( 'NONE', #31377, #17700, #88434, .T. ) ;
#60033 = CYLINDRICAL_SURFACE ( 'NONE', #13701, 2.517500000000005844 ) ;
#60032 = LINE ( 'NONE', #32792, #69715 ) ;
#60034 = DIRECTION ( 'NONE',  ( 0.000000000000000000, 1.000000000000000000, 0.000000000000000000 ) ) ;
#60035 = VECTOR ( 'NONE', #15548, 1000.000000000000000 ) ;
#60036 = AXIS2_PLACEMENT_3D ( 'NONE', #6875, #62283, #7336 ) ;
#60037 = VECTOR ( 'NONE', #84857, 1000.000000000000000 ) ;
#60038 = EDGE_LOOP ( 'NONE', ( #26798, #47255, #61772, #58781 ) ) ;
#60039 = DIRECTION ( 'NONE',  ( 1.000000000000000000, 0.000000000000000000, 0.000000000000000000 ) ) ;
#60040 = EDGE_LOOP ( 'NONE', ( #63892, #54980, #47756, #37793, #66582 ) ) ;
#60041 = CARTESIAN_POINT ( 'NONE',  ( 98.13101841594846064, -32.75189731695859763, 96.99276813305296230 ) ) ;
#60042 = EDGE_CURVE ( 'NONE', #70341, #810, #32543, .T. ) ;
#60044 = ORIENTED_EDGE ( 'NONE', *, *, #5816, .T. ) ;
#60043 = CARTESIAN_POINT ( 'NONE',  ( 12.30956025940465537, 85.78406842316067582, 129.9748705538268325 ) ) ;
#60045 = AXIS2_PLACEMENT_3D ( 'NONE', #87413, #3847, #10216 ) ;
#60046 = CARTESIAN_POINT ( 'NONE',  ( 104.1918496689535090, -26.69446299336411599, 221.2984824187679465 ) ) ;
#60047 = FACE_OUTER_BOUND ( 'NONE', #60120, .T. ) ;
#60048 = LINE ( 'NONE', #25541, #47797 ) ;
#60049 = EDGE_CURVE ( 'NONE', #28641, #7172, #38468, .T. ) ;
#60050 = LINE ( 'NONE', #71926, #18165 ) ;
#60051 = CARTESIAN_POINT ( 'NONE',  ( 115.8254323915925568, -31.73001882795865214, 45.23979194264600778 ) ) ;
#60052 = CARTESIAN_POINT ( 'NONE',  ( 131.5441285970347280, -37.82508440162272478, 2.797770139040990589 ) ) ;
#60053 = CARTESIAN_POINT ( 'NONE',  ( 28.57499999999999929, 77.96728223830730542, 294.9574999999999818 ) ) ;
#60054 = CARTESIAN_POINT ( 'NONE',  ( 108.5509251780138271, -26.47246927008487205, 149.9737205140069420 ) ) ;
#60055 = ORIENTED_EDGE ( 'NONE', *, *, #34710, .F. ) ;
#60056 = VERTEX_POINT ( 'NONE', #3960 ) ;
#60057 = CARTESIAN_POINT ( 'NONE',  ( 97.47186360698646013, -39.79766782782348855, 128.0044404487539396 ) ) ;
#60058 = CARTESIAN_POINT ( 'NONE',  ( 168.0371591254543091, -48.62818131005519717, 313.9678068554149490 ) ) ;
#60060 = DIRECTION ( 'NONE',  ( -1.000000000000000078E-15, 1.000000000000000083E-30, 1.000000000000000000 ) ) ;
#60059 = CARTESIAN_POINT ( 'NONE',  ( 117.4251315444614789, -36.24242395571268816, 264.8518157521010608 ) ) ;
#60061 = CARTESIAN_POINT ( 'NONE',  ( 105.8694971003958614, -26.37070548771162493, 321.6188579224977389 ) ) ;
#60062 = DIRECTION ( 'NONE',  ( 0.000000000000000000, 0.000000000000000000, -1.000000000000000000 ) ) ;
#60063 = CARTESIAN_POINT ( 'NONE',  ( 118.1708971306823486, 74.16967745525860778, -9.551705748360291182 ) ) ;
#60064 = B_SPLINE_CURVE_WITH_KNOTS ( 'NONE', 3,
 ( #77524, #1677, #62540, #49796, #36643, #57513, #48888, #56614, #35273, #23021, #16199, #83440, #762, #64345, #76626, #8488, #84358, #29380, #8030, #62983, #316, #28462, #56152, #29826, #55690, #42972, #43877, #7137, #34833, #22570, #15306, #35724, #63439, #83903, #1225, #21674, #28013, #50243, #14408, #77978, #63900, #49348, #42083, #57057, #69814, #77079, #43424, #7587, #14861 ),
 .UNSPECIFIED., .F., .F.,
 ( 4, 2, 2, 2, 2, 2, 2, 2, 2, 2, 2, 2, 2, 2, 2, 1, 2, 2, 2, 2, 2, 2, 2, 2, 4 ),
 ( 0.01986933033599076401, 0.02111088875730812026, 0.02235244717862547650, 0.02483556402126018900, 0.02607712244257756606, 0.02731868086389493966, 0.02980179770652969379, 0.03228491454916444792, 0.03352647297048182151, 0.03476803139179918817, 0.03725114823443395617, 0.03849270665575131589, 0.03973426507706866173, 0.04221738191970339504, 0.04345894034102079639, 0.04470049876233819081, 0.04594205718365558522, 0.04718361560497297963, 0.04966673244760778927, 0.05090829086892520450, 0.05214984929024261973, 0.05463296613287743630, 0.05587452455419480990, 0.05711608297551218349, 0.05959919981814693069 ),
 .UNSPECIFIED. ) ;
#60065 = LINE ( 'NONE', #40979, #26999 ) ;
#60066 = CARTESIAN_POINT ( 'NONE',  ( 107.0664832912739683, -23.56278049327427482, 308.7195067599733420 ) ) ;
#60067 = CARTESIAN_POINT ( 'NONE',  ( 70.63919639214310564, 100.5999999999999659, 95.21359708083839735 ) ) ;
#60068 = CARTESIAN_POINT ( 'NONE',  ( 117.2701380961606645, -34.52720868313122082, 183.9956252759109532 ) ) ;
#60069 = CARTESIAN_POINT ( 'NONE',  ( 102.0673672214506098, -27.97029977251938959, 170.4888039060526808 ) ) ;
#60070 = ORIENTED_EDGE ( 'NONE', *, *, #15554, .F. ) ;
#60071 = ORIENTED_EDGE ( 'NONE', *, *, #63331, .F. ) ;
#60072 = DIRECTION ( 'NONE',  ( 0.000000000000000000, 1.000000000000000000, 0.000000000000000000 ) ) ;
#60073 = CARTESIAN_POINT ( 'NONE',  ( 81.24992100027586162, -21.21189388394623165, 8.006199623923167863 ) ) ;
#60074 = CARTESIAN_POINT ( 'NONE',  ( 115.0895278777549606, -30.61844485430380303, 184.3443006593670930 ) ) ;
#60075 = LINE ( 'NONE', #18763, #85445 ) ;
#60076 = AXIS2_PLACEMENT_3D ( 'NONE', #25870, #45836, #39041 ) ;
#60077 = CARTESIAN_POINT ( 'NONE',  ( 97.07191748774732787, -35.37976532927168449, 96.21906654814019078 ) ) ;
#60078 = ORIENTED_EDGE ( 'NONE', *, *, #4477, .T. ) ;
#60079 = CARTESIAN_POINT ( 'NONE',  ( 98.30747362804066825, -41.72872748435885626, 61.73977921712166506 ) ) ;
#60080 = CIRCLE ( 'NONE', #34024, 7.143749999999999822 ) ;
#60081 = ADVANCED_FACE ( 'NONE', ( #53866 ), #46616, .F. ) ;
#60082 = CARTESIAN_POINT ( 'NONE',  ( 98.53748378420890219, -30.73418253943381728, 205.8384824187679669 ) ) ;
#60083 = DIRECTION ( 'NONE',  ( 0.000000000000000000, 0.000000000000000000, 1.000000000000000000 ) ) ;
#60084 = ORIENTED_EDGE ( 'NONE', *, *, #23526, .T. ) ;
#60085 = VERTEX_POINT ( 'NONE', #38918 ) ;
#60086 = CARTESIAN_POINT ( 'NONE',  ( 114.6261096459129760, -43.30823112647709650, 64.25718145844111007 ) ) ;
#60087 = DIRECTION ( 'NONE',  ( -0.000000000000000000, 1.000000000000000000, 0.000000000000000000 ) ) ;
#60088 = CARTESIAN_POINT ( 'NONE',  ( 98.38054347145074985, -41.69548487457510078, 166.7398071395968486 ) ) ;
#60089 = CARTESIAN_POINT ( 'NONE',  ( 111.0211786934911231, -29.03130846684521060, 17.52904275054395455 ) ) ;
#60090 = CARTESIAN_POINT ( 'NONE',  ( 117.1846329980857178, -34.12938843674525202, 120.0270538473389479 ) ) ;
#60091 = CARTESIAN_POINT ( 'NONE',  ( -446.0240000000000009, 14.28749999999982201, 95.25000000000000000 ) ) ;
#60092 = ORIENTED_EDGE ( 'NONE', *, *, #78704, .F. ) ;
#60093 = PLANE ( 'NONE',  #2963 ) ;
#60094 = CARTESIAN_POINT ( 'NONE',  ( 82.59705637153267332, -17.65296049054653338, 7.043700149389792387 ) ) ;
#60095 = ORIENTED_EDGE ( 'NONE', *, *, #42537, .T. ) ;
#60096 = ORIENTED_EDGE ( 'NONE', *, *, #78745, .T. ) ;
#60097 = VECTOR ( 'NONE', #49810, 1000.000000000000000 ) ;
#60098 = AXIS2_PLACEMENT_3D ( 'NONE', #514, #22315, #63645 ) ;
#60099 = CARTESIAN_POINT ( 'NONE',  ( 30.48091746481830100, -49.32844715994148288, 300.4678068554150059 ) ) ;
#60100 = AXIS2_PLACEMENT_3D ( 'NONE', #51679, #25324, #66202 ) ;
#60101 = EDGE_LOOP ( 'NONE', ( #28907, #72726, #50625, #53252 ) ) ;
#60102 = VERTEX_POINT ( 'NONE', #45277 ) ;
#60103 = DIRECTION ( 'NONE',  ( 1.000000000000000000, 4.163336342344333240E-14, 0.000000000000000000 ) ) ;
#60104 = VECTOR ( 'NONE', #57911, 1000.000000000000000 ) ;
#60105 = CARTESIAN_POINT ( 'NONE',  ( 98.14502816950557929, -38.28518133910327492, 45.87432458998197404 ) ) ;
#60107 = CARTESIAN_POINT ( 'NONE',  ( 97.07499705966343129, -41.51125058752681696, 216.6937205140059461 ) ) ;
#60106 = CIRCLE ( 'NONE', #20975, 2.116999999999980009 ) ;
#60108 = AXIS2_PLACEMENT_3D ( 'NONE', #49670, #83775, #1093 ) ;
#60109 = CARTESIAN_POINT ( 'NONE',  ( 117.7567108552515265, -34.01230579303179979, 169.0365776568629599 ) ) ;
#60111 = CARTESIAN_POINT ( 'NONE',  ( 112.3382693683599314, -28.20726497302192826, 285.6356252759109680 ) ) ;
#60110 = CARTESIAN_POINT ( 'NONE',  ( 180.3503142329310265, -29.99615139349890569, -5.074374724088000832 ) ) ;
#60112 = CARTESIAN_POINT ( 'NONE',  ( 31.85959712127300847, -23.19206098994050436, -5.074374724088000832 ) ) ;
#60113 = DIRECTION ( 'NONE',  ( -1.000000000000000000, -1.734723475976808672E-15, 0.000000000000000000 ) ) ;
#60115 = ORIENTED_EDGE ( 'NONE', *, *, #14221, .F. ) ;
#60114 = EDGE_CURVE ( 'NONE', #8213, #66245, #69076, .T. ) ;
#60116 = EDGE_CURVE ( 'NONE', #43969, #75973, #66171, .T. ) ;
#60117 = VERTEX_POINT ( 'NONE', #80284 ) ;
#60118 = CARTESIAN_POINT ( 'NONE',  ( 7.661254700127822836, 98.64746158385918307, 320.6630000000000109 ) ) ;
#60119 = CARTESIAN_POINT ( 'NONE',  ( 116.8989603263487567, -40.32514756444775372, 218.5470538473399529 ) ) ;
#60120 = EDGE_LOOP ( 'NONE', ( #69724, #72422, #52153, #65833 ) ) ;
#60121 = CARTESIAN_POINT ( 'NONE',  ( 98.37959078170875671, -29.89446464491232192, 200.8080062282919869 ) ) ;
#60122 = CARTESIAN_POINT ( 'NONE',  ( 90.44969454456416713, -55.86395651782494554, 229.5838068554169809 ) ) ;
#60123 = EDGE_CURVE ( 'NONE', #4783, #49381, #38038, .T. ) ;
#60124 = CARTESIAN_POINT ( 'NONE',  ( 134.0664832912740110, -36.72944715994100306, -5.074374724089001809 ) ) ;
#60125 = CARTESIAN_POINT ( 'NONE',  ( 143.8525571913658894, -140.3399344531919155, 246.6497317326439429 ) ) ;
#60127 = PLANE ( 'NONE',  #50004 ) ;
#60126 = CARTESIAN_POINT ( 'NONE',  ( 114.9425050820284184, -34.80279201792794908, 277.6356252759108543 ) ) ;
#60128 = FACE_OUTER_BOUND ( 'NONE', #29980, .T. ) ;
#60129 = DIRECTION ( 'NONE',  ( 0.000000000000000000, 0.000000000000000000, -1.000000000000000000 ) ) ;
#60130 = DIRECTION ( 'NONE',  ( 1.000000000000000078E-15, 0.000000000000000000, 1.000000000000000000 ) ) ;
#60131 = CARTESIAN_POINT ( 'NONE',  ( 68.01586774711397254, -137.1827438074501799, 247.2088461600285996 ) ) ;
#60132 = CYLINDRICAL_SURFACE ( 'NONE', #41624, 0.9999999999999731326 ) ;
#60133 = EDGE_CURVE ( 'NONE', #8036, #32982, #23613, .T. ) ;
#60134 = CARTESIAN_POINT ( 'NONE',  ( 80.06648329127399677, -8.350947159940998787, 293.6356252759119911 ) ) ;
#60136 = ORIENTED_EDGE ( 'NONE', *, *, #30644, .T. ) ;
#60135 = CARTESIAN_POINT ( 'NONE',  ( 208.9149999999999920, 28.98850000000000193, -58.73749999999999716 ) ) ;
#60137 = DIRECTION ( 'NONE',  ( 1.000000000000000078E-15, -1.000000000000000083E-30, -1.000000000000000000 ) ) ;
#60138 = CARTESIAN_POINT ( 'NONE',  ( 110.2626856154920603, -26.74582790018529366, 234.8299109901969643 ) ) ;
#60139 = CARTESIAN_POINT ( 'NONE',  ( 95.48802730109245829, -34.20477442036718685, 102.1556252759109640 ) ) ;
#60140 = CARTESIAN_POINT ( 'NONE',  ( 97.43303641489029587, -40.91689460032421266, 227.6527681330539679 ) ) ;
#60141 = DIRECTION ( 'NONE',  ( -0.9068632946707805287, 0.4214249218767882610, -9.068632946707800501E-16 ) ) ;
#60142 = DIRECTION ( 'NONE',  ( -1.000000000000000000, -5.512527431108013646E-15, 0.000000000000000000 ) ) ;
#60144 = CARTESIAN_POINT ( 'NONE',  ( 97.06670390244703128, -104.2784471599409244, 17.71780685541799016 ) ) ;
#60143 = CARTESIAN_POINT ( 'NONE',  ( 19.56670390244734747, -25.42844715994192129, 300.4678068554150059 ) ) ;
#60145 = FACE_OUTER_BOUND ( 'NONE', #29457, .T. ) ;
#60146 = LINE ( 'NONE', #33358, #74692 ) ;
#60147 = VECTOR ( 'NONE', #79839, 1000.000000000000000 ) ;
#60148 = ORIENTED_EDGE ( 'NONE', *, *, #87704, .T. ) ;
#60149 = ORIENTED_EDGE ( 'NONE', *, *, #53470, .F. ) ;
#60150 = CARTESIAN_POINT ( 'NONE',  ( 99.43039265704440766, -41.59799905411310306, 141.1886103042669731 ) ) ;
#60151 = ADVANCED_FACE ( 'NONE', ( #72996 ), #73471, .T. ) ;
#60153 = ORIENTED_EDGE ( 'NONE', *, *, #15096, .T. ) ;
#60152 = DIRECTION ( 'NONE',  ( -2.544367396927093358E-16, 0.000000000000000000, -1.000000000000000000 ) ) ;
#60154 = CARTESIAN_POINT ( 'NONE',  ( -479.3614999999999782, 22.53639197104660141, 90.48749999999999716 ) ) ;
#60155 = CARTESIAN_POINT ( 'NONE',  ( 114.7552509866191599, -44.63809267644810319, 114.2022919425779719 ) ) ;
#60156 = DIRECTION ( 'NONE',  ( -0.9254794337955620787, -0.3787978585227822492, 0.000000000000000000 ) ) ;
#60157 = EDGE_CURVE ( 'NONE', #85945, #6718, #85112, .T. ) ;
#60158 = EDGE_CURVE ( 'NONE', #1704, #19337, #63304, .T. ) ;
#60159 = CARTESIAN_POINT ( 'NONE',  ( 270.8910000000000196, 40.03750000000000142, -67.11950000000000216 ) ) ;
#60160 = CARTESIAN_POINT ( 'NONE',  ( 208.9149999999999920, 37.33800000000000097, 50.79999999999999716 ) ) ;
#60161 = DIRECTION ( 'NONE',  ( -1.000000000000000000, -1.541976423090496028E-15, 0.000000000000000000 ) ) ;
#60162 = EDGE_CURVE ( 'NONE', #27495, #47011, #44416, .T. ) ;
#60163 = CARTESIAN_POINT ( 'NONE',  ( 99.77418633167435758, -43.29726106931981633, 56.90991099019693422 ) ) ;
#60164 = ORIENTED_EDGE ( 'NONE', *, *, #24204, .F. ) ;
#60165 = EDGE_LOOP ( 'NONE', ( #69640, #28404, #12548, #46730 ) ) ;
#60166 = ORIENTED_EDGE ( 'NONE', *, *, #85627, .T. ) ;
#60167 = VECTOR ( 'NONE', #65028, 1000.000000000000000 ) ;
#60168 = VECTOR ( 'NONE', #29021, 1000.000000000000114 ) ;
#60169 = CARTESIAN_POINT ( 'NONE',  ( 46.32460016641727663, -48.34074026909785005, 249.9678068554150343 ) ) ;
#60170 = VECTOR ( 'NONE', #57954, 1000.000000000000000 ) ;
#60172 = DIRECTION ( 'NONE',  ( -1.000000000000000000, -1.206764157201257538E-15, 0.000000000000000000 ) ) ;
#60171 = CARTESIAN_POINT ( 'NONE',  ( 112.1511370651176662, -26.84216853020821958, 165.6984824187679521 ) ) ;
#60173 = DIRECTION ( 'NONE',  ( 0.000000000000000000, 0.000000000000000000, 1.000000000000000000 ) ) ;
#60174 = PLANE ( 'NONE',  #88714 ) ;
#60176 = DIRECTION ( 'NONE',  ( -1.821231995776179916E-16, 0.000000000000000000, -1.000000000000000000 ) ) ;
#60175 = AXIS2_PLACEMENT_3D ( 'NONE', #34352, #7113, #5772 ) ;
#60177 = AXIS2_PLACEMENT_3D ( 'NONE', #25439, #54459, #42089 ) ;
#60178 = CARTESIAN_POINT ( 'NONE',  ( 165.9667039024459996, -26.71338133339301635, 193.9678068554150059 ) ) ;
#60179 = CARTESIAN_POINT ( 'NONE',  ( 116.7949810323142117, -39.38834386435669188, 179.6147497770267876 ) ) ;
#60180 = CARTESIAN_POINT ( 'NONE',  ( 107.3204973292724276, -25.70223992296332582, 75.04610146638695767 ) ) ;
#60181 = ORIENTED_EDGE ( 'NONE', *, *, #7024, .F. ) ;
#60182 = VERTEX_POINT ( 'NONE', #719 ) ;
#60183 = DIRECTION ( 'NONE',  ( 1.000000000000000000, 4.443626637970137948E-14, 0.000000000000000000 ) ) ;
#60184 = DIRECTION ( 'NONE',  ( -1.000000000000000000, 0.000000000000000000, -2.108231265501709878E-16 ) ) ;
#60185 = CARTESIAN_POINT ( 'NONE',  ( 131.3179999999999836, 44.45000000000000284, 69.10794311903988785 ) ) ;
#60186 = CARTESIAN_POINT ( 'NONE',  ( 100.6382899380647871, -31.69863749346629689, 153.6166617981629656 ) ) ;
#60187 = AXIS2_PLACEMENT_3D ( 'NONE', #77357, #22857, #56448 ) ;
#60188 = EDGE_CURVE ( 'NONE', #81179, #6628, #2366, .T. ) ;
#60189 = CARTESIAN_POINT ( 'NONE',  ( -89.60916260784479448, 223.9999999999999716, 134.1927865330827103 ) ) ;
#60190 = VERTEX_POINT ( 'NONE', #54311 ) ;
#60191 = VERTEX_POINT ( 'NONE', #7547 ) ;
#60192 = PLANE ( 'NONE',  #81577 ) ;
#60193 = EDGE_LOOP ( 'NONE', ( #24858, #23001, #10174, #45464 ) ) ;
#60194 = ORIENTED_EDGE ( 'NONE', *, *, #4173, .T. ) ;
#60195 = DIRECTION ( 'NONE',  ( 0.000000000000000000, 1.000000000000000000, -0.000000000000000000 ) ) ;
#60196 = CARTESIAN_POINT ( 'NONE',  ( 102.2713888833019240, -44.80927359098731699, 203.5939642582779641 ) ) ;
#60197 = FACE_OUTER_BOUND ( 'NONE', #25034, .T. ) ;
#60198 = CARTESIAN_POINT ( 'NONE',  ( 118.5667039024470313, -104.2784471599408533, 19.21780685541799016 ) ) ;
#60199 = STYLED_ITEM ( 'NONE', ( #45033 ), #80246 ) ;
#60200 = DIRECTION ( 'NONE',  ( 0.7071067811864687469, 0.7071067811866262875, 7.071067811864681542E-16 ) ) ;
#60201 = ORIENTED_EDGE ( 'NONE', *, *, #34177, .F. ) ;
#60202 = ORIENTED_EDGE ( 'NONE', *, *, #40782, .F. ) ;
#60203 = ADVANCED_FACE ( 'NONE', ( #41591 ), #69324, .F. ) ;
#60204 = CIRCLE ( 'NONE', #51525, 27.99999999999999645 ) ;
#60205 = VERTEX_POINT ( 'NONE', #27091 ) ;
#60206 = ORIENTED_EDGE ( 'NONE', *, *, #52171, .F. ) ;
#60207 = ADVANCED_FACE ( 'NONE', ( #83403 ), #21179, .F. ) ;
#60208 = CARTESIAN_POINT ( 'NONE',  ( 99.19750579858670392, -34.55944272753168889, 248.9309475124489950 ) ) ;
#60209 = EDGE_CURVE ( 'NONE', #10240, #27695, #56110, .T. ) ;
#60210 = CARTESIAN_POINT ( 'NONE',  ( 100.2843123851674960, -46.47809700006297362, 87.09276813305393716 ) ) ;
#60211 = CARTESIAN_POINT ( 'NONE',  ( 101.1533894386775074, -27.41820966596953468, 65.51467289495799662 ) ) ;
#60212 = CARTESIAN_POINT ( 'NONE',  ( 112.6007387669400686, -28.69124247953021367, 249.5838068554169240 ) ) ;
#60213 = DIRECTION ( 'NONE',  ( -0.0001713722456127401463, 0.9999999853157766072, 1.713722456137401502E-19 ) ) ;
#60214 = DIRECTION ( 'NONE',  ( -4.012088370409549976E-14, 1.000000000000000000, 0.000000000000000000 ) ) ;
#60215 = CARTESIAN_POINT ( 'NONE',  ( 95.56951908670150431, -39.60249947413915805, 162.5213395616259788 ) ) ;
#60216 = PLANE ( 'NONE',  #17529 ) ;
#60217 = ORIENTED_EDGE ( 'NONE', *, *, #27740, .T. ) ;
#60218 = CARTESIAN_POINT ( 'NONE',  ( 63.06670390244732971, -24.92844715994017690, 300.4678068554150627 ) ) ;
#60220 = ORIENTED_EDGE ( 'NONE', *, *, #6824, .F. ) ;
#60219 = ADVANCED_FACE ( 'NONE', ( #7099, #47510 ), #89329, .T. ) ;
#60221 = EDGE_CURVE ( 'NONE', #27344, #59219, #54760, .T. ) ;
#60222 = VERTEX_POINT ( 'NONE', #62499 ) ;
#60223 = CARTESIAN_POINT ( 'NONE',  ( 97.81541838259728650, -40.52652817096748805, 132.6367908339016424 ) ) ;
#60224 = LINE ( 'NONE', #53397, #66292 ) ;
#60225 = VERTEX_POINT ( 'NONE', #47056 ) ;
#60226 = ADVANCED_FACE ( 'NONE', ( #33451 ), #14370, .F. ) ;
#60227 = VECTOR ( 'NONE', #77964, 1000.000000000000000 ) ;
#60228 = CARTESIAN_POINT ( 'NONE',  ( 87.06648329127425257, -46.72944715994106701, -4.970821333495708316 ) ) ;
#60229 = EDGE_LOOP ( 'NONE', ( #58778, #15286 ) ) ;
#60230 = VECTOR ( 'NONE', #86454, 1000.000000000000114 ) ;
#60231 = VECTOR ( 'NONE', #33271, 1000.000000000000000 ) ;
#60232 = CARTESIAN_POINT ( 'NONE',  ( 104.4081006355542058, -46.45808913331583767, 177.3647919407246434 ) ) ;
#60233 = CARTESIAN_POINT ( 'NONE',  ( 104.2140152791992875, -25.22710339543701963, 90.26991099019693365 ) ) ;
#60234 = CARTESIAN_POINT ( 'NONE',  ( -4.352199961275779572, 70.61852695876001462, 130.4834258897450923 ) ) ;
#60235 = VECTOR ( 'NONE', #14098, 1000.000000000000114 ) ;
#60236 = EDGE_CURVE ( 'NONE', #43365, #59070, #57526, .T. ) ;
#60237 = DIRECTION ( 'NONE',  ( 0.000000000000000000, -1.000000000000000000, 0.000000000000000000 ) ) ;
#60238 = DIRECTION ( 'NONE',  ( 1.000000000000000000, 4.163336342344333240E-14, 0.000000000000000000 ) ) ;
#60241 = CARTESIAN_POINT ( 'NONE',  ( 98.45302666770176359, -29.83944080489372652, 191.7775300378159784 ) ) ;
#60240 = CARTESIAN_POINT ( 'NONE',  ( 97.81225633602475966, -40.51881169864816457, 56.63532730191191433 ) ) ;
#60239 = CARTESIAN_POINT ( 'NONE',  ( 104.4081006511264320, -46.45808913744465229, 143.3647919417593357 ) ) ;
#60242 = CYLINDRICAL_SURFACE ( 'NONE', #59646, 0.4999999999999933387 ) ;
#60243 = CARTESIAN_POINT ( 'NONE',  ( 88.90000000000000568, 69.84999999999999432, 219.0749999999999886 ) ) ;
#60244 = ORIENTED_EDGE ( 'NONE', *, *, #49877, .F. ) ;
#60245 = DIRECTION ( 'NONE',  ( 0.000000000000000000, 0.000000000000000000, -1.000000000000000000 ) ) ;
#60246 = CIRCLE ( 'NONE', #89327, 7.143750000000004263 ) ;
#60247 = DIRECTION ( 'NONE',  ( 0.000000000000000000, 1.000000000000000000, 0.000000000000000000 ) ) ;
#60248 = CARTESIAN_POINT ( 'NONE',  ( 112.1414192606818574, -28.01400143680720944, 134.6564062991808441 ) ) ;
#60249 = ADVANCED_FACE ( 'NONE', ( #48850 ), #26636, .T. ) ;
#60250 = CIRCLE ( 'NONE', #38469, 6.349999999999994316 ) ;
#60251 = DIRECTION ( 'NONE',  ( -1.000000000000000000, 0.000000000000000000, 0.000000000000000000 ) ) ;
#60253 = ORIENTED_EDGE ( 'NONE', *, *, #8953, .F. ) ;
#60252 = CARTESIAN_POINT ( 'NONE',  ( 110.2694181837619141, -26.72479813065621812, 234.8299109901969643 ) ) ;
#60254 = CARTESIAN_POINT ( 'NONE',  ( 63.56670390244800473, -40.82844715994016127, 249.9678068554150343 ) ) ;
#60255 = CARTESIAN_POINT ( 'NONE',  ( 115.9451031845006099, -42.19318012571019949, 14.38705384733995984 ) ) ;
#60256 = CARTESIAN_POINT ( 'NONE',  ( 98.24414503606394078, -31.02815815664761345, 141.8699109901969564 ) ) ;
#60257 = CARTESIAN_POINT ( 'NONE',  ( 19.56670390244740076, -47.82844715994204421, 180.4678068554150911 ) ) ;
#60258 = CARTESIAN_POINT ( 'NONE',  ( 6.359443759653470529, 93.55095829381066608, -130.4015408541779379 ) ) ;
#60259 = AXIS2_PLACEMENT_3D ( 'NONE', #48988, #20425, #35374 ) ;
#60260 = CARTESIAN_POINT ( 'NONE',  ( -15.88716625750469902, 65.60000000000000853, -53.54073290201169044 ) ) ;
#60261 = FACE_OUTER_BOUND ( 'NONE', #71085, .T. ) ;
#60262 = FACE_OUTER_BOUND ( 'NONE', #20305, .T. ) ;
#60263 = VERTEX_POINT ( 'NONE', #88883 ) ;
#60264 = CIRCLE ( 'NONE', #44318, 2.517500000000005844 ) ;
#60265 = VERTEX_POINT ( 'NONE', #48394 ) ;
#60266 = ORIENTED_EDGE ( 'NONE', *, *, #80033, .T. ) ;
#60267 = VERTEX_POINT ( 'NONE', #82079 ) ;
#60268 = DIRECTION ( 'NONE',  ( 0.000000000000000000, -1.000000000000000000, 0.000000000000000000 ) ) ;
#60269 = CARTESIAN_POINT ( 'NONE',  ( 111.3142535964730371, -27.23286288913599051, 20.74133956162494030 ) ) ;
#60270 = DIRECTION ( 'NONE',  ( 0.000000000000000000, 1.000000000000000000, 0.000000000000000000 ) ) ;
#60271 = CARTESIAN_POINT ( 'NONE',  ( 112.3567964431407660, -140.4754596735087375, 246.9959941585700278 ) ) ;
#60272 = VECTOR ( 'NONE', #24811, 1000.000000000000000 ) ;
#60273 = EDGE_CURVE ( 'NONE', #20049, #14493, #76332, .T. ) ;
#60276 = EDGE_CURVE ( 'NONE', #69613, #30635, #22472, .T. ) ;
#60275 = DIRECTION ( 'NONE',  ( 1.000000000000000000, 0.000000000000000000, 0.000000000000000000 ) ) ;
#60274 = CARTESIAN_POINT ( 'NONE',  ( 188.5667039024479834, -62.87844715994099687, 295.9678068554150059 ) ) ;
#60277 = CARTESIAN_POINT ( 'NONE',  ( 115.1107970995275736, -40.88897666221423322, 242.8571817328389670 ) ) ;
#60278 = ORIENTED_EDGE ( 'NONE', *, *, #47635, .T. ) ;
#60279 = ORIENTED_EDGE ( 'NONE', *, *, #70412, .T. ) ;
#60280 = CIRCLE ( 'NONE', #48665, 11.45913725231036118 ) ;
#60281 = ORIENTED_EDGE ( 'NONE', *, *, #29471, .T. ) ;
#60282 = FACE_OUTER_BOUND ( 'NONE', #51315, .T. ) ;
#60283 = VECTOR ( 'NONE', #12426, 1000.000000000000000 ) ;
#60284 = DIRECTION ( 'NONE',  ( 0.000000000000000000, 1.000000000000000000, 0.000000000000000000 ) ) ;
#60285 = LINE ( 'NONE', #13500, #17978 ) ;
#60286 = CARTESIAN_POINT ( 'NONE',  ( 83.06670390244796920, -64.87844715994098976, 207.5838068554149913 ) ) ;
#60287 = CARTESIAN_POINT ( 'NONE',  ( 104.6647032408819200, -45.25937870008434771, 18.79015473446898810 ) ) ;
#60288 = CARTESIAN_POINT ( 'NONE',  ( 118.4880192609368379, 94.60304557064716846, 4.087421425393760188 ) ) ;
#60289 = CARTESIAN_POINT ( 'NONE',  ( 36.65249034007445772, -49.32844715994130524, 180.4678068554150911 ) ) ;
#60290 = CARTESIAN_POINT ( 'NONE',  ( 95.96284676697203508, -37.29622633765243478, 271.3670538473399461 ) ) ;
#60291 = LINE ( 'NONE', #12615, #68946 ) ;
#60292 = ORIENTED_EDGE ( 'NONE', *, *, #19678, .T. ) ;
#60293 = CARTESIAN_POINT ( 'NONE',  ( 61.67079006425787924, -0.9306969701470987344, 394.9756252759102040 ) ) ;
#60294 = CARTESIAN_POINT ( 'NONE',  ( 107.2792697713003776, -24.20934055526686279, 321.5865679059475610 ) ) ;
#60295 = CARTESIAN_POINT ( 'NONE',  ( 104.3513172347134770, -44.42734293102004273, 55.12523322673396109 ) ) ;
#60296 = AXIS2_PLACEMENT_3D ( 'NONE', #20433, #14056, #83556 ) ;
#60297 = CIRCLE ( 'NONE', #55948, 10.04999999999999361 ) ;
#60298 = DIRECTION ( 'NONE',  ( 0.8660254037844392627, 0.000000000000000000, 0.4999999999999990563 ) ) ;
#60299 = DIRECTION ( 'NONE',  ( 0.000000000000000000, -1.000000000000000000, 0.000000000000000000 ) ) ;
#60300 = CARTESIAN_POINT ( 'NONE',  ( 99.04404928436410671, -42.84123934602111206, 192.8438477477418758 ) ) ;
#60301 = ORIENTED_EDGE ( 'NONE', *, *, #64557, .T. ) ;
#60302 = DIRECTION ( 'NONE',  ( 0.000000000000000000, -8.792068030499130893E-15, 1.000000000000000000 ) ) ;
#60303 = CARTESIAN_POINT ( 'NONE',  ( 124.8813761161696476, 57.47090627086830494, -38.07277077706557833 ) ) ;
#60304 = ORIENTED_EDGE ( 'NONE', *, *, #16812, .F. ) ;
#60305 = CARTESIAN_POINT ( 'NONE',  ( 102.3022244709477775, -27.41667396567568815, 120.4527681330539792 ) ) ;
#60306 = ORIENTED_EDGE ( 'NONE', *, *, #64665, .T. ) ;
#60307 = CARTESIAN_POINT ( 'NONE',  ( 100.1216203692562630, -42.54163687813885275, 71.29146744712500094 ) ) ;
#60308 = CARTESIAN_POINT ( 'NONE',  ( 99.87975691711011450, -43.74731000462409725, 87.94166648727369306 ) ) ;
#60309 = CARTESIAN_POINT ( 'NONE',  ( 108.7714652236932835, -45.96901220096565055, 124.1653928297069882 ) ) ;
#60310 = CARTESIAN_POINT ( 'NONE',  ( 156.5667039024485518, -48.82844715993568485, 175.7178068554150059 ) ) ;
#60311 = CARTESIAN_POINT ( 'NONE',  ( 67.05726156256010029, -68.28389950123548147, 246.9923701901030029 ) ) ;
#60312 = CIRCLE ( 'NONE', #15420, 11.45913725231036118 ) ;
#60313 = CARTESIAN_POINT ( 'NONE',  ( 117.4691034930615103, -37.69004686371126667, 74.75276813305397638 ) ) ;
#60314 = DIRECTION ( 'NONE',  ( 0.0001713722456120069274, -0.9999999853157766072, 0.000000000000000000 ) ) ;
#60315 = VERTEX_POINT ( 'NONE', #8906 ) ;
#60316 = PLANE ( 'NONE',  #57522 ) ;
#60317 = ORIENTED_EDGE ( 'NONE', *, *, #74207, .F. ) ;
#60318 = CARTESIAN_POINT ( 'NONE',  ( -118.3861417219090129, 71.54629894495526798, 6.354613972969239910 ) ) ;
#60319 = ORIENTED_EDGE ( 'NONE', *, *, #33229, .F. ) ;
#60320 = CIRCLE ( 'NONE', #53033, 2.999999999999929834 ) ;
#60322 = EDGE_CURVE ( 'NONE', #43121, #7616, #16598, .T. ) ;
#60321 = ORIENTED_EDGE ( 'NONE', *, *, #866, .T. ) ;
#60323 = EDGE_CURVE ( 'NONE', #47465, #43325, #36606, .T. ) ;
#60324 = ADVANCED_FACE ( 'NONE', ( #2077 ), #9334, .F. ) ;
#60325 = DIRECTION ( 'NONE',  ( 4.299999999999999979E-14, -1.000000000000000000, 4.400000000000000367E-29 ) ) ;
#60326 = ORIENTED_EDGE ( 'NONE', *, *, #14150, .F. ) ;
#60327 = CARTESIAN_POINT ( 'NONE',  ( 110.5064767540468296, -26.94654216138279068, 254.8194347997213640 ) ) ;
#60328 = CARTESIAN_POINT ( 'NONE',  ( 142.8821648370248170, -72.54478064608022692, 542.9756252759101471 ) ) ;
#60329 = CARTESIAN_POINT ( 'NONE',  ( 116.7951252646970772, -39.38782981747054635, 189.6147919403582591 ) ) ;
#60330 = CARTESIAN_POINT ( 'NONE',  ( 101.0662023700742935, -27.44663458233410935, 66.54514908543495721 ) ) ;
#60331 = CARTESIAN_POINT ( 'NONE',  ( 0.000000000000000000, 101.5999999999999943, 0.000000000000000000 ) ) ;
#60332 = EDGE_LOOP ( 'NONE', ( #56069, #35716 ) ) ;
#60333 = CARTESIAN_POINT ( 'NONE',  ( 102.0667429138110691, -27.97066660765753099, 115.4919662677435213 ) ) ;
#60334 = ADVANCED_FACE ( 'NONE', ( #42936 ), #77480, .F. ) ;
#60335 = DIRECTION ( 'NONE',  ( 0.000000000000000000, 0.000000000000000000, -1.000000000000000000 ) ) ;
#60336 = VERTEX_POINT ( 'NONE', #2528 ) ;
#60337 = ADVANCED_FACE ( 'NONE', ( #57474 ), #70671, .T. ) ;
#60338 = FACE_OUTER_BOUND ( 'NONE', #54822, .T. ) ;
#60339 = DIRECTION ( 'NONE',  ( 1.000000000000000000, 0.000000000000000000, 0.000000000000000000 ) ) ;
#60340 = CARTESIAN_POINT ( 'NONE',  ( 105.8960369669305805, -47.10223136823075407, 282.4870538473394390 ) ) ;
#60341 = LINE ( 'NONE', #74439, #68991 ) ;
#60342 = DIRECTION ( 'NONE',  ( 1.000000000000000000, 4.163336342344333240E-14, 0.000000000000000000 ) ) ;
#60343 = CARTESIAN_POINT ( 'NONE',  ( 78.35735255112980724, -38.88611802718641286, 2.101554303227473941 ) ) ;
#60344 = EDGE_CURVE ( 'NONE', #45788, #69613, #41896, .T. ) ;
#60345 = CARTESIAN_POINT ( 'NONE',  ( 100.7700969181924506, -30.95782257301981488, 275.1581341137911068 ) ) ;
#60347 = CARTESIAN_POINT ( 'NONE',  ( 116.6546583390152279, -32.60254457569000408, 75.14991099019697174 ) ) ;
#60346 = DIRECTION ( 'NONE',  ( 0.000000000000000000, 0.000000000000000000, 1.000000000000000000 ) ) ;
#60348 = CARTESIAN_POINT ( 'NONE',  ( 118.0314967278394533, 74.00740537028835320, 55.80249333958784774 ) ) ;
#60349 = CARTESIAN_POINT ( 'NONE',  ( 113.5926674049485854, -44.96113684323219672, 168.1099109901969939 ) ) ;
#60350 = ORIENTED_EDGE ( 'NONE', *, *, #45551, .F. ) ;
#60351 = CARTESIAN_POINT ( 'NONE',  ( 84.06648329127399677, -18.82844715994099971, 199.5838068554169524 ) ) ;
#60352 = ORIENTED_EDGE ( 'NONE', *, *, #12507, .T. ) ;
#60353 = DIRECTION ( 'NONE',  ( 1.000000000000000078E-15, -1.000000000000000083E-30, -1.000000000000000000 ) ) ;
#60354 = DIRECTION ( 'NONE',  ( 0.000000000000000000, 0.000000000000000000, -1.000000000000000000 ) ) ;
#60355 = CARTESIAN_POINT ( 'NONE',  ( 21.03715912545829170, -47.82818131006186491, 249.9678068554150059 ) ) ;
#60356 = VERTEX_POINT ( 'NONE', #83861 ) ;
#60357 = EDGE_CURVE ( 'NONE', #26148, #58495, #28535, .T. ) ;
#60358 = CARTESIAN_POINT ( 'NONE',  ( -479.3614999999999782, 18.41194598552324990, 83.34375000000000000 ) ) ;
#60360 = ORIENTED_EDGE ( 'NONE', *, *, #49494, .T. ) ;
#60359 = CARTESIAN_POINT ( 'NONE',  ( 95.62691733261443972, -33.44842233792613229, 141.1041967044829732 ) ) ;
#60361 = DIRECTION ( 'NONE',  ( -0.9254794337955620787, -0.3787978585227822492, 0.000000000000000000 ) ) ;
#60362 = VECTOR ( 'NONE', #75311, 1000.000000000000000 ) ;
#60363 = CARTESIAN_POINT ( 'NONE',  ( -130.4355093393840548, 93.94653598907719072, 5.619751006019208184 ) ) ;
#60364 = CARTESIAN_POINT ( 'NONE',  ( 98.30753418512887265, -41.72887548160911564, 117.7397919417121983 ) ) ;
#60366 = VECTOR ( 'NONE', #7029, 999.9999999999998863 ) ;
#60365 = CARTESIAN_POINT ( 'NONE',  ( 183.5150000000000148, 36.86249999999999716, -35.28456447661465489 ) ) ;
#60367 = ORIENTED_EDGE ( 'NONE', *, *, #15866, .F. ) ;
#60368 = CARTESIAN_POINT ( 'NONE',  ( 101.4890226443523744, -27.89551843606815495, 110.5241967044819944 ) ) ;
#60369 = VECTOR ( 'NONE', #69096, 1000.000000000000000 ) ;
#60370 = AXIS2_PLACEMENT_3D ( 'NONE', #18412, #39310, #44780 ) ;
#60371 = APPLICATION_PROTOCOL_DEFINITION ( 'draft international standard', 'automotive_design', 1998, #26055 ) ;
#60372 = VECTOR ( 'NONE', #33612, 1000.000000000000000 ) ;
#60373 = DIRECTION ( 'NONE',  ( 0.7071067811865192621, 0.7071067811865758834, 7.071067811865186413E-16 ) ) ;
#60374 = DIRECTION ( 'NONE',  ( 0.000000000000000000, 0.000000000000000000, 1.000000000000000000 ) ) ;
#60375 = ORIENTED_EDGE ( 'NONE', *, *, #30625, .F. ) ;
#60376 = ORIENTED_EDGE ( 'NONE', *, *, #51125, .T. ) ;
#60377 = CARTESIAN_POINT ( 'NONE',  ( 162.9033555647784226, -33.89581943343761594, 237.4678068554150059 ) ) ;
#60378 = PRODUCT ( 'Drilling Spindle Head', 'Drilling Spindle Head', '', ( #87210 ) ) ;
#60379 = PLANE ( 'NONE',  #17077 ) ;
#60380 = CARTESIAN_POINT ( 'NONE',  ( 108.0667039024470455, -121.2010968907525239, -21.78219314458149114 ) ) ;
#60381 = CARTESIAN_POINT ( 'NONE',  ( 188.5667039024479834, -58.35344715994099829, 254.4678068554150343 ) ) ;
#60384 = EDGE_CURVE ( 'NONE', #32906, #16372, #56576, .T. ) ;
#60383 = CARTESIAN_POINT ( 'NONE',  ( 123.6837132603318707, -20.11243780205705534, 218.8274735512161158 ) ) ;
#60382 = CARTESIAN_POINT ( 'NONE',  ( 68.06670390244705970, -124.7784471599409954, 55.21780685541800437 ) ) ;
#60385 = CARTESIAN_POINT ( 'NONE',  ( 115.0888856295657803, -30.61760799569063707, 179.3439612979183266 ) ) ;
#60386 = CONICAL_SURFACE ( 'NONE', #27138, 1.258749999999999369, 1.029744258676650093 ) ;
#60387 = VERTEX_POINT ( 'NONE', #25631 ) ;
#60388 = VECTOR ( 'NONE', #31567, 1000.000000000000000 ) ;
#60389 = CARTESIAN_POINT ( 'NONE',  ( 41.56648329127399677, -9.303447159940999356, 136.8086252759119645 ) ) ;
#60390 = CARTESIAN_POINT ( 'NONE',  ( 116.5994914424365021, -40.81117973626238893, 209.5165776568629497 ) ) ;
#60392 = ORIENTED_EDGE ( 'NONE', *, *, #67864, .F. ) ;
#60391 = CARTESIAN_POINT ( 'NONE',  ( 188.5667039024479834, -65.37844715994100397, 252.3428068554150059 ) ) ;
#60393 = CARTESIAN_POINT ( 'NONE',  ( 104.1495640007033501, -46.68084741754449851, 58.33753003781600199 ) ) ;
#60394 = DIRECTION ( 'NONE',  ( 1.639958061481212836E-42, -4.100000000000000342E-29, -1.000000000000000000 ) ) ;
#60395 = CARTESIAN_POINT ( 'NONE',  ( -185.9961463128564958, 20.32000000000000028, -9.525000000000000355 ) ) ;
#60396 = LINE ( 'NONE', #39960, #72125 ) ;
#60397 = ORIENTED_EDGE ( 'NONE', *, *, #79660, .T. ) ;
#60398 = ADVANCED_FACE ( 'NONE', ( #59250 ), #51536, .T. ) ;
#60399 = FACE_OUTER_BOUND ( 'NONE', #21251, .T. ) ;
#60400 = ORIENTED_EDGE ( 'NONE', *, *, #81571, .F. ) ;
#60401 = VERTEX_POINT ( 'NONE', #46504 ) ;
#60402 = CARTESIAN_POINT ( 'NONE',  ( 105.4042388664825722, -28.02512512522124410, 231.6587261630399439 ) ) ;
#60403 = EDGE_CURVE ( 'NONE', #23386, #45281, #10223, .T. ) ;
#60404 = LINE ( 'NONE', #5009, #34247 ) ;
#60405 = CARTESIAN_POINT ( 'NONE',  ( -117.8759966127889527, 83.38015080693119785, -12.67975824297045051 ) ) ;
#60406 = CARTESIAN_POINT ( 'NONE',  ( 108.0667039024470171, -87.35579742913141388, -11.78219314458253741 ) ) ;
#60407 = CARTESIAN_POINT ( 'NONE',  ( 82.72805595269750256, -37.42731094489875687, 2.974216770161541845 ) ) ;
#60408 = ORIENTED_EDGE ( 'NONE', *, *, #67518, .F. ) ;
#60409 = DIRECTION ( 'NONE',  ( 0.000000000000000000, 0.000000000000000000, 1.000000000000000000 ) ) ;
#60410 = CARTESIAN_POINT ( 'NONE',  ( 113.2375207001889947, -28.75257540792464539, 35.55234988136929530 ) ) ;
#60411 = EDGE_LOOP ( 'NONE', ( #86036, #67558, #9079, #11121 ) ) ;
#60412 = CARTESIAN_POINT ( 'NONE',  ( 106.2521265061568130, -26.30051002661620885, 25.13848241876792855 ) ) ;
#60413 = ORIENTED_EDGE ( 'NONE', *, *, #62090, .F. ) ;
#60414 = ORIENTED_EDGE ( 'NONE', *, *, #60273, .T. ) ;
#60415 = CARTESIAN_POINT ( 'NONE',  ( 100.7056284991137289, -31.61385801203766377, 238.6052332267339580 ) ) ;
#60416 = CARTESIAN_POINT ( 'NONE',  ( 95.60734603896362671, -36.72944715994100306, 293.2242906452868851 ) ) ;
#60417 = CARTESIAN_POINT ( 'NONE',  ( 114.0056865186722490, -29.02320718445394476, 159.5051490854349652 ) ) ;
#60418 = CARTESIAN_POINT ( 'NONE',  ( 23.75871628398702740, 82.23812670290168114, 307.6575000000000841 ) ) ;
#60419 = DIRECTION ( 'NONE',  ( 0.000000000000000000, 0.000000000000000000, 1.000000000000000000 ) ) ;
#60420 = CARTESIAN_POINT ( 'NONE',  ( 162.7866693523289996, -36.02818131005891189, -5.074374724088000832 ) ) ;
#60421 = CARTESIAN_POINT ( 'NONE',  ( 101.1761829863686160, -45.38377220964024161, 193.1013395616249682 ) ) ;
#60422 = CARTESIAN_POINT ( 'NONE',  ( 91.61507027739585851, 87.79588542099533299, -75.24778849303586981 ) ) ;
#60423 = ORIENTED_EDGE ( 'NONE', *, *, #83670, .T. ) ;
#60424 = VECTOR ( 'NONE', #17045, 1000.000000000000000 ) ;
#60425 = CARTESIAN_POINT ( 'NONE',  ( 100.9176109441957436, -28.25688269532019348, 71.57562527591099411 ) ) ;
#60426 = VECTOR ( 'NONE', #26362, 1000.000000000000000 ) ;
#60427 = CARTESIAN_POINT ( 'NONE',  ( 107.0664832912739399, -36.72944715994095333, 305.7141315223800007 ) ) ;
#60428 = AXIS2_PLACEMENT_3D ( 'NONE', #65347, #16757, #57176 ) ;
#60429 = EDGE_LOOP ( 'NONE', ( #70303, #10546, #55303, #80352 ) ) ;
#60431 = EDGE_CURVE ( 'NONE', #58396, #85229, #12016, .T. ) ;
#60430 = ORIENTED_EDGE ( 'NONE', *, *, #24152, .T. ) ;
#60433 = ORIENTED_EDGE ( 'NONE', *, *, #75535, .T. ) ;
#60432 = ADVANCED_FACE ( 'NONE', ( #23865, #87421 ), #18365, .T. ) ;
#60434 = EDGE_CURVE ( 'NONE', #84376, #13709, #11571, .T. ) ;
#60435 = LINE ( 'NONE', #18667, #65118 ) ;
#60436 = CARTESIAN_POINT ( 'NONE',  ( 33.92127028473601769, -29.73316016639540749, -5.074374724088000832 ) ) ;
#60437 = DIRECTION ( 'NONE',  ( 1.000000000000000000, 3.999999999999999995E-14, 1.000000000000000078E-15 ) ) ;
#60438 = CARTESIAN_POINT ( 'NONE',  ( 113.0638415271824897, -42.26672268200739069, 121.0509475124479906 ) ) ;
#60439 = CARTESIAN_POINT ( 'NONE',  ( 115.5350430195811668, -29.59021037493291573, 220.3718157521019521 ) ) ;
#60440 = CARTESIAN_POINT ( 'NONE',  ( 188.5667039024479834, -58.35344715994099829, 173.2178068554149775 ) ) ;
#60441 = ORIENTED_EDGE ( 'NONE', *, *, #14985, .F. ) ;
#60442 = EDGE_CURVE ( 'NONE', #47492, #84886, #32431, .T. ) ;
#60443 = VECTOR ( 'NONE', #76333, 1000.000000000000000 ) ;
#60444 = CARTESIAN_POINT ( 'NONE',  ( 141.8164832912740394, -45.62589376934770513, -5.074374724088994704 ) ) ;
#60445 = ORIENTED_EDGE ( 'NONE', *, *, #63881, .F. ) ;
#60446 = ORIENTED_EDGE ( 'NONE', *, *, #27423, .T. ) ;
#60448 = CLOSED_SHELL ( 'NONE', ( #4143, #54990, #67222, #66172 ) ) ;
#60447 = EDGE_CURVE ( 'NONE', #23436, #59530, #17486, .T. ) ;
#60449 = CARTESIAN_POINT ( 'NONE',  ( 70.06670417066790435, -71.37844715994097555, 55.21780685541800437 ) ) ;
#60450 = ORIENTED_EDGE ( 'NONE', *, *, #18090, .T. ) ;
#60451 = ORIENTED_EDGE ( 'NONE', *, *, #14781, .T. ) ;
#60452 = CARTESIAN_POINT ( 'NONE',  ( 104.4091854452810253, -46.45840093360554590, 168.3656309447823674 ) ) ;
#60453 = LINE ( 'NONE', #10969, #76182 ) ;
#60454 = CARTESIAN_POINT ( 'NONE',  ( 117.9332873271178102, -93.05227202534700837, -11.78219314458237044 ) ) ;
#60455 = EDGE_CURVE ( 'NONE', #56594, #31182, #24742, .T. ) ;
#60456 = CARTESIAN_POINT ( 'NONE',  ( 99.13191293290623207, -41.09468066504173578, 176.1371817328389966 ) ) ;
#60457 = CARTESIAN_POINT ( 'NONE',  ( 100.5702229155400858, -28.47427015469623868, 15.60705384733995871 ) ) ;
#60458 = CARTESIAN_POINT ( 'NONE',  ( 116.3265940946004378, -32.93621273019581253, 125.1356252759109680 ) ) ;
#60459 = ORIENTED_EDGE ( 'NONE', *, *, #991, .T. ) ;
#60460 = CARTESIAN_POINT ( 'NONE',  ( -92.06079644778172621, 79.26437155269049128, -74.70173812346064324 ) ) ;
#60461 = ORIENTED_EDGE ( 'NONE', *, *, #68160, .T. ) ;
#60462 = DIRECTION ( 'NONE',  ( 0.000000000000000000, 0.000000000000000000, -1.000000000000000000 ) ) ;
#60463 = ORIENTED_EDGE ( 'NONE', *, *, #73918, .F. ) ;
#60464 = CARTESIAN_POINT ( 'NONE',  ( 97.77633413480816671, -40.43004283583653091, 167.6283907404767888 ) ) ;
#60465 = CARTESIAN_POINT ( 'NONE',  ( -5.580972532898796246, 71.24585594549820655, 118.4251286083983246 ) ) ;
#60466 = CARTESIAN_POINT ( 'NONE',  ( 110.8543515439697558, -45.98428674439771413, 132.8856148800098538 ) ) ;
#60467 = CIRCLE ( 'NONE', #61898, 8.999999999999994671 ) ;
#60468 = FACE_OUTER_BOUND ( 'NONE', #10098, .T. ) ;
#60469 = ORIENTED_EDGE ( 'NONE', *, *, #63709, .T. ) ;
#60470 = CARTESIAN_POINT ( 'NONE',  ( 110.5626142325126153, -46.61202937628593190, 37.84705384733994293 ) ) ;
#60471 = CARTESIAN_POINT ( 'NONE',  ( 96.67154112854022685, -38.24047072676557946, 62.44133956162495025 ) ) ;
#60473 = CARTESIAN_POINT ( 'NONE',  ( -492.0614999999999668, 93.66249999999999432, 11.11250000000040217 ) ) ;
#60472 = DIRECTION ( 'NONE',  ( 0.000000000000000000, 1.000000000000000000, 0.000000000000000000 ) ) ;
#60474 = CARTESIAN_POINT ( 'NONE',  ( -3.968749999999949818, 120.6499999999999915, -105.4788588808462038 ) ) ;
#60475 = CARTESIAN_POINT ( 'NONE',  ( 172.5664832912740110, -32.07844715994070839, 318.9256252759120116 ) ) ;
#60476 = CARTESIAN_POINT ( 'NONE',  ( 97.21111501186732085, -38.70825661063340561, 122.4834732151292087 ) ) ;
#60477 = FACE_OUTER_BOUND ( 'NONE', #55154, .T. ) ;
#60478 = ORIENTED_EDGE ( 'NONE', *, *, #17403, .T. ) ;
#60479 = CARTESIAN_POINT ( 'NONE',  ( 110.4709766755849643, -47.29459308529762041, 57.83657765686300678 ) ) ;
#60480 = CARTESIAN_POINT ( 'NONE',  ( 98.53766203808953605, -30.73430783891158669, 201.8384824187679385 ) ) ;
#60481 = CARTESIAN_POINT ( 'NONE',  ( 117.8789659794968543, -39.13265831612300616, 99.64038718067195077 ) ) ;
#60482 = AXIS2_PLACEMENT_3D ( 'NONE', #54769, #6654, #21646 ) ;
#60483 = VECTOR ( 'NONE', #56257, 1000.000000000000000 ) ;
#60486 = ADVANCED_FACE ( 'NONE', ( #24306 ), #45166, .T. ) ;
#60485 = CARTESIAN_POINT ( 'NONE',  ( 188.5667039024484097, -48.82844715993431350, 257.2178068554150059 ) ) ;
#60484 = CARTESIAN_POINT ( 'NONE',  ( 108.3347997046528093, -46.73470615375604353, 172.6734346717588835 ) ) ;
#60487 = FACE_OUTER_BOUND ( 'NONE', #60987, .T. ) ;
#60488 = VECTOR ( 'NONE', #73676, 1000.000000000000000 ) ;
#60489 = CIRCLE ( 'NONE', #53272, 0.5000000000000104361 ) ;
#60490 = CIRCLE ( 'NONE', #21357, 3.250000000000002665 ) ;
#60491 = CARTESIAN_POINT ( 'NONE',  ( 99.09570913176251850, -30.55043168255618014, 186.8022919354755800 ) ) ;
#60492 = EDGE_LOOP ( 'NONE', ( #7453, #65506, #81993, #79135 ) ) ;
#60493 = CARTESIAN_POINT ( 'NONE',  ( 116.7343647603065619, -32.97833357388816466, 90.10895860924395606 ) ) ;
#60495 = ORIENTED_EDGE ( 'NONE', *, *, #22276, .F. ) ;
#60494 = CARTESIAN_POINT ( 'NONE',  ( 11.66424111575752320, 87.57388405225547956, 130.0339036534010120 ) ) ;
#60496 = CARTESIAN_POINT ( 'NONE',  ( 104.4161250475293485, -26.02246701806305751, 236.2575300378159682 ) ) ;
#60497 = DIRECTION ( 'NONE',  ( 0.000000000000000000, 0.000000000000000000, 1.000000000000000000 ) ) ;
#60498 = PRODUCT ( 'Proximity Switch Housing', 'Proximity Switch Housing', '', ( #67193 ) ) ;
#60499 = CARTESIAN_POINT ( 'NONE',  ( 62.03715912545834499, -47.82818131006021645, 300.4678068554150627 ) ) ;
#60500 = CYLINDRICAL_SURFACE ( 'NONE', #45694, 2.750000000000002665 ) ;
#60501 = PLANE ( 'NONE',  #67378 ) ;
#60502 = CARTESIAN_POINT ( 'NONE',  ( 81.84766347661003749, -124.7784471599409670, 55.21780685541800437 ) ) ;
#60503 = CARTESIAN_POINT ( 'NONE',  ( 183.5150000000000148, 68.61249999999999716, -53.61543552338530105 ) ) ;
#60504 = VECTOR ( 'NONE', #60629, 1000.000000000000000 ) ;
#60506 = CARTESIAN_POINT ( 'NONE',  ( 96.59955023297820276, -32.98040794253977737, 176.0527681330549683 ) ) ;
#60505 = AXIS2_PLACEMENT_3D ( 'NONE', #64837, #87513, #72549 ) ;
#60507 = ORIENTED_EDGE ( 'NONE', *, *, #34202, .T. ) ;
#60508 = VERTEX_POINT ( 'NONE', #38362 ) ;
#60509 = CARTESIAN_POINT ( 'NONE',  ( 112.8270896756726671, -29.95615083465972006, 135.9472975916109476 ) ) ;
#60510 = AXIS2_PLACEMENT_3D ( 'NONE', #86807, #87255, #24574 ) ;
#60511 = ADVANCED_FACE ( 'NONE', ( #65628 ), #60132, .F. ) ;
#60512 = LINE ( 'NONE', #19638, #68945 ) ;
#60514 = CYLINDRICAL_SURFACE ( 'NONE', #21638, 7.937500000000000000 ) ;
#60513 = CARTESIAN_POINT ( 'NONE',  ( 97.60228370342871074, -39.19771807616534431, 272.5299109901961856 ) ) ;
#60515 = CARTESIAN_POINT ( 'NONE',  ( 70.63919639214310564, 91.07499999999996021, -53.97512327982435210 ) ) ;
#60516 = CARTESIAN_POINT ( 'NONE',  ( -98.60478223830740774, 127.0000000000000000, -1.074461880482445986E-12 ) ) ;
#60517 = CARTESIAN_POINT ( 'NONE',  ( 106.5667039024470313, -108.2470741265382799, 2.217806855418114065 ) ) ;
#60518 = DIRECTION ( 'NONE',  ( 0.000000000000000000, 0.000000000000000000, 1.000000000000000000 ) ) ;
#60519 = DIRECTION ( 'NONE',  ( 5.512527431108029424E-15, -1.000000000000000000, 0.000000000000000000 ) ) ;
#60520 = CARTESIAN_POINT ( 'NONE',  ( 98.39792771585416631, -29.90889243069706538, 200.8080062282919869 ) ) ;
#60521 = ORIENTED_EDGE ( 'NONE', *, *, #45371, .F. ) ;
#60522 = EDGE_LOOP ( 'NONE', ( #81369, #44118, #16852, #86347 ) ) ;
#60523 = PRODUCT_RELATED_PRODUCT_CATEGORY ( 'part', '', ( #19058 ) ) ;
#60524 = DIRECTION ( 'NONE',  ( 1.639958061481212836E-42, -4.100000000000000342E-29, -1.000000000000000000 ) ) ;
#60525 = CARTESIAN_POINT ( 'NONE',  ( 194.5664832912739826, -18.82844715994099971, -5.074374724088000832 ) ) ;
#60526 = CARTESIAN_POINT ( 'NONE',  ( 131.3179999999999836, 37.33800000000000097, 50.79999999999999716 ) ) ;
#60527 = CARTESIAN_POINT ( 'NONE',  ( -55.48342271751670296, 20.32000000000000028, 171.1197181046785261 ) ) ;
#60528 = VECTOR ( 'NONE', #2143, 1000.000000000000000 ) ;
#60529 = AXIS2_PLACEMENT_3D ( 'NONE', #31110, #31557, #45607 ) ;
#60530 = DIRECTION ( 'NONE',  ( 0.000000000000000000, 0.000000000000000000, -1.000000000000000000 ) ) ;
#60531 = ORIENTED_EDGE ( 'NONE', *, *, #46475, .T. ) ;
#60532 = CARTESIAN_POINT ( 'NONE',  ( 49.35031423293676056, -29.99615139352232873, 117.4678068554150485 ) ) ;
#60533 = CARTESIAN_POINT ( 'NONE',  ( 96.12498142956854963, -35.16017202033504674, 226.2251490854349640 ) ) ;
#60534 = DIRECTION ( 'NONE',  ( 3.999999999999999995E-14, -1.000000000000000000, 4.100000000000000342E-29 ) ) ;
#60536 = VERTEX_POINT ( 'NONE', #74239 ) ;
#60535 = EDGE_CURVE ( 'NONE', #1304, #80721, #52407, .T. ) ;
#60537 = EDGE_CURVE ( 'NONE', #79701, #10974, #11103, .T. ) ;
#60538 = CARTESIAN_POINT ( 'NONE',  ( -10.91960930477692671, 88.85017151735789298, 118.0522144908983933 ) ) ;
#60539 = CARTESIAN_POINT ( 'NONE',  ( 70.56670390244700286, -67.87844715994098976, 55.21780685541800437 ) ) ;
#60540 = EDGE_CURVE ( 'NONE', #14173, #31404, #45950, .T. ) ;
#60541 = CARTESIAN_POINT ( 'NONE',  ( 97.81944346430564963, -40.53631996860134734, 166.6372505363765413 ) ) ;
#60542 = CARTESIAN_POINT ( 'NONE',  ( 106.7065939435451440, -28.08240114970028856, 37.91570941720995336 ) ) ;
#60543 = CARTESIAN_POINT ( 'NONE',  ( 116.8158478801051530, -32.97616202413719577, 135.1184824187679396 ) ) ;
#60544 = DIRECTION ( 'NONE',  ( 1.000000000000000000, -5.689893001203922423E-12, 0.000000000000000000 ) ) ;
#60545 = ORIENTED_EDGE ( 'NONE', *, *, #39126, .F. ) ;
#60546 = EDGE_CURVE ( 'NONE', #40888, #10162, #72064, .T. ) ;
#60547 = CIRCLE ( 'NONE', #21418, 3.000000000000002665 ) ;
#60548 = DIRECTION ( 'NONE',  ( 1.000000000000000078E-15, -1.000000000000000083E-30, -1.000000000000000000 ) ) ;
#60549 = CARTESIAN_POINT ( 'NONE',  ( 82.73027604518254918, -18.02416100035393853, 6.874390491353741695 ) ) ;
#60550 = ORIENTED_EDGE ( 'NONE', *, *, #25827, .T. ) ;
#60551 = ORIENTED_EDGE ( 'NONE', *, *, #70981, .T. ) ;
#60552 = AXIS2_PLACEMENT_3D ( 'NONE', #72335, #51853, #50978 ) ;
#60553 = CARTESIAN_POINT ( 'NONE',  ( 6.938893903907229955E-15, 67.86880000000000734, 210.4643999999999835 ) ) ;
#60554 = ORIENTED_EDGE ( 'NONE', *, *, #89388, .F. ) ;
#60555 = ORIENTED_EDGE ( 'NONE', *, *, #37709, .T. ) ;
#60556 = DIRECTION ( 'NONE',  ( 2.544367396927093358E-16, -0.000000000000000000, 1.000000000000000000 ) ) ;
#60557 = ADVANCED_FACE ( 'NONE', ( #46050 ), #80616, .F. ) ;
#60558 = CARTESIAN_POINT ( 'NONE',  ( 98.27686124684872482, -40.85414981714398408, 61.09813411379100501 ) ) ;
#60559 = CARTESIAN_POINT ( 'NONE',  ( 113.6996774752161201, -45.60053368046675359, 188.0994347997199725 ) ) ;
#60560 = CIRCLE ( 'NONE', #22931, 4.874999999999990230 ) ;
#60561 = CARTESIAN_POINT ( 'NONE',  ( 104.5678333644583944, -48.28820816006152938, 182.4070538473399665 ) ) ;
#60562 = ADVANCED_FACE ( 'NONE', ( #58366 ), #31101, .F. ) ;
#60564 = CARTESIAN_POINT ( 'NONE',  ( 111.4803918977840169, -26.59589994751270936, 280.7375300378156453 ) ) ;
#60563 = CARTESIAN_POINT ( 'NONE',  ( 98.60180739276366069, -42.06509604122263113, 21.77386757017102425 ) ) ;
#60565 = LINE ( 'NONE', #12893, #11758 ) ;
#60566 = LINE ( 'NONE', #11545, #10506 ) ;
#60567 = EDGE_LOOP ( 'NONE', ( #9935, #6761, #28154, #42700 ) ) ;
#60568 = AXIS2_PLACEMENT_3D ( 'NONE', #82170, #27180, #63038 ) ;
#60569 = ORIENTED_EDGE ( 'NONE', *, *, #86926, .F. ) ;
#60570 = AXIS2_PLACEMENT_3D ( 'NONE', #52675, #17312, #86358 ) ;
#60571 = AXIS2_PLACEMENT_3D ( 'NONE', #34430, #89873, #27623 ) ;
#60572 = CIRCLE ( 'NONE', #59152, 2.750000000000002665 ) ;
#60573 = CARTESIAN_POINT ( 'NONE',  ( 128.8897065959775148, -58.55267046464430791, 14.67562527591099375 ) ) ;
#60574 = CARTESIAN_POINT ( 'NONE',  ( 109.3464976042218524, -26.51141404309336735, 224.9013395616249511 ) ) ;
#60575 = ORIENTED_EDGE ( 'NONE', *, *, #30399, .T. ) ;
#60576 = CARTESIAN_POINT ( 'NONE',  ( 117.7765707488592710, -31.65652763686493998, 214.1784824187679419 ) ) ;
#60577 = CARTESIAN_POINT ( 'NONE',  ( 97.07207204382144994, -35.37844130610024251, 36.21895861776621928 ) ) ;
#60578 = DIRECTION ( 'NONE',  ( 0.000000000000000000, 0.000000000000000000, 1.000000000000000000 ) ) ;
#60579 = DIRECTION ( 'NONE',  ( 6.982966722218760189E-15, 0.000000000000000000, -1.000000000000000000 ) ) ;
#60580 = CARTESIAN_POINT ( 'NONE',  ( -47.18030668273772221, 100.5999999999999659, 75.34738655934135920 ) ) ;
#60582 = CARTESIAN_POINT ( 'NONE',  ( 95.60734603896358408, -36.72944715994100306, 296.0306255462182321 ) ) ;
#60581 = CARTESIAN_POINT ( 'NONE',  ( 105.2412389168119233, -28.82906800083503995, 277.6356252759112522 ) ) ;
#60583 = CYLINDRICAL_SURFACE ( 'NONE', #53930, 0.4999999999999976685 ) ;
#60584 = CARTESIAN_POINT ( 'NONE',  ( 194.5667039024479834, -48.82844715994099971, 10.91780685541479734 ) ) ;
#60585 = CARTESIAN_POINT ( 'NONE',  ( 67.56670413341505821, -124.7784471599409954, 45.21780685541799727 ) ) ;
#60586 = DIRECTION ( 'NONE',  ( -1.000000000000000000, -4.299999999999999979E-14, -1.000000000000000078E-15 ) ) ;
#60587 = DIRECTION ( 'NONE',  ( 0.000000000000000000, 1.000000000000000000, 0.000000000000000000 ) ) ;
#60588 = CARTESIAN_POINT ( 'NONE',  ( 102.0670549698788250, -27.97049805383846888, 76.48979194169342577 ) ) ;
#60590 = ORIENTED_EDGE ( 'NONE', *, *, #78941, .F. ) ;
#60589 = LINE ( 'NONE', #88331, #38483 ) ;
#60591 = FACE_OUTER_BOUND ( 'NONE', #19362, .T. ) ;
#60592 = CARTESIAN_POINT ( 'NONE',  ( 115.4777400244682042, -29.52207584268309759, 229.4022919425779605 ) ) ;
#60593 = CARTESIAN_POINT ( 'NONE',  ( 96.63924282488838458, -37.56250720137591514, 97.38991099019594344 ) ) ;
#60594 = CARTESIAN_POINT ( 'NONE',  ( 96.87194279380025819, -34.19777600025749109, 272.1327681330539576 ) ) ;
#60595 = DIRECTION ( 'NONE',  ( -1.000000000000000000, -4.299999999999999979E-14, -9.351236661543306751E-17 ) ) ;
#60596 = DIRECTION ( 'NONE',  ( -1.000000000000000000, -6.493183223601999383E-14, -1.000000000000000078E-15 ) ) ;
#60597 = VECTOR ( 'NONE', #26474, 1000.000000000000000 ) ;
#60600 = EDGE_CURVE ( 'NONE', #36007, #1586, #50323, .T. ) ;
#60599 = CYLINDRICAL_SURFACE ( 'NONE', #63183, 3.250000000000002665 ) ;
#60598 = CARTESIAN_POINT ( 'NONE',  ( 103.1875000000000000, 127.0000000000000000, 3.602774393244745134E-13 ) ) ;
#60601 = DIRECTION ( 'NONE',  ( 0.000000000000000000, 0.000000000000000000, -1.000000000000000000 ) ) ;
#60602 = AXIS2_PLACEMENT_3D ( 'NONE', #49496, #36786, #84953 ) ;
#60603 = CARTESIAN_POINT ( 'NONE',  ( 133.6902059199370854, -21.46022584114957255, 1.641799370506089595 ) ) ;
#60604 = ADVANCED_FACE ( 'NONE', ( #6099 ), #40603, .F. ) ;
#60605 = ORIENTED_EDGE ( 'NONE', *, *, #31355, .T. ) ;
#60606 = ORIENTED_EDGE ( 'NONE', *, *, #40290, .F. ) ;
#60607 = CARTESIAN_POINT ( 'NONE',  ( 102.0031328989874027, -44.23578847709845263, 151.5143245899819817 ) ) ;
#60609 = EDGE_LOOP ( 'NONE', ( #6951, #30828, #63876, #30981 ) ) ;
#60608 = CARTESIAN_POINT ( 'NONE',  ( 22.09100578693153594, 47.99823937963132892, 31.04264637510191349 ) ) ;
#60610 = CARTESIAN_POINT ( 'NONE',  ( 114.6444261855608460, -91.15344715994180547, -11.78219314458242550 ) ) ;
#60611 = CARTESIAN_POINT ( 'NONE',  ( 96.62907006607247240, -36.88702529232762828, 132.3384824187679669 ) ) ;
#60612 = CARTESIAN_POINT ( 'NONE',  ( 103.1875000000000000, 127.0000000000000000, 3.602774393244745134E-13 ) ) ;
#60613 = CYLINDRICAL_SURFACE ( 'NONE', #50139, 4.874999999999990230 ) ;
#60614 = CARTESIAN_POINT ( 'NONE',  ( -76.39898589339149737, 74.81620433377383961, 90.65754775988004610 ) ) ;
#60615 = DIRECTION ( 'NONE',  ( 0.000000000000000000, 0.000000000000000000, -1.000000000000000000 ) ) ;
#60616 = AXIS2_PLACEMENT_3D ( 'NONE', #88970, #62146, #41686 ) ;
#60617 = CARTESIAN_POINT ( 'NONE',  ( 99.11394507416765975, -43.38496525699394368, 71.86895860924497015 ) ) ;
#60618 = EDGE_LOOP ( 'NONE', ( #2561, #86639 ) ) ;
#60619 = VERTEX_POINT ( 'NONE', #27867 ) ;
#60620 = ORIENTED_EDGE ( 'NONE', *, *, #60857, .F. ) ;
#60621 = AXIS2_PLACEMENT_3D ( 'NONE', #2875, #64644, #8808 ) ;
#60623 = EDGE_CURVE ( 'NONE', #84501, #82293, #88772, .T. ) ;
#60622 = VECTOR ( 'NONE', #23981, 1000.000000000000000 ) ;
#60624 = DIRECTION ( 'NONE',  ( 0.7071067811865516806, -0.7071067811865434649, 7.071067811865511818E-16 ) ) ;
#60626 = CYLINDRICAL_SURFACE ( 'NONE', #57792, 2.116999999999993776 ) ;
#60625 = CARTESIAN_POINT ( 'NONE',  ( 99.89458030379221043, -28.23347241844150091, 146.6356252759109395 ) ) ;
#60627 = DIRECTION ( 'NONE',  ( 0.000000000000000000, 0.000000000000000000, -1.000000000000000000 ) ) ;
#60628 = CARTESIAN_POINT ( 'NONE',  ( 0.000000000000000000, 2.269999999999994245, 0.000000000000000000 ) ) ;
#60629 = DIRECTION ( 'NONE',  ( 1.000000000000000078E-15, -1.000000000000000000, 0.000000000000000000 ) ) ;
#60630 = AXIS2_PLACEMENT_3D ( 'NONE', #12745, #68603, #25922 ) ;
#60631 = DIRECTION ( 'NONE',  ( 1.000000000000000000, 3.999999999999999995E-14, 1.000000000000000078E-15 ) ) ;
#60632 = CARTESIAN_POINT ( 'NONE',  ( 154.5667039024469886, -67.87844715994090450, 190.2178068554179902 ) ) ;
#60633 = CARTESIAN_POINT ( 'NONE',  ( 107.2318599658364207, -25.70055450771768690, 80.07657765686299456 ) ) ;
#60634 = ORIENTED_EDGE ( 'NONE', *, *, #84726, .T. ) ;
#60635 = ORIENTED_EDGE ( 'NONE', *, *, #5940, .F. ) ;
#60636 = EDGE_CURVE ( 'NONE', #32451, #62736, #89503, .T. ) ;
#60637 = LINE ( 'NONE', #61983, #31388 ) ;
#60638 = FACE_OUTER_BOUND ( 'NONE', #7775, .T. ) ;
#60639 = AXIS2_PLACEMENT_3D ( 'NONE', #63385, #16468, #1167 ) ;
#60640 = CARTESIAN_POINT ( 'NONE',  ( 107.0667039024470313, -104.2784471599418197, -11.78219314458200984 ) ) ;
#60641 = CARTESIAN_POINT ( 'NONE',  ( 108.0840670587429599, -45.32394831497818899, 160.5004713219719861 ) ) ;
#60642 = FACE_OUTER_BOUND ( 'NONE', #31282, .T. ) ;
#60643 = ORIENTED_EDGE ( 'NONE', *, *, #16595, .F. ) ;
#60644 = ORIENTED_EDGE ( 'NONE', *, *, #38100, .F. ) ;
#60645 = AXIS2_PLACEMENT_3D ( 'NONE', #74089, #66821, #72753 ) ;
#60646 = DIRECTION ( 'NONE',  ( 0.000000000000000000, 1.000000000000000000, 0.000000000000000000 ) ) ;
#60647 = ORIENTED_EDGE ( 'NONE', *, *, #17491, .F. ) ;
#60648 = VERTEX_POINT ( 'NONE', #26089 ) ;
#60649 = CARTESIAN_POINT ( 'NONE',  ( 77.46225723383568607, -19.61690131754105693, 6.952852217897422804 ) ) ;
#60650 = ADVANCED_FACE ( 'NONE', ( #83296 ), #69660, .F. ) ;
#60651 = CARTESIAN_POINT ( 'NONE',  ( 112.1289716242999361, -44.03925847519028025, 199.4901547344690016 ) ) ;
#60652 = CARTESIAN_POINT ( 'NONE',  ( 41.56670390244801894, -27.57844715994070484, 342.9256252759119548 ) ) ;
#60653 = VECTOR ( 'NONE', #74064, 1000.000000000000000 ) ;
#60654 = LINE ( 'NONE', #88392, #34219 ) ;
#60655 = AXIS2_PLACEMENT_3D ( 'NONE', #45197, #3881, #29815 ) ;
#60656 = CARTESIAN_POINT ( 'NONE',  ( -110.2860940435973873, 61.86465508475756536, 69.87023241873045265 ) ) ;
#60657 = ORIENTED_EDGE ( 'NONE', *, *, #25677, .T. ) ;
#60658 = ORIENTED_EDGE ( 'NONE', *, *, #45303, .T. ) ;
#60659 = DIRECTION ( 'NONE',  ( 0.000000000000000000, 1.000000000000000000, 0.000000000000000000 ) ) ;
#60660 = EDGE_LOOP ( 'NONE', ( #72083, #64528, #7580, #21140, #82027, #9217, #70282, #47286, #7434, #26701 ) ) ;
#60661 = EDGE_LOOP ( 'NONE', ( #66984, #45223, #85770, #32547 ) ) ;
#60662 = EDGE_CURVE ( 'NONE', #8963, #55318, #53757, .T. ) ;
#60663 = CARTESIAN_POINT ( 'NONE',  ( 102.1208986914200665, -43.83170863157916131, 234.8985665600679624 ) ) ;
#60664 = CARTESIAN_POINT ( 'NONE',  ( 116.9960073371140652, -33.48122977351050622, 89.07848241876791917 ) ) ;
#60665 = CARTESIAN_POINT ( 'NONE',  ( 118.8180844208009717, -35.40729807334668067, 83.91562527591095488 ) ) ;
#60666 = CARTESIAN_POINT ( 'NONE',  ( 106.6920129052768544, -28.07392614262452213, 249.5838068554171514 ) ) ;
#60667 = EDGE_CURVE ( 'NONE', #85439, #81096, #37239, .T. ) ;
#60668 = CARTESIAN_POINT ( 'NONE',  ( 133.8780722764265079, -15.97944715994100306, 8.225625275910996237 ) ) ;
#60669 = DIRECTION ( 'NONE',  ( 1.000000000000000078E-15, -1.000000000000000000, 0.000000000000000000 ) ) ;
#60670 = CARTESIAN_POINT ( 'NONE',  ( 117.1921950572609603, -41.16159581679399793, 204.4861014663869696 ) ) ;
#60671 = CARTESIAN_POINT ( 'NONE',  ( -72.96458098368600531, 127.0000000000000000, -72.96458098368781009 ) ) ;
#60672 = ORIENTED_EDGE ( 'NONE', *, *, #18118, .T. ) ;
#60673 = CARTESIAN_POINT ( 'NONE',  ( 130.0906838859329469, 76.18750001922978754, -11.02255322708036900 ) ) ;
#60674 = VERTEX_POINT ( 'NONE', #81522 ) ;
#60675 = CIRCLE ( 'NONE', #50571, 11.49999999999999645 ) ;
#60676 = ORIENTED_EDGE ( 'NONE', *, *, #30964, .T. ) ;
#60677 = CARTESIAN_POINT ( 'NONE',  ( 63.06670390244641311, -24.92844715994017335, 180.4678068554151196 ) ) ;
#60678 = VERTEX_POINT ( 'NONE', #41044 ) ;
#60679 = AXIS2_PLACEMENT_3D ( 'NONE', #66309, #53101, #4551 ) ;
#60680 = CARTESIAN_POINT ( 'NONE',  ( 97.80849178533165400, -40.50961443681259055, 137.6349539298032596 ) ) ;
#60681 = AXIS2_PLACEMENT_3D ( 'NONE', #87876, #32441, #53315 ) ;
#60682 = CARTESIAN_POINT ( 'NONE',  ( 53.56670390244872237, -48.82844715994099971, 300.4678068554149490 ) ) ;
#60683 = CARTESIAN_POINT ( 'NONE',  ( 103.8412645720801493, -46.68052101597508852, 82.32705384733995402 ) ) ;
#60684 = CARTESIAN_POINT ( 'NONE',  ( -11.72824152711724288, 77.67777890152783016, 130.0281412439851465 ) ) ;
#60685 = LINE ( 'NONE', #4405, #85588 ) ;
#60686 = CARTESIAN_POINT ( 'NONE',  ( 168.5667039024544636, -48.82844715994099971, 129.9678068554150059 ) ) ;
#60689 = CARTESIAN_POINT ( 'NONE',  ( 116.3579325164319016, -41.40893824611048757, 199.4556252759109611 ) ) ;
#60688 = DIRECTION ( 'NONE',  ( -0.7071067811865165975, -0.7071067811865784369, -7.071067811865470403E-16 ) ) ;
#60687 = DIRECTION ( 'NONE',  ( -1.000000000000000000, 0.000000000000000000, 0.000000000000000000 ) ) ;
#60690 = CARTESIAN_POINT ( 'NONE',  ( 116.3185006702053244, -32.93849971620830530, 275.1356252759109680 ) ) ;
#60691 = FACE_OUTER_BOUND ( 'NONE', #46232, .T. ) ;
#60692 = ORIENTED_EDGE ( 'NONE', *, *, #55856, .F. ) ;
#60693 = LINE ( 'NONE', #46160, #38186 ) ;
#60694 = VECTOR ( 'NONE', #67699, 1000.000000000000000 ) ;
#60695 = LINE ( 'NONE', #12570, #77623 ) ;
#60696 = DIRECTION ( 'NONE',  ( 0.000000000000000000, 0.000000000000000000, 1.000000000000000000 ) ) ;
#60697 = AXIS2_PLACEMENT_3D ( 'NONE', #86740, #66726, #24951 ) ;
#60698 = DIRECTION ( 'NONE',  ( -4.299999999999999979E-14, 1.000000000000000000, -4.128053709984630540E-29 ) ) ;
#60700 = ORIENTED_EDGE ( 'NONE', *, *, #65451, .F. ) ;
#60699 = CARTESIAN_POINT ( 'NONE',  ( 96.22219577434788107, -34.35999324012363587, 256.1432443235299843 ) ) ;
#60701 = DIRECTION ( 'NONE',  ( 1.000000000000000000, 0.000000000000000000, 0.000000000000000000 ) ) ;
#60702 = CARTESIAN_POINT ( 'NONE',  ( 98.42378885047078541, -42.06819960529416136, 7.768006228291934434 ) ) ;
#60703 = CARTESIAN_POINT ( 'NONE',  ( 102.3408129182306823, -46.07080783562200565, 123.2041967044829818 ) ) ;
#60704 = DIRECTION ( 'NONE',  ( 0.000000000000000000, -1.000000000000000000, 0.000000000000000000 ) ) ;
#60705 = VECTOR ( 'NONE', #8103, 999.9999999999998863 ) ;
#60706 = CARTESIAN_POINT ( 'NONE',  ( 7.746062721843873788, 92.64813751154242993, -130.3278237768880956 ) ) ;
#60708 = CARTESIAN_POINT ( 'NONE',  ( 184.5664832912729878, -71.37844715994266664, 342.9256252759109884 ) ) ;
#60707 = DIRECTION ( 'NONE',  ( 1.705911707540438309E-29, 0.7071067811865391350, -0.7071067811865560104 ) ) ;
#60709 = DIRECTION ( 'NONE',  ( -4.299999999999999979E-14, 1.000000000000000000, -4.400000000000000367E-29 ) ) ;
#60710 = CARTESIAN_POINT ( 'NONE',  ( 94.86917197795301604, -31.06128196069622760, 0.4256252759109587225 ) ) ;
#60711 = VERTEX_POINT ( 'NONE', #40143 ) ;
#60712 = EDGE_CURVE ( 'NONE', #63781, #26765, #21331, .T. ) ;
#60713 = ORIENTED_EDGE ( 'NONE', *, *, #85042, .T. ) ;
#60714 = EDGE_LOOP ( 'NONE', ( #89459, #63324, #45073, #27055 ) ) ;
#60715 = VECTOR ( 'NONE', #79373, 1000.000000000000000 ) ;
#60716 = ORIENTED_EDGE ( 'NONE', *, *, #59534, .T. ) ;
#60717 = CARTESIAN_POINT ( 'NONE',  ( -126.9052826151614823, 49.45974035476580610, 30.65825619889020004 ) ) ;
#60718 = CARTESIAN_POINT ( 'NONE',  ( 104.6539710028519039, -47.49251396406760506, 23.38895860924494841 ) ) ;
#60719 = CARTESIAN_POINT ( 'NONE',  ( 162.5667039024478413, -32.29483332967974718, 193.9678068554149775 ) ) ;
#60720 = CARTESIAN_POINT ( 'NONE',  ( 116.7618137187695595, -39.33727037636729307, 118.6187472951199453 ) ) ;
#60722 = CYLINDRICAL_SURFACE ( 'NONE', #61659, 179.8898777604655095 ) ;
#60721 = CARTESIAN_POINT ( 'NONE',  ( 122.2221484686747459, -111.9108568887688477, -19.23816181211476817 ) ) ;
#60723 = CARTESIAN_POINT ( 'NONE',  ( 110.7878219579318255, -44.41760495294317934, 247.3581341137909533 ) ) ;
#60724 = VERTEX_POINT ( 'NONE', #20618 ) ;
#60725 = AXIS2_PLACEMENT_3D ( 'NONE', #16516, #44193, #59165 ) ;
#60726 = ORIENTED_EDGE ( 'NONE', *, *, #61854, .F. ) ;
#60727 = EDGE_LOOP ( 'NONE', ( #41768, #5289, #12677, #83697 ) ) ;
#60728 = EDGE_CURVE ( 'NONE', #50014, #19244, #47379, .T. ) ;
#60729 = CARTESIAN_POINT ( 'NONE',  ( 151.0371591254576060, -24.95799193692592155, 129.9678068554149775 ) ) ;
#60730 = DIRECTION ( 'NONE',  ( -0.7071067811864671926, -0.7071067811866279529, -7.071067811864664779E-16 ) ) ;
#60731 = LINE ( 'NONE', #68467, #35357 ) ;
#60732 = LINE ( 'NONE', #12610, #57674 ) ;
#60733 = ADVANCED_FACE ( 'NONE', ( #12458 ), #48287, .F. ) ;
#60734 = CARTESIAN_POINT ( 'NONE',  ( 116.5375268006221319, -40.16019621794498562, 19.98158330589694387 ) ) ;
#60735 = CARTESIAN_POINT ( 'NONE',  ( 118.4407179355509072, 94.12556101775334128, 5.241146580996987048 ) ) ;
#60736 = EDGE_CURVE ( 'NONE', #21752, #33552, #41481, .T. ) ;
#60737 = CARTESIAN_POINT ( 'NONE',  ( 7.661254700127833495, 82.54999999999999716, 317.6630000000000109 ) ) ;
#60738 = CARTESIAN_POINT ( 'NONE',  ( 115.9938418408662244, -42.00591315737207054, 283.4137205140066271 ) ) ;
#60739 = DIRECTION ( 'NONE',  ( 0.000000000000000000, 0.000000000000000000, -1.000000000000000000 ) ) ;
#60740 = ADVANCED_FACE ( 'NONE', ( #62385 ), #165, .F. ) ;
#60741 = ORIENTED_EDGE ( 'NONE', *, *, #31629, .F. ) ;
#60742 = VECTOR ( 'NONE', #30993, 1000.000000000000000 ) ;
#60743 = EDGE_CURVE ( 'NONE', #29576, #82508, #63289, .T. ) ;
#60744 = CARTESIAN_POINT ( 'NONE',  ( 188.5667039024479834, -62.87844715994099687, 142.0928068554150059 ) ) ;
#60745 = DIRECTION ( 'NONE',  ( 4.299999999999999979E-14, -1.000000000000000000, 4.400000000000000367E-29 ) ) ;
#60746 = CARTESIAN_POINT ( 'NONE',  ( 99.81817287040931319, -30.93652672145504567, 43.60809036959195595 ) ) ;
#60747 = EDGE_CURVE ( 'NONE', #15026, #61208, #608, .T. ) ;
#60748 = VECTOR ( 'NONE', #34480, 1000.000000000000000 ) ;
#60749 = EDGE_CURVE ( 'NONE', #67882, #11886, #50992, .T. ) ;
#60750 = CARTESIAN_POINT ( 'NONE',  ( 83.06670390244802604, -43.72944715994108122, 231.5838068554169524 ) ) ;
#60751 = ADVANCED_FACE ( 'NONE', ( #62832 ), #28777, .T. ) ;
#60752 = DIRECTION ( 'NONE',  ( 0.000000000000000000, 1.000000000000000000, 0.000000000000000000 ) ) ;
#60753 = CARTESIAN_POINT ( 'NONE',  ( -12.03126724623370336, 86.63797872897063712, 117.9440057874066099 ) ) ;
#60754 = ORIENTED_EDGE ( 'NONE', *, *, #49600, .T. ) ;
#60755 = LINE ( 'NONE', #87584, #33434 ) ;
#60756 = AXIS2_PLACEMENT_3D ( 'NONE', #47801, #61885, #77780 ) ;
#60757 = CARTESIAN_POINT ( 'NONE',  ( 123.4412257795802645, 60.45185376280554834, -42.51366219649503364 ) ) ;
#60758 = ORIENTED_EDGE ( 'NONE', *, *, #41404, .F. ) ;
#60759 = CARTESIAN_POINT ( 'NONE',  ( 108.0341695913198521, -25.71842219955733810, 109.9946728949589811 ) ) ;
#60760 = ORIENTED_EDGE ( 'NONE', *, *, #80203, .T. ) ;
#60761 = CARTESIAN_POINT ( 'NONE',  ( 112.3425469992411649, -30.01235824646559891, 78.96956268521998368 ) ) ;
#60762 = EDGE_CURVE ( 'NONE', #65338, #84820, #27122, .T. ) ;
#60763 = AXIS2_PLACEMENT_3D ( 'NONE', #31920, #11035, #79658 ) ;
#60764 = DIRECTION ( 'NONE',  ( 0.000000000000000000, 0.000000000000000000, -1.000000000000000000 ) ) ;
#60765 = CARTESIAN_POINT ( 'NONE',  ( 104.5515342781392008, -45.22670024980423165, 103.7787261630399911 ) ) ;
#60766 = LINE ( 'NONE', #80341, #12636 ) ;
#60767 = AXIS2_PLACEMENT_3D ( 'NONE', #46618, #47512, #61593 ) ;
#60768 = CARTESIAN_POINT ( 'NONE',  ( 37.36643805256573359, -48.62818131006127231, 129.9678068554150911 ) ) ;
#60769 = CARTESIAN_POINT ( 'NONE',  ( 96.05470400087912708, -37.92356717231275098, 77.40038718067299328 ) ) ;
#60770 = DIRECTION ( 'NONE',  ( 1.000000000000000000, 0.000000000000000000, 0.000000000000000000 ) ) ;
#60771 = FACE_OUTER_BOUND ( 'NONE', #14570, .T. ) ;
#60772 = EDGE_LOOP ( 'NONE', ( #44630, #78416, #4687, #13547 ) ) ;
#60773 = CARTESIAN_POINT ( 'NONE',  ( 77.85525873417948617, -20.37463194332874750, 2.472581811070362789 ) ) ;
#60774 = ORIENTED_EDGE ( 'NONE', *, *, #83540, .T. ) ;
#60775 = EDGE_LOOP ( 'NONE', ( #44821, #42077, #11811, #76765 ) ) ;
#60776 = CONICAL_SURFACE ( 'NONE', #72413, 16.25000000000000000, 0.5235987755982992597 ) ;
#60777 = EDGE_CURVE ( 'NONE', #39460, #28724, #85098, .T. ) ;
#60778 = CARTESIAN_POINT ( 'NONE',  ( 57.56670390244744340, -48.82844715994040286, 170.7178068554150911 ) ) ;
#60779 = ORIENTED_EDGE ( 'NONE', *, *, #36293, .F. ) ;
#60780 = CARTESIAN_POINT ( 'NONE',  ( 100.0046238269856929, -29.91446987444270178, 250.7156252759109520 ) ) ;
#60781 = CARTESIAN_POINT ( 'NONE',  ( 98.26250712568560175, -31.04002435091596368, 141.8699109901969564 ) ) ;
#60782 = ADVANCED_FACE ( 'NONE', ( #22415, #71016 ), #78286, .F. ) ;
#60783 = FACE_OUTER_BOUND ( 'NONE', #57953, .T. ) ;
#60784 = CARTESIAN_POINT ( 'NONE',  ( 105.7140088855255868, -46.72363573100787448, 128.4688416786118523 ) ) ;
#60785 = CARTESIAN_POINT ( 'NONE',  ( 95.48802730109245829, -34.20477442036718685, 102.1556252759109640 ) ) ;
#60787 = EDGE_CURVE ( 'NONE', #24712, #84043, #2413, .T. ) ;
#60786 = DIRECTION ( 'NONE',  ( -0.9068632946707805287, 0.4214249218767882610, -9.068632946707800501E-16 ) ) ;
#60788 = EDGE_LOOP ( 'NONE', ( #55756, #83200, #60716, #58872 ) ) ;
#60789 = DIRECTION ( 'NONE',  ( 0.000000000000000000, -1.000000000000000000, 0.000000000000000000 ) ) ;
#60790 = EDGE_CURVE ( 'NONE', #89625, #41277, #16489, .T. ) ;
#60791 = CARTESIAN_POINT ( 'NONE',  ( 98.06670390244704549, -104.2784471599411376, 2.217806855418003043 ) ) ;
#60793 = VERTEX_POINT ( 'NONE', #63745 ) ;
#60792 = VECTOR ( 'NONE', #81669, 1000.000000000000000 ) ;
#60794 = LINE ( 'NONE', #61681, #63449 ) ;
#60795 = FACE_OUTER_BOUND ( 'NONE', #16218, .T. ) ;
#60796 = CARTESIAN_POINT ( 'NONE',  ( 100.1532602078032568, -44.50350736857021161, 266.9984824187679919 ) ) ;
#60797 = DIRECTION ( 'NONE',  ( 0.000000000000000000, 0.000000000000000000, 1.000000000000000000 ) ) ;
#60798 = CARTESIAN_POINT ( 'NONE',  ( 63.03715912545736444, -24.42818131006017879, 237.4678068554150059 ) ) ;
#60799 = CARTESIAN_POINT ( 'NONE',  ( 77.96454488115740844, -38.51222316632514975, 2.376608873920554643 ) ) ;
#60800 = CARTESIAN_POINT ( 'NONE',  ( 114.5649785483395249, -40.87970871860825639, 262.8467055423626562 ) ) ;
#60802 = CARTESIAN_POINT ( 'NONE',  ( 108.9812119692459049, -46.95502683147942236, 78.72419670448194040 ) ) ;
#60801 = CARTESIAN_POINT ( 'NONE',  ( -3.174999999999644995, 8.255000000000000782, 33.98325472291465132 ) ) ;
#60803 = DIRECTION ( 'NONE',  ( -1.000000000000000000, 0.000000000000000000, -8.503806984168940141E-16 ) ) ;
#60804 = CARTESIAN_POINT ( 'NONE',  ( 116.8478532179160680, -43.50835558345241338, 163.3441967044829823 ) ) ;
#60805 = ORIENTED_EDGE ( 'NONE', *, *, #76391, .T. ) ;
#60806 = FACE_OUTER_BOUND ( 'NONE', #1102, .T. ) ;
#60807 = VERTEX_POINT ( 'NONE', #42824 ) ;
#60808 = DIRECTION ( 'NONE',  ( 0.000000000000000000, -1.000000000000000000, 0.000000000000000000 ) ) ;
#60809 = CARTESIAN_POINT ( 'NONE',  ( 74.15067561874269586, 127.0000000000000000, -68.53801554307419508 ) ) ;
#60810 = CARTESIAN_POINT ( 'NONE',  ( 152.0368932755772562, -23.42844715993587812, 193.9678068554149775 ) ) ;
#60811 = ORIENTED_EDGE ( 'NONE', *, *, #63750, .T. ) ;
#60812 = CIRCLE ( 'NONE', #30360, 0.9999999999999940048 ) ;
#60813 = CARTESIAN_POINT ( 'NONE',  ( 97.81413224952068219, -40.51639846094042952, 101.6360726122380100 ) ) ;
#60815 = ORIENTED_EDGE ( 'NONE', *, *, #83129, .F. ) ;
#60814 = CARTESIAN_POINT ( 'NONE',  ( 105.3088311808849937, -48.49934056980919905, 147.4584824187679715 ) ) ;
#60816 = DIRECTION ( 'NONE',  ( -1.000000000000000000, 0.000000000000000000, 0.000000000000000000 ) ) ;
#60817 = CARTESIAN_POINT ( 'NONE',  ( 128.0667039024480118, -48.82844715994099971, 10.91780685541499807 ) ) ;
#60818 = CARTESIAN_POINT ( 'NONE',  ( 107.0667039024470313, -104.2784471599414502, 0.2178068554180012661 ) ) ;
#60820 = CARTESIAN_POINT ( 'NONE',  ( 104.4081006714045401, -46.45808914282129365, 77.36479194341235655 ) ) ;
#60819 = CIRCLE ( 'NONE', #4286, 9.524999999999998579 ) ;
#60821 = ORIENTED_EDGE ( 'NONE', *, *, #9135, .T. ) ;
#60822 = APPLICATION_PROTOCOL_DEFINITION ( 'draft international standard', 'automotive_design', 1998, #35322 ) ;
#60823 = LINE ( 'NONE', #43404, #10813 ) ;
#60824 = VERTEX_POINT ( 'NONE', #8793 ) ;
#60825 = ADVANCED_BREP_SHAPE_REPRESENTATION ( '', ( #80104, #50656 ), #7165 ) ;
#60826 = VECTOR ( 'NONE', #31498, 1000.000000000000000 ) ;
#60827 = VERTEX_POINT ( 'NONE', #21976 ) ;
#60828 = DIRECTION ( 'NONE',  ( -4.237773401492740281E-14, 1.000000000000000000, 0.000000000000000000 ) ) ;
#60829 = CARTESIAN_POINT ( 'NONE',  ( 92.60677566276832806, 95.25015599858946302, -92.02731164704627531 ) ) ;
#60830 = DIRECTION ( 'NONE',  ( -3.100000000000000258E-29, 3.100000000000000044E-14, 1.000000000000000000 ) ) ;
#60831 = DIRECTION ( 'NONE',  ( -3.100000000000000258E-29, 3.100000000000000044E-14, 1.000000000000000000 ) ) ;
#60832 = VECTOR ( 'NONE', #28778, 1000.000000000000000 ) ;
#60834 = DIRECTION ( 'NONE',  ( -0.7071067811865794361, 0.7071067811865157093, -7.071067811865803697E-16 ) ) ;
#60833 = CARTESIAN_POINT ( 'NONE',  ( 97.81169585860149596, -40.51742224678086046, 106.6356332503197137 ) ) ;
#60835 = DIRECTION ( 'NONE',  ( 1.000000000000000078E-15, -1.000000000000000083E-30, -1.000000000000000000 ) ) ;
#60836 = ORIENTED_EDGE ( 'NONE', *, *, #53890, .T. ) ;
#60837 = EDGE_CURVE ( 'NONE', #70844, #29186, #31446, .T. ) ;
#60838 = FACE_OUTER_BOUND ( 'NONE', #66601, .T. ) ;
#60839 = EDGE_CURVE ( 'NONE', #14129, #39083, #7430, .T. ) ;
#60840 = CARTESIAN_POINT ( 'NONE',  ( 117.1144258088630039, -31.97015794161414703, 210.1784824187679703 ) ) ;
#60841 = AXIS2_PLACEMENT_3D ( 'NONE', #66161, #79381, #45268 ) ;
#60843 = VERTEX_POINT ( 'NONE', #64194 ) ;
#60842 = CARTESIAN_POINT ( 'NONE',  ( 107.0664832912750057, -36.72944715993903486, 9.425625275910970657 ) ) ;
#60844 = ADVANCED_FACE ( 'NONE', ( #55997 ), #49642, .F. ) ;
#60845 = CARTESIAN_POINT ( 'NONE',  ( 116.8435662018513028, -36.99793375417353758, 39.80419670448193159 ) ) ;
#60846 = DIRECTION ( 'NONE',  ( -1.000000000000000000, -1.541976423090496028E-15, 0.000000000000000000 ) ) ;
#60847 = CARTESIAN_POINT ( 'NONE',  ( 116.8182762850237992, -34.15738849411049216, 14.03188649359343110 ) ) ;
#60848 = LINE ( 'NONE', #4106, #80816 ) ;
#60849 = EDGE_CURVE ( 'NONE', #21043, #62123, #56058, .T. ) ;
#60850 = EDGE_LOOP ( 'NONE', ( #14802, #26092 ) ) ;
#60851 = DIRECTION ( 'NONE',  ( -1.000000000000000078E-15, 0.000000000000000000, 1.000000000000000000 ) ) ;
#60852 = EDGE_CURVE ( 'NONE', #60267, #48081, #37827, .T. ) ;
#60853 = ORIENTED_EDGE ( 'NONE', *, *, #39126, .T. ) ;
#60854 = VERTEX_POINT ( 'NONE', #17819 ) ;
#60855 = CIRCLE ( 'NONE', #21721, 5.041900000000001825 ) ;
#60856 = CARTESIAN_POINT ( 'NONE',  ( 110.5184084024339626, -28.56779955429167472, 241.1901547344679670 ) ) ;
#60857 = EDGE_CURVE ( 'NONE', #58867, #22696, #6818, .T. ) ;
#60858 = CARTESIAN_POINT ( 'NONE',  ( 109.6449249915308997, -46.47961346067916111, 53.78125628650596468 ) ) ;
#60859 = B_SPLINE_CURVE_WITH_KNOTS ( 'NONE', 3,
 ( #44280, #9784, #17926, #37492, #58802, #51103, #86097, #45602, #51977, #23870, #79289, #17049, #44730, #72461, #37933, #73334, #3416, #66521, #31998, #79734, #25186, #52848, #80620, #17492, #45172, #46054, #37042, #33348, #19280, #40148, #75133, #66972, #47404, #39267, #88334 ),
 .UNSPECIFIED., .F., .F.,
 ( 4, 2, 2, 1, 1, 2, 2, 2, 2, 2, 2, 1, 1, 2, 2, 2, 1, 1, 1, 2, 4 ),
 ( 0.3333434881890884882, 0.4166701562233637857, 0.4218780729755075565, 0.4270859897276513273, 0.4375018232319339284, 0.4583334902404989086, 0.4999968242576238175, 0.5208284912661862442, 0.5416601582747487820, 0.5624918252833113197, 0.5650957836593817341, 0.5676997420354521484, 0.5729076587875948645, 0.5833234922918794085, 0.6249868263090219145, 0.6275907846850933280, 0.6301947430611646306, 0.6354026598133065695, 0.6458184933175894482, 0.6562343268218724379, 0.6666501603261554276 ),
 .UNSPECIFIED. ) ;
#60860 = CARTESIAN_POINT ( 'NONE',  ( -83.15057989154965412, 85.43248893795411902, 100.6521573293566121 ) ) ;
#60861 = EDGE_CURVE ( 'NONE', #19807, #6482, #66859, .T. ) ;
#60862 = CARTESIAN_POINT ( 'NONE',  ( 117.0608945211236716, -38.08045314457236685, 154.7189586073530165 ) ) ;
#60863 = DIRECTION ( 'NONE',  ( 3.340531404218880531E-13, -1.000000000000000000, 2.910531404218880430E-28 ) ) ;
#60864 = EDGE_LOOP ( 'NONE', ( #69289, #22265, #72542, #59637 ) ) ;
#60865 = CIRCLE ( 'NONE', #23179, 2.117000000000000881 ) ;
#60866 = CARTESIAN_POINT ( 'NONE',  ( 53.56670390244833158, -48.82844715994055917, 249.9678068554150343 ) ) ;
#60867 = DIRECTION ( 'NONE',  ( 0.000000000000000000, 0.000000000000000000, 1.000000000000000000 ) ) ;
#60868 = VERTEX_POINT ( 'NONE', #9663 ) ;
#60869 = CARTESIAN_POINT ( 'NONE',  ( 116.4746376734894255, -32.23794665461475972, 19.18133956162493092 ) ) ;
#60870 = ORIENTED_EDGE ( 'NONE', *, *, #18613, .F. ) ;
#60871 = ORIENTED_EDGE ( 'NONE', *, *, #57691, .F. ) ;
#60872 = CARTESIAN_POINT ( 'NONE',  ( 101.1728908740289512, -31.04189437634028437, 248.5338046553059428 ) ) ;
#60873 = EDGE_CURVE ( 'NONE', #63079, #23299, #79175, .T. ) ;
#60874 = VECTOR ( 'NONE', #7560, 1000.000000000000000 ) ;
#60875 = CARTESIAN_POINT ( 'NONE',  ( 107.0667039024479834, -48.82844715994099971, 160.9178068554150229 ) ) ;
#60876 = CARTESIAN_POINT ( 'NONE',  ( 114.0519814166327563, -29.87813257090970609, 149.4441967044829767 ) ) ;
#60877 = CARTESIAN_POINT ( 'NONE',  ( 23.62182483554943957, 80.43530414067632250, 307.1735616208110855 ) ) ;
#60878 = CARTESIAN_POINT ( 'NONE',  ( 162.5667039024470171, -32.29483332968611364, -5.074374724088000832 ) ) ;
#60879 = CARTESIAN_POINT ( 'NONE',  ( 147.9173673660669124, -72.54478064608022692, 542.9756252759101471 ) ) ;
#60880 = CARTESIAN_POINT ( 'NONE',  ( 9.073998176338214705, 73.66341487109981756, 130.2403208068726030 ) ) ;
#60881 = EDGE_CURVE ( 'NONE', #78112, #17073, #53194, .T. ) ;
#60882 = CARTESIAN_POINT ( 'NONE',  ( 96.72972436280956288, -34.86144565006776475, 237.1841967044819626 ) ) ;
#60884 = CARTESIAN_POINT ( 'NONE',  ( 162.5667039024470171, -32.29483332968611364, 342.9256252759109884 ) ) ;
#60883 = AXIS2_PLACEMENT_3D ( 'NONE', #78435, #72923, #2568 ) ;
#60885 = AXIS2_PLACEMENT_3D ( 'NONE', #33410, #89285, #75651 ) ;
#60886 = ORIENTED_EDGE ( 'NONE', *, *, #25827, .F. ) ;
#60887 = CARTESIAN_POINT ( 'NONE',  ( 117.3964687521579293, -38.63454956243933225, 84.68133956162593279 ) ) ;
#60888 = LINE ( 'NONE', #19553, #13478 ) ;
#60889 = ORIENTED_EDGE ( 'NONE', *, *, #14144, .T. ) ;
#60890 = VERTEX_POINT ( 'NONE', #39153 ) ;
#60891 = ORIENTED_EDGE ( 'NONE', *, *, #80876, .F. ) ;
#60892 = VECTOR ( 'NONE', #21019, 1000.000000000000000 ) ;
#60893 = LINE ( 'NONE', #68617, #26021 ) ;
#60894 = DIRECTION ( 'NONE',  ( 0.000000000000000000, 0.000000000000000000, -1.000000000000000000 ) ) ;
#60895 = VECTOR ( 'NONE', #79665, 1000.000000000000000 ) ;
#60896 = CARTESIAN_POINT ( 'NONE',  ( 99.04383488216355147, -42.84091735427421810, 151.8445027460794279 ) ) ;
#60897 = DIRECTION ( 'NONE',  ( -0.000000000000000000, 1.000000000000000000, 0.000000000000000000 ) ) ;
#60898 = CARTESIAN_POINT ( 'NONE',  ( 112.3727512366848487, -30.49036002617200936, 137.3338046553059826 ) ) ;
#60899 = CARTESIAN_POINT ( 'NONE',  ( 96.99552470177088992, -33.95220897389439330, 247.1127681330539758 ) ) ;
#60901 = EDGE_CURVE ( 'NONE', #31453, #60027, #87314, .T. ) ;
#60900 = CARTESIAN_POINT ( 'NONE',  ( -492.0614999999999668, 14.28749999999982201, 90.48749999999999716 ) ) ;
#60902 = EDGE_LOOP ( 'NONE', ( #29572, #34731, #73024, #36047 ) ) ;
#60903 = CARTESIAN_POINT ( 'NONE',  ( 130.0134714785366157, 87.03008507238369873, -11.89083589963720122 ) ) ;
#60904 = CIRCLE ( 'NONE', #30452, 6.349999999999994316 ) ;
#60905 = ADVANCED_FACE ( 'NONE', ( #3306 ), #3746, .T. ) ;
#60906 = CARTESIAN_POINT ( 'NONE',  ( 142.8841478025725849, -84.11588139007200482, 396.9756252759102040 ) ) ;
#60907 = ORIENTED_EDGE ( 'NONE', *, *, #82841, .F. ) ;
#60908 = ORIENTED_EDGE ( 'NONE', *, *, #23034, .F. ) ;
#60909 = CARTESIAN_POINT ( 'NONE',  ( 179.1667039024460166, -26.71338133339251542, -5.074374724088000832 ) ) ;
#60910 = ORIENTED_EDGE ( 'NONE', *, *, #47667, .T. ) ;
#60911 = ORIENTED_EDGE ( 'NONE', *, *, #35583, .T. ) ;
#60912 = DIRECTION ( 'NONE',  ( -1.000000000000000000, 0.000000000000000000, 0.000000000000000000 ) ) ;
#60913 = CARTESIAN_POINT ( 'NONE',  ( -12.37565694608801437, 79.66829940370548968, -129.9681453810340770 ) ) ;
#60914 = FACE_OUTER_BOUND ( 'NONE', #54811, .T. ) ;
#60915 = PLANE ( 'NONE',  #27232 ) ;
#60916 = VECTOR ( 'NONE', #60579, 1000.000000000000000 ) ;
#60917 = CARTESIAN_POINT ( 'NONE',  ( 99.86829443779211601, -32.07773762820211516, 145.2924198280769872 ) ) ;
#60918 = CARTESIAN_POINT ( 'NONE',  ( 109.6539202653692087, -46.87399426414072678, 47.77562527591094721 ) ) ;
#60919 = CARTESIAN_POINT ( 'NONE',  ( 0.000000000000000000, 1.270000000000000018, 0.000000000000000000 ) ) ;
#60920 = VERTEX_POINT ( 'NONE', #73218 ) ;
#60921 = DIRECTION ( 'NONE',  ( -1.000000000000000078E-15, 1.000000000000000083E-30, 1.000000000000000000 ) ) ;
#60922 = ORIENTED_EDGE ( 'NONE', *, *, #24287, .T. ) ;
#60923 = CYLINDRICAL_SURFACE ( 'NONE', #56227, 6.349999999999997868 ) ;
#60924 = ORIENTED_EDGE ( 'NONE', *, *, #3689, .T. ) ;
#60925 = DIRECTION ( 'NONE',  ( -3.100000000000000258E-29, 3.100000000000000044E-14, 1.000000000000000000 ) ) ;
#60926 = CARTESIAN_POINT ( 'NONE',  ( -10.91422816413673402, 76.24044119408891618, 118.0527134162828276 ) ) ;
#60927 = CARTESIAN_POINT ( 'NONE',  ( 98.54776827858368904, -41.97716740062048757, 131.7658491656293620 ) ) ;
#60928 = AXIS2_PLACEMENT_3D ( 'NONE', #27696, #20887, #13619 ) ;
#60929 = ADVANCED_FACE ( 'NONE', ( #37373 ), #58691, .F. ) ;
#60930 = CARTESIAN_POINT ( 'NONE',  ( 62.03742497533746558, -23.42844715994041849, 300.4678068554150627 ) ) ;
#60931 = VERTEX_POINT ( 'NONE', #31888 ) ;
#60932 = CARTESIAN_POINT ( 'NONE',  ( 101.3720933679328482, -27.97043537882594322, 25.53562527591096654 ) ) ;
#60933 = CARTESIAN_POINT ( 'NONE',  ( 115.6092852924205943, -42.78035731602705027, 49.33562527591095659 ) ) ;
#60935 = CARTESIAN_POINT ( 'NONE',  ( 29.00000000000001421, 172.0000000000000000, 113.8826257785461280 ) ) ;
#60934 = CYLINDRICAL_SURFACE ( 'NONE', #11481, 3.000000000000002665 ) ;
#60936 = CARTESIAN_POINT ( 'NONE',  ( 100.9546813260442519, -28.70701916483188398, 146.5944087211518365 ) ) ;
#60937 = CARTESIAN_POINT ( 'NONE',  ( 97.81168895331838087, -40.51742574516882200, 287.6356252759109680 ) ) ;
#60938 = FACE_OUTER_BOUND ( 'NONE', #1381, .T. ) ;
#60939 = CARTESIAN_POINT ( 'NONE',  ( -41.60202597009397607, 54.97499999999995879, 50.85338361873603219 ) ) ;
#60941 = CARTESIAN_POINT ( 'NONE',  ( 176.7669697523288335, -48.62818131005481348, 180.4678068554150059 ) ) ;
#60940 = VECTOR ( 'NONE', #27772, 1000.000000000000000 ) ;
#60942 = ORIENTED_EDGE ( 'NONE', *, *, #46072, .T. ) ;
#60943 = CARTESIAN_POINT ( 'NONE',  ( 96.79018504364255193, -38.90877927100929412, 31.49276813305495892 ) ) ;
#60944 = CARTESIAN_POINT ( 'NONE',  ( 115.1837411929738977, -43.30572140991047547, 84.28419670448195689 ) ) ;
#60945 = B_SPLINE_CURVE_WITH_KNOTS ( 'NONE', 3,
 ( #53793, #54235, #81112, #19755, #47435 ),
 .UNSPECIFIED., .F., .F.,
 ( 4, 1, 4 ),
 ( 0.000000000000000000, 0.4203864884934794266, 1.000000000000000000 ),
 .UNSPECIFIED. ) ;
#60947 = DIRECTION ( 'NONE',  ( 0.000000000000000000, 0.000000000000000000, -1.000000000000000000 ) ) ;
#60946 = FACE_OUTER_BOUND ( 'NONE', #49835, .T. ) ;
#60948 = DIRECTION ( 'NONE',  ( 0.000000000000000000, 0.000000000000000000, 1.000000000000000000 ) ) ;
#60949 = EDGE_CURVE ( 'NONE', #53618, #89279, #69343, .T. ) ;
#60950 = CIRCLE ( 'NONE', #21811, 4.875000000000017764 ) ;
#60951 = EDGE_CURVE ( 'NONE', #32654, #6676, #5398, .T. ) ;
#60952 = LINE ( 'NONE', #88681, #81087 ) ;
#60953 = ORIENTED_EDGE ( 'NONE', *, *, #37085, .T. ) ;
#60954 = ADVANCED_FACE ( 'NONE', ( #17376 ), #59579, .T. ) ;
#60955 = CARTESIAN_POINT ( 'NONE',  ( 96.20363159075265003, -34.36081134307599427, 102.1556252759109640 ) ) ;
#60956 = AXIS2_PLACEMENT_3D ( 'NONE', #60331, #39893, #32633 ) ;
#60958 = ORIENTED_EDGE ( 'NONE', *, *, #63727, .F. ) ;
#60957 = LINE ( 'NONE', #52757, #54401 ) ;
#60959 = EDGE_CURVE ( 'NONE', #50481, #71480, #24632, .T. ) ;
#60960 = CARTESIAN_POINT ( 'NONE',  ( 96.16101635903912381, -35.07578045570940617, 217.1946728949589840 ) ) ;
#60961 = PLANE ( 'NONE',  #26604 ) ;
#60962 = DIRECTION ( 'NONE',  ( 1.000000000000000000, 0.000000000000000000, 0.000000000000000000 ) ) ;
#60963 = DIRECTION ( 'NONE',  ( 0.000000000000000000, 0.000000000000000000, 1.000000000000000000 ) ) ;
#60964 = CARTESIAN_POINT ( 'NONE',  ( 97.07207206298383539, -35.37844117089505858, 82.21895860700102787 ) ) ;
#60965 = CARTESIAN_POINT ( 'NONE',  ( 131.6729728819749710, -38.08739819366338253, 2.653088468873541661 ) ) ;
#60966 = EDGE_CURVE ( 'NONE', #25485, #18963, #45494, .T. ) ;
#60967 = DIRECTION ( 'NONE',  ( 0.000000000000000000, -1.000000000000000000, 0.000000000000000000 ) ) ;
#60968 = AXIS2_PLACEMENT_3D ( 'NONE', #75350, #27192, #14472 ) ;
#60969 = CARTESIAN_POINT ( 'NONE',  ( 103.1049807579881161, -45.67203811392948865, 177.2441967044829596 ) ) ;
#60970 = ORIENTED_EDGE ( 'NONE', *, *, #14885, .F. ) ;
#60971 = EDGE_LOOP ( 'NONE', ( #73009, #18588, #70986 ) ) ;
#60972 = CARTESIAN_POINT ( 'NONE',  ( 103.0168143257329092, -28.81349422576414554, 116.8844404487539634 ) ) ;
#60973 = EDGE_CURVE ( 'NONE', #26689, #44076, #18261, .T. ) ;
#60974 = FACE_BOUND ( 'NONE', #24548, .T. ) ;
#60976 = PLANE ( 'NONE',  #44815 ) ;
#60975 = CARTESIAN_POINT ( 'NONE',  ( 99.81116105471878086, -29.32005551970522461, 266.7051490854344706 ) ) ;
#60977 = DIRECTION ( 'NONE',  ( 0.000000000000000000, 0.000000000000000000, -1.000000000000000000 ) ) ;
#60978 = EDGE_CURVE ( 'NONE', #37421, #60824, #60024, .T. ) ;
#60979 = AXIS2_PLACEMENT_3D ( 'NONE', #7949, #27490, #13867 ) ;
#60980 = LINE ( 'NONE', #11946, #17096 ) ;
#60981 = LINE ( 'NONE', #53688, #54519 ) ;
#60982 = LINE ( 'NONE', #33729, #30398 ) ;
#60983 = DIRECTION ( 'NONE',  ( -1.000000000000000078E-15, 1.000000000000000083E-30, 1.000000000000000000 ) ) ;
#60984 = CARTESIAN_POINT ( 'NONE',  ( 106.4848323041101850, -24.91801670280273129, 195.1156252759109861 ) ) ;
#60985 = FACE_OUTER_BOUND ( 'NONE', #24589, .T. ) ;
#60986 = ORIENTED_EDGE ( 'NONE', *, *, #1554, .T. ) ;
#60987 = EDGE_LOOP ( 'NONE', ( #1031, #81857, #18451, #85715 ) ) ;
#60988 = DIRECTION ( 'NONE',  ( 0.000000000000000000, 0.000000000000000000, 1.000000000000000000 ) ) ;
#60989 = CARTESIAN_POINT ( 'NONE',  ( 78.64819577387126515, -16.37139167074854385, 1.944749297849994951 ) ) ;
#60990 = DIRECTION ( 'NONE',  ( 1.000000000000000000, 0.000000000000000000, 0.000000000000000000 ) ) ;
#60991 = DIRECTION ( 'NONE',  ( 1.000000000000000000, 0.000000000000000000, 0.000000000000000000 ) ) ;
#60992 = FACE_OUTER_BOUND ( 'NONE', #85013, .T. ) ;
#60993 = ORIENTED_EDGE ( 'NONE', *, *, #15058, .T. ) ;
#60994 = CARTESIAN_POINT ( 'NONE',  ( -10.24823410656255263, 89.89188270629901467, 117.9117007251406335 ) ) ;
#60995 = CARTESIAN_POINT ( 'NONE',  ( 113.0222799004901333, -45.32912119007338703, 203.0584824187679374 ) ) ;
#60996 = ORIENTED_EDGE ( 'NONE', *, *, #49692, .F. ) ;
#60997 = LINE ( 'NONE', #88726, #76728 ) ;
#60998 = CARTESIAN_POINT ( 'NONE',  ( 19.56648329127400032, 15.62155284005900491, 328.6381252759109088 ) ) ;
#60999 = CARTESIAN_POINT ( 'NONE',  ( 72.06648329127396835, -9.729447159941065237, 14.67562527591093513 ) ) ;
#61000 = VECTOR ( 'NONE', #12049, 1000.000000000000000 ) ;
#61001 = CARTESIAN_POINT ( 'NONE',  ( 105.2414988608755522, -45.18937368885499950, 30.23761417911497063 ) ) ;
#61002 = CARTESIAN_POINT ( 'NONE',  ( 108.5929805111718593, -47.10003145027929605, 138.6927681330539883 ) ) ;
#61003 = AXIS2_PLACEMENT_3D ( 'NONE', #44967, #30904, #10027 ) ;
#61004 = CARTESIAN_POINT ( 'NONE',  ( -24.20305689751608824, 65.59999999999998010, 58.62596543806478877 ) ) ;
#61005 = ORIENTED_EDGE ( 'NONE', *, *, #65763, .T. ) ;
#61006 = ADVANCED_FACE ( 'NONE', ( #18713 ), #67769, .F. ) ;
#61007 = CARTESIAN_POINT ( 'NONE',  ( 107.7702177616926065, 120.6499999999999915, 4.179089330879380409E-13 ) ) ;
#61008 = DIRECTION ( 'NONE',  ( 3.999999999999999995E-14, -1.000000000000000000, 4.100000000000000342E-29 ) ) ;
#61009 = EDGE_LOOP ( 'NONE', ( #71164, #7285, #32452, #39881, #50773 ) ) ;
#61011 = EDGE_LOOP ( 'NONE', ( #54479, #77284, #51280, #38787 ) ) ;
#61010 = CIRCLE ( 'NONE', #62445, 2.029999999999997140 ) ;
#61012 = CARTESIAN_POINT ( 'NONE',  ( 5.617021782840719624, 93.94788616487885236, 118.4234307144629383 ) ) ;
#61013 = ORIENTED_EDGE ( 'NONE', *, *, #39589, .F. ) ;
#61014 = ORIENTED_EDGE ( 'NONE', *, *, #6225, .F. ) ;
#61015 = CARTESIAN_POINT ( 'NONE',  ( 46.61670390244704976, -117.2284471599409983, 55.21780685541799727 ) ) ;
#61016 = CARTESIAN_POINT ( 'NONE',  ( 98.58519923211989067, -37.96229866499883343, 65.86384839950598291 ) ) ;
#61017 = VECTOR ( 'NONE', #10856, 1000.000000000000000 ) ;
#61018 = CARTESIAN_POINT ( 'NONE',  ( 107.5109734667377239, -47.16730098390026882, 237.6099109901969655 ) ) ;
#61019 = CARTESIAN_POINT ( 'NONE',  ( 106.9751875180390641, -47.13234726572967759, 187.5699109901969734 ) ) ;
#61021 = CARTESIAN_POINT ( 'NONE',  ( 118.1852327621006538, -40.75705396371408540, 19.54991099019698453 ) ) ;
#61020 = LINE ( 'NONE', #26957, #28688 ) ;
#61022 = FACE_OUTER_BOUND ( 'NONE', #77318, .T. ) ;
#61023 = LINE ( 'NONE', #39240, #61271 ) ;
#61024 = VERTEX_POINT ( 'NONE', #40938 ) ;
#61025 = EDGE_CURVE ( 'NONE', #13532, #18491, #1051, .T. ) ;
#61026 = CARTESIAN_POINT ( 'NONE',  ( 97.81848045301514105, -40.53398251383325146, 111.6370493081401918 ) ) ;
#61027 = CARTESIAN_POINT ( 'NONE',  ( 97.43243490695729747, -40.91715606259069204, 231.6527681330539679 ) ) ;
#61028 = ORIENTED_EDGE ( 'NONE', *, *, #75235, .T. ) ;
#61029 = CARTESIAN_POINT ( 'NONE',  ( 113.1555140577670215, -26.56262906569767068, 204.6470538473399756 ) ) ;
#61030 = DIRECTION ( 'NONE',  ( 0.000000000000000000, 0.000000000000000000, -1.000000000000000000 ) ) ;
#61031 = LINE ( 'NONE', #27407, #59480 ) ;
#61032 = PLANE ( 'NONE',  #74652 ) ;
#61034 = DIRECTION ( 'NONE',  ( 0.000000000000000000, 0.000000000000000000, -1.000000000000000000 ) ) ;
#61033 = CARTESIAN_POINT ( 'NONE',  ( 113.9483801512686370, -32.56050311478266934, 277.6356252759111953 ) ) ;
#61035 = CARTESIAN_POINT ( 'NONE',  ( 116.7951064495445905, -39.38790633866764779, 174.6147857624885660 ) ) ;
#61036 = CARTESIAN_POINT ( 'NONE',  ( 32.09598329127729954, -23.42844715994138838, 237.4678068554150059 ) ) ;
#61037 = AXIS2_PLACEMENT_3D ( 'NONE', #37788, #16011, #23293 ) ;
#61038 = CARTESIAN_POINT ( 'NONE',  ( 92.87912090207764493, -113.5872422955286538, -19.23816181211473975 ) ) ;
#61039 = AXIS2_PLACEMENT_3D ( 'NONE', #47414, #13368, #20631 ) ;
#61040 = CARTESIAN_POINT ( 'NONE',  ( 50.88849390559499142, -32.11662333284530746, -5.074374724088000832 ) ) ;
#61041 = DIRECTION ( 'NONE',  ( 0.000000000000000000, 0.000000000000000000, -1.000000000000000000 ) ) ;
#61042 = AXIS2_PLACEMENT_3D ( 'NONE', #1196, #36621, #64321 ) ;
#61043 = PRODUCT_DEFINITION ( 'UNKNOWN', '', #17401, #89895 ) ;
#61044 = DIRECTION ( 'NONE',  ( 0.000000000000000000, 0.000000000000000000, -1.000000000000000000 ) ) ;
#61046 = ORIENTED_EDGE ( 'NONE', *, *, #59716, .F. ) ;
#61045 = CARTESIAN_POINT ( 'NONE',  ( -4.087988121205965442, 94.58126409692587799, -118.4861679838275990 ) ) ;
#61047 = CARTESIAN_POINT ( 'NONE',  ( 181.8884939055948848, -32.11662333283959470, 117.4678068554150627 ) ) ;
#61048 = CARTESIAN_POINT ( 'NONE',  ( 116.8782924623045290, -40.31758940317881468, 218.5470538473399529 ) ) ;
#61049 = CARTESIAN_POINT ( 'NONE',  ( 101.6782318212999314, -27.07850282373152950, 101.4937205140059575 ) ) ;
#61050 = CARTESIAN_POINT ( 'NONE',  ( 116.6456181429820447, -40.95237922671789477, 249.4956252759109532 ) ) ;
#61051 = CARTESIAN_POINT ( 'NONE',  ( 193.0371591254585724, -47.82818131005411999, 117.4678068554150627 ) ) ;
#61052 = CARTESIAN_POINT ( 'NONE',  ( 71.77848634863079269, 120.6499999999999915, 77.39114642429989033 ) ) ;
#61053 = AXIS2_PLACEMENT_3D ( 'NONE', #19219, #75077, #13305 ) ;
#61055 = DIRECTION ( 'NONE',  ( 1.000000000000000078E-15, -1.000000000000000000, 0.000000000000000000 ) ) ;
#61054 = DIRECTION ( 'NONE',  ( 0.000000000000000000, 1.000000000000000000, 0.000000000000000000 ) ) ;
#61056 = CYLINDRICAL_SURFACE ( 'NONE', #82796, 2.000000000000001776 ) ;
#61057 = CARTESIAN_POINT ( 'NONE',  ( 132.2214349158059861, -20.77077206072004500, 2.188418444514679262 ) ) ;
#61058 = VECTOR ( 'NONE', #54947, 1000.000000000000000 ) ;
#61059 = ORIENTED_EDGE ( 'NONE', *, *, #86822, .T. ) ;
#61060 = ORIENTED_EDGE ( 'NONE', *, *, #30084, .F. ) ;
#61061 = ADVANCED_FACE ( 'NONE', ( #60938 ), #48188, .F. ) ;
#61062 = CARTESIAN_POINT ( 'NONE',  ( 97.81853004928629503, -39.68680891125094234, 130.9952769709339577 ) ) ;
#61064 = EDGE_LOOP ( 'NONE', ( #73406, #49365, #10192, #10279 ) ) ;
#61063 = CARTESIAN_POINT ( 'NONE',  ( 25.56670390244797275, -62.87844715994099687, 137.2178068554150059 ) ) ;
#61065 = CARTESIAN_POINT ( 'NONE',  ( 105.7994081972685194, -26.72404989547063181, 90.17573085178008796 ) ) ;
#61066 = ADVANCED_FACE ( 'NONE', ( #27767 ), #11907, .T. ) ;
#61067 = CARTESIAN_POINT ( 'NONE',  ( 95.69905522618357452, -33.46911247776740339, 137.1041967044819501 ) ) ;
#61068 = CARTESIAN_POINT ( 'NONE',  ( 97.81168895331838087, -40.51742574516882200, 287.6356252759109680 ) ) ;
#61069 = EDGE_CURVE ( 'NONE', #54835, #48081, #53271, .T. ) ;
#61070 = CARTESIAN_POINT ( 'NONE',  ( -47.10523785009519315, 92.57489729980497373, 74.80399995790345713 ) ) ;
#61071 = AXIS2_PLACEMENT_3D ( 'NONE', #62089, #89823, #1678 ) ;
#61072 = CARTESIAN_POINT ( 'NONE',  ( 72.96458098368650269, 101.5999999999999943, 72.96458098368729850 ) ) ;
#61073 = EDGE_CURVE ( 'NONE', #79263, #11190, #28605, .T. ) ;
#61074 = LINE ( 'NONE', #39292, #26562 ) ;
#61075 = CARTESIAN_POINT ( 'NONE',  ( 98.34688518126456813, -32.29864090244028318, 50.95276813305393659 ) ) ;
#61076 = ORIENTED_EDGE ( 'NONE', *, *, #12456, .T. ) ;
#61077 = VERTEX_POINT ( 'NONE', #39593 ) ;
#61079 = ORIENTED_EDGE ( 'NONE', *, *, #71034, .T. ) ;
#61078 = VECTOR ( 'NONE', #83084, 1000.000000000000000 ) ;
#61080 = CARTESIAN_POINT ( 'NONE',  ( -187.8075999999999794, 0.000000000000000000, -12.69999999999999929 ) ) ;
#61082 = CARTESIAN_POINT ( 'NONE',  ( 184.5667039024480118, -67.87844715994100397, 20.91780685541479912 ) ) ;
#61081 = CARTESIAN_POINT ( 'NONE',  ( 113.8941270090216733, -29.67983328691853018, 170.4641967044819637 ) ) ;
#61083 = LINE ( 'NONE', #54690, #85739 ) ;
#61084 = DIRECTION ( 'NONE',  ( -1.000000000000000000, -1.000000000000000078E-15, 0.000000000000000000 ) ) ;
#61085 = ADVANCED_FACE ( 'NONE', ( #89107 ), #67299, .F. ) ;
#61086 = AXIS2_PLACEMENT_3D ( 'NONE', #57096, #22609, #29868 ) ;
#61087 = DIRECTION ( 'NONE',  ( 0.000000000000000000, 0.000000000000000000, 1.000000000000000000 ) ) ;
#61088 = CARTESIAN_POINT ( 'NONE',  ( 91.51255889651523034, 88.18374315479978520, 75.37293521528393114 ) ) ;
#61089 = CARTESIAN_POINT ( 'NONE',  ( -7.661254700127833495, 66.45253841614081125, 317.6630000000000109 ) ) ;
#61090 = CARTESIAN_POINT ( 'NONE',  ( 101.7670726180548115, -27.05576796868577460, 100.4632443235299633 ) ) ;
#61091 = ORIENTED_EDGE ( 'NONE', *, *, #78150, .T. ) ;
#61092 = VERTEX_POINT ( 'NONE', #13251 ) ;
#61093 = VECTOR ( 'NONE', #20388, 1000.000000000000000 ) ;
#61094 = ORIENTED_EDGE ( 'NONE', *, *, #33403, .T. ) ;
#61095 = CARTESIAN_POINT ( 'NONE',  ( 107.0664832912739968, -36.72944715994100306, 287.6356252759109680 ) ) ;
#61096 = CARTESIAN_POINT ( 'NONE',  ( -89.95943163722107272, 94.84315624882771090, -94.61941200740686497 ) ) ;
#61097 = CARTESIAN_POINT ( 'NONE',  ( 76.06670390244796920, -26.72944715994109899, 239.5838068554169809 ) ) ;
#61098 = CARTESIAN_POINT ( 'NONE',  ( 107.7334136049453406, -44.89265071023657327, 175.4595189410199509 ) ) ;
#61099 =( BOUNDED_CURVE ( )  B_SPLINE_CURVE ( 2, ( #107, #50024, #78224 ),
 .UNSPECIFIED., .F., .T. ) 
 B_SPLINE_CURVE_WITH_KNOTS ( ( 3, 3 ),
 ( 0.000000000000000000, 0.5053286420056760653 ),
 .UNSPECIFIED. ) 
 CURVE ( )  GEOMETRIC_REPRESENTATION_ITEM ( )  RATIONAL_B_SPLINE_CURVE ( ( 1.000000000000000000, 1.009299002520649857, 1.000420656333769864 ) ) 
 REPRESENTATION_ITEM ( '' )  );
#61100 = LINE ( 'NONE', #26583, #80888 ) ;
#61101 = ORIENTED_EDGE ( 'NONE', *, *, #13205, .T. ) ;
#61103 = VERTEX_POINT ( 'NONE', #40042 ) ;
#61102 = VERTEX_POINT ( 'NONE', #75920 ) ;
#61104 = DIRECTION ( 'NONE',  ( 1.000000000000000000, 0.000000000000000000, 0.000000000000000000 ) ) ;
#61105 = AXIS2_PLACEMENT_3D ( 'NONE', #54000, #12709, #53095 ) ;
#61106 = CARTESIAN_POINT ( 'NONE',  ( 0.000000000000000000, 92.07499999999998863, 0.000000000000000000 ) ) ;
#61107 = VERTEX_POINT ( 'NONE', #19167 ) ;
#61108 = EDGE_LOOP ( 'NONE', ( #38391, #10044 ) ) ;
#61109 = LINE ( 'NONE', #34295, #21753 ) ;
#61110 = CARTESIAN_POINT ( 'NONE',  ( 104.3066903214637620, -46.41728735870637479, 213.7872975916119458 ) ) ;
#61111 = VECTOR ( 'NONE', #55437, 1000.000000000000000 ) ;
#61112 = EDGE_CURVE ( 'NONE', #52724, #38949, #19919, .T. ) ;
#61113 = LINE ( 'NONE', #6168, #89362 ) ;
#61114 = CARTESIAN_POINT ( 'NONE',  ( 107.0667039024470313, -104.2784471599409528, 24.21780685541800082 ) ) ;
#61115 = ORIENTED_EDGE ( 'NONE', *, *, #47448, .T. ) ;
#61116 = ORIENTED_EDGE ( 'NONE', *, *, #33629, .F. ) ;
#61117 = VECTOR ( 'NONE', #60213, 1000.000000000000000 ) ;
#61118 = CARTESIAN_POINT ( 'NONE',  ( 59.56670390244700997, -79.67844715994098692, 155.2178068554179902 ) ) ;
#61119 = ORIENTED_EDGE ( 'NONE', *, *, #16463, .F. ) ;
#61120 = ORIENTED_EDGE ( 'NONE', *, *, #71571, .T. ) ;
#61121 = EDGE_CURVE ( 'NONE', #72918, #51700, #67759, .T. ) ;
#61122 = CARTESIAN_POINT ( 'NONE',  ( 115.2156275924750020, -36.25915663771239394, 226.6909475124489575 ) ) ;
#61123 = CARTESIAN_POINT ( 'NONE',  ( 106.0743573402139930, -48.56370683269541644, 112.5099109901969712 ) ) ;
#61124 = CARTESIAN_POINT ( 'NONE',  ( 113.4926247784321021, -28.54816540729036589, 79.54705384733995288 ) ) ;
#61125 = CARTESIAN_POINT ( 'NONE',  ( 99.10784393885515442, -37.74513723391706321, 249.5838068554171514 ) ) ;
#61126 = B_SPLINE_SURFACE_WITH_KNOTS ( 'NONE', 3, 3, ( 
 ( #38102, #30842, #73961, #3578, #11739, #73508, #86256 ),
 ( #32611, #45337, #24038, #31274, #58968, #44902, #86706 ),
 ( #10833, #39438, #52144, #45780, #79907, #17662, #60311 ),
 ( #38539, #88048, #53484, #9960, #37663, #47575, #6706 ),
 ( #70626, #8404, #61653, #40773, #13528, #6264, #62115 ) ),
 .UNSPECIFIED., .F., .F., .F.,
 ( 4, 1, 4 ),
 ( 4, 1, 1, 1, 4 ),
 ( 0.000000000000000000, 0.5714285714285709528, 1.000000000000000000 ),
 ( -0.1863387531781160178, 0.9565458916201099449, 3.242315181216560038, 5.528084470813009688, 7.813853760409459781 ),
 .UNSPECIFIED. ) ;
#61127 = CARTESIAN_POINT ( 'NONE',  ( -479.3614999999999782, 3.174999999999999822, -1.387778780781445991E-14 ) ) ;
#61128 = DIRECTION ( 'NONE',  ( 1.000000000000000078E-15, -1.000000000000000000, 0.000000000000000000 ) ) ;
#61129 = CARTESIAN_POINT ( 'NONE',  ( 109.4453082753925770, -25.93522777273083335, 175.8918157521009391 ) ) ;
#61130 = LINE ( 'NONE', #39779, #16111 ) ;
#61131 = ORIENTED_EDGE ( 'NONE', *, *, #44415, .T. ) ;
#61132 = CARTESIAN_POINT ( 'NONE',  ( 129.9777455398983079, 79.26455342200333121, -12.27475243032916907 ) ) ;
#61133 = VERTEX_POINT ( 'NONE', #5548 ) ;
#61134 = VECTOR ( 'NONE', #69027, 1000.000000000000227 ) ;
#61135 = EDGE_LOOP ( 'NONE', ( #36220, #60115, #67213, #14093 ) ) ;
#61136 = CARTESIAN_POINT ( 'NONE',  ( 27.27158787008327678, 184.0000000000000000, 90.32146847885336172 ) ) ;
#61137 = ORIENTED_EDGE ( 'NONE', *, *, #71048, .T. ) ;
#61138 = AXIS2_PLACEMENT_3D ( 'NONE', #56580, #16164, #29786 ) ;
#61139 = DIRECTION ( 'NONE',  ( 0.000000000000000000, 0.000000000000000000, -1.000000000000000000 ) ) ;
#61140 = EDGE_CURVE ( 'NONE', #52939, #20535, #8318, .T. ) ;
#61141 = CARTESIAN_POINT ( 'NONE',  ( 97.31591551022792430, -39.30615138698252053, 92.53147369008412682 ) ) ;
#61142 = CARTESIAN_POINT ( 'NONE',  ( 101.6781192058861762, -27.07830111727894362, 105.4937205140069665 ) ) ;
#61143 = CARTESIAN_POINT ( 'NONE',  ( 108.4212764309556150, -26.73551762798052778, 254.9689079379394059 ) ) ;
#61144 = CARTESIAN_POINT ( 'NONE',  ( 172.5664832912729878, -27.57844715994070484, 261.9256252759120116 ) ) ;
#61145 = LINE ( 'NONE', #26626, #54329 ) ;
#61148 = CARTESIAN_POINT ( 'NONE',  ( 96.16101635903912381, -35.07578045570940617, 217.1946728949589840 ) ) ;
#61147 = CYLINDRICAL_SURFACE ( 'NONE', #54262, 7.874000000000005883 ) ;
#61146 = CARTESIAN_POINT ( 'NONE',  ( 172.5664832912729878, -27.82844715994070484, 78.92562527591199739 ) ) ;
#61149 = DIRECTION ( 'NONE',  ( 1.000000000000000000, 0.000000000000000000, 0.000000000000000000 ) ) ;
#61150 = DIRECTION ( 'NONE',  ( 0.000000000000000000, 0.000000000000000000, -1.000000000000000000 ) ) ;
#61151 = ORIENTED_EDGE ( 'NONE', *, *, #61664, .F. ) ;
#61152 = VECTOR ( 'NONE', #68640, 1000.000000000000000 ) ;
#61153 = LINE ( 'NONE', #68871, #80297 ) ;
#61154 = FACE_OUTER_BOUND ( 'NONE', #68986, .T. ) ;
#61155 = DIRECTION ( 'NONE',  ( 0.000000000000000000, 0.000000000000000000, 1.000000000000000000 ) ) ;
#61156 = VECTOR ( 'NONE', #51968, 1000.000000000000000 ) ;
#61157 = DIRECTION ( 'NONE',  ( -1.000000000000000000, -3.999999999999999995E-14, -1.000000000000000078E-15 ) ) ;
#61159 = ORIENTED_EDGE ( 'NONE', *, *, #49083, .F. ) ;
#61158 = CARTESIAN_POINT ( 'NONE',  ( 96.63812674735558517, -35.80421970836195555, 231.2556252759109725 ) ) ;
#61160 = CYLINDRICAL_SURFACE ( 'NONE', #13241, 9.999999999999998224 ) ;
#61161 = CARTESIAN_POINT ( 'NONE',  ( 117.5407444095047111, -36.54548251031545192, 284.8413395616252615 ) ) ;
#61162 = CARTESIAN_POINT ( 'NONE',  ( 112.5087493249093455, -26.14677957921270846, 165.6984824187679521 ) ) ;
#61163 = DIRECTION ( 'NONE',  ( 0.9963424814100680926, -0.08544974978095698503, 0.000000000000000000 ) ) ;
#61164 = DIRECTION ( 'NONE',  ( -0.0001484127182050486030, 0.8660253910675250744, 0.5000000000000052180 ) ) ;
#61166 = CARTESIAN_POINT ( 'NONE',  ( 44.45000000000000284, 66.67499999999999716, 260.3500000000000227 ) ) ;
#61165 = DIRECTION ( 'NONE',  ( -0.8660254037844380415, -0.5000000000000012212, 1.550000000000001284E-14 ) ) ;
#61167 = CARTESIAN_POINT ( 'NONE',  ( 97.31584368502818450, -39.30597587925219472, 191.5314585994741492 ) ) ;
#61168 = DIRECTION ( 'NONE',  ( 1.000000000000000000, 4.163336342344333240E-14, 0.000000000000000000 ) ) ;
#61169 = ORIENTED_EDGE ( 'NONE', *, *, #72063, .F. ) ;
#61170 = ORIENTED_EDGE ( 'NONE', *, *, #75379, .F. ) ;
#61171 = ORIENTED_EDGE ( 'NONE', *, *, #67623, .T. ) ;
#61172 = EDGE_CURVE ( 'NONE', #16001, #65247, #54706, .T. ) ;
#61173 = AXIS2_PLACEMENT_3D ( 'NONE', #57247, #9570, #85449 ) ;
#61174 = VERTEX_POINT ( 'NONE', #5087 ) ;
#61175 = DIRECTION ( 'NONE',  ( -1.000000000000000078E-15, 1.000000000000000083E-30, 1.000000000000000000 ) ) ;
#61176 = CARTESIAN_POINT ( 'NONE',  ( 100.4929927897290582, -27.87207479535962662, 31.59657765686396758 ) ) ;
#61177 = CARTESIAN_POINT ( 'NONE',  ( 70.05589428573307487, -139.0036297784914723, 247.5065103411480152 ) ) ;
#61178 = EDGE_CURVE ( 'NONE', #45388, #23016, #25684, .T. ) ;
#61179 = CARTESIAN_POINT ( 'NONE',  ( 145.3881220512730295, -139.2530407526492127, 246.1986748867973347 ) ) ;
#61180 = LINE ( 'NONE', #59824, #56952 ) ;
#61181 = CARTESIAN_POINT ( 'NONE',  ( 116.0578256703656308, -35.64850657512946697, 238.3562293518859576 ) ) ;
#61182 = ORIENTED_EDGE ( 'NONE', *, *, #72938, .F. ) ;
#61183 = ORIENTED_EDGE ( 'NONE', *, *, #71273, .F. ) ;
#61184 = ORIENTED_EDGE ( 'NONE', *, *, #17987, .T. ) ;
#61185 = VECTOR ( 'NONE', #17998, 1000.000000000000000 ) ;
#61186 = DIRECTION ( 'NONE',  ( 0.000000000000000000, 1.000000000000000000, 0.000000000000000000 ) ) ;
#61187 = CARTESIAN_POINT ( 'NONE',  ( 98.38058909753313230, -41.69556604885146101, 101.7401552394820214 ) ) ;
#61188 = DIRECTION ( 'NONE',  ( 0.000000000000000000, 1.000000000000000000, 0.000000000000000000 ) ) ;
#61189 = CARTESIAN_POINT ( 'NONE',  ( 167.7413838386819691, -48.33240602328260849, 129.9678068554150059 ) ) ;
#61190 = CARTESIAN_POINT ( 'NONE',  ( 100.4594818976507753, -42.68004899263244312, 53.34158330589694685 ) ) ;
#61191 = CARTESIAN_POINT ( 'NONE',  ( 49.21437657594919557, -35.91149509761192604, 117.4678068554150485 ) ) ;
#61192 = EDGE_CURVE ( 'NONE', #71209, #26208, #11228, .T. ) ;
#61193 = CARTESIAN_POINT ( 'NONE',  ( 98.34939355853579457, -31.65741951873318172, 175.9065341848446451 ) ) ;
#61194 = EDGE_CURVE ( 'NONE', #22726, #28809, #62337, .T. ) ;
#61195 = CARTESIAN_POINT ( 'NONE',  ( 117.9377692877172450, -39.05906590213767515, 258.6584824187686422 ) ) ;
#61196 = CARTESIAN_POINT ( 'NONE',  ( 156.5667039024483813, -48.82844715993569196, 257.2178068554149490 ) ) ;
#61198 = VERTEX_POINT ( 'NONE', #55893 ) ;
#61197 = AXIS2_PLACEMENT_3D ( 'NONE', #24459, #72164, #9939 ) ;
#61199 = CARTESIAN_POINT ( 'NONE',  ( 33.91903122894529332, -35.91149509761239500, 313.9678068554150059 ) ) ;
#61200 = PLANE ( 'NONE',  #80090 ) ;
#61201 = CARTESIAN_POINT ( 'NONE',  ( 112.0721450080970669, -44.54221119967598241, 65.84809036959194373 ) ) ;
#61202 = AXIS2_PLACEMENT_3D ( 'NONE', #42169, #6768, #34468 ) ;
#61203 = AXIS2_PLACEMENT_3D ( 'NONE', #78026, #71210, #36685 ) ;
#61204 = CARTESIAN_POINT ( 'NONE',  ( 97.80798641811291816, -40.50837052410136607, 131.6348463817457457 ) ) ;
#61205 = DIRECTION ( 'NONE',  ( 0.000000000000000000, 0.000000000000000000, 1.000000000000000000 ) ) ;
#61206 = VECTOR ( 'NONE', #22186, 1000.000000000000000 ) ;
#61207 = DIRECTION ( 'NONE',  ( -1.000000000000000000, 1.011922027653136551E-15, 0.000000000000000000 ) ) ;
#61208 = VERTEX_POINT ( 'NONE', #21413 ) ;
#61209 = CARTESIAN_POINT ( 'NONE',  ( 107.0664832912750057, -36.72944715993903486, 6.826283056785790393 ) ) ;
#61210 = ORIENTED_EDGE ( 'NONE', *, *, #12054, .F. ) ;
#61211 = CARTESIAN_POINT ( 'NONE',  ( 114.0810491752689160, -44.48971597834975000, 133.1613395616249989 ) ) ;
#61212 = ORIENTED_EDGE ( 'NONE', *, *, #1209, .F. ) ;
#61214 = AXIS2_PLACEMENT_3D ( 'NONE', #67859, #52838, #13352 ) ;
#61213 = CARTESIAN_POINT ( 'NONE',  ( 114.9386757252747771, -33.34113070369811993, 78.57241982807700253 ) ) ;
#61215 = CARTESIAN_POINT ( 'NONE',  ( 182.5667039024477276, -33.35206098992156853, 237.4678068554150059 ) ) ;
#61216 = CARTESIAN_POINT ( 'NONE',  ( 97.68334685095105385, -37.21243378447991290, 117.8111071154209526 ) ) ;
#61217 = AXIS2_PLACEMENT_3D ( 'NONE', #36664, #50723, #71191 ) ;
#61218 = DIRECTION ( 'NONE',  ( -1.092739197465703932E-16, 1.000000000000000000, 0.000000000000000000 ) ) ;
#61219 = DIRECTION ( 'NONE',  ( 0.000000000000000000, 0.000000000000000000, -1.000000000000000000 ) ) ;
#61220 = CARTESIAN_POINT ( 'NONE',  ( 96.90588099414922851, -39.15831928773680914, 52.51276813305394597 ) ) ;
#61221 = LINE ( 'NONE', #74432, #36724 ) ;
#61222 = CARTESIAN_POINT ( 'NONE',  ( 123.6837132603318707, -22.62993780205705718, 229.5838068554170093 ) ) ;
#61223 = ORIENTED_EDGE ( 'NONE', *, *, #20381, .T. ) ;
#61224 = DIRECTION ( 'NONE',  ( 0.000000000000000000, 0.000000000000000000, -1.000000000000000000 ) ) ;
#61225 = ORIENTED_EDGE ( 'NONE', *, *, #80285, .T. ) ;
#61226 = VERTEX_POINT ( 'NONE', #71365 ) ;
#61227 = EDGE_CURVE ( 'NONE', #24376, #39785, #76369, .T. ) ;
#61228 = DIRECTION ( 'NONE',  ( -3.100000000000000258E-29, 3.100000000000000044E-14, 1.000000000000000000 ) ) ;
#61229 = EDGE_LOOP ( 'NONE', ( #23503, #82771, #31226, #87492 ) ) ;
#61230 = CARTESIAN_POINT ( 'NONE',  ( 99.87094702832891358, -29.26198151734318742, 265.6746728949591443 ) ) ;
#61231 = CARTESIAN_POINT ( 'NONE',  ( 111.8040564975826356, -25.84011059577494152, 130.7499109901969518 ) ) ;
#61232 = DIRECTION ( 'NONE',  ( 0.000000000000000000, 0.000000000000000000, -1.000000000000000000 ) ) ;
#61233 = DIRECTION ( 'NONE',  ( 0.000000000000000000, 1.000000000000000000, 0.000000000000000000 ) ) ;
#61234 = CARTESIAN_POINT ( 'NONE',  ( 96.08760325403525826, -38.00935872415581684, 82.43086337114895912 ) ) ;
#61235 = LINE ( 'NONE', #82161, #24786 ) ;
#61236 = ORIENTED_EDGE ( 'NONE', *, *, #12427, .T. ) ;
#61237 = DIRECTION ( 'NONE',  ( 0.7071067811865487940, -0.7071067811865463515, 0.000000000000000000 ) ) ;
#61238 = DIRECTION ( 'NONE',  ( 0.000000000000000000, 0.000000000000000000, 1.000000000000000000 ) ) ;
#61239 = VECTOR ( 'NONE', #47972, 1000.000000000000000 ) ;
#61240 = ORIENTED_EDGE ( 'NONE', *, *, #10978, .T. ) ;
#61241 = CIRCLE ( 'NONE', #88828, 7.143750000000004263 ) ;
#61242 = LINE ( 'NONE', #27176, #15611 ) ;
#61243 = EDGE_CURVE ( 'NONE', #35189, #7001, #64536, .T. ) ;
#61244 = CARTESIAN_POINT ( 'NONE',  ( 41.56648329127499153, -32.07844715994070839, 258.9256252759120116 ) ) ;
#61245 = CARTESIAN_POINT ( 'NONE',  ( 101.0991643652557173, -45.25116564454923207, 282.0899109901967563 ) ) ;
#61246 = CARTESIAN_POINT ( 'NONE',  ( 179.1667039024460166, -28.27351298637280408, -5.074374724088000832 ) ) ;
#61247 = DIRECTION ( 'NONE',  ( 0.000000000000000000, 0.000000000000000000, -1.000000000000000000 ) ) ;
#61248 = DIRECTION ( 'NONE',  ( 4.299999999999999979E-14, -1.000000000000000000, 4.400000000000000367E-29 ) ) ;
#61249 = CARTESIAN_POINT ( 'NONE',  ( 97.30224646447496184, -33.23681714893609751, 26.06514908543594444 ) ) ;
#61251 = CARTESIAN_POINT ( 'NONE',  ( 113.9025887763447997, -28.07314977735667938, 120.5565776568639507 ) ) ;
#61250 = DIRECTION ( 'NONE',  ( 1.000000000000000000, 1.000000000000000078E-15, 0.000000000000000000 ) ) ;
#61252 = DIRECTION ( 'NONE',  ( 6.982966722218760189E-15, 0.000000000000000000, 1.000000000000000000 ) ) ;
#61253 = CARTESIAN_POINT ( 'NONE',  ( 108.9531560784502915, -26.39541311287850434, 164.9327681330529742 ) ) ;
#61254 = ORIENTED_EDGE ( 'NONE', *, *, #32946, .F. ) ;
#61255 = DIRECTION ( 'NONE',  ( 1.000000000000000078E-15, -1.000000000000000083E-30, -1.000000000000000000 ) ) ;
#61256 = EDGE_LOOP ( 'NONE', ( #63906, #61964, #3021, #4872, #40027, #16319 ) ) ;
#61257 = DIRECTION ( 'NONE',  ( 0.000000000000000000, 1.000000000000000000, 0.000000000000000000 ) ) ;
#61258 = DIRECTION ( 'NONE',  ( 0.000000000000000000, 0.000000000000000000, -1.000000000000000000 ) ) ;
#61259 = VERTEX_POINT ( 'NONE', #1866 ) ;
#61260 = EDGE_CURVE ( 'NONE', #22549, #72980, #15944, .T. ) ;
#61261 = AXIS2_PLACEMENT_3D ( 'NONE', #54356, #6251, #74393 ) ;
#61262 = EDGE_CURVE ( 'NONE', #89527, #63276, #40197, .T. ) ;
#61263 = CARTESIAN_POINT ( 'NONE',  ( 99.09656185782638715, -30.54930221101325927, 61.80248345295675705 ) ) ;
#61265 = ORIENTED_EDGE ( 'NONE', *, *, #79757, .T. ) ;
#61264 = CARTESIAN_POINT ( 'NONE',  ( 111.8142338872566626, -25.81671781287135303, 134.7499109901969518 ) ) ;
#61266 = LINE ( 'NONE', #88549, #40775 ) ;
#61267 = CARTESIAN_POINT ( 'NONE',  ( 107.0664832912750057, -36.72944715993903486, 0.4256252759109709349 ) ) ;
#61268 = DIRECTION ( 'NONE',  ( 5.512527431108029424E-15, -1.000000000000000000, 0.000000000000000000 ) ) ;
#61269 = DIRECTION ( 'NONE',  ( 0.000000000000000000, 0.000000000000000000, 1.000000000000000000 ) ) ;
#61270 = VERTEX_POINT ( 'NONE', #70459 ) ;
#61271 = VECTOR ( 'NONE', #46028, 1000.000000000000000 ) ;
#61272 = EDGE_CURVE ( 'NONE', #77176, #38542, #43621, .T. ) ;
#61273 = ORIENTED_EDGE ( 'NONE', *, *, #53565, .F. ) ;
#61274 = VERTEX_POINT ( 'NONE', #49084 ) ;
#61275 = AXIS2_PLACEMENT_3D ( 'NONE', #72010, #85651, #25177 ) ;
#61276 = EDGE_LOOP ( 'NONE', ( #46538, #13830, #7617, #62354 ) ) ;
#61277 = DIRECTION ( 'NONE',  ( -0.7071067811865376918, 0.7071067811865574537, -9.811119821538231114E-14 ) ) ;
#61278 = CARTESIAN_POINT ( 'NONE',  ( 112.8677825012601375, -28.59025478454122648, 249.5838084826162913 ) ) ;
#61279 = CARTESIAN_POINT ( 'NONE',  ( 179.4595971212720258, -26.00627455219131789, -5.074374724088000832 ) ) ;
#61280 = EDGE_CURVE ( 'NONE', #37453, #8408, #76817, .T. ) ;
#61281 = CARTESIAN_POINT ( 'NONE',  ( -148.0533267522752112, 0.000000000000000000, 160.2664750769289697 ) ) ;
#61283 = LINE ( 'NONE', #6328, #80494 ) ;
#61282 = CARTESIAN_POINT ( 'NONE',  ( 263.3306968374159851, 52.73749999999999716, 10.66800000000000104 ) ) ;
#61284 = CARTESIAN_POINT ( 'NONE',  ( 99.09554038107577867, -30.55064579012594450, 180.8023132925306129 ) ) ;
#61285 = ORIENTED_EDGE ( 'NONE', *, *, #19115, .T. ) ;
#61286 = CYLINDRICAL_SURFACE ( 'NONE', #65949, 2.500000000000002220 ) ;
#61287 = DIRECTION ( 'NONE',  ( 0.000000000000000000, -1.000000000000000000, 0.000000000000000000 ) ) ;
#61288 = CARTESIAN_POINT ( 'NONE',  ( 109.9476544338203041, -26.76763818355061986, 210.8403871806729626 ) ) ;
#61290 = EDGE_LOOP ( 'NONE', ( #33823, #68610, #49488, #37454 ) ) ;
#61289 = DIRECTION ( 'NONE',  ( 0.4999999999999998335, 0.8660254037844387076, -2.684678751731758400E-14 ) ) ;
#61291 = EDGE_CURVE ( 'NONE', #33391, #81541, #30018, .T. ) ;
#61292 = VECTOR ( 'NONE', #1312, 1000.000000000000000 ) ;
#61293 = CARTESIAN_POINT ( 'NONE',  ( 96.20363159075265003, -34.36081134307599427, 102.1556252759109640 ) ) ;
#61295 = EDGE_CURVE ( 'NONE', #37074, #69509, #35464, .T. ) ;
#61294 = DIRECTION ( 'NONE',  ( 0.000000000000000000, -1.000000000000000000, 0.000000000000000000 ) ) ;
#61296 = DIRECTION ( 'NONE',  ( 0.000000000000000000, 1.000000000000000000, 0.000000000000000000 ) ) ;
#61297 = EDGE_CURVE ( 'NONE', #27267, #56032, #14143, .T. ) ;
#61298 = DIRECTION ( 'NONE',  ( 1.367269734760046851E-14, -1.000000000000000000, 0.000000000000000000 ) ) ;
#61299 = VERTEX_POINT ( 'NONE', #961 ) ;
#61300 = DIRECTION ( 'NONE',  ( 0.000000000000000000, 0.000000000000000000, -1.000000000000000000 ) ) ;
#61301 = EDGE_CURVE ( 'NONE', #32654, #1337, #35920, .T. ) ;
#61302 = ORIENTED_EDGE ( 'NONE', *, *, #19498, .F. ) ;
#61303 = ORIENTED_EDGE ( 'NONE', *, *, #76905, .F. ) ;
#61304 = CARTESIAN_POINT ( 'NONE',  ( 115.3890540380527767, -39.77298043176836018, 214.9787261630399655 ) ) ;
#61305 = AXIS2_PLACEMENT_3D ( 'NONE', #59973, #66805, #87706 ) ;
#61306 = CARTESIAN_POINT ( 'NONE',  ( 99.08970433676087453, -42.79570825176563176, 52.84354550488869506 ) ) ;
#61307 = CARTESIAN_POINT ( 'NONE',  ( -118.3663208563465759, 93.33902940301969409, -6.712516165662615109 ) ) ;
#61308 = CARTESIAN_POINT ( 'NONE',  ( 38.10000000000000142, 69.84999999999999432, 346.9005000000000223 ) ) ;
#61309 = CARTESIAN_POINT ( 'NONE',  ( 165.6738106836047280, -28.98061976758432223, 117.4678068554150485 ) ) ;
#61310 = ORIENTED_EDGE ( 'NONE', *, *, #69193, .T. ) ;
#61311 = DIRECTION ( 'NONE',  ( 0.000000000000000000, -1.000000000000000000, 0.000000000000000000 ) ) ;
#61312 = DIRECTION ( 'NONE',  ( 0.000000000000000000, 0.000000000000000000, -1.000000000000000000 ) ) ;
#61313 = ORIENTED_EDGE ( 'NONE', *, *, #38700, .T. ) ;
#61314 = CARTESIAN_POINT ( 'NONE',  ( 116.5166575185069462, -42.41785904284980546, 278.3832443235298797 ) ) ;
#61315 = VERTEX_POINT ( 'NONE', #84997 ) ;
#61316 = CARTESIAN_POINT ( 'NONE',  ( 106.3397725667592368, -45.35341472531973750, 260.3157094172105417 ) ) ;
#61317 = DIRECTION ( 'NONE',  ( 0.000000000000000000, -1.000000000000000000, 0.000000000000000000 ) ) ;
#61318 = CARTESIAN_POINT ( 'NONE',  ( 103.6907823165633005, -45.90921117331532741, 142.2956252759109645 ) ) ;
#61319 = DIRECTION ( 'NONE',  ( 0.000000000000000000, -1.000000000000000000, 0.000000000000000000 ) ) ;
#61320 = DIRECTION ( 'NONE',  ( -1.000000000000000000, 0.000000000000000000, 0.000000000000000000 ) ) ;
#61321 = DIRECTION ( 'NONE',  ( 1.000000000000000078E-15, 1.000000000000000083E-30, -1.000000000000000000 ) ) ;
#61322 = CARTESIAN_POINT ( 'NONE',  ( 9.818283287276351246, 74.49179306748567342, 130.1865249340722812 ) ) ;
#61323 = CARTESIAN_POINT ( 'NONE',  ( 115.2859307195537326, -30.18890446381676540, 240.3613395616249875 ) ) ;
#61324 = CARTESIAN_POINT ( 'NONE',  ( 19.56648329127303043, -81.37844715994266664, 361.9756252759109998 ) ) ;
#61325 = ORIENTED_EDGE ( 'NONE', *, *, #1705, .T. ) ;
#61326 = CARTESIAN_POINT ( 'NONE',  ( 113.4862441490110427, -46.74931658189198913, 64.02991099019695298 ) ) ;
#61327 = DIRECTION ( 'NONE',  ( -3.999999999999999995E-14, 1.000000000000000000, -4.100000000000000342E-29 ) ) ;
#61328 = ORIENTED_EDGE ( 'NONE', *, *, #48131, .F. ) ;
#61329 = ORIENTED_EDGE ( 'NONE', *, *, #39436, .T. ) ;
#61330 = ORIENTED_EDGE ( 'NONE', *, *, #57384, .F. ) ;
#61331 = VECTOR ( 'NONE', #37034, 1000.000000000000000 ) ;
#61332 = CARTESIAN_POINT ( 'NONE',  ( 97.07201853420016846, -35.37896439202069843, 161.2187929919405178 ) ) ;
#61333 = CARTESIAN_POINT ( 'NONE',  ( 34.96670390244699433, -28.27351298637401200, 237.4678068554150059 ) ) ;
#61334 = LINE ( 'NONE', #467, #88636 ) ;
#61335 = CARTESIAN_POINT ( 'NONE',  ( 19.56670390244796920, -67.87844715994100397, 310.9178068554150514 ) ) ;
#61336 = CARTESIAN_POINT ( 'NONE',  ( 99.71285092336476907, -40.27258376677666263, 169.5023760838769817 ) ) ;
#61337 = CARTESIAN_POINT ( 'NONE',  ( 115.0714481855697926, -30.01693675811307571, 265.3813395616251682 ) ) ;
#61338 = CARTESIAN_POINT ( 'NONE',  ( 101.9928070043063002, -45.44557658641289777, 58.15638151446928106 ) ) ;
#61339 = VERTEX_POINT ( 'NONE', #1421 ) ;
#61340 = CARTESIAN_POINT ( 'NONE',  ( 130.0919229099369545, 88.91113633199481114, 10.99998730946224690 ) ) ;
#61341 = CARTESIAN_POINT ( 'NONE',  ( 134.0664832912740110, -39.47944715994100306, 1.625625275910997480 ) ) ;
#61342 = EDGE_LOOP ( 'NONE', ( #35641, #18757 ) ) ;
#61343 = ORIENTED_EDGE ( 'NONE', *, *, #15771, .F. ) ;
#61344 = CARTESIAN_POINT ( 'NONE',  ( 179.8585841295800094, -30.08671355700241179, 342.9256252759119548 ) ) ;
#61345 = EDGE_CURVE ( 'NONE', #13942, #46554, #78186, .T. ) ;
#61346 = VERTEX_POINT ( 'NONE', #84553 ) ;
#61347 = ORIENTED_EDGE ( 'NONE', *, *, #7965, .F. ) ;
#61348 = DIRECTION ( 'NONE',  ( 0.000000000000000000, 0.000000000000000000, -1.000000000000000000 ) ) ;
#61349 = CARTESIAN_POINT ( 'NONE',  ( 97.06382796133792112, -37.34203019285121883, 16.37521711361123167 ) ) ;
#61350 = EDGE_CURVE ( 'NONE', #65691, #25396, #76455, .T. ) ;
#61351 = CARTESIAN_POINT ( 'NONE',  ( 97.81169409577289287, -40.51741657705139232, 81.63570706759205109 ) ) ;
#61352 = CARTESIAN_POINT ( 'NONE',  ( 194.0371591254572934, -24.89890238294407965, 300.4678068554149490 ) ) ;
#61353 = CARTESIAN_POINT ( 'NONE',  ( 107.5470202762386549, -45.24887850357546171, 152.0438483995049523 ) ) ;
#61354 = CARTESIAN_POINT ( 'NONE',  ( 96.13137017992535505, -38.63632546489608188, 46.45181575210094138 ) ) ;
#61355 = EDGE_LOOP ( 'NONE', ( #81658, #88864, #70822, #38598 ) ) ;
#61356 = CARTESIAN_POINT ( 'NONE',  ( 80.75703168202301185, -80.31070608727497984, 249.3055308415380011 ) ) ;
#61357 = VERTEX_POINT ( 'NONE', #49986 ) ;
#61358 = EDGE_CURVE ( 'NONE', #38912, #25851, #42276, .T. ) ;
#61359 = VECTOR ( 'NONE', #8932, 1000.000000000000000 ) ;
#61360 = LINE ( 'NONE', #26844, #73128 ) ;
#61361 = VERTEX_POINT ( 'NONE', #22310 ) ;
#61362 = EDGE_CURVE ( 'NONE', #59415, #77441, #3974, .T. ) ;
#61363 = EDGE_CURVE ( 'NONE', #28268, #26420, #66327, .T. ) ;
#61364 = DIRECTION ( 'NONE',  ( -0.7071067811865561215, 0.000000000000000000, 0.7071067811865389130 ) ) ;
#61365 = VERTEX_POINT ( 'NONE', #18156 ) ;
#61366 = DIRECTION ( 'NONE',  ( 0.000000000000000000, 1.000000000000000000, 0.000000000000000000 ) ) ;
#61367 = CARTESIAN_POINT ( 'NONE',  ( 5.562599999999999767, 60.82030000000000314, 265.5569999999999595 ) ) ;
#61368 = CARTESIAN_POINT ( 'NONE',  ( 116.9857065628338688, -35.32450652603309038, 133.9383772284687382 ) ) ;
#61369 = ADVANCED_FACE ( 'NONE', ( #80404 ), #9573, .F. ) ;
#61370 = ADVANCED_FACE ( 'NONE', ( #44962 ), #17283, .T. ) ;
#61371 = AXIS2_PLACEMENT_3D ( 'NONE', #11133, #87896, #26119 ) ;
#61372 = DIRECTION ( 'NONE',  ( 0.7071067811868035902, 0.7071067811862914443, 7.071067811868029270E-16 ) ) ;
#61373 = ORIENTED_EDGE ( 'NONE', *, *, #2652, .T. ) ;
#61374 = CARTESIAN_POINT ( 'NONE',  ( 99.96564438395634511, -44.39263518965486099, 46.98133956162592284 ) ) ;
#61375 = CARTESIAN_POINT ( 'NONE',  ( 116.1615364674122333, -29.05539214145830229, 70.38419670448192278 ) ) ;
#61376 = EDGE_CURVE ( 'NONE', #70860, #63937, #88074, .T. ) ;
#61378 = CARTESIAN_POINT ( 'NONE',  ( 76.06670390244805446, -58.72944715994109544, 239.5838068554169809 ) ) ;
#61377 = LINE ( 'NONE', #89101, #78227 ) ;
#61379 = CARTESIAN_POINT ( 'NONE',  ( 63.03715912545735023, -24.42818131006027826, 249.9678068554150343 ) ) ;
#61380 = LINE ( 'NONE', #20953, #78986 ) ;
#61381 = EDGE_LOOP ( 'NONE', ( #30353, #7416, #48426, #3531 ) ) ;
#61382 = DIRECTION ( 'NONE',  ( 0.000000000000000000, 0.000000000000000000, -1.000000000000000000 ) ) ;
#61383 = EDGE_CURVE ( 'NONE', #45687, #42534, #83728, .T. ) ;
#61384 = CARTESIAN_POINT ( 'NONE',  ( 41.56648329127399677, 0.2215528400590013880, 138.9256252759119832 ) ) ;
#61385 = CARTESIAN_POINT ( 'NONE',  ( 31.56670390244800828, -32.29483332968611364, -5.074374724088000832 ) ) ;
#61386 = ORIENTED_EDGE ( 'NONE', *, *, #35212, .F. ) ;
#61387 = CARTESIAN_POINT ( 'NONE',  ( 104.7547631156620014, -46.91734236372032996, 68.39848241876794077 ) ) ;
#61389 = DIRECTION ( 'NONE',  ( 0.000000000000000000, 0.7071067811865401342, 0.7071067811865549002 ) ) ;
#61388 = CARTESIAN_POINT ( 'NONE',  ( 143.5667039024469886, -67.87844715994090450, 222.2178068554179902 ) ) ;
#61390 = CARTESIAN_POINT ( 'NONE',  ( 83.06670390244796920, -58.35344715994099829, 210.8338068554149913 ) ) ;
#61391 = TOROIDAL_SURFACE ( 'NONE', #15053, 11.75000000000000000, 2.125000000000000000 ) ;
#61392 = CIRCLE ( 'NONE', #36721, 4.750000000000004441 ) ;
#61393 = FACE_OUTER_BOUND ( 'NONE', #16719, .T. ) ;
#61394 = VERTEX_POINT ( 'NONE', #4541 ) ;
#61395 = CARTESIAN_POINT ( 'NONE',  ( 98.70071965984716655, -42.85747980491196074, 102.8175300378149899 ) ) ;
#61397 = ORIENTED_EDGE ( 'NONE', *, *, #49788, .T. ) ;
#61396 = CARTESIAN_POINT ( 'NONE',  ( 10.80657803997667443, 89.23705086585235335, 130.1082320863853568 ) ) ;
#61398 = CARTESIAN_POINT ( 'NONE',  ( 96.99990081654259200, -39.35482002063352525, 272.5299109901966972 ) ) ;
#61399 = DIRECTION ( 'NONE',  ( -0.000000000000000000, -0.000000000000000000, -1.000000000000000000 ) ) ;
#61400 = CARTESIAN_POINT ( 'NONE',  ( -24.20305689751608824, 53.97499999999997300, 58.62596543806478877 ) ) ;
#61401 = FACE_OUTER_BOUND ( 'NONE', #42658, .T. ) ;
#61402 = CARTESIAN_POINT ( 'NONE',  ( 112.1393456477353539, -28.01282278493161471, 80.65645860868352202 ) ) ;
#61403 = EDGE_CURVE ( 'NONE', #34565, #55396, #58159, .T. ) ;
#61404 = CARTESIAN_POINT ( 'NONE',  ( 68.97389088270736579, -137.8496454943130800, 247.5170344592769993 ) ) ;
#61405 = CARTESIAN_POINT ( 'NONE',  ( -88.80809839403299577, 70.80031561532533146, 95.69968022530751739 ) ) ;
#61406 = EDGE_CURVE ( 'NONE', #13042, #2833, #58588, .T. ) ;
#61407 = CARTESIAN_POINT ( 'NONE',  ( 116.5994914424366016, -40.81117973626242446, 213.5165776568640013 ) ) ;
#61408 = ORIENTED_EDGE ( 'NONE', *, *, #20287, .F. ) ;
#61409 = EDGE_LOOP ( 'NONE', ( #10923, #17465, #81830, #53980 ) ) ;
#61410 = CARTESIAN_POINT ( 'NONE',  ( 98.99527800849182313, -31.91985561591122078, 127.3425356868499705 ) ) ;
#61411 = CARTESIAN_POINT ( 'NONE',  ( 177.4809174648215162, -48.32844715993478246, 180.4678068554150059 ) ) ;
#61413 = CARTESIAN_POINT ( 'NONE',  ( 107.0667039024468039, -18.72944715994100306, 199.5838068554169809 ) ) ;
#61412 = CARTESIAN_POINT ( 'NONE',  ( 101.6507727546967743, -27.01955209951630010, 251.4813395616246510 ) ) ;
#61414 = VECTOR ( 'NONE', #17284, 1000.000000000000000 ) ;
#61415 = CARTESIAN_POINT ( 'NONE',  ( 97.06670390244701707, -98.59953881414098475, 7.717806855417813416 ) ) ;
#61416 = DIRECTION ( 'NONE',  ( -1.000000000000000000, -4.299999999999999979E-14, -1.000000000000000078E-15 ) ) ;
#61417 = PLANE ( 'NONE',  #6695 ) ;
#61418 = VECTOR ( 'NONE', #5107, 1000.000000000000000 ) ;
#61419 = CYLINDRICAL_SURFACE ( 'NONE', #14456, 4.750000000000000888 ) ;
#61420 = DIRECTION ( 'NONE',  ( 0.000000000000000000, 0.000000000000000000, -1.000000000000000000 ) ) ;
#61421 = CARTESIAN_POINT ( 'NONE',  ( 96.66614461754329568, -36.48121138304695421, 196.3070538473399438 ) ) ;
#61422 = CARTESIAN_POINT ( 'NONE',  ( 172.5664832912740110, -9.303447159940999356, 16.80862527591200006 ) ) ;
#61423 = EDGE_LOOP ( 'NONE', ( #7075, #71185, #81697, #88776 ) ) ;
#61424 = ORIENTED_EDGE ( 'NONE', *, *, #21002, .F. ) ;
#61425 = CARTESIAN_POINT ( 'NONE',  ( -92.90380151375030948, 69.84937019662270075, -91.73035097708769570 ) ) ;
#61426 = CARTESIAN_POINT ( 'NONE',  ( 81.20964327717335607, -21.23067567606010542, 8.021372095558360726 ) ) ;
#61427 = CARTESIAN_POINT ( 'NONE',  ( 116.3265940946004378, -32.93621273019581253, 125.1356252759109680 ) ) ;
#61428 = DIRECTION ( 'NONE',  ( -4.237773401492740281E-14, 1.000000000000000000, 0.000000000000000000 ) ) ;
#61429 = CIRCLE ( 'NONE', #55638, 130.5560000000000116 ) ;
#61430 = CARTESIAN_POINT ( 'NONE',  ( 80.06648329127399677, -8.729447159940999512, 293.6356252759119911 ) ) ;
#61431 = VERTEX_POINT ( 'NONE', #37730 ) ;
#61432 = CARTESIAN_POINT ( 'NONE',  ( 115.7817079743517610, -41.80467255062060161, 63.40624212070690646 ) ) ;
#61433 = CARTESIAN_POINT ( 'NONE',  ( 113.1001805014122255, -45.99085015462044623, 223.0480062282919675 ) ) ;
#61434 = VERTEX_POINT ( 'NONE', #11348 ) ;
#61435 = CARTESIAN_POINT ( 'NONE',  ( 170.2205283966864897, 20.32000000000000028, -71.37400000000000944 ) ) ;
#61436 = PLANE ( 'NONE',  #26071 ) ;
#61437 = DIRECTION ( 'NONE',  ( 0.000000000000000000, 1.000000000000000000, 0.000000000000000000 ) ) ;
#61438 = CARTESIAN_POINT ( 'NONE',  ( 115.7905465638341553, -39.88961339014866070, 21.36809036959191843 ) ) ;
#61439 = CARTESIAN_POINT ( 'NONE',  ( 114.2549023322775383, -45.16142510923258868, 149.1508633711489722 ) ) ;
#61440 = CARTESIAN_POINT ( 'NONE',  ( 182.2300522401172032, -33.89581943343727488, 193.9678068554150059 ) ) ;
#61441 = ORIENTED_EDGE ( 'NONE', *, *, #3798, .T. ) ;
#61442 = DIRECTION ( 'NONE',  ( 0.000000000000000000, 0.000000000000000000, -1.000000000000000000 ) ) ;
#61443 = ADVANCED_FACE ( 'NONE', ( #31341 ), #59031, .F. ) ;
#61444 = CARTESIAN_POINT ( 'NONE',  ( 116.7350617727581721, -39.61171646336399732, 68.59767641480858913 ) ) ;
#61445 = EDGE_LOOP ( 'NONE', ( #47230, #5218, #36889, #68839 ) ) ;
#61446 = ORIENTED_EDGE ( 'NONE', *, *, #80736, .F. ) ;
#61447 = VECTOR ( 'NONE', #40141, 1000.000000000000000 ) ;
#61448 = CARTESIAN_POINT ( 'NONE',  ( 4.087988121205971659, 94.58126409692583536, 118.4861679838275847 ) ) ;
#61449 = ORIENTED_EDGE ( 'NONE', *, *, #74317, .T. ) ;
#61450 = VERTEX_POINT ( 'NONE', #24541 ) ;
#61451 = PLANE ( 'NONE',  #52611 ) ;
#61452 = VECTOR ( 'NONE', #12663, 1000.000000000000114 ) ;
#61453 = ADVANCED_FACE ( 'NONE', ( #85889 ), #16834, .T. ) ;
#61454 = EDGE_CURVE ( 'NONE', #65034, #43695, #76527, .T. ) ;
#61455 = CARTESIAN_POINT ( 'NONE',  ( 115.4237413257435918, -38.49363815508749553, 63.08384839950497991 ) ) ;
#61456 = CARTESIAN_POINT ( 'NONE',  ( 110.7409072761653306, -26.27985149715145496, 254.8194347997204545 ) ) ;
#61457 = EDGE_CURVE ( 'NONE', #19136, #57180, #2617, .T. ) ;
#61458 = CARTESIAN_POINT ( 'NONE',  ( 101.4165038149807003, -45.50681337102575696, 222.1213395616249784 ) ) ;
#61460 = CARTESIAN_POINT ( 'NONE',  ( 104.6539710028519039, -47.49251396406760506, 23.38895860924494841 ) ) ;
#61459 = CARTESIAN_POINT ( 'NONE',  ( 116.3162492855249894, -32.94856389518969308, 154.1356252759109680 ) ) ;
#61461 = CARTESIAN_POINT ( 'NONE',  ( 34.33598329127389803, -36.32844715994140472, 180.4678068554150911 ) ) ;
#61462 = FACE_OUTER_BOUND ( 'NONE', #19554, .T. ) ;
#61463 = ADVANCED_FACE ( 'NONE', ( #73571 ), #10020, .F. ) ;
#61464 = ORIENTED_EDGE ( 'NONE', *, *, #70312, .T. ) ;
#61465 = EDGE_CURVE ( 'NONE', #32614, #9318, #87287, .T. ) ;
#61466 = CARTESIAN_POINT ( 'NONE',  ( 98.87588542518393808, -42.07524381596793006, 101.7870538473399620 ) ) ;
#61467 = CARTESIAN_POINT ( 'NONE',  ( 109.9230826530363743, -46.83843495353658426, 72.79562527591099297 ) ) ;
#61469 = VECTOR ( 'NONE', #15984, 1000.000000000000000 ) ;
#61468 = CARTESIAN_POINT ( 'NONE',  ( 112.6874404347162084, -45.56185944854193792, 263.0270538473394026 ) ) ;
#61470 = VERTEX_POINT ( 'NONE', #6770 ) ;
#61471 = CARTESIAN_POINT ( 'NONE',  ( 116.7954078171858896, -40.57313474401875197, 193.5270538473389479 ) ) ;
#61472 = DIRECTION ( 'NONE',  ( -0.9254794337955620787, -0.3787978585227822492, 0.000000000000000000 ) ) ;
#61473 = VECTOR ( 'NONE', #2991, 1000.000000000000000 ) ;
#61475 = SURFACE_SIDE_STYLE ('',( #40593 ) ) ;
#61474 = AXIS2_PLACEMENT_3D ( 'NONE', #11669, #44828, #65289 ) ;
#61476 = CARTESIAN_POINT ( 'NONE',  ( 108.8575270723005133, -46.65742102077504683, 28.72049499546754703 ) ) ;
#61478 = DIRECTION ( 'NONE',  ( 0.000000000000000000, 0.000000000000000000, -1.000000000000000000 ) ) ;
#61477 = CARTESIAN_POINT ( 'NONE',  ( 114.8786280730279401, -39.65240915455324000, 277.6356252759111953 ) ) ;
#61479 = DIRECTION ( 'NONE',  ( 0.000000000000000000, 0.000000000000000000, 1.000000000000000000 ) ) ;
#61481 = ADVANCED_FACE ( 'NONE', ( #81753, #59926 ), #60379, .F. ) ;
#61480 = CYLINDRICAL_SURFACE ( 'NONE', #77301, 38.10000000000000142 ) ;
#61482 = PLANE ( 'NONE',  #77499 ) ;
#61483 = AXIS2_PLACEMENT_3D ( 'NONE', #22393, #1047, #27848 ) ;
#61484 = CARTESIAN_POINT ( 'NONE',  ( 80.06648329127402519, -36.72944715994107412, -5.074374724089057764 ) ) ;
#61485 = CARTESIAN_POINT ( 'NONE',  ( 57.56670390244722313, -42.82844715994040996, 137.2178068554150911 ) ) ;
#61486 = LINE ( 'NONE', #6100, #84083 ) ;
#61487 = EDGE_CURVE ( 'NONE', #81025, #27593, #75372, .T. ) ;
#61489 = EDGE_LOOP ( 'NONE', ( #40313, #38556, #55449, #11839 ) ) ;
#61488 = CARTESIAN_POINT ( 'NONE',  ( 100.7306467531667096, -29.72269365876263336, 195.5838068554173788 ) ) ;
#61490 = CARTESIAN_POINT ( 'NONE',  ( 142.8698897858160421, -0.9167816978817300289, 361.9756252759100335 ) ) ;
#61491 = CARTESIAN_POINT ( 'NONE',  ( 114.8305014334234642, -29.68612513766509053, 209.4127681330539872 ) ) ;
#61492 = CARTESIAN_POINT ( 'NONE',  ( 116.7955140328789412, -32.98399009599280873, 135.1184824187679396 ) ) ;
#61493 = CARTESIAN_POINT ( 'NONE',  ( 96.20418022731425367, -34.44737123974878301, 257.1737205140064475 ) ) ;
#61494 = CARTESIAN_POINT ( 'NONE',  ( 41.56648329127499153, -32.07844715994070839, 254.1756252759120400 ) ) ;
#61495 = CARTESIAN_POINT ( 'NONE',  ( 172.5664832912740110, -18.82844715994099971, 21.04262527591200183 ) ) ;
#61497 = CARTESIAN_POINT ( 'NONE',  ( 0.000000000000000000, 8.255000000000000782, 0.000000000000000000 ) ) ;
#61496 = CARTESIAN_POINT ( 'NONE',  ( -446.0240000000000009, 14.28750000000026077, 11.11249999999970051 ) ) ;
#61498 = LINE ( 'NONE', #39710, #71187 ) ;
#61499 = CARTESIAN_POINT ( 'NONE',  ( 131.9645448811607480, -20.51222316633629106, 2.376608873918129028 ) ) ;
#61500 = ORIENTED_EDGE ( 'NONE', *, *, #21086, .T. ) ;
#61501 = ORIENTED_EDGE ( 'NONE', *, *, #73675, .F. ) ;
#61502 = CARTESIAN_POINT ( 'NONE',  ( 112.1993679394656453, -43.55657132036190404, 142.5124198280769576 ) ) ;
#61504 = ORIENTED_EDGE ( 'NONE', *, *, #75766, .F. ) ;
#61503 = DIRECTION ( 'NONE',  ( 0.000000000000000000, -0.000000000000000000, 1.000000000000000000 ) ) ;
#61505 = CARTESIAN_POINT ( 'NONE',  ( -31.75000000000000000, 17.78000000000000114, -3.174999999999779998 ) ) ;
#61506 = CARTESIAN_POINT ( 'NONE',  ( 96.05093434719803724, -37.29646042206077539, 117.3794347997199594 ) ) ;
#61507 = CARTESIAN_POINT ( 'NONE',  ( 234.0013031625829854, 52.73749999999999716, -2.032000000000000028 ) ) ;
#61508 = CARTESIAN_POINT ( 'NONE',  ( 103.1875000000000000, 127.0000000000000000, 3.602774393244745134E-13 ) ) ;
#61509 = DIRECTION ( 'NONE',  ( 1.000000000000000000, 4.163336342344333240E-14, 0.000000000000000000 ) ) ;
#61510 = CARTESIAN_POINT ( 'NONE',  ( 105.7154773365650158, -46.72385839300680743, 108.4689586097351395 ) ) ;
#61511 = EDGE_CURVE ( 'NONE', #13876, #79449, #88142, .T. ) ;
#61512 = CARTESIAN_POINT ( 'NONE',  ( 101.5079035968563943, -28.64143341885324290, 50.55562527591095545 ) ) ;
#61513 = ORIENTED_EDGE ( 'NONE', *, *, #42997, .T. ) ;
#61514 = ORIENTED_EDGE ( 'NONE', *, *, #27466, .T. ) ;
#61515 = ORIENTED_EDGE ( 'NONE', *, *, #52340, .T. ) ;
#61516 = CIRCLE ( 'NONE', #58655, 27.99999999999999645 ) ;
#61517 = DIRECTION ( 'NONE',  ( 0.9068632946707805287, -0.4214249218767882055, 8.896017825522093530E-16 ) ) ;
#61519 = CARTESIAN_POINT ( 'NONE',  ( 107.0667039024470313, -104.2784471599412086, 7.717806855417980394 ) ) ;
#61518 = CARTESIAN_POINT ( 'NONE',  ( 107.9488082096507213, -26.98745991040269487, 151.0041967044819557 ) ) ;
#61520 = AXIS2_PLACEMENT_3D ( 'NONE', #18691, #32766, #3722 ) ;
#61521 = FACE_OUTER_BOUND ( 'NONE', #80635, .T. ) ;
#61522 = CARTESIAN_POINT ( 'NONE',  ( 25.56670390244797275, -65.37844715994100397, 173.2178068554149775 ) ) ;
#61523 = CARTESIAN_POINT ( 'NONE',  ( 1.387778780781445676E-14, 223.9999999999999716, 97.27542076772557778 ) ) ;
#61524 = CARTESIAN_POINT ( 'NONE',  ( 31.75000000000000000, 17.78000000000000114, -3.174999999999999822 ) ) ;
#61525 = DIRECTION ( 'NONE',  ( 5.512527431108029424E-15, -1.000000000000000000, 0.000000000000000000 ) ) ;
#61526 = CARTESIAN_POINT ( 'NONE',  ( 101.6894933626719819, -27.09867346898205298, 105.4937205140069665 ) ) ;
#61527 = ORIENTED_EDGE ( 'NONE', *, *, #43555, .F. ) ;
#61528 = ORIENTED_EDGE ( 'NONE', *, *, #32347, .F. ) ;
#61529 = VERTEX_POINT ( 'NONE', #68108 ) ;
#61530 = EDGE_CURVE ( 'NONE', #10583, #22550, #39648, .T. ) ;
#61531 = LINE ( 'NONE', #41531, #933 ) ;
#61532 = DIRECTION ( 'NONE',  ( -0.000000000000000000, 1.000000000000000000, 0.000000000000000000 ) ) ;
#61533 = FACE_OUTER_BOUND ( 'NONE', #59119, .T. ) ;
#61534 = CARTESIAN_POINT ( 'NONE',  ( 114.3355458017429811, -42.49630604348746488, 196.1109475124489450 ) ) ;
#61535 = EDGE_CURVE ( 'NONE', #63584, #52727, #48934, .T. ) ;
#61536 = VECTOR ( 'NONE', #33292, 1000.000000000000000 ) ;
#61537 = CIRCLE ( 'NONE', #9491, 27.99999999999999645 ) ;
#61538 = AXIS2_PLACEMENT_3D ( 'NONE', #80803, #87605, #69848 ) ;
#61539 = AXIS2_PLACEMENT_3D ( 'NONE', #20166, #13787, #26975 ) ;
#61540 = CARTESIAN_POINT ( 'NONE',  ( 98.35006428047149996, -31.65621667114429982, 26.90604011017519781 ) ) ;
#61541 = EDGE_LOOP ( 'NONE', ( #58857, #14853, #76490, #59117 ) ) ;
#61543 = ORIENTED_EDGE ( 'NONE', *, *, #1049, .F. ) ;
#61542 = VERTEX_POINT ( 'NONE', #7671 ) ;
#61544 = DIRECTION ( 'NONE',  ( 0.7071067811865171526, 0.7071067811865779928, 7.071067811865164719E-16 ) ) ;
#61545 = AXIS2_PLACEMENT_3D ( 'NONE', #81624, #19374, #32990 ) ;
#61546 = VECTOR ( 'NONE', #61842, 1000.000000000000114 ) ;
#61547 = FACE_OUTER_BOUND ( 'NONE', #27040, .T. ) ;
#61548 = VERTEX_POINT ( 'NONE', #28097 ) ;
#61549 = EDGE_LOOP ( 'NONE', ( #86055, #48363, #13233, #27643 ) ) ;
#61550 = DIRECTION ( 'NONE',  ( 0.000000000000000000, -1.000000000000000000, 0.000000000000000000 ) ) ;
#61551 = CARTESIAN_POINT ( 'NONE',  ( 114.9810172151485546, -40.71547668563403022, 199.8872975916109453 ) ) ;
#61552 = CARTESIAN_POINT ( 'NONE',  ( 49.35031423293201414, -29.99615139349890569, -5.074374724088000832 ) ) ;
#61553 = CARTESIAN_POINT ( 'NONE',  ( -122.6777674792067643, 73.68547069920268200, 44.66800687705570994 ) ) ;
#61554 = VERTEX_POINT ( 'NONE', #49431 ) ;
#61555 = EDGE_LOOP ( 'NONE', ( #27306, #8467, #42065, #32829 ) ) ;
#61556 = DIRECTION ( 'NONE',  ( 0.000000000000000000, 1.000000000000000000, 0.000000000000000000 ) ) ;
#61557 = VERTEX_POINT ( 'NONE', #27664 ) ;
#61558 = ORIENTED_EDGE ( 'NONE', *, *, #44066, .F. ) ;
#61559 = EDGE_CURVE ( 'NONE', #40068, #5885, #40274, .T. ) ;
#61560 = EDGE_CURVE ( 'NONE', #462, #70290, #84444, .T. ) ;
#61561 = CARTESIAN_POINT ( 'NONE',  ( 113.6834210241909346, -31.15118039646248249, 222.1899951314959480 ) ) ;
#61562 = CARTESIAN_POINT ( 'NONE',  ( 102.6883137591737665, -46.90427260131782106, 137.2651490854349561 ) ) ;
#61563 = EDGE_CURVE ( 'NONE', #88639, #26855, #83530, .T. ) ;
#61564 = CARTESIAN_POINT ( 'NONE',  ( 107.8666756518570935, -26.35696637107986717, 70.01562527591099183 ) ) ;
#61565 = CARTESIAN_POINT ( 'NONE',  ( 114.4593534627794895, -41.96027977772990170, 249.5838068554169809 ) ) ;
#61566 = FACE_OUTER_BOUND ( 'NONE', #27789, .T. ) ;
#61567 = CARTESIAN_POINT ( 'NONE',  ( 95.40797249125856183, -38.85400393358575855, 197.4699109901969791 ) ) ;
#61568 = DIRECTION ( 'NONE',  ( 1.000000000000000000, 4.163336342344333240E-14, 0.000000000000000000 ) ) ;
#61569 = EDGE_LOOP ( 'NONE', ( #27819, #8927 ) ) ;
#61570 = CARTESIAN_POINT ( 'NONE',  ( -129.9681746291968238, 79.66695435136418268, 12.37535028237962642 ) ) ;
#61571 = ORIENTED_EDGE ( 'NONE', *, *, #55245, .F. ) ;
#61572 = ADVANCED_FACE ( 'NONE', ( #21300 ), #62628, .F. ) ;
#61573 = ORIENTED_EDGE ( 'NONE', *, *, #44463, .F. ) ;
#61574 = DIRECTION ( 'NONE',  ( 1.000000000000000000, 0.000000000000000000, 0.000000000000000000 ) ) ;
#61575 = ORIENTED_EDGE ( 'NONE', *, *, #55187, .T. ) ;
#61576 = AXIS2_PLACEMENT_3D ( 'NONE', #17721, #4977, #73116 ) ;
#61577 = CARTESIAN_POINT ( 'NONE',  ( 52.06670390244700997, -79.67844715994100113, 55.21780685541800437 ) ) ;
#61578 = CARTESIAN_POINT ( 'NONE',  ( 98.85774631673514534, -43.21346936515602266, 91.85848241876892928 ) ) ;
#61579 = CARTESIAN_POINT ( 'NONE',  ( -4.848965775826784785, 70.81212673990701489, 130.4659219253704237 ) ) ;
#61580 = AXIS2_PLACEMENT_3D ( 'NONE', #32208, #81293, #59906 ) ;
#61581 = CARTESIAN_POINT ( 'NONE',  ( 136.5762189171787782, -35.60488046388145023, 7.068409955839482173 ) ) ;
#61582 = CARTESIAN_POINT ( 'NONE',  ( 51.56670390244899238, -32.29483332968450782, -5.074374724088000832 ) ) ;
#61585 = CARTESIAN_POINT ( 'NONE',  ( 96.14807755961388125, -35.16348456217431107, 222.2251490854349640 ) ) ;
#61584 = FACE_OUTER_BOUND ( 'NONE', #14965, .T. ) ;
#61583 = CARTESIAN_POINT ( 'NONE',  ( 109.6430121229215615, -46.48008673730067386, 143.7814586086184931 ) ) ;
#61586 = CARTESIAN_POINT ( 'NONE',  ( 0.000000000000000000, 2.031999999999865025, 25.39999999999999858 ) ) ;
#61588 = EDGE_CURVE ( 'NONE', #753, #51345, #14496, .T. ) ;
#61587 = CARTESIAN_POINT ( 'NONE',  ( 134.0664832912740110, 0.2215528400590013880, 291.1181252759119502 ) ) ;
#61589 = EDGE_LOOP ( 'NONE', ( #77310, #58321 ) ) ;
#61590 = DIRECTION ( 'NONE',  ( 0.000000000000000000, 0.000000000000000000, -1.000000000000000000 ) ) ;
#61591 = CARTESIAN_POINT ( 'NONE',  ( 182.0667039024469886, -33.35206098992630075, -5.074374724088000832 ) ) ;
#61592 = DIRECTION ( 'NONE',  ( -0.7071067811865573427, -0.7071067811865376918, 0.000000000000000000 ) ) ;
#61593 = DIRECTION ( 'NONE',  ( 0.000000000000000000, 0.000000000000000000, -1.000000000000000000 ) ) ;
#61595 = EDGE_LOOP ( 'NONE', ( #9686, #63502, #1268, #26161, #2892, #19218 ) ) ;
#61594 = CARTESIAN_POINT ( 'NONE',  ( 101.6276731664663089, -45.67517298127779668, 247.1413395616249602 ) ) ;
#61596 = CARTESIAN_POINT ( 'NONE',  ( 109.0243740707360018, -26.89372415866576205, 194.9199838810998529 ) ) ;
#61597 = CARTESIAN_POINT ( 'NONE',  ( 111.7834783340718872, -46.75425468364281301, 283.9146728949586418 ) ) ;
#61598 = CARTESIAN_POINT ( 'NONE',  ( 96.57517526037739231, -36.20937929227457630, 167.2870538473399620 ) ) ;
#61599 = DIRECTION ( 'NONE',  ( 0.000000000000000000, 0.5000000000000012212, -0.8660254037844380415 ) ) ;
#61600 = CYLINDRICAL_SURFACE ( 'NONE', #54746, 2.750000000000002665 ) ;
#61602 = LINE ( 'NONE', #75259, #71815 ) ;
#61601 = CARTESIAN_POINT ( 'NONE',  ( 3.174999999999889688, 24.56180297284579694, -31.75000000000000000 ) ) ;
#61603 = CARTESIAN_POINT ( 'NONE',  ( 97.33784133871502320, -34.07106443143205610, 191.1147919345066555 ) ) ;
#61604 = DIRECTION ( 'NONE',  ( -1.000000000000000000, -8.163404592832032979E-16, 0.000000000000000000 ) ) ;
#61605 = ORIENTED_EDGE ( 'NONE', *, *, #771, .F. ) ;
#61606 = AXIS2_PLACEMENT_3D ( 'NONE', #25027, #3256, #16435 ) ;
#61607 = AXIS2_PLACEMENT_3D ( 'NONE', #9137, #65858, #79074 ) ;
#61608 = AXIS2_PLACEMENT_3D ( 'NONE', #80755, #31692, #59389 ) ;
#61609 = CIRCLE ( 'NONE', #61539, 2.029999999999997140 ) ;
#61610 = ORIENTED_EDGE ( 'NONE', *, *, #3400, .T. ) ;
#61611 = ORIENTED_EDGE ( 'NONE', *, *, #12982, .F. ) ;
#61612 = CIRCLE ( 'NONE', #5015, 1.000000000000000888 ) ;
#61613 = AXIS2_PLACEMENT_3D ( 'NONE', #15965, #10040, #59498 ) ;
#61614 = ORIENTED_EDGE ( 'NONE', *, *, #43533, .T. ) ;
#61615 = CARTESIAN_POINT ( 'NONE',  ( 97.81670390244700286, -68.87844715994096134, 222.2178068554179902 ) ) ;
#61616 = CARTESIAN_POINT ( 'NONE',  ( 97.50674219252222485, -32.62548708300533207, 12.00419670448293985 ) ) ;
#61617 = CARTESIAN_POINT ( 'NONE',  ( 144.0775135191610730, -139.0036297784913870, 247.5065103411480152 ) ) ;
#61618 = CARTESIAN_POINT ( 'NONE',  ( 145.3183308313961675, -139.1845296323008938, 246.4818851000068491 ) ) ;
#61619 = DIRECTION ( 'NONE',  ( 0.000000000000000000, 1.000000000000000000, 0.000000000000000000 ) ) ;
#61620 = EDGE_CURVE ( 'NONE', #1670, #36775, #59123, .T. ) ;
#61621 = CARTESIAN_POINT ( 'NONE',  ( 115.5937312905896022, -36.23733611532740184, 228.2952769709339691 ) ) ;
#61622 = ORIENTED_EDGE ( 'NONE', *, *, #37132, .T. ) ;
#61623 = VERTEX_POINT ( 'NONE', #852 ) ;
#61624 = EDGE_LOOP ( 'NONE', ( #20240, #20490, #2812, #34543 ) ) ;
#61625 = CYLINDRICAL_SURFACE ( 'NONE', #81998, 2.517500000000005844 ) ;
#61626 = CARTESIAN_POINT ( 'NONE',  ( 112.0533716870284593, -45.40352459978532806, 182.9916912538479039 ) ) ;
#61627 = EDGE_CURVE ( 'NONE', #72160, #41798, #35361, .T. ) ;
#61628 = CARTESIAN_POINT ( 'NONE',  ( -186.2398777604659870, 101.5999999999999943, 107.9500000000000028 ) ) ;
#61629 = CIRCLE ( 'NONE', #12303, 2.517499999999998739 ) ;
#61630 = CARTESIAN_POINT ( 'NONE',  ( 2.332952152375709937E-14, 103.1240000000000236, 190.5000000000000000 ) ) ;
#61631 = CYLINDRICAL_SURFACE ( 'NONE', #64753, 2.517500000000000071 ) ;
#61632 = CARTESIAN_POINT ( 'NONE',  ( 97.06112323502817674, -37.99668350201224598, 176.4273135337378449 ) ) ;
#61633 = CARTESIAN_POINT ( 'NONE',  ( 100.5669465097397506, -44.03830869352251653, 266.9984824187685604 ) ) ;
#61634 = LINE ( 'NONE', #42093, #34248 ) ;
#61635 = ORIENTED_EDGE ( 'NONE', *, *, #4776, .F. ) ;
#61636 = DIRECTION ( 'NONE',  ( 1.000000000000000078E-15, -1.000000000000000083E-30, -1.000000000000000000 ) ) ;
#61637 = DIRECTION ( 'NONE',  ( 1.000000000000000000, 4.299999999999999979E-14, 1.000000000000000078E-15 ) ) ;
#61638 = CARTESIAN_POINT ( 'NONE',  ( 102.9084262957273097, -29.13922403623678292, 98.28142370292496821 ) ) ;
#61639 = VECTOR ( 'NONE', #9796, 1000.000000000000000 ) ;
#61640 = EDGE_CURVE ( 'NONE', #78112, #33950, #46085, .T. ) ;
#61641 = VECTOR ( 'NONE', #87087, 1000.000000000000000 ) ;
#61642 = CYLINDRICAL_SURFACE ( 'NONE', #1214, 130.5560000000000116 ) ;
#61643 = CARTESIAN_POINT ( 'NONE',  ( 182.2300522401149863, -33.89581943344511217, -5.074374724088000832 ) ) ;
#61644 = ORIENTED_EDGE ( 'NONE', *, *, #75271, .T. ) ;
#61645 = CARTESIAN_POINT ( 'NONE',  ( 77.33253953643573197, -36.38432368373235448, 6.774690158158751530 ) ) ;
#61646 = VERTEX_POINT ( 'NONE', #71257 ) ;
#61647 = CARTESIAN_POINT ( 'NONE',  ( 103.8073253818723316, -26.82667379764869153, 165.3299109901969643 ) ) ;
#61648 = ORIENTED_EDGE ( 'NONE', *, *, #39043, .F. ) ;
#61649 = PRODUCT_DEFINITION ( 'UNKNOWN', '', #26149, #43264 ) ;
#61650 = PLANE ( 'NONE',  #69267 ) ;
#61651 = CARTESIAN_POINT ( 'NONE',  ( 116.2543158056996333, -38.69420140005939857, 105.1025356868499614 ) ) ;
#61652 = CARTESIAN_POINT ( 'NONE',  ( -47.05885865011399005, 101.2667695899395426, 108.0895340666595672 ) ) ;
#61653 = CARTESIAN_POINT ( 'NONE',  ( 131.8488129342790103, -69.46958951562531581, 247.5788556710219837 ) ) ;
#61654 = CARTESIAN_POINT ( 'NONE',  ( 107.2325526940309288, -25.65435679020650639, 76.07657765686298035 ) ) ;
#61655 = CARTESIAN_POINT ( 'NONE',  ( 48.85858412958099706, -30.08671355700241179, 342.9256252759119548 ) ) ;
#61656 = AXIS2_PLACEMENT_3D ( 'NONE', #69131, #6897, #84118 ) ;
#61657 = EDGE_LOOP ( 'NONE', ( #60657, #60821 ) ) ;
#61658 = CARTESIAN_POINT ( 'NONE',  ( 34.96670390244699433, -28.27351298637401200, 313.9678068554150059 ) ) ;
#61659 = AXIS2_PLACEMENT_3D ( 'NONE', #40289, #53442, #52984 ) ;
#61660 = CIRCLE ( 'NONE', #36983, 118.5560000000000116 ) ;
#61661 = VECTOR ( 'NONE', #16444, 1000.000000000000000 ) ;
#61662 = EDGE_LOOP ( 'NONE', ( #10187, #4836 ) ) ;
#61663 = EDGE_LOOP ( 'NONE', ( #13670, #59081, #26312, #17757 ) ) ;
#61664 = EDGE_CURVE ( 'NONE', #75364, #88639, #15393, .T. ) ;
#61665 = CIRCLE ( 'NONE', #48554, 1.000000000000000888 ) ;
#61666 = CARTESIAN_POINT ( 'NONE',  ( 123.6837132603318707, -20.11243780205705534, 218.0711402470151370 ) ) ;
#61667 = VERTEX_POINT ( 'NONE', #43062 ) ;
#61668 = EDGE_CURVE ( 'NONE', #74810, #24368, #4028, .T. ) ;
#61669 = CARTESIAN_POINT ( 'NONE',  ( 97.63766479707255996, -34.12929003103648284, 251.1127681330543737 ) ) ;
#61670 = CARTESIAN_POINT ( 'NONE',  ( 101.7584646134851596, -45.72734648786122591, 158.1527681330539963 ) ) ;
#61671 = CARTESIAN_POINT ( 'NONE',  ( 194.5667039024485234, -47.82844715993405060, 180.4678068554150343 ) ) ;
#61672 = CARTESIAN_POINT ( 'NONE',  ( 109.7248659254751715, -27.00080518097527360, 140.8647919422406858 ) ) ;
#61673 = EDGE_CURVE ( 'NONE', #11339, #16654, #1308, .T. ) ;
#61674 = CARTESIAN_POINT ( 'NONE',  ( 113.3146854497373965, -28.34009065521201265, 100.5670538473389684 ) ) ;
#61675 = CARTESIAN_POINT ( 'NONE',  ( 144.4532657509292051, -72.54478064608022692, 540.9756252759101471 ) ) ;
#61676 = VERTEX_POINT ( 'NONE', #29462 ) ;
#61677 = LINE ( 'NONE', #19463, #80098 ) ;
#61678 = ADVANCED_FACE ( 'NONE', ( #29016 ), #78074, .F. ) ;
#61679 = CARTESIAN_POINT ( 'NONE',  ( -194.1576000000000022, 20.32000000000000028, -9.525000000000000355 ) ) ;
#61680 = ORIENTED_EDGE ( 'NONE', *, *, #73503, .T. ) ;
#61681 = CARTESIAN_POINT ( 'NONE',  ( 20.56670390244828184, -48.82844715994187368, 300.4678068554150059 ) ) ;
#61682 = FACE_OUTER_BOUND ( 'NONE', #51392, .T. ) ;
#61683 = CARTESIAN_POINT ( 'NONE',  ( 99.41296134609922319, -28.78668791560518514, 265.6746728949588032 ) ) ;
#61684 = FACE_OUTER_BOUND ( 'NONE', #47007, .T. ) ;
#61685 = VECTOR ( 'NONE', #69662, 1000.000000000000000 ) ;
#61686 = CARTESIAN_POINT ( 'NONE',  ( 69.04425121814171007, 92.85005066824639641, 55.64382071430165411 ) ) ;
#61687 = DIRECTION ( 'NONE',  ( -0.000000000000000000, 1.000000000000000000, 0.000000000000000000 ) ) ;
#61688 = CARTESIAN_POINT ( 'NONE',  ( 106.3024736416914493, -26.94527301106431949, 25.13848241876892686 ) ) ;
#61690 = CARTESIAN_POINT ( 'NONE',  ( 104.1140010245780729, -46.70499295924809502, 103.3470538473389411 ) ) ;
#61689 = FACE_OUTER_BOUND ( 'NONE', #37911, .T. ) ;
#61691 = DIRECTION ( 'NONE',  ( 0.000000000000000000, 0.000000000000000000, -1.000000000000000000 ) ) ;
#61692 = CARTESIAN_POINT ( 'NONE',  ( 97.63486134215516188, -41.27380337981261960, 171.6841967044819626 ) ) ;
#61694 = EDGE_CURVE ( 'NONE', #45647, #32225, #27237, .T. ) ;
#61693 = CARTESIAN_POINT ( 'NONE',  ( 3.174999999999889688, 17.78000000000000114, -31.75000000000000000 ) ) ;
#61695 = VERTEX_POINT ( 'NONE', #34918 ) ;
#61696 = CARTESIAN_POINT ( 'NONE',  ( 59.93649209371597664, 82.54999999999999716, -77.89700433585308303 ) ) ;
#61697 = FACE_BOUND ( 'NONE', #88297, .T. ) ;
#61698 = EDGE_CURVE ( 'NONE', #88639, #52430, #22658, .T. ) ;
#61699 = FACE_OUTER_BOUND ( 'NONE', #35016, .T. ) ;
#61700 = ORIENTED_EDGE ( 'NONE', *, *, #7044, .F. ) ;
#61701 = CARTESIAN_POINT ( 'NONE',  ( 97.33808530593822184, -34.07010290169503719, 62.11506100739555336 ) ) ;
#61703 = VERTEX_POINT ( 'NONE', #10787 ) ;
#61702 = CARTESIAN_POINT ( 'NONE',  ( 117.6255004633147507, -33.30599276614662330, 134.0880062282919880 ) ) ;
#61704 = CARTESIAN_POINT ( 'NONE',  ( 41.56648329127499153, -32.07844715994070839, 78.92562527591199739 ) ) ;
#61705 = CARTESIAN_POINT ( 'NONE',  ( -129.9368274816652047, 83.38918798244692709, 12.69999999999955165 ) ) ;
#61706 = CYLINDRICAL_SURFACE ( 'NONE', #24247, 2.116999999999980009 ) ;
#61707 = DIRECTION ( 'NONE',  ( 0.000000000000000000, 0.000000000000000000, 1.000000000000000000 ) ) ;
#61708 = EDGE_LOOP ( 'NONE', ( #73840, #80832 ) ) ;
#61709 = CONTEXT_DEPENDENT_SHAPE_REPRESENTATION ( #57343, #24960 ) ;
#61710 = VECTOR ( 'NONE', #12912, 1000.000000000000000 ) ;
#61711 = ORIENTED_EDGE ( 'NONE', *, *, #49837, .F. ) ;
#61712 = ORIENTED_EDGE ( 'NONE', *, *, #84720, .T. ) ;
#61713 = ORIENTED_EDGE ( 'NONE', *, *, #45674, .T. ) ;
#61714 = DIRECTION ( 'NONE',  ( 0.000000000000000000, 0.000000000000000000, 1.000000000000000000 ) ) ;
#61715 = CARTESIAN_POINT ( 'NONE',  ( 102.6489936009959365, -27.69395558276979941, 250.4388294734751241 ) ) ;
#61716 = CARTESIAN_POINT ( 'NONE',  ( 104.4081005665769624, -46.45808911502702188, 157.3647919348640869 ) ) ;
#61718 = LINE ( 'NONE', #75378, #76144 ) ;
#61717 = DIRECTION ( 'NONE',  ( -0.7071067811865475727, 0.000000000000000000, -0.7071067811865475727 ) ) ;
#61719 = DIRECTION ( 'NONE',  ( 0.000000000000000000, 1.000000000000000000, 0.000000000000000000 ) ) ;
#61720 = ADVANCED_FACE ( 'NONE', ( #2207 ), #21422, .F. ) ;
#61721 = ORIENTED_EDGE ( 'NONE', *, *, #57276, .F. ) ;
#61722 = AXIS2_PLACEMENT_3D ( 'NONE', #81771, #69023, #55801 ) ;
#61723 = ORIENTED_EDGE ( 'NONE', *, *, #4372, .F. ) ;
#61724 = AXIS2_PLACEMENT_3D ( 'NONE', #17849, #58723, #86466 ) ;
#61725 = DIRECTION ( 'NONE',  ( 1.000000000000000000, 0.000000000000000000, 0.000000000000000000 ) ) ;
#61726 = AXIS2_PLACEMENT_3D ( 'NONE', #55402, #466, #62236 ) ;
#61727 = CARTESIAN_POINT ( 'NONE',  ( 154.4532657509292051, -72.54478064608022692, 396.9756252759102040 ) ) ;
#61728 = ADVANCED_FACE ( 'NONE', ( #44860 ), #75093, .T. ) ;
#61729 = CARTESIAN_POINT ( 'NONE',  ( 109.1965444620390286, -27.18343884754229833, 220.9013395616249795 ) ) ;
#61730 = CARTESIAN_POINT ( 'NONE',  ( -446.0240000000000009, 14.28749999999982201, 90.48749999999999716 ) ) ;
#61731 = AXIS2_PLACEMENT_3D ( 'NONE', #29793, #57488, #62955 ) ;
#61732 = CARTESIAN_POINT ( 'NONE',  ( 98.13101841594846064, -32.75189731695859763, 96.99276813305296230 ) ) ;
#61733 = CARTESIAN_POINT ( 'NONE',  ( 110.8561346566681891, -45.98355671804449685, 52.88576822912357756 ) ) ;
#61734 = VECTOR ( 'NONE', #38342, 999.9999999999998863 ) ;
#61735 = CARTESIAN_POINT ( 'NONE',  ( 107.8594798993478747, -26.73948001534716923, 21.01336167101059260 ) ) ;
#61736 = ORIENTED_EDGE ( 'NONE', *, *, #5250, .T. ) ;
#61737 = DIRECTION ( 'NONE',  ( 0.7071067811865449082, 0.7071067811865501263, 7.071067811865448709E-16 ) ) ;
#61738 = ORIENTED_EDGE ( 'NONE', *, *, #40853, .T. ) ;
#61739 = VERTEX_POINT ( 'NONE', #79414 ) ;
#61740 = CIRCLE ( 'NONE', #86416, 4.762500000000002842 ) ;
#61741 = DIRECTION ( 'NONE',  ( 0.000000000000000000, 0.000000000000000000, 1.000000000000000000 ) ) ;
#61742 = CARTESIAN_POINT ( 'NONE',  ( 114.4012193684849734, -41.70236635182605056, 269.7844404487540260 ) ) ;
#61743 = DIRECTION ( 'NONE',  ( 0.7071067811566161820, 0.7071067812164789634, 0.000000000000000000 ) ) ;
#61744 = ADVANCED_FACE ( 'NONE', ( #37620 ), #71697, .T. ) ;
#61745 = DIRECTION ( 'NONE',  ( 1.000000000000000078E-15, -1.000000000000000083E-30, -1.000000000000000000 ) ) ;
#61746 = VECTOR ( 'NONE', #8232, 1000.000000000000000 ) ;
#61747 = CARTESIAN_POINT ( 'NONE',  ( 100.8874677892395084, -44.70022130223561874, 153.0522919331214098 ) ) ;
#61748 = CARTESIAN_POINT ( 'NONE',  ( 80.44338158420812590, -39.47944715994105991, 1.625625275910945300 ) ) ;
#61749 = ORIENTED_EDGE ( 'NONE', *, *, #58407, .F. ) ;
#61750 = CARTESIAN_POINT ( 'NONE',  ( 3.175000000000334666, 8.255000000000000782, 31.75000000000000000 ) ) ;
#61751 = DIRECTION ( 'NONE',  ( 0.000000000000000000, 0.000000000000000000, -1.000000000000000000 ) ) ;
#61752 = EDGE_LOOP ( 'NONE', ( #44296, #33418, #18692, #56073 ) ) ;
#61753 = CARTESIAN_POINT ( 'NONE',  ( 96.92094985624760284, -32.34227964863599425, 61.01372051400599616 ) ) ;
#61754 = ORIENTED_EDGE ( 'NONE', *, *, #40414, .T. ) ;
#61755 = CARTESIAN_POINT ( 'NONE',  ( 99.62303294566419254, -42.26939103296757594, 259.6538046553056915 ) ) ;
#61756 = EDGE_CURVE ( 'NONE', #20396, #72641, #51220, .T. ) ;
#61757 = DIRECTION ( 'NONE',  ( 1.000000000000000078E-15, -1.000000000000000083E-30, -1.000000000000000000 ) ) ;
#61758 = CARTESIAN_POINT ( 'NONE',  ( 107.6167445103326230, -46.48501816386551866, 152.6213395616259731 ) ) ;
#61759 = CARTESIAN_POINT ( 'NONE',  ( 23.05014237293025658, 77.82658263289009426, 303.5238209633477595 ) ) ;
#61760 = LINE ( 'NONE', #47684, #38945 ) ;
#61761 = DIRECTION ( 'NONE',  ( 0.000000000000000000, 0.000000000000000000, -1.000000000000000000 ) ) ;
#61762 = DIRECTION ( 'NONE',  ( -0.000000000000000000, -1.000000000000000000, 0.000000000000000000 ) ) ;
#61763 = CARTESIAN_POINT ( 'NONE',  ( 107.2499990610067329, -24.83081552997016317, 226.0641967044829812 ) ) ;
#61764 = CARTESIAN_POINT ( 'NONE',  ( 91.50010255991666952, 88.17653575778736297, -75.38763434846433142 ) ) ;
#61765 = ORIENTED_EDGE ( 'NONE', *, *, #74070, .T. ) ;
#61766 = ORIENTED_EDGE ( 'NONE', *, *, #53258, .T. ) ;
#61767 = CARTESIAN_POINT ( 'NONE',  ( 99.02072372077822138, -43.42711337151016693, 112.8784824187679732 ) ) ;
#61768 = CARTESIAN_POINT ( 'NONE',  ( 38.10000000000000142, 69.84999999999999432, 358.0130000000000337 ) ) ;
#61769 = AXIS2_PLACEMENT_3D ( 'NONE', #46121, #59758, #32959 ) ;
#61770 = EDGE_CURVE ( 'NONE', #80206, #51938, #65748, .T. ) ;
#61771 = ORIENTED_EDGE ( 'NONE', *, *, #43181, .T. ) ;
#61772 = ORIENTED_EDGE ( 'NONE', *, *, #35992, .T. ) ;
#61773 = ORIENTED_EDGE ( 'NONE', *, *, #52220, .T. ) ;
#61774 = CARTESIAN_POINT ( 'NONE',  ( 163.0822201311030142, 20.32000000000000028, 75.92468371870748456 ) ) ;
#61775 = DIRECTION ( 'NONE',  ( 0.000000000000000000, 0.000000000000000000, 1.000000000000000000 ) ) ;
#61776 = CARTESIAN_POINT ( 'NONE',  ( 59.93649209371435660, 82.54999999999999716, 77.89700433585434780 ) ) ;
#61777 = CARTESIAN_POINT ( 'NONE',  ( 19.56670390244824631, -47.82844715994191631, 300.4678068554150059 ) ) ;
#61778 = EDGE_CURVE ( 'NONE', #41960, #3590, #67829, .T. ) ;
#61779 = CARTESIAN_POINT ( 'NONE',  ( 98.06451646660192978, -38.97900810122609982, 164.3395189410199464 ) ) ;
#61780 = CARTESIAN_POINT ( 'NONE',  ( 95.20664489286731680, -37.33482625718801273, 267.3670538473395482 ) ) ;
#61781 = CARTESIAN_POINT ( 'NONE',  ( 98.15086846876572224, -41.26139812777571336, 57.70070366797900618 ) ) ;
#61782 = ORIENTED_EDGE ( 'NONE', *, *, #22138, .T. ) ;
#61783 = CARTESIAN_POINT ( 'NONE',  ( 130.1467854596290579, 89.94765885072629885, -10.33135106516608204 ) ) ;
#61784 = VECTOR ( 'NONE', #14991, 1000.000000000000000 ) ;
#61785 = DIRECTION ( 'NONE',  ( 0.000000000000000000, 1.000000000000000000, 0.000000000000000000 ) ) ;
#61786 = EDGE_LOOP ( 'NONE', ( #412, #45953, #12099, #63704 ) ) ;
#61787 = EDGE_LOOP ( 'NONE', ( #38183, #59563, #13521, #79265 ) ) ;
#61788 = AXIS2_PLACEMENT_3D ( 'NONE', #39743, #27027, #32038 ) ;
#61789 = CIRCLE ( 'NONE', #21163, 0.5000000000000004441 ) ;
#61790 = CARTESIAN_POINT ( 'NONE',  ( 34.33598329127499227, -36.32844715994100682, -5.074374724088000832 ) ) ;
#61791 = AXIS2_PLACEMENT_3D ( 'NONE', #42747, #28699, #14177 ) ;
#61792 = ORIENTED_EDGE ( 'NONE', *, *, #30825, .F. ) ;
#61793 = ORIENTED_EDGE ( 'NONE', *, *, #6030, .T. ) ;
#61794 = DIRECTION ( 'NONE',  ( 0.000000000000000000, 0.000000000000000000, 1.000000000000000000 ) ) ;
#61795 = CARTESIAN_POINT ( 'NONE',  ( -2.899933897858971488, 70.17843983949715891, -130.5244343740981776 ) ) ;
#61796 = VECTOR ( 'NONE', #55031, 1000.000000000000000 ) ;
#61797 = FACE_OUTER_BOUND ( 'NONE', #1655, .T. ) ;
#61798 = CARTESIAN_POINT ( 'NONE',  ( 138.8167039024479834, -50.82844715994100682, 84.20080685541500998 ) ) ;
#61799 = CARTESIAN_POINT ( 'NONE',  ( 115.3915529780678781, -40.29397869100746021, 212.9390864947429804 ) ) ;
#61800 = CARTESIAN_POINT ( 'NONE',  ( 96.29295924727914269, -41.78513476824832651, 61.67562527591097421 ) ) ;
#61802 = EDGE_CURVE ( 'NONE', #64147, #4701, #11284, .T. ) ;
#61801 = DIRECTION ( 'NONE',  ( -0.7071067811861110330, -0.7071067811869841124, 0.000000000000000000 ) ) ;
#61803 = ORIENTED_EDGE ( 'NONE', *, *, #22841, .F. ) ;
#61804 = EDGE_CURVE ( 'NONE', #15299, #5970, #78965, .T. ) ;
#61805 = CARTESIAN_POINT ( 'NONE',  ( 184.5664832912729878, 15.62155284005731204, 361.9756252759109998 ) ) ;
#61806 = ORIENTED_EDGE ( 'NONE', *, *, #15688, .T. ) ;
#61807 = EDGE_CURVE ( 'NONE', #7823, #53584, #64876, .T. ) ;
#61808 = CARTESIAN_POINT ( 'NONE',  ( -24.20305689751608824, 53.97499999999997300, 74.96110745944689313 ) ) ;
#61809 = EDGE_LOOP ( 'NONE', ( #32279, #43215, #39522, #51768 ) ) ;
#61810 = CARTESIAN_POINT ( 'NONE',  ( 51.34673845256467928, -29.62846900982267329, 117.4678068554150485 ) ) ;
#61811 = EDGE_CURVE ( 'NONE', #21770, #84402, #38843, .T. ) ;
#61812 = CARTESIAN_POINT ( 'NONE',  ( 102.2800657950380696, -137.4712196896787475, 248.4142799812389910 ) ) ;
#61813 = CARTESIAN_POINT ( 'NONE',  ( 110.8659606129244253, -45.97952899714481845, 132.8866131168813354 ) ) ;
#61814 = CIRCLE ( 'NONE', #53096, 2.999999999999929834 ) ;
#61815 = CARTESIAN_POINT ( 'NONE',  ( 107.5667039024470313, -100.3098201933451605, -19.78219314458212708 ) ) ;
#61816 = VERTEX_POINT ( 'NONE', #52543 ) ;
#61817 = CARTESIAN_POINT ( 'NONE',  ( 100.9280588457464489, -46.89575235069233372, 52.14419670448194921 ) ) ;
#61818 = SHAPE_REPRESENTATION_RELATIONSHIP ( 'NONE' , 'NONE' ,  #28740, #44568 ) ;
#61820 = CARTESIAN_POINT ( 'NONE',  ( 88.80809839403359263, 70.80031561532540252, -95.69968022530694896 ) ) ;
#61819 = DIRECTION ( 'NONE',  ( 1.000000000000000000, 4.163336342344333240E-14, 0.000000000000000000 ) ) ;
#61821 = CARTESIAN_POINT ( 'NONE',  ( 62.03715912545639810, -23.42818131006021076, 117.4678068554150485 ) ) ;
#61822 = CARTESIAN_POINT ( 'NONE',  ( 131.9692527705846032, -16.94806367531073832, 2.376725340804930031 ) ) ;
#61823 = ORIENTED_EDGE ( 'NONE', *, *, #81554, .F. ) ;
#61824 = CARTESIAN_POINT ( 'NONE',  ( 97.81262911421374895, -40.51702269960655656, 122.6351715870756323 ) ) ;
#61825 = DIRECTION ( 'NONE',  ( 0.000000000000000000, 1.000000000000000000, 0.000000000000000000 ) ) ;
#61826 = CARTESIAN_POINT ( 'NONE',  ( 6.360060842339565923, 71.54945291875249325, 118.3858484385471286 ) ) ;
#61827 = VERTEX_POINT ( 'NONE', #44404 ) ;
#61828 = CARTESIAN_POINT ( 'NONE',  ( 107.6042626387647090, -26.26092342527675072, 91.03562527591097364 ) ) ;
#61830 = CARTESIAN_POINT ( 'NONE',  ( 143.0664832912740110, -8.729447159940999512, 17.92562527591199739 ) ) ;
#61829 = CARTESIAN_POINT ( 'NONE',  ( 98.04156652576716624, -41.04195827621020243, 171.6811716726206498 ) ) ;
#61831 = DIRECTION ( 'NONE',  ( -4.237773401492740281E-14, 1.000000000000000000, 0.000000000000000000 ) ) ;
#61832 = CARTESIAN_POINT ( 'NONE',  ( 124.0664832912757021, -36.72944715993921960, 14.92562527591098842 ) ) ;
#61833 = VERTEX_POINT ( 'NONE', #31229 ) ;
#61834 = ADVANCED_FACE ( 'NONE', ( #65319 ), #50788, .F. ) ;
#61835 = CARTESIAN_POINT ( 'NONE',  ( 116.9564367646782728, -33.61053620760072391, 125.0575300378159795 ) ) ;
#61837 = EDGE_LOOP ( 'NONE', ( #64477, #22429, #48272, #74418, #80619, #85159 ) ) ;
#61836 = LINE ( 'NONE', #28679, #35556 ) ;
#61838 = CARTESIAN_POINT ( 'NONE',  ( 116.5620552962770802, -42.34175257684895399, 279.4137205140061724 ) ) ;
#61839 = FACE_OUTER_BOUND ( 'NONE', #76268, .T. ) ;
#61840 = DIRECTION ( 'NONE',  ( 1.000000000000000000, 0.000000000000000000, 0.000000000000000000 ) ) ;
#61841 = CARTESIAN_POINT ( 'NONE',  ( -479.3614999999999782, 3.174999999999999822, -1.387778780781445991E-14 ) ) ;
#61842 = DIRECTION ( 'NONE',  ( 0.000000000000000000, -0.5000000000000007772, 0.8660254037844381525 ) ) ;
#61843 = CARTESIAN_POINT ( 'NONE',  ( 7.661254700127844153, 66.45253841614081125, 320.6630000000000109 ) ) ;
#61844 = CARTESIAN_POINT ( 'NONE',  ( -100.8594679592211918, 81.72130195885945625, 82.89895571708260036 ) ) ;
#61845 = VECTOR ( 'NONE', #68939, 1000.000000000000000 ) ;
#61846 = CARTESIAN_POINT ( 'NONE',  ( 97.31640351007376921, -35.61153895465465524, 206.2356252759109623 ) ) ;
#61847 = VERTEX_POINT ( 'NONE', #86663 ) ;
#61848 = ORIENTED_EDGE ( 'NONE', *, *, #82740, .F. ) ;
#61849 = VECTOR ( 'NONE', #30053, 1000.000000000000000 ) ;
#61850 = CARTESIAN_POINT ( 'NONE',  ( 111.3621671965809270, -45.84085784651199447, 134.3587261630399894 ) ) ;
#61851 = VECTOR ( 'NONE', #87088, 1000.000000000000000 ) ;
#61852 = DIRECTION ( 'NONE',  ( 0.7071067811864683028, 0.7071067811866268427, 7.071067811864676611E-16 ) ) ;
#61854 = EDGE_CURVE ( 'NONE', #82640, #9211, #22921, .T. ) ;
#61853 = AXIS2_PLACEMENT_3D ( 'NONE', #80114, #58736, #45992 ) ;
#61856 = CARTESIAN_POINT ( 'NONE',  ( 77.31648329127401098, -36.72944715994107412, 3.101481641215480867 ) ) ;
#61855 = CARTESIAN_POINT ( 'NONE',  ( 98.36824592180721538, -38.57411413555575308, 27.92444044875497156 ) ) ;
#61857 = AXIS2_PLACEMENT_3D ( 'NONE', #81781, #89031, #74052 ) ;
#61858 = DIRECTION ( 'NONE',  ( 1.000000000000000000, 1.261617073437676668E-15, 1.261617073437676668E-15 ) ) ;
#61859 = EDGE_CURVE ( 'NONE', #83766, #78870, #73017, .T. ) ;
#61860 = LINE ( 'NONE', #53687, #72207 ) ;
#61861 = EDGE_CURVE ( 'NONE', #60508, #51043, #18547, .T. ) ;
#61862 = CARTESIAN_POINT ( 'NONE',  ( 97.81168895331838087, -40.51742574516882200, 287.6356252759109680 ) ) ;
#61863 = CARTESIAN_POINT ( 'NONE',  ( -254.0000000000000000, 3.174999999999999822, 142.8750000000000000 ) ) ;
#61864 = LINE ( 'NONE', #56392, #27054 ) ;
#61865 = CARTESIAN_POINT ( 'NONE',  ( 113.0874441278155871, -45.97130050132146550, 223.0480062282919675 ) ) ;
#61866 = DIRECTION ( 'NONE',  ( 0.000000000000000000, 1.000000000000000000, 0.000000000000000000 ) ) ;
#61867 = ORIENTED_EDGE ( 'NONE', *, *, #38525, .T. ) ;
#61868 = ORIENTED_EDGE ( 'NONE', *, *, #4068, .T. ) ;
#61869 = EDGE_CURVE ( 'NONE', #28057, #16260, #66189, .T. ) ;
#61870 = ADVANCED_FACE ( 'NONE', ( #3983 ), #59377, .T. ) ;
#61871 = DIRECTION ( 'NONE',  ( 0.000000000000000000, 0.000000000000000000, -1.000000000000000000 ) ) ;
#61872 = CARTESIAN_POINT ( 'NONE',  ( 82.45326694837569903, -20.09809895854153794, 7.205238605742597890 ) ) ;
#61873 = CARTESIAN_POINT ( 'NONE',  ( 109.7256292845548842, -27.00100760353820206, 184.8651728498700777 ) ) ;
#61874 = CARTESIAN_POINT ( 'NONE',  ( 226.4410000000000025, 65.43750000000000000, -63.94449999999999790 ) ) ;
#61875 = CIRCLE ( 'NONE', #50265, 6.349999999999999645 ) ;
#61876 = ADVANCED_FACE ( 'NONE', ( #36728 ), #27884, .T. ) ;
#61877 = DIRECTION ( 'NONE',  ( -0.7071067811745735954, -0.7071067811985214391, 0.000000000000000000 ) ) ;
#61878 = EDGE_CURVE ( 'NONE', #77969, #30086, #38940, .T. ) ;
#61879 = CLOSED_SHELL ( 'NONE', ( #5843, #61453, #88680, #16379, #43049, #84905, #21487, #61006, #77071, #43508, #30713, #787, #62103, #66129, #69674, #29804, #1709, #35739, #10925, #46988, #26393, #2006, #65220, #69362, #85052, #80568, #69731, #23664, #72, #61085, #87598, #52427, #47921, #83639, #77693, #33088, #87226, #69791, #63529, #26581, #87233, #13789, #60207, #68872, #1848, #48536, #28667, #88378, #82546, #85689, #85119, #4706, #75129, #46165, #6966, #24658, #7595, #44143, #72131, #60324, #62713, #40353, #55802, #63351, #28349, #56787, #54941, #20777, #36174, #80571, #77915, #22523, #47608, #688, #62301, #82223, #24251, #66382, #48447, #72169, #3853, #20467, #8847, #63017, #27654, #88925, #86911, #86678, #49276, #23492, #7245, #86339, #18704, #88030, #79457, #74922, #64486, #83690, #48378, #52518, #17533, #61913, #35033, #73270, #35524, #72568, #24649, #30482, #6341, #70821, #31302, #23565, #4366, #58042, #52003, #31131, #32187, #21440, #68576, #88846, #44651, #86690, #89688, #75855, #6272, #53347, #74586, #55423, #86433, #20655, #7447, #88565, #88346, #32153, #67421, #73476, #55683, #47206, #52631, #27320, #67986, #22700, #32680, #77690, #27522, #37891, #37715, #26923, #36973, #56604, #10321, #67389, #66569, #86299 ) ) ;
#61880 = ORIENTED_EDGE ( 'NONE', *, *, #58090, .F. ) ;
#61881 = CARTESIAN_POINT ( 'NONE',  ( 172.5664832912729878, -27.82844715994070484, 318.9256252759120116 ) ) ;
#61882 = EDGE_CURVE ( 'NONE', #877, #274, #35996, .T. ) ;
#61883 = CARTESIAN_POINT ( 'NONE',  ( 110.6963687344609184, -48.01060035924083280, 207.8241967044819489 ) ) ;
#61884 = ORIENTED_EDGE ( 'NONE', *, *, #12387, .T. ) ;
#61885 = DIRECTION ( 'NONE',  ( 0.000000000000000000, 0.000000000000000000, 1.000000000000000000 ) ) ;
#61886 = EDGE_CURVE ( 'NONE', #63431, #79504, #30245, .T. ) ;
#61887 = FACE_OUTER_BOUND ( 'NONE', #88724, .T. ) ;
#61888 = CARTESIAN_POINT ( 'NONE',  ( 115.0947728502038672, -42.74698383566514082, 168.3144758113602393 ) ) ;
#61889 = EDGE_CURVE ( 'NONE', #28391, #54796, #8463, .T. ) ;
#61890 = CARTESIAN_POINT ( 'NONE',  ( 102.8730905416367278, -29.69395531543277400, 83.32237608387698913 ) ) ;
#61891 = CARTESIAN_POINT ( 'NONE',  ( 98.07189402449054683, -42.11243585264244160, 157.7556252759109725 ) ) ;
#61892 = DIRECTION ( 'NONE',  ( 0.7071067811864907293, 0.7071067811866043051, 7.071067811864901437E-16 ) ) ;
#61893 = ORIENTED_EDGE ( 'NONE', *, *, #50711, .T. ) ;
#61894 = B_SPLINE_CURVE_WITH_KNOTS ( 'NONE', 3,
 ( #14061, #55809, #69930, #13614, #41298, #35386, #14969, #35840, #49457, #28120, #48547, #7697, #83562, #884, #20439, #21329, #77197, #63555 ),
 .UNSPECIFIED., .F., .F.,
 ( 4, 2, 2, 2, 2, 2, 2, 2, 4 ),
 ( 0.4999999979610092460, 0.5624999982158831457, 0.6249999984707569345, 0.6874999987256307232, 0.7499999989805046230, 0.8124999992353785228, 0.8749999994902523115, 0.9374999997451261002, 1.000000000000000000 ),
 .UNSPECIFIED. ) ;
#61895 = DIRECTION ( 'NONE',  ( -1.047445008332813989E-14, 0.000000000000000000, -1.000000000000000000 ) ) ;
#61896 = CARTESIAN_POINT ( 'NONE',  ( 52.65249034007747042, -48.32844715994062312, 129.9678068554150911 ) ) ;
#61897 = ORIENTED_EDGE ( 'NONE', *, *, #26734, .F. ) ;
#61899 = VERTEX_POINT ( 'NONE', #11699 ) ;
#61898 = AXIS2_PLACEMENT_3D ( 'NONE', #67644, #49420, #28086 ) ;
#61900 = DIRECTION ( 'NONE',  ( 0.7071067811865460184, 0.7071067811865489050, 0.000000000000000000 ) ) ;
#61901 = ORIENTED_EDGE ( 'NONE', *, *, #64375, .T. ) ;
#61902 = ORIENTED_EDGE ( 'NONE', *, *, #77395, .T. ) ;
#61903 = DIRECTION ( 'NONE',  ( -1.000000000000000000, 0.000000000000000000, 1.107319919754840046E-14 ) ) ;
#61904 = CARTESIAN_POINT ( 'NONE',  ( 108.2720842404240926, -28.27352272357859420, 104.3867055423629608 ) ) ;
#61905 = CARTESIAN_POINT ( 'NONE',  ( 101.6391055438642894, -45.65636906804281381, 247.1413395616249602 ) ) ;
#61906 = EDGE_CURVE ( 'NONE', #2091, #60004, #76489, .T. ) ;
#61907 = CARTESIAN_POINT ( 'NONE',  ( 117.9257662994440494, -34.79559216868040039, 198.9546728949589749 ) ) ;
#61910 = EDGE_CURVE ( 'NONE', #73841, #54555, #67546, .T. ) ;
#61909 = CARTESIAN_POINT ( 'NONE',  ( 106.2538455105912050, -26.32252419718687619, 21.13848241876792144 ) ) ;
#61908 = PLANE ( 'NONE',  #40286 ) ;
#61911 = DIRECTION ( 'NONE',  ( -1.092739197465703932E-16, 0.000000000000000000, 1.000000000000000000 ) ) ;
#61912 = CARTESIAN_POINT ( 'NONE',  ( 172.5664832912729878, -18.82844715994071194, 195.9256252759120684 ) ) ;
#61913 = ADVANCED_FACE ( 'NONE', ( #74369 ), #46637, .F. ) ;
#61914 = ORIENTED_EDGE ( 'NONE', *, *, #1637, .T. ) ;
#61915 = EDGE_CURVE ( 'NONE', #45031, #22549, #34250, .T. ) ;
#61916 = AXIS2_PLACEMENT_3D ( 'NONE', #58004, #85737, #48925 ) ;
#61917 = CARTESIAN_POINT ( 'NONE',  ( 109.6029845306728419, -46.78454271877410520, 92.78514908543594686 ) ) ;
#61918 = CARTESIAN_POINT ( 'NONE',  ( 117.3971137516355014, -38.63466851614541753, 88.68133956162493803 ) ) ;
#61919 = CARTESIAN_POINT ( 'NONE',  ( 115.7319096639420906, -42.60456859047142331, 273.3527681330537575 ) ) ;
#61920 = EDGE_LOOP ( 'NONE', ( #3492, #50259, #49026, #35300 ) ) ;
#61921 = AXIS2_PLACEMENT_3D ( 'NONE', #62772, #49580, #56398 ) ;
#61922 = CARTESIAN_POINT ( 'NONE',  ( 100.6562259211013384, -44.95110337444964443, 232.0499109901969632 ) ) ;
#61923 = DIRECTION ( 'NONE',  ( 0.000000000000000000, 0.000000000000000000, -1.000000000000000000 ) ) ;
#61924 = CARTESIAN_POINT ( 'NONE',  ( 1.387778780781445676E-14, 239.0000000000000000, 97.27542076772557778 ) ) ;
#61925 = VECTOR ( 'NONE', #331, 1000.000000000000000 ) ;
#61926 = CARTESIAN_POINT ( 'NONE',  ( 117.0720608545349819, -35.46383447611707851, 24.92718395960681477 ) ) ;
#61927 = FACE_OUTER_BOUND ( 'NONE', #323, .T. ) ;
#61929 = CARTESIAN_POINT ( 'NONE',  ( 49.21213752016101495, -29.73316016639650172, -5.074374724088000832 ) ) ;
#61928 = CARTESIAN_POINT ( 'NONE',  ( 115.2527165410365484, -37.46115175898625438, 277.6356252759110248 ) ) ;
#61930 = CARTESIAN_POINT ( 'NONE',  ( 105.7152282706593098, -46.72382676192142981, 173.4689389589050563 ) ) ;
#61931 = CARTESIAN_POINT ( 'NONE',  ( 116.3167039024470029, -67.87844715994093292, 222.2178068554179902 ) ) ;
#61932 = CARTESIAN_POINT ( 'NONE',  ( 12.70000000000000107, 82.54999999999999716, -117.8738102209307641 ) ) ;
#61933 = DIRECTION ( 'NONE',  ( 0.000000000000000000, -1.000000000000000000, 0.000000000000000000 ) ) ;
#61934 = CARTESIAN_POINT ( 'NONE',  ( 108.4095557610607159, -26.73403182108062737, 39.96876094489950759 ) ) ;
#61935 = DIRECTION ( 'NONE',  ( -0.000000000000000000, -1.000000000000000000, -0.000000000000000000 ) ) ;
#61937 = ORIENTED_EDGE ( 'NONE', *, *, #33511, .T. ) ;
#61936 = CARTESIAN_POINT ( 'NONE',  ( 109.7248659092072103, -27.00080517620619602, 259.8647919435812241 ) ) ;
#61938 = LINE ( 'NONE', #89671, #13369 ) ;
#61939 = CARTESIAN_POINT ( 'NONE',  ( 118.1050840190196567, -32.34957160481850025, 249.1270538473389706 ) ) ;
#61940 = CARTESIAN_POINT ( 'NONE',  ( 97.61704402414061121, -30.99515748980318719, 121.8803871806729546 ) ) ;
#61941 = CARTESIAN_POINT ( 'NONE',  ( 104.8319786719434603, -26.46567573359534364, 256.2470538473397710 ) ) ;
#61942 = AXIS2_PLACEMENT_3D ( 'NONE', #67451, #61974, #74726 ) ;
#61943 = LINE ( 'NONE', #6992, #69310 ) ;
#61944 = CIRCLE ( 'NONE', #73558, 130.5560000000000116 ) ;
#61946 = DIRECTION ( 'NONE',  ( 0.000000000000000000, 1.000000000000000000, 0.000000000000000000 ) ) ;
#61945 = DIRECTION ( 'NONE',  ( 0.000000000000000000, 0.000000000000000000, -1.000000000000000000 ) ) ;
#61947 = FACE_BOUND ( 'NONE', #2027, .T. ) ;
#61948 = CARTESIAN_POINT ( 'NONE',  ( 51.34673845256598668, -29.62846900982231446, -5.074374724088000832 ) ) ;
#61949 = VECTOR ( 'NONE', #49123, 1000.000000000000000 ) ;
#61950 = ORIENTED_EDGE ( 'NONE', *, *, #75028, .T. ) ;
#61951 = CARTESIAN_POINT ( 'NONE',  ( 75.31670390244798341, -50.82844715994100682, 60.91780685541480267 ) ) ;
#61952 = ORIENTED_EDGE ( 'NONE', *, *, #76090, .T. ) ;
#61953 = CARTESIAN_POINT ( 'NONE',  ( 116.7432888474544370, -37.52321155953265475, 188.1838483995059619 ) ) ;
#61955 = ORIENTED_EDGE ( 'NONE', *, *, #11132, .T. ) ;
#61954 = DIRECTION ( 'NONE',  ( 0.000000000000000000, -0.8660254037844394848, 0.4999999999999986122 ) ) ;
#61956 = DIRECTION ( 'NONE',  ( -1.000000000000000078E-15, 0.000000000000000000, -1.000000000000000000 ) ) ;
#61957 = CARTESIAN_POINT ( 'NONE',  ( 117.2701380961605651, -34.52720868313124924, 179.9956252759109532 ) ) ;
#61958 = CARTESIAN_POINT ( 'NONE',  ( 48.16670390244701139, -28.27351298637280408, -5.074374724088000832 ) ) ;
#61959 = CARTESIAN_POINT ( 'NONE',  ( 142.8821648370248170, -72.54478064608022692, 396.9756252759102040 ) ) ;
#61960 = CARTESIAN_POINT ( 'NONE',  ( -88.90442867305931429, 72.22378176823141871, 78.43243611888119915 ) ) ;
#61961 = DIRECTION ( 'NONE',  ( -4.012088370409549976E-14, 1.000000000000000000, 0.000000000000000000 ) ) ;
#61962 = CARTESIAN_POINT ( 'NONE',  ( 104.3903674582245742, -25.93822912171379969, 90.26991099019693365 ) ) ;
#61963 = ORIENTED_EDGE ( 'NONE', *, *, #28511, .T. ) ;
#61964 = ORIENTED_EDGE ( 'NONE', *, *, #5802, .T. ) ;
#61966 = EDGE_LOOP ( 'NONE', ( #27901, #46178, #54047 ) ) ;
#61965 = VECTOR ( 'NONE', #25191, 1000.000000000000000 ) ;
#61967 = DIRECTION ( 'NONE',  ( 0.000000000000000000, -1.000000000000000000, 0.000000000000000000 ) ) ;
#61969 = DIRECTION ( 'NONE',  ( 3.100000000000000258E-29, -3.100000000000000044E-14, -1.000000000000000000 ) ) ;
#61968 = CARTESIAN_POINT ( 'NONE',  ( 116.1939227058877719, -40.33550099034467706, 189.5270538473389479 ) ) ;
#61970 = FACE_BOUND ( 'NONE', #46177, .T. ) ;
#61971 = EDGE_CURVE ( 'NONE', #86897, #73831, #28737, .T. ) ;
#61972 = DIRECTION ( 'NONE',  ( 0.000000000000000000, 1.000000000000000000, 0.000000000000000000 ) ) ;
#61973 = EDGE_CURVE ( 'NONE', #56977, #78258, #5536, .T. ) ;
#61974 = DIRECTION ( 'NONE',  ( -0.000000000000000000, -0.000000000000000000, 1.000000000000000000 ) ) ;
#61975 = EDGE_CURVE ( 'NONE', #33837, #11800, #4094, .T. ) ;
#61976 = DIRECTION ( 'NONE',  ( -1.000000000000000000, -4.554376769437570034E-14, 0.000000000000000000 ) ) ;
#61977 = CARTESIAN_POINT ( 'NONE',  ( 67.21995684885473565, -68.02541542198279956, 246.2600046646611816 ) ) ;
#61978 = CARTESIAN_POINT ( 'NONE',  ( 117.4257108620838181, -37.68603989742254612, 78.75276813305399060 ) ) ;
#61979 = ORIENTED_EDGE ( 'NONE', *, *, #71881, .T. ) ;
#61980 = ORIENTED_EDGE ( 'NONE', *, *, #41349, .F. ) ;
#61981 = ORIENTED_EDGE ( 'NONE', *, *, #59934, .F. ) ;
#61982 = EDGE_CURVE ( 'NONE', #71592, #82044, #62847, .T. ) ;
#61983 = CARTESIAN_POINT ( 'NONE',  ( 63.06670390244799052, -40.32844715994017548, 249.9678068554150343 ) ) ;
#61984 = CARTESIAN_POINT ( 'NONE',  ( -90.83954799657452384, 95.08644067748866746, -93.77212533081383583 ) ) ;
#61985 = AXIS2_PLACEMENT_3D ( 'NONE', #52051, #67050, #65703 ) ;
#61986 = PLANE ( 'NONE',  #19255 ) ;
#61987 = CARTESIAN_POINT ( 'NONE',  ( 103.8567473457716375, -28.69212669812176841, 173.2090427505439720 ) ) ;
#61988 = EDGE_CURVE ( 'NONE', #76086, #23079, #55114, .T. ) ;
#61989 = VECTOR ( 'NONE', #35020, 1000.000000000000000 ) ;
#61990 =( REPRESENTATION_RELATIONSHIP ('NONE','NONE', #82876, #47290 ) REPRESENTATION_RELATIONSHIP_WITH_TRANSFORMATION ( #20843 )SHAPE_REPRESENTATION_RELATIONSHIP( ) );
#61991 = CONICAL_SURFACE ( 'NONE', #83731, 14.49999999999997158, 0.7853981633974743692 ) ;
#61992 = VECTOR ( 'NONE', #80227, 1000.000000000000000 ) ;
#61993 = EDGE_CURVE ( 'NONE', #34396, #64746, #11355, .T. ) ;
#61994 = LINE ( 'NONE', #13857, #77975 ) ;
#61995 = ORIENTED_EDGE ( 'NONE', *, *, #51724, .T. ) ;
#61997 = VERTEX_POINT ( 'NONE', #32123 ) ;
#61996 = VERTEX_POINT ( 'NONE', #83765 ) ;
#61998 = CARTESIAN_POINT ( 'NONE',  ( 136.3243469132239909, -20.30306751043745450, 2.518077574358949189 ) ) ;
#61999 = ORIENTED_EDGE ( 'NONE', *, *, #2024, .F. ) ;
#62000 = ORIENTED_EDGE ( 'NONE', *, *, #67452, .T. ) ;
#62001 = DIRECTION ( 'NONE',  ( -1.000000000000000000, 0.000000000000000000, 0.000000000000000000 ) ) ;
#62002 = EDGE_CURVE ( 'NONE', #68541, #81147, #20637, .T. ) ;
#62003 = CARTESIAN_POINT ( 'NONE',  ( 101.7809741706781921, -43.87965855000975068, 253.5015833058971850 ) ) ;
#62004 = VERTEX_POINT ( 'NONE', #66647 ) ;
#62005 = CIRCLE ( 'NONE', #75110, 2.750000000000002665 ) ;
#62006 = VECTOR ( 'NONE', #69863, 1000.000000000000000 ) ;
#62007 = CARTESIAN_POINT ( 'NONE',  ( 97.81168843500762478, -40.51741166756562507, 12.63579318495451176 ) ) ;
#62008 = EDGE_CURVE ( 'NONE', #79518, #52915, #4436, .T. ) ;
#62009 = CARTESIAN_POINT ( 'NONE',  ( -124.9130890353168581, 70.14308647312734024, 37.96932838610722882 ) ) ;
#62010 = ORIENTED_EDGE ( 'NONE', *, *, #26769, .T. ) ;
#62011 = VERTEX_POINT ( 'NONE', #80742 ) ;
#62012 = AXIS2_PLACEMENT_3D ( 'NONE', #24891, #77742, #84569 ) ;
#62013 = DIRECTION ( 'NONE',  ( -8.465970413060558704E-17, 0.000000000000000000, 1.000000000000000000 ) ) ;
#62014 = EDGE_LOOP ( 'NONE', ( #85336, #82894, #12304, #63227, #1348 ) ) ;
#62015 = VERTEX_POINT ( 'NONE', #13815 ) ;
#62016 = CARTESIAN_POINT ( 'NONE',  ( 98.80728567624888115, -32.50078473314371763, 243.7680903695909649 ) ) ;
#62017 = CARTESIAN_POINT ( 'NONE',  ( 102.3831517106511484, -26.69142711411281255, 135.4118157521009493 ) ) ;
#62018 = CARTESIAN_POINT ( 'NONE',  ( 113.3292761056179359, -27.64973082387871628, 89.60800622829195561 ) ) ;
#62019 = CARTESIAN_POINT ( 'NONE',  ( 110.6845584771929794, -28.26525459981584376, 249.5838068554170093 ) ) ;
#62020 = CARTESIAN_POINT ( 'NONE',  ( 172.5667039024478129, -36.32844715993500273, 300.4678068554149490 ) ) ;
#62021 = CARTESIAN_POINT ( 'NONE',  ( 117.0682170987564774, -39.67016276869777869, 179.5984824187679294 ) ) ;
#62022 = CARTESIAN_POINT ( 'NONE',  ( 62.03742497533751532, -23.42844715994046467, 237.4678068554150059 ) ) ;
#62023 = CARTESIAN_POINT ( 'NONE',  ( 97.81168569434709070, -40.51740311210409828, 127.6359003399277441 ) ) ;
#62024 = ORIENTED_EDGE ( 'NONE', *, *, #12456, .F. ) ;
#62025 = CARTESIAN_POINT ( 'NONE',  ( 130.1658077747426319, 74.80151635532865839, 10.09693588310459766 ) ) ;
#62026 = ORIENTED_EDGE ( 'NONE', *, *, #83968, .F. ) ;
#62027 = EDGE_CURVE ( 'NONE', #43505, #86449, #46144, .T. ) ;
#62028 = ORIENTED_EDGE ( 'NONE', *, *, #80998, .F. ) ;
#62029 = FACE_OUTER_BOUND ( 'NONE', #2999, .T. ) ;
#62030 = ADVANCED_FACE ( 'NONE', ( #73917 ), #22430, .T. ) ;
#62031 = VERTEX_POINT ( 'NONE', #76940 ) ;
#62032 = AXIS2_PLACEMENT_3D ( 'NONE', #76773, #83159, #89517 ) ;
#62033 = CARTESIAN_POINT ( 'NONE',  ( 121.2221484686747317, -94.95109689075249548, -21.78219314458229405 ) ) ;
#62034 = CARTESIAN_POINT ( 'NONE',  ( 117.1637410210353210, -34.13475704353096063, 124.0270538473399426 ) ) ;
#62035 = CARTESIAN_POINT ( 'NONE',  ( -10.34205959026443367, 75.17848243421535415, 130.1458012250857337 ) ) ;
#62036 = DIRECTION ( 'NONE',  ( -2.981567257902526681E-15, 0.8571673007021100021, 0.5150380749100580413 ) ) ;
#62037 = DIRECTION ( 'NONE',  ( 4.299999999999999979E-14, -1.000000000000000000, 0.000000000000000000 ) ) ;
#62040 = CARTESIAN_POINT ( 'NONE',  ( 100.7633749303631561, -45.78122309449478422, 233.0803871806729717 ) ) ;
#62039 = CARTESIAN_POINT ( 'NONE',  ( 74.06670390244701707, -90.27844715994098124, 51.21780685541800437 ) ) ;
#62038 = CARTESIAN_POINT ( 'NONE',  ( 99.04406185041210620, -42.84125762927686765, 142.8439586081852894 ) ) ;
#62041 = CARTESIAN_POINT ( 'NONE',  ( 163.2569089553700223, -33.54226604285010893, -5.074374724088000832 ) ) ;
#62042 = CARTESIAN_POINT ( 'NONE',  ( 31.56670390244774893, -33.35206098992784263, 117.4678068554150485 ) ) ;
#62043 = ORIENTED_EDGE ( 'NONE', *, *, #70130, .F. ) ;
#62044 = CARTESIAN_POINT ( 'NONE',  ( 1.387778780781445676E-14, 224.4999999999999432, 97.27542076772557778 ) ) ;
#62045 = CARTESIAN_POINT ( 'NONE',  ( 69.25310000000000343, 82.54999999999999716, 335.3740053999999304 ) ) ;
#62046 = CARTESIAN_POINT ( 'NONE',  ( 31.78666935232887880, -36.02818131005931690, 193.9678068554150911 ) ) ;
#62047 = CARTESIAN_POINT ( 'NONE',  ( 45.76696975232907505, -48.62818131006087441, 249.9678068554150343 ) ) ;
#62048 = EDGE_CURVE ( 'NONE', #83626, #53265, #17137, .T. ) ;
#62050 = ORIENTED_EDGE ( 'NONE', *, *, #14310, .F. ) ;
#62049 = CARTESIAN_POINT ( 'NONE',  ( 116.2574608483823226, -41.81646255891691766, 263.4241967044824833 ) ) ;
#62051 = CARTESIAN_POINT ( 'NONE',  ( 116.3232968930447839, -32.93863405887816498, 194.1356252759109680 ) ) ;
#62052 = CARTESIAN_POINT ( 'NONE',  ( 114.7236970816665860, -44.73335358772728654, 113.1718157521009687 ) ) ;
#62053 = CARTESIAN_POINT ( 'NONE',  ( 116.7448692891101985, -32.85500114480387168, 50.12991099019698282 ) ) ;
#62054 = CARTESIAN_POINT ( 'NONE',  ( 102.9499971297430250, -26.42158413985995580, 171.3908633711489813 ) ) ;
#62055 = AXIS2_PLACEMENT_3D ( 'NONE', #63156, #7308, #27739 ) ;
#62056 = CARTESIAN_POINT ( 'NONE',  ( 107.0664832912739968, -36.72944715994100306, 287.6356252759109680 ) ) ;
#62057 = CARTESIAN_POINT ( 'NONE',  ( 163.2569089553706760, -33.54226604284440327, 313.9678068554149490 ) ) ;
#62059 = DIRECTION ( 'NONE',  ( 0.000000000000000000, -1.000000000000000000, 0.000000000000000000 ) ) ;
#62058 = DIRECTION ( 'NONE',  ( 0.000000000000000000, 0.000000000000000000, 1.000000000000000000 ) ) ;
#62060 = CARTESIAN_POINT ( 'NONE',  ( 50.87649884952473656, -33.54226604284966839, 237.4678068554150059 ) ) ;
#62061 = DIRECTION ( 'NONE',  ( 0.000000000000000000, 0.000000000000000000, 1.000000000000000000 ) ) ;
#62062 = ORIENTED_EDGE ( 'NONE', *, *, #29298, .F. ) ;
#62063 = EDGE_CURVE ( 'NONE', #64817, #47280, #22884, .T. ) ;
#62064 = AXIS2_PLACEMENT_3D ( 'NONE', #51666, #3534, #43962 ) ;
#62065 = AXIS2_PLACEMENT_3D ( 'NONE', #951, #42265, #7765 ) ;
#62066 = VERTEX_POINT ( 'NONE', #77385 ) ;
#62067 = ORIENTED_EDGE ( 'NONE', *, *, #20194, .T. ) ;
#62068 = VECTOR ( 'NONE', #28021, 1000.000000000000000 ) ;
#62069 = EDGE_LOOP ( 'NONE', ( #24600, #2302, #43240, #33060 ) ) ;
#62070 = DIRECTION ( 'NONE',  ( -3.100000000000000258E-29, 3.100000000000000044E-14, 1.000000000000000000 ) ) ;
#62071 = CARTESIAN_POINT ( 'NONE',  ( 115.1902516771092451, -44.19056033372781656, 74.22324432352993995 ) ) ;
#62072 = CARTESIAN_POINT ( 'NONE',  ( 75.61066417432020614, 20.32000000000000028, 189.7379999999999995 ) ) ;
#62073 = AXIS2_PLACEMENT_3D ( 'NONE', #24511, #53058, #46257 ) ;
#62074 = CARTESIAN_POINT ( 'NONE',  ( 164.7830935719630361, -29.99615139349950965, 117.4678068554150485 ) ) ;
#62075 = CARTESIAN_POINT ( 'NONE',  ( 108.8562982717690062, -47.04397778784520057, 163.7127681330539701 ) ) ;
#62076 = AXIS2_PLACEMENT_3D ( 'NONE', #30826, #85816, #43543 ) ;
#62077 = CARTESIAN_POINT ( 'NONE',  ( -33.98325472291460159, 8.255000000000000782, 3.175000000000234746 ) ) ;
#62078 = AXIS2_PLACEMENT_3D ( 'NONE', #14128, #21395, #12791 ) ;
#62079 = CARTESIAN_POINT ( 'NONE',  ( 106.0094748626272434, -28.25366608065910157, 269.5981341137911613 ) ) ;
#62080 = EDGE_LOOP ( 'NONE', ( #3230, #19933, #64965, #24691 ) ) ;
#62081 = ORIENTED_EDGE ( 'NONE', *, *, #65032, .T. ) ;
#62082 = ORIENTED_EDGE ( 'NONE', *, *, #85632, .F. ) ;
#62083 = AXIS2_PLACEMENT_3D ( 'NONE', #2117, #50696, #21215 ) ;
#62084 = DIRECTION ( 'NONE',  ( 0.000000000000000000, 1.000000000000000000, 0.000000000000000000 ) ) ;
#62085 = CARTESIAN_POINT ( 'NONE',  ( 113.6646628792758094, -44.27214913190846346, 183.1483198295319426 ) ) ;
#62086 = CARTESIAN_POINT ( 'NONE',  ( 97.31584371959736757, -39.30597601310159916, 76.53145861037360476 ) ) ;
#62087 = CARTESIAN_POINT ( 'NONE',  ( 109.7212149768214147, -26.99983785526572788, 274.8646644956127147 ) ) ;
#62088 = EDGE_CURVE ( 'NONE', #31310, #79375, #21480, .T. ) ;
#62089 = CARTESIAN_POINT ( 'NONE',  ( 93.91125933621934507, -111.8737466215625744, -11.78219314458178779 ) ) ;
#62090 = EDGE_CURVE ( 'NONE', #44014, #5447, #36939, .T. ) ;
#62091 = DIRECTION ( 'NONE',  ( 0.7071067811865460184, 0.7071067811865489050, 0.000000000000000000 ) ) ;
#62092 = ADVANCED_FACE ( 'NONE', ( #23339 ), #54830, .T. ) ;
#62093 = DIRECTION ( 'NONE',  ( 1.000000000000000078E-15, 0.000000000000000000, -1.000000000000000000 ) ) ;
#62094 = CARTESIAN_POINT ( 'NONE',  ( 116.8464009251322153, -35.91275531464980020, 253.8927681330545454 ) ) ;
#62095 = CYLINDRICAL_SURFACE ( 'NONE', #29857, 4.500000000000003553 ) ;
#62096 = VERTEX_POINT ( 'NONE', #16503 ) ;
#62097 = EDGE_CURVE ( 'NONE', #78672, #69100, #14721, .T. ) ;
#62098 = CARTESIAN_POINT ( 'NONE',  ( -8.960875259515413305, 209.9608752595154044, 75.92175051903070937 ) ) ;
#62099 = AXIS2_PLACEMENT_3D ( 'NONE', #55943, #50029, #1009 ) ;
#62100 = CARTESIAN_POINT ( 'NONE',  ( 25.56670390244828894, -48.82844715994168183, 293.2178068554150059 ) ) ;
#62101 = CARTESIAN_POINT ( 'NONE',  ( 114.4788834064733862, -33.31096057238692509, 101.9880903695909780 ) ) ;
#62102 = VECTOR ( 'NONE', #73813, 1000.000000000000000 ) ;
#62103 = ADVANCED_FACE ( 'NONE', ( #71917 ), #9681, .T. ) ;
#62104 = CARTESIAN_POINT ( 'NONE',  ( 193.0374249753375011, -23.42844715993432558, 249.9678068554149775 ) ) ;
#62105 = EDGE_CURVE ( 'NONE', #16980, #79245, #2432, .T. ) ;
#62106 = DIRECTION ( 'NONE',  ( 4.299999999999999979E-14, -1.000000000000000000, 0.000000000000000000 ) ) ;
#62107 = ORIENTED_EDGE ( 'NONE', *, *, #35583, .F. ) ;
#62108 = DIRECTION ( 'NONE',  ( 0.9068632946707807507, -0.4214249218767881500, 9.028300618466658994E-16 ) ) ;
#62109 = ORIENTED_EDGE ( 'NONE', *, *, #66379, .F. ) ;
#62110 = CARTESIAN_POINT ( 'NONE',  ( 108.5898285964631640, -47.07861824576353627, 142.6927681330539883 ) ) ;
#62111 = ORIENTED_EDGE ( 'NONE', *, *, #11215, .T. ) ;
#62112 = CARTESIAN_POINT ( 'NONE',  ( 1.387778780781445676E-14, 223.9999999999999716, 104.4754207677255806 ) ) ;
#62113 = CARTESIAN_POINT ( 'NONE',  ( 115.1135551441502258, -33.01825958633261848, 100.6015833058969378 ) ) ;
#62114 = CARTESIAN_POINT ( 'NONE',  ( -1.663885868249260769, 95.14749804389165888, 118.5450564992234064 ) ) ;
#62115 = CARTESIAN_POINT ( 'NONE',  ( 67.05404872073289368, -69.57571276584442899, 247.4899279706389734 ) ) ;
#62116 = CARTESIAN_POINT ( 'NONE',  ( 104.7547631156620014, -46.91734236372032996, 68.39848241876794077 ) ) ;
#62117 = DIRECTION ( 'NONE',  ( 1.000000000000000000, 0.000000000000000000, 0.000000000000000000 ) ) ;
#62118 = AXIS2_PLACEMENT_3D ( 'NONE', #62404, #182, #46183 ) ;
#62119 = ORIENTED_EDGE ( 'NONE', *, *, #55239, .F. ) ;
#62120 = VECTOR ( 'NONE', #58148, 999.9999999999998863 ) ;
#62121 = CARTESIAN_POINT ( 'NONE',  ( -117.8738102209307215, 81.72118090664557144, -12.70000000000041496 ) ) ;
#62122 = ORIENTED_EDGE ( 'NONE', *, *, #33739, .T. ) ;
#62123 = VERTEX_POINT ( 'NONE', #42394 ) ;
#62124 = VECTOR ( 'NONE', #50596, 1000.000000000000000 ) ;
#62125 = DIRECTION ( 'NONE',  ( 0.000000000000000000, 0.000000000000000000, 1.000000000000000000 ) ) ;
#62126 = ORIENTED_EDGE ( 'NONE', *, *, #12968, .T. ) ;
#62127 = CARTESIAN_POINT ( 'NONE',  ( 105.8561066403587176, -27.02385992090109568, 270.1756252759109884 ) ) ;
#62128 = CARTESIAN_POINT ( 'NONE',  ( 116.8268856436350518, -43.49382415615948361, 159.3441967044829539 ) ) ;
#62129 = CARTESIAN_POINT ( 'NONE',  ( 1.665763066381118485, 69.93250922127340630, -118.5470808886261125 ) ) ;
#62130 = FACE_OUTER_BOUND ( 'NONE', #24806, .T. ) ;
#62131 = CARTESIAN_POINT ( 'NONE',  ( 104.2140748950419464, -25.22734379144252870, 86.26991099019699050 ) ) ;
#62132 = FACE_OUTER_BOUND ( 'NONE', #8962, .T. ) ;
#62133 = VERTEX_POINT ( 'NONE', #84220 ) ;
#62134 = AXIS2_PLACEMENT_3D ( 'NONE', #38846, #4343, #32029 ) ;
#62135 = CARTESIAN_POINT ( 'NONE',  ( 135.0664832912729878, -36.72944715994189835, 342.9256252759109884 ) ) ;
#62136 = CIRCLE ( 'NONE', #15740, 2.117000000000007987 ) ;
#62137 = CIRCLE ( 'NONE', #83949, 7.999999999999992895 ) ;
#62138 = CARTESIAN_POINT ( 'NONE',  ( 160.2664750769289697, 20.32000000000000028, 148.0533267522752112 ) ) ;
#62139 = EDGE_CURVE ( 'NONE', #40280, #6819, #43241, .T. ) ;
#62140 = VERTEX_POINT ( 'NONE', #1980 ) ;
#62141 = LINE ( 'NONE', #81717, #48963 ) ;
#62142 = CYLINDRICAL_SURFACE ( 'NONE', #47831, 2.116999999999993776 ) ;
#62143 = CARTESIAN_POINT ( 'NONE',  ( 96.93559702949573875, -34.21358363697170546, 276.1327681330537871 ) ) ;
#62144 = CARTESIAN_POINT ( 'NONE',  ( 162.5667039024470171, -33.35206098992711077, -5.074374724088000832 ) ) ;
#62145 = CARTESIAN_POINT ( 'NONE',  ( 68.95544620396594837, 92.96280207012202368, 55.93298909936185481 ) ) ;
#62146 = DIRECTION ( 'NONE',  ( 0.000000000000000000, 0.000000000000000000, -1.000000000000000000 ) ) ;
#62147 = CARTESIAN_POINT ( 'NONE',  ( 116.3037889147421424, -33.73884459347697629, 283.4981341137910249 ) ) ;
#62149 = CARTESIAN_POINT ( 'NONE',  ( 99.70004787478436015, -45.98060041612298221, 118.0413395616259606 ) ) ;
#62148 = DIRECTION ( 'NONE',  ( -1.000000000000000078E-15, 1.000000000000000000, 0.000000000000000000 ) ) ;
#62150 = LINE ( 'NONE', #40364, #62527 ) ;
#62151 = CARTESIAN_POINT ( 'NONE',  ( 97.75494523667518365, -42.77206137223026161, 146.7965776568629508 ) ) ;
#62152 = DIRECTION ( 'NONE',  ( 0.000000000000000000, -1.000000000000000000, 0.000000000000000000 ) ) ;
#62153 = ORIENTED_EDGE ( 'NONE', *, *, #78631, .F. ) ;
#62154 = AXIS2_PLACEMENT_3D ( 'NONE', #23519, #3057, #10743 ) ;
#62155 = DIRECTION ( 'NONE',  ( -1.000000000000000000, -1.000000000000000078E-15, 0.000000000000000000 ) ) ;
#62156 = FACE_BOUND ( 'NONE', #54170, .T. ) ;
#62157 = PLANE ( 'NONE',  #73190 ) ;
#62158 = ORIENTED_EDGE ( 'NONE', *, *, #27037, .T. ) ;
#62160 = ORIENTED_EDGE ( 'NONE', *, *, #52011, .F. ) ;
#62159 = CARTESIAN_POINT ( 'NONE',  ( 114.1106629025095458, -44.52247787522302502, 133.1613395616249989 ) ) ;
#62161 = CARTESIAN_POINT ( 'NONE',  ( -240.5296158183964792, 14.28750000000026077, 11.11249999999970051 ) ) ;
#62162 = CARTESIAN_POINT ( 'NONE',  ( 117.4343095520634108, -35.18433407802718449, 214.9441967044829767 ) ) ;
#62163 = CARTESIAN_POINT ( 'NONE',  ( 100.3415888741731550, 78.07027470200927155, 83.52520760052999549 ) ) ;
#62164 = VECTOR ( 'NONE', #446, 1000.000000000000000 ) ;
#62165 = LINE ( 'NONE', #14931, #28577 ) ;
#62166 = AXIS2_PLACEMENT_3D ( 'NONE', #29143, #59395, #52561 ) ;
#62167 = DIRECTION ( 'NONE',  ( 0.000000000000000000, 0.000000000000000000, -1.000000000000000000 ) ) ;
#62168 = ORIENTED_EDGE ( 'NONE', *, *, #31943, .F. ) ;
#62169 = ADVANCED_FACE ( 'NONE', ( #1540 ), #29679, .T. ) ;
#62170 = EDGE_LOOP ( 'NONE', ( #75643, #70297, #87163 ) ) ;
#62171 = ORIENTED_EDGE ( 'NONE', *, *, #43130, .T. ) ;
#62172 = VERTEX_POINT ( 'NONE', #42839 ) ;
#62173 = DIRECTION ( 'NONE',  ( 0.000000000000000000, 1.000000000000000000, 0.000000000000000000 ) ) ;
#62174 = CARTESIAN_POINT ( 'NONE',  ( 109.3368649739139187, -26.55458330520283994, 220.9013395616249795 ) ) ;
#62175 = CARTESIAN_POINT ( 'NONE',  ( 49.21213752015854936, -29.73316016639470050, 237.4678068554150059 ) ) ;
#62176 = DIRECTION ( 'NONE',  ( 0.000000000000000000, 0.000000000000000000, -1.000000000000000000 ) ) ;
#62177 = AXIS2_PLACEMENT_3D ( 'NONE', #52512, #18020, #45703 ) ;
#62179 = DIRECTION ( 'NONE',  ( 0.000000000000000000, -1.000000000000000000, 0.000000000000000000 ) ) ;
#62178 = CARTESIAN_POINT ( 'NONE',  ( 70.06670390441306040, -140.6784471619069734, 245.4415720117440003 ) ) ;
#62180 = CARTESIAN_POINT ( 'NONE',  ( 74.19170390244705970, -127.9034471599409812, 55.21780685541800437 ) ) ;
#62181 = ORIENTED_EDGE ( 'NONE', *, *, #54280, .F. ) ;
#62182 = VECTOR ( 'NONE', #42729, 1000.000000000000000 ) ;
#62184 = VERTEX_POINT ( 'NONE', #70578 ) ;
#62183 = AXIS2_PLACEMENT_3D ( 'NONE', #6050, #33738, #53248 ) ;
#62185 = DIRECTION ( 'NONE',  ( 0.7071067811865273667, -0.7071067811865676678, 7.071067811865281076E-16 ) ) ;
#62186 = DIRECTION ( 'NONE',  ( 0.000000000000000000, 0.000000000000000000, 1.000000000000000000 ) ) ;
#62187 = CARTESIAN_POINT ( 'NONE',  ( 96.02263050233435138, -38.01213896886783061, 232.4184824187679794 ) ) ;
#62188 = EDGE_CURVE ( 'NONE', #7620, #8519, #2682, .T. ) ;
#62189 = CARTESIAN_POINT ( 'NONE',  ( 94.58945128933383728, -41.88441296220994303, 293.1356252759106837 ) ) ;
#62190 = VECTOR ( 'NONE', #74631, 1000.000000000000000 ) ;
#62191 = CARTESIAN_POINT ( 'NONE',  ( 97.83387747045378546, -32.00739517038279303, 91.96229194257693962 ) ) ;
#62192 = EDGE_CURVE ( 'NONE', #24090, #67994, #22998, .T. ) ;
#62193 = CARTESIAN_POINT ( 'NONE',  ( 50.24780502318014896, 92.07499999999998863, -72.12189744004568581 ) ) ;
#62194 = EDGE_CURVE ( 'NONE', #40277, #37737, #70120, .T. ) ;
#62195 = CIRCLE ( 'NONE', #20131, 3.000000000000002665 ) ;
#62196 = CARTESIAN_POINT ( 'NONE',  ( 104.9990148946446737, -26.93299307437888146, 21.24201732517684960 ) ) ;
#62197 = EDGE_LOOP ( 'NONE', ( #26175, #69890, #55964, #17560, #26068, #21829 ) ) ;
#62198 = FACE_OUTER_BOUND ( 'NONE', #27656, .T. ) ;
#62199 = ADVANCED_FACE ( 'NONE', ( #56927, #30129 ), #57826, .F. ) ;
#62200 = VECTOR ( 'NONE', #61157, 1000.000000000000000 ) ;
#62201 = ORIENTED_EDGE ( 'NONE', *, *, #30094, .T. ) ;
#62202 = ORIENTED_EDGE ( 'NONE', *, *, #43405, .F. ) ;
#62203 = DIRECTION ( 'NONE',  ( 1.000000000000000000, 6.831565154159360295E-14, 0.000000000000000000 ) ) ;
#62204 = CARTESIAN_POINT ( 'NONE',  ( 98.49168440212470443, -38.96576165349271292, 272.9615833058970225 ) ) ;
#62205 = DIRECTION ( 'NONE',  ( 0.000000000000000000, -1.000000000000000000, 0.000000000000000000 ) ) ;
#62206 = CARTESIAN_POINT ( 'NONE',  ( -118.3862315815643882, 93.55466788070663142, 6.352948492897542820 ) ) ;
#62207 = DIRECTION ( 'NONE',  ( 0.000000000000000000, 0.000000000000000000, 1.000000000000000000 ) ) ;
#62208 = EDGE_CURVE ( 'NONE', #2919, #89295, #85369, .T. ) ;
#62209 = VECTOR ( 'NONE', #37687, 1000.000000000000000 ) ;
#62210 = CARTESIAN_POINT ( 'NONE',  ( 0.000000000000000000, 82.54999999999999716, -97.46299999999996544 ) ) ;
#62211 = ORIENTED_EDGE ( 'NONE', *, *, #24471, .F. ) ;
#62212 = DIRECTION ( 'NONE',  ( 0.000000000000000000, 0.000000000000000000, -1.000000000000000000 ) ) ;
#62213 = DIRECTION ( 'NONE',  ( 1.000000000000000078E-15, -1.000000000000000083E-30, -1.000000000000000000 ) ) ;
#62214 = ORIENTED_EDGE ( 'NONE', *, *, #42428, .F. ) ;
#62215 = CARTESIAN_POINT ( 'NONE',  ( 117.0917326185583676, -32.07397045188266560, 59.16038718067295576 ) ) ;
#62216 = ORIENTED_EDGE ( 'NONE', *, *, #9029, .F. ) ;
#62217 = CARTESIAN_POINT ( 'NONE',  ( 108.7463670854851756, -45.85490172528324138, 275.5395189410199919 ) ) ;
#62218 = FACE_OUTER_BOUND ( 'NONE', #39928, .T. ) ;
#62219 = CARTESIAN_POINT ( 'NONE',  ( 116.1942131220466621, -33.21547736372279758, 139.1184824187689628 ) ) ;
#62220 = CARTESIAN_POINT ( 'NONE',  ( -82.89895571708225930, 82.54999999999999716, -100.8594679592215471 ) ) ;
#62221 = CARTESIAN_POINT ( 'NONE',  ( 194.0667039024473297, -24.92844715993408045, 300.4678068554149490 ) ) ;
#62222 = DIRECTION ( 'NONE',  ( 1.000000000000000000, 4.299999999999999979E-14, 1.000000000000000078E-15 ) ) ;
#62223 = CARTESIAN_POINT ( 'NONE',  ( 9.347434767860939075, 73.95160161085279071, 130.2210325332607113 ) ) ;
#62224 = CIRCLE ( 'NONE', #11397, 38.10000000000000853 ) ;
#62225 = CARTESIAN_POINT ( 'NONE',  ( 104.3129624051631907, -25.97697669550431243, 241.2880062282919482 ) ) ;
#62226 = DIRECTION ( 'NONE',  ( 0.000000000000000000, 0.000000000000000000, 1.000000000000000000 ) ) ;
#62227 = ORIENTED_EDGE ( 'NONE', *, *, #12588, .F. ) ;
#62228 = LINE ( 'NONE', #63127, #2361 ) ;
#62229 = ORIENTED_EDGE ( 'NONE', *, *, #44757, .F. ) ;
#62230 = CARTESIAN_POINT ( 'NONE',  ( 117.2645927648968183, -42.86211997589052203, 124.3956252759109731 ) ) ;
#62231 = CARTESIAN_POINT ( 'NONE',  ( 123.6107665481496554, 45.16440871034607341, -42.01786438290864822 ) ) ;
#62232 = VERTEX_POINT ( 'NONE', #38272 ) ;
#62233 = ORIENTED_EDGE ( 'NONE', *, *, #8625, .T. ) ;
#62234 = ORIENTED_EDGE ( 'NONE', *, *, #64790, .F. ) ;
#62235 = DIRECTION ( 'NONE',  ( 0.000000000000000000, 1.000000000000000000, 0.000000000000000000 ) ) ;
#62236 = DIRECTION ( 'NONE',  ( 1.000000000000000000, -1.526556658859588981E-13, 0.000000000000000000 ) ) ;
#62237 = LINE ( 'NONE', #20916, #61058 ) ;
#62238 = DIRECTION ( 'NONE',  ( 0.000000000000000000, 0.000000000000000000, -1.000000000000000000 ) ) ;
#62239 = CARTESIAN_POINT ( 'NONE',  ( 112.1932604131138760, -43.70204218538222563, 180.8871379886389832 ) ) ;
#62240 = CARTESIAN_POINT ( 'NONE',  ( 96.24544184373708333, -34.36507245719054282, 252.1432443235302969 ) ) ;
#62241 = CARTESIAN_POINT ( 'NONE',  ( 97.81547641113768066, -40.52666954525783183, 57.63642061862653065 ) ) ;
#62242 = ORIENTED_EDGE ( 'NONE', *, *, #13910, .F. ) ;
#62243 = CARTESIAN_POINT ( 'NONE',  ( 1.653928925557865748, 69.93042650361837786, 118.5473008259350678 ) ) ;
#62244 = CIRCLE ( 'NONE', #86893, 8.928100000000000591 ) ;
#62245 = CARTESIAN_POINT ( 'NONE',  ( 121.3042370176062548, -43.34581843340460239, 0.4256252759109851458 ) ) ;
#62246 = ADVANCED_FACE ( 'NONE', ( #45955 ), #45072, .F. ) ;
#62247 = ORIENTED_EDGE ( 'NONE', *, *, #16394, .T. ) ;
#62248 = ORIENTED_EDGE ( 'NONE', *, *, #10316, .F. ) ;
#62249 = AXIS2_PLACEMENT_3D ( 'NONE', #36740, #71270, #49443 ) ;
#62250 = AXIS2_PLACEMENT_3D ( 'NONE', #42654, #84493, #10719 ) ;
#62251 = CARTESIAN_POINT ( 'NONE',  ( 150.8164832912740110, -8.729447159940999512, -5.074374724088000832 ) ) ;
#62252 = LINE ( 'NONE', #67730, #67229 ) ;
#62253 = DIRECTION ( 'NONE',  ( 0.000000000000000000, 0.000000000000000000, 1.000000000000000000 ) ) ;
#62254 = ADVANCED_FACE ( 'NONE', ( #3319 ), #59589, .F. ) ;
#62255 = DIRECTION ( 'NONE',  ( 1.000000000000000000, -3.418174336900117128E-15, 0.000000000000000000 ) ) ;
#62256 = CARTESIAN_POINT ( 'NONE',  ( 112.4311324297980406, -44.02555639339375659, 182.4914674471249612 ) ) ;
#62257 = CARTESIAN_POINT ( 'NONE',  ( 110.8102856614596021, -46.50649220725635757, 62.86705384733992474 ) ) ;
#62258 = DIRECTION ( 'NONE',  ( 0.000000000000000000, 1.000000000000000000, 0.000000000000000000 ) ) ;
#62259 = EDGE_LOOP ( 'NONE', ( #8050, #87709, #48947, #45290, #62781 ) ) ;
#62260 = VECTOR ( 'NONE', #1822, 1000.000000000000000 ) ;
#62261 = AXIS2_PLACEMENT_3D ( 'NONE', #49858, #1740, #80161 ) ;
#62262 = CARTESIAN_POINT ( 'NONE',  ( -84.99964240976918006, 69.93120980984940616, -82.65143893653593921 ) ) ;
#62263 = ORIENTED_EDGE ( 'NONE', *, *, #30979, .F. ) ;
#62264 = CARTESIAN_POINT ( 'NONE',  ( 142.8679068202682458, 10.65431904611001634, 540.9756252759101471 ) ) ;
#62265 = ORIENTED_EDGE ( 'NONE', *, *, #58117, .T. ) ;
#62266 = DIRECTION ( 'NONE',  ( -1.000000000000000078E-15, -1.000000000000000083E-30, 1.000000000000000000 ) ) ;
#62267 = CIRCLE ( 'NONE', #39052, 154.1697486074984909 ) ;
#62268 = CARTESIAN_POINT ( 'NONE',  ( 72.52678588541827764, -139.0845773098406823, 247.5112265945679724 ) ) ;
#62269 = LINE ( 'NONE', #34561, #22922 ) ;
#62270 = CARTESIAN_POINT ( 'NONE',  ( -179.6205029264235122, 20.32000000000000028, 123.8612349545196025 ) ) ;
#62271 = VERTEX_POINT ( 'NONE', #80518 ) ;
#62272 = ADVANCED_FACE ( 'NONE', ( #18272 ), #10567, .F. ) ;
#62273 = CARTESIAN_POINT ( 'NONE',  ( 116.4074703635738075, -31.97189281592868682, 44.20133956162491984 ) ) ;
#62275 = DIRECTION ( 'NONE',  ( 0.000000000000000000, 0.000000000000000000, -1.000000000000000000 ) ) ;
#62274 = CARTESIAN_POINT ( 'NONE',  ( 165.2725846195389749, -35.55794170701241086, 193.9678068554149775 ) ) ;
#62276 = DIRECTION ( 'NONE',  ( 0.000000000000000000, 1.000000000000000000, 0.000000000000000000 ) ) ;
#62277 = AXIS2_PLACEMENT_3D ( 'NONE', #61461, #66491, #40581 ) ;
#62278 = FACE_OUTER_BOUND ( 'NONE', #62963, .T. ) ;
#62279 = ORIENTED_EDGE ( 'NONE', *, *, #44415, .F. ) ;
#62280 = VECTOR ( 'NONE', #10868, 1000.000000000000000 ) ;
#62281 = DIRECTION ( 'NONE',  ( 0.000000000000000000, 0.000000000000000000, 1.000000000000000000 ) ) ;
#62282 = DIRECTION ( 'NONE',  ( -1.000000000000000078E-15, 1.000000000000000000, 0.000000000000000000 ) ) ;
#62283 = DIRECTION ( 'NONE',  ( -1.000000000000000078E-15, 1.000000000000000083E-30, 1.000000000000000000 ) ) ;
#62284 = ADVANCED_FACE ( 'NONE', ( #11470, #31449 ), #39605, .T. ) ;
#62285 = VERTEX_POINT ( 'NONE', #52311 ) ;
#62286 = CARTESIAN_POINT ( 'NONE',  ( 113.5195425369480233, -28.51389573442233427, 75.54705384733995288 ) ) ;
#62288 = PLANE ( 'NONE',  #29651 ) ;
#62287 = DIRECTION ( 'NONE',  ( 0.000000000000000000, 0.000000000000000000, 1.000000000000000000 ) ) ;
#62289 = DIRECTION ( 'NONE',  ( 1.000000000000000000, 0.000000000000000000, 0.000000000000000000 ) ) ;
#62290 = VECTOR ( 'NONE', #36077, 1000.000000000000000 ) ;
#62291 = CARTESIAN_POINT ( 'NONE',  ( 137.9639241664444285, -93.39344735187280833, 249.3055338466990065 ) ) ;
#62292 = ORIENTED_EDGE ( 'NONE', *, *, #62497, .F. ) ;
#62293 = CARTESIAN_POINT ( 'NONE',  ( 105.0928733274061813, -25.78792777683075599, 121.2184824187669818 ) ) ;
#62295 = EDGE_LOOP ( 'NONE', ( #80582, #81804, #24162, #69135 ) ) ;
#62294 = CARTESIAN_POINT ( 'NONE',  ( 182.4202572930400095, -33.70561438051981185, 342.9256252759119548 ) ) ;
#62296 = CIRCLE ( 'NONE', #85546, 5.000000000000004441 ) ;
#62297 = CARTESIAN_POINT ( 'NONE',  ( 115.9412561796927577, -30.17946786548973748, 255.3203871806729524 ) ) ;
#62298 = LINE ( 'NONE', #20979, #17919 ) ;
#62299 = CARTESIAN_POINT ( 'NONE',  ( 208.9149999999999920, 28.98850000000000193, -7.937500000000000000 ) ) ;
#62300 = DIRECTION ( 'NONE',  ( 9.299908063537919123E-17, 0.000000000000000000, 1.000000000000000000 ) ) ;
#62301 = ADVANCED_FACE ( 'NONE', ( #45508 ), #31899, .F. ) ;
#62302 = CARTESIAN_POINT ( 'NONE',  ( -3.174999999999644995, 111.1250000000000000, -33.98325472291465132 ) ) ;
#62303 = AXIS2_PLACEMENT_3D ( 'NONE', #38156, #16829, #50435 ) ;
#62304 = CARTESIAN_POINT ( 'NONE',  ( 52.06670390244699576, -67.87844715994100397, 55.21780685541800437 ) ) ;
#62305 = CARTESIAN_POINT ( 'NONE',  ( -97.62852612868731228, 72.47310549519059464, 86.68128281353570230 ) ) ;
#62306 = CARTESIAN_POINT ( 'NONE',  ( 96.73459541816642115, -35.84013382243347223, 186.2461014663879837 ) ) ;
#62307 = EDGE_LOOP ( 'NONE', ( #33143, #7331, #21771, #22260, #61611, #8310 ) ) ;
#62308 = ORIENTED_EDGE ( 'NONE', *, *, #4272, .T. ) ;
#62309 = AXIS2_PLACEMENT_3D ( 'NONE', #9432, #23087, #28985 ) ;
#62310 = CARTESIAN_POINT ( 'NONE',  ( 107.7905181614329564, -45.59160847044328335, 174.0730118773249728 ) ) ;
#62311 = AXIS2_PLACEMENT_3D ( 'NONE', #26043, #59643, #67357 ) ;
#62312 = DIRECTION ( 'NONE',  ( -0.3552177606235690788, 0.000000000000000000, -0.9347835805883503157 ) ) ;
#62314 = CARTESIAN_POINT ( 'NONE',  ( 97.81027290652480133, -40.51396607169345288, 57.63532815071263116 ) ) ;
#62313 = CARTESIAN_POINT ( 'NONE',  ( 111.4826097991074079, -46.11499196468592743, 283.9146728949579597 ) ) ;
#62315 = CARTESIAN_POINT ( 'NONE',  ( 23.58228359103286920, 84.94115763029901700, 298.7645859682927494 ) ) ;
#62316 = DIRECTION ( 'NONE',  ( 0.000000000000000000, 0.000000000000000000, -1.000000000000000000 ) ) ;
#62317 = EDGE_CURVE ( 'NONE', #47865, #7646, #73230, .T. ) ;
#62318 = AXIS2_PLACEMENT_3D ( 'NONE', #35645, #44237, #57431 ) ;
#62319 = CARTESIAN_POINT ( 'NONE',  ( 0.000000000000000000, 111.1250000000000000, 0.000000000000000000 ) ) ;
#62320 = FACE_OUTER_BOUND ( 'NONE', #60567, .T. ) ;
#62321 = DIRECTION ( 'NONE',  ( 0.000000000000000000, -1.000000000000000000, 0.000000000000000000 ) ) ;
#62322 = EDGE_CURVE ( 'NONE', #6493, #66368, #24398, .T. ) ;
#62324 = CARTESIAN_POINT ( 'NONE',  ( 109.9541224118590890, -48.19721710984623542, 242.7727681330539724 ) ) ;
#62323 = PRESENTATION_LAYER_ASSIGNMENT (  '', '', ( #36206 ) ) ;
#62325 = CARTESIAN_POINT ( 'NONE',  ( 97.75867135665099283, -40.38561536396691309, 171.6245721619694109 ) ) ;
#62326 = ORIENTED_EDGE ( 'NONE', *, *, #10511, .T. ) ;
#62327 = ORIENTED_EDGE ( 'NONE', *, *, #11756, .F. ) ;
#62328 = CARTESIAN_POINT ( 'NONE',  ( 116.3191775144681515, -32.94222376661483764, 89.13562527591095375 ) ) ;
#62329 = CARTESIAN_POINT ( 'NONE',  ( -82.65057572782323803, 95.14807216649714405, -84.99753727674128356 ) ) ;
#62330 = AXIS2_PLACEMENT_3D ( 'NONE', #14333, #41114, #82491 ) ;
#62331 = CARTESIAN_POINT ( 'NONE',  ( 97.81916166726549022, -40.53564570812252299, 122.6367379950636405 ) ) ;
#62332 = DIRECTION ( 'NONE',  ( -1.000000000000000000, -5.512527431108013646E-15, 0.000000000000000000 ) ) ;
#62333 = DIRECTION ( 'NONE',  ( -7.723290606088049820E-15, 0.000000000000000000, -1.000000000000000000 ) ) ;
#62334 = ORIENTED_EDGE ( 'NONE', *, *, #29820, .F. ) ;
#62335 = CARTESIAN_POINT ( 'NONE',  ( 118.6189051447874903, -33.88680481589229743, 10.01848241876795953 ) ) ;
#62336 = VECTOR ( 'NONE', #46027, 1000.000000000000114 ) ;
#62337 = B_SPLINE_CURVE_WITH_KNOTS ( 'NONE', 3,
 ( #61824, #41379, #60476, #82308, #75480, #82760, #89557, #88223, #6873, #25980, #53649, #14601, #28201, #57710, #36387, #15044, #70007, #15501, #84095, #22767, #20955, #42717, #2318, #48632 ),
 .UNSPECIFIED., .F., .F.,
 ( 4, 2, 2, 2, 2, 2, 2, 2, 2, 2, 2, 4 ),
 ( 0.5000920265313297808, 0.5625805232149136970, 0.6250690198984975021, 0.6875575165820814183, 0.7500460132656651124, 0.8125345099492488066, 0.8437787582910407647, 0.8750230066328326117, 0.9062672549746244588, 0.9375115033164163059, 0.9687557516582081529, 1.000000000000000000 ),
 .UNSPECIFIED. ) ;
#62338 = CARTESIAN_POINT ( 'NONE',  ( 98.83914287153486100, -29.34771585412822859, 235.7565776568629872 ) ) ;
#62339 = EDGE_LOOP ( 'NONE', ( #35480, #60360, #77793, #66325 ) ) ;
#62340 = VECTOR ( 'NONE', #62036, 1000.000000000000000 ) ;
#62341 = B_SPLINE_CURVE_WITH_KNOTS ( 'NONE', 3,
 ( #27359, #48229, #26469, #20560, #19210, #75964, #54139, #13734, #41419, #60069, #87801, #25567, #41860, #70497, #21455, #48675, #36430, #77309, #35058, #8269, #22805, #42757, #62325, #6916, #15538, #56394, #83238, #29158 ),
 .UNSPECIFIED., .F., .F.,
 ( 4, 2, 2, 2, 2, 2, 2, 2, 2, 2, 1, 1, 1, 1, 2, 4 ),
 ( 0.000000000000000000, 0.06250757335814957627, 0.1250151467162991525, 0.1875227200744487288, 0.2500302934325983051, 0.3125378667907478536, 0.3750454401488974576, 0.4375530135070470061, 0.4688068001861218081, 0.4844336935256593479, 0.4922471401954281456, 0.4961538635303126554, 0.4981072251977549104, 0.4990839060314760101, 0.4995722464483365877, 0.5000605868651970543 ),
 .UNSPECIFIED. ) ;
#62342 = CARTESIAN_POINT ( 'NONE',  ( -9.493160772977415007, 90.87556570329743977, 118.1767503086004183 ) ) ;
#62343 = DIRECTION ( 'NONE',  ( -1.639958061481212836E-42, 4.100000000000000342E-29, 1.000000000000000000 ) ) ;
#62344 = CARTESIAN_POINT ( 'NONE',  ( 110.9050858514773807, -45.96338816205167177, 167.8899810469827685 ) ) ;
#62345 = CARTESIAN_POINT ( 'NONE',  ( 109.7208934110032743, -44.96686374295461519, 55.65475703625794068 ) ) ;
#62346 = CARTESIAN_POINT ( 'NONE',  ( 105.7176149122623485, -24.93101994221251516, 156.1670538473399574 ) ) ;
#62347 = DIRECTION ( 'NONE',  ( -1.000000000000000078E-15, 1.000000000000000083E-30, 1.000000000000000000 ) ) ;
#62348 = ORIENTED_EDGE ( 'NONE', *, *, #44125, .F. ) ;
#62349 = CARTESIAN_POINT ( 'NONE',  ( 107.7702177616926065, 127.0000000000000000, 4.185020385794044591E-13 ) ) ;
#62350 = AXIS2_PLACEMENT_3D ( 'NONE', #52342, #43319, #16093 ) ;
#62351 = ORIENTED_EDGE ( 'NONE', *, *, #59193, .T. ) ;
#62352 = ORIENTED_EDGE ( 'NONE', *, *, #66765, .T. ) ;
#62353 = CARTESIAN_POINT ( 'NONE',  ( 210.2301280605339855, 25.81350000000000477, -7.937500000000000000 ) ) ;
#62354 = ORIENTED_EDGE ( 'NONE', *, *, #41802, .F. ) ;
#62355 = ORIENTED_EDGE ( 'NONE', *, *, #61971, .F. ) ;
#62356 = FACE_OUTER_BOUND ( 'NONE', #82446, .T. ) ;
#62357 = CARTESIAN_POINT ( 'NONE',  ( 98.52552435659306695, -36.63915763587115038, 110.7409912566489680 ) ) ;
#62358 = CARTESIAN_POINT ( 'NONE',  ( 115.2691655829841579, -30.20224515277380917, 244.3613395616249875 ) ) ;
#62359 = VECTOR ( 'NONE', #34156, 1000.000000000000000 ) ;
#62360 = CARTESIAN_POINT ( 'NONE',  ( 103.8265608274144256, -48.10271009292828381, 217.3556252759109668 ) ) ;
#62361 = CARTESIAN_POINT ( 'NONE',  ( 118.0600790064083299, -37.62648441163795354, 34.77372051400695341 ) ) ;
#62362 = CARTESIAN_POINT ( 'NONE',  ( 165.9667039024459996, -26.71338133339301635, -5.074374724088000832 ) ) ;
#62363 = CARTESIAN_POINT ( 'NONE',  ( 99.04382173825221969, -42.84089691445041126, 92.84392477103513386 ) ) ;
#62364 = CIRCLE ( 'NONE', #10120, 2.030000000000003801 ) ;
#62365 = EDGE_LOOP ( 'NONE', ( #81486, #38932 ) ) ;
#62366 = CARTESIAN_POINT ( 'NONE',  ( 70.11541878361150282, -140.6397552082484310, 245.9889283728621763 ) ) ;
#62367 = VECTOR ( 'NONE', #50976, 1000.000000000000000 ) ;
#62368 = CARTESIAN_POINT ( 'NONE',  ( 103.4152017835535844, -27.65577212482025971, 130.3813395616259925 ) ) ;
#62369 = CARTESIAN_POINT ( 'NONE',  ( 116.1621043582934902, -29.05491297703968101, 74.38419670448293175 ) ) ;
#62370 = CARTESIAN_POINT ( 'NONE',  ( 99.50747941120199869, -29.43470559729854230, 250.7156252759109520 ) ) ;
#62371 = EDGE_LOOP ( 'NONE', ( #54380, #89745, #17925, #15831 ) ) ;
#62372 = EDGE_CURVE ( 'NONE', #30425, #15176, #18678, .T. ) ;
#62373 = CARTESIAN_POINT ( 'NONE',  ( 111.1275225509982505, -27.12762490620188771, 244.7584824187679544 ) ) ;
#62374 = DIRECTION ( 'NONE',  ( 0.0001713722456127401463, -0.9999999853157766072, -1.713722456137401502E-19 ) ) ;
#62375 = CARTESIAN_POINT ( 'NONE',  ( 98.04137945595525139, -41.04156525728014770, 22.68116640241568405 ) ) ;
#62376 = DIRECTION ( 'NONE',  ( 0.000000000000000000, 1.000000000000000000, 0.000000000000000000 ) ) ;
#62378 = PLANE ( 'NONE',  #70322 ) ;
#62377 = CARTESIAN_POINT ( 'NONE',  ( 107.9149127458704243, -46.51730135063228744, 277.6356252759110248 ) ) ;
#62379 = FACE_OUTER_BOUND ( 'NONE', #66920, .T. ) ;
#62380 = CYLINDRICAL_SURFACE ( 'NONE', #58416, 1.999999999999995781 ) ;
#62381 = DIRECTION ( 'NONE',  ( -1.000000000000000000, -1.777766061779359009E-15, 2.411074791516012434E-29 ) ) ;
#62383 = EDGE_CURVE ( 'NONE', #16304, #64817, #72801, .T. ) ;
#62382 = AXIS2_PLACEMENT_3D ( 'NONE', #89624, #7391, #41886 ) ;
#62384 = DIRECTION ( 'NONE',  ( 1.000000000000000000, 0.000000000000000000, 9.462128050782575008E-16 ) ) ;
#62385 = FACE_OUTER_BOUND ( 'NONE', #74073, .T. ) ;
#62386 = EDGE_CURVE ( 'NONE', #37616, #39094, #64441, .T. ) ;
#62387 = FACE_OUTER_BOUND ( 'NONE', #71752, .T. ) ;
#62389 = ORIENTED_EDGE ( 'NONE', *, *, #29172, .F. ) ;
#62388 = CARTESIAN_POINT ( 'NONE',  ( 107.0664832912739968, -18.82844715994099971, 333.4006252759120343 ) ) ;
#62390 = ADVANCED_FACE ( 'NONE', ( #24212 ), #43308, .F. ) ;
#62391 = PLANE ( 'NONE',  #48090 ) ;
#62392 = CARTESIAN_POINT ( 'NONE',  ( 96.78703652860848194, -40.85599721901744630, 251.6422919425777138 ) ) ;
#62393 = CARTESIAN_POINT ( 'NONE',  ( 108.2766895582742848, -26.33922418024667422, 125.9841967044819597 ) ) ;
#62394 = CARTESIAN_POINT ( 'NONE',  ( 115.9437545354735306, -30.06674848629992880, 260.3508633711495008 ) ) ;
#62395 = CIRCLE ( 'NONE', #4374, 2.749999999999974687 ) ;
#62396 = DIRECTION ( 'NONE',  ( 0.000000000000000000, 1.000000000000000000, -2.731847993664264698E-16 ) ) ;
#62398 = LINE ( 'NONE', #22426, #67517 ) ;
#62397 = DIRECTION ( 'NONE',  ( 0.000000000000000000, 0.000000000000000000, 1.000000000000000000 ) ) ;
#62399 = LINE ( 'NONE', #55555, #74078 ) ;
#62400 = EDGE_CURVE ( 'NONE', #23269, #31479, #83930, .T. ) ;
#62401 = CARTESIAN_POINT ( 'NONE',  ( 31.46648329127298993, 12.92155284005730387, 355.9756252759109998 ) ) ;
#62402 = EDGE_CURVE ( 'NONE', #30574, #1430, #85442, .T. ) ;
#62403 = VERTEX_POINT ( 'NONE', #47755 ) ;
#62404 = CARTESIAN_POINT ( 'NONE',  ( 52.38749999999999574, 94.53880000000000905, 250.8250000000000171 ) ) ;
#62405 = ORIENTED_EDGE ( 'NONE', *, *, #50205, .F. ) ;
#62406 = CARTESIAN_POINT ( 'NONE',  ( 108.3843752505750331, -28.29029480288096465, 189.3752769709339816 ) ) ;
#62408 = ORIENTED_EDGE ( 'NONE', *, *, #60636, .T. ) ;
#62407 = CARTESIAN_POINT ( 'NONE',  ( 105.7129185420862427, -46.72347023951986955, 187.4693006236904580 ) ) ;
#62409 = CARTESIAN_POINT ( 'NONE',  ( 75.31670390244798341, -50.82844715994100682, 35.51780685541480409 ) ) ;
#62410 = CARTESIAN_POINT ( 'NONE',  ( 98.87380182923587313, -30.31772012733814492, 151.7984824187679465 ) ) ;
#62411 = CARTESIAN_POINT ( 'NONE',  ( 180.2121375201600131, -29.73316016639650172, -5.074374724088000832 ) ) ;
#62412 = CARTESIAN_POINT ( 'NONE',  ( 97.81168731305311326, -40.51740136754563082, 36.63591984386916067 ) ) ;
#62413 = ADVANCED_FACE ( 'NONE', ( #61393 ), #55002, .F. ) ;
#62414 = DIRECTION ( 'NONE',  ( -1.000000000000000078E-15, 1.000000000000000083E-30, 1.000000000000000000 ) ) ;
#62415 = CARTESIAN_POINT ( 'NONE',  ( 123.6837132603318992, -53.34645651782490461, 239.5838068554164693 ) ) ;
#62416 = DIRECTION ( 'NONE',  ( 3.100000000000000258E-29, -3.100000000000000044E-14, -1.000000000000000000 ) ) ;
#62417 = CARTESIAN_POINT ( 'NONE',  ( 107.5699729851651938, -26.92841289699908458, 95.03562527591097364 ) ) ;
#62418 = ORIENTED_EDGE ( 'NONE', *, *, #10795, .T. ) ;
#62419 = AXIS2_PLACEMENT_3D ( 'NONE', #69036, #61311, #6800 ) ;
#62420 = ORIENTED_EDGE ( 'NONE', *, *, #16336, .F. ) ;
#62421 = VERTEX_POINT ( 'NONE', #19619 ) ;
#62422 = DIRECTION ( 'NONE',  ( 0.9659258262890670910, 0.000000000000000000, 0.2588190451025250693 ) ) ;
#62423 =( BOUNDED_CURVE ( )  B_SPLINE_CURVE ( 2, ( #62874, #28352, #56045 ),
 .UNSPECIFIED., .F., .T. ) 
 B_SPLINE_CURVE_WITH_KNOTS ( ( 3, 3 ),
 ( 0.01169420784674039988, 0.5170228498526580063 ),
 .UNSPECIFIED. ) 
 CURVE ( )  GEOMETRIC_REPRESENTATION_ITEM ( )  RATIONAL_B_SPLINE_CURVE ( ( 1.000420656333759872, 1.009299002520659849, 1.000000000000000000 ) ) 
 REPRESENTATION_ITEM ( '' )  );
#62425 = DIRECTION ( 'NONE',  ( 1.000000000000000000, 1.000000000000000078E-15, 0.000000000000000000 ) ) ;
#62424 = CARTESIAN_POINT ( 'NONE',  ( 107.6181574201208520, -47.08485352040289484, 193.6308633711479672 ) ) ;
#62426 = CARTESIAN_POINT ( 'NONE',  ( 130.5667039024479834, -39.24694715994093741, 239.5838068554170377 ) ) ;
#62427 = CYLINDRICAL_SURFACE ( 'NONE', #77105, 4.874999999999990230 ) ;
#62428 = DIRECTION ( 'NONE',  ( 0.5000000000000016653, -0.8660254037844377084, 2.684678751731758716E-14 ) ) ;
#62429 = VECTOR ( 'NONE', #5921, 1000.000000000000000 ) ;
#62430 = EDGE_CURVE ( 'NONE', #84035, #9037, #69568, .T. ) ;
#62431 = CYLINDRICAL_SURFACE ( 'NONE', #55001, 2.030000000002086580 ) ;
#62432 = CARTESIAN_POINT ( 'NONE',  ( 68.23039785489001474, -68.99015375674828476, 247.3122147236876458 ) ) ;
#62433 = EDGE_CURVE ( 'NONE', #4309, #41740, #30293, .T. ) ;
#62434 = CARTESIAN_POINT ( 'NONE',  ( 99.07096106853131801, -43.38529345585687480, 116.8784824187679732 ) ) ;
#62435 = VERTEX_POINT ( 'NONE', #20969 ) ;
#62436 = ORIENTED_EDGE ( 'NONE', *, *, #12054, .T. ) ;
#62437 = ORIENTED_EDGE ( 'NONE', *, *, #30016, .T. ) ;
#62438 = EDGE_CURVE ( 'NONE', #6607, #13307, #47306, .T. ) ;
#62439 = CIRCLE ( 'NONE', #76902, 42.54500000000000171 ) ;
#62440 = CARTESIAN_POINT ( 'NONE',  ( 31.71315051185499811, -33.70561438052111214, 342.9256252759109884 ) ) ;
#62441 = CARTESIAN_POINT ( 'NONE',  ( 0.000000000000000000, 44.45000000000000284, 130.5560000000000116 ) ) ;
#62442 = ADVANCED_FACE ( 'NONE', ( #82770 ), #25565, .F. ) ;
#62443 = DIRECTION ( 'NONE',  ( 9.912705577010326536E-16, 1.000000000000000000, 0.000000000000000000 ) ) ;
#62444 = CARTESIAN_POINT ( 'NONE',  ( 112.3000890867684234, -42.99355894011079471, 190.9480903695919665 ) ) ;
#62445 = AXIS2_PLACEMENT_3D ( 'NONE', #61810, #82745, #12794 ) ;
#62446 = DIRECTION ( 'NONE',  ( -1.000000000000000078E-15, -1.000000000000000083E-30, 1.000000000000000000 ) ) ;
#62447 = DIRECTION ( 'NONE',  ( -3.100000000000000258E-29, 3.100000000000000044E-14, 1.000000000000000000 ) ) ;
#62448 = ORIENTED_EDGE ( 'NONE', *, *, #29678, .T. ) ;
#62450 = ORIENTED_EDGE ( 'NONE', *, *, #3636, .F. ) ;
#62449 = ORIENTED_EDGE ( 'NONE', *, *, #16071, .F. ) ;
#62451 = CIRCLE ( 'NONE', #23325, 4.000000000000006217 ) ;
#62452 = CARTESIAN_POINT ( 'NONE',  ( 136.6880318146010325, -19.56139158947305390, 2.921136715971410336 ) ) ;
#62453 = ORIENTED_EDGE ( 'NONE', *, *, #85813, .F. ) ;
#62454 = ORIENTED_EDGE ( 'NONE', *, *, #7251, .T. ) ;
#62455 = CARTESIAN_POINT ( 'NONE',  ( 78.88274585166998065, -21.21170328186978082, 8.006085407566775558 ) ) ;
#62456 = CARTESIAN_POINT ( 'NONE',  ( 114.8460652499425123, -41.03528437643323201, 259.8558690201828654 ) ) ;
#62457 = ORIENTED_EDGE ( 'NONE', *, *, #61668, .T. ) ;
#62458 = MECHANICAL_DESIGN_GEOMETRIC_PRESENTATION_REPRESENTATION (  '', ( #24725 ), #30374 ) ;
#62459 = LINE ( 'NONE', #55613, #4450 ) ;
#62460 = CARTESIAN_POINT ( 'NONE',  ( -124.6636586881827355, 70.76753038983027011, 38.78354852543069597 ) ) ;
#62461 = EDGE_LOOP ( 'NONE', ( #60970, #10256, #5531, #86412 ) ) ;
#62462 = ORIENTED_EDGE ( 'NONE', *, *, #2519, .T. ) ;
#62463 = DIRECTION ( 'NONE',  ( 9.351236661543306751E-17, -3.725950533538267725E-29, -1.000000000000000000 ) ) ;
#62464 = ORIENTED_EDGE ( 'NONE', *, *, #29617, .F. ) ;
#62465 = EDGE_LOOP ( 'NONE', ( #42116, #23626, #55741, #7893 ) ) ;
#62466 = VECTOR ( 'NONE', #9070, 1000.000000000000000 ) ;
#62467 = CARTESIAN_POINT ( 'NONE',  ( 112.3037015629680866, -30.74301476610424544, 287.3214237029247897 ) ) ;
#62468 = CARTESIAN_POINT ( 'NONE',  ( 117.0544076763083297, -30.30483159375883062, 144.2813395616249750 ) ) ;
#62469 = AXIS2_PLACEMENT_3D ( 'NONE', #1078, #84218, #70573 ) ;
#62470 = CARTESIAN_POINT ( 'NONE',  ( 97.56228874418788166, -32.49873190831181802, 100.9927681330539713 ) ) ;
#62471 = CARTESIAN_POINT ( 'NONE',  ( 46.48091746482135278, -49.32844715994084339, 249.9678068554150343 ) ) ;
#62472 = CARTESIAN_POINT ( 'NONE',  ( 131.7155263566451140, -17.29868341350382366, 7.242354772873104807 ) ) ;
#62473 = CARTESIAN_POINT ( 'NONE',  ( 101.4253818664906959, -46.23481170842615740, 203.1622919425779514 ) ) ;
#62474 = CARTESIAN_POINT ( 'NONE',  ( 107.0664832912730020, -36.72944715994189835, 361.9756252759079871 ) ) ;
#62475 = DIRECTION ( 'NONE',  ( 0.000000000000000000, 0.000000000000000000, -1.000000000000000000 ) ) ;
#62476 = ORIENTED_EDGE ( 'NONE', *, *, #44641, .F. ) ;
#62477 = CARTESIAN_POINT ( 'NONE',  ( -129.9449656991350253, 80.88456863959032717, 12.61750076990854552 ) ) ;
#62478 = ORIENTED_EDGE ( 'NONE', *, *, #83162, .T. ) ;
#62479 = ORIENTED_EDGE ( 'NONE', *, *, #14144, .F. ) ;
#62480 = DIRECTION ( 'NONE',  ( 0.000000000000000000, 0.000000000000000000, -1.000000000000000000 ) ) ;
#62481 = VECTOR ( 'NONE', #83350, 1000.000000000000000 ) ;
#62482 = LINE ( 'NONE', #262, #33030 ) ;
#62483 = VECTOR ( 'NONE', #74979, 1000.000000000000000 ) ;
#62484 = EDGE_CURVE ( 'NONE', #40888, #65495, #41831, .T. ) ;
#62485 = CARTESIAN_POINT ( 'NONE',  ( 103.4683284843053883, -46.51414440030927011, 142.2956252759109645 ) ) ;
#62486 = CARTESIAN_POINT ( 'NONE',  ( -5.206817487757472662, 70.96034413118437101, 130.4525921376586552 ) ) ;
#62487 = DIRECTION ( 'NONE',  ( 1.000000000000000000, 1.734723475976805580E-13, 0.000000000000000000 ) ) ;
#62488 = CARTESIAN_POINT ( 'NONE',  ( 72.96458098368650269, 117.4749999999999943, 72.96458098368729850 ) ) ;
#62489 = ADVANCED_FACE ( 'NONE', ( #35031, #88237 ), #46851, .T. ) ;
#62492 = CARTESIAN_POINT ( 'NONE',  ( 109.3321198358311932, -26.57584895156214699, 220.9013395616249795 ) ) ;
#62491 = CARTESIAN_POINT ( 'NONE',  ( 31.56670390244800828, -33.35206098992711077, -5.074374724088000832 ) ) ;
#62490 = DIRECTION ( 'NONE',  ( 0.9999999853157766072, 0.0001713722456143214551, -0.000000000000000000 ) ) ;
#62493 = DIRECTION ( 'NONE',  ( -1.224646799147351482E-16, 0.000000000000000000, -1.000000000000000000 ) ) ;
#62494 = FACE_OUTER_BOUND ( 'NONE', #8298, .T. ) ;
#62495 = ORIENTED_EDGE ( 'NONE', *, *, #89595, .T. ) ;
#62496 = CARTESIAN_POINT ( 'NONE',  ( -40.89999999999999858, 53.97500000000000142, 40.79999999999999716 ) ) ;
#62497 = EDGE_CURVE ( 'NONE', #46818, #53446, #60952, .T. ) ;
#62498 = CARTESIAN_POINT ( 'NONE',  ( 6.349999999999999645, 82.54999999999999716, 298.1325000000000500 ) ) ;
#62499 = CARTESIAN_POINT ( 'NONE',  ( 51.06648329127400388, -18.82844715994099971, 335.9181252759120184 ) ) ;
#62500 = ADVANCED_FACE ( 'NONE', ( #16400 ), #82509, .T. ) ;
#62501 = DIRECTION ( 'NONE',  ( -3.576143065239989638E-15, 0.000000000000000000, 1.000000000000000000 ) ) ;
#62502 = AXIS2_PLACEMENT_3D ( 'NONE', #10351, #32121, #65317 ) ;
#62504 = EDGE_LOOP ( 'NONE', ( #31401, #42108 ) ) ;
#62503 = CARTESIAN_POINT ( 'NONE',  ( 108.0181136390867636, -24.86676629934084559, 265.0127681330534415 ) ) ;
#62505 = EDGE_CURVE ( 'NONE', #81090, #6159, #28676, .T. ) ;
#62506 = FACE_OUTER_BOUND ( 'NONE', #44583, .T. ) ;
#62507 = CARTESIAN_POINT ( 'NONE',  ( 105.7175586466805157, -24.93052779236126781, 160.1670538473389627 ) ) ;
#62508 = CARTESIAN_POINT ( 'NONE',  ( 103.5987781142019202, -46.56090220241721767, 53.30705384733997221 ) ) ;
#62509 = CARTESIAN_POINT ( 'NONE',  ( 117.0647351476834643, -39.95015185843580952, 154.5784824187679476 ) ) ;
#62510 = CARTESIAN_POINT ( 'NONE',  ( 109.7248658465021549, -27.00080515782364543, 30.86479194874874921 ) ) ;
#62511 = FACE_OUTER_BOUND ( 'NONE', #76988, .T. ) ;
#62513 = DIRECTION ( 'NONE',  ( 0.000000000000000000, 0.000000000000000000, -1.000000000000000000 ) ) ;
#62512 = CARTESIAN_POINT ( 'NONE',  ( 152.5667039024472444, -23.42844715993586036, 300.4678068554149490 ) ) ;
#62514 = DIRECTION ( 'NONE',  ( 0.9130365726098601531, 0.000000000000000000, 0.4078776986755214828 ) ) ;
#62515 = DIRECTION ( 'NONE',  ( 0.7071067811865415775, 0.000000000000000000, 0.7071067811865535679 ) ) ;
#62516 = ORIENTED_EDGE ( 'NONE', *, *, #87021, .F. ) ;
#62517 = VECTOR ( 'NONE', #51652, 1000.000000000000000 ) ;
#62518 = EDGE_CURVE ( 'NONE', #40389, #68948, #15954, .T. ) ;
#62519 = DIRECTION ( 'NONE',  ( 1.000000000000000000, 1.000000000000000078E-15, 0.000000000000000000 ) ) ;
#62520 = EDGE_CURVE ( 'NONE', #57574, #24397, #21425, .T. ) ;
#62521 = ORIENTED_EDGE ( 'NONE', *, *, #37878, .F. ) ;
#62522 = EDGE_LOOP ( 'NONE', ( #76603, #21278, #82829, #5623, #88877, #77900 ) ) ;
#62523 = AXIS2_PLACEMENT_3D ( 'NONE', #53390, #33428, #18904 ) ;
#62524 = ORIENTED_EDGE ( 'NONE', *, *, #62620, .F. ) ;
#62525 = CARTESIAN_POINT ( 'NONE',  ( 107.2318599658364207, -25.70055450771780059, 76.07657765686298035 ) ) ;
#62526 = DIRECTION ( 'NONE',  ( 0.000000000000000000, 1.000000000000000000, 0.000000000000000000 ) ) ;
#62527 = VECTOR ( 'NONE', #68078, 1000.000000000000000 ) ;
#62528 = ADVANCED_FACE ( 'NONE', ( #43184 ), #1431, .F. ) ;
#62529 = CARTESIAN_POINT ( 'NONE',  ( 145.1686704281712821, -139.0359729423161639, 246.8427441825336928 ) ) ;
#62530 = CARTESIAN_POINT ( 'NONE',  ( 117.0586869608412286, -33.60713302236428746, 170.0670538473399631 ) ) ;
#62531 = CARTESIAN_POINT ( 'NONE',  ( 101.4222765643661006, -43.81150905960179642, 271.4514674471243438 ) ) ;
#62532 = EDGE_LOOP ( 'NONE', ( #76815, #58639, #52391, #51714, #43472, #25839 ) ) ;
#62533 = EDGE_CURVE ( 'NONE', #8809, #15378, #84107, .T. ) ;
#62534 = EDGE_LOOP ( 'NONE', ( #89035, #31636, #18772, #77630 ) ) ;
#62535 = ORIENTED_EDGE ( 'NONE', *, *, #13091, .F. ) ;
#62536 = DIRECTION ( 'NONE',  ( 1.000000000000000078E-15, 0.000000000000000000, 1.000000000000000000 ) ) ;
#62537 = CARTESIAN_POINT ( 'NONE',  ( 103.1875000000000000, 127.0000000000000000, 7.143750000000359535 ) ) ;
#62538 = CARTESIAN_POINT ( 'NONE',  ( 117.0667039024470313, -104.2784471599408960, 17.71780685541799016 ) ) ;
#62539 = CARTESIAN_POINT ( 'NONE',  ( 116.3188053082936051, -32.94429434937755019, 19.13562527591095019 ) ) ;
#62540 = CARTESIAN_POINT ( 'NONE',  ( 82.91466710319107847, 83.38002811471483255, 100.8465607796074011 ) ) ;
#62541 = DIRECTION ( 'NONE',  ( -1.000000000000000000, -2.756263715554006823E-15, 0.000000000000000000 ) ) ;
#62542 = DIRECTION ( 'NONE',  ( 0.000000000000000000, 0.000000000000000000, -1.000000000000000000 ) ) ;
#62543 = DIRECTION ( 'NONE',  ( 1.000000000000000000, 1.346944695195362088E-15, 1.000000000000000078E-15 ) ) ;
#62544 = CARTESIAN_POINT ( 'NONE',  ( 96.36668125800717633, -39.40815171121898430, 16.53372051400597798 ) ) ;
#62545 = DIRECTION ( 'NONE',  ( 1.000000000000000000, 0.000000000000000000, 0.000000000000000000 ) ) ;
#62546 = EDGE_LOOP ( 'NONE', ( #25123, #42732, #84981, #57794 ) ) ;
#62547 = EDGE_CURVE ( 'NONE', #31182, #68744, #21877, .T. ) ;
#62548 = CARTESIAN_POINT ( 'NONE',  ( -160.2664750769284865, 101.5999999999999943, 148.0533267522753818 ) ) ;
#62549 = EDGE_CURVE ( 'NONE', #29308, #34288, #35477, .T. ) ;
#62550 = AXIS2_PLACEMENT_3D ( 'NONE', #22924, #3800, #72407 ) ;
#62551 = CARTESIAN_POINT ( 'NONE',  ( -55.94501007020270578, 55.83380253633427515, 70.71393962117267051 ) ) ;
#62552 = CARTESIAN_POINT ( 'NONE',  ( 109.1833626410332130, -45.12109460632434121, 90.60332846482899072 ) ) ;
#62553 = CIRCLE ( 'NONE', #11853, 8.928099999999993486 ) ;
#62554 = FACE_OUTER_BOUND ( 'NONE', #55838, .T. ) ;
#62555 = DIRECTION ( 'NONE',  ( 0.7071067811865493491, -0.7071067811865456854, 7.071067811865500971E-16 ) ) ;
#62556 = VERTEX_POINT ( 'NONE', #63649 ) ;
#62557 = VERTEX_POINT ( 'NONE', #63197 ) ;
#62558 = CARTESIAN_POINT ( 'NONE',  ( 77.53258422225754032, -35.66080143920403600, 7.039723185228990765 ) ) ;
#62559 = VERTEX_POINT ( 'NONE', #55905 ) ;
#62560 = ORIENTED_EDGE ( 'NONE', *, *, #50320, .F. ) ;
#62561 = CIRCLE ( 'NONE', #7460, 7.143750000000004263 ) ;
#62562 = LINE ( 'NONE', #62112, #48882 ) ;
#62563 = CARTESIAN_POINT ( 'NONE',  ( 97.67166470235704878, -36.60562237181873257, 152.7596785439919813 ) ) ;
#62564 = CARTESIAN_POINT ( 'NONE',  ( -3.299336700116765719, 94.84201444875799325, 118.5128796971597467 ) ) ;
#62565 = CARTESIAN_POINT ( 'NONE',  ( 110.1643932622899200, -46.70643130671602705, 93.81562527591097478 ) ) ;
#62566 = VECTOR ( 'NONE', #38366, 999.9999999999998863 ) ;
#62567 = EDGE_CURVE ( 'NONE', #12422, #14878, #29133, .T. ) ;
#62568 = LINE ( 'NONE', #48459, #35796 ) ;
#62569 = VERTEX_POINT ( 'NONE', #2327 ) ;
#62570 = CARTESIAN_POINT ( 'NONE',  ( -117.8738102209307215, 82.54999999999999716, -12.70000000000041318 ) ) ;
#62571 = ORIENTED_EDGE ( 'NONE', *, *, #17487, .F. ) ;
#62572 = ORIENTED_EDGE ( 'NONE', *, *, #8109, .T. ) ;
#62573 = CIRCLE ( 'NONE', #7474, 6.857999999999975671 ) ;
#62574 = CARTESIAN_POINT ( 'NONE',  ( 116.3212776292296127, -32.94146857471318413, 287.6356252759109680 ) ) ;
#62575 = ORIENTED_EDGE ( 'NONE', *, *, #20008, .F. ) ;
#62576 = CARTESIAN_POINT ( 'NONE',  ( 100.4791399132688809, -44.80881982087489490, 12.03276813305398463 ) ) ;
#62577 = CARTESIAN_POINT ( 'NONE',  ( 117.0539910656555094, -30.30509957368958496, 140.2813395616249750 ) ) ;
#62578 = B_SPLINE_CURVE_WITH_KNOTS ( 'NONE', 3,
 ( #23642, #58141, #43604, #57693, #63617, #42699, #15486, #2299, #64519, #65408, #78166, #23211, #64074, #70896, #30002, #1401, #51304, #15025, #16816, #56788, #24081, #30446, #9114, #36813, #50878, #29103, #70439, #44497, #72229, #2746, #84535, #71784, #22293, #85435, #3188, #78615 ),
 .UNSPECIFIED., .F., .F.,
 ( 4, 2, 2, 2, 2, 2, 1, 1, 1, 1, 1, 1, 2, 2, 2, 2, 2, 2, 2, 2, 4 ),
 ( 0.4999721494150220491, 0.5624756307362179797, 0.6249791120574139658, 0.6874825933786099519, 0.7499860746998059380, 0.7501081518117613811, 0.7502302289237168242, 0.7504743831476426985, 0.7509626915954943360, 0.7519393084912020520, 0.7538925422826163736, 0.7577990098654362461, 0.7656119450310676644, 0.7812378153623301680, 0.8124895560248543980, 0.8437412966873787390, 0.8749930373499029690, 0.9062447780124271990, 0.9374965186749515400, 0.9687482593374758810, 1.000000000000000000 ),
 .UNSPECIFIED. ) ;
#62579 = DIRECTION ( 'NONE',  ( 0.9242245927363026414, 0.3818493186865932754, 0.000000000000000000 ) ) ;
#62580 = DIRECTION ( 'NONE',  ( -1.000000000000000000, -1.734723475976808672E-15, 0.000000000000000000 ) ) ;
#62581 = CARTESIAN_POINT ( 'NONE',  ( 107.2322063299336605, -25.67745564896214816, 76.07657765686298035 ) ) ;
#62582 = CIRCLE ( 'NONE', #43706, 34.13125000000000142 ) ;
#62583 = CARTESIAN_POINT ( 'NONE',  ( 108.3334481201889332, -46.73485935054446827, 262.6772919445848515 ) ) ;
#62584 = ORIENTED_EDGE ( 'NONE', *, *, #49953, .T. ) ;
#62585 = CARTESIAN_POINT ( 'NONE',  ( 97.60817236302852962, -39.98324860507392486, 116.5905493758438780 ) ) ;
#62586 = DIRECTION ( 'NONE',  ( 0.000000000000000000, 1.000000000000000000, 0.000000000000000000 ) ) ;
#62588 = ORIENTED_EDGE ( 'NONE', *, *, #43939, .T. ) ;
#62587 = ADVANCED_FACE ( 'NONE', ( #70471 ), #56813, .T. ) ;
#62589 = DIRECTION ( 'NONE',  ( -0.7071067811865436870, 0.7071067811865513475, -7.071067811865430960E-16 ) ) ;
#62590 = DIRECTION ( 'NONE',  ( 1.840813417405305102E-14, 0.000000000000000000, -1.000000000000000000 ) ) ;
#62591 = CARTESIAN_POINT ( 'NONE',  ( 112.9632928630424402, -28.13208318394687524, 44.59848241876795782 ) ) ;
#62592 = DIRECTION ( 'NONE',  ( 0.000000000000000000, 0.000000000000000000, -1.000000000000000000 ) ) ;
#62593 = EDGE_CURVE ( 'NONE', #43862, #29586, #89766, .T. ) ;
#62594 = CARTESIAN_POINT ( 'NONE',  ( 69.21917243687391874, 92.62461542576163254, 55.06468400917383832 ) ) ;
#62595 = DIRECTION ( 'NONE',  ( 0.000000000000000000, 1.000000000000000000, 0.000000000000000000 ) ) ;
#62596 = EDGE_CURVE ( 'NONE', #16017, #82548, #12862, .T. ) ;
#62597 = CARTESIAN_POINT ( 'NONE',  ( 97.69287098190314111, -33.93680905855605801, 31.09562527591097592 ) ) ;
#62599 = CARTESIAN_POINT ( 'NONE',  ( 96.05093434719803724, -37.29646042206077539, 117.3794347997199594 ) ) ;
#62598 = CARTESIAN_POINT ( 'NONE',  ( 107.0667039024479834, -36.72944715994100306, 239.5838068554170093 ) ) ;
#62600 = CARTESIAN_POINT ( 'NONE',  ( 20.03715912545641231, -24.95799193693202156, 180.4678068554150911 ) ) ;
#62601 = DIRECTION ( 'NONE',  ( 0.000000000000000000, 1.000000000000000000, 0.000000000000000000 ) ) ;
#62602 = ORIENTED_EDGE ( 'NONE', *, *, #36838, .T. ) ;
#62603 = PLANE ( 'NONE',  #86061 ) ;
#62604 = AXIS2_PLACEMENT_3D ( 'NONE', #13925, #731, #29354 ) ;
#62605 = ADVANCED_FACE ( 'NONE', ( #64548 ), #30027, .F. ) ;
#62606 = FACE_BOUND ( 'NONE', #42958, .T. ) ;
#62607 = CARTESIAN_POINT ( 'NONE',  ( 142.0664832912740394, -56.72944715994099596, 14.92562527591100618 ) ) ;
#62608 = VERTEX_POINT ( 'NONE', #57720 ) ;
#62609 = CARTESIAN_POINT ( 'NONE',  ( 113.2479660781328050, -28.76056331078183348, 60.55236680792867787 ) ) ;
#62611 = ORIENTED_EDGE ( 'NONE', *, *, #4195, .F. ) ;
#62610 = CARTESIAN_POINT ( 'NONE',  ( 116.8364808817232756, -40.58936182315601116, 193.5270538473389479 ) ) ;
#62613 = CARTESIAN_POINT ( 'NONE',  ( 130.5667039024479834, -33.42944715994100591, 239.5838068554162987 ) ) ;
#62612 = PRODUCT_DEFINITION_CONTEXT ( 'detailed design', #18985, 'design' ) ;
#62614 = CARTESIAN_POINT ( 'NONE',  ( 98.88183825371838509, -29.26641886349639066, 226.7261014663869503 ) ) ;
#62615 = CARTESIAN_POINT ( 'NONE',  ( 88.24354053934726494, 71.14122173980733521, 96.22129751242573548 ) ) ;
#62616 = CIRCLE ( 'NONE', #3103, 2.517500000000005844 ) ;
#62617 = LINE ( 'NONE', #47629, #21328 ) ;
#62618 = CARTESIAN_POINT ( 'NONE',  ( -546.0365000000000464, 53.97500000000000142, 87.37599999999999056 ) ) ;
#62619 = ORIENTED_EDGE ( 'NONE', *, *, #73887, .F. ) ;
#62620 = EDGE_CURVE ( 'NONE', #70341, #75711, #85461, .T. ) ;
#62621 = VECTOR ( 'NONE', #44469, 1000.000000000000000 ) ;
#62622 = ORIENTED_EDGE ( 'NONE', *, *, #5838, .F. ) ;
#62623 = EDGE_CURVE ( 'NONE', #6147, #83969, #42285, .T. ) ;
#62624 = ORIENTED_EDGE ( 'NONE', *, *, #40552, .T. ) ;
#62625 = ORIENTED_EDGE ( 'NONE', *, *, #16121, .F. ) ;
#62626 = CARTESIAN_POINT ( 'NONE',  ( 106.5667039024470313, -100.3098201933451747, -19.78219314458212708 ) ) ;
#62627 = CARTESIAN_POINT ( 'NONE',  ( 116.8848192732620390, -41.80628269293674748, 239.4346728949589647 ) ) ;
#62628 = PLANE ( 'NONE',  #53340 ) ;
#62629 = DIRECTION ( 'NONE',  ( 0.000000000000000000, 1.000000000000000000, 0.000000000000000000 ) ) ;
#62631 = EDGE_CURVE ( 'NONE', #82352, #46935, #88344, .T. ) ;
#62630 = AXIS2_PLACEMENT_3D ( 'NONE', #38739, #38294, #80103 ) ;
#62633 = DIRECTION ( 'NONE',  ( 0.000000000000000000, 1.000000000000000000, 0.000000000000000000 ) ) ;
#62632 = CARTESIAN_POINT ( 'NONE',  ( 151.0371591254572934, -24.42818131005592974, 300.4678068554149490 ) ) ;
#62634 = CARTESIAN_POINT ( 'NONE',  ( 107.0664832912739399, -36.72944715994095333, 311.3356252759109566 ) ) ;
#62635 = CARTESIAN_POINT ( 'NONE',  ( 118.7574168473771152, -34.64232270468420438, 48.96705384733895983 ) ) ;
#62636 = VERTEX_POINT ( 'NONE', #518 ) ;
#62637 = AXIS2_PLACEMENT_3D ( 'NONE', #74023, #53545, #81314 ) ;
#62638 = EDGE_LOOP ( 'NONE', ( #7065, #1737, #13801, #63307 ) ) ;
#62639 = AXIS2_PLACEMENT_3D ( 'NONE', #66399, #25074, #5083 ) ;
#62640 = CARTESIAN_POINT ( 'NONE',  ( 89.17003477451882532, -56.47944715994104570, 14.92562527591095289 ) ) ;
#62641 = FACE_OUTER_BOUND ( 'NONE', #29626, .T. ) ;
#62642 = CARTESIAN_POINT ( 'NONE',  ( 101.2091419812965256, -45.28691980162477648, 238.1108633711489517 ) ) ;
#62643 = CIRCLE ( 'NONE', #40843, 4.000000000000002665 ) ;
#62644 = FACE_OUTER_BOUND ( 'NONE', #17809, .T. ) ;
#62645 = CARTESIAN_POINT ( 'NONE',  ( 114.7602587138392209, -43.68247563549507362, 79.25372051400597684 ) ) ;
#62646 = FACE_OUTER_BOUND ( 'NONE', #72459, .T. ) ;
#62647 = VECTOR ( 'NONE', #16486, 1000.000000000000000 ) ;
#62648 = CARTESIAN_POINT ( 'NONE',  ( 103.2881778167501921, -27.47069784023410577, 21.38479467184932048 ) ) ;
#62649 = EDGE_LOOP ( 'NONE', ( #51910, #86731, #10520, #19144 ) ) ;
#62650 = CARTESIAN_POINT ( 'NONE',  ( 0.000000000000000000, 67.86880000000000734, 265.5569999999999595 ) ) ;
#62651 = ORIENTED_EDGE ( 'NONE', *, *, #64339, .T. ) ;
#62652 = ORIENTED_EDGE ( 'NONE', *, *, #25587, .F. ) ;
#62653 = EDGE_CURVE ( 'NONE', #66921, #49274, #86835, .T. ) ;
#62654 = CARTESIAN_POINT ( 'NONE',  ( -92.31685958143586390, 83.38015080693119785, 74.38497350661531016 ) ) ;
#62655 = CARTESIAN_POINT ( 'NONE',  ( 101.1777422249941338, -43.35145646725580804, 263.4301547344683740 ) ) ;
#62656 = CARTESIAN_POINT ( 'NONE',  ( 34.33598329127499227, -36.32844715994100682, -5.074374724088000832 ) ) ;
#62657 = DIRECTION ( 'NONE',  ( 6.745093096447288888E-17, 1.000000000000000000, 0.000000000000000000 ) ) ;
#62658 = PLANE ( 'NONE',  #53360 ) ;
#62659 = CARTESIAN_POINT ( 'NONE',  ( 76.20754074253719068, 75.15251084995277608, -90.81844170390297677 ) ) ;
#62660 = ORIENTED_EDGE ( 'NONE', *, *, #21401, .T. ) ;
#62661 = LINE ( 'NONE', #76745, #88504 ) ;
#62662 = LINE ( 'NONE', #40867, #38269 ) ;
#62663 = ORIENTED_EDGE ( 'NONE', *, *, #10513, .T. ) ;
#62664 = CARTESIAN_POINT ( 'NONE',  ( 112.7417948769132039, -27.24419935825454431, 54.65943479971996055 ) ) ;
#62665 = ORIENTED_EDGE ( 'NONE', *, *, #28939, .F. ) ;
#62666 = CARTESIAN_POINT ( 'NONE',  ( 113.7913882254195101, -32.05415687329151098, 277.1280903695913480 ) ) ;
#62667 = CARTESIAN_POINT ( 'NONE',  ( 270.8910000000000196, 40.03750000000000142, 10.66800000000000104 ) ) ;
#62668 = CARTESIAN_POINT ( 'NONE',  ( 107.6181574201208662, -47.08485352040301564, 197.6308633711499567 ) ) ;
#62669 = ADVANCED_FACE ( 'NONE', ( #17733 ), #79081, .T. ) ;
#62670 = CARTESIAN_POINT ( 'NONE',  ( 23.58223258890940954, 80.15849456350082392, 298.7647790503681335 ) ) ;
#62671 = CARTESIAN_POINT ( 'NONE',  ( 107.0667039024467329, -36.72944715994091780, 196.2188068554169718 ) ) ;
#62672 = DIRECTION ( 'NONE',  ( -3.100000000000000258E-29, 3.100000000000000044E-14, 1.000000000000000000 ) ) ;
#62673 = CIRCLE ( 'NONE', #85914, 4.762500000000002842 ) ;
#62674 = FACE_OUTER_BOUND ( 'NONE', #34526, .T. ) ;
#62675 = CARTESIAN_POINT ( 'NONE',  ( 98.90868739403623522, -30.16870437830188934, 236.7870538473399336 ) ) ;
#62676 = CARTESIAN_POINT ( 'NONE',  ( 104.6050160698606959, -46.44121287996537717, 117.3807199075759371 ) ) ;
#62677 = ORIENTED_EDGE ( 'NONE', *, *, #44049, .F. ) ;
#62678 = VECTOR ( 'NONE', #54736, 1000.000000000000114 ) ;
#62679 = EDGE_CURVE ( 'NONE', #1672, #40777, #3218, .T. ) ;
#62680 = CARTESIAN_POINT ( 'NONE',  ( 136.4105765916224584, -38.17027654744433107, 7.249284792663315713 ) ) ;
#62681 = ORIENTED_EDGE ( 'NONE', *, *, #3957, .F. ) ;
#62682 = CARTESIAN_POINT ( 'NONE',  ( 98.80568095843470644, -28.16380313737984764, 111.6870538473389587 ) ) ;
#62683 = CARTESIAN_POINT ( 'NONE',  ( 120.4566699508395402, 47.42106607564514320, -50.34970303805386749 ) ) ;
#62684 = EDGE_LOOP ( 'NONE', ( #67254, #39584 ) ) ;
#62685 = VERTEX_POINT ( 'NONE', #74033 ) ;
#62686 = ORIENTED_EDGE ( 'NONE', *, *, #78237, .F. ) ;
#62687 = DIRECTION ( 'NONE',  ( -6.982966722218760189E-15, 0.000000000000000000, 1.000000000000000000 ) ) ;
#62688 = DIRECTION ( 'NONE',  ( 1.000000000000000078E-15, -1.000000000000000000, 0.000000000000000000 ) ) ;
#62689 = DIRECTION ( 'NONE',  ( 0.000000000000000000, 0.000000000000000000, 1.000000000000000000 ) ) ;
#62690 = CARTESIAN_POINT ( 'NONE',  ( 0.000000000000000000, 210.0000000000000000, 145.6557476874258441 ) ) ;
#62691 = CARTESIAN_POINT ( 'NONE',  ( 85.58420390244808118, -58.72944715994107412, 207.5838068554169809 ) ) ;
#62692 = CARTESIAN_POINT ( 'NONE',  ( 106.0125404296577045, -27.51070622278902533, 157.9852332267339534 ) ) ;
#62693 = CARTESIAN_POINT ( 'NONE',  ( 111.7834783340718872, -46.75425468364281301, 283.9146728949586418 ) ) ;
#62694 = AXIS2_PLACEMENT_3D ( 'NONE', #60640, #66566, #12063 ) ;
#62695 = FACE_OUTER_BOUND ( 'NONE', #27060, .T. ) ;
#62696 = ORIENTED_EDGE ( 'NONE', *, *, #68308, .F. ) ;
#62697 = DIRECTION ( 'NONE',  ( 1.000000000000000000, 0.000000000000000000, 0.000000000000000000 ) ) ;
#62698 = ORIENTED_EDGE ( 'NONE', *, *, #39227, .T. ) ;
#62699 = ORIENTED_EDGE ( 'NONE', *, *, #51314, .F. ) ;
#62700 = AXIS2_PLACEMENT_3D ( 'NONE', #75779, #77125, #22169 ) ;
#62701 = DIRECTION ( 'NONE',  ( 3.999999999999999995E-14, -1.000000000000000000, 4.100000000000000342E-29 ) ) ;
#62702 = CARTESIAN_POINT ( 'NONE',  ( 161.4809174648183898, -48.32844715993547879, 249.9678068554149490 ) ) ;
#62703 = CYLINDRICAL_SURFACE ( 'NONE', #51519, 3.000000000000002665 ) ;
#62704 = DIRECTION ( 'NONE',  ( 0.0001713722456133601202, -0.9999999853157766072, -1.713722456133601401E-19 ) ) ;
#62705 = CARTESIAN_POINT ( 'NONE',  ( 53.56670390244833158, -48.82844715994055917, 249.9678068554150343 ) ) ;
#62706 = EDGE_CURVE ( 'NONE', #5742, #27981, #47023, .T. ) ;
#62707 = CARTESIAN_POINT ( 'NONE',  ( 107.2112434921279629, -45.29864470754334604, 212.0124198280769861 ) ) ;
#62708 = AXIS2_PLACEMENT_3D ( 'NONE', #21631, #21174, #77037 ) ;
#62709 = CARTESIAN_POINT ( 'NONE',  ( 96.61245533174189859, -37.29510205964861314, 76.36991099019697060 ) ) ;
#62710 = VERTEX_POINT ( 'NONE', #58170 ) ;
#62711 = CARTESIAN_POINT ( 'NONE',  ( 99.08946256649487339, -99.09543445804985140, -19.78219314458218392 ) ) ;
#62712 = VERTEX_POINT ( 'NONE', #51777 ) ;
#62713 = ADVANCED_FACE ( 'NONE', ( #44522 ), #79530, .F. ) ;
#62714 = CARTESIAN_POINT ( 'NONE',  ( -87.20837788851378036, 70.80054595721396993, -80.31601367611384035 ) ) ;
#62715 = ORIENTED_EDGE ( 'NONE', *, *, #70327, .T. ) ;
#62716 = DIRECTION ( 'NONE',  ( 0.0001211784769825750168, -0.7071067708032372501, 0.7071067811865437980 ) ) ;
#62717 = ADVANCED_FACE ( 'NONE', ( #3656 ), #31796, .F. ) ;
#62718 = ORIENTED_EDGE ( 'NONE', *, *, #37073, .T. ) ;
#62719 = DIRECTION ( 'NONE',  ( 0.9217329428042198014, 0.3878251953515564066, -1.203464411458912131E-14 ) ) ;
#62720 = DIRECTION ( 'NONE',  ( 0.000000000000000000, 0.000000000000000000, -1.000000000000000000 ) ) ;
#62721 = CARTESIAN_POINT ( 'NONE',  ( 68.70620082986425814, -127.7162791817593757, 247.5270151222840127 ) ) ;
#62722 = CARTESIAN_POINT ( 'NONE',  ( 188.5667039024479834, -58.35344715994099829, 134.4678068554150059 ) ) ;
#62723 = ORIENTED_EDGE ( 'NONE', *, *, #32347, .T. ) ;
#62724 = ADVANCED_FACE ( 'NONE', ( #11357 ), #30471, .T. ) ;
#62725 = CARTESIAN_POINT ( 'NONE',  ( 96.69274360309970007, -38.23738870492909570, 66.44133956162495735 ) ) ;
#62727 = CARTESIAN_POINT ( 'NONE',  ( 83.73314995793998605, 12.92155284005730387, 358.9756252759109998 ) ) ;
#62726 = FACE_OUTER_BOUND ( 'NONE', #27314, .T. ) ;
#62728 = DIRECTION ( 'NONE',  ( -0.4999999999999998890, 0.000000000000000000, 0.8660254037844387076 ) ) ;
#62729 = CYLINDRICAL_SURFACE ( 'NONE', #67347, 5.500000000000000888 ) ;
#62730 = ORIENTED_EDGE ( 'NONE', *, *, #14221, .T. ) ;
#62731 = ADVANCED_FACE ( 'NONE', ( #52213 ), #73129, .T. ) ;
#62732 = AXIS2_PLACEMENT_3D ( 'NONE', #41275, #35364, #61717 ) ;
#62733 = CARTESIAN_POINT ( 'NONE',  ( 68.53801554307389665, 127.0000000000000000, 74.15067561874289481 ) ) ;
#62734 = DIRECTION ( 'NONE',  ( 0.7071067811868710917, -0.7071067811862240537, 0.000000000000000000 ) ) ;
#62735 = CARTESIAN_POINT ( 'NONE',  ( 9.275582543403935176, 73.86526018886296185, 118.1929554227103267 ) ) ;
#62736 = VERTEX_POINT ( 'NONE', #46300 ) ;
#62737 = CARTESIAN_POINT ( 'NONE',  ( 108.5410322698540853, -26.38715707682645117, 100.9641967044829727 ) ) ;
#62739 = DIRECTION ( 'NONE',  ( -0.7071067812163274180, 0.7071067811567677275, -6.612322856138636565E-17 ) ) ;
#62738 = FACE_OUTER_BOUND ( 'NONE', #66391, .T. ) ;
#62740 = LINE ( 'NONE', #83205, #46565 ) ;
#62741 = VECTOR ( 'NONE', #40662, 1000.000000000000000 ) ;
#62742 = DIRECTION ( 'NONE',  ( 1.000000000000000000, 0.000000000000000000, 0.000000000000000000 ) ) ;
#62743 = CARTESIAN_POINT ( 'NONE',  ( 103.4152017835536270, -27.65577212482034497, 126.3813395616249835 ) ) ;
#62745 = ORIENTED_EDGE ( 'NONE', *, *, #71938, .F. ) ;
#62744 = DIRECTION ( 'NONE',  ( -2.999999999999999839E-15, 1.000000000000000000, -2.999999999999999900E-30 ) ) ;
#62746 = CARTESIAN_POINT ( 'NONE',  ( 115.8883252675856994, -30.10835006627626953, 260.3508633711493871 ) ) ;
#62747 = DIRECTION ( 'NONE',  ( 0.000000000000000000, 0.000000000000000000, 1.000000000000000000 ) ) ;
#62748 = CARTESIAN_POINT ( 'NONE',  ( -158.9822249764580135, 101.5999999999999943, 107.9500000000000028 ) ) ;
#62749 = CARTESIAN_POINT ( 'NONE',  ( 127.4058501689330996, -85.76982405743852667, 250.2178068554179902 ) ) ;
#62750 = CARTESIAN_POINT ( 'NONE',  ( 48.85858412957969676, -30.08671355700278127, 117.4678068554150485 ) ) ;
#62751 = VECTOR ( 'NONE', #46446, 1000.000000000000000 ) ;
#62752 = CARTESIAN_POINT ( 'NONE',  ( 68.21308206361896964, -138.8248129988772916, 246.0151717635989996 ) ) ;
#62753 = CARTESIAN_POINT ( 'NONE',  ( -100.6522392491099112, 79.66749569656610674, 83.15048135366490101 ) ) ;
#62754 = CARTESIAN_POINT ( 'NONE',  ( 98.96845470676149148, -30.25173782105007803, 195.7775300378159784 ) ) ;
#62755 = ORIENTED_EDGE ( 'NONE', *, *, #7247, .F. ) ;
#62756 = VERTEX_POINT ( 'NONE', #39057 ) ;
#62757 = EDGE_CURVE ( 'NONE', #51366, #35978, #11418, .T. ) ;
#62758 = CARTESIAN_POINT ( 'NONE',  ( 115.6173342623064713, -34.29738501013303420, 145.4787261630399371 ) ) ;
#62759 = VECTOR ( 'NONE', #66275, 1000.000000000000000 ) ;
#62760 = FACE_OUTER_BOUND ( 'NONE', #53370, .T. ) ;
#62761 = CARTESIAN_POINT ( 'NONE',  ( 98.24556308671769500, -33.49403671529641713, 17.46634521065892898 ) ) ;
#62762 = DIRECTION ( 'NONE',  ( 0.000000000000000000, -1.000000000000000000, 0.000000000000000000 ) ) ;
#62763 = ADVANCED_FACE ( 'NONE', ( #85899 ), #38613, .T. ) ;
#62764 = CARTESIAN_POINT ( 'NONE',  ( 63.56670390244800473, -40.82844715994016127, 249.9678068554150343 ) ) ;
#62765 = DIRECTION ( 'NONE',  ( 0.000000000000000000, 0.000000000000000000, 1.000000000000000000 ) ) ;
#62766 = CARTESIAN_POINT ( 'NONE',  ( 109.7248659187796136, -27.00080517901244193, 105.8647919427923370 ) ) ;
#62767 = DIRECTION ( 'NONE',  ( 0.7071067811865116015, 0.000000000000000000, -0.7071067811865835440 ) ) ;
#62768 = CARTESIAN_POINT ( 'NONE',  ( 117.2062538965840304, -41.07097622818930915, 213.5165776568629781 ) ) ;
#62769 = CARTESIAN_POINT ( 'NONE',  ( 72.06648329127402519, -45.72944715994106701, -4.824374724089063982 ) ) ;
#62770 = VERTEX_POINT ( 'NONE', #72257 ) ;
#62771 = ORIENTED_EDGE ( 'NONE', *, *, #53809, .T. ) ;
#62772 = CARTESIAN_POINT ( 'NONE',  ( 154.5667039024470171, -79.67844715994088745, 155.2178068554179902 ) ) ;
#62773 = CARTESIAN_POINT ( 'NONE',  ( -74.36911441044668436, 82.54999999999999716, -92.32962665258587265 ) ) ;
#62774 = CARTESIAN_POINT ( 'NONE',  ( -479.3614999999999782, 85.41360802895360393, 11.11250000000036131 ) ) ;
#62775 = DIRECTION ( 'NONE',  ( 2.999999999999999839E-15, -1.000000000000000000, 2.999999999999999900E-30 ) ) ;
#62776 = LINE ( 'NONE', #7380, #9368 ) ;
#62777 = ORIENTED_EDGE ( 'NONE', *, *, #9830, .T. ) ;
#62778 = EDGE_CURVE ( 'NONE', #397, #52666, #72316, .T. ) ;
#62779 = CARTESIAN_POINT ( 'NONE',  ( -4.055571906748874689, 94.48660284847177593, 118.2871548781509432 ) ) ;
#62780 = CARTESIAN_POINT ( 'NONE',  ( 117.3350766552244977, -34.92860824786317409, 243.9641967044819637 ) ) ;
#62781 = ORIENTED_EDGE ( 'NONE', *, *, #47223, .F. ) ;
#62782 = CIRCLE ( 'NONE', #78774, 7.937500000000000000 ) ;
#62783 = CARTESIAN_POINT ( 'NONE',  ( 77.76062680957220152, -38.22815166919947671, 7.286367513304666588 ) ) ;
#62784 = DIRECTION ( 'NONE',  ( 3.999999999999999995E-14, -1.000000000000000000, 4.100000000000000342E-29 ) ) ;
#62785 = DIRECTION ( 'NONE',  ( -0.000000000000000000, -1.000000000000000000, -0.000000000000000000 ) ) ;
#62786 = CARTESIAN_POINT ( 'NONE',  ( 114.5896176151078976, -33.49137084947443554, 76.96809036959095351 ) ) ;
#62787 = CARTESIAN_POINT ( 'NONE',  ( 108.9491117623569636, -26.41756539094687639, 160.9327681330539690 ) ) ;
#62788 = DIRECTION ( 'NONE',  ( 1.000000000000000000, -1.387778780781444413E-14, 0.000000000000000000 ) ) ;
#62789 = ORIENTED_EDGE ( 'NONE', *, *, #50391, .F. ) ;
#62790 = CARTESIAN_POINT ( 'NONE',  ( 107.0664832912739968, -0.7548456658612000547, 335.0256252759120343 ) ) ;
#62791 = VERTEX_POINT ( 'NONE', #40404 ) ;
#62792 = VERTEX_POINT ( 'NONE', #32694 ) ;
#62793 = VECTOR ( 'NONE', #83150, 1000.000000000000000 ) ;
#62794 = DIRECTION ( 'NONE',  ( -0.7071067811861110330, -0.7071067811869841124, 0.000000000000000000 ) ) ;
#62795 = ORIENTED_EDGE ( 'NONE', *, *, #89512, .F. ) ;
#62796 = ORIENTED_EDGE ( 'NONE', *, *, #47558, .F. ) ;
#62797 = LINE ( 'NONE', #19687, #75871 ) ;
#62798 = CARTESIAN_POINT ( 'NONE',  ( 93.91125933621934507, -111.8737466215629013, -21.78219314458179667 ) ) ;
#62799 = EDGE_CURVE ( 'NONE', #54222, #42800, #6334, .T. ) ;
#62800 = CARTESIAN_POINT ( 'NONE',  ( 115.9068402959922111, -38.69432841718559501, 103.0628960185529763 ) ) ;
#62801 = CARTESIAN_POINT ( 'NONE',  ( 101.3926005705062749, -45.54394758209068073, 222.1213395616249784 ) ) ;
#62802 = CARTESIAN_POINT ( 'NONE',  ( 101.3611157396114066, -46.16939438856412181, 202.1318157521019430 ) ) ;
#62803 = CARTESIAN_POINT ( 'NONE',  ( 101.1533894386775501, -27.41820966596962705, 61.51467289495899138 ) ) ;
#62804 = FACE_OUTER_BOUND ( 'NONE', #4720, .T. ) ;
#62805 = EDGE_CURVE ( 'NONE', #87042, #75851, #39510, .T. ) ;
#62806 = CARTESIAN_POINT ( 'NONE',  ( 116.3244028009478797, -32.94573790848593120, 95.13562527591096796 ) ) ;
#62807 = EDGE_CURVE ( 'NONE', #9127, #16335, #19067, .T. ) ;
#62808 = ORIENTED_EDGE ( 'NONE', *, *, #65169, .F. ) ;
#62809 = CARTESIAN_POINT ( 'NONE',  ( 3.968749999999229949, 120.6499999999999915, 100.8961411191535973 ) ) ;
#62810 = DIRECTION ( 'NONE',  ( -0.000000000000000000, 1.000000000000000000, 0.000000000000000000 ) ) ;
#62811 = CARTESIAN_POINT ( 'NONE',  ( 70.71519666489237466, -139.3982827360871113, 247.4032816585904868 ) ) ;
#62812 = CARTESIAN_POINT ( 'NONE',  ( 116.3126599349421895, -33.43976754494798342, 114.0984824187689668 ) ) ;
#62813 = AXIS2_PLACEMENT_3D ( 'NONE', #29438, #63960, #42148 ) ;
#62814 = CARTESIAN_POINT ( 'NONE',  ( 106.6586145429690475, -26.26807492067915462, 85.10705384733896040 ) ) ;
#62815 = CARTESIAN_POINT ( 'NONE',  ( 115.0886446791137132, -30.00251675211520919, 269.3813395616250546 ) ) ;
#62816 = ORIENTED_EDGE ( 'NONE', *, *, #43037, .T. ) ;
#62817 = CARTESIAN_POINT ( 'NONE',  ( 96.77592423366979801, -40.76472679528808385, 246.6118157521009664 ) ) ;
#62818 = DIRECTION ( 'NONE',  ( 0.000000000000000000, -1.000000000000000000, 0.000000000000000000 ) ) ;
#62819 = FILL_AREA_STYLE_COLOUR ( '', #87111 ) ;
#62820 = VECTOR ( 'NONE', #78260, 999.9999999999998863 ) ;
#62821 = CARTESIAN_POINT ( 'NONE',  ( 31.46648329127298993, 12.92155284005730387, 358.9756252759109998 ) ) ;
#62822 = CARTESIAN_POINT ( 'NONE',  ( 31.56670390244768143, -32.29483332968644049, 237.4678068554150059 ) ) ;
#62824 = CARTESIAN_POINT ( 'NONE',  ( 68.69398407924357741, -139.3018529721033474, 245.7655250590126457 ) ) ;
#62823 = CARTESIAN_POINT ( 'NONE',  ( 108.1902092590197526, -46.32316586329737618, 277.6356252759110816 ) ) ;
#62825 = CARTESIAN_POINT ( 'NONE',  ( 106.4519520244838588, -25.28636983920703329, 320.5381088016924309 ) ) ;
#62826 = CARTESIAN_POINT ( 'NONE',  ( 82.56670390244703128, -104.2784471599409670, 22.21780685541800082 ) ) ;
#62827 = VECTOR ( 'NONE', #24041, 1000.000000000000000 ) ;
#62828 = FACE_OUTER_BOUND ( 'NONE', #61256, .T. ) ;
#62829 = EDGE_CURVE ( 'NONE', #19003, #25445, #41282, .T. ) ;
#62830 = CYLINDRICAL_SURFACE ( 'NONE', #6609, 0.9999999999999731326 ) ;
#62831 = EDGE_CURVE ( 'NONE', #837, #60890, #67209, .T. ) ;
#62832 = FACE_OUTER_BOUND ( 'NONE', #46967, .T. ) ;
#62833 = DIRECTION ( 'NONE',  ( -1.000000000000000078E-15, 1.000000000000000083E-30, 1.000000000000000000 ) ) ;
#62835 = ORIENTED_EDGE ( 'NONE', *, *, #73281, .T. ) ;
#62834 = DIRECTION ( 'NONE',  ( 0.000000000000000000, 0.000000000000000000, -1.000000000000000000 ) ) ;
#62836 = CARTESIAN_POINT ( 'NONE',  ( 89.44289600121260264, -125.4749327540683197, 250.2178068554180470 ) ) ;
#62837 = CARTESIAN_POINT ( 'NONE',  ( 115.7947005615567235, -30.98796762508558444, 254.2899109901966028 ) ) ;
#62838 = CARTESIAN_POINT ( 'NONE',  ( 117.0231160686283687, -39.93674523842013713, 154.5784824187679476 ) ) ;
#62839 = CARTESIAN_POINT ( 'NONE',  ( 115.9636596525004677, -42.20459941147550609, 14.38705384733995984 ) ) ;
#62840 = CARTESIAN_POINT ( 'NONE',  ( 107.0664832912739968, 19.62155284005901024, 333.4006252759110112 ) ) ;
#62842 = CARTESIAN_POINT ( 'NONE',  ( 81.23646709782372000, -34.23881677343926100, 8.012604158003382437 ) ) ;
#62841 = CARTESIAN_POINT ( 'NONE',  ( 188.5667039024484382, -48.82844715993430640, 175.7178068554150343 ) ) ;
#62843 = CARTESIAN_POINT ( 'NONE',  ( 188.5667039024482392, -42.82844715993431350, 295.7178068554150059 ) ) ;
#62844 = CARTESIAN_POINT ( 'NONE',  ( 129.9468070739257257, 84.21348395916258767, 12.59754631664314317 ) ) ;
#62845 = CIRCLE ( 'NONE', #23714, 3.300000000000000711 ) ;
#62846 = VERTEX_POINT ( 'NONE', #67669 ) ;
#62847 = LINE ( 'NONE', #25314, #72253 ) ;
#62848 = ORIENTED_EDGE ( 'NONE', *, *, #16873, .F. ) ;
#62849 = CARTESIAN_POINT ( 'NONE',  ( 98.50657384982324061, -36.30512124771701821, 170.7095626852199359 ) ) ;
#62851 = ORIENTED_EDGE ( 'NONE', *, *, #64532, .T. ) ;
#62850 = CARTESIAN_POINT ( 'NONE',  ( 80.06648329127402519, -46.72944715994105991, -0.8743747240890559214 ) ) ;
#62852 = AXIS2_PLACEMENT_3D ( 'NONE', #50910, #49553, #21884 ) ;
#62853 = DIRECTION ( 'NONE',  ( -0.8944271909999158554, -1.475804865149861278E-14, -0.4472135954999579277 ) ) ;
#62854 = CARTESIAN_POINT ( 'NONE',  ( 117.4355769707882473, -40.49052663852277334, 169.5375300378159693 ) ) ;
#62855 = CARTESIAN_POINT ( 'NONE',  ( 117.0602965032632596, -38.08466649080754252, 149.7193872050756909 ) ) ;
#62856 = CARTESIAN_POINT ( 'NONE',  ( 123.6837132603319560, -53.34645651782485487, 218.8274735512161158 ) ) ;
#62857 = CARTESIAN_POINT ( 'NONE',  ( 102.6857145224375785, -27.71633897165153471, 86.43730029299915429 ) ) ;
#62858 = CARTESIAN_POINT ( 'NONE',  ( -77.68655577178658689, 72.98405218941670114, 89.55818655986143995 ) ) ;
#62859 = FACE_OUTER_BOUND ( 'NONE', #9202, .T. ) ;
#62860 = B_SPLINE_CURVE_WITH_KNOTS ( 'NONE', 3,
 ( #63230, #548, #1007, #22355, #15541, #50483, #84140, #29606, #77312, #15086, #41422, #57295, #34623, #42760, #70500, #8273, #35970, #62328 ),
 .UNSPECIFIED., .F., .F.,
 ( 4, 2, 2, 2, 2, 2, 2, 2, 4 ),
 ( 0.4999999995531766439, 0.5624999996090295218, 0.6249999996648825107, 0.6874999997207353886, 0.7499999997765882664, 0.8124999998324412553, 0.8749999998882941332, 0.9374999999441471221, 1.000000000000000000 ),
 .UNSPECIFIED. ) ;
#62861 = CARTESIAN_POINT ( 'NONE',  ( 116.7343647603066614, -32.97833357388812914, 94.10895860924495082 ) ) ;
#62862 = ORIENTED_EDGE ( 'NONE', *, *, #36466, .T. ) ;
#62863 = ORIENTED_EDGE ( 'NONE', *, *, #53430, .F. ) ;
#62864 = ORIENTED_EDGE ( 'NONE', *, *, #83740, .F. ) ;
#62865 = TOROIDAL_SURFACE ( 'NONE', #7766, 15.69999999999999929, 0.2999999999999999889 ) ;
#62866 = CARTESIAN_POINT ( 'NONE',  ( 101.0434111811767224, -43.22951492638978266, 43.41301187732599232 ) ) ;
#62867 = CARTESIAN_POINT ( 'NONE',  ( 128.5446125969798459, -121.5356829788754709, 250.2178068554179333 ) ) ;
#62869 = CARTESIAN_POINT ( 'NONE',  ( 82.54999999999999716, 95.25000000000000000, 280.2255000000000109 ) ) ;
#62868 = CARTESIAN_POINT ( 'NONE',  ( 113.2764755850017480, -45.03455287549797248, 184.0994347997199725 ) ) ;
#62870 = DIRECTION ( 'NONE',  ( 0.000000000000000000, 0.000000000000000000, 1.000000000000000000 ) ) ;
#62872 = EDGE_CURVE ( 'NONE', #42590, #10255, #4994, .T. ) ;
#62871 = CARTESIAN_POINT ( 'NONE',  ( 179.4595971212889935, -28.98061976758940617, 117.4678068554150627 ) ) ;
#62873 = DIRECTION ( 'NONE',  ( 0.000000000000000000, 0.000000000000000000, 1.000000000000000000 ) ) ;
#62874 = CARTESIAN_POINT ( 'NONE',  ( 121.2221484686747459, -113.6057974291316839, -19.26696060647573105 ) ) ;
#62875 = CARTESIAN_POINT ( 'NONE',  ( 67.15160367789934526, -67.95867621982013418, 246.0731502186970090 ) ) ;
#62876 = CARTESIAN_POINT ( 'NONE',  ( 113.8292797163802561, -28.77778007523021842, 139.5156252759109634 ) ) ;
#62877 = ORIENTED_EDGE ( 'NONE', *, *, #53206, .F. ) ;
#62878 = ORIENTED_EDGE ( 'NONE', *, *, #18224, .F. ) ;
#62879 = VERTEX_POINT ( 'NONE', #81761 ) ;
#62880 = CARTESIAN_POINT ( 'NONE',  ( 143.5667039024469886, -68.87844715994090450, 222.2178068554179902 ) ) ;
#62881 = DIRECTION ( 'NONE',  ( 0.000000000000000000, 0.000000000000000000, -1.000000000000000000 ) ) ;
#62882 = CARTESIAN_POINT ( 'NONE',  ( 116.8171228668576163, -34.15291832144532691, 80.03145860917631182 ) ) ;
#62883 = CARTESIAN_POINT ( 'NONE',  ( 20.56670390244748603, -48.82844715994200158, 129.9678068554150627 ) ) ;
#62884 = CARTESIAN_POINT ( 'NONE',  ( 112.7646070568428911, -30.84607450481293256, 172.2823760838769829 ) ) ;
#62885 = CIRCLE ( 'NONE', #20814, 3.499999999999996003 ) ;
#62886 = EDGE_CURVE ( 'NONE', #61996, #70380, #5897, .T. ) ;
#62887 = CARTESIAN_POINT ( 'NONE',  ( 69.72411017812960665, 127.0000000000000000, 69.72411017813040246 ) ) ;
#62888 = VECTOR ( 'NONE', #81823, 999.9999999999998863 ) ;
#62889 = CARTESIAN_POINT ( 'NONE',  ( 0.000000000000000000, 223.9999999999999716, 154.6557476874258441 ) ) ;
#62890 = ORIENTED_EDGE ( 'NONE', *, *, #51430, .F. ) ;
#62892 = ORIENTED_EDGE ( 'NONE', *, *, #48520, .F. ) ;
#62891 = ORIENTED_EDGE ( 'NONE', *, *, #12792, .T. ) ;
#62893 = FACE_OUTER_BOUND ( 'NONE', #80662, .T. ) ;
#62894 = ORIENTED_EDGE ( 'NONE', *, *, #55173, .F. ) ;
#62895 = EDGE_LOOP ( 'NONE', ( #2032, #88348 ) ) ;
#62896 = CARTESIAN_POINT ( 'NONE',  ( -76.20505178924278766, 120.6499999999999915, -76.20505178924469192 ) ) ;
#62897 = CARTESIAN_POINT ( 'NONE',  ( 99.03278789346684619, -40.46950289042285220, 253.1044404487540760 ) ) ;
#62898 = EDGE_CURVE ( 'NONE', #32750, #52806, #5448, .T. ) ;
#62899 = DIRECTION ( 'NONE',  ( -0.000000000000000000, -0.000000000000000000, 1.000000000000000000 ) ) ;
#62900 = ORIENTED_EDGE ( 'NONE', *, *, #25677, .F. ) ;
#62901 = CARTESIAN_POINT ( 'NONE',  ( 25.56670390244797275, -62.87844715994099687, 293.2178068554150627 ) ) ;
#62902 = CARTESIAN_POINT ( 'NONE',  ( -124.1113515626113326, 71.86650245416660709, 40.51253187952720225 ) ) ;
#62903 = ORIENTED_EDGE ( 'NONE', *, *, #82703, .T. ) ;
#62904 = ORIENTED_EDGE ( 'NONE', *, *, #9115, .F. ) ;
#62905 = VECTOR ( 'NONE', #69936, 1000.000000000000000 ) ;
#62906 = CARTESIAN_POINT ( 'NONE',  ( 70.63919639214310564, 65.60000000000000853, 56.85413200336923012 ) ) ;
#62907 = AXIS2_PLACEMENT_3D ( 'NONE', #46184, #40283, #33474 ) ;
#62908 = ORIENTED_EDGE ( 'NONE', *, *, #38614, .T. ) ;
#62909 = ORIENTED_EDGE ( 'NONE', *, *, #46780, .F. ) ;
#62910 = EDGE_CURVE ( 'NONE', #13427, #52429, #12713, .T. ) ;
#62911 = CARTESIAN_POINT ( 'NONE',  ( 105.4654256982276905, -28.22429988993499350, 278.0547570362579677 ) ) ;
#62913 = CARTESIAN_POINT ( 'NONE',  ( 116.8162545570497741, -32.97600546270004429, 139.1184824187679396 ) ) ;
#62912 = CIRCLE ( 'NONE', #52699, 4.762500000000002842 ) ;
#62914 = CARTESIAN_POINT ( 'NONE',  ( 96.81317962367440089, -38.48968277746988065, 91.46133956162493917 ) ) ;
#62915 = CARTESIAN_POINT ( 'NONE',  ( 116.2163998817092505, -39.91179612511876940, 249.5838068554169524 ) ) ;
#62916 = LINE ( 'NONE', #1613, #19106 ) ;
#62917 = CARTESIAN_POINT ( 'NONE',  ( 107.5100279102752552, -47.14509671329473406, 233.6099109901969655 ) ) ;
#62918 = FACE_OUTER_BOUND ( 'NONE', #25997, .T. ) ;
#62919 = EDGE_CURVE ( 'NONE', #46976, #21223, #33144, .T. ) ;
#62920 = FACE_OUTER_BOUND ( 'NONE', #22613, .T. ) ;
#62921 = EDGE_LOOP ( 'NONE', ( #11247, #5792, #1336, #6520 ) ) ;
#62922 = CARTESIAN_POINT ( 'NONE',  ( 130.2871811975776382, 72.98383416765814502, -8.394281761908146677 ) ) ;
#62923 = EDGE_LOOP ( 'NONE', ( #68993, #31960, #86298, #6071 ) ) ;
#62924 = ORIENTED_EDGE ( 'NONE', *, *, #20893, .T. ) ;
#62925 = CARTESIAN_POINT ( 'NONE',  ( 172.5664832912740110, -18.82844715994099971, 76.80862527591200717 ) ) ;
#62926 = CARTESIAN_POINT ( 'NONE',  ( 104.9606636336513930, -26.94125731171795479, 136.2451343372883912 ) ) ;
#62927 = ORIENTED_EDGE ( 'NONE', *, *, #52790, .F. ) ;
#62928 = CARTESIAN_POINT ( 'NONE',  ( 102.3126588425671315, -26.75045724741508124, 140.4422919425769578 ) ) ;
#62929 = CARTESIAN_POINT ( 'NONE',  ( 102.0693270851732990, -27.96916624019228337, 255.4897280356127567 ) ) ;
#62930 = DIRECTION ( 'NONE',  ( -0.000000000000000000, -1.000000000000000000, -0.000000000000000000 ) ) ;
#62931 = LINE ( 'NONE', #71120, #65950 ) ;
#62934 = CARTESIAN_POINT ( 'NONE',  ( 97.03753386688410387, -33.96379371595042329, 247.1127681330539758 ) ) ;
#62933 = CARTESIAN_POINT ( 'NONE',  ( 97.93479060588762763, -40.80611092822861252, 56.66021516895607846 ) ) ;
#62932 = DIRECTION ( 'NONE',  ( 0.000000000000000000, 1.000000000000000000, 0.000000000000000000 ) ) ;
#62935 = DIRECTION ( 'NONE',  ( 1.000000000000000000, 0.000000000000000000, 0.000000000000000000 ) ) ;
#62936 = LINE ( 'NONE', #42482, #38073 ) ;
#62937 = ORIENTED_EDGE ( 'NONE', *, *, #71386, .T. ) ;
#62938 = DIRECTION ( 'NONE',  ( 0.000000000000000000, -1.000000000000000000, 0.000000000000000000 ) ) ;
#62939 = EDGE_CURVE ( 'NONE', #22291, #8503, #34691, .T. ) ;
#62940 = CARTESIAN_POINT ( 'NONE',  ( 141.0667039024479834, -58.72944715994110254, 250.9178068554160461 ) ) ;
#62941 = EDGE_CURVE ( 'NONE', #62232, #18115, #69015, .T. ) ;
#62942 = DIRECTION ( 'NONE',  ( 0.000000000000000000, 1.000000000000000000, 0.000000000000000000 ) ) ;
#62943 = ADVANCED_FACE ( 'NONE', ( #54452 ), #81143, .F. ) ;
#62944 = DIRECTION ( 'NONE',  ( 0.000000000000000000, 0.000000000000000000, -1.000000000000000000 ) ) ;
#62946 = ORIENTED_EDGE ( 'NONE', *, *, #37600, .F. ) ;
#62945 = CARTESIAN_POINT ( 'NONE',  ( 112.3606361654194075, -28.17110760307337713, 289.6356252759109680 ) ) ;
#62947 = CARTESIAN_POINT ( 'NONE',  ( 179.4595971212720258, -26.00627455219131789, -5.074374724088000832 ) ) ;
#62948 = CARTESIAN_POINT ( 'NONE',  ( 97.98778932149404852, -30.38336575973633913, 160.8289586092449497 ) ) ;
#62949 = CARTESIAN_POINT ( 'NONE',  ( 100.4110913530865332, -28.70521849941338033, 36.62705384733894221 ) ) ;
#62950 = CARTESIAN_POINT ( 'NONE',  ( 117.1680251128577908, -33.85633223813928794, 145.0470538473399529 ) ) ;
#62951 = ADVANCED_FACE ( 'NONE', ( #68570, #60838 ), #82215, .T. ) ;
#62952 = CARTESIAN_POINT ( 'NONE',  ( 152.0368932755770288, -23.42844715993589588, 237.4678068554150059 ) ) ;
#62953 = CARTESIAN_POINT ( 'NONE',  ( 115.0887396973123202, -30.61742992443682354, 100.3440234672758038 ) ) ;
#62955 = DIRECTION ( 'NONE',  ( 1.000000000000000000, 0.000000000000000000, 0.000000000000000000 ) ) ;
#62954 = CARTESIAN_POINT ( 'NONE',  ( 97.81168895331838087, -40.51742574516882200, 287.6356252759109680 ) ) ;
#62956 = CARTESIAN_POINT ( 'NONE',  ( 108.4174892599855866, -26.73503592884603108, 69.96895860861965843 ) ) ;
#62957 = CARTESIAN_POINT ( 'NONE',  ( 72.96458098368650269, 101.5999999999999943, 78.00648098368728256 ) ) ;
#62958 = VERTEX_POINT ( 'NONE', #82665 ) ;
#62959 = AXIS2_PLACEMENT_3D ( 'NONE', #79726, #2525, #2075 ) ;
#62960 = DIRECTION ( 'NONE',  ( 1.000000000000000000, 1.000000000000000078E-15, 0.000000000000000000 ) ) ;
#62961 =( BOUNDED_CURVE ( )  B_SPLINE_CURVE ( 3, ( #27114, #5783, #25762, #81652 ),
 .UNSPECIFIED., .F., .T. ) 
 B_SPLINE_CURVE_WITH_KNOTS ( ( 4, 4 ),
 ( 2.671434693666587812, 3.611750613512999308 ),
 .UNSPECIFIED. ) 
 CURVE ( )  GEOMETRIC_REPRESENTATION_ITEM ( )  RATIONAL_B_SPLINE_CURVE ( ( 1.000000000000000000, 0.9276644927932375939, 0.9276644927932375939, 1.000000000000000000 ) ) 
 REPRESENTATION_ITEM ( '' )  );
#62962 = VECTOR ( 'NONE', #76899, 1000.000000000000000 ) ;
#62963 = EDGE_LOOP ( 'NONE', ( #65136, #64070, #49252, #65743 ) ) ;
#62964 = EDGE_LOOP ( 'NONE', ( #23188, #48134, #43323, #88948 ) ) ;
#62966 = ORIENTED_EDGE ( 'NONE', *, *, #74881, .T. ) ;
#62965 = FACE_OUTER_BOUND ( 'NONE', #68462, .T. ) ;
#62967 = CARTESIAN_POINT ( 'NONE',  ( 101.1541078795468707, -28.12664281037979208, 46.55562527591094835 ) ) ;
#62968 = DIRECTION ( 'NONE',  ( 0.000000000000000000, 0.000000000000000000, 1.000000000000000000 ) ) ;
#62969 = FACE_OUTER_BOUND ( 'NONE', #21483, .T. ) ;
#62970 = CARTESIAN_POINT ( 'NONE',  ( 113.6415746488294047, -45.67179987042115386, 179.0689586092439640 ) ) ;
#62971 = CARTESIAN_POINT ( 'NONE',  ( 114.5649785483395249, -40.87970871860825639, 262.8467055423626562 ) ) ;
#62972 = VERTEX_POINT ( 'NONE', #68117 ) ;
#62973 = ORIENTED_EDGE ( 'NONE', *, *, #13021, .T. ) ;
#62974 = ORIENTED_EDGE ( 'NONE', *, *, #32138, .F. ) ;
#62975 = VECTOR ( 'NONE', #50034, 1000.000000000000000 ) ;
#62976 = ORIENTED_EDGE ( 'NONE', *, *, #55199, .T. ) ;
#62977 = LINE ( 'NONE', #64780, #19599 ) ;
#62978 = AXIS2_PLACEMENT_3D ( 'NONE', #40501, #82763, #75922 ) ;
#62979 = CARTESIAN_POINT ( 'NONE',  ( 199.3900000000000148, 59.08750000000000568, -50.79999999999999716 ) ) ;
#62980 = CARTESIAN_POINT ( 'NONE',  ( 188.5667039024484097, -48.82844715993431350, 257.2178068554150059 ) ) ;
#62981 = AXIS2_PLACEMENT_3D ( 'NONE', #46605, #25282, #60238 ) ;
#62982 = CARTESIAN_POINT ( 'NONE',  ( 115.0889047232446671, -30.61763667893183083, 74.34395860934252198 ) ) ;
#62983 = CARTESIAN_POINT ( 'NONE',  ( 89.38347482486577178, 94.60320878023492241, 95.16331303980217626 ) ) ;
#62984 = DIRECTION ( 'NONE',  ( 0.000000000000000000, 1.000000000000000000, 0.000000000000000000 ) ) ;
#62986 = DIRECTION ( 'NONE',  ( 0.000000000000000000, 0.000000000000000000, -1.000000000000000000 ) ) ;
#62985 = CIRCLE ( 'NONE', #10781, 4.762500000000001066 ) ;
#62987 = DIRECTION ( 'NONE',  ( -1.000000000000000000, 0.000000000000000000, 0.000000000000000000 ) ) ;
#62988 = CARTESIAN_POINT ( 'NONE',  ( 116.1393041698828057, -43.00708073170995505, 13.35657765686298859 ) ) ;
#62989 = PLANE ( 'NONE',  #53007 ) ;
#62990 = ORIENTED_EDGE ( 'NONE', *, *, #72591, .F. ) ;
#62991 = CARTESIAN_POINT ( 'NONE',  ( 29.56670390244797630, -67.87844715994100397, 20.91780685541479912 ) ) ;
#62992 = CARTESIAN_POINT ( 'NONE',  ( -55.79405894393751453, 55.29575870445238195, 70.75673509094546887 ) ) ;
#62993 = CARTESIAN_POINT ( 'NONE',  ( 111.9804352529405804, -29.60526291441071578, 87.42618560768700320 ) ) ;
#62994 = EDGE_CURVE ( 'NONE', #74036, #7464, #48531, .T. ) ;
#62995 = EDGE_CURVE ( 'NONE', #57373, #73910, #1317, .T. ) ;
#62996 = CYLINDRICAL_SURFACE ( 'NONE', #25304, 9.999999999999998224 ) ;
#62997 = CYLINDRICAL_SURFACE ( 'NONE', #30047, 0.2500000000000002220 ) ;
#62998 = ORIENTED_EDGE ( 'NONE', *, *, #25970, .T. ) ;
#62999 = ORIENTED_EDGE ( 'NONE', *, *, #16682, .T. ) ;
#63000 = EDGE_CURVE ( 'NONE', #16763, #77789, #26011, .T. ) ;
#63001 = CARTESIAN_POINT ( 'NONE',  ( 77.31648329127401098, -36.72944715994107412, 6.749768910606400496 ) ) ;
#63002 = ORIENTED_EDGE ( 'NONE', *, *, #25695, .F. ) ;
#63003 = ORIENTED_EDGE ( 'NONE', *, *, #25665, .T. ) ;
#63004 = EDGE_CURVE ( 'NONE', #37766, #64042, #48093, .T. ) ;
#63005 = CARTESIAN_POINT ( 'NONE',  ( 112.1755263188685205, -29.48886997617658423, 126.0187261630399718 ) ) ;
#63006 = EDGE_CURVE ( 'NONE', #64746, #12239, #43075, .T. ) ;
#63007 = CARTESIAN_POINT ( 'NONE',  ( -2.078103260390279150, 95.08570091005914549, 118.5384849238115805 ) ) ;
#63008 = CARTESIAN_POINT ( 'NONE',  ( 114.7233776882958409, -44.73301973330935510, 109.1718157521009687 ) ) ;
#63009 = EDGE_CURVE ( 'NONE', #72100, #14882, #9041, .T. ) ;
#63010 = CIRCLE ( 'NONE', #86240, 2.117000000000000881 ) ;
#63011 = CARTESIAN_POINT ( 'NONE',  ( 108.3334480752073858, -46.73485935666047908, 83.67729194100738255 ) ) ;
#63012 = ORIENTED_EDGE ( 'NONE', *, *, #48728, .F. ) ;
#63013 = DIRECTION ( 'NONE',  ( 0.8660254037844392627, -0.4999999999999990008, 1.549999999999999706E-14 ) ) ;
#63014 = CIRCLE ( 'NONE', #29705, 8.928100000000000591 ) ;
#63015 = ORIENTED_EDGE ( 'NONE', *, *, #71114, .T. ) ;
#63016 = ORIENTED_EDGE ( 'NONE', *, *, #71993, .F. ) ;
#63017 = ADVANCED_FACE ( 'NONE', ( #62641 ), #69915, .T. ) ;
#63018 = DIRECTION ( 'NONE',  ( 1.000000000000000000, -3.885780586188044357E-13, 0.000000000000000000 ) ) ;
#63019 = ORIENTED_EDGE ( 'NONE', *, *, #88559, .F. ) ;
#63020 = CARTESIAN_POINT ( 'NONE',  ( 117.6440887749188846, -33.30491810902906735, 284.0756252759109657 ) ) ;
#63021 = CARTESIAN_POINT ( 'NONE',  ( 98.36161695517027681, -29.88032255785606139, 196.8080062282919869 ) ) ;
#63022 = ADVANCED_FACE ( 'NONE', ( #77624, #14507 ), #7681, .F. ) ;
#63023 = CARTESIAN_POINT ( 'NONE',  ( 182.2300522401149863, -33.89581943344511217, 193.9678068554150059 ) ) ;
#63024 = DIRECTION ( 'NONE',  ( 1.000000000000000078E-15, 1.000000000000000083E-30, -1.000000000000000000 ) ) ;
#63025 = CARTESIAN_POINT ( 'NONE',  ( 109.2014185099688603, -26.52530387367253795, 135.9127681330539872 ) ) ;
#63026 = EDGE_CURVE ( 'NONE', #10101, #59400, #54957, .T. ) ;
#63027 = DIRECTION ( 'NONE',  ( 1.000000000000000000, 4.510281037539788691E-14, 0.000000000000000000 ) ) ;
#63028 = ORIENTED_EDGE ( 'NONE', *, *, #63540, .T. ) ;
#63029 = CARTESIAN_POINT ( 'NONE',  ( 97.80435755565518718, -40.49946745241530266, 116.6343656781801599 ) ) ;
#63030 = DIRECTION ( 'NONE',  ( 0.000000000000000000, 0.000000000000000000, -1.000000000000000000 ) ) ;
#63031 = ORIENTED_EDGE ( 'NONE', *, *, #84610, .T. ) ;
#63032 = AXIS2_PLACEMENT_3D ( 'NONE', #46338, #47688, #25928 ) ;
#63033 = CARTESIAN_POINT ( 'NONE',  ( 76.06670390244792657, -14.72944715994109899, 239.5838068554169809 ) ) ;
#63034 = VECTOR ( 'NONE', #28208, 1000.000000000000000 ) ;
#63035 = AXIS2_PLACEMENT_3D ( 'NONE', #69013, #34023, #89463 ) ;
#63036 = DIRECTION ( 'NONE',  ( 1.000000000000000000, 1.387778780781444413E-14, 0.000000000000000000 ) ) ;
#63037 = CARTESIAN_POINT ( 'NONE',  ( 99.98060178585627966, -44.37649324013435859, 46.98133956162592284 ) ) ;
#63038 = DIRECTION ( 'NONE',  ( -0.7071067811865336949, -0.7071067811865614505, 0.000000000000000000 ) ) ;
#63039 = VECTOR ( 'NONE', #80164, 1000.000000000000000 ) ;
#63040 = LINE ( 'NONE', #33984, #17295 ) ;
#63041 = CARTESIAN_POINT ( 'NONE',  ( -215.9010000000000105, 52.73749999999999716, -52.38749999999999574 ) ) ;
#63042 = CARTESIAN_POINT ( 'NONE',  ( 101.9462936730086113, -46.59842863024385196, 17.19562527591095247 ) ) ;
#63044 = CARTESIAN_POINT ( 'NONE',  ( 117.2009162446674395, -42.82382785266563019, 124.3956252759109731 ) ) ;
#63043 = CARTESIAN_POINT ( 'NONE',  ( 97.39146471609157629, -39.27917510135310408, 111.5315135458968996 ) ) ;
#63045 = CARTESIAN_POINT ( 'NONE',  ( 97.31584371926621202, -39.30597601181960243, 72.53145861026970920 ) ) ;
#63046 = DIRECTION ( 'NONE',  ( 0.000000000000000000, 0.000000000000000000, -1.000000000000000000 ) ) ;
#63047 = ORIENTED_EDGE ( 'NONE', *, *, #25648, .F. ) ;
#63048 = CARTESIAN_POINT ( 'NONE',  ( 82.00856307258283096, -104.2784471599412370, 7.717806855417980394 ) ) ;
#63049 = VECTOR ( 'NONE', #11563, 1000.000000000000000 ) ;
#63050 = CIRCLE ( 'NONE', #3593, 2.999999999999947153 ) ;
#63051 = FACE_BOUND ( 'NONE', #28455, .T. ) ;
#63052 = DIRECTION ( 'NONE',  ( 0.000000000000000000, -1.000000000000000000, -3.491483361109380094E-15 ) ) ;
#63053 = ORIENTED_EDGE ( 'NONE', *, *, #68420, .F. ) ;
#63054 = EDGE_CURVE ( 'NONE', #37163, #27030, #45895, .T. ) ;
#63055 = CARTESIAN_POINT ( 'NONE',  ( 106.5785131942345458, -24.40100501111790621, 323.5352776872487652 ) ) ;
#63057 = ORIENTED_EDGE ( 'NONE', *, *, #32033, .F. ) ;
#63056 = CARTESIAN_POINT ( 'NONE',  ( 97.34100429996045989, -42.07995573552675950, 176.7146728949589658 ) ) ;
#63058 = DIRECTION ( 'NONE',  ( -1.000000000000000000, 0.000000000000000000, -9.713237310806269221E-16 ) ) ;
#63059 = CARTESIAN_POINT ( 'NONE',  ( 115.5350430195811668, -29.59021037493291573, 220.3718157521019521 ) ) ;
#63060 = CARTESIAN_POINT ( 'NONE',  ( 110.3857440325295443, -47.32095349711466525, 48.80610146638797175 ) ) ;
#63061 = EDGE_CURVE ( 'NONE', #77895, #81541, #15409, .T. ) ;
#63062 = DIRECTION ( 'NONE',  ( 0.8660254037844382635, 0.5000000000000008882, -1.550000000000000022E-14 ) ) ;
#63063 = DIRECTION ( 'NONE',  ( 0.000000000000000000, -1.000000000000000000, 0.000000000000000000 ) ) ;
#63064 = CARTESIAN_POINT ( 'NONE',  ( 116.3212776292269552, -32.94146857470667555, 79.13562527591095375 ) ) ;
#63065 = ORIENTED_EDGE ( 'NONE', *, *, #17880, .T. ) ;
#63066 = CONTEXT_DEPENDENT_SHAPE_REPRESENTATION ( #52671, #18427 ) ;
#63067 = VECTOR ( 'NONE', #77030, 1000.000000000000000 ) ;
#63068 = ORIENTED_EDGE ( 'NONE', *, *, #5036, .T. ) ;
#63069 = ORIENTED_EDGE ( 'NONE', *, *, #63194, .T. ) ;
#63070 = ORIENTED_EDGE ( 'NONE', *, *, #80162, .F. ) ;
#63071 = FACE_OUTER_BOUND ( 'NONE', #58542, .T. ) ;
#63072 = CARTESIAN_POINT ( 'NONE',  ( 110.8167803534805813, -26.33188723323253910, 245.7889586092439629 ) ) ;
#63073 = DIRECTION ( 'NONE',  ( 0.8660254037844392627, -0.4999999999999990008, 1.549999999999999706E-14 ) ) ;
#63074 = CARTESIAN_POINT ( 'NONE',  ( -7.205548786489490269E-13, 101.5999999999999943, 108.2293999999999983 ) ) ;
#63076 = DIRECTION ( 'NONE',  ( -1.000000000000000000, -1.541976423090496028E-15, 0.000000000000000000 ) ) ;
#63075 = CARTESIAN_POINT ( 'NONE',  ( -48.02966122971774610, 66.60000000000003695, -43.00307561052233751 ) ) ;
#63077 = CARTESIAN_POINT ( 'NONE',  ( 83.56670390244801183, -34.21194715994113267, 219.5838068554169809 ) ) ;
#63078 = CARTESIAN_POINT ( 'NONE',  ( 95.23402374720009789, -35.71607800568281021, 36.25848241876794731 ) ) ;
#63079 = VERTEX_POINT ( 'NONE', #23128 ) ;
#63080 = AXIS2_PLACEMENT_3D ( 'NONE', #28441, #68102, #83418 ) ;
#63081 = VERTEX_POINT ( 'NONE', #84903 ) ;
#63082 = CYLINDRICAL_SURFACE ( 'NONE', #86266, 11.45913725231036118 ) ;
#63083 = CIRCLE ( 'NONE', #81979, 2.517499999999998739 ) ;
#63084 = DIRECTION ( 'NONE',  ( 0.000000000000000000, 1.000000000000000000, 0.000000000000000000 ) ) ;
#63085 = CARTESIAN_POINT ( 'NONE',  ( 97.63766479707265944, -34.12929003103651127, 247.1127681330529811 ) ) ;
#63086 = FACE_OUTER_BOUND ( 'NONE', #46442, .T. ) ;
#63087 = CARTESIAN_POINT ( 'NONE',  ( 115.9482186066388749, -32.63332544795709111, 100.1699109901959588 ) ) ;
#63088 = FACE_OUTER_BOUND ( 'NONE', #84075, .T. ) ;
#63089 = CARTESIAN_POINT ( 'NONE',  ( 116.0753558654980822, -32.34106755903779629, 20.18725640462358228 ) ) ;
#63090 = EDGE_LOOP ( 'NONE', ( #80053, #73104, #89249, #20056 ) ) ;
#63091 = PLANE ( 'NONE',  #34169 ) ;
#63092 = ORIENTED_EDGE ( 'NONE', *, *, #86810, .T. ) ;
#63093 = ORIENTED_EDGE ( 'NONE', *, *, #86056, .F. ) ;
#63094 = PLANE ( 'NONE',  #39413 ) ;
#63095 = CARTESIAN_POINT ( 'NONE',  ( 98.52374054827556904, -34.37364049580116898, 247.5444404487539600 ) ) ;
#63096 = AXIS2_PLACEMENT_3D ( 'NONE', #30036, #50461, #30483 ) ;
#63097 = PLANE ( 'NONE',  #18291 ) ;
#63098 = AXIS2_PLACEMENT_3D ( 'NONE', #17289, #86774, #71371 ) ;
#63099 = VECTOR ( 'NONE', #81559, 1000.000000000000000 ) ;
#63100 = CARTESIAN_POINT ( 'NONE',  ( 97.06108120487448332, -37.99646459804690579, 141.4272961276924718 ) ) ;
#63101 = VECTOR ( 'NONE', #15000, 1000.000000000000000 ) ;
#63102 = ADVANCED_FACE ( 'NONE', ( #22673 ), #43527, .T. ) ;
#63103 = ADVANCED_FACE ( 'NONE', ( #29930 ), #85357, .T. ) ;
#63104 = DIRECTION ( 'NONE',  ( 0.000000000000000000, 1.000000000000000000, 0.000000000000000000 ) ) ;
#63105 = DIRECTION ( 'NONE',  ( -1.907762142705490052E-15, -7.167082501179359715E-16, 1.000000000000000000 ) ) ;
#63106 = CIRCLE ( 'NONE', #58750, 2.500000000000002220 ) ;
#63107 = ORIENTED_EDGE ( 'NONE', *, *, #28568, .F. ) ;
#63108 = CARTESIAN_POINT ( 'NONE',  ( 142.0664832912739826, -9.729447159940995959, 14.67562527591100441 ) ) ;
#63109 = EDGE_CURVE ( 'NONE', #39484, #40328, #14419, .T. ) ;
#63110 = CARTESIAN_POINT ( 'NONE',  ( 41.56648329127398966, -27.57844715994070484, 258.9256252759120116 ) ) ;
#63111 = ORIENTED_EDGE ( 'NONE', *, *, #85672, .T. ) ;
#63112 = CARTESIAN_POINT ( 'NONE',  ( 107.1954010100577364, -26.30493706674213428, 35.06705384733893283 ) ) ;
#63113 = VERTEX_POINT ( 'NONE', #66660 ) ;
#63114 = CARTESIAN_POINT ( 'NONE',  ( 112.3037015629680866, -30.74301476610424544, 287.3214237029247897 ) ) ;
#63115 = ADVANCED_FACE ( 'NONE', ( #64890 ), #58065, .F. ) ;
#63116 = DIRECTION ( 'NONE',  ( -1.000000000000000078E-15, 1.000000000000000000, 0.000000000000000000 ) ) ;
#63117 = CARTESIAN_POINT ( 'NONE',  ( 100.4443968677459083, -27.79860430499261881, 185.5841967044829630 ) ) ;
#63118 = DIRECTION ( 'NONE',  ( 0.7071067811864683028, 0.7071067811866268427, 7.071067811864676611E-16 ) ) ;
#63119 = DIRECTION ( 'NONE',  ( 4.194175870806139918E-14, -1.000000000000000000, 0.000000000000000000 ) ) ;
#63120 = CARTESIAN_POINT ( 'NONE',  ( 122.2221484686747459, -111.8737466215628018, -19.26696060647578435 ) ) ;
#63121 = DIRECTION ( 'NONE',  ( 0.000000000000000000, 0.000000000000000000, -1.000000000000000000 ) ) ;
#63122 = VECTOR ( 'NONE', #31903, 1000.000000000000000 ) ;
#63123 = CARTESIAN_POINT ( 'NONE',  ( 100.2187443247741783, -45.46477599873944797, 273.0594347997206910 ) ) ;
#63124 = CARTESIAN_POINT ( 'NONE',  ( 102.4232139617314061, -45.66021099449668696, 117.1962128419109774 ) ) ;
#63125 = EDGE_CURVE ( 'NONE', #20097, #42342, #49205, .T. ) ;
#63126 = ORIENTED_EDGE ( 'NONE', *, *, #74133, .T. ) ;
#63127 = CARTESIAN_POINT ( 'NONE',  ( 48.45959712129000252, -28.98061976758940617, -5.074374724088000832 ) ) ;
#63128 = EDGE_LOOP ( 'NONE', ( #13181, #86840 ) ) ;
#63129 = CARTESIAN_POINT ( 'NONE',  ( 108.0381942455320967, -25.67262681319542494, 105.9946728949589811 ) ) ;
#63130 = LINE ( 'NONE', #34524, #3294 ) ;
#63131 = ORIENTED_EDGE ( 'NONE', *, *, #18924, .F. ) ;
#63132 = AXIS2_PLACEMENT_3D ( 'NONE', #54205, #66518, #73786 ) ;
#63133 = CARTESIAN_POINT ( 'NONE',  ( 208.9149999999999920, 28.98850000000000193, -7.937500000000000000 ) ) ;
#63134 = VERTEX_POINT ( 'NONE', #38070 ) ;
#63135 = ORIENTED_EDGE ( 'NONE', *, *, #63219, .F. ) ;
#63136 = EDGE_CURVE ( 'NONE', #80351, #914, #86677, .T. ) ;
#63137 = CARTESIAN_POINT ( 'NONE',  ( -446.0240000000000009, 3.174999999999999822, -1.387778780781445991E-14 ) ) ;
#63138 = DIRECTION ( 'NONE',  ( 0.000000000000000000, 0.000000000000000000, 1.000000000000000000 ) ) ;
#63139 = CARTESIAN_POINT ( 'NONE',  ( 34.96670390244647564, -26.71338133339322951, 193.9678068554150911 ) ) ;
#63140 = DIRECTION ( 'NONE',  ( 0.000000000000000000, 0.000000000000000000, 1.000000000000000000 ) ) ;
#63141 = DIRECTION ( 'NONE',  ( -4.237773401492740281E-14, 1.000000000000000000, 0.000000000000000000 ) ) ;
#63142 = CARTESIAN_POINT ( 'NONE',  ( 105.1635842947561343, -47.00881719185149876, 8.429910990196965770 ) ) ;
#63143 = EDGE_CURVE ( 'NONE', #5947, #37208, #7152, .T. ) ;
#63144 = CARTESIAN_POINT ( 'NONE',  ( 98.60478223830740774, 120.6499999999999915, 3.859079674607175002E-13 ) ) ;
#63145 = ORIENTED_EDGE ( 'NONE', *, *, #14336, .F. ) ;
#63146 = CARTESIAN_POINT ( 'NONE',  ( 3.292116081692606944, 70.27706896417943483, 118.5109511094031944 ) ) ;
#63147 = CARTESIAN_POINT ( 'NONE',  ( 182.0667039024480118, -32.29483332968430886, -5.074374724088000832 ) ) ;
#63148 = VERTEX_POINT ( 'NONE', #31241 ) ;
#63149 = ORIENTED_EDGE ( 'NONE', *, *, #50979, .F. ) ;
#63150 = CIRCLE ( 'NONE', #45667, 0.5000000000000004441 ) ;
#63151 = CARTESIAN_POINT ( 'NONE',  ( 81.36878785333431097, -21.15209318185135601, 1.893168666203115080 ) ) ;
#63152 = CARTESIAN_POINT ( 'NONE',  ( 172.5664832912728457, -18.82844715994071194, 81.92562527591194055 ) ) ;
#63153 = VECTOR ( 'NONE', #59026, 1000.000000000000000 ) ;
#63154 = CARTESIAN_POINT ( 'NONE',  ( 100.9546144035607540, -28.70706938351655779, 15.59396422068609134 ) ) ;
#63155 = CARTESIAN_POINT ( 'NONE',  ( 0.000000000000000000, 117.4749999999999943, -103.1875000000000000 ) ) ;
#63156 = CARTESIAN_POINT ( 'NONE',  ( 51.06648329127400388, 25.62155284005901379, 333.4006252759110112 ) ) ;
#63157 = CARTESIAN_POINT ( 'NONE',  ( 102.2605585157881194, -43.79055321879850027, 196.5238483995059937 ) ) ;
#63158 = CARTESIAN_POINT ( 'NONE',  ( 125.6515680309144329, 67.77259609856692180, 35.44867019240336958 ) ) ;
#63159 = CARTESIAN_POINT ( 'NONE',  ( 97.22485937713641135, -31.59570365635885736, 90.93181575210196854 ) ) ;
#63160 = VERTEX_POINT ( 'NONE', #30808 ) ;
#63161 = FACE_OUTER_BOUND ( 'NONE', #35238, .T. ) ;
#63162 = ORIENTED_EDGE ( 'NONE', *, *, #12167, .T. ) ;
#63163 = CARTESIAN_POINT ( 'NONE',  ( -79.74945239053502632, 71.14137858619481847, -87.72765544449623576 ) ) ;
#63164 = ORIENTED_EDGE ( 'NONE', *, *, #62386, .F. ) ;
#63165 = CARTESIAN_POINT ( 'NONE',  ( 103.1875000000000000, 117.4749999999999943, 3.602774393244745134E-13 ) ) ;
#63166 = ORIENTED_EDGE ( 'NONE', *, *, #52928, .F. ) ;
#63167 = LINE ( 'NONE', #64523, #36324 ) ;
#63168 = DIRECTION ( 'NONE',  ( 1.000000000000000078E-15, 1.000000000000000083E-30, -1.000000000000000000 ) ) ;
#63169 = EDGE_CURVE ( 'NONE', #89450, #33892, #71707, .T. ) ;
#63170 = CARTESIAN_POINT ( 'NONE',  ( 67.06670390244707392, -137.6758869494786950, 245.5072624240089851 ) ) ;
#63172 = CIRCLE ( 'NONE', #13891, 2.517500000000005844 ) ;
#63171 = DIRECTION ( 'NONE',  ( 3.999999999999999995E-14, -1.000000000000000000, 4.100000000000000342E-29 ) ) ;
#63173 = ORIENTED_EDGE ( 'NONE', *, *, #25426, .F. ) ;
#63174 = CARTESIAN_POINT ( 'NONE',  ( 117.4766623710874853, -37.96092365070988706, 53.73276813305394484 ) ) ;
#63175 = VECTOR ( 'NONE', #87338, 1000.000000000000000 ) ;
#63176 = VECTOR ( 'NONE', #61967, 1000.000000000000000 ) ;
#63177 = B_SPLINE_CURVE_WITH_KNOTS ( 'NONE', 3,
 ( #77796, #23734, #72323, #70989, #2391, #8762, #36463, #64169, #10971, #87728, #3717, #38673, #87289, #59553, #25053, #4615, #81390, #52716 ),
 .UNSPECIFIED., .F., .F.,
 ( 4, 2, 2, 2, 2, 2, 2, 2, 4 ),
 ( 0.000000000000000000, 0.06249849733678987385, 0.1249969946735797477, 0.1874954920103696354, 0.2499939893471594954, 0.3124924866839493554, 0.3749909840207392708, 0.4374894813575291308, 0.4999879786943189908 ),
 .UNSPECIFIED. ) ;
#63179 = CARTESIAN_POINT ( 'NONE',  ( 82.89895571708363775, 81.71102547120852932, -100.8594679592203960 ) ) ;
#63178 = DIRECTION ( 'NONE',  ( 0.000000000000000000, 1.000000000000000000, 0.000000000000000000 ) ) ;
#63180 = CARTESIAN_POINT ( 'NONE',  ( 71.25614885437424562, -84.12815644128085069, 542.9756252759101471 ) ) ;
#63181 = DIRECTION ( 'NONE',  ( -0.7071067811734105257, 0.7071067811996846197, 0.000000000000000000 ) ) ;
#63182 = VERTEX_POINT ( 'NONE', #85797 ) ;
#63183 = AXIS2_PLACEMENT_3D ( 'NONE', #75599, #33803, #6111 ) ;
#63184 = DIRECTION ( 'NONE',  ( 4.299999999999999979E-14, -1.000000000000000000, 0.000000000000000000 ) ) ;
#63185 = CARTESIAN_POINT ( 'NONE',  ( 108.4174892977290767, -26.73503593456633709, 154.9689586056143469 ) ) ;
#63186 = VECTOR ( 'NONE', #58493, 1000.000000000000000 ) ;
#63187 = DIRECTION ( 'NONE',  ( 0.000000000000000000, 1.000000000000000000, 0.000000000000000000 ) ) ;
#63188 = ADVANCED_FACE ( 'NONE', ( #10797, #37183 ), #52111, .F. ) ;
#63189 = CARTESIAN_POINT ( 'NONE',  ( 114.7233776882958409, -44.73301973330935510, 109.1718157521009687 ) ) ;
#63191 = LINE ( 'NONE', #74, #35474 ) ;
#63190 = DIRECTION ( 'NONE',  ( 0.000000000000000000, -1.000000000000000000, 0.000000000000000000 ) ) ;
#63192 = DIRECTION ( 'NONE',  ( 1.000000000000000078E-15, -1.000000000000000000, 0.000000000000000000 ) ) ;
#63193 = AXIS2_PLACEMENT_3D ( 'NONE', #60842, #80869, #52658 ) ;
#63194 = EDGE_CURVE ( 'NONE', #11890, #25046, #54580, .T. ) ;
#63195 = ORIENTED_EDGE ( 'NONE', *, *, #56356, .F. ) ;
#63196 = VECTOR ( 'NONE', #73573, 1000.000000000000000 ) ;
#63197 = CARTESIAN_POINT ( 'NONE',  ( 41.56648329127381203, -18.82844715994071194, 141.9256252759118979 ) ) ;
#63198 = CARTESIAN_POINT ( 'NONE',  ( 108.6395843534182291, -26.47938140272626484, 140.9432443235289725 ) ) ;
#63200 = ORIENTED_EDGE ( 'NONE', *, *, #16283, .T. ) ;
#63199 = CARTESIAN_POINT ( 'NONE',  ( 177.4809174648215730, -48.32844715993478246, 129.9678068554150059 ) ) ;
#63201 = CARTESIAN_POINT ( 'NONE',  ( 117.4080659314678314, -35.59792815749688089, 274.9127681330538735 ) ) ;
#63202 = DIRECTION ( 'NONE',  ( -0.9068632946707755327, 0.4214249218767993077, 0.000000000000000000 ) ) ;
#63203 = DIRECTION ( 'NONE',  ( -0.7071067811864671926, -0.7071067811866279529, -7.071067811864664779E-16 ) ) ;
#63204 = CARTESIAN_POINT ( 'NONE',  ( 99.51799851144259890, -77.76606036807547184, 250.2178068554180470 ) ) ;
#63205 = AXIS2_PLACEMENT_3D ( 'NONE', #60652, #46118, #26152 ) ;
#63206 = FACE_OUTER_BOUND ( 'NONE', #54937, .T. ) ;
#63207 = CARTESIAN_POINT ( 'NONE',  ( 67.03432561829117731, -137.6460688757851756, 245.8354721159570033 ) ) ;
#63208 = CARTESIAN_POINT ( 'NONE',  ( -96.71266027437708601, 71.53177522571070313, 87.70409100286397575 ) ) ;
#63209 = CARTESIAN_POINT ( 'NONE',  ( 114.5468542906243243, -29.54732804739393615, 189.4232443235299570 ) ) ;
#63210 = ORIENTED_EDGE ( 'NONE', *, *, #76847, .T. ) ;
#63211 = EDGE_LOOP ( 'NONE', ( #73378, #72311, #52696, #33190 ) ) ;
#63212 = AXIS2_PLACEMENT_3D ( 'NONE', #11311, #66722, #31301 ) ;
#63213 = CARTESIAN_POINT ( 'NONE',  ( 99.32274084468600961, -31.40864097607868999, 162.2911071154209708 ) ) ;
#63214 = CARTESIAN_POINT ( 'NONE',  ( 145.3728389244185450, -136.8603515927981107, 247.4879652615099985 ) ) ;
#63215 = CARTESIAN_POINT ( 'NONE',  ( 99.72008180067200556, -41.26785689822659009, 8.199678543991950619 ) ) ;
#63216 = VECTOR ( 'NONE', #4271, 1000.000000000000000 ) ;
#63217 = LINE ( 'NONE', #42749, #14471 ) ;
#63218 = EDGE_CURVE ( 'NONE', #51167, #34580, #81662, .T. ) ;
#63219 = EDGE_CURVE ( 'NONE', #64147, #2062, #5343, .T. ) ;
#63220 = PLANE ( 'NONE',  #27199 ) ;
#63221 = PLANE ( 'NONE',  #86530 ) ;
#63222 = CARTESIAN_POINT ( 'NONE',  ( 115.0889047235099270, -30.61763667932959621, 105.3439586093056590 ) ) ;
#63223 = EDGE_CURVE ( 'NONE', #8859, #59384, #23125, .T. ) ;
#63224 = LINE ( 'NONE', #15081, #14025 ) ;
#63225 = CARTESIAN_POINT ( 'NONE',  ( 97.11708974113231818, -41.49110554365062598, 216.6937205140059461 ) ) ;
#63226 = CARTESIAN_POINT ( 'NONE',  ( 6.310004044849506499, 93.46397155878921126, 118.1882387953691591 ) ) ;
#63227 = ORIENTED_EDGE ( 'NONE', *, *, #89462, .F. ) ;
#63228 = ORIENTED_EDGE ( 'NONE', *, *, #25206, .F. ) ;
#63229 = ADVANCED_FACE ( 'NONE', ( #33483, #18509 ), #20325, .T. ) ;
#63230 = CARTESIAN_POINT ( 'NONE',  ( 97.81169818311565223, -40.51742792548894556, 86.63555527419073599 ) ) ;
#63231 = CARTESIAN_POINT ( 'NONE',  ( 82.78958961022061658, -19.11755991741142680, 6.789748280180715412 ) ) ;
#63232 = FACE_OUTER_BOUND ( 'NONE', #40798, .T. ) ;
#63233 = CARTESIAN_POINT ( 'NONE',  ( -487.2989999999999782, 97.78694598552380057, 3.968750000000479616 ) ) ;
#63234 = CARTESIAN_POINT ( 'NONE',  ( 98.34688518126465340, -32.29864090244033292, 46.95276813305293473 ) ) ;
#63236 = DIRECTION ( 'NONE',  ( -1.000000000000000078E-15, 1.000000000000000083E-30, 1.000000000000000000 ) ) ;
#63235 = CIRCLE ( 'NONE', #55945, 9.000000000000007105 ) ;
#63237 = EDGE_CURVE ( 'NONE', #71729, #22057, #54346, .T. ) ;
#63238 = ORIENTED_EDGE ( 'NONE', *, *, #61178, .F. ) ;
#63239 = AXIS2_PLACEMENT_3D ( 'NONE', #1440, #43644, #64555 ) ;
#63240 = LINE ( 'NONE', #43226, #39328 ) ;
#63241 = VECTOR ( 'NONE', #56386, 999.9999999999998863 ) ;
#63242 = LINE ( 'NONE', #12520, #62741 ) ;
#63243 = VECTOR ( 'NONE', #66444, 1000.000000000000000 ) ;
#63244 = CARTESIAN_POINT ( 'NONE',  ( 103.0904226585672916, -47.89329182393425555, 252.3041967044823366 ) ) ;
#63245 = ORIENTED_EDGE ( 'NONE', *, *, #12060, .T. ) ;
#63246 = ADVANCED_FACE ( 'NONE', ( #53902 ), #46650, .T. ) ;
#63247 = CARTESIAN_POINT ( 'NONE',  ( 32.09598329127702243, -23.42844715994121785, 313.9678068554150059 ) ) ;
#63248 = DIRECTION ( 'NONE',  ( 0.7071067811865475727, -0.7071067811865475727, 0.000000000000000000 ) ) ;
#63249 = CARTESIAN_POINT ( 'NONE',  ( 112.4431012073915213, -45.17550776473990481, 168.0275481766957171 ) ) ;
#63250 = CARTESIAN_POINT ( 'NONE',  ( 110.8736562448416549, -29.50897902285196039, 57.50809036959092424 ) ) ;
#63251 = CARTESIAN_POINT ( 'NONE',  ( 113.6281748933624556, -28.60039662530314430, 160.5356252759109736 ) ) ;
#63252 = CARTESIAN_POINT ( 'NONE',  ( 122.7090602494120049, -38.07100823150197755, 293.9356252759109793 ) ) ;
#63253 = ORIENTED_EDGE ( 'NONE', *, *, #71496, .F. ) ;
#63254 = CARTESIAN_POINT ( 'NONE',  ( -103.1875000000000000, 127.0000000000000000, 7.937499999998919087 ) ) ;
#63255 = EDGE_LOOP ( 'NONE', ( #82475, #13569, #83924, #36213 ) ) ;
#63256 = ORIENTED_EDGE ( 'NONE', *, *, #8953, .T. ) ;
#63257 = DIRECTION ( 'NONE',  ( 4.299999999999999979E-14, -1.000000000000000000, 0.000000000000000000 ) ) ;
#63258 = ORIENTED_EDGE ( 'NONE', *, *, #70286, .F. ) ;
#63259 = VERTEX_POINT ( 'NONE', #47990 ) ;
#63260 = DIRECTION ( 'NONE',  ( 0.000000000000000000, -1.000000000000000000, 0.000000000000000000 ) ) ;
#63261 = VECTOR ( 'NONE', #49777, 1000.000000000000000 ) ;
#63262 = CARTESIAN_POINT ( 'NONE',  ( 108.0295785460986622, -25.31083404586814112, 321.6169501233419510 ) ) ;
#63263 = CARTESIAN_POINT ( 'NONE',  ( 111.7654875973913278, -45.22591620450738503, 102.4009912566479557 ) ) ;
#63264 = CARTESIAN_POINT ( 'NONE',  ( 115.0717820980658814, -30.01665675799653599, 269.3813395616251682 ) ) ;
#63265 = DIRECTION ( 'NONE',  ( 0.7071067811865370256, 0.000000000000000000, -0.7071067811865580088 ) ) ;
#63266 = FACE_OUTER_BOUND ( 'NONE', #7450, .T. ) ;
#63267 = ORIENTED_EDGE ( 'NONE', *, *, #26575, .T. ) ;
#63268 = DIRECTION ( 'NONE',  ( -2.999999999999999839E-15, 1.000000000000000000, -2.999999999999999900E-30 ) ) ;
#63269 = CARTESIAN_POINT ( 'NONE',  ( 172.5664832912740110, -32.07844715994070839, 18.92562527591200094 ) ) ;
#63270 = EDGE_CURVE ( 'NONE', #87561, #16246, #64275, .T. ) ;
#63271 = CARTESIAN_POINT ( 'NONE',  ( 70.88111044991026688, -139.0101909505960691, 247.5112285516309782 ) ) ;
#63272 = CIRCLE ( 'NONE', #89415, 2.999999999999975131 ) ;
#63273 = CARTESIAN_POINT ( 'NONE',  ( 100.1408543393098682, -45.42701269980184975, 122.0413395616259606 ) ) ;
#63274 = CARTESIAN_POINT ( 'NONE',  ( 109.6949574390794169, -47.51388072328656165, 87.75467289495897205 ) ) ;
#63275 = CARTESIAN_POINT ( 'NONE',  ( 108.0181136390867636, -24.86676629934084559, 265.0127681330534415 ) ) ;
#63276 = VERTEX_POINT ( 'NONE', #77522 ) ;
#63277 = UNCERTAINTY_MEASURE_WITH_UNIT (LENGTH_MEASURE( 1.000000000000000082E-05 ), #42909, 'distance_accuracy_value', 'NONE');
#63278 = CARTESIAN_POINT ( 'NONE',  ( 101.4045521927434805, -45.52538047655821885, 222.1213395616249784 ) ) ;
#63279 = DIRECTION ( 'NONE',  ( 0.02150753337724187197, 0.0009076677972194977960, 0.9997682742251811083 ) ) ;
#63280 =( LENGTH_UNIT ( ) NAMED_UNIT ( * ) SI_UNIT ( .MILLI., .METRE. ) );
#63281 =( NAMED_UNIT ( * ) SI_UNIT ( $, .STERADIAN. ) SOLID_ANGLE_UNIT ( ) );
#63282 = FACE_BOUND ( 'NONE', #4151, .T. ) ;
#63284 = CARTESIAN_POINT ( 'NONE',  ( 68.69238985301161904, -139.3031226333023938, 245.7154487659484232 ) ) ;
#63283 = CARTESIAN_POINT ( 'NONE',  ( 140.8897065959773727, -8.906223855237593412, 14.92562527591100441 ) ) ;
#63285 = DIRECTION ( 'NONE',  ( -1.000000000000000000, 0.000000000000000000, 0.000000000000000000 ) ) ;
#63286 = CARTESIAN_POINT ( 'NONE',  ( -40.89999999999999858, 53.97500000000000142, 60.79999999999999716 ) ) ;
#63287 = DIRECTION ( 'NONE',  ( 0.000000000000000000, -1.000000000000000000, 0.000000000000000000 ) ) ;
#63288 = DIRECTION ( 'NONE',  ( 1.047445008332813989E-14, 0.000000000000000000, 1.000000000000000000 ) ) ;
#63289 = LINE ( 'NONE', #28305, #9675 ) ;
#63290 = CARTESIAN_POINT ( 'NONE',  ( 134.0664832912740110, -46.72944715994100306, 4.925625275910997303 ) ) ;
#63292 = ORIENTED_EDGE ( 'NONE', *, *, #86417, .T. ) ;
#63291 = CARTESIAN_POINT ( 'NONE',  ( 80.54920390244807038, -58.72944715994108833, 207.5838068554169809 ) ) ;
#63293 = DIRECTION ( 'NONE',  ( 0.7071067811864886199, 0.7071067811866064146, 7.071067811865191343E-16 ) ) ;
#63294 = CARTESIAN_POINT ( 'NONE',  ( 112.6756251843347627, -45.54329372032184153, 263.0270538473394026 ) ) ;
#63295 = CARTESIAN_POINT ( 'NONE',  ( 96.60720999893194971, -36.88735532319633847, 132.3384824187679669 ) ) ;
#63296 = CARTESIAN_POINT ( 'NONE',  ( 96.66758392153232649, -32.91525239269808623, 17.03467289495896964 ) ) ;
#63297 = CIRCLE ( 'NONE', #80680, 3.000000000000002665 ) ;
#63298 = DIRECTION ( 'NONE',  ( -0.000000000000000000, 1.000000000000000000, 0.000000000000000000 ) ) ;
#63300 = CARTESIAN_POINT ( 'NONE',  ( 81.57739926165420741, -34.43204134599511690, 7.859568798198143469 ) ) ;
#63299 = CARTESIAN_POINT ( 'NONE',  ( 156.5667039024483529, -48.82844715993569196, 293.2178068554149490 ) ) ;
#63301 = FACE_OUTER_BOUND ( 'NONE', #45384, .T. ) ;
#63302 = CIRCLE ( 'NONE', #86521, 0.9999999999992039701 ) ;
#63303 = ADVANCED_FACE ( 'NONE', ( #55251 ), #84357, .F. ) ;
#63304 = CIRCLE ( 'NONE', #9615, 5.041900000000000048 ) ;
#63305 = AXIS2_PLACEMENT_3D ( 'NONE', #24794, #10271, #79781 ) ;
#63306 = CONICAL_SURFACE ( 'NONE', #15474, 8.928100000000000591, 1.029744258676653645 ) ;
#63307 = ORIENTED_EDGE ( 'NONE', *, *, #66709, .F. ) ;
#63308 = DIRECTION ( 'NONE',  ( 0.000000000000000000, 0.000000000000000000, -1.000000000000000000 ) ) ;
#63309 = ORIENTED_EDGE ( 'NONE', *, *, #66907, .F. ) ;
#63310 = CARTESIAN_POINT ( 'NONE',  ( 105.0150133346707406, -46.21955246553896757, 181.8295626852199689 ) ) ;
#63312 = ORIENTED_EDGE ( 'NONE', *, *, #45006, .F. ) ;
#63311 = CARTESIAN_POINT ( 'NONE',  ( 131.0667039024480403, -51.22944715994093201, 231.5838068554170093 ) ) ;
#63313 = CARTESIAN_POINT ( 'NONE',  ( 107.0664832912739399, -36.72944715994095333, 302.4856252759109907 ) ) ;
#63314 = CARTESIAN_POINT ( 'NONE',  ( 95.93334478249057895, -32.74178691125834462, 172.0527681330539735 ) ) ;
#63315 = DIRECTION ( 'NONE',  ( -1.000000000000000000, -1.541976423090496028E-15, 0.000000000000000000 ) ) ;
#63316 = LINE ( 'NONE', #50569, #82062 ) ;
#63317 = CARTESIAN_POINT ( 'NONE',  ( 97.06063502581739044, -37.99412314152812797, 87.42674140824780693 ) ) ;
#63318 = CARTESIAN_POINT ( 'NONE',  ( -81.76234319299368281, 70.17658267799284033, 85.85227416678179679 ) ) ;
#63319 = CARTESIAN_POINT ( 'NONE',  ( 95.56670390244703128, -104.2784471599408818, 19.21780685541799016 ) ) ;
#63321 = CARTESIAN_POINT ( 'NONE',  ( 103.5913876162975527, -46.49993820617282125, 102.3165776568639700 ) ) ;
#63320 = AXIS2_PLACEMENT_3D ( 'NONE', #4719, #10626, #17888 ) ;
#63322 = ORIENTED_EDGE ( 'NONE', *, *, #43040, .F. ) ;
#63323 = ORIENTED_EDGE ( 'NONE', *, *, #3756, .F. ) ;
#63324 = ORIENTED_EDGE ( 'NONE', *, *, #46072, .F. ) ;
#63325 = CARTESIAN_POINT ( 'NONE',  ( 99.97388925556708728, -42.04201607304819532, 63.27015473446895300 ) ) ;
#63326 = LINE ( 'NONE', #76959, #71872 ) ;
#63328 = CARTESIAN_POINT ( 'NONE',  ( 105.7154774160331954, -46.72385840309821248, 37.46895861606181910 ) ) ;
#63327 = CARTESIAN_POINT ( 'NONE',  ( 116.6595528204498464, -34.65899032542080960, 179.9956252759109532 ) ) ;
#63329 = CARTESIAN_POINT ( 'NONE',  ( 49.16670390244746613, -26.71338133339273924, 237.4678068554150059 ) ) ;
#63330 = CARTESIAN_POINT ( 'NONE',  ( 25.56670390244828894, -48.82844715994168183, 293.2178068554150059 ) ) ;
#63331 = EDGE_CURVE ( 'NONE', #81923, #61676, #89835, .T. ) ;
#63332 = DIRECTION ( 'NONE',  ( 0.000000000000000000, -1.000000000000000000, 0.000000000000000000 ) ) ;
#63333 = CARTESIAN_POINT ( 'NONE',  ( 32.16397622748866070, -34.03355364506487746, 193.9678068554150911 ) ) ;
#63334 = EDGE_CURVE ( 'NONE', #29546, #82906, #15532, .T. ) ;
#63335 = CARTESIAN_POINT ( 'NONE',  ( 188.5667039024483245, -42.82844715993430640, 173.2178068554150059 ) ) ;
#63336 = CARTESIAN_POINT ( 'NONE',  ( 98.47671751366513604, -30.86049585540210671, 120.8499109901969604 ) ) ;
#63337 = ORIENTED_EDGE ( 'NONE', *, *, #61172, .T. ) ;
#63338 = EDGE_CURVE ( 'NONE', #2257, #50856, #69527, .T. ) ;
#63339 = ORIENTED_EDGE ( 'NONE', *, *, #15906, .F. ) ;
#63340 = EDGE_LOOP ( 'NONE', ( #81750, #27553, #14879, #60071 ) ) ;
#63341 = EDGE_CURVE ( 'NONE', #75352, #44089, #48886, .T. ) ;
#63342 = PLANE ( 'NONE',  #56274 ) ;
#63343 = FACE_BOUND ( 'NONE', #39500, .T. ) ;
#63344 = PLANE ( 'NONE',  #30861 ) ;
#63345 = CARTESIAN_POINT ( 'NONE',  ( 114.7326537306653762, -39.53293727251440970, 216.3652332267339773 ) ) ;
#63346 = DIRECTION ( 'NONE',  ( 0.000000000000000000, 0.000000000000000000, -1.000000000000000000 ) ) ;
#63347 = FACE_OUTER_BOUND ( 'NONE', #38676, .T. ) ;
#63348 = ORIENTED_EDGE ( 'NONE', *, *, #54046, .T. ) ;
#63350 = ORIENTED_EDGE ( 'NONE', *, *, #7431, .T. ) ;
#63349 = EDGE_LOOP ( 'NONE', ( #61223, #72977, #50179, #18894 ) ) ;
#63351 = ADVANCED_FACE ( 'NONE', ( #69364 ), #1223, .F. ) ;
#63352 = DIRECTION ( 'NONE',  ( -1.000000000000000000, 0.000000000000000000, 0.000000000000000000 ) ) ;
#63353 = ORIENTED_EDGE ( 'NONE', *, *, #39653, .F. ) ;
#63354 = ORIENTED_EDGE ( 'NONE', *, *, #84999, .F. ) ;
#63355 = CARTESIAN_POINT ( 'NONE',  ( 71.25416588882599456, -72.55705569728901594, 361.9756252759101471 ) ) ;
#63356 = CARTESIAN_POINT ( 'NONE',  ( 114.6260888371869555, -31.15012018194425281, 255.7520594963732492 ) ) ;
#63357 = DIRECTION ( 'NONE',  ( 1.000000000000000000, 4.237773401492740281E-14, 0.000000000000000000 ) ) ;
#63358 = EDGE_LOOP ( 'NONE', ( #79844, #7692, #33589, #57859 ) ) ;
#63359 = AXIS2_PLACEMENT_3D ( 'NONE', #48914, #42552, #8058 ) ;
#63360 = DIRECTION ( 'NONE',  ( 1.000000000000000078E-15, 1.000000000000000083E-30, -1.000000000000000000 ) ) ;
#63361 = CARTESIAN_POINT ( 'NONE',  ( -120.7378339438464678, 74.60054165536443804, 49.68010905324412363 ) ) ;
#63362 = VERTEX_POINT ( 'NONE', #76167 ) ;
#63363 = EDGE_LOOP ( 'NONE', ( #36300, #64040, #57087, #53365 ) ) ;
#63364 = VECTOR ( 'NONE', #47398, 1000.000000000000000 ) ;
#63365 = AXIS2_PLACEMENT_3D ( 'NONE', #80445, #40432, #61757 ) ;
#63366 = CARTESIAN_POINT ( 'NONE',  ( 100.8961411191535973, 120.6499999999999915, 3.968750000000400124 ) ) ;
#63367 = AXIS2_PLACEMENT_3D ( 'NONE', #65678, #36657, #2586 ) ;
#63368 = ORIENTED_EDGE ( 'NONE', *, *, #67904, .F. ) ;
#63369 = EDGE_LOOP ( 'NONE', ( #62454, #85232, #22482, #2166 ) ) ;
#63370 = CARTESIAN_POINT ( 'NONE',  ( 116.1392960594047850, -38.67366927644074082, 256.4766617981626382 ) ) ;
#63371 = CARTESIAN_POINT ( 'NONE',  ( 114.1902268275144507, -45.21166270573645107, 148.1203871806719405 ) ) ;
#63372 = CARTESIAN_POINT ( 'NONE',  ( 98.85726102317293851, -28.21728661942034577, 115.6870538473389587 ) ) ;
#63373 = DIRECTION ( 'NONE',  ( 1.000000000000000000, 0.000000000000000000, 0.000000000000000000 ) ) ;
#63374 = CARTESIAN_POINT ( 'NONE',  ( 107.0667039024470313, -104.2784471599413791, 2.217806855418003043 ) ) ;
#63375 = CARTESIAN_POINT ( 'NONE',  ( 99.08600912489498569, -29.96680234772274787, 211.7670538473399517 ) ) ;
#63376 = DIRECTION ( 'NONE',  ( 0.000000000000000000, 0.000000000000000000, -1.000000000000000000 ) ) ;
#63377 = CARTESIAN_POINT ( 'NONE',  ( 90.06670420047028358, -137.6784471599409585, 55.21780685541800437 ) ) ;
#63378 = EDGE_LOOP ( 'NONE', ( #10193, #476, #83567, #1015, #13167, #45214, #52133, #66385 ) ) ;
#63379 = CARTESIAN_POINT ( 'NONE',  ( 130.3836616406707094, 71.76234181793742550, -6.714949744937471543 ) ) ;
#63380 = ORIENTED_EDGE ( 'NONE', *, *, #45791, .T. ) ;
#63381 = ORIENTED_EDGE ( 'NONE', *, *, #4813, .T. ) ;
#63382 = LINE ( 'NONE', #1164, #37324 ) ;
#63383 = CIRCLE ( 'NONE', #8277, 3.000000000000002665 ) ;
#63384 = EDGE_CURVE ( 'NONE', #61434, #56160, #8486, .T. ) ;
#63385 = CARTESIAN_POINT ( 'NONE',  ( 182.3467384525660009, -36.02818131005237490, 193.9678068554150059 ) ) ;
#63386 = CLOSED_SHELL ( 'NONE', ( #61678, #2679, #86827, #12261, #5814, #21895, #42659, #45554, #33484, #32557, #5283, #73061, #28988, #27627, #84491, #29236, #86399, #2389, #69704, #5407, #56154, #52626, #86459, #43626, #8716, #23311, #13904, #25994, #10828, #431, #40757, #24148, #84328, #46885, #52723, #71478, #37083, #67931, #46874, #11887, #55234, #28123, #45239, #82461, #87547, #70647, #73453, #67941, #44230, #89106, #31655, #54270, #73580, #87847, #1766, #17921, #80975, #82923, #34310, #47368, #21218, #54150, #28124, #13338, #69058, #70750, #45649, #31415, #80343, #60334, #73690, #83801, #49371, #76114, #6452, #35660, #79448, #17504, #54611, #34599, #11361, #59937, #42576, #54722, #66191, #89187, #72839, #25478, #53478, #61061, #883, #47508, #41274, #37998, #63229, #14380, #40760, #71327, #8052, #59134, #45267, #75046, #11199, #75538, #19845, #32544, #10190, #1610, #87934, #39447, #13587, #9701, #69491, #80677, #86233, #29524, #70572, #2623, #2338, #3355, #9024, #81578, #51591, #68131, #3016, #57576, #44332, #59604, #76798, #13931, #51128, #64, #61481, #59114, #5776, #66483, #74139, #82311, #8971, #11432, #62272, #49192, #66, #58420, #755, #65479, #45849, #79823, #25250, #49256, #34910, #23788, #36369, #11944, #85126, #76674, #57596, #35886, #45928, #41900, #80266, #85192, #15042, #68149, #45526, #60562, #78492, #23669, #87121, #71889, #10133, #15164, #75772, #66806, #57736, #32105, #62284, #30448, #370, #60740, #39264, #13183, #73373, #77307, #59641, #18708, #9931, #75984, #35223, #70945, #59625 ) ) ;
#63387 = ORIENTED_EDGE ( 'NONE', *, *, #64532, .F. ) ;
#63388 = CARTESIAN_POINT ( 'NONE',  ( 118.9039262414038944, -36.16781539521252142, 118.8641967044819836 ) ) ;
#63389 = DIRECTION ( 'NONE',  ( -0.7071067811874389708, 0.7071067811856560636, 0.000000000000000000 ) ) ;
#63390 = EDGE_CURVE ( 'NONE', #83770, #20859, #8027, .T. ) ;
#63391 = CARTESIAN_POINT ( 'NONE',  ( 107.0664832912739968, -36.72944715994100306, 287.6356252759109680 ) ) ;
#63392 = CARTESIAN_POINT ( 'NONE',  ( -69.72411017813060141, 127.0000000000000000, 69.72411017812929401 ) ) ;
#63395 = CARTESIAN_POINT ( 'NONE',  ( 110.7254274611715630, -26.32387412717039155, 250.8194347997206819 ) ) ;
#63394 = CARTESIAN_POINT ( 'NONE',  ( 163.0664832912739826, -18.82844715994099971, 333.4006252759120343 ) ) ;
#63393 = DIRECTION ( 'NONE',  ( 0.000000000000000000, 0.8660254037844387076, -0.4999999999999998890 ) ) ;
#63396 = FACE_OUTER_BOUND ( 'NONE', #33082, .T. ) ;
#63397 = LINE ( 'NONE', #83855, #7602 ) ;
#63398 = DIRECTION ( 'NONE',  ( 0.000000000000000000, 0.000000000000000000, 1.000000000000000000 ) ) ;
#63399 = CARTESIAN_POINT ( 'NONE',  ( 128.0667039024480118, -48.82844715994099971, 198.9178068554149945 ) ) ;
#63400 = DIRECTION ( 'NONE',  ( 0.4999999999999995004, 0.000000000000000000, -0.8660254037844390407 ) ) ;
#63401 = PLANE ( 'NONE',  #65128 ) ;
#63403 = EDGE_LOOP ( 'NONE', ( #21938, #75713, #6305, #56983 ) ) ;
#63402 = CARTESIAN_POINT ( 'NONE',  ( 116.3563860081925725, -41.55700552044970664, 288.4441967044822945 ) ) ;
#63404 = CARTESIAN_POINT ( 'NONE',  ( 34.33598329127499227, -36.32844715994100682, 342.9256252759109884 ) ) ;
#63405 = CARTESIAN_POINT ( 'NONE',  ( 98.14931896820920088, -31.28605259387051518, 170.8899109901960003 ) ) ;
#63406 = CARTESIAN_POINT ( 'NONE',  ( 114.8194029112656551, -43.69900416259703491, 34.24419670448197905 ) ) ;
#63407 = CARTESIAN_POINT ( 'NONE',  ( 102.2170635254687454, -46.00716819922848799, 208.1927681330539599 ) ) ;
#63408 = CARTESIAN_POINT ( 'NONE',  ( 102.0670548334093581, -27.97049812994907825, 31.48979195403828157 ) ) ;
#63409 = CARTESIAN_POINT ( 'NONE',  ( 41.56648329127398966, -27.57844715994070484, 258.9256252759120116 ) ) ;
#63411 = CYLINDRICAL_SURFACE ( 'NONE', #48630, 30.99999999999998579 ) ;
#63410 = FACE_OUTER_BOUND ( 'NONE', #60609, .T. ) ;
#63412 = CARTESIAN_POINT ( 'NONE',  ( 31.75000000000000000, 124.5870000000000033, -3.174999999999999822 ) ) ;
#63413 = DIRECTION ( 'NONE',  ( 0.0001713722455994027248, -0.9999999853157766072, 0.000000000000000000 ) ) ;
#63414 = ORIENTED_EDGE ( 'NONE', *, *, #24380, .T. ) ;
#63415 = AXIS2_PLACEMENT_3D ( 'NONE', #86204, #2196, #77600 ) ;
#63416 = CARTESIAN_POINT ( 'NONE',  ( -41.60202597009397607, 40.59999999999997300, 50.85338361873603219 ) ) ;
#63417 = EDGE_CURVE ( 'NONE', #43612, #54367, #42081, .T. ) ;
#63418 = ORIENTED_EDGE ( 'NONE', *, *, #35434, .T. ) ;
#63419 = ORIENTED_EDGE ( 'NONE', *, *, #79357, .F. ) ;
#63421 = VERTEX_POINT ( 'NONE', #42525 ) ;
#63420 = DIRECTION ( 'NONE',  ( 0.000000000000000000, 0.000000000000000000, -1.000000000000000000 ) ) ;
#63422 = CARTESIAN_POINT ( 'NONE',  ( 116.2124334422529870, -31.77159869865918296, 65.22133956162595325 ) ) ;
#63423 = CARTESIAN_POINT ( 'NONE',  ( 37.03715912545342093, -48.62818131006128652, 193.9678068554150911 ) ) ;
#63424 = CARTESIAN_POINT ( 'NONE',  ( 25.56670390244747892, -48.82844715994178841, 139.7178068554150627 ) ) ;
#63425 = CARTESIAN_POINT ( 'NONE',  ( 97.34161151642148013, -42.07962167312376067, 172.7146728949589942 ) ) ;
#63426 = CIRCLE ( 'NONE', #53201, 5.000000000000004441 ) ;
#63427 = AXIS2_PLACEMENT_3D ( 'NONE', #29935, #72159, #78545 ) ;
#63428 = CARTESIAN_POINT ( 'NONE',  ( 103.2261711710990824, -45.64430683061108596, 286.6752769709340782 ) ) ;
#63429 = VERTEX_POINT ( 'NONE', #56612 ) ;
#63430 = EDGE_LOOP ( 'NONE', ( #23932, #12754 ) ) ;
#63431 = VERTEX_POINT ( 'NONE', #63898 ) ;
#63432 = VECTOR ( 'NONE', #63184, 1000.000000000000000 ) ;
#63433 = VECTOR ( 'NONE', #28328, 1000.000000000000000 ) ;
#63434 = ORIENTED_EDGE ( 'NONE', *, *, #67433, .F. ) ;
#63435 = CARTESIAN_POINT ( 'NONE',  ( 108.3334480986085708, -46.73485935347873976, 107.6772919428708946 ) ) ;
#63436 = PLANE ( 'NONE',  #57977 ) ;
#63437 = CARTESIAN_POINT ( 'NONE',  ( -50.35902679310718355, 54.97499999999996589, 27.95514712793348977 ) ) ;
#63438 = CARTESIAN_POINT ( 'NONE',  ( 115.8254323916879258, -31.73001882819412245, 74.23979194262673786 ) ) ;
#63439 = CARTESIAN_POINT ( 'NONE',  ( 96.70003673985384296, 93.55484823631827851, 87.71605664019050153 ) ) ;
#63440 = CARTESIAN_POINT ( 'NONE',  ( 68.53801554307389665, 120.6499999999999915, 74.15067561874289481 ) ) ;
#63441 = CARTESIAN_POINT ( 'NONE',  ( 0.000000000000000000, 67.86880000000000734, 265.5569999999999595 ) ) ;
#63442 = DIRECTION ( 'NONE',  ( 4.299999999999999979E-14, -1.000000000000000000, 4.400000000000000367E-29 ) ) ;
#63443 = CARTESIAN_POINT ( 'NONE',  ( 97.81168895331671820, -40.51742574516950413, 11.63562527591094309 ) ) ;
#63444 = ADVANCED_FACE ( 'NONE', ( #84800 ), #71167, .F. ) ;
#63445 = CARTESIAN_POINT ( 'NONE',  ( -6.715534948705635721, 71.76285132298018254, 118.3661493156453730 ) ) ;
#63446 = VERTEX_POINT ( 'NONE', #8942 ) ;
#63447 = CIRCLE ( 'NONE', #57668, 38.10000000000000142 ) ;
#63448 = CARTESIAN_POINT ( 'NONE',  ( 97.81186544543886896, -40.51730612966257183, 271.6361395295153898 ) ) ;
#63449 = VECTOR ( 'NONE', #89417, 1000.000000000000000 ) ;
#63450 = DIRECTION ( 'NONE',  ( 0.000000000000000000, 1.000000000000000000, 0.000000000000000000 ) ) ;
#63451 = CARTESIAN_POINT ( 'NONE',  ( 113.4406056323916090, -42.58363279299825876, 76.04142370292498754 ) ) ;
#63452 = VECTOR ( 'NONE', #7081, 1000.000000000000000 ) ;
#63453 = CARTESIAN_POINT ( 'NONE',  ( 71.25416588882599456, -72.55705569728901594, 361.9756252759101471 ) ) ;
#63454 = CARTESIAN_POINT ( 'NONE',  ( 73.06670390244801183, -50.82844715994100682, 310.9178068554150514 ) ) ;
#63455 = VERTEX_POINT ( 'NONE', #89820 ) ;
#63456 = ORIENTED_EDGE ( 'NONE', *, *, #84152, .F. ) ;
#63457 = EDGE_CURVE ( 'NONE', #65259, #61997, #34831, .T. ) ;
#63458 = CARTESIAN_POINT ( 'NONE',  ( 182.5667039024480118, -32.29483332968450782, -5.074374724088000832 ) ) ;
#63459 = VERTEX_POINT ( 'NONE', #55687 ) ;
#63460 = ORIENTED_EDGE ( 'NONE', *, *, #35940, .T. ) ;
#63461 = ADVANCED_FACE ( 'NONE', ( #28010 ), #57511, .T. ) ;
#63462 = CARTESIAN_POINT ( 'NONE',  ( 116.0040243724562146, -33.83170925634997417, 130.5196785439929670 ) ) ;
#63463 = CARTESIAN_POINT ( 'NONE',  ( 107.0664832912739541, -36.72944715994095333, 308.7195067599733420 ) ) ;
#63464 = CARTESIAN_POINT ( 'NONE',  ( 113.3277443033378376, -28.32255675095946046, 100.5670538473389684 ) ) ;
#63465 = CIRCLE ( 'NONE', #22831, 4.749999999999976907 ) ;
#63466 = CARTESIAN_POINT ( 'NONE',  ( 107.5667039024470313, -109.0284471599420613, -19.78219314458187839 ) ) ;
#63467 = ORIENTED_EDGE ( 'NONE', *, *, #41078, .T. ) ;
#63468 = VERTEX_POINT ( 'NONE', #86573 ) ;
#63469 = ORIENTED_EDGE ( 'NONE', *, *, #57788, .T. ) ;
#63470 = CYLINDRICAL_SURFACE ( 'NONE', #36855, 9.999999999999998224 ) ;
#63471 = ORIENTED_EDGE ( 'NONE', *, *, #71546, .T. ) ;
#63472 = CARTESIAN_POINT ( 'NONE',  ( 116.1393041698828057, -43.00708073170995505, 13.35657765686298859 ) ) ;
#63473 = CARTESIAN_POINT ( 'NONE',  ( 113.6278897941700876, -45.65318799257786964, 179.0689586092439640 ) ) ;
#63474 = DIRECTION ( 'NONE',  ( 1.000000000000000000, 1.000000000000000078E-15, 0.000000000000000000 ) ) ;
#63475 = LINE ( 'NONE', #30308, #64859 ) ;
#63476 = CARTESIAN_POINT ( 'NONE',  ( 97.93258204476157402, -31.63109636822184711, 106.9213395616259703 ) ) ;
#63477 = CARTESIAN_POINT ( 'NONE',  ( 106.5394234437989667, -24.24056378642895737, 322.0356252759110021 ) ) ;
#63478 = VERTEX_POINT ( 'NONE', #10261 ) ;
#63479 = CARTESIAN_POINT ( 'NONE',  ( 98.34954239462810222, -31.65711219339656424, 115.9083548605937750 ) ) ;
#63480 = AXIS2_PLACEMENT_3D ( 'NONE', #25715, #14677, #84173 ) ;
#63481 = ORIENTED_EDGE ( 'NONE', *, *, #2228, .F. ) ;
#63482 = CARTESIAN_POINT ( 'NONE',  ( 105.7157523590067854, -46.72390646314000406, 133.4701676439947278 ) ) ;
#63483 = VERTEX_POINT ( 'NONE', #23903 ) ;
#63484 = EDGE_LOOP ( 'NONE', ( #77089, #48871, #75299, #33559, #33838 ) ) ;
#63485 = VECTOR ( 'NONE', #3641, 1000.000000000000000 ) ;
#63486 = DIRECTION ( 'NONE',  ( 0.000000000000000000, 1.000000000000000000, 0.000000000000000000 ) ) ;
#63487 = CIRCLE ( 'NONE', #89632, 27.99999999999999645 ) ;
#63488 = FACE_OUTER_BOUND ( 'NONE', #70592, .T. ) ;
#63489 = CARTESIAN_POINT ( 'NONE',  ( 116.4746376734894255, -32.23794665461475972, 19.18133956162493092 ) ) ;
#63490 = CARTESIAN_POINT ( 'NONE',  ( 23.27731929905161934, 54.66493626280016827, 30.16249999999999076 ) ) ;
#63491 = EDGE_CURVE ( 'NONE', #29444, #86064, #8585, .T. ) ;
#63492 = DIRECTION ( 'NONE',  ( 1.000000000000000000, 0.000000000000000000, 0.000000000000000000 ) ) ;
#63493 = DIRECTION ( 'NONE',  ( 0.9130365726098600421, 0.000000000000000000, 0.4078776986755216494 ) ) ;
#63494 = CARTESIAN_POINT ( 'NONE',  ( 96.85055626654745708, -38.51091292166576352, 46.45181575210194325 ) ) ;
#63496 = CARTESIAN_POINT ( 'NONE',  ( 102.3226935662337524, -26.77152163616663927, 136.4422919425779526 ) ) ;
#63495 = CARTESIAN_POINT ( 'NONE',  ( 106.5131950068454216, -24.24167068730766417, 320.8164078654934315 ) ) ;
#63497 = CARTESIAN_POINT ( 'NONE',  ( 102.0670549536967400, -27.97049806286341322, 71.48979194315724328 ) ) ;
#63498 = ORIENTED_EDGE ( 'NONE', *, *, #2468, .T. ) ;
#63499 = PLANE ( 'NONE',  #48269 ) ;
#63500 = DIRECTION ( 'NONE',  ( 0.000000000000000000, 0.000000000000000000, 1.000000000000000000 ) ) ;
#63501 = DIRECTION ( 'NONE',  ( 0.000000000000000000, 0.000000000000000000, 1.000000000000000000 ) ) ;
#63502 = ORIENTED_EDGE ( 'NONE', *, *, #62317, .T. ) ;
#63503 = AXIS2_PLACEMENT_3D ( 'NONE', #10431, #3179, #45812 ) ;
#63504 = CARTESIAN_POINT ( 'NONE',  ( 37.03715912545433042, -48.62818131006122258, 249.9678068554150343 ) ) ;
#63506 = VERTEX_POINT ( 'NONE', #72494 ) ;
#63505 = CARTESIAN_POINT ( 'NONE',  ( 107.5678864575881590, -47.81824684668375625, 192.6003871806729535 ) ) ;
#63507 = DIRECTION ( 'NONE',  ( 1.000000000000000000, 4.299999999999999979E-14, 1.000000000000000078E-15 ) ) ;
#63508 = CARTESIAN_POINT ( 'NONE',  ( 103.2957022058525780, -26.98683617215391806, 211.3699109901969848 ) ) ;
#63509 = CARTESIAN_POINT ( 'NONE',  ( 114.5987772146603731, -44.05082428708011832, 94.21276813305395592 ) ) ;
#63510 = CIRCLE ( 'NONE', #18500, 1.000000000000000888 ) ;
#63511 = CARTESIAN_POINT ( 'NONE',  ( 96.20681132576044092, 71.15434825076368952, 88.25674559704650335 ) ) ;
#63512 = VECTOR ( 'NONE', #55196, 1000.000000000000000 ) ;
#63513 = CARTESIAN_POINT ( 'NONE',  ( 172.5664832912729878, -27.82844715994070484, 195.9256252759119832 ) ) ;
#63514 = CARTESIAN_POINT ( 'NONE',  ( -254.0000000000000000, 93.66249999999999432, 11.11250000000040217 ) ) ;
#63515 = ORIENTED_EDGE ( 'NONE', *, *, #49663, .F. ) ;
#63516 = CIRCLE ( 'NONE', #41712, 15.00000000000000000 ) ;
#63517 = EDGE_CURVE ( 'NONE', #73802, #3245, #47772, .T. ) ;
#63518 = ITEM_DEFINED_TRANSFORMATION ( 'NONE', 'NONE', #82713,  #50656 ) ;
#63519 = EDGE_CURVE ( 'NONE', #976, #65985, #36197, .T. ) ;
#63520 = ORIENTED_EDGE ( 'NONE', *, *, #27758, .T. ) ;
#63521 = ORIENTED_EDGE ( 'NONE', *, *, #33359, .T. ) ;
#63522 = EDGE_CURVE ( 'NONE', #12659, #34867, #64782, .T. ) ;
#63523 = ORIENTED_EDGE ( 'NONE', *, *, #474, .F. ) ;
#63524 = CARTESIAN_POINT ( 'NONE',  ( -3.174999999999664979, 24.56180297284579694, 31.75000000000000000 ) ) ;
#63525 = CARTESIAN_POINT ( 'NONE',  ( 118.0816017896457453, -32.35888884030432422, 245.1270538473389706 ) ) ;
#63526 = DIRECTION ( 'NONE',  ( 0.000000000000000000, 0.000000000000000000, -1.000000000000000000 ) ) ;
#63527 = DIRECTION ( 'NONE',  ( 0.000000000000000000, 0.000000000000000000, -1.000000000000000000 ) ) ;
#63528 = ADVANCED_FACE ( 'NONE', ( #57956 ), #86128, .T. ) ;
#63529 = ADVANCED_FACE ( 'NONE', ( #37528 ), #49268, .F. ) ;
#63531 = DIRECTION ( 'NONE',  ( 0.000000000000000000, 0.000000000000000000, 1.000000000000000000 ) ) ;
#63530 = CARTESIAN_POINT ( 'NONE',  ( -458.3598257906459708, 60.32499999999999574, 3.174999999999999822 ) ) ;
#63532 = CARTESIAN_POINT ( 'NONE',  ( -41.60202597009397607, 65.59999999999998010, 34.51824159735389941 ) ) ;
#63533 = CARTESIAN_POINT ( 'NONE',  ( 97.05407301568530443, -33.74649485729950271, 31.09562527591097592 ) ) ;
#63534 = EDGE_LOOP ( 'NONE', ( #34302, #66480, #56033, #33756 ) ) ;
#63535 = CIRCLE ( 'NONE', #47630, 3.174999999999997158 ) ;
#63536 = EDGE_CURVE ( 'NONE', #57574, #69150, #60819, .T. ) ;
#63537 = ORIENTED_EDGE ( 'NONE', *, *, #84676, .T. ) ;
#63538 = CARTESIAN_POINT ( 'NONE',  ( 33.96670390244699433, -28.27351298637401200, 342.9256252759119548 ) ) ;
#63540 = EDGE_CURVE ( 'NONE', #25358, #8047, #43657, .T. ) ;
#63539 = CARTESIAN_POINT ( 'NONE',  ( 97.31298885056827430, -38.96024362731790802, 17.50578975050363439 ) ) ;
#63541 = CARTESIAN_POINT ( 'NONE',  ( 111.2075884809769803, -27.22220029719803591, 280.7375300378151337 ) ) ;
#63542 = CARTESIAN_POINT ( 'NONE',  ( 20.03715912545735378, -24.42818131006189830, 249.9678068554150059 ) ) ;
#63543 = CARTESIAN_POINT ( 'NONE',  ( 114.2351621074132026, -44.22269940884944361, 109.1718157521009687 ) ) ;
#63544 = CARTESIAN_POINT ( 'NONE',  ( 88.90000000000000568, 66.67499999999999716, 244.4749999999999943 ) ) ;
#63545 = EDGE_CURVE ( 'NONE', #27744, #62140, #24342, .T. ) ;
#63546 = CARTESIAN_POINT ( 'NONE',  ( -75.11741860696075435, 54.02010448448870505, 30.79984509629914768 ) ) ;
#63547 = EDGE_LOOP ( 'NONE', ( #14675, #42759, #29258, #47260, #1585, #49550 ) ) ;
#63548 = CYLINDRICAL_SURFACE ( 'NONE', #16750, 4.875000000000017764 ) ;
#63549 = VECTOR ( 'NONE', #59000, 1000.000000000000000 ) ;
#63550 = ORIENTED_EDGE ( 'NONE', *, *, #3499, .F. ) ;
#63551 = ORIENTED_EDGE ( 'NONE', *, *, #39242, .F. ) ;
#63552 = CARTESIAN_POINT ( 'NONE',  ( -84.99753727674097092, 95.14807216649714405, 82.65057572782355066 ) ) ;
#63553 = CARTESIAN_POINT ( 'NONE',  ( 103.6867908865108916, -46.21882986916993730, 248.7358690201829745 ) ) ;
#63554 = VECTOR ( 'NONE', #74143, 1000.000000000000000 ) ;
#63555 = CARTESIAN_POINT ( 'NONE',  ( 116.3232968930447839, -32.93863405887816498, 194.1356252759109680 ) ) ;
#63556 = AXIS2_PLACEMENT_3D ( 'NONE', #61267, #12691, #19946 ) ;
#63557 = CARTESIAN_POINT ( 'NONE',  ( -118.1268318574024221, 90.28416741362501341, 10.08204661438704619 ) ) ;
#63558 = DIRECTION ( 'NONE',  ( 0.8543009526837940237, 0.03605348183280988883, -0.5185267868599396923 ) ) ;
#63559 = CARTESIAN_POINT ( 'NONE',  ( 80.88709205069450547, 70.52090377575432001, -86.67734222162502533 ) ) ;
#63560 = EDGE_LOOP ( 'NONE', ( #20191, #10314, #8178, #8300 ) ) ;
#63561 = CYLINDRICAL_SURFACE ( 'NONE', #30526, 3.299999999999997158 ) ;
#63562 = EDGE_CURVE ( 'NONE', #24002, #49561, #18803, .T. ) ;
#63563 = DIRECTION ( 'NONE',  ( 0.000000000000000000, 1.000000000000000000, 0.000000000000000000 ) ) ;
#63564 = EDGE_LOOP ( 'NONE', ( #35919, #20694, #75659, #59231 ) ) ;
#63565 = CARTESIAN_POINT ( 'NONE',  ( 106.9273489086460387, -26.26968863985776537, 60.08705384733897858 ) ) ;
#63566 = ORIENTED_EDGE ( 'NONE', *, *, #66890, .F. ) ;
#63567 = EDGE_CURVE ( 'NONE', #32260, #79836, #36013, .T. ) ;
#63568 = CARTESIAN_POINT ( 'NONE',  ( 102.4109068130577356, -29.56832019646944687, 24.95813411379099733 ) ) ;
#63569 = EDGE_CURVE ( 'NONE', #3381, #74492, #64614, .T. ) ;
#63570 = VECTOR ( 'NONE', #35158, 1000.000000000000000 ) ;
#63571 = CARTESIAN_POINT ( 'NONE',  ( 116.7956373554045939, -39.38598825398587877, 128.6149081173567765 ) ) ;
#63572 = CARTESIAN_POINT ( 'NONE',  ( 109.6835627966675162, -27.30531164764922991, 174.8613395616259822 ) ) ;
#63573 = CARTESIAN_POINT ( 'NONE',  ( 80.06648329127402519, -46.72944715994105991, 10.72562527591094295 ) ) ;
#63574 = LINE ( 'NONE', #29058, #9534 ) ;
#63575 = AXIS2_PLACEMENT_3D ( 'NONE', #47564, #68482, #80330 ) ;
#63577 = EDGE_CURVE ( 'NONE', #45437, #52825, #86963, .T. ) ;
#63576 = FACE_BOUND ( 'NONE', #24555, .T. ) ;
#63578 = VECTOR ( 'NONE', #68984, 1000.000000000000000 ) ;
#63579 = CARTESIAN_POINT ( 'NONE',  ( 156.5667039024482108, -48.82844715993569196, 295.7178068554149490 ) ) ;
#63580 = CARTESIAN_POINT ( 'NONE',  ( 96.87194279380025819, -34.19777600025749109, 272.1327681330539576 ) ) ;
#63581 = CARTESIAN_POINT ( 'NONE',  ( 97.80792351950141494, -40.51905676813210988, 116.6359120812046939 ) ) ;
#63582 = VERTEX_POINT ( 'NONE', #35554 ) ;
#63583 = CARTESIAN_POINT ( 'NONE',  ( 136.8105871997951226, -36.91414947189760909, 6.758631288823576888 ) ) ;
#63584 = VERTEX_POINT ( 'NONE', #70084 ) ;
#63585 = CARTESIAN_POINT ( 'NONE',  ( 117.4068710881028323, -38.36326476267787200, 109.7013395616249767 ) ) ;
#63586 = CARTESIAN_POINT ( 'NONE',  ( 120.6819903923023389, 46.87498547512231539, -49.80728659620316989 ) ) ;
#63587 = ORIENTED_EDGE ( 'NONE', *, *, #9850, .F. ) ;
#63588 = ORIENTED_EDGE ( 'NONE', *, *, #15684, .T. ) ;
#63589 = VERTEX_POINT ( 'NONE', #22849 ) ;
#63590 = AXIS2_PLACEMENT_3D ( 'NONE', #5963, #34542, #75446 ) ;
#63591 = DIRECTION ( 'NONE',  ( 0.000000000000000000, 0.000000000000000000, -1.000000000000000000 ) ) ;
#63592 = CARTESIAN_POINT ( 'NONE',  ( 100.9546836996216825, -28.70701758901807210, 266.5939575379834423 ) ) ;
#63593 = DIRECTION ( 'NONE',  ( 0.000000000000000000, 0.000000000000000000, 1.000000000000000000 ) ) ;
#63594 = CARTESIAN_POINT ( 'NONE',  ( 3.174999999999879918, 24.56180297284579694, -33.98325472291465132 ) ) ;
#63595 = CYLINDRICAL_SURFACE ( 'NONE', #27283, 12.99999999999999822 ) ;
#63596 = CARTESIAN_POINT ( 'NONE',  ( 111.1289525437170056, -47.00905435842401658, 18.88800622829195319 ) ) ;
#63597 = CARTESIAN_POINT ( 'NONE',  ( 180.2143765759489895, -35.91149509761070391, -5.074374724088000832 ) ) ;
#63598 = VERTEX_POINT ( 'NONE', #43710 ) ;
#63599 = DIRECTION ( 'NONE',  ( 0.000000000000000000, 0.000000000000000000, -1.000000000000000000 ) ) ;
#63600 = AXIS2_PLACEMENT_3D ( 'NONE', #5937, #75419, #54034 ) ;
#63601 = DIRECTION ( 'NONE',  ( -0.000000000000000000, 1.000000000000000000, -0.000000000000000000 ) ) ;
#63602 = VERTEX_POINT ( 'NONE', #9213 ) ;
#63604 = ORIENTED_EDGE ( 'NONE', *, *, #44343, .F. ) ;
#63603 = VECTOR ( 'NONE', #76499, 1000.000000000000000 ) ;
#63605 = CYLINDRICAL_SURFACE ( 'NONE', #59020, 3.300000000000000711 ) ;
#63606 = CARTESIAN_POINT ( 'NONE',  ( 116.3191307872214821, -32.94748812527954840, 115.1356252759109822 ) ) ;
#63607 = FACE_OUTER_BOUND ( 'NONE', #56956, .T. ) ;
#63608 = DIRECTION ( 'NONE',  ( 1.000000000000000000, 0.000000000000000000, 0.000000000000000000 ) ) ;
#63609 = DIRECTION ( 'NONE',  ( 0.000000000000000000, 0.000000000000000000, -1.000000000000000000 ) ) ;
#63610 = CARTESIAN_POINT ( 'NONE',  ( 108.3843752505750331, -28.29029480288096465, 189.3752769709339816 ) ) ;
#63611 = CARTESIAN_POINT ( 'NONE',  ( 62.03715912545838762, -47.82818131006021645, 249.9678068554150343 ) ) ;
#63612 = CARTESIAN_POINT ( 'NONE',  ( 125.3763439628640128, 68.77237897621238005, 36.41030492311487166 ) ) ;
#63613 = CARTESIAN_POINT ( 'NONE',  ( 103.2628093650484828, -47.15753175352042348, 97.28610146638693834 ) ) ;
#63614 = EDGE_LOOP ( 'NONE', ( #79342, #5823, #29765, #20017 ) ) ;
#63615 = CARTESIAN_POINT ( 'NONE',  ( 107.0664832912739399, -36.72944715994095333, 311.6356252759109680 ) ) ;
#63616 = ORIENTED_EDGE ( 'NONE', *, *, #2457, .T. ) ;
#63617 = CARTESIAN_POINT ( 'NONE',  ( 97.33710672311610779, -34.07376039389686184, 277.1149365882106963 ) ) ;
#63618 = VERTEX_POINT ( 'NONE', #84184 ) ;
#63619 = PLANE ( 'NONE',  #9958 ) ;
#63620 = VERTEX_POINT ( 'NONE', #50528 ) ;
#63621 = CARTESIAN_POINT ( 'NONE',  ( 188.5667039024479834, -67.87844715994100397, 262.0928068554150059 ) ) ;
#63622 = CARTESIAN_POINT ( 'NONE',  ( 67.06674209438934042, -104.4391121967051816, 246.0899098363300084 ) ) ;
#63624 = CARTESIAN_POINT ( 'NONE',  ( 110.2536356736639220, -106.6957733451320394, 2.217806855418086087 ) ) ;
#63623 = AXIS2_PLACEMENT_3D ( 'NONE', #74583, #68229, #67771 ) ;
#63625 = ORIENTED_EDGE ( 'NONE', *, *, #35071, .T. ) ;
#63626 = VECTOR ( 'NONE', #79114, 1000.000000000000000 ) ;
#63627 = CARTESIAN_POINT ( 'NONE',  ( 103.8344565422589767, -46.70152647745319996, 82.32705384733995402 ) ) ;
#63628 = SHAPE_REPRESENTATION_RELATIONSHIP ( 'NONE' , 'NONE' ,  #48599, #83525 ) ;
#63630 = CARTESIAN_POINT ( 'NONE',  ( 96.22129751242547968, 71.14122173980733521, -88.24354053934760600 ) ) ;
#63629 = CARTESIAN_POINT ( 'NONE',  ( 100.9542232131455108, -28.70737172392434644, 165.5940040971896963 ) ) ;
#63631 = LINE ( 'NONE', #29116, #32231 ) ;
#63632 = EDGE_CURVE ( 'NONE', #70197, #39210, #85080, .T. ) ;
#63633 = CARTESIAN_POINT ( 'NONE',  ( 116.7951252696762623, -39.38782979722077471, 143.6147919419995844 ) ) ;
#63634 = ORIENTED_EDGE ( 'NONE', *, *, #39846, .F. ) ;
#63636 = ADVANCED_FACE ( 'NONE', ( #56439 ), #70543, .F. ) ;
#63635 = CIRCLE ( 'NONE', #73806, 4.749999999999976907 ) ;
#63637 = DIRECTION ( 'NONE',  ( 0.7071067811865460184, 0.000000000000000000, 0.7071067811865489050 ) ) ;
#63638 = CARTESIAN_POINT ( 'NONE',  ( 102.0670550253074822, -27.97049802292532306, 155.4897919366790404 ) ) ;
#63639 = AXIS2_PLACEMENT_3D ( 'NONE', #12383, #54130, #4677 ) ;
#63640 = CARTESIAN_POINT ( 'NONE',  ( -446.0240000000000009, 53.97500000000000142, 0.000000000000000000 ) ) ;
#63641 = ADVANCED_FACE ( 'NONE', ( #78269 ), #1046, .F. ) ;
#63643 = ADVANCED_FACE ( 'NONE', ( #14686 ), #77808, .T. ) ;
#63642 = CARTESIAN_POINT ( 'NONE',  ( 97.91349202876114077, -31.62044072442156306, 106.9213395616259703 ) ) ;
#63645 = DIRECTION ( 'NONE',  ( 0.000000000000000000, 0.000000000000000000, 1.000000000000000000 ) ) ;
#63644 = CARTESIAN_POINT ( 'NONE',  ( 141.3509999999999991, 101.5999999999999943, -141.3509999999999991 ) ) ;
#63646 = CARTESIAN_POINT ( 'NONE',  ( 108.0667039024470171, -87.35579742913172652, -21.78219314458254630 ) ) ;
#63647 = EDGE_CURVE ( 'NONE', #73852, #9110, #7217, .T. ) ;
#63648 = ORIENTED_EDGE ( 'NONE', *, *, #60839, .F. ) ;
#63650 = EDGE_CURVE ( 'NONE', #72907, #27384, #29210, .T. ) ;
#63649 = CARTESIAN_POINT ( 'NONE',  ( 86.06670390244796920, -58.72944715994110254, 310.9178068554150514 ) ) ;
#63651 = CARTESIAN_POINT ( 'NONE',  ( 108.5509251780138129, -26.47246927008498929, 145.9737205140059473 ) ) ;
#63652 = CIRCLE ( 'NONE', #40423, 4.749999999999976907 ) ;
#63654 = VERTEX_POINT ( 'NONE', #56893 ) ;
#63653 = LINE ( 'NONE', #14616, #3670 ) ;
#63655 = CARTESIAN_POINT ( 'NONE',  ( 98.07879728544668296, -32.87107120142745487, 12.00419670448193976 ) ) ;
#63656 = PLANE ( 'NONE',  #86091 ) ;
#63657 = CARTESIAN_POINT ( 'NONE',  ( 62.03742497533654188, -23.42844715994041493, 180.4678068554151196 ) ) ;
#63658 = CARTESIAN_POINT ( 'NONE',  ( 110.8821949118856622, -76.97768462775962917, 250.2178068554180470 ) ) ;
#63659 = DIRECTION ( 'NONE',  ( 1.000000000000000000, 1.387778780781444413E-14, 0.000000000000000000 ) ) ;
#63660 = EDGE_CURVE ( 'NONE', #85940, #22487, #84632, .T. ) ;
#63661 = CARTESIAN_POINT ( 'NONE',  ( 152.0371591254582881, -47.82818131005588214, 313.9678068554149490 ) ) ;
#63662 = CYLINDRICAL_SURFACE ( 'NONE', #84985, 9.999999999999998224 ) ;
#63663 = CARTESIAN_POINT ( 'NONE',  ( 97.41213207386795148, -40.51524797426110069, 246.6118157521019896 ) ) ;
#63664 = EDGE_LOOP ( 'NONE', ( #48462, #17520, #46192, #74807 ) ) ;
#63665 = VERTEX_POINT ( 'NONE', #50073 ) ;
#63667 = EDGE_CURVE ( 'NONE', #6135, #3336, #43258, .T. ) ;
#63666 = VECTOR ( 'NONE', #48659, 1000.000000000000000 ) ;
#63668 = CARTESIAN_POINT ( 'NONE',  ( 98.21222678671237816, -37.09057735734792516, 157.7901547344689845 ) ) ;
#63669 = CARTESIAN_POINT ( 'NONE',  ( 103.1875000000000000, 127.0000000000000000, 3.602774393244745134E-13 ) ) ;
#63670 = CARTESIAN_POINT ( 'NONE',  ( 106.3742716537777113, -27.86474340539431793, 21.57015473446893949 ) ) ;
#63671 = DIRECTION ( 'NONE',  ( 0.9999999853157766072, 0.0001713722455994998422, -0.000000000000000000 ) ) ;
#63672 = CARTESIAN_POINT ( 'NONE',  ( 33.96670390244699433, -28.27351298637401200, -5.074374724088000832 ) ) ;
#63673 = DIRECTION ( 'NONE',  ( -0.000000000000000000, -1.000000000000000000, 0.000000000000000000 ) ) ;
#63674 = DIRECTION ( 'NONE',  ( 2.900000000000000265E-14, -2.000000000000000155E-15, 1.000000000000000000 ) ) ;
#63675 = CARTESIAN_POINT ( 'NONE',  ( 107.0667039024470313, -104.2784471599420755, -19.78219314458201694 ) ) ;
#63676 = CARTESIAN_POINT ( 'NONE',  ( 104.1918496689534948, -26.69446299336401296, 225.2984824187679749 ) ) ;
#63677 = CARTESIAN_POINT ( 'NONE',  ( 5.203398961192315042, 94.03281790535285722, 118.2421799489154211 ) ) ;
#63678 = ORIENTED_EDGE ( 'NONE', *, *, #5222, .T. ) ;
#63679 = ORIENTED_EDGE ( 'NONE', *, *, #41167, .T. ) ;
#63680 = EDGE_CURVE ( 'NONE', #44764, #36112, #71028, .T. ) ;
#63681 = VECTOR ( 'NONE', #74565, 1000.000000000000000 ) ;
#63682 = CYLINDRICAL_SURFACE ( 'NONE', #83674, 3.968750000000020872 ) ;
#63683 = CARTESIAN_POINT ( 'NONE',  ( -90.31319802837603561, 90.93089219781636245, -76.80574412431033693 ) ) ;
#63684 = CARTESIAN_POINT ( 'NONE',  ( 172.5664832912740110, -18.82844715994099971, 138.9256252759119832 ) ) ;
#63686 = EDGE_CURVE ( 'NONE', #11403, #26317, #71721, .T. ) ;
#63685 = LINE ( 'NONE', #15994, #12864 ) ;
#63687 = CARTESIAN_POINT ( 'NONE',  ( 111.0600676159102278, -27.80113716328034457, 20.74133956162494030 ) ) ;
#63689 = CARTESIAN_POINT ( 'NONE',  ( 70.98999999999998067, 52.73749999999999716, -36.61250000000002558 ) ) ;
#63688 = AXIS2_PLACEMENT_3D ( 'NONE', #63437, #43422, #48429 ) ;
#63690 = AXIS2_PLACEMENT_3D ( 'NONE', #59752, #87486, #36320 ) ;
#63691 = ORIENTED_EDGE ( 'NONE', *, *, #35262, .F. ) ;
#63692 = CARTESIAN_POINT ( 'NONE',  ( 105.1556394555663445, -47.05180815895162993, 8.429910990196965770 ) ) ;
#63693 = CARTESIAN_POINT ( 'NONE',  ( 51.06648329127400388, -0.2185775633790978945, 333.4006252759120343 ) ) ;
#63694 = CARTESIAN_POINT ( 'NONE',  ( 118.6541713771196527, -39.21258442193070692, 258.6584824187679033 ) ) ;
#63695 = ORIENTED_EDGE ( 'NONE', *, *, #81332, .F. ) ;
#63696 = AXIS2_PLACEMENT_3D ( 'NONE', #50499, #9186, #8746 ) ;
#63697 = CARTESIAN_POINT ( 'NONE',  ( 77.31648329127401098, -36.72944715994107412, 6.749768910606400496 ) ) ;
#63698 = CARTESIAN_POINT ( 'NONE',  ( 172.5664832912729878, -27.82844715994070484, 258.9256252759120116 ) ) ;
#63699 = CARTESIAN_POINT ( 'NONE',  ( 163.5667039024460223, -18.82844715994099971, -5.074374724088000832 ) ) ;
#63700 = CARTESIAN_POINT ( 'NONE',  ( 100.2074232480821365, -30.48050913114499849, 78.55666179816195438 ) ) ;
#63702 = CARTESIAN_POINT ( 'NONE',  ( 116.3696522983621549, -44.11004992080503229, 194.2927681330539542 ) ) ;
#63701 = VECTOR ( 'NONE', #22139, 1000.000000000000000 ) ;
#63703 = DIRECTION ( 'NONE',  ( 0.4999999999999998890, 0.8660254037844387076, 0.000000000000000000 ) ) ;
#63704 = ORIENTED_EDGE ( 'NONE', *, *, #45957, .T. ) ;
#63705 = AXIS2_PLACEMENT_3D ( 'NONE', #51429, #79177, #2415 ) ;
#63706 = DIRECTION ( 'NONE',  ( -0.000000000000000000, -1.000000000000000000, -0.000000000000000000 ) ) ;
#63707 = EDGE_LOOP ( 'NONE', ( #40568, #52872 ) ) ;
#63708 = ORIENTED_EDGE ( 'NONE', *, *, #13993, .F. ) ;
#63709 = EDGE_CURVE ( 'NONE', #86064, #46578, #14234, .T. ) ;
#63710 = DIRECTION ( 'NONE',  ( 1.000000000000000078E-15, -1.000000000000000083E-30, -1.000000000000000000 ) ) ;
#63711 = ORIENTED_EDGE ( 'NONE', *, *, #9191, .F. ) ;
#63712 = ORIENTED_EDGE ( 'NONE', *, *, #54670, .F. ) ;
#63713 = LINE ( 'NONE', #28743, #73011 ) ;
#63714 = DIRECTION ( 'NONE',  ( 1.000000000000000000, 4.163336342344333240E-14, 0.000000000000000000 ) ) ;
#63715 = VECTOR ( 'NONE', #25844, 1000.000000000000000 ) ;
#63716 = CARTESIAN_POINT ( 'NONE',  ( 107.2022627278996652, -27.67438038655213006, 79.49908649474396327 ) ) ;
#63717 = CARTESIAN_POINT ( 'NONE',  ( 116.3368571269942464, -41.54685706111320087, 288.4441967044822945 ) ) ;
#63718 = CARTESIAN_POINT ( 'NONE',  ( -4.481506956522084195, 70.65969245518890318, 130.4796279538066983 ) ) ;
#63719 = B_SPLINE_CURVE_WITH_KNOTS ( 'NONE', 3,
 ( #74193, #20577, #81028, #11971, #40100, #6934, #34181, #68277, #60538, #32844, #67816, #62342, #13750, #54155, #6058, #82363, #88286, #26042, #75536, #55053, #41435, #39654, #6483, #82813, #67356 ),
 .UNSPECIFIED., .F., .F.,
 ( 4, 2, 2, 1, 2, 2, 2, 2, 2, 2, 2, 2, 4 ),
 ( 0.03942115529576777772, 0.04188556809382155272, 0.04311777449284841940, 0.04434998089187528608, 0.04558218729090215277, 0.04681439368992901945, 0.04927880648798271812, 0.05051101288700958480, 0.05174321928603645149, 0.05420763208409021261, 0.05543983848311708623, 0.05667204488214395985, 0.05913645768019770710 ),
 .UNSPECIFIED. ) ;
#63720 = CARTESIAN_POINT ( 'NONE',  ( 0.000000000000000000, 211.0000000000000000, 154.6557476874258441 ) ) ;
#63721 = ORIENTED_EDGE ( 'NONE', *, *, #8686, .T. ) ;
#63722 = ORIENTED_EDGE ( 'NONE', *, *, #86849, .F. ) ;
#63723 = DIRECTION ( 'NONE',  ( 1.000000000000000000, -0.000000000000000000, 2.108231265501709878E-16 ) ) ;
#63724 = DIRECTION ( 'NONE',  ( 1.000000000000000000, 0.000000000000000000, 0.000000000000000000 ) ) ;
#63725 = CARTESIAN_POINT ( 'NONE',  ( 70.81267823946878082, -139.1710219483943263, 247.4769279846591701 ) ) ;
#63727 = EDGE_CURVE ( 'NONE', #84681, #64226, #35102, .T. ) ;
#63726 = VECTOR ( 'NONE', #77086, 1000.000000000000000 ) ;
#63728 = CARTESIAN_POINT ( 'NONE',  ( 102.5967720069230324, -27.99243076246517603, 120.4527681330539792 ) ) ;
#63729 = CARTESIAN_POINT ( 'NONE',  ( 103.1890357985451345, -46.49249970849451330, 117.2756252759109543 ) ) ;
#63730 = CARTESIAN_POINT ( 'NONE',  ( 118.3887371170988132, -33.06383674033636311, 284.0756252759109657 ) ) ;
#63731 = EDGE_LOOP ( 'NONE', ( #37525, #35184, #28909, #64535 ) ) ;
#63732 = CARTESIAN_POINT ( 'NONE',  ( 96.77253738264830929, -34.86918258059447595, 241.1841967044819626 ) ) ;
#63733 = FACE_OUTER_BOUND ( 'NONE', #16919, .T. ) ;
#63734 = CARTESIAN_POINT ( 'NONE',  ( 172.5664832912740110, 0.2215528400590013880, 198.9256252759119832 ) ) ;
#63735 = DIRECTION ( 'NONE',  ( -1.000000000000000078E-15, 1.000000000000000083E-30, 1.000000000000000000 ) ) ;
#63736 = EDGE_CURVE ( 'NONE', #53446, #19496, #10127, .T. ) ;
#63738 = DIRECTION ( 'NONE',  ( 0.000000000000000000, 0.000000000000000000, -1.000000000000000000 ) ) ;
#63737 = PLANE ( 'NONE',  #79645 ) ;
#63739 = CARTESIAN_POINT ( 'NONE',  ( 105.0911950360329712, -25.44184036110743108, 322.1652889949337464 ) ) ;
#63740 = EDGE_CURVE ( 'NONE', #72479, #59669, #81725, .T. ) ;
#63741 = CARTESIAN_POINT ( 'NONE',  ( 31.56670390244700641, -19.82844715994111340, -5.074374724088000832 ) ) ;
#63742 = CARTESIAN_POINT ( 'NONE',  ( 132.2449836194497550, -38.78962918510080016, 7.677444906558990922 ) ) ;
#63743 = EDGE_CURVE ( 'NONE', #26589, #87561, #73909, .T. ) ;
#63744 = CARTESIAN_POINT ( 'NONE',  ( -3.174999999999644995, 17.78000000000000114, 33.98325472291465132 ) ) ;
#63745 = CARTESIAN_POINT ( 'NONE',  ( 62.03742497533745137, -23.42844715994041849, 313.9678068554150059 ) ) ;
#63746 = DIRECTION ( 'NONE',  ( 0.000000000000000000, 0.000000000000000000, 1.000000000000000000 ) ) ;
#63748 = VERTEX_POINT ( 'NONE', #374 ) ;
#63747 = CARTESIAN_POINT ( 'NONE',  ( 83.56670390244798341, -34.21194715994108293, 229.5838068554169524 ) ) ;
#63749 = CIRCLE ( 'NONE', #2803, 0.3000000000000062617 ) ;
#63750 = EDGE_CURVE ( 'NONE', #1770, #20391, #41688, .T. ) ;
#63751 = DIRECTION ( 'NONE',  ( 1.000000000000000000, 1.000000000000000078E-15, 0.000000000000000000 ) ) ;
#63752 = CARTESIAN_POINT ( 'NONE',  ( 117.5128880048294491, -35.85709896013243281, 253.8927681330537780 ) ) ;
#63753 = CARTESIAN_POINT ( 'NONE',  ( 102.0510343613854189, -46.57928231165939081, 168.2137205140059564 ) ) ;
#63754 = CARTESIAN_POINT ( 'NONE',  ( 112.1919128969917097, -27.58564230820396190, 30.66991099019694644 ) ) ;
#63756 = CARTESIAN_POINT ( 'NONE',  ( 98.30753419281403183, -41.72887549490040726, 46.73979194292225969 ) ) ;
#63755 = DIRECTION ( 'NONE',  ( 1.000000000000000078E-15, -1.000000000000000083E-30, -1.000000000000000000 ) ) ;
#63757 = CARTESIAN_POINT ( 'NONE',  ( 98.38051519723421734, -41.69543662888409585, 137.7397802884137263 ) ) ;
#63758 = AXIS2_PLACEMENT_3D ( 'NONE', #76450, #62810, #63724 ) ;
#63759 = VECTOR ( 'NONE', #18775, 1000.000000000000000 ) ;
#63760 = ADVANCED_FACE ( 'NONE', ( #89881 ), #43435, .F. ) ;
#63761 = ORIENTED_EDGE ( 'NONE', *, *, #37486, .T. ) ;
#63762 = CARTESIAN_POINT ( 'NONE',  ( 138.0667039024480971, -58.72944715994091069, 199.5838068554170093 ) ) ;
#63763 = ORIENTED_EDGE ( 'NONE', *, *, #48011, .T. ) ;
#63764 = ADVANCED_FACE ( 'NONE', ( #33987 ), #74893, .T. ) ;
#63765 = CARTESIAN_POINT ( 'NONE',  ( 103.6069473157389922, -44.53891209398362605, 176.6667055423629620 ) ) ;
#63766 = AXIS2_PLACEMENT_3D ( 'NONE', #50848, #43576, #58544 ) ;
#63768 = ORIENTED_EDGE ( 'NONE', *, *, #78733, .T. ) ;
#63767 = DIRECTION ( 'NONE',  ( -1.000000000000000000, -2.756263715554006823E-15, 0.000000000000000000 ) ) ;
#63769 = DIRECTION ( 'NONE',  ( 0.000000000000000000, 0.000000000000000000, 1.000000000000000000 ) ) ;
#63770 = CARTESIAN_POINT ( 'NONE',  ( 117.7567108552514128, -34.01230579303181401, 165.0365776568629315 ) ) ;
#63771 = LINE ( 'NONE', #3327, #26550 ) ;
#63772 =( GEOMETRIC_REPRESENTATION_CONTEXT ( 3 ) GLOBAL_UNCERTAINTY_ASSIGNED_CONTEXT ( ( #19043 ) ) GLOBAL_UNIT_ASSIGNED_CONTEXT ( ( #73666, #11449, #74563 ) ) REPRESENTATION_CONTEXT ( 'NONE', 'WORKASPACE' ) );
#63773 = CARTESIAN_POINT ( 'NONE',  ( 97.06105435396277414, -37.99632269549143615, 151.4278191669818057 ) ) ;
#63774 = CARTESIAN_POINT ( 'NONE',  ( 109.7015479400130999, -27.07733610322067008, 85.86488799970449293 ) ) ;
#63775 = CARTESIAN_POINT ( 'NONE',  ( -78.94931995840738637, 71.76236341258000095, 88.44575049335577432 ) ) ;
#63776 = DIRECTION ( 'NONE',  ( 0.000000000000000000, 1.000000000000000000, 0.000000000000000000 ) ) ;
#63777 = CIRCLE ( 'NONE', #89916, 4.749999999999976907 ) ;
#63778 = CARTESIAN_POINT ( 'NONE',  ( 98.70071965984708129, -42.85747980491203180, 106.8175300378169652 ) ) ;
#63779 = ORIENTED_EDGE ( 'NONE', *, *, #26904, .T. ) ;
#63780 = ORIENTED_EDGE ( 'NONE', *, *, #77805, .T. ) ;
#63781 = VERTEX_POINT ( 'NONE', #5409 ) ;
#63782 = CARTESIAN_POINT ( 'NONE',  ( 114.8570798905637673, -32.50631050113013742, 65.65301187732598009 ) ) ;
#63783 = CARTESIAN_POINT ( 'NONE',  ( 131.3470363009685968, -117.3006669637343293, 250.2178068554179902 ) ) ;
#63785 = CYLINDRICAL_SURFACE ( 'NONE', #18693, 3.000000000000002665 ) ;
#63784 = CARTESIAN_POINT ( 'NONE',  ( 103.8504807240353500, -26.87063827031099450, 206.3394347997199816 ) ) ;
#63786 = DIRECTION ( 'NONE',  ( 0.000000000000000000, 1.000000000000000000, 0.000000000000000000 ) ) ;
#63787 = DIRECTION ( 'NONE',  ( 0.000000000000000000, 0.000000000000000000, -1.000000000000000000 ) ) ;
#63788 = CIRCLE ( 'NONE', #78326, 0.5000000000000004441 ) ;
#63789 = FACE_OUTER_BOUND ( 'NONE', #40825, .T. ) ;
#63790 = LINE ( 'NONE', #70147, #76757 ) ;
#63791 = CARTESIAN_POINT ( 'NONE',  ( 173.9900000000000091, 5.112500000000000711, -58.73749999999999716 ) ) ;
#63792 = CARTESIAN_POINT ( 'NONE',  ( 117.8527506973083518, -39.03601561205234560, 108.6708633711489824 ) ) ;
#63793 = VERTEX_POINT ( 'NONE', #27632 ) ;
#63794 = ORIENTED_EDGE ( 'NONE', *, *, #39326, .F. ) ;
#63795 = ORIENTED_EDGE ( 'NONE', *, *, #89626, .T. ) ;
#63796 = CARTESIAN_POINT ( 'NONE',  ( -2.684158038187649039E-15, 69.84999999999999432, 130.5560000000000116 ) ) ;
#63797 = LINE ( 'NONE', #7487, #66463 ) ;
#63798 = LINE ( 'NONE', #7489, #18928 ) ;
#63800 = ADVANCED_FACE ( 'NONE', ( #61689 ), #33548, .F. ) ;
#63799 = DIRECTION ( 'NONE',  ( 0.000000000000000000, 0.000000000000000000, 1.000000000000000000 ) ) ;
#63801 = CARTESIAN_POINT ( 'NONE',  ( 106.4678557813946043, -44.87017016969328864, 220.3366617981629645 ) ) ;
#63802 = AXIS2_PLACEMENT_3D ( 'NONE', #85143, #65997, #71064 ) ;
#63803 = CYLINDRICAL_SURFACE ( 'NONE', #1557, 1.000000000000000888 ) ;
#63804 = CARTESIAN_POINT ( 'NONE',  ( 98.28068559441094010, -31.05177188324158166, 145.8699109901969848 ) ) ;
#63805 = DIRECTION ( 'NONE',  ( -0.9254794337955620787, -0.3787978585227822492, 0.000000000000000000 ) ) ;
#63806 = ORIENTED_EDGE ( 'NONE', *, *, #42027, .F. ) ;
#63808 = ORIENTED_EDGE ( 'NONE', *, *, #87411, .F. ) ;
#63807 = ORIENTED_EDGE ( 'NONE', *, *, #61243, .F. ) ;
#63809 = VECTOR ( 'NONE', #39629, 1000.000000000000000 ) ;
#63810 = LINE ( 'NONE', #22041, #40408 ) ;
#63811 = EDGE_LOOP ( 'NONE', ( #38529, #29037, #49813, #50961 ) ) ;
#63812 = ORIENTED_EDGE ( 'NONE', *, *, #12068, .F. ) ;
#63813 = CARTESIAN_POINT ( 'NONE',  ( 78.49243652282237349, -20.98954602991689455, 7.829737527532317998 ) ) ;
#63814 = CARTESIAN_POINT ( 'NONE',  ( 105.4788588808462038, 127.0000000000000000, -3.968749999999580336 ) ) ;
#63815 = CARTESIAN_POINT ( 'NONE',  ( 114.0241607691103809, -31.19294522270855907, 240.7930118773259665 ) ) ;
#63816 = VECTOR ( 'NONE', #61054, 1000.000000000000000 ) ;
#63817 = CARTESIAN_POINT ( 'NONE',  ( 142.8698897858160706, -0.9167816978817300289, 542.9756252759101471 ) ) ;
#63818 = EDGE_LOOP ( 'NONE', ( #59813, #41609, #14086, #9514 ) ) ;
#63819 = CARTESIAN_POINT ( 'NONE',  ( 100.5082931581247152, -41.41740168340257355, 9.635625275910943088 ) ) ;
#63820 = CARTESIAN_POINT ( 'NONE',  ( 25.56670390244748248, -48.82844715994178841, 137.2178068554150627 ) ) ;
#63821 = EDGE_LOOP ( 'NONE', ( #17576, #44225 ) ) ;
#63823 = EDGE_LOOP ( 'NONE', ( #89371, #2562, #4378 ) ) ;
#63822 = AXIS2_PLACEMENT_3D ( 'NONE', #35553, #63268, #1044 ) ;
#63824 = EDGE_CURVE ( 'NONE', #49608, #23986, #55313, .T. ) ;
#63825 = DIRECTION ( 'NONE',  ( 0.000000000000000000, 0.000000000000000000, 1.000000000000000000 ) ) ;
#63826 = ORIENTED_EDGE ( 'NONE', *, *, #78443, .F. ) ;
#63827 = ORIENTED_EDGE ( 'NONE', *, *, #84373, .T. ) ;
#63828 = CARTESIAN_POINT ( 'NONE',  ( 110.7250417795893611, -29.43255185136001728, 277.5252332267342581 ) ) ;
#63829 = VECTOR ( 'NONE', #2825, 1000.000000000000000 ) ;
#63830 = CARTESIAN_POINT ( 'NONE',  ( 112.7922847239315161, -45.46795744031502551, 178.0384824187679556 ) ) ;
#63831 = CARTESIAN_POINT ( 'NONE',  ( 112.7897778137182030, -47.07797880090547693, 102.9784824187679817 ) ) ;
#63832 = CARTESIAN_POINT ( 'NONE',  ( 82.54999999999999716, 69.84999999999999432, 346.0750000000000455 ) ) ;
#63833 = DIRECTION ( 'NONE',  ( 1.000000000000000078E-15, 1.000000000000000083E-30, -1.000000000000000000 ) ) ;
#63834 = ORIENTED_EDGE ( 'NONE', *, *, #31026, .T. ) ;
#63835 = CARTESIAN_POINT ( 'NONE',  ( 106.8516137164961464, -47.78059241960190207, 223.5489586092439538 ) ) ;
#63836 = DIRECTION ( 'NONE',  ( -3.100000000000000258E-29, 3.100000000000000044E-14, 1.000000000000000000 ) ) ;
#63837 = DIRECTION ( 'NONE',  ( -1.000000000000000078E-15, 1.000000000000000083E-30, 1.000000000000000000 ) ) ;
#63838 = ORIENTED_EDGE ( 'NONE', *, *, #58524, .F. ) ;
#63839 = LINE ( 'NONE', #1619, #59831 ) ;
#63840 = ORIENTED_EDGE ( 'NONE', *, *, #10823, .T. ) ;
#63841 = ORIENTED_EDGE ( 'NONE', *, *, #3738, .F. ) ;
#63842 = AXIS2_PLACEMENT_3D ( 'NONE', #80836, #4963, #73102 ) ;
#63843 = CARTESIAN_POINT ( 'NONE',  ( 118.9274366748948069, -37.70237179777471681, 188.7613395616259595 ) ) ;
#63844 = EDGE_LOOP ( 'NONE', ( #64601, #84265, #41836, #55144 ) ) ;
#63845 = CARTESIAN_POINT ( 'NONE',  ( 117.2096823498778662, -39.28706705594211712, 123.6299109901969615 ) ) ;
#63846 = CARTESIAN_POINT ( 'NONE',  ( 97.33812887613856901, -34.06989601086925745, 256.1147306920630058 ) ) ;
#63847 = DIRECTION ( 'NONE',  ( 0.000000000000000000, 0.8660254037844428154, -0.4999999999999928946 ) ) ;
#63848 = DIRECTION ( 'NONE',  ( 0.000000000000000000, -1.000000000000000000, 0.000000000000000000 ) ) ;
#63851 = CARTESIAN_POINT ( 'NONE',  ( 118.0177608886752836, -35.41288285714062312, 234.9337205140059552 ) ) ;
#63850 = DIRECTION ( 'NONE',  ( -0.000000000000000000, 0.000000000000000000, -1.000000000000000000 ) ) ;
#63849 = CARTESIAN_POINT ( 'NONE',  ( -47.02966122971771767, 65.60000000000000853, -44.00307561052230199 ) ) ;
#63852 = FACE_OUTER_BOUND ( 'NONE', #70498, .T. ) ;
#63853 = ADVANCED_FACE ( 'NONE', ( #20823 ), #69423, .T. ) ;
#63854 = CARTESIAN_POINT ( 'NONE',  ( 91.91125933621933086, -104.2784471599418339, -11.78219314458200984 ) ) ;
#63855 = AXIS2_PLACEMENT_3D ( 'NONE', #3843, #51963, #10213 ) ;
#63856 = DIRECTION ( 'NONE',  ( 0.000000000000000000, 0.000000000000000000, -1.000000000000000000 ) ) ;
#63857 = ADVANCED_FACE ( 'NONE', ( #8091 ), #14915, .T. ) ;
#63858 = DIRECTION ( 'NONE',  ( -0.9963424814100679816, 0.08544974978095724871, 0.000000000000000000 ) ) ;
#63859 = EDGE_CURVE ( 'NONE', #19807, #75042, #16481, .T. ) ;
#63860 = CARTESIAN_POINT ( 'NONE',  ( 116.3259296754763028, -32.93870509136930025, 260.1356252759109680 ) ) ;
#63861 = CARTESIAN_POINT ( 'NONE',  ( 145.6753386997136488, -136.9877269832281002, 247.4404324032252021 ) ) ;
#63863 = EDGE_LOOP ( 'NONE', ( #42343, #4049, #47649, #25509 ) ) ;
#63862 = DIRECTION ( 'NONE',  ( -0.02150753337724187197, -0.0009076677972194977960, -0.9997682742251811083 ) ) ;
#63864 = EDGE_CURVE ( 'NONE', #56032, #51989, #35781, .T. ) ;
#63865 = CARTESIAN_POINT ( 'NONE',  ( 123.6837132603320413, -56.64645651782492308, 249.5838068554164693 ) ) ;
#63866 = CARTESIAN_POINT ( 'NONE',  ( 117.1474210844629766, -33.86219250605441999, 149.0470538473389581 ) ) ;
#63867 = CARTESIAN_POINT ( 'NONE',  ( 97.07537224739735393, -33.75284044148263973, 27.09562527591097236 ) ) ;
#63868 = CARTESIAN_POINT ( 'NONE',  ( 107.2439061797007156, -47.23213900083308658, 208.5899109901969837 ) ) ;
#63869 = DIRECTION ( 'NONE',  ( 1.000000000000000000, 0.000000000000000000, 0.000000000000000000 ) ) ;
#63870 = DIRECTION ( 'NONE',  ( 0.000000000000000000, 0.000000000000000000, -1.000000000000000000 ) ) ;
#63871 = VECTOR ( 'NONE', #88151, 1000.000000000000000 ) ;
#63873 = DIRECTION ( 'NONE',  ( 1.000000000000000078E-15, -1.000000000000000083E-30, -1.000000000000000000 ) ) ;
#63872 = CARTESIAN_POINT ( 'NONE',  ( 46.48091746482045750, -49.32844715994088602, 180.4678068554150911 ) ) ;
#63874 = CARTESIAN_POINT ( 'NONE',  ( 113.2454987010698773, -28.75867294727909851, 69.55229194226531320 ) ) ;
#63875 = DIRECTION ( 'NONE',  ( 0.000000000000000000, 0.000000000000000000, 1.000000000000000000 ) ) ;
#63876 = ORIENTED_EDGE ( 'NONE', *, *, #25801, .F. ) ;
#63877 = DIRECTION ( 'NONE',  ( 4.237773401492740281E-14, -1.000000000000000000, 0.000000000000000000 ) ) ;
#63878 = EDGE_CURVE ( 'NONE', #26048, #78226, #29887, .T. ) ;
#63879 = ORIENTED_EDGE ( 'NONE', *, *, #66474, .T. ) ;
#63880 = ORIENTED_EDGE ( 'NONE', *, *, #58502, .T. ) ;
#63881 = EDGE_CURVE ( 'NONE', #43132, #31265, #68097, .T. ) ;
#63882 = AXIS2_PLACEMENT_3D ( 'NONE', #32151, #33051, #5357 ) ;
#63884 = EDGE_LOOP ( 'NONE', ( #44911, #31620, #17519, #85779, #61635, #85008 ) ) ;
#63883 = FACE_OUTER_BOUND ( 'NONE', #71513, .T. ) ;
#63885 = CARTESIAN_POINT ( 'NONE',  ( 103.6060256796756960, -46.54035428658114171, 53.30705384733997221 ) ) ;
#63886 = CARTESIAN_POINT ( 'NONE',  ( 53.56670390244743629, -48.82844715994058049, 180.4678068554151196 ) ) ;
#63888 = CARTESIAN_POINT ( 'NONE',  ( 107.0664832912739968, -36.72944715994100306, 287.6356252759109680 ) ) ;
#63887 = VECTOR ( 'NONE', #38705, 1000.000000000000000 ) ;
#63889 = CARTESIAN_POINT ( 'NONE',  ( 112.8039874620816789, -45.48581773443041953, 174.0384824187679556 ) ) ;
#63890 = CARTESIAN_POINT ( 'NONE',  ( 98.36549455146187881, -40.29075363668734155, 11.63562527591094309 ) ) ;
#63891 = EDGE_LOOP ( 'NONE', ( #35253, #82757 ) ) ;
#63892 = ORIENTED_EDGE ( 'NONE', *, *, #39900, .T. ) ;
#63894 = ORIENTED_EDGE ( 'NONE', *, *, #35992, .F. ) ;
#63893 = VECTOR ( 'NONE', #75907, 1000.000000000000000 ) ;
#63895 = ORIENTED_EDGE ( 'NONE', *, *, #53554, .F. ) ;
#63896 = CARTESIAN_POINT ( 'NONE',  ( 113.1782937733034089, -44.75186859099120085, 108.0939586094537646 ) ) ;
#63897 = CARTESIAN_POINT ( 'NONE',  ( 92.81551872686561921, -95.01002112898675023, -19.18411693322930134 ) ) ;
#63898 = CARTESIAN_POINT ( 'NONE',  ( 74.38348329127296665, -1.929447159941392931, 342.9256252759109884 ) ) ;
#63899 = CARTESIAN_POINT ( 'NONE',  ( 115.8262517397711946, -31.73143768449714130, 19.23974975539183063 ) ) ;
#63900 = CARTESIAN_POINT ( 'NONE',  ( 99.78216974382816318, 88.91243380484081626, 84.19383299529444287 ) ) ;
#63901 = DIRECTION ( 'NONE',  ( 1.000000000000000000, 4.163336342344333240E-14, 0.000000000000000000 ) ) ;
#63902 = CIRCLE ( 'NONE', #30560, 4.762500000000002842 ) ;
#63903 = CARTESIAN_POINT ( 'NONE',  ( 8.214917746879109858E-16, 60.82030000000000314, 272.1149787991095081 ) ) ;
#63904 = CARTESIAN_POINT ( 'NONE',  ( 210.2301280605339855, 25.81350000000000477, -7.937500000000000000 ) ) ;
#63905 = CARTESIAN_POINT ( 'NONE',  ( 98.44183741489689510, -42.05700530801252768, 11.76800622829193799 ) ) ;
#63906 = ORIENTED_EDGE ( 'NONE', *, *, #20963, .F. ) ;
#63907 = DIRECTION ( 'NONE',  ( 0.000000000000000000, 0.000000000000000000, -1.000000000000000000 ) ) ;
#63908 = PRESENTATION_LAYER_ASSIGNMENT (  '', '', ( #2820 ) ) ;
#63910 = EDGE_CURVE ( 'NONE', #22927, #79637, #8545, .T. ) ;
#63909 = CARTESIAN_POINT ( 'NONE',  ( 162.5667039024476708, -32.29483332968042930, 237.4678068554150059 ) ) ;
#63911 = CARTESIAN_POINT ( 'NONE',  ( 108.7800423072870046, -44.73859216708707720, 105.5623760838769698 ) ) ;
#63912 = ADVANCED_FACE ( 'NONE', ( #36699 ), #15366, .F. ) ;
#63913 = CARTESIAN_POINT ( 'NONE',  ( 107.0667039024467613, -18.72944715994092135, 196.8538068554170479 ) ) ;
#63914 = DIRECTION ( 'NONE',  ( 0.000000000000000000, 0.000000000000000000, -1.000000000000000000 ) ) ;
#63915 = ORIENTED_EDGE ( 'NONE', *, *, #1919, .F. ) ;
#63916 = ORIENTED_EDGE ( 'NONE', *, *, #49092, .F. ) ;
#63917 = CARTESIAN_POINT ( 'NONE',  ( 99.08983322626940549, -42.79586633336889179, 136.8435279569311263 ) ) ;
#63918 = VERTEX_POINT ( 'NONE', #36243 ) ;
#63919 = ORIENTED_EDGE ( 'NONE', *, *, #5030, .T. ) ;
#63920 = CARTESIAN_POINT ( 'NONE',  ( 98.99527800849182313, -31.91985561591122078, 127.3425356868499705 ) ) ;
#63921 = CARTESIAN_POINT ( 'NONE',  ( 133.5842039024480812, -51.22944715994092491, 207.5838068554170377 ) ) ;
#63922 = VECTOR ( 'NONE', #79894, 1000.000000000000000 ) ;
#63923 = CARTESIAN_POINT ( 'NONE',  ( 100.2845952792443569, -46.47769036989463132, 83.09276813305294240 ) ) ;
#63924 = CARTESIAN_POINT ( 'NONE',  ( 97.81169817874256012, -40.51742791483425776, 82.63555527327814332 ) ) ;
#63925 = ORIENTED_EDGE ( 'NONE', *, *, #78011, .T. ) ;
#63926 = EDGE_CURVE ( 'NONE', #63182, #53038, #14485, .T. ) ;
#63927 = ORIENTED_EDGE ( 'NONE', *, *, #58740, .F. ) ;
#63928 = ORIENTED_EDGE ( 'NONE', *, *, #83854, .T. ) ;
#63929 = CARTESIAN_POINT ( 'NONE',  ( 116.6952228212742995, -32.58508497927773817, 79.14991099019697174 ) ) ;
#63930 = ORIENTED_EDGE ( 'NONE', *, *, #40677, .T. ) ;
#63931 = CARTESIAN_POINT ( 'NONE',  ( 112.1067112481348858, -26.91823048478329738, 19.71086337114896736 ) ) ;
#63932 = CARTESIAN_POINT ( 'NONE',  ( 101.1884425732228436, -45.36575980889334403, 193.1013395616249682 ) ) ;
#63933 = FACE_OUTER_BOUND ( 'NONE', #68304, .T. ) ;
#63934 = CARTESIAN_POINT ( 'NONE',  ( 41.56648329127499153, -32.07844715994070839, 198.9256252759119832 ) ) ;
#63935 = CARTESIAN_POINT ( 'NONE',  ( 113.3313291481109815, -45.06216520097333955, 139.0899109901969553 ) ) ;
#63936 = CARTESIAN_POINT ( 'NONE',  ( -487.2989999999999782, 97.78694598552370110, 18.25625000000050235 ) ) ;
#63937 = VERTEX_POINT ( 'NONE', #64844 ) ;
#63938 = FACE_OUTER_BOUND ( 'NONE', #30298, .T. ) ;
#63939 = VECTOR ( 'NONE', #5442, 1000.000000000000000 ) ;
#63940 = CIRCLE ( 'NONE', #43819, 3.299999999999999822 ) ;
#63941 = ORIENTED_EDGE ( 'NONE', *, *, #13189, .F. ) ;
#63942 = CARTESIAN_POINT ( 'NONE',  ( 97.86658439798891607, -40.64924167897070362, 132.6473872692512259 ) ) ;
#63943 = EDGE_LOOP ( 'NONE', ( #31866, #28506, #23451, #33874 ) ) ;
#63944 = ORIENTED_EDGE ( 'NONE', *, *, #75335, .T. ) ;
#63945 = CIRCLE ( 'NONE', #7395, 8.928100000000000591 ) ;
#63946 = CARTESIAN_POINT ( 'NONE',  ( -3.175000000000109956, 124.5870000000000033, 31.75000000000000000 ) ) ;
#63947 = CARTESIAN_POINT ( 'NONE',  ( 3.258238535833978489, 94.72845588462597277, 118.5118799964233460 ) ) ;
#63948 = CARTESIAN_POINT ( 'NONE',  ( 111.1290374500119498, -47.00926920395730235, 22.88800622829195675 ) ) ;
#63949 = CARTESIAN_POINT ( 'NONE',  ( 13.26698260364423199, 68.06966155350374947, 35.72126630662602054 ) ) ;
#63950 = DIRECTION ( 'NONE',  ( 0.000000000000000000, 0.000000000000000000, -1.000000000000000000 ) ) ;
#63951 = CARTESIAN_POINT ( 'NONE',  ( 115.0372575091651015, -42.90846256308056184, 74.30229194293431760 ) ) ;
#63952 = CARTESIAN_POINT ( 'NONE',  ( 115.1412022171004850, -43.23618977845876543, 43.27467289495995573 ) ) ;
#63954 = CARTESIAN_POINT ( 'NONE',  ( 97.81366378802363215, -42.73395665195496917, 142.7965776568629508 ) ) ;
#63953 = DIRECTION ( 'NONE',  ( 0.000000000000000000, 0.000000000000000000, 1.000000000000000000 ) ) ;
#63955 = CARTESIAN_POINT ( 'NONE',  ( 97.07207205740387224, -35.37844121026580524, 72.21895861013597084 ) ) ;
#63956 = EDGE_CURVE ( 'NONE', #8973, #43788, #73926, .T. ) ;
#63957 = DIRECTION ( 'NONE',  ( 0.000000000000000000, 1.000000000000000000, 0.000000000000000000 ) ) ;
#63958 = ORIENTED_EDGE ( 'NONE', *, *, #30070, .F. ) ;
#63959 = CIRCLE ( 'NONE', #45060, 5.599999999999994316 ) ;
#63960 = DIRECTION ( 'NONE',  ( 1.000000000000000078E-15, 0.000000000000000000, 1.000000000000000000 ) ) ;
#63961 = CARTESIAN_POINT ( 'NONE',  ( 73.06648329127401098, -46.72944715994106701, 14.67562527591093513 ) ) ;
#63962 = DIRECTION ( 'NONE',  ( 0.7071067811864671926, 0.7071067811866279529, -2.899137802865059124E-29 ) ) ;
#63964 = VERTEX_POINT ( 'NONE', #83499 ) ;
#63963 = EDGE_CURVE ( 'NONE', #71994, #67598, #43931, .T. ) ;
#63965 = AXIS2_PLACEMENT_3D ( 'NONE', #46716, #48490, #69425 ) ;
#63966 = CARTESIAN_POINT ( 'NONE',  ( 182.5667039024469886, -33.35206098992650681, -5.074374724088000832 ) ) ;
#63968 = VERTEX_POINT ( 'NONE', #38907 ) ;
#63967 = CARTESIAN_POINT ( 'NONE',  ( 109.8678013061348508, -26.64186650728397865, 174.8613395616249591 ) ) ;
#63969 = PLANE ( 'NONE',  #78486 ) ;
#63970 = CARTESIAN_POINT ( 'NONE',  ( 113.2328747769256410, -45.16229216617723097, 224.0784824187679476 ) ) ;
#63971 = CARTESIAN_POINT ( 'NONE',  ( 115.2006710226633004, -43.31943727361606733, 84.28419670448195689 ) ) ;
#63972 = DIRECTION ( 'NONE',  ( 0.000000000000000000, 1.000000000000000000, 0.000000000000000000 ) ) ;
#63973 = DIRECTION ( 'NONE',  ( -1.000000000000000078E-15, 1.000000000000000083E-30, 1.000000000000000000 ) ) ;
#63974 = DIRECTION ( 'NONE',  ( 0.000000000000000000, 0.000000000000000000, -1.000000000000000000 ) ) ;
#63975 = EDGE_LOOP ( 'NONE', ( #3478, #6470, #79913 ) ) ;
#63976 = ORIENTED_EDGE ( 'NONE', *, *, #38423, .T. ) ;
#63978 = ORIENTED_EDGE ( 'NONE', *, *, #58690, .T. ) ;
#63977 = VECTOR ( 'NONE', #43692, 1000.000000000000000 ) ;
#63979 = EDGE_CURVE ( 'NONE', #60263, #71030, #79384, .T. ) ;
#63980 = VECTOR ( 'NONE', #45407, 1000.000000000000000 ) ;
#63981 = ORIENTED_EDGE ( 'NONE', *, *, #12120, .F. ) ;
#63982 = CARTESIAN_POINT ( 'NONE',  ( 91.91125933621933086, -96.68314769832139177, -21.78219314458224076 ) ) ;
#63983 = CARTESIAN_POINT ( 'NONE',  ( 104.4105741502040701, -26.00004237129247642, 236.2575300378159682 ) ) ;
#63984 = DIRECTION ( 'NONE',  ( -3.278217592397115468E-15, 0.000000000000000000, 1.000000000000000000 ) ) ;
#63985 = EDGE_CURVE ( 'NONE', #47787, #62972, #17328, .T. ) ;
#63986 = CARTESIAN_POINT ( 'NONE',  ( 135.7052281012230992, -16.51875982971419532, 2.060081176905330658 ) ) ;
#63987 = AXIS2_PLACEMENT_3D ( 'NONE', #32555, #33014, #81644 ) ;
#63989 = CARTESIAN_POINT ( 'NONE',  ( 74.36911441044604487, 82.54999999999999716, 92.32962665258637003 ) ) ;
#63988 = DIRECTION ( 'NONE',  ( -1.000000000000000000, -0.000000000000000000, -0.000000000000000000 ) ) ;
#63990 = LINE ( 'NONE', #30800, #63186 ) ;
#63991 = VECTOR ( 'NONE', #86044, 1000.000000000000000 ) ;
#63992 = CARTESIAN_POINT ( 'NONE',  ( 104.6437644399306635, -47.53804903515802494, 27.38895860924395009 ) ) ;
#63993 = EDGE_LOOP ( 'NONE', ( #9492, #35025, #55486, #56826, #31808, #81012, #23671, #68246, #70747, #38304, #64612, #24604, #42967, #26347 ) ) ;
#63994 = ORIENTED_EDGE ( 'NONE', *, *, #65049, .F. ) ;
#63995 = ORIENTED_EDGE ( 'NONE', *, *, #54500, .F. ) ;
#63996 = AXIS2_PLACEMENT_3D ( 'NONE', #26936, #49144, #76880 ) ;
#63997 = LINE ( 'NONE', #29472, #42727 ) ;
#63998 = CARTESIAN_POINT ( 'NONE',  ( 102.0679063313821899, -27.96999881512665098, 16.49307739911019510 ) ) ;
#63999 = CARTESIAN_POINT ( 'NONE',  ( 106.1957191385480854, -47.06291487533366080, 258.4975300378154088 ) ) ;
#64000 = DIRECTION ( 'NONE',  ( 0.7071067811865789920, -0.7071067811865159314, 0.000000000000000000 ) ) ;
#64001 = CARTESIAN_POINT ( 'NONE',  ( 113.5587197313313936, -28.64306037466259625, 115.5261014663869474 ) ) ;
#64002 = DIRECTION ( 'NONE',  ( -0.3600166455925385423, -9.815533969194669696E-15, -0.9329458799396118662 ) ) ;
#64004 = ORIENTED_EDGE ( 'NONE', *, *, #56517, .F. ) ;
#64003 = AXIS2_PLACEMENT_3D ( 'NONE', #41522, #21107, #34724 ) ;
#64005 = CARTESIAN_POINT ( 'NONE',  ( 83.06670390244806867, -58.72944715994108122, 231.5838068554169524 ) ) ;
#64006 = B_SPLINE_CURVE_WITH_KNOTS ( 'NONE', 3,
 ( #86252, #64467, #79454, #24034, #2250, #16321, #44447, #10392, #38534, #29954, #72178, #43998, #57638, #23158, #71734, #9503, #37210, #64911, #58091, #51704, #66229, #38097, #3573, #86701, #60308, #88044, #88937, #53479, #19438, #47571, #40770, #38981, #11736, #53931, #11276, #46223, #68039 ),
 .UNSPECIFIED., .F., .F.,
 ( 4, 2, 2, 2, 2, 2, 2, 2, 2, 2, 2, 2, 2, 2, 2, 1, 1, 1, 2, 4 ),
 ( 0.000000000000000000, 0.06251153962973163281, 0.1250230792594632656, 0.1875346188891948984, 0.2187903887040607287, 0.2500461585189265867, 0.2813019283337924170, 0.3125576981486583028, 0.3438134679635241886, 0.3750692377783900744, 0.4063250075932559047, 0.4375807774081217905, 0.4688365472229876763, 0.4844644321304208412, 0.4922783745841372016, 0.4961853458109952708, 0.4981388314244243887, 0.4991155742311390586, 0.4996039456344963936, 0.5000923170378537286 ),
 .UNSPECIFIED. ) ;
#64007 = CARTESIAN_POINT ( 'NONE',  ( 77.40501520703328708, -36.03131342368239132, 2.974074870387424241 ) ) ;
#64008 = ORIENTED_EDGE ( 'NONE', *, *, #70995, .T. ) ;
#64009 = VERTEX_POINT ( 'NONE', #46155 ) ;
#64010 = CARTESIAN_POINT ( 'NONE',  ( -84.41404664249371592, 95.23005795263748041, 83.24642779537488479 ) ) ;
#64011 = CARTESIAN_POINT ( 'NONE',  ( 114.7786440655094680, -32.32849264894101537, 285.6701547344685537 ) ) ;
#64012 = VECTOR ( 'NONE', #59255, 1000.000000000000000 ) ;
#64013 = DIRECTION ( 'NONE',  ( -1.000000000000000000, -4.299999999999999979E-14, -1.000000000000000078E-15 ) ) ;
#64014 = EDGE_CURVE ( 'NONE', #30738, #26931, #1383, .T. ) ;
#64015 = CYLINDRICAL_SURFACE ( 'NONE', #36011, 7.937500000000000000 ) ;
#64016 = AXIS2_PLACEMENT_3D ( 'NONE', #23411, #50634, #4619 ) ;
#64017 = LINE ( 'NONE', #17208, #37245 ) ;
#64018 = ORIENTED_EDGE ( 'NONE', *, *, #49263, .T. ) ;
#64019 = CYLINDRICAL_SURFACE ( 'NONE', #87134, 10.00000000000000888 ) ;
#64020 = PLANE ( 'NONE',  #29588 ) ;
#64021 = VERTEX_POINT ( 'NONE', #10755 ) ;
#64022 = CARTESIAN_POINT ( 'NONE',  ( 102.5580992528948912, -27.32936716964785262, 95.43276813305395478 ) ) ;
#64023 = EDGE_LOOP ( 'NONE', ( #14997, #64970, #75162 ) ) ;
#64025 = AXIS2_PLACEMENT_3D ( 'NONE', #22630, #57115, #29889 ) ;
#64024 = CARTESIAN_POINT ( 'NONE',  ( 106.3992821860680635, -28.18503700880033236, 24.56099125664901095 ) ) ;
#64026 = CARTESIAN_POINT ( 'NONE',  ( 1.387778780781445676E-14, 239.0000000000000000, 97.27542076772557778 ) ) ;
#64027 = CARTESIAN_POINT ( 'NONE',  ( 107.5349099188610893, -47.08895302312306086, 192.6003871806729535 ) ) ;
#64028 = CARTESIAN_POINT ( 'NONE',  ( -22.68723905695524934, 49.61528013047381336, 30.61088831204059701 ) ) ;
#64029 = CARTESIAN_POINT ( 'NONE',  ( 108.8673596973266058, 37.33800000000000097, 50.79999999999999716 ) ) ;
#64030 = CARTESIAN_POINT ( 'NONE',  ( 74.15067561874209900, 127.0000000000000000, 68.53801554307469246 ) ) ;
#64031 = CARTESIAN_POINT ( 'NONE',  ( 68.91040501423763942, -69.55594750570173801, 247.4992607834631997 ) ) ;
#64032 = CARTESIAN_POINT ( 'NONE',  ( 99.99465048579469340, -28.96254792738658779, 281.6641967044822650 ) ) ;
#64033 = CARTESIAN_POINT ( 'NONE',  ( 105.8119832718298028, -46.66943931204792051, 117.4785273639713239 ) ) ;
#64034 = EDGE_LOOP ( 'NONE', ( #26584, #13766, #19588, #60451 ) ) ;
#64035 = LINE ( 'NONE', #57193, #67642 ) ;
#64036 = ORIENTED_EDGE ( 'NONE', *, *, #24278, .F. ) ;
#64037 = CARTESIAN_POINT ( 'NONE',  ( 103.4533635841105479, -46.55483943026052174, 138.2956252759109645 ) ) ;
#64038 = ADVANCED_FACE ( 'NONE', ( #3503 ), #72558, .F. ) ;
#64039 = CYLINDRICAL_SURFACE ( 'NONE', #29425, 4.749999999999976907 ) ;
#64040 = ORIENTED_EDGE ( 'NONE', *, *, #89567, .F. ) ;
#64041 = EDGE_LOOP ( 'NONE', ( #42105, #24167 ) ) ;
#64042 = VERTEX_POINT ( 'NONE', #4408 ) ;
#64043 = AXIS2_PLACEMENT_3D ( 'NONE', #30898, #10014, #64087 ) ;
#64044 = CARTESIAN_POINT ( 'NONE',  ( 162.7866693523295680, -29.62846900981742237, 237.4678068554150059 ) ) ;
#64045 = CARTESIAN_POINT ( 'NONE',  ( 104.4899648130921008, -26.97880497593449078, 266.2814577675392798 ) ) ;
#64046 = CARTESIAN_POINT ( 'NONE',  ( 0.000000000000000000, 65.60000000000000853, 0.000000000000000000 ) ) ;
#64047 = FACE_BOUND ( 'NONE', #64238, .T. ) ;
#64048 = CARTESIAN_POINT ( 'NONE',  ( 124.7998166246059810, 12.92155284005730387, 355.9756252759109998 ) ) ;
#64049 = CARTESIAN_POINT ( 'NONE',  ( 111.0462345608747796, -47.04136251952688497, 13.85753003781498016 ) ) ;
#64050 = EDGE_CURVE ( 'NONE', #13441, #76709, #73884, .T. ) ;
#64051 = DIRECTION ( 'NONE',  ( 0.000000000000000000, 0.000000000000000000, 1.000000000000000000 ) ) ;
#64052 = ORIENTED_EDGE ( 'NONE', *, *, #23933, .F. ) ;
#64053 = CARTESIAN_POINT ( 'NONE',  ( 12.03224243969232354, 78.46476182159877055, 117.9439065551169108 ) ) ;
#64054 = EDGE_CURVE ( 'NONE', #23269, #31466, #11671, .T. ) ;
#64055 = CARTESIAN_POINT ( 'NONE',  ( 109.6430060329453937, -46.48008849646763707, 42.78103013062236215 ) ) ;
#64056 = AXIS2_PLACEMENT_3D ( 'NONE', #88213, #87744, #25514 ) ;
#64057 = ORIENTED_EDGE ( 'NONE', *, *, #2013, .F. ) ;
#64058 = VERTEX_POINT ( 'NONE', #44830 ) ;
#64059 = VECTOR ( 'NONE', #34420, 1000.000000000000000 ) ;
#64060 = CARTESIAN_POINT ( 'NONE',  ( 80.44338158421174967, -21.47944715994105636, 1.625625275910945078 ) ) ;
#64061 = CARTESIAN_POINT ( 'NONE',  ( 107.0667039024470313, -104.2784471599420897, -20.48315503890502143 ) ) ;
#64062 = DIRECTION ( 'NONE',  ( 1.000000000000000000, 0.000000000000000000, 1.986798540846734824E-16 ) ) ;
#64063 = EDGE_CURVE ( 'NONE', #84622, #68948, #5790, .T. ) ;
#64064 = FACE_BOUND ( 'NONE', #8286, .T. ) ;
#64065 = DIRECTION ( 'NONE',  ( -2.999999999999999839E-15, 1.000000000000000000, -2.999999999999999900E-30 ) ) ;
#64066 = CARTESIAN_POINT ( 'NONE',  ( 107.2162147037312678, -27.02129552338790575, 229.4867055423629836 ) ) ;
#64067 = CYLINDRICAL_SURFACE ( 'NONE', #17092, 4.750000000000004441 ) ;
#64068 = CARTESIAN_POINT ( 'NONE',  ( -7.195828152521259823E-13, 127.0000000000000000, 95.25000000000000000 ) ) ;
#64069 = CARTESIAN_POINT ( 'NONE',  ( 98.29927950267186532, -42.45157995928803984, 101.7870538473399620 ) ) ;
#64070 = ORIENTED_EDGE ( 'NONE', *, *, #85813, .T. ) ;
#64071 = CARTESIAN_POINT ( 'NONE',  ( 128.0667039024480118, -48.82844715994099971, 250.9178068554150514 ) ) ;
#64072 = ORIENTED_EDGE ( 'NONE', *, *, #38592, .F. ) ;
#64073 = CARTESIAN_POINT ( 'NONE',  ( -29.99999999999996092, 172.0000000000000000, 183.8826257785461280 ) ) ;
#64074 = CARTESIAN_POINT ( 'NONE',  ( 103.2777252079319652, -27.47497190407113266, 276.3856931979651108 ) ) ;
#64076 = ORIENTED_EDGE ( 'NONE', *, *, #6012, .T. ) ;
#64075 = EDGE_CURVE ( 'NONE', #83557, #55564, #82505, .T. ) ;
#64077 = VECTOR ( 'NONE', #84914, 1000.000000000000000 ) ;
#64078 = LINE ( 'NONE', #8215, #57796 ) ;
#64079 = EDGE_LOOP ( 'NONE', ( #78912, #40903, #89734, #74090 ) ) ;
#64080 = CARTESIAN_POINT ( 'NONE',  ( 60.32499999999999574, 82.54999999999999716, 358.0130000000000337 ) ) ;
#64081 = CARTESIAN_POINT ( 'NONE',  ( 184.5667039024483813, -48.82844715993448403, 249.9678068554149775 ) ) ;
#64082 = AXIS2_PLACEMENT_3D ( 'NONE', #26986, #54652, #82418 ) ;
#64083 = DIRECTION ( 'NONE',  ( 0.8660254037844392627, -0.4999999999999990008, 1.549999999999999706E-14 ) ) ;
#64084 = ORIENTED_EDGE ( 'NONE', *, *, #17708, .T. ) ;
#64085 = CARTESIAN_POINT ( 'NONE',  ( 98.62940354253828446, -43.90657238178356181, 76.89943479971999807 ) ) ;
#64086 = CARTESIAN_POINT ( 'NONE',  ( 0.000000000000000000, 125.7300000000000040, 0.000000000000000000 ) ) ;
#64087 = DIRECTION ( 'NONE',  ( 0.000000000000000000, 0.000000000000000000, -1.000000000000000000 ) ) ;
#64088 = DIRECTION ( 'NONE',  ( 0.000000000000000000, 0.000000000000000000, -1.000000000000000000 ) ) ;
#64089 = ORIENTED_EDGE ( 'NONE', *, *, #18113, .T. ) ;
#64090 = CIRCLE ( 'NONE', #35138, 7.937500000000000000 ) ;
#64091 = EDGE_CURVE ( 'NONE', #74091, #83131, #38029, .T. ) ;
#64092 = DIRECTION ( 'NONE',  ( 1.000000000000000078E-15, -1.000000000000000000, 0.000000000000000000 ) ) ;
#64093 = EDGE_CURVE ( 'NONE', #58666, #12205, #65721, .T. ) ;
#64094 = DIRECTION ( 'NONE',  ( 1.000000000000000078E-15, 0.000000000000000000, 1.000000000000000000 ) ) ;
#64095 = CIRCLE ( 'NONE', #81478, 4.762500000000002842 ) ;
#64096 = EDGE_CURVE ( 'NONE', #79585, #48818, #81022, .T. ) ;
#64097 = CARTESIAN_POINT ( 'NONE',  ( -72.96458098368600531, 117.4749999999999943, -72.96458098368781009 ) ) ;
#64098 = CARTESIAN_POINT ( 'NONE',  ( 109.5135917660753506, -46.88567278592853427, 128.7641967044819751 ) ) ;
#64099 = EDGE_CURVE ( 'NONE', #50121, #50189, #56332, .T. ) ;
#64101 = LINE ( 'NONE', #27773, #68820 ) ;
#64100 = LINE ( 'NONE', #965, #60940 ) ;
#64102 = CARTESIAN_POINT ( 'NONE',  ( 86.72755763596094880, -122.7870702624433221, 249.2178068554179902 ) ) ;
#64103 = EDGE_LOOP ( 'NONE', ( #37897, #24445, #84483, #42766 ) ) ;
#64104 = CARTESIAN_POINT ( 'NONE',  ( 143.0664832912740110, -18.82844715994099971, 323.8756252759120002 ) ) ;
#64105 = CARTESIAN_POINT ( 'NONE',  ( 116.8150918559699818, -40.26546416881831192, 169.5375300378149745 ) ) ;
#64107 = VERTEX_POINT ( 'NONE', #30330 ) ;
#64106 = CARTESIAN_POINT ( 'NONE',  ( 31.71315051185499811, -33.70561438052090608, -5.074374724088000832 ) ) ;
#64108 = AXIS2_PLACEMENT_3D ( 'NONE', #56589, #21651, #77053 ) ;
#64109 = CARTESIAN_POINT ( 'NONE',  ( 117.8598252335457488, -34.07367295057271406, 10.01848241876795953 ) ) ;
#64110 = PLANE ( 'NONE',  #15024 ) ;
#64111 = DIRECTION ( 'NONE',  ( 0.000000000000000000, 0.000000000000000000, 1.000000000000000000 ) ) ;
#64112 = DIRECTION ( 'NONE',  ( 0.000000000000000000, 0.000000000000000000, 1.000000000000000000 ) ) ;
#64113 = LINE ( 'NONE', #34598, #10849 ) ;
#64114 = CARTESIAN_POINT ( 'NONE',  ( 107.0664832912739968, -8.729447159940999512, 304.4006252759119775 ) ) ;
#64115 = CARTESIAN_POINT ( 'NONE',  ( 101.7545977962314225, -44.98157700518534341, 222.1213395616259731 ) ) ;
#64116 = ORIENTED_EDGE ( 'NONE', *, *, #75934, .F. ) ;
#64117 = VECTOR ( 'NONE', #56690, 1000.000000000000000 ) ;
#64118 = ORIENTED_EDGE ( 'NONE', *, *, #35019, .T. ) ;
#64119 = CARTESIAN_POINT ( 'NONE',  ( 97.58318307924886881, -33.33272491023742390, 172.4844404487539578 ) ) ;
#64120 = MECHANICAL_DESIGN_GEOMETRIC_PRESENTATION_REPRESENTATION (  '', ( #43804 ), #83002 ) ;
#64121 = DIRECTION ( 'NONE',  ( 0.000000000000000000, 0.000000000000000000, 1.000000000000000000 ) ) ;
#64122 = CARTESIAN_POINT ( 'NONE',  ( 104.1188366437555288, -45.08645965563772506, 53.73872616303998484 ) ) ;
#64123 = CARTESIAN_POINT ( 'NONE',  ( 23.44896873141045290, 85.70058346011398953, 299.3102295797750116 ) ) ;
#64124 = LINE ( 'NONE', #69593, #31528 ) ;
#64125 = DIRECTION ( 'NONE',  ( 1.000000000000000000, 3.999999999999999995E-14, 1.000000000000000078E-15 ) ) ;
#64126 = LINE ( 'NONE', #3678, #10168 ) ;
#64127 = DIRECTION ( 'NONE',  ( 4.299999999999999979E-14, -1.000000000000000000, 4.400000000000000367E-29 ) ) ;
#64128 = CARTESIAN_POINT ( 'NONE',  ( 118.0585799961421429, -32.36802338489820841, 249.1270538473389706 ) ) ;
#64129 = PLANE ( 'NONE',  #45977 ) ;
#64130 = ORIENTED_EDGE ( 'NONE', *, *, #88997, .F. ) ;
#64131 = ORIENTED_EDGE ( 'NONE', *, *, #66546, .F. ) ;
#64132 = CIRCLE ( 'NONE', #48147, 2.500000000000002220 ) ;
#64133 = CARTESIAN_POINT ( 'NONE',  ( -82.89895571708225930, 82.54999999999999716, -100.8594679592215471 ) ) ;
#64134 = CARTESIAN_POINT ( 'NONE',  ( -90.13147184857913885, 91.23868085022583330, -77.01901799881255783 ) ) ;
#64135 = CARTESIAN_POINT ( 'NONE',  ( 0.000000000000000000, 50.79999999999999716, 258.6990000000000123 ) ) ;
#64136 = LINE ( 'NONE', #57298, #66533 ) ;
#64137 = AXIS2_PLACEMENT_3D ( 'NONE', #20411, #40390, #5888 ) ;
#64138 = CARTESIAN_POINT ( 'NONE',  ( 104.8797383215544414, -46.86635653470245444, 28.41943479971997988 ) ) ;
#64139 = LINE ( 'NONE', #83692, #12210 ) ;
#64140 = VERTEX_POINT ( 'NONE', #24846 ) ;
#64141 = AXIS2_PLACEMENT_3D ( 'NONE', #27171, #70298, #13545 ) ;
#64142 = CARTESIAN_POINT ( 'NONE',  ( 103.5842829832543686, -46.60199803408937669, 53.30705384733997221 ) ) ;
#64143 = EDGE_CURVE ( 'NONE', #667, #38195, #65862, .T. ) ;
#64144 = CARTESIAN_POINT ( 'NONE',  ( 1.971923734479900239E-14, 11.98343896644750117, 160.4955849403809793 ) ) ;
#64145 = CARTESIAN_POINT ( 'NONE',  ( 100.2480723708022197, -28.84298388537911606, 260.6441967044822263 ) ) ;
#64146 = EDGE_CURVE ( 'NONE', #37208, #5947, #79583, .T. ) ;
#64147 = VERTEX_POINT ( 'NONE', #80717 ) ;
#64148 = VECTOR ( 'NONE', #3407, 1000.000000000000000 ) ;
#64149 = EDGE_CURVE ( 'NONE', #30549, #8470, #87523, .T. ) ;
#64150 = DIRECTION ( 'NONE',  ( 0.5000000000000015543, -0.8660254037844377084, 2.688821387764056676E-14 ) ) ;
#64151 = DIRECTION ( 'NONE',  ( 1.000000000000000000, 0.000000000000000000, -0.000000000000000000 ) ) ;
#64152 = DIRECTION ( 'NONE',  ( 0.000000000000000000, 0.000000000000000000, -1.000000000000000000 ) ) ;
#64153 = AXIS2_PLACEMENT_3D ( 'NONE', #5647, #61479, #54644 ) ;
#64154 = CARTESIAN_POINT ( 'NONE',  ( 115.5148531418241191, -38.60720430987922214, 101.4585665600679647 ) ) ;
#64155 = CARTESIAN_POINT ( 'NONE',  ( 117.4353638176713446, -35.45525114565609215, 189.9241967044829664 ) ) ;
#64156 = ADVANCED_FACE ( 'NONE', ( #18466 ), #51192, .T. ) ;
#64157 = CYLINDRICAL_SURFACE ( 'NONE', #55096, 37.00000000000000711 ) ;
#64158 = VERTEX_POINT ( 'NONE', #27083 ) ;
#64159 = EDGE_CURVE ( 'NONE', #50262, #46964, #37490, .T. ) ;
#64160 = DIRECTION ( 'NONE',  ( -0.000000000000000000, -1.000000000000000000, -0.000000000000000000 ) ) ;
#64161 = ORIENTED_EDGE ( 'NONE', *, *, #76090, .F. ) ;
#64162 = ORIENTED_EDGE ( 'NONE', *, *, #62402, .T. ) ;
#64163 = EDGE_CURVE ( 'NONE', #33465, #62792, #38960, .T. ) ;
#64164 = FACE_OUTER_BOUND ( 'NONE', #57780, .T. ) ;
#64165 = ORIENTED_EDGE ( 'NONE', *, *, #4379, .F. ) ;
#64166 = ORIENTED_EDGE ( 'NONE', *, *, #25891, .T. ) ;
#64167 = CARTESIAN_POINT ( 'NONE',  ( 141.8664832912729992, -1.929447159941394263, 352.4506252759079530 ) ) ;
#64168 = EDGE_CURVE ( 'NONE', #8177, #9584, #1247, .T. ) ;
#64169 = CARTESIAN_POINT ( 'NONE',  ( 105.7976002935269122, -26.72429596296039023, 25.17744450168613213 ) ) ;
#64170 = CARTESIAN_POINT ( 'NONE',  ( 99.28690145085043639, -32.09363259137744251, 130.3333722090289655 ) ) ;
#64171 = CARTESIAN_POINT ( 'NONE',  ( 109.9954698844069156, -26.70111721404902383, 259.8499109901965767 ) ) ;
#64172 = AXIS2_PLACEMENT_3D ( 'NONE', #53441, #12145, #45733 ) ;
#64173 = LINE ( 'NONE', #44142, #38312 ) ;
#64175 = ORIENTED_EDGE ( 'NONE', *, *, #22398, .F. ) ;
#64174 = EDGE_CURVE ( 'NONE', #16125, #24379, #25732, .T. ) ;
#64176 = ORIENTED_EDGE ( 'NONE', *, *, #81492, .F. ) ;
#64177 = DIRECTION ( 'NONE',  ( 1.000000000000000078E-15, -1.000000000000000000, 0.000000000000000000 ) ) ;
#64178 = DIRECTION ( 'NONE',  ( -0.7071067811865634489, 0.7071067811865315855, -7.071067811865330380E-16 ) ) ;
#64179 = CARTESIAN_POINT ( 'NONE',  ( 70.64051057348294194, -139.5687525891779899, 247.3260285211522103 ) ) ;
#64180 = CARTESIAN_POINT ( 'NONE',  ( 117.4149692539380681, -32.71426074976766074, 94.10895860924395606 ) ) ;
#64181 = LINE ( 'NONE', #2850, #72683 ) ;
#64182 = ORIENTED_EDGE ( 'NONE', *, *, #25382, .T. ) ;
#64183 = PRODUCT_DEFINITION_CONTEXT ( 'detailed design', #1124, 'design' ) ;
#64184 = CARTESIAN_POINT ( 'NONE',  ( 115.6954802162012044, -42.57986958318428350, 273.3527681330537575 ) ) ;
#64185 = DIRECTION ( 'NONE',  ( 5.512527431108029424E-15, -1.000000000000000000, 0.000000000000000000 ) ) ;
#64186 = CARTESIAN_POINT ( 'NONE',  ( 11.76728917727518464, 77.77273929673829400, 130.0246156895997274 ) ) ;
#64187 = DIRECTION ( 'NONE',  ( 1.000000000000000000, 0.000000000000000000, 0.000000000000000000 ) ) ;
#64189 = FACE_OUTER_BOUND ( 'NONE', #85670, .T. ) ;
#64188 = CARTESIAN_POINT ( 'NONE',  ( 131.3179999999999836, 37.33800000000000097, 42.86249999999999716 ) ) ;
#64190 = CARTESIAN_POINT ( 'NONE',  ( 41.56670390244801894, -27.57844715994070484, 342.9256252759119548 ) ) ;
#64191 = CARTESIAN_POINT ( 'NONE',  ( 48.16670390244654243, -28.27351298637380950, 193.9678068554150911 ) ) ;
#64192 = LINE ( 'NONE', #2412, #25216 ) ;
#64193 = CARTESIAN_POINT ( 'NONE',  ( -12.05184652617604435, 86.64091671906267322, 129.9989399000961328 ) ) ;
#64194 = CARTESIAN_POINT ( 'NONE',  ( 128.0667039024480118, -58.72944715994110254, 250.9178068554150514 ) ) ;
#64195 = FACE_OUTER_BOUND ( 'NONE', #57532, .T. ) ;
#64196 = VECTOR ( 'NONE', #41094, 1000.000000000000000 ) ;
#64197 = EDGE_CURVE ( 'NONE', #57650, #77070, #46606, .T. ) ;
#64199 = ORIENTED_EDGE ( 'NONE', *, *, #5379, .T. ) ;
#64198 = DIRECTION ( 'NONE',  ( 1.000000000000000078E-15, 0.000000000000000000, -1.000000000000000000 ) ) ;
#64200 = PLANE ( 'NONE',  #59701 ) ;
#64201 = CARTESIAN_POINT ( 'NONE',  ( 111.0013748985821422, -46.40740010236051916, 282.8841967044824628 ) ) ;
#64202 = CARTESIAN_POINT ( 'NONE',  ( 108.8488479242245290, -47.00104215551821341, 163.7127681330539701 ) ) ;
#64203 = CARTESIAN_POINT ( 'NONE',  ( 111.3320466151124322, -27.19308368994588676, 20.74133956162494030 ) ) ;
#64204 = EDGE_CURVE ( 'NONE', #43607, #10009, #20716, .T. ) ;
#64206 = CARTESIAN_POINT ( 'NONE',  ( 82.58878920444031735, -35.63370978841373926, 7.053538376720832836 ) ) ;
#64205 = PLANE ( 'NONE',  #74041 ) ;
#64207 = CARTESIAN_POINT ( 'NONE',  ( -465.6921742093539933, 60.32499999999999574, 3.174999999999999822 ) ) ;
#64208 = AXIS2_PLACEMENT_3D ( 'NONE', #34660, #68743, #13776 ) ;
#64209 = ORIENTED_EDGE ( 'NONE', *, *, #83917, .F. ) ;
#64210 = DIRECTION ( 'NONE',  ( -0.000000000000000000, 1.000000000000000000, -0.000000000000000000 ) ) ;
#64211 = EDGE_LOOP ( 'NONE', ( #48345, #30778 ) ) ;
#64212 = AXIS2_PLACEMENT_3D ( 'NONE', #63286, #27412, #1062 ) ;
#64213 = CARTESIAN_POINT ( 'NONE',  ( 112.4079628628857250, -28.49644221148697198, 65.61848241876694487 ) ) ;
#64215 = VERTEX_POINT ( 'NONE', #32989 ) ;
#64214 = CARTESIAN_POINT ( 'NONE',  ( 107.0664832912750057, -36.72944715993903486, 0.4256252759109709349 ) ) ;
#64216 = DIRECTION ( 'NONE',  ( 0.000000000000000000, -1.000000000000000000, 0.000000000000000000 ) ) ;
#64217 = CARTESIAN_POINT ( 'NONE',  ( 112.1942863616535817, -45.78120396183486918, 208.9870538473389558 ) ) ;
#64218 = CARTESIAN_POINT ( 'NONE',  ( 196.2150000000000034, 43.68799999999999528, 44.45000000000000284 ) ) ;
#64219 = CARTESIAN_POINT ( 'NONE',  ( 109.6427860908511036, -46.48014371229046304, 147.7814644202007059 ) ) ;
#64220 = LINE ( 'NONE', #42403, #35610 ) ;
#64221 = CARTESIAN_POINT ( 'NONE',  ( 101.0090012246669886, -28.74596344506981538, 86.59355491815287564 ) ) ;
#64222 = CARTESIAN_POINT ( 'NONE',  ( 164.7812970173232543, -35.65087443489315433, 237.4678068554150059 ) ) ;
#64223 = CARTESIAN_POINT ( 'NONE',  ( 110.8531357376099891, -45.98478418387610844, 97.88551033190712758 ) ) ;
#64224 = CARTESIAN_POINT ( 'NONE',  ( 103.4440497394145808, -45.85039829771051245, 117.2756252759109543 ) ) ;
#64225 = ORIENTED_EDGE ( 'NONE', *, *, #81656, .F. ) ;
#64226 = VERTEX_POINT ( 'NONE', #88425 ) ;
#64227 = CARTESIAN_POINT ( 'NONE',  ( 101.9660762386545514, -28.83879614530413704, 66.97682140113498406 ) ) ;
#64228 = CARTESIAN_POINT ( 'NONE',  ( 132.1035770464692405, -115.7792181415380099, 250.2178068554179902 ) ) ;
#64230 = DIRECTION ( 'NONE',  ( -0.000000000000000000, -0.000000000000000000, -1.000000000000000000 ) ) ;
#64229 = CARTESIAN_POINT ( 'NONE',  ( 112.7271506738795779, -45.41826929060054852, 219.0480062282919960 ) ) ;
#64231 = CARTESIAN_POINT ( 'NONE',  ( 85.72499999999999432, 66.67499999999999716, 346.0750000000000455 ) ) ;
#64232 = CARTESIAN_POINT ( 'NONE',  ( 113.2454969875984290, -28.75867143562818740, 110.5525043974795381 ) ) ;
#64233 = CARTESIAN_POINT ( 'NONE',  ( 106.5667039024470455, -113.7784471599420613, -19.78219314458171141 ) ) ;
#64234 = VECTOR ( 'NONE', #83318, 1000.000000000000000 ) ;
#64235 = LINE ( 'NONE', #9268, #31877 ) ;
#64236 = CARTESIAN_POINT ( 'NONE',  ( 12.51814237086690262, 80.89737214551436750, 117.8933722897785685 ) ) ;
#64237 = CARTESIAN_POINT ( 'NONE',  ( 116.7861719071672866, -43.46560779248406448, 163.3441967044829823 ) ) ;
#64238 = EDGE_LOOP ( 'NONE', ( #15696, #67537 ) ) ;
#64239 = ORIENTED_EDGE ( 'NONE', *, *, #44765, .F. ) ;
#64240 = EDGE_LOOP ( 'NONE', ( #50155, #75382, #59387, #36371 ) ) ;
#64241 = CARTESIAN_POINT ( 'NONE',  ( 21.03715912545744615, -47.82818131006197149, 129.9678068554150627 ) ) ;
#64242 = CARTESIAN_POINT ( 'NONE',  ( -100.3414980266874039, 87.03008507238371294, -83.52531662946658741 ) ) ;
#64243 = CARTESIAN_POINT ( 'NONE',  ( 98.34937724553353178, -31.65743187412461168, 130.9065372364317454 ) ) ;
#64244 = CARTESIAN_POINT ( 'NONE',  ( 99.08943691707119683, -42.79534522775045957, 102.8439055007673915 ) ) ;
#64245 = CARTESIAN_POINT ( 'NONE',  ( 101.3402310731127329, -30.91225182618282830, 223.5138046553059894 ) ) ;
#64246 = EDGE_CURVE ( 'NONE', #18963, #27831, #44924, .T. ) ;
#64247 = CIRCLE ( 'NONE', #48255, 2.749999999999974687 ) ;
#64248 = DIRECTION ( 'NONE',  ( 5.512527431108029424E-15, -1.000000000000000000, 0.000000000000000000 ) ) ;
#64249 = EDGE_CURVE ( 'NONE', #34414, #35902, #68864, .T. ) ;
#64250 = CARTESIAN_POINT ( 'NONE',  ( 100.8863770005861795, -45.89136241369948976, 152.0918157521009562 ) ) ;
#64251 = EDGE_CURVE ( 'NONE', #64543, #66869, #38190, .T. ) ;
#64252 = DIRECTION ( 'NONE',  ( 1.000000000000000000, 0.000000000000000000, 0.000000000000000000 ) ) ;
#64253 = EDGE_LOOP ( 'NONE', ( #58484, #68018, #11136 ) ) ;
#64255 = VERTEX_POINT ( 'NONE', #18920 ) ;
#64254 = ORIENTED_EDGE ( 'NONE', *, *, #80019, .T. ) ;
#64256 = EDGE_CURVE ( 'NONE', #16018, #20410, #43302, .T. ) ;
#64257 = CARTESIAN_POINT ( 'NONE',  ( 29.56670390244784485, -48.82844715994099971, 180.4678068554150911 ) ) ;
#64258 = EDGE_LOOP ( 'NONE', ( #1501, #6987 ) ) ;
#64259 = ORIENTED_EDGE ( 'NONE', *, *, #9737, .T. ) ;
#64260 = PLANE ( 'NONE',  #31834 ) ;
#64261 = CARTESIAN_POINT ( 'NONE',  ( 52.65249034007825912, -48.32844715994060181, 300.4678068554150059 ) ) ;
#64262 = CARTESIAN_POINT ( 'NONE',  ( 102.7933444172945769, -44.96577155458380304, 15.01380465530593966 ) ) ;
#64263 = ADVANCED_FACE ( 'NONE', ( #4849 ), #53407, .F. ) ;
#64264 = CARTESIAN_POINT ( 'NONE',  ( 117.0608944987687750, -38.08045336284195059, 273.7189585899762960 ) ) ;
#64265 = VERTEX_POINT ( 'NONE', #6636 ) ;
#64266 = CARTESIAN_POINT ( 'NONE',  ( 115.1001406608323947, -41.05364652694197503, 9.635625275910943088 ) ) ;
#64267 = LINE ( 'NONE', #50620, #6757 ) ;
#64268 = VERTEX_POINT ( 'NONE', #20279 ) ;
#64269 = ORIENTED_EDGE ( 'NONE', *, *, #56985, .F. ) ;
#64270 = EDGE_CURVE ( 'NONE', #3353, #47865, #47944, .T. ) ;
#64271 = CARTESIAN_POINT ( 'NONE',  ( 99.50493083782342296, -43.30601922071209486, 111.8960934546087884 ) ) ;
#64272 = ORIENTED_EDGE ( 'NONE', *, *, #69619, .T. ) ;
#64273 = EDGE_LOOP ( 'NONE', ( #25346, #33654, #51522, #28445 ) ) ;
#64274 = CIRCLE ( 'NONE', #71544, 5.599999999999994316 ) ;
#64275 = B_SPLINE_CURVE_WITH_KNOTS ( 'NONE', 3,
 ( #68010, #39404, #68465, #88469, #26223, #5795, #61187, #88914, #26668, #82112, #19866, #75281, #13057, #6239, #33930, #73930, #11709, #27124, #75726, #13497, #54802, #41184, #67109, #4891, #7585 ),
 .UNSPECIFIED., .F., .F.,
 ( 4, 2, 1, 2, 2, 2, 2, 2, 2, 2, 2, 2, 4 ),
 ( 0.5000912566136184179, 0.5039967936713244390, 0.5079023307290305711, 0.5157134048444427243, 0.5313355530752669198, 0.5625798495369156438, 0.6250684424602134248, 0.6875570353835112059, 0.7500456283068088759, 0.8125342212301067679, 0.8750228141534044379, 0.9375114070767023300, 1.000000000000000000 ),
 .UNSPECIFIED. ) ;
#64276 = ADVANCED_FACE ( 'NONE', ( #41140, #34332 ), #27523, .F. ) ;
#64277 = VECTOR ( 'NONE', #76541, 1000.000000000000114 ) ;
#64278 = CARTESIAN_POINT ( 'NONE',  ( 101.7271154311333135, -43.54062005560803073, 274.8776141791153691 ) ) ;
#64279 = CARTESIAN_POINT ( 'NONE',  ( 102.6741928909662391, -27.25030431863982372, 180.4213395616249898 ) ) ;
#64280 = CARTESIAN_POINT ( 'NONE',  ( 113.0643619202157879, -28.22920495858469891, 129.5870538473399449 ) ) ;
#64281 = PLANE ( 'NONE',  #9469 ) ;
#64282 = LINE ( 'NONE', #15234, #26371 ) ;
#64283 = CARTESIAN_POINT ( 'NONE',  ( 115.4598468997141509, -29.53740796227222987, 225.4022919425769658 ) ) ;
#64284 = CARTESIAN_POINT ( 'NONE',  ( 112.0660770571772105, -45.48830407390881447, 98.99134466148210265 ) ) ;
#64285 = CARTESIAN_POINT ( 'NONE',  ( 76.16940679758155852, -115.1634909102945841, 249.3055308415380011 ) ) ;
#64286 = ORIENTED_EDGE ( 'NONE', *, *, #26500, .T. ) ;
#64287 = LINE ( 'NONE', #36123, #65612 ) ;
#64288 = ORIENTED_EDGE ( 'NONE', *, *, #72506, .T. ) ;
#64289 = EDGE_CURVE ( 'NONE', #15997, #17885, #49067, .T. ) ;
#64290 = ORIENTED_EDGE ( 'NONE', *, *, #87127, .T. ) ;
#64291 = CARTESIAN_POINT ( 'NONE',  ( 96.14524839136181811, -32.00129468986670389, 211.0013395616249738 ) ) ;
#64292 = VERTEX_POINT ( 'NONE', #42927 ) ;
#64293 = SHAPE_REPRESENTATION ( 'Feed Lead', ( #50656 ), #27505 ) ;
#64294 = CARTESIAN_POINT ( 'NONE',  ( 95.31140346374353101, -38.27925045402978554, 151.4299109901969871 ) ) ;
#64295 = DIRECTION ( 'NONE',  ( -0.7071067811856560636, -0.7071067811874389708, 0.000000000000000000 ) ) ;
#64296 = VECTOR ( 'NONE', #67414, 1000.000000000000000 ) ;
#64297 = DIRECTION ( 'NONE',  ( 0.000000000000000000, 1.000000000000000000, 0.000000000000000000 ) ) ;
#64298 = PLANE ( 'NONE',  #32561 ) ;
#64301 = CARTESIAN_POINT ( 'NONE',  ( 109.9541224118590321, -48.19721710984605068, 238.7727681330539724 ) ) ;
#64300 = CARTESIAN_POINT ( 'NONE',  ( -41.60202597009397607, 53.97499999999997300, 50.85338361873603219 ) ) ;
#64299 = FACE_OUTER_BOUND ( 'NONE', #40887, .T. ) ;
#64302 = CARTESIAN_POINT ( 'NONE',  ( 194.5667039024485803, -47.82844715993405060, 129.9678068554150343 ) ) ;
#64303 = DIRECTION ( 'NONE',  ( -1.000000000000000078E-15, 1.000000000000000000, -3.100000000000000044E-14 ) ) ;
#64304 = CARTESIAN_POINT ( 'NONE',  ( 98.34910283431625544, -31.65794092288234296, 271.9061491226904081 ) ) ;
#64305 = TOROIDAL_SURFACE ( 'NONE', #1985, 13.50000000000000000, 0.5000000000000000000 ) ;
#64306 = PLANE ( 'NONE',  #89234 ) ;
#64307 = CARTESIAN_POINT ( 'NONE',  ( 113.2454986932114309, -28.75867294076968861, 255.5522919430740387 ) ) ;
#64308 = CARTESIAN_POINT ( 'NONE',  ( 145.3728389244185450, -136.8603515927981107, 247.4879652615099985 ) ) ;
#64310 = EDGE_LOOP ( 'NONE', ( #33640, #69179, #17665, #28920, #17196, #71429 ) ) ;
#64309 = CARTESIAN_POINT ( 'NONE',  ( 113.4887626673159673, -41.81888551505019080, 195.5838068554168103 ) ) ;
#64311 = DIRECTION ( 'NONE',  ( -1.000000000000000000, 0.000000000000000000, -2.108231265501709878E-16 ) ) ;
#64312 = CARTESIAN_POINT ( 'NONE',  ( 117.0383059485392607, -33.61350157978694142, 174.0670538473389399 ) ) ;
#64313 = CARTESIAN_POINT ( 'NONE',  ( 113.4595210239597520, -46.70760751678911049, 64.02991099019695298 ) ) ;
#64314 = CARTESIAN_POINT ( 'NONE',  ( 116.3890555338844450, -44.12544333927958462, 194.2927681330539542 ) ) ;
#64315 = LINE ( 'NONE', #85663, #32935 ) ;
#64316 = EDGE_CURVE ( 'NONE', #47689, #5461, #60675, .T. ) ;
#64317 = CYLINDRICAL_SURFACE ( 'NONE', #66367, 1.000000000000000888 ) ;
#64319 = LINE ( 'NONE', #83874, #26932 ) ;
#64318 = CARTESIAN_POINT ( 'NONE',  ( 162.7866693523280048, -29.62846900982320264, -5.074374724088000832 ) ) ;
#64320 = DIRECTION ( 'NONE',  ( 1.000000000000000078E-15, 0.000000000000000000, 1.000000000000000000 ) ) ;
#64321 = DIRECTION ( 'NONE',  ( 0.000000000000000000, 0.000000000000000000, -1.000000000000000000 ) ) ;
#64322 = ORIENTED_EDGE ( 'NONE', *, *, #69248, .F. ) ;
#64323 = AXIS2_PLACEMENT_3D ( 'NONE', #13533, #33960, #61224 ) ;
#64324 = DIRECTION ( 'NONE',  ( 0.000000000000000000, 0.000000000000000000, -1.000000000000000000 ) ) ;
#64325 = ORIENTED_EDGE ( 'NONE', *, *, #54056, .F. ) ;
#64326 = ORIENTED_EDGE ( 'NONE', *, *, #80577, .F. ) ;
#64328 = ORIENTED_EDGE ( 'NONE', *, *, #41619, .T. ) ;
#64327 = DIRECTION ( 'NONE',  ( 2.108231265501709878E-16, 5.463695987328529395E-16, -1.000000000000000000 ) ) ;
#64329 = CARTESIAN_POINT ( 'NONE',  ( 109.6783822832554591, -47.44587409406599221, 83.75467289495897205 ) ) ;
#64330 = CARTESIAN_POINT ( 'NONE',  ( -454.6936515812919879, 53.97500000000000142, 3.174999999999999822 ) ) ;
#64331 = FACE_OUTER_BOUND ( 'NONE', #23126, .T. ) ;
#64332 = ADVANCED_FACE ( 'NONE', ( #57466 ), #7980, .T. ) ;
#64333 = CARTESIAN_POINT ( 'NONE',  ( 97.07207206336831007, -35.37844116818202878, 177.2189586067734979 ) ) ;
#64334 = CARTESIAN_POINT ( 'NONE',  ( 97.32756240343553600, -42.09278592120095652, 26.72705384733997747 ) ) ;
#64335 = ORIENTED_EDGE ( 'NONE', *, *, #361, .T. ) ;
#64336 = VERTEX_POINT ( 'NONE', #50648 ) ;
#64337 = EDGE_LOOP ( 'NONE', ( #83115, #34148, #74994, #65019 ) ) ;
#64339 = EDGE_CURVE ( 'NONE', #810, #64226, #85207, .T. ) ;
#64338 = VECTOR ( 'NONE', #80282, 1000.000000000000000 ) ;
#64340 = CARTESIAN_POINT ( 'NONE',  ( 70.98999999999998067, 52.73749999999999716, -44.45000000000002416 ) ) ;
#64341 = DIRECTION ( 'NONE',  ( 4.299999999999999979E-14, -1.000000000000000000, 0.000000000000000000 ) ) ;
#64343 = VECTOR ( 'NONE', #28632, 1000.000000000000000 ) ;
#64342 = DIRECTION ( 'NONE',  ( 0.0001211784769825749762, -0.7071067708032375831, -0.7071067811865434649 ) ) ;
#64344 = PLANE ( 'NONE',  #13647 ) ;
#64345 = CARTESIAN_POINT ( 'NONE',  ( 86.19814306825382744, 92.12504059357189590, 98.05663017059126219 ) ) ;
#64346 = CARTESIAN_POINT ( 'NONE',  ( 21.03689327557613709, -23.42844715994197813, 193.9678068554150627 ) ) ;
#64347 = DIRECTION ( 'NONE',  ( 0.000000000000000000, 0.000000000000000000, -1.000000000000000000 ) ) ;
#64348 = DIRECTION ( 'NONE',  ( 0.000000000000000000, 0.000000000000000000, -1.000000000000000000 ) ) ;
#64349 = CARTESIAN_POINT ( 'NONE',  ( 111.1204619107249982, -46.98756979655009047, 22.88800622829195675 ) ) ;
#64350 = ORIENTED_EDGE ( 'NONE', *, *, #47403, .F. ) ;
#64351 = CARTESIAN_POINT ( 'NONE',  ( 105.7995190932148404, -26.72403489713727964, 270.1772918944074604 ) ) ;
#64352 = DIRECTION ( 'NONE',  ( -0.000000000000000000, -0.000000000000000000, -1.000000000000000000 ) ) ;
#64353 = CARTESIAN_POINT ( 'NONE',  ( 114.7830339860594364, -33.98399025413122843, 111.9166617981629486 ) ) ;
#64354 = VECTOR ( 'NONE', #301, 1000.000000000000000 ) ;
#64355 = EDGE_CURVE ( 'NONE', #56606, #18423, #43379, .T. ) ;
#64356 = CARTESIAN_POINT ( 'NONE',  ( 97.31319625472109180, -38.96114016031690852, 96.50548233485649519 ) ) ;
#64357 = ADVANCED_FACE ( 'NONE', ( #76579, #64299 ), #21627, .T. ) ;
#64358 = CYLINDRICAL_SURFACE ( 'NONE', #63367, 0.9999999999999940048 ) ;
#64359 = ORIENTED_EDGE ( 'NONE', *, *, #2526, .F. ) ;
#64360 = VERTEX_POINT ( 'NONE', #41582 ) ;
#64361 = CARTESIAN_POINT ( 'NONE',  ( 104.4082270698484223, -46.45812771010326259, 137.3629473761069448 ) ) ;
#64362 = AXIS2_PLACEMENT_3D ( 'NONE', #12609, #40298, #49795 ) ;
#64363 = EDGE_CURVE ( 'NONE', #13968, #64372, #69316, .T. ) ;
#64364 = VERTEX_POINT ( 'NONE', #71121 ) ;
#64365 = ORIENTED_EDGE ( 'NONE', *, *, #65376, .T. ) ;
#64366 = CARTESIAN_POINT ( 'NONE',  ( 99.08321105494920289, -40.57595765811257138, 168.1158690201829700 ) ) ;
#64367 = ADVANCED_FACE ( 'NONE', ( #56102 ), #7090, .F. ) ;
#64368 = FACE_OUTER_BOUND ( 'NONE', #83571, .T. ) ;
#64369 = CARTESIAN_POINT ( 'NONE',  ( 96.01268936646508223, -41.06948063400285776, 92.62419670448296927 ) ) ;
#64370 = CIRCLE ( 'NONE', #33880, 4.750000000000000888 ) ;
#64371 = CARTESIAN_POINT ( 'NONE',  ( 110.8540151137909930, -45.98442434552481473, 17.88558598347468731 ) ) ;
#64372 = VERTEX_POINT ( 'NONE', #15704 ) ;
#64373 = ORIENTED_EDGE ( 'NONE', *, *, #79929, .F. ) ;
#64374 = ORIENTED_EDGE ( 'NONE', *, *, #7102, .T. ) ;
#64375 = EDGE_CURVE ( 'NONE', #54166, #61695, #269, .T. ) ;
#64376 = CARTESIAN_POINT ( 'NONE',  ( 109.2506105747909828, -28.86437792779224409, 172.6795189410199498 ) ) ;
#64377 = CARTESIAN_POINT ( 'NONE',  ( 117.9477513149503523, -41.48675964724572651, 58.49848241876792798 ) ) ;
#64378 = ORIENTED_EDGE ( 'NONE', *, *, #54099, .T. ) ;
#64379 = CARTESIAN_POINT ( 'NONE',  ( 112.9508454419806043, -28.15023113465287352, 44.59848241876795782 ) ) ;
#64380 = CARTESIAN_POINT ( 'NONE',  ( 102.0405519839503086, -46.59986864225058412, 168.2137205140059564 ) ) ;
#64381 = DIRECTION ( 'NONE',  ( 1.000000000000000000, 0.000000000000000000, 0.000000000000000000 ) ) ;
#64382 = LINE ( 'NONE', #36680, #38704 ) ;
#64383 = CARTESIAN_POINT ( 'NONE',  ( 117.2221417514105610, -42.83659189374058940, 124.3956252759109731 ) ) ;
#64384 = DIRECTION ( 'NONE',  ( -3.100000000000000258E-29, 3.100000000000000044E-14, 1.000000000000000000 ) ) ;
#64385 = ORIENTED_EDGE ( 'NONE', *, *, #44010, .F. ) ;
#64386 = FACE_BOUND ( 'NONE', #27438, .T. ) ;
#64387 = ORIENTED_EDGE ( 'NONE', *, *, #54472, .T. ) ;
#64388 = LINE ( 'NONE', #14904, #18642 ) ;
#64389 = VERTEX_POINT ( 'NONE', #27966 ) ;
#64390 = VERTEX_POINT ( 'NONE', #14360 ) ;
#64391 = AXIS2_PLACEMENT_3D ( 'NONE', #55095, #14250, #75583 ) ;
#64392 = FACE_OUTER_BOUND ( 'NONE', #75314, .T. ) ;
#64393 = CARTESIAN_POINT ( 'NONE',  ( 10.91394734298260794, 88.85994971916933594, 118.0527383321748118 ) ) ;
#64394 = CARTESIAN_POINT ( 'NONE',  ( 96.68578154376476164, -42.44622222083611263, 26.72705384733997747 ) ) ;
#64395 = CARTESIAN_POINT ( 'NONE',  ( 22.90570976208508824, 57.39977848847996000, 30.44578217438603218 ) ) ;
#64396 = VECTOR ( 'NONE', #42797, 1000.000000000000000 ) ;
#64397 = DIRECTION ( 'NONE',  ( 0.000000000000000000, 0.000000000000000000, -1.000000000000000000 ) ) ;
#64398 = DIRECTION ( 'NONE',  ( 1.000000000000000078E-15, -1.000000000000000000, 0.000000000000000000 ) ) ;
#64399 = CARTESIAN_POINT ( 'NONE',  ( 110.2470682213182869, -46.59973918892936240, 57.83657765686300678 ) ) ;
#64401 = CARTESIAN_POINT ( 'NONE',  ( 116.6407469026008243, -40.79910830432089597, 164.5070538473399608 ) ) ;
#64400 = CARTESIAN_POINT ( 'NONE',  ( 170.2205283966864897, 101.5999999999999943, -79.24800000000000466 ) ) ;
#64402 = CARTESIAN_POINT ( 'NONE',  ( 97.80969231062213964, -40.51824920587227297, 266.6357212253427633 ) ) ;
#64403 = FACE_OUTER_BOUND ( 'NONE', #40407, .T. ) ;
#64404 = ORIENTED_EDGE ( 'NONE', *, *, #55853, .F. ) ;
#64405 = DIRECTION ( 'NONE',  ( 0.000000000000000000, 1.000000000000000000, 0.000000000000000000 ) ) ;
#64406 = CARTESIAN_POINT ( 'NONE',  ( -3.175000000000120171, 124.5870000000000033, 33.98325472291460159 ) ) ;
#64407 = ORIENTED_EDGE ( 'NONE', *, *, #10019, .T. ) ;
#64408 = DIRECTION ( 'NONE',  ( 0.000000000000000000, 0.000000000000000000, 1.000000000000000000 ) ) ;
#64410 = ORIENTED_EDGE ( 'NONE', *, *, #89515, .F. ) ;
#64409 = CARTESIAN_POINT ( 'NONE',  ( 116.7015053437751959, -40.82493444377960401, 168.5070538473399608 ) ) ;
#64411 = CARTESIAN_POINT ( 'NONE',  ( 60.32499999999999574, 82.54999999999999716, 344.4418053999999643 ) ) ;
#64412 = CARTESIAN_POINT ( 'NONE',  ( 97.59563580048326514, -41.13856347273024738, 252.6727681330536655 ) ) ;
#64413 = CARTESIAN_POINT ( 'NONE',  ( 108.5441076757828398, -26.36558658937538269, 100.9641967044829727 ) ) ;
#64414 = FACE_OUTER_BOUND ( 'NONE', #6044, .T. ) ;
#64415 = ADVANCED_FACE ( 'NONE', ( #29332 ), #55644, .F. ) ;
#64416 = CARTESIAN_POINT ( 'NONE',  ( 102.0655984279635504, -27.97135235995153835, 191.4897250454755238 ) ) ;
#64417 = CARTESIAN_POINT ( 'NONE',  ( -187.8075999999999794, 101.5999999999999943, -3.174999999999999822 ) ) ;
#64418 = VERTEX_POINT ( 'NONE', #69765 ) ;
#64419 = CIRCLE ( 'NONE', #81799, 0.9999999999999731326 ) ;
#64420 = VECTOR ( 'NONE', #22160, 1000.000000000000000 ) ;
#64421 = EDGE_CURVE ( 'NONE', #75590, #65492, #89761, .T. ) ;
#64422 = CIRCLE ( 'NONE', #76011, 10.00000000000000178 ) ;
#64423 = ORIENTED_EDGE ( 'NONE', *, *, #31953, .F. ) ;
#64424 = VERTEX_POINT ( 'NONE', #77472 ) ;
#64425 = AXIS2_PLACEMENT_3D ( 'NONE', #11097, #71567, #38803 ) ;
#64426 = VERTEX_POINT ( 'NONE', #711 ) ;
#64427 = DIRECTION ( 'NONE',  ( 0.000000000000000000, -1.000000000000000000, 0.000000000000000000 ) ) ;
#64428 = CARTESIAN_POINT ( 'NONE',  ( 115.2517161551258766, -30.21613035964762517, 240.3613395616249875 ) ) ;
#64429 = DIRECTION ( 'NONE',  ( 0.000000000000000000, 0.000000000000000000, -1.000000000000000000 ) ) ;
#64430 = DIRECTION ( 'NONE',  ( 1.986798540846734824E-16, 0.000000000000000000, -1.000000000000000000 ) ) ;
#64432 = DIRECTION ( 'NONE',  ( 1.000000000000000000, 4.299999999999999979E-14, 1.000000000000000078E-15 ) ) ;
#64431 = LINE ( 'NONE', #86667, #51121 ) ;
#64433 = FACE_OUTER_BOUND ( 'NONE', #35152, .T. ) ;
#64434 = CARTESIAN_POINT ( 'NONE',  ( 96.15435578470099642, -38.63231720721949358, 46.45181575210094138 ) ) ;
#64435 = VERTEX_POINT ( 'NONE', #36136 ) ;
#64436 = ORIENTED_EDGE ( 'NONE', *, *, #30825, .T. ) ;
#64437 = ORIENTED_EDGE ( 'NONE', *, *, #74129, .T. ) ;
#64438 = EDGE_CURVE ( 'NONE', #51309, #8809, #49300, .T. ) ;
#64439 = DIRECTION ( 'NONE',  ( 0.7071067811865774377, -0.7071067811865175967, 7.071067811865470403E-16 ) ) ;
#64440 = CARTESIAN_POINT ( 'NONE',  ( 0.000000000000000000, 101.5999999999999943, 0.000000000000000000 ) ) ;
#64441 = B_SPLINE_CURVE_WITH_KNOTS ( 'NONE', 3,
 ( #25534, #38713, #3759, #66417, #10130, #37838, #60491, #23775, #24645, #65537, #32796, #79632, #79192, #87772, #31011, #53209, #58703, #86445 ),
 .UNSPECIFIED., .F., .F.,
 ( 4, 2, 2, 2, 2, 2, 2, 2, 4 ),
 ( 0.5000000021306179043, 0.5625000018642907218, 0.6250000015979634282, 0.6875000013316361347, 0.7500000010653089522, 0.8125000007989817696, 0.8750000005326544761, 0.9375000002663271825, 1.000000000000000000 ),
 .UNSPECIFIED. ) ;
#64442 = CARTESIAN_POINT ( 'NONE',  ( 115.5794671477453761, -31.87256924526127477, 285.2384824187676600 ) ) ;
#64443 = DIRECTION ( 'NONE',  ( 0.7071067811865453523, 0.7071067811865496822, 7.071067811865460542E-16 ) ) ;
#64444 = CARTESIAN_POINT ( 'NONE',  ( 98.20106483660288177, -31.34956418181673854, 121.8803871806729546 ) ) ;
#64445 = CARTESIAN_POINT ( 'NONE',  ( 99.04397839509049106, -42.84113223740011733, 26.84394684677412002 ) ) ;
#64446 = VERTEX_POINT ( 'NONE', #84311 ) ;
#64447 = CARTESIAN_POINT ( 'NONE',  ( 78.00648098368650096, 117.4749999999999943, 72.96458098368729850 ) ) ;
#64448 = CARTESIAN_POINT ( 'NONE',  ( 78.57311110803117060, -34.41810224487900172, 1.981704920704651762 ) ) ;
#64449 = VERTEX_POINT ( 'NONE', #22082 ) ;
#64450 = CARTESIAN_POINT ( 'NONE',  ( -89.13001032377158594, 92.64969027323469675, 78.17826422383558338 ) ) ;
#64451 = CARTESIAN_POINT ( 'NONE',  ( 105.6993345102559942, -28.68213381844667609, 13.02809036959096112 ) ) ;
#64452 = AXIS2_PLACEMENT_3D ( 'NONE', #58585, #86320, #24097 ) ;
#64453 = DIRECTION ( 'NONE',  ( 1.000000000000000078E-15, 1.000000000000000083E-30, -1.000000000000000000 ) ) ;
#64454 = AXIS2_PLACEMENT_3D ( 'NONE', #74454, #17705, #3620 ) ;
#64455 = PLANE ( 'NONE',  #37446 ) ;
#64456 = EDGE_CURVE ( 'NONE', #41571, #53161, #49747, .T. ) ;
#64457 = LINE ( 'NONE', #44889, #57594 ) ;
#64458 = ORIENTED_EDGE ( 'NONE', *, *, #45674, .F. ) ;
#64459 = CARTESIAN_POINT ( 'NONE',  ( 59.56670390244700997, -79.67844715994098692, 190.2178068554179902 ) ) ;
#64460 = DIRECTION ( 'NONE',  ( -0.7071067811865274777, 0.7071067811865675568, -7.071067811865283048E-16 ) ) ;
#64461 = EDGE_CURVE ( 'NONE', #66495, #48789, #44729, .T. ) ;
#64462 = VERTEX_POINT ( 'NONE', #17038 ) ;
#64463 = CARTESIAN_POINT ( 'NONE',  ( 97.26623355869948284, -31.61728591124570542, 90.93181575210196854 ) ) ;
#64464 = EDGE_LOOP ( 'NONE', ( #89530, #29746, #67185, #62755 ) ) ;
#64465 = EDGE_CURVE ( 'NONE', #893, #628, #3403, .T. ) ;
#64466 = CARTESIAN_POINT ( 'NONE',  ( 111.7162562550164608, -28.95820004563618610, 54.08194363760093637 ) ) ;
#64467 = CARTESIAN_POINT ( 'NONE',  ( 116.5614777235394399, -33.52755762741292500, 90.08470898062006427 ) ) ;
#64468 = CARTESIAN_POINT ( 'NONE',  ( 106.9806506443342755, -46.50983917909375265, 187.5699109901969734 ) ) ;
#64469 = CARTESIAN_POINT ( 'NONE',  ( -23.20326867387899128, 52.20473367193696390, 30.22006327746032284 ) ) ;
#64470 = EDGE_CURVE ( 'NONE', #9022, #83591, #86533, .T. ) ;
#64471 = B_SPLINE_CURVE_WITH_KNOTS ( 'NONE', 3,
 ( #65119, #42977, #72827, #70717, #10593, #42533, #4232, #86912, #51905, #80107, #63445, #38297, #10158, #25116, #38742, #44659, #86474, #65996, #77530, #9712, #3788, #28934, #37416, #56620, #31475, #2903 ),
 .UNSPECIFIED., .F., .F.,
 ( 4, 2, 2, 2, 2, 2, 2, 2, 2, 2, 2, 2, 4 ),
 ( 0.01987185114512061979, 0.02111326483159428266, 0.02235467851806794207, 0.02483750589101525741, 0.02607891957748890294, 0.02732033326396255193, 0.02980316063690985340, 0.03228598800985715833, 0.03352740169633080386, 0.03476881538280444939, 0.03725164275575171269, 0.03849305644222534434, 0.03973447012869897599 ),
 .UNSPECIFIED. ) ;
#64472 = LINE ( 'NONE', #51259, #53113 ) ;
#64473 = DIRECTION ( 'NONE',  ( -0.7071067708032326982, -0.0001211784769776692866, -0.7071067811865484609 ) ) ;
#64474 = CARTESIAN_POINT ( 'NONE',  ( 96.72029611048706954, -35.13276604965626859, 262.2041967044821149 ) ) ;
#64475 = VERTEX_POINT ( 'NONE', #30221 ) ;
#64476 = CARTESIAN_POINT ( 'NONE',  ( -28.99999999999997513, 172.0000000000000000, 183.8826257785461280 ) ) ;
#64477 = ORIENTED_EDGE ( 'NONE', *, *, #45725, .F. ) ;
#64478 = CARTESIAN_POINT ( 'NONE',  ( 114.5432832596865325, -29.39626808186021378, 145.4441967044819819 ) ) ;
#64479 = LINE ( 'NONE', #84503, #75842 ) ;
#64480 = AXIS2_PLACEMENT_3D ( 'NONE', #79186, #26437, #74141 ) ;
#64481 = CIRCLE ( 'NONE', #9371, 2.029999999999997140 ) ;
#64482 = AXIS2_PLACEMENT_3D ( 'NONE', #14810, #15703, #8438 ) ;
#64483 = ORIENTED_EDGE ( 'NONE', *, *, #51306, .T. ) ;
#64484 = ORIENTED_EDGE ( 'NONE', *, *, #35960, .T. ) ;
#64485 = ORIENTED_EDGE ( 'NONE', *, *, #68038, .T. ) ;
#64486 = ADVANCED_FACE ( 'NONE', ( #31094 ), #72006, .F. ) ;
#64487 = CONICAL_SURFACE ( 'NONE', #64425, 1.624999999999987566, 1.029744258676650093 ) ;
#64488 = CARTESIAN_POINT ( 'NONE',  ( 72.96458098368650269, 117.4749999999999943, 72.96458098368729850 ) ) ;
#64489 = VECTOR ( 'NONE', #51451, 1000.000000000000000 ) ;
#64490 = CARTESIAN_POINT ( 'NONE',  ( 151.0371591254584871, -46.82818131005582529, 180.4678068554149775 ) ) ;
#64491 = CARTESIAN_POINT ( 'NONE',  ( 108.1128363339379632, -46.45408497333518483, 202.6613395616259652 ) ) ;
#64493 = EDGE_CURVE ( 'NONE', #72226, #84886, #68157, .T. ) ;
#64492 = CARTESIAN_POINT ( 'NONE',  ( 107.0664832912739968, -36.72944715994100306, 287.6356252759109680 ) ) ;
#64494 = CARTESIAN_POINT ( 'NONE',  ( 144.1872586526515647, -138.0587248278176844, 247.6570847665630026 ) ) ;
#64495 = CARTESIAN_POINT ( 'NONE',  ( 134.0664832912740110, -8.350947159940998787, 293.6356252759119911 ) ) ;
#64496 = CARTESIAN_POINT ( 'NONE',  ( 100.5976686157419806, -28.50914727160554207, 11.60705384733995515 ) ) ;
#64497 = FACE_BOUND ( 'NONE', #45400, .T. ) ;
#64498 = VERTEX_POINT ( 'NONE', #38802 ) ;
#64499 = SURFACE_STYLE_FILL_AREA ( #23624 ) ;
#64500 = CARTESIAN_POINT ( 'NONE',  ( 116.8171211726486405, -34.15291134256264627, 44.03120960089060532 ) ) ;
#64501 = ORIENTED_EDGE ( 'NONE', *, *, #13261, .T. ) ;
#64502 = EDGE_LOOP ( 'NONE', ( #31374, #36661 ) ) ;
#64503 = DIRECTION ( 'NONE',  ( 0.000000000000000000, 0.000000000000000000, -1.000000000000000000 ) ) ;
#64504 = DIRECTION ( 'NONE',  ( -0.000000000000000000, 1.000000000000000000, 0.000000000000000000 ) ) ;
#64505 = CARTESIAN_POINT ( 'NONE',  ( 116.3308458273176456, -44.07926308385601999, 198.2927681330539542 ) ) ;
#64506 = CARTESIAN_POINT ( 'NONE',  ( 172.5664832912740110, -18.82844715994099971, 138.9256252759119832 ) ) ;
#64507 = LINE ( 'NONE', #22736, #59356 ) ;
#64508 = CARTESIAN_POINT ( 'NONE',  ( 41.56648329127381203, -18.82844715994071194, 261.9256252759119548 ) ) ;
#64509 = CARTESIAN_POINT ( 'NONE',  ( 99.57203460073428403, -40.82693060065560076, 221.1467055423629517 ) ) ;
#64511 = CARTESIAN_POINT ( 'NONE',  ( 104.4960957391109559, -46.84663716100901354, 43.37848241876896083 ) ) ;
#64510 = CARTESIAN_POINT ( 'NONE',  ( -69.72411017813060141, 120.6499999999999915, 69.72411017812929401 ) ) ;
#64512 = CARTESIAN_POINT ( 'NONE',  ( 172.5664832912740110, -36.32844715994070839, 18.92562527591200094 ) ) ;
#64513 = CARTESIAN_POINT ( 'NONE',  ( 117.9212005353621322, -39.05065313503074975, 108.6708633711489824 ) ) ;
#64514 = ORIENTED_EDGE ( 'NONE', *, *, #11965, .T. ) ;
#64515 = CARTESIAN_POINT ( 'NONE',  ( 131.3780189692435556, -19.30949827215296821, 6.839365140900929951 ) ) ;
#64516 = ORIENTED_EDGE ( 'NONE', *, *, #15058, .F. ) ;
#64517 = CARTESIAN_POINT ( 'NONE',  ( 63.56670390244800473, -40.82844715994016127, 249.9678068554150343 ) ) ;
#64518 = B_SPLINE_CURVE_WITH_KNOTS ( 'NONE', 3,
 ( #1064, #21975, #29226, #36490, #85097, #42822, #64193, #70559, #8331, #76924, #1967, #7429, #15601, #35119, #607, #71465, #43728, #28304, #70103, #36030, #55996, #10456, #49189, #42374, #56912, #22867 ),
 .UNSPECIFIED., .F., .F.,
 ( 4, 2, 2, 2, 2, 2, 2, 2, 2, 2, 2, 2, 4 ),
 ( 0.01986933033599076748, 0.02111058882927465200, 0.02235184732255853651, 0.02483436430912634718, 0.02607562280241026986, 0.02731688129569419254, 0.02979939828226201015, 0.03228191526882982776, 0.03352317376211373656, 0.03476443225539763843, 0.03724694924196543522, 0.03848820773524934402, 0.03972946622853323895 ),
 .UNSPECIFIED. ) ;
#64519 = CARTESIAN_POINT ( 'NONE',  ( 102.0645642710494769, -27.97192201181788462, 276.4899936502032460 ) ) ;
#64520 = ORIENTED_EDGE ( 'NONE', *, *, #53357, .F. ) ;
#64521 = DIRECTION ( 'NONE',  ( 0.000000000000000000, 1.000000000000000000, 0.000000000000000000 ) ) ;
#64522 = ORIENTED_EDGE ( 'NONE', *, *, #81098, .F. ) ;
#64523 = CARTESIAN_POINT ( 'NONE',  ( 99.08946256649485917, -109.4614598618343138, -19.78219314458184996 ) ) ;
#64524 = CARTESIAN_POINT ( 'NONE',  ( 37.03715912545347777, -48.62818131006128652, 129.9678068554150911 ) ) ;
#64525 = EDGE_CURVE ( 'NONE', #34621, #31568, #52835, .T. ) ;
#64526 = PRESENTATION_LAYER_ASSIGNMENT (  '', '', ( #25336 ) ) ;
#64527 = CARTESIAN_POINT ( 'NONE',  ( -28.99999999999999289, 127.0000000000000000, 113.8826257785461280 ) ) ;
#64528 = ORIENTED_EDGE ( 'NONE', *, *, #52590, .F. ) ;
#64529 = CARTESIAN_POINT ( 'NONE',  ( 96.61701384456422659, -37.56428313387978335, 101.3899109901969524 ) ) ;
#64530 = CIRCLE ( 'NONE', #4993, 7.999999999999992895 ) ;
#64532 = EDGE_CURVE ( 'NONE', #55038, #36478, #40585, .T. ) ;
#64531 = CARTESIAN_POINT ( 'NONE',  ( 97.81051247419222250, -40.51455135576280497, 166.6353777005785446 ) ) ;
#64533 = CARTESIAN_POINT ( 'NONE',  ( 52.06670390244700286, -77.67844715994100113, 55.21780685541800437 ) ) ;
#64534 = LINE ( 'NONE', #2316, #74621 ) ;
#64535 = ORIENTED_EDGE ( 'NONE', *, *, #89281, .F. ) ;
#64536 = LINE ( 'NONE', #8230, #70703 ) ;
#64537 = CARTESIAN_POINT ( 'NONE',  ( 112.1393456662218568, -28.01282279633491967, 154.6564586069755762 ) ) ;
#64538 = CARTESIAN_POINT ( 'NONE',  ( 51.06670390244768498, -32.29483332968566600, 237.4678068554150059 ) ) ;
#64540 = FACE_OUTER_BOUND ( 'NONE', #50643, .T. ) ;
#64539 = DIRECTION ( 'NONE',  ( 0.000000000000000000, 0.000000000000000000, -1.000000000000000000 ) ) ;
#64541 = CARTESIAN_POINT ( 'NONE',  ( 107.0664832912739399, -36.72944715994095333, 311.6356252759109680 ) ) ;
#64542 = VECTOR ( 'NONE', #23710, 1000.000000000000114 ) ;
#64543 = VERTEX_POINT ( 'NONE', #78829 ) ;
#64544 = ADVANCED_FACE ( 'NONE', ( #65179 ), #72447, .T. ) ;
#64545 = CIRCLE ( 'NONE', #55810, 12.99999999999999822 ) ;
#64546 = AXIS2_PLACEMENT_3D ( 'NONE', #36181, #757, #29376 ) ;
#64547 = CIRCLE ( 'NONE', #9428, 17.00000000000090239 ) ;
#64548 = FACE_OUTER_BOUND ( 'NONE', #63255, .T. ) ;
#64549 = CARTESIAN_POINT ( 'NONE',  ( 116.4020974974655047, -33.81230083437814216, 170.0670538473389684 ) ) ;
#64551 = ORIENTED_EDGE ( 'NONE', *, *, #56255, .T. ) ;
#64550 = CARTESIAN_POINT ( 'NONE',  ( 172.5664832912729878, -27.82844715994070484, 258.9256252759120116 ) ) ;
#64552 = AXIS2_PLACEMENT_3D ( 'NONE', #76465, #42817, #7871 ) ;
#64553 = CARTESIAN_POINT ( 'NONE',  ( 98.95751068421678553, -41.73716824282166016, 7.768006228290936122 ) ) ;
#64554 = DIRECTION ( 'NONE',  ( 1.000000000000000078E-15, -1.000000000000000000, 0.000000000000000000 ) ) ;
#64555 = DIRECTION ( 'NONE',  ( -1.000000000000000078E-15, 1.000000000000000083E-30, 1.000000000000000000 ) ) ;
#64556 = CARTESIAN_POINT ( 'NONE',  ( 143.5667039024469886, -67.87844715994090450, 96.96780685541800437 ) ) ;
#64557 = EDGE_CURVE ( 'NONE', #65511, #22487, #23425, .T. ) ;
#64558 = DIRECTION ( 'NONE',  ( -1.000000000000000078E-15, 1.000000000000000000, 0.000000000000000000 ) ) ;
#64559 = CARTESIAN_POINT ( 'NONE',  ( 99.40370404213540212, -29.74227323812493751, 230.7261014663879735 ) ) ;
#64560 = VERTEX_POINT ( 'NONE', #37030 ) ;
#64561 = ORIENTED_EDGE ( 'NONE', *, *, #8218, .F. ) ;
#64562 = AXIS2_PLACEMENT_3D ( 'NONE', #71920, #86885, #64648 ) ;
#64563 = CARTESIAN_POINT ( 'NONE',  ( 115.6778139412940192, -34.63821234579798158, 205.4472975916109476 ) ) ;
#64564 = DIRECTION ( 'NONE',  ( 0.7071067708032339194, 0.0001211784769776690833, -0.7071067811865472397 ) ) ;
#64565 = CARTESIAN_POINT ( 'NONE',  ( 102.0302726170450711, -29.40150668315268234, 46.98729759161196284 ) ) ;
#64566 = CARTESIAN_POINT ( 'NONE',  ( 23.62187231118733521, 84.66434562521884288, 307.1737385415713675 ) ) ;
#64567 = FACE_OUTER_BOUND ( 'NONE', #61409, .T. ) ;
#64568 = DIRECTION ( 'NONE',  ( 0.000000000000000000, 1.000000000000000000, 0.000000000000000000 ) ) ;
#64569 = ORIENTED_EDGE ( 'NONE', *, *, #35732, .F. ) ;
#64570 = CARTESIAN_POINT ( 'NONE',  ( 182.0667039024479550, -33.35206098992058799, 117.4678068554150627 ) ) ;
#64571 = CARTESIAN_POINT ( 'NONE',  ( 97.81169266289590780, -40.51741659614882707, 92.63571255866972365 ) ) ;
#64572 = CARTESIAN_POINT ( 'NONE',  ( 105.6350724880777392, -47.03380199863529754, 257.4670538473393435 ) ) ;
#64573 = CARTESIAN_POINT ( 'NONE',  ( 72.96458098368701428, 127.0000000000000000, -72.96458098368670164 ) ) ;
#64574 = EDGE_LOOP ( 'NONE', ( #73868, #21295, #32293, #30671 ) ) ;
#64576 = VERTEX_POINT ( 'NONE', #71566 ) ;
#64575 = EDGE_CURVE ( 'NONE', #32749, #49587, #23856, .T. ) ;
#64577 = DIRECTION ( 'NONE',  ( 0.1811243268507065352, -0.9834602067307444129, 0.000000000000000000 ) ) ;
#64578 = CARTESIAN_POINT ( 'NONE',  ( 32.06670390244800473, -32.29483332968611364, 342.9256252759119548 ) ) ;
#64579 = DIRECTION ( 'NONE',  ( 1.000000000000000000, 0.000000000000000000, -6.982966722218760189E-15 ) ) ;
#64580 = CARTESIAN_POINT ( 'NONE',  ( 72.24325998657057823, -9.906223855237664466, 14.92562527591093691 ) ) ;
#64582 = CARTESIAN_POINT ( 'NONE',  ( 111.8051046833288353, -27.50533224649500497, 15.71086337114796549 ) ) ;
#64581 = VECTOR ( 'NONE', #12779, 1000.000000000000000 ) ;
#64583 = CARTESIAN_POINT ( 'NONE',  ( 8.621919111718908013, 73.35264728006647772, 118.0418996292485190 ) ) ;
#64584 = ORIENTED_EDGE ( 'NONE', *, *, #46555, .F. ) ;
#64585 = CARTESIAN_POINT ( 'NONE',  ( 104.4799455178094405, -46.91020534057368963, 43.37848241876896083 ) ) ;
#64586 = CARTESIAN_POINT ( 'NONE',  ( 0.000000000000000000, 184.0000000000000000, 90.32146847885337593 ) ) ;
#64587 = AXIS2_PLACEMENT_3D ( 'NONE', #52842, #87420, #9779 ) ;
#64588 = CARTESIAN_POINT ( 'NONE',  ( 101.5973605122076862, -47.27098594307553725, 17.19562527591095247 ) ) ;
#64589 = ORIENTED_EDGE ( 'NONE', *, *, #79850, .T. ) ;
#64590 = EDGE_CURVE ( 'NONE', #83417, #8508, #52399, .T. ) ;
#64591 = CARTESIAN_POINT ( 'NONE',  ( 77.31652006362757845, -36.90534128960240423, 6.749824347015199066 ) ) ;
#64593 = ADVANCED_FACE ( 'NONE', ( #87412 ), #10215, .T. ) ;
#64592 = CARTESIAN_POINT ( 'NONE',  ( 98.38045758784420514, -41.69533782386550769, 17.73958850095263884 ) ) ;
#64594 = LINE ( 'NONE', #2375, #48005 ) ;
#64595 = CARTESIAN_POINT ( 'NONE',  ( 106.2913146648166531, -45.97580021205838818, 110.3280903695919903 ) ) ;
#64596 = CARTESIAN_POINT ( 'NONE',  ( 98.53347975398118308, -44.98838784992466344, 187.9384824187679612 ) ) ;
#64597 = DIRECTION ( 'NONE',  ( 0.000000000000000000, 0.000000000000000000, 1.000000000000000000 ) ) ;
#64598 = ORIENTED_EDGE ( 'NONE', *, *, #79148, .F. ) ;
#64599 = DIRECTION ( 'NONE',  ( 1.000000000000000000, -5.337610695313248426E-16, 0.000000000000000000 ) ) ;
#64600 = ORIENTED_EDGE ( 'NONE', *, *, #16895, .T. ) ;
#64601 = ORIENTED_EDGE ( 'NONE', *, *, #43130, .F. ) ;
#64602 = VECTOR ( 'NONE', #36056, 1000.000000000000000 ) ;
#64603 = DIRECTION ( 'NONE',  ( -0.1858654557293184517, 0.9825752044329902901, 0.000000000000000000 ) ) ;
#64604 = ORIENTED_EDGE ( 'NONE', *, *, #71720, .T. ) ;
#64605 = ORIENTED_EDGE ( 'NONE', *, *, #22626, .F. ) ;
#64606 = DIRECTION ( 'NONE',  ( 1.000000000000000078E-15, -1.000000000000000000, 0.000000000000000000 ) ) ;
#64607 = DIRECTION ( 'NONE',  ( 0.000000000000000000, 0.000000000000000000, 1.000000000000000000 ) ) ;
#64608 = CARTESIAN_POINT ( 'NONE',  ( 113.3792027166817320, -43.22269317268541755, 117.6248007804579458 ) ) ;
#64609 = CARTESIAN_POINT ( 'NONE',  ( 112.6756251843347627, -45.54329372032184153, 263.0270538473394026 ) ) ;
#64610 = CARTESIAN_POINT ( 'NONE',  ( 1.475953350320055108E-14, 238.8000000000000114, 90.07542076772557493 ) ) ;
#64611 = ORIENTED_EDGE ( 'NONE', *, *, #18787, .T. ) ;
#64612 = ORIENTED_EDGE ( 'NONE', *, *, #66512, .F. ) ;
#64613 = DIRECTION ( 'NONE',  ( -1.000000000000000000, 0.000000000000000000, 0.000000000000000000 ) ) ;
#64614 = LINE ( 'NONE', #7855, #42007 ) ;
#64615 = CARTESIAN_POINT ( 'NONE',  ( 107.0664832912739257, -49.89611382660765315, 311.6356252759109680 ) ) ;
#64616 = VECTOR ( 'NONE', #24113, 1000.000000000000000 ) ;
#64617 = CARTESIAN_POINT ( 'NONE',  ( 63.06670390244699576, -67.87844715994098976, 85.21780685541799016 ) ) ;
#64618 = ORIENTED_EDGE ( 'NONE', *, *, #26341, .F. ) ;
#64619 = CARTESIAN_POINT ( 'NONE',  ( 101.2938852305094173, -26.37968400006201719, 255.4813395616251626 ) ) ;
#64620 = CARTESIAN_POINT ( 'NONE',  ( 97.06107111146356203, -37.99641208148336347, 36.42729195195173020 ) ) ;
#64621 = PLANE ( 'NONE',  #9725 ) ;
#64622 = VECTOR ( 'NONE', #16052, 1000.000000000000000 ) ;
#64625 = EDGE_CURVE ( 'NONE', #89932, #19776, #40459, .T. ) ;
#64624 = CARTESIAN_POINT ( 'NONE',  ( 68.91268721346291670, -139.0876414149588527, 246.7345552620604678 ) ) ;
#64623 = LINE ( 'NONE', #31429, #50638 ) ;
#64626 = FACE_OUTER_BOUND ( 'NONE', #49522, .T. ) ;
#64627 = LINE ( 'NONE', #3743, #87417 ) ;
#64628 = DIRECTION ( 'NONE',  ( 0.000000000000000000, 1.000000000000000000, 0.000000000000000000 ) ) ;
#64629 = CARTESIAN_POINT ( 'NONE',  ( 99.09570904781570277, -30.55043178906333523, 11.80229194609280441 ) ) ;
#64630 = DIRECTION ( 'NONE',  ( -1.000000000000000078E-15, 1.000000000000000000, 0.000000000000000000 ) ) ;
#64631 = CARTESIAN_POINT ( 'NONE',  ( 180.2143765759489895, -35.91149509761070391, -5.074374724088000832 ) ) ;
#64632 = DIRECTION ( 'NONE',  ( 1.000000000000000000, 1.314511288311335947E-16, 0.000000000000000000 ) ) ;
#64633 = CARTESIAN_POINT ( 'NONE',  ( 111.4898014013570560, -26.57429697695857129, 284.7375300378155316 ) ) ;
#64634 = CARTESIAN_POINT ( 'NONE',  ( 114.9650091533680722, -29.92534717146685708, 180.3927681330539770 ) ) ;
#64635 = CARTESIAN_POINT ( 'NONE',  ( 117.5340331363998985, -37.28601590683526723, 14.78419670448294454 ) ) ;
#64637 = DIRECTION ( 'NONE',  ( 0.000000000000000000, 0.000000000000000000, -1.000000000000000000 ) ) ;
#64636 = DIRECTION ( 'NONE',  ( 4.299999999999999979E-14, -1.000000000000000000, 0.000000000000000000 ) ) ;
#64638 = CARTESIAN_POINT ( 'NONE',  ( 83.06670390244796920, -58.35344715994099829, 231.5838068554150198 ) ) ;
#64639 = CIRCLE ( 'NONE', #52988, 14.50000000000001243 ) ;
#64640 = EDGE_CURVE ( 'NONE', #64576, #51214, #31540, .T. ) ;
#64641 = AXIS2_PLACEMENT_3D ( 'NONE', #68318, #6098, #69210 ) ;
#64642 = EDGE_LOOP ( 'NONE', ( #16761, #34385, #39562, #81545 ) ) ;
#64643 = EDGE_CURVE ( 'NONE', #83823, #30447, #17912, .T. ) ;
#64644 = DIRECTION ( 'NONE',  ( -3.100000000000000258E-29, 3.100000000000000044E-14, 1.000000000000000000 ) ) ;
#64645 = ORIENTED_EDGE ( 'NONE', *, *, #15049, .F. ) ;
#64646 = CARTESIAN_POINT ( 'NONE',  ( 103.8130989789263765, -45.95327097697893493, 53.30705384733897034 ) ) ;
#64647 = EDGE_CURVE ( 'NONE', #63602, #58568, #70631, .T. ) ;
#64649 = ORIENTED_EDGE ( 'NONE', *, *, #63341, .F. ) ;
#64648 = DIRECTION ( 'NONE',  ( -0.7071067811865476838, -0.7071067811865473507, 0.000000000000000000 ) ) ;
#64650 = DIRECTION ( 'NONE',  ( 0.000000000000000000, 0.000000000000000000, 1.000000000000000000 ) ) ;
#64651 = CARTESIAN_POINT ( 'NONE',  ( 95.43233898611183008, -38.84956357215551037, 197.4699109901969791 ) ) ;
#64652 = CARTESIAN_POINT ( 'NONE',  ( 161.4809174648185603, -48.32844715993547169, 180.4678068554150059 ) ) ;
#64653 = CARTESIAN_POINT ( 'NONE',  ( 110.8600349841776307, -45.98195914306448628, 147.8861036193170264 ) ) ;
#64654 = DIRECTION ( 'NONE',  ( 0.000000000000000000, 0.000000000000000000, -1.000000000000000000 ) ) ;
#64655 = CARTESIAN_POINT ( 'NONE',  ( 107.0664832912750057, -36.72944715993903486, 0.7256252759109708128 ) ) ;
#64656 = EDGE_CURVE ( 'NONE', #42067, #81257, #1518, .T. ) ;
#64657 = EDGE_CURVE ( 'NONE', #45431, #10945, #77361, .T. ) ;
#64658 = DIRECTION ( 'NONE',  ( 0.3818493186865919986, -0.9242245927363031965, 0.000000000000000000 ) ) ;
#64659 = CARTESIAN_POINT ( 'NONE',  ( 100.8867824969240559, -44.69965576686789888, 97.05229191759698892 ) ) ;
#64660 = CARTESIAN_POINT ( 'NONE',  ( 112.9441315310009628, -44.54716313336201949, 143.0899109901969553 ) ) ;
#64661 = EDGE_LOOP ( 'NONE', ( #86593, #45816, #75811, #89076 ) ) ;
#64662 = ORIENTED_EDGE ( 'NONE', *, *, #72338, .T. ) ;
#64663 = EDGE_CURVE ( 'NONE', #55378, #50747, #49184, .T. ) ;
#64664 = CARTESIAN_POINT ( 'NONE',  ( 102.4863184357179051, -28.52587382674474981, 101.9253928297069791 ) ) ;
#64665 = EDGE_CURVE ( 'NONE', #23593, #23091, #15140, .T. ) ;
#64666 = AXIS2_PLACEMENT_3D ( 'NONE', #51784, #30478, #17300 ) ;
#64667 = CARTESIAN_POINT ( 'NONE',  ( 184.5667039024485518, -48.82844715993447693, 180.4678068554150343 ) ) ;
#64668 = AXIS2_PLACEMENT_3D ( 'NONE', #14630, #62312, #35495 ) ;
#64670 = DIRECTION ( 'NONE',  ( 1.000000000000000000, 8.843517682682131024E-16, 1.000000000000000078E-15 ) ) ;
#64669 = CARTESIAN_POINT ( 'NONE',  ( 101.0349934672011614, -27.38958028709088310, 216.5327681330529686 ) ) ;
#64671 = CIRCLE ( 'NONE', #76272, 1.523999999999997579 ) ;
#64672 = LINE ( 'NONE', #9265, #11612 ) ;
#64673 = EDGE_CURVE ( 'NONE', #76993, #17950, #41922, .T. ) ;
#64674 = CARTESIAN_POINT ( 'NONE',  ( 99.09569929578050562, -30.55044413325101260, 111.8027284342002048 ) ) ;
#64675 = DIRECTION ( 'NONE',  ( 0.000000000000000000, -1.000000000000000000, 0.000000000000000000 ) ) ;
#64676 = PLANE ( 'NONE',  #52145 ) ;
#64677 = DIRECTION ( 'NONE',  ( -1.000000000000000000, -4.299999999999999979E-14, -1.000000000000000078E-15 ) ) ;
#64678 = ADVANCED_FACE ( 'NONE', ( #70097 ), #1059, .T. ) ;
#64679 = CARTESIAN_POINT ( 'NONE',  ( 105.7232414704440941, -24.98023492732636441, 160.1670538473389627 ) ) ;
#64680 = VERTEX_POINT ( 'NONE', #69653 ) ;
#64681 = ORIENTED_EDGE ( 'NONE', *, *, #68176, .T. ) ;
#64683 = ORIENTED_EDGE ( 'NONE', *, *, #64916, .T. ) ;
#64682 = EDGE_CURVE ( 'NONE', #36722, #19524, #49635, .T. ) ;
#64684 = DIRECTION ( 'NONE',  ( 1.175184669632759901E-16, -1.000000000000000000, -2.000000000000003705E-15 ) ) ;
#64685 = CARTESIAN_POINT ( 'NONE',  ( 97.81170668756638520, -40.51744870325870806, 152.6352702516163902 ) ) ;
#64686 = CARTESIAN_POINT ( 'NONE',  ( 182.4202572930269923, -31.94127993907680718, -5.074374724088000832 ) ) ;
#64687 = PLANE ( 'NONE',  #78736 ) ;
#64689 = CARTESIAN_POINT ( 'NONE',  ( 111.2851091291901042, -43.74983776777182953, 235.8252332267339852 ) ) ;
#64688 = AXIS2_PLACEMENT_3D ( 'NONE', #53738, #88314, #40128 ) ;
#64690 = CARTESIAN_POINT ( 'NONE',  ( 117.0608941297925156, -38.08045696544419201, 269.7189583031694156 ) ) ;
#64691 = AXIS2_PLACEMENT_3D ( 'NONE', #32685, #81755, #60831 ) ;
#64692 = CARTESIAN_POINT ( 'NONE',  ( 118.8775732333442647, -37.69828162312832376, 188.7613395616259595 ) ) ;
#64693 = LINE ( 'NONE', #57421, #59059 ) ;
#64694 = ORIENTED_EDGE ( 'NONE', *, *, #37517, .F. ) ;
#64696 = ORIENTED_EDGE ( 'NONE', *, *, #89848, .T. ) ;
#64695 = ORIENTED_EDGE ( 'NONE', *, *, #60546, .T. ) ;
#64697 = EDGE_CURVE ( 'NONE', #64904, #8126, #7422, .T. ) ;
#64698 = DIRECTION ( 'NONE',  ( 0.000000000000000000, 1.000000000000000000, 0.000000000000000000 ) ) ;
#64699 = VERTEX_POINT ( 'NONE', #29220 ) ;
#64700 = ORIENTED_EDGE ( 'NONE', *, *, #58100, .F. ) ;
#64702 = EDGE_CURVE ( 'NONE', #7755, #28641, #35114, .T. ) ;
#64701 = DIRECTION ( 'NONE',  ( -1.000000000000000000, 0.000000000000000000, 0.000000000000000000 ) ) ;
#64703 = DIRECTION ( 'NONE',  ( -1.000000000000000000, 0.000000000000000000, 0.000000000000000000 ) ) ;
#64704 = EDGE_CURVE ( 'NONE', #34216, #14767, #8784, .T. ) ;
#64705 = CARTESIAN_POINT ( 'NONE',  ( 110.3188062821955242, -28.45390942821411429, 266.2101547344684604 ) ) ;
#64706 = CARTESIAN_POINT ( 'NONE',  ( 3.175000000000334666, 104.3431970271541616, -31.75000000000000000 ) ) ;
#64707 = ORIENTED_EDGE ( 'NONE', *, *, #53755, .F. ) ;
#64708 = EDGE_CURVE ( 'NONE', #77564, #34120, #1311, .T. ) ;
#64709 = CARTESIAN_POINT ( 'NONE',  ( 105.4444412749903677, -44.73895730596940723, 9.635625275910939536 ) ) ;
#64710 = CARTESIAN_POINT ( 'NONE',  ( -126.7366439761708818, 60.90736961166211216, 31.34868955532726886 ) ) ;
#64711 = ORIENTED_EDGE ( 'NONE', *, *, #76335, .F. ) ;
#64712 = EDGE_LOOP ( 'NONE', ( #77100, #7948 ) ) ;
#64713 = FACE_OUTER_BOUND ( 'NONE', #58856, .T. ) ;
#64714 = ORIENTED_EDGE ( 'NONE', *, *, #4873, .F. ) ;
#64715 = VERTEX_POINT ( 'NONE', #8326 ) ;
#64716 = CARTESIAN_POINT ( 'NONE',  ( 115.6047007430436366, -36.96391350797230757, 43.22670554236196239 ) ) ;
#64717 = CARTESIAN_POINT ( 'NONE',  ( 117.4794452684060104, -40.50643855513092007, 173.5375300378159693 ) ) ;
#64718 = CARTESIAN_POINT ( 'NONE',  ( 95.69905522618344662, -33.46911247776736786, 141.1041967044829732 ) ) ;
#64719 = DIRECTION ( 'NONE',  ( 1.000000000000000000, 4.163336342344333240E-14, 0.000000000000000000 ) ) ;
#64720 = CARTESIAN_POINT ( 'NONE',  ( 117.4913186190917855, -36.80221964929349809, 259.8213395616249386 ) ) ;
#64721 = CARTESIAN_POINT ( 'NONE',  ( 156.5667039024484097, -42.82844715993568485, 175.7178068554150059 ) ) ;
#64722 = CARTESIAN_POINT ( 'NONE',  ( 86.74776510736894863, -122.7922775461496627, 250.2190963482990185 ) ) ;
#64723 = DIRECTION ( 'NONE',  ( 0.000000000000000000, -1.000000000000000000, 0.000000000000000000 ) ) ;
#64724 = ORIENTED_EDGE ( 'NONE', *, *, #81334, .T. ) ;
#64725 = VERTEX_POINT ( 'NONE', #64188 ) ;
#64726 = CIRCLE ( 'NONE', #37172, 17.00000000000000000 ) ;
#64727 = AXIS2_PLACEMENT_3D ( 'NONE', #74728, #26570, #59733 ) ;
#64729 = CARTESIAN_POINT ( 'NONE',  ( 104.5519768891453651, -48.36156025571956718, 182.4070538473399665 ) ) ;
#64728 = AXIS2_PLACEMENT_3D ( 'NONE', #62046, #34793, #35234 ) ;
#64730 = VERTEX_POINT ( 'NONE', #1962 ) ;
#64731 = CARTESIAN_POINT ( 'NONE',  ( 98.09046607155295305, -42.10132104613245474, 161.7556252759109725 ) ) ;
#64732 = LINE ( 'NONE', #49297, #63067 ) ;
#64733 = CIRCLE ( 'NONE', #79274, 2.517500000000005844 ) ;
#64734 = CARTESIAN_POINT ( 'NONE',  ( 127.0664832912740110, -46.72944715994101017, 14.67562527591099197 ) ) ;
#64735 = DIRECTION ( 'NONE',  ( -0.000000000000000000, -0.000000000000000000, 1.000000000000000000 ) ) ;
#64738 = CARTESIAN_POINT ( 'NONE',  ( 98.95962429139169103, -30.20966935044063462, 236.7870538473399336 ) ) ;
#64737 = DIRECTION ( 'NONE',  ( 0.000000000000000000, 0.000000000000000000, -1.000000000000000000 ) ) ;
#64736 = CARTESIAN_POINT ( 'NONE',  ( 98.00804396577686362, -39.67311905263231608, 277.6356252759111385 ) ) ;
#64739 = CARTESIAN_POINT ( 'NONE',  ( 147.0667039024469886, -67.87844716047348470, 245.4920193514540188 ) ) ;
#64740 = DIRECTION ( 'NONE',  ( 0.000000000000000000, -1.000000000000000000, 0.000000000000000000 ) ) ;
#64741 = DIRECTION ( 'NONE',  ( 1.000000000000000000, 0.000000000000000000, 0.000000000000000000 ) ) ;
#64742 = DIRECTION ( 'NONE',  ( 0.07779791923983175872, 0.07779791925944627706, 0.9939290555773350189 ) ) ;
#64743 = CARTESIAN_POINT ( 'NONE',  ( 113.1782937836032659, -44.75186858293219672, 259.0939586104858563 ) ) ;
#64744 = CARTESIAN_POINT ( 'NONE',  ( 126.8164832912740394, -46.47944715994101017, -5.074374724089010691 ) ) ;
#64746 = VERTEX_POINT ( 'NONE', #28769 ) ;
#64745 = CARTESIAN_POINT ( 'NONE',  ( 115.3517163442624707, -37.78381771408454171, 195.5838068554166966 ) ) ;
#64747 = CARTESIAN_POINT ( 'NONE',  ( 131.0667039024480118, -61.87844715994100397, 207.5838068554149913 ) ) ;
#64748 = CARTESIAN_POINT ( 'NONE',  ( 98.53312381531716824, -44.98873235655736380, 191.9384824187679612 ) ) ;
#64749 = CARTESIAN_POINT ( 'NONE',  ( 107.3210293350295501, -25.67914459413323058, 71.04610146638795243 ) ) ;
#64750 = CARTESIAN_POINT ( 'NONE',  ( 96.60079736239889314, -36.47965167166085365, 192.3070538473399438 ) ) ;
#64751 = CARTESIAN_POINT ( 'NONE',  ( 72.26648329127297643, -71.52944715994141234, 352.4506252759078961 ) ) ;
#64752 = DIRECTION ( 'NONE',  ( -1.000000000000000078E-15, 1.000000000000000083E-30, 1.000000000000000000 ) ) ;
#64753 = AXIS2_PLACEMENT_3D ( 'NONE', #27129, #12612, #41632 ) ;
#64755 = DIRECTION ( 'NONE',  ( 0.000000000000000000, -1.000000000000000000, 0.000000000000000000 ) ) ;
#64754 = CARTESIAN_POINT ( 'NONE',  ( -135.2444258376730204, 0.000000000000000000, 147.4575741623271767 ) ) ;
#64756 = DIRECTION ( 'NONE',  ( 0.000000000000000000, 0.000000000000000000, -1.000000000000000000 ) ) ;
#64757 = PLANE ( 'NONE',  #19469 ) ;
#64758 = EDGE_LOOP ( 'NONE', ( #57534, #22445, #29087, #77847 ) ) ;
#64759 = FACE_OUTER_BOUND ( 'NONE', #17549, .T. ) ;
#64760 = AXIS2_PLACEMENT_3D ( 'NONE', #51560, #66085, #65647 ) ;
#64761 = ADVANCED_FACE ( 'NONE', ( #71010 ), #63737, .F. ) ;
#64762 = ORIENTED_EDGE ( 'NONE', *, *, #26669, .T. ) ;
#64763 = ADVANCED_FACE ( 'NONE', ( #50084 ), #43269, .T. ) ;
#64764 = EDGE_LOOP ( 'NONE', ( #55207, #80942, #73592, #79871 ) ) ;
#64765 = CARTESIAN_POINT ( 'NONE',  ( 115.9068402959922111, -38.69432841718559501, 103.0628960185529763 ) ) ;
#64766 = EDGE_CURVE ( 'NONE', #3629, #11834, #13790, .T. ) ;
#64768 = ORIENTED_EDGE ( 'NONE', *, *, #57810, .T. ) ;
#64767 = CARTESIAN_POINT ( 'NONE',  ( -11.41209158312316774, 88.18445188672595236, -130.0566639163490095 ) ) ;
#64769 = CARTESIAN_POINT ( 'NONE',  ( 101.7220374796297335, -27.76276858577408291, 81.50419670448295051 ) ) ;
#64770 = DIRECTION ( 'NONE',  ( 0.000000000000000000, 1.000000000000000000, 0.000000000000000000 ) ) ;
#64771 = DIRECTION ( 'NONE',  ( 0.000000000000000000, 0.000000000000000000, 1.000000000000000000 ) ) ;
#64772 = ADVANCED_FACE ( 'NONE', ( #6977 ), #27422, .T. ) ;
#64773 = EDGE_CURVE ( 'NONE', #84886, #72226, #34681, .T. ) ;
#64774 = CYLINDRICAL_SURFACE ( 'NONE', #82487, 0.5000000000000004441 ) ;
#64775 = CARTESIAN_POINT ( 'NONE',  ( 100.9534786964907482, -28.35269599622599301, 30.56610146638794134 ) ) ;
#64776 = ORIENTED_EDGE ( 'NONE', *, *, #4192, .T. ) ;
#64777 = ORIENTED_EDGE ( 'NONE', *, *, #2556, .F. ) ;
#64778 = ORIENTED_EDGE ( 'NONE', *, *, #24705, .T. ) ;
#64779 = ADVANCED_FACE ( 'NONE', ( #85983 ), #86865, .T. ) ;
#64780 = CARTESIAN_POINT ( 'NONE',  ( 51.42025729302656600, -31.94127993907661889, 313.9678068554150059 ) ) ;
#64781 = CYLINDRICAL_SURFACE ( 'NONE', #85382, 16.00000000000090239 ) ;
#64782 = LINE ( 'NONE', #30704, #8651 ) ;
#64783 = DIRECTION ( 'NONE',  ( -1.776356839400250465E-15, 0.000000000000000000, -1.000000000000000000 ) ) ;
#64784 = CARTESIAN_POINT ( 'NONE',  ( 180.3503142329366824, -29.99615139351640636, 313.9678068554149490 ) ) ;
#64785 = EDGE_CURVE ( 'NONE', #20525, #48933, #45489, .T. ) ;
#64786 = CARTESIAN_POINT ( 'NONE',  ( 102.0674824855994842, -27.97024723768227261, 51.49124353025893441 ) ) ;
#64787 = CARTESIAN_POINT ( 'NONE',  ( 182.5667039024469886, -33.35206098992650681, 193.9678068554150059 ) ) ;
#64788 = CARTESIAN_POINT ( 'NONE',  ( 78.95116244206022316, 93.33902940301967988, 88.44409384119040851 ) ) ;
#64789 = CARTESIAN_POINT ( 'NONE',  ( 104.0490797691969647, -47.33883444496888160, 67.36800622829191809 ) ) ;
#64791 = ORIENTED_EDGE ( 'NONE', *, *, #42687, .T. ) ;
#64790 = EDGE_CURVE ( 'NONE', #26777, #33481, #57805, .T. ) ;
#64792 = CARTESIAN_POINT ( 'NONE',  ( 100.9546734967587156, -28.70702521494872173, 270.5939585418061029 ) ) ;
#64793 = CIRCLE ( 'NONE', #9670, 7.937500000000000000 ) ;
#64794 = CARTESIAN_POINT ( 'NONE',  ( 86.72755763596092038, -85.76982405743865456, 250.2178068554179902 ) ) ;
#64795 = CARTESIAN_POINT ( 'NONE',  ( 115.2991214174112002, -34.06025354975611918, 131.9061856076869788 ) ) ;
#64796 = EDGE_CURVE ( 'NONE', #60920, #137, #57351, .T. ) ;
#64797 = AXIS2_PLACEMENT_3D ( 'NONE', #30497, #15983, #71838 ) ;
#64798 = AXIS2_PLACEMENT_3D ( 'NONE', #47850, #5651, #68768 ) ;
#64799 = VECTOR ( 'NONE', #26801, 1000.000000000000000 ) ;
#64800 = AXIS2_PLACEMENT_3D ( 'NONE', #3020, #17103, #63914 ) ;
#64801 = CARTESIAN_POINT ( 'NONE',  ( 97.81168883536605563, -40.51740680051663190, 96.63562987897269352 ) ) ;
#64802 = DIRECTION ( 'NONE',  ( 0.000000000000000000, 1.000000000000000000, 0.000000000000000000 ) ) ;
#64803 = VERTEX_POINT ( 'NONE', #50986 ) ;
#64804 = ORIENTED_EDGE ( 'NONE', *, *, #23192, .T. ) ;
#64805 = CARTESIAN_POINT ( 'NONE',  ( 97.83897911476498166, -40.58352276682783355, 136.6416734916348616 ) ) ;
#64806 = ORIENTED_EDGE ( 'NONE', *, *, #10906, .F. ) ;
#64807 = ORIENTED_EDGE ( 'NONE', *, *, #13072, .T. ) ;
#64808 = EDGE_CURVE ( 'NONE', #42743, #79424, #9657, .T. ) ;
#64809 = CARTESIAN_POINT ( 'NONE',  ( 106.9887167903908392, -45.59072421142732168, 184.0015833058969577 ) ) ;
#64810 = FACE_OUTER_BOUND ( 'NONE', #66136, .T. ) ;
#64811 = EDGE_CURVE ( 'NONE', #85401, #43446, #65951, .T. ) ;
#64812 = CIRCLE ( 'NONE', #21241, 0.9999999999999974465 ) ;
#64813 = CARTESIAN_POINT ( 'NONE',  ( 109.2058805625337925, -26.50397703278076733, 135.9127681330539872 ) ) ;
#64814 = DIRECTION ( 'NONE',  ( 1.000000000000000000, 3.999999999999999995E-14, 1.000000000000000078E-15 ) ) ;
#64815 = CARTESIAN_POINT ( 'NONE',  ( 116.9194122960482929, -38.69773298920891591, 18.66981024198805628 ) ) ;
#64816 = VERTEX_POINT ( 'NONE', #73212 ) ;
#64817 = VERTEX_POINT ( 'NONE', #24626 ) ;
#64818 = ORIENTED_EDGE ( 'NONE', *, *, #86409, .F. ) ;
#64819 = CARTESIAN_POINT ( 'NONE',  ( 111.7296936849409406, -43.46273440104761221, 200.8766617981629565 ) ) ;
#64820 = CARTESIAN_POINT ( 'NONE',  ( 95.32417067969559810, -34.95402877631575222, 71.20705384733993526 ) ) ;
#64821 = EDGE_LOOP ( 'NONE', ( #86504, #9572, #28105, #61901 ) ) ;
#64822 = CARTESIAN_POINT ( 'NONE',  ( 100.5643946202652330, -27.81952766013690237, 30.56610146638794134 ) ) ;
#64823 = CARTESIAN_POINT ( 'NONE',  ( 96.62257978078039855, -36.48017157545621814, 192.3070538473399438 ) ) ;
#64824 = LINE ( 'NONE', #15343, #14717 ) ;
#64825 = PLANE ( 'NONE',  #61916 ) ;
#64826 = CARTESIAN_POINT ( 'NONE',  ( 109.0722782120600840, -47.59916505968618594, 123.7337205140059666 ) ) ;
#64827 = DIRECTION ( 'NONE',  ( -1.000000000000000000, 0.000000000000000000, 0.000000000000000000 ) ) ;
#64828 = ORIENTED_EDGE ( 'NONE', *, *, #79349, .T. ) ;
#64829 = FACE_BOUND ( 'NONE', #42872, .T. ) ;
#64830 = EDGE_CURVE ( 'NONE', #18386, #75279, #30108, .T. ) ;
#64831 = ORIENTED_EDGE ( 'NONE', *, *, #36681, .F. ) ;
#64832 = DIRECTION ( 'NONE',  ( -1.000000000000000000, 0.000000000000000000, 0.000000000000000000 ) ) ;
#64833 = ORIENTED_EDGE ( 'NONE', *, *, #26418, .T. ) ;
#64834 = ORIENTED_EDGE ( 'NONE', *, *, #79452, .F. ) ;
#64835 = VECTOR ( 'NONE', #34459, 1000.000000000000114 ) ;
#64836 = EDGE_CURVE ( 'NONE', #4499, #52329, #38691, .T. ) ;
#64837 = CARTESIAN_POINT ( 'NONE',  ( 107.0664832912750057, -36.72944715993903486, 9.425625275910970657 ) ) ;
#64838 = CARTESIAN_POINT ( 'NONE',  ( 114.5019750680372113, -29.98747414221284302, 130.4130031197996402 ) ) ;
#64839 = CARTESIAN_POINT ( 'NONE',  ( 96.95653860995706452, -32.26087848594701057, 55.98324432352897162 ) ) ;
#64840 = CARTESIAN_POINT ( 'NONE',  ( 7.511964023296719084, 69.63594209550339542, 37.35831287037660076 ) ) ;
#64841 = DIRECTION ( 'NONE',  ( 1.000000000000000000, 0.000000000000000000, 0.000000000000000000 ) ) ;
#64842 = CARTESIAN_POINT ( 'NONE',  ( 151.0371591254584587, -46.82818131005592477, 193.9678068554149775 ) ) ;
#64843 = CARTESIAN_POINT ( 'NONE',  ( 104.1495640007033217, -46.68084741754461220, 62.33753003781600199 ) ) ;
#64845 = CARTESIAN_POINT ( 'NONE',  ( 101.9826776100855881, -46.51815199768660847, 163.1832443235299763 ) ) ;
#64844 = CARTESIAN_POINT ( 'NONE',  ( 25.56670390244797275, -62.87844715994099687, 288.3428068554150059 ) ) ;
#64846 = CARTESIAN_POINT ( 'NONE',  ( 115.8228084649852860, -31.72548357239955763, 59.24020506417635801 ) ) ;
#64847 = DIRECTION ( 'NONE',  ( -1.749395751137010036E-15, 0.000000000000000000, -1.000000000000000000 ) ) ;
#64848 = ORIENTED_EDGE ( 'NONE', *, *, #28781, .T. ) ;
#64849 = CARTESIAN_POINT ( 'NONE',  ( 107.5667039024470455, -113.2645475377471058, 2.217806855418280598 ) ) ;
#64850 = FACE_OUTER_BOUND ( 'NONE', #79925, .T. ) ;
#64851 = DIRECTION ( 'NONE',  ( -1.000000000000000000, 0.000000000000000000, 1.046082768126375896E-16 ) ) ;
#64852 = CARTESIAN_POINT ( 'NONE',  ( 140.0667039024470455, -118.2784471599408960, 51.21780685541800437 ) ) ;
#64854 = VERTEX_POINT ( 'NONE', #85092 ) ;
#64853 = CARTESIAN_POINT ( 'NONE',  ( 110.7116931949060614, -48.05822654157750407, 207.8241967044819489 ) ) ;
#64855 = AXIS2_PLACEMENT_3D ( 'NONE', #83871, #77049, #14829 ) ;
#64856 = CARTESIAN_POINT ( 'NONE',  ( 162.0667039024470171, -77.67844715994088745, 222.2178068554179902 ) ) ;
#64857 = CARTESIAN_POINT ( 'NONE',  ( 96.49610902845032001, -31.31747537214017640, 241.9499109901969689 ) ) ;
#64858 = CARTESIAN_POINT ( 'NONE',  ( 96.59840162804212582, -36.61878533396502888, 107.3184824187679567 ) ) ;
#64859 = VECTOR ( 'NONE', #29416, 1000.000000000000000 ) ;
#64860 = LINE ( 'NONE', #37158, #76655 ) ;
#64861 = CARTESIAN_POINT ( 'NONE',  ( -141.3509999999999991, 0.000000000000000000, -141.3509999999999991 ) ) ;
#64862 = EDGE_CURVE ( 'NONE', #49976, #31872, #9223, .T. ) ;
#64863 = CARTESIAN_POINT ( 'NONE',  ( 0.000000000000000000, 239.0000000000000000, 154.6557476874258441 ) ) ;
#64864 = ORIENTED_EDGE ( 'NONE', *, *, #52896, .T. ) ;
#64865 = AXIS2_PLACEMENT_3D ( 'NONE', #34122, #13690, #54545 ) ;
#64866 = VECTOR ( 'NONE', #61871, 1000.000000000000000 ) ;
#64867 = AXIS2_PLACEMENT_3D ( 'NONE', #85157, #15205, #8394 ) ;
#64868 = EDGE_CURVE ( 'NONE', #84879, #41258, #17813, .T. ) ;
#64869 = ORIENTED_EDGE ( 'NONE', *, *, #30209, .T. ) ;
#64870 = EDGE_CURVE ( 'NONE', #74824, #54956, #86426, .T. ) ;
#64871 = ORIENTED_EDGE ( 'NONE', *, *, #43210, .T. ) ;
#64872 = EDGE_CURVE ( 'NONE', #56957, #6370, #64623, .T. ) ;
#64873 = ORIENTED_EDGE ( 'NONE', *, *, #78640, .F. ) ;
#64874 = CYLINDRICAL_SURFACE ( 'NONE', #56852, 1.000000000002049694 ) ;
#64875 = CARTESIAN_POINT ( 'NONE',  ( 112.1867106929447573, -26.95862322015898016, 10.68038718067299087 ) ) ;
#64876 = LINE ( 'NONE', #2660, #78032 ) ;
#64877 = DIRECTION ( 'NONE',  ( -0.7071067811865477948, 0.7071067811865473507, 0.000000000000000000 ) ) ;
#64878 = EDGE_CURVE ( 'NONE', #701, #1745, #21615, .T. ) ;
#64880 = CARTESIAN_POINT ( 'NONE',  ( 79.74945239053440105, 71.14137858619484689, 87.72765544449677577 ) ) ;
#64879 = CARTESIAN_POINT ( 'NONE',  ( 107.0664832912750057, -36.72944715993903486, 0.7256252759109708128 ) ) ;
#64881 = DIRECTION ( 'NONE',  ( 0.000000000000000000, 1.000000000000000000, 0.000000000000000000 ) ) ;
#64882 = CIRCLE ( 'NONE', #43068, 13.31747058675099993 ) ;
#64883 = CARTESIAN_POINT ( 'NONE',  ( 115.5441482490607257, -35.68765611295631857, 193.3467055423629688 ) ) ;
#64884 = VERTEX_POINT ( 'NONE', #65073 ) ;
#64885 = EDGE_LOOP ( 'NONE', ( #55636, #54609 ) ) ;
#64886 = VERTEX_POINT ( 'NONE', #24190 ) ;
#64888 = EDGE_CURVE ( 'NONE', #57610, #45317, #17370, .T. ) ;
#64887 = VECTOR ( 'NONE', #84302, 1000.000000000000000 ) ;
#64889 = DIRECTION ( 'NONE',  ( 1.000000000000000000, 0.000000000000000000, 0.000000000000000000 ) ) ;
#64890 = FACE_OUTER_BOUND ( 'NONE', #87256, .T. ) ;
#64891 = CARTESIAN_POINT ( 'NONE',  ( 116.8470136369841725, -36.79772195930840439, 259.8213395616247681 ) ) ;
#64892 = EDGE_CURVE ( 'NONE', #64449, #17979, #38254, .T. ) ;
#64893 = DIRECTION ( 'NONE',  ( 1.017460296392624983E-15, 1.000000000000000000, 0.000000000000000000 ) ) ;
#64894 = CARTESIAN_POINT ( 'NONE',  ( 112.0650656126721429, -45.48886803529176603, 27.98971541558280052 ) ) ;
#64895 = ORIENTED_EDGE ( 'NONE', *, *, #64766, .T. ) ;
#64896 = CARTESIAN_POINT ( 'NONE',  ( 77.51853161617805199, -35.69475198630856738, 2.828485944707570532 ) ) ;
#64897 = ORIENTED_EDGE ( 'NONE', *, *, #78560, .T. ) ;
#64898 = DIRECTION ( 'NONE',  ( -0.9659258262890706437, 0.000000000000000000, 0.2588190451025119132 ) ) ;
#64899 = CARTESIAN_POINT ( 'NONE',  ( 114.6641587241874873, -32.58502278776634142, 22.02999513149600475 ) ) ;
#64900 = AXIS2_PLACEMENT_3D ( 'NONE', #65200, #22536, #9344 ) ;
#64901 = CARTESIAN_POINT ( 'NONE',  ( 136.8164812439618743, -18.63640413216975844, 6.749771997051317918 ) ) ;
#64902 = FACE_OUTER_BOUND ( 'NONE', #12647, .T. ) ;
#64903 = CARTESIAN_POINT ( 'NONE',  ( 191.6377717143134873, -67.87844715994100397, 13.84673904354931651 ) ) ;
#64904 = VERTEX_POINT ( 'NONE', #50537 ) ;
#64905 = CARTESIAN_POINT ( 'NONE',  ( 41.56670390244689628, -36.32844715994109208, 180.4678068554150911 ) ) ;
#64906 = CARTESIAN_POINT ( 'NONE',  ( 131.0667039024480118, -58.35344715994099829, 210.8338068554149913 ) ) ;
#64907 = ORIENTED_EDGE ( 'NONE', *, *, #65488, .T. ) ;
#64908 = CARTESIAN_POINT ( 'NONE',  ( 96.08737379349030050, -38.00938547453511518, 86.43086337114897333 ) ) ;
#64909 = EDGE_LOOP ( 'NONE', ( #75901, #79700 ) ) ;
#64910 = CARTESIAN_POINT ( 'NONE',  ( 105.7183000297088284, -45.16381338481517815, 36.87241982807598362 ) ) ;
#64911 = CARTESIAN_POINT ( 'NONE',  ( 107.7442340506927252, -46.73693967930866933, 88.62940955498838491 ) ) ;
#64912 = CARTESIAN_POINT ( 'NONE',  ( 98.73617028912649118, -32.38405755445656808, 87.36348806780198117 ) ) ;
#64913 = CARTESIAN_POINT ( 'NONE',  ( 105.7147715443256715, -46.72375139838595004, 13.46890240877466383 ) ) ;
#64914 = DIRECTION ( 'NONE',  ( -0.000000000000000000, -0.000000000000000000, 1.000000000000000000 ) ) ;
#64915 = VECTOR ( 'NONE', #69532, 1000.000000000000000 ) ;
#64916 = EDGE_CURVE ( 'NONE', #89511, #88009, #16043, .T. ) ;
#64917 = CARTESIAN_POINT ( 'NONE',  ( 68.89066010437798582, -69.53878131779040928, 247.4962434065126331 ) ) ;
#64918 = CARTESIAN_POINT ( 'NONE',  ( 99.34942397265413661, -29.65555323683921074, 271.7356252759109907 ) ) ;
#64919 = FACE_OUTER_BOUND ( 'NONE', #74449, .T. ) ;
#64920 = ORIENTED_EDGE ( 'NONE', *, *, #53660, .F. ) ;
#64921 = LINE ( 'NONE', #58102, #53075 ) ;
#64922 = VERTEX_POINT ( 'NONE', #19162 ) ;
#64923 = CARTESIAN_POINT ( 'NONE',  ( 114.4937323636162176, -28.48121435373123589, 155.5051490854349652 ) ) ;
#64924 = AXIS2_PLACEMENT_3D ( 'NONE', #12937, #40166, #81546 ) ;
#64925 = CARTESIAN_POINT ( 'NONE',  ( 79.87807227642528574, -21.47944715994105991, 1.625625275910942635 ) ) ;
#64926 = EDGE_LOOP ( 'NONE', ( #61963, #82379 ) ) ;
#64927 = ORIENTED_EDGE ( 'NONE', *, *, #14262, .T. ) ;
#64928 = VERTEX_POINT ( 'NONE', #68210 ) ;
#64929 = CYLINDRICAL_SURFACE ( 'NONE', #33353, 0.5000000000000073275 ) ;
#64930 = CARTESIAN_POINT ( 'NONE',  ( 34.67381068360336371, -28.98061976759059988, 193.9678068554150911 ) ) ;
#64931 = CARTESIAN_POINT ( 'NONE',  ( 116.2522929705883712, -40.08866370952549829, 218.5470538473399529 ) ) ;
#64932 = CARTESIAN_POINT ( 'NONE',  ( 107.0667039024479834, -18.72944715994100306, 239.5838068554170377 ) ) ;
#64933 = CARTESIAN_POINT ( 'NONE',  ( 145.0437226634070669, -139.7014121172837804, 246.0198185477100026 ) ) ;
#64934 = CARTESIAN_POINT ( 'NONE',  ( 31.89136050872298966, -31.76306994223740432, -5.074374724088000832 ) ) ;
#64935 = CARTESIAN_POINT ( 'NONE',  ( 96.68927247633037325, -32.92320750051204215, 17.03467289495896964 ) ) ;
#64936 = CARTESIAN_POINT ( 'NONE',  ( 248.6659999999999968, 52.73749999999999716, 10.66800000000000104 ) ) ;
#64937 = ORIENTED_EDGE ( 'NONE', *, *, #29983, .F. ) ;
#64938 = CIRCLE ( 'NONE', #18498, 6.349999999999999645 ) ;
#64939 = CARTESIAN_POINT ( 'NONE',  ( 97.60786201319120892, -39.98234442571827429, 172.5900479121347928 ) ) ;
#64940 = CIRCLE ( 'NONE', #88231, 10.00000000000000178 ) ;
#64941 = VECTOR ( 'NONE', #35774, 1000.000000000000000 ) ;
#64942 = CARTESIAN_POINT ( 'NONE',  ( 117.0608951760848555, -38.08044937632849525, 43.71866473332352143 ) ) ;
#64943 = ORIENTED_EDGE ( 'NONE', *, *, #68202, .F. ) ;
#64944 = AXIS2_PLACEMENT_3D ( 'NONE', #40959, #20539, #21432 ) ;
#64945 = ADVANCED_FACE ( 'NONE', ( #40037 ), #46389, .F. ) ;
#64946 = CARTESIAN_POINT ( 'NONE',  ( 81.77804793994209831, -20.88970947304156311, 2.099345637348018823 ) ) ;
#64947 = CARTESIAN_POINT ( 'NONE',  ( 31.56670390244800828, -32.29483332968611364, -5.074374724088000832 ) ) ;
#64948 = CARTESIAN_POINT ( 'NONE',  ( 105.6350724880777392, -47.03380199863529754, 257.4670538473393435 ) ) ;
#64949 = SURFACE_SIDE_STYLE ('',( #16802 ) ) ;
#64950 = DIRECTION ( 'NONE',  ( 0.9068632946707807507, -0.4214249218767881500, 9.028300618466658994E-16 ) ) ;
#64951 = DIRECTION ( 'NONE',  ( 0.000000000000000000, 1.000000000000000000, 0.000000000000000000 ) ) ;
#64952 = CARTESIAN_POINT ( 'NONE',  ( 110.3936857311090023, -28.86269079874493571, 244.1809912566479568 ) ) ;
#64954 = CARTESIAN_POINT ( 'NONE',  ( 116.7246412902988908, -32.86309880586080823, 50.12991099019698282 ) ) ;
#64953 = FACE_OUTER_BOUND ( 'NONE', #13579, .T. ) ;
#64955 = CARTESIAN_POINT ( 'NONE',  ( 126.9549993752607264, 57.49093265451766399, 30.45191747052217934 ) ) ;
#64956 = CARTESIAN_POINT ( 'NONE',  ( 117.3823636748946058, -32.63121637840519895, 99.13943479972098771 ) ) ;
#64957 = VERTEX_POINT ( 'NONE', #33235 ) ;
#64958 = CARTESIAN_POINT ( 'NONE',  ( 131.4241199117880683, -19.49143581485983034, 6.902478035882034568 ) ) ;
#64959 = ORIENTED_EDGE ( 'NONE', *, *, #38621, .F. ) ;
#64960 = CARTESIAN_POINT ( 'NONE',  ( 137.0667039024470739, -118.2784471599408960, 222.2178068554179902 ) ) ;
#64961 = CARTESIAN_POINT ( 'NONE',  ( 0.000000000000000000, 17.78000000000000114, 0.000000000000000000 ) ) ;
#64962 = ORIENTED_EDGE ( 'NONE', *, *, #12979, .F. ) ;
#64963 = PRODUCT_RELATED_PRODUCT_CATEGORY ( 'part', '', ( #11164 ) ) ;
#64964 = CARTESIAN_POINT ( 'NONE',  ( 116.3212776292296127, -32.94146857471318413, 287.6356252759109680 ) ) ;
#64965 = ORIENTED_EDGE ( 'NONE', *, *, #1604, .F. ) ;
#64966 = DIRECTION ( 'NONE',  ( -1.000000000000000000, -8.953411488912552682E-16, 0.000000000000000000 ) ) ;
#64967 = DIRECTION ( 'NONE',  ( 0.9999999853157766072, 0.0001713722456134972175, 0.000000000000000000 ) ) ;
#64968 = VECTOR ( 'NONE', #7887, 1000.000000000000114 ) ;
#64969 = CARTESIAN_POINT ( 'NONE',  ( 123.6837132603318992, -53.34645651782490461, 239.5838068554164693 ) ) ;
#64970 = ORIENTED_EDGE ( 'NONE', *, *, #38035, .T. ) ;
#64971 = CARTESIAN_POINT ( 'NONE',  ( 98.28768183251310120, -28.73153112808589427, 80.73848241876795839 ) ) ;
#64972 = DIRECTION ( 'NONE',  ( 1.346944695195362088E-15, -1.000000000000000000, 3.469446951953620425E-31 ) ) ;
#64973 = CARTESIAN_POINT ( 'NONE',  ( -13.40680633928201004, 239.0000000000000000, 102.7987842159323151 ) ) ;
#64974 = DIRECTION ( 'NONE',  ( 0.000000000000000000, 0.000000000000000000, 1.000000000000000000 ) ) ;
#64975 = ORIENTED_EDGE ( 'NONE', *, *, #26072, .T. ) ;
#64976 = EDGE_CURVE ( 'NONE', #53519, #24962, #45935, .T. ) ;
#64977 = EDGE_CURVE ( 'NONE', #52826, #77857, #18705, .T. ) ;
#64978 = CARTESIAN_POINT ( 'NONE',  ( 183.6524903400783444, -49.32844715993451956, 300.4678068554149490 ) ) ;
#64979 = DIRECTION ( 'NONE',  ( 0.000000000000000000, -1.000000000000000000, 0.000000000000000000 ) ) ;
#64980 = ADVANCED_FACE ( 'NONE', ( #31882 ), #39146, .T. ) ;
#64981 = CARTESIAN_POINT ( 'NONE',  ( -215.9000000000000057, 104.7749999999999915, -41.27499999999999858 ) ) ;
#64982 = ADVANCED_FACE ( 'NONE', ( #4186 ), #60934, .F. ) ;
#64983 = B_SPLINE_CURVE_WITH_KNOTS ( 'NONE', 3,
 ( #65857, #72700, #86773, #3213, #10466, #38167 ),
 .UNSPECIFIED., .F., .F.,
 ( 4, 2, 4 ),
 ( 0.000000000000000000, 0.05514354140252886172, 0.1102870828050577234 ),
 .UNSPECIFIED. ) ;
#64985 = DIRECTION ( 'NONE',  ( 0.9242245927363033076, 0.3818493186865918876, 0.000000000000000000 ) ) ;
#64984 = DIRECTION ( 'NONE',  ( -4.237773401492740281E-14, 1.000000000000000000, 0.000000000000000000 ) ) ;
#64986 = DIRECTION ( 'NONE',  ( 0.000000000000000000, 1.000000000000000000, 0.000000000000000000 ) ) ;
#64987 = VECTOR ( 'NONE', #72140, 1000.000000000000000 ) ;
#64988 = ORIENTED_EDGE ( 'NONE', *, *, #7998, .T. ) ;
#64989 = AXIS2_PLACEMENT_3D ( 'NONE', #79162, #16923, #37357 ) ;
#64990 = DIRECTION ( 'NONE',  ( 0.000000000000000000, 0.000000000000000000, 1.000000000000000000 ) ) ;
#64991 = CARTESIAN_POINT ( 'NONE',  ( 97.29384000864243376, -37.12803473146956890, 157.3584824187679487 ) ) ;
#64992 = EDGE_CURVE ( 'NONE', #89473, #7800, #25944, .T. ) ;
#64994 = ORIENTED_EDGE ( 'NONE', *, *, #20573, .F. ) ;
#64993 = CYLINDRICAL_SURFACE ( 'NONE', #54466, 5.562600000000000655 ) ;
#64995 = AXIS2_PLACEMENT_3D ( 'NONE', #85492, #72731, #79562 ) ;
#64996 = CARTESIAN_POINT ( 'NONE',  ( 107.1874307469290244, -26.94942635195924652, 31.06705384733893283 ) ) ;
#64997 = CARTESIAN_POINT ( 'NONE',  ( 49.21213752015869858, -29.73316016639558512, 193.9678068554150911 ) ) ;
#64998 = CARTESIAN_POINT ( 'NONE',  ( 97.82529242725978236, -40.55051696138422557, 51.63847270892774333 ) ) ;
#64999 = CARTESIAN_POINT ( 'NONE',  ( 99.04383725273962114, -42.84092021590794275, 11.84399581657901379 ) ) ;
#65000 = VECTOR ( 'NONE', #39677, 1000.000000000000000 ) ;
#65001 = PLANE ( 'NONE',  #45691 ) ;
#65002 = AXIS2_PLACEMENT_3D ( 'NONE', #5358, #61205, #32598 ) ;
#65004 = CARTESIAN_POINT ( 'NONE',  ( 101.9853755998761073, -45.08682593082395584, 247.1413395616259550 ) ) ;
#65003 = CIRCLE ( 'NONE', #69356, 2.500000000000002220 ) ;
#65005 = ORIENTED_EDGE ( 'NONE', *, *, #39658, .T. ) ;
#65006 = ORIENTED_EDGE ( 'NONE', *, *, #44854, .T. ) ;
#65007 = CARTESIAN_POINT ( 'NONE',  ( 101.0667092185316989, -28.63788266170726260, 182.0158690201829756 ) ) ;
#65008 = CARTESIAN_POINT ( 'NONE',  ( 116.3212776292269837, -32.94146857470673240, 74.13562527591093954 ) ) ;
#65009 = CARTESIAN_POINT ( 'NONE',  ( 116.4244759746951985, -37.56879123375174601, 30.17491663923099665 ) ) ;
#65010 = CARTESIAN_POINT ( 'NONE',  ( -87.71605664018947834, 93.55484823631826430, 96.70003673985476667 ) ) ;
#65011 = DIRECTION ( 'NONE',  ( 0.000000000000000000, 0.000000000000000000, -1.000000000000000000 ) ) ;
#65012 = CIRCLE ( 'NONE', #63590, 2.999999999999999112 ) ;
#65013 = DIRECTION ( 'NONE',  ( 0.000000000000000000, -1.000000000000000000, 0.000000000000000000 ) ) ;
#65014 = ORIENTED_EDGE ( 'NONE', *, *, #8041, .F. ) ;
#65015 = CARTESIAN_POINT ( 'NONE',  ( 98.58946256649485917, -108.5954344580498514, -19.78219314458187839 ) ) ;
#65016 = LINE ( 'NONE', #65460, #61849 ) ;
#65017 = CARTESIAN_POINT ( 'NONE',  ( 106.5683798796750779, -47.15615894637593897, 247.5384824187679556 ) ) ;
#65018 = CYLINDRICAL_SURFACE ( 'NONE', #75112, 10.04999999999999361 ) ;
#65019 = ORIENTED_EDGE ( 'NONE', *, *, #72773, .F. ) ;
#65020 = PLANE ( 'NONE',  #45951 ) ;
#65021 = DIRECTION ( 'NONE',  ( 1.000000000000000000, 4.163336342344333240E-14, 0.000000000000000000 ) ) ;
#65022 = DIRECTION ( 'NONE',  ( -0.9254794337955620787, -0.3787978585227822492, 0.000000000000000000 ) ) ;
#65023 = DIRECTION ( 'NONE',  ( 0.000000000000000000, -1.000000000000000000, 0.000000000000000000 ) ) ;
#65024 = AXIS2_PLACEMENT_3D ( 'NONE', #36871, #86369, #15993 ) ;
#65025 = EDGE_CURVE ( 'NONE', #64475, #79712, #5543, .T. ) ;
#65026 = VECTOR ( 'NONE', #57504, 999.9999999999998863 ) ;
#65027 = CARTESIAN_POINT ( 'NONE',  ( 116.8435662018513028, -36.99793375417353758, 39.80419670448193159 ) ) ;
#65028 = DIRECTION ( 'NONE',  ( 0.000000000000000000, 0.000000000000000000, 1.000000000000000000 ) ) ;
#65029 = ORIENTED_EDGE ( 'NONE', *, *, #44797, .T. ) ;
#65030 = CARTESIAN_POINT ( 'NONE',  ( 116.4265620360770725, -31.96216903954944399, 40.20133956162496958 ) ) ;
#65031 = DIRECTION ( 'NONE',  ( 1.000000000000000000, -0.000000000000000000, 2.108231265501709878E-16 ) ) ;
#65032 = EDGE_CURVE ( 'NONE', #26697, #36849, #88218, .T. ) ;
#65033 = CARTESIAN_POINT ( 'NONE',  ( 118.1032226039154267, -36.12160442421116358, 273.8822919425776945 ) ) ;
#65034 = VERTEX_POINT ( 'NONE', #81415 ) ;
#65035 = CARTESIAN_POINT ( 'NONE',  ( 82.73250004807569269, -18.03188439721439096, 2.979900720421670979 ) ) ;
#65036 = CARTESIAN_POINT ( 'NONE',  ( 98.54772661365011288, -41.97710352008375168, 17.76566672626352528 ) ) ;
#65037 = DIRECTION ( 'NONE',  ( -1.000000000000000078E-15, 1.000000000000000000, 0.000000000000000000 ) ) ;
#65038 = CARTESIAN_POINT ( 'NONE',  ( 108.2186271136511095, -28.64846388872622285, 102.7823760838769687 ) ) ;
#65039 = CARTESIAN_POINT ( 'NONE',  ( 109.6111442688334563, -26.56067652042401406, 195.8813395616249977 ) ) ;
#65040 = FACE_BOUND ( 'NONE', #9872, .T. ) ;
#65041 = PLANE ( 'NONE',  #7287 ) ;
#65042 = EDGE_LOOP ( 'NONE', ( #10850, #36360 ) ) ;
#65043 = VECTOR ( 'NONE', #76120, 1000.000000000000000 ) ;
#65044 = DIRECTION ( 'NONE',  ( 1.000000000000000000, 0.000000000000000000, 9.868649107779159826E-16 ) ) ;
#65045 = ORIENTED_EDGE ( 'NONE', *, *, #54686, .F. ) ;
#65046 = ORIENTED_EDGE ( 'NONE', *, *, #34286, .T. ) ;
#65047 = VECTOR ( 'NONE', #21537, 1000.000000000000000 ) ;
#65049 = EDGE_CURVE ( 'NONE', #44952, #51066, #62244, .T. ) ;
#65048 = VECTOR ( 'NONE', #85331, 1000.000000000000000 ) ;
#65050 = DIRECTION ( 'NONE',  ( -2.999999999999999839E-15, 1.000000000000000000, -2.999999999999999900E-30 ) ) ;
#65051 = ORIENTED_EDGE ( 'NONE', *, *, #84149, .T. ) ;
#65052 = ORIENTED_EDGE ( 'NONE', *, *, #23681, .F. ) ;
#65053 = DIRECTION ( 'NONE',  ( -1.000000000000000000, -8.163404592832032979E-16, 0.000000000000000000 ) ) ;
#65054 = CARTESIAN_POINT ( 'NONE',  ( 110.9595727330559072, -27.46627978870682441, 40.76010958015512387 ) ) ;
#65055 = CARTESIAN_POINT ( 'NONE',  ( 103.2375202873391800, -28.52263824056898756, 134.8343245899819465 ) ) ;
#65056 = CARTESIAN_POINT ( 'NONE',  ( 95.20615018136085439, -37.33485150947186781, 271.3670538473392639 ) ) ;
#65057 = AXIS2_PLACEMENT_3D ( 'NONE', #6809, #69044, #76304 ) ;
#65058 = CARTESIAN_POINT ( 'NONE',  ( -1.665555919329872792, 69.93248702128259708, 130.5479027315182066 ) ) ;
#65059 = ORIENTED_EDGE ( 'NONE', *, *, #48532, .T. ) ;
#65060 = CIRCLE ( 'NONE', #79539, 10.00000000000000711 ) ;
#65061 = EDGE_CURVE ( 'NONE', #69092, #49439, #5080, .T. ) ;
#65062 = CARTESIAN_POINT ( 'NONE',  ( 114.7429578716709386, -30.29548818356803608, 135.3815280204426017 ) ) ;
#65063 = ORIENTED_EDGE ( 'NONE', *, *, #79757, .F. ) ;
#65064 = LINE ( 'NONE', #70542, #39165 ) ;
#65065 = VECTOR ( 'NONE', #44946, 1000.000000000000000 ) ;
#65066 = LINE ( 'NONE', #85534, #24146 ) ;
#65067 = CARTESIAN_POINT ( 'NONE',  ( 98.04152589100374371, -41.04187113461722447, 131.6812034471568040 ) ) ;
#65068 = CARTESIAN_POINT ( 'NONE',  ( -13.86911000615384104, 238.5000000000000000, 102.9892450244911828 ) ) ;
#65069 = VERTEX_POINT ( 'NONE', #67754 ) ;
#65070 = CARTESIAN_POINT ( 'NONE',  ( 100.2471064434660093, -45.42859581790747825, 277.0594347997204636 ) ) ;
#65071 = CARTESIAN_POINT ( 'NONE',  ( 99.09426955137945470, -44.45222557475181446, 37.95086337114900488 ) ) ;
#65072 = CARTESIAN_POINT ( 'NONE',  ( 116.8171228667130634, -34.15291832109217296, 120.0314586092066520 ) ) ;
#65074 = CARTESIAN_POINT ( 'NONE',  ( 69.76189330943638822, -138.2438803413000130, 247.6262417895221120 ) ) ;
#65073 = CARTESIAN_POINT ( 'NONE',  ( -215.9000000000000057, 53.97500000000000142, 30.16249999999999787 ) ) ;
#65075 = LINE ( 'NONE', #68212, #81549 ) ;
#65076 = CYLINDRICAL_SURFACE ( 'NONE', #11875, 7.837499999999996803 ) ;
#65077 = CARTESIAN_POINT ( 'NONE',  ( 131.3780189692434703, -37.30949827216404913, 6.839365140900705242 ) ) ;
#65078 = CONICAL_SURFACE ( 'NONE', #54919, 25.39999999999999858, 0.7853981633974984611 ) ;
#65079 = DIRECTION ( 'NONE',  ( -0.7071067811865503483, -0.7071067811865445751, 0.000000000000000000 ) ) ;
#65080 = EDGE_CURVE ( 'NONE', #39780, #8105, #54093, .T. ) ;
#65081 = CARTESIAN_POINT ( 'NONE',  ( 100.8875763982592844, -44.70031131295115756, 162.0521131232090397 ) ) ;
#65082 = CARTESIAN_POINT ( 'NONE',  ( 134.0664832912739826, -8.729447159941003065, 4.925625275910997303 ) ) ;
#65083 = CARTESIAN_POINT ( 'NONE',  ( 131.0667039024480118, -61.87844715994100397, 228.3338068554150198 ) ) ;
#65084 = CARTESIAN_POINT ( 'NONE',  ( 109.2165397428488376, -48.40897078886088423, 277.7213395616254843 ) ) ;
#65085 = CARTESIAN_POINT ( 'NONE',  ( 96.04670619665022002, -35.87009084903410638, 187.2765776568629406 ) ) ;
#65086 = CARTESIAN_POINT ( 'NONE',  ( 117.9472974416529638, -41.48656121291797660, 54.49848241876792088 ) ) ;
#65088 = CARTESIAN_POINT ( 'NONE',  ( 75.31670390244798341, -67.87844715994100397, 60.91780685541480267 ) ) ;
#65087 = FACE_OUTER_BOUND ( 'NONE', #83095, .T. ) ;
#65089 = CARTESIAN_POINT ( 'NONE',  ( 82.51836309791163160, -35.48272428399237555, 2.716753546975698264 ) ) ;
#65090 = AXIS2_PLACEMENT_3D ( 'NONE', #7796, #69130, #33714 ) ;
#65091 = ORIENTED_EDGE ( 'NONE', *, *, #46823, .T. ) ;
#65092 = CARTESIAN_POINT ( 'NONE',  ( 177.0371591254545933, -48.62818131005479927, 129.9678068554150059 ) ) ;
#65093 = ORIENTED_EDGE ( 'NONE', *, *, #36985, .T. ) ;
#65094 = CARTESIAN_POINT ( 'NONE',  ( 97.00151786184787284, -41.45262973156711439, 57.67562527591096710 ) ) ;
#65095 = EDGE_CURVE ( 'NONE', #87937, #53694, #61377, .T. ) ;
#65097 = VERTEX_POINT ( 'NONE', #75015 ) ;
#65096 = CARTESIAN_POINT ( 'NONE',  ( 68.86456684384336313, 100.5999999999999659, 56.22171674193015889 ) ) ;
#65098 = FACE_OUTER_BOUND ( 'NONE', #88752, .T. ) ;
#65099 = CARTESIAN_POINT ( 'NONE',  ( 117.1759530674218865, -34.27439392744689428, 205.0156252759109634 ) ) ;
#65100 = LINE ( 'NONE', #64218, #419 ) ;
#65101 = CARTESIAN_POINT ( 'NONE',  ( 98.38057750414245106, -41.69554516216643947, 146.7398124929533196 ) ) ;
#65102 = EDGE_CURVE ( 'NONE', #32236, #34136, #23118, .T. ) ;
#65103 = DIRECTION ( 'NONE',  ( 0.7071067811865491270, -0.7071067811865459074, 7.071067811865492096E-16 ) ) ;
#65104 = CARTESIAN_POINT ( 'NONE',  ( 106.5667039024470313, -108.2470741265389620, -19.78219314458190681 ) ) ;
#65105 = CARTESIAN_POINT ( 'NONE',  ( -27.27158787008326968, 184.0000000000000000, 0.000000000000000000 ) ) ;
#65106 = CYLINDRICAL_SURFACE ( 'NONE', #51479, 4.750000000000000888 ) ;
#65107 = CARTESIAN_POINT ( 'NONE',  ( 97.25364341294451265, -36.87759583893578252, 136.3384824187689333 ) ) ;
#65108 = VERTEX_POINT ( 'NONE', #4633 ) ;
#65109 = ORIENTED_EDGE ( 'NONE', *, *, #81901, .F. ) ;
#65110 = CARTESIAN_POINT ( 'NONE',  ( 100.0889724914296863, -42.24093267880301994, 88.29015473446894191 ) ) ;
#65111 = VECTOR ( 'NONE', #61428, 1000.000000000000000 ) ;
#65112 = DIRECTION ( 'NONE',  ( 0.000000000000000000, 0.000000000000000000, -1.000000000000000000 ) ) ;
#65114 = CARTESIAN_POINT ( 'NONE',  ( -446.0240000000000009, 14.28750000000026077, 11.11249999999970051 ) ) ;
#65113 = CARTESIAN_POINT ( 'NONE',  ( 97.40895461294502411, -34.98419235835276453, 237.1841967044819626 ) ) ;
#65115 = CARTESIAN_POINT ( 'NONE',  ( 182.3467384525658019, -29.62846900981657683, 117.4678068554150627 ) ) ;
#65116 = DIRECTION ( 'NONE',  ( -0.02150753337723538411, -0.0009076677972193728959, -0.9997682742251812194 ) ) ;
#65117 = CARTESIAN_POINT ( 'NONE',  ( 118.1052048222230724, 75.15251084995277608, -10.33146714902655816 ) ) ;
#65118 = VECTOR ( 'NONE', #46347, 1000.000000000000000 ) ;
#65119 = CARTESIAN_POINT ( 'NONE',  ( 1.796236281188243881E-22, 69.84999999999999432, 118.5560000000000116 ) ) ;
#65120 = DIRECTION ( 'NONE',  ( 9.000537910253610245E-13, -1.000000000000000000, 9.010537910253610534E-28 ) ) ;
#65121 = CARTESIAN_POINT ( 'NONE',  ( 0.000000000000000000, 127.0000000000000000, -188.9759999999999991 ) ) ;
#65122 = CARTESIAN_POINT ( 'NONE',  ( 95.59354794629800267, -39.59649474372138656, 166.5213395616259788 ) ) ;
#65123 = VERTEX_POINT ( 'NONE', #80499 ) ;
#65124 = ORIENTED_EDGE ( 'NONE', *, *, #79652, .T. ) ;
#65125 = AXIS2_PLACEMENT_3D ( 'NONE', #19640, #40531, #11941 ) ;
#65126 = CARTESIAN_POINT ( 'NONE',  ( 89.65393875053220540, -82.56959722164945958, 250.2201230397200220 ) ) ;
#65127 = LINE ( 'NONE', #45540, #78106 ) ;
#65128 = AXIS2_PLACEMENT_3D ( 'NONE', #77941, #21639, #15712 ) ;
#65129 = DIRECTION ( 'NONE',  ( 0.000000000000000000, 0.000000000000000000, -1.000000000000000000 ) ) ;
#65130 = FACE_OUTER_BOUND ( 'NONE', #14430, .T. ) ;
#65131 = CARTESIAN_POINT ( 'NONE',  ( 98.50976710839005079, -35.43193677023271704, 219.0128522743539747 ) ) ;
#65132 = LINE ( 'NONE', #2916, #85789 ) ;
#65133 = ADVANCED_FACE ( 'NONE', ( #52736 ), #12806, .F. ) ;
#65134 = CARTESIAN_POINT ( 'NONE',  ( 104.4536708109005332, -26.63686367483539996, 200.2784824187679362 ) ) ;
#65135 = CARTESIAN_POINT ( 'NONE',  ( 25.56670390244797275, -62.87844715994099687, 257.2178068554150059 ) ) ;
#65136 = ORIENTED_EDGE ( 'NONE', *, *, #17692, .F. ) ;
#65138 = VERTEX_POINT ( 'NONE', #40932 ) ;
#65137 = ORIENTED_EDGE ( 'NONE', *, *, #4784, .T. ) ;
#65139 = AXIS2_PLACEMENT_3D ( 'NONE', #29991, #57680, #85423 ) ;
#65140 = LINE ( 'NONE', #2923, #76660 ) ;
#65141 = DIRECTION ( 'NONE',  ( 0.000000000000000000, 1.000000000000000000, 0.000000000000000000 ) ) ;
#65142 = CARTESIAN_POINT ( 'NONE',  ( 131.5441285970327101, -35.63380991826300459, 7.053480412778572628 ) ) ;
#65143 = CARTESIAN_POINT ( 'NONE',  ( 109.5858817268311611, -44.49374890974875285, 10.64523322673399619 ) ) ;
#65144 = DIRECTION ( 'NONE',  ( -4.237773401492740281E-14, 1.000000000000000000, 0.000000000000000000 ) ) ;
#65145 = ORIENTED_EDGE ( 'NONE', *, *, #89908, .T. ) ;
#65146 = CARTESIAN_POINT ( 'NONE',  ( 116.7802871385218282, -39.10473973501323286, 9.635625275910941312 ) ) ;
#65147 = VECTOR ( 'NONE', #60631, 1000.000000000000000 ) ;
#65148 = DIRECTION ( 'NONE',  ( -0.7967329428042217998, 0.6043315462976631691, -1.875669758399923617E-14 ) ) ;
#65149 = ORIENTED_EDGE ( 'NONE', *, *, #21146, .F. ) ;
#65150 = ORIENTED_EDGE ( 'NONE', *, *, #59086, .F. ) ;
#65151 = ADVANCED_FACE ( 'NONE', ( #20059 ), #18256, .F. ) ;
#65152 = CARTESIAN_POINT ( 'NONE',  ( 116.9914377788273327, -35.36134890089079619, 113.9354139663191177 ) ) ;
#65153 = ORIENTED_EDGE ( 'NONE', *, *, #60546, .F. ) ;
#65154 = ORIENTED_EDGE ( 'NONE', *, *, #11365, .F. ) ;
#65155 = CARTESIAN_POINT ( 'NONE',  ( 103.5342718762226895, -27.68543744656516026, 19.79527697093397265 ) ) ;
#65156 = EDGE_CURVE ( 'NONE', #51214, #21223, #7327, .T. ) ;
#65157 = CARTESIAN_POINT ( 'NONE',  ( 114.4785830672529130, -28.49803820358978612, 159.5051490854349652 ) ) ;
#65158 = CARTESIAN_POINT ( 'NONE',  ( 97.63679352021414104, -31.00714225716590278, 125.8803871806719599 ) ) ;
#65159 = CARTESIAN_POINT ( 'NONE',  ( 194.0371591254585155, -46.82818131005407736, 129.9678068554150343 ) ) ;
#65160 = CARTESIAN_POINT ( 'NONE',  ( 100.2482148738244661, -28.84314871041893014, 256.6441967044821695 ) ) ;
#65161 = CARTESIAN_POINT ( 'NONE',  ( 135.2444258376730204, 101.5999999999999943, -147.4575741623271767 ) ) ;
#65162 = CARTESIAN_POINT ( 'NONE',  ( 84.13799348605135719, -119.9310939662431537, 250.2190963482990185 ) ) ;
#65163 = CARTESIAN_POINT ( 'NONE',  ( -130.2063869749194964, 74.16976894168006140, 9.551794474071689578 ) ) ;
#65165 = ORIENTED_EDGE ( 'NONE', *, *, #14117, .F. ) ;
#65164 = ADVANCED_FACE ( 'NONE', ( #62726 ), #21407, .T. ) ;
#65166 = VECTOR ( 'NONE', #42058, 1000.000000000000000 ) ;
#65167 = EDGE_CURVE ( 'NONE', #37741, #75634, #22305, .T. ) ;
#65168 = VERTEX_POINT ( 'NONE', #55440 ) ;
#65169 = EDGE_CURVE ( 'NONE', #27939, #65845, #63749, .T. ) ;
#65170 = VECTOR ( 'NONE', #4447, 1000.000000000000000 ) ;
#65171 = VECTOR ( 'NONE', #39089, 1000.000000000000000 ) ;
#65172 = CARTESIAN_POINT ( 'NONE',  ( 99.97821182074206092, -27.16988623491039334, 185.5841967044829630 ) ) ;
#65173 = ORIENTED_EDGE ( 'NONE', *, *, #83539, .T. ) ;
#65174 = CARTESIAN_POINT ( 'NONE',  ( 98.85647153018690858, -30.30415715074617111, 155.7984824187679465 ) ) ;
#65175 = LINE ( 'NONE', #86081, #15227 ) ;
#65176 = EDGE_CURVE ( 'NONE', #36821, #11860, #69551, .T. ) ;
#65177 = DIRECTION ( 'NONE',  ( 1.000000000000000000, 3.999999999999999995E-14, 1.000000000000000078E-15 ) ) ;
#65178 = DIRECTION ( 'NONE',  ( 1.000000000000000078E-15, 0.000000000000000000, 1.000000000000000000 ) ) ;
#65181 = CARTESIAN_POINT ( 'NONE',  ( 105.8960369669305948, -47.10223136823062617, 278.4870538473395527 ) ) ;
#65180 = CARTESIAN_POINT ( 'NONE',  ( 0.000000000000000000, 2.031999999999865025, 0.000000000000000000 ) ) ;
#65179 = FACE_OUTER_BOUND ( 'NONE', #32665, .T. ) ;
#65182 = CARTESIAN_POINT ( 'NONE',  ( -72.96458098368600531, 127.0000000000000000, -80.10833098368780725 ) ) ;
#65183 = CARTESIAN_POINT ( 'NONE',  ( 179.1667039024474661, -26.71338133338671739, 237.4678068554150059 ) ) ;
#65184 = ADVANCED_BREP_SHAPE_REPRESENTATION ( '', ( #50041, #50656 ), #34903 ) ;
#65185 = DIRECTION ( 'NONE',  ( 1.000000000000000000, -9.073094938289460781E-13, 0.000000000000000000 ) ) ;
#65186 = AXIS2_PLACEMENT_3D ( 'NONE', #89513, #82262, #26817 ) ;
#65187 = DIRECTION ( 'NONE',  ( 0.000000000000000000, -0.000000000000000000, 1.000000000000000000 ) ) ;
#65188 =( GEOMETRIC_REPRESENTATION_CONTEXT ( 3 ) GLOBAL_UNCERTAINTY_ASSIGNED_CONTEXT ( ( #35109 ) ) GLOBAL_UNIT_ASSIGNED_CONTEXT ( ( #20515, #76361, #55885 ) ) REPRESENTATION_CONTEXT ( 'NONE', 'WORKASPACE' ) );
#65189 = CARTESIAN_POINT ( 'NONE',  ( 99.04406187972965370, -42.84125766729550833, 257.8439586119762339 ) ) ;
#65190 = EDGE_CURVE ( 'NONE', #8827, #46455, #7209, .T. ) ;
#65191 = FACE_OUTER_BOUND ( 'NONE', #80077, .T. ) ;
#65193 = ORIENTED_EDGE ( 'NONE', *, *, #50273, .F. ) ;
#65192 = CARTESIAN_POINT ( 'NONE',  ( 106.2659377814683808, -44.71837661912690010, 195.5838068554170093 ) ) ;
#65194 = LINE ( 'NONE', #11107, #62566 ) ;
#65195 = CARTESIAN_POINT ( 'NONE',  ( 116.3972416472496434, -41.42873566659991269, 203.4556252759109611 ) ) ;
#65196 = CARTESIAN_POINT ( 'NONE',  ( 96.71481148478426348, -38.23418088628295664, 62.44133956162495025 ) ) ;
#65197 = CARTESIAN_POINT ( 'NONE',  ( 118.9266961287330560, -37.70231105260669580, 184.7613395616249647 ) ) ;
#65198 = CYLINDRICAL_SURFACE ( 'NONE', #41616, 4.762500000000000178 ) ;
#65199 = VECTOR ( 'NONE', #13799, 1000.000000000000000 ) ;
#65200 = CARTESIAN_POINT ( 'NONE',  ( 107.0664832912739968, -36.72944715994100306, 311.6356252759112522 ) ) ;
#65202 = CARTESIAN_POINT ( 'NONE',  ( 116.4174193679775300, -33.16718996298826738, 40.11587310748063118 ) ) ;
#65201 = CARTESIAN_POINT ( 'NONE',  ( 167.7413838386817133, -48.33240602328261559, 300.4678068554149490 ) ) ;
#65203 = CARTESIAN_POINT ( 'NONE',  ( -44.45000000000000284, 50.79999999999999716, 275.4630000000000223 ) ) ;
#65204 = CARTESIAN_POINT ( 'NONE',  ( 27.27158787008328389, 127.0000000000000000, 111.9860621927989683 ) ) ;
#65205 = ORIENTED_EDGE ( 'NONE', *, *, #89227, .T. ) ;
#65206 = DIRECTION ( 'NONE',  ( 1.000000000000000000, 0.000000000000000000, 0.000000000000000000 ) ) ;
#65207 = ORIENTED_EDGE ( 'NONE', *, *, #70625, .T. ) ;
#65208 = ORIENTED_EDGE ( 'NONE', *, *, #70026, .F. ) ;
#65209 = CIRCLE ( 'NONE', #47800, 16.09746158385918946 ) ;
#65210 = CARTESIAN_POINT ( 'NONE',  ( 112.7653361951733473, -30.36711996764882571, 113.9181341137909556 ) ) ;
#65211 = ADVANCED_FACE ( 'NONE', ( #57 ), #503, .T. ) ;
#65213 = ORIENTED_EDGE ( 'NONE', *, *, #69619, .F. ) ;
#65212 = CARTESIAN_POINT ( 'NONE',  ( -9.549815870737166534, 90.93248498521381862, -130.2065322450556550 ) ) ;
#65214 = CARTESIAN_POINT ( 'NONE',  ( 97.56228874418796693, -32.49873190831186776, 96.99276813305395706 ) ) ;
#65215 = DIRECTION ( 'NONE',  ( 1.000000000000000078E-15, 0.000000000000000000, 1.000000000000000000 ) ) ;
#65216 = EDGE_CURVE ( 'NONE', #11190, #79263, #28936, .T. ) ;
#65217 = EDGE_CURVE ( 'NONE', #81504, #10881, #76811, .T. ) ;
#65218 = CARTESIAN_POINT ( 'NONE',  ( 77.85525873416526110, -17.08426237657415570, 7.378668740738687504 ) ) ;
#65219 = CARTESIAN_POINT ( 'NONE',  ( 147.0667039024470171, -79.67844715994090166, 222.2178068554179902 ) ) ;
#65220 = ADVANCED_FACE ( 'NONE', ( #27310 ), #75915, .F. ) ;
#65221 = CARTESIAN_POINT ( 'NONE',  ( 115.3461623907574563, -31.52268719801062957, 34.27276813305396530 ) ) ;
#65222 = EDGE_LOOP ( 'NONE', ( #74311, #71867, #21, #67751 ) ) ;
#65223 = CONICAL_SURFACE ( 'NONE', #46317, 16.25000000000000000, 0.5235987755982992597 ) ;
#65224 = ORIENTED_EDGE ( 'NONE', *, *, #15384, .F. ) ;
#65225 = VERTEX_POINT ( 'NONE', #14594 ) ;
#65226 = CARTESIAN_POINT ( 'NONE',  ( 179.1667039024460166, -28.27351298637280408, 117.4678068554150627 ) ) ;
#65227 = DIRECTION ( 'NONE',  ( 1.000000000000000000, 8.673617379883546378E-16, 9.757819552368989676E-16 ) ) ;
#65228 = DIRECTION ( 'NONE',  ( 0.000000000000000000, 0.000000000000000000, -1.000000000000000000 ) ) ;
#65229 = CYLINDRICAL_SURFACE ( 'NONE', #33934, 3.250000000000002665 ) ;
#65230 = CARTESIAN_POINT ( 'NONE',  ( 183.5150000000000148, 68.61249999999999716, -53.61543552338530105 ) ) ;
#65231 = CARTESIAN_POINT ( 'NONE',  ( 113.2462210345366316, -28.75922547209470181, 50.55319279321858517 ) ) ;
#65232 = LINE ( 'NONE', #45642, #80844 ) ;
#65233 = CIRCLE ( 'NONE', #5779, 10.04999999999999361 ) ;
#65234 = CARTESIAN_POINT ( 'NONE',  ( -10.55958528308446986, 89.60586021078158581, 130.1282609435105826 ) ) ;
#65235 = CARTESIAN_POINT ( 'NONE',  ( 110.3650187231686743, -47.25482062520524096, 52.80610146638697699 ) ) ;
#65236 = ORIENTED_EDGE ( 'NONE', *, *, #38605, .F. ) ;
#65237 = CIRCLE ( 'NONE', #46398, 7.143750000000004263 ) ;
#65238 = CARTESIAN_POINT ( 'NONE',  ( 6.710386649963810513, 93.34051461951031570, 130.3838978039176482 ) ) ;
#65239 = DIRECTION ( 'NONE',  ( 0.000000000000000000, 1.000000000000000000, 0.000000000000000000 ) ) ;
#65240 = CARTESIAN_POINT ( 'NONE',  ( 183.5150000000000148, 36.86249999999999716, -53.61543552338530105 ) ) ;
#65241 = CARTESIAN_POINT ( 'NONE',  ( 100.3248355287147291, -41.38056247698398238, 124.6252332267339682 ) ) ;
#65242 = AXIS2_PLACEMENT_3D ( 'NONE', #2178, #1732, #29433 ) ;
#65243 = VECTOR ( 'NONE', #79240, 1000.000000000000114 ) ;
#65244 = LINE ( 'NONE', #44786, #74579 ) ;
#65245 = LINE ( 'NONE', #77538, #11158 ) ;
#65246 = VERTEX_POINT ( 'NONE', #956 ) ;
#65247 = VERTEX_POINT ( 'NONE', #89551 ) ;
#65248 = VECTOR ( 'NONE', #35721, 1000.000000000000000 ) ;
#65249 = CARTESIAN_POINT ( 'NONE',  ( 107.0667039024470313, -104.2784471599409528, 45.21780685541799727 ) ) ;
#65250 = ORIENTED_EDGE ( 'NONE', *, *, #61988, .F. ) ;
#65251 = ORIENTED_EDGE ( 'NONE', *, *, #68840, .F. ) ;
#65252 = MECHANICAL_DESIGN_GEOMETRIC_PRESENTATION_REPRESENTATION (  '', ( #11570 ), #65188 ) ;
#65253 = CARTESIAN_POINT ( 'NONE',  ( 97.70553735687687436, -35.92370728225471055, 182.6777737820879679 ) ) ;
#65254 = FACE_OUTER_BOUND ( 'NONE', #19540, .T. ) ;
#65255 = CARTESIAN_POINT ( 'NONE',  ( 114.7874576214283167, -44.67122033332078246, 114.2022919425779719 ) ) ;
#65256 = DIRECTION ( 'NONE',  ( 0.000000000000000000, 0.000000000000000000, -1.000000000000000000 ) ) ;
#65257 = CARTESIAN_POINT ( 'NONE',  ( 97.82725377794338328, -40.55524675897819975, 16.63888027222046873 ) ) ;
#65258 = ORIENTED_EDGE ( 'NONE', *, *, #119, .T. ) ;
#65259 = VERTEX_POINT ( 'NONE', #42271 ) ;
#65260 = ORIENTED_EDGE ( 'NONE', *, *, #3570, .F. ) ;
#65261 = ADVANCED_FACE ( 'NONE', ( #69999 ), #35459, .F. ) ;
#65262 = AXIS2_PLACEMENT_3D ( 'NONE', #156, #55088, #20165 ) ;
#65263 = CARTESIAN_POINT ( 'NONE',  ( 100.3885320853208896, -32.03533449533603772, 203.6566617981629577 ) ) ;
#65264 = EDGE_CURVE ( 'NONE', #74158, #88283, #84089, .T. ) ;
#65265 = CARTESIAN_POINT ( 'NONE',  ( 96.93519779220999055, -32.25144590123284161, 55.98324432352897162 ) ) ;
#65266 = ORIENTED_EDGE ( 'NONE', *, *, #24809, .F. ) ;
#65267 = CARTESIAN_POINT ( 'NONE',  ( 100.4250012405661039, -28.72198927997973783, 40.62705384733894221 ) ) ;
#65268 = CARTESIAN_POINT ( 'NONE',  ( 41.56648329127399677, -9.303447159940999356, 198.9256252759119832 ) ) ;
#65269 = FACE_BOUND ( 'NONE', #88038, .T. ) ;
#65270 = FACE_OUTER_BOUND ( 'NONE', #39138, .T. ) ;
#65271 = CARTESIAN_POINT ( 'NONE',  ( 101.7695353289030322, -45.70857994070590991, 158.1527681330539963 ) ) ;
#65272 = FACE_OUTER_BOUND ( 'NONE', #36299, .T. ) ;
#65273 = VERTEX_POINT ( 'NONE', #49531 ) ;
#65274 = CARTESIAN_POINT ( 'NONE',  ( 177.0371591254543375, -48.62818131005480637, 300.4678068554149490 ) ) ;
#65275 = EDGE_CURVE ( 'NONE', #15124, #66455, #5635, .T. ) ;
#65276 = EDGE_CURVE ( 'NONE', #52666, #397, #21681, .T. ) ;
#65277 = EDGE_LOOP ( 'NONE', ( #47039, #40478, #56991, #57952 ) ) ;
#65278 = FACE_OUTER_BOUND ( 'NONE', #24228, .T. ) ;
#65279 = FACE_OUTER_BOUND ( 'NONE', #43419, .T. ) ;
#65281 = ORIENTED_EDGE ( 'NONE', *, *, #56333, .F. ) ;
#65280 = AXIS2_PLACEMENT_3D ( 'NONE', #28128, #40866, #7702 ) ;
#65282 = EDGE_CURVE ( 'NONE', #80581, #53161, #70909, .T. ) ;
#65283 = CARTESIAN_POINT ( 'NONE',  ( 41.56648329127398966, -27.57844715994070484, 318.9256252759120116 ) ) ;
#65284 = FACE_OUTER_BOUND ( 'NONE', #65351, .T. ) ;
#65285 = CARTESIAN_POINT ( 'NONE',  ( 96.71459513300293054, -38.23421233548538112, 66.44133956162495735 ) ) ;
#65286 = DIRECTION ( 'NONE',  ( -1.424786214935630051E-15, 0.000000000000000000, 1.000000000000000000 ) ) ;
#65287 = EDGE_CURVE ( 'NONE', #4960, #27387, #86960, .T. ) ;
#65288 = FACE_OUTER_BOUND ( 'NONE', #36662, .T. ) ;
#65289 = DIRECTION ( 'NONE',  ( 0.000000000000000000, 0.000000000000000000, -1.000000000000000000 ) ) ;
#65290 = CARTESIAN_POINT ( 'NONE',  ( 110.3395589168170972, -45.98151452052003663, 37.84705384733994293 ) ) ;
#65292 = CARTESIAN_POINT ( 'NONE',  ( 117.1049515565468226, -33.87427183379793405, 145.0470538473399529 ) ) ;
#65291 = CARTESIAN_POINT ( 'NONE',  ( 142.8698897858160706, -0.9167816978817300289, 394.9756252759102040 ) ) ;
#65293 = DIRECTION ( 'NONE',  ( 0.000000000000000000, -1.000000000000000000, 0.000000000000000000 ) ) ;
#65294 = DIRECTION ( 'NONE',  ( 1.000000000000000078E-15, -1.000000000000000083E-30, -1.000000000000000000 ) ) ;
#65295 = ORIENTED_EDGE ( 'NONE', *, *, #25713, .F. ) ;
#65296 = DIRECTION ( 'NONE',  ( 1.000000000000000000, 0.000000000000000000, 0.000000000000000000 ) ) ;
#65297 = AXIS2_PLACEMENT_3D ( 'NONE', #78099, #15865, #38082 ) ;
#65298 = FACE_OUTER_BOUND ( 'NONE', #55232, .T. ) ;
#65299 = DIRECTION ( 'NONE',  ( 0.000000000000000000, 0.000000000000000000, -1.000000000000000000 ) ) ;
#65300 = EDGE_CURVE ( 'NONE', #837, #69025, #1379, .T. ) ;
#65301 = AXIS2_PLACEMENT_3D ( 'NONE', #31894, #16943, #85555 ) ;
#65302 = CARTESIAN_POINT ( 'NONE',  ( -72.96458098368751166, 127.0000000000000000, 72.96458098368620426 ) ) ;
#65304 = ORIENTED_EDGE ( 'NONE', *, *, #70425, .T. ) ;
#65303 = CARTESIAN_POINT ( 'NONE',  ( 114.1546619933443480, -29.02461823700197741, 199.4841967044819739 ) ) ;
#65305 = CYLINDRICAL_SURFACE ( 'NONE', #1656, 13.99999999999999822 ) ;
#65306 = CARTESIAN_POINT ( 'NONE',  ( 96.74182981399745529, -35.13608925046722220, 262.2041967044821149 ) ) ;
#65307 = CARTESIAN_POINT ( 'NONE',  ( 110.1708544452211100, -46.72723989065711692, 93.81562527591097478 ) ) ;
#65308 = CARTESIAN_POINT ( 'NONE',  ( 99.09685934341746361, -30.54889812966678164, 251.8073641162624199 ) ) ;
#65309 = DIRECTION ( 'NONE',  ( 0.000000000000000000, 0.000000000000000000, 1.000000000000000000 ) ) ;
#65310 = CARTESIAN_POINT ( 'NONE',  ( 0.000000000000000000, 0.000000000000000000, 0.000000000000000000 ) ) ;
#65311 = DIRECTION ( 'NONE',  ( -1.000000000000000000, 0.000000000000000000, 0.000000000000000000 ) ) ;
#65312 = VERTEX_POINT ( 'NONE', #30012 ) ;
#65313 = ORIENTED_EDGE ( 'NONE', *, *, #57164, .F. ) ;
#65314 = ORIENTED_EDGE ( 'NONE', *, *, #84610, .F. ) ;
#65315 = VECTOR ( 'NONE', #59985, 1000.000000000000000 ) ;
#65316 = ORIENTED_EDGE ( 'NONE', *, *, #4550, .T. ) ;
#65317 = DIRECTION ( 'NONE',  ( 0.000000000000000000, 0.000000000000000000, 1.000000000000000000 ) ) ;
#65318 = CARTESIAN_POINT ( 'NONE',  ( 96.56373827543593791, -40.17738982329606046, 282.5908633711490552 ) ) ;
#65319 = FACE_OUTER_BOUND ( 'NONE', #4669, .T. ) ;
#65320 = CARTESIAN_POINT ( 'NONE',  ( -75.61066417432020614, 20.32000000000000028, 177.0380000000000109 ) ) ;
#65321 = VERTEX_POINT ( 'NONE', #53743 ) ;
#65322 = EDGE_CURVE ( 'NONE', #8105, #74330, #60812, .T. ) ;
#65325 = EDGE_CURVE ( 'NONE', #45090, #85483, #57705, .T. ) ;
#65324 = CARTESIAN_POINT ( 'NONE',  ( 91.51265874544223777, 76.91656954603719498, 75.37281393334542656 ) ) ;
#65323 = LINE ( 'NONE', #37624, #36628 ) ;
#65326 = LINE ( 'NONE', #3102, #24033 ) ;
#65327 = CARTESIAN_POINT ( 'NONE',  ( 98.55184737119530780, -35.75319039346454986, 205.6581341137909646 ) ) ;
#65328 = EDGE_LOOP ( 'NONE', ( #78366, #23175, #57508, #15647 ) ) ;
#65329 = ORIENTED_EDGE ( 'NONE', *, *, #42602, .T. ) ;
#65330 = ORIENTED_EDGE ( 'NONE', *, *, #4655, .F. ) ;
#65331 = LINE ( 'NONE', #24448, #7933 ) ;
#65332 = CARTESIAN_POINT ( 'NONE',  ( 97.81168844167092402, -40.51740470302234343, 181.6357138554620576 ) ) ;
#65333 = CARTESIAN_POINT ( 'NONE',  ( 104.9788083641148972, -27.14010996210895499, 256.2470538473390889 ) ) ;
#65334 = CIRCLE ( 'NONE', #58130, 4.874999999999990230 ) ;
#65335 = FACE_OUTER_BOUND ( 'NONE', #48079, .T. ) ;
#65336 = CARTESIAN_POINT ( 'NONE',  ( -68.91674821478457602, 82.54999999999999716, 68.91674821478434865 ) ) ;
#65337 = DIRECTION ( 'NONE',  ( -0.000000000000000000, -0.000000000000000000, -1.000000000000000000 ) ) ;
#65338 = VERTEX_POINT ( 'NONE', #65848 ) ;
#65339 = CARTESIAN_POINT ( 'NONE',  ( 103.2765498915109248, -27.47545316653152625, 56.38579426906439807 ) ) ;
#65340 = VERTEX_POINT ( 'NONE', #85448 ) ;
#65341 = AXIS2_PLACEMENT_3D ( 'NONE', #64905, #30387, #56736 ) ;
#65342 = CARTESIAN_POINT ( 'NONE',  ( 59.68306514483415270, -72.55903866283681225, 540.9756252759101471 ) ) ;
#65343 = CARTESIAN_POINT ( 'NONE',  ( 110.4041361119612930, -44.93847832680074106, 279.3158690201827881 ) ) ;
#65344 =( BOUNDED_CURVE ( )  B_SPLINE_CURVE ( 2, ( #37474, #42925, #8894 ),
 .UNSPECIFIED., .F., .F. ) 
 B_SPLINE_CURVE_WITH_KNOTS ( ( 3, 3 ),
 ( 0.01169420784673960018, 0.5170228498526590055 ),
 .UNSPECIFIED. ) 
 CURVE ( )  GEOMETRIC_REPRESENTATION_ITEM ( )  RATIONAL_B_SPLINE_CURVE ( ( 1.000420656333759872, 1.009299002520659849, 1.000000000000000000 ) ) 
 REPRESENTATION_ITEM ( '' )  );
#65345 = CYLINDRICAL_SURFACE ( 'NONE', #24694, 2.517499999999998739 ) ;
#65346 = CARTESIAN_POINT ( 'NONE',  ( 33.81648329127298780, 12.92155284005802862, 355.9756252759109998 ) ) ;
#65347 = CARTESIAN_POINT ( 'NONE',  ( 179.8585841295800094, -30.08671355700241179, -5.074374724088000832 ) ) ;
#65348 = ORIENTED_EDGE ( 'NONE', *, *, #55118, .T. ) ;
#65349 = DIRECTION ( 'NONE',  ( 0.000000000000000000, -1.000000000000000000, 0.000000000000000000 ) ) ;
#65350 = DIRECTION ( 'NONE',  ( -4.093947403305260305E-16, 1.000000000000000000, -6.162975822039159109E-32 ) ) ;
#65351 = EDGE_LOOP ( 'NONE', ( #84843, #42645, #33911, #58194, #55492, #69447, #50220, #36082, #53679, #36124, #55923, #71188 ) ) ;
#65352 = CARTESIAN_POINT ( 'NONE',  ( 118.0022803299065686, -38.33799637688264994, 73.72229194257801055 ) ) ;
#65353 = EDGE_LOOP ( 'NONE', ( #17715, #11471 ) ) ;
#65354 = CARTESIAN_POINT ( 'NONE',  ( 102.0478764085966361, -45.04113848309104640, 51.56670554236298187 ) ) ;
#65355 = AXIS2_PLACEMENT_3D ( 'NONE', #78191, #31345, #59037 ) ;
#65356 = DIRECTION ( 'NONE',  ( 2.056463827196271584E-15, -0.8571673007021100021, 0.5150380749100580413 ) ) ;
#65357 = CARTESIAN_POINT ( 'NONE',  ( 107.7480938161759951, -27.89408153625565845, 66.44729759161194238 ) ) ;
#65358 = CARTESIAN_POINT ( 'NONE',  ( 97.81168843500762478, -40.51741166756562507, 12.63579318495451176 ) ) ;
#65359 = CARTESIAN_POINT ( 'NONE',  ( 94.87702571208245672, -114.7407331754002229, -21.02845593540777003 ) ) ;
#65360 = DIRECTION ( 'NONE',  ( 1.000000000000000078E-15, -1.000000000000000000, 0.000000000000000000 ) ) ;
#65361 = EDGE_CURVE ( 'NONE', #62172, #64372, #57965, .T. ) ;
#65362 = CARTESIAN_POINT ( 'NONE',  ( 115.6911227382933873, -43.67932486773085543, 39.27467289495895386 ) ) ;
#65363 = CIRCLE ( 'NONE', #55151, 2.517499999999998739 ) ;
#65364 = LINE ( 'NONE', #11281, #51215 ) ;
#65365 = ORIENTED_EDGE ( 'NONE', *, *, #15525, .F. ) ;
#65366 = LINE ( 'NONE', #33522, #48746 ) ;
#65367 = EDGE_LOOP ( 'NONE', ( #85181, #76317 ) ) ;
#65368 = CARTESIAN_POINT ( 'NONE',  ( 97.94860405783340696, -41.87310908463563663, 132.7356252759109623 ) ) ;
#65369 = CARTESIAN_POINT ( 'NONE',  ( 79.18623681047911589, -21.33528726900534522, 1.744847506584294106 ) ) ;
#65370 = ORIENTED_EDGE ( 'NONE', *, *, #85922, .T. ) ;
#65372 = EDGE_CURVE ( 'NONE', #73425, #64021, #30457, .T. ) ;
#65371 = ORIENTED_EDGE ( 'NONE', *, *, #84347, .F. ) ;
#65373 = EDGE_CURVE ( 'NONE', #21680, #68103, #81560, .T. ) ;
#65374 = VECTOR ( 'NONE', #80362, 1000.000000000000000 ) ;
#65375 = CYLINDRICAL_SURFACE ( 'NONE', #28955, 2.117000000000000881 ) ;
#65376 = EDGE_CURVE ( 'NONE', #43971, #72757, #23223, .T. ) ;
#65377 = CARTESIAN_POINT ( 'NONE',  ( -479.3614999999999782, 6.038608028953049711, 90.48749999999999716 ) ) ;
#65378 = CARTESIAN_POINT ( 'NONE',  ( 106.3491918589965763, -46.48387837312656501, 222.5184824187689401 ) ) ;
#65379 = CARTESIAN_POINT ( 'NONE',  ( 72.96458098368650269, 127.0000000000000000, 72.96458098368729850 ) ) ;
#65380 = CARTESIAN_POINT ( 'NONE',  ( 75.31670390244798341, -57.40094715994099772, 86.31780685541500020 ) ) ;
#65381 = FACE_OUTER_BOUND ( 'NONE', #78859, .T. ) ;
#65382 = CARTESIAN_POINT ( 'NONE',  ( 117.2667774650794428, -38.88269731149204489, 59.66133956162595098 ) ) ;
#65383 = DIRECTION ( 'NONE',  ( 0.000000000000000000, 0.000000000000000000, -1.000000000000000000 ) ) ;
#65384 = ORIENTED_EDGE ( 'NONE', *, *, #51235, .T. ) ;
#65385 = CARTESIAN_POINT ( 'NONE',  ( 111.0446433595016913, -27.50350014455446868, 170.7527502710815952 ) ) ;
#65386 = EDGE_CURVE ( 'NONE', #2920, #11510, #50889, .T. ) ;
#65387 = CARTESIAN_POINT ( 'NONE',  ( -479.3614999999999782, 3.174999999999999822, 101.5999999999999943 ) ) ;
#65388 = EDGE_LOOP ( 'NONE', ( #38422, #68068, #37999, #28200 ) ) ;
#65389 = EDGE_CURVE ( 'NONE', #69283, #16139, #86764, .T. ) ;
#65390 = LINE ( 'NONE', #59886, #45972 ) ;
#65391 = DIRECTION ( 'NONE',  ( 3.100000000000000258E-29, -3.100000000000000044E-14, -1.000000000000000000 ) ) ;
#65392 = CARTESIAN_POINT ( 'NONE',  ( 116.8642987764957297, -41.79567201640977459, 243.4346728949589647 ) ) ;
#65393 = DIRECTION ( 'NONE',  ( 8.881784197001248379E-16, 0.000000000000000000, 1.000000000000000000 ) ) ;
#65394 = FACE_BOUND ( 'NONE', #21910, .T. ) ;
#65395 = CARTESIAN_POINT ( 'NONE',  ( 135.0664832912729878, -36.72944715994189835, 361.9756252759109998 ) ) ;
#65396 = EDGE_CURVE ( 'NONE', #66271, #84986, #71020, .T. ) ;
#65397 = AXIS2_PLACEMENT_3D ( 'NONE', #35531, #568, #21023 ) ;
#65398 = CARTESIAN_POINT ( 'NONE',  ( 114.2672205647202048, -43.24251175450689288, 232.6638483995059801 ) ) ;
#65400 = CARTESIAN_POINT ( 'NONE',  ( 112.7298150101557610, -27.26422151970083263, 50.65943479972101215 ) ) ;
#65399 = DIRECTION ( 'NONE',  ( -0.3818493186865920541, 0.9242245927363033076, 0.000000000000000000 ) ) ;
#65401 = CARTESIAN_POINT ( 'NONE',  ( 111.7869510898867276, 66.18006229446802990, 67.44307826104233072 ) ) ;
#65402 = CARTESIAN_POINT ( 'NONE',  ( 97.57695254711111943, -30.97082841205668657, 125.8803871806719599 ) ) ;
#65403 = VERTEX_POINT ( 'NONE', #51319 ) ;
#65404 = DIRECTION ( 'NONE',  ( -2.900000000000000265E-14, 2.000000000000000155E-15, -1.000000000000000000 ) ) ;
#65405 = VERTEX_POINT ( 'NONE', #9568 ) ;
#65406 = FACE_OUTER_BOUND ( 'NONE', #34827, .T. ) ;
#65407 = CARTESIAN_POINT ( 'NONE',  ( 105.7995184603037870, -26.72403496900519926, 66.17729194474850374 ) ) ;
#65408 = CARTESIAN_POINT ( 'NONE',  ( 103.2782266777140165, -27.47476627046264142, 276.3856500783257957 ) ) ;
#65410 = EDGE_LOOP ( 'NONE', ( #63068, #9762, #20449, #39759 ) ) ;
#65409 = VECTOR ( 'NONE', #89345, 1000.000000000000000 ) ;
#65411 = EDGE_CURVE ( 'NONE', #26375, #37766, #52199, .T. ) ;
#65412 = CARTESIAN_POINT ( 'NONE',  ( 97.31310622223200824, -38.96075413463563564, 51.50544982982146536 ) ) ;
#65413 = VERTEX_POINT ( 'NONE', #34351 ) ;
#65414 = LINE ( 'NONE', #31774, #68288 ) ;
#65415 = DIRECTION ( 'NONE',  ( 1.000000000000000078E-15, 0.000000000000000000, 1.000000000000000000 ) ) ;
#65416 = VECTOR ( 'NONE', #70547, 1000.000000000000000 ) ;
#65417 = DIRECTION ( 'NONE',  ( 0.000000000000000000, 1.000000000000000000, 0.000000000000000000 ) ) ;
#65418 = VERTEX_POINT ( 'NONE', #81641 ) ;
#65419 = CARTESIAN_POINT ( 'NONE',  ( 107.3215719809018083, -25.65558735872630081, 75.04610146638695767 ) ) ;
#65420 = DIRECTION ( 'NONE',  ( 0.000000000000000000, 0.000000000000000000, 1.000000000000000000 ) ) ;
#65421 = CARTESIAN_POINT ( 'NONE',  ( 97.53191591005956695, -39.74918175134386900, 166.5705498172278851 ) ) ;
#65422 = DIRECTION ( 'NONE',  ( 0.000000000000000000, -1.000000000000000000, 0.000000000000000000 ) ) ;
#65423 = CARTESIAN_POINT ( 'NONE',  ( -12.59999999999999964, 81.71744534370293422, 117.6834004267381601 ) ) ;
#65424 = EDGE_LOOP ( 'NONE', ( #57595, #7031 ) ) ;
#65425 = CARTESIAN_POINT ( 'NONE',  ( 100.8594679592218171, 82.96445444011519044, -82.89895571708193245 ) ) ;
#65426 = DIRECTION ( 'NONE',  ( 1.000000000000000000, 4.299999999999999979E-14, 1.000000000000000078E-15 ) ) ;
#65427 = LINE ( 'NONE', #1868, #6662 ) ;
#65428 = AXIS2_PLACEMENT_3D ( 'NONE', #82567, #8031, #21216 ) ;
#65431 = EDGE_CURVE ( 'NONE', #67028, #12546, #23190, .T. ) ;
#65430 = CARTESIAN_POINT ( 'NONE',  ( -31.75000000000000000, 24.56180297284579694, 3.175000000000219647 ) ) ;
#65429 = FACE_OUTER_BOUND ( 'NONE', #19019, .T. ) ;
#65432 = CARTESIAN_POINT ( 'NONE',  ( 25.56670390244797275, -65.37844715994100397, 262.0928068554150059 ) ) ;
#65433 = VECTOR ( 'NONE', #19944, 1000.000000000000000 ) ;
#65434 = ORIENTED_EDGE ( 'NONE', *, *, #12240, .F. ) ;
#65435 = B_SPLINE_CURVE_WITH_KNOTS ( 'NONE', 3,
 ( #56429, #19804, #15117, #65497, #86400, #29636, #15575, #37348, #43701, #43247, #57783, #37797, #16460, #1939, #30089, #44139, #50062, #29199, #3281, #79594, #2835, #24174, #16910, #58235, #51840, #56880, #79149, #51397, #30534, #84624, #30974, #17353, #45034, #57327, #85525, #58662, #72761, #9205, #85072, #10531, #22837, #23301, #85963, #65054, #50966, #22384, #78261, #78709, #71877, #44587, #50518 ),
 .UNSPECIFIED., .F., .F.,
 ( 4, 2, 1, 1, 1, 1, 1, 1, 2, 2, 2, 2, 2, 2, 2, 1, 1, 1, 1, 1, 1, 1, 2, 2, 2, 2, 2, 2, 2, 2, 2, 4 ),
 ( 0.5000144963954069599, 0.5001365631688001745, 0.5002586299421935001, 0.5005027634889802624, 0.5009910305825536758, 0.5019675647696999476, 0.5039206331439923803, 0.5078267698925770235, 0.5156390433897460879, 0.5312635903840843277, 0.5625126843727610293, 0.6250108723501143215, 0.6875090603274676138, 0.7500072483048209060, 0.7500682816915176243, 0.7501293150782144536, 0.7502513818516167721, 0.7504955153982477700, 0.7509837824914034066, 0.7519603166777120151, 0.7539133850503294543, 0.7578195217955624452, 0.7656317952860278719, 0.7812563422669582813, 0.8125054362288213206, 0.8437545301906844708, 0.8750036241525475100, 0.9062527181144106603, 0.9375018120762736995, 0.9687509060381367387, 0.9843754530190684804, 1.000000000000000000 ),
 .UNSPECIFIED. ) ;
#65436 = DIRECTION ( 'NONE',  ( 0.000000000000000000, 0.000000000000000000, 1.000000000000000000 ) ) ;
#65437 = CARTESIAN_POINT ( 'NONE',  ( 109.2982854457139297, -26.60236246699155416, 175.8918157521009391 ) ) ;
#65439 = VERTEX_POINT ( 'NONE', #33907 ) ;
#65438 = CARTESIAN_POINT ( 'NONE',  ( 6.938893903907229955E-15, 50.79999999999999716, 216.0269999999999868 ) ) ;
#65440 = CARTESIAN_POINT ( 'NONE',  ( 104.8797383215544414, -46.86635653470245444, 28.41943479971997988 ) ) ;
#65441 = CARTESIAN_POINT ( 'NONE',  ( 63.06670390244711655, -40.32844715994016838, 129.9678068554150911 ) ) ;
#65442 = CARTESIAN_POINT ( 'NONE',  ( 138.8167039024479834, -57.40094715994099772, 86.31780685541500020 ) ) ;
#65443 = LINE ( 'NONE', #79090, #70323 ) ;
#65444 = AXIS2_PLACEMENT_3D ( 'NONE', #50303, #7644, #36245 ) ;
#65445 = ORIENTED_EDGE ( 'NONE', *, *, #27127, .F. ) ;
#65446 = EDGE_CURVE ( 'NONE', #85611, #43607, #19838, .T. ) ;
#65447 = CARTESIAN_POINT ( 'NONE',  ( 97.31581552154544568, -39.30590672086626824, 31.53167568815738164 ) ) ;
#65448 = ORIENTED_EDGE ( 'NONE', *, *, #26418, .F. ) ;
#65449 = VERTEX_POINT ( 'NONE', #74358 ) ;
#65450 = CARTESIAN_POINT ( 'NONE',  ( 114.9810172151485546, -40.71547668563403022, 199.8872975916109453 ) ) ;
#65451 = EDGE_CURVE ( 'NONE', #20936, #2985, #40269, .T. ) ;
#65452 = LINE ( 'NONE', #79547, #69078 ) ;
#65453 = CARTESIAN_POINT ( 'NONE',  ( 98.26720277155988015, -37.77870449121756025, 37.85301187732598294 ) ) ;
#65454 = CARTESIAN_POINT ( 'NONE',  ( 23.49602257209429723, 85.45800003945487333, 306.6792945138783466 ) ) ;
#65455 = CARTESIAN_POINT ( 'NONE',  ( 109.7248659253242522, -27.00080518093118442, 79.86479194225255185 ) ) ;
#65456 = DIRECTION ( 'NONE',  ( -1.000000000000000000, 0.000000000000000000, 0.000000000000000000 ) ) ;
#65458 = ORIENTED_EDGE ( 'NONE', *, *, #11122, .F. ) ;
#65457 = CIRCLE ( 'NONE', #55257, 13.99999999999999822 ) ;
#65459 = DIRECTION ( 'NONE',  ( 1.000000000000000000, 4.299999999999999979E-14, 1.000000000000000078E-15 ) ) ;
#65460 = CARTESIAN_POINT ( 'NONE',  ( 41.56648329127399677, -9.303447159940999356, 21.04262527591200183 ) ) ;
#65461 = ORIENTED_EDGE ( 'NONE', *, *, #11350, .F. ) ;
#65462 = CARTESIAN_POINT ( 'NONE',  ( 100.2624651760415304, -28.85963121439194623, 260.6441967044822263 ) ) ;
#65463 = DIRECTION ( 'NONE',  ( 1.000000000000000000, 0.000000000000000000, 0.000000000000000000 ) ) ;
#65464 = VERTEX_POINT ( 'NONE', #13923 ) ;
#65465 = CARTESIAN_POINT ( 'NONE',  ( -3.175000000000109956, 111.1250000000000000, 31.75000000000000000 ) ) ;
#65466 = CARTESIAN_POINT ( 'NONE',  ( -64.50026246089650783, 54.97499999999996589, 59.61038444174924678 ) ) ;
#65467 = CARTESIAN_POINT ( 'NONE',  ( 63.03715912545735023, -46.82818131006016671, 180.4678068554151196 ) ) ;
#65468 = CARTESIAN_POINT ( 'NONE',  ( 75.91207007020635444, -69.50612193463149424, 247.5400045958994042 ) ) ;
#65469 = CARTESIAN_POINT ( 'NONE',  ( 99.72256515790628839, -29.26889448616327982, 221.6956252759109702 ) ) ;
#65470 = LINE ( 'NONE', #58209, #21026 ) ;
#65471 = ORIENTED_EDGE ( 'NONE', *, *, #69624, .F. ) ;
#65472 = VECTOR ( 'NONE', #87501, 999.9999999999998863 ) ;
#65473 = CARTESIAN_POINT ( 'NONE',  ( 99.09426955137945470, -44.45222557475181446, 37.95086337114900488 ) ) ;
#65474 = PLANE ( 'NONE',  #71520 ) ;
#65475 = CARTESIAN_POINT ( 'NONE',  ( 96.56351739100374232, -40.17746103522156176, 286.5908633711491120 ) ) ;
#65476 = ADVANCED_FACE ( 'NONE', ( #67989 ), #82541, .F. ) ;
#65478 = VERTEX_POINT ( 'NONE', #27989 ) ;
#65477 = EDGE_CURVE ( 'NONE', #77124, #73910, #26204, .T. ) ;
#65479 = ADVANCED_FACE ( 'NONE', ( #68442 ), #75258, .F. ) ;
#65480 = DIRECTION ( 'NONE',  ( 1.000000000000000000, 4.299999999999999979E-14, 1.000000000000000078E-15 ) ) ;
#65481 = CARTESIAN_POINT ( 'NONE',  ( 116.8164944309794606, -34.15047750347410727, 20.03140278090121029 ) ) ;
#65482 = LINE ( 'NONE', #22368, #71268 ) ;
#65483 = CARTESIAN_POINT ( 'NONE',  ( 103.8598393684536632, -44.23592174987565073, 90.07380465530594904 ) ) ;
#65484 = CARTESIAN_POINT ( 'NONE',  ( 108.6783733978936226, -26.40767070732865562, 185.9527681330539792 ) ) ;
#65485 = AXIS2_PLACEMENT_3D ( 'NONE', #33831, #42417, #207 ) ;
#65486 = DIRECTION ( 'NONE',  ( -1.000000000000000000, 0.000000000000000000, 1.047445008332813989E-14 ) ) ;
#65487 = ORIENTED_EDGE ( 'NONE', *, *, #30863, .F. ) ;
#65488 = EDGE_CURVE ( 'NONE', #71019, #75012, #47522, .T. ) ;
#65489 = DIRECTION ( 'NONE',  ( 0.7071067811873692488, 0.7071067811857258967, -2.899137802861360256E-29 ) ) ;
#65490 = ORIENTED_EDGE ( 'NONE', *, *, #82786, .T. ) ;
#65492 = VERTEX_POINT ( 'NONE', #53878 ) ;
#65491 = AXIS2_PLACEMENT_3D ( 'NONE', #13467, #88888, #27096 ) ;
#65493 = CARTESIAN_POINT ( 'NONE',  ( 130.0664832912740110, -18.72922654876702353, 239.5838068554170377 ) ) ;
#65494 = EDGE_LOOP ( 'NONE', ( #24874, #85686, #12086, #35845 ) ) ;
#65495 = VERTEX_POINT ( 'NONE', #47066 ) ;
#65496 = CARTESIAN_POINT ( 'NONE',  ( -31.75000000000000000, 8.255000000000000782, 3.175000000000219647 ) ) ;
#65497 = CARTESIAN_POINT ( 'NONE',  ( 97.80783779089463792, -40.50800376726066077, 42.63481548141047028 ) ) ;
#65498 = EDGE_CURVE ( 'NONE', #9337, #25266, #40718, .T. ) ;
#65499 = CARTESIAN_POINT ( 'NONE',  ( 115.2323353771322445, -31.47685829367418009, 143.7038483995059721 ) ) ;
#65500 = AXIS2_PLACEMENT_3D ( 'NONE', #63377, #8883, #49736 ) ;
#65501 = CARTESIAN_POINT ( 'NONE',  ( 99.09377177006922466, -44.45270778143659385, 41.95086337114900488 ) ) ;
#65502 = CARTESIAN_POINT ( 'NONE',  ( -10.79079172156231081, 75.84006377869074811, 130.1095006741098530 ) ) ;
#65503 = AXIS2_PLACEMENT_3D ( 'NONE', #25735, #54306, #47051 ) ;
#65504 = ORIENTED_EDGE ( 'NONE', *, *, #48016, .F. ) ;
#65505 = CARTESIAN_POINT ( 'NONE',  ( 97.12554930137042675, -37.99679140698025748, 137.4272600898537462 ) ) ;
#65506 = ORIENTED_EDGE ( 'NONE', *, *, #54805, .T. ) ;
#65507 = DIRECTION ( 'NONE',  ( 0.000000000000000000, 0.000000000000000000, -1.000000000000000000 ) ) ;
#65508 = CARTESIAN_POINT ( 'NONE',  ( -0.4111448617337906675, 69.95000000000001705, 118.5560000000000258 ) ) ;
#65509 = CARTESIAN_POINT ( 'NONE',  ( 37.06648329127298780, 12.92155284005730387, 355.9756252759109998 ) ) ;
#65510 = PLANE ( 'NONE',  #75597 ) ;
#65511 = VERTEX_POINT ( 'NONE', #89342 ) ;
#65512 = CARTESIAN_POINT ( 'NONE',  ( 96.97860658150185031, -39.36037357437717787, 276.5299109901967540 ) ) ;
#65513 = CARTESIAN_POINT ( 'NONE',  ( 105.1556394555663445, -47.05180815895162993, 8.429910990196965770 ) ) ;
#65514 = FILL_AREA_STYLE ('',( #86423 ) ) ;
#65515 = DIRECTION ( 'NONE',  ( 0.9242245927363033076, 0.3818493186865918876, 0.000000000000000000 ) ) ;
#65517 = DIRECTION ( 'NONE',  ( -4.093947403305260305E-16, 1.000000000000000000, -6.162975822039159109E-32 ) ) ;
#65516 = DIRECTION ( 'NONE',  ( 0.000000000000000000, 0.000000000000000000, 1.000000000000000000 ) ) ;
#65518 = CARTESIAN_POINT ( 'NONE',  ( 105.4062783216046313, -25.39030566700975555, 322.9818289795172177 ) ) ;
#65519 = DIRECTION ( 'NONE',  ( 0.000000000000000000, 1.000000000000000000, 0.000000000000000000 ) ) ;
#65520 = CARTESIAN_POINT ( 'NONE',  ( 130.0664832912740110, -18.82844715994099971, 284.9256252759119548 ) ) ;
#65521 = CIRCLE ( 'NONE', #55320, 11.45913725231036118 ) ;
#65522 = CARTESIAN_POINT ( 'NONE',  ( 130.0664832912740110, -18.82844715994099971, 17.92562527591199739 ) ) ;
#65523 = B_SPLINE_CURVE_WITH_KNOTS ( 'NONE', 3,
 ( #74476, #47187, #53996, #81754, #19504, #61716, #74926, #19961, #66757, #4542, #11805, #12247, #26757, #74026, #67661, #40831, #68109, #13151 ),
 .UNSPECIFIED., .F., .F.,
 ( 4, 2, 2, 2, 2, 2, 2, 2, 4 ),
 ( 0.4999999978220436292, 0.5624999980942881894, 0.6249999983665327496, 0.6874999986387773099, 0.7499999989110217591, 0.8124999991832664303, 0.8749999994555108795, 0.9374999997277554398, 1.000000000000000000 ),
 .UNSPECIFIED. ) ;
#65524 = FACE_OUTER_BOUND ( 'NONE', #86645, .T. ) ;
#65525 = CARTESIAN_POINT ( 'NONE',  ( 168.3595971214162148, -48.62134037890298544, 300.4678068554149490 ) ) ;
#65526 = CARTESIAN_POINT ( 'NONE',  ( 110.2977701465690643, -46.68767980799292872, 12.82705384733995402 ) ) ;
#65527 = CARTESIAN_POINT ( 'NONE',  ( 97.67470816545109358, -41.25460433215529577, 167.6841967044829573 ) ) ;
#65528 = CARTESIAN_POINT ( 'NONE',  ( 96.15481094519168437, -38.63223783578033022, 42.45181575210199298 ) ) ;
#65529 = CIRCLE ( 'NONE', #9017, 11.49999999999999645 ) ;
#65532 = ADVANCED_FACE ( 'NONE', ( #27102 ), #89793, .T. ) ;
#65531 = CYLINDRICAL_SURFACE ( 'NONE', #15135, 190.5000000000000000 ) ;
#65530 = DIRECTION ( 'NONE',  ( -4.237773401492740281E-14, 1.000000000000000000, 0.000000000000000000 ) ) ;
#65533 = CARTESIAN_POINT ( 'NONE',  ( 31.78666935232998725, -36.02818131005891189, -5.074374724088000832 ) ) ;
#65534 = AXIS2_PLACEMENT_3D ( 'NONE', #72538, #38008, #65702 ) ;
#65535 = EDGE_CURVE ( 'NONE', #38582, #74068, #55225, .T. ) ;
#65536 = ORIENTED_EDGE ( 'NONE', *, *, #134, .T. ) ;
#65537 = CARTESIAN_POINT ( 'NONE',  ( 104.4899545120944566, -26.97880756954710080, 186.2814586043616032 ) ) ;
#65538 = VERTEX_POINT ( 'NONE', #88893 ) ;
#65539 = CARTESIAN_POINT ( 'NONE',  ( 108.8666348730871078, -46.34312957481623840, 78.72419670448194040 ) ) ;
#65541 = EDGE_LOOP ( 'NONE', ( #48242, #1331, #72299, #28534 ) ) ;
#65540 = DIRECTION ( 'NONE',  ( 0.000000000000000000, 0.000000000000000000, 1.000000000000000000 ) ) ;
#65542 = CARTESIAN_POINT ( 'NONE',  ( 150.5667039024473297, -25.42844715993594562, 300.4678068554149490 ) ) ;
#65543 = CARTESIAN_POINT ( 'NONE',  ( 118.8526415125688800, -37.69623653580512013, 184.7613395616249647 ) ) ;
#65544 = CARTESIAN_POINT ( 'NONE',  ( 25.56670390244797275, -67.87844715994100397, 168.3428068554150059 ) ) ;
#65545 = DIRECTION ( 'NONE',  ( -0.7071067811865462405, 0.000000000000000000, 0.7071067811865486830 ) ) ;
#65546 = FACE_OUTER_BOUND ( 'NONE', #70744, .T. ) ;
#65547 = CARTESIAN_POINT ( 'NONE',  ( 100.9546728013743149, -28.70702573470092389, 46.59395861020129104 ) ) ;
#65548 = VECTOR ( 'NONE', #58512, 1000.000000000000000 ) ;
#65549 = CARTESIAN_POINT ( 'NONE',  ( 145.9684219307273452, -136.2709667195323959, 247.3967439480269945 ) ) ;
#65550 = CARTESIAN_POINT ( 'NONE',  ( 116.4060884429800922, -40.43037349191362040, 98.52600069756960011 ) ) ;
#65551 = CARTESIAN_POINT ( 'NONE',  ( 111.5019814087853831, -26.53443175268781218, 134.7499109901969518 ) ) ;
#65552 = ORIENTED_EDGE ( 'NONE', *, *, #57066, .T. ) ;
#65553 = ORIENTED_EDGE ( 'NONE', *, *, #72788, .T. ) ;
#65554 = VECTOR ( 'NONE', #28545, 1000.000000000000000 ) ;
#65555 = CARTESIAN_POINT ( 'NONE',  ( 110.4802244392091950, -27.25226000720831721, 96.23301187732596418 ) ) ;
#65557 = EDGE_CURVE ( 'NONE', #64158, #5232, #82983, .T. ) ;
#65556 = AXIS2_PLACEMENT_3D ( 'NONE', #23947, #58444, #43918 ) ;
#65558 = CARTESIAN_POINT ( 'NONE',  ( -47.02966122971774610, 92.07499999999998863, 74.26049396966043048 ) ) ;
#65560 = DIRECTION ( 'NONE',  ( 0.000000000000000000, 1.000000000000000000, 0.000000000000000000 ) ) ;
#65559 = CARTESIAN_POINT ( 'NONE',  ( 117.3720538532506623, -35.57445771113446398, 229.9032443235289520 ) ) ;
#65561 = DIRECTION ( 'NONE',  ( 0.000000000000000000, 0.000000000000000000, 1.000000000000000000 ) ) ;
#65562 = CARTESIAN_POINT ( 'NONE',  ( 115.8254330622582415, -31.73001971111901653, 110.2399483882993820 ) ) ;
#65563 = VECTOR ( 'NONE', #12225, 1000.000000000000000 ) ;
#65564 = CARTESIAN_POINT ( 'NONE',  ( 118.5214325610856605, 70.17658267799284033, -2.892017926149469620 ) ) ;
#65565 = CARTESIAN_POINT ( 'NONE',  ( 62.03742497533652767, -23.42844715994041493, 193.9678068554150911 ) ) ;
#65566 = FACE_OUTER_BOUND ( 'NONE', #39098, .T. ) ;
#65567 = DIRECTION ( 'NONE',  ( 1.000000000000000078E-15, -1.000000000000000083E-30, -1.000000000000000000 ) ) ;
#65568 = CARTESIAN_POINT ( 'NONE',  ( 98.02603654163375779, -30.41010087969369735, 160.8289586092449497 ) ) ;
#65569 = ORIENTED_EDGE ( 'NONE', *, *, #54447, .F. ) ;
#65570 = AXIS2_PLACEMENT_3D ( 'NONE', #30995, #38256, #52295 ) ;
#65571 = ORIENTED_EDGE ( 'NONE', *, *, #76173, .F. ) ;
#65572 = ORIENTED_CLOSED_SHELL ( 'NONE', *, #34327, .F. );
#65573 = AXIS2_PLACEMENT_3D ( 'NONE', #53374, #25245, #52909 ) ;
#65574 = CARTESIAN_POINT ( 'NONE',  ( 127.5395909587422949, -72.61999453823881367, 248.4067532124560103 ) ) ;
#65575 = CARTESIAN_POINT ( 'NONE',  ( 146.4947614284610609, -68.42932138493740979, 246.8950229379430539 ) ) ;
#65576 = DIRECTION ( 'NONE',  ( 3.100000000000000258E-29, -3.100000000000000044E-14, -1.000000000000000000 ) ) ;
#65577 = CARTESIAN_POINT ( 'NONE',  ( 108.3330205148376706, -46.73491748175980831, 103.6772580696607378 ) ) ;
#65578 = DIRECTION ( 'NONE',  ( -1.907762142705490052E-15, -7.167082501179359715E-16, 1.000000000000000000 ) ) ;
#65579 = CARTESIAN_POINT ( 'NONE',  ( 117.0173010276973287, -33.62006509304910651, 174.0670538473389399 ) ) ;
#65580 = DIRECTION ( 'NONE',  ( 0.000000000000000000, 1.000000000000000000, 0.000000000000000000 ) ) ;
#65581 = ORIENTED_EDGE ( 'NONE', *, *, #29520, .F. ) ;
#65584 = ORIENTED_EDGE ( 'NONE', *, *, #74407, .T. ) ;
#65583 = ORIENTED_EDGE ( 'NONE', *, *, #37926, .T. ) ;
#65582 = EDGE_CURVE ( 'NONE', #51180, #23464, #47969, .T. ) ;
#65585 = CARTESIAN_POINT ( 'NONE',  ( 115.7473634667994560, -41.72957221166183928, 64.41119945959614768 ) ) ;
#65586 = LINE ( 'NONE', #9293, #68100 ) ;
#65587 = CARTESIAN_POINT ( 'NONE',  ( 131.4004675426835718, -36.03188136816541487, 6.871351212842790268 ) ) ;
#65588 = CARTESIAN_POINT ( 'NONE',  ( 114.3671945862968045, -31.65384462053443571, 275.7415833058969952 ) ) ;
#65589 = CARTESIAN_POINT ( 'NONE',  ( 20.03715912545644073, -24.42818131006202265, 129.9678068554150627 ) ) ;
#65590 = VERTEX_POINT ( 'NONE', #26645 ) ;
#65591 = ADVANCED_FACE ( 'NONE', ( #55662 ), #18943, .T. ) ;
#65592 = VECTOR ( 'NONE', #27549, 1000.000000000000000 ) ;
#65593 = CARTESIAN_POINT ( 'NONE',  ( 106.1388935886583624, -44.86984817071454046, 9.635625275910941312 ) ) ;
#65594 = DIRECTION ( 'NONE',  ( -4.237773401492740281E-14, 1.000000000000000000, 0.000000000000000000 ) ) ;
#65595 = VERTEX_POINT ( 'NONE', #5320 ) ;
#65596 = ORIENTED_EDGE ( 'NONE', *, *, #73281, .F. ) ;
#65597 = CIRCLE ( 'NONE', #69952, 32.50000000000001421 ) ;
#65598 = CARTESIAN_POINT ( 'NONE',  ( 110.8925242491656320, -45.96859375203237619, 112.8888992892811700 ) ) ;
#65599 = ORIENTED_EDGE ( 'NONE', *, *, #63143, .F. ) ;
#65600 = ORIENTED_EDGE ( 'NONE', *, *, #44170, .F. ) ;
#65601 = EDGE_CURVE ( 'NONE', #20396, #70423, #5771, .T. ) ;
#65602 = CARTESIAN_POINT ( 'NONE',  ( 100.5114817196218411, -42.97801697403279775, 36.34289601855395091 ) ) ;
#65603 = CARTESIAN_POINT ( 'NONE',  ( 115.0566306311886819, -29.05787713660226856, 189.4232443235299570 ) ) ;
#65604 = CARTESIAN_POINT ( 'NONE',  ( 108.7397100058831541, -25.82697924850565840, 144.9432443235299672 ) ) ;
#65605 = EDGE_CURVE ( 'NONE', #54909, #3107, #88444, .T. ) ;
#65606 = DIRECTION ( 'NONE',  ( 3.100000000000000258E-29, -3.100000000000000044E-14, -1.000000000000000000 ) ) ;
#65607 = CARTESIAN_POINT ( 'NONE',  ( 111.8640475646460857, -46.02486053542493494, 268.9556252759110180 ) ) ;
#65608 = CARTESIAN_POINT ( 'NONE',  ( 99.04407452439549786, -42.84127747802013175, 97.84479291583183169 ) ) ;
#65609 = CARTESIAN_POINT ( 'NONE',  ( -130.1093520674644139, 75.84295037288958952, -10.79257909650410951 ) ) ;
#65610 = ORIENTED_EDGE ( 'NONE', *, *, #85198, .F. ) ;
#65611 = ORIENTED_EDGE ( 'NONE', *, *, #11939, .F. ) ;
#65612 = VECTOR ( 'NONE', #30206, 1000.000000000000000 ) ;
#65613 = CARTESIAN_POINT ( 'NONE',  ( 95.99995219064309993, -35.86644482699779246, 191.2765776568629690 ) ) ;
#65614 = VERTEX_POINT ( 'NONE', #78409 ) ;
#65615 = CARTESIAN_POINT ( 'NONE',  ( 108.8488851759622804, -47.00125683367996032, 167.7127681330539701 ) ) ;
#65616 = DIRECTION ( 'NONE',  ( 1.639958061481212836E-42, -4.100000000000000342E-29, -1.000000000000000000 ) ) ;
#65617 = CARTESIAN_POINT ( 'NONE',  ( 33.96670390244653959, -28.27351298637442056, 193.9678068554150911 ) ) ;
#65618 = CARTESIAN_POINT ( 'NONE',  ( 134.0664832912740110, -9.029447159941003775, 1.625625275910997480 ) ) ;
#65619 = CARTESIAN_POINT ( 'NONE',  ( 143.6448735140314454, -139.9068108329578308, 247.1123908456728486 ) ) ;
#65622 = CARTESIAN_POINT ( 'NONE',  ( 115.8929840288991642, -32.51563116083749350, 15.18133956162492915 ) ) ;
#65621 = DIRECTION ( 'NONE',  ( 0.000000000000000000, 0.000000000000000000, 1.000000000000000000 ) ) ;
#65620 = CARTESIAN_POINT ( 'NONE',  ( 50.87649884952499946, -33.54226604284930602, -5.074374724088000832 ) ) ;
#65623 = CARTESIAN_POINT ( 'NONE',  ( 80.06648329127402519, -46.72944715994105991, 10.72562527591094295 ) ) ;
#65624 = CARTESIAN_POINT ( 'NONE',  ( 83.06670390244796920, -58.72944715994094622, 210.8338068554149913 ) ) ;
#65625 = VECTOR ( 'NONE', #68869, 1000.000000000000000 ) ;
#65626 = DIRECTION ( 'NONE',  ( -9.073094938289460781E-13, -1.000000000000000000, 0.000000000000000000 ) ) ;
#65627 = DIRECTION ( 'NONE',  ( -0.9254794337955620787, -0.3787978585227822492, 0.000000000000000000 ) ) ;
#65628 = FACE_OUTER_BOUND ( 'NONE', #70090, .T. ) ;
#65629 = DIRECTION ( 'NONE',  ( 1.000000000000000000, 0.000000000000000000, 0.000000000000000000 ) ) ;
#65631 = ORIENTED_EDGE ( 'NONE', *, *, #9397, .T. ) ;
#65630 = CARTESIAN_POINT ( 'NONE',  ( 114.5288898844889047, -31.71472813432939830, 195.5838068554168672 ) ) ;
#65632 = CYLINDRICAL_SURFACE ( 'NONE', #53847, 7.999999999999992895 ) ;
#65633 = CARTESIAN_POINT ( 'NONE',  ( 117.9557474314311349, -34.69982462793587530, 203.9851490854349549 ) ) ;
#65634 = CARTESIAN_POINT ( 'NONE',  ( 101.7108440984968212, -27.74398881808361850, 81.50419670448295051 ) ) ;
#65635 = CARTESIAN_POINT ( 'NONE',  ( 111.6274790011277247, -46.15230754745154940, 243.9356252759109509 ) ) ;
#65636 = DIRECTION ( 'NONE',  ( 4.299999999999999979E-14, -1.000000000000000000, 4.400000000000000367E-29 ) ) ;
#65637 = CARTESIAN_POINT ( 'NONE',  ( 52.99265158129170317, 95.25000000000000000, 358.0130000000000337 ) ) ;
#65639 = LINE ( 'NONE', #23877, #19666 ) ;
#65638 = FACE_OUTER_BOUND ( 'NONE', #80031, .T. ) ;
#65640 = CARTESIAN_POINT ( 'NONE',  ( 100.8961411191535973, 127.0000000000000000, -3.968749999999580336 ) ) ;
#65641 = DIRECTION ( 'NONE',  ( 0.000000000000000000, -0.000000000000000000, -1.000000000000000000 ) ) ;
#65642 = CARTESIAN_POINT ( 'NONE',  ( 112.1419326622839776, -28.01430185457018496, 64.65734975839959020 ) ) ;
#65643 = EDGE_CURVE ( 'NONE', #89346, #66826, #49320, .T. ) ;
#65644 = VERTEX_POINT ( 'NONE', #29352 ) ;
#65645 = ORIENTED_EDGE ( 'NONE', *, *, #5716, .F. ) ;
#65646 = CARTESIAN_POINT ( 'NONE',  ( 102.6518059180641416, -28.82227990381128180, 104.9162293518859599 ) ) ;
#65648 = ORIENTED_EDGE ( 'NONE', *, *, #18600, .T. ) ;
#65647 = DIRECTION ( 'NONE',  ( 1.000000000000000000, 0.000000000000000000, 0.000000000000000000 ) ) ;
#65649 = AXIS2_PLACEMENT_3D ( 'NONE', #74373, #67551, #88460 ) ;
#65650 = CARTESIAN_POINT ( 'NONE',  ( 100.3128846869253294, -46.43702735306945328, 83.09276813305294240 ) ) ;
#65651 = DIRECTION ( 'NONE',  ( -0.9659258262890706437, 0.000000000000000000, 0.2588190451025119132 ) ) ;
#65652 = CARTESIAN_POINT ( 'NONE',  ( 79.00802158143734744, -16.19118199975294203, 8.051357469095744790 ) ) ;
#65653 = CARTESIAN_POINT ( 'NONE',  ( 102.0670549777755696, -27.97049804943433315, 176.4897919409716280 ) ) ;
#65654 = CARTESIAN_POINT ( 'NONE',  ( 99.56037394151441333, -43.88466257697688633, 36.92038718067297509 ) ) ;
#65655 = ORIENTED_EDGE ( 'NONE', *, *, #83984, .F. ) ;
#65656 = ORIENTED_EDGE ( 'NONE', *, *, #55348, .T. ) ;
#65657 = ORIENTED_EDGE ( 'NONE', *, *, #19126, .F. ) ;
#65658 = EDGE_CURVE ( 'NONE', #67267, #23819, #7147, .T. ) ;
#65659 = CARTESIAN_POINT ( 'NONE',  ( -487.2989999999999782, 14.28750000000023945, 19.36139197104649767 ) ) ;
#65660 = CARTESIAN_POINT ( 'NONE',  ( 116.3212776292296127, -32.94146857471318413, 287.6356252759109680 ) ) ;
#65661 = CARTESIAN_POINT ( 'NONE',  ( 113.2454986995014394, -28.75867294597971124, 115.5522919424271038 ) ) ;
#65662 = DIRECTION ( 'NONE',  ( 1.000000000000000000, -5.337610695313248426E-16, 0.000000000000000000 ) ) ;
#65663 = DIRECTION ( 'NONE',  ( 0.000000000000000000, 1.000000000000000000, 0.000000000000000000 ) ) ;
#65664 = LINE ( 'NONE', #43878, #11807 ) ;
#65665 = DIRECTION ( 'NONE',  ( 0.000000000000000000, 0.000000000000000000, 1.000000000000000000 ) ) ;
#65666 = CARTESIAN_POINT ( 'NONE',  ( 76.79137032886029601, 90.93965867633433220, 90.32698471909210980 ) ) ;
#65667 = CARTESIAN_POINT ( 'NONE',  ( 104.4960957391109417, -46.84663716100912012, 47.37848241876796607 ) ) ;
#65668 = VERTEX_POINT ( 'NONE', #9345 ) ;
#65669 = VERTEX_POINT ( 'NONE', #64754 ) ;
#65670 = EDGE_CURVE ( 'NONE', #57314, #24899, #43399, .T. ) ;
#65671 = FACE_OUTER_BOUND ( 'NONE', #89307, .T. ) ;
#65672 = DIRECTION ( 'NONE',  ( -1.000000000000000078E-15, 1.000000000000000083E-30, 1.000000000000000000 ) ) ;
#65673 = CARTESIAN_POINT ( 'NONE',  ( 196.2150000000000034, 43.68799999999999528, 44.45000000000000284 ) ) ;
#65674 = CARTESIAN_POINT ( 'NONE',  ( 104.7498880507309451, -44.55652276380406818, 105.1652332267339602 ) ) ;
#65675 = AXIS2_PLACEMENT_3D ( 'NONE', #51515, #64723, #78819 ) ;
#65676 = ADVANCED_FACE ( 'NONE', ( #1651 ), #15721, .F. ) ;
#65677 = VECTOR ( 'NONE', #60129, 1000.000000000000000 ) ;
#65678 = CARTESIAN_POINT ( 'NONE',  ( 181.5667039024459939, -22.48495420874030515, -5.074374724088000832 ) ) ;
#65679 = ORIENTED_EDGE ( 'NONE', *, *, #4468, .F. ) ;
#65680 = ORIENTED_EDGE ( 'NONE', *, *, #8349, .T. ) ;
#65681 = FACE_OUTER_BOUND ( 'NONE', #47402, .T. ) ;
#65682 = ORIENTED_EDGE ( 'NONE', *, *, #67191, .F. ) ;
#65683 = ORIENTED_EDGE ( 'NONE', *, *, #64977, .T. ) ;
#65684 = DIRECTION ( 'NONE',  ( 0.000000000000000000, 0.000000000000000000, 1.000000000000000000 ) ) ;
#65685 = ADVANCED_FACE ( 'NONE', ( #15272 ), #8457, .F. ) ;
#65686 = CARTESIAN_POINT ( 'NONE',  ( 98.18569924386140713, -36.28921507361370402, 167.7187261630399462 ) ) ;
#65687 = DIRECTION ( 'NONE',  ( 1.000000000000000000, 0.000000000000000000, 0.000000000000000000 ) ) ;
#65688 = CARTESIAN_POINT ( 'NONE',  ( 117.2306693829537210, -39.29235896168534481, 119.6299109901969615 ) ) ;
#65689 = CARTESIAN_POINT ( 'NONE',  ( 99.09570915332048457, -30.55043165520475767, 120.8022919327240601 ) ) ;
#65690 = CARTESIAN_POINT ( 'NONE',  ( 98.38055655239837449, -41.69550781276469564, 16.73980917770007437 ) ) ;
#65691 = VERTEX_POINT ( 'NONE', #70681 ) ;
#65692 = ORIENTED_EDGE ( 'NONE', *, *, #977, .T. ) ;
#65693 = ORIENTED_EDGE ( 'NONE', *, *, #85284, .T. ) ;
#65694 = EDGE_CURVE ( 'NONE', #75348, #45281, #22537, .T. ) ;
#65695 = CARTESIAN_POINT ( 'NONE',  ( 109.0547627366692041, -28.78404389176943212, 197.6995189410199600 ) ) ;
#65697 = CARTESIAN_POINT ( 'NONE',  ( 96.63442969565970486, -37.29391305320381633, 76.36991099019697060 ) ) ;
#65696 = AXIS2_PLACEMENT_3D ( 'NONE', #59713, #3879, #5678 ) ;
#65698 = ORIENTED_EDGE ( 'NONE', *, *, #78125, .T. ) ;
#65699 = CARTESIAN_POINT ( 'NONE',  ( 95.28387218206118803, -35.72034718286344201, 36.25848241876794731 ) ) ;
#65700 = CARTESIAN_POINT ( 'NONE',  ( 112.0632082999805448, -45.48990328828745078, 252.9899119478660623 ) ) ;
#65701 = ADVANCED_FACE ( 'NONE', ( #71140 ), #14831, .F. ) ;
#65702 = DIRECTION ( 'NONE',  ( 1.000000000000000000, 4.299999999999999979E-14, 1.000000000000000078E-15 ) ) ;
#65703 = DIRECTION ( 'NONE',  ( -1.000000000000000000, -2.756263715554006823E-15, 0.000000000000000000 ) ) ;
#65704 = CARTESIAN_POINT ( 'NONE',  ( 101.9720301123653883, -46.53865341315756154, 163.1832443235299763 ) ) ;
#65706 = EDGE_CURVE ( 'NONE', #17773, #32982, #2540, .T. ) ;
#65705 = DIRECTION ( 'NONE',  ( -1.000000000000000000, 0.000000000000000000, 0.000000000000000000 ) ) ;
#65707 = ORIENTED_EDGE ( 'NONE', *, *, #58672, .T. ) ;
#65708 = FACE_BOUND ( 'NONE', #79715, .T. ) ;
#65709 = EDGE_CURVE ( 'NONE', #54710, #17992, #36156, .T. ) ;
#65710 = ORIENTED_EDGE ( 'NONE', *, *, #34600, .F. ) ;
#65711 = CARTESIAN_POINT ( 'NONE',  ( 29.77381068363827055, -48.62134037875150483, 300.4678068554150059 ) ) ;
#65712 = ORIENTED_EDGE ( 'NONE', *, *, #7325, .F. ) ;
#65713 = EDGE_LOOP ( 'NONE', ( #6191, #75723 ) ) ;
#65714 = FACE_OUTER_BOUND ( 'NONE', #15484, .T. ) ;
#65715 = PLANE ( 'NONE',  #18876 ) ;
#65716 = CARTESIAN_POINT ( 'NONE',  ( 116.7450715690984140, -32.85492016819326722, 54.12991099019698282 ) ) ;
#65717 = PLANE ( 'NONE',  #76540 ) ;
#65718 = DIRECTION ( 'NONE',  ( 1.000000000000000000, 0.000000000000000000, 0.000000000000000000 ) ) ;
#65719 = CARTESIAN_POINT ( 'NONE',  ( 99.04406186618773233, -42.84125764973450856, 72.84395861022517238 ) ) ;
#65720 = CARTESIAN_POINT ( 'NONE',  ( 107.3052971647831555, -26.36210646096926524, 75.04610146638796664 ) ) ;
#65722 = CARTESIAN_POINT ( 'NONE',  ( 101.9951592035502586, -45.85337710724431304, 183.1727681330539781 ) ) ;
#65721 = LINE ( 'NONE', #11207, #20112 ) ;
#65723 = CARTESIAN_POINT ( 'NONE',  ( 97.31592924394860233, -39.30618500135939541, 61.53147658036623824 ) ) ;
#65724 = CARTESIAN_POINT ( 'NONE',  ( 83.56670390244801183, -36.72944715994108122, 218.8274735512160589 ) ) ;
#65725 = VERTEX_POINT ( 'NONE', #83413 ) ;
#65726 = DIRECTION ( 'NONE',  ( 1.000000000000000000, 0.000000000000000000, 0.000000000000000000 ) ) ;
#65727 = DIRECTION ( 'NONE',  ( 0.000000000000000000, 1.000000000000000000, 0.000000000000000000 ) ) ;
#65728 = CARTESIAN_POINT ( 'NONE',  ( 109.7268104826868722, -27.00131123978085768, 134.8646848310448263 ) ) ;
#65729 = DIRECTION ( 'NONE',  ( 4.299999999999999979E-14, -1.000000000000000000, 4.400000000000000367E-29 ) ) ;
#65731 = ORIENTED_EDGE ( 'NONE', *, *, #18603, .F. ) ;
#65730 = CARTESIAN_POINT ( 'NONE',  ( 98.50147650033493107, -30.70887204493662281, 205.8384824187679669 ) ) ;
#65732 = CARTESIAN_POINT ( 'NONE',  ( 107.0664832912739399, -36.72944715994095333, 311.6343304127839815 ) ) ;
#65733 = CARTESIAN_POINT ( 'NONE',  ( 117.3563231384421357, -34.92488217824808316, 239.9641967044819637 ) ) ;
#65734 = CARTESIAN_POINT ( 'NONE',  ( 108.2817482635038147, -26.29579267872783177, 125.9841967044819597 ) ) ;
#65735 = DIRECTION ( 'NONE',  ( 0.000000000000000000, 0.000000000000000000, -1.000000000000000000 ) ) ;
#65736 = CARTESIAN_POINT ( 'NONE',  ( 9.572882853229341293, 90.93765695308120200, -130.2059221945669947 ) ) ;
#65737 = DIRECTION ( 'NONE',  ( 0.000000000000000000, 0.000000000000000000, -1.000000000000000000 ) ) ;
#65738 = CARTESIAN_POINT ( 'NONE',  ( 173.9900000000000091, 20.32000000000000028, -71.37400000000000944 ) ) ;
#65739 = EDGE_LOOP ( 'NONE', ( #52372, #39027 ) ) ;
#65740 = VECTOR ( 'NONE', #64405, 1000.000000000000000 ) ;
#65741 = VECTOR ( 'NONE', #47267, 999.9999999999998863 ) ;
#65742 = ADVANCED_FACE ( 'NONE', ( #84330 ), #50668, .T. ) ;
#65743 = ORIENTED_EDGE ( 'NONE', *, *, #42687, .F. ) ;
#65744 = VERTEX_POINT ( 'NONE', #84771 ) ;
#65745 = VERTEX_POINT ( 'NONE', #28903 ) ;
#65746 = CARTESIAN_POINT ( 'NONE',  ( 30.48091746481741637, -48.32844715994156815, 180.4678068554150911 ) ) ;
#65747 = CARTESIAN_POINT ( 'NONE',  ( 106.1383564330493812, -47.74364531592736682, 258.4975300378158636 ) ) ;
#65748 = LINE ( 'NONE', #78524, #31579 ) ;
#65749 = CARTESIAN_POINT ( 'NONE',  ( 131.5185316161781088, -35.69475198630853896, 2.828485944707569644 ) ) ;
#65751 = DIRECTION ( 'NONE',  ( -3.100000000000000258E-29, 3.100000000000000044E-14, 1.000000000000000000 ) ) ;
#65750 = CARTESIAN_POINT ( 'NONE',  ( -15.89999999999999680, 53.97500000000000142, 50.79999999999999716 ) ) ;
#65752 = CARTESIAN_POINT ( 'NONE',  ( 107.9802517323619355, -45.22186489331556203, 202.0838483995049728 ) ) ;
#65753 = ORIENTED_EDGE ( 'NONE', *, *, #84262, .F. ) ;
#65754 = EDGE_LOOP ( 'NONE', ( #67481, #22053, #53898, #24472 ) ) ;
#65755 = ORIENTED_EDGE ( 'NONE', *, *, #29390, .T. ) ;
#65756 = EDGE_CURVE ( 'NONE', #28103, #27899, #35698, .T. ) ;
#65757 = FACE_OUTER_BOUND ( 'NONE', #21695, .T. ) ;
#65758 = CARTESIAN_POINT ( 'NONE',  ( 97.86672394365611183, -40.64956911969122189, 181.6470188064607214 ) ) ;
#65759 = DIRECTION ( 'NONE',  ( 0.000000000000000000, 0.000000000000000000, 1.000000000000000000 ) ) ;
#65760 = EDGE_CURVE ( 'NONE', #45346, #6826, #77951, .T. ) ;
#65761 = CARTESIAN_POINT ( 'NONE',  ( 111.4279401658702682, -28.40658880358809668, 11.11205949637394852 ) ) ;
#65762 = CARTESIAN_POINT ( 'NONE',  ( 118.0447731586489084, 88.91144712388913263, 10.99980504627958133 ) ) ;
#65763 = EDGE_CURVE ( 'NONE', #10951, #41323, #36617, .T. ) ;
#65764 = VECTOR ( 'NONE', #85015, 1000.000000000000000 ) ;
#65765 = DIRECTION ( 'NONE',  ( 0.7071067811865461294, 0.000000000000000000, 0.7071067811865489050 ) ) ;
#65766 = CARTESIAN_POINT ( 'NONE',  ( 168.5667039024542362, -48.82844715994099971, 249.9678068554149775 ) ) ;
#65767 = ADVANCED_FACE ( 'NONE', ( #63410 ), #1193, .F. ) ;
#65768 = ORIENTED_EDGE ( 'NONE', *, *, #10292, .F. ) ;
#65769 = EDGE_CURVE ( 'NONE', #36938, #86605, #49765, .T. ) ;
#65770 = CARTESIAN_POINT ( 'NONE',  ( 104.6834293286043760, -27.01143314437436160, 56.26782653584942295 ) ) ;
#65771 = ORIENTED_EDGE ( 'NONE', *, *, #49594, .T. ) ;
#65772 = CARTESIAN_POINT ( 'NONE',  ( -148.0533267522752112, 0.000000000000000000, 160.2664750769289697 ) ) ;
#65773 = CARTESIAN_POINT ( 'NONE',  ( 114.4327864602578870, -33.21273682179715792, 16.99951894101997496 ) ) ;
#65774 = EDGE_CURVE ( 'NONE', #88630, #49587, #73981, .T. ) ;
#65775 = VECTOR ( 'NONE', #36100, 1000.000000000000000 ) ;
#65776 = LINE ( 'NONE', #44886, #17439 ) ;
#65777 = EDGE_CURVE ( 'NONE', #40724, #80398, #66978, .T. ) ;
#65778 = DIRECTION ( 'NONE',  ( 1.000000000000000000, 4.299999999999999979E-14, 1.000000000000000078E-15 ) ) ;
#65779 = CARTESIAN_POINT ( 'NONE',  ( 92.12462914090806976, 79.66725693986900581, -74.62294912200620445 ) ) ;
#65780 = ORIENTED_EDGE ( 'NONE', *, *, #20074, .F. ) ;
#65781 = CARTESIAN_POINT ( 'NONE',  ( 97.81305373959743577, -40.51655628150228949, 62.63606721061723448 ) ) ;
#65782 = CARTESIAN_POINT ( 'NONE',  ( 124.4917145262460565, 58.80722411771389346, -39.32846460224703833 ) ) ;
#65783 = EDGE_CURVE ( 'NONE', #14127, #24560, #72507, .T. ) ;
#65784 = VERTEX_POINT ( 'NONE', #52855 ) ;
#65785 = CARTESIAN_POINT ( 'NONE',  ( 108.9848901524495801, -47.61516268848960465, 122.7032443235299723 ) ) ;
#65786 = ORIENTED_EDGE ( 'NONE', *, *, #62941, .F. ) ;
#65787 = CARTESIAN_POINT ( 'NONE',  ( 98.15782025887804707, -38.35683565110198145, 50.90480078045794698 ) ) ;
#65788 = EDGE_CURVE ( 'NONE', #58630, #29906, #4353, .T. ) ;
#65789 = CARTESIAN_POINT ( 'NONE',  ( 102.0296606431220994, -28.79805742369273958, 61.94634521065894717 ) ) ;
#65790 = CARTESIAN_POINT ( 'NONE',  ( 116.3181387014812458, -32.94505625723229514, 15.13562527591094664 ) ) ;
#65791 = CARTESIAN_POINT ( 'NONE',  ( 51.06670390244678970, -32.29483332968568021, 117.4678068554150485 ) ) ;
#65792 = FACE_OUTER_BOUND ( 'NONE', #43373, .T. ) ;
#65793 = CARTESIAN_POINT ( 'NONE',  ( 96.15481094519168437, -38.63223783578033022, 42.45181575210199298 ) ) ;
#65794 = LINE ( 'NONE', #52147, #85881 ) ;
#65795 = VERTEX_POINT ( 'NONE', #3867 ) ;
#65796 = AXIS2_PLACEMENT_3D ( 'NONE', #3073, #24852, #23969 ) ;
#65797 = CARTESIAN_POINT ( 'NONE',  ( 130.0664832912740110, -18.82844715994099971, 239.5838068554170377 ) ) ;
#65798 = ORIENTED_EDGE ( 'NONE', *, *, #53450, .F. ) ;
#65799 = DIRECTION ( 'NONE',  ( 0.000000000000000000, 0.000000000000000000, 1.000000000000000000 ) ) ;
#65800 = AXIS2_PLACEMENT_3D ( 'NONE', #4051, #52608, #30871 ) ;
#65801 = ORIENTED_EDGE ( 'NONE', *, *, #60537, .F. ) ;
#65802 = ORIENTED_EDGE ( 'NONE', *, *, #42935, .T. ) ;
#65803 = CARTESIAN_POINT ( 'NONE',  ( 1.978343425214599878E-14, 0.000000000000000000, 161.5439999999999827 ) ) ;
#65804 = EDGE_CURVE ( 'NONE', #37435, #34937, #79780, .T. ) ;
#65805 = CARTESIAN_POINT ( 'NONE',  ( 114.8736367985563334, -30.83777597042981711, 219.3413395616259720 ) ) ;
#65806 = ADVANCED_FACE ( 'NONE', ( #57933 ), #80625, .F. ) ;
#65807 = CARTESIAN_POINT ( 'NONE',  ( 97.80998548426093464, -40.51326460879650426, 126.6348148350811584 ) ) ;
#65808 = DIRECTION ( 'NONE',  ( 1.000000000000000000, 0.000000000000000000, 0.000000000000000000 ) ) ;
#65809 = CARTESIAN_POINT ( 'NONE',  ( 117.4545169724989648, -37.95830395151629943, 49.73276813305393773 ) ) ;
#65811 = EDGE_CURVE ( 'NONE', #82359, #68139, #46060, .T. ) ;
#65810 = CARTESIAN_POINT ( 'NONE',  ( 112.0656721949375481, -45.48853664962202004, 43.98977015968678472 ) ) ;
#65812 = ORIENTED_EDGE ( 'NONE', *, *, #44313, .F. ) ;
#65813 = CARTESIAN_POINT ( 'NONE',  ( 103.4714990137023278, -27.39756209775824303, 171.3690893672466871 ) ) ;
#65814 = ADVANCED_FACE ( 'NONE', ( #65638 ), #40583, .F. ) ;
#65815 = DIRECTION ( 'NONE',  ( 4.299999999999999979E-14, -1.000000000000000000, 4.400000000000000367E-29 ) ) ;
#65816 = VERTEX_POINT ( 'NONE', #87433 ) ;
#65817 = AXIS2_PLACEMENT_3D ( 'NONE', #83458, #76643, #14428 ) ;
#65818 = CARTESIAN_POINT ( 'NONE',  ( 59.67079009362632291, -0.9310397146383332379, 396.9756252759102040 ) ) ;
#65819 = AXIS2_PLACEMENT_3D ( 'NONE', #1208, #56600, #75716 ) ;
#65820 = CARTESIAN_POINT ( 'NONE',  ( 116.7940759412587539, -39.39156663991244756, 114.6154222936379767 ) ) ;
#65821 = CARTESIAN_POINT ( 'NONE',  ( 105.1150531980676277, -26.51080800785435443, 235.2270538473399313 ) ) ;
#65822 = LINE ( 'NONE', #3606, #67557 ) ;
#65823 = DIRECTION ( 'NONE',  ( 0.000000000000000000, 1.000000000000000000, 0.000000000000000000 ) ) ;
#65824 = DIRECTION ( 'NONE',  ( -2.900000000000000265E-14, 2.000000000000000155E-15, -1.000000000000000000 ) ) ;
#65825 = CARTESIAN_POINT ( 'NONE',  ( 104.7063189284543370, -28.49041042582816630, 224.7209912566489720 ) ) ;
#65828 = B_SPLINE_CURVE_WITH_KNOTS ( 'NONE', 3,
 ( #39256, #75124, #6529, #33784, #61035, #47393, #89212, #81068, #75581, #87862, #46944, #61930, #53749, #5191, #46046, #40139, #89662, #12453, #82407, #20169, #33339, #47843, #12908, #11564, #41039, #88325, #68761, #73778 ),
 .UNSPECIFIED., .F., .F.,
 ( 4, 2, 2, 2, 2, 2, 2, 2, 2, 2, 1, 1, 1, 1, 2, 4 ),
 ( 0.000000000000000000, 0.06250376353546895081, 0.1250075270709379016, 0.1875112906064068663, 0.2500150541418758032, 0.3125188176773447402, 0.3750225812128137326, 0.4375263447482826695, 0.4687782265160169715, 0.4844041673998840669, 0.4922171378418173648, 0.4961236230627839028, 0.4980768656732669775, 0.4990534869785083760, 0.4995417976311288810, 0.5000301082837493860 ),
 .UNSPECIFIED. ) ;
#65827 = CARTESIAN_POINT ( 'NONE',  ( 97.28692064948108964, -31.62807703868918807, 86.93181575210095957 ) ) ;
#65826 = LINE ( 'NONE', #25392, #2638 ) ;
#65829 = CARTESIAN_POINT ( 'NONE',  ( 122.2627588294752030, 73.99831669748220975, 45.79086873724280338 ) ) ;
#65830 = CARTESIAN_POINT ( 'NONE',  ( 103.1890357985451345, -46.49249970849451330, 117.2756252759109543 ) ) ;
#65831 = ORIENTED_EDGE ( 'NONE', *, *, #16353, .F. ) ;
#65832 = CARTESIAN_POINT ( 'NONE',  ( 132.4924365228261536, -20.98954602992296614, 7.829737527534494923 ) ) ;
#65833 = ORIENTED_EDGE ( 'NONE', *, *, #80588, .F. ) ;
#65834 = DIRECTION ( 'NONE',  ( 0.000000000000000000, 1.000000000000000000, 0.000000000000000000 ) ) ;
#65835 = VECTOR ( 'NONE', #41629, 1000.000000000000000 ) ;
#65836 = DIRECTION ( 'NONE',  ( -4.237773401492740281E-14, 1.000000000000000000, 0.000000000000000000 ) ) ;
#65837 = DIRECTION ( 'NONE',  ( 0.000000000000000000, 1.000000000000000000, 0.000000000000000000 ) ) ;
#65838 = ORIENTED_EDGE ( 'NONE', *, *, #24705, .F. ) ;
#65839 = CARTESIAN_POINT ( 'NONE',  ( 97.53193540606868339, -39.74924357547732967, 51.57055488991837677 ) ) ;
#65841 = ORIENTED_EDGE ( 'NONE', *, *, #30339, .T. ) ;
#65840 = CARTESIAN_POINT ( 'NONE',  ( 97.89382931228060158, -31.60946541130721954, 110.9213395616259703 ) ) ;
#65842 = DIRECTION ( 'NONE',  ( 0.8660254037844380415, 0.5000000000000012212, -1.550000000000001284E-14 ) ) ;
#65843 = DIRECTION ( 'NONE',  ( 0.000000000000000000, 0.000000000000000000, -1.000000000000000000 ) ) ;
#65844 = CARTESIAN_POINT ( 'NONE',  ( 56.06670390244699576, -67.87844715994098976, 120.2178068554179902 ) ) ;
#65845 = VERTEX_POINT ( 'NONE', #18376 ) ;
#65846 = CARTESIAN_POINT ( 'NONE',  ( 114.7877796877764922, -44.67155160988957618, 118.2022919425779719 ) ) ;
#65847 = DIRECTION ( 'NONE',  ( 3.745918078535842888E-15, 0.000000000000000000, -1.000000000000000000 ) ) ;
#65848 = CARTESIAN_POINT ( 'NONE',  ( 162.9033555647770015, -33.89581943344391135, -5.074374724088000832 ) ) ;
#65849 = FACE_OUTER_BOUND ( 'NONE', #32252, .T. ) ;
#65850 = CARTESIAN_POINT ( 'NONE',  ( 107.0664832912739399, -36.72944715994095333, 299.5571190294419921 ) ) ;
#65851 = FACE_OUTER_BOUND ( 'NONE', #71529, .T. ) ;
#65852 = VERTEX_POINT ( 'NONE', #85666 ) ;
#65853 = ORIENTED_EDGE ( 'NONE', *, *, #26281, .F. ) ;
#65854 = DIRECTION ( 'NONE',  ( 0.000000000000000000, 1.000000000000000000, -0.000000000000000000 ) ) ;
#65855 = DIRECTION ( 'NONE',  ( 1.000000000000000000, 0.000000000000000000, -2.505701470911820065E-15 ) ) ;
#65856 = LINE ( 'NONE', #32232, #79303 ) ;
#65858 = DIRECTION ( 'NONE',  ( -3.100000000000000258E-29, 3.100000000000000044E-14, 1.000000000000000000 ) ) ;
#65857 = CARTESIAN_POINT ( 'NONE',  ( 116.3186249068867539, -32.94868901193379429, 250.1356252759109395 ) ) ;
#65859 = LINE ( 'NONE', #36833, #52317 ) ;
#65860 = CIRCLE ( 'NONE', #7839, 4.875000000000017764 ) ;
#65861 = ORIENTED_EDGE ( 'NONE', *, *, #15384, .T. ) ;
#65862 =( BOUNDED_CURVE ( )  B_SPLINE_CURVE ( 3, ( #85758, #59791, #58022, #23530 ),
 .UNSPECIFIED., .F., .T. ) 
 B_SPLINE_CURVE_WITH_KNOTS ( ( 4, 4 ),
 ( 1.040426005086875085E-11, 1.570796326807755605 ),
 .UNSPECIFIED. ) 
 CURVE ( )  GEOMETRIC_REPRESENTATION_ITEM ( )  RATIONAL_B_SPLINE_CURVE ( ( 1.000000000000000000, 0.8047378541237864003, 0.8047378541237864003, 1.000000000000000000 ) ) 
 REPRESENTATION_ITEM ( '' )  );
#65863 = VECTOR ( 'NONE', #79154, 1000.000000000000000 ) ;
#65864 = EDGE_CURVE ( 'NONE', #41538, #76165, #32005, .T. ) ;
#65865 = CARTESIAN_POINT ( 'NONE',  ( -64.50026246089650783, 54.97499999999996589, 59.61038444174924678 ) ) ;
#65866 = ADVANCED_FACE ( 'NONE', ( #51983 ), #78850, .F. ) ;
#65867 = CARTESIAN_POINT ( 'NONE',  ( 116.6769215743979800, -34.91203320259896259, 154.9756252759109714 ) ) ;
#65869 = VERTEX_POINT ( 'NONE', #79297 ) ;
#65868 = CARTESIAN_POINT ( 'NONE',  ( 142.8679068202682458, 10.65431904611001634, 540.9756252759101471 ) ) ;
#65870 = EDGE_CURVE ( 'NONE', #49327, #81785, #25192, .T. ) ;
#65871 = CARTESIAN_POINT ( 'NONE',  ( 115.8115096128641284, -32.27542772465451293, 40.20133956162496958 ) ) ;
#65872 = CARTESIAN_POINT ( 'NONE',  ( 97.86672743208310976, -40.64957730801459235, 51.64701951407019465 ) ) ;
#65873 = CARTESIAN_POINT ( 'NONE',  ( 184.5667039024486087, -48.82844715993447693, 129.9678068554150059 ) ) ;
#65874 = EDGE_CURVE ( 'NONE', #89527, #8395, #62364, .T. ) ;
#65875 = VERTEX_POINT ( 'NONE', #10667 ) ;
#65876 = LINE ( 'NONE', #46761, #35607 ) ;
#65877 = ORIENTED_EDGE ( 'NONE', *, *, #57843, .F. ) ;
#65878 = ORIENTED_EDGE ( 'NONE', *, *, #56675, .T. ) ;
#65879 = CARTESIAN_POINT ( 'NONE',  ( 104.8455658278054017, -28.15064746346142144, 196.7101547344689720 ) ) ;
#65880 = ADVANCED_FACE ( 'NONE', ( #86992 ), #45608, .T. ) ;
#65881 = CIRCLE ( 'NONE', #54253, 7.143750000000004263 ) ;
#65882 = FACE_OUTER_BOUND ( 'NONE', #63844, .T. ) ;
#65883 = CIRCLE ( 'NONE', #38329, 9.571100913904478702 ) ;
#65884 = AXIS2_PLACEMENT_3D ( 'NONE', #11751, #47138, #73972 ) ;
#65885 = CARTESIAN_POINT ( 'NONE',  ( -100.1374281256141217, 87.79544278253753475, 83.76986456925436642 ) ) ;
#65886 = CIRCLE ( 'NONE', #19473, 11.57110091390449469 ) ;
#65887 = ADVANCED_FACE ( 'NONE', ( #51546 ), #10235, .T. ) ;
#65888 = CARTESIAN_POINT ( 'NONE',  ( 116.3251852747984003, -32.94148267319277323, 269.1356252759109680 ) ) ;
#65889 = DIRECTION ( 'NONE',  ( 0.000000000000000000, 0.000000000000000000, 1.000000000000000000 ) ) ;
#65890 = AXIS2_PLACEMENT_3D ( 'NONE', #86974, #52836, #18359 ) ;
#65891 = ORIENTED_EDGE ( 'NONE', *, *, #78627, .F. ) ;
#65892 = CARTESIAN_POINT ( 'NONE',  ( 25.56670390244816815, -42.82844715994167473, 295.7178068554150059 ) ) ;
#65893 = AXIS2_PLACEMENT_3D ( 'NONE', #2443, #38725, #52764 ) ;
#65894 = CARTESIAN_POINT ( 'NONE',  ( 97.80400447685593690, -40.49859989475246635, 37.63371632713159443 ) ) ;
#65895 = VERTEX_POINT ( 'NONE', #37498 ) ;
#65896 = CARTESIAN_POINT ( 'NONE',  ( 104.8459308146384643, -26.52976224399699134, 260.2470538473397710 ) ) ;
#65897 = CARTESIAN_POINT ( 'NONE',  ( 80.06648329127399677, -41.22944715994105280, 1.625625275910943746 ) ) ;
#65898 = VERTEX_POINT ( 'NONE', #65201 ) ;
#65899 = EDGE_CURVE ( 'NONE', #27672, #63459, #44921, .T. ) ;
#65900 = PLANE ( 'NONE',  #63365 ) ;
#65901 = LINE ( 'NONE', #10500, #89713 ) ;
#65902 = LINE ( 'NONE', #73163, #50487 ) ;
#65903 = CARTESIAN_POINT ( 'NONE',  ( 34.27482367531500529, -30.08671355700301575, -5.074374724088000832 ) ) ;
#65904 = EDGE_CURVE ( 'NONE', #57650, #20562, #37939, .T. ) ;
#65905 = CARTESIAN_POINT ( 'NONE',  ( 106.2987435450237541, -47.16992394167115776, 218.5184824187679453 ) ) ;
#65906 = DIRECTION ( 'NONE',  ( 0.000000000000000000, 0.000000000000000000, -1.000000000000000000 ) ) ;
#65907 = ORIENTED_EDGE ( 'NONE', *, *, #3957, .T. ) ;
#65908 = CARTESIAN_POINT ( 'NONE',  ( 97.73362116697985869, -31.98701483920769206, 46.95276813305393659 ) ) ;
#65909 = CARTESIAN_POINT ( 'NONE',  ( 72.17003668186622178, -9.772340378754034163, -5.074374724089137700 ) ) ;
#65910 = CARTESIAN_POINT ( 'NONE',  ( 100.4512775726424820, -44.84301714363712676, 12.03276813305398463 ) ) ;
#65911 = ORIENTED_EDGE ( 'NONE', *, *, #31518, .T. ) ;
#65912 = CARTESIAN_POINT ( 'NONE',  ( 81.01407827912979087, -16.14703303315387117, 1.764000745017404004 ) ) ;
#65913 = DIRECTION ( 'NONE',  ( 0.000000000000000000, 0.000000000000000000, 1.000000000000000000 ) ) ;
#65914 = CARTESIAN_POINT ( 'NONE',  ( 116.3162492855249894, -32.94856389518969308, 154.1356252759109680 ) ) ;
#65915 = CARTESIAN_POINT ( 'NONE',  ( 108.6369934722860506, -45.24028864696019525, 125.5518998934009574 ) ) ;
#65916 = CARTESIAN_POINT ( 'NONE',  ( 114.6212291911790402, -29.51397259194560263, 230.4327681330539690 ) ) ;
#65917 = FACE_OUTER_BOUND ( 'NONE', #48258, .T. ) ;
#65918 = ORIENTED_EDGE ( 'NONE', *, *, #68840, .T. ) ;
#65919 = ADVANCED_FACE ( 'NONE', ( #19287 ), #8711, .T. ) ;
#65920 = CARTESIAN_POINT ( 'NONE',  ( 135.7780479399384603, -38.88970947304356685, 2.099345637345863658 ) ) ;
#65921 = ORIENTED_EDGE ( 'NONE', *, *, #20497, .F. ) ;
#65922 = EDGE_LOOP ( 'NONE', ( #67953, #27595 ) ) ;
#65923 = VECTOR ( 'NONE', #39932, 1000.000000000000000 ) ;
#65924 = CARTESIAN_POINT ( 'NONE',  ( 180.2143765759500980, -35.91149509760582248, 237.4678068554150059 ) ) ;
#65925 = ORIENTED_EDGE ( 'NONE', *, *, #84066, .T. ) ;
#65926 = EDGE_LOOP ( 'NONE', ( #51102, #77684, #25833, #34372 ) ) ;
#65927 = CARTESIAN_POINT ( 'NONE',  ( 80.06648329127398256, -18.72944715994105991, 14.92562527591094224 ) ) ;
#65928 = VECTOR ( 'NONE', #31659, 1000.000000000000000 ) ;
#65929 = CARTESIAN_POINT ( 'NONE',  ( 142.0664832912739826, -9.729447159940995959, 14.67562527591100441 ) ) ;
#65930 = DIRECTION ( 'NONE',  ( 0.000000000000000000, 1.000000000000000000, 0.000000000000000000 ) ) ;
#65931 = CARTESIAN_POINT ( 'NONE',  ( 108.6382307137633205, -45.64809506003439310, 122.1257531614099747 ) ) ;
#65932 = CARTESIAN_POINT ( 'NONE',  ( 105.3130012014428445, -26.40811315510063295, 15.20991099019697401 ) ) ;
#65933 = VERTEX_POINT ( 'NONE', #12925 ) ;
#65934 = CARTESIAN_POINT ( 'NONE',  ( -90.65754775987979031, 74.81620433377383961, -76.39898589339183843 ) ) ;
#65935 = ORIENTED_EDGE ( 'NONE', *, *, #13025, .F. ) ;
#65936 = EDGE_CURVE ( 'NONE', #31578, #1197, #5662, .T. ) ;
#65937 = CARTESIAN_POINT ( 'NONE',  ( 147.0667039024469886, -67.87844715994090450, 222.2178068554179902 ) ) ;
#65938 = ORIENTED_EDGE ( 'NONE', *, *, #41731, .T. ) ;
#65939 = DIRECTION ( 'NONE',  ( 6.524622321627019585E-16, 3.741823817616790462E-31, 1.000000000000000000 ) ) ;
#65940 = DIRECTION ( 'NONE',  ( -0.9254794337955620787, -0.3787978585227822492, 0.000000000000000000 ) ) ;
#65941 = CARTESIAN_POINT ( 'NONE',  ( 72.06648329127402519, -56.72944715994105991, 14.92562527591093691 ) ) ;
#65942 = EDGE_CURVE ( 'NONE', #2982, #89416, #68331, .T. ) ;
#65944 = VECTOR ( 'NONE', #73166, 1000.000000000000000 ) ;
#65943 = CYLINDRICAL_SURFACE ( 'NONE', #77025, 2.517500000000005844 ) ;
#65945 = EDGE_LOOP ( 'NONE', ( #60149, #75115, #82447, #79569, #70540 ) ) ;
#65946 = CARTESIAN_POINT ( 'NONE',  ( 118.1077515449285613, -36.21032982800684152, 268.8518157521015723 ) ) ;
#65947 = CIRCLE ( 'NONE', #61607, 15.50000000000000000 ) ;
#65948 = CARTESIAN_POINT ( 'NONE',  ( 116.1963150171851851, -43.04653558477239272, 9.356577656862985037 ) ) ;
#65949 = AXIS2_PLACEMENT_3D ( 'NONE', #89010, #26766, #73235 ) ;
#65950 = VECTOR ( 'NONE', #70209, 1000.000000000000000 ) ;
#65952 = CARTESIAN_POINT ( 'NONE',  ( 68.74877429598565470, -139.2496317701004784, 246.2158363995229706 ) ) ;
#65951 = LINE ( 'NONE', #37819, #14349 ) ;
#65953 = CARTESIAN_POINT ( 'NONE',  ( 106.4181540149052694, -25.28825685635689879, 323.5297110109900132 ) ) ;
#65954 = FACE_OUTER_BOUND ( 'NONE', #49578, .T. ) ;
#65955 = CARTESIAN_POINT ( 'NONE',  ( 50.56670390244696733, -18.82844715994099971, 342.9256252759109884 ) ) ;
#65956 = CARTESIAN_POINT ( 'NONE',  ( -41.60202597009397607, 65.59999999999998010, 33.51824159735392783 ) ) ;
#65957 = CYLINDRICAL_SURFACE ( 'NONE', #51504, 2.749999999999974687 ) ;
#65958 = CARTESIAN_POINT ( 'NONE',  ( 102.7370178780992234, -25.64411770250132250, 20.37276813305294354 ) ) ;
#65959 = CARTESIAN_POINT ( 'NONE',  ( 107.2431676328701684, -47.18842012194354396, 208.5899109901969837 ) ) ;
#65960 = CARTESIAN_POINT ( 'NONE',  ( 99.11086226171772751, -44.43615201859483932, 37.95086337114900488 ) ) ;
#65962 = CARTESIAN_POINT ( 'NONE',  ( 109.6430121329437952, -46.48008673454590678, 47.78145860943909895 ) ) ;
#65961 = LINE ( 'NONE', #3753, #5851 ) ;
#65963 = CARTESIAN_POINT ( 'NONE',  ( 82.68053975348409779, -35.85322261660355281, 2.908039740960799868 ) ) ;
#65964 = CIRCLE ( 'NONE', #25387, 2.999999999999929834 ) ;
#65965 = ORIENTED_EDGE ( 'NONE', *, *, #20893, .F. ) ;
#65966 = ADVANCED_FACE ( 'NONE', ( #47412 ), #25642, .T. ) ;
#65967 = CARTESIAN_POINT ( 'NONE',  ( 186.6899999999999977, 52.73749999999999716, -44.45000000000000284 ) ) ;
#65968 = ORIENTED_EDGE ( 'NONE', *, *, #6516, .T. ) ;
#65969 = EDGE_CURVE ( 'NONE', #27146, #52484, #87027, .T. ) ;
#65970 = CARTESIAN_POINT ( 'NONE',  ( 97.58158007118578325, -32.53714515026965870, 51.98324432352896451 ) ) ;
#65972 = EDGE_LOOP ( 'NONE', ( #72530, #65645, #2047, #21013 ) ) ;
#65971 = CARTESIAN_POINT ( 'NONE',  ( 2.820233448801842346, 94.93988138122190890, 130.5258113771150192 ) ) ;
#65973 = CARTESIAN_POINT ( 'NONE',  ( 50.56670390244699576, -18.82844715994031048, -5.074374724088000832 ) ) ;
#65974 = EDGE_CURVE ( 'NONE', #28680, #62123, #75140, .T. ) ;
#65975 = CARTESIAN_POINT ( 'NONE',  ( 117.1710321396410421, -41.15233254730026147, 204.4861014663869696 ) ) ;
#65976 = CARTESIAN_POINT ( 'NONE',  ( 99.50407054466384693, -43.30503144106609881, 252.8967269992471358 ) ) ;
#65977 = CARTESIAN_POINT ( 'NONE',  ( 110.8545073367433105, -45.98422289188966516, 147.8856283147305248 ) ) ;
#65978 = PLANE ( 'NONE',  #70449 ) ;
#65979 = CARTESIAN_POINT ( 'NONE',  ( 119.2563820928116343, -93.81616114448401333, -21.02845593540860492 ) ) ;
#65980 = CARTESIAN_POINT ( 'NONE',  ( 132.9844404253383630, -39.25772566032902944, 1.807989669955520684 ) ) ;
#65981 = EDGE_CURVE ( 'NONE', #30848, #26828, #40614, .T. ) ;
#65982 = CARTESIAN_POINT ( 'NONE',  ( -83.41556370846475943, 78.46683822717000112, 100.4327019155588090 ) ) ;
#65983 = CARTESIAN_POINT ( 'NONE',  ( 98.99072789581755671, -31.21169308021397981, 120.8499109901969604 ) ) ;
#65984 = ORIENTED_EDGE ( 'NONE', *, *, #13499, .T. ) ;
#65985 = VERTEX_POINT ( 'NONE', #54660 ) ;
#65986 = CIRCLE ( 'NONE', #10887, 3.814291549405317117 ) ;
#65987 = CARTESIAN_POINT ( 'NONE',  ( 109.6943014565619450, -45.19247559555673632, 94.24729759161093057 ) ) ;
#65988 = EDGE_CURVE ( 'NONE', #13052, #80177, #24635, .T. ) ;
#65989 = CARTESIAN_POINT ( 'NONE',  ( 80.06648329127399677, -8.729447159940999512, 4.925625275911999168 ) ) ;
#65991 = LINE ( 'NONE', #16970, #28828 ) ;
#65990 = CARTESIAN_POINT ( 'NONE',  ( 107.2322476904470108, -46.54200526979089858, 208.5899109901959605 ) ) ;
#65992 = DIRECTION ( 'NONE',  ( 4.299999999999999979E-14, -1.000000000000000000, 0.000000000000000000 ) ) ;
#65993 = PLANE ( 'NONE',  #62630 ) ;
#65994 = EDGE_CURVE ( 'NONE', #44882, #26742, #89229, .T. ) ;
#65995 = CARTESIAN_POINT ( 'NONE',  ( 118.3250318368774856, 72.22378176823140450, 7.404816947595408649 ) ) ;
#65996 = CARTESIAN_POINT ( 'NONE',  ( -11.39405732433012375, 76.92513621822203618, 118.0073709438022576 ) ) ;
#65997 = DIRECTION ( 'NONE',  ( -0.000000000000000000, 1.000000000000000000, -0.000000000000000000 ) ) ;
#65998 = CARTESIAN_POINT ( 'NONE',  ( 57.14999999999999858, 95.25000000000000000, 326.2630000000000337 ) ) ;
#65999 = CARTESIAN_POINT ( 'NONE',  ( 108.2752786314947429, -47.69320359391970499, 157.6518157521019532 ) ) ;
#66000 = ORIENTED_EDGE ( 'NONE', *, *, #49367, .F. ) ;
#66001 = VERTEX_POINT ( 'NONE', #76030 ) ;
#66002 = PLANE ( 'NONE',  #61853 ) ;
#66003 = CARTESIAN_POINT ( 'NONE',  ( 71.24189083761805819, -0.9290567490904538817, 361.9756252759101471 ) ) ;
#66004 = DIRECTION ( 'NONE',  ( 2.170915417798913171E-16, 0.000000000000000000, 1.000000000000000000 ) ) ;
#66005 = DIRECTION ( 'NONE',  ( 0.000000000000000000, -1.000000000000000000, 0.000000000000000000 ) ) ;
#66006 = VECTOR ( 'NONE', #50232, 1000.000000000000000 ) ;
#66007 = CIRCLE ( 'NONE', #68892, 3.174999999999997158 ) ;
#66008 = CARTESIAN_POINT ( 'NONE',  ( 117.0718958548293784, -35.46248428096206595, 269.9272917895399360 ) ) ;
#66009 = AXIS2_PLACEMENT_3D ( 'NONE', #27571, #5794, #47989 ) ;
#66010 = AXIS2_PLACEMENT_3D ( 'NONE', #69166, #62343, #55955 ) ;
#66011 = CARTESIAN_POINT ( 'NONE',  ( 98.66574799139598895, -30.49618532553466110, 180.8184824187679567 ) ) ;
#66012 = LINE ( 'NONE', #74188, #13954 ) ;
#66013 = ORIENTED_EDGE ( 'NONE', *, *, #71441, .F. ) ;
#66015 = EDGE_LOOP ( 'NONE', ( #73843, #11760, #14627, #13169 ) ) ;
#66014 = ORIENTED_EDGE ( 'NONE', *, *, #36211, .T. ) ;
#66016 = CIRCLE ( 'NONE', #79085, 2.749999999999974687 ) ;
#66017 = CARTESIAN_POINT ( 'NONE',  ( -6.364907348149458244, 71.52879593750107290, 118.3870396030140029 ) ) ;
#66018 = PLANE ( 'NONE',  #56473 ) ;
#66019 = CARTESIAN_POINT ( 'NONE',  ( 131.5867845949809691, -35.53883969338462379, 7.103318745415927893 ) ) ;
#66020 = CARTESIAN_POINT ( 'NONE',  ( 105.4026065362546802, -27.48239143091520020, 271.6377737820876632 ) ) ;
#66021 = AXIS2_PLACEMENT_3D ( 'NONE', #71107, #55183, #76105 ) ;
#66022 = DIRECTION ( 'NONE',  ( 1.346944695195362088E-15, -1.000000000000000000, 3.469446951953620425E-31 ) ) ;
#66023 = ORIENTED_EDGE ( 'NONE', *, *, #50108, .T. ) ;
#66024 = EDGE_CURVE ( 'NONE', #31809, #46288, #36253, .T. ) ;
#66025 = VECTOR ( 'NONE', #10473, 1000.000000000000000 ) ;
#66026 = LINE ( 'NONE', #46011, #45074 ) ;
#66027 = PLANE ( 'NONE',  #76392 ) ;
#66028 = VERTEX_POINT ( 'NONE', #88784 ) ;
#66029 = ORIENTED_EDGE ( 'NONE', *, *, #77614, .T. ) ;
#66030 = CARTESIAN_POINT ( 'NONE',  ( 152.0371591254585724, -47.82818131005588214, 129.9678068554149775 ) ) ;
#66031 = EDGE_LOOP ( 'NONE', ( #61712, #54588, #10607, #76036 ) ) ;
#66032 = ORIENTED_EDGE ( 'NONE', *, *, #13872, .T. ) ;
#66033 = CARTESIAN_POINT ( 'NONE',  ( 97.33768314765630691, -34.07170803572551421, 157.1146345946560530 ) ) ;
#66034 = VECTOR ( 'NONE', #5198, 1000.000000000000000 ) ;
#66035 = CARTESIAN_POINT ( 'NONE',  ( 101.0819131387675611, -42.86434890131523900, 21.38384839950496641 ) ) ;
#66036 = CARTESIAN_POINT ( 'NONE',  ( 100.6239562591623695, -26.75308202300568539, 220.5327681330539633 ) ) ;
#66037 = CARTESIAN_POINT ( 'NONE',  ( 118.8526415125689937, -37.69623653580512723, 188.7613395616259595 ) ) ;
#66038 = DIRECTION ( 'NONE',  ( 0.000000000000000000, 1.000000000000000000, 0.000000000000000000 ) ) ;
#66039 = CARTESIAN_POINT ( 'NONE',  ( 96.24939603668094890, -34.45687069020234361, 257.1737205140064475 ) ) ;
#66040 = DIRECTION ( 'NONE',  ( 0.000000000000000000, 0.000000000000000000, 1.000000000000000000 ) ) ;
#66041 = CARTESIAN_POINT ( 'NONE',  ( 75.31670390244798341, -57.40094715994099772, 60.91780685541480267 ) ) ;
#66042 = ORIENTED_EDGE ( 'NONE', *, *, #40222, .F. ) ;
#66043 = ORIENTED_EDGE ( 'NONE', *, *, #42587, .F. ) ;
#66044 = CIRCLE ( 'NONE', #24003, 0.5000000000000004441 ) ;
#66045 = EDGE_CURVE ( 'NONE', #12494, #71312, #65237, .T. ) ;
#66046 = CARTESIAN_POINT ( 'NONE',  ( 118.8398422492546018, -38.46634565031615693, 223.7099109901969598 ) ) ;
#66047 = ORIENTED_EDGE ( 'NONE', *, *, #64075, .F. ) ;
#66048 = CARTESIAN_POINT ( 'NONE',  ( 109.8560245667294311, -26.68427469084152293, 174.8613395616249591 ) ) ;
#66049 = CARTESIAN_POINT ( 'NONE',  ( 131.5667039024470455, -104.2784471599409244, 23.21780685541800082 ) ) ;
#66050 = AXIS2_PLACEMENT_3D ( 'NONE', #49641, #77366, #1524 ) ;
#66051 = DIRECTION ( 'NONE',  ( -0.7071067811734105257, 0.7071067811996846197, 0.000000000000000000 ) ) ;
#66052 = FACE_OUTER_BOUND ( 'NONE', #60165, .T. ) ;
#66053 = CARTESIAN_POINT ( 'NONE',  ( 143.5298718395760602, -139.6521136699046792, 247.2811342184976695 ) ) ;
#66054 = B_SPLINE_CURVE_WITH_KNOTS ( 'NONE', 3,
 ( #46747, #11809, #53999, #13154, #26760, #66760, #74479, #80408, #5443, #53552, #53094, #67664, #4546, #59931, #81757, #33139, #19508, #68563, #40835, #11353, #18615, #47190, #25425, #74930, #68113 ),
 .UNSPECIFIED., .F., .F.,
 ( 4, 2, 2, 2, 2, 2, 2, 2, 2, 1, 2, 2, 4 ),
 ( 0.05960646776571127542, 0.06208810814592213845, 0.06332892833602757343, 0.06456974852613300841, 0.06705138890634392002, 0.06829220909644936888, 0.06953302928655483162, 0.07201466966676572934, 0.07325548985687117820, 0.07449631004697662706, 0.07573713023708206205, 0.07697795042718751091, 0.07945959080739838087 ),
 .UNSPECIFIED. ) ;
#66057 = CARTESIAN_POINT ( 'NONE',  ( 110.8002664325828164, -46.40403567634503901, 13.85753003781498016 ) ) ;
#66056 = DIRECTION ( 'NONE',  ( 1.000000000000000000, 0.000000000000000000, 0.000000000000000000 ) ) ;
#66055 = DIRECTION ( 'NONE',  ( -4.237773401492740281E-14, 1.000000000000000000, 0.000000000000000000 ) ) ;
#66058 = CARTESIAN_POINT ( 'NONE',  ( 107.0664832912739968, -36.72944715994100306, 293.2242906452868851 ) ) ;
#66059 = CARTESIAN_POINT ( 'NONE',  ( 85.06670390244700286, -71.37844715994096134, 222.2178068554179902 ) ) ;
#66060 = CARTESIAN_POINT ( 'NONE',  ( 164.9212702847350442, -29.73316016639542170, 342.9256252759109884 ) ) ;
#66061 = CARTESIAN_POINT ( 'NONE',  ( 107.0664832912739968, -36.72944715994100306, 287.6356252759109680 ) ) ;
#66062 = DIRECTION ( 'NONE',  ( 0.000000000000000000, 0.000000000000000000, 1.000000000000000000 ) ) ;
#66063 = CARTESIAN_POINT ( 'NONE',  ( 162.5667039024470171, -32.29483332968611364, -5.074374724088000832 ) ) ;
#66065 = ORIENTED_EDGE ( 'NONE', *, *, #16917, .T. ) ;
#66064 = CARTESIAN_POINT ( 'NONE',  ( 100.1227369335950215, -41.05608255646721005, 195.5838068554172935 ) ) ;
#66066 = CARTESIAN_POINT ( 'NONE',  ( 126.9629299006807059, -54.68655584847603279, 14.92562527591094579 ) ) ;
#66067 = CARTESIAN_POINT ( 'NONE',  ( 97.40467406345878487, -42.14653896106843689, 181.7451490854349743 ) ) ;
#66068 = CARTESIAN_POINT ( 'NONE',  ( 109.6838526317122273, -47.46831852615197533, 83.75467289495897205 ) ) ;
#66069 = CARTESIAN_POINT ( 'NONE',  ( 118.0968619800241299, -35.49322535880637020, 229.9032443235299468 ) ) ;
#66070 = LINE ( 'NONE', #74687, #35856 ) ;
#66071 = DIRECTION ( 'NONE',  ( 0.000000000000000000, 0.000000000000000000, 1.000000000000000000 ) ) ;
#66073 = CARTESIAN_POINT ( 'NONE',  ( 99.41715255677500807, -43.19881440323307231, 37.88476161017977972 ) ) ;
#66072 = DIRECTION ( 'NONE',  ( 1.000000000000000000, 1.000000000000000078E-15, 0.000000000000000000 ) ) ;
#66074 = FACE_OUTER_BOUND ( 'NONE', #58846, .T. ) ;
#66075 = FACE_OUTER_BOUND ( 'NONE', #80046, .T. ) ;
#66076 = CARTESIAN_POINT ( 'NONE',  ( 97.75843116786518294, -40.38500386429194577, 66.62475028590972670 ) ) ;
#66077 = CIRCLE ( 'NONE', #58814, 24.63800000000000168 ) ;
#66078 = AXIS2_PLACEMENT_3D ( 'NONE', #40062, #88691, #47763 ) ;
#66079 = CIRCLE ( 'NONE', #10970, 0.5000000000000031086 ) ;
#66080 = ORIENTED_EDGE ( 'NONE', *, *, #3551, .T. ) ;
#66081 = ORIENTED_EDGE ( 'NONE', *, *, #22960, .F. ) ;
#66082 = ADVANCED_FACE ( 'NONE', ( #53769 ), #13808, .T. ) ;
#66083 = VECTOR ( 'NONE', #56588, 1000.000000000000114 ) ;
#66084 = CARTESIAN_POINT ( 'NONE',  ( 115.6929481903037100, -41.18531195142565338, 92.86956268521994673 ) ) ;
#66086 = EDGE_LOOP ( 'NONE', ( #85928, #35514, #12990, #22562 ) ) ;
#66085 = DIRECTION ( 'NONE',  ( 0.000000000000000000, 0.000000000000000000, 1.000000000000000000 ) ) ;
#66087 = ADVANCED_FACE ( 'NONE', ( #81534 ), #18834, .T. ) ;
#66088 = CARTESIAN_POINT ( 'NONE',  ( 95.51222647996985415, -34.21005103128004521, 102.1556252759109640 ) ) ;
#66089 = DIRECTION ( 'NONE',  ( 0.000000000000000000, -1.000000000000000000, 0.000000000000000000 ) ) ;
#66090 = EDGE_CURVE ( 'NONE', #88057, #68436, #26069, .T. ) ;
#66091 = AXIS2_PLACEMENT_3D ( 'NONE', #58283, #16514, #37851 ) ;
#66092 = DIRECTION ( 'NONE',  ( 1.000000000000000000, 0.000000000000000000, 0.000000000000000000 ) ) ;
#66093 = CARTESIAN_POINT ( 'NONE',  ( 97.06107109313440162, -37.99641192960685032, 177.4272919398598560 ) ) ;
#66094 = EDGE_CURVE ( 'NONE', #27069, #67994, #69224, .T. ) ;
#66096 = CARTESIAN_POINT ( 'NONE',  ( 101.9462936730086113, -46.59842863024385196, 17.19562527591095247 ) ) ;
#66095 = VECTOR ( 'NONE', #22221, 999.9999999999998863 ) ;
#66097 = ORIENTED_EDGE ( 'NONE', *, *, #34809, .T. ) ;
#66098 = ORIENTED_EDGE ( 'NONE', *, *, #14236, .F. ) ;
#66099 = EDGE_LOOP ( 'NONE', ( #67713, #32170, #86945, #57316 ) ) ;
#66100 = PLANE ( 'NONE',  #9424 ) ;
#66102 = CARTESIAN_POINT ( 'NONE',  ( 123.6837132603319702, -55.86395651782485317, 219.5838068554170093 ) ) ;
#66101 = CARTESIAN_POINT ( 'NONE',  ( 98.54774150848832903, -41.53511815344519675, 132.7356252759109623 ) ) ;
#66103 = DIRECTION ( 'NONE',  ( 0.000000000000000000, 0.000000000000000000, 1.000000000000000000 ) ) ;
#66104 = CIRCLE ( 'NONE', #57419, 7.937500000000000000 ) ;
#66105 = LINE ( 'NONE', #16638, #69361 ) ;
#66106 = CARTESIAN_POINT ( 'NONE',  ( 5.635138049808393390, 71.13823012824934722, -130.4366002064613212 ) ) ;
#66107 = ADVANCED_FACE ( 'NONE', ( #12470 ), #74252, .T. ) ;
#66108 = DIRECTION ( 'NONE',  ( -7.723290606088049820E-15, 0.000000000000000000, 1.000000000000000000 ) ) ;
#66109 = CARTESIAN_POINT ( 'NONE',  ( -7.735609141604705030, 92.62441004919340060, 130.3265751744775400 ) ) ;
#66110 = CARTESIAN_POINT ( 'NONE',  ( 63.06670390244707392, -40.32844715994016838, 180.4678068554151196 ) ) ;
#66111 = CARTESIAN_POINT ( 'NONE',  ( 105.9906760191434358, -26.38192068051316141, 50.15848241876796720 ) ) ;
#66112 = ORIENTED_EDGE ( 'NONE', *, *, #41864, .T. ) ;
#66113 = EDGE_LOOP ( 'NONE', ( #3041, #66644 ) ) ;
#66114 = CARTESIAN_POINT ( 'NONE',  ( -479.3614999999999782, 104.7749999999999915, 101.5999999999999943 ) ) ;
#66115 = CARTESIAN_POINT ( 'NONE',  ( 126.7715183016628657, 47.48007084238671638, 31.20684018435030538 ) ) ;
#66116 = FACE_OUTER_BOUND ( 'NONE', #81737, .T. ) ;
#66117 = CARTESIAN_POINT ( 'NONE',  ( 114.6841822258597148, -33.79680514827971649, 136.9366617981629588 ) ) ;
#66118 = AXIS2_PLACEMENT_3D ( 'NONE', #81491, #52377, #66939 ) ;
#66119 = CARTESIAN_POINT ( 'NONE',  ( 59.67078992371373403, -0.9290567490904538817, 540.9756252759101471 ) ) ;
#66120 = ORIENTED_EDGE ( 'NONE', *, *, #76853, .F. ) ;
#66121 = EDGE_LOOP ( 'NONE', ( #30888, #85117, #224, #63616 ) ) ;
#66122 = CARTESIAN_POINT ( 'NONE',  ( 44.45000000000000284, 114.2999999999999972, 275.4630000000000223 ) ) ;
#66123 = EDGE_LOOP ( 'NONE', ( #32854, #47080, #9404, #25303 ) ) ;
#66124 = ORIENTED_EDGE ( 'NONE', *, *, #14142, .T. ) ;
#66125 = DIRECTION ( 'NONE',  ( -8.673617379884035472E-16, -1.000000000000000000, 0.000000000000000000 ) ) ;
#66126 = CARTESIAN_POINT ( 'NONE',  ( 112.5904859203986206, -43.69705252635404236, 164.5415833058969781 ) ) ;
#66127 = LINE ( 'NONE', #18887, #25461 ) ;
#66128 = VECTOR ( 'NONE', #16330, 1000.000000000000000 ) ;
#66129 = ADVANCED_FACE ( 'NONE', ( #50099 ), #22425, .F. ) ;
#66130 = DIRECTION ( 'NONE',  ( 0.000000000000000000, 0.000000000000000000, 1.000000000000000000 ) ) ;
#66131 = DIRECTION ( 'NONE',  ( 0.000000000000000000, 0.000000000000000000, 1.000000000000000000 ) ) ;
#66132 = AXIS2_PLACEMENT_3D ( 'NONE', #54137, #12390, #19647 ) ;
#66133 = ORIENTED_EDGE ( 'NONE', *, *, #88470, .F. ) ;
#66134 = VECTOR ( 'NONE', #84579, 1000.000000000000000 ) ;
#66135 = VECTOR ( 'NONE', #26676, 1000.000000000000000 ) ;
#66136 = EDGE_LOOP ( 'NONE', ( #12932, #53844, #70248, #16337 ) ) ;
#66137 = VERTEX_POINT ( 'NONE', #28314 ) ;
#66138 = EDGE_CURVE ( 'NONE', #10255, #36562, #76837, .T. ) ;
#66139 = CARTESIAN_POINT ( 'NONE',  ( 107.2048247310825388, -44.91868093929326022, 210.4080903695909512 ) ) ;
#66140 = CARTESIAN_POINT ( 'NONE',  ( 116.9427733469681385, -33.21558069166144378, 114.0984824187679720 ) ) ;
#66141 = CARTESIAN_POINT ( 'NONE',  ( 107.1951288810177090, -26.32694189238797833, 35.06705384733893283 ) ) ;
#66142 = PRESENTATION_STYLE_ASSIGNMENT (( #85413 ) ) ;
#66143 = CARTESIAN_POINT ( 'NONE',  ( 91.91125933621951560, -96.57698625956682292, -11.78219314458225853 ) ) ;
#66144 = DIRECTION ( 'NONE',  ( 0.000000000000000000, 0.000000000000000000, 1.000000000000000000 ) ) ;
#66145 = CARTESIAN_POINT ( 'NONE',  ( 109.8559662660393172, -26.68448463234438606, 170.8613395616249591 ) ) ;
#66146 = CARTESIAN_POINT ( 'NONE',  ( -479.3614999999999782, 21.43125000000035030, 6.988054014476359654 ) ) ;
#66147 = ORIENTED_EDGE ( 'NONE', *, *, #9282, .F. ) ;
#66148 = DIRECTION ( 'NONE',  ( 0.000000000000000000, 1.000000000000000000, -0.000000000000000000 ) ) ;
#66149 = ORIENTED_EDGE ( 'NONE', *, *, #66094, .F. ) ;
#66150 = EDGE_LOOP ( 'NONE', ( #235, #60006, #52899, #69830, #55373, #42028, #32066, #4810, #19490, #530, #38523, #87786, #13984 ) ) ;
#66151 = CARTESIAN_POINT ( 'NONE',  ( 97.81169818311565223, -40.51742792548894556, 86.63555527419073599 ) ) ;
#66152 = CARTESIAN_POINT ( 'NONE',  ( 91.91229609755362162, -96.60849280716382737, -19.21046202161324956 ) ) ;
#66153 = ORIENTED_EDGE ( 'NONE', *, *, #74293, .F. ) ;
#66154 = PLANE ( 'NONE',  #83820 ) ;
#66155 = EDGE_CURVE ( 'NONE', #84840, #39332, #56007, .T. ) ;
#66156 = VERTEX_POINT ( 'NONE', #77835 ) ;
#66157 = FACE_OUTER_BOUND ( 'NONE', #79222, .T. ) ;
#66158 = CARTESIAN_POINT ( 'NONE',  ( 101.9604343285081569, -27.64015156285208974, 60.48419670448296159 ) ) ;
#66159 = LINE ( 'NONE', #81171, #82331 ) ;
#66160 = CIRCLE ( 'NONE', #44433, 14.00000000000000888 ) ;
#66161 = CARTESIAN_POINT ( 'NONE',  ( 138.8167039024479834, -50.82844715994100682, 60.91780685541480267 ) ) ;
#66162 = CARTESIAN_POINT ( 'NONE',  ( 99.08946256649487339, -99.09543445804985140, -19.78219314458218392 ) ) ;
#66163 = CARTESIAN_POINT ( 'NONE',  ( 99.36524671511898532, -42.81259845621070781, 91.85848241876892928 ) ) ;
#66165 = CARTESIAN_POINT ( 'NONE',  ( 101.2129617469313132, -45.32973500739954886, 193.1013395616249682 ) ) ;
#66164 = CARTESIAN_POINT ( 'NONE',  ( 72.06648329127393993, -45.72944715994110965, 14.82207188531764253 ) ) ;
#66166 = DIRECTION ( 'NONE',  ( 0.000000000000000000, 0.000000000000000000, -1.000000000000000000 ) ) ;
#66167 = CARTESIAN_POINT ( 'NONE',  ( 142.8682495647594806, 8.654319075478467127, 394.9756252759102040 ) ) ;
#66168 = EDGE_LOOP ( 'NONE', ( #72815, #31172, #78444, #61981, #21995, #88797 ) ) ;
#66169 = DIRECTION ( 'NONE',  ( -0.7071067811865660024, 8.659560562355160888E-17, 0.7071067811865291430 ) ) ;
#66170 = DIRECTION ( 'NONE',  ( 0.000000000000000000, 0.000000000000000000, -1.000000000000000000 ) ) ;
#66171 = LINE ( 'NONE', #80724, #61851 ) ;
#66172 = ADVANCED_FACE ( 'NONE', ( #56468 ), #84216, .F. ) ;
#66173 = CARTESIAN_POINT ( 'NONE',  ( 25.56670390244832447, -48.82844715994168183, 257.2178068554150059 ) ) ;
#66175 = ORIENTED_EDGE ( 'NONE', *, *, #89403, .T. ) ;
#66174 = CARTESIAN_POINT ( 'NONE',  ( 97.36106687025375095, -40.65520290104787904, 206.6327681330539860 ) ) ;
#66176 = DIRECTION ( 'NONE',  ( -4.237773401492740281E-14, 1.000000000000000000, 0.000000000000000000 ) ) ;
#66177 = CARTESIAN_POINT ( 'NONE',  ( 100.7369725318012570, -45.81913908486538389, 233.0803871806729717 ) ) ;
#66178 = CARTESIAN_POINT ( 'NONE',  ( 103.1892778894433320, -46.49189014610453086, 113.2756252759109827 ) ) ;
#66179 = CARTESIAN_POINT ( 'NONE',  ( 3.175000000000334666, 104.3431970271541616, -31.75000000000000000 ) ) ;
#66180 = CARTESIAN_POINT ( 'NONE',  ( 81.24992100026079811, -39.21189388395703190, 8.006199623928925035 ) ) ;
#66181 = DIRECTION ( 'NONE',  ( 4.299999999999999979E-14, -1.000000000000000000, 4.400000000000000367E-29 ) ) ;
#66182 = LINE ( 'NONE', #59370, #26234 ) ;
#66183 = ORIENTED_EDGE ( 'NONE', *, *, #77021, .F. ) ;
#66184 = ORIENTED_EDGE ( 'NONE', *, *, #87464, .F. ) ;
#66185 = ORIENTED_EDGE ( 'NONE', *, *, #68772, .T. ) ;
#66186 = ORIENTED_EDGE ( 'NONE', *, *, #80783, .T. ) ;
#66187 = CARTESIAN_POINT ( 'NONE',  ( 117.0718954856852321, -35.46248235822151429, 73.92729194242146207 ) ) ;
#66188 = CARTESIAN_POINT ( 'NONE',  ( 111.7736368399375522, -46.73334422087322082, 283.9146728949585849 ) ) ;
#66189 = LINE ( 'NONE', #38489, #41743 ) ;
#66190 = CARTESIAN_POINT ( 'NONE',  ( 41.56648329127398966, -27.82844715994070484, 195.9256252759119832 ) ) ;
#66191 = ADVANCED_FACE ( 'NONE', ( #15612 ), #56922, .F. ) ;
#66193 = CARTESIAN_POINT ( 'NONE',  ( 68.58297366894557001, -139.1947169264394688, 246.0943807925750093 ) ) ;
#66192 = CARTESIAN_POINT ( 'NONE',  ( 150.5667039024473297, -25.42844715993594562, 300.4678068554149490 ) ) ;
#66194 = CIRCLE ( 'NONE', #89438, 29.49999999999998579 ) ;
#66195 = CARTESIAN_POINT ( 'NONE',  ( 115.5432862745613676, -35.46615253551063063, 218.3667055423629790 ) ) ;
#66196 = VERTEX_POINT ( 'NONE', #71025 ) ;
#66197 = ORIENTED_EDGE ( 'NONE', *, *, #9742, .T. ) ;
#66198 = VECTOR ( 'NONE', #20107, 1000.000000000000000 ) ;
#66199 = VERTEX_POINT ( 'NONE', #62841 ) ;
#66200 = AXIS2_PLACEMENT_3D ( 'NONE', #38244, #73201, #65940 ) ;
#66201 = CIRCLE ( 'NONE', #16886, 2.030000000000003801 ) ;
#66202 = DIRECTION ( 'NONE',  ( 1.000000000000000000, 0.000000000000000000, 0.000000000000000000 ) ) ;
#66203 = CIRCLE ( 'NONE', #37182, 4.762500000000002842 ) ;
#66204 = CARTESIAN_POINT ( 'NONE',  ( 110.8542088300284263, -45.98434506554588097, 182.8856026504752492 ) ) ;
#66205 = DIRECTION ( 'NONE',  ( 0.000000000000000000, 0.000000000000000000, -1.000000000000000000 ) ) ;
#66206 = CARTESIAN_POINT ( 'NONE',  ( 100.2657625843003899, -43.21224928579215430, 33.35205949637398959 ) ) ;
#66207 = CARTESIAN_POINT ( 'NONE',  ( 118.1262036371151680, 90.29828471680512791, 10.09645181158910354 ) ) ;
#66208 = EDGE_CURVE ( 'NONE', #10101, #44089, #15157, .T. ) ;
#66209 = DIRECTION ( 'NONE',  ( 3.999999999999999995E-14, -1.000000000000000000, 4.100000000000000342E-29 ) ) ;
#66210 = EDGE_CURVE ( 'NONE', #37176, #12768, #76483, .T. ) ;
#66211 = CARTESIAN_POINT ( 'NONE',  ( 0.000000000000000000, 184.0000000000000000, 101.0189074266571794 ) ) ;
#66212 = ORIENTED_EDGE ( 'NONE', *, *, #72403, .T. ) ;
#66213 = DIRECTION ( 'NONE',  ( -0.7071067708032339194, -0.0001211784769831122661, 0.7071067811865472397 ) ) ;
#66214 = ORIENTED_EDGE ( 'NONE', *, *, #67706, .T. ) ;
#66215 = AXIS2_PLACEMENT_3D ( 'NONE', #72859, #31963, #74647 ) ;
#66216 = DIRECTION ( 'NONE',  ( 0.000000000000000000, 1.000000000000000000, 0.000000000000000000 ) ) ;
#66217 = CARTESIAN_POINT ( 'NONE',  ( 101.5184502652259084, -42.71685524349225460, 44.79951894101996857 ) ) ;
#66218 = VECTOR ( 'NONE', #39784, 1000.000000000000114 ) ;
#66219 = CARTESIAN_POINT ( 'NONE',  ( 134.0664832912739826, -15.97944715994100306, 8.225625275910998013 ) ) ;
#66220 = CARTESIAN_POINT ( 'NONE',  ( 241.3336515812914911, 65.43750000000000000, -2.032000000000000028 ) ) ;
#66221 = CARTESIAN_POINT ( 'NONE',  ( -9.568504969587623421, 90.94163949856141471, 118.1706967199356626 ) ) ;
#66222 = EDGE_LOOP ( 'NONE', ( #38303, #34290, #66519, #74629, #80265 ) ) ;
#66223 = CARTESIAN_POINT ( 'NONE',  ( 143.5667039024469886, -68.87844715994090450, 222.2178068554179902 ) ) ;
#66224 = CARTESIAN_POINT ( 'NONE',  ( 120.7589990805706037, 58.78128315956222139, -49.62150920525567699 ) ) ;
#66225 = EDGE_LOOP ( 'NONE', ( #78, #9353, #7667 ) ) ;
#66226 = CARTESIAN_POINT ( 'NONE',  ( 117.1637410210353210, -34.13475704353096063, 124.0270538473399426 ) ) ;
#66227 = ORIENTED_EDGE ( 'NONE', *, *, #66374, .F. ) ;
#66228 = CARTESIAN_POINT ( 'NONE',  ( 98.75910798445569583, -38.71530899645634349, 55.93527697093397677 ) ) ;
#66229 = CARTESIAN_POINT ( 'NONE',  ( 104.4690831045889894, -46.42484882949283076, 88.36765422304442552 ) ) ;
#66230 = CARTESIAN_POINT ( 'NONE',  ( 107.2073525216087120, -27.33494443775582639, 76.50824997256394511 ) ) ;
#66231 = CARTESIAN_POINT ( 'NONE',  ( 136.8165183345649041, -18.90056224776383687, 3.101534470964332879 ) ) ;
#66232 = LINE ( 'NONE', #32166, #28505 ) ;
#66233 = CARTESIAN_POINT ( 'NONE',  ( 186.6899999999999977, 59.08750000000000568, -50.79999999999999716 ) ) ;
#66234 = CARTESIAN_POINT ( 'NONE',  ( 105.4175444341163939, -47.04536977979798706, 33.44991099019695469 ) ) ;
#66235 = CIRCLE ( 'NONE', #75010, 17.00000000000000000 ) ;
#66236 = DIRECTION ( 'NONE',  ( 0.000000000000000000, 1.000000000000000000, 0.000000000000000000 ) ) ;
#66237 = ORIENTED_EDGE ( 'NONE', *, *, #87867, .F. ) ;
#66238 = DIRECTION ( 'NONE',  ( -3.100000000000000258E-29, 3.100000000000000044E-14, 1.000000000000000000 ) ) ;
#66239 = ORIENTED_EDGE ( 'NONE', *, *, #43429, .F. ) ;
#66240 = CARTESIAN_POINT ( 'NONE',  ( -118.0058494126929389, 76.91656954603718077, 11.41259371393320521 ) ) ;
#66241 = ORIENTED_EDGE ( 'NONE', *, *, #20140, .T. ) ;
#66242 = ORIENTED_EDGE ( 'NONE', *, *, #83533, .F. ) ;
#66243 = ADVANCED_FACE ( 'NONE', ( #42833 ), #27877, .T. ) ;
#66244 = CARTESIAN_POINT ( 'NONE',  ( 138.8167039024479834, -57.40094715994099772, 60.91780685541480267 ) ) ;
#66245 = VERTEX_POINT ( 'NONE', #14265 ) ;
#66246 = CARTESIAN_POINT ( 'NONE',  ( 112.8396959964676682, -44.62460075896473910, 228.0784824187689708 ) ) ;
#66247 = CARTESIAN_POINT ( 'NONE',  ( 114.4495774554661836, -29.91993045966185250, 124.4189032693139865 ) ) ;
#66248 = DIRECTION ( 'NONE',  ( 1.000000000000000000, 0.000000000000000000, -4.277118011829300531E-15 ) ) ;
#66249 = CARTESIAN_POINT ( 'NONE',  ( 110.4565933333529699, -47.24995733706104062, 53.83657765686300678 ) ) ;
#66250 = FACE_OUTER_BOUND ( 'NONE', #14517, .T. ) ;
#66251 = VERTEX_POINT ( 'NONE', #70114 ) ;
#66252 = CARTESIAN_POINT ( 'NONE',  ( 100.9537918767618976, -28.70771463842614679, 171.5940036888151781 ) ) ;
#66253 = AXIS2_PLACEMENT_3D ( 'NONE', #74752, #88842, #47473 ) ;
#66254 = FACE_OUTER_BOUND ( 'NONE', #54325, .T. ) ;
#66255 = ORIENTED_EDGE ( 'NONE', *, *, #77082, .F. ) ;
#66256 = VECTOR ( 'NONE', #36491, 1000.000000000000000 ) ;
#66257 = CARTESIAN_POINT ( 'NONE',  ( -479.3614999999999782, 100.8062500000000057, 86.36305401447658880 ) ) ;
#66259 = ADVANCED_FACE ( 'NONE', ( #84657 ), #64205, .F. ) ;
#66258 = AXIS2_PLACEMENT_3D ( 'NONE', #52245, #16430, #44106 ) ;
#66260 = DIRECTION ( 'NONE',  ( 1.000000000000000078E-15, 1.000000000000000083E-30, -1.000000000000000000 ) ) ;
#66261 = CARTESIAN_POINT ( 'NONE',  ( 109.9541224118590890, -48.19721710984623542, 242.7727681330539724 ) ) ;
#66262 = LINE ( 'NONE', #79488, #41408 ) ;
#66263 = AXIS2_PLACEMENT_3D ( 'NONE', #22690, #50361, #9057 ) ;
#66264 = CARTESIAN_POINT ( 'NONE',  ( 173.9900000000000091, 101.5999999999999943, 71.37400000000000944 ) ) ;
#66265 = CARTESIAN_POINT ( 'NONE',  ( 121.2862831202667167, -94.98932219798427923, -19.21046202161327798 ) ) ;
#66266 = CARTESIAN_POINT ( 'NONE',  ( 98.72788526414296939, -31.75567473670096774, 280.3209912566482558 ) ) ;
#66268 = CARTESIAN_POINT ( 'NONE',  ( 114.3378803067696197, -44.16957155219873243, 69.19276813305397411 ) ) ;
#66267 = CARTESIAN_POINT ( 'NONE',  ( 168.0371591254545365, -48.62818131005519007, 193.9678068554149775 ) ) ;
#66269 = CARTESIAN_POINT ( 'NONE',  ( 115.5056795903910825, 72.00002230228413680, 60.85563221252769495 ) ) ;
#66270 = CARTESIAN_POINT ( 'NONE',  ( 102.2821109723304431, -27.37735778705684098, 120.4527681330539792 ) ) ;
#66271 = VERTEX_POINT ( 'NONE', #49652 ) ;
#66272 = DIRECTION ( 'NONE',  ( 0.000000000000000000, 1.000000000000000000, 0.000000000000000000 ) ) ;
#66273 = ORIENTED_EDGE ( 'NONE', *, *, #61770, .F. ) ;
#66274 = EDGE_CURVE ( 'NONE', #70541, #4931, #69670, .T. ) ;
#66275 = DIRECTION ( 'NONE',  ( 0.000000000000000000, 0.000000000000000000, 1.000000000000000000 ) ) ;
#66276 = CARTESIAN_POINT ( 'NONE',  ( 4.163101094985349692E-14, 127.0000000000000000, -98.60478223830740774 ) ) ;
#66277 = PRODUCT_DEFINITION_SHAPE ( 'NONE', 'NONE',  #89941 ) ;
#66278 = CARTESIAN_POINT ( 'NONE',  ( 194.5667039024480403, -40.82844715993405771, 249.9678068554149775 ) ) ;
#66279 = ORIENTED_EDGE ( 'NONE', *, *, #10737, .T. ) ;
#66280 = ADVANCED_FACE ( 'NONE', ( #77379 ), #8803, .F. ) ;
#66281 = EDGE_CURVE ( 'NONE', #64435, #54341, #42070, .T. ) ;
#66282 = LINE ( 'NONE', #32662, #40350 ) ;
#66284 = ORIENTED_EDGE ( 'NONE', *, *, #15170, .T. ) ;
#66283 = CARTESIAN_POINT ( 'NONE',  ( 98.42220671263785903, -30.82325138971081557, 120.8499109901969604 ) ) ;
#66285 = FACE_OUTER_BOUND ( 'NONE', #30311, .T. ) ;
#66286 = AXIS2_PLACEMENT_3D ( 'NONE', #88371, #40185, #5694 ) ;
#66287 = DIRECTION ( 'NONE',  ( 4.194175870806139918E-14, -1.000000000000000000, 0.000000000000000000 ) ) ;
#66288 = AXIS2_PLACEMENT_3D ( 'NONE', #79033, #53051, #23627 ) ;
#66289 = EDGE_CURVE ( 'NONE', #55083, #462, #36501, .T. ) ;
#66290 = LINE ( 'NONE', #45391, #88698 ) ;
#66291 = ORIENTED_EDGE ( 'NONE', *, *, #84432, .T. ) ;
#66292 = VECTOR ( 'NONE', #74331, 1000.000000000000000 ) ;
#66293 = CARTESIAN_POINT ( 'NONE',  ( 117.6304226258691727, -33.39798698885631012, 129.0575300378159795 ) ) ;
#66294 = DIRECTION ( 'NONE',  ( -6.982962677686266711E-15, 0.000000000000000000, 1.000000000000000000 ) ) ;
#66295 = EDGE_CURVE ( 'NONE', #29586, #17964, #31955, .T. ) ;
#66296 = CARTESIAN_POINT ( 'NONE',  ( 167.7413838386817702, -48.33240602328261559, 249.9678068554149775 ) ) ;
#66297 = CARTESIAN_POINT ( 'NONE',  ( 107.0664832912739399, -36.72944715994095333, 312.1356252759112522 ) ) ;
#66298 = ORIENTED_EDGE ( 'NONE', *, *, #52564, .F. ) ;
#66299 = EDGE_LOOP ( 'NONE', ( #16128, #76830, #49033, #53473 ) ) ;
#66300 = DIRECTION ( 'NONE',  ( 0.000000000000000000, 0.000000000000000000, 1.000000000000000000 ) ) ;
#66301 = LINE ( 'NONE', #10897, #480 ) ;
#66302 = EDGE_CURVE ( 'NONE', #49032, #63259, #22879, .T. ) ;
#66303 = DIRECTION ( 'NONE',  ( 0.000000000000000000, -1.000000000000000000, 0.000000000000000000 ) ) ;
#66305 = CARTESIAN_POINT ( 'NONE',  ( 131.0667039024480118, -61.87844715994100397, 231.5838068554150198 ) ) ;
#66304 = CARTESIAN_POINT ( 'NONE',  ( 72.96458098368650269, 117.4749999999999943, 65.02708098368729850 ) ) ;
#66306 = FACE_OUTER_BOUND ( 'NONE', #17349, .T. ) ;
#66307 = AXIS2_PLACEMENT_3D ( 'NONE', #77050, #78849, #37497 ) ;
#66308 = EDGE_LOOP ( 'NONE', ( #62026, #24607, #68485, #62476, #69834, #1504, #19397 ) ) ;
#66309 = CARTESIAN_POINT ( 'NONE',  ( 107.0620278373210539, -36.73691869758540207, 394.9756252759100903 ) ) ;
#66310 = CARTESIAN_POINT ( 'NONE',  ( 114.8736367985562623, -30.83777597042988106, 215.3413395616249773 ) ) ;
#66312 = VERTEX_POINT ( 'NONE', #85996 ) ;
#66311 = DIRECTION ( 'NONE',  ( -1.000000000000000078E-15, -1.000000000000000083E-30, 1.000000000000000000 ) ) ;
#66313 = EDGE_CURVE ( 'NONE', #67833, #74158, #10124, .T. ) ;
#66314 = CARTESIAN_POINT ( 'NONE',  ( 116.6363502066642468, -38.74961609181404043, 59.66133956162394725 ) ) ;
#66316 = ADVANCED_FACE ( 'NONE', ( #31004, #51873 ), #86438, .F. ) ;
#66315 = CARTESIAN_POINT ( 'NONE',  ( 105.7152859519171244, -46.72382961504868604, 52.46901143198183348 ) ) ;
#66317 = CARTESIAN_POINT ( 'NONE',  ( 25.56670390244797275, -58.35344715994099829, 175.9678068554150059 ) ) ;
#66318 = ADVANCED_FACE ( 'NONE', ( #24206 ), #30567, .T. ) ;
#66319 = CARTESIAN_POINT ( 'NONE',  ( 31.56670390244700641, -19.82844715994111340, -5.074374724088000832 ) ) ;
#66320 = VERTEX_POINT ( 'NONE', #36935 ) ;
#66321 = DIRECTION ( 'NONE',  ( 0.000000000000000000, 0.000000000000000000, 1.000000000000000000 ) ) ;
#66322 = ADVANCED_FACE ( 'NONE', ( #65087 ), #2870, .T. ) ;
#66323 = AXIS2_PLACEMENT_3D ( 'NONE', #39891, #13105, #356 ) ;
#66324 = ORIENTED_EDGE ( 'NONE', *, *, #2662, .F. ) ;
#66325 = ORIENTED_EDGE ( 'NONE', *, *, #68222, .F. ) ;
#66326 = CARTESIAN_POINT ( 'NONE',  ( 114.1399574501865999, -31.39144735336052605, 215.7730118773249899 ) ) ;
#66327 = CIRCLE ( 'NONE', #85249, 2.517500000000005844 ) ;
#66328 = CARTESIAN_POINT ( 'NONE',  ( 40.31648329127400388, 12.92155284005802507, 336.5756252759108520 ) ) ;
#66329 = VECTOR ( 'NONE', #65356, 1000.000000000000000 ) ;
#66330 = CONICAL_SURFACE ( 'NONE', #86657, 82.41591158490092539, 0.7853981633974760346 ) ;
#66331 = CARTESIAN_POINT ( 'NONE',  ( -118.5472366675172253, 95.16897323824362331, 1.658320819117713674 ) ) ;
#66332 = DIRECTION ( 'NONE',  ( -9.073094938289460781E-13, -1.000000000000000000, 0.000000000000000000 ) ) ;
#66333 = CARTESIAN_POINT ( 'NONE',  ( 0.000000000000000000, 127.0000000000000000, -103.1875000000000000 ) ) ;
#66334 = VERTEX_POINT ( 'NONE', #58267 ) ;
#66335 = CARTESIAN_POINT ( 'NONE',  ( 107.0664832912739399, -36.72944715994095333, 293.6356252759109680 ) ) ;
#66336 = DIRECTION ( 'NONE',  ( 0.000000000000000000, 0.8660254037844379305, 0.5000000000000011102 ) ) ;
#66337 = EDGE_LOOP ( 'NONE', ( #69711, #62067, #85642, #36327 ) ) ;
#66338 = CARTESIAN_POINT ( 'NONE',  ( 111.4711666614669099, -26.61707918639087822, 284.7375300378156453 ) ) ;
#66339 = DIRECTION ( 'NONE',  ( 0.000000000000000000, 0.000000000000000000, -1.000000000000000000 ) ) ;
#66340 = ORIENTED_EDGE ( 'NONE', *, *, #50738, .T. ) ;
#66341 = VECTOR ( 'NONE', #74336, 1000.000000000000000 ) ;
#66342 = CARTESIAN_POINT ( 'NONE',  ( 116.7951252707350562, -39.38782979291476494, 83.61479194234540557 ) ) ;
#66343 = CARTESIAN_POINT ( 'NONE',  ( 70.06670417066791856, -83.77844715994098124, 55.21780685541800437 ) ) ;
#66344 = DIRECTION ( 'NONE',  ( -1.000000000000000000, 0.000000000000000000, 0.000000000000000000 ) ) ;
#66345 = AXIS2_PLACEMENT_3D ( 'NONE', #29595, #78217, #41854 ) ;
#66346 = DIRECTION ( 'NONE',  ( -0.1858654557293118459, 0.9825752044329915114, 0.000000000000000000 ) ) ;
#66347 = VECTOR ( 'NONE', #37581, 1000.000000000000000 ) ;
#66348 = CARTESIAN_POINT ( 'NONE',  ( 117.4559332992660075, -35.18111149946130922, 214.9441967044829767 ) ) ;
#66349 = DIRECTION ( 'NONE',  ( 0.000000000000000000, 0.000000000000000000, -1.000000000000000000 ) ) ;
#66350 = VECTOR ( 'NONE', #33433, 1000.000000000000000 ) ;
#66351 = ORIENTED_EDGE ( 'NONE', *, *, #302, .F. ) ;
#66352 = CARTESIAN_POINT ( 'NONE',  ( 118.0344259573852810, -38.43289426264998099, 64.69181575210097890 ) ) ;
#66353 = CARTESIAN_POINT ( 'NONE',  ( 107.0664832912739399, -48.47944715994096043, 307.1356252759109680 ) ) ;
#66354 = ORIENTED_EDGE ( 'NONE', *, *, #19837, .F. ) ;
#66355 = ORIENTED_EDGE ( 'NONE', *, *, #47730, .F. ) ;
#66356 = VERTEX_POINT ( 'NONE', #30124 ) ;
#66357 = DIRECTION ( 'NONE',  ( 4.299999999999999979E-14, -1.000000000000000000, 4.400000000000000367E-29 ) ) ;
#66358 = CARTESIAN_POINT ( 'NONE',  ( 1.978343425214599878E-14, 0.000000000000000000, 161.5439999999999827 ) ) ;
#66359 = FACE_OUTER_BOUND ( 'NONE', #61809, .T. ) ;
#66360 = CARTESIAN_POINT ( 'NONE',  ( 103.5819438468105744, -44.65149928713079674, 130.0528522743539668 ) ) ;
#66361 = CARTESIAN_POINT ( 'NONE',  ( 115.8735763837842256, -44.69546008661756531, 229.2413395616249545 ) ) ;
#66362 = DIRECTION ( 'NONE',  ( -1.000000000000000000, 0.000000000000000000, 0.000000000000000000 ) ) ;
#66363 = ORIENTED_EDGE ( 'NONE', *, *, #31977, .T. ) ;
#66364 = CIRCLE ( 'NONE', #89609, 5.599999999999994316 ) ;
#66365 = CARTESIAN_POINT ( 'NONE',  ( 136.6734006051289612, -37.60624470236170680, 2.902100967938293863 ) ) ;
#66366 = ORIENTED_EDGE ( 'NONE', *, *, #35761, .F. ) ;
#66368 = VERTEX_POINT ( 'NONE', #58698 ) ;
#66367 = AXIS2_PLACEMENT_3D ( 'NONE', #30238, #16607, #2976 ) ;
#66369 = LINE ( 'NONE', #39564, #37194 ) ;
#66370 = ORIENTED_EDGE ( 'NONE', *, *, #51125, .F. ) ;
#66371 = ORIENTED_EDGE ( 'NONE', *, *, #53885, .F. ) ;
#66372 = CARTESIAN_POINT ( 'NONE',  ( 101.9943922633895710, -45.44653761360012112, 168.1571991305824270 ) ) ;
#66373 = CARTESIAN_POINT ( 'NONE',  ( 156.5667039024485518, -48.82844715993568485, 170.7178068554149775 ) ) ;
#66374 = EDGE_CURVE ( 'NONE', #18008, #44647, #72357, .T. ) ;
#66375 = DIRECTION ( 'NONE',  ( 0.000000000000000000, 0.000000000000000000, 1.000000000000000000 ) ) ;
#66376 = CARTESIAN_POINT ( 'NONE',  ( 103.6638222329471262, -28.86385020797125733, 154.8238483995059767 ) ) ;
#66377 = CARTESIAN_POINT ( 'NONE',  ( 107.1959452681378053, -26.26092741545045328, 35.06705384733893283 ) ) ;
#66378 = ORIENTED_EDGE ( 'NONE', *, *, #61559, .T. ) ;
#66379 = EDGE_CURVE ( 'NONE', #59900, #69275, #59584, .T. ) ;
#66380 = DIRECTION ( 'NONE',  ( 1.000000000000000000, 0.000000000000000000, 2.671820169801660301E-13 ) ) ;
#66381 = EDGE_LOOP ( 'NONE', ( #81197, #46806, #68033, #85579 ) ) ;
#66382 = ADVANCED_FACE ( 'NONE', ( #3313 ), #51436, .T. ) ;
#66383 = EDGE_CURVE ( 'NONE', #33468, #56522, #65961, .T. ) ;
#66384 = CARTESIAN_POINT ( 'NONE',  ( 70.06670390244705970, -124.7784471599409812, 55.21780685541800437 ) ) ;
#66385 = ORIENTED_EDGE ( 'NONE', *, *, #44504, .T. ) ;
#66386 = LINE ( 'NONE', #86856, #46469 ) ;
#66387 = CARTESIAN_POINT ( 'NONE',  ( -3.273551063997644839, 70.35480798052911666, 118.5135525315334633 ) ) ;
#66388 = DIRECTION ( 'NONE',  ( 4.299999999999999979E-14, -1.000000000000000000, 0.000000000000000000 ) ) ;
#66389 = EDGE_CURVE ( 'NONE', #5020, #16533, #13111, .T. ) ;
#66390 = DIRECTION ( 'NONE',  ( 1.000000000000000078E-15, -1.000000000000000000, 0.000000000000000000 ) ) ;
#66391 = EDGE_LOOP ( 'NONE', ( #64161, #17882, #63780, #9349 ) ) ;
#66392 = AXIS2_PLACEMENT_3D ( 'NONE', #17836, #86887, #51446 ) ;
#66393 = CARTESIAN_POINT ( 'NONE',  ( 114.8359307259106856, -43.71386199060815869, 38.24419670448192221 ) ) ;
#66394 = CARTESIAN_POINT ( 'NONE',  ( 116.4265620360770725, -31.96216903954944399, 40.20133956162496958 ) ) ;
#66395 = EDGE_CURVE ( 'NONE', #89416, #11922, #27618, .T. ) ;
#66397 = CARTESIAN_POINT ( 'NONE',  ( 68.96108109926477425, -139.0395986478499708, 246.8356254435167614 ) ) ;
#66396 = DIRECTION ( 'NONE',  ( 0.000000000000000000, 0.000000000000000000, 1.000000000000000000 ) ) ;
#66398 = DIRECTION ( 'NONE',  ( 0.000000000000000000, 1.000000000000000000, 0.000000000000000000 ) ) ;
#66399 = CARTESIAN_POINT ( 'NONE',  ( 188.5667039024483245, -42.82844715993430640, 173.2178068554150059 ) ) ;
#66400 = LINE ( 'NONE', #40040, #67288 ) ;
#66401 = AXIS2_PLACEMENT_3D ( 'NONE', #53807, #61532, #19321 ) ;
#66402 = DIRECTION ( 'NONE',  ( 0.000000000000000000, 0.000000000000000000, 1.000000000000000000 ) ) ;
#66403 = EDGE_CURVE ( 'NONE', #76842, #611, #16026, .T. ) ;
#66404 = AXIS2_PLACEMENT_3D ( 'NONE', #27564, #40732, #13050 ) ;
#66405 = DIRECTION ( 'NONE',  ( -0.9963424814100678706, 0.08544974978095865037, 0.000000000000000000 ) ) ;
#66406 = CARTESIAN_POINT ( 'NONE',  ( 116.7859321266972330, -32.83856289285826335, 54.12991099019698282 ) ) ;
#66407 = CARTESIAN_POINT ( 'NONE',  ( 103.6386224297199163, -26.22117658871400181, 206.3394347997209763 ) ) ;
#66408 = CARTESIAN_POINT ( 'NONE',  ( 103.9509101786591287, -47.35857741242491414, 58.33753003781600199 ) ) ;
#66409 = AXIS2_PLACEMENT_3D ( 'NONE', #89379, #88929, #81678 ) ;
#66410 = AXIS2_PLACEMENT_3D ( 'NONE', #28184, #89090, #13673 ) ;
#66412 = LINE ( 'NONE', #4202, #71747 ) ;
#66411 = DIRECTION ( 'NONE',  ( 1.000000000000000000, 0.000000000000000000, 0.000000000000000000 ) ) ;
#66413 = DIRECTION ( 'NONE',  ( -0.9254794337955623007, -0.3787978585227819162, 0.000000000000000000 ) ) ;
#66414 = EDGE_CURVE ( 'NONE', #88572, #74091, #17444, .T. ) ;
#66415 = CIRCLE ( 'NONE', #44625, 3.000000000000002665 ) ;
#66416 = VERTEX_POINT ( 'NONE', #45499 ) ;
#66417 = CARTESIAN_POINT ( 'NONE',  ( 97.07207207479322619, -35.37844108757092698, 187.2189586003667330 ) ) ;
#66418 = ORIENTED_EDGE ( 'NONE', *, *, #25449, .F. ) ;
#66419 = CARTESIAN_POINT ( 'NONE',  ( 98.99072789581764198, -31.21169308021403310, 116.8499109901959514 ) ) ;
#66421 = ORIENTED_EDGE ( 'NONE', *, *, #20873, .F. ) ;
#66420 = CARTESIAN_POINT ( 'NONE',  ( 12.69999999999999929, 82.54999999999999716, 129.9368274816650057 ) ) ;
#66422 = DIRECTION ( 'NONE',  ( -0.7071067811866279529, 0.7071067811864671926, -7.071067811865978232E-16 ) ) ;
#66423 = CARTESIAN_POINT ( 'NONE',  ( 111.5990003564989479, -46.09347164638224825, 243.9356252759109509 ) ) ;
#66424 = FACE_OUTER_BOUND ( 'NONE', #48595, .T. ) ;
#66425 = CARTESIAN_POINT ( 'NONE',  ( 117.0520078648838336, -35.94494220078347269, 148.8889094017758907 ) ) ;
#66426 = DIRECTION ( 'NONE',  ( 1.000000000000000000, 1.000000000000000078E-15, 0.000000000000000000 ) ) ;
#66427 = CARTESIAN_POINT ( 'NONE',  ( -487.2989999999999782, 14.28749999999982201, 95.25000000000000000 ) ) ;
#66428 = EDGE_CURVE ( 'NONE', #18949, #32855, #86877, .T. ) ;
#66429 = CARTESIAN_POINT ( 'NONE',  ( 134.0664832912740110, -39.47944715994100306, 1.625625275910997480 ) ) ;
#66430 = CARTESIAN_POINT ( 'NONE',  ( -84.72210942531908984, 75.15271101351805783, 99.33321048326511971 ) ) ;
#66431 = EDGE_CURVE ( 'NONE', #829, #43897, #17825, .T. ) ;
#66432 = CARTESIAN_POINT ( 'NONE',  ( 102.0969121991172557, -45.15362633196983211, 162.1527681330539679 ) ) ;
#66433 = VECTOR ( 'NONE', #32833, 1000.000000000000000 ) ;
#66434 = VERTEX_POINT ( 'NONE', #87322 ) ;
#66435 = VERTEX_POINT ( 'NONE', #71475 ) ;
#66436 = CIRCLE ( 'NONE', #12773, 4.762500000000000178 ) ;
#66437 = CARTESIAN_POINT ( 'NONE',  ( 97.73412737207827661, -37.81740788287748956, 82.86253568684892912 ) ) ;
#66438 = CARTESIAN_POINT ( 'NONE',  ( 192.5667039024475002, -23.42844715993433624, 129.9678068554150343 ) ) ;
#66440 = DIRECTION ( 'NONE',  ( -1.000000000000000000, 0.000000000000000000, 0.000000000000000000 ) ) ;
#66439 = CARTESIAN_POINT ( 'NONE',  ( 104.9788083641148972, -27.14010996210895499, 256.2470538473390889 ) ) ;
#66441 = CARTESIAN_POINT ( 'NONE',  ( 107.0667039024479834, -36.72944715994099596, 239.5838068554170093 ) ) ;
#66442 = CARTESIAN_POINT ( 'NONE',  ( 52.65249034007741358, -48.32844715994062312, 180.4678068554151196 ) ) ;
#66443 = CARTESIAN_POINT ( 'NONE',  ( 117.8825533107838908, 80.89685143461888117, 12.61964884581579049 ) ) ;
#66444 = DIRECTION ( 'NONE',  ( -0.000000000000000000, -1.000000000000000000, -0.000000000000000000 ) ) ;
#66445 = DIRECTION ( 'NONE',  ( -1.000000000000000000, -4.299999999999999979E-14, 1.230419385187874527E-43 ) ) ;
#66446 = CARTESIAN_POINT ( 'NONE',  ( -215.9000000000000057, 101.5999999999999943, -45.33899999999999864 ) ) ;
#66447 = CARTESIAN_POINT ( 'NONE',  ( 101.9951592035502017, -45.85337710724439830, 187.1727681330539781 ) ) ;
#66448 = ORIENTED_EDGE ( 'NONE', *, *, #28911, .T. ) ;
#66449 = VERTEX_POINT ( 'NONE', #57821 ) ;
#66450 = DIRECTION ( 'NONE',  ( 1.000000000000000078E-15, -1.000000000000000000, 0.000000000000000000 ) ) ;
#66451 = CARTESIAN_POINT ( 'NONE',  ( 97.07207207582297315, -35.37844108030525092, 152.2189585997880386 ) ) ;
#66452 = CARTESIAN_POINT ( 'NONE',  ( 162.5667039024460223, -19.82844715994111340, 342.9256252759109884 ) ) ;
#66453 = FACE_OUTER_BOUND ( 'NONE', #46760, .T. ) ;
#66454 = EDGE_CURVE ( 'NONE', #21457, #24776, #23334, .T. ) ;
#66455 = VERTEX_POINT ( 'NONE', #16497 ) ;
#66456 = CIRCLE ( 'NONE', #44672, 3.000000000000002665 ) ;
#66457 = CARTESIAN_POINT ( 'NONE',  ( 100.8874524663688277, -44.70020958072196748, 268.0522904122051955 ) ) ;
#66458 = CARTESIAN_POINT ( 'NONE',  ( 108.8488851759622804, -47.00125683367996032, 167.7127681330539701 ) ) ;
#66459 = FACE_OUTER_BOUND ( 'NONE', #16451, .T. ) ;
#66460 = VERTEX_POINT ( 'NONE', #74576 ) ;
#66462 = ORIENTED_EDGE ( 'NONE', *, *, #56252, .F. ) ;
#66461 = ORIENTED_EDGE ( 'NONE', *, *, #27630, .F. ) ;
#66463 = VECTOR ( 'NONE', #9275, 1000.000000000000000 ) ;
#66464 = CARTESIAN_POINT ( 'NONE',  ( 99.13948424873241549, -42.84779535630594438, 62.85003987030304984 ) ) ;
#66465 = CYLINDRICAL_SURFACE ( 'NONE', #84855, 10.00000000000000711 ) ;
#66466 = CARTESIAN_POINT ( 'NONE',  ( 117.0606841593708225, -38.08193661114533057, 164.7188404860883395 ) ) ;
#66467 = CARTESIAN_POINT ( 'NONE',  ( 111.6835086010359532, -29.99796862204811987, 42.41666179816294857 ) ) ;
#66468 = AXIS2_PLACEMENT_3D ( 'NONE', #45637, #87460, #85691 ) ;
#66469 = CARTESIAN_POINT ( 'NONE',  ( 80.06648329127402519, -46.72944715994105991, 1.625625275910943746 ) ) ;
#66470 = VERTEX_POINT ( 'NONE', #19613 ) ;
#66471 = AXIS2_PLACEMENT_3D ( 'NONE', #28931, #56617, #42974 ) ;
#66472 = VECTOR ( 'NONE', #15818, 1000.000000000000000 ) ;
#66473 = CARTESIAN_POINT ( 'NONE',  ( -47.11752803141010304, 65.68786680169236547, 108.7909173056707317 ) ) ;
#66474 = EDGE_CURVE ( 'NONE', #86124, #7001, #11464, .T. ) ;
#66475 = LINE ( 'NONE', #4715, #2422 ) ;
#66476 = EDGE_LOOP ( 'NONE', ( #74210, #33310 ) ) ;
#66477 = VERTEX_POINT ( 'NONE', #12358 ) ;
#66478 = CARTESIAN_POINT ( 'NONE',  ( 116.3212776292278363, -32.94146857470881429, 179.1356252759109395 ) ) ;
#66479 = VERTEX_POINT ( 'NONE', #27325 ) ;
#66480 = ORIENTED_EDGE ( 'NONE', *, *, #28038, .T. ) ;
#66481 = CARTESIAN_POINT ( 'NONE',  ( 2.849336855536075284E-14, 184.0000000000000000, 111.9860621927989683 ) ) ;
#66482 = EDGE_CURVE ( 'NONE', #16780, #10687, #6434, .T. ) ;
#66483 = ADVANCED_FACE ( 'NONE', ( #60946 ), #74140, .F. ) ;
#66484 = VECTOR ( 'NONE', #46805, 1000.000000000000000 ) ;
#66485 = CARTESIAN_POINT ( 'NONE',  ( 102.5950791370611768, -45.34791940167762192, 16.61813411379198158 ) ) ;
#66486 = CARTESIAN_POINT ( 'NONE',  ( 104.4481554933880716, -26.61555950438322427, 200.2784824187679362 ) ) ;
#66487 = EDGE_CURVE ( 'NONE', #5130, #73456, #68, .T. ) ;
#66488 = CARTESIAN_POINT ( 'NONE',  ( 114.3286968523004248, -29.23113535793732254, 174.4641967044819637 ) ) ;
#66490 = CARTESIAN_POINT ( 'NONE',  ( 112.4893506266177070, -46.36098340020668473, 253.9965776568634510 ) ) ;
#66489 = CARTESIAN_POINT ( 'NONE',  ( 97.93091671000914289, -40.79819621030469534, 21.65960399723592289 ) ) ;
#66491 = DIRECTION ( 'NONE',  ( -4.299999999999999979E-14, 1.000000000000000000, -4.400000000000000367E-29 ) ) ;
#66492 = DIRECTION ( 'NONE',  ( 1.000000000000000078E-15, -1.000000000000000083E-30, -1.000000000000000000 ) ) ;
#66493 = ORIENTED_EDGE ( 'NONE', *, *, #47200, .T. ) ;
#66494 = EDGE_CURVE ( 'NONE', #86558, #50049, #40049, .T. ) ;
#66495 = VERTEX_POINT ( 'NONE', #33696 ) ;
#66496 = AXIS2_PLACEMENT_3D ( 'NONE', #66799, #32271, #59965 ) ;
#66497 = VECTOR ( 'NONE', #33370, 1000.000000000000000 ) ;
#66498 = EDGE_CURVE ( 'NONE', #22506, #54510, #36315, .T. ) ;
#66499 = CARTESIAN_POINT ( 'NONE',  ( 97.82529773858178146, -40.55052980792035555, 111.6384738132450991 ) ) ;
#66500 = CARTESIAN_POINT ( 'NONE',  ( 96.47340144944560336, -31.30584922022854144, 245.9499109901969689 ) ) ;
#66501 = ORIENTED_EDGE ( 'NONE', *, *, #38096, .F. ) ;
#66502 = CARTESIAN_POINT ( 'NONE',  ( 97.40186843559010299, -40.63869902605510731, 206.6327681330539860 ) ) ;
#66503 = CARTESIAN_POINT ( 'NONE',  ( 105.7984081882492120, -26.72418595412763764, 265.1773184473723290 ) ) ;
#66504 = CARTESIAN_POINT ( 'NONE',  ( -5.491540717450776654, 69.94491574763448227, 37.72695927949112615 ) ) ;
#66505 = CARTESIAN_POINT ( 'NONE',  ( -240.5296158183964792, 93.66249999999999432, 11.11250000000040217 ) ) ;
#66506 = CARTESIAN_POINT ( 'NONE',  ( 143.9181536748402266, -140.4668907707514052, 246.4376387225517533 ) ) ;
#66509 = CARTESIAN_POINT ( 'NONE',  ( 97.23737678141888807, -33.32131919061086478, 282.0613395616252888 ) ) ;
#66508 = DIRECTION ( 'NONE',  ( 0.000000000000000000, -1.000000000000000000, 0.000000000000000000 ) ) ;
#66507 = CARTESIAN_POINT ( 'NONE',  ( 97.81281252356875200, -40.52015776331121089, 277.6356251289804504 ) ) ;
#66510 = CARTESIAN_POINT ( 'NONE',  ( 83.06670390244796920, -61.87844715994100397, 231.5838068554150198 ) ) ;
#66512 = EDGE_CURVE ( 'NONE', #38542, #89690, #39162, .T. ) ;
#66511 = FACE_BOUND ( 'NONE', #61589, .T. ) ;
#66513 = CARTESIAN_POINT ( 'NONE',  ( 62.03715912545731470, -23.42818131006022142, 249.9678068554150343 ) ) ;
#66514 = CARTESIAN_POINT ( 'NONE',  ( 67.85198242736144891, -137.2567436070751796, 247.0961534730330982 ) ) ;
#66515 = DIRECTION ( 'NONE',  ( 0.000000000000000000, -1.000000000000000000, 0.000000000000000000 ) ) ;
#66516 = DIRECTION ( 'NONE',  ( 0.000000000000000000, 1.000000000000000000, 0.000000000000000000 ) ) ;
#66517 = ADVANCED_FACE ( 'NONE', ( #4646 ), #40944, .T. ) ;
#66519 = ORIENTED_EDGE ( 'NONE', *, *, #2165, .F. ) ;
#66518 = DIRECTION ( 'NONE',  ( 0.7071067811862279395, -0.7071067811868672059, 7.071067811862286363E-16 ) ) ;
#66520 = VECTOR ( 'NONE', #84754, 1000.000000000000000 ) ;
#66521 = CARTESIAN_POINT ( 'NONE',  ( 136.4975570085109382, -20.01506174167543506, 7.157201688892354419 ) ) ;
#66522 = CARTESIAN_POINT ( 'NONE',  ( 98.36125384756333290, -29.88003685912757490, 200.8080062282919869 ) ) ;
#66523 = CARTESIAN_POINT ( 'NONE',  ( 99.68461964852595258, -45.99997598619422234, 118.0413395616259606 ) ) ;
#66524 = CARTESIAN_POINT ( 'NONE',  ( 96.81585423491817721, -34.60398634006848795, 212.1641967044819808 ) ) ;
#66525 = LINE ( 'NONE', #4314, #64296 ) ;
#66526 = DIRECTION ( 'NONE',  ( 0.000000000000000000, 0.000000000000000000, -1.000000000000000000 ) ) ;
#66528 = CARTESIAN_POINT ( 'NONE',  ( 0.000000000000000000, 2.031999999999865025, 25.39999999999999858 ) ) ;
#66527 = CARTESIAN_POINT ( 'NONE',  ( 131.0667039024480118, -58.35344715994099829, 231.5838068554150198 ) ) ;
#66529 = CYLINDRICAL_SURFACE ( 'NONE', #79882, 9.999999999999998224 ) ;
#66530 = CARTESIAN_POINT ( 'NONE',  ( 70.06670390244703128, -96.32844715994099261, 55.21780685541800437 ) ) ;
#66531 = DIRECTION ( 'NONE',  ( -0.8571673007021110013, 1.917331853055865018E-16, 0.5150380749100563760 ) ) ;
#66532 = AXIS2_PLACEMENT_3D ( 'NONE', #9141, #36837, #14613 ) ;
#66533 = VECTOR ( 'NONE', #70963, 1000.000000000000000 ) ;
#66534 = EDGE_LOOP ( 'NONE', ( #17640, #66124, #14806, #18825 ) ) ;
#66535 = ORIENTED_EDGE ( 'NONE', *, *, #38690, .F. ) ;
#66536 = CARTESIAN_POINT ( 'NONE',  ( 110.3568814055478242, -27.59468345507334064, 99.22384839950498758 ) ) ;
#66537 = VECTOR ( 'NONE', #34958, 1000.000000000000000 ) ;
#66539 = ORIENTED_EDGE ( 'NONE', *, *, #61172, .F. ) ;
#66538 = CARTESIAN_POINT ( 'NONE',  ( 163.5667039024460223, -22.48495420874110806, -5.074374724088000832 ) ) ;
#66540 = CARTESIAN_POINT ( 'NONE',  ( 96.69266148864274157, -35.94780844399463149, 142.2670538473399517 ) ) ;
#66541 = LINE ( 'NONE', #75153, #46819 ) ;
#66542 = CARTESIAN_POINT ( 'NONE',  ( 79.11888855178470692, -16.14703303315388183, 8.087249882925839017 ) ) ;
#66543 = CARTESIAN_POINT ( 'NONE',  ( 51.24204729617298426, -31.76306994223730840, -5.074374724088000832 ) ) ;
#66544 = DIRECTION ( 'NONE',  ( 1.000000000000000000, 8.163404592831600092E-16, 1.020425574103949962E-15 ) ) ;
#66545 = AXIS2_PLACEMENT_3D ( 'NONE', #30776, #86197, #38470 ) ;
#66546 = EDGE_CURVE ( 'NONE', #74639, #6566, #60032, .T. ) ;
#66547 = CARTESIAN_POINT ( 'NONE',  ( 99.23822674327645643, -42.59304969680529496, 66.83848241876894747 ) ) ;
#66548 = EDGE_LOOP ( 'NONE', ( #11413, #15212, #45421, #15784 ) ) ;
#66549 = ORIENTED_EDGE ( 'NONE', *, *, #57640, .T. ) ;
#66550 = ORIENTED_EDGE ( 'NONE', *, *, #21948, .F. ) ;
#66551 = CARTESIAN_POINT ( 'NONE',  ( -240.5296158183964792, 14.28749999999982201, 90.48749999999999716 ) ) ;
#66553 = CARTESIAN_POINT ( 'NONE',  ( 162.5667039024470171, -33.35206098992711077, -5.074374724088000832 ) ) ;
#66552 = CARTESIAN_POINT ( 'NONE',  ( 109.3575602964533289, -46.23809593081413993, 128.7641967044819751 ) ) ;
#66554 = CARTESIAN_POINT ( 'NONE',  ( -487.2989999999999782, 14.28750000000036025, 2.863608028952925100 ) ) ;
#66555 = CARTESIAN_POINT ( 'NONE',  ( 107.0667039024470313, -104.2784471599413791, 2.217806855418003043 ) ) ;
#66556 = VECTOR ( 'NONE', #45361, 1000.000000000000000 ) ;
#66557 = FACE_OUTER_BOUND ( 'NONE', #21851, .T. ) ;
#66558 = DIRECTION ( 'NONE',  ( 0.000000000000000000, -1.000000000000000000, 5.463695987328529395E-16 ) ) ;
#66559 = CARTESIAN_POINT ( 'NONE',  ( 115.7828637914807786, -41.80272134509917947, 179.4064208818603561 ) ) ;
#66560 = CARTESIAN_POINT ( 'NONE',  ( 98.73996931189270754, -42.96625968561445319, 66.83848241876793850 ) ) ;
#66561 = ORIENTED_EDGE ( 'NONE', *, *, #59729, .F. ) ;
#66562 = EDGE_LOOP ( 'NONE', ( #32857, #78616, #75091, #11058, #41516 ) ) ;
#66563 = EDGE_CURVE ( 'NONE', #68206, #73498, #29278, .T. ) ;
#66564 = CARTESIAN_POINT ( 'NONE',  ( 63.03715912545640521, -24.89890238295017255, 180.4678068554151196 ) ) ;
#66565 = CARTESIAN_POINT ( 'NONE',  ( 183.5150000000000148, 37.33800000000000097, 69.13087104677069306 ) ) ;
#66566 = DIRECTION ( 'NONE',  ( -3.100000000000000258E-29, 3.100000000000000044E-14, 1.000000000000000000 ) ) ;
#66567 = CARTESIAN_POINT ( 'NONE',  ( 98.06451646660192978, -38.97900810122609982, 164.3395189410199464 ) ) ;
#66568 = CIRCLE ( 'NONE', #27399, 218.1859999999999786 ) ;
#66569 = ADVANCED_FACE ( 'NONE', ( #8235 ), #35028, .T. ) ;
#66570 = DIRECTION ( 'NONE',  ( 0.8660254037844380415, 0.5000000000000012212, -1.550000000000001284E-14 ) ) ;
#66571 = ORIENTED_EDGE ( 'NONE', *, *, #76437, .F. ) ;
#66572 = ORIENTED_EDGE ( 'NONE', *, *, #59885, .F. ) ;
#66573 = DIRECTION ( 'NONE',  ( 0.1811243268507098381, -0.9834602067307437467, 0.000000000000000000 ) ) ;
#66574 = ORIENTED_EDGE ( 'NONE', *, *, #70347, .F. ) ;
#66575 = ORIENTED_EDGE ( 'NONE', *, *, #72271, .T. ) ;
#66576 = DIRECTION ( 'NONE',  ( 0.000000000000000000, -1.000000000000000000, 0.000000000000000000 ) ) ;
#66577 = CARTESIAN_POINT ( 'NONE',  ( 100.1238157808075186, -30.39889478464921524, 227.1577737820879577 ) ) ;
#66578 = VECTOR ( 'NONE', #13245, 1000.000000000000000 ) ;
#66579 = CARTESIAN_POINT ( 'NONE',  ( 122.2221484686747317, -96.68314769832130651, -19.26696060647622843 ) ) ;
#66580 = CARTESIAN_POINT ( 'NONE',  ( 177.3246001664174969, -48.34074026909178912, 180.4678068554150059 ) ) ;
#66581 = DIRECTION ( 'NONE',  ( 0.000000000000000000, 0.000000000000000000, 1.000000000000000000 ) ) ;
#66582 = ORIENTED_EDGE ( 'NONE', *, *, #86621, .F. ) ;
#66584 = ORIENTED_EDGE ( 'NONE', *, *, #57709, .T. ) ;
#66583 = VECTOR ( 'NONE', #53372, 1000.000000000000000 ) ;
#66585 = ORIENTED_EDGE ( 'NONE', *, *, #51008, .F. ) ;
#66586 = VERTEX_POINT ( 'NONE', #13696 ) ;
#66587 = ADVANCED_FACE ( 'NONE', ( #62738 ), #8694, .T. ) ;
#66588 = CARTESIAN_POINT ( 'NONE',  ( 109.4041143893713297, -28.39659615353044231, 217.6890427505439902 ) ) ;
#66589 = AXIS2_PLACEMENT_3D ( 'NONE', #83596, #62235, #48585 ) ;
#66590 = CARTESIAN_POINT ( 'NONE',  ( 102.9623509218069302, -46.33686416246144546, 92.25562527591097250 ) ) ;
#66591 = EDGE_CURVE ( 'NONE', #66826, #67802, #62439, .T. ) ;
#66592 = CARTESIAN_POINT ( 'NONE',  ( 103.8480726019013218, -46.65951555449696997, 82.32705384733995402 ) ) ;
#66593 = CARTESIAN_POINT ( 'NONE',  ( -446.0240000000000009, 14.28750000000026077, 6.349999999999710099 ) ) ;
#66594 = CARTESIAN_POINT ( 'NONE',  ( 154.4439038579832300, -17.91479848270203945, 396.9756252759102040 ) ) ;
#66595 = LINE ( 'NONE', #52926, #2559 ) ;
#66596 = EDGE_CURVE ( 'NONE', #74769, #73841, #14152, .T. ) ;
#66597 = CARTESIAN_POINT ( 'NONE',  ( 95.31164914186729220, -38.27921806354234491, 147.4299109901969871 ) ) ;
#66598 = CARTESIAN_POINT ( 'NONE',  ( -7.661254700127833495, 95.64746158385918307, 320.6630000000000109 ) ) ;
#66599 = EDGE_LOOP ( 'NONE', ( #10895, #913 ) ) ;
#66600 = DIRECTION ( 'NONE',  ( -0.000000000000000000, -1.000000000000000000, -0.000000000000000000 ) ) ;
#66601 = EDGE_LOOP ( 'NONE', ( #82550, #17009 ) ) ;
#66602 = EDGE_CURVE ( 'NONE', #14890, #62756, #36395, .T. ) ;
#66603 = ORIENTED_EDGE ( 'NONE', *, *, #12488, .F. ) ;
#66604 = AXIS2_PLACEMENT_3D ( 'NONE', #72893, #44726, #73331 ) ;
#66605 = DIRECTION ( 'NONE',  ( 1.000000000000000000, 4.299999999999999979E-14, 1.000000000000000078E-15 ) ) ;
#66606 = FACE_OUTER_BOUND ( 'NONE', #72380, .T. ) ;
#66607 = ORIENTED_EDGE ( 'NONE', *, *, #61878, .F. ) ;
#66608 = DIRECTION ( 'NONE',  ( 1.000000000000000000, 0.000000000000000000, 0.000000000000000000 ) ) ;
#66609 = EDGE_CURVE ( 'NONE', #52361, #65845, #14606, .T. ) ;
#66610 = ORIENTED_EDGE ( 'NONE', *, *, #7142, .F. ) ;
#66611 = FACE_OUTER_BOUND ( 'NONE', #49438, .T. ) ;
#66612 = CARTESIAN_POINT ( 'NONE',  ( 103.9573432206533283, -47.33663036165624050, 62.33753003781600199 ) ) ;
#66613 = DIRECTION ( 'NONE',  ( -0.000000000000000000, -0.000000000000000000, 1.000000000000000000 ) ) ;
#66614 = LINE ( 'NONE', #73881, #76816 ) ;
#66615 = CARTESIAN_POINT ( 'NONE',  ( 0.000000000000000000, 127.0000000000000000, -95.25000000000000000 ) ) ;
#66616 = CARTESIAN_POINT ( 'NONE',  ( 116.0809032858471852, -32.84949784884745583, 79.14991099019697174 ) ) ;
#66618 = CARTESIAN_POINT ( 'NONE',  ( 102.8528367378537922, -46.24122135049434235, 173.2441967044829596 ) ) ;
#66617 = CARTESIAN_POINT ( 'NONE',  ( 25.56670390244797275, -62.87844715994099687, 137.2178068554150059 ) ) ;
#66620 = VECTOR ( 'NONE', #67382, 1000.000000000000000 ) ;
#66619 = CARTESIAN_POINT ( 'NONE',  ( 182.5667039024459939, -22.48495420874030515, -5.074374724088000832 ) ) ;
#66622 = EDGE_CURVE ( 'NONE', #16372, #10976, #76822, .T. ) ;
#66621 = CARTESIAN_POINT ( 'NONE',  ( 107.0667039024470313, -104.2784471599409528, 22.21780685541800082 ) ) ;
#66623 = ORIENTED_EDGE ( 'NONE', *, *, #53536, .F. ) ;
#66624 = AXIS2_PLACEMENT_3D ( 'NONE', #75340, #76227, #12667 ) ;
#66625 = DIRECTION ( 'NONE',  ( -1.000000000000000000, 0.000000000000000000, 0.000000000000000000 ) ) ;
#66626 = DIRECTION ( 'NONE',  ( 0.000000000000000000, 0.000000000000000000, 1.000000000000000000 ) ) ;
#66627 = DIRECTION ( 'NONE',  ( 0.000000000000000000, 1.000000000000000000, 0.000000000000000000 ) ) ;
#66628 = CARTESIAN_POINT ( 'NONE',  ( 97.81169607051373305, -40.51742273377266912, 46.63562653399714009 ) ) ;
#66630 = VERTEX_POINT ( 'NONE', #84102 ) ;
#66629 = CARTESIAN_POINT ( 'NONE',  ( 113.0474237710022578, -45.36542684395109148, 203.0584824187679374 ) ) ;
#66631 = CARTESIAN_POINT ( 'NONE',  ( -487.2989999999999782, 22.53639197104660141, 90.48749999999999716 ) ) ;
#66632 = CARTESIAN_POINT ( 'NONE',  ( 105.1049547281328671, -25.82818065531082041, 271.2061014663873380 ) ) ;
#66633 = CARTESIAN_POINT ( 'NONE',  ( 113.8717716195138792, -28.72781827743602889, 135.5156252759109634 ) ) ;
#66634 = CARTESIAN_POINT ( 'NONE',  ( -3.175000000000109956, 124.5870000000000033, 31.75000000000000000 ) ) ;
#66635 = CARTESIAN_POINT ( 'NONE',  ( 12.53577546185475988, 84.62767492864718122, -129.9527996235914884 ) ) ;
#66636 = AXIS2_PLACEMENT_3D ( 'NONE', #13842, #41524, #15188 ) ;
#66637 = DIRECTION ( 'NONE',  ( 1.000000000000000078E-15, -1.000000000000000083E-30, -1.000000000000000000 ) ) ;
#66638 = LINE ( 'NONE', #58916, #38048 ) ;
#66639 = EDGE_LOOP ( 'NONE', ( #58957, #16745, #36760, #77920 ) ) ;
#66640 =( REPRESENTATION_RELATIONSHIP ('NONE','NONE', #82876, #19449 ) REPRESENTATION_RELATIONSHIP_WITH_TRANSFORMATION ( #34008 )SHAPE_REPRESENTATION_RELATIONSHIP( ) );
#66641 = ORIENTED_EDGE ( 'NONE', *, *, #46853, .F. ) ;
#66642 = ORIENTED_EDGE ( 'NONE', *, *, #75547, .F. ) ;
#66643 = AXIS2_PLACEMENT_3D ( 'NONE', #87461, #52881, #58840 ) ;
#66644 = ORIENTED_EDGE ( 'NONE', *, *, #33409, .F. ) ;
#66645 = CARTESIAN_POINT ( 'NONE',  ( 25.56670390244805091, -42.82844715994167473, 293.2178068554150059 ) ) ;
#66646 = CARTESIAN_POINT ( 'NONE',  ( 98.44183741489698036, -42.05700530801248505, 7.768006228291934434 ) ) ;
#66647 = CARTESIAN_POINT ( 'NONE',  ( 37.35959712133899302, -48.62134037883190985, 300.4678068554150059 ) ) ;
#66648 = CARTESIAN_POINT ( 'NONE',  ( 112.3595036205099689, -139.4350393735792579, 247.7272646988739950 ) ) ;
#66649 = VECTOR ( 'NONE', #64972, 1000.000000000000000 ) ;
#66651 = CARTESIAN_POINT ( 'NONE',  ( 69.08968514148706674, -139.7014121172838657, 246.0198185477100026 ) ) ;
#66650 = DIRECTION ( 'NONE',  ( 0.000000000000000000, 1.000000000000000000, 0.000000000000000000 ) ) ;
#66652 = EDGE_CURVE ( 'NONE', #32905, #23593, #513, .T. ) ;
#66653 = CARTESIAN_POINT ( 'NONE',  ( 106.5889295881363950, -27.03189230550456656, 194.5381341137909601 ) ) ;
#66654 = VERTEX_POINT ( 'NONE', #28207 ) ;
#66655 = VERTEX_POINT ( 'NONE', #55898 ) ;
#66656 = VECTOR ( 'NONE', #27185, 1000.000000000000000 ) ;
#66658 = ORIENTED_EDGE ( 'NONE', *, *, #81841, .F. ) ;
#66657 = VECTOR ( 'NONE', #19228, 1000.000000000000000 ) ;
#66659 = LINE ( 'NONE', #17630, #54328 ) ;
#66660 = CARTESIAN_POINT ( 'NONE',  ( -187.8075999999999794, 0.000000000000000000, -6.349999999999999645 ) ) ;
#66661 = ADVANCED_FACE ( 'NONE', ( #49094 ), #83649, .T. ) ;
#66662 = CARTESIAN_POINT ( 'NONE',  ( 33.78129701732998313, -35.65087443492610930, -5.074374724088000832 ) ) ;
#66663 = CARTESIAN_POINT ( 'NONE',  ( 114.3823783366371316, -42.62471689273790076, 39.70634521065896649 ) ) ;
#66664 = PLANE ( 'NONE',  #45846 ) ;
#66665 = AXIS2_PLACEMENT_3D ( 'NONE', #57883, #65144, #63357 ) ;
#66666 = CARTESIAN_POINT ( 'NONE',  ( 49.35211078756498893, -35.65087443492551245, -5.074374724088000832 ) ) ;
#66667 = AXIS2_PLACEMENT_3D ( 'NONE', #78628, #30896, #45394 ) ;
#66668 = CARTESIAN_POINT ( 'NONE',  ( 112.1213531720970309, -45.14146623880455422, 238.0070538473399324 ) ) ;
#66669 = LINE ( 'NONE', #46203, #5141 ) ;
#66670 = VERTEX_POINT ( 'NONE', #69117 ) ;
#66671 = CARTESIAN_POINT ( 'NONE',  ( 103.3201801717304136, -27.45767654545007375, 56.38204572563600436 ) ) ;
#66672 = ORIENTED_EDGE ( 'NONE', *, *, #33901, .F. ) ;
#66673 = FACE_OUTER_BOUND ( 'NONE', #88058, .T. ) ;
#66674 = CARTESIAN_POINT ( 'NONE',  ( 101.8554017947406862, -30.44658510084856218, 38.44523322673398980 ) ) ;
#66675 = EDGE_CURVE ( 'NONE', #48555, #38912, #18933, .T. ) ;
#66676 = AXIS2_PLACEMENT_3D ( 'NONE', #23349, #8818, #23785 ) ;
#66677 = CARTESIAN_POINT ( 'NONE',  ( 136.5887892044422642, -17.63370978841804870, 7.053538376718607950 ) ) ;
#66678 = DIRECTION ( 'NONE',  ( 1.000000000000000000, 6.055337108828351666E-16, 0.000000000000000000 ) ) ;
#66679 = VECTOR ( 'NONE', #35224, 1000.000000000000000 ) ;
#66680 = CARTESIAN_POINT ( 'NONE',  ( -12.61954384753730096, 84.20405175638288142, 117.8825647057245192 ) ) ;
#66681 = ORIENTED_EDGE ( 'NONE', *, *, #79153, .F. ) ;
#66682 = CARTESIAN_POINT ( 'NONE',  ( 67.06670390244701707, -79.67844715994098692, 180.4678068554179902 ) ) ;
#66683 = DIRECTION ( 'NONE',  ( 0.000000000000000000, 0.000000000000000000, 1.000000000000000000 ) ) ;
#66684 = EDGE_LOOP ( 'NONE', ( #21582, #19211 ) ) ;
#66685 = CARTESIAN_POINT ( 'NONE',  ( 95.77883191840808763, -40.33907488607122360, 131.5727681330539554 ) ) ;
#66686 = ORIENTED_EDGE ( 'NONE', *, *, #45855, .T. ) ;
#66687 = CARTESIAN_POINT ( 'NONE',  ( 115.5717340297064197, -37.51483979961712123, 78.17527697093396455 ) ) ;
#66688 = ORIENTED_CLOSED_SHELL ( 'NONE', *, #76417, .F. );
#66689 = CARTESIAN_POINT ( 'NONE',  ( 151.0371591254575776, -24.42818131005592264, 129.9678068554149775 ) ) ;
#66690 = CARTESIAN_POINT ( 'NONE',  ( 115.8107094469502272, -38.34209669562990541, 85.11301187732594542 ) ) ;
#66691 = CARTESIAN_POINT ( 'NONE',  ( 132.2857443282839824, -83.77844715994092439, 55.21780685541800437 ) ) ;
#66692 = CARTESIAN_POINT ( 'NONE',  ( 107.0667039024470313, -104.2784471599409528, 24.21780685541800082 ) ) ;
#66693 = AXIS2_PLACEMENT_3D ( 'NONE', #11498, #39193, #40980 ) ;
#66694 = CARTESIAN_POINT ( 'NONE',  ( 96.81221355789537597, -38.90410760351644370, 27.49276813305395706 ) ) ;
#66695 = LINE ( 'NONE', #50838, #52617 ) ;
#66696 = ORIENTED_EDGE ( 'NONE', *, *, #81519, .T. ) ;
#66697 = CARTESIAN_POINT ( 'NONE',  ( 177.8371591254545478, -47.82818131005477369, 129.9678068554150059 ) ) ;
#66698 = ORIENTED_EDGE ( 'NONE', *, *, #85850, .T. ) ;
#66699 = CARTESIAN_POINT ( 'NONE',  ( -118.3867465934798702, 71.53193882405243187, -6.370299515174613347 ) ) ;
#66700 = EDGE_LOOP ( 'NONE', ( #33147, #2751 ) ) ;
#66701 = EDGE_LOOP ( 'NONE', ( #31853, #54569, #10958, #15415 ) ) ;
#66702 = EDGE_CURVE ( 'NONE', #49269, #28852, #64100, .T. ) ;
#66703 = VECTOR ( 'NONE', #3785, 1000.000000000000000 ) ;
#66704 = CARTESIAN_POINT ( 'NONE',  ( -187.8075999999999794, 20.32000000000000028, -3.174999999999999822 ) ) ;
#66705 = ORIENTED_EDGE ( 'NONE', *, *, #17540, .F. ) ;
#66706 = CARTESIAN_POINT ( 'NONE',  ( 96.93540839703290146, -34.51582869190840341, 256.1432443235307232 ) ) ;
#66707 = DIRECTION ( 'NONE',  ( 0.000000000000000000, 0.000000000000000000, -1.000000000000000000 ) ) ;
#66708 = CARTESIAN_POINT ( 'NONE',  ( 115.7831076508929300, -41.80230954465056215, 189.4064586061371358 ) ) ;
#66709 = EDGE_CURVE ( 'NONE', #58383, #26947, #1572, .T. ) ;
#66710 = CARTESIAN_POINT ( 'NONE',  ( 104.0427601340384030, -47.36105469373795529, 63.36800622829197494 ) ) ;
#66711 = CARTESIAN_POINT ( 'NONE',  ( 117.0719050840518065, -35.46253235289662342, 44.92728796927281110 ) ) ;
#66712 = ORIENTED_EDGE ( 'NONE', *, *, #38419, .T. ) ;
#66713 = CARTESIAN_POINT ( 'NONE',  ( 113.2456828512594598, -28.75880519094399546, 114.5535222254891750 ) ) ;
#66714 = AXIS2_PLACEMENT_3D ( 'NONE', #87878, #32901, #82425 ) ;
#66715 = ADVANCED_FACE ( 'NONE', ( #49542 ), #75925, .F. ) ;
#66716 = CARTESIAN_POINT ( 'NONE',  ( -48.02966122971776741, 93.07500000000001705, 75.53254848357481421 ) ) ;
#66717 = VERTEX_POINT ( 'NONE', #29568 ) ;
#66718 = VECTOR ( 'NONE', #8993, 1000.000000000000000 ) ;
#66719 = CARTESIAN_POINT ( 'NONE',  ( 46.03715912545343514, -48.62818131006090283, 180.4678068554150911 ) ) ;
#66720 = CARTESIAN_POINT ( 'NONE',  ( 100.8868559669706713, -44.69971346806422474, 113.0528871607769332 ) ) ;
#66721 = CARTESIAN_POINT ( 'NONE',  ( 97.03753386688401861, -33.96379371595038776, 251.1127681330538337 ) ) ;
#66722 = DIRECTION ( 'NONE',  ( -3.100000000000000258E-29, 3.100000000000000044E-14, 1.000000000000000000 ) ) ;
#66723 = CARTESIAN_POINT ( 'NONE',  ( 72.06648329127396835, -9.729447159941065237, 14.67562527591093513 ) ) ;
#66724 = CARTESIAN_POINT ( 'NONE',  ( 78.22143491579828378, -38.77077206071901117, 2.188418444519958150 ) ) ;
#66725 = CARTESIAN_POINT ( 'NONE',  ( 102.3370036867683268, -28.24990410829322940, 254.9038483995052502 ) ) ;
#66727 = CARTESIAN_POINT ( 'NONE',  ( 98.60777729073579678, -43.80857954853289016, 67.86895860924497015 ) ) ;
#66726 = DIRECTION ( 'NONE',  ( -1.000000000000000000, 0.000000000000000000, 0.000000000000000000 ) ) ;
#66728 = CARTESIAN_POINT ( 'NONE',  ( 114.8489081444445645, 71.25364465473249709, 62.08545131505363202 ) ) ;
#66729 = CARTESIAN_POINT ( 'NONE',  ( 113.1024245609201984, -28.17526227570857955, 129.5870538473399449 ) ) ;
#66730 = ORIENTED_EDGE ( 'NONE', *, *, #27922, .T. ) ;
#66732 = ADVANCED_FACE ( 'NONE', ( #73 ), #57254, .F. ) ;
#66731 = CARTESIAN_POINT ( 'NONE',  ( 132.6453213455548337, -21.08531275930677040, 7.905164235256782135 ) ) ;
#66733 = VERTEX_POINT ( 'NONE', #77730 ) ;
#66734 = VECTOR ( 'NONE', #75086, 1000.000000000000000 ) ;
#66735 = PLANE ( 'NONE',  #6172 ) ;
#66736 = DIRECTION ( 'NONE',  ( -0.000000000000000000, -1.000000000000000000, -0.000000000000000000 ) ) ;
#66737 = EDGE_CURVE ( 'NONE', #19244, #34907, #6879, .T. ) ;
#66738 = CARTESIAN_POINT ( 'NONE',  ( 103.1875000000000000, 120.6499999999999915, 7.937500000000369482 ) ) ;
#66739 = ORIENTED_EDGE ( 'NONE', *, *, #78329, .T. ) ;
#66740 = CARTESIAN_POINT ( 'NONE',  ( 98.34969834581170289, -31.65685598046560045, 50.90648325210623426 ) ) ;
#66742 = ORIENTED_EDGE ( 'NONE', *, *, #5734, .F. ) ;
#66741 = CARTESIAN_POINT ( 'NONE',  ( 116.9635770353169733, -33.20817898692279613, 114.0984824187679720 ) ) ;
#66743 = LINE ( 'NONE', #10447, #55230 ) ;
#66744 = CONICAL_SURFACE ( 'NONE', #7299, 10.41399999999997839, 0.7853981633974744803 ) ;
#66745 = CARTESIAN_POINT ( 'NONE',  ( -129.9368274816650626, 82.54999999999999716, -12.70000000000045404 ) ) ;
#66746 = DIRECTION ( 'NONE',  ( 0.000000000000000000, 0.000000000000000000, 1.000000000000000000 ) ) ;
#66747 = ORIENTED_EDGE ( 'NONE', *, *, #19785, .T. ) ;
#66748 = CARTESIAN_POINT ( 'NONE',  ( 114.7424063621565722, -43.81651770963347303, 123.2327681330539519 ) ) ;
#66749 = APPLICATION_PROTOCOL_DEFINITION ( 'draft international standard', 'automotive_design', 1998, #32907 ) ;
#66750 = DIRECTION ( 'NONE',  ( 0.000000000000000000, 0.000000000000000000, 1.000000000000000000 ) ) ;
#66751 = DIRECTION ( 'NONE',  ( 0.000000000000000000, 0.000000000000000000, -1.000000000000000000 ) ) ;
#66752 = ORIENTED_EDGE ( 'NONE', *, *, #50230, .T. ) ;
#66753 = AXIS2_PLACEMENT_3D ( 'NONE', #4740, #53299, #87858 ) ;
#66754 = VERTEX_POINT ( 'NONE', #20960 ) ;
#66755 = FACE_OUTER_BOUND ( 'NONE', #86137, .T. ) ;
#66756 = CARTESIAN_POINT ( 'NONE',  ( 107.0664832912739399, -36.72944715994095333, 357.5272416190308604 ) ) ;
#66757 = CARTESIAN_POINT ( 'NONE',  ( 109.6430120585716281, -46.48008675498888209, 157.7814586033456692 ) ) ;
#66758 = CARTESIAN_POINT ( 'NONE',  ( 44.45000000000000284, 111.1250000000000000, 257.1750000000000114 ) ) ;
#66760 = CARTESIAN_POINT ( 'NONE',  ( -12.03342778677654934, 78.46830267626332045, -117.9437853765525404 ) ) ;
#66759 = CARTESIAN_POINT ( 'NONE',  ( 113.2452453786383728, -28.75847917007356003, 104.5523170862238800 ) ) ;
#66761 = PLANE ( 'NONE',  #89266 ) ;
#66762 = VECTOR ( 'NONE', #25456, 1000.000000000000000 ) ;
#66763 = EDGE_LOOP ( 'NONE', ( #44130, #64225 ) ) ;
#66764 = DIRECTION ( 'NONE',  ( 1.000000000000000000, 0.000000000000000000, 0.000000000000000000 ) ) ;
#66765 = EDGE_CURVE ( 'NONE', #73152, #85115, #16837, .T. ) ;
#66766 = CARTESIAN_POINT ( 'NONE',  ( 110.4719531740380063, -47.31314961125941210, 203.8241967044819489 ) ) ;
#66768 = ORIENTED_EDGE ( 'NONE', *, *, #85011, .F. ) ;
#66767 = DIRECTION ( 'NONE',  ( 0.000000000000000000, 1.000000000000000000, 0.000000000000000000 ) ) ;
#66769 = AXIS2_PLACEMENT_3D ( 'NONE', #80432, #66783, #74049 ) ;
#66770 = CARTESIAN_POINT ( 'NONE',  ( 101.5079035968564654, -28.64143341885332816, 46.55562527591094835 ) ) ;
#66771 = CARTESIAN_POINT ( 'NONE',  ( 116.9902980441214595, -35.35395306989185116, 53.93600868140660509 ) ) ;
#66772 = DIRECTION ( 'NONE',  ( 1.000000000000000000, 0.000000000000000000, -9.299908063537909262E-17 ) ) ;
#66773 = CARTESIAN_POINT ( 'NONE',  ( 162.7866693523297954, -29.62846900981741527, 117.4678068554150485 ) ) ;
#66774 = VECTOR ( 'NONE', #68668, 1000.000000000000000 ) ;
#66775 = ORIENTED_EDGE ( 'NONE', *, *, #62484, .T. ) ;
#66776 = CYLINDRICAL_SURFACE ( 'NONE', #55880, 12.44599999999999795 ) ;
#66777 = ORIENTED_EDGE ( 'NONE', *, *, #65217, .F. ) ;
#66778 = ORIENTED_EDGE ( 'NONE', *, *, #89274, .F. ) ;
#66779 = CARTESIAN_POINT ( 'NONE',  ( 116.3948728625927060, -35.60798670905003860, 235.3653928297059679 ) ) ;
#66780 = CIRCLE ( 'NONE', #58098, 2.517500000000005844 ) ;
#66781 = DIRECTION ( 'NONE',  ( 1.000000000000000078E-15, -1.000000000000000000, 0.000000000000000000 ) ) ;
#66782 = EDGE_CURVE ( 'NONE', #62285, #9081, #21870, .T. ) ;
#66783 = DIRECTION ( 'NONE',  ( -0.000000000000000000, 1.000000000000000000, 0.000000000000000000 ) ) ;
#66784 = LINE ( 'NONE', #61308, #30122 ) ;
#66785 = AXIS2_PLACEMENT_3D ( 'NONE', #60440, #88185, #25940 ) ;
#66786 = CARTESIAN_POINT ( 'NONE',  ( 82.64938057483485068, -37.67376371870361851, 2.871651383883024433 ) ) ;
#66787 = ORIENTED_EDGE ( 'NONE', *, *, #32770, .T. ) ;
#66788 = CARTESIAN_POINT ( 'NONE',  ( 60.32499999999999574, 82.54999999999999716, 344.4418053999999643 ) ) ;
#66789 = DIRECTION ( 'NONE',  ( 4.299999999999999979E-14, -1.000000000000000000, 0.000000000000000000 ) ) ;
#66790 = ORIENTED_EDGE ( 'NONE', *, *, #10937, .T. ) ;
#66791 = CARTESIAN_POINT ( 'NONE',  ( 111.7637953458032172, -46.71243375810367837, 287.9146728949587555 ) ) ;
#66792 = ORIENTED_EDGE ( 'NONE', *, *, #73679, .T. ) ;
#66793 = VERTEX_POINT ( 'NONE', #66304 ) ;
#66795 = EDGE_CURVE ( 'NONE', #65852, #24816, #71211, .T. ) ;
#66794 = CARTESIAN_POINT ( 'NONE',  ( 101.6725443455464131, -43.49748584897681525, 269.8471379886391901 ) ) ;
#66796 = EDGE_CURVE ( 'NONE', #23298, #85840, #16396, .T. ) ;
#66797 = DIRECTION ( 'NONE',  ( 0.000000000000000000, 1.000000000000000000, 0.000000000000000000 ) ) ;
#66798 = CARTESIAN_POINT ( 'NONE',  ( 23.18019461599323350, 78.27143315885348329, 300.7803427218691468 ) ) ;
#66799 = CARTESIAN_POINT ( 'NONE',  ( 184.5667039024480118, -48.82844715994099971, 300.9178068554150514 ) ) ;
#66800 = DIRECTION ( 'NONE',  ( 0.000000000000000000, -0.8660254037844336006, -0.5000000000000088818 ) ) ;
#66801 = CARTESIAN_POINT ( 'NONE',  ( 98.39890672360048995, -29.79614961819730468, 191.7775300378159784 ) ) ;
#66802 = LINE ( 'NONE', #24144, #64542 ) ;
#66803 = ORIENTED_EDGE ( 'NONE', *, *, #41452, .T. ) ;
#66804 = CARTESIAN_POINT ( 'NONE',  ( 101.0411209824609813, -27.40783209567417700, 66.54514908543495721 ) ) ;
#66805 = DIRECTION ( 'NONE',  ( 0.000000000000000000, 1.000000000000000000, 0.000000000000000000 ) ) ;
#66806 = ADVANCED_FACE ( 'NONE', ( #24106 ), #23666, .F. ) ;
#66807 = VERTEX_POINT ( 'NONE', #78642 ) ;
#66808 = ORIENTED_EDGE ( 'NONE', *, *, #42935, .F. ) ;
#66809 = VERTEX_POINT ( 'NONE', #17729 ) ;
#66810 = AXIS2_PLACEMENT_3D ( 'NONE', #40437, #61762, #33631 ) ;
#66811 = AXIS2_PLACEMENT_3D ( 'NONE', #15159, #21535, #42835 ) ;
#66812 = CARTESIAN_POINT ( 'NONE',  ( 103.1875000000000000, 127.0000000000000000, -7.143749999999640110 ) ) ;
#66813 = LINE ( 'NONE', #81809, #58744 ) ;
#66814 = CARTESIAN_POINT ( 'NONE',  ( 0.000000000000000000, 0.000000000000000000, 0.000000000000000000 ) ) ;
#66815 = ADVANCED_FACE ( 'NONE', ( #45404 ), #57714, .T. ) ;
#66816 = CARTESIAN_POINT ( 'NONE',  ( 101.2865843167392654, -43.98814532200950822, 119.8595189410199566 ) ) ;
#66817 = CARTESIAN_POINT ( 'NONE',  ( 96.49610902845032001, -31.31747537214017640, 241.9499109901969689 ) ) ;
#66818 = DIRECTION ( 'NONE',  ( 0.7071067809773464719, -0.7071067813957485626, 7.071067809773472419E-16 ) ) ;
#66819 = EDGE_LOOP ( 'NONE', ( #39172, #1128, #2191, #5159 ) ) ;
#66820 = CARTESIAN_POINT ( 'NONE',  ( 130.4924867222204341, 94.58014758961630264, -4.091264198875782299 ) ) ;
#66821 = DIRECTION ( 'NONE',  ( 0.000000000000000000, -1.000000000000000000, 0.000000000000000000 ) ) ;
#66822 = VECTOR ( 'NONE', #10385, 1000.000000000000000 ) ;
#66823 = ORIENTED_EDGE ( 'NONE', *, *, #485, .T. ) ;
#66824 = ORIENTED_EDGE ( 'NONE', *, *, #29455, .T. ) ;
#66825 = FACE_OUTER_BOUND ( 'NONE', #77591, .T. ) ;
#66826 = VERTEX_POINT ( 'NONE', #4091 ) ;
#66827 = ORIENTED_EDGE ( 'NONE', *, *, #18411, .T. ) ;
#66828 = CARTESIAN_POINT ( 'NONE',  ( -215.9000000000000057, 53.97500000000000142, 50.79999999999999716 ) ) ;
#66829 = LINE ( 'NONE', #65929, #34150 ) ;
#66830 = DIRECTION ( 'NONE',  ( 0.000000000000000000, 0.000000000000000000, 1.000000000000000000 ) ) ;
#66831 = CARTESIAN_POINT ( 'NONE',  ( 115.2191710476659665, -34.18193581181276386, 173.4895626852199371 ) ) ;
#66832 = CARTESIAN_POINT ( 'NONE',  ( 117.4283214861109457, -38.22576773620406954, 28.71276813305395592 ) ) ;
#66834 = ADVANCED_FACE ( 'NONE', ( #65429 ), #10899, .T. ) ;
#66833 = DIRECTION ( 'NONE',  ( 0.000000000000000000, -1.000000000000000000, 0.000000000000000000 ) ) ;
#66835 = EDGE_LOOP ( 'NONE', ( #5056, #4465, #35968, #48774 ) ) ;
#66836 = EDGE_CURVE ( 'NONE', #80800, #43956, #29125, .T. ) ;
#66837 = PLANE ( 'NONE',  #71665 ) ;
#66838 = VECTOR ( 'NONE', #12952, 1000.000000000000000 ) ;
#66839 = ORIENTED_EDGE ( 'NONE', *, *, #43620, .T. ) ;
#66840 = EDGE_CURVE ( 'NONE', #17885, #26732, #31792, .T. ) ;
#66841 = CIRCLE ( 'NONE', #81400, 0.9999999999999940048 ) ;
#66842 = FACE_OUTER_BOUND ( 'NONE', #10348, .T. ) ;
#66843 = ORIENTED_EDGE ( 'NONE', *, *, #53549, .F. ) ;
#66844 = CARTESIAN_POINT ( 'NONE',  ( 98.32086286370073935, -31.82106486744336493, 166.9192892379911655 ) ) ;
#66845 = ADVANCED_FACE ( 'NONE', ( #71803 ), #9576, .F. ) ;
#66846 = CARTESIAN_POINT ( 'NONE',  ( 101.9931413102871005, -45.44577570166600822, 32.15663476389070752 ) ) ;
#66847 = DIRECTION ( 'NONE',  ( 0.000000000000000000, 0.000000000000000000, 1.000000000000000000 ) ) ;
#66848 = VECTOR ( 'NONE', #70787, 1000.000000000000000 ) ;
#66849 = PLANE ( 'NONE',  #71263 ) ;
#66850 = ORIENTED_EDGE ( 'NONE', *, *, #23571, .F. ) ;
#66851 = CARTESIAN_POINT ( 'NONE',  ( 115.9640307963821186, -42.20482783266999149, 18.38705384733896153 ) ) ;
#66852 = CARTESIAN_POINT ( 'NONE',  ( 101.9391980234526187, -27.60234874203171884, 56.48419670448296159 ) ) ;
#66853 = SHAPE_REPRESENTATION_RELATIONSHIP ( 'NONE' , 'NONE' ,  #42769, #43438 ) ;
#66855 = FACE_OUTER_BOUND ( 'NONE', #13156, .T. ) ;
#66854 = DIRECTION ( 'NONE',  ( -0.7071067811865475727, 0.000000000000000000, 0.7071067811865475727 ) ) ;
#66856 = CARTESIAN_POINT ( 'NONE',  ( 108.4175026908246622, -26.73503768359202937, 145.9693458669439110 ) ) ;
#66857 = FACE_BOUND ( 'NONE', #70400, .T. ) ;
#66858 = VECTOR ( 'NONE', #81710, 1000.000000000000000 ) ;
#66859 = LINE ( 'NONE', #16935, #41553 ) ;
#66860 = CIRCLE ( 'NONE', #84400, 3.500000000000003109 ) ;
#66861 = CYLINDRICAL_SURFACE ( 'NONE', #8087, 5.041900000000001825 ) ;
#66862 = ORIENTED_EDGE ( 'NONE', *, *, #27986, .F. ) ;
#66863 = CARTESIAN_POINT ( 'NONE',  ( 116.4271464750313498, -31.96187137292554681, 44.20133956162491984 ) ) ;
#66864 = CARTESIAN_POINT ( 'NONE',  ( 104.1858290503737408, -26.67344577167302688, 221.2984824187679465 ) ) ;
#66865 = CARTESIAN_POINT ( 'NONE',  ( 107.6079817216441796, -48.59237387041279987, 38.61276813305397582 ) ) ;
#66867 = DIRECTION ( 'NONE',  ( 0.000000000000000000, 0.000000000000000000, 1.000000000000000000 ) ) ;
#66866 = DIRECTION ( 'NONE',  ( -0.7071067811865274777, 0.7071067811865675568, -7.071067811864971448E-16 ) ) ;
#66868 = DIRECTION ( 'NONE',  ( -0.9217329428042198014, -0.3878251953515564066, 1.203464411458912131E-14 ) ) ;
#66869 = VERTEX_POINT ( 'NONE', #85894 ) ;
#66870 = CARTESIAN_POINT ( 'NONE',  ( -469.3583484187089994, 53.97500000000000142, 3.174999999999999822 ) ) ;
#66871 = ORIENTED_EDGE ( 'NONE', *, *, #23977, .T. ) ;
#66872 = CARTESIAN_POINT ( 'NONE',  ( 114.6661721138974315, -42.88640786233941782, 84.28419670448195689 ) ) ;
#66874 = VERTEX_POINT ( 'NONE', #85456 ) ;
#66873 = CARTESIAN_POINT ( 'NONE',  ( 8.586325160335727347, 91.92393960641707906, 130.2739338507628020 ) ) ;
#66875 = AXIS2_PLACEMENT_3D ( 'NONE', #71372, #79525, #10901 ) ;
#66876 = CARTESIAN_POINT ( 'NONE',  ( 101.6619702986603073, -45.61876124157276280, 243.1413395616249886 ) ) ;
#66877 = DIRECTION ( 'NONE',  ( 1.000000000000000000, 0.000000000000000000, 0.000000000000000000 ) ) ;
#66878 = CARTESIAN_POINT ( 'NONE',  ( 29.56648329127298069, -71.37844715994266664, 342.9256252759109884 ) ) ;
#66879 = LINE ( 'NONE', #10142, #8061 ) ;
#66880 = CARTESIAN_POINT ( 'NONE',  ( 177.0371591254543375, -48.62818131005480637, 300.4678068554149490 ) ) ;
#66881 = DIRECTION ( 'NONE',  ( 0.000000000000000000, 0.000000000000000000, -1.000000000000000000 ) ) ;
#66882 = DIRECTION ( 'NONE',  ( 0.000000000000000000, 0.000000000000000000, -1.000000000000000000 ) ) ;
#66883 = CARTESIAN_POINT ( 'NONE',  ( 116.8431970675092515, -40.18699730018606431, 178.5680062282919778 ) ) ;
#66884 = ORIENTED_EDGE ( 'NONE', *, *, #85507, .F. ) ;
#66885 = VECTOR ( 'NONE', #31424, 1000.000000000000227 ) ;
#66886 = ORIENTED_EDGE ( 'NONE', *, *, #809, .F. ) ;
#66887 = CARTESIAN_POINT ( 'NONE',  ( 108.0951925567892431, -27.89746624773302841, 126.4158690201829813 ) ) ;
#66888 = AXIS2_PLACEMENT_3D ( 'NONE', #8290, #86381, #71860 ) ;
#66889 = PLANE ( 'NONE',  #83471 ) ;
#66890 = EDGE_CURVE ( 'NONE', #47202, #70326, #85004, .T. ) ;
#66892 = DIRECTION ( 'NONE',  ( 0.000000000000000000, 1.000000000000000000, 0.000000000000000000 ) ) ;
#66891 = CARTESIAN_POINT ( 'NONE',  ( 115.2378349030890092, -31.35427756934441845, 250.2899109901960344 ) ) ;
#66893 = DIRECTION ( 'NONE',  ( 4.299999999999999979E-14, -1.000000000000000000, 0.000000000000000000 ) ) ;
#66894 = DIRECTION ( 'NONE',  ( 2.775557561562888827E-14, -1.000000000000000000, 0.000000000000000000 ) ) ;
#66895 = EDGE_CURVE ( 'NONE', #84235, #5137, #64983, .T. ) ;
#66896 = CARTESIAN_POINT ( 'NONE',  ( 19.56648329127400032, 12.92155284005902516, 333.4006252759108975 ) ) ;
#66897 = ADVANCED_FACE ( 'NONE', ( #3646 ), #72626, .F. ) ;
#66898 = DIRECTION ( 'NONE',  ( 1.365069428641121829E-15, 0.000000000000000000, 1.000000000000000000 ) ) ;
#66899 = FACE_OUTER_BOUND ( 'NONE', #87373, .T. ) ;
#66900 = CARTESIAN_POINT ( 'NONE',  ( -72.96458098368600531, 117.4749999999999943, -80.10833098368780725 ) ) ;
#66901 = B_SPLINE_SURFACE_WITH_KNOTS ( 'NONE', 3, 3, ( 
 ( #39581, #62721, #42705, #70444, #6863 ),
 ( #15031, #41809, #69546, #498, #14132 ),
 ( #15491, #83629, #35910, #49973, #1857 ),
 ( #8219, #69097, #63622, #49525, #20943 ),
 ( #63170, #1409, #70902, #41364, #69994 ) ),
 .UNSPECIFIED., .F., .F., .F.,
 ( 4, 1, 4 ),
 ( 4, 1, 4 ),
 ( 0.000000000000000000, 0.5714285714285709528, 1.000000000000000000 ),
 ( 0.1438910682813560049, 3.135239217345689777, 7.123703416098150498 ),
 .UNSPECIFIED. ) ;
#66902 = CARTESIAN_POINT ( 'NONE',  ( 113.1426608820138426, -26.58408993604425419, 204.6470538473399756 ) ) ;
#66903 = ORIENTED_EDGE ( 'NONE', *, *, #76441, .T. ) ;
#66904 = ORIENTED_EDGE ( 'NONE', *, *, #38192, .F. ) ;
#66905 = EDGE_CURVE ( 'NONE', #79856, #36953, #24545, .T. ) ;
#66906 = AXIS2_PLACEMENT_3D ( 'NONE', #51466, #77866, #23799 ) ;
#66907 = EDGE_CURVE ( 'NONE', #8413, #74068, #84253, .T. ) ;
#66908 = LINE ( 'NONE', #32831, #79336 ) ;
#66909 = CARTESIAN_POINT ( 'NONE',  ( 80.06648329127399677, -15.97944715994105813, 1.625625275910943746 ) ) ;
#66910 = CARTESIAN_POINT ( 'NONE',  ( 33.98325472291465132, 124.5870000000000033, -3.174999999999999822 ) ) ;
#66911 = CARTESIAN_POINT ( 'NONE',  ( 138.8167039024479834, -57.40094715994099772, 60.91780685541480267 ) ) ;
#66912 = VECTOR ( 'NONE', #20294, 1000.000000000000000 ) ;
#66913 = ADVANCED_FACE ( 'NONE', ( #30023 ), #82208, .F. ) ;
#66914 = CARTESIAN_POINT ( 'NONE',  ( -24.79284581386642827, 184.0000000000000000, 0.000000000000000000 ) ) ;
#66915 = VERTEX_POINT ( 'NONE', #25424 ) ;
#66916 = CARTESIAN_POINT ( 'NONE',  ( -7.205548786489490269E-13, 117.4749999999999943, 103.1875000000000000 ) ) ;
#66917 = EDGE_CURVE ( 'NONE', #79853, #68630, #26195, .T. ) ;
#66918 = CARTESIAN_POINT ( 'NONE',  ( 117.1973380236488111, -34.26920065746595867, 209.0156252759109634 ) ) ;
#66919 = CARTESIAN_POINT ( 'NONE',  ( 172.5664832912740110, -9.303447159940999356, 138.9256252759119832 ) ) ;
#66920 = EDGE_LOOP ( 'NONE', ( #56662, #65173, #908, #42667, #23486, #6622 ) ) ;
#66921 = VERTEX_POINT ( 'NONE', #40834 ) ;
#66922 = CIRCLE ( 'NONE', #27766, 3.299999999999997158 ) ;
#66923 = CARTESIAN_POINT ( 'NONE',  ( 98.09052178646700781, -41.13971508595705728, 62.69037633451134184 ) ) ;
#66924 = DIRECTION ( 'NONE',  ( 0.000000000000000000, 0.000000000000000000, 1.000000000000000000 ) ) ;
#66925 = B_SPLINE_CURVE_WITH_KNOTS ( 'NONE', 3,
 ( #34745, #66231, #87153, #19779, #48800, #62452, #27043, #74743, #19335, #75195, #76535, #226, #40663, #82480, #61998, #12521, #40205, #55606, #38536, #31723, #24919, #53816, #81583, #67925, #20234, #12975, #5712, #68384, #47906, #6161 ),
 .UNSPECIFIED., .F., .F.,
 ( 4, 2, 2, 2, 1, 2, 2, 2, 2, 2, 2, 2, 1, 2, 2, 4 ),
 ( 0.5000000000000000000, 0.5624999999999806821, 0.5937499999999708011, 0.6093749999999663602, 0.6171874999999658051, 0.6210937499999669154, 0.6249999999999680256, 0.6874999999999692468, 0.7187499999999715783, 0.7499999999999740208, 0.8124999999999727995, 0.8437499999999724665, 0.8593749999999686917, 0.8671874999999705791, 0.8749999999999724665, 1.000000000000000000 ),
 .UNSPECIFIED. ) ;
#66926 = CARTESIAN_POINT ( 'NONE',  ( 97.92338036926128098, -40.78103718271854916, 166.6584133301706458 ) ) ;
#66927 = AXIS2_PLACEMENT_3D ( 'NONE', #24302, #9330, #51531 ) ;
#66928 = EDGE_CURVE ( 'NONE', #65246, #29858, #4987, .T. ) ;
#66929 = CARTESIAN_POINT ( 'NONE',  ( 107.1674220045319288, -28.56736792770730560, 32.88523322673398042 ) ) ;
#66930 = LINE ( 'NONE', #4711, #20330 ) ;
#66931 = ORIENTED_EDGE ( 'NONE', *, *, #23337, .T. ) ;
#66932 = LINE ( 'NONE', #73746, #17482 ) ;
#66933 = CARTESIAN_POINT ( 'NONE',  ( 81.91948822002333941, -16.69035895458603846, 7.660272404653420963 ) ) ;
#66934 = EDGE_LOOP ( 'NONE', ( #59441, #84041, #60181, #2230, #68812, #48413, #23988 ) ) ;
#66935 = EDGE_LOOP ( 'NONE', ( #63625, #57423, #70674, #57140 ) ) ;
#66936 = FACE_OUTER_BOUND ( 'NONE', #2242, .T. ) ;
#66937 = ORIENTED_EDGE ( 'NONE', *, *, #24154, .T. ) ;
#66938 = ORIENTED_EDGE ( 'NONE', *, *, #12463, .T. ) ;
#66939 = DIRECTION ( 'NONE',  ( 0.000000000000000000, 0.000000000000000000, -1.000000000000000000 ) ) ;
#66940 = CARTESIAN_POINT ( 'NONE',  ( 111.7162562550164608, -28.95820004563618610, 54.08194363760093637 ) ) ;
#66941 = CARTESIAN_POINT ( 'NONE',  ( 117.4357963365922615, -35.45519799489562729, 193.9241967044829664 ) ) ;
#66942 = AXIS2_PLACEMENT_3D ( 'NONE', #51320, #85885, #17278 ) ;
#66943 = CARTESIAN_POINT ( 'NONE',  ( 113.6008039948045933, -28.63430547549723570, 164.5356252759109736 ) ) ;
#66945 = CARTESIAN_POINT ( 'NONE',  ( 111.7736368399375522, -46.73334422087322082, 283.9146728949585849 ) ) ;
#66944 = CARTESIAN_POINT ( 'NONE',  ( 31.71315051186898870, -31.94127993907790852, 237.4678068554150059 ) ) ;
#66946 = DIRECTION ( 'NONE',  ( 0.000000000000000000, 0.000000000000000000, 1.000000000000000000 ) ) ;
#66947 = FACE_OUTER_BOUND ( 'NONE', #4580, .T. ) ;
#66948 = VERTEX_POINT ( 'NONE', #80861 ) ;
#66949 = EDGE_CURVE ( 'NONE', #16246, #38148, #8693, .T. ) ;
#66950 = ORIENTED_EDGE ( 'NONE', *, *, #37105, .T. ) ;
#66951 = EDGE_CURVE ( 'NONE', #75328, #26178, #74028, .T. ) ;
#66952 = AXIS2_PLACEMENT_3D ( 'NONE', #46831, #4629, #60011 ) ;
#66953 = VECTOR ( 'NONE', #48924, 1000.000000000000000 ) ;
#66954 = CARTESIAN_POINT ( 'NONE',  ( 123.6837132603318707, -17.59493780205716362, 219.5838068554170093 ) ) ;
#66955 = CARTESIAN_POINT ( 'NONE',  ( 112.2268274879326668, -45.83864656583022423, 212.9870538473389558 ) ) ;
#66956 = ORIENTED_EDGE ( 'NONE', *, *, #83207, .F. ) ;
#66957 = CARTESIAN_POINT ( 'NONE',  ( 108.6750451637706618, -26.42898313331718541, 189.9527681330539792 ) ) ;
#66958 = CYLINDRICAL_SURFACE ( 'NONE', #83373, 7.143750000000004263 ) ;
#66959 = PLANE ( 'NONE',  #54971 ) ;
#66960 = CYLINDRICAL_SURFACE ( 'NONE', #42044, 4.762500000000001066 ) ;
#66961 = CARTESIAN_POINT ( 'NONE',  ( 107.0664832912739399, -36.72944715994096754, 299.5704287327187103 ) ) ;
#66963 = DIRECTION ( 'NONE',  ( 0.000000000000000000, 1.000000000000000000, -0.000000000000000000 ) ) ;
#66962 = CARTESIAN_POINT ( 'NONE',  ( 112.8804553289902799, -43.12032145944222350, 277.6356252759110816 ) ) ;
#66964 = LINE ( 'NONE', #74675, #85891 ) ;
#66965 = DIRECTION ( 'NONE',  ( 3.213938816075602116E-15, 0.000000000000000000, 1.000000000000000000 ) ) ;
#66966 = CARTESIAN_POINT ( 'NONE',  ( -186.2398777604659870, 101.5999999999999943, 107.9500000000000028 ) ) ;
#66967 = FACE_OUTER_BOUND ( 'NONE', #80205, .T. ) ;
#66968 = DIRECTION ( 'NONE',  ( 1.000000000000000000, 1.000000000000000078E-15, -0.000000000000000000 ) ) ;
#66969 = DIRECTION ( 'NONE',  ( 1.000000000000000000, 1.000000000000000078E-15, 0.000000000000000000 ) ) ;
#66971 = ORIENTED_EDGE ( 'NONE', *, *, #87, .T. ) ;
#66970 = FACE_OUTER_BOUND ( 'NONE', #32563, .T. ) ;
#66972 = CARTESIAN_POINT ( 'NONE',  ( 136.8105871997954921, -18.91414947189459994, 6.758631288822851246 ) ) ;
#66973 = CARTESIAN_POINT ( 'NONE',  ( 98.92532678050559980, -30.18208626920050719, 240.7870538473399620 ) ) ;
#66974 = CARTESIAN_POINT ( 'NONE',  ( 117.5953528424095254, -42.16796915894857278, 89.44705384733997278 ) ) ;
#66975 = CARTESIAN_POINT ( 'NONE',  ( 96.72972436280956288, -34.86144565006776475, 237.1841967044819626 ) ) ;
#66976 = FACE_OUTER_BOUND ( 'NONE', #75919, .T. ) ;
#66977 = LINE ( 'NONE', #25640, #6864 ) ;
#66979 = CARTESIAN_POINT ( 'NONE',  ( 115.5712346005784354, -42.04052312869856678, 39.38203999088909057 ) ) ;
#66978 = LINE ( 'NONE', #17932, #2 ) ;
#66980 = DIRECTION ( 'NONE',  ( -3.100000000000000258E-29, 3.100000000000000044E-14, 1.000000000000000000 ) ) ;
#66981 = VECTOR ( 'NONE', #16053, 1000.000000000000000 ) ;
#66982 = DIRECTION ( 'NONE',  ( 1.000000000000000000, 0.000000000000000000, 0.000000000000000000 ) ) ;
#66983 = AXIS2_PLACEMENT_3D ( 'NONE', #71463, #36924, #30111 ) ;
#66984 = ORIENTED_EDGE ( 'NONE', *, *, #14724, .T. ) ;
#66985 = ORIENTED_EDGE ( 'NONE', *, *, #43555, .T. ) ;
#66986 = CARTESIAN_POINT ( 'NONE',  ( 115.7614890496577402, -39.26115509793221747, 138.0114674471239766 ) ) ;
#66988 = ORIENTED_EDGE ( 'NONE', *, *, #48226, .T. ) ;
#66987 = CARTESIAN_POINT ( 'NONE',  ( 20.90327949605574887, 45.74637997433028858, 31.85781312205738303 ) ) ;
#66989 = CARTESIAN_POINT ( 'NONE',  ( 51.06648329127400388, 0.2215528400590083269, 330.1506252759110680 ) ) ;
#66990 = CARTESIAN_POINT ( 'NONE',  ( 97.81366378802363215, -42.73395665195496917, 142.7965776568629508 ) ) ;
#66991 = CARTESIAN_POINT ( 'NONE',  ( -31.75000000000000000, 17.78000000000000114, -3.174999999999779998 ) ) ;
#66992 = CIRCLE ( 'NONE', #24984, 4.874999999999990230 ) ;
#66993 = CARTESIAN_POINT ( 'NONE',  ( 78.35735255114492759, -16.57277629268521224, 7.749696248603636484 ) ) ;
#66994 = FACE_OUTER_BOUND ( 'NONE', #70523, .T. ) ;
#66995 = CARTESIAN_POINT ( 'NONE',  ( 68.06670390244704549, -114.5284471599409812, 55.21780685541800437 ) ) ;
#66996 = CARTESIAN_POINT ( 'NONE',  ( 117.3137205126584348, -38.32096045344801638, 68.69181575210198787 ) ) ;
#66997 = ORIENTED_EDGE ( 'NONE', *, *, #76159, .F. ) ;
#66998 = ADVANCED_FACE ( 'NONE', ( #75377 ), #11808, .F. ) ;
#66999 = ORIENTED_EDGE ( 'NONE', *, *, #10919, .F. ) ;
#67000 = ORIENTED_EDGE ( 'NONE', *, *, #73704, .F. ) ;
#67001 = CARTESIAN_POINT ( 'NONE',  ( 142.8679068202682458, 10.65431904611001634, 396.9756252759102040 ) ) ;
#67003 = DIRECTION ( 'NONE',  ( -1.000000000000000000, -1.734723475976808672E-15, 0.000000000000000000 ) ) ;
#67002 = CARTESIAN_POINT ( 'NONE',  ( 98.25516505653069999, -40.97492784622581041, 167.6841967044819626 ) ) ;
#67004 = DIRECTION ( 'NONE',  ( 0.000000000000000000, 0.000000000000000000, 1.000000000000000000 ) ) ;
#67005 = EDGE_CURVE ( 'NONE', #19900, #84272, #12249, .T. ) ;
#67006 = DIRECTION ( 'NONE',  ( 0.000000000000000000, -1.000000000000000000, 0.000000000000000000 ) ) ;
#67007 = EDGE_CURVE ( 'NONE', #83824, #23447, #59930, .T. ) ;
#67008 = CARTESIAN_POINT ( 'NONE',  ( -100.8961411191535973, 120.6499999999999915, -3.968750000001104894 ) ) ;
#67009 = EDGE_CURVE ( 'NONE', #49381, #54125, #54441, .T. ) ;
#67010 = CARTESIAN_POINT ( 'NONE',  ( 180.3521107875639871, -35.65087443492551245, -5.074374724088000832 ) ) ;
#67011 = CARTESIAN_POINT ( 'NONE',  ( 67.06803888862225449, -67.87902570666702218, 245.5599109093815002 ) ) ;
#67012 = CARTESIAN_POINT ( 'NONE',  ( 102.9796410358629828, -46.29638950891627047, 92.25562527591097250 ) ) ;
#67013 = ORIENTED_EDGE ( 'NONE', *, *, #73110, .F. ) ;
#67014 = EDGE_LOOP ( 'NONE', ( #87041, #83153, #80598, #9700 ) ) ;
#67015 = EDGE_CURVE ( 'NONE', #53062, #58845, #89005, .T. ) ;
#67016 = CARTESIAN_POINT ( 'NONE',  ( 10.08079905861141867, 90.28579524239225407, 130.1664991954059474 ) ) ;
#67017 = DIRECTION ( 'NONE',  ( 1.000000000000000078E-15, -1.000000000000000000, 0.000000000000000000 ) ) ;
#67018 = AXIS2_PLACEMENT_3D ( 'NONE', #64863, #71247, #37160 ) ;
#67019 = DIRECTION ( 'NONE',  ( 0.000000000000000000, -1.000000000000000000, 0.000000000000000000 ) ) ;
#67020 = CARTESIAN_POINT ( 'NONE',  ( 103.8146984276687022, -29.21261587019397155, 153.2195189410199418 ) ) ;
#67021 = EDGE_CURVE ( 'NONE', #34082, #75654, #81756, .T. ) ;
#67022 = CIRCLE ( 'NONE', #53900, 3.299999999999997158 ) ;
#67023 = ADVANCED_FACE ( 'NONE', ( #13153 ), #80407, .T. ) ;
#67024 = CARTESIAN_POINT ( 'NONE',  ( -68.53801554307499089, 120.6499999999999915, 74.15067561874188584 ) ) ;
#67025 = EDGE_LOOP ( 'NONE', ( #68352, #46632 ) ) ;
#67026 = ORIENTED_EDGE ( 'NONE', *, *, #10906, .T. ) ;
#67027 = CARTESIAN_POINT ( 'NONE',  ( 84.19170390244700286, -68.87844715994097555, 138.7178068554180186 ) ) ;
#67028 = VERTEX_POINT ( 'NONE', #12707 ) ;
#67029 = PRODUCT_DEFINITION_SHAPE ( 'NONE', 'NONE',  #3331 ) ;
#67030 = VERTEX_POINT ( 'NONE', #59485 ) ;
#67031 = CARTESIAN_POINT ( 'NONE',  ( 77.31652006362755003, -18.90534128960216620, 6.749824347015198178 ) ) ;
#67033 = ADVANCED_FACE ( 'NONE', ( #73576 ), #11352, .T. ) ;
#67032 = AXIS2_PLACEMENT_3D ( 'NONE', #32046, #46998, #19322 ) ;
#67034 = CARTESIAN_POINT ( 'NONE',  ( 108.9963713912396912, -28.08052754339530921, 221.3330118773259585 ) ) ;
#67035 = CARTESIAN_POINT ( 'NONE',  ( 41.56648329127399677, -18.82844715994099971, 141.0426252759120018 ) ) ;
#67036 = CARTESIAN_POINT ( 'NONE',  ( 31.71315051186898870, -31.94127993907790852, -5.074374724088000832 ) ) ;
#67037 = VECTOR ( 'NONE', #29911, 1000.000000000000000 ) ;
#67038 = LINE ( 'NONE', #88393, #18345 ) ;
#67039 = ORIENTED_EDGE ( 'NONE', *, *, #77706, .T. ) ;
#67040 = ORIENTED_EDGE ( 'NONE', *, *, #79747, .F. ) ;
#67041 = VECTOR ( 'NONE', #30754, 999.9999999999998863 ) ;
#67042 = VERTEX_POINT ( 'NONE', #63075 ) ;
#67043 = VERTEX_POINT ( 'NONE', #7232 ) ;
#67044 = AXIS2_PLACEMENT_3D ( 'NONE', #22086, #7984, #69769 ) ;
#67045 = CARTESIAN_POINT ( 'NONE',  ( 114.7858077920586908, -40.64262416812939449, 246.2833284648299639 ) ) ;
#67046 = CARTESIAN_POINT ( 'NONE',  ( 96.01222827763220380, -41.06966167057572648, 96.62419670448197451 ) ) ;
#67047 = CARTESIAN_POINT ( 'NONE',  ( 117.0329088946583624, -32.00354160957719074, 64.19086337114899266 ) ) ;
#67048 = CARTESIAN_POINT ( 'NONE',  ( 112.6580179424443884, -28.69101886885839647, 249.5838068554166398 ) ) ;
#67049 = DIRECTION ( 'NONE',  ( 0.000000000000000000, -1.000000000000000000, 0.000000000000000000 ) ) ;
#67050 = DIRECTION ( 'NONE',  ( -2.999999999999999839E-15, 1.000000000000000000, -2.999999999999999900E-30 ) ) ;
#67051 = CARTESIAN_POINT ( 'NONE',  ( 105.7204281913532355, -24.95562743476950018, 156.1670538473399574 ) ) ;
#67052 = DIRECTION ( 'NONE',  ( 0.000000000000000000, -0.000000000000000000, -1.000000000000000000 ) ) ;
#67053 = VERTEX_POINT ( 'NONE', #62178 ) ;
#67054 = FACE_OUTER_BOUND ( 'NONE', #10967, .T. ) ;
#67055 = VERTEX_POINT ( 'NONE', #77615 ) ;
#67056 = ORIENTED_EDGE ( 'NONE', *, *, #70705, .T. ) ;
#67057 = CARTESIAN_POINT ( 'NONE',  ( 134.0664832912740110, -8.729447159940999512, 306.1181252759120071 ) ) ;
#67058 = DIRECTION ( 'NONE',  ( 0.000000000000000000, -1.000000000000000000, 0.000000000000000000 ) ) ;
#67059 = EDGE_CURVE ( 'NONE', #34506, #29469, #6772, .T. ) ;
#67060 = VERTEX_POINT ( 'NONE', #70348 ) ;
#67061 = B_SPLINE_CURVE_WITH_KNOTS ( 'NONE', 3,
 ( #10301, #3047, #17997, #52049, #79810, #4386, #73411, #38436, #4828, #65700, #30745, #17564, #32511, #38007, #3929, #16674, #25258, #73862 ),
 .UNSPECIFIED., .F., .F.,
 ( 4, 2, 2, 2, 2, 2, 2, 2, 4 ),
 ( 0.5000523659440618829, 0.5625458202010541475, 0.6250392744580464122, 0.6875327287150386768, 0.7500261829720309414, 0.8125196372290232061, 0.8750130914860154707, 0.9375065457430077354, 1.000000000000000000 ),
 .UNSPECIFIED. ) ;
#67062 = DIRECTION ( 'NONE',  ( 0.000000000000000000, 0.000000000000000000, 1.000000000000000000 ) ) ;
#67063 = ORIENTED_EDGE ( 'NONE', *, *, #57495, .T. ) ;
#67064 = CARTESIAN_POINT ( 'NONE',  ( 112.0659116076490136, -45.48839626926737623, 177.9897919413786553 ) ) ;
#67065 = CARTESIAN_POINT ( 'NONE',  ( 117.8566403422286299, -39.12769616061267186, 103.6403871806729455 ) ) ;
#67066 = CARTESIAN_POINT ( 'NONE',  ( 134.0664832912740110, -46.72944715994100306, 8.225625275910998013 ) ) ;
#67067 = CARTESIAN_POINT ( 'NONE',  ( 63.03715912545637678, -24.42818131006026761, 193.9678068554150911 ) ) ;
#67068 = PLANE ( 'NONE',  #41185 ) ;
#67069 = CARTESIAN_POINT ( 'NONE',  ( 98.13101841594837538, -32.75189731695855500, 100.9927681330539713 ) ) ;
#67071 = CARTESIAN_POINT ( 'NONE',  ( 118.8526415125688800, -37.69623653580512013, 184.7613395616249647 ) ) ;
#67070 = CARTESIAN_POINT ( 'NONE',  ( 98.58946256649487339, -99.96145986183361742, 2.217806855417864043 ) ) ;
#67072 = CARTESIAN_POINT ( 'NONE',  ( 2.332952152375709937E-14, 125.4759999999999991, 190.5000000000000000 ) ) ;
#67073 = CARTESIAN_POINT ( 'NONE',  ( 33.98325472291465132, 17.78000000000000114, 3.174999999999999822 ) ) ;
#67074 = EDGE_LOOP ( 'NONE', ( #32145, #57884 ) ) ;
#67075 = CARTESIAN_POINT ( 'NONE',  ( 210.2301280605339855, 25.81350000000000477, -58.73749999999999716 ) ) ;
#67076 = VECTOR ( 'NONE', #4438, 1000.000000000000000 ) ;
#67077 = DIRECTION ( 'NONE',  ( -1.821231995776179916E-16, 0.000000000000000000, -1.000000000000000000 ) ) ;
#67078 = CARTESIAN_POINT ( 'NONE',  ( 183.5150000000000148, 37.33800000000000097, 69.13087104677069306 ) ) ;
#67079 = FACE_BOUND ( 'NONE', #382, .T. ) ;
#67080 = EDGE_CURVE ( 'NONE', #43693, #21567, #28551, .T. ) ;
#67082 = EDGE_LOOP ( 'NONE', ( #30638, #12083, #47807, #9549, #10364, #9729, #77162, #65692, #79825, #32639, #23491, #21197 ) ) ;
#67081 = CARTESIAN_POINT ( 'NONE',  ( 107.5119097530387933, -47.18928756557821202, 237.6099109901969655 ) ) ;
#67083 = CYLINDRICAL_SURFACE ( 'NONE', #30614, 3.000000000000002665 ) ;
#67084 = CARTESIAN_POINT ( 'NONE',  ( 112.1974349349366804, -26.93816038506360755, 10.68038718067299087 ) ) ;
#67085 = CARTESIAN_POINT ( 'NONE',  ( 107.9492956907162267, -25.66517399690753720, 111.0251490854349754 ) ) ;
#67086 = PLANE ( 'NONE',  #79528 ) ;
#67087 = CARTESIAN_POINT ( 'NONE',  ( 80.81782300813070208, -39.40255221908358862, 8.160479982094777540 ) ) ;
#67088 = CARTESIAN_POINT ( 'NONE',  ( 19.56648329127303043, -71.37844715994266664, 342.9256252759109884 ) ) ;
#67089 = DIRECTION ( 'NONE',  ( 0.000000000000000000, 0.000000000000000000, -1.000000000000000000 ) ) ;
#67090 = VERTEX_POINT ( 'NONE', #34921 ) ;
#67091 = AXIS2_PLACEMENT_3D ( 'NONE', #1474, #61544, #89280 ) ;
#67092 = EDGE_CURVE ( 'NONE', #4783, #70047, #27910, .T. ) ;
#67093 = ORIENTED_EDGE ( 'NONE', *, *, #14776, .F. ) ;
#67094 = VERTEX_POINT ( 'NONE', #27668 ) ;
#67095 = VERTEX_POINT ( 'NONE', #27213 ) ;
#67096 = DIRECTION ( 'NONE',  ( 0.000000000000000000, 0.000000000000000000, 1.000000000000000000 ) ) ;
#67097 = CARTESIAN_POINT ( 'NONE',  ( 96.20032699425235023, -38.62430069186628856, 42.45181575210199298 ) ) ;
#67098 = CARTESIAN_POINT ( 'NONE',  ( 107.0664832912739968, -36.72944715994100306, 287.6356252759109680 ) ) ;
#67099 = CARTESIAN_POINT ( 'NONE',  ( 112.3589615562450774, -139.8532878908926307, 247.5529029630430102 ) ) ;
#67100 = CIRCLE ( 'NONE', #3308, 2.029999999999997140 ) ;
#67102 = CARTESIAN_POINT ( 'NONE',  ( 98.06670390244704549, -104.2784471599414076, 2.217806855418003043 ) ) ;
#67101 = CARTESIAN_POINT ( 'NONE',  ( 69.72411017812960665, 120.6499999999999915, 69.72411017813040246 ) ) ;
#67103 = CARTESIAN_POINT ( 'NONE',  ( 106.8904373410712481, -45.78382058659838094, 226.9714674471249509 ) ) ;
#67104 = VERTEX_POINT ( 'NONE', #70803 ) ;
#67105 = ORIENTED_EDGE ( 'NONE', *, *, #28078, .T. ) ;
#67106 = ORIENTED_EDGE ( 'NONE', *, *, #19166, .T. ) ;
#67107 = AXIS2_PLACEMENT_3D ( 'NONE', #12435, #40123, #52824 ) ;
#67108 = PLANE ( 'NONE',  #34039 ) ;
#67109 = CARTESIAN_POINT ( 'NONE',  ( 117.0718539717828008, -35.46213750492159278, 103.9271830989822263 ) ) ;
#67110 = DIRECTION ( 'NONE',  ( -1.000000000000000078E-15, 1.000000000000000083E-30, 1.000000000000000000 ) ) ;
#67111 = CARTESIAN_POINT ( 'NONE',  ( 179.8608231853560255, -35.55794170701751256, -5.074374724088000832 ) ) ;
#67112 = ADVANCED_FACE ( 'NONE', ( #83100 ), #8122, .T. ) ;
#67113 = CARTESIAN_POINT ( 'NONE',  ( 98.24556308671769500, -33.49403671529641713, 17.46634521065892898 ) ) ;
#67114 = EDGE_CURVE ( 'NONE', #65744, #50718, #48978, .T. ) ;
#67115 = CARTESIAN_POINT ( 'NONE',  ( 117.8914297010764756, 84.62843115047675724, 12.53565398905701578 ) ) ;
#67116 = EDGE_CURVE ( 'NONE', #63079, #11460, #56241, .T. ) ;
#67117 = DIRECTION ( 'NONE',  ( 0.000000000000000000, 0.000000000000000000, 1.000000000000000000 ) ) ;
#67118 = CARTESIAN_POINT ( 'NONE',  ( 107.9555263298577330, -25.64695713395843413, 265.0127681330543510 ) ) ;
#67119 = DIRECTION ( 'NONE',  ( -1.000000000000000000, 0.000000000000000000, 0.000000000000000000 ) ) ;
#67120 = ORIENTED_EDGE ( 'NONE', *, *, #71459, .T. ) ;
#67121 = ADVANCED_FACE ( 'NONE', ( #76715 ), #14499, .T. ) ;
#67122 = CARTESIAN_POINT ( 'NONE',  ( 98.34917020181003977, -31.65781948494475628, 56.90649411614629827 ) ) ;
#67123 = CARTESIAN_POINT ( 'NONE',  ( 0.000000000000000000, 82.54999999999999716, 92.46299999999996544 ) ) ;
#67124 = CARTESIAN_POINT ( 'NONE',  ( 113.8488019003066825, -42.10541956792432217, 46.12332846482897253 ) ) ;
#67125 = LINE ( 'NONE', #80329, #87086 ) ;
#67126 = CARTESIAN_POINT ( 'NONE',  ( 163.0959832912771219, -23.42844715993521021, 237.4678068554150059 ) ) ;
#67127 = EDGE_CURVE ( 'NONE', #72016, #56141, #42173, .T. ) ;
#67128 = CARTESIAN_POINT ( 'NONE',  ( -0.8397198549841756732, 95.25000000000002842, 118.5560000000000258 ) ) ;
#67129 = VERTEX_POINT ( 'NONE', #29020 ) ;
#67130 = CARTESIAN_POINT ( 'NONE',  ( 89.60916260784479448, 239.0000000000000000, 134.1927865330827103 ) ) ;
#67131 = CARTESIAN_POINT ( 'NONE',  ( 119.6090684540881171, 53.82079221388885770, -52.33119174590274270 ) ) ;
#67132 = VECTOR ( 'NONE', #46530, 1000.000000000000114 ) ;
#67133 = ORIENTED_EDGE ( 'NONE', *, *, #71601, .F. ) ;
#67134 = CARTESIAN_POINT ( 'NONE',  ( 118.9039262414038944, -36.16781539521252142, 118.8641967044819836 ) ) ;
#67135 = ORIENTED_EDGE ( 'NONE', *, *, #60025, .T. ) ;
#67136 = CARTESIAN_POINT ( 'NONE',  ( 116.0261628859374383, -38.04732875056770780, 73.14480078045792766 ) ) ;
#67137 = CARTESIAN_POINT ( 'NONE',  ( 160.5667039024485518, -48.82844715993551432, 180.4678068554150059 ) ) ;
#67138 = CARTESIAN_POINT ( 'NONE',  ( 103.0168143257329092, -28.81349422576414554, 116.8844404487539634 ) ) ;
#67139 = CARTESIAN_POINT ( 'NONE',  ( 81.84766347661002328, -83.77844715994098124, 222.2178068554179902 ) ) ;
#67140 = DIRECTION ( 'NONE',  ( -0.7071067811865426878, 0.000000000000000000, -0.7071067811865524577 ) ) ;
#67141 = CARTESIAN_POINT ( 'NONE',  ( 107.1956677504039135, -26.28336798021810239, 31.06705384733893283 ) ) ;
#67142 = DIRECTION ( 'NONE',  ( 1.000000000000000000, 0.000000000000000000, 0.000000000000000000 ) ) ;
#67143 = ORIENTED_EDGE ( 'NONE', *, *, #44114, .F. ) ;
#67144 = CIRCLE ( 'NONE', #14906, 2.125000000000001776 ) ;
#67145 = FACE_OUTER_BOUND ( 'NONE', #72579, .T. ) ;
#67146 = ORIENTED_EDGE ( 'NONE', *, *, #67555, .T. ) ;
#67147 = CARTESIAN_POINT ( 'NONE',  ( -117.8738102209308494, 81.71068249639866110, 12.69999999999959250 ) ) ;
#67148 = ORIENTED_EDGE ( 'NONE', *, *, #51911, .F. ) ;
#67149 = VERTEX_POINT ( 'NONE', #48086 ) ;
#67150 = CARTESIAN_POINT ( 'NONE',  ( 31.75000000000000000, 69.84999999999999432, 342.8999999999999773 ) ) ;
#67151 = ORIENTED_EDGE ( 'NONE', *, *, #12427, .F. ) ;
#67152 = CARTESIAN_POINT ( 'NONE',  ( 100.6696166679599003, -29.33055989933767904, 260.6441967044828516 ) ) ;
#67153 = CARTESIAN_POINT ( 'NONE',  ( 97.19489835230788799, -38.38517845848406296, 126.4581417767985698 ) ) ;
#67154 = CARTESIAN_POINT ( 'NONE',  ( 0.000000000000000000, 95.25000000000000000, 0.000000000000000000 ) ) ;
#67155 = CARTESIAN_POINT ( 'NONE',  ( 100.9411170126626587, -46.87412574091977291, 48.14419670448194211 ) ) ;
#67156 = FACE_OUTER_BOUND ( 'NONE', #2708, .T. ) ;
#67157 = EDGE_LOOP ( 'NONE', ( #4537, #73735, #75145, #51556 ) ) ;
#67158 = LINE ( 'NONE', #33092, #87348 ) ;
#67159 = LINE ( 'NONE', #17681, #66556 ) ;
#67160 = EDGE_CURVE ( 'NONE', #47420, #87937, #39514, .T. ) ;
#67161 = ORIENTED_EDGE ( 'NONE', *, *, #52274, .F. ) ;
#67162 = AXIS2_PLACEMENT_3D ( 'NONE', #54418, #39915, #60808 ) ;
#67163 = CARTESIAN_POINT ( 'NONE',  ( 45.66030316258350297, 82.54999999999999716, 358.0130000000000337 ) ) ;
#67164 = CARTESIAN_POINT ( 'NONE',  ( 196.2150000000000034, 30.98800000000000310, 57.14999999999999858 ) ) ;
#67165 = CARTESIAN_POINT ( 'NONE',  ( 104.5933598291445463, -26.62426044571792616, 285.2670538473396391 ) ) ;
#67166 = CARTESIAN_POINT ( 'NONE',  ( 62.03742497533746558, -23.42844715994041849, 300.4678068554150627 ) ) ;
#67167 = AXIS2_PLACEMENT_3D ( 'NONE', #53167, #59996, #39124 ) ;
#67168 = CARTESIAN_POINT ( 'NONE',  ( 107.0667039024469886, -67.87844715994094713, 173.2178068554179902 ) ) ;
#67169 = CARTESIAN_POINT ( 'NONE',  ( -194.1576000000000022, 101.5999999999999943, -45.33899999999999864 ) ) ;
#67170 = CARTESIAN_POINT ( 'NONE',  ( 106.8780034376490278, -45.26880352128168283, 271.9809912566482808 ) ) ;
#67173 = CARTESIAN_POINT ( 'NONE',  ( 96.67837842349544530, -37.29153504031420141, 72.36991099019596163 ) ) ;
#67172 = CARTESIAN_POINT ( 'NONE',  ( 172.5664832912729878, -18.82844715994071194, 258.9256252759120116 ) ) ;
#67171 = CIRCLE ( 'NONE', #19133, 12.60000000000000142 ) ;
#67174 = CARTESIAN_POINT ( 'NONE',  ( 115.0304089598074171, 71.47004980129892715, 61.74880860687861173 ) ) ;
#67175 = CARTESIAN_POINT ( 'NONE',  ( 108.8564100269821608, -47.04462182233018552, 167.7127681330539701 ) ) ;
#67176 = ORIENTED_EDGE ( 'NONE', *, *, #53761, .T. ) ;
#67177 = DIRECTION ( 'NONE',  ( -3.100000000000000258E-29, 3.100000000000000044E-14, 1.000000000000000000 ) ) ;
#67178 = EDGE_LOOP ( 'NONE', ( #14526, #46281, #11245, #20036 ) ) ;
#67179 = FACE_OUTER_BOUND ( 'NONE', #64023, .T. ) ;
#67180 = CARTESIAN_POINT ( 'NONE',  ( 115.0889047208644627, -30.61763667535547029, 65.34395860967845238 ) ) ;
#67181 = DIRECTION ( 'NONE',  ( 0.000000000000000000, -1.000000000000000000, 0.000000000000000000 ) ) ;
#67182 = ORIENTED_EDGE ( 'NONE', *, *, #50617, .T. ) ;
#67183 = CARTESIAN_POINT ( 'NONE',  ( 63.06670390244707392, -40.32844715994016838, 180.4678068554151196 ) ) ;
#67185 = ORIENTED_EDGE ( 'NONE', *, *, #42607, .T. ) ;
#67184 = CARTESIAN_POINT ( 'NONE',  ( 95.96722792477895325, -36.58315769931292749, 156.3280062282919687 ) ) ;
#67186 = LINE ( 'NONE', #88102, #43632 ) ;
#67187 = CARTESIAN_POINT ( 'NONE',  ( -130.5559693845970060, 95.24968527363473925, 0.8339068267398820344 ) ) ;
#67188 = LINE ( 'NONE', #4971, #22774 ) ;
#67189 = CARTESIAN_POINT ( 'NONE',  ( 167.6524903400753033, -48.32844715993521589, 300.4678068554149490 ) ) ;
#67190 = ORIENTED_EDGE ( 'NONE', *, *, #86925, .F. ) ;
#67191 = EDGE_CURVE ( 'NONE', #74209, #53860, #43065, .T. ) ;
#67192 = CARTESIAN_POINT ( 'NONE',  ( 111.8042541167996546, -25.83965636698058432, 134.7499109901969518 ) ) ;
#67193 = PRODUCT_CONTEXT ( 'NONE', #14364, 'mechanical' ) ;
#67194 = CIRCLE ( 'NONE', #59917, 2.000000000000001776 ) ;
#67195 = CYLINDRICAL_SURFACE ( 'NONE', #24006, 5.599999999999994316 ) ;
#67196 = DIRECTION ( 'NONE',  ( 0.000000000000000000, -1.000000000000000000, 0.000000000000000000 ) ) ;
#67197 = VERTEX_POINT ( 'NONE', #41721 ) ;
#67198 = CIRCLE ( 'NONE', #45452, 2.500000000000002220 ) ;
#67199 = ORIENTED_EDGE ( 'NONE', *, *, #44125, .T. ) ;
#67200 = CARTESIAN_POINT ( 'NONE',  ( 77.39114642429960611, 120.6499999999999915, -71.77848634863110533 ) ) ;
#67201 = DIRECTION ( 'NONE',  ( 0.000000000000000000, 1.000000000000000000, 0.000000000000000000 ) ) ;
#67202 = DIRECTION ( 'NONE',  ( 1.000000000000000000, 0.000000000000000000, 0.000000000000000000 ) ) ;
#67203 = DIRECTION ( 'NONE',  ( 0.000000000000000000, 0.000000000000000000, -1.000000000000000000 ) ) ;
#67205 = DIRECTION ( 'NONE',  ( 0.000000000000000000, 0.000000000000000000, 1.000000000000000000 ) ) ;
#67204 = CARTESIAN_POINT ( 'NONE',  ( 116.3183303039212291, -32.94226276200836878, 104.1356252759109680 ) ) ;
#67206 = CARTESIAN_POINT ( 'NONE',  ( 104.4897722840256904, -26.97885345335833662, 180.2814733255143551 ) ) ;
#67207 = CIRCLE ( 'NONE', #52654, 0.5000000000000004441 ) ;
#67208 = ORIENTED_EDGE ( 'NONE', *, *, #57918, .F. ) ;
#67209 = LINE ( 'NONE', #89011, #40399 ) ;
#67210 = CARTESIAN_POINT ( 'NONE',  ( 98.91665286848252947, -30.31703347128394910, 196.8080062282909637 ) ) ;
#67211 = EDGE_CURVE ( 'NONE', #19079, #89932, #77170, .T. ) ;
#67213 = ORIENTED_EDGE ( 'NONE', *, *, #7878, .F. ) ;
#67212 = DIRECTION ( 'NONE',  ( 0.7071067811865758834, -0.7071067811865192621, 7.071067811865766226E-16 ) ) ;
#67214 = CARTESIAN_POINT ( 'NONE',  ( 99.11394507416773081, -43.38496525699387973, 67.86895860924396118 ) ) ;
#67215 = ADVANCED_FACE ( 'NONE', ( #83992 ), #21765, .F. ) ;
#67216 = CARTESIAN_POINT ( 'NONE',  ( 117.0886499745419513, -37.65698274825507497, 53.75263814202077839 ) ) ;
#67217 = ADVANCED_FACE ( 'NONE', ( #42616, #22211 ), #54893, .F. ) ;
#67218 = CARTESIAN_POINT ( 'NONE',  ( 46.83715912545429205, -47.82818131006082751, 249.9678068554150343 ) ) ;
#67219 = CARTESIAN_POINT ( 'NONE',  ( 97.78478733939310530, -40.45112047135063449, 22.62993014185689944 ) ) ;
#67220 = ORIENTED_EDGE ( 'NONE', *, *, #26154, .T. ) ;
#67221 = DIRECTION ( 'NONE',  ( 1.000000000000000000, 0.000000000000000000, 0.000000000000000000 ) ) ;
#67222 = ADVANCED_FACE ( 'NONE', ( #13589 ), #69005, .T. ) ;
#67223 = VERTEX_POINT ( 'NONE', #31232 ) ;
#67224 = ORIENTED_EDGE ( 'NONE', *, *, #257, .T. ) ;
#67225 = CARTESIAN_POINT ( 'NONE',  ( 100.1238157808075186, -30.39889478464921524, 227.1577737820879577 ) ) ;
#67226 = AXIS2_PLACEMENT_3D ( 'NONE', #62496, #76586, #56108 ) ;
#67227 = CARTESIAN_POINT ( 'NONE',  ( 108.3351572350362062, -46.73467433967125118, 53.67707132820591909 ) ) ;
#67228 = CARTESIAN_POINT ( 'NONE',  ( -117.8738102209307215, 82.54999999999999716, -12.70000000000041318 ) ) ;
#67229 = VECTOR ( 'NONE', #34991, 1000.000000000000000 ) ;
#67230 = CARTESIAN_POINT ( 'NONE',  ( 97.06107109568941382, -37.99641195077763456, 81.42729194155585049 ) ) ;
#67231 = ADVANCED_FACE ( 'NONE', ( #52102 ), #71699, .T. ) ;
#67232 = DIRECTION ( 'NONE',  ( 0.000000000000000000, -1.000000000000000000, 0.000000000000000000 ) ) ;
#67233 = ORIENTED_EDGE ( 'NONE', *, *, #38318, .T. ) ;
#67234 = CARTESIAN_POINT ( 'NONE',  ( 123.6837132603318992, -20.11243780205710507, 239.5838068554165545 ) ) ;
#67235 = CARTESIAN_POINT ( 'NONE',  ( 100.9506838420298749, -28.71014652038285320, 36.59397677644053459 ) ) ;
#67236 = ADVANCED_FACE ( 'NONE', ( #9462 ), #78528, .T. ) ;
#67237 = ORIENTED_EDGE ( 'NONE', *, *, #22224, .F. ) ;
#67238 = CARTESIAN_POINT ( 'NONE',  ( 111.0463177226254174, -47.04157800189014438, 17.85753003781598380 ) ) ;
#67239 = ORIENTED_EDGE ( 'NONE', *, *, #21379, .T. ) ;
#67240 = EDGE_LOOP ( 'NONE', ( #199, #21375 ) ) ;
#67241 = CARTESIAN_POINT ( 'NONE',  ( 102.1781415585801511, -43.87122846086534622, 239.9290427505439709 ) ) ;
#67242 = CARTESIAN_POINT ( 'NONE',  ( 98.36735121233621726, -42.37464764417353535, 146.7965776568640024 ) ) ;
#67243 = FACE_OUTER_BOUND ( 'NONE', #35882, .T. ) ;
#67244 = DIRECTION ( 'NONE',  ( 1.000000000000000078E-15, -1.000000000000000083E-30, -1.000000000000000000 ) ) ;
#67245 = CARTESIAN_POINT ( 'NONE',  ( 182.3467384525650061, -36.02818131005800950, -5.074374724088000832 ) ) ;
#67246 = CARTESIAN_POINT ( 'NONE',  ( 103.7092163704185026, -26.14992651007402813, 201.3089586092439731 ) ) ;
#67247 = DIRECTION ( 'NONE',  ( 1.000000000000000000, 0.000000000000000000, 0.000000000000000000 ) ) ;
#67248 = ORIENTED_EDGE ( 'NONE', *, *, #46986, .F. ) ;
#67249 = AXIS2_PLACEMENT_3D ( 'NONE', #55711, #68032, #28482 ) ;
#67250 = CARTESIAN_POINT ( 'NONE',  ( 113.3686263934108780, -27.59268128360266914, 85.60800622829195561 ) ) ;
#67251 = DIRECTION ( 'NONE',  ( 1.387778780781444492E-15, 0.000000000000000000, -1.000000000000000000 ) ) ;
#67252 = VECTOR ( 'NONE', #25315, 1000.000000000000000 ) ;
#67253 = EDGE_LOOP ( 'NONE', ( #42782, #76178 ) ) ;
#67254 = ORIENTED_EDGE ( 'NONE', *, *, #43934, .T. ) ;
#67255 = ORIENTED_EDGE ( 'NONE', *, *, #43447, .T. ) ;
#67256 = AXIS2_PLACEMENT_3D ( 'NONE', #37080, #2569, #24343 ) ;
#67257 = CARTESIAN_POINT ( 'NONE',  ( 165.6738106836030227, -28.98061976758901892, -5.074374724088000832 ) ) ;
#67258 = LINE ( 'NONE', #5042, #71810 ) ;
#67259 = CARTESIAN_POINT ( 'NONE',  ( 117.0603328428218077, -38.08441083969534446, 153.7194074594665381 ) ) ;
#67260 = CARTESIAN_POINT ( 'NONE',  ( 101.0810522191901981, -29.63898995574150419, 148.4538046553059587 ) ) ;
#67261 = CARTESIAN_POINT ( 'NONE',  ( 113.1126646695910409, -46.01001268607183903, 219.0480062282919960 ) ) ;
#67262 = CARTESIAN_POINT ( 'NONE',  ( -27.27158787008326968, 184.0000000000000000, 0.000000000000000000 ) ) ;
#67263 = ORIENTED_EDGE ( 'NONE', *, *, #40125, .T. ) ;
#67264 = PRESENTATION_STYLE_ASSIGNMENT (( #88187 ) ) ;
#67265 = CARTESIAN_POINT ( 'NONE',  ( 7.661254700127833495, 82.54999999999999716, 320.6630000000000109 ) ) ;
#67266 = EDGE_CURVE ( 'NONE', #31158, #66754, #65323, .T. ) ;
#67267 = VERTEX_POINT ( 'NONE', #37170 ) ;
#67268 = VERTEX_POINT ( 'NONE', #79868 ) ;
#67269 = CIRCLE ( 'NONE', #32447, 1.000000000000000888 ) ;
#67270 = DIRECTION ( 'NONE',  ( -0.000000000000000000, 1.000000000000000000, -0.000000000000000000 ) ) ;
#67271 = ORIENTED_EDGE ( 'NONE', *, *, #32024, .T. ) ;
#67272 = ORIENTED_EDGE ( 'NONE', *, *, #66379, .T. ) ;
#67273 = CARTESIAN_POINT ( 'NONE',  ( 107.0664832912739399, -36.72944715994095333, 293.1356252759106837 ) ) ;
#67274 = LINE ( 'NONE', #80477, #2215 ) ;
#67275 = EDGE_CURVE ( 'NONE', #79236, #311, #29362, .T. ) ;
#67276 = DIRECTION ( 'NONE',  ( -0.9068632946707806397, 0.4214249218767882055, -9.068632946707802473E-16 ) ) ;
#67277 = CARTESIAN_POINT ( 'NONE',  ( 97.92582740012257148, -33.45545302834237589, 175.4752769709339759 ) ) ;
#67278 = CARTESIAN_POINT ( 'NONE',  ( 102.7370178780992234, -25.64411770250132250, 20.37276813305294354 ) ) ;
#67279 = CARTESIAN_POINT ( 'NONE',  ( 0.000000000000000000, 127.0000000000000000, 0.000000000000000000 ) ) ;
#67280 = ORIENTED_EDGE ( 'NONE', *, *, #85322, .T. ) ;
#67281 = CARTESIAN_POINT ( 'NONE',  ( -92.32962665258511947, 81.71068249639866110, -74.36911441044765070 ) ) ;
#67282 = ORIENTED_EDGE ( 'NONE', *, *, #88385, .T. ) ;
#67283 = CARTESIAN_POINT ( 'NONE',  ( 147.0667039024469886, -67.87844715994090450, 222.2178068554179902 ) ) ;
#67284 = VERTEX_POINT ( 'NONE', #85347 ) ;
#67285 = DIRECTION ( 'NONE',  ( 3.100000000000000258E-29, -3.100000000000000044E-14, -1.000000000000000000 ) ) ;
#67286 = CARTESIAN_POINT ( 'NONE',  ( 123.5302891131021710, -139.7352204321790339, 247.5112265945679724 ) ) ;
#67287 = CARTESIAN_POINT ( 'NONE',  ( 110.8534530311471400, -45.98465435386854949, 132.8855376447518211 ) ) ;
#67288 = VECTOR ( 'NONE', #31886, 1000.000000000000000 ) ;
#67289 = CARTESIAN_POINT ( 'NONE',  ( 116.3167039024470029, -68.87844715994093292, 222.2178068554179902 ) ) ;
#67290 = ORIENTED_EDGE ( 'NONE', *, *, #85286, .T. ) ;
#67291 = CARTESIAN_POINT ( 'NONE',  ( 112.1921266949303373, -27.58526089107821733, 34.66991099019695355 ) ) ;
#67292 = CARTESIAN_POINT ( 'NONE',  ( 100.9176109441957436, -28.25688269532019348, 71.57562527591099411 ) ) ;
#67293 = AXIS2_PLACEMENT_3D ( 'NONE', #57331, #23305, #9208 ) ;
#67295 = FACE_OUTER_BOUND ( 'NONE', #28629, .T. ) ;
#67294 = CARTESIAN_POINT ( 'NONE',  ( 60.32499999999999574, 82.54999999999999716, 344.4418053999999643 ) ) ;
#67296 = CARTESIAN_POINT ( 'NONE',  ( 113.2455109352893743, -28.75868235514402116, 145.5526372974719322 ) ) ;
#67297 = DIRECTION ( 'NONE',  ( 1.000000000000000000, 0.000000000000000000, 0.000000000000000000 ) ) ;
#67298 = FACE_BOUND ( 'NONE', #61662, .T. ) ;
#67299 = PLANE ( 'NONE',  #69266 ) ;
#67300 = CARTESIAN_POINT ( 'NONE',  ( 147.0664286958740945, -101.1139857980062118, 246.2087142436340059 ) ) ;
#67301 = EDGE_CURVE ( 'NONE', #8428, #76842, #26481, .T. ) ;
#67302 = ORIENTED_EDGE ( 'NONE', *, *, #14524, .T. ) ;
#67303 = CARTESIAN_POINT ( 'NONE',  ( 96.91385697446291658, -32.24201331651869396, 55.98324432352897162 ) ) ;
#67304 = CARTESIAN_POINT ( 'NONE',  ( 109.6058369744873886, -26.58188510553521056, 195.8813395616249977 ) ) ;
#67305 = CARTESIAN_POINT ( 'NONE',  ( 110.1643932622899200, -46.70643130671602705, 93.81562527591097478 ) ) ;
#67307 = LINE ( 'NONE', #74577, #36916 ) ;
#67306 = CARTESIAN_POINT ( 'NONE',  ( 104.4090054903168578, -46.45835489918496819, 172.3615705418780522 ) ) ;
#67308 = FACE_OUTER_BOUND ( 'NONE', #86917, .T. ) ;
#67309 = AXIS2_PLACEMENT_3D ( 'NONE', #55491, #116, #75972 ) ;
#67310 = AXIS2_PLACEMENT_3D ( 'NONE', #53037, #5382, #33081 ) ;
#67311 = DIRECTION ( 'NONE',  ( 0.000000000000000000, -1.000000000000000000, 2.048885995248194949E-16 ) ) ;
#67312 = EDGE_LOOP ( 'NONE', ( #9856, #75370, #87374, #56803 ) ) ;
#67313 = CARTESIAN_POINT ( 'NONE',  ( 116.9446180447426826, -41.83184233209001235, 89.44705384733897802 ) ) ;
#67315 = ORIENTED_EDGE ( 'NONE', *, *, #78534, .F. ) ;
#67314 = CARTESIAN_POINT ( 'NONE',  ( 11.32062350639499293, 88.30991999289778960, 130.0643505849274391 ) ) ;
#67316 = CIRCLE ( 'NONE', #4962, 25.39999999999999858 ) ;
#67317 = CARTESIAN_POINT ( 'NONE',  ( 116.5068947302721369, -41.18400185692900806, 224.4756252759109714 ) ) ;
#67318 = CARTESIAN_POINT ( 'NONE',  ( 116.7949704630636063, -39.38841653000326914, 254.6162222944404334 ) ) ;
#67319 = CARTESIAN_POINT ( 'NONE',  ( 114.5888079921489719, -43.35084876185531044, 148.2521628986096971 ) ) ;
#67320 = DIRECTION ( 'NONE',  ( 0.000000000000000000, 0.000000000000000000, 1.000000000000000000 ) ) ;
#67321 = EDGE_CURVE ( 'NONE', #60536, #11261, #64431, .T. ) ;
#67322 = CARTESIAN_POINT ( 'NONE',  ( 113.2454986953204781, -28.75867294251674267, 45.55229194285107752 ) ) ;
#67323 = CARTESIAN_POINT ( 'NONE',  ( 51.24204729617298426, -31.76306994223730840, -5.074374724088000832 ) ) ;
#67324 = CARTESIAN_POINT ( 'NONE',  ( -187.8075999999999794, 101.5999999999999943, 107.9500000000000028 ) ) ;
#67325 = CARTESIAN_POINT ( 'NONE',  ( 114.0056865186722490, -29.02320718445394476, 159.5051490854349652 ) ) ;
#67326 = VERTEX_POINT ( 'NONE', #9032 ) ;
#67327 = VERTEX_POINT ( 'NONE', #3100 ) ;
#67328 = CARTESIAN_POINT ( 'NONE',  ( 104.0080147226004925, -45.04654038386073012, 138.7272975916119435 ) ) ;
#67329 = CARTESIAN_POINT ( 'NONE',  ( 165.3359832912740046, -36.32844715994100682, -5.074374724088000832 ) ) ;
#67331 = DIRECTION ( 'NONE',  ( 0.000000000000000000, 0.000000000000000000, 1.000000000000000000 ) ) ;
#67330 = CARTESIAN_POINT ( 'NONE',  ( 104.1325824198641783, -27.39908484284276469, 246.3184824187669619 ) ) ;
#67332 = DIRECTION ( 'NONE',  ( -1.000000000000000000, 0.000000000000000000, 0.000000000000000000 ) ) ;
#67333 = CARTESIAN_POINT ( 'NONE',  ( 182.5667039024469886, -33.35206098992650681, -5.074374724088000832 ) ) ;
#67334 = EDGE_CURVE ( 'NONE', #36063, #46977, #44406, .T. ) ;
#67335 = FACE_OUTER_BOUND ( 'NONE', #77602, .T. ) ;
#67336 = DIRECTION ( 'NONE',  ( 0.000000000000000000, 0.000000000000000000, -1.000000000000000000 ) ) ;
#67337 = LINE ( 'NONE', #45535, #44413 ) ;
#67338 = EDGE_CURVE ( 'NONE', #39978, #12989, #9918, .T. ) ;
#67339 = CARTESIAN_POINT ( 'NONE',  ( 117.4047238282099102, -30.98758422922431066, 179.2299109901959753 ) ) ;
#67340 = PLANE ( 'NONE',  #35891 ) ;
#67341 = VERTEX_POINT ( 'NONE', #30798 ) ;
#67342 = ORIENTED_EDGE ( 'NONE', *, *, #6030, .F. ) ;
#67343 = CARTESIAN_POINT ( 'NONE',  ( -89.37861919290428148, 70.52006616879377532, -95.16559702356661887 ) ) ;
#67344 = CYLINDRICAL_SURFACE ( 'NONE', #8468, 7.999999999999992895 ) ;
#67345 = CARTESIAN_POINT ( 'NONE',  ( 188.5667039024479834, -65.37844715994100397, 132.3428068554150343 ) ) ;
#67346 = CARTESIAN_POINT ( 'NONE',  ( 7.778756678762479992E-15, 50.79999999999999716, 222.8849999999999909 ) ) ;
#67347 = AXIS2_PLACEMENT_3D ( 'NONE', #56350, #54986, #75018 ) ;
#67348 = CARTESIAN_POINT ( 'NONE',  ( 4.163101094985349692E-14, 127.0000000000000000, -98.60478223830740774 ) ) ;
#67349 = VERTEX_POINT ( 'NONE', #58491 ) ;
#67350 = FACE_OUTER_BOUND ( 'NONE', #8777, .T. ) ;
#67351 = AXIS2_PLACEMENT_3D ( 'NONE', #19486, #83506, #76694 ) ;
#67352 = CARTESIAN_POINT ( 'NONE',  ( 103.8197072928965810, -48.12676840017521585, 217.3556252759109668 ) ) ;
#67353 = CARTESIAN_POINT ( 'NONE',  ( 134.8178230081300910, -39.40255221908513761, 8.160479982094942741 ) ) ;
#67354 = ORIENTED_EDGE ( 'NONE', *, *, #4194, .T. ) ;
#67355 = ORIENTED_EDGE ( 'NONE', *, *, #29850, .T. ) ;
#67356 = CARTESIAN_POINT ( 'NONE',  ( 0.000000000000000000, 95.14999999999999147, 118.5560000000000116 ) ) ;
#67357 = DIRECTION ( 'NONE',  ( 0.7071067811865460184, 0.000000000000000000, 0.7071067811865487940 ) ) ;
#67358 = CARTESIAN_POINT ( 'NONE',  ( 97.81168148112675453, -40.51739256386586163, 162.6360428395636859 ) ) ;
#67359 = CARTESIAN_POINT ( 'NONE',  ( 99.24357903948710202, -34.39880452655780374, 28.91380465530596311 ) ) ;
#67360 = CARTESIAN_POINT ( 'NONE',  ( 117.2592865896494345, -39.02220311275136311, 144.6499109901969859 ) ) ;
#67361 = DIRECTION ( 'NONE',  ( 0.000000000000000000, 1.000000000000000000, 0.000000000000000000 ) ) ;
#67362 = VERTEX_POINT ( 'NONE', #2209 ) ;
#67363 = DIRECTION ( 'NONE',  ( 0.2588190451025131344, 0.000000000000000000, 0.9659258262890704216 ) ) ;
#67364 = CARTESIAN_POINT ( 'NONE',  ( 62.03715912545748523, -47.82818131006031592, 193.9678068554150911 ) ) ;
#67365 = ORIENTED_EDGE ( 'NONE', *, *, #76037, .T. ) ;
#67366 = ORIENTED_EDGE ( 'NONE', *, *, #42294, .T. ) ;
#67367 = VECTOR ( 'NONE', #29813, 1000.000000000000000 ) ;
#67368 = CIRCLE ( 'NONE', #52808, 2.999999999999919176 ) ;
#67369 = LINE ( 'NONE', #39228, #72023 ) ;
#67370 = AXIS2_PLACEMENT_3D ( 'NONE', #38500, #38951, #73929 ) ;
#67371 = VERTEX_POINT ( 'NONE', #23997 ) ;
#67372 = ORIENTED_EDGE ( 'NONE', *, *, #51323, .T. ) ;
#67373 = CARTESIAN_POINT ( 'NONE',  ( 72.96458098368650269, 127.0000000000000000, 72.96458098368729850 ) ) ;
#67374 = VECTOR ( 'NONE', #20611, 1000.000000000000000 ) ;
#67375 = ADVANCED_FACE ( 'NONE', ( #51668, #17179 ), #50791, .F. ) ;
#67376 = CARTESIAN_POINT ( 'NONE',  ( 115.9627085491522536, -40.61889491704908295, 57.92099125664801562 ) ) ;
#67377 = CARTESIAN_POINT ( 'NONE',  ( 115.4056828889858650, -30.43626719779562251, 219.3413395616249773 ) ) ;
#67378 = AXIS2_PLACEMENT_3D ( 'NONE', #66880, #18735, #39615 ) ;
#67379 = CARTESIAN_POINT ( 'NONE',  ( 117.0023065291009061, -39.93004192841232936, 158.5784824187679476 ) ) ;
#67381 = CARTESIAN_POINT ( 'NONE',  ( 99.77739493559407435, -44.20163642594127396, 17.96133956162493206 ) ) ;
#67380 = DIRECTION ( 'NONE',  ( -4.012088370409549976E-14, 1.000000000000000000, 0.000000000000000000 ) ) ;
#67382 = DIRECTION ( 'NONE',  ( 0.000000000000000000, 0.000000000000000000, -1.000000000000000000 ) ) ;
#67383 = LINE ( 'NONE', #18342, #74379 ) ;
#67384 = ORIENTED_EDGE ( 'NONE', *, *, #12391, .T. ) ;
#67385 = ORIENTED_EDGE ( 'NONE', *, *, #53750, .F. ) ;
#67386 = DIRECTION ( 'NONE',  ( 0.000000000000000000, 0.000000000000000000, -1.000000000000000000 ) ) ;
#67387 = CARTESIAN_POINT ( 'NONE',  ( 97.05395071892901626, -41.52132310946490890, 216.6937205140059461 ) ) ;
#67388 = EDGE_LOOP ( 'NONE', ( #50861, #78899, #36913, #17063 ) ) ;
#67389 = ADVANCED_FACE ( 'NONE', ( #36278 ), #38062, .T. ) ;
#67390 = CARTESIAN_POINT ( 'NONE',  ( 112.2051334037466432, -45.80035149650004200, 212.9870538473389558 ) ) ;
#67391 = CARTESIAN_POINT ( 'NONE',  ( 149.4532656544376721, -72.54365454176046057, 361.9756252759100335 ) ) ;
#67392 = CARTESIAN_POINT ( 'NONE',  ( -22.33653601812255474, 59.36077262818345446, 30.86733950792826775 ) ) ;
#67393 = CARTESIAN_POINT ( 'NONE',  ( 97.81542051716436958, -40.52653337087284058, 22.63640890594763633 ) ) ;
#67394 = DIRECTION ( 'NONE',  ( 0.000000000000000000, 0.000000000000000000, 1.000000000000000000 ) ) ;
#67395 = VECTOR ( 'NONE', #61923, 1000.000000000000000 ) ;
#67396 = EDGE_CURVE ( 'NONE', #55229, #56684, #8578, .T. ) ;
#67398 = CARTESIAN_POINT ( 'NONE',  ( 72.96458098368650269, 117.4749999999999943, 72.96458098368729850 ) ) ;
#67397 = CARTESIAN_POINT ( 'NONE',  ( 109.6536531575482769, -29.13850702246578095, 277.6356252759110816 ) ) ;
#67399 = CARTESIAN_POINT ( 'NONE',  ( -160.2664750769284865, 0.000000000000000000, 148.0533267522753818 ) ) ;
#67400 = DIRECTION ( 'NONE',  ( 0.000000000000000000, -1.000000000000000000, 0.000000000000000000 ) ) ;
#67401 = LINE ( 'NONE', #5193, #10688 ) ;
#67402 = EDGE_CURVE ( 'NONE', #34477, #51283, #57146, .T. ) ;
#67403 = CARTESIAN_POINT ( 'NONE',  ( 0.000000000000000000, 215.0000000000000000, 164.6557476874258441 ) ) ;
#67404 = CARTESIAN_POINT ( 'NONE',  ( 51.06670390244764945, -33.35206098992665602, 313.9678068554150059 ) ) ;
#67405 = EDGE_CURVE ( 'NONE', #31634, #42012, #84892, .T. ) ;
#67406 = CARTESIAN_POINT ( 'NONE',  ( 107.0667039024470313, -104.2784471599420755, -19.78219314458201694 ) ) ;
#67408 = ORIENTED_EDGE ( 'NONE', *, *, #66313, .T. ) ;
#67407 = CARTESIAN_POINT ( 'NONE',  ( 154.4409905298078058, -0.9147987323338667709, 542.9756252759101471 ) ) ;
#67409 = EDGE_CURVE ( 'NONE', #72895, #54496, #75767, .T. ) ;
#67410 = DIRECTION ( 'NONE',  ( 1.000000000000000000, 4.299999999999999979E-14, 1.000000000000000078E-15 ) ) ;
#67411 = CARTESIAN_POINT ( 'NONE',  ( 103.2955449146038376, -26.98642977692344758, 215.3699109901969848 ) ) ;
#67412 = CARTESIAN_POINT ( 'NONE',  ( 108.3194443806174405, -47.07896772641721839, 113.6727681330539639 ) ) ;
#67413 = CARTESIAN_POINT ( 'NONE',  ( 96.47406283524195203, -31.30618784601239923, 241.9499109901969689 ) ) ;
#67414 = DIRECTION ( 'NONE',  ( -0.000000000000000000, -1.000000000000000000, -0.000000000000000000 ) ) ;
#67415 = CARTESIAN_POINT ( 'NONE',  ( -487.2989999999999782, 97.78694598552380057, 3.968750000000479616 ) ) ;
#67417 = DIRECTION ( 'NONE',  ( 0.000000000000000000, 0.000000000000000000, 1.000000000000000000 ) ) ;
#67416 = DIRECTION ( 'NONE',  ( 1.000000000000000000, 0.000000000000000000, 0.000000000000000000 ) ) ;
#67418 = DIRECTION ( 'NONE',  ( 0.000000000000000000, -1.000000000000000000, 0.000000000000000000 ) ) ;
#67419 = EDGE_CURVE ( 'NONE', #64922, #60205, #61180, .T. ) ;
#67420 = CARTESIAN_POINT ( 'NONE',  ( 134.0664832912739826, -21.47944715994100306, 1.625625275910997480 ) ) ;
#67421 = ADVANCED_FACE ( 'NONE', ( #18055 ), #88003, .T. ) ;
#67422 = AXIS2_PLACEMENT_3D ( 'NONE', #46615, #60247, #66170 ) ;
#67423 = EDGE_CURVE ( 'NONE', #49178, #24254, #11241, .T. ) ;
#67424 = ORIENTED_EDGE ( 'NONE', *, *, #31874, .T. ) ;
#67425 = ORIENTED_EDGE ( 'NONE', *, *, #74276, .F. ) ;
#67426 = CARTESIAN_POINT ( 'NONE',  ( 111.2069583914694419, -45.51165039160690640, 137.3495626852199507 ) ) ;
#67428 = ORIENTED_EDGE ( 'NONE', *, *, #49988, .F. ) ;
#67427 = DIRECTION ( 'NONE',  ( 0.000000000000000000, 0.000000000000000000, -1.000000000000000000 ) ) ;
#67429 = CARTESIAN_POINT ( 'NONE',  ( 72.96458098368701428, 127.0000000000000000, -72.96458098368670164 ) ) ;
#67430 = CARTESIAN_POINT ( 'NONE',  ( 97.59110611908495514, -31.08311649095520934, 126.9108633711489915 ) ) ;
#67431 = EDGE_CURVE ( 'NONE', #46552, #88862, #17796, .T. ) ;
#67432 = DIRECTION ( 'NONE',  ( -0.9834602067153815907, -0.1811243269341220596, 0.000000000000000000 ) ) ;
#67433 = EDGE_CURVE ( 'NONE', #25068, #20813, #25765, .T. ) ;
#67434 = DIRECTION ( 'NONE',  ( 1.000000000000000078E-15, 1.000000000000000083E-30, -1.000000000000000000 ) ) ;
#67435 = FACE_OUTER_BOUND ( 'NONE', #71692, .T. ) ;
#67436 = DIRECTION ( 'NONE',  ( 1.639958061481212836E-42, -4.100000000000000342E-29, -1.000000000000000000 ) ) ;
#67437 = CARTESIAN_POINT ( 'NONE',  ( 107.2219638487720488, -26.36052190073617041, 80.07657765686398932 ) ) ;
#67438 = ORIENTED_EDGE ( 'NONE', *, *, #33681, .T. ) ;
#67439 = ORIENTED_EDGE ( 'NONE', *, *, #60712, .F. ) ;
#67440 = ORIENTED_EDGE ( 'NONE', *, *, #63686, .F. ) ;
#67441 = VECTOR ( 'NONE', #23009, 1000.000000000000000 ) ;
#67442 = CIRCLE ( 'NONE', #83419, 4.762500000000000178 ) ;
#67443 = DIRECTION ( 'NONE',  ( 0.000000000000000000, 0.000000000000000000, -1.000000000000000000 ) ) ;
#67444 = VECTOR ( 'NONE', #76622, 1000.000000000000000 ) ;
#67446 = LINE ( 'NONE', #33379, #73740 ) ;
#67445 = CARTESIAN_POINT ( 'NONE',  ( 99.36405074150921735, -30.70139697576588134, 151.7984824187679465 ) ) ;
#67447 = CIRCLE ( 'NONE', #2174, 3.300000000000000711 ) ;
#67448 = CARTESIAN_POINT ( 'NONE',  ( 74.06670390244701707, -90.27844715994098124, 51.21780685541800437 ) ) ;
#67449 = CARTESIAN_POINT ( 'NONE',  ( 12.03144885753538595, 78.46257116061715919, -130.0004926519013111 ) ) ;
#67451 = CARTESIAN_POINT ( 'NONE',  ( 107.0664832912739968, -36.72944715994100306, 293.2242906452868851 ) ) ;
#67450 = AXIS2_PLACEMENT_3D ( 'NONE', #65310, #24428, #73906 ) ;
#67452 = EDGE_CURVE ( 'NONE', #27298, #43762, #5333, .T. ) ;
#67453 = AXIS2_PLACEMENT_3D ( 'NONE', #14864, #15753, #30273 ) ;
#67454 = CARTESIAN_POINT ( 'NONE',  ( 130.3998166246059895, 12.92155284005730387, 355.9756252759109998 ) ) ;
#67455 = DIRECTION ( 'NONE',  ( 0.000000000000000000, 1.000000000000000000, 0.000000000000000000 ) ) ;
#67456 = EDGE_CURVE ( 'NONE', #24524, #62958, #35162, .T. ) ;
#67457 = CARTESIAN_POINT ( 'NONE',  ( 114.5517459224756749, -44.00510994954056088, 98.21276813305395592 ) ) ;
#67458 = ORIENTED_EDGE ( 'NONE', *, *, #28026, .T. ) ;
#67459 = EDGE_LOOP ( 'NONE', ( #5877, #20250 ) ) ;
#67460 = EDGE_CURVE ( 'NONE', #80917, #25435, #45328, .T. ) ;
#67461 = CARTESIAN_POINT ( 'NONE',  ( 162.7866693523297101, -29.62846900981741527, 193.9678068554149775 ) ) ;
#67462 = DIRECTION ( 'NONE',  ( 0.000000000000000000, 0.000000000000000000, 1.000000000000000000 ) ) ;
#67463 = EDGE_CURVE ( 'NONE', #7253, #51570, #33028, .T. ) ;
#67464 = DIRECTION ( 'NONE',  ( -0.7071067811607679721, 0.7071067812123270624, 0.000000000000000000 ) ) ;
#67466 = CARTESIAN_POINT ( 'NONE',  ( 108.2592170473780300, -44.83253820548913637, 140.5109475124479559 ) ) ;
#67465 = VECTOR ( 'NONE', #61954, 999.9999999999998863 ) ;
#67467 = CIRCLE ( 'NONE', #79101, 2.517500000000005844 ) ;
#67468 = DIRECTION ( 'NONE',  ( 0.000000000000000000, 0.000000000000000000, 1.000000000000000000 ) ) ;
#67469 = ORIENTED_EDGE ( 'NONE', *, *, #7188, .F. ) ;
#67470 = ORIENTED_EDGE ( 'NONE', *, *, #43553, .T. ) ;
#67471 = DIRECTION ( 'NONE',  ( 1.000000000000000078E-15, -1.000000000000000083E-30, -1.000000000000000000 ) ) ;
#67472 = ORIENTED_EDGE ( 'NONE', *, *, #72717, .T. ) ;
#67473 = ORIENTED_EDGE ( 'NONE', *, *, #56043, .F. ) ;
#67474 = DIRECTION ( 'NONE',  ( 1.000000000000000000, 0.000000000000000000, 0.000000000000000000 ) ) ;
#67475 = CARTESIAN_POINT ( 'NONE',  ( 114.1399574501865999, -31.39144735336052605, 215.7730118773249899 ) ) ;
#67476 = DIRECTION ( 'NONE',  ( 0.000000000000000000, 0.000000000000000000, -1.000000000000000000 ) ) ;
#67477 = DIRECTION ( 'NONE',  ( 0.7071067811571405404, 0.7071067812159546051, 0.000000000000000000 ) ) ;
#67478 = MECHANICAL_DESIGN_GEOMETRIC_PRESENTATION_REPRESENTATION (  '', ( #60199 ), #18146 ) ;
#67479 = CARTESIAN_POINT ( 'NONE',  ( 62.03715912545833078, -47.82818131006032303, 313.9678068554150059 ) ) ;
#67480 = VERTEX_POINT ( 'NONE', #74820 ) ;
#67481 = ORIENTED_EDGE ( 'NONE', *, *, #11813, .F. ) ;
#67482 = VECTOR ( 'NONE', #88328, 1000.000000000000000 ) ;
#67483 = ORIENTED_EDGE ( 'NONE', *, *, #54256, .T. ) ;
#67484 = ORIENTED_EDGE ( 'NONE', *, *, #8787, .F. ) ;
#67485 = CARTESIAN_POINT ( 'NONE',  ( 98.61142602524013512, -34.88203500400037882, 253.9614237029248613 ) ) ;
#67486 = CARTESIAN_POINT ( 'NONE',  ( 117.8794170024721240, -39.13275856168890243, 103.6403871806729455 ) ) ;
#67487 = CARTESIAN_POINT ( 'NONE',  ( 98.32466564902610173, -28.76522518762216052, 80.73848241876795839 ) ) ;
#67488 = CARTESIAN_POINT ( 'NONE',  ( 110.7648612237299801, -44.41958673050639561, 249.5838068554167535 ) ) ;
#67489 = CARTESIAN_POINT ( 'NONE',  ( 131.3164832912739826, -18.72944715994100662, 6.749768910606465333 ) ) ;
#67490 = DIRECTION ( 'NONE',  ( -0.7071067811865789920, 0.7071067811865159314, 0.000000000000000000 ) ) ;
#67491 = CARTESIAN_POINT ( 'NONE',  ( 114.1247157756359769, -29.05716968555177004, 195.4841967044819739 ) ) ;
#67492 = CARTESIAN_POINT ( 'NONE',  ( 100.1135588076987943, -43.99268716865574902, 276.9687004125333942 ) ) ;
#67493 = EDGE_LOOP ( 'NONE', ( #43182, #52553 ) ) ;
#67494 = CARTESIAN_POINT ( 'NONE',  ( 177.8371591254545478, -47.82818131005478079, 117.4678068554150485 ) ) ;
#67495 = ORIENTED_EDGE ( 'NONE', *, *, #30932, .F. ) ;
#67496 = ORIENTED_EDGE ( 'NONE', *, *, #65694, .F. ) ;
#67497 = LINE ( 'NONE', #61136, #18380 ) ;
#67498 = ORIENTED_EDGE ( 'NONE', *, *, #51168, .T. ) ;
#67499 = AXIS2_PLACEMENT_3D ( 'NONE', #51787, #32703, #39962 ) ;
#67500 = CYLINDRICAL_SURFACE ( 'NONE', #35950, 16.09746158385918946 ) ;
#67501 = VECTOR ( 'NONE', #41517, 1000.000000000000000 ) ;
#67502 = CARTESIAN_POINT ( 'NONE',  ( 97.33761227910700597, -34.07199620930350648, 92.11486736599003677 ) ) ;
#67503 = CARTESIAN_POINT ( 'NONE',  ( 96.63902489370863691, -37.56252461247890295, 101.3899109901969524 ) ) ;
#67504 = CARTESIAN_POINT ( 'NONE',  ( -7.017469736778876310, 71.96484654754983978, 130.3672675077506256 ) ) ;
#67505 = CIRCLE ( 'NONE', #76202, 7.937500000000000000 ) ;
#67506 = ADVANCED_FACE ( 'NONE', ( #54339 ), #18501, .F. ) ;
#67507 = CARTESIAN_POINT ( 'NONE',  ( 57.56670390244804736, -42.82844715994040286, 290.7178068554150627 ) ) ;
#67508 = CARTESIAN_POINT ( 'NONE',  ( 124.0667039024470313, -101.5893827172045860, -9.937637710810113489 ) ) ;
#67509 = EDGE_CURVE ( 'NONE', #38678, #89615, #38897, .T. ) ;
#67512 = CARTESIAN_POINT ( 'NONE',  ( 96.70388795518327640, -35.81005419191409089, 227.2556252759109725 ) ) ;
#67511 = CARTESIAN_POINT ( 'NONE',  ( 97.82866780357528569, -40.55868606849465152, 56.63876441442555887 ) ) ;
#67510 = CARTESIAN_POINT ( 'NONE',  ( 107.0667039024470313, -104.2784471599409528, 23.21780685541800082 ) ) ;
#67513 = DIRECTION ( 'NONE',  ( 1.000000000000000000, -1.000000000000000078E-15, 0.000000000000000000 ) ) ;
#67514 = LINE ( 'NONE', #40253, #65625 ) ;
#67515 = VERTEX_POINT ( 'NONE', #39833 ) ;
#67516 = DIRECTION ( 'NONE',  ( 1.000000000000000000, -1.000000000000000078E-15, 0.000000000000000000 ) ) ;
#67517 = VECTOR ( 'NONE', #43739, 1000.000000000000000 ) ;
#67518 = EDGE_CURVE ( 'NONE', #3872, #60536, #32126, .T. ) ;
#67519 = DIRECTION ( 'NONE',  ( 0.8571673007021118895, 0.000000000000000000, 0.5150380749100549327 ) ) ;
#67520 = CARTESIAN_POINT ( 'NONE',  ( 104.4911451993404370, -26.97846757028417031, 135.2813199360520287 ) ) ;
#67521 = AXIS2_PLACEMENT_3D ( 'NONE', #62474, #63376, #34771 ) ;
#67522 = EDGE_CURVE ( 'NONE', #4391, #13427, #40937, .T. ) ;
#67523 = CYLINDRICAL_SURFACE ( 'NONE', #21647, 5.000000000000004441 ) ;
#67525 = VERTEX_POINT ( 'NONE', #82105 ) ;
#67524 = CARTESIAN_POINT ( 'NONE',  ( 116.0932472193867966, -42.03267250216092776, 238.4041967044829562 ) ) ;
#67526 = EDGE_CURVE ( 'NONE', #17905, #72562, #1797, .T. ) ;
#67527 = DIRECTION ( 'NONE',  ( 0.000000000000000000, 1.000000000000000000, 0.000000000000000000 ) ) ;
#67528 = CARTESIAN_POINT ( 'NONE',  ( 99.31704471179752147, -28.81544643672065220, 266.7051490854347549 ) ) ;
#67529 = CARTESIAN_POINT ( 'NONE',  ( 116.8361817273313790, -32.96833395228159702, 135.1184824187679396 ) ) ;
#67530 = CARTESIAN_POINT ( 'NONE',  ( 68.86456684384336313, 93.07500000000001705, 56.22171674193015889 ) ) ;
#67531 = CARTESIAN_POINT ( 'NONE',  ( 12.05184652617604613, 86.64091671906268743, -129.9989399000961612 ) ) ;
#67532 = CIRCLE ( 'NONE', #35630, 2.750000000000002665 ) ;
#67534 = LINE ( 'NONE', #5321, #37061 ) ;
#67533 = DIRECTION ( 'NONE',  ( 0.000000000000000000, 0.000000000000000000, -1.000000000000000000 ) ) ;
#67535 = DIRECTION ( 'NONE',  ( -2.900000000000000265E-14, 2.000000000000000155E-15, -1.000000000000000000 ) ) ;
#67536 = CARTESIAN_POINT ( 'NONE',  ( 73.10937651008747196, -8.833000550534334749, 14.92562527591099375 ) ) ;
#67537 = ORIENTED_EDGE ( 'NONE', *, *, #85470, .F. ) ;
#67538 = EDGE_CURVE ( 'NONE', #37523, #8565, #10536, .T. ) ;
#67539 = CIRCLE ( 'NONE', #2326, 3.250000000000002665 ) ;
#67540 = ADVANCED_FACE ( 'NONE', ( #87112 ), #81654, .F. ) ;
#67541 = VERTEX_POINT ( 'NONE', #60274 ) ;
#67542 = ORIENTED_EDGE ( 'NONE', *, *, #65095, .T. ) ;
#67543 = EDGE_LOOP ( 'NONE', ( #59960, #74420, #59986, #28376, #78660 ) ) ;
#67544 = DIRECTION ( 'NONE',  ( 0.000000000000000000, 0.000000000000000000, -1.000000000000000000 ) ) ;
#67545 = CARTESIAN_POINT ( 'NONE',  ( 109.6066175024219831, -25.17973177368044801, 25.90419670448196143 ) ) ;
#67546 = LINE ( 'NONE', #41500, #48999 ) ;
#67547 = CARTESIAN_POINT ( 'NONE',  ( 134.0664832912740110, -33.97944715994100306, 1.625625275910997480 ) ) ;
#67548 = CIRCLE ( 'NONE', #9528, 13.16666666666670160 ) ;
#67549 = EDGE_CURVE ( 'NONE', #41311, #59373, #24998, .T. ) ;
#67550 = DIRECTION ( 'NONE',  ( 1.000000000000000000, 4.163336342344333240E-14, 0.000000000000000000 ) ) ;
#67552 = CARTESIAN_POINT ( 'NONE',  ( 34.96670390244699433, -26.71338133339301635, -5.074374724088000832 ) ) ;
#67551 = DIRECTION ( 'NONE',  ( -1.175184669632759901E-16, 1.000000000000000000, 2.000000000000003705E-15 ) ) ;
#67553 = CARTESIAN_POINT ( 'NONE',  ( 115.4795240695424923, -35.25402295475319647, 243.3867055423619661 ) ) ;
#67554 = ORIENTED_EDGE ( 'NONE', *, *, #35935, .T. ) ;
#67555 = EDGE_CURVE ( 'NONE', #36722, #12182, #26216, .T. ) ;
#67556 = ORIENTED_EDGE ( 'NONE', *, *, #88887, .F. ) ;
#67557 = VECTOR ( 'NONE', #60797, 1000.000000000000000 ) ;
#67558 = ORIENTED_EDGE ( 'NONE', *, *, #51810, .F. ) ;
#67559 = CARTESIAN_POINT ( 'NONE',  ( 75.31670390244798341, -50.82844715994100682, 37.63480685541480852 ) ) ;
#67560 = AXIS2_PLACEMENT_3D ( 'NONE', #52040, #17555, #85722 ) ;
#67561 = CARTESIAN_POINT ( 'NONE',  ( 116.9160198271895723, -38.71580271627102832, 183.6683563841668843 ) ) ;
#67562 = CARTESIAN_POINT ( 'NONE',  ( -69.72411017812909506, 120.6499999999999915, -69.72411017813089984 ) ) ;
#67563 = DIRECTION ( 'NONE',  ( -3.201858731750027727E-15, 1.000000000000000000, -3.201858731750027724E-30 ) ) ;
#67564 = CARTESIAN_POINT ( 'NONE',  ( 114.1881255536272022, -42.05338753103387717, 24.74729759161198217 ) ) ;
#67565 = CARTESIAN_POINT ( 'NONE',  ( 223.2659999999999911, 36.86249999999999716, -2.032000000000000028 ) ) ;
#67566 = DIRECTION ( 'NONE',  ( 1.000000000000000000, 0.000000000000000000, 0.000000000000000000 ) ) ;
#67567 = CARTESIAN_POINT ( 'NONE',  ( 117.4251315444616353, -36.24242395571270237, 268.8518157521021408 ) ) ;
#67568 = DIRECTION ( 'NONE',  ( -1.000000000000000000, 0.000000000000000000, -0.000000000000000000 ) ) ;
#67569 = ORIENTED_EDGE ( 'NONE', *, *, #47538, .F. ) ;
#67570 = EDGE_CURVE ( 'NONE', #11954, #67267, #41176, .T. ) ;
#67571 = CARTESIAN_POINT ( 'NONE',  ( 131.0667039024480118, -61.87844715994100397, 201.9838068554149970 ) ) ;
#67572 = EDGE_CURVE ( 'NONE', #14773, #37741, #49689, .T. ) ;
#67573 = FACE_OUTER_BOUND ( 'NONE', #46575, .T. ) ;
#67574 = CARTESIAN_POINT ( 'NONE',  ( 104.6321197217979488, -45.03455396584281800, 60.15570941721099274 ) ) ;
#67575 = VECTOR ( 'NONE', #77190, 999.9999999999998863 ) ;
#67576 = AXIS2_PLACEMENT_3D ( 'NONE', #33599, #60394, #61294 ) ;
#67577 = VECTOR ( 'NONE', #72719, 1000.000000000000000 ) ;
#67578 = CARTESIAN_POINT ( 'NONE',  ( 136.6005499775785665, -17.66120003907372649, 7.039521718172665921 ) ) ;
#67579 = AXIS2_PLACEMENT_3D ( 'NONE', #21902, #42753, #41415 ) ;
#67580 = DIRECTION ( 'NONE',  ( 0.000000000000000000, 1.000000000000000000, 0.000000000000000000 ) ) ;
#67581 = CARTESIAN_POINT ( 'NONE',  ( 105.7154054197770137, -46.72384757748508122, 193.4688856702615851 ) ) ;
#67582 = ORIENTED_EDGE ( 'NONE', *, *, #46067, .F. ) ;
#67583 = CARTESIAN_POINT ( 'NONE',  ( 172.5664832912729878, -27.57844715994070484, 15.92562527591200094 ) ) ;
#67584 = CARTESIAN_POINT ( 'NONE',  ( 124.0808947512391711, 59.70268277206753282, -40.60803669063014354 ) ) ;
#67585 = ORIENTED_EDGE ( 'NONE', *, *, #70927, .F. ) ;
#67586 = CARTESIAN_POINT ( 'NONE',  ( 108.2767148518004490, -26.33900702273897565, 129.9841967044819739 ) ) ;
#67587 = ORIENTED_EDGE ( 'NONE', *, *, #55807, .F. ) ;
#67588 = CARTESIAN_POINT ( 'NONE',  ( 98.58519923211989067, -37.96229866499883343, 65.86384839950598291 ) ) ;
#67589 = CARTESIAN_POINT ( 'NONE',  ( 90.44969454456416713, -55.86395651782489580, 219.5838068554169809 ) ) ;
#67590 = CARTESIAN_POINT ( 'NONE',  ( 98.70151408295986073, -32.45115127476004346, 92.39396425827794701 ) ) ;
#67591 = DIRECTION ( 'NONE',  ( 0.000000000000000000, 0.000000000000000000, -1.000000000000000000 ) ) ;
#67592 = CARTESIAN_POINT ( 'NONE',  ( -24.20305689751608824, 54.97499999999995879, 58.62596543806478877 ) ) ;
#67593 = AXIS2_PLACEMENT_3D ( 'NONE', #54350, #27576, #89366 ) ;
#67594 = CARTESIAN_POINT ( 'NONE',  ( 98.62975546523678361, -43.90627301359564427, 72.89943479972099283 ) ) ;
#67595 = CARTESIAN_POINT ( 'NONE',  ( 97.31583286222694085, -39.30594983826361499, 182.5319644226825062 ) ) ;
#67596 = EDGE_CURVE ( 'NONE', #56630, #30852, #68905, .T. ) ;
#67597 = CARTESIAN_POINT ( 'NONE',  ( 163.0664832912739826, -0.2185775633789972805, 335.9181252759120184 ) ) ;
#67598 = VERTEX_POINT ( 'NONE', #75718 ) ;
#67599 = DIRECTION ( 'NONE',  ( 6.524622321627019585E-16, 3.741823817616790462E-31, 1.000000000000000000 ) ) ;
#67600 = ORIENTED_EDGE ( 'NONE', *, *, #33494, .F. ) ;
#67601 = TOROIDAL_SURFACE ( 'NONE', #15361, 15.69999999999999929, 0.2999999999999999889 ) ;
#67602 = ORIENTED_EDGE ( 'NONE', *, *, #82969, .F. ) ;
#67603 = FACE_OUTER_BOUND ( 'NONE', #80798, .T. ) ;
#67604 = EDGE_LOOP ( 'NONE', ( #15340, #50026, #5778, #15699 ) ) ;
#67605 = CARTESIAN_POINT ( 'NONE',  ( 97.78144721833423603, -39.80378292816726571, 241.5813395616259811 ) ) ;
#67606 = CARTESIAN_POINT ( 'NONE',  ( 108.7467188015556729, -25.78131109771034701, 140.9432443235299672 ) ) ;
#67607 = CYLINDRICAL_SURFACE ( 'NONE', #85794, 11.57110091390439699 ) ;
#67608 = CARTESIAN_POINT ( 'NONE',  ( 115.7815011880635723, -41.80502153836215484, 129.4062101450579689 ) ) ;
#67609 = CARTESIAN_POINT ( 'NONE',  ( 103.2788791697577295, -47.11347506355160419, 93.28610146638693834 ) ) ;
#67610 = DIRECTION ( 'NONE',  ( 0.7071067811865171526, 0.7071067811865779928, 7.071067811865164719E-16 ) ) ;
#67611 = ORIENTED_EDGE ( 'NONE', *, *, #13689, .T. ) ;
#67612 = PLANE ( 'NONE',  #36590 ) ;
#67613 = DIRECTION ( 'NONE',  ( 0.000000000000000000, 0.000000000000000000, 1.000000000000000000 ) ) ;
#67615 = VERTEX_POINT ( 'NONE', #62077 ) ;
#67614 = EDGE_CURVE ( 'NONE', #82741, #57074, #13490, .T. ) ;
#67616 = LINE ( 'NONE', #26718, #38791 ) ;
#67617 = FACE_OUTER_BOUND ( 'NONE', #53242, .T. ) ;
#67618 = CARTESIAN_POINT ( 'NONE',  ( 110.2841844748215578, -46.64581212076017636, 12.82705384733995402 ) ) ;
#67619 = DIRECTION ( 'NONE',  ( 0.7071067811865503483, -0.7071067811865445751, 7.071067811865509846E-16 ) ) ;
#67620 = EDGE_CURVE ( 'NONE', #6826, #82100, #57729, .T. ) ;
#67621 = LINE ( 'NONE', #45369, #63715 ) ;
#67622 = LINE ( 'NONE', #11770, #25810 ) ;
#67623 = EDGE_CURVE ( 'NONE', #37178, #19677, #47539, .T. ) ;
#67624 = CARTESIAN_POINT ( 'NONE',  ( 101.9719466847405158, -43.62131184885326007, 256.4924198280769474 ) ) ;
#67626 = CARTESIAN_POINT ( 'NONE',  ( 97.64212626138838402, -32.24102647341089778, 71.97276813305397525 ) ) ;
#67625 = CARTESIAN_POINT ( 'NONE',  ( 97.37543214736597008, -39.21170434501622992, 101.5265497855716035 ) ) ;
#67627 = LINE ( 'NONE', #27634, #81420 ) ;
#67628 = CARTESIAN_POINT ( 'NONE',  ( 112.8043457091679471, -45.48636447812791062, 178.0384824187679556 ) ) ;
#67629 = VERTEX_POINT ( 'NONE', #69355 ) ;
#67630 = DIRECTION ( 'NONE',  ( 0.000000000000000000, 0.000000000000000000, -1.000000000000000000 ) ) ;
#67631 = ORIENTED_EDGE ( 'NONE', *, *, #59574, .T. ) ;
#67632 = DIRECTION ( 'NONE',  ( 1.000000000000000000, 4.237773401492740281E-14, 0.000000000000000000 ) ) ;
#67633 = EDGE_CURVE ( 'NONE', #32172, #21819, #33091, .T. ) ;
#67634 = CARTESIAN_POINT ( 'NONE',  ( 113.2454986895939726, -28.75867293777369227, 65.55229194344597943 ) ) ;
#67635 = CARTESIAN_POINT ( 'NONE',  ( 135.0807008692675311, -34.17316201338590531, 1.785258157648855093 ) ) ;
#67636 = ORIENTED_EDGE ( 'NONE', *, *, #28024, .T. ) ;
#67637 = DIRECTION ( 'NONE',  ( 0.000000000000000000, 0.000000000000000000, 1.000000000000000000 ) ) ;
#67638 = EDGE_CURVE ( 'NONE', #52633, #51180, #56217, .T. ) ;
#67640 = ORIENTED_EDGE ( 'NONE', *, *, #28772, .T. ) ;
#67639 = CARTESIAN_POINT ( 'NONE',  ( 97.53097521295029537, -31.04728477963730171, 130.9108633711489915 ) ) ;
#67641 = LINE ( 'NONE', #12235, #11741 ) ;
#67642 = VECTOR ( 'NONE', #69953, 1000.000000000000000 ) ;
#67643 = CARTESIAN_POINT ( 'NONE',  ( -130.5169520046879086, 94.84315624882769669, -3.295103719954349142 ) ) ;
#67644 = CARTESIAN_POINT ( 'NONE',  ( 107.0667039024470313, -104.2784471599413934, 2.217806855418003043 ) ) ;
#67646 = VECTOR ( 'NONE', #49573, 1000.000000000000000 ) ;
#67645 = CARTESIAN_POINT ( 'NONE',  ( 98.30753419779586011, -41.72887550351619979, 76.73979194370691914 ) ) ;
#67647 = ORIENTED_EDGE ( 'NONE', *, *, #1493, .T. ) ;
#67648 = EDGE_CURVE ( 'NONE', #9719, #5415, #13938, .T. ) ;
#67649 = AXIS2_PLACEMENT_3D ( 'NONE', #59798, #59359, #4416 ) ;
#67650 = AXIS2_PLACEMENT_3D ( 'NONE', #77639, #52022, #37972 ) ;
#67651 = SHAPE_DEFINITION_REPRESENTATION ( #11803, #82876 ) ;
#67652 = VECTOR ( 'NONE', #35844, 1000.000000000000114 ) ;
#67653 = LINE ( 'NONE', #4535, #16738 ) ;
#67654 = FACE_OUTER_BOUND ( 'NONE', #9183, .T. ) ;
#67655 = ORIENTED_EDGE ( 'NONE', *, *, #43727, .F. ) ;
#67656 = EDGE_CURVE ( 'NONE', #19003, #12758, #89355, .T. ) ;
#67657 = ORIENTED_EDGE ( 'NONE', *, *, #46799, .F. ) ;
#67658 = CARTESIAN_POINT ( 'NONE',  ( -24.79284581386642827, 184.0000000000000000, 90.32146847885337593 ) ) ;
#67659 = B_SPLINE_SURFACE_WITH_KNOTS ( 'NONE', 1, 1, ( 
 ( #67530, #26643 ),
 ( #46624, #4863 ) ),
 .UNSPECIFIED., .F., .F., .F.,
 ( 2, 2 ),
 ( 2, 2 ),
 ( 0.000000000000000000, 1.000000000000000000 ),
 ( 0.000000000000000000, 1.000000000000000000 ),
 .UNSPECIFIED. ) ;
#67660 = CARTESIAN_POINT ( 'NONE',  ( 83.22850972642787326, 85.83513192049075258, -100.5877680347017957 ) ) ;
#67661 = CARTESIAN_POINT ( 'NONE',  ( 117.0608945212226786, -38.08045314360793299, 158.7189586074293288 ) ) ;
#67662 = CARTESIAN_POINT ( 'NONE',  ( 0.000000000000000000, 101.5999999999999943, 0.000000000000000000 ) ) ;
#67664 = CARTESIAN_POINT ( 'NONE',  ( -9.554550254943340093, 74.17292945273928240, -118.1706666865833455 ) ) ;
#67663 = CARTESIAN_POINT ( 'NONE',  ( 25.56670390244832092, -48.82844715994168183, 259.7178068554150059 ) ) ;
#67665 = CARTESIAN_POINT ( 'NONE',  ( 97.31309884004055277, -38.96072181228549880, 181.5054471926127349 ) ) ;
#67666 = VECTOR ( 'NONE', #39669, 1000.000000000000000 ) ;
#67667 = ORIENTED_EDGE ( 'NONE', *, *, #62898, .T. ) ;
#67668 = AXIS2_PLACEMENT_3D ( 'NONE', #50226, #14842, #57498 ) ;
#67669 = CARTESIAN_POINT ( 'NONE',  ( 171.4664832912730219, 12.92155284005730387, 361.9756252759109998 ) ) ;
#67670 = CARTESIAN_POINT ( 'NONE',  ( 116.1939227058877719, -40.33550099034467706, 189.5270538473389479 ) ) ;
#67672 = VERTEX_POINT ( 'NONE', #61459 ) ;
#67671 = CARTESIAN_POINT ( 'NONE',  ( 106.3178592879830973, -25.29212102876796919, 321.3196247216901043 ) ) ;
#67673 = CARTESIAN_POINT ( 'NONE',  ( 97.35451824726690973, -37.88753622196094284, 37.42133956162496844 ) ) ;
#67674 = CARTESIAN_POINT ( 'NONE',  ( 97.81168895331838087, -40.51742574516882200, 287.6356252759109680 ) ) ;
#67675 = CARTESIAN_POINT ( 'NONE',  ( 82.89895571708156297, 82.54999999999999716, 100.8594679592221155 ) ) ;
#67676 = CARTESIAN_POINT ( 'NONE',  ( 97.81058606723590287, -40.51473118396398831, 22.63539394696516638 ) ) ;
#67677 = EDGE_LOOP ( 'NONE', ( #23925, #53555 ) ) ;
#67678 = FACE_OUTER_BOUND ( 'NONE', #20889, .T. ) ;
#67679 = ORIENTED_EDGE ( 'NONE', *, *, #66155, .T. ) ;
#67680 = VERTEX_POINT ( 'NONE', #66944 ) ;
#67681 = EDGE_CURVE ( 'NONE', #47987, #38464, #54624, .T. ) ;
#67682 = AXIS2_PLACEMENT_3D ( 'NONE', #33066, #54374, #32610 ) ;
#67683 = CARTESIAN_POINT ( 'NONE',  ( 98.59150690531237160, -40.78546747480537249, 213.1253928297069535 ) ) ;
#67684 = CARTESIAN_POINT ( 'NONE',  ( 173.9900000000000091, 52.73749999999999716, -26.11912895322935313 ) ) ;
#67685 = CARTESIAN_POINT ( 'NONE',  ( -118.3048154812336321, 92.64969027323465411, -7.744053933098289377 ) ) ;
#67686 = B_SPLINE_CURVE_WITH_KNOTS ( 'NONE', 3,
 ( #59331, #80254, #23943, #51620, #73413, #37570, #86614, #17999, #12998, #67947, #70534, #40229, #6183, #5278, #33871, #63262, #49614, #36001, #82050, #42346, #32973, #33426, #54286, #577, #42792, #28277 ),
 .UNSPECIFIED., .F., .F.,
 ( 4, 2, 2, 2, 2, 2, 2, 2, 2, 2, 2, 2, 4 ),
 ( 0.004694703549784783395, 0.005281399525416200988, 0.005868095501047617714, 0.006161443488863340388, 0.006454791476679063063, 0.006748139464494785737, 0.007041487452310508412, 0.007334835440126231086, 0.007628183427941953761, 0.007921531415757677302, 0.008214879403573398242, 0.008801575379204814101, 0.009388271354836229959 ),
 .UNSPECIFIED. ) ;
#67687 = LINE ( 'NONE', #88148, #38790 ) ;
#67688 = DIRECTION ( 'NONE',  ( -0.1858654557293118459, 0.9825752044329915114, 0.000000000000000000 ) ) ;
#67689 = ORIENTED_EDGE ( 'NONE', *, *, #49774, .F. ) ;
#67690 = FACE_OUTER_BOUND ( 'NONE', #27436, .T. ) ;
#67691 = CARTESIAN_POINT ( 'NONE',  ( 97.07185578696417849, -35.38051917764914123, 37.21882853886443598 ) ) ;
#67692 = ORIENTED_EDGE ( 'NONE', *, *, #46250, .F. ) ;
#67693 = CARTESIAN_POINT ( 'NONE',  ( 117.4970320020027259, -36.54623693216564106, 288.8413395616252615 ) ) ;
#67694 = ORIENTED_EDGE ( 'NONE', *, *, #79312, .F. ) ;
#67695 = EDGE_LOOP ( 'NONE', ( #37704, #65755, #14403, #47665 ) ) ;
#67696 = CARTESIAN_POINT ( 'NONE',  ( 113.8227294809096435, -41.31015272151215356, 271.1709475124484925 ) ) ;
#67697 = PLANE ( 'NONE',  #994 ) ;
#67698 = CARTESIAN_POINT ( 'NONE',  ( 98.56701561008806323, -30.78824967682747271, 160.8289586092449497 ) ) ;
#67699 = DIRECTION ( 'NONE',  ( 0.000000000000000000, 0.000000000000000000, 1.000000000000000000 ) ) ;
#67700 = PLANE ( 'NONE',  #9921 ) ;
#67701 = FACE_OUTER_BOUND ( 'NONE', #27233, .T. ) ;
#67702 = VECTOR ( 'NONE', #24926, 1000.000000000000000 ) ;
#67703 = CARTESIAN_POINT ( 'NONE',  ( 118.1276453766531915, -32.34061975111649190, 245.1270538473389706 ) ) ;
#67704 = DIRECTION ( 'NONE',  ( 1.000000000000000000, 0.000000000000000000, 0.000000000000000000 ) ) ;
#67705 = ORIENTED_EDGE ( 'NONE', *, *, #32887, .T. ) ;
#67706 = EDGE_CURVE ( 'NONE', #4391, #89126, #31970, .T. ) ;
#67707 = AXIS2_PLACEMENT_3D ( 'NONE', #73784, #66968, #53307 ) ;
#67708 = CARTESIAN_POINT ( 'NONE',  ( 117.4143231396408851, -32.71451144048268844, 90.10895860924395606 ) ) ;
#67709 = AXIS2_PLACEMENT_3D ( 'NONE', #46333, #61317, #68150 ) ;
#67710 = CARTESIAN_POINT ( 'NONE',  ( 87.06648329127423835, -46.72944715994107412, 14.82207188531761055 ) ) ;
#67711 = ORIENTED_EDGE ( 'NONE', *, *, #36164, .F. ) ;
#67712 = EDGE_LOOP ( 'NONE', ( #72597, #52312 ) ) ;
#67713 = ORIENTED_EDGE ( 'NONE', *, *, #78062, .F. ) ;
#67714 = DIRECTION ( 'NONE',  ( 1.000000000000000000, 0.000000000000000000, 0.000000000000000000 ) ) ;
#67715 = FACE_OUTER_BOUND ( 'NONE', #21030, .T. ) ;
#67716 = DIRECTION ( 'NONE',  ( 0.000000000000000000, 0.000000000000000000, -1.000000000000000000 ) ) ;
#67717 = CARTESIAN_POINT ( 'NONE',  ( 98.92690986002996567, -36.11615286530263091, 144.0852332267349709 ) ) ;
#67718 = CARTESIAN_POINT ( 'NONE',  ( 106.9401787849546537, -47.80506239865356122, 228.5794347997199907 ) ) ;
#67719 = CARTESIAN_POINT ( 'NONE',  ( 97.83891474888318385, -40.58336863229884273, 57.64130287487746074 ) ) ;
#67720 = ORIENTED_EDGE ( 'NONE', *, *, #69947, .F. ) ;
#67721 = CARTESIAN_POINT ( 'NONE',  ( 130.4942851453020012, 94.60320878023495084, 4.086962795942436166 ) ) ;
#67722 = VECTOR ( 'NONE', #68184, 999.9999999999998863 ) ;
#67723 = CARTESIAN_POINT ( 'NONE',  ( 136.7280559526967636, -37.42731094490868315, 2.974216770160591494 ) ) ;
#67724 = ORIENTED_EDGE ( 'NONE', *, *, #22923, .F. ) ;
#67725 = EDGE_LOOP ( 'NONE', ( #11968, #83641 ) ) ;
#67726 = CIRCLE ( 'NONE', #28560, 4.500000000000003553 ) ;
#67727 = CARTESIAN_POINT ( 'NONE',  ( 107.9747653995834327, -87.30271670975442078, -11.78219314458253741 ) ) ;
#67728 = ORIENTED_EDGE ( 'NONE', *, *, #50234, .F. ) ;
#67729 = ORIENTED_EDGE ( 'NONE', *, *, #66907, .T. ) ;
#67730 = CARTESIAN_POINT ( 'NONE',  ( 107.5667039024470171, -94.77844715994206126, -19.78219314458232247 ) ) ;
#67731 = CARTESIAN_POINT ( 'NONE',  ( -12.69999999999999929, 81.71142461540233626, -129.9368274816650626 ) ) ;
#67732 = CARTESIAN_POINT ( 'NONE',  ( 263.3306968374159851, 52.73749999999999716, -2.032000000000000028 ) ) ;
#67733 = CYLINDRICAL_SURFACE ( 'NONE', #30097, 7.873999999999991672 ) ;
#67734 = ADVANCED_FACE ( 'NONE', ( #11991 ), #75562, .F. ) ;
#67735 = CARTESIAN_POINT ( 'NONE',  ( 115.5545030166667146, -32.01519760825960503, 178.6524198280769724 ) ) ;
#67736 = CARTESIAN_POINT ( 'NONE',  ( 111.9494872540039694, -27.46861899264377982, 59.68991099019693536 ) ) ;
#67737 = ORIENTED_EDGE ( 'NONE', *, *, #16583, .T. ) ;
#67738 = CARTESIAN_POINT ( 'NONE',  ( 86.74776500631861609, -85.76461670310806085, 250.2190963482990185 ) ) ;
#67739 = EDGE_LOOP ( 'NONE', ( #72876, #14774, #61373, #72230 ) ) ;
#67740 = EDGE_CURVE ( 'NONE', #56065, #59400, #20149, .T. ) ;
#67741 = DIRECTION ( 'NONE',  ( -1.000000000000000000, 0.000000000000000000, 0.000000000000000000 ) ) ;
#67742 = EDGE_CURVE ( 'NONE', #8195, #86716, #6077, .T. ) ;
#67743 = ORIENTED_EDGE ( 'NONE', *, *, #10669, .T. ) ;
#67744 = DIRECTION ( 'NONE',  ( -0.9254794337955620787, -0.3787978585227822492, 0.000000000000000000 ) ) ;
#67745 = EDGE_CURVE ( 'NONE', #54700, #75621, #53281, .T. ) ;
#67746 = ORIENTED_EDGE ( 'NONE', *, *, #42492, .T. ) ;
#67747 = CARTESIAN_POINT ( 'NONE',  ( 110.6340492874757473, -27.31029447320501191, 165.7874528756242682 ) ) ;
#67748 = FACE_BOUND ( 'NONE', #4072, .T. ) ;
#67749 = CARTESIAN_POINT ( 'NONE',  ( 110.8556210833095435, -45.98376701427152113, 132.8857240236057748 ) ) ;
#67750 = FACE_OUTER_BOUND ( 'NONE', #46952, .T. ) ;
#67751 = ORIENTED_EDGE ( 'NONE', *, *, #19256, .T. ) ;
#67752 = CARTESIAN_POINT ( 'NONE',  ( 112.1280348295452001, -26.87672238358117127, 19.71086337114896736 ) ) ;
#67753 = CARTESIAN_POINT ( 'NONE',  ( 95.30017103329034001, -34.95040006919153086, 67.20705384733894050 ) ) ;
#67755 = FACE_OUTER_BOUND ( 'NONE', #85022, .T. ) ;
#67754 = CARTESIAN_POINT ( 'NONE',  ( 90.44969454456439450, -16.81243780205712568, 249.5838068554174924 ) ) ;
#67756 = DIRECTION ( 'NONE',  ( -3.100000000000000258E-29, 3.100000000000000044E-14, 1.000000000000000000 ) ) ;
#67757 = CARTESIAN_POINT ( 'NONE',  ( -544.5124999999999318, 53.97500000000000142, 12.69999999999999929 ) ) ;
#67758 = EDGE_CURVE ( 'NONE', #52712, #77239, #61020, .T. ) ;
#67759 = LINE ( 'NONE', #74570, #14085 ) ;
#67760 = LINE ( 'NONE', #80507, #37139 ) ;
#67761 = ORIENTED_EDGE ( 'NONE', *, *, #76718, .T. ) ;
#67762 = CARTESIAN_POINT ( 'NONE',  ( 117.5318583147471401, -37.01683481156648980, 43.80419670448293346 ) ) ;
#67763 = CARTESIAN_POINT ( 'NONE',  ( 117.3749687695755171, -38.63058443890392368, 84.68133956162593279 ) ) ;
#67764 = AXIS2_PLACEMENT_3D ( 'NONE', #55660, #34348, #82981 ) ;
#67765 = AXIS2_PLACEMENT_3D ( 'NONE', #39518, #25441, #53108 ) ;
#67767 = CARTESIAN_POINT ( 'NONE',  ( 31.71315051185499811, -33.70561438052090608, 313.9678068554150059 ) ) ;
#67766 = DIRECTION ( 'NONE',  ( 0.7071067811578790607, 0.7071067812152160847, 0.000000000000000000 ) ) ;
#67768 = CARTESIAN_POINT ( 'NONE',  ( 121.5762960060074960, -43.47224590996763993, 9.125625275910984158 ) ) ;
#67769 = CONICAL_SURFACE ( 'NONE', #80885, 39.10000000000005116, 0.7853981633974587151 ) ;
#67770 = AXIS2_PLACEMENT_3D ( 'NONE', #77883, #2026, #15658 ) ;
#67771 = DIRECTION ( 'NONE',  ( 0.000000000000000000, 0.000000000000000000, -1.000000000000000000 ) ) ;
#67772 = ORIENTED_EDGE ( 'NONE', *, *, #38639, .F. ) ;
#67773 = CARTESIAN_POINT ( 'NONE',  ( 96.71749658230667990, -40.79275330125899046, 92.62419670448196030 ) ) ;
#67775 = ORIENTED_EDGE ( 'NONE', *, *, #80565, .F. ) ;
#67774 = CARTESIAN_POINT ( 'NONE',  ( -21.42842094847161860, 65.59999999999998010, 41.97446389704171565 ) ) ;
#67776 = CARTESIAN_POINT ( 'NONE',  ( 104.3301552612371523, -26.04411461992211230, 241.2880062282919482 ) ) ;
#67777 = CARTESIAN_POINT ( 'NONE',  ( 109.6421070598780290, -46.48033137427756856, 253.7835689616865125 ) ) ;
#67778 = CARTESIAN_POINT ( 'NONE',  ( 107.0664832912739968, -18.82844715994099971, 168.9256252759119832 ) ) ;
#67779 = DIRECTION ( 'NONE',  ( 0.000000000000000000, 0.000000000000000000, 1.000000000000000000 ) ) ;
#67780 = CARTESIAN_POINT ( 'NONE',  ( 179.1667039024460166, -28.27351298637280408, 193.9678068554150059 ) ) ;
#67781 = CARTESIAN_POINT ( 'NONE',  ( 91.06648329127500574, -36.72944715993925513, 9.125625275910953960 ) ) ;
#67782 = LINE ( 'NONE', #4667, #58741 ) ;
#67783 = AXIS2_PLACEMENT_3D ( 'NONE', #22454, #649, #49233 ) ;
#67785 = CARTESIAN_POINT ( 'NONE',  ( 116.0678243078411498, -40.55558035091543445, 168.5070538473399608 ) ) ;
#67784 = CIRCLE ( 'NONE', #41708, 6.857999999999975671 ) ;
#67786 = EDGE_LOOP ( 'NONE', ( #22821, #60643, #73871, #38588 ) ) ;
#67787 = ORIENTED_EDGE ( 'NONE', *, *, #779, .T. ) ;
#67788 = EDGE_CURVE ( 'NONE', #30574, #16547, #4277, .T. ) ;
#67789 = CARTESIAN_POINT ( 'NONE',  ( 100.7916921807572379, -44.60965664144636378, 118.4730118773259733 ) ) ;
#67790 = CIRCLE ( 'NONE', #8348, 2.116999999999993776 ) ;
#67791 = CARTESIAN_POINT ( 'NONE',  ( 89.06648329127401098, -18.82844715994099971, 17.92562527591199739 ) ) ;
#67793 = CARTESIAN_POINT ( 'NONE',  ( 182.4202572930400095, -33.70561438051981185, 193.9678068554150059 ) ) ;
#67792 = CARTESIAN_POINT ( 'NONE',  ( 115.9511604134431195, -42.07746527072326614, 274.3832443235294249 ) ) ;
#67794 = DIRECTION ( 'NONE',  ( -1.000000000000000078E-15, 0.000000000000000000, -1.000000000000000000 ) ) ;
#67795 = ADVANCED_FACE ( 'NONE', ( #59664, #38783 ), #5630, .F. ) ;
#67796 = DIRECTION ( 'NONE',  ( -0.9254794337955620787, -0.3787978585227822492, 0.000000000000000000 ) ) ;
#67797 = CARTESIAN_POINT ( 'NONE',  ( 177.8371591254545194, -47.82818131005477369, 180.4678068554150343 ) ) ;
#67798 = LINE ( 'NONE', #73257, #72488 ) ;
#67799 = CARTESIAN_POINT ( 'NONE',  ( 95.60734603896362671, -36.72944715994100306, 293.2242906452868851 ) ) ;
#67800 = CARTESIAN_POINT ( 'NONE',  ( 116.7748712849171966, -40.56502120445013304, 193.5270538473389479 ) ) ;
#67801 = CARTESIAN_POINT ( 'NONE',  ( 51.06670390244772761, -33.35206098992665602, 237.4678068554150059 ) ) ;
#67802 = VERTEX_POINT ( 'NONE', #68297 ) ;
#67803 = ORIENTED_EDGE ( 'NONE', *, *, #66563, .F. ) ;
#67804 = CARTESIAN_POINT ( 'NONE',  ( 31.89136050872298966, -31.76306994223740432, 313.9678068554150059 ) ) ;
#67805 = DIRECTION ( 'NONE',  ( -0.9834602067153815907, -0.1811243269341220596, 0.000000000000000000 ) ) ;
#67806 = DIRECTION ( 'NONE',  ( 1.000000000000000000, 0.000000000000000000, -9.299908063537909262E-17 ) ) ;
#67807 = DIRECTION ( 'NONE',  ( 0.8660254037844389297, -0.4999999999999993894, 1.550000000000000968E-14 ) ) ;
#67808 = VECTOR ( 'NONE', #72467, 1000.000000000000000 ) ;
#67809 = LINE ( 'NONE', #5597, #61536 ) ;
#67810 = EDGE_LOOP ( 'NONE', ( #5745, #49326, #29101, #1570 ) ) ;
#67811 = EDGE_CURVE ( 'NONE', #2099, #13645, #52853, .T. ) ;
#67812 = DIRECTION ( 'NONE',  ( -3.491483361109380094E-15, 0.000000000000000000, -1.000000000000000000 ) ) ;
#67813 = CARTESIAN_POINT ( 'NONE',  ( 97.40186843559010299, -40.63869902605510731, 206.6327681330539860 ) ) ;
#67814 = CARTESIAN_POINT ( 'NONE',  ( 136.8164806451553659, -36.72944715939129168, 6.749772901088312516 ) ) ;
#67815 = ORIENTED_EDGE ( 'NONE', *, *, #53872, .T. ) ;
#67816 = CARTESIAN_POINT ( 'NONE',  ( -10.01454657728489472, 90.24125983913356208, 118.1331779202407262 ) ) ;
#67817 = DIRECTION ( 'NONE',  ( 0.000000000000000000, -1.000000000000000000, -2.913971193241881161E-15 ) ) ;
#67818 = CARTESIAN_POINT ( 'NONE',  ( 105.7148838627258556, -46.72376843215531750, 163.4689113525691084 ) ) ;
#67819 = CARTESIAN_POINT ( 'NONE',  ( 113.9764273654521674, -32.38405892540742315, 32.09094751244895605 ) ) ;
#67820 = CARTESIAN_POINT ( 'NONE',  ( 103.1665349694895895, -27.03781871365087142, 126.3813395616259783 ) ) ;
#67821 = ORIENTED_CLOSED_SHELL ( 'NONE', *, #83693, .F. );
#67822 = LINE ( 'NONE', #74638, #88541 ) ;
#67823 = ORIENTED_EDGE ( 'NONE', *, *, #87592, .T. ) ;
#67824 = AXIS2_PLACEMENT_3D ( 'NONE', #59998, #66375, #53169 ) ;
#67825 = CYLINDRICAL_SURFACE ( 'NONE', #72662, 7.873999999999991672 ) ;
#67826 = CARTESIAN_POINT ( 'NONE',  ( 82.41409441626767318, -17.29397280664446868, 7.245803660798958212 ) ) ;
#67827 = ORIENTED_EDGE ( 'NONE', *, *, #24979, .T. ) ;
#67828 = ORIENTED_EDGE ( 'NONE', *, *, #30435, .T. ) ;
#67829 = CIRCLE ( 'NONE', #82375, 2.124999999999994227 ) ;
#67830 = AXIS2_PLACEMENT_3D ( 'NONE', #65941, #10543, #86415 ) ;
#67831 = CARTESIAN_POINT ( 'NONE',  ( 70.63919639214310564, 100.5999999999999659, 95.21359708083839735 ) ) ;
#67832 = ORIENTED_EDGE ( 'NONE', *, *, #70408, .T. ) ;
#67833 = VERTEX_POINT ( 'NONE', #12891 ) ;
#67834 = LINE ( 'NONE', #61015, #74829 ) ;
#67835 = CARTESIAN_POINT ( 'NONE',  ( 105.1764056618614944, -45.05913732685939976, 71.82099125664798578 ) ) ;
#67836 = CARTESIAN_POINT ( 'NONE',  ( 112.4658351597014843, -45.71473303307890035, 238.0070538473389377 ) ) ;
#67837 = AXIS2_PLACEMENT_3D ( 'NONE', #44781, #37540, #80221 ) ;
#67838 = CARTESIAN_POINT ( 'NONE',  ( 96.64068249873260186, -36.21262657180042766, 171.2870538473399620 ) ) ;
#67840 = CARTESIAN_POINT ( 'NONE',  ( 111.7390528236686436, -27.41013440965690862, 275.7070538473395800 ) ) ;
#67839 = DIRECTION ( 'NONE',  ( 1.000000000000000078E-15, 1.000000000000000083E-30, -1.000000000000000000 ) ) ;
#67841 = LINE ( 'NONE', #12433, #59403 ) ;
#67842 = EDGE_CURVE ( 'NONE', #85483, #30005, #83816, .T. ) ;
#67843 = CARTESIAN_POINT ( 'NONE',  ( 142.8696205427243626, 0.6543191929522240713, 540.9756252759101471 ) ) ;
#67844 = ORIENTED_EDGE ( 'NONE', *, *, #69690, .F. ) ;
#67845 = AXIS2_PLACEMENT_3D ( 'NONE', #64510, #78607, #30437 ) ;
#67846 = ORIENTED_EDGE ( 'NONE', *, *, #29814, .T. ) ;
#67847 = AXIS2_PLACEMENT_3D ( 'NONE', #5123, #34157, #12849 ) ;
#67848 = VECTOR ( 'NONE', #12553, 1000.000000000000000 ) ;
#67849 = VECTOR ( 'NONE', #48206, 999.9999999999998863 ) ;
#67850 = CARTESIAN_POINT ( 'NONE',  ( 97.83900843593762886, -40.58359296468890420, 111.6413228214579050 ) ) ;
#67851 = CARTESIAN_POINT ( 'NONE',  ( 107.2500105196458549, -24.83007258495691616, 230.0641967044819580 ) ) ;
#67852 = ORIENTED_EDGE ( 'NONE', *, *, #36902, .F. ) ;
#67853 = CARTESIAN_POINT ( 'NONE',  ( 116.3775870818408151, -41.41883695635522145, 203.4556252759109611 ) ) ;
#67854 = FACE_OUTER_BOUND ( 'NONE', #50275, .T. ) ;
#67855 = FILL_AREA_STYLE_COLOUR ( '', #21776 ) ;
#67856 = CARTESIAN_POINT ( 'NONE',  ( 62.56670390244669022, -48.82844715994099971, 129.9678068554150911 ) ) ;
#67858 = DIRECTION ( 'NONE',  ( 0.000000000000000000, 1.000000000000000000, 0.000000000000000000 ) ) ;
#67857 = CARTESIAN_POINT ( 'NONE',  ( 98.05617819296176663, -37.43095703503473004, 277.6356252759115932 ) ) ;
#67859 = CARTESIAN_POINT ( 'NONE',  ( -18.39335205926253280, -13.32818131006344231, 237.4678068554150059 ) ) ;
#67860 = CARTESIAN_POINT ( 'NONE',  ( 234.0013031625829854, 52.73749999999999716, -2.032000000000000028 ) ) ;
#67861 = CARTESIAN_POINT ( 'NONE',  ( 25.56670390244797275, -67.87844715994100397, 293.2178068554150627 ) ) ;
#67862 = ADVANCED_FACE ( 'NONE', ( #85427 ), #23202, .T. ) ;
#67863 = CARTESIAN_POINT ( 'NONE',  ( 107.0664832912739968, -36.72944715994100306, 0.4256252759109701023 ) ) ;
#67864 = EDGE_CURVE ( 'NONE', #84928, #31634, #1392, .T. ) ;
#67865 = CARTESIAN_POINT ( 'NONE',  ( 98.34816318742551289, -31.65962802882244631, 40.90603857251151965 ) ) ;
#67866 = PLANE ( 'NONE',  #76804 ) ;
#67868 = VERTEX_POINT ( 'NONE', #56780 ) ;
#67867 = DIRECTION ( 'NONE',  ( -0.000000000000000000, 1.000000000000000000, 0.000000000000000000 ) ) ;
#67869 = CARTESIAN_POINT ( 'NONE',  ( 0.000000000000000000, 223.9999999999999716, 159.6557476874258441 ) ) ;
#67870 = CARTESIAN_POINT ( 'NONE',  ( 113.8136090879065563, -26.95650955708257257, 239.5956252759109759 ) ) ;
#67871 = CARTESIAN_POINT ( 'NONE',  ( 116.9217636815068033, -33.22305568060546932, 110.0984824187679578 ) ) ;
#67872 = CARTESIAN_POINT ( 'NONE',  ( 105.8886828556765494, -47.16740550586902003, 278.4870538473396664 ) ) ;
#67873 = CARTESIAN_POINT ( 'NONE',  ( 74.06670390244701707, -90.27844715994098124, 51.21780685541800437 ) ) ;
#67874 = CARTESIAN_POINT ( 'NONE',  ( -72.96458098368751166, 101.5999999999999943, 67.92268098368620599 ) ) ;
#67875 = VECTOR ( 'NONE', #75970, 1000.000000000000000 ) ;
#67877 = CYLINDRICAL_SURFACE ( 'NONE', #38522, 34.13125000000000142 ) ;
#67876 = CARTESIAN_POINT ( 'NONE',  ( 41.56648329127499153, -32.07844715994070839, 314.1756252759120116 ) ) ;
#67878 = DIRECTION ( 'NONE',  ( 0.000000000000000000, -1.000000000000000000, 0.000000000000000000 ) ) ;
#67879 = VECTOR ( 'NONE', #49945, 1000.000000000000000 ) ;
#67880 = CARTESIAN_POINT ( 'NONE',  ( 132.4277392773811073, -20.94013506380670719, 2.060080721657580494 ) ) ;
#67881 = VERTEX_POINT ( 'NONE', #77695 ) ;
#67882 = VERTEX_POINT ( 'NONE', #42692 ) ;
#67883 = CARTESIAN_POINT ( 'NONE',  ( 100.8033404080456705, -29.31000718268690619, 150.0581341137909703 ) ) ;
#67885 = VERTEX_POINT ( 'NONE', #2737 ) ;
#67884 = CARTESIAN_POINT ( 'NONE',  ( 23.25885318707441485, 53.08705262765686683, 30.17677895551207001 ) ) ;
#67886 = LINE ( 'NONE', #60154, #76528 ) ;
#67887 = CARTESIAN_POINT ( 'NONE',  ( 113.3182355088850386, -45.04474967211692160, 139.0899109901969553 ) ) ;
#67888 = DIRECTION ( 'NONE',  ( 1.000000000000000078E-15, 0.000000000000000000, 1.000000000000000000 ) ) ;
#67889 = DIRECTION ( 'NONE',  ( 0.000000000000000000, 0.000000000000000000, -1.000000000000000000 ) ) ;
#67890 = DIRECTION ( 'NONE',  ( 1.000000000000000078E-15, 0.000000000000000000, -1.000000000000000000 ) ) ;
#67891 = PLANE ( 'NONE',  #70070 ) ;
#67892 = VECTOR ( 'NONE', #61248, 1000.000000000000000 ) ;
#67893 = CARTESIAN_POINT ( 'NONE',  ( 118.0115280580378396, -34.77548253539073642, 48.96705384733996169 ) ) ;
#67894 = EDGE_LOOP ( 'NONE', ( #88792, #43454, #22431, #6836 ) ) ;
#67895 = ORIENTED_EDGE ( 'NONE', *, *, #55241, .T. ) ;
#67896 = ORIENTED_EDGE ( 'NONE', *, *, #18787, .F. ) ;
#67897 = VECTOR ( 'NONE', #83311, 1000.000000000000000 ) ;
#67898 = CIRCLE ( 'NONE', #89705, 4.749999999999976907 ) ;
#67899 = DIRECTION ( 'NONE',  ( 9.351236661543306751E-17, -3.725950533538267725E-29, -1.000000000000000000 ) ) ;
#67901 = LINE ( 'NONE', #6571, #69411 ) ;
#67900 = CARTESIAN_POINT ( 'NONE',  ( 105.4244293397739085, -47.72525222749315787, 143.4584824187679715 ) ) ;
#67902 = PLANE ( 'NONE',  #78477 ) ;
#67904 = EDGE_CURVE ( 'NONE', #60678, #20709, #38856, .T. ) ;
#67903 = CARTESIAN_POINT ( 'NONE',  ( 11.00676631360785862, 76.20068480870281746, -130.0913480697105342 ) ) ;
#67905 = CARTESIAN_POINT ( 'NONE',  ( 193.0374249753375011, -23.42844715993436111, 237.4678068554150059 ) ) ;
#67906 = AXIS2_PLACEMENT_3D ( 'NONE', #40089, #18760, #67805 ) ;
#67907 = CARTESIAN_POINT ( 'NONE',  ( 81.47101467905535799, 94.84303900880917126, 86.13165781700368484 ) ) ;
#67908 = CARTESIAN_POINT ( 'NONE',  ( 117.0719695477731790, -35.46309620022125841, 179.9272431197764206 ) ) ;
#67909 = CARTESIAN_POINT ( 'NONE',  ( 112.7897778137182030, -47.07797880090547693, 102.9784824187679817 ) ) ;
#67910 = ORIENTED_EDGE ( 'NONE', *, *, #75738, .F. ) ;
#67911 = ORIENTED_EDGE ( 'NONE', *, *, #55788, .F. ) ;
#67912 = VECTOR ( 'NONE', #17694, 1000.000000000000114 ) ;
#67913 = DIRECTION ( 'NONE',  ( 0.000000000000000000, 0.000000000000000000, 1.000000000000000000 ) ) ;
#67914 = CARTESIAN_POINT ( 'NONE',  ( -84.37439091330328722, 89.26666702275849730, -99.62873342662643950 ) ) ;
#67915 = CIRCLE ( 'NONE', #85330, 2.500000000000002220 ) ;
#67916 = VECTOR ( 'NONE', #23644, 1000.000000000000000 ) ;
#67917 = CARTESIAN_POINT ( 'NONE',  ( -76.20505178924449297, 127.0000000000000000, 76.20505178924310030 ) ) ;
#67918 = CARTESIAN_POINT ( 'NONE',  ( 111.8340120402796032, -28.76913304608537914, 202.4652332267339716 ) ) ;
#67919 = EDGE_CURVE ( 'NONE', #10270, #10148, #21842, .T. ) ;
#67920 = LINE ( 'NONE', #24800, #76461 ) ;
#67921 = VERTEX_POINT ( 'NONE', #58132 ) ;
#67922 = ORIENTED_EDGE ( 'NONE', *, *, #41452, .F. ) ;
#67923 = CIRCLE ( 'NONE', #41776, 38.10000000000000142 ) ;
#67924 = CARTESIAN_POINT ( 'NONE',  ( -487.2989999999999782, 21.43125000000035030, 6.988054014476359654 ) ) ;
#67925 = CARTESIAN_POINT ( 'NONE',  ( 135.3099588813078924, -21.18301917768702225, 1.868341932368159153 ) ) ;
#67926 = VERTEX_POINT ( 'NONE', #84970 ) ;
#67927 = ORIENTED_EDGE ( 'NONE', *, *, #34600, .T. ) ;
#67928 = CARTESIAN_POINT ( 'NONE',  ( 77.49051321912324397, -19.69637952318584340, 6.988870342679232017 ) ) ;
#67929 = ADVANCED_FACE ( 'NONE', ( #70433 ), #64067, .F. ) ;
#67930 = CARTESIAN_POINT ( 'NONE',  ( 113.0661788413732580, -30.20779614827405624, 195.9158690201829529 ) ) ;
#67931 = ADVANCED_FACE ( 'NONE', ( #70889 ), #22286, .F. ) ;
#67932 = CONICAL_SURFACE ( 'NONE', #70878, 17.36499999999999844, 0.7853981633974490562 ) ;
#67933 = DIRECTION ( 'NONE',  ( -0.000000000000000000, 1.000000000000000000, 0.000000000000000000 ) ) ;
#67934 = VECTOR ( 'NONE', #2994, 1000.000000000000000 ) ;
#67935 = CARTESIAN_POINT ( 'NONE',  ( -109.2774118001976120, 53.97500000000000142, 71.43750000000000000 ) ) ;
#67936 = ORIENTED_EDGE ( 'NONE', *, *, #22542, .T. ) ;
#67937 = ORIENTED_EDGE ( 'NONE', *, *, #80627, .F. ) ;
#67938 = CARTESIAN_POINT ( 'NONE',  ( 41.56648329127399677, 0.2215528400590013880, 141.0426252759120018 ) ) ;
#67939 = ORIENTED_EDGE ( 'NONE', *, *, #16583, .F. ) ;
#67940 = EDGE_LOOP ( 'NONE', ( #53111, #70984, #23419, #44029 ) ) ;
#67941 = ADVANCED_FACE ( 'NONE', ( #2290 ), #22740, .F. ) ;
#67942 = CARTESIAN_POINT ( 'NONE',  ( 98.49961498605385657, -35.50075171889626091, 224.0433284648299548 ) ) ;
#67943 = CARTESIAN_POINT ( 'NONE',  ( 112.5258771334048475, -27.82206915948941273, 94.63848241876793566 ) ) ;
#67944 = CARTESIAN_POINT ( 'NONE',  ( 96.67837842349533162, -37.29153504031420141, 76.36991099019697060 ) ) ;
#67945 = CARTESIAN_POINT ( 'NONE',  ( 115.0636728013147945, -41.29441372593446857, 249.5838068554169809 ) ) ;
#67946 = DIRECTION ( 'NONE',  ( 0.7071067811865389130, 0.000000000000000000, 0.7071067811865561215 ) ) ;
#67947 = CARTESIAN_POINT ( 'NONE',  ( 108.0188260930178217, -25.30989513122313994, 322.4896988899195662 ) ) ;
#67948 = CARTESIAN_POINT ( 'NONE',  ( 99.28859025714638165, -29.78777103691475858, 186.7470538473389752 ) ) ;
#67949 = EDGE_CURVE ( 'NONE', #75765, #21614, #15918, .T. ) ;
#67950 = CARTESIAN_POINT ( 'NONE',  ( 106.0667039024470171, -87.35579742913164125, -19.26696060647653397 ) ) ;
#67951 = ORIENTED_EDGE ( 'NONE', *, *, #80428, .T. ) ;
#67952 = CARTESIAN_POINT ( 'NONE',  ( 129.9681746291969375, 79.66695435136418268, -12.37535028237872226 ) ) ;
#67953 = ORIENTED_EDGE ( 'NONE', *, *, #42477, .T. ) ;
#67954 = AXIS2_PLACEMENT_3D ( 'NONE', #52072, #3067, #72109 ) ;
#67955 = ORIENTED_EDGE ( 'NONE', *, *, #47071, .T. ) ;
#67956 = CARTESIAN_POINT ( 'NONE',  ( 152.0368932755770288, -23.42844715993588522, 300.4678068554149490 ) ) ;
#67957 = ORIENTED_EDGE ( 'NONE', *, *, #89810, .F. ) ;
#67958 = VECTOR ( 'NONE', #33591, 1000.000000000000000 ) ;
#67959 = CARTESIAN_POINT ( 'NONE',  ( 97.79627051079565092, -40.47954843556247084, 137.6323705464966167 ) ) ;
#67960 = AXIS2_PLACEMENT_3D ( 'NONE', #8736, #15545, #37771 ) ;
#67961 = CARTESIAN_POINT ( 'NONE',  ( 109.6430121110707319, -46.48008674055821388, 177.7814586078273464 ) ) ;
#67962 = CARTESIAN_POINT ( 'NONE',  ( 110.1579966911880888, -46.68583080861444756, 97.81562527591097478 ) ) ;
#67963 = CARTESIAN_POINT ( 'NONE',  ( -6.975949578566201126, 71.93738766389279249, 130.3694979861350873 ) ) ;
#67964 = CARTESIAN_POINT ( 'NONE',  ( 136.8000579002614074, -36.42904715602825405, 6.774297104451916240 ) ) ;
#67965 = CARTESIAN_POINT ( 'NONE',  ( 122.2221484686745185, -96.57698625956679450, -11.78219314458225853 ) ) ;
#67968 = CARTESIAN_POINT ( 'NONE',  ( 118.0279888096067396, -35.50094427011356402, 229.9032443235299468 ) ) ;
#67967 = DIRECTION ( 'NONE',  ( 0.000000000000000000, 1.000000000000000000, 0.000000000000000000 ) ) ;
#67966 = CARTESIAN_POINT ( 'NONE',  ( 113.1782937664330859, -44.75186859636650638, 144.0939586087628754 ) ) ;
#67969 = DIRECTION ( 'NONE',  ( 1.000000000000000078E-15, -1.000000000000000000, 0.000000000000000000 ) ) ;
#67970 = DIRECTION ( 'NONE',  ( 3.339108161477000479E-13, -1.000000000000000000, 6.848429599184487071E-29 ) ) ;
#67971 = ORIENTED_EDGE ( 'NONE', *, *, #36547, .F. ) ;
#67972 = DIRECTION ( 'NONE',  ( 1.000000000000000078E-15, -1.000000000000000083E-30, -1.000000000000000000 ) ) ;
#67973 = ADVANCED_FACE ( 'NONE', ( #71334 ), #71774, .F. ) ;
#67974 = AXIS2_PLACEMENT_3D ( 'NONE', #69277, #27483, #83359 ) ;
#67975 = CARTESIAN_POINT ( 'NONE',  ( 142.8838050580815775, -82.11588141944044139, 394.9756252759102040 ) ) ;
#67976 = ADVANCED_FACE ( 'NONE', ( #57684 ), #9545, .F. ) ;
#67977 = CARTESIAN_POINT ( 'NONE',  ( 50.87649884952377022, -33.54226604284969682, 193.9678068554150911 ) ) ;
#67978 = ADVANCED_FACE ( 'NONE', ( #64953 ), #23634, .T. ) ;
#67979 = CIRCLE ( 'NONE', #76731, 34.13125000000000142 ) ;
#67980 = DIRECTION ( 'NONE',  ( 1.000000000000000078E-15, -1.000000000000000083E-30, -1.000000000000000000 ) ) ;
#67982 = ORIENTED_EDGE ( 'NONE', *, *, #65396, .F. ) ;
#67981 = CARTESIAN_POINT ( 'NONE',  ( 104.3993058286337146, -25.95452033834810024, 240.2575300378159682 ) ) ;
#67983 = CARTESIAN_POINT ( 'NONE',  ( 144.0667039024470739, -137.6784471599409017, 222.2178068554179902 ) ) ;
#67984 = CARTESIAN_POINT ( 'NONE',  ( 112.1172674779030558, -26.89768192312349271, 15.71086337114896381 ) ) ;
#67985 = CARTESIAN_POINT ( 'NONE',  ( 108.3715344132687051, -47.75189438633907457, 158.6822919425779617 ) ) ;
#67986 = ADVANCED_FACE ( 'NONE', ( #27394 ), #61908, .F. ) ;
#67987 = CARTESIAN_POINT ( 'NONE',  ( 107.0667039024480260, -36.72944715994099596, 199.5838068554169809 ) ) ;
#67988 = CARTESIAN_POINT ( 'NONE',  ( 97.60785222787119153, -39.98231739658664452, 102.5900457468837743 ) ) ;
#67990 = DIRECTION ( 'NONE',  ( 0.000000000000000000, 0.000000000000000000, 1.000000000000000000 ) ) ;
#67989 = FACE_OUTER_BOUND ( 'NONE', #8022, .T. ) ;
#67991 = PLANE ( 'NONE',  #36489 ) ;
#67992 = CYLINDRICAL_SURFACE ( 'NONE', #80132, 13.99999999999999822 ) ;
#67993 = ORIENTED_EDGE ( 'NONE', *, *, #67745, .F. ) ;
#67994 = VERTEX_POINT ( 'NONE', #84070 ) ;
#67995 = ORIENTED_EDGE ( 'NONE', *, *, #4635, .F. ) ;
#67996 = CIRCLE ( 'NONE', #31736, 2.999999999999947153 ) ;
#67997 = ORIENTED_EDGE ( 'NONE', *, *, #72995, .T. ) ;
#67998 = DIRECTION ( 'NONE',  ( 0.000000000000000000, 0.000000000000000000, -1.000000000000000000 ) ) ;
#67999 = CARTESIAN_POINT ( 'NONE',  ( 96.85498737197835339, -38.89503640450122646, 27.49276813305395706 ) ) ;
#68000 = CARTESIAN_POINT ( 'NONE',  ( 29.56670390244797630, -67.87844715994100397, 10.91780685541479734 ) ) ;
#68001 = CARTESIAN_POINT ( 'NONE',  ( 34.92499999999999716, 87.13271776169258942, 310.8325000000000387 ) ) ;
#68003 = CARTESIAN_POINT ( 'NONE',  ( 53.35959712126192755, -48.62134037875358672, 180.4678068554151196 ) ) ;
#68002 = DIRECTION ( 'NONE',  ( 0.000000000000000000, 0.000000000000000000, -1.000000000000000000 ) ) ;
#68004 = CARTESIAN_POINT ( 'NONE',  ( 110.0705912124663968, -28.18614534367760172, 254.2419436376007695 ) ) ;
#68005 = VERTEX_POINT ( 'NONE', #77248 ) ;
#68006 = VECTOR ( 'NONE', #17635, 1000.000000000000000 ) ;
#68007 = ORIENTED_EDGE ( 'NONE', *, *, #8575, .F. ) ;
#68008 = ORIENTED_EDGE ( 'NONE', *, *, #40752, .T. ) ;
#68009 = DIRECTION ( 'NONE',  ( 1.000000000000000000, 0.000000000000000000, 0.000000000000000000 ) ) ;
#68010 = CARTESIAN_POINT ( 'NONE',  ( 97.81413224952068219, -40.51639846094042952, 101.6360726122380100 ) ) ;
#68011 = CARTESIAN_POINT ( 'NONE',  ( 20.56670390244740076, -48.82844715994099971, 300.4678068554149490 ) ) ;
#68012 = LINE ( 'NONE', #68468, #5490 ) ;
#68013 = CARTESIAN_POINT ( 'NONE',  ( 99.19755098026091389, -30.44051964901187191, 42.22158330589692810 ) ) ;
#68014 = CYLINDRICAL_SURFACE ( 'NONE', #89394, 0.9999999999999800160 ) ;
#68015 = CYLINDRICAL_SURFACE ( 'NONE', #21594, 2.517499999999998739 ) ;
#68016 = CARTESIAN_POINT ( 'NONE',  ( 106.8506556707805260, -46.50783423188027399, 272.5584824187685626 ) ) ;
#68017 = FACE_OUTER_BOUND ( 'NONE', #8988, .T. ) ;
#68018 = ORIENTED_EDGE ( 'NONE', *, *, #70932, .T. ) ;
#68019 = VECTOR ( 'NONE', #21969, 1000.000000000000114 ) ;
#68020 = CARTESIAN_POINT ( 'NONE',  ( 100.8961411191535973, 120.6499999999999915, -3.968749999999580336 ) ) ;
#68021 = DIRECTION ( 'NONE',  ( -1.000000000000000078E-15, 1.000000000000000000, -3.100000000000000044E-14 ) ) ;
#68022 = CARTESIAN_POINT ( 'NONE',  ( 113.2960346059783774, -42.04690695427109404, 61.08237608387695161 ) ) ;
#68023 = VECTOR ( 'NONE', #41730, 999.9999999999998863 ) ;
#68024 = CIRCLE ( 'NONE', #43371, 2.517500000000005844 ) ;
#68025 = ADVANCED_FACE ( 'NONE', ( #15018 ), #11772, .T. ) ;
#68026 = CARTESIAN_POINT ( 'NONE',  ( 136.3178028891481119, -17.14744377622660210, 7.339349742399202903 ) ) ;
#68027 = EDGE_CURVE ( 'NONE', #42257, #66654, #1137, .T. ) ;
#68028 = CARTESIAN_POINT ( 'NONE',  ( 101.9935804828795369, -45.44604673876975909, 193.1563667090017020 ) ) ;
#68029 = VERTEX_POINT ( 'NONE', #52618 ) ;
#68031 = ADVANCED_FACE ( 'NONE', ( #86292 ), #9892, .T. ) ;
#68030 = VECTOR ( 'NONE', #76318, 1000.000000000000000 ) ;
#68032 = DIRECTION ( 'NONE',  ( -4.237773401492740281E-14, 1.000000000000000000, 0.000000000000000000 ) ) ;
#68033 = ORIENTED_EDGE ( 'NONE', *, *, #74615, .T. ) ;
#68034 = CARTESIAN_POINT ( 'NONE',  ( 105.7204000585623191, -24.95538135984382677, 160.1670538473389627 ) ) ;
#68035 = ORIENTED_EDGE ( 'NONE', *, *, #62027, .F. ) ;
#68036 = CARTESIAN_POINT ( 'NONE',  ( 104.5891003629744631, -45.44008686965874944, 66.79051506617194889 ) ) ;
#68037 = AXIS2_PLACEMENT_3D ( 'NONE', #87351, #25111, #52774 ) ;
#68038 = EDGE_CURVE ( 'NONE', #81729, #23402, #11300, .T. ) ;
#68039 = CARTESIAN_POINT ( 'NONE',  ( 97.81373435033219721, -40.51654435448209313, 87.63515866765291662 ) ) ;
#68040 = CARTESIAN_POINT ( 'NONE',  ( 115.4437480007128443, -33.74891607059462473, 110.5301547344689794 ) ) ;
#68041 = EDGE_CURVE ( 'NONE', #87716, #50621, #10871, .T. ) ;
#68042 = FACE_OUTER_BOUND ( 'NONE', #10862, .T. ) ;
#68043 = VECTOR ( 'NONE', #19713, 1000.000000000000000 ) ;
#68044 = LINE ( 'NONE', #33518, #71636 ) ;
#68045 = CARTESIAN_POINT ( 'NONE',  ( 100.9283148882350787, -46.89532829952024429, 48.14419670448194211 ) ) ;
#68047 = EDGE_CURVE ( 'NONE', #64058, #35419, #16806, .T. ) ;
#68046 = PLANE ( 'NONE',  #4805 ) ;
#68048 = PLANE ( 'NONE',  #12599 ) ;
#68049 = ORIENTED_EDGE ( 'NONE', *, *, #28568, .T. ) ;
#68050 = CARTESIAN_POINT ( 'NONE',  ( -117.8738102209307925, 82.54999999999999716, 12.69999999999959073 ) ) ;
#68051 = ORIENTED_EDGE ( 'NONE', *, *, #23826, .F. ) ;
#68052 = ORIENTED_EDGE ( 'NONE', *, *, #45860, .T. ) ;
#68053 = EDGE_CURVE ( 'NONE', #53519, #42410, #21496, .T. ) ;
#68054 = AXIS2_PLACEMENT_3D ( 'NONE', #9988, #84525, #64950 ) ;
#68055 = CARTESIAN_POINT ( 'NONE',  ( 115.5439452383992176, -108.5954344580498372, -19.78219314458187839 ) ) ;
#68056 = VERTEX_POINT ( 'NONE', #39016 ) ;
#68057 = CARTESIAN_POINT ( 'NONE',  ( 101.9853755998761073, -45.08682593082395584, 247.1413395616259550 ) ) ;
#68058 = CARTESIAN_POINT ( 'NONE',  ( 114.2683966348991760, -44.29710505712337465, 154.1813395616249807 ) ) ;
#68059 = CARTESIAN_POINT ( 'NONE',  ( 8.690994986491583418, 73.28026231907210786, -118.2373793989773247 ) ) ;
#68060 = DIRECTION ( 'NONE',  ( 0.000000000000000000, -1.000000000000000000, 0.000000000000000000 ) ) ;
#68061 = CARTESIAN_POINT ( 'NONE',  ( 113.4153195569882087, -27.68144967124534261, 80.57753003781597556 ) ) ;
#68062 = EDGE_CURVE ( 'NONE', #68436, #88057, #80965, .T. ) ;
#68063 = CARTESIAN_POINT ( 'NONE',  ( 99.09675058860776176, -30.54904317927480761, 96.80150208561718728 ) ) ;
#68064 = ORIENTED_EDGE ( 'NONE', *, *, #62, .T. ) ;
#68065 = CARTESIAN_POINT ( 'NONE',  ( 52.65249034007746332, -49.32844715994061602, 180.4678068554151196 ) ) ;
#68066 = CARTESIAN_POINT ( 'NONE',  ( 99.04409650882432459, -42.84130985989413176, 157.8437691819532063 ) ) ;
#68068 = ORIENTED_EDGE ( 'NONE', *, *, #7761, .F. ) ;
#68067 = VECTOR ( 'NONE', #5240, 1000.000000000000114 ) ;
#68069 = CARTESIAN_POINT ( 'NONE',  ( 107.0667039024470313, -104.2784471599409528, 23.21780685541800082 ) ) ;
#68070 = PLANE ( 'NONE',  #20322 ) ;
#68071 = CARTESIAN_POINT ( 'NONE',  ( 99.39760893136102027, -29.69972230079146769, 275.7356252759109907 ) ) ;
#68072 = CYLINDRICAL_SURFACE ( 'NONE', #31525, 5.041900000000001825 ) ;
#68073 = CYLINDRICAL_SURFACE ( 'NONE', #18773, 2.500000000000002220 ) ;
#68074 = CARTESIAN_POINT ( 'NONE',  ( 184.5667039024480118, -67.87844715994100397, 300.9178068554150514 ) ) ;
#68075 = CARTESIAN_POINT ( 'NONE',  ( 103.8089036935402021, -45.87596577953674881, 251.7267055423626516 ) ) ;
#68077 = CARTESIAN_POINT ( 'NONE',  ( 95.80265872640110558, -40.33145541733360773, 127.5727681330539554 ) ) ;
#68076 = CARTESIAN_POINT ( 'NONE',  ( 114.8007373875590531, -30.34631565586484925, 99.37626092783206389 ) ) ;
#68078 = DIRECTION ( 'NONE',  ( 0.000000000000000000, 0.000000000000000000, 1.000000000000000000 ) ) ;
#68079 = CARTESIAN_POINT ( 'NONE',  ( 98.13053560861905567, -31.27458647820624549, 170.8899109901960003 ) ) ;
#68080 = ORIENTED_EDGE ( 'NONE', *, *, #5088, .T. ) ;
#68081 = DIRECTION ( 'NONE',  ( 0.000000000000000000, 0.000000000000000000, 1.000000000000000000 ) ) ;
#68082 = ORIENTED_EDGE ( 'NONE', *, *, #14668, .F. ) ;
#68083 = CARTESIAN_POINT ( 'NONE',  ( 88.90000000000000568, 69.84999999999999432, 346.0750000000000455 ) ) ;
#68084 = CARTESIAN_POINT ( 'NONE',  ( 109.7248659029457798, -27.00080517437059768, 65.86479194409724869 ) ) ;
#68085 = DIRECTION ( 'NONE',  ( -0.7396053187813123042, -0.6730408400909958511, 0.000000000000000000 ) ) ;
#68086 = ORIENTED_EDGE ( 'NONE', *, *, #35303, .T. ) ;
#68087 = EDGE_CURVE ( 'NONE', #58498, #61827, #65826, .T. ) ;
#68088 = AXIS2_PLACEMENT_3D ( 'NONE', #71795, #59025, #58582 ) ;
#68089 = CARTESIAN_POINT ( 'NONE',  ( 105.8017600360789174, -26.72373307582276780, 61.17738641589737369 ) ) ;
#68091 = ORIENTED_EDGE ( 'NONE', *, *, #26740, .T. ) ;
#68090 = CARTESIAN_POINT ( 'NONE',  ( 108.6554276816787734, -25.75039326353942926, 149.9737205140059473 ) ) ;
#68093 = CARTESIAN_POINT ( 'NONE',  ( 80.06648329127402519, -46.42944715994105565, 10.42562527591094401 ) ) ;
#68092 = UNCERTAINTY_MEASURE_WITH_UNIT (LENGTH_MEASURE( 1.000000000000000082E-05 ), #72782, 'distance_accuracy_value', 'NONE');
#68094 = EDGE_CURVE ( 'NONE', #75654, #63113, #11315, .T. ) ;
#68095 = CARTESIAN_POINT ( 'NONE',  ( -130.2877996231769941, 92.12504059357188169, -8.385216644674851949 ) ) ;
#68096 = CARTESIAN_POINT ( 'NONE',  ( 172.5664832912740110, -9.303447159940999356, 21.04262527591200183 ) ) ;
#68098 = CARTESIAN_POINT ( 'NONE',  ( 172.5667039024482960, -42.82844715993499563, 180.4678068554150059 ) ) ;
#68097 = CIRCLE ( 'NONE', #72438, 4.750000000000004441 ) ;
#68099 = EDGE_LOOP ( 'NONE', ( #67585, #58198, #28088, #57964, #27369 ) ) ;
#68100 = VECTOR ( 'NONE', #22935, 999.9999999999998863 ) ;
#68101 = DIRECTION ( 'NONE',  ( 1.000000000000000000, 5.130477113903179357E-17, -1.573642578468252162E-16 ) ) ;
#68102 = DIRECTION ( 'NONE',  ( -0.000000000000000000, 1.000000000000000000, 0.000000000000000000 ) ) ;
#68103 = VERTEX_POINT ( 'NONE', #31757 ) ;
#68104 = ORIENTED_EDGE ( 'NONE', *, *, #53700, .T. ) ;
#68105 = CIRCLE ( 'NONE', #62318, 3.000000000000002665 ) ;
#68106 = EDGE_LOOP ( 'NONE', ( #85078, #54883, #68947 ) ) ;
#68107 = CARTESIAN_POINT ( 'NONE',  ( 21.03715912545823130, -47.82818131006186491, 313.9678068554150059 ) ) ;
#68108 = CARTESIAN_POINT ( 'NONE',  ( -7.301849239715819957E-13, 127.0000000000000000, 98.60478223830740774 ) ) ;
#68109 = CARTESIAN_POINT ( 'NONE',  ( 116.8171228686926639, -34.15291832592715338, 159.0314586087905582 ) ) ;
#68110 = PLANE ( 'NONE',  #24110 ) ;
#68111 = CIRCLE ( 'NONE', #49292, 3.499999999999996003 ) ;
#68113 = CARTESIAN_POINT ( 'NONE',  ( -6.802569982901797644E-16, 69.84999999999999432, -118.5560000000000116 ) ) ;
#68112 = CARTESIAN_POINT ( 'NONE',  ( 194.0371591254582313, -46.82818131005407736, 300.4678068554149490 ) ) ;
#68114 = CARTESIAN_POINT ( 'NONE',  ( 183.5150000000000148, 68.61249999999999716, -35.28456447661459805 ) ) ;
#68115 = ORIENTED_EDGE ( 'NONE', *, *, #14038, .T. ) ;
#68116 = DIRECTION ( 'NONE',  ( 0.9242245927363033076, 0.3818493186865917766, 0.000000000000000000 ) ) ;
#68117 = CARTESIAN_POINT ( 'NONE',  ( 95.56670390244703128, -104.2784471599414644, 0.2178068554180012661 ) ) ;
#68118 = CARTESIAN_POINT ( 'NONE',  ( 99.06478422775796844, -31.10483629442216014, 201.8384824187669437 ) ) ;
#68119 = AXIS2_PLACEMENT_3D ( 'NONE', #69314, #34330, #20714 ) ;
#68121 = ORIENTED_EDGE ( 'NONE', *, *, #87045, .T. ) ;
#68120 = CARTESIAN_POINT ( 'NONE',  ( 116.3186249068867539, -32.94868901193379429, 250.1356252759109395 ) ) ;
#68122 = CARTESIAN_POINT ( 'NONE',  ( 96.71749658230667990, -40.79275330125899046, 92.62419670448196030 ) ) ;
#68123 = CARTESIAN_POINT ( 'NONE',  ( 116.3427928135287885, -40.59072558610812820, 53.51233718776536108 ) ) ;
#68124 = DIRECTION ( 'NONE',  ( 0.000000000000000000, 0.000000000000000000, -1.000000000000000000 ) ) ;
#68125 = CARTESIAN_POINT ( 'NONE',  ( 182.2300522401149863, -33.89581943344511217, -5.074374724088000832 ) ) ;
#68126 = ORIENTED_EDGE ( 'NONE', *, *, #81613, .F. ) ;
#68127 = FACE_OUTER_BOUND ( 'NONE', #24831, .T. ) ;
#68128 = ORIENTED_EDGE ( 'NONE', *, *, #3169, .F. ) ;
#68129 = EDGE_LOOP ( 'NONE', ( #56988, #56972 ) ) ;
#68131 = ADVANCED_FACE ( 'NONE', ( #45374, #9991 ), #24072, .F. ) ;
#68130 = VECTOR ( 'NONE', #43773, 1000.000000000000000 ) ;
#68132 = CARTESIAN_POINT ( 'NONE',  ( 102.4628740603001233, -44.30143901548009211, 243.5730118773259676 ) ) ;
#68133 = LINE ( 'NONE', #19528, #29927 ) ;
#68134 = CARTESIAN_POINT ( 'NONE',  ( -118.5385583271987713, 95.08639429146512612, -2.073938160688237442 ) ) ;
#68135 = EDGE_CURVE ( 'NONE', #74274, #82155, #14230, .T. ) ;
#68136 = EDGE_CURVE ( 'NONE', #54444, #35904, #24352, .T. ) ;
#68137 = CARTESIAN_POINT ( 'NONE',  ( 108.3334480117198666, -46.73485936529269935, 153.6772919359582943 ) ) ;
#68138 = CARTESIAN_POINT ( 'NONE',  ( 204.2160000000000082, 52.73749999999999716, -44.45000000000000284 ) ) ;
#68139 = VERTEX_POINT ( 'NONE', #79492 ) ;
#68140 = AXIS2_PLACEMENT_3D ( 'NONE', #25113, #89143, #47778 ) ;
#68141 = CYLINDRICAL_SURFACE ( 'NONE', #81249, 2.517500000000000071 ) ;
#68142 = EDGE_CURVE ( 'NONE', #74286, #11288, #88224, .T. ) ;
#68143 = CARTESIAN_POINT ( 'NONE',  ( 71.25529199314597406, -79.12815651470191369, 361.9756252759101471 ) ) ;
#68144 = EDGE_LOOP ( 'NONE', ( #84652, #8636, #42886, #31675, #12253, #7853, #63126, #60423, #40388 ) ) ;
#68145 = CARTESIAN_POINT ( 'NONE',  ( 118.3173389373707920, -33.08695204176926552, 284.0756252759109657 ) ) ;
#68146 = ORIENTED_EDGE ( 'NONE', *, *, #64289, .F. ) ;
#68147 = CARTESIAN_POINT ( 'NONE',  ( 110.2461554203946292, -29.21150786992351911, 242.5766617981629452 ) ) ;
#68148 = VECTOR ( 'NONE', #33355, 1000.000000000000000 ) ;
#68149 = ADVANCED_FACE ( 'NONE', ( #31306 ), #59002, .F. ) ;
#68150 = DIRECTION ( 'NONE',  ( 0.000000000000000000, 0.000000000000000000, 1.000000000000000000 ) ) ;
#68151 = CARTESIAN_POINT ( 'NONE',  ( 109.0694692412632492, -27.15596902575777349, 139.9127681330539872 ) ) ;
#68152 = DIRECTION ( 'NONE',  ( 0.000000000000000000, 0.000000000000000000, 1.000000000000000000 ) ) ;
#68153 = DIRECTION ( 'NONE',  ( -0.7071067811865270336, 0.7071067811865680008, -7.071067811864966518E-16 ) ) ;
#68154 = DIRECTION ( 'NONE',  ( 0.000000000000000000, 0.000000000000000000, 1.000000000000000000 ) ) ;
#68155 = CARTESIAN_POINT ( 'NONE',  ( 7.064474567469056332, 71.99617586329878804, 130.3647280704349782 ) ) ;
#68156 = CARTESIAN_POINT ( 'NONE',  ( 112.4768706805521248, -45.73309770202773450, 234.0070538473389377 ) ) ;
#68158 = DIRECTION ( 'NONE',  ( -0.000000000000000000, -1.000000000000000000, -0.000000000000000000 ) ) ;
#68157 = CIRCLE ( 'NONE', #79786, 2.517499999999998739 ) ;
#68159 = AXIS2_PLACEMENT_3D ( 'NONE', #29427, #43025, #14459 ) ;
#68160 = EDGE_CURVE ( 'NONE', #78132, #41012, #79938, .T. ) ;
#68161 = VERTEX_POINT ( 'NONE', #73093 ) ;
#68162 = CARTESIAN_POINT ( 'NONE',  ( 116.2698991418618419, -31.74044761805202342, 65.22133956162595325 ) ) ;
#68163 = CARTESIAN_POINT ( 'NONE',  ( 138.0667039024480403, -58.72944715994091069, 239.5838068554170377 ) ) ;
#68164 = ORIENTED_EDGE ( 'NONE', *, *, #38700, .F. ) ;
#68165 = ORIENTED_EDGE ( 'NONE', *, *, #63004, .F. ) ;
#68166 = B_SPLINE_CURVE_WITH_KNOTS ( 'NONE', 3,
 ( #55569, #48767, #87113, #24881, #38494, #52548, #18056, #16075, #36948, #70131, #1092, #76949, #85573, #56486, #9253, #63773, #29689, #57835 ),
 .UNSPECIFIED., .F., .F.,
 ( 4, 2, 2, 2, 2, 2, 2, 2, 4 ),
 ( 0.000000000000000000, 0.06250571285318999581, 0.1250114257063799916, 0.1875171385595699736, 0.2500228514127599833, 0.3125285642659499930, 0.3750342771191399471, 0.4375399899723299568, 0.5000457028255199665 ),
 .UNSPECIFIED. ) ;
#68167 = ORIENTED_EDGE ( 'NONE', *, *, #21849, .T. ) ;
#68168 = EDGE_CURVE ( 'NONE', #8740, #54700, #56280, .T. ) ;
#68169 = AXIS2_PLACEMENT_3D ( 'NONE', #38323, #66022, #73741 ) ;
#68170 = CARTESIAN_POINT ( 'NONE',  ( 100.9536334643938886, -28.70783906175689992, 160.5938426771316188 ) ) ;
#68171 = FACE_OUTER_BOUND ( 'NONE', #31764, .T. ) ;
#68172 = FACE_OUTER_BOUND ( 'NONE', #81398, .T. ) ;
#68173 = CARTESIAN_POINT ( 'NONE',  ( 69.72411017813010403, 127.0000000000000000, -69.72411017812979139 ) ) ;
#68174 = CARTESIAN_POINT ( 'NONE',  ( 112.6937225954192172, -42.64246220573352275, 155.9995189410199714 ) ) ;
#68175 = CARTESIAN_POINT ( 'NONE',  ( 104.8366293861751330, -26.48703790372925937, 256.2470538473397710 ) ) ;
#68176 = EDGE_CURVE ( 'NONE', #29586, #43862, #27317, .T. ) ;
#68177 = LINE ( 'NONE', #88629, #58109 ) ;
#68178 = ORIENTED_EDGE ( 'NONE', *, *, #7054, .F. ) ;
#68179 =( NAMED_UNIT ( * ) PLANE_ANGLE_UNIT ( ) SI_UNIT ( $, .RADIAN. ) );
#68180 = VECTOR ( 'NONE', #9521, 1000.000000000000114 ) ;
#68181 = DIRECTION ( 'NONE',  ( 1.000000000000000078E-15, -1.000000000000000083E-30, -1.000000000000000000 ) ) ;
#68182 = ORIENTED_EDGE ( 'NONE', *, *, #32048, .T. ) ;
#68183 = EDGE_LOOP ( 'NONE', ( #52495, #43922, #60575, #21953 ) ) ;
#68184 = DIRECTION ( 'NONE',  ( -0.7071067812162665778, -0.7071067811568285677, -7.071067812162659944E-16 ) ) ;
#68185 = ORIENTED_EDGE ( 'NONE', *, *, #40134, .T. ) ;
#68186 = ORIENTED_EDGE ( 'NONE', *, *, #6919, .T. ) ;
#68187 = FACE_OUTER_BOUND ( 'NONE', #66308, .T. ) ;
#68188 = CARTESIAN_POINT ( 'NONE',  ( -6.720195294977327372, 71.76561749959921599, -130.3833905926466628 ) ) ;
#68189 = FACE_OUTER_BOUND ( 'NONE', #2891, .T. ) ;
#68190 = CARTESIAN_POINT ( 'NONE',  ( 124.9629318080292251, -56.47944715994101728, 14.92562527591098842 ) ) ;
#68191 = AXIS2_PLACEMENT_3D ( 'NONE', #39252, #11094, #58785 ) ;
#68192 = CARTESIAN_POINT ( 'NONE',  ( 115.8434954054525292, -34.49858887834006538, 168.4590864947439854 ) ) ;
#68193 = CARTESIAN_POINT ( 'NONE',  ( 113.4866449958868770, -46.74994221786862880, 68.02991099019695298 ) ) ;
#68194 = DIRECTION ( 'NONE',  ( 0.000000000000000000, -1.000000000000000000, 0.000000000000000000 ) ) ;
#68195 = ORIENTED_EDGE ( 'NONE', *, *, #28895, .T. ) ;
#68196 = LINE ( 'NONE', #27297, #33961 ) ;
#68197 = ORIENTED_EDGE ( 'NONE', *, *, #49334, .F. ) ;
#68198 = DIRECTION ( 'NONE',  ( -0.6253590364320038564, 0.4667463455728951827, -0.6253590364320190664 ) ) ;
#68199 = VERTEX_POINT ( 'NONE', #52007 ) ;
#68200 = CARTESIAN_POINT ( 'NONE',  ( 107.0664832912748068, -36.72944715993923381, 13.92562527591097066 ) ) ;
#68201 = DIRECTION ( 'NONE',  ( -0.7071067811865516806, 0.7071067811865433539, -7.071067811865510832E-16 ) ) ;
#68202 = EDGE_CURVE ( 'NONE', #35758, #53395, #40402, .T. ) ;
#68203 = CARTESIAN_POINT ( 'NONE',  ( 114.6570493066734002, -43.27250257336863370, 133.2604112297873371 ) ) ;
#68204 = VECTOR ( 'NONE', #20445, 1000.000000000000000 ) ;
#68205 = CARTESIAN_POINT ( 'NONE',  ( 162.7866693523294828, -29.62846900981742237, 313.9678068554149490 ) ) ;
#68206 = VERTEX_POINT ( 'NONE', #25219 ) ;
#68207 = CARTESIAN_POINT ( 'NONE',  ( 113.7561043996362287, -29.08408549058404091, 289.5032443235301116 ) ) ;
#68208 = CARTESIAN_POINT ( 'NONE',  ( 96.87875409107806490, -32.32403320637130406, 57.01372051400599616 ) ) ;
#68209 = SURFACE_STYLE_USAGE ( .BOTH. , #60016 ) ;
#68211 = DIRECTION ( 'NONE',  ( 0.000000000000000000, 0.000000000000000000, 1.000000000000000000 ) ) ;
#68210 = CARTESIAN_POINT ( 'NONE',  ( 71.06670390244705970, -118.2784471599409812, 51.21780685541800437 ) ) ;
#68212 = CARTESIAN_POINT ( 'NONE',  ( 136.8164832912740110, -36.72944715994100306, -5.074374724088999145 ) ) ;
#68213 = B_SPLINE_CURVE_WITH_KNOTS ( 'NONE', 3,
 ( #18250, #45482, #10983, #4181, #73203, #45927, #57798, #16472, #44149, #65067, #40487, #75009, #60927, #4628, #25969, #88655, #81843, #74557, #27303, #33675, #40030, #60466, #32774, #88211, #67287, #11443, #13240, #67749, #39141, #61813, #26852, #19592, #26417, #18699, #80951, #53634, #82747, #6415, #12337, #54087, #68203, #33230, #54978, #34107, #87743, #5071, #60009, #61368, #5535, #25512, #54532 ),
 .UNSPECIFIED., .F., .F.,
 ( 4, 2, 1, 1, 1, 1, 1, 1, 2, 2, 2, 2, 2, 2, 2, 1, 1, 1, 1, 1, 1, 1, 2, 2, 2, 2, 2, 2, 2, 2, 2, 4 ),
 ( 0.5000150437144960103, 0.5001371103542051610, 0.5002591769939142008, 0.5005033102733320582, 0.5009915768321673291, 0.5019681099498382038, 0.5039211761851796201, 0.5078273086558623417, 0.5156395735972280070, 0.5312641034799590045, 0.5625131632454207775, 0.6250112827763437684, 0.6875094023072667593, 0.7500075218381896391, 0.7500685551580437149, 0.7501295884778977907, 0.7502516551176239279, 0.7504957883970906352, 0.7509840549560078404, 0.7519605880738274850, 0.7539136543094671072, 0.7578197867807463517, 0.7656320517233036194, 0.7812565816084167114, 0.8125056413786428955, 0.8437547011488690796, 0.8750037609190952637, 0.9062528206893214477, 0.9375018804595476318, 0.9687509402297738159, 0.9843754701148869080, 1.000000000000000000 ),
 .UNSPECIFIED. ) ;
#68214 = CARTESIAN_POINT ( 'NONE',  ( 1.232595164407830946E-29, 69.95000000000000284, 118.3560000000000088 ) ) ;
#68215 = ORIENTED_EDGE ( 'NONE', *, *, #35140, .F. ) ;
#68216 = CIRCLE ( 'NONE', #84176, 2.999999999999933387 ) ;
#68217 = DIRECTION ( 'NONE',  ( -0.000000000000000000, -0.000000000000000000, 1.000000000000000000 ) ) ;
#68218 = CARTESIAN_POINT ( 'NONE',  ( 147.0663630288289880, -77.84642232681920859, 246.0747600069850023 ) ) ;
#68220 = DIRECTION ( 'NONE',  ( 0.000000000000000000, 0.000000000000000000, -1.000000000000000000 ) ) ;
#68219 = VECTOR ( 'NONE', #18267, 1000.000000000000000 ) ;
#68221 = ORIENTED_EDGE ( 'NONE', *, *, #15294, .T. ) ;
#68222 = EDGE_CURVE ( 'NONE', #7923, #3091, #10260, .T. ) ;
#68223 = CARTESIAN_POINT ( 'NONE',  ( 103.3547197592076969, -47.16534756318074528, 98.31657765686297523 ) ) ;
#68225 = LINE ( 'NONE', #6006, #70307 ) ;
#68224 = CARTESIAN_POINT ( 'NONE',  ( 122.8585116216235065, -38.08382569396911776, 302.4856252759109907 ) ) ;
#68226 = LINE ( 'NONE', #89565, #32055 ) ;
#68227 = AXIS2_PLACEMENT_3D ( 'NONE', #56890, #64613, #84631 ) ;
#68228 = EDGE_CURVE ( 'NONE', #79315, #71373, #37527, .T. ) ;
#68229 = DIRECTION ( 'NONE',  ( 4.237773401492740281E-14, -1.000000000000000000, 0.000000000000000000 ) ) ;
#68230 = ORIENTED_EDGE ( 'NONE', *, *, #78051, .T. ) ;
#68231 = CARTESIAN_POINT ( 'NONE',  ( 116.3126599349420900, -33.43976754494801185, 110.0984824187669631 ) ) ;
#68232 = VECTOR ( 'NONE', #77679, 1000.000000000000000 ) ;
#68234 = ORIENTED_EDGE ( 'NONE', *, *, #69083, .F. ) ;
#68233 = CARTESIAN_POINT ( 'NONE',  ( 11.69661972370231773, 87.49773257406484106, 130.0309910664321649 ) ) ;
#68235 = CARTESIAN_POINT ( 'NONE',  ( 116.0363244534468237, -41.99923036749492411, 234.4041967044819899 ) ) ;
#68236 = DIRECTION ( 'NONE',  ( 0.000000000000000000, 1.000000000000000000, 0.000000000000000000 ) ) ;
#68237 = CARTESIAN_POINT ( 'NONE',  ( 112.0504773937687872, -45.40517505809263810, 147.9914262990938312 ) ) ;
#68238 = DIRECTION ( 'NONE',  ( 0.000000000000000000, 1.000000000000000000, 0.000000000000000000 ) ) ;
#68239 = B_SPLINE_CURVE_WITH_KNOTS ( 'NONE', 3,
 ( #947, #79052, #85438, #28644, #56334, #84080, #21852, #15027, #42701, #35907, #80840, #52188, #66740, #24084, #38146, #46272, #4070, #65412, #51755, #65839, #53070, #18589, #79951, #86753, #3622, #74006, #25404, #81297, #38580 ),
 .UNSPECIFIED., .F., .F.,
 ( 4, 2, 2, 2, 2, 2, 2, 2, 2, 2, 1, 1, 1, 1, 1, 2, 4 ),
 ( 0.000000000000000000, 0.06250187945002849688, 0.1250037589000569938, 0.1875056383500854906, 0.2500075178001139875, 0.3125093972501424844, 0.3750112767001709813, 0.4375131561501994781, 0.4687640958752137266, 0.4843895657377207953, 0.4922023006689741909, 0.4961086681346009719, 0.4980618518674143624, 0.4990384437338208912, 0.4995267396670242110, 0.4997708876336256489, 0.5000150356002270868 ),
 .UNSPECIFIED. ) ;
#68240 = CARTESIAN_POINT ( 'NONE',  ( 97.31584370783238569, -39.30597596754859779, 82.53145860666462852 ) ) ;
#68241 = DIRECTION ( 'NONE',  ( -1.387778780781444413E-14, -1.000000000000000000, 0.000000000000000000 ) ) ;
#68242 = CARTESIAN_POINT ( 'NONE',  ( -95.16559702356633466, 70.52006616879377532, 89.37861919290460833 ) ) ;
#68243 = AXIS2_PLACEMENT_3D ( 'NONE', #43603, #2297, #16370 ) ;
#68244 = CARTESIAN_POINT ( 'NONE',  ( 113.2097911582632861, -29.11871762112820150, 164.5356252759109736 ) ) ;
#68245 = ORIENTED_EDGE ( 'NONE', *, *, #64590, .F. ) ;
#68246 = ORIENTED_EDGE ( 'NONE', *, *, #49419, .F. ) ;
#68247 = CARTESIAN_POINT ( 'NONE',  ( 107.2938360571228600, -27.87074582556254398, 116.4872975916119771 ) ) ;
#68248 = FACE_BOUND ( 'NONE', #14213, .T. ) ;
#68250 = CARTESIAN_POINT ( 'NONE',  ( 12.70000000000000107, 82.54999999999999716, 117.8738102209307641 ) ) ;
#68249 = CARTESIAN_POINT ( 'NONE',  ( 104.4938967476557821, -26.68352342390111787, 241.2880062282909535 ) ) ;
#68251 = CARTESIAN_POINT ( 'NONE',  ( 97.81477617152367543, -40.51601309134415629, 21.63528831556280707 ) ) ;
#68252 = EDGE_CURVE ( 'NONE', #46739, #81819, #38396, .T. ) ;
#68253 = EDGE_CURVE ( 'NONE', #18676, #32980, #18400, .T. ) ;
#68254 = AXIS2_PLACEMENT_3D ( 'NONE', #39664, #74641, #38769 ) ;
#68255 = CARTESIAN_POINT ( 'NONE',  ( 144.4532657278588204, -72.54451140298851897, 540.9756252759101471 ) ) ;
#68256 = FACE_OUTER_BOUND ( 'NONE', #70640, .T. ) ;
#68257 = AXIS2_PLACEMENT_3D ( 'NONE', #20187, #60601, #74691 ) ;
#68258 = CARTESIAN_POINT ( 'NONE',  ( -3.174999999999644995, 124.5870000000000033, -33.98325472291465132 ) ) ;
#68259 = ADVANCED_FACE ( 'NONE', ( #45204 ), #41822, .F. ) ;
#68260 = FACE_OUTER_BOUND ( 'NONE', #63863, .T. ) ;
#68261 = CARTESIAN_POINT ( 'NONE',  ( 117.9098725419245000, -34.70837513311212064, 203.9851490854349549 ) ) ;
#68262 = DIRECTION ( 'NONE',  ( -1.000000000000000000, 0.000000000000000000, -9.974659986866630932E-16 ) ) ;
#68263 = ORIENTED_EDGE ( 'NONE', *, *, #54589, .F. ) ;
#68264 = ORIENTED_EDGE ( 'NONE', *, *, #63569, .T. ) ;
#68265 = ADVANCED_FACE ( 'NONE', ( #37960 ), #64781, .F. ) ;
#68266 = CARTESIAN_POINT ( 'NONE',  ( 140.9629299006806775, -8.979447159940995959, -5.074374724088994704 ) ) ;
#68267 = CARTESIAN_POINT ( 'NONE',  ( 78.94209639488890673, -16.21971364483396982, 1.822997995688476980 ) ) ;
#68268 = DIRECTION ( 'NONE',  ( -3.999999999999999995E-14, 1.000000000000000000, -4.100000000000000342E-29 ) ) ;
#68269 = DIRECTION ( 'NONE',  ( 0.000000000000000000, 1.000000000000000000, 0.000000000000000000 ) ) ;
#68270 = LINE ( 'NONE', #6052, #592 ) ;
#68271 = ORIENTED_EDGE ( 'NONE', *, *, #44176, .T. ) ;
#68272 = DIRECTION ( 'NONE',  ( 3.100000000000000258E-29, -3.100000000000000044E-14, -1.000000000000000000 ) ) ;
#68273 =( BOUNDED_CURVE ( )  B_SPLINE_CURVE ( 3, ( #13008, #60228, #74333, #82510 ),
 .UNSPECIFIED., .F., .F. ) 
 B_SPLINE_CURVE_WITH_KNOTS ( ( 4, 4 ),
 ( 6.752864695426161603E-13, 1.570796326796150222 ),
 .UNSPECIFIED. ) 
 CURVE ( )  GEOMETRIC_REPRESENTATION_ITEM ( )  RATIONAL_B_SPLINE_CURVE ( ( 1.000000000000000000, 0.8047378541242287131, 0.8047378541242287131, 1.000000000000000000 ) ) 
 REPRESENTATION_ITEM ( '' )  );
#68274 = CARTESIAN_POINT ( 'NONE',  ( 100.6375269748662760, -26.77409651225141474, 220.5327681330539633 ) ) ;
#68275 = VERTEX_POINT ( 'NONE', #66102 ) ;
#68276 = EDGE_CURVE ( 'NONE', #80932, #79375, #58399, .T. ) ;
#68277 = CARTESIAN_POINT ( 'NONE',  ( -11.30816021491739853, 88.12274986616640149, 118.0156291604116205 ) ) ;
#68278 = FACE_OUTER_BOUND ( 'NONE', #68099, .T. ) ;
#68279 = CARTESIAN_POINT ( 'NONE',  ( 41.56648329127499153, -36.32844715994070839, 138.9256252759119832 ) ) ;
#68280 = CARTESIAN_POINT ( 'NONE',  ( 114.6641587241874873, -32.58502278776634142, 22.02999513149600475 ) ) ;
#68281 = CARTESIAN_POINT ( 'NONE',  ( 98.64836624540230048, -30.48328824330908660, 176.8184824187679567 ) ) ;
#68282 = AXIS2_PLACEMENT_3D ( 'NONE', #30465, #44072, #51328 ) ;
#68283 = CARTESIAN_POINT ( 'NONE',  ( 59.56670390244700997, -79.67844715994098692, 120.2178068554179902 ) ) ;
#68284 = VERTEX_POINT ( 'NONE', #31583 ) ;
#68285 = DIRECTION ( 'NONE',  ( 0.000000000000000000, -1.000000000000000000, 0.000000000000000000 ) ) ;
#68286 = CARTESIAN_POINT ( 'NONE',  ( 80.06648329127398256, -15.97944715994105813, 8.225625275910942946 ) ) ;
#68287 = ORIENTED_EDGE ( 'NONE', *, *, #24475, .F. ) ;
#68289 = ORIENTED_EDGE ( 'NONE', *, *, #20921, .T. ) ;
#68288 = VECTOR ( 'NONE', #30891, 1000.000000000000000 ) ;
#68290 = CARTESIAN_POINT ( 'NONE',  ( 9.549789689180780528, 90.93251752167836344, 118.1710524764279029 ) ) ;
#68291 = ORIENTED_EDGE ( 'NONE', *, *, #76638, .T. ) ;
#68292 = ORIENTED_EDGE ( 'NONE', *, *, #6562, .T. ) ;
#68293 = DIRECTION ( 'NONE',  ( 0.000000000000000000, 0.000000000000000000, 1.000000000000000000 ) ) ;
#68294 = CARTESIAN_POINT ( 'NONE',  ( 116.0152812585483275, -38.11929796734737863, 68.11432458998100969 ) ) ;
#68295 = CARTESIAN_POINT ( 'NONE',  ( 115.7947005615567235, -30.98796762508558444, 254.2899109901966028 ) ) ;
#68296 = CARTESIAN_POINT ( 'NONE',  ( 96.16101635903902434, -35.07578045570937775, 221.1946728949589840 ) ) ;
#68298 = CARTESIAN_POINT ( 'NONE',  ( 100.6111884388667335, -28.52632756463412633, 11.60705384733995515 ) ) ;
#68297 = CARTESIAN_POINT ( 'NONE',  ( 5.210259806972410633E-15, 127.0000000000000000, -42.54500000000000171 ) ) ;
#68299 = CARTESIAN_POINT ( 'NONE',  ( 80.06648329127399677, -21.47944715994105991, 1.625625275910943746 ) ) ;
#68300 = CYLINDRICAL_SURFACE ( 'NONE', #3316, 2.116999999999993776 ) ;
#68301 = ORIENTED_EDGE ( 'NONE', *, *, #81837, .F. ) ;
#68302 = CARTESIAN_POINT ( 'NONE',  ( 117.0169231590003562, -33.47438763928646210, 89.07848241876791917 ) ) ;
#68303 = CARTESIAN_POINT ( 'NONE',  ( 96.71965009938165281, -35.13266635363193302, 266.2041967044820581 ) ) ;
#68304 = EDGE_LOOP ( 'NONE', ( #20680, #33741, #68412, #75888, #47478 ) ) ;
#68305 = CARTESIAN_POINT ( 'NONE',  ( 97.76227787611212250, -41.51041654567812600, 196.7041967044819728 ) ) ;
#68306 = FACE_OUTER_BOUND ( 'NONE', #22775, .T. ) ;
#68307 = DIRECTION ( 'NONE',  ( 1.000000000000000000, 0.000000000000000000, 0.000000000000000000 ) ) ;
#68308 = EDGE_CURVE ( 'NONE', #38663, #1545, #8473, .T. ) ;
#68309 = CARTESIAN_POINT ( 'NONE',  ( 97.81930832768965445, -40.53599170015394293, 22.63722267858115345 ) ) ;
#68310 = CARTESIAN_POINT ( 'NONE',  ( 106.1976517883881144, -46.78020009823125491, 28.50853215074594260 ) ) ;
#68312 = DIRECTION ( 'NONE',  ( 0.000000000000000000, 0.000000000000000000, 1.000000000000000000 ) ) ;
#68311 = CARTESIAN_POINT ( 'NONE',  ( 101.6180013298386768, -30.49747046846794518, 277.6356252759111385 ) ) ;
#68313 = LINE ( 'NONE', #26978, #3210 ) ;
#68314 = LINE ( 'NONE', #33786, #35200 ) ;
#68315 = CIRCLE ( 'NONE', #59591, 16.00000000000000000 ) ;
#68316 = DIRECTION ( 'NONE',  ( 0.000000000000000000, -1.000000000000000000, 0.000000000000000000 ) ) ;
#68317 = CIRCLE ( 'NONE', #7428, 0.3000000000000016542 ) ;
#68318 = CARTESIAN_POINT ( 'NONE',  ( 51.06648329127400388, -18.82844715994099971, 333.4006252759120343 ) ) ;
#68319 = DIRECTION ( 'NONE',  ( 1.000000000000000000, -5.337610695313248426E-16, 0.000000000000000000 ) ) ;
#68320 = VECTOR ( 'NONE', #52423, 1000.000000000000000 ) ;
#68321 = FACE_OUTER_BOUND ( 'NONE', #24367, .T. ) ;
#68323 = ORIENTED_EDGE ( 'NONE', *, *, #17087, .T. ) ;
#68322 = CARTESIAN_POINT ( 'NONE',  ( -4.868064396069518907, 94.30179516618007085, -118.4578665249601386 ) ) ;
#68324 = CARTESIAN_POINT ( 'NONE',  ( 138.8167039024479834, -67.87844715994100397, 88.43480685541499042 ) ) ;
#68325 = CARTESIAN_POINT ( 'NONE',  ( 105.1067973254952790, -26.46757623491196298, 235.2270538473399313 ) ) ;
#68326 = CARTESIAN_POINT ( 'NONE',  ( 108.5897967589408495, -47.07840195076833112, 138.6927681330539883 ) ) ;
#68327 = CARTESIAN_POINT ( 'NONE',  ( 103.0738860297313266, -47.93972279484852095, 248.3041967044829619 ) ) ;
#68328 = CARTESIAN_POINT ( 'NONE',  ( 0.000000000000000000, 101.5999999999999943, 89.89999999999997726 ) ) ;
#68329 = CARTESIAN_POINT ( 'NONE',  ( -254.0000000000000000, 3.174999999999999822, 142.8750000000000000 ) ) ;
#68330 = VECTOR ( 'NONE', #3295, 1000.000000000000000 ) ;
#68332 = LINE ( 'NONE', #68779, #42866 ) ;
#68331 = LINE ( 'NONE', #81974, #56529 ) ;
#68333 = LINE ( 'NONE', #82873, #3025 ) ;
#68334 = CYLINDRICAL_SURFACE ( 'NONE', #76112, 3.499999999999996003 ) ;
#68335 = CIRCLE ( 'NONE', #63996, 2.500000000000002220 ) ;
#68336 = EDGE_CURVE ( 'NONE', #54616, #64730, #2695, .T. ) ;
#68337 = ORIENTED_EDGE ( 'NONE', *, *, #86023, .T. ) ;
#68338 = ORIENTED_EDGE ( 'NONE', *, *, #17380, .F. ) ;
#68339 = CARTESIAN_POINT ( 'NONE',  ( 111.9909297607753160, -29.75048171432638355, 129.0095626852189525 ) ) ;
#68341 = ORIENTED_EDGE ( 'NONE', *, *, #86919, .T. ) ;
#68340 = CARTESIAN_POINT ( 'NONE',  ( 0.000000000000000000, 223.9999999999999716, 154.6557476874258441 ) ) ;
#68342 = CARTESIAN_POINT ( 'NONE',  ( 152.0368932755770857, -23.42844715993588522, 249.9678068554149490 ) ) ;
#68343 = CARTESIAN_POINT ( 'NONE',  ( 103.2134869792596135, -46.43093390711685231, 113.2756252759109827 ) ) ;
#68344 = CARTESIAN_POINT ( 'NONE',  ( 108.3313360409339907, -46.73509903638382923, 148.6777836749537585 ) ) ;
#68345 = DIRECTION ( 'NONE',  ( 1.639958061481212836E-42, -4.100000000000000342E-29, -1.000000000000000000 ) ) ;
#68346 = PRODUCT_DEFINITION ( 'UNKNOWN', '', #84135, #2404 ) ;
#68347 = AXIS2_PLACEMENT_3D ( 'NONE', #39303, #4791, #32032 ) ;
#68348 = DIRECTION ( 'NONE',  ( -0.0001713722456120069274, 0.9999999853157766072, 0.000000000000000000 ) ) ;
#68349 = CARTESIAN_POINT ( 'NONE',  ( 61.00843881761244347, 49.07499999999999574, -33.74458626278666884 ) ) ;
#68350 = CARTESIAN_POINT ( 'NONE',  ( 117.2535196871930481, -41.18324016912744412, 58.49848241876892985 ) ) ;
#68351 = ORIENTED_EDGE ( 'NONE', *, *, #21319, .T. ) ;
#68352 = ORIENTED_EDGE ( 'NONE', *, *, #53550, .T. ) ;
#68354 = ORIENTED_EDGE ( 'NONE', *, *, #12257, .F. ) ;
#68353 = AXIS2_PLACEMENT_3D ( 'NONE', #83512, #28082, #68987 ) ;
#68355 = PLANE ( 'NONE',  #23955 ) ;
#68357 = LINE ( 'NONE', #46544, #86788 ) ;
#68356 = CARTESIAN_POINT ( 'NONE',  ( 108.4956486572523602, -46.43878675094416764, 138.6927681330529936 ) ) ;
#68358 = CARTESIAN_POINT ( 'NONE',  ( 88.06670390244791236, -14.72944715994105991, 239.5838068554169809 ) ) ;
#68359 = DIRECTION ( 'NONE',  ( 0.000000000000000000, 1.000000000000000000, 0.000000000000000000 ) ) ;
#68360 = EDGE_CURVE ( 'NONE', #29833, #74616, #38919, .T. ) ;
#68361 = AXIS2_PLACEMENT_3D ( 'NONE', #42696, #36361, #29545 ) ;
#68362 = FACE_OUTER_BOUND ( 'NONE', #85281, .T. ) ;
#68363 = CARTESIAN_POINT ( 'NONE',  ( 84.99816483510821286, 95.16897323824359489, 82.65294504194773140 ) ) ;
#68364 = EDGE_CURVE ( 'NONE', #32750, #40462, #9820, .T. ) ;
#68365 = FACE_OUTER_BOUND ( 'NONE', #12653, .T. ) ;
#68366 = CARTESIAN_POINT ( 'NONE',  ( 96.81317962367440089, -38.48968277746988065, 91.46133956162493917 ) ) ;
#68367 = ORIENTED_EDGE ( 'NONE', *, *, #57899, .F. ) ;
#68368 = EDGE_CURVE ( 'NONE', #89731, #37957, #9372, .T. ) ;
#68369 = VERTEX_POINT ( 'NONE', #17079 ) ;
#68370 = AXIS2_PLACEMENT_3D ( 'NONE', #72560, #45272, #58024 ) ;
#68371 = ORIENTED_EDGE ( 'NONE', *, *, #61295, .T. ) ;
#68372 = EDGE_CURVE ( 'NONE', #28990, #41770, #80654, .T. ) ;
#68373 = DIRECTION ( 'NONE',  ( -1.000000000000000000, -4.299999999999999979E-14, -1.000000000000000078E-15 ) ) ;
#68374 = DIRECTION ( 'NONE',  ( 0.000000000000000000, 1.000000000000000000, 0.000000000000000000 ) ) ;
#68375 = CARTESIAN_POINT ( 'NONE',  ( -487.2989999999999782, 10.16305401447645984, 83.34375000000000000 ) ) ;
#68376 = CARTESIAN_POINT ( 'NONE',  ( 101.5399107887468944, -29.27606352979315574, 183.4023760838769590 ) ) ;
#68377 = DIRECTION ( 'NONE',  ( 0.000000000000000000, 0.000000000000000000, -1.000000000000000000 ) ) ;
#68378 = ORIENTED_EDGE ( 'NONE', *, *, #58519, .F. ) ;
#68380 = VERTEX_POINT ( 'NONE', #44315 ) ;
#68379 = ORIENTED_EDGE ( 'NONE', *, *, #71881, .F. ) ;
#68381 = EDGE_CURVE ( 'NONE', #76536, #37688, #59206, .T. ) ;
#68382 = CARTESIAN_POINT ( 'NONE',  ( 150.5667039024482960, -47.82844715993594775, 300.4678068554149490 ) ) ;
#68383 = AXIS2_PLACEMENT_3D ( 'NONE', #6219, #69338, #40271 ) ;
#68384 = CARTESIAN_POINT ( 'NONE',  ( 134.8178559631273856, -21.40256188477526678, 1.690787648081120143 ) ) ;
#68385 = ORIENTED_EDGE ( 'NONE', *, *, #70949, .F. ) ;
#68386 = ORIENTED_EDGE ( 'NONE', *, *, #57159, .F. ) ;
#68387 = EDGE_CURVE ( 'NONE', #32579, #18726, #59727, .T. ) ;
#68388 = DIRECTION ( 'NONE',  ( 0.8660254037844311581, -0.5000000000000132117, 0.000000000000000000 ) ) ;
#68389 = CARTESIAN_POINT ( 'NONE',  ( 99.39098736499681763, -43.25305561222647555, 223.3187261630399689 ) ) ;
#68390 = CIRCLE ( 'NONE', #78597, 2.500000000000002220 ) ;
#68391 = LINE ( 'NONE', #52910, #83521 ) ;
#68392 = CARTESIAN_POINT ( 'NONE',  ( -125.0340203103765759, 69.82055466749729078, 37.56983117113036030 ) ) ;
#68393 = ORIENTED_EDGE ( 'NONE', *, *, #77579, .F. ) ;
#68394 = ORIENTED_EDGE ( 'NONE', *, *, #88171, .F. ) ;
#68395 = AXIS2_PLACEMENT_3D ( 'NONE', #20365, #41667, #62579 ) ;
#68396 = DIRECTION ( 'NONE',  ( -0.7071067811866258435, 0.7071067811864693020, -7.071067811866266166E-16 ) ) ;
#68397 = ORIENTED_EDGE ( 'NONE', *, *, #59147, .T. ) ;
#68398 = EDGE_LOOP ( 'NONE', ( #83045, #8397 ) ) ;
#68399 = CARTESIAN_POINT ( 'NONE',  ( 103.9533468823514823, -45.47040322110986210, 250.1223760838773273 ) ) ;
#68400 = CARTESIAN_POINT ( 'NONE',  ( 99.40582560697848180, -27.65448416857716651, 150.6356252759109680 ) ) ;
#68401 = CARTESIAN_POINT ( 'NONE',  ( 116.9541756933415257, -33.49491404195858735, 89.07848241876791917 ) ) ;
#68402 = CARTESIAN_POINT ( 'NONE',  ( 99.19001052970209287, -35.07347417754516528, 249.5838068554172935 ) ) ;
#68403 = B_SPLINE_SURFACE_WITH_KNOTS ( 'NONE', 1, 1, ( 
 ( #31452, #17395 ),
 ( #23343, #85566 ) ),
 .UNSPECIFIED., .F., .F., .F.,
 ( 2, 2 ),
 ( 2, 2 ),
 ( 0.000000000000000000, 1.000000000000000000 ),
 ( 0.000000000000000000, 1.000000000000000000 ),
 .UNSPECIFIED. ) ;
#68404 = CARTESIAN_POINT ( 'NONE',  ( 107.0664832912739968, -36.72944715994100306, 195.5838068554169809 ) ) ;
#68405 = LINE ( 'NONE', #35542, #53266 ) ;
#68406 = CARTESIAN_POINT ( 'NONE',  ( 98.37977233551227130, -29.89460749427659181, 196.8080062282919869 ) ) ;
#68407 = DIRECTION ( 'NONE',  ( -1.000000000000000000, 0.000000000000000000, 0.000000000000000000 ) ) ;
#68408 = ORIENTED_EDGE ( 'NONE', *, *, #87532, .T. ) ;
#68409 = CARTESIAN_POINT ( 'NONE',  ( 130.5560612649026950, 69.84937019662270075, -0.8297548318604713868 ) ) ;
#68410 = VERTEX_POINT ( 'NONE', #57955 ) ;
#68411 = CIRCLE ( 'NONE', #19122, 2.517500000000005844 ) ;
#68412 = ORIENTED_EDGE ( 'NONE', *, *, #619, .T. ) ;
#68413 = LINE ( 'NONE', #87510, #82277 ) ;
#68414 = EDGE_LOOP ( 'NONE', ( #56421, #10793, #11639, #57041, #86941 ) ) ;
#68415 = EDGE_CURVE ( 'NONE', #7688, #72189, #16634, .T. ) ;
#68416 = AXIS2_PLACEMENT_3D ( 'NONE', #3965, #11219, #38924 ) ;
#68417 = DIRECTION ( 'NONE',  ( 0.000000000000000000, -1.000000000000000000, 0.000000000000000000 ) ) ;
#68418 = CARTESIAN_POINT ( 'NONE',  ( 116.9219696586192754, -33.22298239640010564, 114.0984824187679720 ) ) ;
#68419 = CARTESIAN_POINT ( 'NONE',  ( -6.727371441648950956, 71.77714599857043254, 130.3826064408659704 ) ) ;
#68420 = EDGE_CURVE ( 'NONE', #89067, #46473, #4788, .T. ) ;
#68421 = LINE ( 'NONE', #47046, #13074 ) ;
#68422 = CARTESIAN_POINT ( 'NONE',  ( 130.5667039024480118, -36.72944715994093912, 229.5838068554170093 ) ) ;
#68425 = CARTESIAN_POINT ( 'NONE',  ( 116.5068947302721369, -41.18400185692900806, 224.4756252759109714 ) ) ;
#68424 = CARTESIAN_POINT ( 'NONE',  ( 116.3167039024470029, -67.87844715994093292, 55.21780685541800437 ) ) ;
#68423 = DIRECTION ( 'NONE',  ( -4.237773401492740281E-14, 1.000000000000000000, 0.000000000000000000 ) ) ;
#68426 = CARTESIAN_POINT ( 'NONE',  ( 0.000000000000000000, 124.5870000000000033, 0.000000000000000000 ) ) ;
#68427 = CARTESIAN_POINT ( 'NONE',  ( 151.0371591254575208, -24.42818131005592264, 180.4678068554149775 ) ) ;
#68428 = ORIENTED_EDGE ( 'NONE', *, *, #17855, .T. ) ;
#68429 = AXIS2_PLACEMENT_3D ( 'NONE', #53518, #39913, #67630 ) ;
#68430 = DIRECTION ( 'NONE',  ( 0.000000000000000000, 1.000000000000000000, 0.000000000000000000 ) ) ;
#68431 = PLANE ( 'NONE',  #12323 ) ;
#68432 = DIRECTION ( 'NONE',  ( 1.000000000000000078E-15, 1.000000000000000083E-30, -1.000000000000000000 ) ) ;
#68433 = VECTOR ( 'NONE', #12113, 1000.000000000000000 ) ;
#68434 = CARTESIAN_POINT ( 'NONE',  ( 194.0667039024473297, -24.92844715993408045, 300.4678068554149490 ) ) ;
#68436 = VERTEX_POINT ( 'NONE', #27457 ) ;
#68435 = CARTESIAN_POINT ( 'NONE',  ( 104.8318391505165010, -26.46503486849124087, 260.2470538473397710 ) ) ;
#68437 = FACE_OUTER_BOUND ( 'NONE', #5887, .T. ) ;
#68438 = CARTESIAN_POINT ( 'NONE',  ( 111.4896171341011666, -26.57472070863446589, 280.7375300378156453 ) ) ;
#68439 = CARTESIAN_POINT ( 'NONE',  ( 102.0300696065151982, -46.62045497284175610, 168.2137205140059564 ) ) ;
#68440 = CARTESIAN_POINT ( 'NONE',  ( 97.31584378032250982, -39.30597624822549108, 32.53145862952089118 ) ) ;
#68441 = DIRECTION ( 'NONE',  ( -1.000000000000000000, 0.000000000000000000, 0.000000000000000000 ) ) ;
#68443 = DIRECTION ( 'NONE',  ( 1.000000000000000000, 1.000000000000000078E-15, 0.000000000000000000 ) ) ;
#68442 = FACE_OUTER_BOUND ( 'NONE', #30760, .T. ) ;
#68444 = CARTESIAN_POINT ( 'NONE',  ( 99.09570912936477782, -30.55043168559838307, 190.8022919357809997 ) ) ;
#68445 = CARTESIAN_POINT ( 'NONE',  ( 116.3212776292296127, -32.94146857471318413, 287.6356252759109680 ) ) ;
#68446 = VERTEX_POINT ( 'NONE', #87905 ) ;
#68447 = EDGE_CURVE ( 'NONE', #28440, #64498, #65060, .T. ) ;
#68448 = ORIENTED_EDGE ( 'NONE', *, *, #70336, .T. ) ;
#68449 = ORIENTED_EDGE ( 'NONE', *, *, #30428, .F. ) ;
#68450 = VECTOR ( 'NONE', #74805, 1000.000000000000000 ) ;
#68451 = ORIENTED_EDGE ( 'NONE', *, *, #15902, .F. ) ;
#68452 = CARTESIAN_POINT ( 'NONE',  ( -126.9619601814429046, 50.67986003389061267, 30.42261724897560882 ) ) ;
#68453 = CARTESIAN_POINT ( 'NONE',  ( 118.1852327621006538, -40.75705396371408540, 19.54991099019698453 ) ) ;
#68454 = CARTESIAN_POINT ( 'NONE',  ( 87.68258360185966183, -140.6784122025596560, 246.0580355273719988 ) ) ;
#68455 = CARTESIAN_POINT ( 'NONE',  ( 51.06670390244671154, -32.29483332968568021, 193.9678068554150911 ) ) ;
#68456 = ADVANCED_FACE ( 'NONE', ( #12951 ), #60626, .F. ) ;
#68457 = CARTESIAN_POINT ( 'NONE',  ( 183.5150000000000148, 14.63749999999999929, -14.28749999999999964 ) ) ;
#68458 = CIRCLE ( 'NONE', #82997, 2.000000000000007550 ) ;
#68459 = CARTESIAN_POINT ( 'NONE',  ( 98.95796485450003388, -39.41423029504880304, 241.0038483995049603 ) ) ;
#68460 = ORIENTED_EDGE ( 'NONE', *, *, #3953, .F. ) ;
#68461 = VERTEX_POINT ( 'NONE', #19311 ) ;
#68462 = EDGE_LOOP ( 'NONE', ( #86557, #44814, #40736, #57878 ) ) ;
#68463 = CONICAL_SURFACE ( 'NONE', #22055, 7.249999999999998224, 0.7853981633974772558 ) ;
#68464 = FACE_BOUND ( 'NONE', #37489, .T. ) ;
#68466 = EDGE_CURVE ( 'NONE', #54909, #75220, #20069, .T. ) ;
#68465 = CARTESIAN_POINT ( 'NONE',  ( 97.87459229980032660, -40.66846143049065887, 101.6490831034139433 ) ) ;
#68467 = CARTESIAN_POINT ( 'NONE',  ( 151.0371591254575492, -24.95799193692592155, 180.4678068554149775 ) ) ;
#68468 = CARTESIAN_POINT ( 'NONE',  ( 0.000000000000000000, 61.59999999999999432, 118.5560000000000116 ) ) ;
#68469 = CARTESIAN_POINT ( 'NONE',  ( -72.96458098368751166, 127.0000000000000000, 72.96458098368620426 ) ) ;
#68470 = CARTESIAN_POINT ( 'NONE',  ( 3.968750000000050182, 120.6499999999999915, -100.8961411191535973 ) ) ;
#68471 = CARTESIAN_POINT ( 'NONE',  ( 115.1619974903381518, -42.21817061296157192, 273.3527681330542691 ) ) ;
#68472 = EDGE_CURVE ( 'NONE', #8309, #81558, #67446, .T. ) ;
#68473 = DIRECTION ( 'NONE',  ( 0.000000000000000000, 0.000000000000000000, 1.000000000000000000 ) ) ;
#68475 = ORIENTED_EDGE ( 'NONE', *, *, #23258, .F. ) ;
#68474 = CIRCLE ( 'NONE', #4664, 34.13125000000000142 ) ;
#68476 = CARTESIAN_POINT ( 'NONE',  ( 36.23715912545339535, -47.82818131006131779, 180.4678068554150911 ) ) ;
#68477 = CARTESIAN_POINT ( 'NONE',  ( 132.1248447323112316, -104.2784471599408818, 17.71780685541799016 ) ) ;
#68478 = CARTESIAN_POINT ( 'NONE',  ( 99.67188489287487130, -33.20771423803368094, 73.79094751244896599 ) ) ;
#68479 = AXIS2_PLACEMENT_3D ( 'NONE', #50329, #16279, #83986 ) ;
#68480 = AXIS2_PLACEMENT_3D ( 'NONE', #53952, #5391, #18563 ) ;
#68481 = CARTESIAN_POINT ( 'NONE',  ( 116.3212776292293995, -32.94146857471265122, 80.13562527591095375 ) ) ;
#68482 = DIRECTION ( 'NONE',  ( -1.000000000000000000, 0.000000000000000000, 0.000000000000000000 ) ) ;
#68483 = VECTOR ( 'NONE', #73437, 1000.000000000000114 ) ;
#68484 = CARTESIAN_POINT ( 'NONE',  ( 98.34985891086999743, -31.65658481233683830, 45.90645860949901191 ) ) ;
#68485 = ORIENTED_EDGE ( 'NONE', *, *, #5605, .T. ) ;
#68486 = EDGE_CURVE ( 'NONE', #60056, #75262, #40346, .T. ) ;
#68487 = CARTESIAN_POINT ( 'NONE',  ( 79.18623681049682261, -34.12360705087682078, 8.106403045242537075 ) ) ;
#68488 = EDGE_LOOP ( 'NONE', ( #21468, #66787, #88638, #17610 ) ) ;
#68489 = CARTESIAN_POINT ( 'NONE',  ( 102.3930168087890422, -26.71257147495026274, 135.4118157521009493 ) ) ;
#68490 = ORIENTED_EDGE ( 'NONE', *, *, #18826, .F. ) ;
#68491 = EDGE_CURVE ( 'NONE', #66245, #54835, #68357, .T. ) ;
#68492 = VECTOR ( 'NONE', #4299, 1000.000000000000000 ) ;
#68493 = EDGE_CURVE ( 'NONE', #49775, #74329, #5691, .T. ) ;
#68494 = CARTESIAN_POINT ( 'NONE',  ( 101.9936209862019467, -45.44607156465968245, 68.15645861336898292 ) ) ;
#68495 = CARTESIAN_POINT ( 'NONE',  ( 115.8195149170444296, -38.11245691049232676, 110.1330118773259699 ) ) ;
#68496 = CARTESIAN_POINT ( 'NONE',  ( -4.090931056105388208, 94.60184303864161848, 118.4878965444427763 ) ) ;
#68497 = EDGE_CURVE ( 'NONE', #30248, #39757, #82000, .T. ) ;
#68498 = CARTESIAN_POINT ( 'NONE',  ( 184.5667039024480118, -48.82844715994099971, 10.91780685541479734 ) ) ;
#68499 = CARTESIAN_POINT ( 'NONE',  ( 103.8345913547307333, -46.70111052772084292, 78.32705384733995402 ) ) ;
#68500 = FACE_OUTER_BOUND ( 'NONE', #70842, .T. ) ;
#68501 = VERTEX_POINT ( 'NONE', #53344 ) ;
#68502 = CARTESIAN_POINT ( 'NONE',  ( 110.2536356736639220, -106.6957733451320394, 2.217806855418086087 ) ) ;
#68503 = EDGE_LOOP ( 'NONE', ( #24004, #66239 ) ) ;
#68504 = ORIENTED_EDGE ( 'NONE', *, *, #71708, .T. ) ;
#68505 = B_SPLINE_CURVE_WITH_KNOTS ( 'NONE', 3,
 ( #6869, #63179, #49980, #54984, #29115, #48625, #34117, #84090, #15497, #83637, #35013, #504, #49532, #76365, #42712, #957, #82754, #34570, #61820, #89552, #70454, #28197, #84547, #69552, #35916, #1416, #70000, #28656, #49079, #77719, #63630, #76812, #20517, #14138, #43168, #75916, #13684, #41816, #41374, #25749, #87992, #53426, #80733, #59369, #17167, #79403, #86652, #81194 ),
 .UNSPECIFIED., .F., .F.,
 ( 4, 2, 2, 2, 2, 2, 2, 2, 2, 1, 2, 2, 2, 2, 2, 2, 2, 2, 2, 2, 2, 1, 2, 2, 4 ),
 ( 0.05959919981814691681, 0.06208168506169069872, 0.06332292768346259315, 0.06456417030523449452, 0.06704665554877822786, 0.06828789817055011535, 0.06952914079232200284, 0.07201162603586573618, 0.07325286865763760979, 0.07449411127940946953, 0.07573535390118135702, 0.07697659652295323063, 0.07945908176649693622, 0.08194156701004066956, 0.08318280963181254317, 0.08442405225358443066, 0.08690653749712810849, 0.08814778011889994047, 0.08938902274067177245, 0.09187150798421545028, 0.09311275060598728226, 0.09435399322775911424, 0.09559523584953094621, 0.09683647847130277819, 0.09931896371484644215 ),
 .UNSPECIFIED. ) ;
#68506 = CARTESIAN_POINT ( 'NONE',  ( 52.38749999999999574, 94.53880000000000905, 225.4249999999999829 ) ) ;
#68507 = ORIENTED_EDGE ( 'NONE', *, *, #69862, .T. ) ;
#68508 = CARTESIAN_POINT ( 'NONE',  ( 97.40014589274343848, -35.23768424668791965, 266.2041967044829676 ) ) ;
#68509 = CARTESIAN_POINT ( 'NONE',  ( 108.6520215831686329, -25.77392822130451577, 145.9737205140069420 ) ) ;
#68510 = DIRECTION ( 'NONE',  ( 0.000000000000000000, 0.000000000000000000, 1.000000000000000000 ) ) ;
#68511 = CARTESIAN_POINT ( 'NONE',  ( 97.81169461453751524, -40.51741999607308742, 142.6356648221729131 ) ) ;
#68512 = CARTESIAN_POINT ( 'NONE',  ( 118.8426969166518319, -35.40452897077508965, 79.91562527591095488 ) ) ;
#68513 = LINE ( 'NONE', #61675, #77061 ) ;
#68514 = ORIENTED_EDGE ( 'NONE', *, *, #86349, .T. ) ;
#68515 = LINE ( 'NONE', #12206, #20763 ) ;
#68516 = LINE ( 'NONE', #61679, #53433 ) ;
#68517 = AXIS2_PLACEMENT_3D ( 'NONE', #29795, #76602, #85228 ) ;
#68518 = ORIENTED_EDGE ( 'NONE', *, *, #28084, .T. ) ;
#68519 = VECTOR ( 'NONE', #6160, 1000.000000000000000 ) ;
#68520 = DIRECTION ( 'NONE',  ( 9.032638163712999905E-13, -1.000000000000000000, 1.217258424823508649E-28 ) ) ;
#68521 = DIRECTION ( 'NONE',  ( 0.000000000000000000, 0.000000000000000000, 1.000000000000000000 ) ) ;
#68522 = CARTESIAN_POINT ( 'NONE',  ( 102.3890460933095170, -47.58756240099349100, 287.2527681330536780 ) ) ;
#68523 = DIRECTION ( 'NONE',  ( 1.000000000000000000, 0.000000000000000000, 0.000000000000000000 ) ) ;
#68524 = EDGE_CURVE ( 'NONE', #78468, #22617, #82897, .T. ) ;
#68525 = LINE ( 'NONE', #21267, #2777 ) ;
#68526 = CARTESIAN_POINT ( 'NONE',  ( 51.23005224011683367, -33.89581943344270343, 117.4678068554150485 ) ) ;
#68527 = CARTESIAN_POINT ( 'NONE',  ( 110.0852322082900372, -46.03269033891531592, 12.82705384733995402 ) ) ;
#68529 = CARTESIAN_POINT ( 'NONE',  ( 109.5033840998383994, -46.84330794493973826, 128.7641967044819751 ) ) ;
#68528 = CARTESIAN_POINT ( 'NONE',  ( 107.2382243570020961, -26.63832244206171751, 100.0631150270457255 ) ) ;
#68530 = LINE ( 'NONE', #6298, #61093 ) ;
#68531 = CARTESIAN_POINT ( 'NONE',  ( 112.5090891374639313, -26.14611880238131647, 169.6984824187679521 ) ) ;
#68532 = CARTESIAN_POINT ( 'NONE',  ( -446.0240000000000009, 104.7749999999999915, 101.5999999999999943 ) ) ;
#68533 = ORIENTED_EDGE ( 'NONE', *, *, #49469, .T. ) ;
#68534 = CYLINDRICAL_SURFACE ( 'NONE', #49724, 9.999999999999998224 ) ;
#68535 = DIRECTION ( 'NONE',  ( 1.000000000000000078E-15, 1.000000000000000083E-30, -1.000000000000000000 ) ) ;
#68536 = DIRECTION ( 'NONE',  ( -0.7071067811607679721, 0.7071067812123270624, 0.000000000000000000 ) ) ;
#68537 = ORIENTED_EDGE ( 'NONE', *, *, #1089, .T. ) ;
#68538 = VECTOR ( 'NONE', #4243, 1000.000000000000000 ) ;
#68539 = CARTESIAN_POINT ( 'NONE',  ( -462.0260000000000105, 53.97500000000000142, -2.412999999999919876 ) ) ;
#68541 = VERTEX_POINT ( 'NONE', #39301 ) ;
#68540 = CARTESIAN_POINT ( 'NONE',  ( 117.2652295300992193, -42.86250289712283745, 128.3956252759109873 ) ) ;
#68542 = FACE_OUTER_BOUND ( 'NONE', #61489, .T. ) ;
#68543 = CARTESIAN_POINT ( 'NONE',  ( -129.9761744276715092, 85.85000629251466364, -12.29186252049120931 ) ) ;
#68544 = CARTESIAN_POINT ( 'NONE',  ( 100.8961411191535973, 120.6499999999999915, 3.968750000000400124 ) ) ;
#68545 = CARTESIAN_POINT ( 'NONE',  ( 94.12733899296569007, -42.07533762155324553, 293.1356252759106837 ) ) ;
#68546 = ORIENTED_EDGE ( 'NONE', *, *, #44096, .T. ) ;
#68547 = AXIS2_PLACEMENT_3D ( 'NONE', #32867, #81053, #32408 ) ;
#68548 = EDGE_CURVE ( 'NONE', #40328, #65691, #46164, .T. ) ;
#68549 = CONTEXT_DEPENDENT_SHAPE_REPRESENTATION ( #23658, #45964 ) ;
#68550 = EDGE_CURVE ( 'NONE', #77621, #86161, #67901, .T. ) ;
#68551 = VERTEX_POINT ( 'NONE', #88812 ) ;
#68552 = ORIENTED_EDGE ( 'NONE', *, *, #50743, .F. ) ;
#68553 = AXIS2_PLACEMENT_3D ( 'NONE', #7873, #35569, #56910 ) ;
#68554 = ADVANCED_FACE ( 'NONE', ( #39736, #32471 ), #34269, .T. ) ;
#68555 = ORIENTED_EDGE ( 'NONE', *, *, #46931, .F. ) ;
#68556 = CARTESIAN_POINT ( 'NONE',  ( 103.1875000000000000, 117.4749999999999943, 5.041900000000359761 ) ) ;
#68557 = CARTESIAN_POINT ( 'NONE',  ( 83.15057989155033624, 85.43248893795414745, -100.6521573293560294 ) ) ;
#68558 = CARTESIAN_POINT ( 'NONE',  ( -487.2989999999999782, 93.66249999999999432, 98.73639197104678544 ) ) ;
#68559 = CARTESIAN_POINT ( 'NONE',  ( 13.40680633928208465, 223.9999999999999716, 102.7987842159323151 ) ) ;
#68560 = EDGE_CURVE ( 'NONE', #17136, #15221, #25895, .T. ) ;
#68561 = EDGE_CURVE ( 'NONE', #25149, #5538, #5549, .T. ) ;
#68563 = CARTESIAN_POINT ( 'NONE',  ( -5.627926923415666138, 71.15750911566317427, -118.4229113093306438 ) ) ;
#68562 = CARTESIAN_POINT ( 'NONE',  ( 193.0371591254575208, -23.42818131005411786, 129.9678068554150343 ) ) ;
#68564 = CARTESIAN_POINT ( 'NONE',  ( 97.53192512710711526, -39.74921111115579464, 181.5705521802071871 ) ) ;
#68565 = ORIENTED_EDGE ( 'NONE', *, *, #84883, .T. ) ;
#68566 = EDGE_CURVE ( 'NONE', #10240, #81584, #88290, .T. ) ;
#68567 = EDGE_CURVE ( 'NONE', #67053, #67104, #47409, .T. ) ;
#68568 = VERTEX_POINT ( 'NONE', #42415 ) ;
#68569 = CARTESIAN_POINT ( 'NONE',  ( -7.661254700127833495, 82.54999999999999716, 317.6630000000000109 ) ) ;
#68571 = EDGE_CURVE ( 'NONE', #14287, #68627, #42861, .T. ) ;
#68570 = FACE_BOUND ( 'NONE', #67459, .T. ) ;
#68572 = CARTESIAN_POINT ( 'NONE',  ( 115.2378349030890092, -31.35427756934441845, 250.2899109901960344 ) ) ;
#68573 = LINE ( 'NONE', #21314, #19679 ) ;
#68574 = AXIS2_PLACEMENT_3D ( 'NONE', #28099, #21303, #55782 ) ;
#68575 = CARTESIAN_POINT ( 'NONE',  ( 113.4367438382843716, -44.15125393826585309, 104.1413395616249744 ) ) ;
#68576 = ADVANCED_FACE ( 'NONE', ( #76510 ), #7471, .F. ) ;
#68577 = DIRECTION ( 'NONE',  ( 0.000000000000000000, 1.000000000000000000, 0.000000000000000000 ) ) ;
#68578 = EDGE_CURVE ( 'NONE', #50184, #74884, #77407, .T. ) ;
#68579 = CARTESIAN_POINT ( 'NONE',  ( 105.9764260794164983, -26.77672323648842578, 21.16324968342363277 ) ) ;
#68580 = ORIENTED_EDGE ( 'NONE', *, *, #65275, .T. ) ;
#68581 = CARTESIAN_POINT ( 'NONE',  ( 156.5667039024483529, -48.82844715993569196, 293.2178068554149490 ) ) ;
#68582 = VERTEX_POINT ( 'NONE', #57397 ) ;
#68583 = ORIENTED_EDGE ( 'NONE', *, *, #10355, .F. ) ;
#68584 = DIRECTION ( 'NONE',  ( 1.639958061481212836E-42, -4.100000000000000342E-29, -1.000000000000000000 ) ) ;
#68585 = CARTESIAN_POINT ( 'NONE',  ( 98.43690990026183840, -34.58641363334965035, 272.5644404487542829 ) ) ;
#68586 = AXIS2_PLACEMENT_3D ( 'NONE', #4592, #25031, #47243 ) ;
#68587 = CARTESIAN_POINT ( 'NONE',  ( 49.21213752016101495, -29.73316016639650172, -5.074374724088000832 ) ) ;
#68588 = CARTESIAN_POINT ( 'NONE',  ( 183.5150000000000148, 36.86249999999999716, -35.28456447661465489 ) ) ;
#68589 = CARTESIAN_POINT ( 'NONE',  ( 75.31670390244798341, -57.40094715994099772, 86.31780685541500020 ) ) ;
#68590 = DIRECTION ( 'NONE',  ( 0.000000000000000000, 0.000000000000000000, -1.000000000000000000 ) ) ;
#68591 = ORIENTED_EDGE ( 'NONE', *, *, #82936, .T. ) ;
#68592 = PLANE ( 'NONE',  #58013 ) ;
#68593 = EDGE_CURVE ( 'NONE', #84402, #44354, #44755, .T. ) ;
#68594 = CARTESIAN_POINT ( 'NONE',  ( 144.5667039024470455, -118.2784471599408960, 45.21780685541799727 ) ) ;
#68595 = EDGE_LOOP ( 'NONE', ( #21353, #32057, #72518, #50735, #47266 ) ) ;
#68596 = CARTESIAN_POINT ( 'NONE',  ( 115.6733145644062262, -43.66497474544748059, 43.27467289495795200 ) ) ;
#68597 = VERTEX_POINT ( 'NONE', #83330 ) ;
#68598 = EDGE_CURVE ( 'NONE', #83603, #83684, #77864, .T. ) ;
#68599 = CARTESIAN_POINT ( 'NONE',  ( 99.00928370863422856, -39.88895027456798914, 244.4299951314959571 ) ) ;
#68600 = EDGE_CURVE ( 'NONE', #37791, #22595, #8831, .T. ) ;
#68601 = CARTESIAN_POINT ( 'NONE',  ( -492.0614999999999668, 93.66249999999999432, 95.25000000000000000 ) ) ;
#68602 = CARTESIAN_POINT ( 'NONE',  ( 116.4077482568849859, -39.73851878533137238, 158.5784824187689708 ) ) ;
#68603 = DIRECTION ( 'NONE',  ( 1.000000000000000078E-15, -1.000000000000000000, 0.000000000000000000 ) ) ;
#68604 = FACE_OUTER_BOUND ( 'NONE', #89112, .T. ) ;
#68606 = EDGE_CURVE ( 'NONE', #84043, #32962, #24416, .T. ) ;
#68605 = DIRECTION ( 'NONE',  ( -0.7071067811865758834, 0.7071067811865192621, -7.071067811865766226E-16 ) ) ;
#68607 = CARTESIAN_POINT ( 'NONE',  ( 4.881240125921706863, 70.82551138040557248, 130.4647181642625924 ) ) ;
#68608 = CARTESIAN_POINT ( 'NONE',  ( 110.7484172854196629, -26.25849398357808084, 250.8194347997207387 ) ) ;
#68609 = PLANE ( 'NONE',  #81928 ) ;
#68610 = ORIENTED_EDGE ( 'NONE', *, *, #31144, .T. ) ;
#68611 = AXIS2_PLACEMENT_3D ( 'NONE', #3186, #77803, #15580 ) ;
#68612 = CARTESIAN_POINT ( 'NONE',  ( 112.8257383337702606, -47.14300054286279362, 98.97848241876793907 ) ) ;
#68613 = CARTESIAN_POINT ( 'NONE',  ( 121.0092027855660035, 46.23352279840064938, -49.00708929922899415 ) ) ;
#68614 = ORIENTED_EDGE ( 'NONE', *, *, #67211, .F. ) ;
#68615 = ORIENTED_EDGE ( 'NONE', *, *, #68710, .F. ) ;
#68616 = EDGE_LOOP ( 'NONE', ( #76164, #67832, #17335, #39771, #15734, #32564 ) ) ;
#68617 = CARTESIAN_POINT ( 'NONE',  ( 141.0667039024479834, -48.82844715994099971, 198.9178068554149945 ) ) ;
#68618 = DIRECTION ( 'NONE',  ( 0.000000000000000000, 0.000000000000000000, 1.000000000000000000 ) ) ;
#68619 = DIRECTION ( 'NONE',  ( 1.000000000000000000, 4.163336342344333240E-14, 0.000000000000000000 ) ) ;
#68620 = DIRECTION ( 'NONE',  ( 0.000000000000000000, -1.000000000000000000, 0.000000000000000000 ) ) ;
#68621 = CARTESIAN_POINT ( 'NONE',  ( 103.8146984276687022, -29.21261587019397155, 153.2195189410199418 ) ) ;
#68622 = CARTESIAN_POINT ( 'NONE',  ( 101.2819412958853320, -26.35826957050098329, 251.4813395616249920 ) ) ;
#68623 = CARTESIAN_POINT ( 'NONE',  ( 105.7141124688251352, -46.72365530278647583, 58.46884690485195790 ) ) ;
#68624 = ORIENTED_EDGE ( 'NONE', *, *, #26769, .F. ) ;
#68625 = CARTESIAN_POINT ( 'NONE',  ( 130.2266700119015752, 91.23859726994547259, -9.271983876140096115 ) ) ;
#68626 = FACE_BOUND ( 'NONE', #7015, .T. ) ;
#68627 = VERTEX_POINT ( 'NONE', #62869 ) ;
#68628 = ORIENTED_EDGE ( 'NONE', *, *, #45802, .F. ) ;
#68629 = CARTESIAN_POINT ( 'NONE',  ( 121.3140869715381314, -95.00417761012944595, -11.78219314458228695 ) ) ;
#68630 = VERTEX_POINT ( 'NONE', #36071 ) ;
#68631 = AXIS2_PLACEMENT_3D ( 'NONE', #68558, #89454, #32684 ) ;
#68632 = EDGE_LOOP ( 'NONE', ( #84059, #27757, #39729, #62904 ) ) ;
#68633 = CARTESIAN_POINT ( 'NONE',  ( 37.56670390244749314, -48.82844715994126261, 129.9678068554150911 ) ) ;
#68634 = CARTESIAN_POINT ( 'NONE',  ( 172.5664832912729878, -27.57844715994070484, 138.9256252759119832 ) ) ;
#68635 = CARTESIAN_POINT ( 'NONE',  ( 0.000000000000000000, 239.0000000000000000, 0.000000000000000000 ) ) ;
#68636 = DIRECTION ( 'NONE',  ( 0.000000000000000000, -1.000000000000000000, 0.000000000000000000 ) ) ;
#68637 = CARTESIAN_POINT ( 'NONE',  ( 110.0404421551223209, -45.97207645956791566, 207.2467055423619513 ) ) ;
#68638 = CARTESIAN_POINT ( 'NONE',  ( 115.0563813407508889, -43.54951484902237979, 63.26419670448196797 ) ) ;
#68639 = ORIENTED_EDGE ( 'NONE', *, *, #25390, .F. ) ;
#68640 = DIRECTION ( 'NONE',  ( 0.000000000000000000, -1.000000000000000000, 0.000000000000000000 ) ) ;
#68641 = VERTEX_POINT ( 'NONE', #70599 ) ;
#68642 = AXIS2_PLACEMENT_3D ( 'NONE', #2555, #57043, #37951 ) ;
#68643 = CARTESIAN_POINT ( 'NONE',  ( -76.38829385798634064, 74.80137413886474462, -90.66736180499671605 ) ) ;
#68644 = ORIENTED_EDGE ( 'NONE', *, *, #58196, .T. ) ;
#68645 = DIRECTION ( 'NONE',  ( 0.000000000000000000, 0.7071067811865426878, 0.7071067811865524577 ) ) ;
#68646 = ORIENTED_EDGE ( 'NONE', *, *, #39103, .F. ) ;
#68647 = CARTESIAN_POINT ( 'NONE',  ( 71.25614885437424562, -84.12815644128085069, 542.9756252759101471 ) ) ;
#68648 = CARTESIAN_POINT ( 'NONE',  ( 119.2077814229834729, -133.9288653316829141, 249.3173333679100097 ) ) ;
#68649 = DIRECTION ( 'NONE',  ( 0.7071067811865969777, -0.7071067811864980568, 0.000000000000000000 ) ) ;
#68650 = CIRCLE ( 'NONE', #23729, 3.250000000000002665 ) ;
#68651 = DIRECTION ( 'NONE',  ( 1.000000000000000000, 0.000000000000000000, 0.000000000000000000 ) ) ;
#68652 = EDGE_LOOP ( 'NONE', ( #8051, #57407, #72204, #8483 ) ) ;
#68653 = CARTESIAN_POINT ( 'NONE',  ( 101.1283730419716562, -27.37881681735623829, 65.51467289495799662 ) ) ;
#68654 = ADVANCED_FACE ( 'NONE', ( #645 ), #63785, .F. ) ;
#68656 = DIRECTION ( 'NONE',  ( 0.8660254037844380415, 0.5000000000000012212, -1.550000000000001284E-14 ) ) ;
#68655 = CARTESIAN_POINT ( 'NONE',  ( 98.34960815996063843, -31.65702116157642720, 165.9064988554816864 ) ) ;
#68657 = DIRECTION ( 'NONE',  ( 0.000000000000000000, 0.000000000000000000, 1.000000000000000000 ) ) ;
#68658 = EDGE_CURVE ( 'NONE', #58653, #63781, #12690, .T. ) ;
#68659 = CYLINDRICAL_SURFACE ( 'NONE', #28190, 2.500000000000002220 ) ;
#68660 = ORIENTED_EDGE ( 'NONE', *, *, #40125, .F. ) ;
#68661 = ADVANCED_FACE ( 'NONE', ( #56499 ), #21105, .T. ) ;
#68662 = DIRECTION ( 'NONE',  ( 0.000000000000000000, 0.000000000000000000, 1.000000000000000000 ) ) ;
#68663 = FACE_OUTER_BOUND ( 'NONE', #77460, .T. ) ;
#68664 = CARTESIAN_POINT ( 'NONE',  ( 10.33363185139394957, 75.15554654547490543, 118.1050150300115007 ) ) ;
#68665 = ADVANCED_FACE ( 'NONE', ( #205 ), #22012, .F. ) ;
#68666 = VERTEX_POINT ( 'NONE', #17851 ) ;
#68667 = CARTESIAN_POINT ( 'NONE',  ( 97.24595611328004452, -31.60670846949429347, 86.93181575210095957 ) ) ;
#68669 = LINE ( 'NONE', #61830, #48479 ) ;
#68668 = DIRECTION ( 'NONE',  ( 1.821299053822143307E-16, 0.000000000000000000, -1.000000000000000000 ) ) ;
#68670 = CARTESIAN_POINT ( 'NONE',  ( 172.5664832912729878, -27.82844715994070484, 78.92562527591199739 ) ) ;
#68671 = EDGE_CURVE ( 'NONE', #44708, #8522, #88356, .T. ) ;
#68672 = CIRCLE ( 'NONE', #87545, 5.000000000000004441 ) ;
#68673 = VECTOR ( 'NONE', #9639, 1000.000000000000000 ) ;
#68674 = DIRECTION ( 'NONE',  ( 0.000000000000000000, 0.000000000000000000, 1.000000000000000000 ) ) ;
#68675 = ORIENTED_EDGE ( 'NONE', *, *, #76567, .F. ) ;
#68676 = CARTESIAN_POINT ( 'NONE',  ( 102.6513375509277779, -45.45698538002849176, 123.2041967044819870 ) ) ;
#68678 = ORIENTED_EDGE ( 'NONE', *, *, #862, .T. ) ;
#68677 = CARTESIAN_POINT ( 'NONE',  ( -69.72411017813060141, 120.6499999999999915, 69.72411017812929401 ) ) ;
#68679 = CARTESIAN_POINT ( 'NONE',  ( 96.27200394136428940, -34.46162041542912391, 257.1737205140064475 ) ) ;
#68680 = CARTESIAN_POINT ( 'NONE',  ( 97.82477004090156925, -40.54925333673140386, 252.6383302522648364 ) ) ;
#68681 = LINE ( 'NONE', #42737, #14176 ) ;
#68682 = DIRECTION ( 'NONE',  ( 1.000000000000000078E-15, 1.000000000000000083E-30, -1.000000000000000000 ) ) ;
#68683 = DIRECTION ( 'NONE',  ( 1.000000000000000000, 0.000000000000000000, 0.000000000000000000 ) ) ;
#68684 = EDGE_CURVE ( 'NONE', #64158, #19304, #67979, .T. ) ;
#68685 = CARTESIAN_POINT ( 'NONE',  ( 6.123233995736773185E-16, 215.0000000000000000, 149.6557476874258441 ) ) ;
#68686 = DIRECTION ( 'NONE',  ( 0.000000000000000000, 1.000000000000000000, 0.000000000000000000 ) ) ;
#68687 = CARTESIAN_POINT ( 'NONE',  ( 107.5349099188610893, -47.08895302312306086, 192.6003871806729535 ) ) ;
#68688 = ORIENTED_EDGE ( 'NONE', *, *, #2200, .F. ) ;
#68689 = VERTEX_POINT ( 'NONE', #78322 ) ;
#68690 = EDGE_CURVE ( 'NONE', #87834, #40086, #65991, .T. ) ;
#68691 = CARTESIAN_POINT ( 'NONE',  ( 97.67976800739046439, -37.13700294324897300, 112.7806309249449441 ) ) ;
#68692 = DIRECTION ( 'NONE',  ( 0.000000000000000000, 0.000000000000000000, -1.000000000000000000 ) ) ;
#68694 = DIRECTION ( 'NONE',  ( 0.000000000000000000, 1.000000000000000000, 0.000000000000000000 ) ) ;
#68693 = CARTESIAN_POINT ( 'NONE',  ( 100.4593337790148837, -29.47290724209160828, 281.6641967044818671 ) ) ;
#68695 = VECTOR ( 'NONE', #58488, 1000.000000000000000 ) ;
#68696 = CARTESIAN_POINT ( 'NONE',  ( 107.0664832912739399, -36.72944715994095333, 305.7141315223800007 ) ) ;
#68697 = DIRECTION ( 'NONE',  ( -1.000000000000000000, 0.000000000000000000, 0.000000000000000000 ) ) ;
#68698 = DIRECTION ( 'NONE',  ( -0.7071067811869841124, 0.7071067811861110330, 0.000000000000000000 ) ) ;
#68699 = AXIS2_PLACEMENT_3D ( 'NONE', #52761, #11476, #17838 ) ;
#68700 = FACE_OUTER_BOUND ( 'NONE', #17015, .T. ) ;
#68701 = DIRECTION ( 'NONE',  ( 0.000000000000000000, 1.000000000000000000, 0.000000000000000000 ) ) ;
#68702 = CARTESIAN_POINT ( 'NONE',  ( 95.31970492887376167, -38.09378048407036488, 236.4184824187679510 ) ) ;
#68703 = CARTESIAN_POINT ( 'NONE',  ( 107.0664832912739968, -36.72944715994100306, 0.4256252759109701023 ) ) ;
#68704 = ORIENTED_EDGE ( 'NONE', *, *, #89710, .T. ) ;
#68705 = EDGE_LOOP ( 'NONE', ( #47976, #84037 ) ) ;
#68706 = CARTESIAN_POINT ( 'NONE',  ( -100.0338904447226582, 76.91670260214422683, -83.89393544538330616 ) ) ;
#68707 = CARTESIAN_POINT ( 'NONE',  ( 82.41057659162025573, -20.17027654744481779, 7.249284792665543264 ) ) ;
#68708 = CARTESIAN_POINT ( 'NONE',  ( 97.31582652829270330, -39.30593436283783149, 186.5319638594795038 ) ) ;
#68710 = EDGE_CURVE ( 'NONE', #33465, #85262, #50582, .T. ) ;
#68709 = CARTESIAN_POINT ( 'NONE',  ( -215.9000000000000057, 53.97500000000000142, 50.79999999999999716 ) ) ;
#68711 = VECTOR ( 'NONE', #73285, 1000.000000000000000 ) ;
#68712 = DIRECTION ( 'NONE',  ( -0.9254794337955623007, -0.3787978585227819162, 0.000000000000000000 ) ) ;
#68713 = EDGE_LOOP ( 'NONE', ( #36081, #71241, #13136, #32088 ) ) ;
#68714 = CARTESIAN_POINT ( 'NONE',  ( -6.657255383333532173, 93.25572935329275026, 118.1691278487518986 ) ) ;
#68715 = CARTESIAN_POINT ( 'NONE',  ( 110.0520778049922939, -26.08682939676148038, 219.8708633711489711 ) ) ;
#68716 = ORIENTED_EDGE ( 'NONE', *, *, #81308, .F. ) ;
#68717 = CARTESIAN_POINT ( 'NONE',  ( 90.44969454456416713, -53.34645651782494724, 218.8274735512160589 ) ) ;
#68718 = FACE_OUTER_BOUND ( 'NONE', #20922, .T. ) ;
#68719 = CARTESIAN_POINT ( 'NONE',  ( 116.7467640915520093, -34.14836189904143993, 169.0338844110338812 ) ) ;
#68720 = CARTESIAN_POINT ( 'NONE',  ( 97.89197038913195570, -35.34227587553755257, 69.02523322673498285 ) ) ;
#68721 = CARTESIAN_POINT ( 'NONE',  ( 99.08473320778040261, -45.52208679145996939, 152.9899109901969894 ) ) ;
#68722 = LINE ( 'NONE', #12416, #42088 ) ;
#68723 = ORIENTED_EDGE ( 'NONE', *, *, #80865, .T. ) ;
#68724 = EDGE_CURVE ( 'NONE', #2670, #44910, #51032, .T. ) ;
#68725 = PLANE ( 'NONE',  #26227 ) ;
#68726 = CARTESIAN_POINT ( 'NONE',  ( 98.35383060353775875, -41.64759613607919420, 66.73610187141720473 ) ) ;
#68727 = ORIENTED_EDGE ( 'NONE', *, *, #6455, .F. ) ;
#68728 = ORIENTED_EDGE ( 'NONE', *, *, #10140, .F. ) ;
#68730 = ADVANCED_FACE ( 'NONE', ( #30597 ), #30151, .F. ) ;
#68729 = CIRCLE ( 'NONE', #19445, 0.5000000000000004441 ) ;
#68731 = CARTESIAN_POINT ( 'NONE',  ( 1.145694247088684285E-22, 95.25000000000000000, 118.5560000000000116 ) ) ;
#68732 = ORIENTED_EDGE ( 'NONE', *, *, #6745, .T. ) ;
#68733 = EDGE_LOOP ( 'NONE', ( #27814, #49786, #23400, #83856 ) ) ;
#68734 = CARTESIAN_POINT ( 'NONE',  ( 46.83715912545422100, -47.82818131006082751, 313.9678068554150059 ) ) ;
#68735 = VECTOR ( 'NONE', #47154, 1000.000000000000000 ) ;
#68736 = CARTESIAN_POINT ( 'NONE',  ( 104.4240671743138478, -44.88234475468695450, 81.74956268521998481 ) ) ;
#68737 = CARTESIAN_POINT ( 'NONE',  ( 115.8739437555936718, -44.69579237430344421, 233.2413395616259493 ) ) ;
#68738 = CARTESIAN_POINT ( 'NONE',  ( 104.1918496689534948, -26.69446299336401296, 225.2984824187679749 ) ) ;
#68740 = CARTESIAN_POINT ( 'NONE',  ( 111.1204619107249556, -46.98756979654999810, 18.88800622829195319 ) ) ;
#68739 = CARTESIAN_POINT ( 'NONE',  ( -50.03799999999999670, 101.5999999999999943, 206.3750000000000000 ) ) ;
#68741 = CARTESIAN_POINT ( 'NONE',  ( 126.8507000869722390, 59.56822751209651301, 30.88457633610675046 ) ) ;
#68742 = DIRECTION ( 'NONE',  ( 1.000000000000000000, 0.000000000000000000, 0.000000000000000000 ) ) ;
#68743 = DIRECTION ( 'NONE',  ( -0.000000000000000000, -0.000000000000000000, 1.000000000000000000 ) ) ;
#68744 = VERTEX_POINT ( 'NONE', #37410 ) ;
#68745 = ORIENTED_EDGE ( 'NONE', *, *, #27093, .F. ) ;
#68746 = CARTESIAN_POINT ( 'NONE',  ( 114.7602587138392920, -43.68247563549513046, 83.25372051400698581 ) ) ;
#68747 = CARTESIAN_POINT ( 'NONE',  ( 114.3840247170090407, -44.21678670926648635, 73.19276813305397411 ) ) ;
#68749 = VECTOR ( 'NONE', #19537, 1000.000000000000000 ) ;
#68748 = CARTESIAN_POINT ( 'NONE',  ( 114.4461924768642405, -27.39302975889309266, 274.5441967044824878 ) ) ;
#68750 = ORIENTED_EDGE ( 'NONE', *, *, #53013, .T. ) ;
#68751 = CARTESIAN_POINT ( 'NONE',  ( 110.2559530472221923, -26.76685766971437630, 234.8299109901969643 ) ) ;
#68752 = CARTESIAN_POINT ( 'NONE',  ( 104.4899543942856042, -26.97880759920951732, 35.28145861393137039 ) ) ;
#68753 = AXIS2_PLACEMENT_3D ( 'NONE', #78853, #2543, #11117 ) ;
#68754 = DIRECTION ( 'NONE',  ( 0.000000000000000000, 1.000000000000000000, 0.000000000000000000 ) ) ;
#68756 = DIRECTION ( 'NONE',  ( -1.000000000000000000, -2.756263715554006823E-15, 0.000000000000000000 ) ) ;
#68755 = AXIS2_PLACEMENT_3D ( 'NONE', #59789, #89319, #75237 ) ;
#68757 = DIRECTION ( 'NONE',  ( 0.000000000000000000, 0.000000000000000000, 1.000000000000000000 ) ) ;
#68758 = ADVANCED_FACE ( 'NONE', ( #45529 ), #44654, .F. ) ;
#68760 = LINE ( 'NONE', #12010, #28219 ) ;
#68759 = CARTESIAN_POINT ( 'NONE',  ( 110.4768011403582904, -29.48025783594732729, 277.6356252759111385 ) ) ;
#68761 = CARTESIAN_POINT ( 'NONE',  ( 97.81476338439986762, -40.52493715572875033, 172.6362716151192274 ) ) ;
#68762 = EDGE_CURVE ( 'NONE', #82635, #71852, #1266, .T. ) ;
#68763 = LINE ( 'NONE', #74676, #17832 ) ;
#68764 = CARTESIAN_POINT ( 'NONE',  ( 82.54999999999999716, 95.25000000000000000, 358.0130000000000337 ) ) ;
#68765 = AXIS2_PLACEMENT_3D ( 'NONE', #47093, #54347, #40740 ) ;
#68766 = EDGE_CURVE ( 'NONE', #45547, #75555, #24233, .T. ) ;
#68767 = CARTESIAN_POINT ( 'NONE',  ( -479.3614999999999782, 3.174999999999999822, 101.5999999999999943 ) ) ;
#68768 = DIRECTION ( 'NONE',  ( 0.000000000000000000, 0.000000000000000000, -1.000000000000000000 ) ) ;
#68769 = FACE_OUTER_BOUND ( 'NONE', #71778, .T. ) ;
#68771 = ORIENTED_EDGE ( 'NONE', *, *, #25292, .F. ) ;
#68770 = DIRECTION ( 'NONE',  ( 0.000000000000000000, 0.000000000000000000, -1.000000000000000000 ) ) ;
#68772 = EDGE_CURVE ( 'NONE', #80177, #13052, #86853, .T. ) ;
#68773 = DIRECTION ( 'NONE',  ( 1.000000000000000000, 1.000000000000000078E-15, 1.000000000000000078E-15 ) ) ;
#68774 = CARTESIAN_POINT ( 'NONE',  ( 96.11487883884397831, -35.06878432418778146, 221.1946728949589840 ) ) ;
#68775 = CARTESIAN_POINT ( 'NONE',  ( 117.6079501356808947, -33.40507394795707796, 125.0575300378149706 ) ) ;
#68776 = CARTESIAN_POINT ( 'NONE',  ( 96.93665061341955891, -39.37131572480267749, 272.5299109901966972 ) ) ;
#68777 = LINE ( 'NONE', #40153, #89610 ) ;
#68779 = CARTESIAN_POINT ( 'NONE',  ( 123.6837132603318992, -50.04645651782490745, 239.5838068554164693 ) ) ;
#68778 = DIRECTION ( 'NONE',  ( 0.000000000000000000, 0.000000000000000000, 1.000000000000000000 ) ) ;
#68780 = CARTESIAN_POINT ( 'NONE',  ( 107.0664832912739399, -36.72944715994095333, 247.7440089327910755 ) ) ;
#68781 = CARTESIAN_POINT ( 'NONE',  ( 172.5667039024480687, -42.82844715993500273, 300.4678068554149490 ) ) ;
#68782 = ADVANCED_FACE ( 'NONE', ( #51899 ), #10153, .T. ) ;
#68783 = VERTEX_POINT ( 'NONE', #37862 ) ;
#68784 = ORIENTED_EDGE ( 'NONE', *, *, #2706, .F. ) ;
#68785 = ADVANCED_FACE ( 'NONE', ( #58295 ), #86026, .F. ) ;
#68786 = CARTESIAN_POINT ( 'NONE',  ( 105.3429517235655766, -27.17434032488695550, 124.6409912566479647 ) ) ;
#68788 = ORIENTED_EDGE ( 'NONE', *, *, #84814, .T. ) ;
#68787 = FACE_OUTER_BOUND ( 'NONE', #49354, .T. ) ;
#68789 = DIRECTION ( 'NONE',  ( -4.299999999999999979E-14, 1.000000000000000000, -4.400000000000000367E-29 ) ) ;
#68790 = CARTESIAN_POINT ( 'NONE',  ( 114.2383551682309815, -44.26553795382356071, 154.1813395616249807 ) ) ;
#68791 = FACE_OUTER_BOUND ( 'NONE', #49051, .T. ) ;
#68792 = CARTESIAN_POINT ( 'NONE',  ( 107.0664832912739968, -18.82844715994099971, 168.9256252759119832 ) ) ;
#68793 = CARTESIAN_POINT ( 'NONE',  ( -92.05992619857299530, 79.25941250729452747, 74.70281015415477555 ) ) ;
#68794 = CARTESIAN_POINT ( 'NONE',  ( 31.56670390244800828, -32.29483332968611364, 237.4678068554150059 ) ) ;
#68795 = CARTESIAN_POINT ( 'NONE',  ( 109.9668656698224822, -46.07028316908886723, 97.81562527591097478 ) ) ;
#68796 = ORIENTED_EDGE ( 'NONE', *, *, #15782, .F. ) ;
#68797 = VERTEX_POINT ( 'NONE', #80101 ) ;
#68798 = ORIENTED_EDGE ( 'NONE', *, *, #31826, .T. ) ;
#68799 = AXIS2_PLACEMENT_3D ( 'NONE', #57037, #295, #21194 ) ;
#68800 = CARTESIAN_POINT ( 'NONE',  ( -41.60202597009397607, 65.59999999999998010, 50.85338361873603219 ) ) ;
#68801 =( BOUNDED_CURVE ( )  B_SPLINE_CURVE ( 3, ( #76682, #27628, #48485, #55310 ),
 .UNSPECIFIED., .F., .F. ) 
 B_SPLINE_CURVE_WITH_KNOTS ( ( 4, 4 ),
 ( 3.141592653598349827, 4.712388980395617821 ),
 .UNSPECIFIED. ) 
 CURVE ( )  GEOMETRIC_REPRESENTATION_ITEM ( )  RATIONAL_B_SPLINE_CURVE ( ( 1.000000000000000000, 0.8047378541238059402, 0.8047378541238059402, 1.000000000000000000 ) ) 
 REPRESENTATION_ITEM ( '' )  );
#68803 = DIRECTION ( 'NONE',  ( 0.000000000000000000, 0.000000000000000000, -1.000000000000000000 ) ) ;
#68802 = CARTESIAN_POINT ( 'NONE',  ( 96.28008679191522390, -39.42493101749851547, 162.5213395616249841 ) ) ;
#68804 = AXIS2_PLACEMENT_3D ( 'NONE', #64961, #8212, #44048 ) ;
#68805 = DIRECTION ( 'NONE',  ( -1.000000000000000078E-15, 1.000000000000000000, 0.000000000000000000 ) ) ;
#68806 = PLANE ( 'NONE',  #1642 ) ;
#68807 = CYLINDRICAL_SURFACE ( 'NONE', #21372, 0.2500000000000002220 ) ;
#68808 = DIRECTION ( 'NONE',  ( 0.5000000000000061062, 0.000000000000000000, -0.8660254037844351549 ) ) ;
#68809 = CARTESIAN_POINT ( 'NONE',  ( 67.99030470749720223, -68.76354271653610795, 247.1802073626070353 ) ) ;
#68810 = CARTESIAN_POINT ( 'NONE',  ( 98.35456548258453324, -42.41549619454043096, 101.7870538473399620 ) ) ;
#68811 = VERTEX_POINT ( 'NONE', #73251 ) ;
#68812 = ORIENTED_EDGE ( 'NONE', *, *, #74202, .T. ) ;
#68813 = EDGE_LOOP ( 'NONE', ( #16476, #29518, #39536, #3134 ) ) ;
#68814 = DIRECTION ( 'NONE',  ( 0.000000000000000000, 1.000000000000000000, 0.000000000000000000 ) ) ;
#68815 = PLANE ( 'NONE',  #36004 ) ;
#68817 = EDGE_CURVE ( 'NONE', #67341, #45837, #75249, .T. ) ;
#68816 = LINE ( 'NONE', #49243, #59822 ) ;
#68818 = CARTESIAN_POINT ( 'NONE',  ( 114.8977050226898484, -39.03198754188770891, 181.4166617981629486 ) ) ;
#68819 = VECTOR ( 'NONE', #50256, 1000.000000000000000 ) ;
#68820 = VECTOR ( 'NONE', #84103, 1000.000000000000114 ) ;
#68821 = TOROIDAL_SURFACE ( 'NONE', #45566, 13.09746158385919124, 3.000000000000000000 ) ;
#68822 = VECTOR ( 'NONE', #77929, 1000.000000000000000 ) ;
#68823 = DIRECTION ( 'NONE',  ( 1.387778780781444492E-15, 0.000000000000000000, -1.000000000000000000 ) ) ;
#68824 = ORIENTED_EDGE ( 'NONE', *, *, #74187, .T. ) ;
#68826 = EDGE_LOOP ( 'NONE', ( #34926, #52680, #88022, #35906 ) ) ;
#68825 = VERTEX_POINT ( 'NONE', #4227 ) ;
#68827 = LINE ( 'NONE', #41102, #3233 ) ;
#68828 = AXIS2_PLACEMENT_3D ( 'NONE', #13455, #47945, #34333 ) ;
#68829 = VECTOR ( 'NONE', #14280, 1000.000000000000000 ) ;
#68830 = CARTESIAN_POINT ( 'NONE',  ( 52.56670390244699576, -68.37844715994100397, 55.21780685541800437 ) ) ;
#68831 = ORIENTED_EDGE ( 'NONE', *, *, #2239, .T. ) ;
#68832 = ORIENTED_EDGE ( 'NONE', *, *, #89275, .T. ) ;
#68833 = CARTESIAN_POINT ( 'NONE',  ( -215.9010000000000105, 52.73749999999999716, -44.45000000000000284 ) ) ;
#68834 = CARTESIAN_POINT ( 'NONE',  ( 102.1597156073931671, -27.93204209654597037, 251.9130118773254026 ) ) ;
#68835 = ORIENTED_EDGE ( 'NONE', *, *, #85933, .F. ) ;
#68836 = DIRECTION ( 'NONE',  ( 1.777766061779359009E-15, -1.000000000000000000, 3.100000000000000044E-14 ) ) ;
#68837 = CARTESIAN_POINT ( 'NONE',  ( -119.9775062457194537, 74.60142784138798788, 51.48081989348475673 ) ) ;
#68838 = ORIENTED_EDGE ( 'NONE', *, *, #15951, .F. ) ;
#68839 = ORIENTED_EDGE ( 'NONE', *, *, #82694, .F. ) ;
#68840 = EDGE_CURVE ( 'NONE', #38380, #69742, #22905, .T. ) ;
#68841 = DIRECTION ( 'NONE',  ( 0.9068632946707805287, -0.4214249218767882610, 1.035655806553318316E-15 ) ) ;
#68842 = ORIENTED_EDGE ( 'NONE', *, *, #71368, .F. ) ;
#68843 = ORIENTED_EDGE ( 'NONE', *, *, #30926, .T. ) ;
#68844 = CARTESIAN_POINT ( 'NONE',  ( 102.1781415585801511, -43.87122846086534622, 239.9290427505439709 ) ) ;
#68845 = CARTESIAN_POINT ( 'NONE',  ( 97.59689953814545049, -30.98293302709309671, 125.8803871806719599 ) ) ;
#68846 = CARTESIAN_POINT ( 'NONE',  ( 98.87507392487043489, -43.19978241230797522, 91.85848241876892928 ) ) ;
#68847 = CARTESIAN_POINT ( 'NONE',  ( 103.3391524833590438, -29.24345965735583519, 249.5838068554172366 ) ) ;
#68848 = CARTESIAN_POINT ( 'NONE',  ( 131.6146038194016796, -17.48272374588585620, 7.134497377256392880 ) ) ;
#68849 = CARTESIAN_POINT ( 'NONE',  ( 104.5626002042890974, -48.31241677248981858, 178.4070538473399665 ) ) ;
#68850 = LINE ( 'NONE', #26171, #140 ) ;
#68851 = ORIENTED_EDGE ( 'NONE', *, *, #306, .F. ) ;
#68852 = CARTESIAN_POINT ( 'NONE',  ( 130.4924045281959764, 70.52074417248461202, -4.093845692692696936 ) ) ;
#68853 = ORIENTED_EDGE ( 'NONE', *, *, #23258, .T. ) ;
#68854 = EDGE_LOOP ( 'NONE', ( #8587, #60414 ) ) ;
#68855 = CARTESIAN_POINT ( 'NONE',  ( 162.8595971212720031, -23.19206098994050436, -5.074374724088000832 ) ) ;
#68856 = ORIENTED_EDGE ( 'NONE', *, *, #59717, .F. ) ;
#68857 = AXIS2_PLACEMENT_3D ( 'NONE', #56769, #924, #22274 ) ;
#68858 = CARTESIAN_POINT ( 'NONE',  ( 162.7131505118680082, -31.94127993907151009, 237.4678068554150059 ) ) ;
#68859 = CARTESIAN_POINT ( 'NONE',  ( 102.3930168087890422, -26.71257147495026274, 135.4118157521009493 ) ) ;
#68860 = CARTESIAN_POINT ( 'NONE',  ( -11.03427668835723274, 76.24857023526358546, 130.0890678893988763 ) ) ;
#68861 = VECTOR ( 'NONE', #42589, 1000.000000000000000 ) ;
#68862 = DIRECTION ( 'NONE',  ( 0.000000000000000000, 0.000000000000000000, 1.000000000000000000 ) ) ;
#68863 = DIRECTION ( 'NONE',  ( 0.000000000000000000, -1.000000000000000000, 0.000000000000000000 ) ) ;
#68866 = CARTESIAN_POINT ( 'NONE',  ( 98.85650974919605005, -29.36329775763232774, 231.7565776568629587 ) ) ;
#68865 = LINE ( 'NONE', #13901, #81873 ) ;
#68864 = LINE ( 'NONE', #67070, #31701 ) ;
#68867 = CARTESIAN_POINT ( 'NONE',  ( 179.7974245136200011, -36.32844715994040996, -5.074374724088000832 ) ) ;
#68868 = ADVANCED_FACE ( 'NONE', ( #38737 ), #43768, .T. ) ;
#68869 = DIRECTION ( 'NONE',  ( 1.000000000000000078E-15, 0.000000000000000000, 1.000000000000000000 ) ) ;
#68870 = ORIENTED_EDGE ( 'NONE', *, *, #17514, .F. ) ;
#68871 = CARTESIAN_POINT ( 'NONE',  ( 182.5667039024469886, -33.35206098992650681, -5.074374724088000832 ) ) ;
#68872 = ADVANCED_FACE ( 'NONE', ( #57849 ), #85585, .F. ) ;
#68873 = LINE ( 'NONE', #48848, #2218 ) ;
#68874 = ADVANCED_FACE ( 'NONE', ( #32818 ), #60514, .F. ) ;
#68875 = DIRECTION ( 'NONE',  ( 0.000000000000000000, 0.000000000000000000, -1.000000000000000000 ) ) ;
#68876 = DIRECTION ( 'NONE',  ( 0.000000000000000000, 1.000000000000000000, 0.000000000000000000 ) ) ;
#68878 = VERTEX_POINT ( 'NONE', #47329 ) ;
#68877 = CARTESIAN_POINT ( 'NONE',  ( 100.7233752965418034, -45.83866581990632483, 237.0803871806729717 ) ) ;
#68879 = ADVANCED_FACE ( 'NONE', ( #54576 ), #53231, .T. ) ;
#68880 = DIRECTION ( 'NONE',  ( 1.000000000000000078E-15, 1.000000000000000083E-30, -1.000000000000000000 ) ) ;
#68881 = CARTESIAN_POINT ( 'NONE',  ( 109.2059698035850914, -26.50355049596284118, 139.9127681330539872 ) ) ;
#68882 = CARTESIAN_POINT ( 'NONE',  ( 106.2521435260052698, -26.30072798870746453, 21.13848241876792144 ) ) ;
#68883 = CARTESIAN_POINT ( 'NONE',  ( 114.4937323636162176, -28.48121435373123589, 155.5051490854349652 ) ) ;
#68884 = DIRECTION ( 'NONE',  ( 1.000000000000000000, 0.000000000000000000, 6.982966722218760189E-15 ) ) ;
#68885 = CARTESIAN_POINT ( 'NONE',  ( 116.3185177584062444, -32.94221225046054968, 100.1356252759109680 ) ) ;
#68887 = FACE_OUTER_BOUND ( 'NONE', #19844, .T. ) ;
#68886 = DIRECTION ( 'NONE',  ( 9.351236661543306751E-17, -3.725950533538267725E-29, -1.000000000000000000 ) ) ;
#68888 = CARTESIAN_POINT ( 'NONE',  ( 107.0664832912739968, -8.729447159940999512, 6.425625275911999168 ) ) ;
#68889 = CARTESIAN_POINT ( 'NONE',  ( 107.0664832912739399, -36.72944715994095333, 311.6343304127839815 ) ) ;
#68890 = VERTEX_POINT ( 'NONE', #82341 ) ;
#68891 = VECTOR ( 'NONE', #86818, 1000.000000000000114 ) ;
#68892 = AXIS2_PLACEMENT_3D ( 'NONE', #47644, #33585, #39943 ) ;
#68893 = CIRCLE ( 'NONE', #29727, 4.875000000000017764 ) ;
#68894 = ORIENTED_EDGE ( 'NONE', *, *, #61140, .T. ) ;
#68895 = ORIENTED_EDGE ( 'NONE', *, *, #39746, .F. ) ;
#68896 = EDGE_CURVE ( 'NONE', #30158, #28826, #17285, .T. ) ;
#68897 = AXIS2_PLACEMENT_3D ( 'NONE', #73213, #10993, #52737 ) ;
#68898 = VECTOR ( 'NONE', #56376, 1000.000000000000000 ) ;
#68899 = ORIENTED_EDGE ( 'NONE', *, *, #47618, .F. ) ;
#68900 = CARTESIAN_POINT ( 'NONE',  ( 85.72499999999999432, 69.84999999999999432, 346.0750000000000455 ) ) ;
#68901 = CARTESIAN_POINT ( 'NONE',  ( 97.12559377168382468, -39.79659400623918231, 17.56419670448195092 ) ) ;
#68902 = CARTESIAN_POINT ( 'NONE',  ( 63.03715912545820999, -46.82818131006018092, 300.4678068554150627 ) ) ;
#68903 = CARTESIAN_POINT ( 'NONE',  ( 70.14948329127297200, -1.929447159941395817, 361.9756252759109998 ) ) ;
#68904 = CARTESIAN_POINT ( 'NONE',  ( 98.51568282078342520, -45.00561318155631341, 187.9384824187679612 ) ) ;
#68905 = LINE ( 'NONE', #47984, #54789 ) ;
#68906 = CARTESIAN_POINT ( 'NONE',  ( 102.3370036867683268, -28.24990410829322940, 254.9038483995052502 ) ) ;
#68907 = ORIENTED_EDGE ( 'NONE', *, *, #87729, .F. ) ;
#68908 = ORIENTED_EDGE ( 'NONE', *, *, #66155, .F. ) ;
#68909 = ORIENTED_EDGE ( 'NONE', *, *, #10429, .T. ) ;
#68910 = DIRECTION ( 'NONE',  ( 0.000000000000000000, -1.000000000000000000, 0.000000000000000000 ) ) ;
#68911 = CARTESIAN_POINT ( 'NONE',  ( 116.5686102693484685, -33.54593647048663740, 184.0836522168384874 ) ) ;
#68912 = LINE ( 'NONE', #54803, #4897 ) ;
#68913 = AXIS2_PLACEMENT_3D ( 'NONE', #21624, #8893, #29771 ) ;
#68914 = CARTESIAN_POINT ( 'NONE',  ( 97.06115611282805844, -37.99685616895267515, 276.4268913949732109 ) ) ;
#68915 = CARTESIAN_POINT ( 'NONE',  ( 97.81151460250711693, -40.51751193867107759, 182.6359910548048333 ) ) ;
#68916 = CARTESIAN_POINT ( 'NONE',  ( 210.2301280605339855, 25.81350000000000477, -58.73749999999999716 ) ) ;
#68917 = CARTESIAN_POINT ( 'NONE',  ( 108.4153195593449510, -26.73476064541128849, 174.9691313568370106 ) ) ;
#68918 = CARTESIAN_POINT ( 'NONE',  ( 101.6507727546967175, -27.01955209951621129, 255.4813395616254468 ) ) ;
#68919 = CARTESIAN_POINT ( 'NONE',  ( 107.0667039024479834, -36.72944715994099596, 239.5838068554170093 ) ) ;
#68920 = VERTEX_POINT ( 'NONE', #87791 ) ;
#68921 = CARTESIAN_POINT ( 'NONE',  ( 151.5667039024486087, -48.82844715993590512, 129.9678068554149775 ) ) ;
#68923 = EDGE_CURVE ( 'NONE', #18950, #41648, #75512, .T. ) ;
#68922 = DIRECTION ( 'NONE',  ( -1.000000000000000000, 0.000000000000000000, 0.000000000000000000 ) ) ;
#68924 = CARTESIAN_POINT ( 'NONE',  ( 100.2074232480821365, -30.48050913114499849, 78.55666179816195438 ) ) ;
#68925 = VECTOR ( 'NONE', #74545, 1000.000000000000000 ) ;
#68926 = EDGE_CURVE ( 'NONE', #25618, #75654, #11435, .T. ) ;
#68927 = FACE_OUTER_BOUND ( 'NONE', #19935, .T. ) ;
#68928 = FACE_OUTER_BOUND ( 'NONE', #566, .T. ) ;
#68929 = ORIENTED_EDGE ( 'NONE', *, *, #84824, .T. ) ;
#68930 = CARTESIAN_POINT ( 'NONE',  ( 78.64593636903484253, -34.36767598604495788, 7.908804215170622598 ) ) ;
#68931 = ORIENTED_EDGE ( 'NONE', *, *, #45954, .T. ) ;
#68932 = CARTESIAN_POINT ( 'NONE',  ( 117.7037197400453437, -39.73414628438690244, 143.6194347997209775 ) ) ;
#68933 = ORIENTED_EDGE ( 'NONE', *, *, #27052, .T. ) ;
#68934 = CARTESIAN_POINT ( 'NONE',  ( 117.0718954842606507, -35.46248235080364708, 69.92729194301183782 ) ) ;
#68935 = CARTESIAN_POINT ( 'NONE',  ( 106.2249424221556922, -46.76750045321607985, 108.9415833058969554 ) ) ;
#68936 = DIRECTION ( 'NONE',  ( 1.000000000000000078E-15, -1.000000000000000083E-30, -1.000000000000000000 ) ) ;
#68937 = CARTESIAN_POINT ( 'NONE',  ( 89.17003477451885374, -56.47944715994104570, -5.074374724089047106 ) ) ;
#68938 = CARTESIAN_POINT ( 'NONE',  ( 117.0746561606024869, -31.98374578269911339, 60.19086337114898555 ) ) ;
#68939 = DIRECTION ( 'NONE',  ( 0.000000000000000000, -1.000000000000000000, 0.000000000000000000 ) ) ;
#68940 = CIRCLE ( 'NONE', #63096, 7.199999999999998401 ) ;
#68941 = EDGE_LOOP ( 'NONE', ( #10206, #45201, #3456, #62516 ) ) ;
#68942 = EDGE_CURVE ( 'NONE', #75252, #66874, #69471, .T. ) ;
#68943 = DIRECTION ( 'NONE',  ( -2.900000000000000265E-14, 2.000000000000000155E-15, -1.000000000000000000 ) ) ;
#68944 = CIRCLE ( 'NONE', #22596, 37.00000000000000711 ) ;
#68945 = VECTOR ( 'NONE', #47326, 1000.000000000000000 ) ;
#68946 = VECTOR ( 'NONE', #60739, 1000.000000000000000 ) ;
#68947 = ORIENTED_EDGE ( 'NONE', *, *, #10088, .F. ) ;
#68948 = VERTEX_POINT ( 'NONE', #88704 ) ;
#68949 = AXIS2_PLACEMENT_3D ( 'NONE', #60473, #25976, #68211 ) ;
#68950 = DIRECTION ( 'NONE',  ( 1.000000000000000000, 6.145690160522480771E-16, 0.000000000000000000 ) ) ;
#68951 = ORIENTED_EDGE ( 'NONE', *, *, #14907, .T. ) ;
#68952 = CARTESIAN_POINT ( 'NONE',  ( 102.6689224787387502, -46.93780143634764812, 287.2527681330543601 ) ) ;
#68953 = CARTESIAN_POINT ( 'NONE',  ( 97.93745859118190822, -30.45679909449765432, 161.8594347997199918 ) ) ;
#68954 = DIRECTION ( 'NONE',  ( -0.1811243269279065315, 0.9834602067165264527, 0.000000000000000000 ) ) ;
#68955 = CARTESIAN_POINT ( 'NONE',  ( 105.7995184936499271, -26.72403496521869215, 141.1772919420962751 ) ) ;
#68956 = CARTESIAN_POINT ( 'NONE',  ( 106.6603377114791300, -26.31227224467070158, 81.10705384733896040 ) ) ;
#68957 = CARTESIAN_POINT ( 'NONE',  ( 98.35059589455165963, -31.65526352089521822, 96.90576211103469007 ) ) ;
#68958 = ORIENTED_EDGE ( 'NONE', *, *, #9703, .T. ) ;
#68959 = VECTOR ( 'NONE', #49285, 1000.000000000000000 ) ;
#68960 = CARTESIAN_POINT ( 'NONE',  ( 1.415352702357284018E-13, 20.32000000000000028, -179.8898777604655095 ) ) ;
#68961 = EDGE_CURVE ( 'NONE', #68284, #73560, #38980, .T. ) ;
#68962 = CARTESIAN_POINT ( 'NONE',  ( -158.9822249764575020, 20.32000000000000028, 139.6999999999999886 ) ) ;
#68963 = AXIS2_PLACEMENT_3D ( 'NONE', #40954, #75936, #35034 ) ;
#68964 = ORIENTED_EDGE ( 'NONE', *, *, #55495, .T. ) ;
#68965 = DIRECTION ( 'NONE',  ( 1.000000000000000000, 0.000000000000000000, 0.000000000000000000 ) ) ;
#68966 = FACE_OUTER_BOUND ( 'NONE', #80348, .T. ) ;
#68967 = CARTESIAN_POINT ( 'NONE',  ( 115.6772654923307613, -42.56752007954070649, 273.3527681330537575 ) ) ;
#68968 = CYLINDRICAL_SURFACE ( 'NONE', #33025, 2.999999999999975131 ) ;
#68969 = VECTOR ( 'NONE', #34232, 1000.000000000000000 ) ;
#68970 = CARTESIAN_POINT ( 'NONE',  ( 41.56648329127499153, -36.32844715994070839, 134.1756252759119832 ) ) ;
#68971 = DIRECTION ( 'NONE',  ( 1.000000000000000000, 0.000000000000000000, 0.000000000000000000 ) ) ;
#68972 = CARTESIAN_POINT ( 'NONE',  ( 116.1702204290647984, -31.76348745297265808, 24.21181575210196257 ) ) ;
#68974 = CARTESIAN_POINT ( 'NONE',  ( 101.5125196766230857, -27.93273449574876111, 106.5241967044819944 ) ) ;
#68973 = CARTESIAN_POINT ( 'NONE',  ( 97.80409164390904664, -40.49886389222051264, 101.6344799213053136 ) ) ;
#68975 = LINE ( 'NONE', #6742, #71237 ) ;
#68976 = CARTESIAN_POINT ( 'NONE',  ( 102.8260968645185045, -46.30158323273214904, 177.2441967044819648 ) ) ;
#68977 = CARTESIAN_POINT ( 'NONE',  ( 46.48091746482130304, -49.32844715994084339, 300.4678068554150059 ) ) ;
#68978 = EDGE_LOOP ( 'NONE', ( #12071, #11417, #52229, #74662 ) ) ;
#68979 = LINE ( 'NONE', #21736, #87477 ) ;
#68980 = CARTESIAN_POINT ( 'NONE',  ( -462.0260000000000105, 53.97500000000000142, -3.174999999999999822 ) ) ;
#68981 = CYLINDRICAL_SURFACE ( 'NONE', #22451, 4.000000000000002665 ) ;
#68983 = ORIENTED_EDGE ( 'NONE', *, *, #8162, .F. ) ;
#68982 = EDGE_CURVE ( 'NONE', #43693, #2920, #26017, .T. ) ;
#68984 = DIRECTION ( 'NONE',  ( -0.000000000000000000, -1.000000000000000000, -0.000000000000000000 ) ) ;
#68986 = EDGE_LOOP ( 'NONE', ( #71631, #36215 ) ) ;
#68985 = CARTESIAN_POINT ( 'NONE',  ( 96.62682903746573970, -35.94284815129010013, 146.2670538473399517 ) ) ;
#68987 = DIRECTION ( 'NONE',  ( 0.000000000000000000, 0.000000000000000000, 1.000000000000000000 ) ) ;
#68988 = CARTESIAN_POINT ( 'NONE',  ( 114.8301775850900128, -29.68641892472961175, 205.4127681330539872 ) ) ;
#68989 = CARTESIAN_POINT ( 'NONE',  ( 87.70409100286292414, 71.53177522571066049, 96.71266027437792445 ) ) ;
#68990 = CARTESIAN_POINT ( 'NONE',  ( 172.5664832912740110, -9.303447159940999356, 318.9256252759120116 ) ) ;
#68991 = VECTOR ( 'NONE', #39904, 1000.000000000000000 ) ;
#68992 = CARTESIAN_POINT ( 'NONE',  ( 51.23005224011598102, -33.89581943344511217, 313.9678068554150059 ) ) ;
#68993 = ORIENTED_EDGE ( 'NONE', *, *, #71559, .T. ) ;
#68994 = CONTEXT_DEPENDENT_SHAPE_REPRESENTATION ( #48049, #80837 ) ;
#68995 = AXIS2_PLACEMENT_3D ( 'NONE', #27865, #78285, #43275 ) ;
#68996 = ORIENTED_EDGE ( 'NONE', *, *, #42865, .T. ) ;
#68997 = VERTEX_POINT ( 'NONE', #68250 ) ;
#68998 = ADVANCED_FACE ( 'NONE', ( #46871 ), #74605, .F. ) ;
#68999 = VERTEX_POINT ( 'NONE', #5120 ) ;
#69000 = CARTESIAN_POINT ( 'NONE',  ( 107.0664832912749915, -36.72944715993903486, 25.56312527591096995 ) ) ;
#69001 = CARTESIAN_POINT ( 'NONE',  ( 115.3879430501622636, -30.44965457351534255, 215.3413395616249773 ) ) ;
#69002 = CARTESIAN_POINT ( 'NONE',  ( 83.89391322244436822, 88.18319050751493648, -100.0339087179661703 ) ) ;
#69003 = EDGE_CURVE ( 'NONE', #13721, #81923, #6462, .T. ) ;
#69004 = CARTESIAN_POINT ( 'NONE',  ( 77.39114642429960611, 120.6499999999999915, -71.77848634863110533 ) ) ;
#69006 = CARTESIAN_POINT ( 'NONE',  ( 92.32962665258456525, 81.71068249639864689, 74.36911441044827598 ) ) ;
#69005 = PLANE ( 'NONE',  #71442 ) ;
#69007 = CARTESIAN_POINT ( 'NONE',  ( 1.888034891575249936E-14, 11.42999999999999972, 154.1697486074984909 ) ) ;
#69008 = ORIENTED_EDGE ( 'NONE', *, *, #18600, .F. ) ;
#69009 = VECTOR ( 'NONE', #83114, 999.9999999999998863 ) ;
#69010 = ORIENTED_EDGE ( 'NONE', *, *, #42823, .T. ) ;
#69011 = VECTOR ( 'NONE', #51341, 1000.000000000000000 ) ;
#69012 = VECTOR ( 'NONE', #26459, 1000.000000000000000 ) ;
#69013 = CARTESIAN_POINT ( 'NONE',  ( 107.0664832912739968, -36.72944715994100306, 287.6356252759109680 ) ) ;
#69014 = AXIS2_PLACEMENT_3D ( 'NONE', #6686, #21679, #47999 ) ;
#69015 = LINE ( 'NONE', #6780, #78234 ) ;
#69016 = CARTESIAN_POINT ( 'NONE',  ( 97.41213207386813622, -40.51524797426102253, 242.6118157521009664 ) ) ;
#69017 = CARTESIAN_POINT ( 'NONE',  ( 173.9900000000000091, 53.21300000000000097, 41.63456447661469895 ) ) ;
#69018 = CARTESIAN_POINT ( 'NONE',  ( 107.5699729851651938, -26.92841289699918050, 91.03562527591097364 ) ) ;
#69019 = CARTESIAN_POINT ( 'NONE',  ( 50.36513554127332526, 91.40845232887433269, -72.85198609231717626 ) ) ;
#69020 = VECTOR ( 'NONE', #44255, 1000.000000000000000 ) ;
#69021 = CARTESIAN_POINT ( 'NONE',  ( 97.31304403385813373, -38.96047841033755077, 22.50539973119484927 ) ) ;
#69022 = ORIENTED_EDGE ( 'NONE', *, *, #48520, .T. ) ;
#69023 = DIRECTION ( 'NONE',  ( -4.237773401492740281E-14, 1.000000000000000000, 0.000000000000000000 ) ) ;
#69024 = ORIENTED_EDGE ( 'NONE', *, *, #64647, .F. ) ;
#69025 = VERTEX_POINT ( 'NONE', #81452 ) ;
#69026 = CIRCLE ( 'NONE', #63193, 7.799999999999994493 ) ;
#69027 = DIRECTION ( 'NONE',  ( -0.5000000000000069944, 0.8660254037844344888, -2.684678751731748934E-14 ) ) ;
#69028 = CARTESIAN_POINT ( 'NONE',  ( 100.4929819111635538, -30.01635508975405031, 267.1368214011352507 ) ) ;
#69029 = DIRECTION ( 'NONE',  ( -4.237773401492740281E-14, 1.000000000000000000, 0.000000000000000000 ) ) ;
#69030 = CARTESIAN_POINT ( 'NONE',  ( 105.7991499238894875, -26.72408508578766018, 140.1773212550283745 ) ) ;
#69031 = AXIS2_PLACEMENT_3D ( 'NONE', #75921, #47747, #6874 ) ;
#69032 = EDGE_CURVE ( 'NONE', #19365, #19408, #40076, .T. ) ;
#69033 = DIRECTION ( 'NONE',  ( -3.100000000000000258E-29, 3.100000000000000044E-14, 1.000000000000000000 ) ) ;
#69034 = CARTESIAN_POINT ( 'NONE',  ( 76.39898589339213686, 74.81620433377382540, -90.65754775987947767 ) ) ;
#69035 = ORIENTED_EDGE ( 'NONE', *, *, #16033, .T. ) ;
#69036 = CARTESIAN_POINT ( 'NONE',  ( 0.000000000000000000, 67.86880000000000734, 265.5569999999999595 ) ) ;
#69037 = CARTESIAN_POINT ( 'NONE',  ( 117.0604431937161678, -38.08363390023102824, 184.7192988456124851 ) ) ;
#69038 = ORIENTED_EDGE ( 'NONE', *, *, #5392, .F. ) ;
#69039 = CARTESIAN_POINT ( 'NONE',  ( 106.5180884070038161, -25.68959433010697779, 45.12800622829193742 ) ) ;
#69040 = EDGE_LOOP ( 'NONE', ( #74923, #65371, #67355, #45444 ) ) ;
#69041 = CARTESIAN_POINT ( 'NONE',  ( 105.4654256982276905, -28.22429988993499350, 278.0547570362579677 ) ) ;
#69042 = DIRECTION ( 'NONE',  ( 0.000000000000000000, 0.000000000000000000, -1.000000000000000000 ) ) ;
#69043 = CARTESIAN_POINT ( 'NONE',  ( 108.4956486572523744, -46.43878675094428843, 142.6927681330539883 ) ) ;
#69044 = DIRECTION ( 'NONE',  ( -3.100000000000000258E-29, 3.100000000000000044E-14, 1.000000000000000000 ) ) ;
#69045 = LINE ( 'NONE', #56284, #79188 ) ;
#69046 = CARTESIAN_POINT ( 'NONE',  ( 57.56670390244735103, -42.82844715994040996, 139.7178068554150911 ) ) ;
#69047 = CARTESIAN_POINT ( 'NONE',  ( 6.677588726327760682, 71.73758720873208006, 130.3856720512892764 ) ) ;
#69048 = CARTESIAN_POINT ( 'NONE',  ( 100.2197142693901668, -28.81018370247272742, 256.6441967044821695 ) ) ;
#69049 = FACE_OUTER_BOUND ( 'NONE', #20974, .T. ) ;
#69050 = VERTEX_POINT ( 'NONE', #67793 ) ;
#69051 = ORIENTED_EDGE ( 'NONE', *, *, #41135, .F. ) ;
#69052 = CARTESIAN_POINT ( 'NONE',  ( 98.42274642353920910, -30.82362014679692308, 116.8499109901969604 ) ) ;
#69053 = ADVANCED_FACE ( 'NONE', ( #33273 ), #60976, .T. ) ;
#69054 = DIRECTION ( 'NONE',  ( 0.000000000000000000, 1.000000000000000000, 0.000000000000000000 ) ) ;
#69055 = VERTEX_POINT ( 'NONE', #61413 ) ;
#69056 = ORIENTED_EDGE ( 'NONE', *, *, #65325, .F. ) ;
#69057 = EDGE_LOOP ( 'NONE', ( #45512, #74663, #41337, #30651 ) ) ;
#69058 = ADVANCED_FACE ( 'NONE', ( #89142 ), #26901, .F. ) ;
#69059 = CARTESIAN_POINT ( 'NONE',  ( 0.000000000000000000, 0.000000000000000000, 0.000000000000000000 ) ) ;
#69060 = LINE ( 'NONE', #76319, #60235 ) ;
#69061 = DIRECTION ( 'NONE',  ( 0.000000000000000000, -0.000000000000000000, 1.000000000000000000 ) ) ;
#69062 = LINE ( 'NONE', #13209, #40309 ) ;
#69063 = CARTESIAN_POINT ( 'NONE',  ( 115.2258025850914862, -39.61500320815195408, 176.3861856076869685 ) ) ;
#69064 = CARTESIAN_POINT ( 'NONE',  ( 109.2164500608077873, -48.40848361911378817, 273.7213395616253706 ) ) ;
#69065 = EDGE_CURVE ( 'NONE', #60002, #45648, #56415, .T. ) ;
#69066 = CARTESIAN_POINT ( 'NONE',  ( 98.54763480789691243, -41.97695032525800940, 57.76580044582079410 ) ) ;
#69067 = ORIENTED_EDGE ( 'NONE', *, *, #67080, .F. ) ;
#69068 = CARTESIAN_POINT ( 'NONE',  ( 173.9900000000000091, 37.33800000000000097, 58.73749999999999716 ) ) ;
#69069 = EDGE_CURVE ( 'NONE', #68999, #14487, #24477, .T. ) ;
#69070 = VECTOR ( 'NONE', #9074, 1000.000000000000000 ) ;
#69071 = CARTESIAN_POINT ( 'NONE',  ( 100.8874565155974494, -44.70021274534146727, 42.05175877296590414 ) ) ;
#69072 = ORIENTED_EDGE ( 'NONE', *, *, #86857, .T. ) ;
#69073 = ORIENTED_EDGE ( 'NONE', *, *, #69395, .T. ) ;
#69074 = EDGE_CURVE ( 'NONE', #75636, #43807, #71715, .T. ) ;
#69075 = AXIS2_PLACEMENT_3D ( 'NONE', #88709, #33281, #11043 ) ;
#69076 = CIRCLE ( 'NONE', #56012, 29.00000000000000000 ) ;
#69077 = CARTESIAN_POINT ( 'NONE',  ( 28.57499999999999929, 82.54999999999999716, 298.1325000000000500 ) ) ;
#69078 = VECTOR ( 'NONE', #85024, 1000.000000000000000 ) ;
#69079 = ORIENTED_EDGE ( 'NONE', *, *, #29712, .T. ) ;
#69080 = CARTESIAN_POINT ( 'NONE',  ( 188.5667039024486087, -48.82844715993430640, 137.2178068554150059 ) ) ;
#69081 = CARTESIAN_POINT ( 'NONE',  ( -10.08507579090307971, 74.81978989419388881, -130.1661673264300418 ) ) ;
#69082 = AXIS2_PLACEMENT_3D ( 'NONE', #49462, #49911, #7260 ) ;
#69083 = EDGE_CURVE ( 'NONE', #71344, #37315, #75595, .T. ) ;
#69084 = CARTESIAN_POINT ( 'NONE',  ( 29.56648329127298069, 15.62155284005731204, 361.9756252759109998 ) ) ;
#69085 = DIRECTION ( 'NONE',  ( -1.000000000000000000, 0.000000000000000000, 0.000000000000000000 ) ) ;
#69086 = CARTESIAN_POINT ( 'NONE',  ( 115.4440039095595409, -34.92134030032634939, 183.4181341137909556 ) ) ;
#69087 = CARTESIAN_POINT ( 'NONE',  ( 118.7820429505835733, -34.63792632846725184, 48.96705384733895983 ) ) ;
#69088 = DIRECTION ( 'NONE',  ( 0.7071067811874264253, -0.7071067811856686092, 7.071067811873959532E-16 ) ) ;
#69089 = VERTEX_POINT ( 'NONE', #2229 ) ;
#69090 = CARTESIAN_POINT ( 'NONE',  ( 107.5667039024470455, -112.2628068712777036, -19.78219314458176825 ) ) ;
#69092 = VERTEX_POINT ( 'NONE', #1333 ) ;
#69091 = EDGE_CURVE ( 'NONE', #37650, #75315, #62195, .T. ) ;
#69093 = CARTESIAN_POINT ( 'NONE',  ( 173.9900000000000091, 101.5999999999999943, -71.37400000000000944 ) ) ;
#69094 = EDGE_LOOP ( 'NONE', ( #42773, #858 ) ) ;
#69095 = CARTESIAN_POINT ( 'NONE',  ( 111.6951833200829043, -27.79749774200430323, 165.6959612989590482 ) ) ;
#69096 = DIRECTION ( 'NONE',  ( -1.000000000000000000, -4.299999999999999979E-14, -1.000000000000000078E-15 ) ) ;
#69097 = CARTESIAN_POINT ( 'NONE',  ( 67.06680637612726059, -127.7071673695392917, 245.9559769091540034 ) ) ;
#69098 = AXIS2_PLACEMENT_3D ( 'NONE', #37636, #37186, #64893 ) ;
#69099 = PLANE ( 'NONE',  #75655 ) ;
#69100 = VERTEX_POINT ( 'NONE', #85364 ) ;
#69101 = CARTESIAN_POINT ( 'NONE',  ( 100.3969032678572262, -28.68811230323557027, 40.62705384733894221 ) ) ;
#69102 = VECTOR ( 'NONE', #46526, 1000.000000000000000 ) ;
#69104 = CARTESIAN_POINT ( 'NONE',  ( 192.5667039024475002, -23.42844715993433624, 129.9678068554150343 ) ) ;
#69103 = CARTESIAN_POINT ( 'NONE',  ( 102.0665444595604328, -27.97079262611111972, 165.4898391514462332 ) ) ;
#69105 = CARTESIAN_POINT ( 'NONE',  ( 68.77377604071689632, -69.45229246467815187, 247.4784000562319761 ) ) ;
#69106 = CARTESIAN_POINT ( 'NONE',  ( 131.4050152070336424, -18.03131342368210710, 2.974074870386957503 ) ) ;
#69107 = ORIENTED_EDGE ( 'NONE', *, *, #59421, .T. ) ;
#69108 = ADVANCED_FACE ( 'NONE', ( #23579 ), #44426, .T. ) ;
#69109 = DIRECTION ( 'NONE',  ( 1.000000000000000000, 0.000000000000000000, 0.000000000000000000 ) ) ;
#69110 = ADVANCED_FACE ( 'NONE', ( #50812 ), #78549, .T. ) ;
#69111 = EDGE_CURVE ( 'NONE', #11696, #23732, #34388, .T. ) ;
#69112 = CARTESIAN_POINT ( 'NONE',  ( -105.4788588808464027, 120.6499999999999915, 3.968749999998844924 ) ) ;
#69113 = FACE_OUTER_BOUND ( 'NONE', #80881, .T. ) ;
#69114 = VERTEX_POINT ( 'NONE', #25787 ) ;
#69115 = CARTESIAN_POINT ( 'NONE',  ( 118.8673094125028200, -35.40175986820349152, 79.91562527591095488 ) ) ;
#69116 = EDGE_CURVE ( 'NONE', #70690, #86125, #45318, .T. ) ;
#69118 = CARTESIAN_POINT ( 'NONE',  ( 1.475953350320055108E-14, 223.9999999999999716, 104.4754207677255806 ) ) ;
#69117 = CARTESIAN_POINT ( 'NONE',  ( 31.56670390244800828, -32.29483332968611364, 313.9678068554150059 ) ) ;
#69119 = LINE ( 'NONE', #77277, #33556 ) ;
#69120 = DIRECTION ( 'NONE',  ( 1.000000000000000000, 4.163336342344333240E-14, 0.000000000000000000 ) ) ;
#69121 = ORIENTED_EDGE ( 'NONE', *, *, #70705, .F. ) ;
#69122 = CARTESIAN_POINT ( 'NONE',  ( 101.2684584845352163, -45.32493232151062301, 148.0918157521009562 ) ) ;
#69124 = VERTEX_POINT ( 'NONE', #44883 ) ;
#69123 = DIRECTION ( 'NONE',  ( -1.000000000000000000, -1.734723475976808672E-15, 0.000000000000000000 ) ) ;
#69125 = CARTESIAN_POINT ( 'NONE',  ( 114.3996560367811099, -27.45190519937929707, 270.5441967044823741 ) ) ;
#69126 = CARTESIAN_POINT ( 'NONE',  ( 97.92284106446184921, -40.77982016931672149, 252.6583389871856582 ) ) ;
#69127 = DIRECTION ( 'NONE',  ( 0.000000000000000000, 0.000000000000000000, -1.000000000000000000 ) ) ;
#69128 = DIRECTION ( 'NONE',  ( -0.9825752044165969590, -0.1858654558159821002, 0.000000000000000000 ) ) ;
#69129 = DIRECTION ( 'NONE',  ( 0.000000000000000000, 0.000000000000000000, 1.000000000000000000 ) ) ;
#69130 = DIRECTION ( 'NONE',  ( 1.000000000000000078E-15, -1.000000000000000083E-30, -1.000000000000000000 ) ) ;
#69131 = CARTESIAN_POINT ( 'NONE',  ( 107.0664832912739968, -36.72944715994100306, 287.6356252759109680 ) ) ;
#69132 = AXIS2_PLACEMENT_3D ( 'NONE', #70633, #49721, #36107 ) ;
#69133 = CARTESIAN_POINT ( 'NONE',  ( 104.6152064257953498, -27.26083179018618452, 200.2784824187689310 ) ) ;
#69134 = VERTEX_POINT ( 'NONE', #24457 ) ;
#69135 = ORIENTED_EDGE ( 'NONE', *, *, #80515, .T. ) ;
#69136 = AXIS2_PLACEMENT_3D ( 'NONE', #76856, #13291, #68701 ) ;
#69137 = CARTESIAN_POINT ( 'NONE',  ( 116.1725082674369816, -34.41496348756209755, 165.4682499725639957 ) ) ;
#69138 = VECTOR ( 'NONE', #66627, 1000.000000000000000 ) ;
#69139 = DIRECTION ( 'NONE',  ( 0.000000000000000000, 0.000000000000000000, 1.000000000000000000 ) ) ;
#69141 = CARTESIAN_POINT ( 'NONE',  ( 97.78478700746286734, -40.45111962689370699, 57.62993004767697158 ) ) ;
#69140 = CARTESIAN_POINT ( 'NONE',  ( 105.9660761217308931, -46.48152529548401901, 278.4870538473389843 ) ) ;
#69142 = VECTOR ( 'NONE', #10383, 1000.000000000000000 ) ;
#69143 = DIRECTION ( 'NONE',  ( 1.000000000000000078E-15, -1.000000000000000083E-30, -1.000000000000000000 ) ) ;
#69144 = DIRECTION ( 'NONE',  ( 0.000000000000000000, 1.000000000000000000, 0.000000000000000000 ) ) ;
#69145 = CARTESIAN_POINT ( 'NONE',  ( 162.8913605087219878, -31.76306994223740432, 193.9678068554150059 ) ) ;
#69146 = CARTESIAN_POINT ( 'NONE',  ( 97.06107109826302803, -37.99641197210306132, 107.4272919432525413 ) ) ;
#69147 = DIRECTION ( 'NONE',  ( -0.000000000000000000, -1.000000000000000000, -0.000000000000000000 ) ) ;
#69148 = CARTESIAN_POINT ( 'NONE',  ( 103.6457867198658107, -26.24313906103844474, 210.3394347997209763 ) ) ;
#69149 = CARTESIAN_POINT ( 'NONE',  ( -3.175000000000109956, 17.78000000000000114, -31.75000000000000000 ) ) ;
#69150 = VERTEX_POINT ( 'NONE', #52124 ) ;
#69151 = ORIENTED_EDGE ( 'NONE', *, *, #25886, .T. ) ;
#69152 = FACE_OUTER_BOUND ( 'NONE', #56661, .T. ) ;
#69153 = CARTESIAN_POINT ( 'NONE',  ( -82.35292268805503113, 95.08639429146515454, -85.28591416242375089 ) ) ;
#69154 = CARTESIAN_POINT ( 'NONE',  ( 193.5667039024483529, -48.82844715993410034, 300.4678068554149490 ) ) ;
#69155 = CARTESIAN_POINT ( 'NONE',  ( 73.17003668186727339, -8.979447159941065237, 14.92562527591093691 ) ) ;
#69156 = VECTOR ( 'NONE', #53273, 1000.000000000000000 ) ;
#69157 = CARTESIAN_POINT ( 'NONE',  ( 36.74138383868079671, -48.33240602328870494, 180.4678068554150911 ) ) ;
#69158 = EDGE_LOOP ( 'NONE', ( #53985, #60397 ) ) ;
#69159 = CARTESIAN_POINT ( 'NONE',  ( 117.4276745381585556, -38.22567431247780689, 24.71276813305395237 ) ) ;
#69160 = ADVANCED_FACE ( 'NONE', ( #9937 ), #72610, .T. ) ;
#69161 = CARTESIAN_POINT ( 'NONE',  ( 109.9893001866846163, -26.72224116339410571, 259.8499109901965767 ) ) ;
#69162 = EDGE_CURVE ( 'NONE', #39686, #10389, #38961, .T. ) ;
#69163 = ORIENTED_EDGE ( 'NONE', *, *, #78959, .T. ) ;
#69164 = ADVANCED_FACE ( 'NONE', ( #59844 ), #73035, .T. ) ;
#69165 = DIRECTION ( 'NONE',  ( -4.237773401492740281E-14, 1.000000000000000000, 0.000000000000000000 ) ) ;
#69166 = CARTESIAN_POINT ( 'NONE',  ( -18.39335205926253280, -13.32818131006344231, 237.4678068554150059 ) ) ;
#69167 = CARTESIAN_POINT ( 'NONE',  ( 112.0854389607193724, -45.38515269226328996, 167.9946301825848138 ) ) ;
#69168 = CARTESIAN_POINT ( 'NONE',  ( 99.12746238500623974, -38.62725459667914407, 54.33094751244893672 ) ) ;
#69169 = CARTESIAN_POINT ( 'NONE',  ( 117.8014899757583578, -34.00092425788908912, 165.0365776568629315 ) ) ;
#69170 = EDGE_CURVE ( 'NONE', #1704, #51660, #25333, .T. ) ;
#69171 = CARTESIAN_POINT ( 'NONE',  ( 234.0013031625829854, 52.73749999999999716, 10.66800000000000104 ) ) ;
#69172 = ORIENTED_EDGE ( 'NONE', *, *, #79126, .F. ) ;
#69173 = EDGE_CURVE ( 'NONE', #51938, #53561, #80769, .T. ) ;
#69174 = DIRECTION ( 'NONE',  ( -0.7071067811865192621, -0.7071067811865758834, -7.071067811865186413E-16 ) ) ;
#69175 = ORIENTED_EDGE ( 'NONE', *, *, #41903, .T. ) ;
#69176 = ORIENTED_EDGE ( 'NONE', *, *, #424, .F. ) ;
#69177 = ADVANCED_FACE ( 'NONE', ( #39415 ), #4903, .T. ) ;
#69178 = PLANE ( 'NONE',  #22756 ) ;
#69179 = ORIENTED_EDGE ( 'NONE', *, *, #56380, .T. ) ;
#69180 = ORIENTED_EDGE ( 'NONE', *, *, #57066, .F. ) ;
#69181 = DIRECTION ( 'NONE',  ( -1.000000000000000078E-15, 1.000000000000000083E-30, 1.000000000000000000 ) ) ;
#69182 = EDGE_CURVE ( 'NONE', #68582, #1430, #34502, .T. ) ;
#69183 = CARTESIAN_POINT ( 'NONE',  ( 104.6424027498074025, -44.91968313032340632, 106.7695626852199808 ) ) ;
#69184 = CARTESIAN_POINT ( 'NONE',  ( 98.88149684619317270, -29.26610755689610599, 230.7261014663869503 ) ) ;
#69185 = CARTESIAN_POINT ( 'NONE',  ( 98.39792771585416631, -29.90889243069706538, 200.8080062282919869 ) ) ;
#69186 = CARTESIAN_POINT ( 'NONE',  ( 100.9539191370902387, -46.85292318231929443, 48.14419670448194211 ) ) ;
#69187 = DIRECTION ( 'NONE',  ( -1.000000000000000000, 7.570719237730541270E-15, 0.000000000000000000 ) ) ;
#69188 = CARTESIAN_POINT ( 'NONE',  ( 116.8183557169515154, -34.15769664919192650, 95.03106952027322052 ) ) ;
#69189 = EDGE_CURVE ( 'NONE', #75973, #49111, #21224, .T. ) ;
#69190 = CIRCLE ( 'NONE', #51788, 0.5000000000000004441 ) ;
#69191 = ORIENTED_EDGE ( 'NONE', *, *, #4382, .T. ) ;
#69192 = AXIS2_PLACEMENT_3D ( 'NONE', #74428, #5845, #33533 ) ;
#69193 = EDGE_CURVE ( 'NONE', #28735, #15500, #13066, .T. ) ;
#69194 = CARTESIAN_POINT ( 'NONE',  ( 108.2018929880948832, -26.98138995270364759, 129.9841967044829687 ) ) ;
#69195 = CARTESIAN_POINT ( 'NONE',  ( 112.7839950898761288, -27.91685089337277503, 69.61848241876793963 ) ) ;
#69197 = CARTESIAN_POINT ( 'NONE',  ( 103.9260401568723324, -26.74224119611745820, 250.3184824187677577 ) ) ;
#69196 = AXIS2_PLACEMENT_3D ( 'NONE', #82862, #6984, #76021 ) ;
#69198 = VERTEX_POINT ( 'NONE', #83015 ) ;
#69199 = CIRCLE ( 'NONE', #61921, 3.500000000000003109 ) ;
#69200 = CARTESIAN_POINT ( 'NONE',  ( 100.6375269748662760, -26.77409651225141474, 220.5327681330539633 ) ) ;
#69201 = CYLINDRICAL_SURFACE ( 'NONE', #38415, 3.249999999999975131 ) ;
#69202 = SHAPE_REPRESENTATION_RELATIONSHIP ( 'NONE' , 'NONE' ,  #885, #65184 ) ;
#69203 = CARTESIAN_POINT ( 'NONE',  ( 83.06670390244804025, -43.72944715994108122, 207.5838068554169809 ) ) ;
#69204 = DIRECTION ( 'NONE',  ( 0.000000000000000000, 0.000000000000000000, -1.000000000000000000 ) ) ;
#69206 = CARTESIAN_POINT ( 'NONE',  ( 12.59999999999999964, 82.54999999999999716, -190.5010000000000048 ) ) ;
#69205 = DIRECTION ( 'NONE',  ( -1.000000000000000000, 0.000000000000000000, -1.000000000000000078E-15 ) ) ;
#69207 = PLANE ( 'NONE',  #11889 ) ;
#69208 = CARTESIAN_POINT ( 'NONE',  ( 163.0664832912739826, 25.62155284005901379, 333.4006252759110112 ) ) ;
#69209 = CARTESIAN_POINT ( 'NONE',  ( 3.299336700116783483, 94.84201444875797904, -118.5128796971597609 ) ) ;
#69210 = DIRECTION ( 'NONE',  ( 0.000000000000000000, 0.000000000000000000, -1.000000000000000000 ) ) ;
#69211 = CARTESIAN_POINT ( 'NONE',  ( 142.8841478025725849, -84.11588139007199061, 396.9756252759102040 ) ) ;
#69212 = CYLINDRICAL_SURFACE ( 'NONE', #57931, 5.499999999999999112 ) ;
#69213 = EDGE_CURVE ( 'NONE', #9112, #12734, #89832, .T. ) ;
#69215 = ORIENTED_EDGE ( 'NONE', *, *, #86750, .F. ) ;
#69214 = DIRECTION ( 'NONE',  ( -3.100000000000000258E-29, 3.100000000000000044E-14, 1.000000000000000000 ) ) ;
#69216 = DIRECTION ( 'NONE',  ( -2.900000000000000265E-14, 2.000000000000000155E-15, -1.000000000000000000 ) ) ;
#69217 = CARTESIAN_POINT ( 'NONE',  ( 105.1048729065459355, -25.82772592887830854, 275.2061014663870537 ) ) ;
#69218 = CARTESIAN_POINT ( 'NONE',  ( 114.5275249938671465, -28.57771476791114296, 150.4746728949579619 ) ) ;
#69219 = CARTESIAN_POINT ( 'NONE',  ( 111.8841015539045713, -46.06371569386821818, 268.9556252759110180 ) ) ;
#69220 = CIRCLE ( 'NONE', #24289, 15.84999999999999964 ) ;
#69221 = EDGE_CURVE ( 'NONE', #87720, #28273, #53912, .T. ) ;
#69222 = CARTESIAN_POINT ( 'NONE',  ( 73.17003668186728760, -8.979447159941065237, -5.074374724089063982 ) ) ;
#69223 = AXIS2_PLACEMENT_3D ( 'NONE', #16798, #31296, #18569 ) ;
#69225 = CARTESIAN_POINT ( 'NONE',  ( 32.16397622746000451, -34.03355364505800651, -5.074374724088000832 ) ) ;
#69224 = LINE ( 'NONE', #67876, #20315 ) ;
#69226 = CARTESIAN_POINT ( 'NONE',  ( 97.82719644921415636, -40.55510830976606229, 137.6388683552902137 ) ) ;
#69227 = DIRECTION ( 'NONE',  ( -1.000000000000000078E-15, 0.000000000000000000, -1.000000000000000000 ) ) ;
#69228 = VECTOR ( 'NONE', #83385, 1000.000000000000000 ) ;
#69229 = EDGE_LOOP ( 'NONE', ( #50622, #81261 ) ) ;
#69230 = CARTESIAN_POINT ( 'NONE',  ( 116.0667039024470313, -104.2784471599413791, 2.217806855418003043 ) ) ;
#69231 = ORIENTED_EDGE ( 'NONE', *, *, #45632, .F. ) ;
#69232 = B_SPLINE_CURVE_WITH_KNOTS ( 'NONE', 3,
 ( #5649, #61038, #19710, #88769 ),
 .UNSPECIFIED., .F., .F.,
 ( 4, 4 ),
 ( -0.6035999334370369951, -0.5903216970416030884 ),
 .UNSPECIFIED. ) ;
#69233 = B_SPLINE_CURVE_WITH_KNOTS ( 'NONE', 3,
 ( #36804, #35442, #16364, #77696, #64955, #68741, #44041, #2739, #15480, #2292, #84071, #50417, #43149, #7751, #15920, #77249, #63158, #78160, #57686, #63612, #15019, #1393, #36358, #42693, #84530, #43597, #70890, #8660, #70434, #85429, #1844, #28637, #71776, #50871, #29542, #9547, #940, #65829, #4513, #72222, #87189, #10873, #37702, #73543, #4956, #32201, #59455, #45814, #59898, #79494, #73995, #86294, #45376, #60348, #52177, #3613, #44490, #38571, #88086, #66269, #87630, #67174, #24513, #66728, #11317, #9993, #53060, #86742, #11774, #16808, #80830, #39471, #32652, #25394, #73095, #4060, #24953, #65401, #51296, #18579, #46259, #17256, #79043, #3181, #30880, #44936, #58564, #24074, #52620, #31759, #39018, #79940, #72666, #51744, #31308, #10433, #38136, #59004, #17696, #80381, #18130, #76232 ),
 .UNSPECIFIED., .F., .F.,
 ( 4, 2, 2, 2, 2, 1, 2, 2, 2, 2, 2, 2, 1, 2, 2, 2, 1, 1, 2, 2, 2, 1, 2, 2, 1, 1, 1, 2, 2, 2, 2, 2, 2, 2, 1, 1, 2, 2, 2, 1, 1, 2, 2, 2, 1, 1, 1, 2, 2, 2, 1, 1, 1, 2, 2, 2, 1, 1, 2, 2, 4 ),
 ( 0.000000000000000000, 0.03124999999999782813, 0.06249999999999565625, 0.1249999999999916456, 0.1562499999999896472, 0.1718749999999886480, 0.1796874999999883982, 0.1874999999999881484, 0.2187499999999845957, 0.2343749999999827083, 0.2499999999999808209, 0.2812499999999776845, 0.2968749999999760192, 0.3046874999999750755, 0.3124999999999740763, 0.3437499999999703570, 0.3593749999999687472, 0.3671874999999680256, 0.3710937499999676925, 0.3749999999999674150, 0.4062499999999646394, 0.4218749999999635292, 0.4296874999999631961, 0.4374999999999628630, 0.4687499999999621969, 0.4843749999999618638, 0.4921874999999616973, 0.4960937499999618638, 0.4999999999999620304, 0.5312499999999621414, 0.5624999999999623634, 0.5937499999999624745, 0.6249999999999626965, 0.6562499999999628075, 0.6718749999999631406, 0.6796874999999633626, 0.6835937499999635847, 0.6874999999999639178, 0.7187499999999693578, 0.7343749999999724665, 0.7421874999999742428, 0.7460937499999750200, 0.7499999999999756861, 0.7812499999999787947, 0.7968749999999805711, 0.8046874999999814593, 0.8085937499999823475, 0.8105468749999829026, 0.8124999999999833467, 0.8437499999999903411, 0.8593749999999934497, 0.8671874999999950040, 0.8710937499999956701, 0.8730468749999957812, 0.8749999999999960032, 0.9062499999999967804, 0.9218749999999971134, 0.9296874999999972244, 0.9335937499999974465, 0.9374999999999975575, 1.000000000000000000 ),
 .UNSPECIFIED. ) ;
#69234 = CARTESIAN_POINT ( 'NONE',  ( 110.6311418553464279, -45.76071711580824086, 172.2981341137909794 ) ) ;
#69236 = ORIENTED_EDGE ( 'NONE', *, *, #71341, .T. ) ;
#69235 = DIRECTION ( 'NONE',  ( 0.7071067811869259367, -0.7071067811861692087, 2.899137802863410076E-29 ) ) ;
#69237 = CARTESIAN_POINT ( 'NONE',  ( 107.0664832912730020, -36.72944715994189835, 361.9756252759109998 ) ) ;
#69238 = CARTESIAN_POINT ( 'NONE',  ( 108.3633857348901159, -47.68307073960293963, 158.6822919425779617 ) ) ;
#69239 = DIRECTION ( 'NONE',  ( -0.9068632946707805287, 0.4214249218767882610, -9.068632946707800501E-16 ) ) ;
#69240 = CARTESIAN_POINT ( 'NONE',  ( 80.06648329127398256, -18.72944715994105991, 14.92562527591094224 ) ) ;
#69241 = LINE ( 'NONE', #7461, #9924 ) ;
#69242 = DIRECTION ( 'NONE',  ( 0.000000000000000000, -0.000000000000000000, 1.000000000000000000 ) ) ;
#69243 = CARTESIAN_POINT ( 'NONE',  ( 110.8343066518040416, -26.26926122352943338, 99.80133956162498521 ) ) ;
#69244 = ORIENTED_EDGE ( 'NONE', *, *, #75040, .F. ) ;
#69245 = VERTEX_POINT ( 'NONE', #67571 ) ;
#69247 = ORIENTED_EDGE ( 'NONE', *, *, #3450, .F. ) ;
#69246 = AXIS2_PLACEMENT_3D ( 'NONE', #81082, #80183, #17497 ) ;
#69248 = EDGE_CURVE ( 'NONE', #66449, #6147, #5352, .T. ) ;
#69249 = CYLINDRICAL_SURFACE ( 'NONE', #15332, 3.000000864267367895 ) ;
#69251 = CARTESIAN_POINT ( 'NONE',  ( 107.0664832912739968, -36.72944715994100306, 292.6356252759106837 ) ) ;
#69250 = CARTESIAN_POINT ( 'NONE',  ( 112.4269750522866076, -44.91043508143932428, 174.0384824187679556 ) ) ;
#69252 = CARTESIAN_POINT ( 'NONE',  ( 108.4182423179703392, -26.73513332281806854, 54.96773263005526644 ) ) ;
#69253 = FACE_OUTER_BOUND ( 'NONE', #86225, .T. ) ;
#69254 = CARTESIAN_POINT ( 'NONE',  ( 107.0667039024480260, -36.72944715994100306, 199.5838068554169809 ) ) ;
#69255 = FACE_OUTER_BOUND ( 'NONE', #30072, .T. ) ;
#69256 = DIRECTION ( 'NONE',  ( 1.000000000000000000, 0.000000000000000000, 0.000000000000000000 ) ) ;
#69257 = CARTESIAN_POINT ( 'NONE',  ( 106.0785370228624913, -48.51385081415340750, 112.5099109901969712 ) ) ;
#69258 = ORIENTED_EDGE ( 'NONE', *, *, #83635, .F. ) ;
#69259 = ORIENTED_EDGE ( 'NONE', *, *, #3756, .T. ) ;
#69260 = EDGE_LOOP ( 'NONE', ( #84341, #67636 ) ) ;
#69261 = DIRECTION ( 'NONE',  ( 0.000000000000000000, 0.000000000000000000, 1.000000000000000000 ) ) ;
#69262 = CARTESIAN_POINT ( 'NONE',  ( -96.70003673985446824, 93.55484823631823588, -87.71605664018984783 ) ) ;
#69263 = FACE_OUTER_BOUND ( 'NONE', #26145, .T. ) ;
#69264 = CARTESIAN_POINT ( 'NONE',  ( 98.98344471881878803, -35.59181213353920725, 179.0338046553059712 ) ) ;
#69265 = EDGE_CURVE ( 'NONE', #7678, #18507, #72196, .T. ) ;
#69266 = AXIS2_PLACEMENT_3D ( 'NONE', #33241, #65, #54991 ) ;
#69267 = AXIS2_PLACEMENT_3D ( 'NONE', #6703, #7166, #41651 ) ;
#69268 = DIRECTION ( 'NONE',  ( 0.000000000000000000, 0.000000000000000000, -1.000000000000000000 ) ) ;
#69269 = AXIS2_PLACEMENT_3D ( 'NONE', #75642, #28370, #68823 ) ;
#69270 = ADVANCED_FACE ( 'NONE', ( #33046 ), #34386, .F. ) ;
#69271 = EDGE_CURVE ( 'NONE', #3921, #79223, #83448, .T. ) ;
#69272 = DIRECTION ( 'NONE',  ( -0.02992792722492259097, 3.665114028111639174E-18, 0.9995520592605567911 ) ) ;
#69273 = EDGE_LOOP ( 'NONE', ( #85030, #57436, #17343, #75948 ) ) ;
#69275 = VERTEX_POINT ( 'NONE', #324 ) ;
#69274 = ORIENTED_EDGE ( 'NONE', *, *, #13593, .F. ) ;
#69276 = EDGE_CURVE ( 'NONE', #8408, #41728, #48440, .T. ) ;
#69277 = CARTESIAN_POINT ( 'NONE',  ( 107.0664832912739399, -36.72944715994096754, 296.0306255462182321 ) ) ;
#69278 = ORIENTED_EDGE ( 'NONE', *, *, #20090, .F. ) ;
#69279 = ORIENTED_EDGE ( 'NONE', *, *, #46486, .F. ) ;
#69280 = CARTESIAN_POINT ( 'NONE',  ( 21.56670390244726576, -23.42844715994183957, 300.4678068554150059 ) ) ;
#69281 = CARTESIAN_POINT ( 'NONE',  ( 110.5184084024339626, -28.56779955429167472, 241.1901547344679670 ) ) ;
#69282 = AXIS2_PLACEMENT_3D ( 'NONE', #17582, #45266, #38454 ) ;
#69283 = VERTEX_POINT ( 'NONE', #76179 ) ;
#69284 = AXIS2_PLACEMENT_3D ( 'NONE', #68255, #13287, #54133 ) ;
#69285 = CONICAL_SURFACE ( 'NONE', #77988, 17.36499999999999844, 0.7853981633974490562 ) ;
#69286 = DIRECTION ( 'NONE',  ( 0.000000000000000000, 0.000000000000000000, 1.000000000000000000 ) ) ;
#69287 = CARTESIAN_POINT ( 'NONE',  ( -121.3915910346715492, 74.42942291849823278, 48.05185983205323907 ) ) ;
#69288 = ORIENTED_EDGE ( 'NONE', *, *, #50555, .F. ) ;
#69289 = ORIENTED_EDGE ( 'NONE', *, *, #77024, .F. ) ;
#69291 = ADVANCED_FACE ( 'NONE', ( #13510 ), #89372, .F. ) ;
#69290 = VECTOR ( 'NONE', #25777, 1000.000000000000000 ) ;
#69292 = CARTESIAN_POINT ( 'NONE',  ( 83.06670390244796920, -61.87844715994100397, 207.5838068554149913 ) ) ;
#69293 = EDGE_LOOP ( 'NONE', ( #55171, #19243 ) ) ;
#69294 = ORIENTED_EDGE ( 'NONE', *, *, #1410, .F. ) ;
#69295 = EDGE_CURVE ( 'NONE', #8752, #65418, #6250, .T. ) ;
#69296 = CARTESIAN_POINT ( 'NONE',  ( 106.3397725667592368, -45.35341472531973750, 260.3157094172105417 ) ) ;
#69297 = CARTESIAN_POINT ( 'NONE',  ( 117.6033054121008945, -33.31318886634804954, 134.0880062282919880 ) ) ;
#69298 = CARTESIAN_POINT ( 'NONE',  ( 107.9437834512411598, -25.73425880284244016, 115.0251490854349612 ) ) ;
#69299 = CARTESIAN_POINT ( 'NONE',  ( 101.2293520222977747, -30.88460422255789695, 249.5838068554171798 ) ) ;
#69300 = LINE ( 'NONE', #54285, #23483 ) ;
#69301 = CARTESIAN_POINT ( 'NONE',  ( 98.43498668633466764, -29.82501040932825020, 191.7775300378159784 ) ) ;
#69302 = DIRECTION ( 'NONE',  ( 1.000000000000000078E-15, -1.000000000000000083E-30, -1.000000000000000000 ) ) ;
#69303 = CARTESIAN_POINT ( 'NONE',  ( 97.06111640307527466, -37.99664788389067382, 127.4273107009638295 ) ) ;
#69304 = ORIENTED_EDGE ( 'NONE', *, *, #72051, .F. ) ;
#69305 = DIRECTION ( 'NONE',  ( 0.000000000000000000, 1.000000000000000000, 0.000000000000000000 ) ) ;
#69306 = VERTEX_POINT ( 'NONE', #26237 ) ;
#69307 = EDGE_CURVE ( 'NONE', #56630, #9798, #6688, .T. ) ;
#69308 = VERTEX_POINT ( 'NONE', #13953 ) ;
#69309 = CARTESIAN_POINT ( 'NONE',  ( 156.5667039024483529, -48.82844715993569196, 290.7178068554149490 ) ) ;
#69310 = VECTOR ( 'NONE', #19286, 1000.000000000000114 ) ;
#69311 = CARTESIAN_POINT ( 'NONE',  ( -446.0240000000000009, 3.174999999999999822, -1.387778780781445991E-14 ) ) ;
#69312 = CARTESIAN_POINT ( 'NONE',  ( 113.8435853237685933, -28.76095960330615142, 139.5156252759109634 ) ) ;
#69313 = CARTESIAN_POINT ( 'NONE',  ( -8.784747902566598654, 73.37422592973923940, 130.2602619110634521 ) ) ;
#69314 = CARTESIAN_POINT ( 'NONE',  ( 0.000000000000000000, 215.0000000000000000, 154.6557476874258441 ) ) ;
#69315 = DIRECTION ( 'NONE',  ( 1.000000000000000078E-15, -1.000000000000000083E-30, -1.000000000000000000 ) ) ;
#69318 = CARTESIAN_POINT ( 'NONE',  ( 107.2488531970940073, -24.90511003128411360, 226.0641967044829812 ) ) ;
#69317 = CARTESIAN_POINT ( 'NONE',  ( 97.81257721367181546, -40.51959608142212943, 56.63539486199441342 ) ) ;
#69316 = LINE ( 'NONE', #1632, #66520 ) ;
#69319 = CARTESIAN_POINT ( 'NONE',  ( 0.000000000000000000, 65.60000000000000853, 0.000000000000000000 ) ) ;
#69320 = CARTESIAN_POINT ( 'NONE',  ( 126.8164832912740110, -54.62589567669621005, 14.92562527591099020 ) ) ;
#69321 = ORIENTED_EDGE ( 'NONE', *, *, #32572, .F. ) ;
#69322 = LINE ( 'NONE', #82966, #22258 ) ;
#69323 = DIRECTION ( 'NONE',  ( 1.000000000000000078E-15, -1.000000000000000083E-30, -1.000000000000000000 ) ) ;
#69324 = CYLINDRICAL_SURFACE ( 'NONE', #21229, 5.599999999999994316 ) ;
#69325 = LINE ( 'NONE', #81634, #15798 ) ;
#69327 = VERTEX_POINT ( 'NONE', #60744 ) ;
#69326 = CARTESIAN_POINT ( 'NONE',  ( 100.1483249706684546, -45.40999835672980112, 272.0289586092442278 ) ) ;
#69328 = CARTESIAN_POINT ( 'NONE',  ( 107.0664832912739968, -36.72944715994100306, 287.6356252759109680 ) ) ;
#69329 = CARTESIAN_POINT ( 'NONE',  ( 108.9491902927665734, -26.41713524962505133, 164.9327681330529742 ) ) ;
#69330 = CARTESIAN_POINT ( 'NONE',  ( 112.1812230000633832, -27.60471316448668588, 30.66991099019694644 ) ) ;
#69331 = CARTESIAN_POINT ( 'NONE',  ( 95.26251351713513316, -38.28569616102737427, 147.4299109901969871 ) ) ;
#69332 = AXIS2_PLACEMENT_3D ( 'NONE', #43592, #57681, #63609 ) ;
#69333 = CARTESIAN_POINT ( 'NONE',  ( 115.0889047114336847, -30.61763666118805460, 30.34395861100747283 ) ) ;
#69334 = EDGE_CURVE ( 'NONE', #29733, #45890, #74841, .T. ) ;
#69335 = FACE_OUTER_BOUND ( 'NONE', #7116, .T. ) ;
#69337 = CARTESIAN_POINT ( 'NONE',  ( 183.5150000000000148, 53.21300000000000097, 59.96543552338529537 ) ) ;
#69336 = DIRECTION ( 'NONE',  ( 0.000000000000000000, 1.000000000000000000, 0.000000000000000000 ) ) ;
#69338 = DIRECTION ( 'NONE',  ( 1.000000000000000078E-15, -1.000000000000000000, 0.000000000000000000 ) ) ;
#69339 = CARTESIAN_POINT ( 'NONE',  ( 57.56670390244747892, -48.82844715994040286, 139.7178068554150911 ) ) ;
#69340 = ORIENTED_EDGE ( 'NONE', *, *, #24465, .F. ) ;
#69341 = AXIS2_PLACEMENT_3D ( 'NONE', #404, #83098, #56700 ) ;
#69342 = VECTOR ( 'NONE', #3729, 1000.000000000000000 ) ;
#69343 =( BOUNDED_CURVE ( )  B_SPLINE_CURVE ( 3, ( #44613, #51865, #25524, #52742 ),
 .UNSPECIFIED., .F., .T. ) 
 B_SPLINE_CURVE_WITH_KNOTS ( ( 4, 4 ),
 ( 4.646092198350402214, 4.710762098922305796 ),
 .UNSPECIFIED. ) 
 CURVE ( )  GEOMETRIC_REPRESENTATION_ITEM ( )  RATIONAL_B_SPLINE_CURVE ( ( 1.000000000000000000, 0.9996515140281859724, 0.9996515140281859724, 1.000000000000000000 ) ) 
 REPRESENTATION_ITEM ( '' )  );
#69344 = ORIENTED_EDGE ( 'NONE', *, *, #49692, .T. ) ;
#69345 = ORIENTED_EDGE ( 'NONE', *, *, #53019, .T. ) ;
#69346 = AXIS2_PLACEMENT_3D ( 'NONE', #8496, #50706, #77533 ) ;
#69347 = ORIENTED_EDGE ( 'NONE', *, *, #49577, .F. ) ;
#69348 = CARTESIAN_POINT ( 'NONE',  ( 104.0490797691970073, -47.33883444496879633, 63.36800622829197494 ) ) ;
#69349 = LINE ( 'NONE', #42960, #26667 ) ;
#69350 = AXIS2_PLACEMENT_3D ( 'NONE', #68457, #55244, #6671 ) ;
#69351 = CARTESIAN_POINT ( 'NONE',  ( 145.2008403534674699, -139.0679250929170792, 246.7780077290963163 ) ) ;
#69352 = EDGE_CURVE ( 'NONE', #79236, #87720, #69373, .T. ) ;
#69353 = CARTESIAN_POINT ( 'NONE',  ( 113.7132347973738575, -45.61866494189415988, 184.0994347997199725 ) ) ;
#69354 = AXIS2_PLACEMENT_3D ( 'NONE', #43989, #71724, #72617 ) ;
#69355 = CARTESIAN_POINT ( 'NONE',  ( 0.000000000000000000, 8.255000000000000782, 25.39999999999999858 ) ) ;
#69356 = AXIS2_PLACEMENT_3D ( 'NONE', #39577, #46377, #10979 ) ;
#69357 = CARTESIAN_POINT ( 'NONE',  ( 105.2812310726300922, -46.37359664056156561, 12.42991099019696932 ) ) ;
#69358 = ORIENTED_EDGE ( 'NONE', *, *, #17792, .F. ) ;
#69359 = ORIENTED_EDGE ( 'NONE', *, *, #70288, .F. ) ;
#69360 = EDGE_LOOP ( 'NONE', ( #58050, #32011 ) ) ;
#69361 = VECTOR ( 'NONE', #24783, 1000.000000000000000 ) ;
#69362 = ADVANCED_FACE ( 'NONE', ( #88923 ), #54355, .F. ) ;
#69363 = FACE_OUTER_BOUND ( 'NONE', #87106, .T. ) ;
#69364 = FACE_OUTER_BOUND ( 'NONE', #84831, .T. ) ;
#69365 = FACE_OUTER_BOUND ( 'NONE', #43471, .T. ) ;
#69366 = CARTESIAN_POINT ( 'NONE',  ( 97.33757460489749747, -34.07214903665462202, 276.1144460151012368 ) ) ;
#69367 = DIRECTION ( 'NONE',  ( 0.000000000000000000, 0.000000000000000000, -1.000000000000000000 ) ) ;
#69368 = DIRECTION ( 'NONE',  ( -0.7071067811865171526, -0.7071067811865779928, -7.071067811865164719E-16 ) ) ;
#69369 = CARTESIAN_POINT ( 'NONE',  ( -12.10688491755598939, 86.39173550988738270, 129.9936122529997249 ) ) ;
#69370 = CARTESIAN_POINT ( 'NONE',  ( 105.3240584539683766, -26.47319898023375728, 15.20991099019697401 ) ) ;
#69371 = DIRECTION ( 'NONE',  ( 3.999999999999999995E-14, -1.000000000000000000, 4.100000000000000342E-29 ) ) ;
#69372 = ORIENTED_EDGE ( 'NONE', *, *, #64339, .F. ) ;
#69373 = LINE ( 'NONE', #61199, #46094 ) ;
#69374 = TOROIDAL_SURFACE ( 'NONE', #88251, 154.1697486074984909, 6.349999999999999645 ) ;
#69375 = PLANE ( 'NONE',  #81587 ) ;
#69376 = CARTESIAN_POINT ( 'NONE',  ( 107.1962421797556289, -28.07588791089852265, 77.89475703625792846 ) ) ;
#69377 = CIRCLE ( 'NONE', #72296, 2.117000000000007987 ) ;
#69378 = CARTESIAN_POINT ( 'NONE',  ( 163.0664832912739826, -0.2185775633789972805, 330.8831252759119934 ) ) ;
#69379 = EDGE_CURVE ( 'NONE', #57152, #54835, #16207, .T. ) ;
#69380 = CARTESIAN_POINT ( 'NONE',  ( 72.31648329127402519, -36.72944715994106701, -4.824374724089063982 ) ) ;
#69381 = ORIENTED_EDGE ( 'NONE', *, *, #54081, .T. ) ;
#69382 = ORIENTED_EDGE ( 'NONE', *, *, #34700, .F. ) ;
#69383 = DIRECTION ( 'NONE',  ( 0.000000000000000000, 0.000000000000000000, -1.000000000000000000 ) ) ;
#69384 = EDGE_CURVE ( 'NONE', #1305, #65168, #32125, .T. ) ;
#69385 = ORIENTED_EDGE ( 'NONE', *, *, #53322, .T. ) ;
#69386 = CARTESIAN_POINT ( 'NONE',  ( 98.00691293156391737, -30.39673331971502179, 160.8289586092449497 ) ) ;
#69387 = ORIENTED_EDGE ( 'NONE', *, *, #66591, .F. ) ;
#69388 = CARTESIAN_POINT ( 'NONE',  ( 113.1782937928648352, -44.75186857568589716, 69.09395861141521777 ) ) ;
#69389 = CARTESIAN_POINT ( 'NONE',  ( 107.8658914883948512, -27.90296577952642210, 151.4358690201829631 ) ) ;
#69390 = EDGE_CURVE ( 'NONE', #46470, #6854, #43884, .T. ) ;
#69391 = CARTESIAN_POINT ( 'NONE',  ( 99.66264782090949836, -39.75983002812326106, 9.635625275910941312 ) ) ;
#69392 = CARTESIAN_POINT ( 'NONE',  ( 113.4728825864854116, -46.72846204934055692, 64.02991099019695298 ) ) ;
#69393 = DIRECTION ( 'NONE',  ( 1.000000000000000000, 5.440892098500631367E-15, -1.376676550535195643E-28 ) ) ;
#69394 = ORIENTED_EDGE ( 'NONE', *, *, #37162, .T. ) ;
#69395 = EDGE_CURVE ( 'NONE', #34249, #19610, #60560, .T. ) ;
#69396 = CIRCLE ( 'NONE', #12802, 2.999999999999919176 ) ;
#69397 = CARTESIAN_POINT ( 'NONE',  ( -118.2371168503542407, 73.28361289573329884, -8.694557611692772525 ) ) ;
#69398 = EDGE_LOOP ( 'NONE', ( #49368, #61014, #1133, #441 ) ) ;
#69399 = VERTEX_POINT ( 'NONE', #8037 ) ;
#69400 = ADVANCED_FACE ( 'NONE', ( #83911 ), #56622, .T. ) ;
#69401 = AXIS2_PLACEMENT_3D ( 'NONE', #80008, #10939, #59073 ) ;
#69402 = DIRECTION ( 'NONE',  ( -6.524622321627019585E-16, -4.013151879589939944E-16, -1.000000000000000000 ) ) ;
#69403 = ORIENTED_EDGE ( 'NONE', *, *, #68308, .T. ) ;
#69404 = CARTESIAN_POINT ( 'NONE',  ( 110.7503262618283344, -45.78994064700705735, 282.8841967044829744 ) ) ;
#69405 = CARTESIAN_POINT ( 'NONE',  ( 117.1470005940874728, -33.86231210335883901, 145.0470538473399529 ) ) ;
#69406 = DIRECTION ( 'NONE',  ( 1.000000000000000078E-15, 1.000000000000000083E-30, -1.000000000000000000 ) ) ;
#69407 = CARTESIAN_POINT ( 'NONE',  ( 117.0723825543308294, -35.46652509195462954, 129.9269704041947762 ) ) ;
#69408 = CARTESIAN_POINT ( 'NONE',  ( 116.5333143132291269, -32.36348817604392991, 100.1699109901969535 ) ) ;
#69409 = CARTESIAN_POINT ( 'NONE',  ( 116.3162594664470788, -32.94075446336835000, 20.13562527591095019 ) ) ;
#69410 = ORIENTED_EDGE ( 'NONE', *, *, #67758, .T. ) ;
#69411 = VECTOR ( 'NONE', #81114, 1000.000000000000000 ) ;
#69412 = PLANE ( 'NONE',  #62700 ) ;
#69413 = AXIS2_PLACEMENT_3D ( 'NONE', #75005, #68198, #61364 ) ;
#69414 = DIRECTION ( 'NONE',  ( -4.237773401492740281E-14, 1.000000000000000000, 0.000000000000000000 ) ) ;
#69415 = EDGE_LOOP ( 'NONE', ( #55051, #43348, #79511, #8140, #1853, #65045, #18410, #53432, #21927, #30682, #80323, #72367 ) ) ;
#69416 = CARTESIAN_POINT ( 'NONE',  ( 163.0959832912742797, -23.42844715993517113, 193.9678068554149775 ) ) ;
#69417 = CARTESIAN_POINT ( 'NONE',  ( 5.586628598344671737, 93.87391117675657881, 118.4267587378186306 ) ) ;
#69418 = CARTESIAN_POINT ( 'NONE',  ( 96.68905559037375497, -32.92312794843576995, 21.03467289495897319 ) ) ;
#69419 = DIRECTION ( 'NONE',  ( 0.000000000000000000, 1.000000000000000000, 0.000000000000000000 ) ) ;
#69420 = DIRECTION ( 'NONE',  ( -0.000000000000000000, -0.000000000000000000, -1.000000000000000000 ) ) ;
#69421 = LINE ( 'NONE', #47158, #20051 ) ;
#69422 = CARTESIAN_POINT ( 'NONE',  ( 106.1055101188695602, -45.24582830394255240, 281.9095626852197825 ) ) ;
#69424 = CARTESIAN_POINT ( 'NONE',  ( 114.6914383512287543, -44.69963429152225132, 109.1718157521009687 ) ) ;
#69423 = CYLINDRICAL_SURFACE ( 'NONE', #33268, 29.00000000000000000 ) ;
#69425 = DIRECTION ( 'NONE',  ( 0.000000000000000000, 0.000000000000000000, -1.000000000000000000 ) ) ;
#69426 = CARTESIAN_POINT ( 'NONE',  ( 117.2401079361024898, -34.25881411750412298, 209.0156252759109634 ) ) ;
#69427 = LINE ( 'NONE', #40367, #42328 ) ;
#69428 = ORIENTED_EDGE ( 'NONE', *, *, #40043, .T. ) ;
#69429 = AXIS2_PLACEMENT_3D ( 'NONE', #70302, #76676, #64832 ) ;
#69430 = CARTESIAN_POINT ( 'NONE',  ( -254.0000000000000000, 3.174999999999999822, -41.27499999999999858 ) ) ;
#69431 = CARTESIAN_POINT ( 'NONE',  ( 109.4488842849793997, 50.66243909899585418, 71.17456644476511940 ) ) ;
#69432 = DIRECTION ( 'NONE',  ( -1.150535366796005147E-15, 1.000000000000000000, -3.100000000000000044E-14 ) ) ;
#69433 = EDGE_LOOP ( 'NONE', ( #3723, #20431, #41753, #39078 ) ) ;
#69434 = CARTESIAN_POINT ( 'NONE',  ( 44.45000000000000284, 66.67499999999999716, 219.0749999999999886 ) ) ;
#69436 = ORIENTED_EDGE ( 'NONE', *, *, #71459, .F. ) ;
#69435 = CARTESIAN_POINT ( 'NONE',  ( 96.00724586008001893, -35.77752748456175169, 186.2461014663869889 ) ) ;
#69437 = CARTESIAN_POINT ( 'NONE',  ( 0.000000000000000000, 44.45000000000000284, 38.10000000000000142 ) ) ;
#69438 = CARTESIAN_POINT ( 'NONE',  ( 103.6314581395739793, -26.19921411638948427, 206.3394347997209763 ) ) ;
#69439 = CARTESIAN_POINT ( 'NONE',  ( 98.82395782888086444, 74.16976894168011825, 85.31568053864990020 ) ) ;
#69440 = EDGE_CURVE ( 'NONE', #77124, #81899, #88152, .T. ) ;
#69441 = FACE_OUTER_BOUND ( 'NONE', #74434, .T. ) ;
#69442 = CIRCLE ( 'NONE', #34606, 17.00000000000000000 ) ;
#69443 = B_SPLINE_CURVE_WITH_KNOTS ( 'NONE', 3,
 ( #79311, #85682, #11130, #73812, #38836, #52439, #66542, #51564, #65652, #87004, #73359, #3436, #86564, #66993, #37953, #3880, #4775, #65218, #10251, #11597, #52868, #51998, #86120, #17069, #72037, #17516, #45624, #2993, #31571, #45196, #32461 ),
 .UNSPECIFIED., .F., .F.,
 ( 4, 2, 2, 1, 2, 2, 2, 2, 2, 2, 2, 1, 1, 2, 2, 2, 4 ),
 ( 0.000000000000000000, 0.1250000000000044409, 0.1875000000000065226, 0.2187500000000075773, 0.2343750000000083267, 0.2500000000000090483, 0.3750000000000039968, 0.4375000000000053846, 0.5000000000000067724, 0.6250000000000158762, 0.6875000000000174305, 0.7187500000000174305, 0.7343750000000156541, 0.7421875000000148770, 0.7500000000000142109, 0.8750000000000071054, 1.000000000000000000 ),
 .UNSPECIFIED. ) ;
#69444 = DIRECTION ( 'NONE',  ( 1.000000000000000000, 0.000000000000000000, 0.000000000000000000 ) ) ;
#69445 = VERTEX_POINT ( 'NONE', #36650 ) ;
#69446 = EDGE_CURVE ( 'NONE', #32225, #54314, #18553, .T. ) ;
#69447 = ORIENTED_EDGE ( 'NONE', *, *, #77880, .T. ) ;
#69448 = EDGE_LOOP ( 'NONE', ( #54757, #49466, #25268, #22575 ) ) ;
#69449 = ORIENTED_EDGE ( 'NONE', *, *, #72969, .T. ) ;
#69450 = DIRECTION ( 'NONE',  ( 0.000000000000000000, 0.000000000000000000, 1.000000000000000000 ) ) ;
#69451 = CARTESIAN_POINT ( 'NONE',  ( 96.68218458626328982, -35.80812861978466799, 227.2556252759109725 ) ) ;
#69452 = CARTESIAN_POINT ( 'NONE',  ( -97.46299999999996544, 82.54999999999999716, -3.402902457276681768E-13 ) ) ;
#69453 = DIRECTION ( 'NONE',  ( 1.049727191138617833E-16, -0.5150380749100549327, 0.8571673007021118895 ) ) ;
#69454 = VECTOR ( 'NONE', #55991, 1000.000000000000000 ) ;
#69456 = DIRECTION ( 'NONE',  ( -4.554376769437570034E-14, 1.000000000000000000, 0.000000000000000000 ) ) ;
#69455 = DIRECTION ( 'NONE',  ( -4.237773401492740281E-14, 1.000000000000000000, 0.000000000000000000 ) ) ;
#69457 = LINE ( 'NONE', #42175, #2249 ) ;
#69458 = CARTESIAN_POINT ( 'NONE',  ( 99.74655714901966519, -44.23324885335900802, 21.96133956162593748 ) ) ;
#69459 = VERTEX_POINT ( 'NONE', #85264 ) ;
#69460 = VECTOR ( 'NONE', #81429, 1000.000000000000000 ) ;
#69462 = VERTEX_POINT ( 'NONE', #29834 ) ;
#69461 = AXIS2_PLACEMENT_3D ( 'NONE', #72733, #35973, #36872 ) ;
#69463 = EDGE_CURVE ( 'NONE', #64854, #29557, #22577, .T. ) ;
#69464 = CARTESIAN_POINT ( 'NONE',  ( -12.70000000000000107, 82.54999999999999716, 92.46299999999996544 ) ) ;
#69465 = CARTESIAN_POINT ( 'NONE',  ( 105.8007643231009496, -26.72386559662977845, 16.18055911409852854 ) ) ;
#69466 = CARTESIAN_POINT ( 'NONE',  ( 116.8310051202517457, -36.16593252570071115, 224.8727681330539667 ) ) ;
#69467 = FACE_OUTER_BOUND ( 'NONE', #16777, .T. ) ;
#69468 = VECTOR ( 'NONE', #35639, 1000.000000000000000 ) ;
#69469 = CARTESIAN_POINT ( 'NONE',  ( 110.8343066518039990, -26.26926122352955062, 95.80133956162396203 ) ) ;
#69470 = DIRECTION ( 'NONE',  ( -0.9254794337955620787, -0.3787978585227822492, 0.000000000000000000 ) ) ;
#69471 = CIRCLE ( 'NONE', #65125, 1.000000000000000888 ) ;
#69472 = CARTESIAN_POINT ( 'NONE',  ( -76.77511553011653689, 55.83576417482189669, 30.88625753091331561 ) ) ;
#69473 = ORIENTED_EDGE ( 'NONE', *, *, #64785, .F. ) ;
#69474 = FACE_OUTER_BOUND ( 'NONE', #12266, .T. ) ;
#69475 = AXIS2_PLACEMENT_3D ( 'NONE', #22983, #14371, #1183 ) ;
#69476 = ORIENTED_EDGE ( 'NONE', *, *, #3030, .F. ) ;
#69477 = ORIENTED_EDGE ( 'NONE', *, *, #75222, .F. ) ;
#69478 = CARTESIAN_POINT ( 'NONE',  ( -74.43373480440688184, 84.21498941703525531, 92.27768215250002015 ) ) ;
#69479 = CARTESIAN_POINT ( 'NONE',  ( 114.0851551000824600, -43.95502333027237540, 264.6215833058971043 ) ) ;
#69480 = CARTESIAN_POINT ( 'NONE',  ( 163.0664832912739826, 0.2215528400590083269, 336.6506252759110112 ) ) ;
#69481 = CARTESIAN_POINT ( 'NONE',  ( 138.8167039024479834, -50.82844715994100682, 86.31780685541500020 ) ) ;
#69482 = CARTESIAN_POINT ( 'NONE',  ( 107.0667039024470313, -104.2784471599420755, -19.78219314458201694 ) ) ;
#69483 = EDGE_CURVE ( 'NONE', #65340, #79836, #1683, .T. ) ;
#69484 = VECTOR ( 'NONE', #74890, 1000.000000000000000 ) ;
#69485 = CARTESIAN_POINT ( 'NONE',  ( 74.36911441044797755, 81.71068249639866110, -92.32962665258484947 ) ) ;
#69486 = ORIENTED_EDGE ( 'NONE', *, *, #13956, .T. ) ;
#69487 = CARTESIAN_POINT ( 'NONE',  ( 69.25310000000000343, 82.54999999999999716, 358.0130000000000337 ) ) ;
#69488 = ORIENTED_EDGE ( 'NONE', *, *, #72506, .F. ) ;
#69489 = CARTESIAN_POINT ( 'NONE',  ( 115.7287795988047634, -43.59557489936061359, 48.30514908543492680 ) ) ;
#69490 = ORIENTED_EDGE ( 'NONE', *, *, #40637, .F. ) ;
#69491 = ADVANCED_FACE ( 'NONE', ( #36194 ), #14416, .T. ) ;
#69492 = CARTESIAN_POINT ( 'NONE',  ( 110.5225122084979574, -28.79501634926980458, 282.5557094172103803 ) ) ;
#69493 = LINE ( 'NONE', #56281, #8321 ) ;
#69494 = CARTESIAN_POINT ( 'NONE',  ( 97.28849942844331622, -36.49606577720025768, 196.3070538473399438 ) ) ;
#69495 = DIRECTION ( 'NONE',  ( 1.000000000000000078E-15, -1.000000000000000000, 0.000000000000000000 ) ) ;
#69496 = ADVANCED_FACE ( 'NONE', ( #35281 ), #29386, .T. ) ;
#69497 = CARTESIAN_POINT ( 'NONE',  ( 75.25757238336808541, -1.944390235229870978, 361.9756252759101471 ) ) ;
#69498 = FACE_OUTER_BOUND ( 'NONE', #15573, .T. ) ;
#69499 = CARTESIAN_POINT ( 'NONE',  ( 3.226834594885171104, 70.23869239023346722, 130.5183031135091483 ) ) ;
#69500 = AXIS2_PLACEMENT_3D ( 'NONE', #56618, #13949, #36189 ) ;
#69501 = CARTESIAN_POINT ( 'NONE',  ( 96.47406283524195203, -31.30618784601239923, 241.9499109901969689 ) ) ;
#69502 = CARTESIAN_POINT ( 'NONE',  ( 86.13165781700342905, 94.84303900880917126, -81.47101467905569905 ) ) ;
#69503 = ORIENTED_EDGE ( 'NONE', *, *, #68087, .T. ) ;
#69504 = CARTESIAN_POINT ( 'NONE',  ( 136.6795104150274653, -37.60592655294975373, 6.943955837751754068 ) ) ;
#69505 = ORIENTED_EDGE ( 'NONE', *, *, #51821, .T. ) ;
#69506 = CARTESIAN_POINT ( 'NONE',  ( 108.2817482635038147, -26.29579267872783177, 125.9841967044819597 ) ) ;
#69507 = CARTESIAN_POINT ( 'NONE',  ( 120.9243902208823584, 46.38490584264999228, -49.21592832199778655 ) ) ;
#69508 = ORIENTED_EDGE ( 'NONE', *, *, #78534, .T. ) ;
#69509 = VERTEX_POINT ( 'NONE', #15313 ) ;
#69510 = ORIENTED_EDGE ( 'NONE', *, *, #38046, .T. ) ;
#69511 = EDGE_CURVE ( 'NONE', #2874, #79206, #12736, .T. ) ;
#69512 = CARTESIAN_POINT ( 'NONE',  ( 117.0608945203887572, -38.08045315175083090, 123.7189586067809017 ) ) ;
#69513 = CARTESIAN_POINT ( 'NONE',  ( 109.7248724210130462, -27.00080708520160044, 265.8647914069468925 ) ) ;
#69515 = EDGE_CURVE ( 'NONE', #21770, #31466, #11550, .T. ) ;
#69514 = CARTESIAN_POINT ( 'NONE',  ( -44.45000000000000284, 114.2999999999999972, 275.4630000000000223 ) ) ;
#69516 = CARTESIAN_POINT ( 'NONE',  ( 194.5667039024479834, -40.82844715993405771, 300.4678068554149490 ) ) ;
#69517 = DIRECTION ( 'NONE',  ( 0.7071067811868672059, 0.7071067811862279395, -2.899137802863419044E-29 ) ) ;
#69518 = CARTESIAN_POINT ( 'NONE',  ( 115.0725392204758890, -35.00151292932243052, 181.8138046553059723 ) ) ;
#69519 = CARTESIAN_POINT ( 'NONE',  ( 115.6732227570775819, -30.74586734987101622, 275.3099109901965562 ) ) ;
#69520 = CARTESIAN_POINT ( 'NONE',  ( 170.2205283966864897, 101.5999999999999943, 71.37400000000000944 ) ) ;
#69521 = ORIENTED_EDGE ( 'NONE', *, *, #39321, .F. ) ;
#69522 = DIRECTION ( 'NONE',  ( 0.000000000000000000, 0.000000000000000000, 1.000000000000000000 ) ) ;
#69523 = VECTOR ( 'NONE', #31335, 1000.000000000000000 ) ;
#69524 = DIRECTION ( 'NONE',  ( -1.000000000000000000, -2.756263715554006823E-15, 0.000000000000000000 ) ) ;
#69525 = ORIENTED_EDGE ( 'NONE', *, *, #17792, .T. ) ;
#69526 = ORIENTED_EDGE ( 'NONE', *, *, #54718, .F. ) ;
#69527 = CIRCLE ( 'NONE', #86899, 3.000000000000002665 ) ;
#69528 = DIRECTION ( 'NONE',  ( 0.9834602067019598826, 0.1811243270069988198, 0.000000000000000000 ) ) ;
#69529 = DIRECTION ( 'NONE',  ( 0.000000000000000000, 0.000000000000000000, -1.000000000000000000 ) ) ;
#69530 = CARTESIAN_POINT ( 'NONE',  ( 97.81168921572486852, -40.51740600946125426, 16.63579259794490284 ) ) ;
#69531 = PLANE ( 'NONE',  #86934 ) ;
#69532 = DIRECTION ( 'NONE',  ( 1.000000000000000000, 4.299999999999999979E-14, -1.230419385187874527E-43 ) ) ;
#69533 = CARTESIAN_POINT ( 'NONE',  ( 105.0150133346707406, -46.21955246553896757, 181.8295626852199689 ) ) ;
#69534 = CARTESIAN_POINT ( 'NONE',  ( 103.5840655562901134, -46.60261447156455716, 57.30705384733997221 ) ) ;
#69535 = VERTEX_POINT ( 'NONE', #79331 ) ;
#69536 = PLANE ( 'NONE',  #74191 ) ;
#69537 = ORIENTED_EDGE ( 'NONE', *, *, #68364, .T. ) ;
#69538 = VECTOR ( 'NONE', #69165, 1000.000000000000000 ) ;
#69539 = CARTESIAN_POINT ( 'NONE',  ( -81.76240029069585091, 70.17671898886891313, -85.85219768521579908 ) ) ;
#69540 = ORIENTED_EDGE ( 'NONE', *, *, #32541, .F. ) ;
#69541 = CARTESIAN_POINT ( 'NONE',  ( -48.02966122971775320, 91.07499999999996021, -8.747637655308301746E-15 ) ) ;
#69542 = EDGE_LOOP ( 'NONE', ( #78821, #17075, #15842, #69525 ) ) ;
#69543 = DIRECTION ( 'NONE',  ( 1.000000000000000000, 0.000000000000000000, 4.811757763307910244E-15 ) ) ;
#69544 = AXIS2_PLACEMENT_3D ( 'NONE', #40604, #5197, #54203 ) ;
#69545 = DIRECTION ( 'NONE',  ( -0.7071067811865434649, -0.7071067811865516806, -7.071067811865441807E-16 ) ) ;
#69546 = CARTESIAN_POINT ( 'NONE',  ( 68.02453369492833701, -104.4395081749008796, 247.5031975998799965 ) ) ;
#69547 = CARTESIAN_POINT ( 'NONE',  ( 107.0664832912739968, -18.82844715994099971, 168.9256252759119832 ) ) ;
#69548 = ORIENTED_EDGE ( 'NONE', *, *, #52668, .T. ) ;
#69549 = CARTESIAN_POINT ( 'NONE',  ( 111.9392231810069944, -27.48808525092397304, 59.68991099019693536 ) ) ;
#69550 =( LENGTH_UNIT ( ) NAMED_UNIT ( * ) SI_UNIT ( .MILLI., .METRE. ) );
#69553 = ADVANCED_FACE ( 'NONE', ( #17095 ), #73833, .F. ) ;
#69552 = CARTESIAN_POINT ( 'NONE',  ( 91.73035097708802255, 69.84937019662271496, -92.90380151375003948 ) ) ;
#69551 = LINE ( 'NONE', #42711, #34751 ) ;
#69554 = CARTESIAN_POINT ( 'NONE',  ( -89.60916260784479448, 238.5000000000000000, 134.1927865330827103 ) ) ;
#69555 = FACE_OUTER_BOUND ( 'NONE', #1658, .T. ) ;
#69556 = ORIENTED_EDGE ( 'NONE', *, *, #83386, .F. ) ;
#69557 = AXIS2_PLACEMENT_3D ( 'NONE', #9880, #23527, #16695 ) ;
#69558 = DIRECTION ( 'NONE',  ( -3.100000000000000258E-29, 3.100000000000000044E-14, 1.000000000000000000 ) ) ;
#69559 = DIRECTION ( 'NONE',  ( 0.000000000000000000, 0.000000000000000000, -1.000000000000000000 ) ) ;
#69560 = CYLINDRICAL_SURFACE ( 'NONE', #17971, 4.875000000000017764 ) ;
#69561 = ORIENTED_EDGE ( 'NONE', *, *, #80991, .T. ) ;
#69562 = CARTESIAN_POINT ( 'NONE',  ( 104.1016336957795261, -46.74677842777965253, 103.3470538473389411 ) ) ;
#69564 = FACE_OUTER_BOUND ( 'NONE', #20708, .T. ) ;
#69563 = CARTESIAN_POINT ( 'NONE',  ( 194.5664832912739826, -18.82844715994099971, 342.9256252759119548 ) ) ;
#69565 = CARTESIAN_POINT ( 'NONE',  ( 116.3197976069899795, -32.94561274469138112, 134.1356252759109680 ) ) ;
#69566 = VECTOR ( 'NONE', #51469, 1000.000000000000000 ) ;
#69567 = EDGE_CURVE ( 'NONE', #83239, #71292, #37973, .T. ) ;
#69568 = LINE ( 'NONE', #89122, #69460 ) ;
#69569 = CARTESIAN_POINT ( 'NONE',  ( 108.2018929880948548, -26.98138995270375062, 125.9841967044819597 ) ) ;
#69571 = ORIENTED_EDGE ( 'NONE', *, *, #24426, .T. ) ;
#69570 = CARTESIAN_POINT ( 'NONE',  ( -487.2989999999999782, 93.66249999999999432, 98.73639197104678544 ) ) ;
#69572 = AXIS2_PLACEMENT_3D ( 'NONE', #35497, #21897, #35052 ) ;
#69573 = CARTESIAN_POINT ( 'NONE',  ( 117.4688788178165737, -35.86077403649778716, 249.8927681330537780 ) ) ;
#69574 = CARTESIAN_POINT ( 'NONE',  ( 172.5664832912729878, -27.82844715994070484, 258.9256252759120116 ) ) ;
#69575 = LINE ( 'NONE', #83660, #25772 ) ;
#69576 = CARTESIAN_POINT ( 'NONE',  ( 51.27381068362099370, -23.19206098993950604, -5.074374724088000832 ) ) ;
#69577 = FACE_OUTER_BOUND ( 'NONE', #18196, .T. ) ;
#69578 = EDGE_CURVE ( 'NONE', #27916, #89573, #79671, .T. ) ;
#69579 = VECTOR ( 'NONE', #8918, 1000.000000000000114 ) ;
#69580 = EDGE_CURVE ( 'NONE', #67349, #20321, #51586, .T. ) ;
#69581 = CARTESIAN_POINT ( 'NONE',  ( 68.37671137566576363, -137.2574698224148904, 247.4285129581799936 ) ) ;
#69582 = DIRECTION ( 'NONE',  ( 0.000000000000000000, 0.8660254037844387076, -0.4999999999999998890 ) ) ;
#69583 = CARTESIAN_POINT ( 'NONE',  ( 97.67678136301120162, -41.13084272647608941, 211.6632443235309893 ) ) ;
#69584 = ORIENTED_EDGE ( 'NONE', *, *, #48277, .T. ) ;
#69585 = EDGE_LOOP ( 'NONE', ( #48460, #57258 ) ) ;
#69586 = AXIS2_PLACEMENT_3D ( 'NONE', #63269, #15126, #21958 ) ;
#69587 = CARTESIAN_POINT ( 'NONE',  ( 99.36575536895223593, -31.34657530650553880, 157.2606309249449623 ) ) ;
#69588 = VECTOR ( 'NONE', #80127, 1000.000000000000000 ) ;
#69589 = DIRECTION ( 'NONE',  ( 0.000000000000000000, 0.000000000000000000, -1.000000000000000000 ) ) ;
#69590 = CARTESIAN_POINT ( 'NONE',  ( 114.6135591410776016, -41.37377328621888495, 14.81872616303997425 ) ) ;
#69591 = CARTESIAN_POINT ( 'NONE',  ( 147.0667039024457665, -137.6758868153238780, 245.5072646551060132 ) ) ;
#69592 = ADVANCED_FACE ( 'NONE', ( #17967 ), #10705, .F. ) ;
#69593 = CARTESIAN_POINT ( 'NONE',  ( 29.00000000000003553, 172.0000000000000000, 183.8826257785461280 ) ) ;
#69594 = VECTOR ( 'NONE', #39661, 1000.000000000000000 ) ;
#69595 = CARTESIAN_POINT ( 'NONE',  ( 82.54999999999999716, 69.84999999999999432, 280.2255000000000109 ) ) ;
#69596 = CYLINDRICAL_SURFACE ( 'NONE', #55061, 0.5000000000000007772 ) ;
#69597 = LINE ( 'NONE', #47784, #77838 ) ;
#69599 = CARTESIAN_POINT ( 'NONE',  ( 116.8642987764957297, -41.79567201640977459, 243.4346728949589647 ) ) ;
#69598 = AXIS2_PLACEMENT_3D ( 'NONE', #23652, #85447, #79960 ) ;
#69600 = DIRECTION ( 'NONE',  ( 1.000000000000000000, 0.000000000000000000, 0.000000000000000000 ) ) ;
#69601 = ORIENTED_EDGE ( 'NONE', *, *, #5898, .T. ) ;
#69603 = ORIENTED_EDGE ( 'NONE', *, *, #66596, .F. ) ;
#69602 = EDGE_CURVE ( 'NONE', #60012, #18422, #78885, .T. ) ;
#69604 = FACE_OUTER_BOUND ( 'NONE', #61555, .T. ) ;
#69605 = CARTESIAN_POINT ( 'NONE',  ( 82.80376800125165460, -19.00431460297814468, 6.768845952122303444 ) ) ;
#69606 = VECTOR ( 'NONE', #82933, 1000.000000000000000 ) ;
#69607 = CARTESIAN_POINT ( 'NONE',  ( 97.92310196018878798, -40.78040932546785768, 122.6578565618004006 ) ) ;
#69608 = DIRECTION ( 'NONE',  ( 1.000000000000000000, 0.000000000000000000, 0.000000000000000000 ) ) ;
#69609 = CARTESIAN_POINT ( 'NONE',  ( -92.32962665258507684, 82.54999999999999716, -74.36911441044765070 ) ) ;
#69610 = EDGE_LOOP ( 'NONE', ( #76199, #50841, #49536 ) ) ;
#69611 = CARTESIAN_POINT ( 'NONE',  ( 116.1963150171851851, -43.04653558477239272, 9.356577656862985037 ) ) ;
#69612 = CARTESIAN_POINT ( 'NONE',  ( 96.80868943730629894, -40.84730494075294871, 251.6422919425777138 ) ) ;
#69613 = VERTEX_POINT ( 'NONE', #51147 ) ;
#69614 = VECTOR ( 'NONE', #51526, 1000.000000000000000 ) ;
#69615 = ADVANCED_FACE ( 'NONE', ( #44327 ), #45216, .T. ) ;
#69616 = CARTESIAN_POINT ( 'NONE',  ( 77.65458752640685702, -38.05177997653564859, 7.178113714831590997 ) ) ;
#69617 = CARTESIAN_POINT ( 'NONE',  ( -479.3614999999999782, 21.43125000000035030, 6.988054014476359654 ) ) ;
#69618 = CARTESIAN_POINT ( 'NONE',  ( 111.2674639284623908, -45.80588075472486764, 167.9214246773950947 ) ) ;
#69619 = EDGE_CURVE ( 'NONE', #10090, #78353, #11152, .T. ) ;
#69620 = CARTESIAN_POINT ( 'NONE',  ( 109.6406350139562136, -27.81487066565610888, 62.67094751244894724 ) ) ;
#69621 = CARTESIAN_POINT ( 'NONE',  ( 108.3688181871424945, -47.72895317076035582, 158.6822919425779617 ) ) ;
#69622 = FACE_OUTER_BOUND ( 'NONE', #27712, .T. ) ;
#69623 = VERTEX_POINT ( 'NONE', #4355 ) ;
#69624 = EDGE_CURVE ( 'NONE', #45185, #849, #72059, .T. ) ;
#69625 = LINE ( 'NONE', #63254, #3019 ) ;
#69626 = ORIENTED_EDGE ( 'NONE', *, *, #21957, .F. ) ;
#69627 = ORIENTED_EDGE ( 'NONE', *, *, #74187, .F. ) ;
#69628 = CARTESIAN_POINT ( 'NONE',  ( 12.61753767970230200, 84.21537865765687059, 117.8827776564339302 ) ) ;
#69629 = ORIENTED_EDGE ( 'NONE', *, *, #83520, .F. ) ;
#69630 = EDGE_LOOP ( 'NONE', ( #41801, #10420 ) ) ;
#69631 = DIRECTION ( 'NONE',  ( 0.000000000000000000, 0.000000000000000000, 1.000000000000000000 ) ) ;
#69632 = CARTESIAN_POINT ( 'NONE',  ( 115.2923595980251434, -39.02968425817515197, 98.03241982807698207 ) ) ;
#69633 = CARTESIAN_POINT ( 'NONE',  ( 111.6181759772156994, -46.13308781976898842, 247.9356252759109509 ) ) ;
#69634 = AXIS2_PLACEMENT_3D ( 'NONE', #22238, #30824, #71722 ) ;
#69635 = CARTESIAN_POINT ( 'NONE',  ( 110.1310368924891350, -26.13358316477604504, 214.8403871806729342 ) ) ;
#69636 = CARTESIAN_POINT ( 'NONE',  ( 96.97787942770426639, -32.27031107066119375, 51.98324432352996638 ) ) ;
#69637 = CARTESIAN_POINT ( 'NONE',  ( 82.81648329127399677, -18.72944715994105636, -5.074374724089055100 ) ) ;
#69638 = LINE ( 'NONE', #7407, #54040 ) ;
#69639 = VECTOR ( 'NONE', #88340, 1000.000000000000000 ) ;
#69640 = ORIENTED_EDGE ( 'NONE', *, *, #14319, .F. ) ;
#69641 = CARTESIAN_POINT ( 'NONE',  ( -479.3614999999999782, 10.16305401447644030, 97.63125000000000853 ) ) ;
#69642 = CARTESIAN_POINT ( 'NONE',  ( 6.174546696621030198E-16, 127.0000000000000000, -108.2293999999999983 ) ) ;
#69643 = CARTESIAN_POINT ( 'NONE',  ( -487.2989999999999782, 7.143750000000339995, 6.988054014476278830 ) ) ;
#69644 = VECTOR ( 'NONE', #31193, 1000.000000000000000 ) ;
#69645 = CARTESIAN_POINT ( 'NONE',  ( 107.9743429475490615, -26.39917242597363867, 109.9946728949599759 ) ) ;
#69646 = CARTESIAN_POINT ( 'NONE',  ( 117.3100546213214699, -38.89183298362549834, 63.66133956162494911 ) ) ;
#69647 = CARTESIAN_POINT ( 'NONE',  ( 110.7486471836621860, -26.25784018214204707, 254.8194347997204545 ) ) ;
#69648 = EDGE_LOOP ( 'NONE', ( #38124, #60805, #29215, #61766 ) ) ;
#69649 = CARTESIAN_POINT ( 'NONE',  ( 98.89873792621239090, -29.28182854020744230, 230.7261014663869503 ) ) ;
#69650 = FACE_BOUND ( 'NONE', #31527, .T. ) ;
#69651 = CARTESIAN_POINT ( 'NONE',  ( 10.61518134898173216, 75.57796106687908377, 130.1237400822467407 ) ) ;
#69652 = CARTESIAN_POINT ( 'NONE',  ( 117.0667039024470313, -104.2784471599412086, 7.717806855417980394 ) ) ;
#69654 = CARTESIAN_POINT ( 'NONE',  ( 68.69272960418753371, -139.3028697034590664, 245.7287393302975147 ) ) ;
#69653 = CARTESIAN_POINT ( 'NONE',  ( 116.3185177584062444, -32.94221225046054968, 100.1356252759109680 ) ) ;
#69655 = FACE_OUTER_BOUND ( 'NONE', #50161, .T. ) ;
#69656 = CARTESIAN_POINT ( 'NONE',  ( 143.0667039024470171, -118.2784471599408960, 51.21780685541800437 ) ) ;
#69657 = CARTESIAN_POINT ( 'NONE',  ( 31.71315051185499811, -33.70561438052090608, -5.074374724088000832 ) ) ;
#69658 = VECTOR ( 'NONE', #85953, 1000.000000000000000 ) ;
#69659 = FACE_OUTER_BOUND ( 'NONE', #52433, .T. ) ;
#69660 = CYLINDRICAL_SURFACE ( 'NONE', #74969, 3.250000000000002665 ) ;
#69661 = DIRECTION ( 'NONE',  ( 0.000000000000000000, 0.000000000000000000, 1.000000000000000000 ) ) ;
#69663 = ORIENTED_EDGE ( 'NONE', *, *, #79452, .T. ) ;
#69662 = DIRECTION ( 'NONE',  ( 1.000000000000000078E-15, 0.000000000000000000, -1.000000000000000000 ) ) ;
#69664 = CARTESIAN_POINT ( 'NONE',  ( 88.01156830653452801, -124.1980709993373750, 250.2178068554179333 ) ) ;
#69665 = CARTESIAN_POINT ( 'NONE',  ( 115.3410742220599872, -45.24796585940374882, 268.1899109901965517 ) ) ;
#69666 = CARTESIAN_POINT ( 'NONE',  ( 118.9175753851156401, -36.92810247848812821, 149.8127681330539644 ) ) ;
#69667 = CARTESIAN_POINT ( 'NONE',  ( 97.77292256144662019, -40.53329279276322694, 7.635625275910939536 ) ) ;
#69668 = AXIS2_PLACEMENT_3D ( 'NONE', #70179, #27059, #20248 ) ;
#69669 = FACE_BOUND ( 'NONE', #47088, .T. ) ;
#69671 = DIRECTION ( 'NONE',  ( -0.7071067811865197061, -0.7071067811865753283, -7.071067811865190357E-16 ) ) ;
#69670 = LINE ( 'NONE', #21072, #56601 ) ;
#69672 = DIRECTION ( 'NONE',  ( 1.000000000000000000, 3.555032108465730541E-16, 0.000000000000000000 ) ) ;
#69673 = FACE_OUTER_BOUND ( 'NONE', #57047, .T. ) ;
#69674 = ADVANCED_FACE ( 'NONE', ( #72933 ), #31153, .F. ) ;
#69675 = ORIENTED_EDGE ( 'NONE', *, *, #65216, .T. ) ;
#69676 = EDGE_CURVE ( 'NONE', #37713, #86716, #37372, .T. ) ;
#69677 = DIRECTION ( 'NONE',  ( 0.000000000000000000, 1.000000000000000000, 0.000000000000000000 ) ) ;
#69678 = VERTEX_POINT ( 'NONE', #59298 ) ;
#69679 = AXIS2_PLACEMENT_3D ( 'NONE', #82928, #55165, #20687 ) ;
#69680 = CARTESIAN_POINT ( 'NONE',  ( 102.8925193805077498, -44.76628084087394654, 166.6057531614099503 ) ) ;
#69681 = ADVANCED_FACE ( 'NONE', ( #87030 ), #24795, .T. ) ;
#69683 = ORIENTED_EDGE ( 'NONE', *, *, #39987, .F. ) ;
#69682 = CARTESIAN_POINT ( 'NONE',  ( 223.2659999999999911, 52.73749999999999716, -44.45000000000000284 ) ) ;
#69684 = CARTESIAN_POINT ( 'NONE',  ( -30.89999999999999858, 53.97499999999997300, 60.80000000000001137 ) ) ;
#69685 = CARTESIAN_POINT ( 'NONE',  ( 105.7232414704440941, -24.98023492732646744, 156.1670538473399574 ) ) ;
#69686 = CARTESIAN_POINT ( 'NONE',  ( 117.0724543456819902, -35.46712184163512660, 149.9277079111001854 ) ) ;
#69687 = LINE ( 'NONE', #36516, #77714 ) ;
#69688 = CARTESIAN_POINT ( 'NONE',  ( 97.33920838924730390, -34.06551626165290969, 87.11420987653328041 ) ) ;
#69689 = EDGE_CURVE ( 'NONE', #77142, #46008, #47533, .T. ) ;
#69690 = EDGE_CURVE ( 'NONE', #36508, #19483, #8399, .T. ) ;
#69691 = CARTESIAN_POINT ( 'NONE',  ( 86.06670390244796920, -58.72944715994112386, 198.9178068554149945 ) ) ;
#69692 = LINE ( 'NONE', #20205, #19307 ) ;
#69693 = CARTESIAN_POINT ( 'NONE',  ( 114.7602587138392920, -43.68247563549513046, 83.25372051400698581 ) ) ;
#69694 = EDGE_LOOP ( 'NONE', ( #57546, #77543, #51332, #39756 ) ) ;
#69695 = AXIS2_PLACEMENT_3D ( 'NONE', #21579, #69268, #35633 ) ;
#69696 = VERTEX_POINT ( 'NONE', #26577 ) ;
#69697 = VERTEX_POINT ( 'NONE', #7038 ) ;
#69698 = ADVANCED_FACE ( 'NONE', ( #81573 ), #27246, .F. ) ;
#69699 = CARTESIAN_POINT ( 'NONE',  ( 109.9481718979998277, -45.67217584368548700, 54.26824997256396443 ) ) ;
#69700 = CARTESIAN_POINT ( 'NONE',  ( 127.4058501689331280, -122.7870702624433221, 250.2178068554179902 ) ) ;
#69702 = CARTESIAN_POINT ( 'NONE',  ( -31.75000000000000000, 124.5870000000000033, -3.175000000000219647 ) ) ;
#69701 = CARTESIAN_POINT ( 'NONE',  ( 98.80555182512732415, -41.96590078842027793, 182.7756252759109543 ) ) ;
#69703 = CARTESIAN_POINT ( 'NONE',  ( 97.06103120714826105, -37.99613185989743869, 56.42650901886334935 ) ) ;
#69704 = ADVANCED_FACE ( 'NONE', ( #26141 ), #12513, .F. ) ;
#69705 = DIRECTION ( 'NONE',  ( -1.000000000000000000, -1.000000000000000078E-15, 0.000000000000000000 ) ) ;
#69706 = CYLINDRICAL_SURFACE ( 'NONE', #19945, 9.999999999999998224 ) ;
#69707 = AXIS2_PLACEMENT_3D ( 'NONE', #84256, #35628, #22030 ) ;
#69708 = DIRECTION ( 'NONE',  ( 0.7071067811865507924, 0.7071067811865441310, 0.000000000000000000 ) ) ;
#69709 = DIRECTION ( 'NONE',  ( -1.665334536937733296E-13, -1.000000000000000000, 0.000000000000000000 ) ) ;
#69710 = CARTESIAN_POINT ( 'NONE',  ( 113.9025887763448566, -28.07314977735658701, 124.5565776568629559 ) ) ;
#69711 = ORIENTED_EDGE ( 'NONE', *, *, #82900, .F. ) ;
#69712 = VERTEX_POINT ( 'NONE', #13408 ) ;
#69714 = ORIENTED_EDGE ( 'NONE', *, *, #24481, .T. ) ;
#69713 = ADVANCED_FACE ( 'NONE', ( #88823 ), #19771, .F. ) ;
#69715 = VECTOR ( 'NONE', #66866, 1000.000000000000000 ) ;
#69716 = CARTESIAN_POINT ( 'NONE',  ( 11.89174298505462524, 78.07232539501590907, 130.0133884065672589 ) ) ;
#69717 = CARTESIAN_POINT ( 'NONE',  ( 145.8234706062852979, -69.06773314681258569, 247.3490213069128458 ) ) ;
#69718 = CARTESIAN_POINT ( 'NONE',  ( 107.0664832912739399, -36.72944715994095333, 312.1356252759112522 ) ) ;
#69719 = CARTESIAN_POINT ( 'NONE',  ( 100.1721853667017825, -41.09961673838238028, 184.5938046553059735 ) ) ;
#69720 = CIRCLE ( 'NONE', #45047, 3.174999999999983391 ) ;
#69721 = DIRECTION ( 'NONE',  ( 3.100000000000000258E-29, -3.100000000000000044E-14, -1.000000000000000000 ) ) ;
#69722 = CARTESIAN_POINT ( 'NONE',  ( 193.0374249753374443, -23.42844715993432558, 300.4678068554149490 ) ) ;
#69723 = ORIENTED_EDGE ( 'NONE', *, *, #27585, .F. ) ;
#69725 = ORIENTED_EDGE ( 'NONE', *, *, #83033, .T. ) ;
#69724 = ORIENTED_EDGE ( 'NONE', *, *, #62631, .F. ) ;
#69726 = AXIS2_PLACEMENT_3D ( 'NONE', #23187, #55852, #2273 ) ;
#69727 = DIRECTION ( 'NONE',  ( 4.299999999999999979E-14, -1.000000000000000000, 4.400000000000000367E-29 ) ) ;
#69728 = VERTEX_POINT ( 'NONE', #34281 ) ;
#69729 = ORIENTED_EDGE ( 'NONE', *, *, #72456, .F. ) ;
#69730 = CARTESIAN_POINT ( 'NONE',  ( 78.11989406983862239, -20.67261125154402990, 7.590611884336022186 ) ) ;
#69731 = ADVANCED_FACE ( 'NONE', ( #60638 ), #68815, .T. ) ;
#69732 = CARTESIAN_POINT ( 'NONE',  ( 98.31652346514815122, -35.14820314722400241, 237.6158690201829415 ) ) ;
#69733 = LINE ( 'NONE', #25354, #86066 ) ;
#69734 = ORIENTED_EDGE ( 'NONE', *, *, #42745, .F. ) ;
#69735 = EDGE_CURVE ( 'NONE', #70474, #14878, #55920, .T. ) ;
#69736 = CARTESIAN_POINT ( 'NONE',  ( 172.5667039024480687, -42.82844715993500273, 300.4678068554149490 ) ) ;
#69737 = CARTESIAN_POINT ( 'NONE',  ( -123.8170101655531425, 72.35301567669330325, 41.40434455345861409 ) ) ;
#69738 = ORIENTED_EDGE ( 'NONE', *, *, #24101, .T. ) ;
#69739 = ORIENTED_EDGE ( 'NONE', *, *, #7485, .T. ) ;
#69740 = FACE_OUTER_BOUND ( 'NONE', #17186, .T. ) ;
#69741 = ORIENTED_EDGE ( 'NONE', *, *, #14214, .F. ) ;
#69742 = VERTEX_POINT ( 'NONE', #1575 ) ;
#69743 = VECTOR ( 'NONE', #63706, 1000.000000000000000 ) ;
#69744 = CARTESIAN_POINT ( 'NONE',  ( 105.3241794147103008, -28.72650611001668608, 258.0652332267344491 ) ) ;
#69745 = CARTESIAN_POINT ( 'NONE',  ( 103.1663722902654001, -27.03741444506403724, 130.3813395616259925 ) ) ;
#69746 = CARTESIAN_POINT ( 'NONE',  ( 117.8338636819851644, -39.12263375953642708, 103.6403871806729455 ) ) ;
#69747 = DIRECTION ( 'NONE',  ( 1.000000000000000000, 4.163336342344333240E-14, 0.000000000000000000 ) ) ;
#69748 = DIRECTION ( 'NONE',  ( -1.000000000000000078E-15, 1.000000000000000083E-30, 1.000000000000000000 ) ) ;
#69749 = CARTESIAN_POINT ( 'NONE',  ( 114.6054725695487946, -29.52902160936550047, 230.4327681330539690 ) ) ;
#69750 = DIRECTION ( 'NONE',  ( 1.000000000000000000, 4.163336342344333240E-14, 0.000000000000000000 ) ) ;
#69751 = DIRECTION ( 'NONE',  ( 1.000000000000000078E-15, -1.000000000000000083E-30, -1.000000000000000000 ) ) ;
#69752 = ORIENTED_EDGE ( 'NONE', *, *, #58987, .T. ) ;
#69753 = CARTESIAN_POINT ( 'NONE',  ( 130.2664984484595720, 73.28356282573680858, 8.694507028641202950 ) ) ;
#69754 = ORIENTED_EDGE ( 'NONE', *, *, #61859, .T. ) ;
#69755 = ORIENTED_EDGE ( 'NONE', *, *, #23161, .T. ) ;
#69756 = DIRECTION ( 'NONE',  ( -0.9254794337955620787, -0.3787978585227822492, 0.000000000000000000 ) ) ;
#69757 = CONICAL_SURFACE ( 'NONE', #55263, 1.624999999999987566, 1.029744258676650093 ) ;
#69758 = CARTESIAN_POINT ( 'NONE',  ( 103.2779695159621696, -27.47487189271723196, 136.3856721692480107 ) ) ;
#69759 = CIRCLE ( 'NONE', #17558, 4.762500000000001066 ) ;
#69760 = EDGE_LOOP ( 'NONE', ( #23206, #83083, #49612, #87298, #25162, #37006, #60352, #56659 ) ) ;
#69761 = CARTESIAN_POINT ( 'NONE',  ( 108.2767148518004490, -26.33900702273897565, 129.9841967044819739 ) ) ;
#69762 = CARTESIAN_POINT ( 'NONE',  ( 98.35067341706619004, -31.65512452754220263, 255.9063942260654869 ) ) ;
#69763 = CYLINDRICAL_SURFACE ( 'NONE', #68119, 5.000000000000004441 ) ;
#69764 = CYLINDRICAL_SURFACE ( 'NONE', #80433, 12.59999999999999964 ) ;
#69767 = CARTESIAN_POINT ( 'NONE',  ( 115.0380569359701326, -30.04493676975927485, 265.3813395616251682 ) ) ;
#69766 = CARTESIAN_POINT ( 'NONE',  ( 98.12663683250418956, -41.21668256917149620, 56.69630050190792758 ) ) ;
#69765 = CARTESIAN_POINT ( 'NONE',  ( 182.2420472961719895, -31.76306994223730840, -5.074374724088000832 ) ) ;
#69768 = CYLINDRICAL_SURFACE ( 'NONE', #71296, 118.3560000000000088 ) ;
#69769 = DIRECTION ( 'NONE',  ( 0.000000000000000000, 0.000000000000000000, -1.000000000000000000 ) ) ;
#69770 = VERTEX_POINT ( 'NONE', #22917 ) ;
#69771 = CARTESIAN_POINT ( 'NONE',  ( 134.0664832912740110, -41.22944715994101017, 4.925625275910997303 ) ) ;
#69772 = CARTESIAN_POINT ( 'NONE',  ( 163.0667039024470171, -32.29483332968611364, -5.074374724088000832 ) ) ;
#69773 = AXIS2_PLACEMENT_3D ( 'NONE', #35159, #41967, #62870 ) ;
#69774 = CYLINDRICAL_SURFACE ( 'NONE', #26032, 0.2500000000000002220 ) ;
#69775 = VECTOR ( 'NONE', #29381, 1000.000000000000000 ) ;
#69777 = ORIENTED_EDGE ( 'NONE', *, *, #37622, .T. ) ;
#69776 = CARTESIAN_POINT ( 'NONE',  ( 99.99420790045508056, -28.96206233275049158, 285.6641967044822650 ) ) ;
#69778 = CARTESIAN_POINT ( 'NONE',  ( -40.89999999999999858, 53.97500000000000142, 50.79999999999999716 ) ) ;
#69779 = CARTESIAN_POINT ( 'NONE',  ( 102.9045757522767843, -27.10877478265368623, 155.4013395616249795 ) ) ;
#69780 = CARTESIAN_POINT ( 'NONE',  ( 104.4907123320104461, -46.86782655419724364, 43.37848241876896083 ) ) ;
#69781 = CARTESIAN_POINT ( 'NONE',  ( 96.69998679698829847, -35.27043030541812385, 177.2156252759109805 ) ) ;
#69782 = CARTESIAN_POINT ( 'NONE',  ( 100.9546726858703920, -28.70702582103217182, 31.59395862158653046 ) ) ;
#69783 = CARTESIAN_POINT ( 'NONE',  ( 113.2453581294647478, -28.75857153267794075, 100.5523746408958061 ) ) ;
#69785 = CYLINDRICAL_SURFACE ( 'NONE', #32625, 0.4999999999999933387 ) ;
#69784 = DIRECTION ( 'NONE',  ( 1.000000000000000000, 1.000000000000000078E-15, 0.000000000000000000 ) ) ;
#69786 = CYLINDRICAL_SURFACE ( 'NONE', #36554, 10.00000000000000888 ) ;
#69787 = CARTESIAN_POINT ( 'NONE',  ( 41.56648329127399677, -9.303447159940999356, 261.0426252759119734 ) ) ;
#69788 = ORIENTED_EDGE ( 'NONE', *, *, #66951, .T. ) ;
#69789 = VECTOR ( 'NONE', #22195, 1000.000000000000000 ) ;
#69790 = CARTESIAN_POINT ( 'NONE',  ( 172.5664832912740110, -27.82844715994070484, 263.6756252759120116 ) ) ;
#69791 = ADVANCED_FACE ( 'NONE', ( #21573 ), #36085, .F. ) ;
#69792 = ORIENTED_EDGE ( 'NONE', *, *, #53755, .T. ) ;
#69793 = EDGE_CURVE ( 'NONE', #53364, #55247, #83884, .T. ) ;
#69794 = ORIENTED_EDGE ( 'NONE', *, *, #52302, .T. ) ;
#69795 = VECTOR ( 'NONE', #64384, 1000.000000000000000 ) ;
#69796 = EDGE_CURVE ( 'NONE', #50035, #12421, #22465, .T. ) ;
#69797 = VERTEX_POINT ( 'NONE', #83797 ) ;
#69798 = CARTESIAN_POINT ( 'NONE',  ( 117.9791962420229794, -38.33460093242096178, 69.72229194257801055 ) ) ;
#69799 = CARTESIAN_POINT ( 'NONE',  ( 41.56648329127399677, -9.303447159940999356, 196.8086252759119645 ) ) ;
#69800 = AXIS2_PLACEMENT_3D ( 'NONE', #49962, #37252, #41019 ) ;
#69801 = DIRECTION ( 'NONE',  ( -1.150535366796005147E-15, 1.000000000000000000, -3.100000000000000044E-14 ) ) ;
#69802 = EDGE_CURVE ( 'NONE', #49324, #39002, #15649, .T. ) ;
#69803 = CARTESIAN_POINT ( 'NONE',  ( 96.60651355459405920, -37.15606806638657389, 157.3584824187679487 ) ) ;
#69804 = CARTESIAN_POINT ( 'NONE',  ( 117.8597870418416562, -34.07357964055000821, 14.01848241876896317 ) ) ;
#69805 = EDGE_LOOP ( 'NONE', ( #66792, #55775, #30936, #48344, #23193, #55510, #83183, #59543, #4162, #48472, #71267, #59933, #24076, #27029 ) ) ;
#69806 = ORIENTED_EDGE ( 'NONE', *, *, #22224, .T. ) ;
#69807 = VERTEX_POINT ( 'NONE', #78338 ) ;
#69808 = EDGE_CURVE ( 'NONE', #59384, #62421, #76978, .T. ) ;
#69809 = ORIENTED_EDGE ( 'NONE', *, *, #73899, .T. ) ;
#69810 = CARTESIAN_POINT ( 'NONE',  ( 71.24162159452610865, 0.6420441417434794573, 540.9756252759101471 ) ) ;
#69811 = LINE ( 'NONE', #7584, #88402 ) ;
#69812 = DIRECTION ( 'NONE',  ( 0.2588190451025269012, 0.000000000000000000, -0.9659258262890665359 ) ) ;
#69813 = CARTESIAN_POINT ( 'NONE',  ( 80.06648329127398256, -9.029447159941060619, 8.225625275910942946 ) ) ;
#69814 = CARTESIAN_POINT ( 'NONE',  ( 100.5877680347015399, 85.83513192049082363, 83.22850972642827116 ) ) ;
#69815 = FACE_OUTER_BOUND ( 'NONE', #85394, .T. ) ;
#69816 = EDGE_CURVE ( 'NONE', #87073, #1742, #14761, .T. ) ;
#69817 = DIRECTION ( 'NONE',  ( -0.7071067811865197061, -0.7071067811865753283, -7.071067811865190357E-16 ) ) ;
#69818 = AXIS2_PLACEMENT_3D ( 'NONE', #70015, #15052, #55454 ) ;
#69819 = CARTESIAN_POINT ( 'NONE',  ( -11.87509116337306025, 87.05477402842780066, 130.0148473914468639 ) ) ;
#69820 = CARTESIAN_POINT ( 'NONE',  ( 112.0124476237221103, -28.73397683645135814, 289.6356252759109680 ) ) ;
#69821 = PLANE ( 'NONE',  #87885 ) ;
#69823 = ORIENTED_EDGE ( 'NONE', *, *, #4248, .F. ) ;
#69822 = EDGE_CURVE ( 'NONE', #48773, #81111, #63797, .T. ) ;
#69824 = DIRECTION ( 'NONE',  ( 1.000000000000000078E-15, -1.000000000000000000, 0.000000000000000000 ) ) ;
#69825 = CARTESIAN_POINT ( 'NONE',  ( -55.92138610381699948, 55.69374223142005320, 70.72646601424236223 ) ) ;
#69826 = CARTESIAN_POINT ( 'NONE',  ( 113.4089301560035068, -41.86784124614906233, 86.10237608387694763 ) ) ;
#69827 = VECTOR ( 'NONE', #57549, 1000.000000000000000 ) ;
#69828 = CARTESIAN_POINT ( 'NONE',  ( 72.96458098368701428, 127.0000000000000000, -72.96458098368670164 ) ) ;
#69829 = DIRECTION ( 'NONE',  ( -0.7071067811865279218, 0.7071067811865670016, -2.899137802865041747E-29 ) ) ;
#69830 = ORIENTED_EDGE ( 'NONE', *, *, #73179, .T. ) ;
#69831 = ORIENTED_EDGE ( 'NONE', *, *, #61982, .T. ) ;
#69832 = CARTESIAN_POINT ( 'NONE',  ( 79.05226586200586780, -34.17316201338598347, 8.065992442480940383 ) ) ;
#69833 = ORIENTED_EDGE ( 'NONE', *, *, #67788, .F. ) ;
#69834 = ORIENTED_EDGE ( 'NONE', *, *, #49569, .T. ) ;
#69835 = VECTOR ( 'NONE', #78880, 999.9999999999998863 ) ;
#69836 = CARTESIAN_POINT ( 'NONE',  ( 105.7154773740255251, -46.72385839776377026, 68.46895861271767103 ) ) ;
#69837 = CARTESIAN_POINT ( 'NONE',  ( 103.2835872187480533, -45.32980894545860906, 128.6663452106589887 ) ) ;
#69838 = CARTESIAN_POINT ( 'NONE',  ( 99.65722331657703137, -39.76205027262535907, 10.08425333485812025 ) ) ;
#69839 = EDGE_CURVE ( 'NONE', #88397, #75550, #44680, .T. ) ;
#69840 = CARTESIAN_POINT ( 'NONE',  ( 113.4285887376619968, -27.66253919562607422, 80.57753003781597556 ) ) ;
#69841 = VECTOR ( 'NONE', #71133, 1000.000000000000000 ) ;
#69842 = CARTESIAN_POINT ( 'NONE',  ( 112.0659116089343996, -45.48839626851365381, 83.98979194134383874 ) ) ;
#69843 = VERTEX_POINT ( 'NONE', #35627 ) ;
#69844 = CYLINDRICAL_SURFACE ( 'NONE', #55577, 2.999999999999988898 ) ;
#69845 = VERTEX_POINT ( 'NONE', #56962 ) ;
#69846 = VERTEX_POINT ( 'NONE', #62441 ) ;
#69847 = CIRCLE ( 'NONE', #77114, 5.035202529042049235 ) ;
#69848 = DIRECTION ( 'NONE',  ( 0.000000000000000000, 1.000000000000000000, 0.000000000000000000 ) ) ;
#69849 = EDGE_LOOP ( 'NONE', ( #61504, #76089, #73271, #74005, #80335, #27134 ) ) ;
#69850 = CARTESIAN_POINT ( 'NONE',  ( 116.7892270726677140, -35.66563809581925426, 278.9127681330543851 ) ) ;
#69851 = CARTESIAN_POINT ( 'NONE',  ( 96.03095270115332482, -35.77956804193283347, 182.2461014663869889 ) ) ;
#69852 = CARTESIAN_POINT ( 'NONE',  ( 8.383266637423213652, 73.00087262779534569, -118.2596760195012848 ) ) ;
#69853 = DIRECTION ( 'NONE',  ( 1.000000000000000000, -0.000000000000000000, -0.000000000000000000 ) ) ;
#69854 = CARTESIAN_POINT ( 'NONE',  ( 117.6790090996954632, -39.81947568642139856, 134.5889586092439743 ) ) ;
#69855 = VECTOR ( 'NONE', #32537, 1000.000000000000000 ) ;
#69856 = LINE ( 'NONE', #8528, #11750 ) ;
#69857 = EDGE_LOOP ( 'NONE', ( #42438, #58978, #9080, #1130 ) ) ;
#69858 = CARTESIAN_POINT ( 'NONE',  ( 0.000000000000000000, 103.1240000000000236, 0.000000000000000000 ) ) ;
#69859 = ADVANCED_FACE ( 'NONE', ( #27918 ), #63342, .T. ) ;
#69860 = DIRECTION ( 'NONE',  ( 0.000000000000000000, 1.000000000000000000, 0.000000000000000000 ) ) ;
#69861 = EDGE_LOOP ( 'NONE', ( #31425, #8676, #61614, #26480, #43457, #11785, #38066, #73168, #43098, #16703, #71265, #54525, #19452, #66747, #85621, #82930 ) ) ;
#69862 = EDGE_CURVE ( 'NONE', #53716, #20346, #87320, .T. ) ;
#69863 = DIRECTION ( 'NONE',  ( 1.000000000000000078E-15, -1.000000000000000000, 3.100000000000000044E-14 ) ) ;
#69864 = CARTESIAN_POINT ( 'NONE',  ( 2.859107348890838729, 94.82819007650195431, 118.5222036340525591 ) ) ;
#69865 = CARTESIAN_POINT ( 'NONE',  ( 100.5506404981706510, -27.80068015945615656, 30.56610146638794134 ) ) ;
#69866 = CARTESIAN_POINT ( 'NONE',  ( 127.4058501689331280, -85.76982405743856930, 249.2178068554179902 ) ) ;
#69867 = DIRECTION ( 'NONE',  ( 0.000000000000000000, -1.000000000000000000, 0.000000000000000000 ) ) ;
#69868 = CARTESIAN_POINT ( 'NONE',  ( 0.000000000000000000, 224.4999999999999432, 164.6557476874258441 ) ) ;
#69869 = CARTESIAN_POINT ( 'NONE',  ( 101.2965385564679792, -30.39239502954603367, 285.0867055423626084 ) ) ;
#69871 = CARTESIAN_POINT ( 'NONE',  ( 109.0680860650138300, -47.57644715601873742, 123.7337205140059666 ) ) ;
#69870 = DIRECTION ( 'NONE',  ( -0.8660254037844392627, 0.4999999999999990008, -1.549999999999999706E-14 ) ) ;
#69872 = DIRECTION ( 'NONE',  ( 3.999999999999999995E-14, -1.000000000000000000, 4.100000000000000342E-29 ) ) ;
#69873 = DIRECTION ( 'NONE',  ( -1.000000000000000000, 0.000000000000000000, 0.000000000000000000 ) ) ;
#69874 = EDGE_LOOP ( 'NONE', ( #46541, #1316, #68555, #75277, #48798, #65504 ) ) ;
#69875 = LINE ( 'NONE', #15371, #9154 ) ;
#69876 = AXIS2_PLACEMENT_3D ( 'NONE', #55664, #71587, #9347 ) ;
#69877 = CARTESIAN_POINT ( 'NONE',  ( 109.6522639851457228, 49.12997694320977615, 70.86078145649237570 ) ) ;
#69878 = CARTESIAN_POINT ( 'NONE',  ( 136.6003823147690355, -35.66080131299383993, 2.811527311783425187 ) ) ;
#69879 = ORIENTED_EDGE ( 'NONE', *, *, #14957, .F. ) ;
#69880 = DIRECTION ( 'NONE',  ( 0.000000000000000000, 0.000000000000000000, -1.000000000000000000 ) ) ;
#69882 = ORIENTED_EDGE ( 'NONE', *, *, #12979, .T. ) ;
#69881 = CARTESIAN_POINT ( 'NONE',  ( 98.05257159168807846, -42.12399974224388188, 161.7556252759109725 ) ) ;
#69883 = FACE_OUTER_BOUND ( 'NONE', #44694, .T. ) ;
#69884 = CARTESIAN_POINT ( 'NONE',  ( 118.0739042565516712, -35.49579832924209910, 229.9032443235299468 ) ) ;
#69885 = CARTESIAN_POINT ( 'NONE',  ( 97.73362116697985869, -31.98701483920769206, 46.95276813305393659 ) ) ;
#69886 = DIRECTION ( 'NONE',  ( -0.7071067811868642083, -0.7071067811862309371, -7.071067811868635707E-16 ) ) ;
#69887 = VECTOR ( 'NONE', #46280, 1000.000000000000000 ) ;
#69888 = CARTESIAN_POINT ( 'NONE',  ( 97.81461822720238786, -40.51595288653417981, 132.6359866545674890 ) ) ;
#69889 = FACE_OUTER_BOUND ( 'NONE', #26414, .T. ) ;
#69890 = ORIENTED_EDGE ( 'NONE', *, *, #46666, .T. ) ;
#69891 = AXIS2_PLACEMENT_3D ( 'NONE', #10636, #71987, #17461 ) ;
#69892 = ITEM_DEFINED_TRANSFORMATION ( 'NONE', 'NONE', #66667,  #50656 ) ;
#69893 = EDGE_CURVE ( 'NONE', #82764, #17557, #51587, .T. ) ;
#69894 = VERTEX_POINT ( 'NONE', #57863 ) ;
#69895 = EDGE_CURVE ( 'NONE', #67030, #74870, #52786, .T. ) ;
#69896 = ORIENTED_EDGE ( 'NONE', *, *, #20194, .F. ) ;
#69897 = EDGE_CURVE ( 'NONE', #18950, #8582, #53349, .T. ) ;
#69898 = ORIENTED_EDGE ( 'NONE', *, *, #24256, .T. ) ;
#69899 = DIRECTION ( 'NONE',  ( 0.000000000000000000, 1.000000000000000000, 0.000000000000000000 ) ) ;
#69900 = CARTESIAN_POINT ( 'NONE',  ( 117.3348620442827865, -34.92864588493001321, 239.9641967044819637 ) ) ;
#69901 = CARTESIAN_POINT ( 'NONE',  ( -479.3614999999999782, 86.51875000000001137, 94.61194598552339130 ) ) ;
#69902 = CARTESIAN_POINT ( 'NONE',  ( 136.8164482479830895, -18.55833207211816926, 3.101428811466735880 ) ) ;
#69903 = VECTOR ( 'NONE', #71717, 1000.000000000000000 ) ;
#69904 = EDGE_CURVE ( 'NONE', #1995, #45788, #65127, .T. ) ;
#69906 = DIRECTION ( 'NONE',  ( 0.000000000000000000, 0.000000000000000000, -1.000000000000000000 ) ) ;
#69905 = DIRECTION ( 'NONE',  ( -1.000000000000000000, 0.000000000000000000, 0.000000000000000000 ) ) ;
#69907 = CARTESIAN_POINT ( 'NONE',  ( 142.0664832912739826, -8.729447159940995959, 14.92562527591100618 ) ) ;
#69908 = CARTESIAN_POINT ( 'NONE',  ( 117.4065409050533617, -38.22262247076111663, 28.71276813305395592 ) ) ;
#69909 = EDGE_LOOP ( 'NONE', ( #27095, #75334, #80675, #74221 ) ) ;
#69910 = AXIS2_PLACEMENT_3D ( 'NONE', #84653, #48742, #49647 ) ;
#69911 = ORIENTED_EDGE ( 'NONE', *, *, #28768, .T. ) ;
#69912 = EDGE_CURVE ( 'NONE', #47987, #39785, #73309, .T. ) ;
#69913 = VECTOR ( 'NONE', #80962, 1000.000000000000000 ) ;
#69914 = PRESENTATION_STYLE_ASSIGNMENT (( #14954 ) ) ;
#69915 = CYLINDRICAL_SURFACE ( 'NONE', #47709, 4.762500000000001066 ) ;
#69916 = CARTESIAN_POINT ( 'NONE',  ( 99.40370404213548738, -29.74227323812501211, 226.7261014663869503 ) ) ;
#69917 = ADVANCED_FACE ( 'NONE', ( #75525 ), #82354, .F. ) ;
#69918 = AXIS2_PLACEMENT_3D ( 'NONE', #51643, #30771, #58461 ) ;
#69919 = DIRECTION ( 'NONE',  ( -1.000000000000000078E-15, 1.000000000000000000, 0.000000000000000000 ) ) ;
#69920 = CARTESIAN_POINT ( 'NONE',  ( 114.1038288540492687, -43.56973530630599356, 94.21276813305296116 ) ) ;
#69921 = CARTESIAN_POINT ( 'NONE',  ( 98.30749153155636577, -41.72877165996427351, 31.74000518241274804 ) ) ;
#69922 = CARTESIAN_POINT ( 'NONE',  ( 103.2818408434572177, -27.47328781080362248, 21.38533937723293477 ) ) ;
#69923 = ORIENTED_EDGE ( 'NONE', *, *, #33251, .F. ) ;
#69924 = DIRECTION ( 'NONE',  ( 0.000000000000000000, 0.000000000000000000, 1.000000000000000000 ) ) ;
#69925 = VECTOR ( 'NONE', #58863, 1000.000000000000000 ) ;
#69926 = EDGE_LOOP ( 'NONE', ( #55, #24014, #76255, #62279, #59747 ) ) ;
#69927 = ORIENTED_EDGE ( 'NONE', *, *, #80457, .T. ) ;
#69928 = CARTESIAN_POINT ( 'NONE',  ( -75.37293521528297902, 88.18374315479975678, 91.51255889651606878 ) ) ;
#69929 = CARTESIAN_POINT ( 'NONE',  ( 110.2543409660563043, -27.89122963701645830, 246.2206309249449703 ) ) ;
#69930 = CARTESIAN_POINT ( 'NONE',  ( 99.04406178633300328, -42.84125754617969051, 191.8439585998989685 ) ) ;
#69931 = CARTESIAN_POINT ( 'NONE',  ( -117.9083627453486827, 85.43299024555680887, 12.37536754217487101 ) ) ;
#69932 = CYLINDRICAL_SURFACE ( 'NONE', #17163, 3.999999999999998224 ) ;
#69933 = DIRECTION ( 'NONE',  ( 1.000000000000000000, 0.000000000000000000, 0.000000000000000000 ) ) ;
#69934 = ORIENTED_EDGE ( 'NONE', *, *, #23151, .F. ) ;
#69935 = LINE ( 'NONE', #42207, #24687 ) ;
#69936 = DIRECTION ( 'NONE',  ( 0.000000000000000000, 0.000000000000000000, 1.000000000000000000 ) ) ;
#69937 = ORIENTED_EDGE ( 'NONE', *, *, #6692, .F. ) ;
#69938 = CARTESIAN_POINT ( 'NONE',  ( 104.4906584979394211, -46.86803844812923359, 47.37848241876796607 ) ) ;
#69939 = EDGE_LOOP ( 'NONE', ( #37655, #68951, #73870, #32556 ) ) ;
#69940 = CARTESIAN_POINT ( 'NONE',  ( 112.8202834993214481, -29.45004372636961065, 272.3623760838771091 ) ) ;
#69941 = DIRECTION ( 'NONE',  ( 0.000000000000000000, 0.000000000000000000, 1.000000000000000000 ) ) ;
#69942 = CARTESIAN_POINT ( 'NONE',  ( 109.4488926988246646, -27.20905326525207357, 199.8813395616259925 ) ) ;
#69943 = DIRECTION ( 'NONE',  ( 1.000000000000000000, 0.000000000000000000, 0.000000000000000000 ) ) ;
#69944 = CARTESIAN_POINT ( 'NONE',  ( 95.05156358570199870, -41.69348830286664764, 289.6356252759107406 ) ) ;
#69945 = DIRECTION ( 'NONE',  ( 1.110223024625155531E-13, -1.000000000000000000, 0.000000000000000000 ) ) ;
#69946 = CIRCLE ( 'NONE', #53895, 8.636000000000004562 ) ;
#69947 = EDGE_CURVE ( 'NONE', #11982, #60807, #34575, .T. ) ;
#69948 = CARTESIAN_POINT ( 'NONE',  ( 61.56670390244639890, -23.42844715994043270, 129.9678068554150911 ) ) ;
#69949 = CARTESIAN_POINT ( 'NONE',  ( 115.9437545354735306, -30.06674848629992880, 260.3508633711495008 ) ) ;
#69950 = CARTESIAN_POINT ( 'NONE',  ( 74.43373480440749290, 84.21498941703526953, -92.27768215249952277 ) ) ;
#69951 = ORIENTED_EDGE ( 'NONE', *, *, #89872, .F. ) ;
#69952 = AXIS2_PLACEMENT_3D ( 'NONE', #4365, #30725, #81133 ) ;
#69953 = DIRECTION ( 'NONE',  ( 0.000000000000000000, 0.000000000000000000, 1.000000000000000000 ) ) ;
#69954 = ORIENTED_EDGE ( 'NONE', *, *, #79427, .F. ) ;
#69955 = CARTESIAN_POINT ( 'NONE',  ( 111.0993040117788979, -25.53357873718133320, 95.80133956162495679 ) ) ;
#69956 = CARTESIAN_POINT ( 'NONE',  ( 124.3636858901310802, 46.33258218398187722, -39.73348582418787345 ) ) ;
#69957 = ORIENTED_EDGE ( 'NONE', *, *, #28661, .T. ) ;
#69958 = DIRECTION ( 'NONE',  ( 0.000000000000000000, -1.000000000000000000, 0.000000000000000000 ) ) ;
#69959 = ORIENTED_EDGE ( 'NONE', *, *, #49290, .T. ) ;
#69960 = ORIENTED_EDGE ( 'NONE', *, *, #47730, .T. ) ;
#69961 = CYLINDRICAL_SURFACE ( 'NONE', #44949, 10.00000000000000888 ) ;
#69962 = CARTESIAN_POINT ( 'NONE',  ( 184.5667039024480118, -48.82844715994099971, 310.9178068554150514 ) ) ;
#69963 = CARTESIAN_POINT ( 'NONE',  ( 183.5150000000000148, 52.73749999999999716, -62.78087104677060637 ) ) ;
#69964 = CARTESIAN_POINT ( 'NONE',  ( 63.06670390244794078, -40.32844715994017548, 300.4678068554150627 ) ) ;
#69965 = LINE ( 'NONE', #54502, #22901 ) ;
#69966 = CARTESIAN_POINT ( 'NONE',  ( 116.5562423158612972, -42.44168660689859962, 274.3832443235299365 ) ) ;
#69967 = VECTOR ( 'NONE', #81232, 1000.000000000000000 ) ;
#69968 = LINE ( 'NONE', #471, #55157 ) ;
#69969 = ORIENTED_EDGE ( 'NONE', *, *, #86116, .T. ) ;
#69970 = CARTESIAN_POINT ( 'NONE',  ( 12.37510959950097877, 79.66588461411475919, 117.9083898578959833 ) ) ;
#69971 = CARTESIAN_POINT ( 'NONE',  ( 80.48314995794039817, 12.92155284005802685, 349.2756252759109543 ) ) ;
#69972 = VERTEX_POINT ( 'NONE', #53697 ) ;
#69973 = EDGE_LOOP ( 'NONE', ( #15730, #69675 ) ) ;
#69975 = EDGE_CURVE ( 'NONE', #76954, #67284, #4692, .T. ) ;
#69974 = VECTOR ( 'NONE', #10307, 1000.000000000000000 ) ;
#69976 = CARTESIAN_POINT ( 'NONE',  ( 81.55985452235577782, -21.04079274305108527, 1.981704437698954768 ) ) ;
#69977 = FACE_OUTER_BOUND ( 'NONE', #52917, .T. ) ;
#69978 = CARTESIAN_POINT ( 'NONE',  ( 97.79631277754322127, -40.47965291819907918, 16.63237950705615731 ) ) ;
#69979 = CARTESIAN_POINT ( 'NONE',  ( 72.96458098368701428, 127.0000000000000000, -80.90208098368670164 ) ) ;
#69980 = CARTESIAN_POINT ( 'NONE',  ( 122.2221484686747459, -111.8737466215628018, -19.26696060647578435 ) ) ;
#69981 = CARTESIAN_POINT ( 'NONE',  ( 112.5429177363308924, -43.28420096851815657, 192.5524198280769781 ) ) ;
#69982 = CIRCLE ( 'NONE', #19204, 5.041900000000000048 ) ;
#69983 = CARTESIAN_POINT ( 'NONE',  ( 113.3411949225463502, -28.30449682957925717, 104.5670538473399347 ) ) ;
#69984 = VERTEX_POINT ( 'NONE', #54143 ) ;
#69985 = LINE ( 'NONE', #70893, #48033 ) ;
#69986 = ORIENTED_EDGE ( 'NONE', *, *, #8773, .F. ) ;
#69987 = CARTESIAN_POINT ( 'NONE',  ( 263.3306968374159851, 52.73749999999999716, -2.032000000000000028 ) ) ;
#69988 = ORIENTED_EDGE ( 'NONE', *, *, #73501, .F. ) ;
#69989 = PRODUCT_DEFINITION ( 'UNKNOWN', '', #21763, #70549 ) ;
#69990 = CARTESIAN_POINT ( 'NONE',  ( 97.07203916560013113, -35.37876108158648947, 262.2190116196141503 ) ) ;
#69991 = ORIENTED_EDGE ( 'NONE', *, *, #87642, .F. ) ;
#69992 = CARTESIAN_POINT ( 'NONE',  ( 165.6738106836030227, -28.98061976758901892, -5.074374724088000832 ) ) ;
#69993 = CARTESIAN_POINT ( 'NONE',  ( 186.6899999999999977, 59.08750000000000568, -50.79999999999999716 ) ) ;
#69994 = CARTESIAN_POINT ( 'NONE',  ( 67.06670390244700286, -67.87844715994098976, 245.4920193514479934 ) ) ;
#69995 = CARTESIAN_POINT ( 'NONE',  ( 107.0667039024470313, -119.4690460831833150, -11.78219314458153733 ) ) ;
#69996 = ORIENTED_EDGE ( 'NONE', *, *, #36838, .F. ) ;
#69997 = CARTESIAN_POINT ( 'NONE',  ( 95.32417067969559810, -34.95402877631575222, 71.20705384733993526 ) ) ;
#69998 = SHAPE_REPRESENTATION_RELATIONSHIP ( 'NONE' , 'NONE' ,  #14421, #3408 ) ;
#70000 = CARTESIAN_POINT ( 'NONE',  ( 94.33955404248733601, 70.17666187254644683, -90.25011051337669699 ) ) ;
#69999 = FACE_OUTER_BOUND ( 'NONE', #89866, .T. ) ;
#70001 = DIRECTION ( 'NONE',  ( 1.000000000000000000, 0.000000000000000000, 0.000000000000000000 ) ) ;
#70002 = CARTESIAN_POINT ( 'NONE',  ( 132.8230071953907725, -16.27587548316543931, 1.868342134761751483 ) ) ;
#70003 = ORIENTED_EDGE ( 'NONE', *, *, #72993, .T. ) ;
#70004 = ADVANCED_FACE ( 'NONE', ( #81903 ), #67344, .F. ) ;
#70005 = AXIS2_PLACEMENT_3D ( 'NONE', #32573, #80307, #73463 ) ;
#70006 = EDGE_CURVE ( 'NONE', #40462, #26689, #19214, .T. ) ;
#70007 = CARTESIAN_POINT ( 'NONE',  ( 110.7480548206264785, -27.39964114457682598, 120.7761619811009126 ) ) ;
#70008 = FACE_OUTER_BOUND ( 'NONE', #20545, .T. ) ;
#70009 = EDGE_CURVE ( 'NONE', #53062, #59219, #84119, .T. ) ;
#70010 = LINE ( 'NONE', #7779, #82097 ) ;
#70011 = CARTESIAN_POINT ( 'NONE',  ( 96.62018903270816850, -36.61901565639288236, 107.3184824187679567 ) ) ;
#70012 = EDGE_CURVE ( 'NONE', #54782, #84272, #1909, .T. ) ;
#70014 = CARTESIAN_POINT ( 'NONE',  ( 51.42025729302574888, -31.94127993907664731, 117.4678068554150485 ) ) ;
#70013 = DIRECTION ( 'NONE',  ( 0.000000000000000000, 1.000000000000000000, 0.000000000000000000 ) ) ;
#70015 = CARTESIAN_POINT ( 'NONE',  ( 130.3998166246070127, 12.92155284005802685, 335.5992267699912190 ) ) ;
#70016 = AXIS2_PLACEMENT_3D ( 'NONE', #17, #21356, #35412 ) ;
#70017 = ORIENTED_EDGE ( 'NONE', *, *, #42607, .F. ) ;
#70018 = DIRECTION ( 'NONE',  ( -1.000000000000000078E-15, 1.000000000000000000, 0.000000000000000000 ) ) ;
#70019 = CARTESIAN_POINT ( 'NONE',  ( 107.6167445103326230, -46.48501816386541208, 148.6213395616249784 ) ) ;
#70020 = EDGE_CURVE ( 'NONE', #68005, #12422, #59146, .T. ) ;
#70022 = ORIENTED_EDGE ( 'NONE', *, *, #79471, .F. ) ;
#70021 = DIRECTION ( 'NONE',  ( 0.000000000000000000, 0.000000000000000000, -1.000000000000000000 ) ) ;
#70023 = CARTESIAN_POINT ( 'NONE',  ( 104.8459308146384785, -26.52976224399709082, 256.2470538473397141 ) ) ;
#70024 = CARTESIAN_POINT ( 'NONE',  ( 107.0664832912739399, -36.72944715994095333, 315.1356252759112522 ) ) ;
#70025 = FACE_OUTER_BOUND ( 'NONE', #41610, .T. ) ;
#70026 = EDGE_CURVE ( 'NONE', #48723, #84365, #65901, .T. ) ;
#70027 = CARTESIAN_POINT ( 'NONE',  ( 188.5667039024479834, -62.87844715994099687, 132.3428068554150343 ) ) ;
#70028 = DIRECTION ( 'NONE',  ( -1.000000000000000000, 0.000000000000000000, -7.067626426349370916E-15 ) ) ;
#70029 = AXIS2_PLACEMENT_3D ( 'NONE', #56964, #84705, #7490 ) ;
#70030 = CARTESIAN_POINT ( 'NONE',  ( 67.62344788955067543, -138.2352025272443825, 245.9283337036430055 ) ) ;
#70031 = CARTESIAN_POINT ( 'NONE',  ( -99.77245543246419857, 76.20343663217359165, 84.20430400022985395 ) ) ;
#70032 = CARTESIAN_POINT ( 'NONE',  ( 99.06478422775786896, -31.10483629442210329, 205.8384824187689617 ) ) ;
#70033 = ORIENTED_EDGE ( 'NONE', *, *, #70814, .T. ) ;
#70034 = VERTEX_POINT ( 'NONE', #17763 ) ;
#70035 = CARTESIAN_POINT ( 'NONE',  ( 100.2959224756171466, -44.18784923124425035, 153.4215833058969736 ) ) ;
#70036 = CONICAL_SURFACE ( 'NONE', #4733, 89.90000000000000568, 0.7853981633974206344 ) ;
#70037 = CARTESIAN_POINT ( 'NONE',  ( 123.6837132603321692, -20.11243780205712639, 249.5838068554165261 ) ) ;
#70038 = CARTESIAN_POINT ( 'NONE',  ( 103.4018642804673789, -27.34641595622759169, 16.80444044875395448 ) ) ;
#70039 = DIRECTION ( 'NONE',  ( -1.000000000000000000, 1.011922027653136551E-15, 0.000000000000000000 ) ) ;
#70040 = VECTOR ( 'NONE', #76017, 1000.000000000000000 ) ;
#70041 = FACE_OUTER_BOUND ( 'NONE', #3813, .T. ) ;
#70042 = DIRECTION ( 'NONE',  ( 1.000000000000000000, 0.000000000000000000, 0.000000000000000000 ) ) ;
#70043 = DIRECTION ( 'NONE',  ( 5.512527431108029424E-15, -1.000000000000000000, 0.000000000000000000 ) ) ;
#70044 = LINE ( 'NONE', #75962, #28474 ) ;
#70045 = CARTESIAN_POINT ( 'NONE',  ( 98.91597900623158068, -29.29754952351876796, 230.7261014663869503 ) ) ;
#70046 = CARTESIAN_POINT ( 'NONE',  ( 4.059057582146186505, 94.50683581605682093, 118.2888403985303256 ) ) ;
#70047 = VERTEX_POINT ( 'NONE', #38641 ) ;
#70048 = ORIENTED_EDGE ( 'NONE', *, *, #86023, .F. ) ;
#70049 = CARTESIAN_POINT ( 'NONE',  ( -83.63178471058881769, 77.68489675156565966, -100.2530235599237329 ) ) ;
#70050 = CARTESIAN_POINT ( 'NONE',  ( -75.38763434846467248, 88.17653575778736297, -91.50010255991641372 ) ) ;
#70051 = CARTESIAN_POINT ( 'NONE',  ( 99.50465472078816731, -43.30570863480165400, 122.8950840663260209 ) ) ;
#70052 = DIRECTION ( 'NONE',  ( 0.000000000000000000, 0.000000000000000000, -1.000000000000000000 ) ) ;
#70053 = EDGE_CURVE ( 'NONE', #41893, #21752, #78681, .T. ) ;
#70054 = CARTESIAN_POINT ( 'NONE',  ( 12.17631217095389573, 79.28385973135301867, 117.7280539260733008 ) ) ;
#70055 = ORIENTED_EDGE ( 'NONE', *, *, #70728, .F. ) ;
#70056 = CARTESIAN_POINT ( 'NONE',  ( 101.5861822943782755, -47.29253114347246623, 13.19562527591094891 ) ) ;
#70057 = EDGE_CURVE ( 'NONE', #85412, #18386, #28747, .T. ) ;
#70058 = CARTESIAN_POINT ( 'NONE',  ( 106.5673262220758772, -47.17821497701651623, 247.5384824187679556 ) ) ;
#70059 = ORIENTED_EDGE ( 'NONE', *, *, #82440, .T. ) ;
#70060 = DIRECTION ( 'NONE',  ( -0.9254794337955620787, -0.3787978585227822492, 0.000000000000000000 ) ) ;
#70061 = CARTESIAN_POINT ( 'NONE',  ( 90.44969454456439450, -20.11243780205712639, 249.5838068554174924 ) ) ;
#70062 = CARTESIAN_POINT ( 'NONE',  ( -194.1576000000000022, 101.5999999999999943, -12.69999999999999929 ) ) ;
#70063 = CARTESIAN_POINT ( 'NONE',  ( 114.8864029495430685, -33.02137736771143750, 62.00904275054391945 ) ) ;
#70064 = CARTESIAN_POINT ( 'NONE',  ( 108.2803420215754500, -47.73912846947793298, 153.6518157521009584 ) ) ;
#70065 = DIRECTION ( 'NONE',  ( 0.000000000000000000, -1.000000000000000000, 0.000000000000000000 ) ) ;
#70066 = ORIENTED_EDGE ( 'NONE', *, *, #64197, .T. ) ;
#70067 = CARTESIAN_POINT ( 'NONE',  ( 182.4202572930269923, -31.94127993907680718, -5.074374724088000832 ) ) ;
#70068 = VERTEX_POINT ( 'NONE', #31379 ) ;
#70069 = VERTEX_POINT ( 'NONE', #38205 ) ;
#70070 = AXIS2_PLACEMENT_3D ( 'NONE', #45626, #60615, #73361 ) ;
#70071 = EDGE_CURVE ( 'NONE', #7861, #84435, #40335, .T. ) ;
#70072 = CARTESIAN_POINT ( 'NONE',  ( 12.03238568418269416, 86.63481793440479350, 117.9438919316608008 ) ) ;
#70073 = ORIENTED_EDGE ( 'NONE', *, *, #76473, .F. ) ;
#70074 = ORIENTED_EDGE ( 'NONE', *, *, #23681, .T. ) ;
#70075 = DIRECTION ( 'NONE',  ( 1.000000000000000078E-15, -1.000000000000000083E-30, -1.000000000000000000 ) ) ;
#70076 = FACE_OUTER_BOUND ( 'NONE', #6778, .T. ) ;
#70077 = CARTESIAN_POINT ( 'NONE',  ( 109.2815815313881558, -45.51044995646627456, 92.20765792331498290 ) ) ;
#70078 = CARTESIAN_POINT ( 'NONE',  ( 105.8910851810002356, -47.14611527663348056, 282.4870538473393253 ) ) ;
#70079 = CARTESIAN_POINT ( 'NONE',  ( 101.2129617469312564, -45.32973500739964834, 197.1013395616249966 ) ) ;
#70080 = LINE ( 'NONE', #35549, #42639 ) ;
#70081 = DIRECTION ( 'NONE',  ( 0.000000000000000000, 0.000000000000000000, 1.000000000000000000 ) ) ;
#70082 = ORIENTED_EDGE ( 'NONE', *, *, #61804, .T. ) ;
#70083 = CARTESIAN_POINT ( 'NONE',  ( 97.81169266289590780, -40.51741659614882707, 92.63571255866972365 ) ) ;
#70084 = CARTESIAN_POINT ( 'NONE',  ( 93.94797395270801132, -35.60435878782501362, 293.6356252759106837 ) ) ;
#70085 = CARTESIAN_POINT ( 'NONE',  ( 134.0664832912739826, -8.729447159941003065, 8.525625275911005829 ) ) ;
#70086 = CARTESIAN_POINT ( 'NONE',  ( 114.2526777242401437, -43.36435822665426087, 123.2327681330539519 ) ) ;
#70087 = AXIS2_PLACEMENT_3D ( 'NONE', #44836, #52078, #65296 ) ;
#70088 = CARTESIAN_POINT ( 'NONE',  ( 96.61245533174189859, -37.29510205964861314, 76.36991099019697060 ) ) ;
#70089 = CARTESIAN_POINT ( 'NONE',  ( 99.36439196449877898, -28.73628302914087840, 265.6746728949588032 ) ) ;
#70090 = EDGE_LOOP ( 'NONE', ( #61648, #42871, #34953, #51791 ) ) ;
#70091 = CARTESIAN_POINT ( 'NONE',  ( 96.12498142956854963, -35.16017202033504674, 226.2251490854349640 ) ) ;
#70092 = CARTESIAN_POINT ( 'NONE',  ( 94.06648329127393993, -36.72944715994095333, 293.6356252759106837 ) ) ;
#70093 =( LENGTH_UNIT ( ) NAMED_UNIT ( * ) SI_UNIT ( .MILLI., .METRE. ) );
#70094 = CIRCLE ( 'NONE', #48276, 6.350000000000659561 ) ;
#70095 = CARTESIAN_POINT ( 'NONE',  ( 12.70000000000000107, 81.76374953821583347, 129.9368274816650057 ) ) ;
#70096 = DIRECTION ( 'NONE',  ( -0.7071067811865259234, 0.7071067811865692221, -2.899137802865049595E-29 ) ) ;
#70098 = CARTESIAN_POINT ( 'NONE',  ( 167.6524903400756159, -49.32844715993520879, 129.9678068554150059 ) ) ;
#70097 = FACE_OUTER_BOUND ( 'NONE', #75302, .T. ) ;
#70099 = DIRECTION ( 'NONE',  ( 0.000000000000000000, 0.000000000000000000, 1.000000000000000000 ) ) ;
#70100 = DIRECTION ( 'NONE',  ( -0.000000000000000000, 1.000000000000000000, -0.000000000000000000 ) ) ;
#70101 = VECTOR ( 'NONE', #67297, 1000.000000000000000 ) ;
#70102 = CARTESIAN_POINT ( 'NONE',  ( 11.57394144444449502, 87.79471777913514074, -117.9898073157514915 ) ) ;
#70103 = CARTESIAN_POINT ( 'NONE',  ( -5.244075232672812170, 94.12423341047687586, 130.4512049017868094 ) ) ;
#70104 = CARTESIAN_POINT ( 'NONE',  ( 108.4174892294855681, -26.73503592422339992, 10.96895861100186309 ) ) ;
#70105 = ADVANCED_FACE ( 'NONE', ( #87258 ), #72292, .T. ) ;
#70106 = CARTESIAN_POINT ( 'NONE',  ( 165.6738106836044722, -28.98061976758450342, 193.9678068554149775 ) ) ;
#70108 = ORIENTED_EDGE ( 'NONE', *, *, #79929, .T. ) ;
#70107 = DIRECTION ( 'NONE',  ( -0.000000000000000000, -0.000000000000000000, -1.000000000000000000 ) ) ;
#70109 = DIRECTION ( 'NONE',  ( 3.999999999999999995E-14, -1.000000000000000000, 4.100000000000000342E-29 ) ) ;
#70110 = CARTESIAN_POINT ( 'NONE',  ( 96.74139913992713957, -35.13602278645100796, 266.2041967044820581 ) ) ;
#70111 = CARTESIAN_POINT ( 'NONE',  ( 113.3313291481109815, -45.06216520097333955, 139.0899109901969553 ) ) ;
#70112 = CARTESIAN_POINT ( 'NONE',  ( 107.1956677504039135, -26.28336798021810239, 31.06705384733893283 ) ) ;
#70113 = DIRECTION ( 'NONE',  ( 1.000000000000000000, 0.000000000000000000, 0.000000000000000000 ) ) ;
#70115 = CARTESIAN_POINT ( 'NONE',  ( 97.81169607051373305, -40.51742273377266912, 46.63562653399714009 ) ) ;
#70114 = CARTESIAN_POINT ( 'NONE',  ( 103.1875000000000000, 101.5999999999999943, 5.041900000000359761 ) ) ;
#70116 = CARTESIAN_POINT ( 'NONE',  ( 97.81170238817014706, -40.51743819009087844, 137.6355114220584994 ) ) ;
#70117 = VECTOR ( 'NONE', #44067, 1000.000000000000000 ) ;
#70119 = ORIENTED_EDGE ( 'NONE', *, *, #47966, .F. ) ;
#70118 = B_SPLINE_CURVE_WITH_KNOTS ( 'NONE', 3,
 ( #46453, #39650, #67353, #73277, #32842, #24252, #88282, #37881, #11055, #51922, #52793, #45546, #79679, #80563, #72842, #62680, #35408, #28604, #35864, #76311, #8173, #20904, #7280, #69504, #34966, #14546, #1362, #40098, #42660, #46899, #8631, #63583, #56292, #84500, #67814 ),
 .UNSPECIFIED., .F., .F.,
 ( 4, 2, 2, 1, 1, 2, 2, 2, 2, 2, 2, 1, 1, 2, 2, 2, 1, 1, 1, 2, 4 ),
 ( 0.3333434881890902091, 0.4166701562233744438, 0.4218780729755153280, 0.4270859897276562123, 0.4375018232319381473, 0.4583334902404970213, 0.4999968242576139366, 0.5208284912661723665, 0.5416601582747307964, 0.5624918252832892263, 0.5650957836593583083, 0.5676997420354273904, 0.5729076587875665538, 0.5833234922918473231, 0.6249868263089795040, 0.6275907846850493632, 0.6301947430611192225, 0.6354026598132580528, 0.6458184933175352693, 0.6562343268218123749, 0.6666501603260894804 ),
 .UNSPECIFIED. ) ;
#70120 = LINE ( 'NONE', #7892, #40327 ) ;
#70121 = ORIENTED_EDGE ( 'NONE', *, *, #38614, .F. ) ;
#70122 = CARTESIAN_POINT ( 'NONE',  ( 111.7477409549918690, -43.87381266066567775, 177.4609912566479579 ) ) ;
#70123 = EDGE_CURVE ( 'NONE', #36708, #877, #78230, .T. ) ;
#70125 = ORIENTED_EDGE ( 'NONE', *, *, #19055, .T. ) ;
#70124 = CYLINDRICAL_SURFACE ( 'NONE', #52894, 2.517500000000005844 ) ;
#70126 = AXIS2_PLACEMENT_3D ( 'NONE', #44637, #72370, #8817 ) ;
#70127 = DIRECTION ( 'NONE',  ( -3.100000000000000258E-29, 3.100000000000000044E-14, 1.000000000000000000 ) ) ;
#70128 = CARTESIAN_POINT ( 'NONE',  ( 108.8451227504523189, -46.97957433935474825, 163.7127681330539701 ) ) ;
#70129 = CARTESIAN_POINT ( 'NONE',  ( 176.7738106835049052, -48.62134037887551585, 180.4678068554150059 ) ) ;
#70130 = EDGE_CURVE ( 'NONE', #56709, #22947, #58204, .T. ) ;
#70131 = CARTESIAN_POINT ( 'NONE',  ( 102.0674588022921228, -27.97026135298835925, 150.4901954177360039 ) ) ;
#70132 = CARTESIAN_POINT ( 'NONE',  ( 110.4024638856497518, -27.29981427005776951, 85.80618083057217405 ) ) ;
#70133 = CARTESIAN_POINT ( 'NONE',  ( -91.72954454028258908, 77.68452069048194630, 75.10852668448676184 ) ) ;
#70134 = DIRECTION ( 'NONE',  ( 0.9834602067019604377, 0.1811243270069963496, 0.000000000000000000 ) ) ;
#70135 = CARTESIAN_POINT ( 'NONE',  ( 116.3624975636024317, -33.68846805112525544, 89.07848241876791917 ) ) ;
#70136 = VERTEX_POINT ( 'NONE', #23705 ) ;
#70137 = VERTEX_POINT ( 'NONE', #30945 ) ;
#70138 = VERTEX_POINT ( 'NONE', #16431 ) ;
#70139 = VECTOR ( 'NONE', #1024, 1000.000000000000000 ) ;
#70140 = CARTESIAN_POINT ( 'NONE',  ( 109.8610415383596148, -27.05157811987473337, 61.28444044875497099 ) ) ;
#70141 = FACE_OUTER_BOUND ( 'NONE', #1930, .T. ) ;
#70143 = CARTESIAN_POINT ( 'NONE',  ( 70.06968321367156705, -140.6784088069870222, 245.5331728854790185 ) ) ;
#70142 = CARTESIAN_POINT ( 'NONE',  ( 116.5710038106514759, -34.42130396933982439, 205.0156252759109634 ) ) ;
#70144 = FACE_OUTER_BOUND ( 'NONE', #18854, .T. ) ;
#70145 = DIRECTION ( 'NONE',  ( 6.524622321627019585E-16, 3.741823817616790462E-31, 1.000000000000000000 ) ) ;
#70146 = FACE_OUTER_BOUND ( 'NONE', #84566, .T. ) ;
#70147 = CARTESIAN_POINT ( 'NONE',  ( 31.56670390244800828, -33.35206098992711077, -5.074374724088000832 ) ) ;
#70148 = DIRECTION ( 'NONE',  ( 0.000000000000000000, 0.000000000000000000, -1.000000000000000000 ) ) ;
#70149 = CARTESIAN_POINT ( 'NONE',  ( 97.95167206076190780, -31.64175201202206011, 110.9213395616259703 ) ) ;
#70150 = ORIENTED_EDGE ( 'NONE', *, *, #23655, .F. ) ;
#70151 = ORIENTED_EDGE ( 'NONE', *, *, #9230, .F. ) ;
#70152 = ORIENTED_EDGE ( 'NONE', *, *, #31545, .F. ) ;
#70153 = SURFACE_STYLE_USAGE ( .BOTH. , #76977 ) ;
#70154 = DIRECTION ( 'NONE',  ( -0.000000000000000000, 1.000000000000000000, -0.000000000000000000 ) ) ;
#70155 = CARTESIAN_POINT ( 'NONE',  ( 97.60799287394519297, -39.98272528114131319, 131.5900899984870875 ) ) ;
#70156 = DIRECTION ( 'NONE',  ( 1.000000000000000000, 4.299999999999999979E-14, 1.000000000000000078E-15 ) ) ;
#70157 = CARTESIAN_POINT ( 'NONE',  ( 104.5243549119882829, -45.65320838865366682, 215.1738046553059860 ) ) ;
#70158 = CIRCLE ( 'NONE', #49789, 9.571100913904368568 ) ;
#70159 = FACE_OUTER_BOUND ( 'NONE', #1859, .T. ) ;
#70160 = AXIS2_PLACEMENT_3D ( 'NONE', #10424, #87619, #38127 ) ;
#70161 = EDGE_CURVE ( 'NONE', #21770, #378, #2805, .T. ) ;
#70162 = DIRECTION ( 'NONE',  ( -1.000000000000000000, 0.000000000000000000, -0.000000000000000000 ) ) ;
#70163 = ORIENTED_EDGE ( 'NONE', *, *, #60025, .F. ) ;
#70165 = VERTEX_POINT ( 'NONE', #50484 ) ;
#70164 = VERTEX_POINT ( 'NONE', #16875 ) ;
#70166 = CARTESIAN_POINT ( 'NONE',  ( 70.63919639214310564, 49.07499999999999574, -53.97512327982435210 ) ) ;
#70167 = VERTEX_POINT ( 'NONE', #52246 ) ;
#70168 = ORIENTED_EDGE ( 'NONE', *, *, #78019, .T. ) ;
#70169 = CARTESIAN_POINT ( 'NONE',  ( 63.56670390244824631, -47.82844715994016127, 300.4678068554150627 ) ) ;
#70170 = CARTESIAN_POINT ( 'NONE',  ( 97.06047953529140671, -37.89159766150721964, 232.8501547344689584 ) ) ;
#70171 = CARTESIAN_POINT ( 'NONE',  ( 86.98314995794039817, 12.92155284005802507, 349.2756252759109543 ) ) ;
#70172 = EDGE_LOOP ( 'NONE', ( #67063, #56563, #13481, #74989, #57889 ) ) ;
#70173 = DIRECTION ( 'NONE',  ( -0.7071067811734105257, 0.7071067811996846197, 0.000000000000000000 ) ) ;
#70174 = CARTESIAN_POINT ( 'NONE',  ( -111.8086192760389679, 66.24298264774402867, 67.40841616357421628 ) ) ;
#70175 = ORIENTED_EDGE ( 'NONE', *, *, #42187, .T. ) ;
#70176 = ORIENTED_EDGE ( 'NONE', *, *, #47418, .F. ) ;
#70177 = AXIS2_PLACEMENT_3D ( 'NONE', #61209, #21235, #62108 ) ;
#70178 = EDGE_CURVE ( 'NONE', #16533, #5020, #70840, .T. ) ;
#70179 = CARTESIAN_POINT ( 'NONE',  ( 162.7866693523289996, -36.02818131005891189, -5.074374724088000832 ) ) ;
#70180 = AXIS2_PLACEMENT_3D ( 'NONE', #5330, #12143, #40730 ) ;
#70181 = EDGE_LOOP ( 'NONE', ( #47076, #13304 ) ) ;
#70182 = VERTEX_POINT ( 'NONE', #23273 ) ;
#70183 = EDGE_CURVE ( 'NONE', #69535, #72716, #38914, .T. ) ;
#70184 = CARTESIAN_POINT ( 'NONE',  ( 115.7079196686036653, -36.25352450022288764, 271.7004713219723726 ) ) ;
#70185 = EDGE_CURVE ( 'NONE', #19998, #61434, #43250, .T. ) ;
#70187 = CARTESIAN_POINT ( 'NONE',  ( 113.0897370140187235, -28.19324317000061697, 129.5870538473399449 ) ) ;
#70186 = AXIS2_PLACEMENT_3D ( 'NONE', #44979, #6240, #24116 ) ;
#70188 = CARTESIAN_POINT ( 'NONE',  ( 108.5348814579965904, -26.43029805172848867, 104.9641967044819779 ) ) ;
#70189 = CARTESIAN_POINT ( 'NONE',  ( 116.4683302779955767, -39.73499081598242100, 249.5838068554167819 ) ) ;
#70190 = PRESENTATION_STYLE_ASSIGNMENT (( #28861 ) ) ;
#70191 = CARTESIAN_POINT ( 'NONE',  ( 118.0509465330791983, -35.49837129967784222, 229.9032443235299468 ) ) ;
#70192 = FACE_OUTER_BOUND ( 'NONE', #26376, .T. ) ;
#70193 = FACE_OUTER_BOUND ( 'NONE', #39400, .T. ) ;
#70194 = ORIENTED_EDGE ( 'NONE', *, *, #64256, .F. ) ;
#70195 = CARTESIAN_POINT ( 'NONE',  ( 188.5667039024479834, -48.82844715994099971, 139.9678068554150059 ) ) ;
#70197 = VERTEX_POINT ( 'NONE', #50937 ) ;
#70196 = EDGE_CURVE ( 'NONE', #85915, #59995, #24138, .T. ) ;
#70198 = ADVANCED_FACE ( 'NONE', ( #15991 ), #43671, .T. ) ;
#70199 = ORIENTED_EDGE ( 'NONE', *, *, #39048, .F. ) ;
#70200 = CARTESIAN_POINT ( 'NONE',  ( 134.0664832912740110, -46.72944715994100306, 10.72562527591099801 ) ) ;
#70201 = ADVANCED_FACE ( 'NONE', ( #9608 ), #51812, .F. ) ;
#70202 = EDGE_CURVE ( 'NONE', #18115, #35754, #81027, .T. ) ;
#70203 = DIRECTION ( 'NONE',  ( 1.907762142705490052E-15, 7.167082501179359715E-16, -1.000000000000000000 ) ) ;
#70204 = ORIENTED_EDGE ( 'NONE', *, *, #73167, .F. ) ;
#70205 = CARTESIAN_POINT ( 'NONE',  ( 97.61684652917979577, -30.99503764212949264, 125.8803871806719599 ) ) ;
#70206 = CARTESIAN_POINT ( 'NONE',  ( 97.06097939450964418, -37.99593194579918531, 256.4272396045237201 ) ) ;
#70207 = EDGE_CURVE ( 'NONE', #63654, #86303, #23003, .T. ) ;
#70208 = CYLINDRICAL_SURFACE ( 'NONE', #11643, 9.999999999999998224 ) ;
#70209 = DIRECTION ( 'NONE',  ( 0.000000000000000000, 0.000000000000000000, -1.000000000000000000 ) ) ;
#70212 = CARTESIAN_POINT ( 'NONE',  ( 116.5858064714420976, -40.92601143571967270, 249.4956252759109532 ) ) ;
#70211 = CARTESIAN_POINT ( 'NONE',  ( 107.0624707424859849, -46.75563725778415147, 57.57597174261474748 ) ) ;
#70210 = DIRECTION ( 'NONE',  ( -1.000000000000000078E-15, 1.000000000000000000, 0.000000000000000000 ) ) ;
#70213 = FACE_OUTER_BOUND ( 'NONE', #3913, .T. ) ;
#70214 = CARTESIAN_POINT ( 'NONE',  ( 97.81169822462854313, -40.51742973538109993, 111.6355314416972391 ) ) ;
#70215 = CARTESIAN_POINT ( 'NONE',  ( 7.661254700127844153, 69.45253841614081125, 320.6630000000000109 ) ) ;
#70216 = CYLINDRICAL_SURFACE ( 'NONE', #87726, 0.2500000000000002220 ) ;
#70217 = CARTESIAN_POINT ( 'NONE',  ( 25.56670390244797275, -48.82844715994099971, 137.2178068554150059 ) ) ;
#70218 = ADVANCED_FACE ( 'NONE', ( #67243 ), #53132, .F. ) ;
#70219 = CARTESIAN_POINT ( 'NONE',  ( 128.8897065959775432, -58.55267046464430791, -4.824374724089007138 ) ) ;
#70221 = ORIENTED_EDGE ( 'NONE', *, *, #813, .T. ) ;
#70220 = CARTESIAN_POINT ( 'NONE',  ( 118.3887371170988132, -33.06383674033636311, 284.0756252759109657 ) ) ;
#70222 = CARTESIAN_POINT ( 'NONE',  ( 112.4976487814606685, -26.16836495570049337, 169.6984824187679521 ) ) ;
#70223 = CARTESIAN_POINT ( 'NONE',  ( 117.4545169724989648, -37.95830395151629943, 49.73276813305393773 ) ) ;
#70224 = CARTESIAN_POINT ( 'NONE',  ( 113.6415746488294047, -45.67179987042115386, 179.0689586092439640 ) ) ;
#70225 = LINE ( 'NONE', #21187, #5393 ) ;
#70226 = DIRECTION ( 'NONE',  ( 1.000000000000000078E-15, -1.000000000000000083E-30, -1.000000000000000000 ) ) ;
#70228 = CARTESIAN_POINT ( 'NONE',  ( 172.5664832912729878, -27.57844715994070484, 318.9256252759120116 ) ) ;
#70227 = DIRECTION ( 'NONE',  ( 0.000000000000000000, 1.000000000000000000, 0.000000000000000000 ) ) ;
#70229 = CARTESIAN_POINT ( 'NONE',  ( 71.25416588882602298, -72.55705569728901594, 394.9756252759101471 ) ) ;
#70230 = DIRECTION ( 'NONE',  ( 0.000000000000000000, 1.000000000000000000, 0.000000000000000000 ) ) ;
#70231 = ORIENTED_EDGE ( 'NONE', *, *, #43628, .F. ) ;
#70232 = VECTOR ( 'NONE', #46393, 1000.000000000000000 ) ;
#70233 = DIRECTION ( 'NONE',  ( 1.000000000000000000, 0.000000000000000000, 0.000000000000000000 ) ) ;
#70234 = AXIS2_PLACEMENT_3D ( 'NONE', #45920, #38239, #80943 ) ;
#70235 = VERTEX_POINT ( 'NONE', #82247 ) ;
#70236 = ORIENTED_EDGE ( 'NONE', *, *, #49557, .T. ) ;
#70237 = EDGE_CURVE ( 'NONE', #13431, #71967, #14224, .T. ) ;
#70239 = ORIENTED_EDGE ( 'NONE', *, *, #68387, .F. ) ;
#70238 = DIRECTION ( 'NONE',  ( -4.237773401492740281E-14, 1.000000000000000000, 0.000000000000000000 ) ) ;
#70240 = CARTESIAN_POINT ( 'NONE',  ( 117.9659426345831719, -38.42225801833666310, 64.69181575210097890 ) ) ;
#70241 = DIRECTION ( 'NONE',  ( 0.000000000000000000, 0.000000000000000000, 1.000000000000000000 ) ) ;
#70242 = EDGE_CURVE ( 'NONE', #5474, #33479, #46783, .T. ) ;
#70243 = EDGE_CURVE ( 'NONE', #72171, #51571, #37438, .T. ) ;
#70244 = CARTESIAN_POINT ( 'NONE',  ( 226.4410000000000025, 65.43750000000000000, -2.032000000000000028 ) ) ;
#70245 = CARTESIAN_POINT ( 'NONE',  ( 118.9266961287330560, -37.70231105260669580, 184.7613395616249647 ) ) ;
#70246 = EDGE_CURVE ( 'NONE', #24376, #55351, #49008, .T. ) ;
#70247 = CARTESIAN_POINT ( 'NONE',  ( 106.1055101188695602, -45.24582830394255240, 281.9095626852197825 ) ) ;
#70248 = ORIENTED_EDGE ( 'NONE', *, *, #56157, .T. ) ;
#70249 = ORIENTED_EDGE ( 'NONE', *, *, #42568, .T. ) ;
#70250 = EDGE_LOOP ( 'NONE', ( #2060, #7267, #41887, #55172, #53842, #57841, #55020, #23806 ) ) ;
#70251 = ORIENTED_EDGE ( 'NONE', *, *, #25076, .F. ) ;
#70252 = AXIS2_PLACEMENT_3D ( 'NONE', #27430, #33356, #47861 ) ;
#70253 = CARTESIAN_POINT ( 'NONE',  ( -48.02966122971775320, 91.07499999999996021, -8.747637655308301746E-15 ) ) ;
#70254 = VECTOR ( 'NONE', #39448, 1000.000000000000000 ) ;
#70255 = DIRECTION ( 'NONE',  ( 1.000000000000000000, 0.000000000000000000, -1.147230458779309805E-16 ) ) ;
#70256 = CARTESIAN_POINT ( 'NONE',  ( 97.81168148112675453, -40.51739256386586163, 162.6360428395636859 ) ) ;
#70257 = CARTESIAN_POINT ( 'NONE',  ( 115.0898634087918850, -30.61888143515580296, 19.34376026548776650 ) ) ;
#70258 = FACE_OUTER_BOUND ( 'NONE', #65328, .T. ) ;
#70259 = DIRECTION ( 'NONE',  ( 3.100000000000000258E-29, -3.100000000000000044E-14, -1.000000000000000000 ) ) ;
#70261 = CARTESIAN_POINT ( 'NONE',  ( 0.000000000000000000, 124.5870000000000033, 0.000000000000000000 ) ) ;
#70260 = AXIS2_PLACEMENT_3D ( 'NONE', #5301, #26628, #48387 ) ;
#70262 = CARTESIAN_POINT ( 'NONE',  ( -11.13171314038108584, 88.66704411686306742, 130.0806558683388801 ) ) ;
#70263 = CARTESIAN_POINT ( 'NONE',  ( 110.2773916389478188, -46.62487827714380018, 12.82705384733995402 ) ) ;
#70264 = LINE ( 'NONE', #52341, #45834 ) ;
#70265 = ORIENTED_EDGE ( 'NONE', *, *, #83201, .F. ) ;
#70266 = CARTESIAN_POINT ( 'NONE',  ( 52.06670390244699576, -67.87844715994100397, 55.21780685541800437 ) ) ;
#70267 = CARTESIAN_POINT ( 'NONE',  ( -55.84590893209900031, 55.42534759972548386, 70.74779723465208292 ) ) ;
#70268 = CARTESIAN_POINT ( 'NONE',  ( 103.8598393684536632, -44.23592174987565073, 90.07380465530594904 ) ) ;
#70269 = DIRECTION ( 'NONE',  ( 0.7071067811865535679, -0.7071067811865415775, 7.071067811865543372E-16 ) ) ;
#70270 = CARTESIAN_POINT ( 'NONE',  ( 99.09570907421795027, -30.55043175556566482, 45.80229194281738359 ) ) ;
#70271 = EDGE_LOOP ( 'NONE', ( #9244, #5101 ) ) ;
#70272 = EDGE_LOOP ( 'NONE', ( #8079, #44689 ) ) ;
#70273 = DIRECTION ( 'NONE',  ( -0.9254794337955620787, -0.3787978585227822492, 0.000000000000000000 ) ) ;
#70274 = VERTEX_POINT ( 'NONE', #18654 ) ;
#70275 = ORIENTED_EDGE ( 'NONE', *, *, #3146, .T. ) ;
#70276 = CARTESIAN_POINT ( 'NONE',  ( 115.5299003720540014, -39.45574047089768754, 155.0101547344689550 ) ) ;
#70277 = FACE_OUTER_BOUND ( 'NONE', #722, .T. ) ;
#70278 = VECTOR ( 'NONE', #87391, 1000.000000000000000 ) ;
#70279 = CARTESIAN_POINT ( 'NONE',  ( 112.5256494142567192, -27.82244069900259476, 90.63848241876793566 ) ) ;
#70280 = CONICAL_SURFACE ( 'NONE', #29630, 11.57110091390437034, 0.7853981633974457255 ) ;
#70281 = DIRECTION ( 'NONE',  ( -1.150535366796005147E-15, 1.000000000000000000, -3.100000000000000044E-14 ) ) ;
#70282 = ORIENTED_EDGE ( 'NONE', *, *, #1503, .T. ) ;
#70283 = VECTOR ( 'NONE', #15928, 1000.000000000000000 ) ;
#70284 = VERTEX_POINT ( 'NONE', #40434 ) ;
#70286 = EDGE_CURVE ( 'NONE', #5023, #16980, #5936, .T. ) ;
#70285 = ORIENTED_EDGE ( 'NONE', *, *, #57102, .F. ) ;
#70287 = EDGE_CURVE ( 'NONE', #4284, #29468, #59964, .T. ) ;
#70288 = EDGE_CURVE ( 'NONE', #26221, #78242, #89041, .T. ) ;
#70289 = DIRECTION ( 'NONE',  ( -0.9254794337955620787, -0.3787978585227822492, 0.000000000000000000 ) ) ;
#70290 = VERTEX_POINT ( 'NONE', #74062 ) ;
#70291 = CARTESIAN_POINT ( 'NONE',  ( 115.9265467165008232, -42.18176083994495684, 18.38705384733896153 ) ) ;
#70292 = CARTESIAN_POINT ( 'NONE',  ( 117.4790109288255309, -40.50628101140208770, 169.5375300378159693 ) ) ;
#70293 = DIRECTION ( 'NONE',  ( 3.100000000000000258E-29, -3.100000000000000044E-14, -1.000000000000000000 ) ) ;
#70294 = DIRECTION ( 'NONE',  ( 2.056463827196271584E-15, -0.8571673007021100021, 0.5150380749100580413 ) ) ;
#70295 = CARTESIAN_POINT ( 'NONE',  ( 111.7941755367341443, -25.86282203548705283, 130.7499109901969518 ) ) ;
#70296 = DIRECTION ( 'NONE',  ( 0.7071067811989697471, 0.7071067811741252873, 7.071067811989691343E-16 ) ) ;
#70297 = ORIENTED_EDGE ( 'NONE', *, *, #65282, .T. ) ;
#70298 = DIRECTION ( 'NONE',  ( 0.7071067811866279529, -0.7071067811864671926, 7.071067811866286874E-16 ) ) ;
#70299 = EDGE_CURVE ( 'NONE', #72137, #86716, #20003, .T. ) ;
#70300 = EDGE_CURVE ( 'NONE', #34776, #16780, #45882, .T. ) ;
#70301 = ORIENTED_EDGE ( 'NONE', *, *, #39839, .F. ) ;
#70302 = CARTESIAN_POINT ( 'NONE',  ( 0.000000000000000000, -245.0000000000000000, 142.8750000000000000 ) ) ;
#70303 = ORIENTED_EDGE ( 'NONE', *, *, #56022, .F. ) ;
#70304 = EDGE_CURVE ( 'NONE', #56973, #70579, #16854, .T. ) ;
#70305 = AXIS2_PLACEMENT_3D ( 'NONE', #30066, #8739, #14651 ) ;
#70306 = FACE_OUTER_BOUND ( 'NONE', #47666, .T. ) ;
#70307 = VECTOR ( 'NONE', #61389, 1000.000000000000000 ) ;
#70308 = CARTESIAN_POINT ( 'NONE',  ( 11.30280982162985026, 88.13356536631488325, 118.0161419656921140 ) ) ;
#70309 = CARTESIAN_POINT ( 'NONE',  ( 96.71451373887593661, -37.96385262316839260, 41.42133956162496844 ) ) ;
#70310 = CARTESIAN_POINT ( 'NONE',  ( 20.75871628398702384, 82.54999999999999716, 317.6630000000000109 ) ) ;
#70311 = VECTOR ( 'NONE', #65178, 1000.000000000000000 ) ;
#70312 = EDGE_CURVE ( 'NONE', #41323, #58627, #36076, .T. ) ;
#70313 = CARTESIAN_POINT ( 'NONE',  ( 167.6524903400753601, -49.32844715993521589, 300.4678068554149490 ) ) ;
#70314 = CARTESIAN_POINT ( 'NONE',  ( 116.7951252721156266, -39.38782978729904727, 74.61479194280059346 ) ) ;
#70315 = CARTESIAN_POINT ( 'NONE',  ( 97.58158007118568378, -32.53714515026960896, 55.98324432352996638 ) ) ;
#70317 = CARTESIAN_POINT ( 'NONE',  ( 108.0049669398584911, -26.36739623290736390, 151.0041967044829505 ) ) ;
#70316 = CARTESIAN_POINT ( 'NONE',  ( 98.34959472676385417, -31.65703098628569379, 110.9064992847184783 ) ) ;
#70318 = FACE_OUTER_BOUND ( 'NONE', #31700, .T. ) ;
#70319 = CARTESIAN_POINT ( 'NONE',  ( 107.0667039024470313, -104.2784471599413934, 2.217806855418003043 ) ) ;
#70320 = ORIENTED_EDGE ( 'NONE', *, *, #19232, .F. ) ;
#70321 = LINE ( 'NONE', #41695, #36720 ) ;
#70322 = AXIS2_PLACEMENT_3D ( 'NONE', #159, #77362, #42369 ) ;
#70323 = VECTOR ( 'NONE', #10916, 1000.000000000000000 ) ;
#70324 = CARTESIAN_POINT ( 'NONE',  ( 110.2901544400639722, 45.91391880550399662, 69.86957027353565763 ) ) ;
#70325 = DIRECTION ( 'NONE',  ( 0.000000000000000000, 1.000000000000000000, 0.000000000000000000 ) ) ;
#70326 = VERTEX_POINT ( 'NONE', #15437 ) ;
#70327 = EDGE_CURVE ( 'NONE', #4991, #48663, #63635, .T. ) ;
#70328 = DIRECTION ( 'NONE',  ( -0.7071067811865773267, 0.7071067811865178188, -7.071067811865781017E-16 ) ) ;
#70330 = ORIENTED_EDGE ( 'NONE', *, *, #79338, .T. ) ;
#70329 = CARTESIAN_POINT ( 'NONE',  ( 117.3348906646497909, -34.51323323996641079, 183.9956252759109532 ) ) ;
#70331 = DIRECTION ( 'NONE',  ( 0.000000000000000000, 0.000000000000000000, 1.000000000000000000 ) ) ;
#70332 = CARTESIAN_POINT ( 'NONE',  ( 98.51983665003312751, -30.72177789114069313, 201.8384824187679385 ) ) ;
#70333 = CARTESIAN_POINT ( 'NONE',  ( 117.1483892680215888, -39.54869380112744892, 94.60991099019693706 ) ) ;
#70334 = CARTESIAN_POINT ( 'NONE',  ( 94.62072105690005230, 70.27892663483461888, 89.95524642164141937 ) ) ;
#70335 = CARTESIAN_POINT ( 'NONE',  ( 115.8236631867570878, -31.72696035637653011, 190.2397867966467402 ) ) ;
#70336 = EDGE_CURVE ( 'NONE', #59590, #65933, #76753, .T. ) ;
#70337 = CARTESIAN_POINT ( 'NONE',  ( 165.3359832912740046, -36.32844715994100682, 342.9256252759119548 ) ) ;
#70338 = ORIENTED_EDGE ( 'NONE', *, *, #29375, .T. ) ;
#70339 = CIRCLE ( 'NONE', #89209, 7.499999999999992895 ) ;
#70340 = ORIENTED_EDGE ( 'NONE', *, *, #43696, .T. ) ;
#70341 = VERTEX_POINT ( 'NONE', #42652 ) ;
#70342 = ORIENTED_EDGE ( 'NONE', *, *, #31975, .T. ) ;
#70343 = DIRECTION ( 'NONE',  ( -1.000000000000000000, -1.206764157201257538E-15, 0.000000000000000000 ) ) ;
#70344 = CARTESIAN_POINT ( 'NONE',  ( 105.6320745483020147, -47.05538338894268691, 253.4670538473393719 ) ) ;
#70345 = DIRECTION ( 'NONE',  ( -1.000000000000000000, -4.299999999999999979E-14, -1.000000000000000078E-15 ) ) ;
#70346 = CARTESIAN_POINT ( 'NONE',  ( 6.938893903907229955E-15, 60.82030000000000314, 216.0269999999999868 ) ) ;
#70347 = EDGE_CURVE ( 'NONE', #26346, #57531, #8520, .T. ) ;
#70350 = EDGE_CURVE ( 'NONE', #72189, #849, #5604, .T. ) ;
#70349 = LINE ( 'NONE', #8579, #73272 ) ;
#70348 = CARTESIAN_POINT ( 'NONE',  ( 28.57499999999999929, 73.38456447661469895, 302.8950000000000387 ) ) ;
#70351 = CARTESIAN_POINT ( 'NONE',  ( 136.8164832912739826, -18.72944715994099951, 14.92562527591100263 ) ) ;
#70352 = CARTESIAN_POINT ( 'NONE',  ( 112.1921266949303373, -27.58526089107821733, 34.66991099019695355 ) ) ;
#70353 = ORIENTED_EDGE ( 'NONE', *, *, #78173, .T. ) ;
#70354 = AXIS2_PLACEMENT_3D ( 'NONE', #76486, #41941, #41495 ) ;
#70355 = ORIENTED_EDGE ( 'NONE', *, *, #11535, .F. ) ;
#70356 = CARTESIAN_POINT ( 'NONE',  ( 134.0664832912740110, -41.22944715994101017, 8.225625275910998013 ) ) ;
#70357 = VECTOR ( 'NONE', #72565, 1000.000000000000000 ) ;
#70358 = CARTESIAN_POINT ( 'NONE',  ( 99.09613892721601758, -30.54985836692837964, 16.80516855958618549 ) ) ;
#70359 = B_SPLINE_CURVE_WITH_KNOTS ( 'NONE', 3,
 ( #61932, #82857, #34227, #89664, #1063, #41479, #83742, #70102, #49640, #20171, #35118, #54646, #82409, #6532, #49188, #7426, #83294, #76922, #77365, #47845, #69209, #14701, #15144, #6981, #42820, #55541 ),
 .UNSPECIFIED., .F., .F.,
 ( 4, 2, 2, 2, 2, 2, 2, 2, 2, 2, 2, 2, 4 ),
 ( 0.01987186023414422298, 0.02111327400948153146, 0.02235468778481883648, 0.02483751533549341181, 0.02607892911083071683, 0.02732034288616802531, 0.02980317043684266656, 0.03228599798751731476, 0.03352741176285463365, 0.03476882553819194560, 0.03725165308886656951, 0.03849306686420388146, 0.03973448063954118648 ),
 .UNSPECIFIED. ) ;
#70360 = CARTESIAN_POINT ( 'NONE',  ( 103.3362402991319584, -47.20309360805207177, 248.3041967044819387 ) ) ;
#70361 = CYLINDRICAL_SURFACE ( 'NONE', #32707, 0.5000000000000197620 ) ;
#70362 = CARTESIAN_POINT ( 'NONE',  ( 96.71010325458821910, -37.26253042779857338, 117.3794347997199594 ) ) ;
#70363 = DIRECTION ( 'NONE',  ( 0.000000000000000000, 1.000000000000000000, 0.000000000000000000 ) ) ;
#70364 = CARTESIAN_POINT ( 'NONE',  ( -76.20994146752570941, 54.60582892396201515, 30.80975041202057341 ) ) ;
#70365 = ORIENTED_EDGE ( 'NONE', *, *, #22132, .F. ) ;
#70366 = CARTESIAN_POINT ( 'NONE',  ( -103.1875000000000000, 117.4749999999999943, -1.080832317973422076E-12 ) ) ;
#70367 = ORIENTED_EDGE ( 'NONE', *, *, #83337, .T. ) ;
#70368 = ORIENTED_EDGE ( 'NONE', *, *, #10532, .F. ) ;
#70369 = CARTESIAN_POINT ( 'NONE',  ( -88.44409384118955586, 93.33902940301969409, 78.95116244206113265 ) ) ;
#70370 = CARTESIAN_POINT ( 'NONE',  ( 97.00631399252166887, -37.24296311215223909, 267.7987261630397029 ) ) ;
#70371 = EDGE_CURVE ( 'NONE', #70652, #14566, #14537, .T. ) ;
#70372 = VECTOR ( 'NONE', #5113, 1000.000000000000000 ) ;
#70373 = CARTESIAN_POINT ( 'NONE',  ( 51.42025729304100423, -33.70561438051981185, -5.074374724088000832 ) ) ;
#70374 = VECTOR ( 'NONE', #50444, 1000.000000000000000 ) ;
#70375 = VECTOR ( 'NONE', #46087, 1000.000000000000000 ) ;
#70376 = CARTESIAN_POINT ( 'NONE',  ( 102.0668027733616441, -27.97064593957984968, 140.4898149731944272 ) ) ;
#70377 = LINE ( 'NONE', #14971, #40349 ) ;
#70378 = CARTESIAN_POINT ( 'NONE',  ( 80.06648329127401098, -39.47944715994105991, 1.625625275910943746 ) ) ;
#70379 = AXIS2_PLACEMENT_3D ( 'NONE', #19602, #80500, #25072 ) ;
#70380 = VERTEX_POINT ( 'NONE', #29057 ) ;
#70381 = CARTESIAN_POINT ( 'NONE',  ( 6.938893903907229955E-15, 67.86880000000000734, 210.4643999999999835 ) ) ;
#70382 = DIRECTION ( 'NONE',  ( 0.9254794337955621897, 0.3787978585227821382, 0.000000000000000000 ) ) ;
#70383 = ORIENTED_EDGE ( 'NONE', *, *, #52222, .T. ) ;
#70384 = CARTESIAN_POINT ( 'NONE',  ( 115.6114045197296178, -28.51818617053012161, 39.43562527591099354 ) ) ;
#70385 = VERTEX_POINT ( 'NONE', #35855 ) ;
#70386 = CARTESIAN_POINT ( 'NONE',  ( 105.5338363264665986, -28.21170577469638729, 273.0242808457819592 ) ) ;
#70387 = CIRCLE ( 'NONE', #18176, 0.5000000000000004441 ) ;
#70388 = CARTESIAN_POINT ( 'NONE',  ( 109.6443389294615542, -46.47974508850531805, 127.7816520840981980 ) ) ;
#70389 = CARTESIAN_POINT ( 'NONE',  ( 114.5468542906243243, -29.54732804739393615, 189.4232443235299570 ) ) ;
#70390 = CARTESIAN_POINT ( 'NONE',  ( 23.71377214814948076, 81.30938561711869283, 298.2863242343943284 ) ) ;
#70391 = DIRECTION ( 'NONE',  ( -1.000000000000000000, 0.000000000000000000, 0.000000000000000000 ) ) ;
#70392 = FACE_OUTER_BOUND ( 'NONE', #72695, .T. ) ;
#70393 = PLANE ( 'NONE',  #43593 ) ;
#70394 = AXIS2_PLACEMENT_3D ( 'NONE', #82774, #48202, #35479 ) ;
#70395 = EDGE_CURVE ( 'NONE', #27672, #5931, #14075, .T. ) ;
#70396 = CARTESIAN_POINT ( 'NONE',  ( 96.49300521333343283, -40.10570368261699059, 277.5603871806730467 ) ) ;
#70397 = CARTESIAN_POINT ( 'NONE',  ( 104.0320542673484852, -46.27522442963353200, 117.3334030146819202 ) ) ;
#70398 = EDGE_LOOP ( 'NONE', ( #39745, #53722, #786, #68728 ) ) ;
#70399 = CARTESIAN_POINT ( 'NONE',  ( 141.8664832912740223, -71.52944715994085811, 394.9756252759100903 ) ) ;
#70400 = EDGE_LOOP ( 'NONE', ( #2436, #4884 ) ) ;
#70401 = CARTESIAN_POINT ( 'NONE',  ( 101.6557087385557736, -27.03816153323032268, 101.4937205140059575 ) ) ;
#70402 = LINE ( 'NONE', #55394, #39582 ) ;
#70403 =( BOUNDED_CURVE ( )  B_SPLINE_CURVE ( 2, ( #37662, #65359, #3142 ),
 .UNSPECIFIED., .F., .T. ) 
 B_SPLINE_CURVE_WITH_KNOTS ( ( 3, 3 ),
 ( 0.000000000000000000, 0.5053286420056780637 ),
 .UNSPECIFIED. ) 
 CURVE ( )  GEOMETRIC_REPRESENTATION_ITEM ( )  RATIONAL_B_SPLINE_CURVE ( ( 1.000000000000000000, 1.009299002520649857, 1.000420656333769864 ) ) 
 REPRESENTATION_ITEM ( '' )  );
#70404 = B_SPLINE_CURVE_WITH_KNOTS ( 'NONE', 3,
 ( #52158, #45355, #10413, #73075, #31289, #38553, #52599 ),
 .UNSPECIFIED., .F., .F.,
 ( 4, 1, 1, 1, 4 ),
 ( -0.1863381261298940050, 0.9565458916201099449, 3.242315181216560038, 5.528084470813009688, 7.813853433339420285 ),
 .UNSPECIFIED. ) ;
#70405 = ORIENTED_EDGE ( 'NONE', *, *, #45571, .F. ) ;
#70406 = VECTOR ( 'NONE', #68770, 1000.000000000000000 ) ;
#70408 = EDGE_CURVE ( 'NONE', #11616, #23269, #14368, .T. ) ;
#70407 = ORIENTED_EDGE ( 'NONE', *, *, #65658, .F. ) ;
#70410 = VERTEX_POINT ( 'NONE', #27255 ) ;
#70409 = EDGE_CURVE ( 'NONE', #66948, #34067, #41761, .T. ) ;
#70411 = DIRECTION ( 'NONE',  ( 0.000000000000000000, 0.000000000000000000, 1.000000000000000000 ) ) ;
#70412 = EDGE_CURVE ( 'NONE', #57634, #36122, #24469, .T. ) ;
#70413 = CARTESIAN_POINT ( 'NONE',  ( 97.33784628398525740, -34.07104680458591162, 267.1147904887237701 ) ) ;
#70414 = DIRECTION ( 'NONE',  ( 1.000000000000000000, -3.885780586187990841E-13, 0.000000000000000000 ) ) ;
#70415 = CARTESIAN_POINT ( 'NONE',  ( 143.0536128999585515, -139.9914422477621088, 247.3423811826519909 ) ) ;
#70416 = DIRECTION ( 'NONE',  ( 0.000000000000000000, 1.000000000000000000, 0.000000000000000000 ) ) ;
#70417 = CARTESIAN_POINT ( 'NONE',  ( 106.2521435260052698, -26.30072798870746453, 21.13848241876792144 ) ) ;
#70418 = CARTESIAN_POINT ( 'NONE',  ( -215.9000000000000057, 3.174999999999999822, 142.8750000000000000 ) ) ;
#70419 = ORIENTED_EDGE ( 'NONE', *, *, #58682, .F. ) ;
#70420 = CARTESIAN_POINT ( 'NONE',  ( 106.1318921495875145, -121.2375349704976486, -19.21044887263748180 ) ) ;
#70421 = EDGE_CURVE ( 'NONE', #82662, #83342, #900, .T. ) ;
#70422 = CARTESIAN_POINT ( 'NONE',  ( 113.1782915013152007, -44.75187050426813329, 43.09357499818941051 ) ) ;
#70423 = VERTEX_POINT ( 'NONE', #77657 ) ;
#70424 = ORIENTED_EDGE ( 'NONE', *, *, #55304, .T. ) ;
#70425 = EDGE_CURVE ( 'NONE', #18492, #39136, #27373, .T. ) ;
#70426 = CARTESIAN_POINT ( 'NONE',  ( 82.81648329127398256, -18.72944715994105636, 3.101481641215461327 ) ) ;
#70427 = LINE ( 'NONE', #9538, #28066 ) ;
#70428 = VECTOR ( 'NONE', #81521, 1000.000000000000000 ) ;
#70429 = LINE ( 'NONE', #69979, #75318 ) ;
#70430 = PLANE ( 'NONE',  #40322 ) ;
#70431 = EDGE_CURVE ( 'NONE', #13582, #58432, #89494, .T. ) ;
#70432 = CARTESIAN_POINT ( 'NONE',  ( 102.4446420578519934, -44.51733865501087450, 206.5848007804579538 ) ) ;
#70433 = FACE_OUTER_BOUND ( 'NONE', #65972, .T. ) ;
#70434 = CARTESIAN_POINT ( 'NONE',  ( 123.9191631267440528, 72.20435897694871130, 41.10135031971049813 ) ) ;
#70435 = CARTESIAN_POINT ( 'NONE',  ( 112.5373769503831625, -27.80330641407773840, 94.63848241876793566 ) ) ;
#70436 = ORIENTED_EDGE ( 'NONE', *, *, #36483, .F. ) ;
#70437 = CARTESIAN_POINT ( 'NONE',  ( -479.3614999999999782, 104.7749999999999915, -1.387778780781445991E-14 ) ) ;
#70438 = ORIENTED_EDGE ( 'NONE', *, *, #54800, .T. ) ;
#70439 = CARTESIAN_POINT ( 'NONE',  ( 106.6049069045543405, -26.71869322362929822, 276.1132126703095082 ) ) ;
#70440 = ORIENTED_EDGE ( 'NONE', *, *, #46264, .T. ) ;
#70441 = LINE ( 'NONE', #64964, #88294 ) ;
#70442 = ORIENTED_EDGE ( 'NONE', *, *, #50108, .F. ) ;
#70443 = CARTESIAN_POINT ( 'NONE',  ( -215.9000000000000057, 104.7749999999999915, 142.8750000000000000 ) ) ;
#70444 = CARTESIAN_POINT ( 'NONE',  ( 68.70813896271630483, -81.16137653295078280, 247.5270838628449894 ) ) ;
#70446 = CIRCLE ( 'NONE', #47192, 2.500000000000002220 ) ;
#70445 = DIRECTION ( 'NONE',  ( 1.000000000000000000, 0.000000000000000000, 0.000000000000000000 ) ) ;
#70447 = VERTEX_POINT ( 'NONE', #82695 ) ;
#70448 = CARTESIAN_POINT ( 'NONE',  ( 118.0253644177900156, -38.34139182134431678, 73.72229194257801055 ) ) ;
#70449 = AXIS2_PLACEMENT_3D ( 'NONE', #72372, #17840, #4215 ) ;
#70450 = AXIS2_PLACEMENT_3D ( 'NONE', #10151, #43766, #65112 ) ;
#70451 =( LENGTH_UNIT ( ) NAMED_UNIT ( * ) SI_UNIT ( .MILLI., .METRE. ) );
#70452 = AXIS2_PLACEMENT_3D ( 'NONE', #30416, #58113, #70869 ) ;
#70454 = CARTESIAN_POINT ( 'NONE',  ( 89.95524642164112095, 70.27892663483459046, -94.62072105690033652 ) ) ;
#70453 = CARTESIAN_POINT ( 'NONE',  ( 105.7988705769415958, -26.72411980046145530, 165.1773442352779853 ) ) ;
#70455 = DIRECTION ( 'NONE',  ( 1.000000000000000000, 0.000000000000000000, 0.000000000000000000 ) ) ;
#70456 = CARTESIAN_POINT ( 'NONE',  ( 113.1782937596609457, -44.75186860166526515, 143.0939586080882577 ) ) ;
#70457 = ORIENTED_EDGE ( 'NONE', *, *, #50333, .F. ) ;
#70458 = AXIS2_PLACEMENT_3D ( 'NONE', #36502, #78295, #76484 ) ;
#70459 = CARTESIAN_POINT ( 'NONE',  ( -103.1875000000000000, 117.4749999999999943, 7.143749999998919797 ) ) ;
#70460 = DIRECTION ( 'NONE',  ( -4.237773401492740281E-14, 1.000000000000000000, 0.000000000000000000 ) ) ;
#70461 = CIRCLE ( 'NONE', #73154, 0.5000000000000104361 ) ;
#70462 = FACE_OUTER_BOUND ( 'NONE', #49426, .T. ) ;
#70463 = CARTESIAN_POINT ( 'NONE',  ( 108.9888594788934029, -47.63768604335348300, 118.7032443235299723 ) ) ;
#70466 = ADVANCED_FACE ( 'NONE', ( #20454, #48124 ), #75858, .F. ) ;
#70465 = LINE ( 'NONE', #84558, #57198 ) ;
#70464 = DIRECTION ( 'NONE',  ( -1.000000000000000078E-15, -1.000000000000000083E-30, 1.000000000000000000 ) ) ;
#70467 = CARTESIAN_POINT ( 'NONE',  ( 107.0667039024470313, -104.2784471599409528, 23.21780685541800082 ) ) ;
#70468 = AXIS2_PLACEMENT_3D ( 'NONE', #43531, #86230, #15850 ) ;
#70469 = ORIENTED_EDGE ( 'NONE', *, *, #5216, .T. ) ;
#70470 = VECTOR ( 'NONE', #17821, 1000.000000000000000 ) ;
#70471 = FACE_OUTER_BOUND ( 'NONE', #9118, .T. ) ;
#70472 = CARTESIAN_POINT ( 'NONE',  ( 98.82386243697619932, -31.40279086140556331, 141.8699109901959616 ) ) ;
#70474 = VERTEX_POINT ( 'NONE', #62220 ) ;
#70473 = CARTESIAN_POINT ( 'NONE',  ( 123.6837132603318423, -20.11243780205705534, 239.5838068554170377 ) ) ;
#70475 = CARTESIAN_POINT ( 'NONE',  ( 97.57986484199628308, -43.79006170206856297, 257.8356252759109566 ) ) ;
#70476 = PLANE ( 'NONE',  #62852 ) ;
#70477 = DIRECTION ( 'NONE',  ( 0.000000000000000000, -0.4999999999999998890, -0.8660254037844387076 ) ) ;
#70478 = CARTESIAN_POINT ( 'NONE',  ( 103.3797721312301405, -102.7271463785351671, 2.217806855417947531 ) ) ;
#70479 = DIRECTION ( 'NONE',  ( 1.000000000000000000, 0.000000000000000000, 0.000000000000000000 ) ) ;
#70480 = FACE_OUTER_BOUND ( 'NONE', #37871, .T. ) ;
#70481 = CARTESIAN_POINT ( 'NONE',  ( 173.9900000000000091, 20.32000000000000028, -131.6533725204174061 ) ) ;
#70482 = CARTESIAN_POINT ( 'NONE',  ( 102.5357197525641766, -45.39752751535337438, 212.1927681330539599 ) ) ;
#70483 = EDGE_LOOP ( 'NONE', ( #43816, #71388, #59843, #30389, #81349, #42789, #17774, #39646 ) ) ;
#70484 = ORIENTED_EDGE ( 'NONE', *, *, #83522, .T. ) ;
#70485 = AXIS2_PLACEMENT_3D ( 'NONE', #62221, #8623, #82696 ) ;
#70486 = CARTESIAN_POINT ( 'NONE',  ( 101.8133294234851860, -44.51716929413077395, 148.5234880678019351 ) ) ;
#70487 = EDGE_CURVE ( 'NONE', #65273, #77074, #5, .T. ) ;
#70488 = CARTESIAN_POINT ( 'NONE',  ( -186.2398777604659870, 101.5999999999999943, 107.9500000000000028 ) ) ;
#70489 = CARTESIAN_POINT ( 'NONE',  ( 110.6847694559308621, -28.64017749364363397, 21.17301187732595480 ) ) ;
#70490 = VECTOR ( 'NONE', #26593, 1000.000000000000000 ) ;
#70491 = FACE_OUTER_BOUND ( 'NONE', #24850, .T. ) ;
#70492 = DIRECTION ( 'NONE',  ( 2.056463827196271584E-15, -0.8571673007021100021, 0.5150380749100580413 ) ) ;
#70493 = LINE ( 'NONE', #29596, #22672 ) ;
#70494 = CARTESIAN_POINT ( 'NONE',  ( 99.09570907225396752, -30.55043175805740674, 106.8022919430684539 ) ) ;
#70495 = CARTESIAN_POINT ( 'NONE',  ( 22.62762465138245460, 171.9999999999999716, 183.8826257785461280 ) ) ;
#70496 = CARTESIAN_POINT ( 'NONE',  ( 98.05565822401619869, -44.38798742045811707, 226.8870538473399563 ) ) ;
#70497 = CARTESIAN_POINT ( 'NONE',  ( 97.33770779590314248, -34.07148707886162953, 171.1142724482292863 ) ) ;
#70498 = EDGE_LOOP ( 'NONE', ( #82055, #73181 ) ) ;
#70499 = ORIENTED_EDGE ( 'NONE', *, *, #31019, .F. ) ;
#70500 = CARTESIAN_POINT ( 'NONE',  ( 117.0608945230788578, -38.08045312548524919, 88.71895860887195795 ) ) ;
#70501 = CARTESIAN_POINT ( 'NONE',  ( -81.47101467905596905, 94.84303900880915705, -86.13165781700311641 ) ) ;
#70502 = CARTESIAN_POINT ( 'NONE',  ( 101.9936016578518974, -45.44608281785205861, 123.1551631644055220 ) ) ;
#70503 = DIRECTION ( 'NONE',  ( 0.000000000000000000, 1.000000000000000000, 0.000000000000000000 ) ) ;
#70504 = CARTESIAN_POINT ( 'NONE',  ( 106.5519926023875712, -26.37212682281792198, 41.12800622829093555 ) ) ;
#70506 = CYLINDRICAL_SURFACE ( 'NONE', #83281, 2.000000000000007550 ) ;
#70505 = CIRCLE ( 'NONE', #51605, 4.750000000000000888 ) ;
#70507 = ORIENTED_EDGE ( 'NONE', *, *, #44793, .F. ) ;
#70508 = AXIS2_PLACEMENT_3D ( 'NONE', #80988, #67320, #5110 ) ;
#70509 = FACE_OUTER_BOUND ( 'NONE', #49311, .T. ) ;
#70510 = CIRCLE ( 'NONE', #35674, 0.5000000000000004441 ) ;
#70511 = CARTESIAN_POINT ( 'NONE',  ( 63.06670390244732971, -24.92844715994017690, 300.4678068554150627 ) ) ;
#70512 = CARTESIAN_POINT ( 'NONE',  ( 97.16957671423683962, -40.00637722736999535, 241.5813395616249863 ) ) ;
#70514 = EDGE_LOOP ( 'NONE', ( #63111, #4107, #48318, #7316, #42585 ) ) ;
#70513 = EDGE_CURVE ( 'NONE', #27030, #21043, #49336, .T. ) ;
#70515 = EDGE_CURVE ( 'NONE', #15623, #4781, #1805, .T. ) ;
#70516 = PLANE ( 'NONE',  #63696 ) ;
#70517 = LINE ( 'NONE', #40998, #26861 ) ;
#70518 = EDGE_CURVE ( 'NONE', #73072, #25446, #50371, .T. ) ;
#70519 = CARTESIAN_POINT ( 'NONE',  ( 116.3573301164176712, -40.55459570680316972, 168.5154237022636039 ) ) ;
#70520 = CARTESIAN_POINT ( 'NONE',  ( 113.2960346059783774, -42.04690695427109404, 61.08237608387695161 ) ) ;
#70521 = CARTESIAN_POINT ( 'NONE',  ( 96.02367466659750050, -35.86829477906547226, 187.2765776568629406 ) ) ;
#70522 = CARTESIAN_POINT ( 'NONE',  ( 57.56670390244744340, -48.82844715994040286, 175.7178068554150911 ) ) ;
#70523 = EDGE_LOOP ( 'NONE', ( #61880, #75507, #31656, #56050 ) ) ;
#70524 = ADVANCED_FACE ( 'NONE', ( #71736 ), #52142, .T. ) ;
#70525 = VECTOR ( 'NONE', #64443, 1000.000000000000000 ) ;
#70526 = FACE_OUTER_BOUND ( 'NONE', #79746, .T. ) ;
#70527 = ORIENTED_EDGE ( 'NONE', *, *, #55173, .T. ) ;
#70528 = ORIENTED_EDGE ( 'NONE', *, *, #3657, .F. ) ;
#70529 = FACE_OUTER_BOUND ( 'NONE', #5263, .T. ) ;
#70530 = EDGE_LOOP ( 'NONE', ( #37009, #74503, #3713, #6802, #22048, #53897, #34528, #31016 ) ) ;
#70531 = ORIENTED_EDGE ( 'NONE', *, *, #11329, .F. ) ;
#70532 = DIRECTION ( 'NONE',  ( 0.000000000000000000, 0.000000000000000000, -1.000000000000000000 ) ) ;
#70533 = AXIS2_PLACEMENT_3D ( 'NONE', #67662, #6326, #13152 ) ;
#70534 = CARTESIAN_POINT ( 'NONE',  ( 108.0458233943899273, -25.31222262750819851, 322.3938544957129011 ) ) ;
#70535 = EDGE_CURVE ( 'NONE', #84821, #8522, #30395, .T. ) ;
#70536 = CARTESIAN_POINT ( 'NONE',  ( 99.71754419879584930, -32.37637629707774778, 85.32384839950596245 ) ) ;
#70537 = CARTESIAN_POINT ( 'NONE',  ( 97.59524074137092953, -41.13874739096760891, 256.6727681330537507 ) ) ;
#70538 = LINE ( 'NONE', #8307, #31051 ) ;
#70539 = CARTESIAN_POINT ( 'NONE',  ( 115.5439452383992176, -108.5954344580498372, -19.78219314458187839 ) ) ;
#70540 = ORIENTED_EDGE ( 'NONE', *, *, #52612, .T. ) ;
#70541 = VERTEX_POINT ( 'NONE', #85385 ) ;
#70542 = CARTESIAN_POINT ( 'NONE',  ( -479.3614999999999782, 89.53805401447691281, 18.25625000000039933 ) ) ;
#70543 = CYLINDRICAL_SURFACE ( 'NONE', #69586, 4.750000000000000888 ) ;
#70544 = DIRECTION ( 'NONE',  ( -0.000000000000000000, -0.000000000000000000, -1.000000000000000000 ) ) ;
#70545 = CARTESIAN_POINT ( 'NONE',  ( 117.1895451461017643, -38.97942580829906944, 103.6403871806739545 ) ) ;
#70546 = CARTESIAN_POINT ( 'NONE',  ( 117.2525043769621362, -39.29786468180206782, 123.6299109901969615 ) ) ;
#70547 = DIRECTION ( 'NONE',  ( 0.000000000000000000, 0.000000000000000000, 1.000000000000000000 ) ) ;
#70548 = VERTEX_POINT ( 'NONE', #16323 ) ;
#70549 = PRODUCT_DEFINITION_CONTEXT ( 'detailed design', #85250, 'design' ) ;
#70550 = CARTESIAN_POINT ( 'NONE',  ( 104.1857688441879191, -26.67323559945603151, 225.2984824187679749 ) ) ;
#70551 = FACE_OUTER_BOUND ( 'NONE', #46825, .T. ) ;
#70552 = CARTESIAN_POINT ( 'NONE',  ( 11.02744467571318054, 76.24661008267737827, 130.0895381633343391 ) ) ;
#70553 = PLANE ( 'NONE',  #16989 ) ;
#70555 = CARTESIAN_POINT ( 'NONE',  ( 41.56648329127398966, -27.57844715994070484, 138.9256252759119832 ) ) ;
#70554 = CARTESIAN_POINT ( 'NONE',  ( 34.67381068362099228, -26.00627455219321860, -5.074374724088000832 ) ) ;
#70556 = DIRECTION ( 'NONE',  ( 0.000000000000000000, 1.000000000000000000, 0.000000000000000000 ) ) ;
#70557 = DIRECTION ( 'NONE',  ( 0.000000000000000000, 0.000000000000000000, -1.000000000000000000 ) ) ;
#70558 = CARTESIAN_POINT ( 'NONE',  ( 132.1654742078777360, -38.71744337671164971, 7.623533105443405233 ) ) ;
#70559 = CARTESIAN_POINT ( 'NONE',  ( -11.57415360872103172, 87.79424630570802890, 130.0420457590604144 ) ) ;
#70560 = DIRECTION ( 'NONE',  ( -1.000000000000000000, 0.000000000000000000, -1.047445008332813989E-14 ) ) ;
#70561 = FACE_OUTER_BOUND ( 'NONE', #40490, .T. ) ;
#70563 = ORIENTED_EDGE ( 'NONE', *, *, #72659, .T. ) ;
#70562 = DIRECTION ( 'NONE',  ( 0.000000000000000000, 0.000000000000000000, -1.000000000000000000 ) ) ;
#70564 = CARTESIAN_POINT ( 'NONE',  ( 123.0664832912757163, -36.72944715993921960, -5.074374724089014244 ) ) ;
#70565 = CARTESIAN_POINT ( 'NONE',  ( 99.52336843529489840, -29.45003914207232754, 250.7156252759109520 ) ) ;
#70566 = CARTESIAN_POINT ( 'NONE',  ( 112.7801043229996338, -45.44936815460292934, 174.0384824187679556 ) ) ;
#70567 = CARTESIAN_POINT ( 'NONE',  ( 96.51983850151567879, -40.19180362902228865, 282.5908633711491120 ) ) ;
#70568 = VECTOR ( 'NONE', #11967, 999.9999999999997726 ) ;
#70569 = DIRECTION ( 'NONE',  ( -0.000000000000000000, 1.000000000000000000, 0.000000000000000000 ) ) ;
#70572 = ADVANCED_FACE ( 'NONE', ( #44899 ), #10394, .T. ) ;
#70571 = CARTESIAN_POINT ( 'NONE',  ( 82.06789631128971507, -34.84294903900328677, 7.549690073101738008 ) ) ;
#70570 = CARTESIAN_POINT ( 'NONE',  ( -479.3614999999999782, 93.66249999999999432, 82.23860802895320887 ) ) ;
#70573 = DIRECTION ( 'NONE',  ( 0.000000000000000000, 0.000000000000000000, -1.000000000000000000 ) ) ;
#70574 = AXIS2_PLACEMENT_3D ( 'NONE', #76128, #13911, #40258 ) ;
#70575 = AXIS2_PLACEMENT_3D ( 'NONE', #56267, #6794, #8147 ) ;
#70576 = EDGE_CURVE ( 'NONE', #87053, #29939, #58966, .T. ) ;
#70577 = ORIENTED_EDGE ( 'NONE', *, *, #39315, .F. ) ;
#70578 = CARTESIAN_POINT ( 'NONE',  ( -3.174999999999644995, 111.1250000000000000, -33.98325472291465132 ) ) ;
#70579 = VERTEX_POINT ( 'NONE', #58529 ) ;
#70580 = CARTESIAN_POINT ( 'NONE',  ( 103.4754675462218927, -28.97956086136533926, 179.8438483995059869 ) ) ;
#70582 = ORIENTED_EDGE ( 'NONE', *, *, #80901, .F. ) ;
#70581 = LINE ( 'NONE', #13819, #32637 ) ;
#70583 = LINE ( 'NONE', #34703, #27239 ) ;
#70584 = CARTESIAN_POINT ( 'NONE',  ( 98.68348088377354088, -30.50934295487602199, 176.8184824187679567 ) ) ;
#70585 = DIRECTION ( 'NONE',  ( 0.7071067811865473507, 0.000000000000000000, -0.7071067811865476838 ) ) ;
#70586 = PLANE ( 'NONE',  #26925 ) ;
#70587 = CARTESIAN_POINT ( 'NONE',  ( 102.1022249014249184, -28.02397532599129093, 86.48945707807658323 ) ) ;
#70588 = CARTESIAN_POINT ( 'NONE',  ( 36.23715912545424089, -47.82818131006125384, 300.4678068554150059 ) ) ;
#70589 = CYLINDRICAL_SURFACE ( 'NONE', #87512, 2.116999999999980009 ) ;
#70591 = CARTESIAN_POINT ( 'NONE',  ( 100.7170190823676279, -45.85612711270997011, 87.09276813305393716 ) ) ;
#70590 = VECTOR ( 'NONE', #75989, 1000.000000000000000 ) ;
#70592 = EDGE_LOOP ( 'NONE', ( #75889, #41646, #19016, #82934 ) ) ;
#70593 = ORIENTED_EDGE ( 'NONE', *, *, #50070, .F. ) ;
#70594 = EDGE_LOOP ( 'NONE', ( #56113, #88712, #69556, #29715 ) ) ;
#70595 = CARTESIAN_POINT ( 'NONE',  ( 116.3620231750148406, -38.09673052741934640, 70.15396425827796634 ) ) ;
#70596 = ADVANCED_FACE ( 'NONE', ( #79904, #51706 ), #79456, .T. ) ;
#70597 = CARTESIAN_POINT ( 'NONE',  ( 133.3245970085671104, -95.93364041391147623, 250.2178068554180470 ) ) ;
#70599 = CARTESIAN_POINT ( 'NONE',  ( 116.3229784443844324, -32.93528945216412041, 94.13562527591096796 ) ) ;
#70598 = CARTESIAN_POINT ( 'NONE',  ( 115.7764676695377517, -43.63945112744033850, 194.2927681330539542 ) ) ;
#70600 = DIRECTION ( 'NONE',  ( 1.000000000000000000, 4.163336342344333240E-14, 0.000000000000000000 ) ) ;
#70601 = CARTESIAN_POINT ( 'NONE',  ( 80.06648329127399677, 0.2215528400590013880, 4.925625275911999168 ) ) ;
#70602 = LINE ( 'NONE', #29709, #72143 ) ;
#70603 = CARTESIAN_POINT ( 'NONE',  ( -7.195828152521259823E-13, 117.4749999999999943, 95.25000000000000000 ) ) ;
#70604 = CARTESIAN_POINT ( 'NONE',  ( 67.34197081037864052, -68.14385895291664497, 246.5134725747785751 ) ) ;
#70605 = CARTESIAN_POINT ( 'NONE',  ( 117.2009162446675390, -42.82382785266567993, 128.3956252759109873 ) ) ;
#70606 = ORIENTED_EDGE ( 'NONE', *, *, #77607, .T. ) ;
#70607 = ORIENTED_EDGE ( 'NONE', *, *, #42269, .T. ) ;
#70608 = ORIENTED_EDGE ( 'NONE', *, *, #18724, .F. ) ;
#70609 = CARTESIAN_POINT ( 'NONE',  ( 10.08507579090307971, 74.81978989419388881, 130.1661673264300418 ) ) ;
#70610 = DIRECTION ( 'NONE',  ( -0.7071067811865536790, 0.7071067811865414665, 0.000000000000000000 ) ) ;
#70611 = CARTESIAN_POINT ( 'NONE',  ( 113.1782937644530307, -44.75186859791577376, 79.09395860856413663 ) ) ;
#70612 = LINE ( 'NONE', #42878, #9089 ) ;
#70613 = CARTESIAN_POINT ( 'NONE',  ( 115.2156275924750020, -36.25915663771239394, 226.6909475124489575 ) ) ;
#70614 = AXIS2_PLACEMENT_3D ( 'NONE', #87593, #88047, #73506 ) ;
#70615 = LINE ( 'NONE', #15656, #24751 ) ;
#70616 = CYLINDRICAL_SURFACE ( 'NONE', #8324, 9.999999999999998224 ) ;
#70617 = ORIENTED_EDGE ( 'NONE', *, *, #11437, .T. ) ;
#70620 = ORIENTED_EDGE ( 'NONE', *, *, #31343, .T. ) ;
#70619 = ORIENTED_EDGE ( 'NONE', *, *, #7630, .F. ) ;
#70618 = EDGE_CURVE ( 'NONE', #17829, #70235, #3575, .T. ) ;
#70621 = DIRECTION ( 'NONE',  ( -3.100000000000000258E-29, 3.100000000000000044E-14, 1.000000000000000000 ) ) ;
#70622 = ORIENTED_EDGE ( 'NONE', *, *, #83235, .T. ) ;
#70623 = ORIENTED_EDGE ( 'NONE', *, *, #48510, .T. ) ;
#70624 = DIRECTION ( 'NONE',  ( 0.000000000000000000, 0.000000000000000000, -1.000000000000000000 ) ) ;
#70625 = EDGE_CURVE ( 'NONE', #2213, #84589, #58041, .T. ) ;
#70626 = CARTESIAN_POINT ( 'NONE',  ( 147.0793590841609841, -69.57571276584434372, 247.4899279706389734 ) ) ;
#70627 = CARTESIAN_POINT ( 'NONE',  ( 100.1609931986295976, -31.17584605865120295, 237.2187261630399746 ) ) ;
#70628 = CARTESIAN_POINT ( 'NONE',  ( 97.81186544543886896, -40.51730612966257183, 271.6361395295153898 ) ) ;
#70629 = EDGE_LOOP ( 'NONE', ( #1319, #79358 ) ) ;
#70630 = AXIS2_PLACEMENT_3D ( 'NONE', #77443, #17008, #43801 ) ;
#70631 = B_SPLINE_CURVE_WITH_KNOTS ( 'NONE', 3,
 ( #66507, #4296, #31986, #25173, #43827, #9327, #16590, #64736, #2520, #53747, #74673, #67857, #12451, #41037, #26081, #54642, #47841, #88764, #26522, #81515, #12906, #40595, #11562, #87860, #54195, #68311, #19268, #34223, #32882, #46942, #39254, #60581, #88323, #53301, #39692, #12009, #67397, #68759, #73776, #75579, #18358, #6527, #82405, #32423, #40137, #46043, #61033, #5645, #18813, #33337, #60126, #25625, #47391, #13350, #61928, #81958, #5189, #46495, #61477, #6093, #89659, #20167, #27409, #4742, #19706, #66962, #81066, #74233, #33782, #75122, #89210, #26976, #80609, #20612, #28299, #62823, #36024, #83737, #62377, #21514, #21057, #35566 ),
 .UNSPECIFIED., .F., .F.,
 ( 4, 2, 2, 2, 2, 2, 2, 2, 2, 2, 2, 2, 2, 2, 2, 2, 2, 2, 2, 2, 2, 2, 2, 2, 2, 2, 2, 2, 2, 2, 2, 2, 2, 2, 2, 2, 2, 2, 2, 2, 4 ),
 ( 7.021675287307244464E-05, 0.0002385562018683249643, 0.0004068956508635774975, 0.0007435745488541031095, 0.001416932344835133408, 0.002763647936797193356, 0.004110363528759253086, 0.005457079120721313251, 0.006803794712683372548, 0.007477152508664412604, 0.008150510304645452661, 0.009497225896607553591, 0.01084394148856965626, 0.01219065708053175892, 0.01353737267249385812, 0.01488408826445596078, 0.01623080385641805998, 0.01892423504034226531, 0.02027095063230434716, 0.02161766622426642900, 0.02296438181622851432, 0.02431109740819059617, 0.02498445520417162669, 0.02565781300015265720, 0.02700452859211470436, 0.02835124418407675845, 0.02969795977603881601, 0.03104467536800087010, 0.03239139095996292766, 0.03306474875594395124, 0.03373810655192497482, 0.03508482214388704973, 0.03643153773584913158, 0.03777825332781119955, 0.03912496891977328140, 0.04047168451173535630, 0.04181840010369743815, 0.04249175789967847561, 0.04282843679766901168, 0.04299677624666430054, 0.04316511569565958245 ),
 .UNSPECIFIED. ) ;
#70632 = DIRECTION ( 'NONE',  ( 1.000000000000000000, 4.299999999999999979E-14, 1.000000000000000078E-15 ) ) ;
#70633 = CARTESIAN_POINT ( 'NONE',  ( 107.0664832912739399, -36.72944715994095333, 315.6356252759111953 ) ) ;
#70634 = VERTEX_POINT ( 'NONE', #34292 ) ;
#70635 = ORIENTED_EDGE ( 'NONE', *, *, #3874, .F. ) ;
#70636 = AXIS2_PLACEMENT_3D ( 'NONE', #43276, #56457, #57357 ) ;
#70637 = CIRCLE ( 'NONE', #47382, 2.029999999999997140 ) ;
#70638 = LINE ( 'NONE', #23401, #82145 ) ;
#70639 = AXIS2_PLACEMENT_3D ( 'NONE', #8609, #57630, #70837 ) ;
#70640 = EDGE_LOOP ( 'NONE', ( #15297, #46019, #47035, #59199 ) ) ;
#70641 = ORIENTED_EDGE ( 'NONE', *, *, #3814, .F. ) ;
#70642 = EDGE_CURVE ( 'NONE', #86777, #46470, #7050, .T. ) ;
#70643 = CARTESIAN_POINT ( 'NONE',  ( 101.0492827672293714, -31.21374014463884805, 273.5538046553056688 ) ) ;
#70644 = CARTESIAN_POINT ( 'NONE',  ( 102.9045757522767843, -27.10877478265368623, 155.4013395616249795 ) ) ;
#70645 = CARTESIAN_POINT ( 'NONE',  ( 96.66376384204015437, -36.61947630124858932, 111.3184824187679567 ) ) ;
#70646 = LINE ( 'NONE', #36117, #21075 ) ;
#70647 = ADVANCED_FACE ( 'NONE', ( #41541 ), #33851, .T. ) ;
#70648 = CARTESIAN_POINT ( 'NONE',  ( 105.5982380168385930, -102.8532777164006262, -19.78219314458207378 ) ) ;
#70649 = CARTESIAN_POINT ( 'NONE',  ( 113.1000543987032785, -45.99065659369661319, 219.0480062282919960 ) ) ;
#70650 = FACE_OUTER_BOUND ( 'NONE', #73050, .T. ) ;
#70651 = CARTESIAN_POINT ( 'NONE',  ( 46.32460016641637424, -48.34074026909789268, 180.4678068554150911 ) ) ;
#70652 = VERTEX_POINT ( 'NONE', #21128 ) ;
#70653 = CARTESIAN_POINT ( 'NONE',  ( -130.4017839623309669, 71.54617234588344843, 6.354402276675589434 ) ) ;
#70654 = ORIENTED_EDGE ( 'NONE', *, *, #59885, .T. ) ;
#70655 = ORIENTED_EDGE ( 'NONE', *, *, #43413, .F. ) ;
#70656 = CARTESIAN_POINT ( 'NONE',  ( 0.000000000000000000, 124.5870000000000033, 0.000000000000000000 ) ) ;
#70657 = CIRCLE ( 'NONE', #37319, 7.199999999999998401 ) ;
#70658 = CIRCLE ( 'NONE', #82272, 2.517499999999998739 ) ;
#70659 = ORIENTED_EDGE ( 'NONE', *, *, #11540, .F. ) ;
#70660 = CARTESIAN_POINT ( 'NONE',  ( 102.6975360555999259, -46.88284006984166297, 137.2651490854349561 ) ) ;
#70661 = DIRECTION ( 'NONE',  ( 0.000000000000000000, -1.000000000000000000, 0.000000000000000000 ) ) ;
#70662 = CARTESIAN_POINT ( 'NONE',  ( 136.2652213603992948, -35.07517613920733623, 7.387586420634884021 ) ) ;
#70663 = DIRECTION ( 'NONE',  ( 1.000000000000000078E-15, -1.000000000000000083E-30, -1.000000000000000000 ) ) ;
#70666 = CARTESIAN_POINT ( 'NONE',  ( 116.8642987764956160, -41.79567201640973195, 239.4346728949589647 ) ) ;
#70665 = CARTESIAN_POINT ( 'NONE',  ( 93.56648329127393993, -36.72944715994093912, 311.6356252759112522 ) ) ;
#70664 = DIRECTION ( 'NONE',  ( 8.568612280716163558E-05, -0.4999999926578935772, -0.8660254037844357100 ) ) ;
#70667 = DIRECTION ( 'NONE',  ( -3.100000000000000258E-29, 3.100000000000000044E-14, 1.000000000000000000 ) ) ;
#70668 = CARTESIAN_POINT ( 'NONE',  ( 107.0664832912739683, -25.27030990763060103, 305.0306255462182321 ) ) ;
#70669 = FACE_OUTER_BOUND ( 'NONE', #87963, .T. ) ;
#70670 = CYLINDRICAL_SURFACE ( 'NONE', #86316, 5.599999999999994316 ) ;
#70671 = PLANE ( 'NONE',  #19861 ) ;
#70672 = CARTESIAN_POINT ( 'NONE',  ( 147.0667039024457665, -137.6758868153238780, 245.5072646551060132 ) ) ;
#70674 = ORIENTED_EDGE ( 'NONE', *, *, #35821, .T. ) ;
#70673 = CARTESIAN_POINT ( 'NONE',  ( 118.1543649935527185, -36.20813824561556515, 268.8518157521014587 ) ) ;
#70675 = DIRECTION ( 'NONE',  ( 1.825781832977094175E-16, -0.4999999999999998890, -0.8660254037844387076 ) ) ;
#70676 = CARTESIAN_POINT ( 'NONE',  ( 113.3446846601215441, -45.07992904040708737, 143.0899109901969553 ) ) ;
#70677 = CARTESIAN_POINT ( 'NONE',  ( 110.5551769720564863, -46.59100632561725064, 33.84705384733993583 ) ) ;
#70678 = CARTESIAN_POINT ( 'NONE',  ( 107.5678551521628492, -47.81755451042874228, 188.6003871806729535 ) ) ;
#70679 = DIRECTION ( 'NONE',  ( 0.000000000000000000, 0.000000000000000000, 1.000000000000000000 ) ) ;
#70680 = DIRECTION ( 'NONE',  ( 4.299999999999999979E-14, -1.000000000000000000, 4.400000000000000367E-29 ) ) ;
#70682 = DIRECTION ( 'NONE',  ( 0.000000000000000000, 1.000000000000000000, 0.000000000000000000 ) ) ;
#70681 = CARTESIAN_POINT ( 'NONE',  ( 100.4020455594773722, -108.7036397175021136, -19.78219314458187839 ) ) ;
#70683 = CARTESIAN_POINT ( 'NONE',  ( 120.3352449817834895, -37.86742168929413310, 299.5704287327187103 ) ) ;
#70684 = CARTESIAN_POINT ( 'NONE',  ( 122.2221484686746322, -104.2784471599418055, -11.78219314458200984 ) ) ;
#70685 = ORIENTED_EDGE ( 'NONE', *, *, #22923, .T. ) ;
#70686 = VECTOR ( 'NONE', #26309, 1000.000000000000000 ) ;
#70687 = LINE ( 'NONE', #22543, #71719 ) ;
#70688 = EDGE_CURVE ( 'NONE', #63748, #7464, #46216, .T. ) ;
#70689 = EDGE_LOOP ( 'NONE', ( #74732, #80443, #16964, #54509, #19767, #5413, #57004, #81487, #42399, #41406, #35651, #48044 ) ) ;
#70690 = VERTEX_POINT ( 'NONE', #59420 ) ;
#70692 = ORIENTED_EDGE ( 'NONE', *, *, #40986, .T. ) ;
#70691 = CARTESIAN_POINT ( 'NONE',  ( 213.1962561210690126, 52.73749999999999716, -44.45000000000000284 ) ) ;
#70693 = CARTESIAN_POINT ( 'NONE',  ( 100.9539191370902387, -46.85292318231929443, 48.14419670448194211 ) ) ;
#70694 = CARTESIAN_POINT ( 'NONE',  ( 21.03689327557711763, -23.42844715994186089, 249.9678068554150059 ) ) ;
#70695 = CARTESIAN_POINT ( 'NONE',  ( 20.03715912545637678, -24.42818131006202265, 193.9678068554150627 ) ) ;
#70696 = CARTESIAN_POINT ( 'NONE',  ( 113.6418603426413938, -28.58344220020606130, 160.5356252759109736 ) ) ;
#70697 = CIRCLE ( 'NONE', #37295, 0.4999999999999932832 ) ;
#70698 = VECTOR ( 'NONE', #9478, 1000.000000000000000 ) ;
#70699 = CARTESIAN_POINT ( 'NONE',  ( 107.8428746604417654, -27.05123223485975714, 264.4352769709337849 ) ) ;
#70700 = ORIENTED_EDGE ( 'NONE', *, *, #28258, .F. ) ;
#70701 = ORIENTED_EDGE ( 'NONE', *, *, #78966, .F. ) ;
#70702 = ORIENTED_EDGE ( 'NONE', *, *, #17207, .T. ) ;
#70703 = VECTOR ( 'NONE', #49538, 1000.000000000000114 ) ;
#70705 = EDGE_CURVE ( 'NONE', #1627, #27673, #37656, .T. ) ;
#70704 = VECTOR ( 'NONE', #50369, 1000.000000000000000 ) ;
#70706 = ORIENTED_EDGE ( 'NONE', *, *, #79687, .T. ) ;
#70707 = CARTESIAN_POINT ( 'NONE',  ( 116.7951252717554098, -39.38782978876485430, 108.6147919426823734 ) ) ;
#70708 = CARTESIAN_POINT ( 'NONE',  ( 68.06670390244704549, -114.5284471599409812, 45.21780685541799727 ) ) ;
#70709 = CIRCLE ( 'NONE', #47458, 37.00000000000000711 ) ;
#70710 = CARTESIAN_POINT ( 'NONE',  ( 85.06670390244700286, -74.11757344603526576, 222.2178068554179902 ) ) ;
#70711 = CARTESIAN_POINT ( 'NONE',  ( 93.91125933621933086, -96.68314769832137756, -21.78219314458224076 ) ) ;
#70712 = CARTESIAN_POINT ( 'NONE',  ( 134.0664832912740110, 0.2215528400590013880, 4.925625275911999168 ) ) ;
#70713 = DIRECTION ( 'NONE',  ( 0.000000000000000000, 0.000000000000000000, 1.000000000000000000 ) ) ;
#70714 = CARTESIAN_POINT ( 'NONE',  ( 172.5664832912740110, 0.2215528400590013880, 138.9256252759119832 ) ) ;
#70715 = DIRECTION ( 'NONE',  ( 0.000000000000000000, 0.000000000000000000, -1.000000000000000000 ) ) ;
#70716 = CARTESIAN_POINT ( 'NONE',  ( 99.08262072259961428, -44.34008189452615056, 36.92038718067297509 ) ) ;
#70717 = CARTESIAN_POINT ( 'NONE',  ( -1.663375835020804772, 69.95244002925302595, 118.5450630894975603 ) ) ;
#70718 = ADVANCED_FACE ( 'NONE', ( #33406 ), #82919, .F. ) ;
#70719 = ORIENTED_EDGE ( 'NONE', *, *, #10486, .T. ) ;
#70720 = AXIS2_PLACEMENT_3D ( 'NONE', #87076, #25278, #52506 ) ;
#70721 = EDGE_CURVE ( 'NONE', #15112, #50271, #17211, .T. ) ;
#70722 = CARTESIAN_POINT ( 'NONE',  ( 140.0667039024470171, -90.27844715994091018, 51.21780685541800437 ) ) ;
#70723 = CIRCLE ( 'NONE', #14108, 218.1859999999999786 ) ;
#70724 = VECTOR ( 'NONE', #42135, 1000.000000000000000 ) ;
#70725 = CARTESIAN_POINT ( 'NONE',  ( 204.2160000000000082, 52.73749999999999716, -49.21249999999999858 ) ) ;
#70726 = CARTESIAN_POINT ( 'NONE',  ( 112.5586783213544066, -42.80550525696455821, 130.9795189410199612 ) ) ;
#70727 = CIRCLE ( 'NONE', #9766, 0.5000000000000004441 ) ;
#70728 = EDGE_CURVE ( 'NONE', #13444, #89348, #66925, .T. ) ;
#70729 = CARTESIAN_POINT ( 'NONE',  ( 97.81168844167092402, -40.51740470302234343, 181.6357138554620576 ) ) ;
#70730 = DIRECTION ( 'NONE',  ( -0.7396053187813123042, -0.6730408400909958511, 0.000000000000000000 ) ) ;
#70731 = ORIENTED_EDGE ( 'NONE', *, *, #65446, .F. ) ;
#70732 = ORIENTED_EDGE ( 'NONE', *, *, #36016, .F. ) ;
#70733 = CARTESIAN_POINT ( 'NONE',  ( 115.0375080342936940, -42.90814572238593172, 138.3000974113143684 ) ) ;
#70734 = ORIENTED_EDGE ( 'NONE', *, *, #44350, .F. ) ;
#70735 = EDGE_LOOP ( 'NONE', ( #87240, #36064, #74147, #42447 ) ) ;
#70736 = ADVANCED_FACE ( 'NONE', ( #61547 ), #75648, .T. ) ;
#70737 = CARTESIAN_POINT ( 'NONE',  ( 103.7583319442197052, -28.50847317404091186, 126.8130118773259625 ) ) ;
#70738 = DIRECTION ( 'NONE',  ( 0.000000000000000000, 0.000000000000000000, -1.000000000000000000 ) ) ;
#70739 = CARTESIAN_POINT ( 'NONE',  ( 98.82287431334749783, -28.18163096472671469, 111.6870538473389587 ) ) ;
#70740 = VECTOR ( 'NONE', #46059, 1000.000000000000000 ) ;
#70741 = DIRECTION ( 'NONE',  ( 3.999999999999999995E-14, -1.000000000000000000, 4.100000000000000342E-29 ) ) ;
#70742 = ORIENTED_EDGE ( 'NONE', *, *, #33186, .T. ) ;
#70743 = ORIENTED_EDGE ( 'NONE', *, *, #59975, .T. ) ;
#70744 = EDGE_LOOP ( 'NONE', ( #24728, #31280, #40220, #48802 ) ) ;
#70745 = EDGE_CURVE ( 'NONE', #31377, #34776, #29737, .T. ) ;
#70746 = CARTESIAN_POINT ( 'NONE',  ( 118.0120547386033678, -38.42941975617429762, 68.69181575210198787 ) ) ;
#70747 = ORIENTED_EDGE ( 'NONE', *, *, #8151, .F. ) ;
#70748 = CARTESIAN_POINT ( 'NONE',  ( 117.4208826026019779, -36.15918394850536544, 273.8822919425783198 ) ) ;
#70749 = CARTESIAN_POINT ( 'NONE',  ( 103.5350399278988078, -26.85989278392735002, 186.3499109901969746 ) ) ;
#70750 = ADVANCED_FACE ( 'NONE', ( #21585 ), #29292, .F. ) ;
#70751 = CARTESIAN_POINT ( 'NONE',  ( 107.0664832912748068, -36.72944715993923381, -5.074374724089029343 ) ) ;
#70752 = CARTESIAN_POINT ( 'NONE',  ( 99.04385435236613944, -42.84094592217979169, 127.8439293676477462 ) ) ;
#70753 = CARTESIAN_POINT ( 'NONE',  ( 95.77906782739819391, -40.33899944578667629, 127.5727681330539554 ) ) ;
#70755 = EDGE_CURVE ( 'NONE', #5050, #26855, #36555, .T. ) ;
#70754 = LINE ( 'NONE', #63936, #19008 ) ;
#70756 = ORIENTED_EDGE ( 'NONE', *, *, #58899, .T. ) ;
#70757 = FACE_OUTER_BOUND ( 'NONE', #36860, .T. ) ;
#70758 = EDGE_CURVE ( 'NONE', #50262, #73333, #43341, .T. ) ;
#70759 = CIRCLE ( 'NONE', #6878, 0.5000000000000004441 ) ;
#70760 = VERTEX_POINT ( 'NONE', #64257 ) ;
#70761 = DIRECTION ( 'NONE',  ( -1.000000000000000000, -2.422134843531340666E-15, 0.000000000000000000 ) ) ;
#70762 = ORIENTED_EDGE ( 'NONE', *, *, #54903, .F. ) ;
#70763 = ORIENTED_EDGE ( 'NONE', *, *, #61487, .F. ) ;
#70764 = VECTOR ( 'NONE', #57601, 1000.000000000000000 ) ;
#70765 = FACE_BOUND ( 'NONE', #57746, .T. ) ;
#70766 = AXIS2_PLACEMENT_3D ( 'NONE', #84227, #55121, #61956 ) ;
#70767 = DIRECTION ( 'NONE',  ( 0.000000000000000000, 0.000000000000000000, 1.000000000000000000 ) ) ;
#70768 = CARTESIAN_POINT ( 'NONE',  ( 116.3877942521162936, -31.98191425893181261, 44.20133956162491984 ) ) ;
#70769 = CARTESIAN_POINT ( 'NONE',  ( 49.35211078756498893, -35.65087443492551245, -5.074374724088000832 ) ) ;
#70770 = CARTESIAN_POINT ( 'NONE',  ( 101.3983180920321985, -48.92675847326103167, 9.425625275910963552 ) ) ;
#70771 = CARTESIAN_POINT ( 'NONE',  ( 6.938893903907229955E-15, 50.79999999999999716, 216.0269999999999868 ) ) ;
#70772 = CARTESIAN_POINT ( 'NONE',  ( 102.2761128416349123, -28.20209198692209185, 60.48419670448296159 ) ) ;
#70774 = CARTESIAN_POINT ( 'NONE',  ( 96.67182511810091228, -37.15340426533111895, 157.3584824187679487 ) ) ;
#70773 = CARTESIAN_POINT ( 'NONE',  ( 97.12561475596668004, -37.99732759006241878, 111.4273445057939824 ) ) ;
#70775 = CARTESIAN_POINT ( 'NONE',  ( 168.5667039024483813, -48.82844715993517326, 249.9678068554149775 ) ) ;
#70776 = CYLINDRICAL_SURFACE ( 'NONE', #35074, 4.874999999999990230 ) ;
#70777 = EDGE_LOOP ( 'NONE', ( #71596, #62625, #52789, #66790 ) ) ;
#70778 = DIRECTION ( 'NONE',  ( 0.000000000000000000, 0.000000000000000000, 1.000000000000000000 ) ) ;
#70779 = AXIS2_PLACEMENT_3D ( 'NONE', #79782, #3899, #31596 ) ;
#70780 = CARTESIAN_POINT ( 'NONE',  ( -20.82352280117506282, 62.28388828036364799, 31.90676034344724243 ) ) ;
#70781 = CARTESIAN_POINT ( 'NONE',  ( 172.5664832912740110, -18.82844715994099971, 318.9256252759120116 ) ) ;
#70782 = VERTEX_POINT ( 'NONE', #85161 ) ;
#70783 = VECTOR ( 'NONE', #43595, 1000.000000000000000 ) ;
#70784 = DIRECTION ( 'NONE',  ( -3.100000000000000258E-29, 3.100000000000000044E-14, 1.000000000000000000 ) ) ;
#70786 = ORIENTED_EDGE ( 'NONE', *, *, #84686, .F. ) ;
#70785 = CARTESIAN_POINT ( 'NONE',  ( 98.13053560861905567, -31.27458647820624549, 170.8899109901960003 ) ) ;
#70787 = DIRECTION ( 'NONE',  ( 3.596091637922019804E-15, 0.000000000000000000, 1.000000000000000000 ) ) ;
#70788 = CARTESIAN_POINT ( 'NONE',  ( 106.3003414554210764, -47.14819399153626023, 218.5184824187679453 ) ) ;
#70789 = CARTESIAN_POINT ( 'NONE',  ( 117.0163018969640376, -33.47459087099611708, 85.07848241876791917 ) ) ;
#70790 = VECTOR ( 'NONE', #44543, 1000.000000000000000 ) ;
#70791 = CARTESIAN_POINT ( 'NONE',  ( 100.8068867829397703, 80.88456863959029874, 82.96304607088372052 ) ) ;
#70792 = AXIS2_PLACEMENT_3D ( 'NONE', #69311, #7084, #44592 ) ;
#70793 = DIRECTION ( 'NONE',  ( 0.000000000000000000, 0.000000000000000000, 1.000000000000000000 ) ) ;
#70794 = LINE ( 'NONE', #35799, #64117 ) ;
#70795 = ORIENTED_EDGE ( 'NONE', *, *, #63143, .T. ) ;
#70796 = ORIENTED_EDGE ( 'NONE', *, *, #20308, .F. ) ;
#70797 = VERTEX_POINT ( 'NONE', #49257 ) ;
#70798 = VERTEX_POINT ( 'NONE', #1132 ) ;
#70799 = PLANE ( 'NONE',  #59759 ) ;
#70800 = CARTESIAN_POINT ( 'NONE',  ( 96.24939603668094890, -34.45687069020234361, 257.1737205140064475 ) ) ;
#70801 = CARTESIAN_POINT ( 'NONE',  ( 97.12053416263984218, -35.23531894072210946, 251.2083665227183928 ) ) ;
#70802 = CARTESIAN_POINT ( 'NONE',  ( 135.4870310422650732, -16.36767655970465540, 1.942446731291206596 ) ) ;
#70804 = CARTESIAN_POINT ( 'NONE',  ( 25.56670390244797275, -48.82844715994099971, 139.9678068554150059 ) ) ;
#70803 = CARTESIAN_POINT ( 'NONE',  ( 70.06968321367156705, -140.6784088069870222, 245.5331728854790185 ) ) ;
#70805 = DIRECTION ( 'NONE',  ( 0.000000000000000000, 7.536132396315209176E-17, -1.000000000000000000 ) ) ;
#70806 = CIRCLE ( 'NONE', #24372, 7.937500000000000000 ) ;
#70807 = CARTESIAN_POINT ( 'NONE',  ( 96.81178581975444786, -38.90419831550661911, 31.49276813305495892 ) ) ;
#70808 = VERTEX_POINT ( 'NONE', #14772 ) ;
#70809 = VECTOR ( 'NONE', #32899, 999.9999999999998863 ) ;
#70810 = ORIENTED_EDGE ( 'NONE', *, *, #48335, .F. ) ;
#70811 = EDGE_LOOP ( 'NONE', ( #5979, #44112, #61013, #53544 ) ) ;
#70812 = DIRECTION ( 'NONE',  ( -1.000000000000000078E-15, -1.000000000000000083E-30, 1.000000000000000000 ) ) ;
#70813 = CARTESIAN_POINT ( 'NONE',  ( 100.9553767296363702, -28.70647492237798559, 16.59715524421730137 ) ) ;
#70814 = EDGE_CURVE ( 'NONE', #58395, #72856, #22932, .T. ) ;
#70815 = CARTESIAN_POINT ( 'NONE',  ( 115.3604274781776411, -30.50455558986046256, 260.3508633711485345 ) ) ;
#70816 = FACE_OUTER_BOUND ( 'NONE', #65410, .T. ) ;
#70817 = EDGE_CURVE ( 'NONE', #88126, #86096, #63810, .T. ) ;
#70818 = CARTESIAN_POINT ( 'NONE',  ( 116.5394839232219510, -34.29517225379352396, 120.0270538473389479 ) ) ;
#70819 = CARTESIAN_POINT ( 'NONE',  ( 50.42303506447345285, 91.07499999999996021, -73.21698938693724301 ) ) ;
#70820 = LINE ( 'NONE', #71712, #1045 ) ;
#70821 = ADVANCED_FACE ( 'NONE', ( #50154 ), #28841, .T. ) ;
#70822 = ORIENTED_EDGE ( 'NONE', *, *, #30326, .T. ) ;
#70823 = DIRECTION ( 'NONE',  ( 0.7071067811874278686, -0.7071067811856670549, 2.899137802861351288E-29 ) ) ;
#70824 = ADVANCED_FACE ( 'NONE', ( #50609, #41995 ), #36096, .F. ) ;
#70825 = CARTESIAN_POINT ( 'NONE',  ( 77.50946880809780737, -35.71735499139281700, 2.839545688279709434 ) ) ;
#70826 = VECTOR ( 'NONE', #9543, 1000.000000000000000 ) ;
#70827 = ORIENTED_EDGE ( 'NONE', *, *, #19869, .T. ) ;
#70828 = EDGE_LOOP ( 'NONE', ( #34752, #31066, #49785, #17902, #13940, #67120 ) ) ;
#70829 = CARTESIAN_POINT ( 'NONE',  ( -84.12159398442656766, 95.25015226514366873, 83.54193218351881001 ) ) ;
#70830 = CARTESIAN_POINT ( 'NONE',  ( 111.0712550167563677, -29.58490437025668740, 32.48809036959193719 ) ) ;
#70831 = EDGE_CURVE ( 'NONE', #12282, #72980, #77433, .T. ) ;
#70832 = VECTOR ( 'NONE', #44182, 1000.000000000000000 ) ;
#70833 = CIRCLE ( 'NONE', #85370, 2.117000000000000881 ) ;
#70834 = DIRECTION ( 'NONE',  ( 4.194175870806139918E-14, -1.000000000000000000, 0.000000000000000000 ) ) ;
#70835 = EDGE_CURVE ( 'NONE', #86595, #77621, #57425, .T. ) ;
#70836 = CARTESIAN_POINT ( 'NONE',  ( 112.1393456466975636, -28.01282278429165729, 84.65645860877889106 ) ) ;
#70837 = DIRECTION ( 'NONE',  ( -0.9254794337955620787, -0.3787978585227822492, 0.000000000000000000 ) ) ;
#70838 = ORIENTED_EDGE ( 'NONE', *, *, #55348, .F. ) ;
#70839 = DIRECTION ( 'NONE',  ( 2.900000000000000265E-14, -2.000000000000000155E-15, 1.000000000000000000 ) ) ;
#70840 = CIRCLE ( 'NONE', #82458, 7.937500000000000000 ) ;
#70841 = CARTESIAN_POINT ( 'NONE',  ( 182.0374245136140701, -23.42844715993459559, 237.4678068554150059 ) ) ;
#70842 = EDGE_LOOP ( 'NONE', ( #5286, #87455, #28388, #35604, #6876, #81872, #30971, #22037, #36684, #77748, #26279, #88819 ) ) ;
#70843 = CARTESIAN_POINT ( 'NONE',  ( 117.4476241407275978, -37.68806341539836069, 78.75276813305399060 ) ) ;
#70844 = VERTEX_POINT ( 'NONE', #8400 ) ;
#70845 = CARTESIAN_POINT ( 'NONE',  ( 98.84295822536005005, -39.42912807745279480, 284.4090427505438470 ) ) ;
#70846 = ADVANCED_FACE ( 'NONE', ( #22480 ), #35182, .T. ) ;
#70847 = AXIS2_PLACEMENT_3D ( 'NONE', #51573, #59287, #44767 ) ;
#70848 = LINE ( 'NONE', #7270, #2494 ) ;
#70849 = CARTESIAN_POINT ( 'NONE',  ( 118.1473594538626486, -37.63838399483783093, 188.7613395616259595 ) ) ;
#70850 = DIRECTION ( 'NONE',  ( 0.000000000000000000, 0.000000000000000000, 1.000000000000000000 ) ) ;
#70851 = CARTESIAN_POINT ( 'NONE',  ( 131.3179999999999836, 44.45000000000000284, 32.49205688096009936 ) ) ;
#70852 = VECTOR ( 'NONE', #57174, 999.9999999999998863 ) ;
#70853 = DIRECTION ( 'NONE',  ( 0.000000000000000000, 0.000000000000000000, 1.000000000000000000 ) ) ;
#70854 = AXIS2_PLACEMENT_3D ( 'NONE', #36815, #16818, #15930 ) ;
#70855 = LINE ( 'NONE', #57644, #24739 ) ;
#70856 = CARTESIAN_POINT ( 'NONE',  ( 111.7585843298372197, -27.37117935058896379, 275.7070538473396937 ) ) ;
#70857 = CARTESIAN_POINT ( 'NONE',  ( 74.36911441044797755, 83.38952084682853183, -92.32962665258484947 ) ) ;
#70858 = ORIENTED_EDGE ( 'NONE', *, *, #3023, .F. ) ;
#70859 = PLANE ( 'NONE',  #73398 ) ;
#70860 = VERTEX_POINT ( 'NONE', #16112 ) ;
#70861 = CARTESIAN_POINT ( 'NONE',  ( 108.7502231993919395, -25.75847702231262204, 140.9432443235299672 ) ) ;
#70862 = LINE ( 'NONE', #79012, #80208 ) ;
#70863 = ORIENTED_EDGE ( 'NONE', *, *, #79133, .F. ) ;
#70864 = ORIENTED_EDGE ( 'NONE', *, *, #58143, .T. ) ;
#70865 = EDGE_LOOP ( 'NONE', ( #29441, #73642, #58757, #73965 ) ) ;
#70866 = VECTOR ( 'NONE', #65489, 1000.000000000000114 ) ;
#70867 = CARTESIAN_POINT ( 'NONE',  ( 105.7154772066486288, -46.72385837650929830, 122.4689585993907457 ) ) ;
#70868 = CARTESIAN_POINT ( 'NONE',  ( -41.60202597009397607, 40.59999999999997300, 47.03909206933071374 ) ) ;
#70869 = DIRECTION ( 'NONE',  ( 0.000000000000000000, 0.000000000000000000, -1.000000000000000000 ) ) ;
#70870 = FACE_OUTER_BOUND ( 'NONE', #17698, .T. ) ;
#70871 = DIRECTION ( 'NONE',  ( 0.2588190451025229599, 0.000000000000000000, 0.9659258262890676461 ) ) ;
#70872 = CARTESIAN_POINT ( 'NONE',  ( 95.25919473906076007, -35.71823372881362957, 32.25848241876794020 ) ) ;
#70874 = ADVANCED_FACE ( 'NONE', ( #62893 ), #38974, .F. ) ;
#70873 = DIRECTION ( 'NONE',  ( -0.8660254037844384856, 0.000000000000000000, 0.5000000000000003331 ) ) ;
#70875 = EDGE_LOOP ( 'NONE', ( #46343, #39480 ) ) ;
#70876 = PLANE ( 'NONE',  #22507 ) ;
#70877 = ADVANCED_FACE ( 'NONE', ( #71528 ), #8857, .F. ) ;
#70878 = AXIS2_PLACEMENT_3D ( 'NONE', #62671, #84029, #15438 ) ;
#70879 = DIRECTION ( 'NONE',  ( 0.000000000000000000, 1.000000000000000000, 0.000000000000000000 ) ) ;
#70880 = ORIENTED_EDGE ( 'NONE', *, *, #19345, .F. ) ;
#70882 = ORIENTED_EDGE ( 'NONE', *, *, #47718, .T. ) ;
#70881 = AXIS2_PLACEMENT_3D ( 'NONE', #53041, #59438, #86722 ) ;
#70883 = CARTESIAN_POINT ( 'NONE',  ( 81.24991378862624458, -21.21189172703844861, 1.845048092480171320 ) ) ;
#70884 = CARTESIAN_POINT ( 'NONE',  ( 152.5667039024474718, -23.42844715993585325, 180.4678068554149775 ) ) ;
#70885 = DIRECTION ( 'NONE',  ( 0.000000000000000000, 0.000000000000000000, 1.000000000000000000 ) ) ;
#70886 = FACE_BOUND ( 'NONE', #80818, .T. ) ;
#70887 = DIRECTION ( 'NONE',  ( 1.000000000000000078E-15, -1.000000000000000083E-30, -1.000000000000000000 ) ) ;
#70888 = CARTESIAN_POINT ( 'NONE',  ( 109.6796103444932129, -28.56711482602328900, 234.2524198280769951 ) ) ;
#70889 = FACE_OUTER_BOUND ( 'NONE', #36583, .T. ) ;
#70890 = CARTESIAN_POINT ( 'NONE',  ( 124.3463864195482387, 71.42811502680554270, 39.78527854427932198 ) ) ;
#70891 = CARTESIAN_POINT ( 'NONE',  ( 112.8260979389708183, -47.14365076028245483, 102.9784824187679817 ) ) ;
#70892 = ORIENTED_EDGE ( 'NONE', *, *, #53404, .F. ) ;
#70893 = CARTESIAN_POINT ( 'NONE',  ( 82.54999999999999716, 69.84999999999999432, 280.2255000000000109 ) ) ;
#70894 = ORIENTED_EDGE ( 'NONE', *, *, #31629, .T. ) ;
#70895 = DIRECTION ( 'NONE',  ( 1.000000000000000000, 0.000000000000000000, 0.000000000000000000 ) ) ;
#70896 = CARTESIAN_POINT ( 'NONE',  ( 103.2784163218621529, -27.47468898029232065, 276.3856337844811719 ) ) ;
#70897 = ORIENTED_EDGE ( 'NONE', *, *, #65386, .T. ) ;
#70898 = AXIS2_PLACEMENT_3D ( 'NONE', #32534, #39793, #54752 ) ;
#70899 = DIRECTION ( 'NONE',  ( 0.000000000000000000, 0.000000000000000000, 1.000000000000000000 ) ) ;
#70900 = ORIENTED_EDGE ( 'NONE', *, *, #43175, .F. ) ;
#70901 = DIRECTION ( 'NONE',  ( -3.999999999999999995E-14, 1.000000000000000000, -4.100000000000000342E-29 ) ) ;
#70902 = CARTESIAN_POINT ( 'NONE',  ( 67.06670390244704549, -104.4390062815841844, 245.7240875270999823 ) ) ;
#70904 = LINE ( 'NONE', #21858, #82927 ) ;
#70903 = VECTOR ( 'NONE', #8240, 1000.000000000000000 ) ;
#70905 = ORIENTED_EDGE ( 'NONE', *, *, #81339, .F. ) ;
#70906 = CIRCLE ( 'NONE', #31707, 1.000000000000000888 ) ;
#70907 = CARTESIAN_POINT ( 'NONE',  ( 117.6177984774595870, -42.17956309877360610, 93.44705384733897802 ) ) ;
#70908 =( NAMED_UNIT ( * ) SI_UNIT ( $, .STERADIAN. ) SOLID_ANGLE_UNIT ( ) );
#70909 = LINE ( 'NONE', #16386, #40519 ) ;
#70910 = DIRECTION ( 'NONE',  ( 1.000000000000000078E-15, -1.000000000000000083E-30, -1.000000000000000000 ) ) ;
#70911 = CARTESIAN_POINT ( 'NONE',  ( -10.00862986831341317, 74.85114111836281836, 117.9329634167659293 ) ) ;
#70912 = EDGE_LOOP ( 'NONE', ( #60304, #32771, #19197, #82948, #7906 ) ) ;
#70913 = AXIS2_PLACEMENT_3D ( 'NONE', #37212, #23160, #10831 ) ;
#70914 = CARTESIAN_POINT ( 'NONE',  ( 107.2978958415778123, -24.20855449189627251, 322.4523926293242653 ) ) ;
#70915 = DIRECTION ( 'NONE',  ( -0.7071067811865475727, 0.000000000000000000, 0.7071067811865475727 ) ) ;
#70916 = DIRECTION ( 'NONE',  ( -0.7071067811865165975, -0.7071067811865784369, -7.071067811865158803E-16 ) ) ;
#70917 = CARTESIAN_POINT ( 'NONE',  ( 102.2923668651898339, -27.39740514546159389, 116.4527681330539650 ) ) ;
#70918 = VECTOR ( 'NONE', #54312, 1000.000000000000000 ) ;
#70920 = CARTESIAN_POINT ( 'NONE',  ( 116.3212776292296127, -32.94146857471318413, 287.6356252759109680 ) ) ;
#70919 = CARTESIAN_POINT ( 'NONE',  ( 0.000000000000000000, 127.0000000000000000, 0.000000000000000000 ) ) ;
#70921 = DIRECTION ( 'NONE',  ( 0.000000000000000000, 0.000000000000000000, 1.000000000000000000 ) ) ;
#70922 = EDGE_CURVE ( 'NONE', #9197, #50419, #9290, .T. ) ;
#70923 = B_SPLINE_CURVE_WITH_KNOTS ( 'NONE', 3,
 ( #5569, #68240, #55014, #60964, #26003, #81878, #82780, #19628, #46419, #74153, #5111, #20541, #6022, #61402, #88692, #4662, #26448, #26890 ),
 .UNSPECIFIED., .F., .F.,
 ( 4, 2, 2, 2, 2, 2, 2, 2, 4 ),
 ( 0.5000000005383744561, 0.5625000004710776214, 0.6250000004037807866, 0.6875000003364840628, 0.7500000002691872281, 0.8125000002018903933, 0.8750000001345936695, 0.9375000000672968348, 1.000000000000000000 ),
 .UNSPECIFIED. ) ;
#70924 = ORIENTED_EDGE ( 'NONE', *, *, #73227, .T. ) ;
#70925 = EDGE_CURVE ( 'NONE', #26742, #44745, #10615, .T. ) ;
#70926 = CARTESIAN_POINT ( 'NONE',  ( 167.2371591254544967, -47.82818131005522133, 180.4678068554150059 ) ) ;
#70927 = EDGE_CURVE ( 'NONE', #11510, #56608, #17440, .T. ) ;
#70928 = CARTESIAN_POINT ( 'NONE',  ( 98.56701561008813428, -30.78824967682752245, 156.8289586092439549 ) ) ;
#70929 = VECTOR ( 'NONE', #814, 1000.000000000000000 ) ;
#70931 = ORIENTED_EDGE ( 'NONE', *, *, #62593, .F. ) ;
#70930 = LINE ( 'NONE', #65868, #85007 ) ;
#70932 = EDGE_CURVE ( 'NONE', #73971, #42802, #65140, .T. ) ;
#70933 = CARTESIAN_POINT ( 'NONE',  ( 117.4022237771661281, -37.57280582802024327, 34.77372051400595865 ) ) ;
#70934 = CARTESIAN_POINT ( 'NONE',  ( 31.71315051185499811, -33.70561438052111214, -5.074374724088000832 ) ) ;
#70935 = CARTESIAN_POINT ( 'NONE',  ( 142.8698897858160706, -0.9167816978817300289, 540.9756252759101471 ) ) ;
#70936 = FACE_OUTER_BOUND ( 'NONE', #31512, .T. ) ;
#70937 = DIRECTION ( 'NONE',  ( -1.000000000000000078E-15, 1.000000000000000083E-30, 1.000000000000000000 ) ) ;
#70938 = EDGE_CURVE ( 'NONE', #37445, #40480, #78960, .T. ) ;
#70939 = DIRECTION ( 'NONE',  ( 1.000000000000000000, 0.000000000000000000, 2.108231265501709878E-16 ) ) ;
#70940 = CARTESIAN_POINT ( 'NONE',  ( 115.3120223323506792, -44.18753462406608179, 233.2413395616259493 ) ) ;
#70941 = ORIENTED_EDGE ( 'NONE', *, *, #10355, .T. ) ;
#70942 = VERTEX_POINT ( 'NONE', #18774 ) ;
#70943 = CIRCLE ( 'NONE', #65090, 2.029999999999997140 ) ;
#70944 = CARTESIAN_POINT ( 'NONE',  ( 104.2961655698287302, -28.31198801876947613, 161.7615833058969486 ) ) ;
#70945 = ADVANCED_FACE ( 'NONE', ( #12871 ), #40556, .F. ) ;
#70946 = LINE ( 'NONE', #82788, #66134 ) ;
#70947 = CARTESIAN_POINT ( 'NONE',  ( 104.0154917791352744, -27.12933488216606648, 51.75301187732594599 ) ) ;
#70948 = DIRECTION ( 'NONE',  ( -1.000000000000000000, 0.000000000000000000, -7.867884063170659983E-16 ) ) ;
#70949 = EDGE_CURVE ( 'NONE', #74767, #6162, #13310, .T. ) ;
#70950 = CARTESIAN_POINT ( 'NONE',  ( 142.8679068202682458, 10.65431904611001634, 542.9756252759101471 ) ) ;
#70951 = CARTESIAN_POINT ( 'NONE',  ( 74.06670390244701707, -90.27844715994098124, 45.21780685541799727 ) ) ;
#70952 = CYLINDRICAL_SURFACE ( 'NONE', #21785, 2.517500000000005844 ) ;
#70953 = DIRECTION ( 'NONE',  ( 1.387778780781444413E-14, -1.000000000000000000, 0.000000000000000000 ) ) ;
#70954 = CARTESIAN_POINT ( 'NONE',  ( 96.93559702949573875, -34.21358363697170546, 276.1327681330537871 ) ) ;
#70955 = CARTESIAN_POINT ( 'NONE',  ( 11.30434615783713248, 88.13056155020463223, 117.8150791733652341 ) ) ;
#70956 = ORIENTED_EDGE ( 'NONE', *, *, #44395, .F. ) ;
#70957 = ORIENTED_EDGE ( 'NONE', *, *, #40466, .T. ) ;
#70958 = ADVANCED_FACE ( 'NONE', ( #89617 ), #18751, .F. ) ;
#70959 = VECTOR ( 'NONE', #48280, 1000.000000000000000 ) ;
#70960 = CARTESIAN_POINT ( 'NONE',  ( 123.6837132603321692, -53.34645651782491882, 249.5838068554164693 ) ) ;
#70961 = CARTESIAN_POINT ( 'NONE',  ( -78.95116244206084843, 93.33902940301970830, -88.44409384118986850 ) ) ;
#70962 = CARTESIAN_POINT ( 'NONE',  ( 51.06648329127400388, 22.62155284005901024, 333.4006252759110112 ) ) ;
#70963 = DIRECTION ( 'NONE',  ( 1.000000000000000078E-15, -1.000000000000000083E-30, -1.000000000000000000 ) ) ;
#70964 = CARTESIAN_POINT ( 'NONE',  ( 117.5198883501232103, -40.51604253736888950, 19.54991099019698453 ) ) ;
#70966 = LINE ( 'NONE', #76870, #62975 ) ;
#70965 = VECTOR ( 'NONE', #53449, 1000.000000000000000 ) ;
#70967 = VECTOR ( 'NONE', #41317, 1000.000000000000000 ) ;
#70968 = ORIENTED_EDGE ( 'NONE', *, *, #70312, .F. ) ;
#70969 = CARTESIAN_POINT ( 'NONE',  ( 168.5667039024480687, -48.82844715993497431, 300.4678068554149490 ) ) ;
#70970 = DIRECTION ( 'NONE',  ( -1.000000000000000000, 0.000000000000000000, 0.000000000000000000 ) ) ;
#70971 = CARTESIAN_POINT ( 'NONE',  ( 104.3243669996922307, -26.02151151870134171, 245.2880062282919482 ) ) ;
#70972 = ORIENTED_EDGE ( 'NONE', *, *, #61563, .T. ) ;
#70973 = CIRCLE ( 'NONE', #31785, 218.1859999999999786 ) ;
#70974 = DIRECTION ( 'NONE',  ( 1.000000000000000000, 0.000000000000000000, -2.544367396927093851E-16 ) ) ;
#70975 = CARTESIAN_POINT ( 'NONE',  ( 104.4085690792836942, -46.45823401906362449, 18.36525018442977952 ) ) ;
#70976 = CARTESIAN_POINT ( 'NONE',  ( 116.3348466390194460, -36.28970630669515174, 116.6823760838769601 ) ) ;
#70977 = CARTESIAN_POINT ( 'NONE',  ( 107.2435369062854420, -47.21027956138831883, 208.5899109901969837 ) ) ;
#70978 = CARTESIAN_POINT ( 'NONE',  ( 83.06670390244796920, -64.87844715994098976, 201.9838068554149970 ) ) ;
#70979 = EDGE_LOOP ( 'NONE', ( #76733, #53627 ) ) ;
#70980 = VECTOR ( 'NONE', #50993, 1000.000000000000000 ) ;
#70981 = EDGE_CURVE ( 'NONE', #69843, #70068, #63719, .T. ) ;
#70982 = FACE_OUTER_BOUND ( 'NONE', #15335, .T. ) ;
#70983 = EDGE_LOOP ( 'NONE', ( #47916, #68126, #37667, #80346 ) ) ;
#70984 = ORIENTED_EDGE ( 'NONE', *, *, #27242, .F. ) ;
#70985 = CARTESIAN_POINT ( 'NONE',  ( 161.4809174648183614, -49.32844715993547879, 300.4678068554149490 ) ) ;
#70986 = ORIENTED_EDGE ( 'NONE', *, *, #86417, .F. ) ;
#70987 = ORIENTED_EDGE ( 'NONE', *, *, #84900, .F. ) ;
#70988 = CARTESIAN_POINT ( 'NONE',  ( -179.8898777604655095, 0.000000000000000000, -12.69999999999999929 ) ) ;
#70989 = CARTESIAN_POINT ( 'NONE',  ( 113.2433028214677790, -28.75699364625837262, 24.55250987863361090 ) ) ;
#70990 = CIRCLE ( 'NONE', #73890, 3.000000864267343026 ) ;
#70991 = CARTESIAN_POINT ( 'NONE',  ( 103.1716831446340166, -28.55367798840643090, 139.8648007804579549 ) ) ;
#70992 = CARTESIAN_POINT ( 'NONE',  ( 112.5009111935468411, -46.38151608383146396, 257.9965776568635647 ) ) ;
#70993 = CARTESIAN_POINT ( 'NONE',  ( 182.5667039024479550, -33.35206098992156143, 117.4678068554150627 ) ) ;
#70994 = VERTEX_POINT ( 'NONE', #5147 ) ;
#70995 = EDGE_CURVE ( 'NONE', #60117, #39460, #19227, .T. ) ;
#70996 = VERTEX_POINT ( 'NONE', #12410 ) ;
#70997 = DIRECTION ( 'NONE',  ( -1.000000000000000000, -8.163404592832032979E-16, 0.000000000000000000 ) ) ;
#70998 = CARTESIAN_POINT ( 'NONE',  ( 182.2420472961719895, -31.76306994223730840, 342.9256252759119548 ) ) ;
#70999 = CARTESIAN_POINT ( 'NONE',  ( 41.56648329127399677, -9.303447159940999356, 18.92562527591200094 ) ) ;
#71000 = VECTOR ( 'NONE', #1111, 1000.000000000000000 ) ;
#71001 = EDGE_CURVE ( 'NONE', #89295, #70165, #19668, .T. ) ;
#71002 = CARTESIAN_POINT ( 'NONE',  ( 96.65525155030036331, -37.83077348759547220, 126.4099109901969626 ) ) ;
#71003 = CARTESIAN_POINT ( 'NONE',  ( 162.7131505118682639, -31.94127993907177299, 313.9678068554149490 ) ) ;
#71004 = ORIENTED_EDGE ( 'NONE', *, *, #18951, .F. ) ;
#71005 = CARTESIAN_POINT ( 'NONE',  ( 116.5366478410923463, -42.42989196264584706, 278.3832443235298797 ) ) ;
#71006 = DIRECTION ( 'NONE',  ( -0.000000000000000000, -0.000000000000000000, 1.000000000000000000 ) ) ;
#71007 =( NAMED_UNIT ( * ) SI_UNIT ( $, .STERADIAN. ) SOLID_ANGLE_UNIT ( ) );
#71008 = LINE ( 'NONE', #62821, #82793 ) ;
#71009 = CARTESIAN_POINT ( 'NONE',  ( 80.06648329127399677, -8.729447159940999512, 7.443125275912000127 ) ) ;
#71011 = DIRECTION ( 'NONE',  ( 0.7071067811566161820, 0.7071067812164789634, 0.000000000000000000 ) ) ;
#71010 = FACE_OUTER_BOUND ( 'NONE', #80257, .T. ) ;
#71012 = CARTESIAN_POINT ( 'NONE',  ( -446.0240000000000009, 3.174999999999999822, 101.5999999999999943 ) ) ;
#71013 = CARTESIAN_POINT ( 'NONE',  ( 0.000000000000000000, 100.5999999999999659, 0.000000000000000000 ) ) ;
#71014 = DIRECTION ( 'NONE',  ( 0.5000000000000061062, 0.8660254037844351549, 0.000000000000000000 ) ) ;
#71015 = PLANE ( 'NONE',  #55863 ) ;
#71016 = FACE_OUTER_BOUND ( 'NONE', #5351, .T. ) ;
#71017 = CARTESIAN_POINT ( 'NONE',  ( 107.0664832912739257, -52.57944715994094764, 302.7856252759109452 ) ) ;
#71019 = VERTEX_POINT ( 'NONE', #53709 ) ;
#71018 = CARTESIAN_POINT ( 'NONE',  ( 53.06670390244699576, -67.87844715994100397, 180.4678068554179902 ) ) ;
#71020 = CIRCLE ( 'NONE', #84056, 24.63800000000000168 ) ;
#71021 = LINE ( 'NONE', #14258, #8968 ) ;
#71022 = CARTESIAN_POINT ( 'NONE',  ( 117.3567523603254159, -34.92480690411444044, 243.9641967044819637 ) ) ;
#71023 = CARTESIAN_POINT ( 'NONE',  ( 116.8065287754011337, -43.47971597432173496, 159.3441967044829539 ) ) ;
#71024 = CARTESIAN_POINT ( 'NONE',  ( 113.7840377202001036, -29.05235663984046823, 285.5032443235299979 ) ) ;
#71026 = CARTESIAN_POINT ( 'NONE',  ( 104.4081006642920215, -46.45808914093545638, 47.36479194283237604 ) ) ;
#71025 = CARTESIAN_POINT ( 'NONE',  ( 72.96458098368701428, 127.0000000000000000, -65.02708098368670164 ) ) ;
#71027 = CARTESIAN_POINT ( 'NONE',  ( 112.0658486739693274, -45.48843317147805720, 138.9897862770318113 ) ) ;
#71028 = CIRCLE ( 'NONE', #59385, 3.250000000000002665 ) ;
#71029 = AXIS2_PLACEMENT_3D ( 'NONE', #88287, #60087, #25586 ) ;
#71030 = VERTEX_POINT ( 'NONE', #33300 ) ;
#71031 = EDGE_CURVE ( 'NONE', #53045, #35189, #28886, .T. ) ;
#71032 = CARTESIAN_POINT ( 'NONE',  ( -72.96458098368600531, 117.4749999999999943, -72.96458098368781009 ) ) ;
#71033 = VERTEX_POINT ( 'NONE', #61435 ) ;
#71034 = EDGE_CURVE ( 'NONE', #48373, #84162, #60997, .T. ) ;
#71035 = CARTESIAN_POINT ( 'NONE',  ( 101.2834890806669677, -28.93024170975123255, 185.0067055423629938 ) ) ;
#71036 = VECTOR ( 'NONE', #45126, 1000.000000000000000 ) ;
#71038 = VERTEX_POINT ( 'NONE', #47352 ) ;
#71037 = DIRECTION ( 'NONE',  ( 0.000000000000000000, 0.000000000000000000, -1.000000000000000000 ) ) ;
#71039 = DIRECTION ( 'NONE',  ( 0.000000000000000000, 0.000000000000000000, -1.000000000000000000 ) ) ;
#71040 = ADVANCED_FACE ( 'NONE', ( #26933 ), #54601, .F. ) ;
#71041 = CARTESIAN_POINT ( 'NONE',  ( 113.7366723824214318, -44.71300795807891149, 189.1299109901969757 ) ) ;
#71042 = CARTESIAN_POINT ( 'NONE',  ( 98.06670390244705970, -124.7784471599409528, 55.21780685541800437 ) ) ;
#71043 = CARTESIAN_POINT ( 'NONE',  ( 274.0659999999999741, 40.03750000000000142, -58.73749999999999716 ) ) ;
#71044 = PRESENTATION_LAYER_ASSIGNMENT (  '', '', ( #11570 ) ) ;
#71045 = LINE ( 'NONE', #43300, #64602 ) ;
#71046 = CARTESIAN_POINT ( 'NONE',  ( 110.9271686604937202, -27.50474214131384443, 85.76118691643459613 ) ) ;
#71047 = CARTESIAN_POINT ( 'NONE',  ( 147.0990821866028568, -137.6460688757850050, 245.8354721159570033 ) ) ;
#71048 = EDGE_CURVE ( 'NONE', #42743, #10090, #56411, .T. ) ;
#71049 = DIRECTION ( 'NONE',  ( 0.000000000000000000, 0.000000000000000000, 1.000000000000000000 ) ) ;
#71050 = AXIS2_PLACEMENT_3D ( 'NONE', #38113, #2715, #30411 ) ;
#71051 = CARTESIAN_POINT ( 'NONE',  ( 112.7054497023526807, -28.73785826246136921, 129.5870538473399449 ) ) ;
#71052 = ORIENTED_EDGE ( 'NONE', *, *, #59088, .F. ) ;
#71053 = ORIENTED_EDGE ( 'NONE', *, *, #6920, .F. ) ;
#71054 = CARTESIAN_POINT ( 'NONE',  ( 113.9863769398668296, -43.08488557356476889, 74.65491663922996679 ) ) ;
#71056 = AXIS2_PLACEMENT_3D ( 'NONE', #61400, #75045, #73701 ) ;
#71055 = FACE_OUTER_BOUND ( 'NONE', #48398, .T. ) ;
#71058 = DIRECTION ( 'NONE',  ( -1.784063995862374817E-16, 0.000000000000000000, -1.000000000000000000 ) ) ;
#71057 = CARTESIAN_POINT ( 'NONE',  ( 103.7602102885707467, -27.48919103108776341, 186.3499109901959798 ) ) ;
#71059 = CARTESIAN_POINT ( 'NONE',  ( 100.9551113561145286, -28.70668612591127200, 55.59250746033355739 ) ) ;
#71060 = CARTESIAN_POINT ( 'NONE',  ( 104.4899445637129674, -26.97881004783198122, 111.2818017522332781 ) ) ;
#71061 = EDGE_CURVE ( 'NONE', #62271, #77006, #21469, .T. ) ;
#71062 = VECTOR ( 'NONE', #54857, 1000.000000000000000 ) ;
#71063 = DIRECTION ( 'NONE',  ( -1.000000000000000078E-15, 1.000000000000000000, 0.000000000000000000 ) ) ;
#71064 = DIRECTION ( 'NONE',  ( 0.000000000000000000, 0.000000000000000000, -1.000000000000000000 ) ) ;
#71065 = CARTESIAN_POINT ( 'NONE',  ( 10.24823761126901722, 75.20812216786193005, 118.1124527501650618 ) ) ;
#71066 = CARTESIAN_POINT ( 'NONE',  ( 117.3423061886548879, -38.35306328171704848, 113.7013395616249767 ) ) ;
#71067 = ORIENTED_EDGE ( 'NONE', *, *, #43328, .T. ) ;
#71068 = EDGE_LOOP ( 'NONE', ( #19348, #38160, #33958, #75132 ) ) ;
#71069 = ORIENTED_EDGE ( 'NONE', *, *, #48300, .F. ) ;
#71070 = CARTESIAN_POINT ( 'NONE',  ( 4.100932966941606139, 70.52316614063619227, 130.4921811224707824 ) ) ;
#71071 = CARTESIAN_POINT ( 'NONE',  ( -100.5877680347020799, 85.83513192049078100, -83.22850972642753220 ) ) ;
#71072 = CARTESIAN_POINT ( 'NONE',  ( 97.53195389500311308, -39.74930131913054510, 131.5705599381032584 ) ) ;
#71073 = CARTESIAN_POINT ( 'NONE',  ( 112.0656190437874784, -45.48856781368362334, 103.9897653055920870 ) ) ;
#71074 = CARTESIAN_POINT ( 'NONE',  ( 113.9479352111735295, -42.95371825284467349, 231.0595189410199453 ) ) ;
#71075 = CIRCLE ( 'NONE', #34738, 2.517499999999998739 ) ;
#71076 = CARTESIAN_POINT ( 'NONE',  ( 223.2659999999999911, 52.73749999999999716, -44.45000000000000284 ) ) ;
#71077 = CARTESIAN_POINT ( 'NONE',  ( 95.31140346374353101, -38.27925045402978554, 151.4299109901969871 ) ) ;
#71078 = CARTESIAN_POINT ( 'NONE',  ( 62.03715912545828814, -47.82818131006021645, 249.9678068554150343 ) ) ;
#71079 = ORIENTED_EDGE ( 'NONE', *, *, #16201, .F. ) ;
#71081 = EDGE_LOOP ( 'NONE', ( #59873, #83031, #27846, #63919 ) ) ;
#71080 = ORIENTED_EDGE ( 'NONE', *, *, #49594, .F. ) ;
#71082 = VECTOR ( 'NONE', #58296, 1000.000000000000000 ) ;
#71083 = DIRECTION ( 'NONE',  ( -1.000000000000000078E-15, 0.000000000000000000, 1.000000000000000000 ) ) ;
#71084 = ORIENTED_EDGE ( 'NONE', *, *, #13395, .F. ) ;
#71085 = EDGE_LOOP ( 'NONE', ( #78171, #77652, #6310, #4400, #77311, #45378, #81686, #66574, #63520, #8507, #46865, #27729 ) ) ;
#71086 = CARTESIAN_POINT ( 'NONE',  ( 78.16547420788155875, -20.71744337671388436, 7.623533105446029801 ) ) ;
#71087 = DIRECTION ( 'NONE',  ( 8.755702086949183871E-16, 1.000000000000000000, 0.000000000000000000 ) ) ;
#71088 = CARTESIAN_POINT ( 'NONE',  ( 111.5476492967639359, -29.48535330821865941, 286.0672975916113501 ) ) ;
#71089 = AXIS2_PLACEMENT_3D ( 'NONE', #39708, #68778, #82871 ) ;
#71090 = PLANE ( 'NONE',  #59394 ) ;
#71091 = ORIENTED_EDGE ( 'NONE', *, *, #5397, .F. ) ;
#71092 = EDGE_CURVE ( 'NONE', #37008, #80917, #15557, .T. ) ;
#71093 = CARTESIAN_POINT ( 'NONE',  ( 116.4917448565859104, -39.22821409912334190, 9.635625275910937759 ) ) ;
#71094 = CARTESIAN_POINT ( 'NONE',  ( 165.9667039024459996, -26.71338133339301635, 117.4678068554150485 ) ) ;
#71095 = ORIENTED_EDGE ( 'NONE', *, *, #57983, .T. ) ;
#71097 = ORIENTED_EDGE ( 'NONE', *, *, #67191, .T. ) ;
#71096 = CIRCLE ( 'NONE', #59445, 50.79999999999999716 ) ;
#71098 = CARTESIAN_POINT ( 'NONE',  ( 117.0877018078255389, -37.67114210324087509, 113.7515134788750970 ) ) ;
#71099 = ORIENTED_EDGE ( 'NONE', *, *, #17540, .T. ) ;
#71100 = VERTEX_POINT ( 'NONE', #49595 ) ;
#71101 = EDGE_CURVE ( 'NONE', #26573, #81352, #57919, .T. ) ;
#71102 = CARTESIAN_POINT ( 'NONE',  ( 114.2324904129858112, -40.69568343359240714, 261.2423760838772182 ) ) ;
#71103 = VECTOR ( 'NONE', #83703, 1000.000000000000000 ) ;
#71104 = CARTESIAN_POINT ( 'NONE',  ( 109.4503794976336764, -25.91221646008812840, 179.8918157521019339 ) ) ;
#71105 = CARTESIAN_POINT ( 'NONE',  ( 96.03721982003239077, -36.58408020053186505, 156.3280062282919687 ) ) ;
#71106 = CARTESIAN_POINT ( 'NONE',  ( 103.8197751496740011, -48.12653019911325458, 213.3556252759109668 ) ) ;
#71107 = CARTESIAN_POINT ( 'NONE',  ( -240.5296158183964792, 93.66249999999999432, 11.11250000000040217 ) ) ;
#71108 = CARTESIAN_POINT ( 'NONE',  ( 75.31670390244798341, -67.87844715994100397, 58.80080685541479824 ) ) ;
#71109 = ORIENTED_EDGE ( 'NONE', *, *, #63218, .F. ) ;
#71110 = CARTESIAN_POINT ( 'NONE',  ( -130.4924667154230633, 70.52006616879378953, -4.092011266637315181 ) ) ;
#71111 = VERTEX_POINT ( 'NONE', #21014 ) ;
#71112 = ORIENTED_EDGE ( 'NONE', *, *, #60431, .T. ) ;
#71113 = CIRCLE ( 'NONE', #45003, 0.2999999999999943823 ) ;
#71114 = EDGE_CURVE ( 'NONE', #1202, #48691, #85055, .T. ) ;
#71115 = CARTESIAN_POINT ( 'NONE',  ( 110.5134301196510620, -26.84384026877932072, 209.8099109901969541 ) ) ;
#71116 = ORIENTED_EDGE ( 'NONE', *, *, #70299, .T. ) ;
#71117 = CARTESIAN_POINT ( 'NONE',  ( 99.42196222650996162, -27.67359991961172128, 150.6356252759109680 ) ) ;
#71118 = LINE ( 'NONE', #2516, #55774 ) ;
#71119 = CARTESIAN_POINT ( 'NONE',  ( 29.56648329127400388, 15.62155284005900491, 323.8756252759109202 ) ) ;
#71120 = CARTESIAN_POINT ( 'NONE',  ( 127.4058501689331280, -85.76982405743856930, 250.2178068554179902 ) ) ;
#71123 = CARTESIAN_POINT ( 'NONE',  ( 99.41296134609930846, -28.78668791560525975, 261.6746728949588032 ) ) ;
#71122 = CARTESIAN_POINT ( 'NONE',  ( 116.3173461584868278, -32.93718857426866720, 59.13562527591098217 ) ) ;
#71121 = CARTESIAN_POINT ( 'NONE',  ( 165.6738106836211557, -26.00627455218794637, 237.4678068554150059 ) ) ;
#71124 = DIRECTION ( 'NONE',  ( 0.7071067811865165975, 0.7071067811865784369, 7.071067811865470403E-16 ) ) ;
#71125 = DIRECTION ( 'NONE',  ( 1.000000000000000000, 0.000000000000000000, 2.108231265501709878E-16 ) ) ;
#71126 = VECTOR ( 'NONE', #74231, 1000.000000000000114 ) ;
#71127 = DIRECTION ( 'NONE',  ( 1.000000000000000000, 0.000000000000000000, 0.000000000000000000 ) ) ;
#71128 = DIRECTION ( 'NONE',  ( 5.512527431108029424E-15, -1.000000000000000000, 0.000000000000000000 ) ) ;
#71129 = CARTESIAN_POINT ( 'NONE',  ( 116.3136297247243078, -32.94478793390952376, 255.1356252759109395 ) ) ;
#71130 = FACE_OUTER_BOUND ( 'NONE', #13977, .T. ) ;
#71132 = VERTEX_POINT ( 'NONE', #22822 ) ;
#71131 = CARTESIAN_POINT ( 'NONE',  ( 115.4962543148458423, -35.12635383809098499, 195.5838068554167535 ) ) ;
#71133 = DIRECTION ( 'NONE',  ( 0.000000000000000000, -1.000000000000000000, 0.000000000000000000 ) ) ;
#71134 = CARTESIAN_POINT ( 'NONE',  ( 117.4794452684060104, -40.50643855513092007, 173.5375300378159693 ) ) ;
#71135 = CARTESIAN_POINT ( 'NONE',  ( 114.3531094850664260, -44.18515411228707279, 69.19276813305397411 ) ) ;
#71136 = CARTESIAN_POINT ( 'NONE',  ( 103.7092163704185026, -26.14992651007402813, 201.3089586092439731 ) ) ;
#71137 = CARTESIAN_POINT ( 'NONE',  ( 183.5150000000000148, 14.63749999999999929, -57.14999999999999858 ) ) ;
#71138 = CYLINDRICAL_SURFACE ( 'NONE', #56179, 1.000000000000000888 ) ;
#71139 = CIRCLE ( 'NONE', #44970, 0.5000000000000004441 ) ;
#71141 = LINE ( 'NONE', #28904, #66083 ) ;
#71140 = FACE_OUTER_BOUND ( 'NONE', #62532, .T. ) ;
#71142 = LINE ( 'NONE', #63412, #82918 ) ;
#71143 = CARTESIAN_POINT ( 'NONE',  ( 69.68306499799194853, -72.55732494037970071, 540.9756252759101471 ) ) ;
#71144 = EDGE_LOOP ( 'NONE', ( #83353, #84427, #12630, #49726 ) ) ;
#71145 = LINE ( 'NONE', #27995, #48458 ) ;
#71146 = ORIENTED_EDGE ( 'NONE', *, *, #65095, .F. ) ;
#71147 = VERTEX_POINT ( 'NONE', #42774 ) ;
#71148 = EDGE_CURVE ( 'NONE', #84501, #67129, #8288, .T. ) ;
#71149 = VECTOR ( 'NONE', #41300, 1000.000000000000114 ) ;
#71151 = EDGE_LOOP ( 'NONE', ( #52375, #80650, #80243, #40338 ) ) ;
#71150 = LINE ( 'NONE', #19962, #13981 ) ;
#71152 = ADVANCED_FACE ( 'NONE', ( #1923 ), #70516, .F. ) ;
#71153 = CARTESIAN_POINT ( 'NONE',  ( 96.66376384204026806, -36.61947630124858932, 107.3184824187679567 ) ) ;
#71154 = CYLINDRICAL_SURFACE ( 'NONE', #81683, 2.517500000000005844 ) ;
#71155 = ADVANCED_FACE ( 'NONE', ( #35984 ), #14658, .T. ) ;
#71157 = DIRECTION ( 'NONE',  ( 0.4214249218767882055, 0.9068632946707806397, 4.214249218767890910E-16 ) ) ;
#71156 = AXIS2_PLACEMENT_3D ( 'NONE', #79185, #37834, #38265 ) ;
#71158 = CARTESIAN_POINT ( 'NONE',  ( 154.5667039024470171, -79.67844715994088745, 190.2178068554179902 ) ) ;
#71159 = EDGE_CURVE ( 'NONE', #20491, #31568, #75300, .T. ) ;
#71160 = CARTESIAN_POINT ( 'NONE',  ( 102.1671273105904447, -43.72604531649727733, 281.5124198280768155 ) ) ;
#71161 = VERTEX_POINT ( 'NONE', #78245 ) ;
#71162 = ORIENTED_EDGE ( 'NONE', *, *, #74070, .F. ) ;
#71164 = ORIENTED_EDGE ( 'NONE', *, *, #86587, .T. ) ;
#71163 = CIRCLE ( 'NONE', #10257, 10.00000000000002665 ) ;
#71165 = CARTESIAN_POINT ( 'NONE',  ( 105.7154773345749135, -46.72385839275415265, 107.4689586095794738 ) ) ;
#71166 = FACE_OUTER_BOUND ( 'NONE', #44088, .T. ) ;
#71167 = CYLINDRICAL_SURFACE ( 'NONE', #5667, 2.500000000000002220 ) ;
#71168 = DIRECTION ( 'NONE',  ( 1.000000000000000078E-15, -1.000000000000000083E-30, -1.000000000000000000 ) ) ;
#71169 = LINE ( 'NONE', #28929, #30192 ) ;
#71170 = CARTESIAN_POINT ( 'NONE',  ( 97.39127856926108961, -39.27846915049015308, 52.53132659260805326 ) ) ;
#71171 = EDGE_CURVE ( 'NONE', #47557, #42953, #29178, .T. ) ;
#71172 = AXIS2_PLACEMENT_3D ( 'NONE', #44472, #37683, #65383 ) ;
#71173 = CARTESIAN_POINT ( 'NONE',  ( 115.0439452383991892, -99.09543445804983719, -19.78219314458218392 ) ) ;
#71174 = CARTESIAN_POINT ( 'NONE',  ( -12.29034155828684405, 85.77798403344019107, 129.9765768215993091 ) ) ;
#71175 = EDGE_CURVE ( 'NONE', #37060, #72283, #84344, .T. ) ;
#71176 = CARTESIAN_POINT ( 'NONE',  ( 97.82554479137630210, -33.52525840161893456, 286.0613395616258572 ) ) ;
#71177 = EDGE_LOOP ( 'NONE', ( #57542, #4630, #68397, #50892, #62730, #62891, #51266, #50728, #86544 ) ) ;
#71178 = CARTESIAN_POINT ( 'NONE',  ( 126.4970673974017643, 44.81588728400144106, 32.30169817395221088 ) ) ;
#71179 = CARTESIAN_POINT ( 'NONE',  ( -55.41748140693382396, 54.70421759738486855, 70.78752196261643803 ) ) ;
#71180 = CARTESIAN_POINT ( 'NONE',  ( 103.5819438468105744, -44.65149928713079674, 130.0528522743539668 ) ) ;
#71181 = DIRECTION ( 'NONE',  ( 1.000000000000000000, 0.000000000000000000, -6.982966722218760189E-15 ) ) ;
#71182 = VECTOR ( 'NONE', #43563, 1000.000000000000000 ) ;
#71183 = CYLINDRICAL_SURFACE ( 'NONE', #3906, 0.5000000000000197620 ) ;
#71184 = ORIENTED_EDGE ( 'NONE', *, *, #79800, .T. ) ;
#71185 = ORIENTED_EDGE ( 'NONE', *, *, #72502, .F. ) ;
#71186 = CARTESIAN_POINT ( 'NONE',  ( 105.7156386614864658, -46.72388412106460720, 137.4669372650166679 ) ) ;
#71187 = VECTOR ( 'NONE', #12472, 1000.000000000000000 ) ;
#71188 = ORIENTED_EDGE ( 'NONE', *, *, #46078, .T. ) ;
#71189 = ORIENTED_EDGE ( 'NONE', *, *, #54497, .T. ) ;
#71190 = CARTESIAN_POINT ( 'NONE',  ( 117.1402439185659006, -36.89830975172036887, 150.2444404487539487 ) ) ;
#71191 = DIRECTION ( 'NONE',  ( -0.7071067811734105257, 0.7071067811996846197, 0.000000000000000000 ) ) ;
#71193 = ADVANCED_FACE ( 'NONE', ( #73630 ), #86379, .T. ) ;
#71192 = CARTESIAN_POINT ( 'NONE',  ( 114.5831001172654595, -44.03558617456690172, 94.21276813305395592 ) ) ;
#71194 = CARTESIAN_POINT ( 'NONE',  ( 110.8549378340421470, -45.98404676291230686, 17.88566530162140467 ) ) ;
#71195 = ORIENTED_EDGE ( 'NONE', *, *, #19973, .F. ) ;
#71196 = ORIENTED_EDGE ( 'NONE', *, *, #54480, .F. ) ;
#71197 = EDGE_LOOP ( 'NONE', ( #8598, #72487, #74042, #85499 ) ) ;
#71198 = EDGE_CURVE ( 'NONE', #4290, #5461, #44570, .T. ) ;
#71199 = CARTESIAN_POINT ( 'NONE',  ( 108.4620505914581798, -44.77196653648033475, 165.5309475124489609 ) ) ;
#71200 = CARTESIAN_POINT ( 'NONE',  ( 107.8700610081582738, -26.31308374369285730, 70.01562527591099183 ) ) ;
#71201 = ORIENTED_EDGE ( 'NONE', *, *, #45461, .T. ) ;
#71202 = CARTESIAN_POINT ( 'NONE',  ( 115.4270991047691410, -42.97960947038953350, 28.31562527591097123 ) ) ;
#71203 = CARTESIAN_POINT ( 'NONE',  ( 114.1394676070193839, -29.04113448922185370, 195.4841967044819739 ) ) ;
#71204 = DIRECTION ( 'NONE',  ( 1.000000000000000078E-15, -1.000000000000000083E-30, -1.000000000000000000 ) ) ;
#71205 = FACE_OUTER_BOUND ( 'NONE', #39815, .T. ) ;
#71206 = CARTESIAN_POINT ( 'NONE',  ( 98.45631125714150755, -42.66967193002393088, 122.8070538473389490 ) ) ;
#71207 = AXIS2_PLACEMENT_3D ( 'NONE', #3448, #31584, #86575 ) ;
#71208 = DIRECTION ( 'NONE',  ( 0.000000000000000000, 1.000000000000000000, 0.000000000000000000 ) ) ;
#71209 = VERTEX_POINT ( 'NONE', #24155 ) ;
#71210 = DIRECTION ( 'NONE',  ( -1.907762142705490052E-15, -7.167082501179359715E-16, 1.000000000000000000 ) ) ;
#71211 = CIRCLE ( 'NONE', #87149, 1.000000000000000888 ) ;
#71212 = CIRCLE ( 'NONE', #82820, 0.5000000000000004441 ) ;
#71213 = ORIENTED_EDGE ( 'NONE', *, *, #20765, .F. ) ;
#71214 = CARTESIAN_POINT ( 'NONE',  ( 97.81930656603341845, -40.53598742125645060, 132.6376059489711849 ) ) ;
#71215 = ORIENTED_EDGE ( 'NONE', *, *, #58701, .T. ) ;
#71216 = ORIENTED_EDGE ( 'NONE', *, *, #69265, .F. ) ;
#71217 = AXIS2_PLACEMENT_3D ( 'NONE', #52191, #4526, #79954 ) ;
#71218 = DIRECTION ( 'NONE',  ( -1.000000000000000000, -1.734723475976808672E-15, 0.000000000000000000 ) ) ;
#71219 = EDGE_CURVE ( 'NONE', #39785, #32919, #53867, .T. ) ;
#71220 = CARTESIAN_POINT ( 'NONE',  ( 116.3212776292296127, -32.94146857471318413, 287.6356252759109680 ) ) ;
#71221 = CARTESIAN_POINT ( 'NONE',  ( 118.0757533234433083, -37.71689883586016379, 33.74324432352998571 ) ) ;
#71222 = DIRECTION ( 'NONE',  ( 0.000000000000000000, -1.000000000000000000, 0.000000000000000000 ) ) ;
#71223 = CARTESIAN_POINT ( 'NONE',  ( 97.81170986510684884, -40.51745644794008427, 172.6354259520616097 ) ) ;
#71224 = DIRECTION ( 'NONE',  ( 1.000000000000000000, 1.199348956600846523E-15, 0.000000000000000000 ) ) ;
#71225 = CARTESIAN_POINT ( 'NONE',  ( 115.0831197249980420, -29.02584261466826021, 39.43562527591099354 ) ) ;
#71227 = CARTESIAN_POINT ( 'NONE',  ( 116.7861719071672155, -43.46560779248400763, 159.3441967044829539 ) ) ;
#71226 = CARTESIAN_POINT ( 'NONE',  ( 97.81002727075654946, -40.51336424107649492, 111.6352756744173007 ) ) ;
#71228 = DIRECTION ( 'NONE',  ( -1.000000000000000000, -4.299999999999999979E-14, -1.000000000000000078E-15 ) ) ;
#71229 = LINE ( 'NONE', #23090, #82965 ) ;
#71230 = ORIENTED_EDGE ( 'NONE', *, *, #57696, .T. ) ;
#71231 = B_SPLINE_CURVE_WITH_KNOTS ( 'NONE', 3,
 ( #70628, #36102, #43796, #7947, #9297, #51493, #1138, #17003, #22940, #77894, #36999, #86054, #2928, #16119, #64264, #56982, #42894, #2485 ),
 .UNSPECIFIED., .F., .F.,
 ( 4, 2, 2, 2, 2, 2, 2, 2, 4 ),
 ( 0.4999999768783345844, 0.5624999797685428238, 0.6249999826587508966, 0.6874999855489591916, 0.7499999884391672644, 0.8124999913293755593, 0.8749999942195836322, 0.9374999971097919271, 1.000000000000000000 ),
 .UNSPECIFIED. ) ;
#71232 = AXIS2_PLACEMENT_3D ( 'NONE', #11187, #44813, #4390 ) ;
#71233 = CARTESIAN_POINT ( 'NONE',  ( 33.92127028473603900, -29.73316016639542170, 342.9256252759109884 ) ) ;
#71234 = CARTESIAN_POINT ( 'NONE',  ( 34.92499999999999716, 77.96728223830740490, 310.8325000000000387 ) ) ;
#71235 = CARTESIAN_POINT ( 'NONE',  ( 100.1253875378072848, -39.57043109886186727, 0.4256252759109631079 ) ) ;
#71236 = ORIENTED_EDGE ( 'NONE', *, *, #2732, .F. ) ;
#71237 = VECTOR ( 'NONE', #34441, 1000.000000000000000 ) ;
#71238 = EDGE_CURVE ( 'NONE', #25358, #83795, #23286, .T. ) ;
#71239 = CARTESIAN_POINT ( 'NONE',  ( 77.31648329127399677, -18.72944715994106346, 6.749768910606400496 ) ) ;
#71241 = ORIENTED_EDGE ( 'NONE', *, *, #51808, .F. ) ;
#71240 = CARTESIAN_POINT ( 'NONE',  ( 117.4576385420935338, -35.45251388149282690, 193.9241967044829664 ) ) ;
#71242 = DIRECTION ( 'NONE',  ( 0.000000000000000000, 0.000000000000000000, 1.000000000000000000 ) ) ;
#71243 = CARTESIAN_POINT ( 'NONE',  ( 118.0636334930051987, -35.40736804548507877, 234.9337205140059552 ) ) ;
#71244 = CARTESIAN_POINT ( 'NONE',  ( 108.9932425643425802, -47.01927604342903777, 78.72419670448194040 ) ) ;
#71245 = CARTESIAN_POINT ( 'NONE',  ( 84.36969927706093131, 75.84295037288958952, 99.63271100832298544 ) ) ;
#71246 = CARTESIAN_POINT ( 'NONE',  ( 97.31590013278544404, -39.30611206075547415, 192.5313402528328481 ) ) ;
#71247 = DIRECTION ( 'NONE',  ( 0.000000000000000000, 1.000000000000000000, -0.000000000000000000 ) ) ;
#71248 = VERTEX_POINT ( 'NONE', #16443 ) ;
#71249 = ADVANCED_FACE ( 'NONE', ( #10076 ), #44120, .F. ) ;
#71250 = ORIENTED_EDGE ( 'NONE', *, *, #32250, .F. ) ;
#71252 = ORIENTED_EDGE ( 'NONE', *, *, #22738, .F. ) ;
#71251 = AXIS2_PLACEMENT_3D ( 'NONE', #6944, #49153, #27830 ) ;
#71253 = VECTOR ( 'NONE', #20962, 1000.000000000000000 ) ;
#71254 = ORIENTED_EDGE ( 'NONE', *, *, #55961, .T. ) ;
#71255 = CARTESIAN_POINT ( 'NONE',  ( 130.3998166246070127, 12.92155284005802685, 336.5756252759110225 ) ) ;
#71256 = CARTESIAN_POINT ( 'NONE',  ( 96.77275252345162926, -34.86922145964237529, 237.1841967044819626 ) ) ;
#71257 = CARTESIAN_POINT ( 'NONE',  ( 44.45000000000000284, 69.84999999999999432, 257.1750000000000114 ) ) ;
#71258 = CARTESIAN_POINT ( 'NONE',  ( 131.8592257737628586, -35.08568546291017043, 2.471387922376259816 ) ) ;
#71259 = EDGE_CURVE ( 'NONE', #80300, #62557, #1324, .T. ) ;
#71261 = CARTESIAN_POINT ( 'NONE',  ( 74.70281015415382342, 79.25941250729455589, 92.05992619857379111 ) ) ;
#71260 = CARTESIAN_POINT ( 'NONE',  ( 179.1667039024460166, -28.27351298637280408, -5.074374724088000832 ) ) ;
#71262 = LINE ( 'NONE', #77458, #35625 ) ;
#71263 = AXIS2_PLACEMENT_3D ( 'NONE', #58673, #3732, #32314 ) ;
#71264 = CARTESIAN_POINT ( 'NONE',  ( 116.7906267970580103, -31.42506456344890964, 24.21181575210196257 ) ) ;
#71265 = ORIENTED_EDGE ( 'NONE', *, *, #38112, .T. ) ;
#71266 = ORIENTED_EDGE ( 'NONE', *, *, #83356, .T. ) ;
#71267 = ORIENTED_EDGE ( 'NONE', *, *, #45425, .F. ) ;
#71268 = VECTOR ( 'NONE', #3268, 1000.000000000000000 ) ;
#71269 = CARTESIAN_POINT ( 'NONE',  ( 105.0982380168385930, -104.8375911996990766, -19.78219314458198852 ) ) ;
#71270 = DIRECTION ( 'NONE',  ( 0.000000000000000000, 0.000000000000000000, -1.000000000000000000 ) ) ;
#71271 = CARTESIAN_POINT ( 'NONE',  ( 99.85651329999866732, -30.12038005271842422, 271.7356252759109907 ) ) ;
#71272 = LINE ( 'NONE', #1322, #55962 ) ;
#71273 = EDGE_CURVE ( 'NONE', #18666, #51113, #74079, .T. ) ;
#71274 = CARTESIAN_POINT ( 'NONE',  ( 107.9743429475490615, -26.39917242597376301, 105.9946728949579864 ) ) ;
#71275 = EDGE_CURVE ( 'NONE', #21656, #43367, #34070, .T. ) ;
#71276 = CARTESIAN_POINT ( 'NONE',  ( 104.4076007111484614, -46.45794255853319754, 27.36475074168719601 ) ) ;
#71278 = ORIENTED_EDGE ( 'NONE', *, *, #59034, .T. ) ;
#71277 = CIRCLE ( 'NONE', #29184, 9.525000000000000355 ) ;
#71279 = DIRECTION ( 'NONE',  ( 0.000000000000000000, 0.000000000000000000, -1.000000000000000000 ) ) ;
#71280 = DIRECTION ( 'NONE',  ( -1.000000000000000000, -8.163404592832032979E-16, 0.000000000000000000 ) ) ;
#71281 = ORIENTED_EDGE ( 'NONE', *, *, #71275, .T. ) ;
#71282 = CARTESIAN_POINT ( 'NONE',  ( -89.55214429302371570, 92.12496802699141085, 77.69357874334745873 ) ) ;
#71283 = CARTESIAN_POINT ( 'NONE',  ( 107.1674220045319288, -28.56736792770730560, 32.88523322673398042 ) ) ;
#71284 = VECTOR ( 'NONE', #89222, 1000.000000000000000 ) ;
#71285 = DIRECTION ( 'NONE',  ( 1.639958061481212836E-42, -4.100000000000000342E-29, -1.000000000000000000 ) ) ;
#71286 = LINE ( 'NONE', #23584, #83892 ) ;
#71287 = VECTOR ( 'NONE', #38574, 1000.000000000000000 ) ;
#71288 = CARTESIAN_POINT ( 'NONE',  ( 51.06648329127400388, -8.350947159940998787, 333.4006252759120343 ) ) ;
#71289 = ORIENTED_EDGE ( 'NONE', *, *, #23151, .T. ) ;
#71290 = CARTESIAN_POINT ( 'NONE',  ( 141.8164832912739826, -9.833000550534297446, 14.92562527591100618 ) ) ;
#71291 = DIRECTION ( 'NONE',  ( 1.000000000000000000, 0.000000000000000000, 1.047444401652940007E-14 ) ) ;
#71292 = VERTEX_POINT ( 'NONE', #81371 ) ;
#71293 = CARTESIAN_POINT ( 'NONE',  ( 117.1066318038510303, -39.53701698219273908, 98.60991099019594230 ) ) ;
#71294 = ORIENTED_EDGE ( 'NONE', *, *, #10203, .T. ) ;
#71296 = AXIS2_PLACEMENT_3D ( 'NONE', #69319, #35683, #49750 ) ;
#71295 = CARTESIAN_POINT ( 'NONE',  ( 115.2801527212906336, -32.91522314707135166, 58.58289601855292972 ) ) ;
#71297 = DIRECTION ( 'NONE',  ( -1.000000000000000000, 0.000000000000000000, 0.000000000000000000 ) ) ;
#71298 = CARTESIAN_POINT ( 'NONE',  ( 96.72778144249456034, -35.92320320382069099, 191.2765776568639922 ) ) ;
#71299 = CARTESIAN_POINT ( 'NONE',  ( 142.8698897858160706, -0.9167816978817300289, 542.9756252759101471 ) ) ;
#71300 = DIRECTION ( 'NONE',  ( -1.000000000000000000, -3.999999999999999995E-14, 4.193851878741028267E-47 ) ) ;
#71301 = CARTESIAN_POINT ( 'NONE',  ( -492.0614999999999668, 93.66249999999999432, 90.48749999999999716 ) ) ;
#71302 = CARTESIAN_POINT ( 'NONE',  ( 151.0371591254582597, -46.82818131005593187, 300.4678068554149490 ) ) ;
#71303 = CARTESIAN_POINT ( 'NONE',  ( 110.2908372810403819, -46.66631795110420455, 8.827053847339950465 ) ) ;
#71304 = ORIENTED_EDGE ( 'NONE', *, *, #26906, .T. ) ;
#71305 = CARTESIAN_POINT ( 'NONE',  ( 71.06670390244705970, -118.2784471599409812, 230.7030882296565721 ) ) ;
#71306 = ORIENTED_EDGE ( 'NONE', *, *, #68276, .T. ) ;
#71307 = CARTESIAN_POINT ( 'NONE',  ( 117.7479605218750862, -39.74664297364158472, 139.6194347997199827 ) ) ;
#71308 = DIRECTION ( 'NONE',  ( 0.000000000000000000, 0.000000000000000000, -1.000000000000000000 ) ) ;
#71309 = VERTEX_POINT ( 'NONE', #4597 ) ;
#71310 = ORIENTED_EDGE ( 'NONE', *, *, #64656, .F. ) ;
#71311 = EDGE_CURVE ( 'NONE', #84869, #33481, #5500, .T. ) ;
#71312 = VERTEX_POINT ( 'NONE', #66812 ) ;
#71313 = CIRCLE ( 'NONE', #16203, 3.299999999999999822 ) ;
#71314 = CARTESIAN_POINT ( 'NONE',  ( 107.0667039024467329, -53.45944715994091467, 195.5838068554169524 ) ) ;
#71315 = DIRECTION ( 'NONE',  ( -2.900000000000000265E-14, 2.000000000000000155E-15, -1.000000000000000000 ) ) ;
#71316 = DIRECTION ( 'NONE',  ( 0.000000000000000000, 0.000000000000000000, 1.000000000000000000 ) ) ;
#71317 = DIRECTION ( 'NONE',  ( 1.907762142705490052E-15, 7.167082501179359715E-16, -1.000000000000000000 ) ) ;
#71318 = FACE_OUTER_BOUND ( 'NONE', #79253, .T. ) ;
#71319 = CARTESIAN_POINT ( 'NONE',  ( 104.2409529242390391, -46.76432966167102023, 18.35848241876792031 ) ) ;
#71320 = FACE_OUTER_BOUND ( 'NONE', #70689, .T. ) ;
#71321 = ORIENTED_EDGE ( 'NONE', *, *, #87449, .T. ) ;
#71322 = DIRECTION ( 'NONE',  ( 0.000000000000000000, 0.000000000000000000, -1.000000000000000000 ) ) ;
#71323 = DIRECTION ( 'NONE',  ( 9.351236661543306751E-17, -3.725950533538267725E-29, -1.000000000000000000 ) ) ;
#71324 = VERTEX_POINT ( 'NONE', #54050 ) ;
#71325 = ORIENTED_EDGE ( 'NONE', *, *, #72591, .T. ) ;
#71326 = DIRECTION ( 'NONE',  ( 1.000000000000000000, 0.000000000000000000, 0.000000000000000000 ) ) ;
#71327 = ADVANCED_FACE ( 'NONE', ( #26377, #40450 ), #47696, .T. ) ;
#71328 = DIRECTION ( 'NONE',  ( -1.000000000000000000, 0.000000000000000000, -3.576143065239989638E-15 ) ) ;
#71329 = CARTESIAN_POINT ( 'NONE',  ( -3.175000000000109956, 8.255000000000000782, -31.75000000000000000 ) ) ;
#71330 = EDGE_CURVE ( 'NONE', #5931, #83484, #49140, .T. ) ;
#71331 = CARTESIAN_POINT ( 'NONE',  ( 3.175000000000355094, 8.255000000000000782, 33.98325472291460159 ) ) ;
#71332 = CARTESIAN_POINT ( 'NONE',  ( 263.3306968374159851, 52.73749999999999716, -2.032000000000000028 ) ) ;
#71333 = CARTESIAN_POINT ( 'NONE',  ( 99.66831329903114067, -43.01734891331329891, 226.3095626852189639 ) ) ;
#71335 = CARTESIAN_POINT ( 'NONE',  ( 100.4250012405661607, -28.72198927997979823, 36.62705384733894221 ) ) ;
#71334 = FACE_OUTER_BOUND ( 'NONE', #60522, .T. ) ;
#71336 = LINE ( 'NONE', #58134, #45124 ) ;
#71337 = CARTESIAN_POINT ( 'NONE',  ( 102.9537058647788967, -46.35710148923402585, 92.25562527591097250 ) ) ;
#71338 = ORIENTED_EDGE ( 'NONE', *, *, #17352, .T. ) ;
#71339 = CARTESIAN_POINT ( 'NONE',  ( 131.3333327974766576, -19.08363404519706208, 6.775960187534563417 ) ) ;
#71340 = ORIENTED_EDGE ( 'NONE', *, *, #39135, .T. ) ;
#71341 = EDGE_CURVE ( 'NONE', #21246, #75279, #12934, .T. ) ;
#71342 = CARTESIAN_POINT ( 'NONE',  ( 194.0667039024480118, -40.32844715993407902, 249.9678068554149775 ) ) ;
#71343 = CARTESIAN_POINT ( 'NONE',  ( 25.56670390244797275, -58.35344715994099829, 257.2178068554150059 ) ) ;
#71344 = VERTEX_POINT ( 'NONE', #25935 ) ;
#71345 = EDGE_CURVE ( 'NONE', #57944, #83877, #60893, .T. ) ;
#71346 = EDGE_CURVE ( 'NONE', #4781, #48555, #44806, .T. ) ;
#71347 = CARTESIAN_POINT ( 'NONE',  ( 32.06670390244579494, -32.29483332968550258, 117.4678068554150485 ) ) ;
#71348 = VERTEX_POINT ( 'NONE', #12306 ) ;
#71349 = CARTESIAN_POINT ( 'NONE',  ( 107.0664832912739683, -18.82844715994099971, 199.5838068554169809 ) ) ;
#71350 = DIRECTION ( 'NONE',  ( 1.000000000000000000, 4.299999999999999979E-14, 1.000000000000000078E-15 ) ) ;
#71351 = AXIS2_PLACEMENT_3D ( 'NONE', #44617, #39046, #25873 ) ;
#71352 = ADVANCED_FACE ( 'NONE', ( #13648 ), #32282, .F. ) ;
#71353 = FACE_OUTER_BOUND ( 'NONE', #48171, .T. ) ;
#71354 = EDGE_CURVE ( 'NONE', #54231, #38331, #53972, .T. ) ;
#71355 = ORIENTED_EDGE ( 'NONE', *, *, #20372, .T. ) ;
#71356 = CARTESIAN_POINT ( 'NONE',  ( 100.2843123851674960, -46.47809700006297362, 87.09276813305393716 ) ) ;
#71357 = DIRECTION ( 'NONE',  ( 1.000000000000000000, 0.000000000000000000, 0.000000000000000000 ) ) ;
#71358 = EDGE_CURVE ( 'NONE', #25435, #1233, #60435, .T. ) ;
#71359 = CARTESIAN_POINT ( 'NONE',  ( 141.8164832912740394, -45.62589376934770513, -5.074374724088994704 ) ) ;
#71360 = DIRECTION ( 'NONE',  ( 1.000000000000000078E-15, -1.000000000000000000, 0.000000000000000000 ) ) ;
#71361 = CARTESIAN_POINT ( 'NONE',  ( 61.67078992371376245, -0.9290567490904538817, 542.9756252759101471 ) ) ;
#71362 = EDGE_LOOP ( 'NONE', ( #84266, #7631 ) ) ;
#71363 = AXIS2_PLACEMENT_3D ( 'NONE', #39474, #73998, #11777 ) ;
#71364 = EDGE_CURVE ( 'NONE', #34865, #36283, #39553, .T. ) ;
#71365 = CARTESIAN_POINT ( 'NONE',  ( 12.70000000000000107, 82.54999999999999716, 129.9368274816650910 ) ) ;
#71366 = CARTESIAN_POINT ( 'NONE',  ( 80.06648281188262217, -21.47944715903999224, 8.225259175037979986 ) ) ;
#71367 = AXIS2_PLACEMENT_3D ( 'NONE', #40039, #87310, #13247 ) ;
#71368 = EDGE_CURVE ( 'NONE', #6360, #19900, #49492, .T. ) ;
#71369 = LINE ( 'NONE', #30903, #45789 ) ;
#71371 = DIRECTION ( 'NONE',  ( 0.000000000000000000, 0.000000000000000000, 1.000000000000000000 ) ) ;
#71370 = CARTESIAN_POINT ( 'NONE',  ( 181.8764988495240118, -33.54226604284930602, 342.9256252759119548 ) ) ;
#71372 = CARTESIAN_POINT ( 'NONE',  ( 41.56648329127399677, -18.82844715994099971, 318.9256252759120116 ) ) ;
#71373 = VERTEX_POINT ( 'NONE', #77227 ) ;
#71374 = DIRECTION ( 'NONE',  ( 0.000000000000000000, 0.000000000000000000, -1.000000000000000000 ) ) ;
#71375 = CARTESIAN_POINT ( 'NONE',  ( 106.9806506443342755, -46.50983917909364607, 183.5699109901959787 ) ) ;
#71377 = ORIENTED_EDGE ( 'NONE', *, *, #25991, .F. ) ;
#71376 = CARTESIAN_POINT ( 'NONE',  ( -77.39114642430010349, 127.0000000000000000, 71.77848634863050847 ) ) ;
#71378 = EDGE_CURVE ( 'NONE', #4111, #28081, #916, .T. ) ;
#71379 = CARTESIAN_POINT ( 'NONE',  ( 111.0600676159102278, -27.80113716328034457, 20.74133956162494030 ) ) ;
#71380 = DIRECTION ( 'NONE',  ( 0.9834602067019598826, 0.1811243270069988198, 0.000000000000000000 ) ) ;
#71382 = EDGE_CURVE ( 'NONE', #17509, #21135, #72391, .T. ) ;
#71381 = CARTESIAN_POINT ( 'NONE',  ( 45.66030316258350297, 82.54999999999999716, 346.9005000000000223 ) ) ;
#71383 = CARTESIAN_POINT ( 'NONE',  ( 108.3314583620718849, -46.73508509281070644, 12.67747797925112963 ) ) ;
#71384 = EDGE_CURVE ( 'NONE', #20155, #55721, #7731, .T. ) ;
#71385 = DIRECTION ( 'NONE',  ( 1.000000000000000078E-15, 0.000000000000000000, -1.000000000000000000 ) ) ;
#71386 = EDGE_CURVE ( 'NONE', #1463, #231, #1371, .T. ) ;
#71387 = CARTESIAN_POINT ( 'NONE',  ( 97.32398421004032230, -35.86507053846867166, 231.2556252759109725 ) ) ;
#71388 = ORIENTED_EDGE ( 'NONE', *, *, #13480, .T. ) ;
#71389 = CIRCLE ( 'NONE', #72795, 2.500000000000002220 ) ;
#71390 = VERTEX_POINT ( 'NONE', #69962 ) ;
#71391 = CARTESIAN_POINT ( 'NONE',  ( 99.72946911866242203, -30.86048229651775543, 192.2092023535159626 ) ) ;
#71392 = CIRCLE ( 'NONE', #3171, 32.50000000000000711 ) ;
#71393 = DIRECTION ( 'NONE',  ( 0.000000000000000000, 0.000000000000000000, 1.000000000000000000 ) ) ;
#71394 = CARTESIAN_POINT ( 'NONE',  ( 109.9481718979998277, -45.67217584368548700, 54.26824997256396443 ) ) ;
#71395 = CARTESIAN_POINT ( 'NONE',  ( 23.18025296944486868, 86.82834877582368449, 300.7800082948225509 ) ) ;
#71396 = DIRECTION ( 'NONE',  ( -1.000000000000000078E-15, 1.000000000000000083E-30, 1.000000000000000000 ) ) ;
#71397 = PLANE ( 'NONE',  #3842 ) ;
#71398 = EDGE_LOOP ( 'NONE', ( #86949, #89265 ) ) ;
#71399 = CARTESIAN_POINT ( 'NONE',  ( 12.60000000000000142, 82.54999999999999716, 92.46299999999996544 ) ) ;
#71400 = FACE_OUTER_BOUND ( 'NONE', #59309, .T. ) ;
#71401 = CARTESIAN_POINT ( 'NONE',  ( 112.4005920293390233, -46.38403708128156921, 252.9661014663871583 ) ) ;
#71402 = CYLINDRICAL_SURFACE ( 'NONE', #60510, 5.599999999999994316 ) ;
#71403 = ORIENTED_EDGE ( 'NONE', *, *, #6345, .F. ) ;
#71404 = ORIENTED_EDGE ( 'NONE', *, *, #65694, .T. ) ;
#71405 = VECTOR ( 'NONE', #15761, 1000.000000000000000 ) ;
#71406 = CARTESIAN_POINT ( 'NONE',  ( 115.7831076680295723, -41.80230951391620664, 83.40645860891918062 ) ) ;
#71407 = DIRECTION ( 'NONE',  ( 1.000000000000000000, 1.000000000000000078E-15, 0.000000000000000000 ) ) ;
#71408 = FACE_OUTER_BOUND ( 'NONE', #69857, .T. ) ;
#71409 = CARTESIAN_POINT ( 'NONE',  ( 0.000000000000000000, 124.5870000000000033, 0.000000000000000000 ) ) ;
#71410 = VECTOR ( 'NONE', #85782, 999.9999999999998863 ) ;
#71411 = CARTESIAN_POINT ( 'NONE',  ( 107.1874307469290244, -26.94942635195924652, 31.06705384733893283 ) ) ;
#71412 = DIRECTION ( 'NONE',  ( -2.127927463864879951E-15, 0.000000000000000000, -1.000000000000000000 ) ) ;
#71413 = EDGE_LOOP ( 'NONE', ( #44325, #73818, #16278, #62686 ) ) ;
#71414 = VECTOR ( 'NONE', #1719, 999.9999999999998863 ) ;
#71415 = CARTESIAN_POINT ( 'NONE',  ( 118.1215414109737196, -37.72100569522838498, 29.74324432352998215 ) ) ;
#71416 = CARTESIAN_POINT ( 'NONE',  ( 167.2371591254542693, -47.82818131005522844, 300.4678068554149490 ) ) ;
#71417 = CARTESIAN_POINT ( 'NONE',  ( 100.5838780899822922, -28.49162262467549667, 15.60705384733995871 ) ) ;
#71418 = ORIENTED_EDGE ( 'NONE', *, *, #59325, .T. ) ;
#71419 = CIRCLE ( 'NONE', #84528, 13.31747058675099993 ) ;
#71420 = DIRECTION ( 'NONE',  ( -0.000000000000000000, -0.000000000000000000, 1.000000000000000000 ) ) ;
#71421 = CARTESIAN_POINT ( 'NONE',  ( 142.8838050580813785, -82.11588141944044139, 394.9756252759102040 ) ) ;
#71422 = DIRECTION ( 'NONE',  ( 0.000000000000000000, 0.000000000000000000, 1.000000000000000000 ) ) ;
#71423 = CONICAL_SURFACE ( 'NONE', #27894, 81.91591158490091118, 0.7853981633974760346 ) ;
#71424 = CARTESIAN_POINT ( 'NONE',  ( 109.4870457054322941, -44.52499740455228761, 95.63380465530596553 ) ) ;
#71425 = CARTESIAN_POINT ( 'NONE',  ( 112.2157656529268763, -45.81911987206276393, 208.9870538473389558 ) ) ;
#71426 = DIRECTION ( 'NONE',  ( 0.000000000000000000, 0.000000000000000000, -1.000000000000000000 ) ) ;
#71427 = ORIENTED_EDGE ( 'NONE', *, *, #44664, .T. ) ;
#71428 = DIRECTION ( 'NONE',  ( 4.299999999999999979E-14, -1.000000000000000000, 4.400000000000000367E-29 ) ) ;
#71429 = ORIENTED_EDGE ( 'NONE', *, *, #58122, .T. ) ;
#71430 = ORIENTED_EDGE ( 'NONE', *, *, #81443, .T. ) ;
#71431 = B_SPLINE_CURVE_WITH_KNOTS ( 'NONE', 3,
 ( #50400, #15463, #43134, #69970, #84957, #64053, #7738, #56309, #1831, #48593, #473, #22723, #57213, #21371, #28168, #41338, #6837, #28624, #49046, #55855, #63146, #34540, #62243, #30, #84055 ),
 .UNSPECIFIED., .F., .F.,
 ( 4, 2, 2, 2, 2, 2, 2, 2, 2, 1, 2, 2, 4 ),
 ( 0.000000000000000000, 0.002483981393139995941, 0.003725972089710014295, 0.004967962786280032648, 0.007451944179420071090, 0.008693934875990107225, 0.009935925572560145094, 0.01241990696570024859, 0.01366189766227030901, 0.01490388835884037290, 0.01614587905541043159, 0.01738786975198049548, 0.01987185114512061979 ),
 .UNSPECIFIED. ) ;
#71432 = CARTESIAN_POINT ( 'NONE',  ( -100.8961411191535973, 120.6499999999999915, -3.968750000001104894 ) ) ;
#71433 = EDGE_LOOP ( 'NONE', ( #65798, #21866, #74298, #17425 ) ) ;
#71434 = ORIENTED_EDGE ( 'NONE', *, *, #77772, .F. ) ;
#71435 = DIRECTION ( 'NONE',  ( 0.7071067811989676377, 0.7071067811741275078, 7.071067811989670636E-16 ) ) ;
#71436 = EDGE_CURVE ( 'NONE', #38972, #22588, #6279, .T. ) ;
#71437 = EDGE_CURVE ( 'NONE', #19975, #6147, #70973, .T. ) ;
#71438 = DIRECTION ( 'NONE',  ( 1.000000000000000078E-15, -1.000000000000000083E-30, -1.000000000000000000 ) ) ;
#71439 = CARTESIAN_POINT ( 'NONE',  ( 115.1410662219050067, -33.85660664540706222, 113.5209912566479744 ) ) ;
#71440 = CARTESIAN_POINT ( 'NONE',  ( 96.95731234646120811, -39.36592712812080208, 276.5299109901967540 ) ) ;
#71441 = EDGE_CURVE ( 'NONE', #80932, #72917, #82584, .T. ) ;
#71442 = AXIS2_PLACEMENT_3D ( 'NONE', #86220, #58057, #2663 ) ;
#71443 = CARTESIAN_POINT ( 'NONE',  ( 180.2143765759489895, -35.91149509761070391, -5.074374724088000832 ) ) ;
#71444 = ORIENTED_EDGE ( 'NONE', *, *, #75330, .F. ) ;
#71445 = EDGE_CURVE ( 'NONE', #24211, #83168, #43385, .T. ) ;
#71446 = ORIENTED_EDGE ( 'NONE', *, *, #70196, .T. ) ;
#71447 = LINE ( 'NONE', #37355, #4358 ) ;
#71448 = DIRECTION ( 'NONE',  ( 0.000000000000000000, 0.000000000000000000, 1.000000000000000000 ) ) ;
#71449 = CARTESIAN_POINT ( 'NONE',  ( 70.62220382094542970, -139.6100950337742290, 247.3042842130787733 ) ) ;
#71450 = ADVANCED_FACE ( 'NONE', ( #56761 ), #50392, .F. ) ;
#71451 = AXIS2_PLACEMENT_3D ( 'NONE', #70511, #82479, #19333 ) ;
#71452 = CARTESIAN_POINT ( 'NONE',  ( 117.4075167370973958, -38.36336677748749224, 113.7013395616249767 ) ) ;
#71453 = CARTESIAN_POINT ( 'NONE',  ( 182.4202572930407769, -33.70561438051400671, 237.4678068554150059 ) ) ;
#71454 = ORIENTED_EDGE ( 'NONE', *, *, #60852, .T. ) ;
#71455 = UNCERTAINTY_MEASURE_WITH_UNIT (LENGTH_MEASURE( 1.000000000000000082E-05 ), #87751, 'distance_accuracy_value', 'NONE');
#71456 = CARTESIAN_POINT ( 'NONE',  ( 106.2268934648462420, -47.75097955688366369, 267.5280062282920994 ) ) ;
#71457 = CARTESIAN_POINT ( 'NONE',  ( 90.44969454456405344, -21.37118780205715396, 218.8274735512160589 ) ) ;
#71458 = DIRECTION ( 'NONE',  ( 9.002638163713000033E-13, -1.000000000000000000, 4.100000000000000342E-29 ) ) ;
#71459 = EDGE_CURVE ( 'NONE', #84598, #69696, #21363, .T. ) ;
#71461 = CARTESIAN_POINT ( 'NONE',  ( 68.96471483387718138, -139.0359911094384699, 246.8427143030575337 ) ) ;
#71460 = DIRECTION ( 'NONE',  ( 0.000000000000000000, 6.982966722218760189E-15, -1.000000000000000000 ) ) ;
#71462 = CARTESIAN_POINT ( 'NONE',  ( 173.9900000000000091, 53.21300000000000097, 59.96543552338539484 ) ) ;
#71463 = CARTESIAN_POINT ( 'NONE',  ( 57.56670390244744340, -48.82844715994040286, 173.2178068554150911 ) ) ;
#71464 = CARTESIAN_POINT ( 'NONE',  ( 131.3164832912740110, -36.72944715994100306, 6.749768910606454675 ) ) ;
#71465 = CARTESIAN_POINT ( 'NONE',  ( -6.714856022345324860, 93.33757043186105307, 130.3836582748265585 ) ) ;
#71466 = CARTESIAN_POINT ( 'NONE',  ( 97.31584373246833763, -39.30597606293734714, 12.53145861429736030 ) ) ;
#71467 = CARTESIAN_POINT ( 'NONE',  ( 117.0609946685736276, -38.07974641096466684, 163.7188594754593964 ) ) ;
#71469 = EDGE_CURVE ( 'NONE', #53210, #37453, #84509, .T. ) ;
#71468 = VECTOR ( 'NONE', #71518, 1000.000000000000000 ) ;
#71470 = DIRECTION ( 'NONE',  ( -0.9963424814100680926, 0.08544974978095698503, 0.000000000000000000 ) ) ;
#71471 = LINE ( 'NONE', #67200, #66981 ) ;
#71472 = CARTESIAN_POINT ( 'NONE',  ( 116.1589316287842735, -31.54115767207924748, 289.2384824187681716 ) ) ;
#71473 = CARTESIAN_POINT ( 'NONE',  ( 102.9671325615611437, -26.46449201736525225, 171.3908633711489813 ) ) ;
#71474 = CARTESIAN_POINT ( 'NONE',  ( 118.2318068709390815, -40.77392476355825579, 19.54991099019698453 ) ) ;
#71476 = CARTESIAN_POINT ( 'NONE',  ( 82.60054997757750073, -35.66120003907148117, 7.039521718173837428 ) ) ;
#71475 = CARTESIAN_POINT ( 'NONE',  ( -27.27158787008326968, 184.0000000000000000, 101.0189074266571794 ) ) ;
#71477 = CARTESIAN_POINT ( 'NONE',  ( 82.41744075320353602, -35.29868422066351030, 2.608896314039987452 ) ) ;
#71478 = ADVANCED_FACE ( 'NONE', ( #83156 ), #29522, .F. ) ;
#71479 = AXIS2_PLACEMENT_3D ( 'NONE', #89196, #41905, #1040 ) ;
#71480 = VERTEX_POINT ( 'NONE', #8639 ) ;
#71481 = DIRECTION ( 'NONE',  ( 4.299999999999999979E-14, -1.000000000000000000, 0.000000000000000000 ) ) ;
#71482 = ORIENTED_EDGE ( 'NONE', *, *, #37979, .F. ) ;
#71483 = AXIS2_PLACEMENT_3D ( 'NONE', #73780, #11565, #5648 ) ;
#71484 = CARTESIAN_POINT ( 'NONE',  ( 100.7170190823677132, -45.85612711270987774, 83.09276813305294240 ) ) ;
#71486 = ORIENTED_EDGE ( 'NONE', *, *, #83663, .T. ) ;
#71485 = LINE ( 'NONE', #9685, #34133 ) ;
#71487 = CARTESIAN_POINT ( 'NONE',  ( 117.0607673848196839, -38.08134988825185729, 49.71888720434603215 ) ) ;
#71488 = CARTESIAN_POINT ( 'NONE',  ( 117.9098725419244005, -34.70837513311213485, 199.9851490854349549 ) ) ;
#71489 = CARTESIAN_POINT ( 'NONE',  ( 126.8897065959774295, -54.55267237199291230, 14.92562527591099020 ) ) ;
#71490 = DIRECTION ( 'NONE',  ( 0.000000000000000000, 1.000000000000000000, 1.541976423090495239E-15 ) ) ;
#71491 = CARTESIAN_POINT ( 'NONE',  ( 107.0664832912739968, -36.72944715994100306, 277.6356252759110248 ) ) ;
#71492 = CARTESIAN_POINT ( 'NONE',  ( 114.4222700328740245, -29.92353839607118715, 85.42008522968446016 ) ) ;
#71493 = EDGE_CURVE ( 'NONE', #7158, #72087, #77674, .T. ) ;
#71494 = CARTESIAN_POINT ( 'NONE',  ( 145.3303304183568514, -139.4148206440309821, 246.0960064844549890 ) ) ;
#71495 = DIRECTION ( 'NONE',  ( 0.000000000000000000, 0.000000000000000000, -1.000000000000000000 ) ) ;
#71496 = EDGE_CURVE ( 'NONE', #83946, #26848, #23131, .T. ) ;
#71497 = CARTESIAN_POINT ( 'NONE',  ( 114.0519814166327563, -29.87813257090970609, 149.4441967044829767 ) ) ;
#71498 = EDGE_LOOP ( 'NONE', ( #48787, #80671, #9926, #86165 ) ) ;
#71499 = ORIENTED_EDGE ( 'NONE', *, *, #55856, .T. ) ;
#71500 = CARTESIAN_POINT ( 'NONE',  ( 103.8469135698534416, -45.55616208374542708, 93.71777378208700782 ) ) ;
#71501 = FACE_OUTER_BOUND ( 'NONE', #80702, .T. ) ;
#71503 = CARTESIAN_POINT ( 'NONE',  ( 0.000000000000000000, 8.255000000000000782, 0.000000000000000000 ) ) ;
#71502 = CARTESIAN_POINT ( 'NONE',  ( 109.1965444620390286, -27.18343884754229833, 220.9013395616249795 ) ) ;
#71504 = DIRECTION ( 'NONE',  ( 1.000000000000000000, 2.999999999999999839E-15, 1.000000000000000078E-15 ) ) ;
#71505 = CARTESIAN_POINT ( 'NONE',  ( 108.4174825185799733, -26.73503487134302503, 110.9692457430530652 ) ) ;
#71506 = FACE_OUTER_BOUND ( 'NONE', #80123, .T. ) ;
#71507 = CIRCLE ( 'NONE', #88933, 2.749999999999974687 ) ;
#71508 = CARTESIAN_POINT ( 'NONE',  ( 50.03799999999999670, 101.5999999999999943, 206.3750000000000000 ) ) ;
#71509 = CARTESIAN_POINT ( 'NONE',  ( 46.83715912545337545, -47.82818131006086304, 193.9678068554150911 ) ) ;
#71510 = CARTESIAN_POINT ( 'NONE',  ( 98.87380182923577365, -30.31772012733808808, 155.7984824187679465 ) ) ;
#71511 = ORIENTED_EDGE ( 'NONE', *, *, #70409, .F. ) ;
#71512 = ORIENTED_EDGE ( 'NONE', *, *, #57062, .F. ) ;
#71513 = EDGE_LOOP ( 'NONE', ( #83001, #10016, #15238, #50875 ) ) ;
#71514 = ADVANCED_FACE ( 'NONE', ( #58111 ), #78587, .F. ) ;
#71515 = CARTESIAN_POINT ( 'NONE',  ( 9.554664674393775314, 74.17305037928137779, 130.2061759407760633 ) ) ;
#71516 = DIRECTION ( 'NONE',  ( 1.000000000000000000, 0.000000000000000000, 0.000000000000000000 ) ) ;
#71517 = CARTESIAN_POINT ( 'NONE',  ( 97.39142042132525035, -39.27900364432255742, 131.5314998150807639 ) ) ;
#71518 = DIRECTION ( 'NONE',  ( 0.000000000000000000, 1.000000000000000000, 0.000000000000000000 ) ) ;
#71519 = CARTESIAN_POINT ( 'NONE',  ( 99.99635294717694478, -42.73853927783394369, 224.7052332267339807 ) ) ;
#71520 = AXIS2_PLACEMENT_3D ( 'NONE', #86821, #65031, #23282 ) ;
#71521 = EDGE_CURVE ( 'NONE', #31761, #30540, #37225, .T. ) ;
#71522 = CARTESIAN_POINT ( 'NONE',  ( 116.7951241094207830, -39.38783451605569752, 269.6147915599842122 ) ) ;
#71523 = CARTESIAN_POINT ( 'NONE',  ( 117.4874684240972300, -40.41484487456647656, 178.5680062282919778 ) ) ;
#71524 = DIRECTION ( 'NONE',  ( -1.000000000000000000, 0.000000000000000000, -2.301579500234999682E-14 ) ) ;
#71525 = ORIENTED_EDGE ( 'NONE', *, *, #10243, .T. ) ;
#71527 = VERTEX_POINT ( 'NONE', #16339 ) ;
#71526 = ORIENTED_EDGE ( 'NONE', *, *, #51904, .T. ) ;
#71528 = FACE_OUTER_BOUND ( 'NONE', #72040, .T. ) ;
#71529 = EDGE_LOOP ( 'NONE', ( #87051, #67823, #42993, #8364 ) ) ;
#71530 = VERTEX_POINT ( 'NONE', #64930 ) ;
#71531 = CYLINDRICAL_SURFACE ( 'NONE', #30427, 3.000000000000002665 ) ;
#71532 = DIRECTION ( 'NONE',  ( -1.000000000000000000, 0.000000000000000000, 0.000000000000000000 ) ) ;
#71533 = CARTESIAN_POINT ( 'NONE',  ( 104.9598549460505126, -28.12176414095025834, 281.6987261630399644 ) ) ;
#71534 = CARTESIAN_POINT ( 'NONE',  ( 72.96458098368701428, 127.0000000000000000, -65.02708098368670164 ) ) ;
#71535 = ORIENTED_EDGE ( 'NONE', *, *, #20206, .F. ) ;
#71536 = CARTESIAN_POINT ( 'NONE',  ( 107.5239001228424058, -44.99862095125077133, 9.635625275910943088 ) ) ;
#71537 = CARTESIAN_POINT ( 'NONE',  ( 34.92499999999999716, 73.38456447661469895, 302.8950000000000387 ) ) ;
#71538 = ORIENTED_EDGE ( 'NONE', *, *, #40949, .F. ) ;
#71539 = EDGE_LOOP ( 'NONE', ( #53379, #16916, #66273, #45009 ) ) ;
#71540 = VECTOR ( 'NONE', #37708, 1000.000000000000000 ) ;
#71541 = CARTESIAN_POINT ( 'NONE',  ( 98.04155473296256673, -41.04193254465488394, 111.6812086568694440 ) ) ;
#71542 = ORIENTED_EDGE ( 'NONE', *, *, #59303, .T. ) ;
#71543 = VERTEX_POINT ( 'NONE', #24052 ) ;
#71544 = AXIS2_PLACEMENT_3D ( 'NONE', #72321, #88195, #80936 ) ;
#71545 = ADVANCED_FACE ( 'NONE', ( #23180 ), #17234, .T. ) ;
#71546 = EDGE_CURVE ( 'NONE', #52594, #11728, #51273, .T. ) ;
#71547 = AXIS2_PLACEMENT_3D ( 'NONE', #79616, #10995, #17816 ) ;
#71548 = CARTESIAN_POINT ( 'NONE',  ( 116.0863591824327443, -37.53846460971577415, 33.16575316141096152 ) ) ;
#71549 = CARTESIAN_POINT ( 'NONE',  ( 102.8350101556302434, -46.28146260531957523, 177.2441967044819648 ) ) ;
#71550 = EDGE_CURVE ( 'NONE', #87063, #70690, #71755, .T. ) ;
#71551 = CARTESIAN_POINT ( 'NONE',  ( 104.9672558511365992, -25.09151557957600076, 125.2184824187689856 ) ) ;
#71552 = CARTESIAN_POINT ( 'NONE',  ( 96.13817600250692408, -35.07231702426307152, 217.1946728949589840 ) ) ;
#71553 = CARTESIAN_POINT ( 'NONE',  ( 115.7832353055570280, -41.80209406143853812, 99.40770611954226865 ) ) ;
#71554 = CARTESIAN_POINT ( 'NONE',  ( 68.77555145974430673, -69.40287493179035039, 247.4783998280180128 ) ) ;
#71555 = CARTESIAN_POINT ( 'NONE',  ( -130.5246120830808820, 70.17656663518266669, 2.891956274607122790 ) ) ;
#71556 = EDGE_LOOP ( 'NONE', ( #33914, #59064, #36385, #89801 ) ) ;
#71557 = EDGE_CURVE ( 'NONE', #71147, #70860, #29969, .T. ) ;
#71558 = ORIENTED_EDGE ( 'NONE', *, *, #64149, .F. ) ;
#71559 = EDGE_CURVE ( 'NONE', #40087, #74344, #37677, .T. ) ;
#71560 = CARTESIAN_POINT ( 'NONE',  ( 114.9985205141181837, -29.89647917087096118, 184.3927681330539770 ) ) ;
#71561 = ORIENTED_EDGE ( 'NONE', *, *, #49361, .F. ) ;
#71562 = CARTESIAN_POINT ( 'NONE',  ( 108.3661291232776023, -47.70624136733754028, 162.6822919425769669 ) ) ;
#71563 = LINE ( 'NONE', #9324, #22495 ) ;
#71564 = CARTESIAN_POINT ( 'NONE',  ( 135.6272734918642868, -34.46583755400483540, 7.833212107639223376 ) ) ;
#71565 = LINE ( 'NONE', #22515, #15203 ) ;
#71568 = CARTESIAN_POINT ( 'NONE',  ( 108.0121126588926046, -24.94157235513516468, 261.0127681330534415 ) ) ;
#71567 = DIRECTION ( 'NONE',  ( -4.093947403305260305E-16, 1.000000000000000000, -6.162975822039159109E-32 ) ) ;
#71566 = CARTESIAN_POINT ( 'NONE',  ( 27.27158787008328389, 184.0000000000000000, 111.9860621927989683 ) ) ;
#71569 = CARTESIAN_POINT ( 'NONE',  ( 0.000000000000000000, 50.79999999999999716, 265.5569999999999595 ) ) ;
#71571 = EDGE_CURVE ( 'NONE', #24085, #56828, #86273, .T. ) ;
#71570 = CARTESIAN_POINT ( 'NONE',  ( 165.6738106836030227, -28.98061976758901537, 342.9256252759109884 ) ) ;
#71572 = CARTESIAN_POINT ( 'NONE',  ( 97.81373435033219721, -40.51654435448209313, 87.63515866765291662 ) ) ;
#71573 = AXIS2_PLACEMENT_3D ( 'NONE', #33708, #82326, #50456 ) ;
#71574 = CYLINDRICAL_SURFACE ( 'NONE', #84902, 50.79999999999999716 ) ;
#71575 = CARTESIAN_POINT ( 'NONE',  ( 97.33784130303931192, -34.07106455859420890, 257.1147919449370534 ) ) ;
#71576 = CARTESIAN_POINT ( 'NONE',  ( 146.4497560438693711, -137.3344668342741670, 246.9543106399991075 ) ) ;
#71578 = ORIENTED_EDGE ( 'NONE', *, *, #77485, .T. ) ;
#71577 = CARTESIAN_POINT ( 'NONE',  ( 111.9759329535769297, -43.13121445202460791, 195.5838068554168103 ) ) ;
#71579 = DIRECTION ( 'NONE',  ( 1.000000000000000000, 0.000000000000000000, 0.000000000000000000 ) ) ;
#71580 = CARTESIAN_POINT ( 'NONE',  ( 109.8619129364321481, -26.66307059906275612, 174.8613395616249591 ) ) ;
#71581 = CARTESIAN_POINT ( 'NONE',  ( 104.0427601340384030, -47.36105469373795529, 63.36800622829197494 ) ) ;
#71582 = CARTESIAN_POINT ( 'NONE',  ( 103.6242938494280423, -26.17725164406494542, 206.3394347997209763 ) ) ;
#71583 = FACE_OUTER_BOUND ( 'NONE', #6260, .T. ) ;
#71584 = DIRECTION ( 'NONE',  ( -4.237773401492740281E-14, 1.000000000000000000, 0.000000000000000000 ) ) ;
#71586 = FACE_OUTER_BOUND ( 'NONE', #77680, .T. ) ;
#71585 = DIRECTION ( 'NONE',  ( 0.7071067811861728725, -0.7071067811869222730, 0.000000000000000000 ) ) ;
#71587 = DIRECTION ( 'NONE',  ( 0.000000000000000000, 0.000000000000000000, 1.000000000000000000 ) ) ;
#71588 = PLANE ( 'NONE',  #15136 ) ;
#71589 = EDGE_LOOP ( 'NONE', ( #59626, #67694, #81445, #30276 ) ) ;
#71590 = AXIS2_PLACEMENT_3D ( 'NONE', #53787, #26556, #60161 ) ;
#71591 = LINE ( 'NONE', #80188, #38428 ) ;
#71592 = VERTEX_POINT ( 'NONE', #79474 ) ;
#71593 = ORIENTED_EDGE ( 'NONE', *, *, #11756, .T. ) ;
#71594 = CARTESIAN_POINT ( 'NONE',  ( 98.64819939953339656, -38.17465580927972724, 90.88384839950496996 ) ) ;
#71596 = ORIENTED_EDGE ( 'NONE', *, *, #50626, .T. ) ;
#71595 = CARTESIAN_POINT ( 'NONE',  ( -2.883471595053325398, 94.92538689125282758, -130.5247975405367526 ) ) ;
#71597 = CARTESIAN_POINT ( 'NONE',  ( 116.9541756933414263, -33.49491404195861577, 85.07848241876791917 ) ) ;
#71598 = DIRECTION ( 'NONE',  ( 0.000000000000000000, -1.000000000000000000, 0.000000000000000000 ) ) ;
#71599 = DIRECTION ( 'NONE',  ( 1.000000000000000078E-15, -1.000000000000000083E-30, -1.000000000000000000 ) ) ;
#71600 = CARTESIAN_POINT ( 'NONE',  ( 100.9546728288143527, -28.70702571419132809, 176.5939586075147929 ) ) ;
#71601 = EDGE_CURVE ( 'NONE', #42662, #5137, #52117, .T. ) ;
#71602 = CARTESIAN_POINT ( 'NONE',  ( 112.5987260342905358, -28.66361022110268308, 44.59848241876795782 ) ) ;
#71603 = VERTEX_POINT ( 'NONE', #64490 ) ;
#71604 = ORIENTED_EDGE ( 'NONE', *, *, #23811, .F. ) ;
#71605 = ORIENTED_EDGE ( 'NONE', *, *, #52115, .F. ) ;
#71606 = AXIS2_PLACEMENT_3D ( 'NONE', #35685, #56574, #1638 ) ;
#71607 = DIRECTION ( 'NONE',  ( 0.000000000000000000, 0.000000000000000000, 1.000000000000000000 ) ) ;
#71608 = DIRECTION ( 'NONE',  ( 0.000000000000000000, 1.000000000000000000, -0.000000000000000000 ) ) ;
#71610 = VECTOR ( 'NONE', #1837, 1000.000000000000000 ) ;
#71609 = CARTESIAN_POINT ( 'NONE',  ( 97.06107109598296745, -37.99641195321030551, 117.4272919417498144 ) ) ;
#71611 = DIRECTION ( 'NONE',  ( 1.000000000000000078E-15, -1.000000000000000000, 0.000000000000000000 ) ) ;
#71612 = DIRECTION ( 'NONE',  ( -1.000000000000000000, 0.000000000000000000, -3.491481338843133355E-15 ) ) ;
#71613 = CARTESIAN_POINT ( 'NONE',  ( 108.4182074779043603, -26.73512707025641433, 50.97033420604262943 ) ) ;
#71614 = CARTESIAN_POINT ( 'NONE',  ( 67.06670390244700286, -67.87844716047356997, 245.4920193514540188 ) ) ;
#71615 = CARTESIAN_POINT ( 'NONE',  ( 74.44936585838333087, 84.21376545118702950, 92.26493792250116144 ) ) ;
#71616 = CARTESIAN_POINT ( 'NONE',  ( 104.7644060343265409, -46.87484541886973943, 72.39848241876795498 ) ) ;
#71617 = ORIENTED_EDGE ( 'NONE', *, *, #33916, .F. ) ;
#71618 = CARTESIAN_POINT ( 'NONE',  ( 116.3251852747984003, -32.94148267319277323, 269.1356252759109680 ) ) ;
#71619 = CARTESIAN_POINT ( 'NONE',  ( 50.03799999999999670, 101.5999999999999943, 206.3750000000000000 ) ) ;
#71620 = CARTESIAN_POINT ( 'NONE',  ( 99.95702547362903090, -40.74009991652987139, 134.5538046553059530 ) ) ;
#71621 = ADVANCED_FACE ( 'NONE', ( #57660 ), #28459, .T. ) ;
#71622 = AXIS2_PLACEMENT_3D ( 'NONE', #5928, #33617, #61312 ) ;
#71623 = VECTOR ( 'NONE', #46638, 1000.000000000000000 ) ;
#71624 = LINE ( 'NONE', #16651, #48477 ) ;
#71625 = FACE_OUTER_BOUND ( 'NONE', #61276, .T. ) ;
#71626 = VERTEX_POINT ( 'NONE', #2113 ) ;
#71627 = EDGE_LOOP ( 'NONE', ( #57334, #31524 ) ) ;
#71628 = DIRECTION ( 'NONE',  ( 0.000000000000000000, 0.000000000000000000, 1.000000000000000000 ) ) ;
#71629 = AXIS2_PLACEMENT_3D ( 'NONE', #33444, #54753, #19821 ) ;
#71630 = VERTEX_POINT ( 'NONE', #63897 ) ;
#71631 = ORIENTED_EDGE ( 'NONE', *, *, #84371, .T. ) ;
#71632 = CARTESIAN_POINT ( 'NONE',  ( 115.3361691346596558, -39.99662111280561305, 189.9587261630399553 ) ) ;
#71633 = DIRECTION ( 'NONE',  ( 1.000000000000000000, 4.299999999999999979E-14, 1.000000000000000078E-15 ) ) ;
#71634 = CARTESIAN_POINT ( 'NONE',  ( 107.9474582775578568, -25.68820226555254749, 111.0251490854349754 ) ) ;
#71635 = CARTESIAN_POINT ( 'NONE',  ( 105.7995185650176779, -26.72403495711487764, 120.1772919364191665 ) ) ;
#71636 = VECTOR ( 'NONE', #40323, 1000.000000000000000 ) ;
#71637 = CARTESIAN_POINT ( 'NONE',  ( 98.30753417424557483, -41.72887546278693094, 82.73979193999794290 ) ) ;
#71638 = VERTEX_POINT ( 'NONE', #29377 ) ;
#71639 = ORIENTED_EDGE ( 'NONE', *, *, #76963, .F. ) ;
#71640 = ORIENTED_EDGE ( 'NONE', *, *, #49136, .T. ) ;
#71641 = EDGE_CURVE ( 'NONE', #65538, #18397, #56148, .T. ) ;
#71642 = CARTESIAN_POINT ( 'NONE',  ( 108.3259390676978455, -28.66449228317154763, 187.7709475124489700 ) ) ;
#71643 = CARTESIAN_POINT ( 'NONE',  ( 98.57199122844706096, -43.83852907894476658, 71.86895860924397539 ) ) ;
#71644 = ORIENTED_EDGE ( 'NONE', *, *, #51013, .T. ) ;
#71645 = ADVANCED_FACE ( 'NONE', ( #1674 ), #78434, .T. ) ;
#71646 = CARTESIAN_POINT ( 'NONE',  ( 106.2538455105912050, -26.32252419718678027, 25.13848241876792855 ) ) ;
#71647 = CARTESIAN_POINT ( 'NONE',  ( 99.27233432241882838, -29.77326281039884037, 186.7470538473389752 ) ) ;
#71648 = DIRECTION ( 'NONE',  ( 1.000000000000000078E-15, 1.000000000000000083E-30, -1.000000000000000000 ) ) ;
#71649 = FACE_BOUND ( 'NONE', #24724, .T. ) ;
#71650 = EDGE_CURVE ( 'NONE', #3324, #53629, #79727, .T. ) ;
#71651 = CARTESIAN_POINT ( 'NONE',  ( 114.7713543040237454, -44.65465650488444993, 114.2022919425779719 ) ) ;
#71652 = DIRECTION ( 'NONE',  ( -0.7071067811865370256, 0.000000000000000000, 0.7071067811865580088 ) ) ;
#71653 = ORIENTED_EDGE ( 'NONE', *, *, #21949, .F. ) ;
#71654 = FACE_OUTER_BOUND ( 'NONE', #10227, .T. ) ;
#71655 = EDGE_CURVE ( 'NONE', #42544, #19998, #49345, .T. ) ;
#71656 = ORIENTED_EDGE ( 'NONE', *, *, #56713, .F. ) ;
#71657 = CARTESIAN_POINT ( 'NONE',  ( 27.27158787008325902, 127.0000000000000000, -5.920431057502157584E-15 ) ) ;
#71658 = DIRECTION ( 'NONE',  ( 6.745093096447288888E-17, 1.000000000000000000, 0.000000000000000000 ) ) ;
#71659 = VERTEX_POINT ( 'NONE', #42524 ) ;
#71660 = CIRCLE ( 'NONE', #10746, 7.937500000000000000 ) ;
#71661 = LINE ( 'NONE', #50293, #64941 ) ;
#71662 = CARTESIAN_POINT ( 'NONE',  ( 108.1495617321014748, -26.75831605517002387, 130.9904251009939173 ) ) ;
#71663 = CARTESIAN_POINT ( 'NONE',  ( 97.28826076399516865, -33.11373220042904109, 66.04419670448297097 ) ) ;
#71664 = CARTESIAN_POINT ( 'NONE',  ( 14.46226641585351835, 67.55286469922893389, 35.25428405273846266 ) ) ;
#71665 = AXIS2_PLACEMENT_3D ( 'NONE', #74107, #52722, #66380 ) ;
#71666 = CARTESIAN_POINT ( 'NONE',  ( 163.0667039024470171, -33.35206098992711077, -5.074374724088000832 ) ) ;
#71667 = CARTESIAN_POINT ( 'NONE',  ( 115.7831076719501056, -41.80230950688442704, 74.40645860955640956 ) ) ;
#71668 = CARTESIAN_POINT ( 'NONE',  ( 112.4622727538958884, -27.87370092883236694, 49.62895860924398761 ) ) ;
#71670 = CARTESIAN_POINT ( 'NONE',  ( 114.4965984691700953, -29.44205611023144087, 145.4441967044819819 ) ) ;
#71669 = CARTESIAN_POINT ( 'NONE',  ( 105.7992162164682384, -26.72406929376951723, 110.1773159172848722 ) ) ;
#71671 = CARTESIAN_POINT ( 'NONE',  ( 116.3173461584868278, -32.93718857426866720, 59.13562527591098217 ) ) ;
#71673 = ADVANCED_FACE ( 'NONE', ( #71166 ), #77076, .F. ) ;
#71672 = CARTESIAN_POINT ( 'NONE',  ( -469.3583484187089994, 53.97500000000000142, 3.174999999999999822 ) ) ;
#71674 = ORIENTED_EDGE ( 'NONE', *, *, #42801, .T. ) ;
#71675 = DIRECTION ( 'NONE',  ( 0.000000000000000000, 0.000000000000000000, -1.000000000000000000 ) ) ;
#71676 = DIRECTION ( 'NONE',  ( 0.000000000000000000, 0.000000000000000000, -1.000000000000000000 ) ) ;
#71677 = CARTESIAN_POINT ( 'NONE',  ( 4.163101094985349692E-14, 127.0000000000000000, -107.7702177616926065 ) ) ;
#71678 = LINE ( 'NONE', #57580, #72333 ) ;
#71680 = ORIENTED_EDGE ( 'NONE', *, *, #30467, .T. ) ;
#71679 = CARTESIAN_POINT ( 'NONE',  ( 107.2439172579031919, -47.23279478401654075, 212.5899109901969837 ) ) ;
#71681 = DIRECTION ( 'NONE',  ( -1.000000000000000000, -5.512527431108013646E-15, 0.000000000000000000 ) ) ;
#71682 = CARTESIAN_POINT ( 'NONE',  ( 98.92566635982139189, -30.18235936901480443, 236.7870538473399336 ) ) ;
#71683 = CARTESIAN_POINT ( 'NONE',  ( 98.11234142011190329, -43.28847465721014487, 102.8175300378159847 ) ) ;
#71684 = CARTESIAN_POINT ( 'NONE',  ( 111.3555650440039528, -119.3022720253473210, -21.78219314458154798 ) ) ;
#71685 = CARTESIAN_POINT ( 'NONE',  ( 116.3231543710223121, -32.93883412237410369, 190.1356252759109680 ) ) ;
#71686 = CARTESIAN_POINT ( 'NONE',  ( -7.661254700127833495, 69.45253841614081125, 320.6630000000000109 ) ) ;
#71687 = ORIENTED_EDGE ( 'NONE', *, *, #63457, .T. ) ;
#71688 = VECTOR ( 'NONE', #49586, 1000.000000000000000 ) ;
#71689 = AXIS2_PLACEMENT_3D ( 'NONE', #51986, #86106, #65641 ) ;
#71690 = AXIS2_PLACEMENT_3D ( 'NONE', #68422, #81622, #12560 ) ;
#71691 = ORIENTED_EDGE ( 'NONE', *, *, #68690, .T. ) ;
#71692 = EDGE_LOOP ( 'NONE', ( #71744, #41569, #75821, #42230, #9621, #21758 ) ) ;
#71693 = AXIS2_PLACEMENT_3D ( 'NONE', #27084, #5753, #41141 ) ;
#71694 = EDGE_LOOP ( 'NONE', ( #20910, #49694, #34358, #28947 ) ) ;
#71695 = LINE ( 'NONE', #2658, #36393 ) ;
#71696 = CARTESIAN_POINT ( 'NONE',  ( 100.1387811872355371, -44.51978932219680019, 262.9984824187678782 ) ) ;
#71697 = PLANE ( 'NONE',  #8391 ) ;
#71698 = DIRECTION ( 'NONE',  ( 1.000000000000000000, 0.000000000000000000, 4.811757763307910244E-15 ) ) ;
#71700 = DIRECTION ( 'NONE',  ( 8.659560562355369197E-17, 0.7071067811865120456, -0.7071067811865829889 ) ) ;
#71699 = CYLINDRICAL_SURFACE ( 'NONE', #17737, 7.199999999999998401 ) ;
#71701 = DIRECTION ( 'NONE',  ( 1.000000000000000078E-15, 1.000000000000000083E-30, -1.000000000000000000 ) ) ;
#71702 = ADVANCED_FACE ( 'NONE', ( #84356, #14858 ), #63436, .T. ) ;
#71703 = CARTESIAN_POINT ( 'NONE',  ( 101.0745446329174655, -30.64234581064881269, 225.1181341137909442 ) ) ;
#71704 = ORIENTED_EDGE ( 'NONE', *, *, #82116, .T. ) ;
#71705 = VERTEX_POINT ( 'NONE', #22566 ) ;
#71706 = ORIENTED_EDGE ( 'NONE', *, *, #54056, .T. ) ;
#71707 = LINE ( 'NONE', #38952, #65170 ) ;
#71708 = EDGE_CURVE ( 'NONE', #76254, #57775, #12993, .T. ) ;
#71709 = CARTESIAN_POINT ( 'NONE',  ( 107.9555263298577188, -25.64695713395855137, 261.0127681330532710 ) ) ;
#71710 = CARTESIAN_POINT ( 'NONE',  ( 180.3521107875703535, -35.65087443489212404, 237.4678068554150059 ) ) ;
#71711 = CARTESIAN_POINT ( 'NONE',  ( 98.15811136316406760, -31.42099212808723863, 126.9108633711489915 ) ) ;
#71712 = CARTESIAN_POINT ( 'NONE',  ( -487.2989999999999782, 93.66249999999999432, 82.23860802895320887 ) ) ;
#71713 = VERTEX_POINT ( 'NONE', #16196 ) ;
#71714 = LINE ( 'NONE', #56721, #87882 ) ;
#71715 = LINE ( 'NONE', #56722, #8530 ) ;
#71716 = ORIENTED_EDGE ( 'NONE', *, *, #29229, .F. ) ;
#71717 = DIRECTION ( 'NONE',  ( 0.000000000000000000, -1.000000000000000000, 0.000000000000000000 ) ) ;
#71718 = CARTESIAN_POINT ( 'NONE',  ( 105.5764564592757466, -44.77785207962899250, 10.24809036959195652 ) ) ;
#71719 = VECTOR ( 'NONE', #1657, 999.9999999999998863 ) ;
#71720 = EDGE_CURVE ( 'NONE', #5050, #28392, #50240, .T. ) ;
#71721 =( BOUNDED_CURVE ( )  B_SPLINE_CURVE ( 2, ( #21044, #48717, #587 ),
 .UNSPECIFIED., .F., .T. ) 
 B_SPLINE_CURVE_WITH_KNOTS ( ( 3, 3 ),
 ( 0.01169420784673960018, 0.5170228498526580063 ),
 .UNSPECIFIED. ) 
 CURVE ( )  GEOMETRIC_REPRESENTATION_ITEM ( )  RATIONAL_B_SPLINE_CURVE ( ( 1.000420656333759872, 1.009299002520659849, 1.000000000000000000 ) ) 
 REPRESENTATION_ITEM ( '' )  );
#71722 = DIRECTION ( 'NONE',  ( 0.7071067811866516006, -0.7071067811864434338, 0.000000000000000000 ) ) ;
#71723 = AXIS2_PLACEMENT_3D ( 'NONE', #62607, #6304, #33997 ) ;
#71724 = DIRECTION ( 'NONE',  ( 0.000000000000000000, 0.000000000000000000, 1.000000000000000000 ) ) ;
#71725 = CARTESIAN_POINT ( 'NONE',  ( 92.27899210470920366, 80.89685143461889538, -74.43211355457083300 ) ) ;
#71726 = ORIENTED_EDGE ( 'NONE', *, *, #64421, .T. ) ;
#71727 = DIRECTION ( 'NONE',  ( 1.000000000000000078E-15, -1.000000000000000083E-30, -1.000000000000000000 ) ) ;
#71728 = DIRECTION ( 'NONE',  ( 0.000000000000000000, 0.000000000000000000, 1.000000000000000000 ) ) ;
#71729 = VERTEX_POINT ( 'NONE', #8485 ) ;
#71730 = CARTESIAN_POINT ( 'NONE',  ( 104.0426969376867987, -47.36127689622573200, 67.36800622829191809 ) ) ;
#71731 = EDGE_LOOP ( 'NONE', ( #9395, #49030, #30160, #57426 ) ) ;
#71732 = CARTESIAN_POINT ( 'NONE',  ( 102.8831062096190436, -29.28260300185988996, 59.90670554236199052 ) ) ;
#71733 = EDGE_CURVE ( 'NONE', #12494, #69459, #42080, .T. ) ;
#71734 = CARTESIAN_POINT ( 'NONE',  ( 111.4018971211722544, -45.77100106855414197, 88.93158766652720715 ) ) ;
#71735 = CARTESIAN_POINT ( 'NONE',  ( 103.5852769812406535, -44.87864842379759978, 88.68729759161098514 ) ) ;
#71736 = FACE_OUTER_BOUND ( 'NONE', #73748, .T. ) ;
#71737 = CARTESIAN_POINT ( 'NONE',  ( 49.16670390244745192, -28.27351298637373489, 313.9678068554150059 ) ) ;
#71738 = CARTESIAN_POINT ( 'NONE',  ( 22.49563609058251146, -67.87844715994100397, 307.9888746672805269 ) ) ;
#71739 = CARTESIAN_POINT ( 'NONE',  ( 111.0094172226674374, -46.42718045843506047, 278.8841967044824059 ) ) ;
#71740 = CARTESIAN_POINT ( 'NONE',  ( 22.62762465138245460, 171.9999999999999716, 183.8826257785461280 ) ) ;
#71741 = VERTEX_POINT ( 'NONE', #43874 ) ;
#71742 = PLANE ( 'NONE',  #25546 ) ;
#71743 = VECTOR ( 'NONE', #43866, 1000.000000000000114 ) ;
#71744 = ORIENTED_EDGE ( 'NONE', *, *, #23771, .F. ) ;
#71745 = CARTESIAN_POINT ( 'NONE',  ( 108.2828737166157964, -47.76209090725709672, 153.6518157521009584 ) ) ;
#71746 = DIRECTION ( 'NONE',  ( 1.000000000000000000, 4.299999999999999979E-14, 1.000000000000000078E-15 ) ) ;
#71747 = VECTOR ( 'NONE', #31895, 1000.000000000000000 ) ;
#71748 = AXIS2_PLACEMENT_3D ( 'NONE', #6779, #66422, #34479 ) ;
#71749 = AXIS2_PLACEMENT_3D ( 'NONE', #80608, #79720, #18357 ) ;
#71750 = EDGE_LOOP ( 'NONE', ( #85595, #17245, #83898, #8985 ) ) ;
#71751 = VERTEX_POINT ( 'NONE', #22124 ) ;
#71752 = EDGE_LOOP ( 'NONE', ( #21939, #71992, #19500, #3275 ) ) ;
#71753 = DIRECTION ( 'NONE',  ( -1.000000000000000000, 0.000000000000000000, 0.000000000000000000 ) ) ;
#71754 = AXIS2_PLACEMENT_3D ( 'NONE', #59048, #52223, #79987 ) ;
#71755 = LINE ( 'NONE', #9522, #7224 ) ;
#71756 = CARTESIAN_POINT ( 'NONE',  ( 114.9950743857441608, -30.04541929558963886, 224.3718157521019521 ) ) ;
#71757 = CARTESIAN_POINT ( 'NONE',  ( 41.56648329127499153, -36.32844715994070839, 14.17562527591199917 ) ) ;
#71758 = CARTESIAN_POINT ( 'NONE',  ( 31.56670390244621771, -32.29483332968584364, 193.9678068554150911 ) ) ;
#71759 = CYLINDRICAL_SURFACE ( 'NONE', #60602, 3.249999999999975131 ) ;
#71760 = EDGE_CURVE ( 'NONE', #56062, #14566, #7134, .T. ) ;
#71761 = CARTESIAN_POINT ( 'NONE',  ( 99.76212870471702843, -44.21728614272981872, 17.96133956162493206 ) ) ;
#71762 = DIRECTION ( 'NONE',  ( 1.000000000000000000, 0.000000000000000000, 0.000000000000000000 ) ) ;
#71763 = EDGE_LOOP ( 'NONE', ( #45617, #15208 ) ) ;
#71764 = CARTESIAN_POINT ( 'NONE',  ( 116.3153332067577850, -32.94059133099460723, 170.1356252759109680 ) ) ;
#71765 = DIRECTION ( 'NONE',  ( 0.000000000000000000, 1.000000000000000000, 0.000000000000000000 ) ) ;
#71766 = ORIENTED_EDGE ( 'NONE', *, *, #87464, .T. ) ;
#71767 = CARTESIAN_POINT ( 'NONE',  ( 82.10314251156495402, -20.57949487819488255, 2.327894807232544938 ) ) ;
#71768 = DIRECTION ( 'NONE',  ( 3.100000000000000258E-29, -3.100000000000000044E-14, -1.000000000000000000 ) ) ;
#71769 = CARTESIAN_POINT ( 'NONE',  ( 110.2492204789523242, -26.78788743924345184, 234.8299109901969643 ) ) ;
#71770 = DIRECTION ( 'NONE',  ( -4.299999999999999979E-14, 1.000000000000000000, -4.400000000000000367E-29 ) ) ;
#71771 = FACE_BOUND ( 'NONE', #2693, .T. ) ;
#71772 = LINE ( 'NONE', #77692, #70826 ) ;
#71773 = CARTESIAN_POINT ( 'NONE',  ( 115.1107970995275736, -40.88897666221423322, 242.8571817328389670 ) ) ;
#71775 = CARTESIAN_POINT ( 'NONE',  ( 96.20032699425235023, -38.62430069186628856, 42.45181575210199298 ) ) ;
#71774 = CYLINDRICAL_SURFACE ( 'NONE', #82389, 2.517499999999998739 ) ;
#71776 = CARTESIAN_POINT ( 'NONE',  ( 123.1816666992336167, 73.18476051486229039, 43.25682771927707648 ) ) ;
#71777 = CARTESIAN_POINT ( 'NONE',  ( 113.8852007176727028, -44.67373811025045427, 108.1413395616249744 ) ) ;
#71778 = EDGE_LOOP ( 'NONE', ( #43290, #88848, #50305, #46361 ) ) ;
#71780 = EDGE_CURVE ( 'NONE', #15679, #73188, #34830, .T. ) ;
#71779 = CARTESIAN_POINT ( 'NONE',  ( 131.7480217999322747, -20.20859666167233470, 7.273989459504827337 ) ) ;
#71781 = ORIENTED_EDGE ( 'NONE', *, *, #2228, .T. ) ;
#71782 = CARTESIAN_POINT ( 'NONE',  ( 83.06670390244796920, -61.87844715994100397, 231.5838068554150198 ) ) ;
#71783 = EDGE_CURVE ( 'NONE', #69275, #55699, #28009, .T. ) ;
#71784 = CARTESIAN_POINT ( 'NONE',  ( 112.7628927828184402, -28.45360054538134520, 275.5965050139159302 ) ) ;
#71785 = ORIENTED_EDGE ( 'NONE', *, *, #45616, .T. ) ;
#71786 = DIRECTION ( 'NONE',  ( 0.000000000000000000, 0.000000000000000000, -1.000000000000000000 ) ) ;
#71787 = ORIENTED_EDGE ( 'NONE', *, *, #84269, .T. ) ;
#71788 = CARTESIAN_POINT ( 'NONE',  ( 194.0371591254572650, -24.42818131005417825, 313.9678068554149490 ) ) ;
#71789 = FACE_OUTER_BOUND ( 'NONE', #25321, .T. ) ;
#71790 = DIRECTION ( 'NONE',  ( 0.000000000000000000, 0.000000000000000000, -1.000000000000000000 ) ) ;
#71791 = EDGE_LOOP ( 'NONE', ( #86461, #21125, #37971, #35533 ) ) ;
#71792 = CARTESIAN_POINT ( 'NONE',  ( 103.2708046866033129, -47.13561192255075838, 97.28610146638693834 ) ) ;
#71793 = CARTESIAN_POINT ( 'NONE',  ( 0.000000000000000000, 0.000000000000000000, 0.000000000000000000 ) ) ;
#71794 = AXIS2_PLACEMENT_3D ( 'NONE', #45276, #72994, #10761 ) ;
#71795 = CARTESIAN_POINT ( 'NONE',  ( 188.5667039024486087, -48.82844715993430640, 137.2178068554150059 ) ) ;
#71796 = CARTESIAN_POINT ( 'NONE',  ( 165.6738106836030227, -28.98061976758901892, -5.074374724088000832 ) ) ;
#71797 = CARTESIAN_POINT ( 'NONE',  ( -12.60000000000000142, 82.54999999999999716, 117.6834004267381744 ) ) ;
#71798 = ORIENTED_EDGE ( 'NONE', *, *, #67275, .F. ) ;
#71799 = APPLICATION_CONTEXT ( 'automotive_design' ) ;
#71800 = CARTESIAN_POINT ( 'NONE',  ( 100.0213216842705748, 88.17609398443094904, -83.90854149456399114 ) ) ;
#71801 = DIRECTION ( 'NONE',  ( 0.000000000000000000, 1.000000000000000000, 0.000000000000000000 ) ) ;
#71802 = DIRECTION ( 'NONE',  ( 0.000000000000000000, 0.000000000000000000, 1.000000000000000000 ) ) ;
#71804 = LINE ( 'NONE', #78192, #15200 ) ;
#71803 = FACE_OUTER_BOUND ( 'NONE', #4269, .T. ) ;
#71805 = LINE ( 'NONE', #78644, #59596 ) ;
#71806 = AXIS2_PLACEMENT_3D ( 'NONE', #39544, #20460, #81797 ) ;
#71807 = ORIENTED_EDGE ( 'NONE', *, *, #16992, .T. ) ;
#71808 = AXIS2_PLACEMENT_3D ( 'NONE', #52652, #87663, #26326 ) ;
#71809 = TOROIDAL_SURFACE ( 'NONE', #5077, 11.75000000000000000, 2.125000000000000000 ) ;
#71810 = VECTOR ( 'NONE', #32740, 1000.000000000000000 ) ;
#71811 = CARTESIAN_POINT ( 'NONE',  ( 60.32499999999999574, 82.54999999999999716, 344.4418053999999643 ) ) ;
#71812 = CARTESIAN_POINT ( 'NONE',  ( 98.51953950620418254, -30.85675296092865239, 161.8594347997199918 ) ) ;
#71814 = ORIENTED_EDGE ( 'NONE', *, *, #18304, .F. ) ;
#71813 = CARTESIAN_POINT ( 'NONE',  ( 71.06648329127399677, -18.82844715994099971, 284.9256252759119548 ) ) ;
#71815 = VECTOR ( 'NONE', #13474, 1000.000000000000000 ) ;
#71816 = VECTOR ( 'NONE', #34144, 1000.000000000000000 ) ;
#71817 = CARTESIAN_POINT ( 'NONE',  ( 98.36549455146196408, -40.29075363668730603, 7.635625275910939536 ) ) ;
#71818 = FACE_BOUND ( 'NONE', #34417, .T. ) ;
#71819 = CARTESIAN_POINT ( 'NONE',  ( 103.3797721312301405, -102.7271463785358492, -19.78219314458207378 ) ) ;
#71820 = PLANE ( 'NONE',  #12284 ) ;
#71821 = CARTESIAN_POINT ( 'NONE',  ( 108.4186682723848634, -26.73518572642002411, 29.96909420486912268 ) ) ;
#71822 = CARTESIAN_POINT ( 'NONE',  ( 97.44287158780957725, -40.59272077381807975, 251.6422919425783675 ) ) ;
#71823 = EDGE_LOOP ( 'NONE', ( #77462, #68221, #88699, #25720 ) ) ;
#71824 = ORIENTED_EDGE ( 'NONE', *, *, #88887, .T. ) ;
#71825 = VECTOR ( 'NONE', #51780, 1000.000000000000114 ) ;
#71826 = CARTESIAN_POINT ( 'NONE',  ( 102.0804048320179618, -44.05524405925518039, 193.5330118773259755 ) ) ;
#71827 = DIRECTION ( 'NONE',  ( 0.000000000000000000, -1.000000000000000000, 0.000000000000000000 ) ) ;
#71828 = ADVANCED_FACE ( 'NONE', ( #55686 ), #42969, .T. ) ;
#71829 = CARTESIAN_POINT ( 'NONE',  ( 114.3297541623348224, -29.74979092151301074, 35.86729759161094933 ) ) ;
#71830 = CARTESIAN_POINT ( 'NONE',  ( 23.11215236101587323, 87.06814822297243950, 304.4331722187091032 ) ) ;
#71831 = AXIS2_PLACEMENT_3D ( 'NONE', #77468, #2067, #56565 ) ;
#71832 = CARTESIAN_POINT ( 'NONE',  ( 112.1393456441725931, -28.01282278273417603, 79.65645860901210540 ) ) ;
#71834 = EDGE_CURVE ( 'NONE', #82808, #52812, #69811, .T. ) ;
#71833 = B_SPLINE_CURVE_WITH_KNOTS ( 'NONE', 3,
 ( #37198, #64901, #58076, #85814, #23583, #31257, #12173, #74847, #39857, #53465, #67578, #52570, #66677, #88029, #74395, #4461, #18074, #45322, #68026, #81677, #40310, #80776, #45762, #46211, #73490, #11266, #87137, #38968, #73040, #87580, #46667, #4007, #32596, #25337, #12623, #25794, #66219 ),
 .UNSPECIFIED., .F., .F.,
 ( 4, 2, 2, 1, 2, 2, 2, 1, 1, 2, 2, 2, 2, 1, 2, 2, 2, 1, 1, 1, 2, 4 ),
 ( 0.6666501603261554276, 0.6874845253057836336, 0.6926931165506905463, 0.6979017077955975701, 0.7083188902854107294, 0.7499876202446639217, 0.7525919158671158238, 0.7551962114895677258, 0.7604048027344691985, 0.7708219852242721437, 0.7916563502038780342, 0.8124907151834839247, 0.8176993064283852863, 0.8229078976732865369, 0.8333250801630887050, 0.8749938101222999309, 0.8775981057447522771, 0.8802024013672045122, 0.8854109926121092045, 0.8958281751019185890, 0.9166625400815370250, 1.000000000000000000 ),
 .UNSPECIFIED. ) ;
#71835 = DIRECTION ( 'NONE',  ( 0.000000000000000000, 0.000000000000000000, -1.000000000000000000 ) ) ;
#71836 = ORIENTED_EDGE ( 'NONE', *, *, #51520, .F. ) ;
#71837 = CARTESIAN_POINT ( 'NONE',  ( 172.5664832912729878, -27.82844715994070484, 315.9256252759120116 ) ) ;
#71838 = DIRECTION ( 'NONE',  ( 0.7071067811866516006, -0.7071067811864434338, 0.000000000000000000 ) ) ;
#71839 = CARTESIAN_POINT ( 'NONE',  ( 110.7254274611716056, -26.32387412717027786, 254.8194347997205682 ) ) ;
#71840 = CARTESIAN_POINT ( 'NONE',  ( 11.00055736134227757, 88.91004291464058440, 118.0447018028153394 ) ) ;
#71841 = ORIENTED_EDGE ( 'NONE', *, *, #71092, .F. ) ;
#71842 = EDGE_CURVE ( 'NONE', #39081, #83239, #37444, .T. ) ;
#71843 = EDGE_CURVE ( 'NONE', #89451, #66196, #29299, .T. ) ;
#71844 = CARTESIAN_POINT ( 'NONE',  ( 104.4081006514864924, -46.45808913754018477, 82.36479194178809848 ) ) ;
#71845 = DIRECTION ( 'NONE',  ( 0.000000000000000000, 1.000000000000000000, 0.000000000000000000 ) ) ;
#71846 = DIRECTION ( 'NONE',  ( 0.000000000000000000, 0.000000000000000000, -1.000000000000000000 ) ) ;
#71847 = FACE_BOUND ( 'NONE', #83355, .T. ) ;
#71848 = EDGE_CURVE ( 'NONE', #40542, #45509, #68105, .T. ) ;
#71850 = CARTESIAN_POINT ( 'NONE',  ( 105.5226833586260966, -46.38761039419742360, 33.44991099019595282 ) ) ;
#71849 = PRESENTATION_LAYER_ASSIGNMENT (  '', '', ( #60199 ) ) ;
#71851 = CARTESIAN_POINT ( 'NONE',  ( 19.56670390244796920, -48.82844715994099971, 310.9178068554150514 ) ) ;
#71852 = VERTEX_POINT ( 'NONE', #8864 ) ;
#71853 = CARTESIAN_POINT ( 'NONE',  ( 117.1334281162953346, -32.05460809866745109, 55.16038718067301261 ) ) ;
#71854 = FACE_OUTER_BOUND ( 'NONE', #32307, .T. ) ;
#71855 = ADVANCED_FACE ( 'NONE', ( #30184 ), #22486, .F. ) ;
#71856 = CARTESIAN_POINT ( 'NONE',  ( 96.91416677013903325, -34.20826173260762459, 276.1327681330537871 ) ) ;
#71857 = ORIENTED_EDGE ( 'NONE', *, *, #43102, .F. ) ;
#71858 = CARTESIAN_POINT ( 'NONE',  ( 21.03715912545824551, -47.82818131006186491, 300.4678068554150059 ) ) ;
#71859 = PLANE ( 'NONE',  #22547 ) ;
#71860 = DIRECTION ( 'NONE',  ( 0.000000000000000000, 0.000000000000000000, 1.000000000000000000 ) ) ;
#71861 = ADVANCED_FACE ( 'NONE', ( #29745, #9739 ), #56530, .F. ) ;
#71862 = CARTESIAN_POINT ( 'NONE',  ( 98.42956409136928642, -40.12054696651731689, 94.44237608387695104 ) ) ;
#71863 = CARTESIAN_POINT ( 'NONE',  ( 110.0582552220427175, -26.06480902925029497, 215.8708633711489711 ) ) ;
#71864 = CARTESIAN_POINT ( 'NONE',  ( 182.0374245136140132, -23.42844715993459559, 313.9678068554149490 ) ) ;
#71865 = EDGE_LOOP ( 'NONE', ( #49486, #53951 ) ) ;
#71866 = CARTESIAN_POINT ( 'NONE',  ( 37.03715912545433042, -48.62818131006122258, 249.9678068554150343 ) ) ;
#71867 = ORIENTED_EDGE ( 'NONE', *, *, #51672, .F. ) ;
#71868 = EDGE_LOOP ( 'NONE', ( #89854, #57877, #42695, #68385 ) ) ;
#71869 = CIRCLE ( 'NONE', #89252, 2.117000000000000881 ) ;
#71870 = VECTOR ( 'NONE', #27893, 1000.000000000000000 ) ;
#71871 = DIRECTION ( 'NONE',  ( 0.000000000000000000, -1.000000000000000000, 0.000000000000000000 ) ) ;
#71872 = VECTOR ( 'NONE', #14744, 1000.000000000000000 ) ;
#71873 = ORIENTED_EDGE ( 'NONE', *, *, #59471, .F. ) ;
#71874 = ORIENTED_EDGE ( 'NONE', *, *, #55118, .F. ) ;
#71875 = CARTESIAN_POINT ( 'NONE',  ( 226.4410000000000025, 65.43750000000000000, -63.94449999999999790 ) ) ;
#71876 = AXIS2_PLACEMENT_3D ( 'NONE', #88021, #81671, #24454 ) ;
#71877 = CARTESIAN_POINT ( 'NONE',  ( 115.7741036766735618, -31.77434046802498457, 40.23810575919497978 ) ) ;
#71878 = CARTESIAN_POINT ( 'NONE',  ( 98.57243884988349691, -37.62796858414048273, 125.8324198280769650 ) ) ;
#71879 = CARTESIAN_POINT ( 'NONE',  ( 111.8742750991676758, -46.04467666623092015, 272.9556252759110180 ) ) ;
#71880 = EDGE_CURVE ( 'NONE', #36969, #51954, #89907, .T. ) ;
#71881 = EDGE_CURVE ( 'NONE', #65168, #46193, #71231, .T. ) ;
#71882 = CARTESIAN_POINT ( 'NONE',  ( -2.684158038187649039E-15, 69.84999999999999432, 130.5560000000000116 ) ) ;
#71883 = ORIENTED_EDGE ( 'NONE', *, *, #53660, .T. ) ;
#71884 = ADVANCED_FACE ( 'NONE', ( #50615 ), #78798, .F. ) ;
#71885 = AXIS2_PLACEMENT_3D ( 'NONE', #50338, #9034, #72146 ) ;
#71886 = DIRECTION ( 'NONE',  ( 1.387778780781444492E-15, 0.000000000000000000, -1.000000000000000000 ) ) ;
#71887 = VERTEX_POINT ( 'NONE', #50160 ) ;
#71888 = CARTESIAN_POINT ( 'NONE',  ( 97.81670390244700286, -67.87844715994096134, 222.2178068554179902 ) ) ;
#71889 = ADVANCED_FACE ( 'NONE', ( #8407 ), #71090, .F. ) ;
#71890 = DIRECTION ( 'NONE',  ( -5.773159642023980606E-15, -5.773159642023980170E-30, -1.000000000000000000 ) ) ;
#71891 = DIRECTION ( 'NONE',  ( 1.000000000000000078E-15, -1.000000000000000000, 0.000000000000000000 ) ) ;
#71892 = VECTOR ( 'NONE', #54904, 1000.000000000000000 ) ;
#71893 = DIRECTION ( 'NONE',  ( -3.406823656978775284E-15, 0.000000000000000000, -1.000000000000000000 ) ) ;
#71894 = VERTEX_POINT ( 'NONE', #51060 ) ;
#71895 = CARTESIAN_POINT ( 'NONE',  ( 116.2188219837490522, -41.79507674895632618, 263.4241967044824833 ) ) ;
#71896 = CARTESIAN_POINT ( 'NONE',  ( 118.1291538054787509, -37.63212066291781355, 34.77372051400695341 ) ) ;
#71897 =( NAMED_UNIT ( * ) PLANE_ANGLE_UNIT ( ) SI_UNIT ( $, .RADIAN. ) );
#71898 = CARTESIAN_POINT ( 'NONE',  ( 31.90335556477799628, -33.89581943344391135, -5.074374724088000832 ) ) ;
#71899 = AXIS2_PLACEMENT_3D ( 'NONE', #43731, #51431, #72791 ) ;
#71901 = DIRECTION ( 'NONE',  ( 0.000000000000000000, 0.000000000000000000, -1.000000000000000000 ) ) ;
#71900 = CARTESIAN_POINT ( 'NONE',  ( 0.000000000000000000, 127.0000000000000000, 90.32146847885336172 ) ) ;
#71902 = FACE_OUTER_BOUND ( 'NONE', #37466, .T. ) ;
#71903 = FACE_OUTER_BOUND ( 'NONE', #1979, .T. ) ;
#71904 = CARTESIAN_POINT ( 'NONE',  ( 83.06670390244796920, -61.87844715994100397, 234.8338068554150198 ) ) ;
#71905 = DIRECTION ( 'NONE',  ( 0.000000000000000000, 0.000000000000000000, 1.000000000000000000 ) ) ;
#71906 = CARTESIAN_POINT ( 'NONE',  ( -28.99999999999999289, 172.0000000000000000, 113.8826257785461280 ) ) ;
#71907 = CARTESIAN_POINT ( 'NONE',  ( 168.3664380525667639, -48.62818131005477795, 300.4678068554149490 ) ) ;
#71908 = CARTESIAN_POINT ( 'NONE',  ( 33.96670390244699433, -26.71338133339301635, 342.9256252759119548 ) ) ;
#71909 = CARTESIAN_POINT ( 'NONE',  ( 116.1968789481791191, -43.04691504047773520, 13.35657765686298859 ) ) ;
#71910 = CARTESIAN_POINT ( 'NONE',  ( 98.66592356458792779, -30.49631559909255074, 176.8184824187679567 ) ) ;
#71911 = CARTESIAN_POINT ( 'NONE',  ( 96.90588099414922851, -39.15831928773680914, 52.51276813305394597 ) ) ;
#71913 = CARTESIAN_POINT ( 'NONE',  ( 172.5664832912729878, -27.57844715994070484, 321.9256252759120116 ) ) ;
#71912 = CARTESIAN_POINT ( 'NONE',  ( 83.73314995793998605, 12.92155284005730387, 355.9756252759109998 ) ) ;
#71914 = CARTESIAN_POINT ( 'NONE',  ( 82.16842210270093005, -34.94667169166114462, 2.376609173395129115 ) ) ;
#71915 = CIRCLE ( 'NONE', #67560, 0.5000000000000073275 ) ;
#71916 = VERTEX_POINT ( 'NONE', #16555 ) ;
#71917 = FACE_OUTER_BOUND ( 'NONE', #79822, .T. ) ;
#71918 = ORIENTED_EDGE ( 'NONE', *, *, #51843, .T. ) ;
#71919 = CARTESIAN_POINT ( 'NONE',  ( 116.1466984671187248, -33.09446055034466383, 50.12991099019598096 ) ) ;
#71921 = ORIENTED_EDGE ( 'NONE', *, *, #70286, .T. ) ;
#71920 = CARTESIAN_POINT ( 'NONE',  ( 29.56648329127298069, -71.37844715994266664, 342.9256252759109884 ) ) ;
#71922 = CARTESIAN_POINT ( 'NONE',  ( 161.5667039024469886, -68.37844715994089029, 222.2178068554179902 ) ) ;
#71923 = CARTESIAN_POINT ( 'NONE',  ( 108.6716496925947126, -26.45072611336629720, 185.9527681330539792 ) ) ;
#71924 = LINE ( 'NONE', #44189, #52576 ) ;
#71925 = CARTESIAN_POINT ( 'NONE',  ( 97.86673084626464458, -40.64958532137394087, 146.6470202068057063 ) ) ;
#71926 = CARTESIAN_POINT ( 'NONE',  ( 68.06670390244701707, -86.77844715994098124, 55.21780685541800437 ) ) ;
#71927 = LINE ( 'NONE', #85574, #13711 ) ;
#71928 = CARTESIAN_POINT ( 'NONE',  ( 182.2300522401173168, -33.89581943343755910, 237.4678068554150059 ) ) ;
#71929 = CARTESIAN_POINT ( 'NONE',  ( 108.3313117362001492, -46.73510236842512455, 97.67716632620181372 ) ) ;
#71930 = CARTESIAN_POINT ( 'NONE',  ( 107.3174176841070846, -26.95189801805063823, 120.0556252759109555 ) ) ;
#71931 = EDGE_LOOP ( 'NONE', ( #50749, #40855, #44297, #31491 ) ) ;
#71932 = ORIENTED_EDGE ( 'NONE', *, *, #74991, .F. ) ;
#71933 = VECTOR ( 'NONE', #69924, 1000.000000000000000 ) ;
#71934 = CARTESIAN_POINT ( 'NONE',  ( 98.33263373320089329, -38.22883053613415427, 87.89301187732596077 ) ) ;
#71935 = CIRCLE ( 'NONE', #18231, 16.00000000000000000 ) ;
#71936 = CARTESIAN_POINT ( 'NONE',  ( 115.5439452383992176, -108.5954344580498372, -19.78219314458187839 ) ) ;
#71938 = EDGE_CURVE ( 'NONE', #54510, #74974, #30629, .T. ) ;
#71937 = VECTOR ( 'NONE', #30044, 1000.000000000000000 ) ;
#71940 = CARTESIAN_POINT ( 'NONE',  ( 83.56670390244801183, -36.72944715994108122, 219.5838068554169809 ) ) ;
#71939 = CARTESIAN_POINT ( 'NONE',  ( 99.44473759953889669, -30.59981194223820467, 236.7870538473389388 ) ) ;
#71941 = VECTOR ( 'NONE', #34841, 1000.000000000000000 ) ;
#71942 = CARTESIAN_POINT ( 'NONE',  ( 46.03715912545342093, -48.62818131006090283, 193.9678068554150911 ) ) ;
#71943 = CARTESIAN_POINT ( 'NONE',  ( 116.3212776292293569, -32.94146857471253753, 110.1356252759109822 ) ) ;
#71944 = EDGE_CURVE ( 'NONE', #39083, #40784, #28846, .T. ) ;
#71945 = LINE ( 'NONE', #78773, #1140 ) ;
#71946 = EDGE_CURVE ( 'NONE', #64140, #83074, #22047, .T. ) ;
#71947 = LINE ( 'NONE', #80108, #68130 ) ;
#71948 = CARTESIAN_POINT ( 'NONE',  ( 3.266167974950230146, 70.37369935891477724, 118.5116585762504684 ) ) ;
#71949 = CARTESIAN_POINT ( 'NONE',  ( 108.5866130067098538, -47.05677245125747277, 142.6927681330539883 ) ) ;
#71950 = VERTEX_POINT ( 'NONE', #53264 ) ;
#71951 = ORIENTED_EDGE ( 'NONE', *, *, #57221, .F. ) ;
#71952 = EDGE_CURVE ( 'NONE', #51807, #79449, #87829, .T. ) ;
#71953 = EDGE_CURVE ( 'NONE', #42074, #69327, #17881, .T. ) ;
#71954 = CARTESIAN_POINT ( 'NONE',  ( 165.9667039024459996, -28.27351298637401200, -5.074374724088000832 ) ) ;
#71955 = CARTESIAN_POINT ( 'NONE',  ( 77.45963244950117144, -17.85248396558682416, 2.902015641458085771 ) ) ;
#71956 = DIRECTION ( 'NONE',  ( 0.000000000000000000, -1.000000000000000000, 0.000000000000000000 ) ) ;
#71957 = LINE ( 'NONE', #9723, #71468 ) ;
#71959 = CARTESIAN_POINT ( 'NONE',  ( 102.0474437309886184, -43.16675777147634108, 229.8680903695919540 ) ) ;
#71958 = CONICAL_SURFACE ( 'NONE', #77787, 16.33514202138212923, 0.7853981633974482790 ) ;
#71960 = EDGE_CURVE ( 'NONE', #63602, #83432, #18326, .T. ) ;
#71961 = CARTESIAN_POINT ( 'NONE',  ( 177.0664832912740110, 12.92155284005802685, 335.5992267699913327 ) ) ;
#71962 = AXIS2_PLACEMENT_3D ( 'NONE', #17728, #88564, #11351 ) ;
#71963 = EDGE_CURVE ( 'NONE', #26343, #61899, #33278, .T. ) ;
#71964 = CARTESIAN_POINT ( 'NONE',  ( 117.9487373648833426, -34.79150140969374405, 198.9546728949589749 ) ) ;
#71965 = CYLINDRICAL_SURFACE ( 'NONE', #2496, 3.299999999999999822 ) ;
#71966 = ORIENTED_EDGE ( 'NONE', *, *, #18510, .T. ) ;
#71968 = VERTEX_POINT ( 'NONE', #59208 ) ;
#71967 = VERTEX_POINT ( 'NONE', #18779 ) ;
#71969 = CARTESIAN_POINT ( 'NONE',  ( 117.0679413654940646, -37.57840742081197050, 64.75943071796990580 ) ) ;
#71970 = ORIENTED_EDGE ( 'NONE', *, *, #19617, .T. ) ;
#71971 = CARTESIAN_POINT ( 'NONE',  ( 196.2150000000000034, 30.98800000000000310, 44.45000000000000284 ) ) ;
#71972 = CARTESIAN_POINT ( 'NONE',  ( 49.35211078756945824, -35.65087443489821339, 117.4678068554150485 ) ) ;
#71973 = ADVANCED_FACE ( 'NONE', ( #25591 ), #73935, .F. ) ;
#71974 = CARTESIAN_POINT ( 'NONE',  ( 114.4012193684849734, -41.70236635182605056, 269.7844404487540260 ) ) ;
#71975 = CARTESIAN_POINT ( 'NONE',  ( 140.0667039024470171, -90.27844715994091018, 230.7030882296565721 ) ) ;
#71976 = ORIENTED_EDGE ( 'NONE', *, *, #30359, .F. ) ;
#71977 = CARTESIAN_POINT ( 'NONE',  ( 116.3568090314797132, -39.36905942218098176, 9.635625275910941312 ) ) ;
#71978 = CARTESIAN_POINT ( 'NONE',  ( -126.2750494843262175, 64.71055288310594733, 33.16032879022311164 ) ) ;
#71979 = VERTEX_POINT ( 'NONE', #60091 ) ;
#71980 = ORIENTED_EDGE ( 'NONE', *, *, #39427, .T. ) ;
#71981 = CARTESIAN_POINT ( 'NONE',  ( 108.3335591113261245, -46.73484676085423217, 112.6773436138281141 ) ) ;
#71982 = ORIENTED_EDGE ( 'NONE', *, *, #37508, .T. ) ;
#71983 = ORIENTED_EDGE ( 'NONE', *, *, #27353, .T. ) ;
#71984 = CARTESIAN_POINT ( 'NONE',  ( 115.6248209149117940, -37.18450138507482450, 18.20670554236297889 ) ) ;
#71985 = CARTESIAN_POINT ( 'NONE',  ( 108.0089373620841826, -26.32355773090834816, 155.0041967044819557 ) ) ;
#71986 = CARTESIAN_POINT ( 'NONE',  ( 114.2249171546291677, -45.12625265263336871, 153.1508633711489722 ) ) ;
#71987 = DIRECTION ( 'NONE',  ( 0.000000000000000000, 1.000000000000000000, 0.000000000000000000 ) ) ;
#71988 = CARTESIAN_POINT ( 'NONE',  ( 97.61538875609650745, -41.12936756086440226, 252.6727681330536655 ) ) ;
#71989 = FACE_OUTER_BOUND ( 'NONE', #75263, .T. ) ;
#71990 = CARTESIAN_POINT ( 'NONE',  ( 188.5667039024482392, -48.82844715993431350, 295.7178068554150059 ) ) ;
#71991 = CARTESIAN_POINT ( 'NONE',  ( 107.0664832912748068, -36.72944715993923381, -5.074374724089029343 ) ) ;
#71992 = ORIENTED_EDGE ( 'NONE', *, *, #56339, .F. ) ;
#71993 = EDGE_CURVE ( 'NONE', #71968, #74301, #73288, .T. ) ;
#71994 = VERTEX_POINT ( 'NONE', #31061 ) ;
#71995 = EDGE_CURVE ( 'NONE', #34216, #34233, #10075, .T. ) ;
#71996 = CIRCLE ( 'NONE', #22668, 2.500000000000002220 ) ;
#71998 = CARTESIAN_POINT ( 'NONE',  ( 109.6166107820099569, -26.53883167775938645, 199.8813395616249977 ) ) ;
#71997 = AXIS2_PLACEMENT_3D ( 'NONE', #14588, #44387, #65299 ) ;
#71999 = ORIENTED_EDGE ( 'NONE', *, *, #70938, .T. ) ;
#72000 = CIRCLE ( 'NONE', #19793, 2.030000000000003801 ) ;
#72001 = CARTESIAN_POINT ( 'NONE',  ( 114.3440588962603215, -29.21527388614784115, 174.4641967044819637 ) ) ;
#72002 = DIRECTION ( 'NONE',  ( 0.9825752044328148749, 0.1858654557302456822, 0.000000000000000000 ) ) ;
#72003 = B_SPLINE_CURVE_WITH_KNOTS ( 'NONE', 3,
 ( #28508, #818, #56202, #69864, #63947, #7634, #57106, #69417, #29880, #84852, #49845, #36693, #367, #22619, #35775, #50755, #64393, #70308, #22177, #50294, #57562, #83953, #34882, #21264, #21724 ),
 .UNSPECIFIED., .F., .F.,
 ( 4, 2, 2, 2, 2, 2, 2, 2, 2, 1, 2, 2, 4 ),
 ( 0.05913645768019770710, 0.06159852758862928435, 0.06282956254284507991, 0.06406059749706087547, 0.06652266740549245272, 0.06775370235970824828, 0.06898473731392402997, 0.07144680722235557946, 0.07267784217657137502, 0.07390887713078717058, 0.07513991208500296615, 0.07637094703921876171, 0.07883301694765033896 ),
 .UNSPECIFIED. ) ;
#72004 = CARTESIAN_POINT ( 'NONE',  ( 136.1934021726305275, -34.98608769072284730, 7.448832051633326401 ) ) ;
#72005 = DIRECTION ( 'NONE',  ( 0.000000000000000000, 0.000000000000000000, -1.000000000000000000 ) ) ;
#72008 = CARTESIAN_POINT ( 'NONE',  ( 115.3963619165045458, -41.85549553236474196, 14.38705384733895976 ) ) ;
#72007 = LINE ( 'NONE', #3404, #13710 ) ;
#72006 = PLANE ( 'NONE',  #17387 ) ;
#72009 = DIRECTION ( 'NONE',  ( 0.000000000000000000, 0.000000000000000000, -1.000000000000000000 ) ) ;
#72010 = CARTESIAN_POINT ( 'NONE',  ( 80.06648329127402519, -36.72944715994107412, -5.074374724089057764 ) ) ;
#72011 = DIRECTION ( 'NONE',  ( -1.000000000000000000, 0.000000000000000000, -3.491481338843133355E-15 ) ) ;
#72012 = CARTESIAN_POINT ( 'NONE',  ( 67.53185150639035328, -137.4071337290076826, 246.7901045206692459 ) ) ;
#72013 = CARTESIAN_POINT ( 'NONE',  ( 104.4899544351757612, -26.97880758891392006, 256.2814586106100592 ) ) ;
#72014 = CARTESIAN_POINT ( 'NONE',  ( 131.0667039024480403, -42.21678055153905262, 207.5838068554170377 ) ) ;
#72016 = VERTEX_POINT ( 'NONE', #86940 ) ;
#72015 = CARTESIAN_POINT ( 'NONE',  ( 115.2539372359732255, -38.22674572785330582, 195.5838068554167251 ) ) ;
#72017 = CARTESIAN_POINT ( 'NONE',  ( 126.8164832912740110, -54.62589567669621005, 14.92562527591099020 ) ) ;
#72018 = CARTESIAN_POINT ( 'NONE',  ( 102.6741928909662391, -27.25030431863982372, 180.4213395616249898 ) ) ;
#72019 = CARTESIAN_POINT ( 'NONE',  ( 118.8426969166518319, -35.40452897077508965, 79.91562527591095488 ) ) ;
#72020 = CARTESIAN_POINT ( 'NONE',  ( 98.39890672360048995, -29.79614961819730468, 191.7775300378159784 ) ) ;
#72021 = DIRECTION ( 'NONE',  ( 1.000000000000000000, 0.000000000000000000, 0.000000000000000000 ) ) ;
#72022 = DIRECTION ( 'NONE',  ( 0.2884130866282236250, 0.7071067811865507924, -0.6456143519637524975 ) ) ;
#72023 = VECTOR ( 'NONE', #74208, 1000.000000000000000 ) ;
#72025 = CARTESIAN_POINT ( 'NONE',  ( 112.2334563547038755, -45.33745837553901481, 39.00654346520547477 ) ) ;
#72024 = DIRECTION ( 'NONE',  ( 3.100000000000000258E-29, -3.100000000000000044E-14, -1.000000000000000000 ) ) ;
#72026 = CARTESIAN_POINT ( 'NONE',  ( 126.8164832912739826, -36.72944715994101017, 14.92562527591099020 ) ) ;
#72027 = DIRECTION ( 'NONE',  ( 1.000000000000000078E-15, -1.000000000000000083E-30, -1.000000000000000000 ) ) ;
#72028 = ORIENTED_EDGE ( 'NONE', *, *, #37246, .F. ) ;
#72029 = CARTESIAN_POINT ( 'NONE',  ( 181.5667039024459939, -18.82844715994031048, -5.074374724088000832 ) ) ;
#72030 = ORIENTED_EDGE ( 'NONE', *, *, #44285, .T. ) ;
#72031 = EDGE_LOOP ( 'NONE', ( #19343, #45119 ) ) ;
#72032 = CARTESIAN_POINT ( 'NONE',  ( 112.7360809596688966, -29.66769577629168353, 118.9486103042669782 ) ) ;
#72034 = VERTEX_POINT ( 'NONE', #46463 ) ;
#72033 = CARTESIAN_POINT ( 'NONE',  ( -6.349842397765894653, 93.55646220832403515, -130.4020064843512614 ) ) ;
#72035 = CARTESIAN_POINT ( 'NONE',  ( 98.11562048848820439, -31.42749274529986536, 81.90133956162493689 ) ) ;
#72036 = LINE ( 'NONE', #30692, #6257 ) ;
#72037 = CARTESIAN_POINT ( 'NONE',  ( 77.53592152231050250, -17.65293368212969227, 7.043713522541727556 ) ) ;
#72038 = DIRECTION ( 'NONE',  ( 1.000000000000000000, 0.000000000000000000, 9.462128050782575008E-16 ) ) ;
#72039 = CARTESIAN_POINT ( 'NONE',  ( 111.0600676157742726, -27.80113716294804505, 24.74133956162494030 ) ) ;
#72040 = EDGE_LOOP ( 'NONE', ( #413, #4443, #15731, #73967 ) ) ;
#72041 = EDGE_CURVE ( 'NONE', #48350, #83417, #72418, .T. ) ;
#72042 = ORIENTED_EDGE ( 'NONE', *, *, #31975, .F. ) ;
#72043 = ORIENTED_EDGE ( 'NONE', *, *, #28543, .F. ) ;
#72044 = CARTESIAN_POINT ( 'NONE',  ( 50.96943157743499597, -34.03355364505720360, -5.074374724088000832 ) ) ;
#72045 = CARTESIAN_POINT ( 'NONE',  ( -135.1318726873890341, 20.32000000000000028, 118.7423475625884066 ) ) ;
#72046 = DIRECTION ( 'NONE',  ( 0.000000000000000000, 0.000000000000000000, -1.000000000000000000 ) ) ;
#72047 = DIRECTION ( 'NONE',  ( 0.000000000000000000, 0.000000000000000000, 1.000000000000000000 ) ) ;
#72048 = CARTESIAN_POINT ( 'NONE',  ( -21.42842094847162926, 53.97499999999997300, 41.97446389704172987 ) ) ;
#72049 = EDGE_CURVE ( 'NONE', #60012, #11178, #24703, .T. ) ;
#72050 = CARTESIAN_POINT ( 'NONE',  ( 115.0895152844205143, -30.61842842605814496, 50.34448410232288040 ) ) ;
#72051 = EDGE_CURVE ( 'NONE', #4843, #37315, #3372, .T. ) ;
#72052 = CARTESIAN_POINT ( 'NONE',  ( 45.77381068363443006, -48.62134037875091508, 180.4678068554150911 ) ) ;
#72053 = EDGE_CURVE ( 'NONE', #13427, #4391, #76852, .T. ) ;
#72054 = CARTESIAN_POINT ( 'NONE',  ( -7.057748139868313508, 93.10832354271467182, 130.3650924429668407 ) ) ;
#72055 = CARTESIAN_POINT ( 'NONE',  ( 97.82856912889580769, -29.34641599088746133, 45.78991099019697231 ) ) ;
#72056 = ORIENTED_EDGE ( 'NONE', *, *, #71842, .F. ) ;
#72057 = EDGE_CURVE ( 'NONE', #42074, #59810, #81224, .T. ) ;
#72058 = PLANE ( 'NONE',  #60370 ) ;
#72059 = LINE ( 'NONE', #3458, #76534 ) ;
#72060 = AXIS2_PLACEMENT_3D ( 'NONE', #39767, #66131, #40214 ) ;
#72061 = FACE_OUTER_BOUND ( 'NONE', #1099, .T. ) ;
#72062 = CARTESIAN_POINT ( 'NONE',  ( 113.0492235774716363, -42.98306560958572931, 110.9899951314959594 ) ) ;
#72063 = EDGE_CURVE ( 'NONE', #42164, #37640, #53604, .T. ) ;
#72064 = CIRCLE ( 'NONE', #54633, 0.5000000000000004441 ) ;
#72065 = STYLED_ITEM ( 'NONE', ( #23704 ), #50495 ) ;
#72066 = CIRCLE ( 'NONE', #38711, 1.000000000000000888 ) ;
#72067 = CARTESIAN_POINT ( 'NONE',  ( 97.79840183623460348, -40.48482318767148769, 96.63282328633124507 ) ) ;
#72068 = EDGE_CURVE ( 'NONE', #74492, #82359, #74200, .T. ) ;
#72069 = DIRECTION ( 'NONE',  ( 0.000000000000000000, 0.000000000000000000, 1.000000000000000000 ) ) ;
#72070 = ORIENTED_EDGE ( 'NONE', *, *, #17692, .T. ) ;
#72071 = ORIENTED_EDGE ( 'NONE', *, *, #45261, .F. ) ;
#72072 = DIRECTION ( 'NONE',  ( -0.9130365726098600421, 0.000000000000000000, -0.4078776986755215939 ) ) ;
#72073 = ORIENTED_EDGE ( 'NONE', *, *, #46201, .T. ) ;
#72074 = ORIENTED_EDGE ( 'NONE', *, *, #12159, .F. ) ;
#72075 = EDGE_CURVE ( 'NONE', #17322, #45997, #17445, .T. ) ;
#72076 = CARTESIAN_POINT ( 'NONE',  ( 104.9381124493903457, -46.57529615900893560, 178.8387261630399507 ) ) ;
#72077 = CARTESIAN_POINT ( 'NONE',  ( 85.06670390244701707, -80.35669973212957018, 55.21780685541800437 ) ) ;
#72078 = VECTOR ( 'NONE', #50862, 1000.000000000000000 ) ;
#72079 = CARTESIAN_POINT ( 'NONE',  ( 97.77490566832175034, -42.75910828249967466, 142.7965776568629508 ) ) ;
#72080 = CARTESIAN_POINT ( 'NONE',  ( 0.000000000000000000, 238.5000000000000000, 154.6557476874258441 ) ) ;
#72081 = CARTESIAN_POINT ( 'NONE',  ( 100.8874678619102241, -44.70022135782634365, 83.05229194033439910 ) ) ;
#72082 = VERTEX_POINT ( 'NONE', #11523 ) ;
#72083 = ORIENTED_EDGE ( 'NONE', *, *, #46466, .F. ) ;
#72084 = ORIENTED_EDGE ( 'NONE', *, *, #9001, .F. ) ;
#72085 = CARTESIAN_POINT ( 'NONE',  ( 107.9397346479727418, -44.84530559174715592, 200.4795189410199612 ) ) ;
#72086 = CARTESIAN_POINT ( 'NONE',  ( 118.8678016624199358, -35.40170448615204890, 83.91562527591095488 ) ) ;
#72087 = VERTEX_POINT ( 'NONE', #59649 ) ;
#72088 = CARTESIAN_POINT ( 'NONE',  ( 96.20032699425225076, -38.62430069186631698, 46.45181575210094138 ) ) ;
#72089 = CARTESIAN_POINT ( 'NONE',  ( 111.7740190377046758, -28.54012605827362137, 249.5838068554168956 ) ) ;
#72090 = CARTESIAN_POINT ( 'NONE',  ( 107.0664832912739968, -18.82844715994099971, 168.9256252759119832 ) ) ;
#72091 = DIRECTION ( 'NONE',  ( -4.299999999999999979E-14, 1.000000000000000000, 0.000000000000000000 ) ) ;
#72092 = CARTESIAN_POINT ( 'NONE',  ( 114.5275249938671465, -28.57771476791114296, 150.4746728949579619 ) ) ;
#72093 = FACE_OUTER_BOUND ( 'NONE', #82378, .T. ) ;
#72094 = EDGE_LOOP ( 'NONE', ( #21508, #57039 ) ) ;
#72095 = DIRECTION ( 'NONE',  ( 0.000000000000000000, 1.000000000000000000, 0.000000000000000000 ) ) ;
#72096 = EDGE_LOOP ( 'NONE', ( #68842, #84337, #70617, #59041 ) ) ;
#72097 = CARTESIAN_POINT ( 'NONE',  ( 68.53801554307389665, 127.0000000000000000, 74.15067561874289481 ) ) ;
#72098 = DIRECTION ( 'NONE',  ( 0.000000000000000000, 0.000000000000000000, 1.000000000000000000 ) ) ;
#72099 = ADVANCED_FACE ( 'NONE', ( #52801 ), #80575, .T. ) ;
#72100 = VERTEX_POINT ( 'NONE', #3812 ) ;
#72101 = VECTOR ( 'NONE', #20403, 1000.000000000000000 ) ;
#72102 = FACE_OUTER_BOUND ( 'NONE', #79409, .T. ) ;
#72103 = CARTESIAN_POINT ( 'NONE',  ( 97.43481369731881614, -33.83398838518805007, 132.0936288413114141 ) ) ;
#72104 = CARTESIAN_POINT ( 'NONE',  ( 103.4771249150381749, -25.43533399052049049, 55.32133956162594046 ) ) ;
#72105 = CARTESIAN_POINT ( 'NONE',  ( 22.34055959819741233, 59.35018981749909983, 30.86443047836608855 ) ) ;
#72106 = DIRECTION ( 'NONE',  ( 0.000000000000000000, 0.000000000000000000, 1.000000000000000000 ) ) ;
#72107 = CARTESIAN_POINT ( 'NONE',  ( 112.0659116278142164, -45.48839625744306403, 73.98979194306805596 ) ) ;
#72108 = CARTESIAN_POINT ( 'NONE',  ( 116.6363502066643321, -38.74961609181406175, 63.66133956162595098 ) ) ;
#72110 = CARTESIAN_POINT ( 'NONE',  ( 117.0023065291008066, -39.93004192841230804, 154.5784824187679476 ) ) ;
#72109 = DIRECTION ( 'NONE',  ( 0.000000000000000000, 0.000000000000000000, 1.000000000000000000 ) ) ;
#72111 = FACE_OUTER_BOUND ( 'NONE', #16711, .T. ) ;
#72112 = DIRECTION ( 'NONE',  ( -1.000000000000000000, 0.000000000000000000, 2.170915417798913171E-16 ) ) ;
#72113 = EDGE_LOOP ( 'NONE', ( #20304, #24793, #69734, #10780 ) ) ;
#72114 = LINE ( 'NONE', #30336, #42521 ) ;
#72115 = CARTESIAN_POINT ( 'NONE',  ( 22.49541547940852126, 22.69262065192448574, 328.6381252759109088 ) ) ;
#72116 = CARTESIAN_POINT ( 'NONE',  ( 77.74851419028676958, -134.1785091737438051, 248.4142799812389910 ) ) ;
#72117 = FACE_OUTER_BOUND ( 'NONE', #46489, .T. ) ;
#72118 = EDGE_CURVE ( 'NONE', #85626, #79928, #66930, .T. ) ;
#72120 = ORIENTED_EDGE ( 'NONE', *, *, #48527, .T. ) ;
#72119 = CARTESIAN_POINT ( 'NONE',  ( 117.2401079361024898, -34.25881411750412298, 209.0156252759109634 ) ) ;
#72121 = CIRCLE ( 'NONE', #56138, 9.999999999999998224 ) ;
#72122 = CARTESIAN_POINT ( 'NONE',  ( 97.80799470936521800, -40.50839083839967714, 146.6348481252984755 ) ) ;
#72123 = CARTESIAN_POINT ( 'NONE',  ( 96.22678813199759418, -34.45212096497557042, 257.1737205140064475 ) ) ;
#72124 = CARTESIAN_POINT ( 'NONE',  ( 104.2021517265174992, -25.17926459036136322, 86.26991099019699050 ) ) ;
#72125 = VECTOR ( 'NONE', #80421, 1000.000000000000000 ) ;
#72126 = CARTESIAN_POINT ( 'NONE',  ( 97.81399931465544739, -40.51646775427786196, 252.6355816051047896 ) ) ;
#72127 = CARTESIAN_POINT ( 'NONE',  ( 63.03715912545646205, -24.42818131006026761, 116.4678068554151054 ) ) ;
#72128 = DIRECTION ( 'NONE',  ( 1.000000000000000078E-15, -1.000000000000000000, 0.000000000000000000 ) ) ;
#72129 = CARTESIAN_POINT ( 'NONE',  ( 117.0720556136961648, -35.46381013733837051, 264.9274461759231372 ) ) ;
#72130 = ORIENTED_EDGE ( 'NONE', *, *, #24152, .F. ) ;
#72131 = ADVANCED_FACE ( 'NONE', ( #69622 ), #52182, .T. ) ;
#72132 = VECTOR ( 'NONE', #66402, 1000.000000000000000 ) ;
#72133 = VECTOR ( 'NONE', #4917, 1000.000000000000000 ) ;
#72134 = AXIS2_PLACEMENT_3D ( 'NONE', #65135, #84711, #78345 ) ;
#72135 = ORIENTED_EDGE ( 'NONE', *, *, #61993, .T. ) ;
#72136 = ORIENTED_EDGE ( 'NONE', *, *, #7082, .F. ) ;
#72137 = VERTEX_POINT ( 'NONE', #12877 ) ;
#72138 = DIRECTION ( 'NONE',  ( 0.000000000000000000, 1.000000000000000000, 0.000000000000000000 ) ) ;
#72139 = CARTESIAN_POINT ( 'NONE',  ( 111.4803918977840169, -26.59589994751270936, 280.7375300378156453 ) ) ;
#72140 = DIRECTION ( 'NONE',  ( 0.8571673007021115565, -0.5150380749100554878, 7.521945815882500121E-16 ) ) ;
#72141 = DIRECTION ( 'NONE',  ( 0.000000000000000000, 0.000000000000000000, -1.000000000000000000 ) ) ;
#72142 = AXIS2_PLACEMENT_3D ( 'NONE', #48483, #69419, #34434 ) ;
#72143 = VECTOR ( 'NONE', #84693, 1000.000000000000114 ) ;
#72145 = CARTESIAN_POINT ( 'NONE',  ( 87.71317827224373787, 71.15456258041355397, 79.76251016565973373 ) ) ;
#72144 = DIRECTION ( 'NONE',  ( 1.000000000000000078E-15, -1.000000000000000000, 0.000000000000000000 ) ) ;
#72146 = DIRECTION ( 'NONE',  ( 0.000000000000000000, 0.000000000000000000, -1.000000000000000000 ) ) ;
#72147 = TOROIDAL_SURFACE ( 'NONE', #40212, 15.69999999999999929, 0.2999999999999999889 ) ;
#72148 = CARTESIAN_POINT ( 'NONE',  ( 113.5483862797134549, -30.40508126489656604, 193.8762293518859678 ) ) ;
#72149 = VERTEX_POINT ( 'NONE', #40105 ) ;
#72150 = ORIENTED_EDGE ( 'NONE', *, *, #60276, .F. ) ;
#72151 = ORIENTED_EDGE ( 'NONE', *, *, #25161, .F. ) ;
#72152 = FACE_OUTER_BOUND ( 'NONE', #19848, .T. ) ;
#72153 = CARTESIAN_POINT ( 'NONE',  ( 48.45959712127140051, -26.00627455219179751, 193.9678068554150911 ) ) ;
#72154 = CARTESIAN_POINT ( 'NONE',  ( 96.91794407517411969, -34.59732685048010126, 257.1737205140059928 ) ) ;
#72155 = EDGE_CURVE ( 'NONE', #77070, #5714, #67822, .T. ) ;
#72156 = CARTESIAN_POINT ( 'NONE',  ( 172.5667039024478129, -36.32844715993500273, 300.4678068554149490 ) ) ;
#72157 = EDGE_CURVE ( 'NONE', #34504, #43897, #54608, .T. ) ;
#72158 = FACE_OUTER_BOUND ( 'NONE', #63349, .T. ) ;
#72159 = DIRECTION ( 'NONE',  ( 0.000000000000000000, 0.000000000000000000, -1.000000000000000000 ) ) ;
#72160 = VERTEX_POINT ( 'NONE', #13316 ) ;
#72161 = EDGE_CURVE ( 'NONE', #18505, #69050, #565, .T. ) ;
#72162 = CARTESIAN_POINT ( 'NONE',  ( 78.82300719538731926, -34.27587548317108457, 1.868342134763057549 ) ) ;
#72163 = ORIENTED_EDGE ( 'NONE', *, *, #75229, .F. ) ;
#72164 = DIRECTION ( 'NONE',  ( 9.351236661543306751E-17, -3.725950533538267725E-29, -1.000000000000000000 ) ) ;
#72165 = CARTESIAN_POINT ( 'NONE',  ( 106.4288663150950214, -28.56390168778064975, 22.95666179816197072 ) ) ;
#72166 = VECTOR ( 'NONE', #10666, 1000.000000000000000 ) ;
#72167 = DIRECTION ( 'NONE',  ( 0.000000000000000000, 0.000000000000000000, -1.000000000000000000 ) ) ;
#72168 = CARTESIAN_POINT ( 'NONE',  ( 0.000000000000000000, 125.4759999999999991, 0.000000000000000000 ) ) ;
#72169 = ADVANCED_FACE ( 'NONE', ( #40562 ), #6941, .T. ) ;
#72170 = CARTESIAN_POINT ( 'NONE',  ( 91.72954497613136482, 77.68452076096559722, -75.10852726169345317 ) ) ;
#72171 = VERTEX_POINT ( 'NONE', #41002 ) ;
#72172 = PLANE ( 'NONE',  #65341 ) ;
#72173 = DIRECTION ( 'NONE',  ( 1.000000000000000000, 0.000000000000000000, 0.000000000000000000 ) ) ;
#72174 = ORIENTED_EDGE ( 'NONE', *, *, #76847, .F. ) ;
#72175 = CARTESIAN_POINT ( 'NONE',  ( 115.2074362016368099, -44.20634311780637660, 78.22324432352995416 ) ) ;
#72176 = ORIENTED_EDGE ( 'NONE', *, *, #25532, .F. ) ;
#72177 = CARTESIAN_POINT ( 'NONE',  ( 101.6136182267745056, -30.15507309768812050, 40.04956268521897300 ) ) ;
#72178 = CARTESIAN_POINT ( 'NONE',  ( 114.6397582406955422, -43.29253298239483172, 89.25751118873346002 ) ) ;
#72179 = CARTESIAN_POINT ( 'NONE',  ( 109.2913206311583707, -45.85778897805103327, 84.18634521065892784 ) ) ;
#72180 = CARTESIAN_POINT ( 'NONE',  ( 109.6420608605809406, -46.48032619938765464, 13.78138133162124568 ) ) ;
#72181 = CARTESIAN_POINT ( 'NONE',  ( 100.8961411191535973, 120.6499999999999915, -3.968749999999580336 ) ) ;
#72182 = CIRCLE ( 'NONE', #33008, 13.44999999999999396 ) ;
#72183 = DIRECTION ( 'NONE',  ( 1.000000000000000000, 0.000000000000000000, 0.000000000000000000 ) ) ;
#72184 = CARTESIAN_POINT ( 'NONE',  ( 101.5975885682485398, -47.27054607199826819, 13.19562527591094891 ) ) ;
#72185 = DIRECTION ( 'NONE',  ( 0.000000000000000000, 0.000000000000000000, 1.000000000000000000 ) ) ;
#72186 = ORIENTED_EDGE ( 'NONE', *, *, #17626, .T. ) ;
#72187 = DIRECTION ( 'NONE',  ( 0.9825752044328147639, 0.1858654557302462929, 0.000000000000000000 ) ) ;
#72188 = AXIS2_PLACEMENT_3D ( 'NONE', #10896, #66300, #72245 ) ;
#72189 = VERTEX_POINT ( 'NONE', #46908 ) ;
#72190 = CARTESIAN_POINT ( 'NONE',  ( 114.2834173682332732, -44.31288860877327807, 154.1813395616249807 ) ) ;
#72191 = AXIS2_PLACEMENT_3D ( 'NONE', #63313, #71039, #29248 ) ;
#72192 = CYLINDRICAL_SURFACE ( 'NONE', #56967, 9.524999999999998579 ) ;
#72193 = EDGE_LOOP ( 'NONE', ( #4978, #67910, #76518, #61610 ) ) ;
#72194 = VERTEX_POINT ( 'NONE', #33751 ) ;
#72195 = CARTESIAN_POINT ( 'NONE',  ( 33.91903122894598965, -35.91149509761181235, -5.074374724088000832 ) ) ;
#72196 = CIRCLE ( 'NONE', #40481, 2.117000000000000881 ) ;
#72197 = CARTESIAN_POINT ( 'NONE',  ( 25.56670390244797275, -65.37844715994100397, 298.0928068554150627 ) ) ;
#72198 = CARTESIAN_POINT ( 'NONE',  ( 117.1144258088630750, -31.97015794161411861, 214.1784824187679419 ) ) ;
#72199 = DIRECTION ( 'NONE',  ( 0.000000000000000000, 1.000000000000000000, 0.000000000000000000 ) ) ;
#72200 = CYLINDRICAL_SURFACE ( 'NONE', #8955, 2.116999999999993776 ) ;
#72201 = DIRECTION ( 'NONE',  ( 4.194175870806139918E-14, -1.000000000000000000, 0.000000000000000000 ) ) ;
#72202 = CARTESIAN_POINT ( 'NONE',  ( 96.83360046493686468, -38.89957200400883863, 27.49276813305395706 ) ) ;
#72203 = DIRECTION ( 'NONE',  ( -1.000000000000000078E-15, 1.000000000000000000, 0.000000000000000000 ) ) ;
#72204 = ORIENTED_EDGE ( 'NONE', *, *, #12811, .F. ) ;
#72205 = AXIS2_PLACEMENT_3D ( 'NONE', #85309, #50757, #38025 ) ;
#72206 = CARTESIAN_POINT ( 'NONE',  ( 97.33770338515772380, -34.07162276509023258, 172.1147621535543806 ) ) ;
#72207 = VECTOR ( 'NONE', #61416, 1000.000000000000000 ) ;
#72208 = CIRCLE ( 'NONE', #21501, 30.99999999999998579 ) ;
#72209 = DIRECTION ( 'NONE',  ( 0.000000000000000000, 0.000000000000000000, 1.000000000000000000 ) ) ;
#72210 = EDGE_CURVE ( 'NONE', #65745, #58445, #75433, .T. ) ;
#72211 = ORIENTED_EDGE ( 'NONE', *, *, #7131, .T. ) ;
#72212 = VECTOR ( 'NONE', #4448, 1000.000000000000000 ) ;
#72213 = DIRECTION ( 'NONE',  ( 0.000000000000000000, -0.8660254037844387076, -0.4999999999999998890 ) ) ;
#72214 = LINE ( 'NONE', #38561, #54173 ) ;
#72215 = CARTESIAN_POINT ( 'NONE',  ( 95.31970492887376167, -38.09378048407036488, 236.4184824187679510 ) ) ;
#72216 = EDGE_CURVE ( 'NONE', #27685, #39084, #24648, .T. ) ;
#72217 = FACE_OUTER_BOUND ( 'NONE', #51731, .T. ) ;
#72218 = PLANE ( 'NONE',  #57713 ) ;
#72219 = CARTESIAN_POINT ( 'NONE',  ( 115.8412394166662835, -32.57321297090945933, 213.6009912566489675 ) ) ;
#72221 = CARTESIAN_POINT ( 'NONE',  ( 107.6057229598026197, -48.54288983744045538, 38.61276813305397582 ) ) ;
#72220 = DIRECTION ( 'NONE',  ( -0.000000000000000000, 1.000000000000000000, 0.000000000000000000 ) ) ;
#72222 = CARTESIAN_POINT ( 'NONE',  ( 121.8942133281728957, 74.21437598052153817, 46.76216900032968482 ) ) ;
#72223 = CARTESIAN_POINT ( 'NONE',  ( 114.1106629025095458, -44.52247787522302502, 133.1613395616249989 ) ) ;
#72224 = ORIENTED_EDGE ( 'NONE', *, *, #37615, .T. ) ;
#72225 = CARTESIAN_POINT ( 'NONE',  ( 25.56670390244797275, -58.35344715994099829, 254.4678068554150343 ) ) ;
#72226 = VERTEX_POINT ( 'NONE', #89171 ) ;
#72227 = DIRECTION ( 'NONE',  ( 2.108231265501709878E-16, 0.000000000000000000, -1.000000000000000000 ) ) ;
#72228 = CARTESIAN_POINT ( 'NONE',  ( 72.31648329127401098, -45.72944715994106701, 14.92562527591093691 ) ) ;
#72229 = CARTESIAN_POINT ( 'NONE',  ( 108.6469982457124104, -26.82183733066701237, 275.9507284248297765 ) ) ;
#72230 = ORIENTED_EDGE ( 'NONE', *, *, #19235, .T. ) ;
#72231 = DIRECTION ( 'NONE',  ( 0.000000000000000000, 0.000000000000000000, 1.000000000000000000 ) ) ;
#72232 = VERTEX_POINT ( 'NONE', #6488 ) ;
#72233 = LINE ( 'NONE', #17268, #84335 ) ;
#72234 = DIRECTION ( 'NONE',  ( 0.000000000000000000, 0.000000000000000000, -1.000000000000000000 ) ) ;
#72235 = AXIS2_PLACEMENT_3D ( 'NONE', #56006, #70569, #56467 ) ;
#72236 = CARTESIAN_POINT ( 'NONE',  ( 88.17226027475707895, -14.72944715994102616, 249.5838068554175777 ) ) ;
#72237 = ORIENTED_EDGE ( 'NONE', *, *, #12167, .F. ) ;
#72238 = EDGE_CURVE ( 'NONE', #21668, #71852, #68722, .T. ) ;
#72239 = CARTESIAN_POINT ( 'NONE',  ( 110.1645224859485808, -46.70684747839494833, 97.81562527591097478 ) ) ;
#72240 = DIRECTION ( 'NONE',  ( 0.000000000000000000, 0.000000000000000000, 1.000000000000000000 ) ) ;
#72241 = CARTESIAN_POINT ( 'NONE',  ( 97.12558202918494032, -37.99705770278674066, 166.4273231845742487 ) ) ;
#72242 = DIRECTION ( 'NONE',  ( 1.000000000000000000, 4.163336342344333240E-14, 0.000000000000000000 ) ) ;
#72243 = CARTESIAN_POINT ( 'NONE',  ( 97.81169952324414396, -40.51743120087827776, 141.6355106266202313 ) ) ;
#72244 = VERTEX_POINT ( 'NONE', #69171 ) ;
#72245 = DIRECTION ( 'NONE',  ( 1.000000000000000000, 0.000000000000000000, 0.000000000000000000 ) ) ;
#72246 = DIRECTION ( 'NONE',  ( 1.075267683398002218E-15, -1.000000000000000000, 3.100000000000000044E-14 ) ) ;
#72247 = LINE ( 'NONE', #79071, #34201 ) ;
#72248 = ORIENTED_CLOSED_SHELL ( 'NONE', *, #1014, .F. );
#72249 = AXIS2_PLACEMENT_3D ( 'NONE', #73539, #65824, #17252 ) ;
#72251 = CARTESIAN_POINT ( 'NONE',  ( 67.06670390244707392, -137.6773508471079595, 245.4788304630789924 ) ) ;
#72250 = CARTESIAN_POINT ( 'NONE',  ( 3.174999999999889688, 104.3431970271541900, 31.75000000000000000 ) ) ;
#72252 = DIRECTION ( 'NONE',  ( 0.000000000000000000, 0.000000000000000000, 1.000000000000000000 ) ) ;
#72253 = VECTOR ( 'NONE', #27437, 999.9999999999998863 ) ;
#72254 = ORIENTED_EDGE ( 'NONE', *, *, #77607, .F. ) ;
#72255 = VECTOR ( 'NONE', #50429, 1000.000000000000000 ) ;
#72256 =( BOUNDED_CURVE ( )  B_SPLINE_CURVE ( 3, ( #25373, #9976, #37681, #46241 ),
 .UNSPECIFIED., .F., .T. ) 
 B_SPLINE_CURVE_WITH_KNOTS ( ( 4, 4 ),
 ( 2.671434693666588700, 3.141592653589793116 ),
 .UNSPECIFIED. ) 
 CURVE ( )  GEOMETRIC_REPRESENTATION_ITEM ( )  RATIONAL_B_SPLINE_CURVE ( ( 1.000000000000000000, 0.9816639655796102204, 0.9816639655796102204, 1.000000000000000000 ) ) 
 REPRESENTATION_ITEM ( '' )  );
#72257 = CARTESIAN_POINT ( 'NONE',  ( 164.9190312289449878, -35.91149509761181235, 117.4678068554150627 ) ) ;
#72258 = CARTESIAN_POINT ( 'NONE',  ( 97.98063455390173715, -41.72806076336409120, 172.7146728949579710 ) ) ;
#72259 = ADVANCED_FACE ( 'NONE', ( #5613 ), #33305, .F. ) ;
#72261 = ORIENTED_EDGE ( 'NONE', *, *, #66836, .F. ) ;
#72260 = LINE ( 'NONE', #64106, #8081 ) ;
#72262 = VECTOR ( 'NONE', #33626, 1000.000000000000000 ) ;
#72263 = CARTESIAN_POINT ( 'NONE',  ( 106.6352542858682284, -26.36832623700844280, 36.09753003781596448 ) ) ;
#72264 = LINE ( 'NONE', #1880, #65764 ) ;
#72265 = LINE ( 'NONE', #30918, #69011 ) ;
#72266 = EDGE_CURVE ( 'NONE', #28799, #6003, #29012, .T. ) ;
#72267 = LINE ( 'NONE', #30479, #18107 ) ;
#72268 = AXIS2_PLACEMENT_3D ( 'NONE', #75274, #34367, #82996 ) ;
#72269 = ORIENTED_EDGE ( 'NONE', *, *, #77180, .F. ) ;
#72270 = CARTESIAN_POINT ( 'NONE',  ( 107.0667039024470313, -104.2784471599408676, 19.21780685541799016 ) ) ;
#72271 = EDGE_CURVE ( 'NONE', #33917, #58383, #26941, .T. ) ;
#72272 = AXIS2_PLACEMENT_3D ( 'NONE', #28580, #84476, #1792 ) ;
#72273 = CARTESIAN_POINT ( 'NONE',  ( 110.0587659310071729, -27.38278898179161658, 234.8299109901969643 ) ) ;
#72274 = EDGE_LOOP ( 'NONE', ( #42106, #36971, #11389, #79469 ) ) ;
#72275 = ORIENTED_EDGE ( 'NONE', *, *, #26955, .F. ) ;
#72276 = CARTESIAN_POINT ( 'NONE',  ( 112.7482059764288778, -43.52991081625548020, 189.5615833058969883 ) ) ;
#72277 = CARTESIAN_POINT ( 'NONE',  ( 127.1498166246059753, 12.92155284005802862, 355.9756252759109998 ) ) ;
#72278 = CARTESIAN_POINT ( 'NONE',  ( 111.4141554795631492, -28.97316737322958957, 31.10158330589696263 ) ) ;
#72279 = CARTESIAN_POINT ( 'NONE',  ( 23.11423962701955759, 87.05952208832691497, 301.3555005791828307 ) ) ;
#72280 = PLANE ( 'NONE',  #43135 ) ;
#72281 = EDGE_CURVE ( 'NONE', #37406, #56556, #83258, .T. ) ;
#72282 = DIRECTION ( 'NONE',  ( 0.000000000000000000, 0.000000000000000000, -1.000000000000000000 ) ) ;
#72283 = VERTEX_POINT ( 'NONE', #75545 ) ;
#72284 = DIRECTION ( 'NONE',  ( -3.100000000000000258E-29, 3.100000000000000044E-14, 1.000000000000000000 ) ) ;
#72285 = CARTESIAN_POINT ( 'NONE',  ( -100.8594679592206802, 82.54999999999999716, -82.89895571708333932 ) ) ;
#72286 = EDGE_CURVE ( 'NONE', #82640, #35753, #75982, .T. ) ;
#72287 = ORIENTED_EDGE ( 'NONE', *, *, #64557, .F. ) ;
#72288 = CARTESIAN_POINT ( 'NONE',  ( 112.4780167374716058, -46.34085331822173970, 257.9965776568635647 ) ) ;
#72289 = CARTESIAN_POINT ( 'NONE',  ( 116.3212776292303090, -32.94146857471486811, 175.1356252759109680 ) ) ;
#72290 = EDGE_LOOP ( 'NONE', ( #43818, #70719 ) ) ;
#72291 = CARTESIAN_POINT ( 'NONE',  ( 115.0372575036200828, -42.90846257047583379, 83.30229194220611078 ) ) ;
#72292 = CYLINDRICAL_SURFACE ( 'NONE', #18626, 32.50000000000000711 ) ;
#72293 = LINE ( 'NONE', #45004, #8430 ) ;
#72294 = CARTESIAN_POINT ( 'NONE',  ( 68.91678303834669350, -69.56165394957326953, 247.5002289977139753 ) ) ;
#72295 = CIRCLE ( 'NONE', #54876, 4.750000000000004441 ) ;
#72296 = AXIS2_PLACEMENT_3D ( 'NONE', #45796, #59876, #65808 ) ;
#72297 = CARTESIAN_POINT ( 'NONE',  ( 112.2265052985635236, -45.83807782717671131, 208.9870538473389558 ) ) ;
#72298 = CARTESIAN_POINT ( 'NONE',  ( 4.446183819022752282, 70.75330535436950186, 118.2730736275787251 ) ) ;
#72299 = ORIENTED_EDGE ( 'NONE', *, *, #21901, .T. ) ;
#72300 = CARTESIAN_POINT ( 'NONE',  ( 97.31101637507774171, -32.83472251844465717, 37.02419670448292521 ) ) ;
#72301 = CARTESIAN_POINT ( 'NONE',  ( 20.03715912545637678, -24.42818131006202265, 193.9678068554150627 ) ) ;
#72302 = CARTESIAN_POINT ( 'NONE',  ( 109.2120108049357299, -48.38436871983039111, 277.7213395616254843 ) ) ;
#72303 = ORIENTED_EDGE ( 'NONE', *, *, #45198, .F. ) ;
#72304 = CARTESIAN_POINT ( 'NONE',  ( 82.41744075321345520, -17.29868422067037770, 2.608896314050102472 ) ) ;
#72305 = CARTESIAN_POINT ( 'NONE',  ( 0.000000000000000000, 184.0000000000000000, 85.23828826961327820 ) ) ;
#72306 = CARTESIAN_POINT ( 'NONE',  ( 62.03742497533745137, -23.42844715994041849, 313.9678068554150059 ) ) ;
#72307 = CARTESIAN_POINT ( 'NONE',  ( 102.9084262957273097, -29.13922403623678292, 98.28142370292496821 ) ) ;
#72308 = CARTESIAN_POINT ( 'NONE',  ( 103.2957022058525780, -26.98683617215391806, 211.3699109901969848 ) ) ;
#72309 = CARTESIAN_POINT ( 'NONE',  ( 77.31648329127398256, -18.72944715994106346, 14.92562527591094046 ) ) ;
#72310 = CYLINDRICAL_SURFACE ( 'NONE', #34893, 10.00000000000000888 ) ;
#72311 = ORIENTED_EDGE ( 'NONE', *, *, #1919, .T. ) ;
#72312 = FACE_OUTER_BOUND ( 'NONE', #30056, .T. ) ;
#72313 = B_SPLINE_CURVE_WITH_KNOTS ( 'NONE', 3,
 ( #38526, #53925, #80782, #4912, #59852, #88492, #87585, #25343, #24912, #60303, #33057, #80334, #88037, #11730, #65782, #18989, #52575, #67584, #72621, #12179, #60757, #53472, #38975, #53014, #18530, #31264, #44892, #39863, #81240, #26247, #58959, #73953, #86696, #24470, #66224, #52135, #11271, #87143, #79895, #46217, #39426, #17651, #59411, #45327, #73047, #67131, #4013, #18082 ),
 .UNSPECIFIED., .F., .F.,
 ( 4, 2, 2, 2, 2, 2, 2, 2, 2, 2, 2, 2, 2, 2, 2, 2, 2, 2, 2, 2, 2, 2, 2, 4 ),
 ( 1.387778780781445521E-17, 0.001601933432478720850, 0.002402900148718063820, 0.003203866864957407440, 0.004805800297436112895, 0.005606767013675474295, 0.006407733729914834829, 0.007208700446154196230, 0.008009667162393556764, 0.009611600594872257014, 0.01121353402735095726, 0.01281546745982965578, 0.01361643417606901198, 0.01441740089230836991, 0.01601933432478708577, 0.01682030104102645238, 0.01762126775726581898, 0.01922320118974451750, 0.02002416790598385288, 0.02082513462222318826, 0.02162610133846252364, 0.02242706805470186249, 0.02402900148718053325, 0.02563093491965920748 ),
 .UNSPECIFIED. ) ;
#72314 = ORIENTED_EDGE ( 'NONE', *, *, #39133, .F. ) ;
#72315 = ORIENTED_EDGE ( 'NONE', *, *, #28687, .T. ) ;
#72316 = CIRCLE ( 'NONE', #33141, 5.800000000000000711 ) ;
#72317 = VECTOR ( 'NONE', #29790, 999.9999999999998863 ) ;
#72318 = CARTESIAN_POINT ( 'NONE',  ( 2.332952152375709937E-14, 103.1240000000000236, -190.5000000000000000 ) ) ;
#72319 = ORIENTED_EDGE ( 'NONE', *, *, #76280, .T. ) ;
#72320 = VERTEX_POINT ( 'NONE', #55058 ) ;
#72321 = CARTESIAN_POINT ( 'NONE',  ( 163.0664832912739826, 25.62155284005901379, 333.4006252759110112 ) ) ;
#72322 = EDGE_CURVE ( 'NONE', #62403, #30864, #50784, .T. ) ;
#72323 = CARTESIAN_POINT ( 'NONE',  ( 115.0870504499182374, -30.61523282038012184, 24.34419833761608487 ) ) ;
#72324 = CARTESIAN_POINT ( 'NONE',  ( 97.81853004928629503, -39.68680891125094234, 130.9952769709339577 ) ) ;
#72325 = CARTESIAN_POINT ( 'NONE',  ( 114.8522965031571630, -43.72857415363870359, 38.24419670448192221 ) ) ;
#72326 = AXIS2_PLACEMENT_3D ( 'NONE', #1589, #57876, #64698 ) ;
#72327 = CARTESIAN_POINT ( 'NONE',  ( 172.5664832912740110, -36.32844715994070839, 263.6756252759120116 ) ) ;
#72328 = ORIENTED_EDGE ( 'NONE', *, *, #7140, .T. ) ;
#72329 = AXIS2_PLACEMENT_3D ( 'NONE', #31138, #3444, #3001 ) ;
#72330 = CARTESIAN_POINT ( 'NONE',  ( 116.3168070826688876, -32.94156582961523583, 135.1356252759109680 ) ) ;
#72331 = EDGE_LOOP ( 'NONE', ( #50288, #56299, #42557, #66023, #7033, #65841, #87838, #57287, #84485, #30578 ) ) ;
#72332 = LINE ( 'NONE', #57335, #33398 ) ;
#72333 = VECTOR ( 'NONE', #58035, 999.9999999999998863 ) ;
#72334 = PLANE ( 'NONE',  #3779 ) ;
#72335 = CARTESIAN_POINT ( 'NONE',  ( 37.06648329127298780, 12.92155284005730387, 355.9756252759109998 ) ) ;
#72336 = DIRECTION ( 'NONE',  ( 1.000000000000000078E-15, -1.000000000000000083E-30, -1.000000000000000000 ) ) ;
#72337 = ORIENTED_EDGE ( 'NONE', *, *, #27025, .F. ) ;
#72338 = EDGE_CURVE ( 'NONE', #11985, #25266, #31902, .T. ) ;
#72339 = UNCERTAINTY_MEASURE_WITH_UNIT (LENGTH_MEASURE( 1.000000000000000082E-05 ), #81063, 'distance_accuracy_value', 'NONE');
#72340 = CARTESIAN_POINT ( 'NONE',  ( 105.1090048964814940, -25.85068961359000284, 275.2061014663871674 ) ) ;
#72341 = CARTESIAN_POINT ( 'NONE',  ( 95.20983985305964836, -35.71400682071400468, 32.25848241876794020 ) ) ;
#72342 = CARTESIAN_POINT ( 'NONE',  ( 117.0608945233633165, -38.08045312270508731, 119.7189586090938036 ) ) ;
#72344 = CARTESIAN_POINT ( 'NONE',  ( 68.94728689011853362, -139.0532934344234093, 246.8082357644148317 ) ) ;
#72343 = CARTESIAN_POINT ( 'NONE',  ( 151.0371591254575208, -24.42818131005592264, 180.4678068554149775 ) ) ;
#72345 = DIRECTION ( 'NONE',  ( -0.8571673007021110013, 1.917331853055865018E-16, 0.5150380749100563760 ) ) ;
#72346 = CYLINDRICAL_SURFACE ( 'NONE', #263, 3.299999999999997158 ) ;
#72347 = LINE ( 'NONE', #16047, #22317 ) ;
#72348 = AXIS2_PLACEMENT_3D ( 'NONE', #16684, #4395, #38445 ) ;
#72349 = DIRECTION ( 'NONE',  ( -0.7071067811865506814, 0.7071067811865443531, -7.071067811865500971E-16 ) ) ;
#72350 = CARTESIAN_POINT ( 'NONE',  ( 131.0667039024480118, -67.87844715994100397, 213.1838068554149856 ) ) ;
#72351 = CYLINDRICAL_SURFACE ( 'NONE', #12362, 7.937500000000000000 ) ;
#72352 = EDGE_CURVE ( 'NONE', #7662, #21135, #88732, .T. ) ;
#72353 = DIRECTION ( 'NONE',  ( 0.000000000000000000, 0.000000000000000000, -1.000000000000000000 ) ) ;
#72354 = CARTESIAN_POINT ( 'NONE',  ( 116.5143565283028266, -32.21898467494469998, 19.18133956162493092 ) ) ;
#72355 = CARTESIAN_POINT ( 'NONE',  ( 113.6144894440835031, -28.61735105040022376, 160.5356252759109736 ) ) ;
#72356 = CARTESIAN_POINT ( 'NONE',  ( 103.5915305487281302, -46.58145011825330783, 53.30705384733997221 ) ) ;
#72358 = CARTESIAN_POINT ( 'NONE',  ( 162.8913605087221015, -31.76306994223262947, 313.9678068554149490 ) ) ;
#72357 = LINE ( 'NONE', #45068, #84181 ) ;
#72359 = CARTESIAN_POINT ( 'NONE',  ( 25.56670390244808644, -42.82844715994167473, 254.7178068554150059 ) ) ;
#72360 = CIRCLE ( 'NONE', #4204, 1.571100913904360796 ) ;
#72361 = EDGE_CURVE ( 'NONE', #15453, #68541, #50505, .T. ) ;
#72362 = ORIENTED_EDGE ( 'NONE', *, *, #56232, .F. ) ;
#72363 = DIRECTION ( 'NONE',  ( 1.000000000000000078E-15, 0.000000000000000000, -1.000000000000000000 ) ) ;
#72364 = ORIENTED_EDGE ( 'NONE', *, *, #24762, .F. ) ;
#72365 = CARTESIAN_POINT ( 'NONE',  ( 102.2761128416349692, -28.20209198692217356, 56.48419670448195973 ) ) ;
#72367 = ORIENTED_EDGE ( 'NONE', *, *, #13480, .F. ) ;
#72366 = DIRECTION ( 'NONE',  ( 0.000000000000000000, 0.000000000000000000, -1.000000000000000000 ) ) ;
#72368 = CARTESIAN_POINT ( 'NONE',  ( 80.48314995794042659, 12.92155284005802685, 336.5756252759109657 ) ) ;
#72369 = CARTESIAN_POINT ( 'NONE',  ( 96.06973772670292533, -35.87188691900273341, 187.2765776568629406 ) ) ;
#72370 = DIRECTION ( 'NONE',  ( 0.8660254037844351549, 0.000000000000000000, 0.5000000000000061062 ) ) ;
#72371 = CARTESIAN_POINT ( 'NONE',  ( 99.50487655220703687, -43.30595522777451123, 146.8960869441339412 ) ) ;
#72372 = CARTESIAN_POINT ( 'NONE',  ( 149.4512091874902922, -60.54365471797113685, 361.9756252759100335 ) ) ;
#72373 = EDGE_CURVE ( 'NONE', #47593, #29714, #39170, .T. ) ;
#72374 = CARTESIAN_POINT ( 'NONE',  ( 98.34985890484145443, -31.65658482251759054, 46.90645861040638209 ) ) ;
#72375 = AXIS2_PLACEMENT_3D ( 'NONE', #79170, #2855, #30555 ) ;
#72376 = DIRECTION ( 'NONE',  ( -0.000000000000000000, 1.000000000000000000, 0.000000000000000000 ) ) ;
#72377 = CARTESIAN_POINT ( 'NONE',  ( 97.92335910827921452, -40.78098889029146079, 96.65840926232698394 ) ) ;
#72378 = CARTESIAN_POINT ( 'NONE',  ( 114.2526777242401437, -43.36435822665426087, 123.2327681330539519 ) ) ;
#72379 = ORIENTED_EDGE ( 'NONE', *, *, #36290, .T. ) ;
#72380 = EDGE_LOOP ( 'NONE', ( #41715, #41077, #37164, #31073 ) ) ;
#72381 = AXIS2_PLACEMENT_3D ( 'NONE', #62980, #1675, #36641 ) ;
#72382 = CARTESIAN_POINT ( 'NONE',  ( 99.64559906019141522, -41.57287113897975672, 98.21872616303994619 ) ) ;
#72383 = DIRECTION ( 'NONE',  ( -6.982966722218760189E-15, 0.000000000000000000, -1.000000000000000000 ) ) ;
#72385 = DIRECTION ( 'NONE',  ( 1.000000000000000000, 0.000000000000000000, 0.000000000000000000 ) ) ;
#72384 = CARTESIAN_POINT ( 'NONE',  ( 97.48942487598456808, -34.74365074496814998, 212.1641967044819808 ) ) ;
#72386 = FACE_OUTER_BOUND ( 'NONE', #47566, .T. ) ;
#72387 = DIRECTION ( 'NONE',  ( 0.000000000000000000, -3.785359618865284342E-16, -1.000000000000000000 ) ) ;
#72388 = B_SPLINE_CURVE_WITH_KNOTS ( 'NONE', 3,
 ( #29003, #56688, #14021, #55330, #35347, #20838 ),
 .UNSPECIFIED., .F., .F.,
 ( 4, 1, 1, 4 ),
 ( 0.000000000000000000, 0.5730588445129599640, 0.7191761746442985048, 1.000000000000000000 ),
 .UNSPECIFIED. ) ;
#72389 = CARTESIAN_POINT ( 'NONE',  ( 118.3034456680046134, 72.47328848629021536, 7.741103959108575516 ) ) ;
#72390 = EDGE_CURVE ( 'NONE', #75837, #61357, #9629, .T. ) ;
#72391 = CIRCLE ( 'NONE', #5673, 4.750000000000000888 ) ;
#72392 = DIRECTION ( 'NONE',  ( 0.000000000000000000, 0.000000000000000000, 1.000000000000000000 ) ) ;
#72393 = CARTESIAN_POINT ( 'NONE',  ( 52.38749999999999574, 94.53880000000000905, 246.8562499999999886 ) ) ;
#72394 = CARTESIAN_POINT ( 'NONE',  ( 10.00076313689444696, 74.87425971760926302, 118.1337365946718876 ) ) ;
#72395 = EDGE_CURVE ( 'NONE', #10129, #17742, #33342, .T. ) ;
#72396 = CARTESIAN_POINT ( 'NONE',  ( 112.4747680694540861, -26.21285726233885427, 169.6984824187679521 ) ) ;
#72397 = ORIENTED_EDGE ( 'NONE', *, *, #27567, .T. ) ;
#72398 = ORIENTED_EDGE ( 'NONE', *, *, #71783, .F. ) ;
#72399 = ADVANCED_FACE ( 'NONE', ( #16448 ), #65041, .F. ) ;
#72400 = AXIS2_PLACEMENT_3D ( 'NONE', #47777, #67331, #18747 ) ;
#72401 = CARTESIAN_POINT ( 'NONE',  ( 94.91729554090750298, -74.61471936332451094, 249.3134381260879877 ) ) ;
#72402 = CARTESIAN_POINT ( 'NONE',  ( 104.4899545160106129, -26.97880756856109841, 151.2814586040433653 ) ) ;
#72403 = EDGE_CURVE ( 'NONE', #21297, #87703, #44126, .T. ) ;
#72404 = VECTOR ( 'NONE', #62501, 1000.000000000000000 ) ;
#72405 = DIRECTION ( 'NONE',  ( 0.000000000000000000, 0.000000000000000000, -1.000000000000000000 ) ) ;
#72406 = CARTESIAN_POINT ( 'NONE',  ( 117.0608820234855756, -38.08057516226932648, 104.7189489036250762 ) ) ;
#72407 = DIRECTION ( 'NONE',  ( 1.000000000000000000, 1.000000000000000078E-15, 0.000000000000000000 ) ) ;
#72408 = CARTESIAN_POINT ( 'NONE',  ( 117.4139541310910175, -35.45788210829842058, 193.9241967044829664 ) ) ;
#72409 = LINE ( 'NONE', #31053, #19786 ) ;
#72410 = EDGE_LOOP ( 'NONE', ( #60758, #83780, #57065, #21096 ) ) ;
#72412 = ORIENTED_EDGE ( 'NONE', *, *, #47004, .T. ) ;
#72411 = ORIENTED_EDGE ( 'NONE', *, *, #83569, .T. ) ;
#72413 = AXIS2_PLACEMENT_3D ( 'NONE', #48940, #55749, #33545 ) ;
#72414 = CARTESIAN_POINT ( 'NONE',  ( 116.9529224355460428, -35.09431523556290244, 64.95720187668048595 ) ) ;
#72415 = FACE_OUTER_BOUND ( 'NONE', #19791, .T. ) ;
#72416 = CARTESIAN_POINT ( 'NONE',  ( 133.4132809338266554, -34.05633243510674646, 8.161687850942930922 ) ) ;
#72417 = CARTESIAN_POINT ( 'NONE',  ( 115.9514134386872826, -36.57345012324869060, 285.2730118773255867 ) ) ;
#72418 = LINE ( 'NONE', #65589, #84076 ) ;
#72419 = VERTEX_POINT ( 'NONE', #35528 ) ;
#72420 = CARTESIAN_POINT ( 'NONE',  ( 111.5136026189559715, -44.03072630541131360, 9.635625275910941312 ) ) ;
#72421 = CARTESIAN_POINT ( 'NONE',  ( -126.5337430658103841, 62.85728282860507221, 32.15843782321050526 ) ) ;
#72422 = ORIENTED_EDGE ( 'NONE', *, *, #36171, .T. ) ;
#72423 = ORIENTED_EDGE ( 'NONE', *, *, #14839, .T. ) ;
#72424 = CARTESIAN_POINT ( 'NONE',  ( 112.3881417993268883, -45.21006700246557841, 113.0223899637873615 ) ) ;
#72425 = ORIENTED_EDGE ( 'NONE', *, *, #32706, .T. ) ;
#72426 = VERTEX_POINT ( 'NONE', #77785 ) ;
#72427 = EDGE_CURVE ( 'NONE', #63148, #54616, #42779, .T. ) ;
#72428 = CARTESIAN_POINT ( 'NONE',  ( 105.0857350373783561, -45.56626257478142605, 26.81146744712498275 ) ) ;
#72429 = CARTESIAN_POINT ( 'NONE',  ( 96.03049237414208505, -35.77952841945960216, 186.2461014663869889 ) ) ;
#72430 = CARTESIAN_POINT ( 'NONE',  ( 113.8292797163802561, -28.77778007523021842, 139.5156252759109634 ) ) ;
#72431 = FACE_OUTER_BOUND ( 'NONE', #12316, .T. ) ;
#72432 = CARTESIAN_POINT ( 'NONE',  ( 110.7330907359209107, -26.30208074597294754, 250.8194347997206819 ) ) ;
#72433 = CARTESIAN_POINT ( 'NONE',  ( 115.0374028803999238, -42.90827821187051683, 99.30364407749972600 ) ) ;
#72434 = LINE ( 'NONE', #58776, #84522 ) ;
#72435 = ORIENTED_EDGE ( 'NONE', *, *, #32785, .T. ) ;
#72436 = VECTOR ( 'NONE', #24534, 1000.000000000000000 ) ;
#72437 = VERTEX_POINT ( 'NONE', #71864 ) ;
#72438 = AXIS2_PLACEMENT_3D ( 'NONE', #78496, #49852, #15809 ) ;
#72439 = CARTESIAN_POINT ( 'NONE',  ( 99.25559070964938257, -29.75831933708737864, 190.7470538473399415 ) ) ;
#72440 = EDGE_LOOP ( 'NONE', ( #89474, #85036, #29088, #4471, #16347 ) ) ;
#72441 = ADVANCED_FACE ( 'NONE', ( #2378 ), #64157, .F. ) ;
#72442 = CARTESIAN_POINT ( 'NONE',  ( 113.6146262985763258, -28.61718150614917633, 164.5356252759109736 ) ) ;
#72443 = CARTESIAN_POINT ( 'NONE',  ( 162.7866693523289996, -36.02818131005891189, 342.9256252759119548 ) ) ;
#72444 = DIRECTION ( 'NONE',  ( 0.000000000000000000, 0.000000000000000000, 1.000000000000000000 ) ) ;
#72445 = CARTESIAN_POINT ( 'NONE',  ( 51.06648329127400388, 0.2215528400590083269, 333.4006252759110112 ) ) ;
#72446 = EDGE_CURVE ( 'NONE', #34033, #59761, #9192, .T. ) ;
#72449 = CARTESIAN_POINT ( 'NONE',  ( 111.8803037788896262, -27.54327565145516488, 10.68038718067199078 ) ) ;
#72448 = DIRECTION ( 'NONE',  ( 0.000000000000000000, 0.000000000000000000, 1.000000000000000000 ) ) ;
#72447 = PLANE ( 'NONE',  #33137 ) ;
#72450 = FACE_OUTER_BOUND ( 'NONE', #69273, .T. ) ;
#72451 = CARTESIAN_POINT ( 'NONE',  ( 142.8821648370247885, -72.54478064608022692, 361.9756252759100335 ) ) ;
#72452 = CARTESIAN_POINT ( 'NONE',  ( 100.9529263512021231, -28.70839242353804011, 271.5937037379645176 ) ) ;
#72453 = EDGE_CURVE ( 'NONE', #3527, #39861, #4364, .T. ) ;
#72454 = DIRECTION ( 'NONE',  ( 0.000000000000000000, 0.000000000000000000, 1.000000000000000000 ) ) ;
#72455 = DIRECTION ( 'NONE',  ( 0.000000000000000000, 0.000000000000000000, 1.000000000000000000 ) ) ;
#72456 = EDGE_CURVE ( 'NONE', #18132, #16891, #21474, .T. ) ;
#72457 = CARTESIAN_POINT ( 'NONE',  ( 0.000000000000000000, 17.78000000000000114, 0.000000000000000000 ) ) ;
#72459 = EDGE_LOOP ( 'NONE', ( #78300, #89549 ) ) ;
#72458 = CARTESIAN_POINT ( 'NONE',  ( 115.5237354892296793, -35.57185660929852133, 195.5838068554167535 ) ) ;
#72460 = EDGE_CURVE ( 'NONE', #46472, #69509, #47847, .T. ) ;
#72461 = CARTESIAN_POINT ( 'NONE',  ( 136.2679348343054926, -20.38027623201341143, 7.385026757011662113 ) ) ;
#72462 = CARTESIAN_POINT ( 'NONE',  ( 103.5348926201861985, -26.85948109348520418, 190.3499109901969746 ) ) ;
#72463 = CARTESIAN_POINT ( 'NONE',  ( 117.0537825276303749, -31.99364369613817161, 60.19086337114898555 ) ) ;
#72464 = CARTESIAN_POINT ( 'NONE',  ( 97.99904154034810233, -44.43610744809739543, 222.8870538473399563 ) ) ;
#72465 = FACE_OUTER_BOUND ( 'NONE', #46631, .T. ) ;
#72466 = CIRCLE ( 'NONE', #56490, 0.1499999999999973577 ) ;
#72467 = DIRECTION ( 'NONE',  ( -0.7071067811865758834, 0.7071067811865192621, -7.071067811865765240E-16 ) ) ;
#72469 = CARTESIAN_POINT ( 'NONE',  ( 97.80893753052176010, -40.51861053356429920, 37.63533870039827178 ) ) ;
#72468 = CARTESIAN_POINT ( 'NONE',  ( 193.0371591254582881, -47.82818131005411999, 300.4678068554149490 ) ) ;
#72470 = CARTESIAN_POINT ( 'NONE',  ( 85.06670390244700286, -71.37844715994096134, 55.21780685541800437 ) ) ;
#72471 = LINE ( 'NONE', #57936, #68320 ) ;
#72472 = EDGE_CURVE ( 'NONE', #9965, #59337, #1929, .T. ) ;
#72473 = CARTESIAN_POINT ( 'NONE',  ( 97.06381610791373760, -37.34192999475997254, 66.37606947914083833 ) ) ;
#72474 = ADVANCED_FACE ( 'NONE', ( #57772 ), #23291, .T. ) ;
#72475 = ORIENTED_EDGE ( 'NONE', *, *, #20798, .T. ) ;
#72476 = ORIENTED_EDGE ( 'NONE', *, *, #29285, .T. ) ;
#72477 = CARTESIAN_POINT ( 'NONE',  ( 102.7155009198991280, -28.78705314239651969, 99.88575316140996563 ) ) ;
#72479 = VERTEX_POINT ( 'NONE', #29625 ) ;
#72478 = CARTESIAN_POINT ( 'NONE',  ( -12.03249045273851969, 86.63451674300236505, -130.0003965276981432 ) ) ;
#72480 = CARTESIAN_POINT ( 'NONE',  ( 114.6914383512287543, -44.69963429152225132, 109.1718157521009687 ) ) ;
#72481 = ADVANCED_FACE ( 'NONE', ( #57313 ), #85060, .F. ) ;
#72482 = CYLINDRICAL_SURFACE ( 'NONE', #52695, 2.500000000000002220 ) ;
#72483 = EDGE_CURVE ( 'NONE', #81489, #15404, #18880, .T. ) ;
#72484 = CARTESIAN_POINT ( 'NONE',  ( -446.0240000000000009, 14.28750000000026077, 15.87499999999969802 ) ) ;
#72485 = CARTESIAN_POINT ( 'NONE',  ( 104.4899544686384445, -26.97880758048861338, 176.2814586078853836 ) ) ;
#72486 = CARTESIAN_POINT ( 'NONE',  ( 97.72045520820927322, -39.61305636501506910, 21.56419670448295278 ) ) ;
#72487 = ORIENTED_EDGE ( 'NONE', *, *, #46853, .T. ) ;
#72488 = VECTOR ( 'NONE', #66445, 1000.000000000000000 ) ;
#72489 = ORIENTED_EDGE ( 'NONE', *, *, #28165, .T. ) ;
#72490 = EDGE_LOOP ( 'NONE', ( #69777, #79733, #3429, #64700, #38054, #46647 ) ) ;
#72491 =( REPRESENTATION_RELATIONSHIP ('NONE','NONE', #82876, #885 ) REPRESENTATION_RELATIONSHIP_WITH_TRANSFORMATION ( #56692 )SHAPE_REPRESENTATION_RELATIONSHIP( ) );
#72492 = CARTESIAN_POINT ( 'NONE',  ( 182.0374245136140132, -23.42844715993459559, 313.9678068554149490 ) ) ;
#72493 = DIRECTION ( 'NONE',  ( 0.000000000000000000, 0.000000000000000000, -1.000000000000000000 ) ) ;
#72494 = CARTESIAN_POINT ( 'NONE',  ( 29.77381068363397887, -48.62134037875510018, 129.9678068554150627 ) ) ;
#72495 = DIRECTION ( 'NONE',  ( -8.538276166416950255E-16, 1.000000000000000000, -3.100000000000000044E-14 ) ) ;
#72496 = DIRECTION ( 'NONE',  ( 0.000000000000000000, 0.000000000000000000, 1.000000000000000000 ) ) ;
#72497 = CARTESIAN_POINT ( 'NONE',  ( 97.80830042520018708, -40.50914691106578402, 52.63449809795601197 ) ) ;
#72498 = DIRECTION ( 'NONE',  ( 1.000000000000000000, 1.000000000000000078E-15, 0.000000000000000000 ) ) ;
#72499 = CIRCLE ( 'NONE', #50767, 2.030000000000003801 ) ;
#72500 = EDGE_CURVE ( 'NONE', #14741, #18083, #8723, .T. ) ;
#72501 = CARTESIAN_POINT ( 'NONE',  ( 75.38763434846404721, 88.17653575778740560, 91.50010255991693953 ) ) ;
#72502 = EDGE_CURVE ( 'NONE', #65852, #73636, #49603, .T. ) ;
#72503 = CARTESIAN_POINT ( 'NONE',  ( 117.0329088946583624, -32.00354160957719074, 64.19086337114899266 ) ) ;
#72504 = ORIENTED_EDGE ( 'NONE', *, *, #21918, .F. ) ;
#72505 = ORIENTED_EDGE ( 'NONE', *, *, #62402, .F. ) ;
#72506 = EDGE_CURVE ( 'NONE', #73586, #44183, #24161, .T. ) ;
#72507 = CIRCLE ( 'NONE', #50770, 7.937500000000000000 ) ;
#72508 = FACE_OUTER_BOUND ( 'NONE', #53243, .T. ) ;
#72509 = DIRECTION ( 'NONE',  ( 0.1811243268507065352, -0.9834602067307444129, 0.000000000000000000 ) ) ;
#72510 = EDGE_CURVE ( 'NONE', #22204, #48918, #45459, .T. ) ;
#72511 = CARTESIAN_POINT ( 'NONE',  ( 97.81170051792484799, -40.51743816602341752, 61.63542871443850402 ) ) ;
#72512 = CARTESIAN_POINT ( 'NONE',  ( 100.0846959373945566, -41.84369885408329992, 104.6357094172109470 ) ) ;
#72513 = AXIS2_PLACEMENT_3D ( 'NONE', #1174, #70664, #62490 ) ;
#72514 = CIRCLE ( 'NONE', #33328, 2.517500000000005844 ) ;
#72515 = CARTESIAN_POINT ( 'NONE',  ( 51.06648329127400388, -0.2185775633790978945, 335.9181252759120184 ) ) ;
#72516 = PLANE ( 'NONE',  #51738 ) ;
#72517 = EDGE_LOOP ( 'NONE', ( #47695, #23682, #23168, #55167 ) ) ;
#72518 = ORIENTED_EDGE ( 'NONE', *, *, #48110, .F. ) ;
#72519 = AXIS2_PLACEMENT_3D ( 'NONE', #4604, #73635, #39559 ) ;
#72520 = DIRECTION ( 'NONE',  ( 0.000000000000000000, 0.000000000000000000, -1.000000000000000000 ) ) ;
#72521 = ORIENTED_EDGE ( 'NONE', *, *, #68228, .T. ) ;
#72522 = ORIENTED_EDGE ( 'NONE', *, *, #83582, .F. ) ;
#72523 = CARTESIAN_POINT ( 'NONE',  ( 107.4908894006829172, -46.11541567637532069, 189.0320594963729661 ) ) ;
#72524 = CARTESIAN_POINT ( 'NONE',  ( 67.65734841870819594, 95.25000000000000000, 346.9005000000000223 ) ) ;
#72525 = AXIS2_PLACEMENT_3D ( 'NONE', #56077, #35652, #55170 ) ;
#72526 = CARTESIAN_POINT ( 'NONE',  ( 112.1306244020896941, -47.47080300746646486, 133.9270538473399768 ) ) ;
#72527 = DIRECTION ( 'NONE',  ( 0.000000000000000000, 0.000000000000000000, 1.000000000000000000 ) ) ;
#72528 = CARTESIAN_POINT ( 'NONE',  ( 98.15099476832955361, -41.26164693790821048, 16.70074034222754733 ) ) ;
#72529 = ORIENTED_EDGE ( 'NONE', *, *, #75533, .F. ) ;
#72530 = ORIENTED_EDGE ( 'NONE', *, *, #47718, .F. ) ;
#72531 = ORIENTED_EDGE ( 'NONE', *, *, #50469, .F. ) ;
#72532 = STYLED_ITEM ( 'NONE', ( #28766 ), #20639 ) ;
#72533 = CARTESIAN_POINT ( 'NONE',  ( 112.5929834642309117, -30.72215809952430376, 197.3023760838769647 ) ) ;
#72534 = CARTESIAN_POINT ( 'NONE',  ( 106.9270552135175620, -26.24760940922973163, 60.08705384733897858 ) ) ;
#72535 = ORIENTED_EDGE ( 'NONE', *, *, #52027, .T. ) ;
#72536 = CARTESIAN_POINT ( 'NONE',  ( 116.3681181406587370, -31.99193570193495262, 44.20133956162491984 ) ) ;
#72537 = CYLINDRICAL_SURFACE ( 'NONE', #31237, 2.117000000000007987 ) ;
#72538 = CARTESIAN_POINT ( 'NONE',  ( 172.5667039024480118, -36.32844715993499563, 193.9678068554150059 ) ) ;
#72539 = DIRECTION ( 'NONE',  ( -1.000000000000000000, 0.000000000000000000, 0.000000000000000000 ) ) ;
#72540 = CARTESIAN_POINT ( 'NONE',  ( 117.0231160686283687, -39.93674523842013713, 154.5784824187679476 ) ) ;
#72541 = CARTESIAN_POINT ( 'NONE',  ( 116.8171228658513741, -34.15291831898669273, 264.0314586093876414 ) ) ;
#72542 = ORIENTED_EDGE ( 'NONE', *, *, #49597, .T. ) ;
#72543 = CARTESIAN_POINT ( 'NONE',  ( 179.1667039024460166, -28.27351298637280408, -5.074374724088000832 ) ) ;
#72544 = EDGE_LOOP ( 'NONE', ( #25993, #15856, #59722, #69359 ) ) ;
#72545 = CARTESIAN_POINT ( 'NONE',  ( 167.2371591254545535, -47.82818131005522133, 129.9678068554149775 ) ) ;
#72546 = VERTEX_POINT ( 'NONE', #18225 ) ;
#72548 = ORIENTED_EDGE ( 'NONE', *, *, #49696, .F. ) ;
#72547 = VECTOR ( 'NONE', #34949, 1000.000000000000000 ) ;
#72549 = DIRECTION ( 'NONE',  ( 0.9068632946707805287, -0.4214249218767882055, 8.839355291601567287E-16 ) ) ;
#72550 = CARTESIAN_POINT ( 'NONE',  ( 77.39114642429899504, 127.0000000000000000, 71.77848634863160271 ) ) ;
#72551 = CARTESIAN_POINT ( 'NONE',  ( 107.3210346550871179, -25.67891364084480799, 75.04610146638695767 ) ) ;
#72552 = CARTESIAN_POINT ( 'NONE',  ( 32.16397622746000451, -34.03355364505800651, -5.074374724088000832 ) ) ;
#72553 = EDGE_CURVE ( 'NONE', #30852, #45804, #79581, .T. ) ;
#72554 = CARTESIAN_POINT ( 'NONE',  ( -179.6205029264235122, 0.000000000000000000, 123.8612349545196025 ) ) ;
#72555 = CARTESIAN_POINT ( 'NONE',  ( 98.30753419713312269, -41.72887550236994514, 72.73979194360303779 ) ) ;
#72556 = EDGE_CURVE ( 'NONE', #66435, #25689, #3271, .T. ) ;
#72557 = CARTESIAN_POINT ( 'NONE',  ( 115.5638989210038119, -29.55965564860105843, 74.38419670448293175 ) ) ;
#72559 = CARTESIAN_POINT ( 'NONE',  ( 117.2701380961605651, -34.52720868313124924, 179.9956252759109532 ) ) ;
#72558 = PLANE ( 'NONE',  #5591 ) ;
#72560 = CARTESIAN_POINT ( 'NONE',  ( -72.96458098368751166, 117.4749999999999943, 72.96458098368620426 ) ) ;
#72561 = LINE ( 'NONE', #23533, #80105 ) ;
#72562 = VERTEX_POINT ( 'NONE', #31397 ) ;
#72563 = CARTESIAN_POINT ( 'NONE',  ( 25.56670390244744695, -48.82844715994178841, 173.2178068554150627 ) ) ;
#72564 = ADVANCED_FACE ( 'NONE', ( #25484 ), #58649, .T. ) ;
#72565 = DIRECTION ( 'NONE',  ( -0.000000000000000000, -0.000000000000000000, -1.000000000000000000 ) ) ;
#72566 = DIRECTION ( 'NONE',  ( -3.360405532702990443E-14, 1.000000000000000000, 0.000000000000000000 ) ) ;
#72567 = AXIS2_PLACEMENT_3D ( 'NONE', #37384, #52306, #59149 ) ;
#72568 = ADVANCED_FACE ( 'NONE', ( #65917 ), #17342, .F. ) ;
#72569 = CYLINDRICAL_SURFACE ( 'NONE', #30317, 7.143750000000004263 ) ;
#72571 = ORIENTED_EDGE ( 'NONE', *, *, #71384, .F. ) ;
#72570 = CARTESIAN_POINT ( 'NONE',  ( 113.1256532486054880, -46.02994946121840769, 223.0480062282919675 ) ) ;
#72572 = CARTESIAN_POINT ( 'NONE',  ( 116.3212776292272537, -32.94146857470742162, 144.1356252759109680 ) ) ;
#72573 = CARTESIAN_POINT ( 'NONE',  ( 117.5131067102741582, -36.80237174509009179, 259.8213395616249386 ) ) ;
#72574 = CARTESIAN_POINT ( 'NONE',  ( 98.42032043187158763, -42.69450228079005427, 122.8070538473389490 ) ) ;
#72575 = CARTESIAN_POINT ( 'NONE',  ( 164.9212702847350158, -29.73316016639540749, -5.074374724088000832 ) ) ;
#72576 = CARTESIAN_POINT ( 'NONE',  ( 82.31791107858728651, -38.31136518418592374, 7.339178645746792462 ) ) ;
#72577 = CARTESIAN_POINT ( 'NONE',  ( 51.56670390244899238, -32.29483332968450782, 342.9256252759119548 ) ) ;
#72578 = CARTESIAN_POINT ( 'NONE',  ( 180.2143765759489895, -35.91149509761070391, 117.4678068554150627 ) ) ;
#72579 = EDGE_LOOP ( 'NONE', ( #87296, #3817, #60292, #64436 ) ) ;
#72580 = CIRCLE ( 'NONE', #76908, 3.299999999999999822 ) ;
#72581 = ADVANCED_FACE ( 'NONE', ( #18672 ), #45022, .F. ) ;
#72582 = ORIENTED_EDGE ( 'NONE', *, *, #45303, .F. ) ;
#72583 = EDGE_CURVE ( 'NONE', #61646, #82905, #46353, .T. ) ;
#72584 = EDGE_LOOP ( 'NONE', ( #88252, #49499, #30486, #53736 ) ) ;
#72585 = VECTOR ( 'NONE', #22721, 1000.000000000000000 ) ;
#72586 = EDGE_LOOP ( 'NONE', ( #72043, #20177, #7223, #77961 ) ) ;
#72587 = DIRECTION ( 'NONE',  ( 3.999999999999999995E-14, -1.000000000000000000, 4.100000000000000342E-29 ) ) ;
#72588 = CARTESIAN_POINT ( 'NONE',  ( 96.97881741550158097, -39.36031858868991407, 272.5299109901966972 ) ) ;
#72589 = CARTESIAN_POINT ( 'NONE',  ( 107.0667039024470313, -104.2784471599418197, -11.78219314458200984 ) ) ;
#72590 = DIRECTION ( 'NONE',  ( 0.7071067812158990940, 0.7071067811571960515, 0.000000000000000000 ) ) ;
#72591 = EDGE_CURVE ( 'NONE', #28958, #54712, #59511, .T. ) ;
#72592 = CIRCLE ( 'NONE', #81301, 88.90000000000000568 ) ;
#72594 = CARTESIAN_POINT ( 'NONE',  ( 74.62294912200587760, 79.66725693986900581, 92.12462914090833976 ) ) ;
#72593 = DIRECTION ( 'NONE',  ( 1.000000000000000000, -0.000000000000000000, 2.108231265501709878E-16 ) ) ;
#72595 = DIRECTION ( 'NONE',  ( 0.000000000000000000, 0.000000000000000000, 1.000000000000000000 ) ) ;
#72596 = CARTESIAN_POINT ( 'NONE',  ( 101.7992505034292350, -28.57304559719056058, 219.9552769709339657 ) ) ;
#72597 = ORIENTED_EDGE ( 'NONE', *, *, #11015, .F. ) ;
#72598 = EDGE_CURVE ( 'NONE', #35866, #71111, #63902, .T. ) ;
#72599 = EDGE_LOOP ( 'NONE', ( #73629, #35872 ) ) ;
#72600 = ORIENTED_EDGE ( 'NONE', *, *, #65557, .F. ) ;
#72601 = FACE_OUTER_BOUND ( 'NONE', #21141, .T. ) ;
#72602 = CARTESIAN_POINT ( 'NONE',  ( 110.8602461355434912, -45.98187261348512322, 182.8861217718651915 ) ) ;
#72603 = DIRECTION ( 'NONE',  ( 1.000000000000000000, 1.261617073437676668E-15, 9.462128050782575008E-16 ) ) ;
#72604 = CARTESIAN_POINT ( 'NONE',  ( 95.96284676697312932, -37.29622633765301032, 267.3670538473388092 ) ) ;
#72605 = AXIS2_PLACEMENT_3D ( 'NONE', #87383, #19236, #88295 ) ;
#72606 = LINE ( 'NONE', #10370, #66095 ) ;
#72607 = CARTESIAN_POINT ( 'NONE',  ( 193.0374249753374443, -23.42844715993432558, 313.9678068554149490 ) ) ;
#72608 = CYLINDRICAL_SURFACE ( 'NONE', #63427, 9.999999999999998224 ) ;
#72609 = ORIENTED_EDGE ( 'NONE', *, *, #33229, .T. ) ;
#72610 = PLANE ( 'NONE',  #57861 ) ;
#72611 = ORIENTED_EDGE ( 'NONE', *, *, #76501, .T. ) ;
#72612 = ADVANCED_FACE ( 'NONE', ( #17781 ), #72310, .T. ) ;
#72613 = VECTOR ( 'NONE', #59410, 1000.000000000000000 ) ;
#72614 = LINE ( 'NONE', #10377, #78617 ) ;
#72615 = CARTESIAN_POINT ( 'NONE',  ( 100.8629568432159260, -42.03472619363567730, 29.70809036959193250 ) ) ;
#72616 = CARTESIAN_POINT ( 'NONE',  ( 80.06648329127399677, -18.72944715994105991, -5.074374724089057764 ) ) ;
#72617 = DIRECTION ( 'NONE',  ( -0.9825752044165969590, -0.1858654558159821002, 0.000000000000000000 ) ) ;
#72618 = CYLINDRICAL_SURFACE ( 'NONE', #41498, 1.000000000000000888 ) ;
#72619 = ORIENTED_EDGE ( 'NONE', *, *, #9906, .T. ) ;
#72620 = CARTESIAN_POINT ( 'NONE',  ( 50.56670390244696733, -18.82844715994099971, 330.9332325604117955 ) ) ;
#72621 = CARTESIAN_POINT ( 'NONE',  ( 123.9304707123681766, 59.93532171591466096, -41.06530013989648609 ) ) ;
#72622 = ORIENTED_EDGE ( 'NONE', *, *, #78150, .F. ) ;
#72623 = CARTESIAN_POINT ( 'NONE',  ( 96.79149040999978126, -38.49340627261485537, 91.46133956162493917 ) ) ;
#72624 = ORIENTED_EDGE ( 'NONE', *, *, #63540, .F. ) ;
#72625 = CARTESIAN_POINT ( 'NONE',  ( 114.1180452634077369, -42.41171291218270767, 42.69718173283898466 ) ) ;
#72626 = CONICAL_SURFACE ( 'NONE', #65355, 5.562600000000000655, 1.029744258676653645 ) ;
#72627 = CARTESIAN_POINT ( 'NONE',  ( 33.98325472291465132, 124.5870000000000033, -3.174999999999999822 ) ) ;
#72628 = CARTESIAN_POINT ( 'NONE',  ( 104.6418561626188364, -26.95233673609813962, 86.70158330589694629 ) ) ;
#72629 = ADVANCED_FACE ( 'NONE', ( #11412 ), #86384, .F. ) ;
#72630 = CARTESIAN_POINT ( 'NONE',  ( 99.04396218797715790, -42.84110790024666926, 12.84394456308144328 ) ) ;
#72631 = DIRECTION ( 'NONE',  ( -1.000000000000000000, -8.741913579725640327E-16, -2.913971193241879977E-15 ) ) ;
#72632 = CARTESIAN_POINT ( 'NONE',  ( 90.06648329127389729, -36.72944715993924802, 14.92562527591095289 ) ) ;
#72633 = CARTESIAN_POINT ( 'NONE',  ( 101.3723308891022157, -27.97080072976544685, 21.53562527591096298 ) ) ;
#72634 = VECTOR ( 'NONE', #84539, 1000.000000000000000 ) ;
#72635 = DIRECTION ( 'NONE',  ( 0.000000000000000000, 1.000000000000000000, 0.000000000000000000 ) ) ;
#72636 = EDGE_LOOP ( 'NONE', ( #60531, #86259, #69072, #15813 ) ) ;
#72637 = ADVANCED_FACE ( 'NONE', ( #73180 ), #24599, .F. ) ;
#72638 = DIRECTION ( 'NONE',  ( -3.100000000000000258E-29, 3.100000000000000044E-14, 1.000000000000000000 ) ) ;
#72639 = VERTEX_POINT ( 'NONE', #59542 ) ;
#72640 = CARTESIAN_POINT ( 'NONE',  ( 103.8797721312301405, -101.8611209747507189, 2.217806855417919998 ) ) ;
#72641 = VERTEX_POINT ( 'NONE', #10957 ) ;
#72642 = ORIENTED_EDGE ( 'NONE', *, *, #33511, .F. ) ;
#72643 = CIRCLE ( 'NONE', #79917, 1.000000000000000888 ) ;
#72644 = FACE_OUTER_BOUND ( 'NONE', #45975, .T. ) ;
#72645 = CARTESIAN_POINT ( 'NONE',  ( 112.7271506738796347, -45.41826929060063378, 223.0480062282919675 ) ) ;
#72646 = CARTESIAN_POINT ( 'NONE',  ( 107.4535518903492033, -26.65157354815539748, 125.0442608526201838 ) ) ;
#72647 = CARTESIAN_POINT ( 'NONE',  ( 0.000000000000000000, 224.4999999999999432, 164.6557476874258441 ) ) ;
#72648 = CARTESIAN_POINT ( 'NONE',  ( 109.9110140596799425, -46.79572638734455126, 68.79562527591099297 ) ) ;
#72649 = DIRECTION ( 'NONE',  ( 0.7967329428042202455, -0.6043315462976655006, 1.908195823574484964E-14 ) ) ;
#72650 = ORIENTED_EDGE ( 'NONE', *, *, #71031, .F. ) ;
#72651 = CARTESIAN_POINT ( 'NONE',  ( 99.09516693519820763, -30.55115414915417560, 171.8022944752187016 ) ) ;
#72652 = CARTESIAN_POINT ( 'NONE',  ( 184.5667039024480118, -67.87844715994100397, 300.9178068554150514 ) ) ;
#72653 = ORIENTED_EDGE ( 'NONE', *, *, #4444, .F. ) ;
#72654 = B_SPLINE_CURVE_WITH_KNOTS ( 'NONE', 3,
 ( #63581, #77217, #22256, #7716, #83143, #35406, #63124, #70397, #62676, #64033, #1811, #55835, #451, #28143, #1360, #29509, #57191, #304, #89809, #54790, #41173, #82555, #60720, #19403, #40287, #83427, #20316, #34363 ),
 .UNSPECIFIED., .F., .F.,
 ( 4, 2, 2, 2, 2, 2, 2, 2, 2, 2, 2, 2, 2, 4 ),
 ( 0.5000628611168262960, 0.5625550034772225372, 0.6250471458376188894, 0.6875392881980151305, 0.7187853593782136397, 0.7500314305584121488, 0.7812775017386106580, 0.8125235729188091671, 0.8437696440990075653, 0.8750157152792059634, 0.9062617864594044725, 0.9375078576396029817, 0.9687539288198014908, 1.000000000000000000 ),
 .UNSPECIFIED. ) ;
#72655 = DIRECTION ( 'NONE',  ( 0.000000000000000000, 1.000000000000000000, 0.000000000000000000 ) ) ;
#72656 = CARTESIAN_POINT ( 'NONE',  ( 134.0664832912739826, -18.72944715994100306, -5.074374724089001809 ) ) ;
#72657 = CARTESIAN_POINT ( 'NONE',  ( 115.4423046205436947, -29.55243945206539280, 229.4022919425779605 ) ) ;
#72658 = CARTESIAN_POINT ( 'NONE',  ( 48.79742451362081823, -36.32844715994077944, 237.4678068554150059 ) ) ;
#72659 = EDGE_CURVE ( 'NONE', #74753, #81257, #88593, .T. ) ;
#72660 = FACE_BOUND ( 'NONE', #60332, .T. ) ;
#72661 = CARTESIAN_POINT ( 'NONE',  ( 80.06648329127401098, -39.47944715994105991, 1.625625275910943746 ) ) ;
#72662 = AXIS2_PLACEMENT_3D ( 'NONE', #59652, #72854, #17883 ) ;
#72663 = CARTESIAN_POINT ( 'NONE',  ( 101.0745446329174655, -30.64234581064881269, 225.1181341137909442 ) ) ;
#72665 = CARTESIAN_POINT ( 'NONE',  ( 102.9796410358630254, -46.29638950891617100, 88.25562527591095829 ) ) ;
#72664 = DIRECTION ( 'NONE',  ( 3.100000000000000258E-29, -3.100000000000000044E-14, -1.000000000000000000 ) ) ;
#72666 = CARTESIAN_POINT ( 'NONE',  ( 110.0341319374553706, 60.86293649591723920, 70.26678365844557561 ) ) ;
#72667 = CARTESIAN_POINT ( 'NONE',  ( 113.9459708190624241, -28.01821676562244789, 124.5565776568629559 ) ) ;
#72668 = ORIENTED_EDGE ( 'NONE', *, *, #14423, .T. ) ;
#72669 = CARTESIAN_POINT ( 'NONE',  ( 69.25310000000000343, 82.54999999999999716, 335.3740053999999304 ) ) ;
#72670 = ORIENTED_EDGE ( 'NONE', *, *, #2635, .F. ) ;
#72671 = PLANE ( 'NONE',  #72874 ) ;
#72672 = VECTOR ( 'NONE', #54552, 1000.000000000000000 ) ;
#72673 = EDGE_CURVE ( 'NONE', #82826, #11696, #24553, .T. ) ;
#72674 = DIRECTION ( 'NONE',  ( 1.000000000000000000, 0.000000000000000000, 0.000000000000000000 ) ) ;
#72675 = CARTESIAN_POINT ( 'NONE',  ( 223.2659999999999911, 52.73749999999999716, -44.45000000000000284 ) ) ;
#72677 = ORIENTED_EDGE ( 'NONE', *, *, #19389, .F. ) ;
#72676 = VECTOR ( 'NONE', #47069, 1000.000000000000000 ) ;
#72678 = CARTESIAN_POINT ( 'NONE',  ( -194.1576000000000022, 0.000000000000000000, 114.2999999999999972 ) ) ;
#72679 = ADVANCED_FACE ( 'NONE', ( #13214 ), #75882, .T. ) ;
#72680 = ORIENTED_EDGE ( 'NONE', *, *, #63026, .F. ) ;
#72681 = CYLINDRICAL_SURFACE ( 'NONE', #36398, 9.999999999999998224 ) ;
#72682 = CARTESIAN_POINT ( 'NONE',  ( -194.1576000000000022, 20.32000000000000028, -12.69999999999999929 ) ) ;
#72683 = VECTOR ( 'NONE', #2401, 1000.000000000000000 ) ;
#72684 = LINE ( 'NONE', #65844, #36563 ) ;
#72685 = VERTEX_POINT ( 'NONE', #34077 ) ;
#72686 = ADVANCED_FACE ( 'NONE', ( #41336 ), #48591, .T. ) ;
#72687 = VECTOR ( 'NONE', #7292, 1000.000000000000000 ) ;
#72688 = CARTESIAN_POINT ( 'NONE',  ( 117.8983839226775387, -39.04577396070462214, 108.6708633711489824 ) ) ;
#72689 = DIRECTION ( 'NONE',  ( 1.000000000000000000, 0.000000000000000000, 0.000000000000000000 ) ) ;
#72690 = CARTESIAN_POINT ( 'NONE',  ( 97.79831359961421811, -40.48460542285404529, 166.6328045679836691 ) ) ;
#72691 = LINE ( 'NONE', #9125, #78585 ) ;
#72692 = CARTESIAN_POINT ( 'NONE',  ( -30.89999999999999858, 53.97500000000000142, 40.80000000000000426 ) ) ;
#72693 = ORIENTED_EDGE ( 'NONE', *, *, #17959, .F. ) ;
#72694 = EDGE_CURVE ( 'NONE', #4177, #49608, #33648, .T. ) ;
#72695 = EDGE_LOOP ( 'NONE', ( #26209, #79818, #37222, #73607 ) ) ;
#72696 = DIRECTION ( 'NONE',  ( -1.000000000000000000, -2.756263715554006823E-15, 0.000000000000000000 ) ) ;
#72697 = DIRECTION ( 'NONE',  ( -1.000000000000000000, -4.299999999999999979E-14, -1.000000000000000078E-15 ) ) ;
#72698 = DIRECTION ( 'NONE',  ( 0.000000000000000000, 0.000000000000000000, 1.000000000000000000 ) ) ;
#72699 = AXIS2_PLACEMENT_3D ( 'NONE', #8489, #35274, #7588 ) ;
#72701 = CARTESIAN_POINT ( 'NONE',  ( -446.0240000000000009, 3.174999999999999822, -1.387778780781445991E-14 ) ) ;
#72700 = CARTESIAN_POINT ( 'NONE',  ( 116.7602698800575212, -34.01575108322786889, 250.0437193735734525 ) ) ;
#72702 = LINE ( 'NONE', #16398, #79946 ) ;
#72703 = AXIS2_PLACEMENT_3D ( 'NONE', #43946, #49864, #71242 ) ;
#72704 = ORIENTED_EDGE ( 'NONE', *, *, #8697, .T. ) ;
#72705 = CARTESIAN_POINT ( 'NONE',  ( 172.5664832912740110, -9.303447159940999356, 198.9256252759119832 ) ) ;
#72706 = CARTESIAN_POINT ( 'NONE',  ( 104.7173522264389618, -47.59653351925012288, 178.4070538473389718 ) ) ;
#72707 = AXIS2_PLACEMENT_3D ( 'NONE', #88067, #19461, #89865 ) ;
#72709 = ORIENTED_EDGE ( 'NONE', *, *, #83582, .T. ) ;
#72708 = CARTESIAN_POINT ( 'NONE',  ( 51.27381068362099370, -23.19206098993950604, 342.9256252759119548 ) ) ;
#72710 = CARTESIAN_POINT ( 'NONE',  ( 110.2470682213182300, -46.59973918892927003, 53.83657765686300678 ) ) ;
#72711 = CYLINDRICAL_SURFACE ( 'NONE', #64666, 2.030000000001869864 ) ;
#72712 = DIRECTION ( 'NONE',  ( 0.000000000000000000, 0.000000000000000000, -1.000000000000000000 ) ) ;
#72713 = ORIENTED_EDGE ( 'NONE', *, *, #69862, .F. ) ;
#72714 = LINE ( 'NONE', #52226, #41426 ) ;
#72715 = ORIENTED_EDGE ( 'NONE', *, *, #33758, .F. ) ;
#72716 = VERTEX_POINT ( 'NONE', #74983 ) ;
#72717 = EDGE_CURVE ( 'NONE', #48829, #85625, #68177, .T. ) ;
#72718 = CARTESIAN_POINT ( 'NONE',  ( 102.7466871476783581, -44.50128676613118728, 183.6044404487539623 ) ) ;
#72719 = DIRECTION ( 'NONE',  ( -1.000000000000000000, 0.000000000000000000, 0.000000000000000000 ) ) ;
#72720 = CARTESIAN_POINT ( 'NONE',  ( 23.74045948899717473, 83.33176929200182315, 307.5955140303815369 ) ) ;
#72721 = DIRECTION ( 'NONE',  ( 0.7071067708032326982, 0.0001211784769794325652, 0.7071067811865484609 ) ) ;
#72722 = CARTESIAN_POINT ( 'NONE',  ( 81.84766347661003749, -124.7784471599409670, 55.21780685541800437 ) ) ;
#72723 = VERTEX_POINT ( 'NONE', #20026 ) ;
#72724 = CARTESIAN_POINT ( 'NONE',  ( 62.03742497533654188, -23.42844715994041493, 180.4678068554151196 ) ) ;
#72725 = CARTESIAN_POINT ( 'NONE',  ( 172.5664832912729878, -27.57844715994070484, 78.92562527591199739 ) ) ;
#72726 = ORIENTED_EDGE ( 'NONE', *, *, #58519, .T. ) ;
#72727 = CARTESIAN_POINT ( 'NONE',  ( 116.5858064714421829, -40.92601143571970823, 253.4956252759109532 ) ) ;
#72728 = CARTESIAN_POINT ( 'NONE',  ( 4.478078041421492017, 94.44158826854035738, 118.4720215458495147 ) ) ;
#72729 = ORIENTED_EDGE ( 'NONE', *, *, #5186, .F. ) ;
#72730 = DIRECTION ( 'NONE',  ( 1.000000000000000078E-15, -1.000000000000000083E-30, -1.000000000000000000 ) ) ;
#72731 = DIRECTION ( 'NONE',  ( 0.000000000000000000, 0.000000000000000000, 1.000000000000000000 ) ) ;
#72732 = FACE_BOUND ( 'NONE', #58610, .T. ) ;
#72733 = CARTESIAN_POINT ( 'NONE',  ( -186.2398777604655038, 101.5999999999999943, -6.349999999999999645 ) ) ;
#72734 = AXIS2_PLACEMENT_3D ( 'NONE', #29111, #49527, #70445 ) ;
#72735 = CARTESIAN_POINT ( 'NONE',  ( 101.3810039469494200, -45.56196318943892010, 218.1213395616249784 ) ) ;
#72736 = CARTESIAN_POINT ( 'NONE',  ( 130.5667039024480118, -36.72944715994093912, 218.8274735512161158 ) ) ;
#72737 = EDGE_LOOP ( 'NONE', ( #1397, #19409, #44600, #85248 ) ) ;
#72738 = CIRCLE ( 'NONE', #33570, 2.550000000000006040 ) ;
#72739 = EDGE_CURVE ( 'NONE', #26268, #61703, #10265, .T. ) ;
#72740 = CARTESIAN_POINT ( 'NONE',  ( 106.6049252239556608, -25.63961115983148176, 36.09753003781596448 ) ) ;
#72741 = CARTESIAN_POINT ( 'NONE',  ( 274.0659999999999741, 40.03750000000000142, -7.937500000000000000 ) ) ;
#72742 = CARTESIAN_POINT ( 'NONE',  ( 106.8364329414440874, -47.15221585624544787, 272.5584824187680510 ) ) ;
#72743 = ORIENTED_EDGE ( 'NONE', *, *, #75148, .T. ) ;
#72744 = B_SPLINE_CURVE_WITH_KNOTS ( 'NONE', 3,
 ( #76692, #42588, #48497, #82182, #69431, #41696, #49409, #42149, #83505, #69877, #14921, #48064, #70324, #19937 ),
 .UNSPECIFIED., .F., .F.,
 ( 4, 2, 2, 1, 1, 2, 2, 4 ),
 ( 0.000000000000000000, 0.2499999999999814593, 0.3749999999999724110, 0.4374999999999666933, 0.4687499999999643618, 0.4843749999999638622, 0.4999999999999633626, 1.000000000000000000 ),
 .UNSPECIFIED. ) ;
#72745 = CARTESIAN_POINT ( 'NONE',  ( 79.31518617683019556, -39.40257939794701514, 8.160477455080144438 ) ) ;
#72746 = CARTESIAN_POINT ( 'NONE',  ( 100.8875449613382358, -44.70030174540323742, 18.05248020336808779 ) ) ;
#72747 = CARTESIAN_POINT ( 'NONE',  ( -41.60202597009397607, 65.59999999999998010, 54.66767516814134353 ) ) ;
#72748 = CARTESIAN_POINT ( 'NONE',  ( 100.6392880577574687, -41.80624237711439406, 89.67666179816296790 ) ) ;
#72749 = CARTESIAN_POINT ( 'NONE',  ( 97.90015701271006776, -41.74100594024375965, 217.7241967044829494 ) ) ;
#72750 = VECTOR ( 'NONE', #16748, 1000.000000000000114 ) ;
#72751 = DIRECTION ( 'NONE',  ( 0.000000000000000000, 0.000000000000000000, 1.000000000000000000 ) ) ;
#72752 = VERTEX_POINT ( 'NONE', #55408 ) ;
#72753 = DIRECTION ( 'NONE',  ( 0.000000000000000000, 0.000000000000000000, -1.000000000000000000 ) ) ;
#72754 = ORIENTED_EDGE ( 'NONE', *, *, #55245, .T. ) ;
#72755 = ORIENTED_EDGE ( 'NONE', *, *, #80928, .T. ) ;
#72756 = DIRECTION ( 'NONE',  ( 0.7071067811865604513, 0.000000000000000000, -0.7071067811865344721 ) ) ;
#72757 = VERTEX_POINT ( 'NONE', #69520 ) ;
#72758 = ORIENTED_EDGE ( 'NONE', *, *, #39103, .T. ) ;
#72759 = DIRECTION ( 'NONE',  ( 0.000000000000000000, 0.000000000000000000, -1.000000000000000000 ) ) ;
#72760 = DIRECTION ( 'NONE',  ( 0.000000000000000000, 0.000000000000000000, 1.000000000000000000 ) ) ;
#72761 = CARTESIAN_POINT ( 'NONE',  ( 104.5239601885372309, -27.05251041699375136, 41.28092177733371670 ) ) ;
#72762 = ADVANCED_FACE ( 'NONE', ( #27276 ), #54951, .F. ) ;
#72763 = CARTESIAN_POINT ( 'NONE',  ( 107.7867742379091567, -27.70205266993799142, 114.4476579233149636 ) ) ;
#72764 = VECTOR ( 'NONE', #34098, 1000.000000000000000 ) ;
#72765 = CARTESIAN_POINT ( 'NONE',  ( 97.75295786963341982, -40.54146432227403807, 11.63562527591094309 ) ) ;
#72766 = EDGE_LOOP ( 'NONE', ( #3296, #38871, #88073, #4324 ) ) ;
#72767 = EDGE_CURVE ( 'NONE', #56556, #1304, #53610, .T. ) ;
#72768 = CARTESIAN_POINT ( 'NONE',  ( -12.61959663417972521, 80.89626266586573422, 129.9447639770759508 ) ) ;
#72769 = EDGE_CURVE ( 'NONE', #24182, #20410, #12767, .T. ) ;
#72770 = AXIS2_PLACEMENT_3D ( 'NONE', #8899, #37033, #59683 ) ;
#72771 = ORIENTED_EDGE ( 'NONE', *, *, #87405, .T. ) ;
#72772 = PLANE ( 'NONE',  #31598 ) ;
#72773 = EDGE_CURVE ( 'NONE', #19408, #44789, #5505, .T. ) ;
#72774 = ORIENTED_EDGE ( 'NONE', *, *, #15796, .F. ) ;
#72775 = CARTESIAN_POINT ( 'NONE',  ( 102.5037471771102986, -27.80297507283301428, 166.4518860084373557 ) ) ;
#72776 = CARTESIAN_POINT ( 'NONE',  ( 114.0075790447407087, -33.88846322102013175, 0.4256252759109769856 ) ) ;
#72777 = CARTESIAN_POINT ( 'NONE',  ( -103.1875000000000000, 117.4749999999999943, -5.041900000001080073 ) ) ;
#72778 = DIRECTION ( 'NONE',  ( 3.999999999999999995E-14, -1.000000000000000000, 4.100000000000000342E-29 ) ) ;
#72779 = ORIENTED_EDGE ( 'NONE', *, *, #40222, .T. ) ;
#72780 = CARTESIAN_POINT ( 'NONE',  ( 115.0549195170180639, -30.03079676387787345, 269.3813395616251682 ) ) ;
#72781 = CARTESIAN_POINT ( 'NONE',  ( 105.4141053104174830, -47.06688527371949249, 33.44991099019695469 ) ) ;
#72782 =( LENGTH_UNIT ( ) NAMED_UNIT ( * ) SI_UNIT ( .MILLI., .METRE. ) );
#72784 = FACE_OUTER_BOUND ( 'NONE', #32810, .T. ) ;
#72783 = CARTESIAN_POINT ( 'NONE',  ( 162.8913605087222436, -31.76306994223276092, 313.9678068554149490 ) ) ;
#72785 = PLANE ( 'NONE',  #38011 ) ;
#72786 = CARTESIAN_POINT ( 'NONE',  ( 70.56670390244700286, -68.87844715994098976, 55.21780685541800437 ) ) ;
#72787 = DIRECTION ( 'NONE',  ( 1.000000000000000000, 4.299999999999999979E-14, 1.000000000000000078E-15 ) ) ;
#72788 = EDGE_CURVE ( 'NONE', #34853, #35731, #86335, .T. ) ;
#72789 = DIRECTION ( 'NONE',  ( -1.000000000000000078E-15, 1.000000000000000000, -3.100000000000000044E-14 ) ) ;
#72790 = CARTESIAN_POINT ( 'NONE',  ( 97.81136857603131318, -40.51756142711754194, 161.6353372277744143 ) ) ;
#72791 = DIRECTION ( 'NONE',  ( 0.000000000000000000, 7.536132396315209176E-17, -1.000000000000000000 ) ) ;
#72792 = CARTESIAN_POINT ( 'NONE',  ( 116.7680724212777079, -31.33574231247038355, 29.24229194257799236 ) ) ;
#72793 = CARTESIAN_POINT ( 'NONE',  ( 106.4836140971313654, -24.89327890070114435, 191.1156252759109861 ) ) ;
#72794 = CARTESIAN_POINT ( 'NONE',  ( 112.8297475082234484, -27.27058933724656953, 45.62895860924398761 ) ) ;
#72795 = AXIS2_PLACEMENT_3D ( 'NONE', #49869, #21751, #63974 ) ;
#72797 = CARTESIAN_POINT ( 'NONE',  ( 179.4595971212889935, -28.98061976758940617, 342.9256252759119548 ) ) ;
#72796 = DIRECTION ( 'NONE',  ( 0.000000000000000000, 0.000000000000000000, 1.000000000000000000 ) ) ;
#72798 = CARTESIAN_POINT ( 'NONE',  ( 134.0664832912740110, -36.72944715994100306, -5.074374724089001809 ) ) ;
#72799 = CIRCLE ( 'NONE', #33635, 7.937500000000000000 ) ;
#72800 = VERTEX_POINT ( 'NONE', #19566 ) ;
#72801 = LINE ( 'NONE', #11008, #79587 ) ;
#72802 = ORIENTED_EDGE ( 'NONE', *, *, #31407, .F. ) ;
#72803 = CARTESIAN_POINT ( 'NONE',  ( 99.11394507416773081, -43.38496525699387973, 67.86895860924396118 ) ) ;
#72805 = ORIENTED_EDGE ( 'NONE', *, *, #66702, .F. ) ;
#72804 = CARTESIAN_POINT ( 'NONE',  ( 6.114111144840049583, 93.68330544519889713, 130.4128344644624917 ) ) ;
#72806 = CARTESIAN_POINT ( 'NONE',  ( 115.7827153205794133, -41.80297204315836268, 49.40639791532688463 ) ) ;
#72807 = CARTESIAN_POINT ( 'NONE',  ( 97.11708974113240345, -41.49110554365059045, 212.6937205140059461 ) ) ;
#72808 = DIRECTION ( 'NONE',  ( -1.000000000000000000, -3.999999999999999995E-14, -1.000000000000000078E-15 ) ) ;
#72809 = CARTESIAN_POINT ( 'NONE',  ( 99.08981748339620310, -42.79584291293824805, 146.8439966323671513 ) ) ;
#72810 = CARTESIAN_POINT ( 'NONE',  ( 57.91199999999999903, 20.32000000000000028, 191.3008000794699797 ) ) ;
#72811 = CARTESIAN_POINT ( 'NONE',  ( 163.2449138992999735, -32.11662333284611748, -5.074374724088000832 ) ) ;
#72812 = DIRECTION ( 'NONE',  ( 0.7071067811739274456, -0.7071067811991676999, 0.000000000000000000 ) ) ;
#72813 = FACE_OUTER_BOUND ( 'NONE', #69939, .T. ) ;
#72814 = CARTESIAN_POINT ( 'NONE',  ( 96.47668441219802560, -40.11591174724604514, 131.5727681330539554 ) ) ;
#72815 = ORIENTED_EDGE ( 'NONE', *, *, #79294, .T. ) ;
#72816 = EDGE_LOOP ( 'NONE', ( #37259, #76547, #77164, #82630, #29632, #7827 ) ) ;
#72817 = ADVANCED_FACE ( 'NONE', ( #62695 ), #57211, .F. ) ;
#72818 = CARTESIAN_POINT ( 'NONE',  ( 97.69004538871082843, -40.41090301495324155, 93.05586902018298190 ) ) ;
#72819 = AXIS2_PLACEMENT_3D ( 'NONE', #33973, #47595, #81268 ) ;
#72820 = DIRECTION ( 'NONE',  ( 0.7071067811865449082, 0.7071067811865501263, 7.071067811865448709E-16 ) ) ;
#72822 = DIRECTION ( 'NONE',  ( 0.000000000000000000, 1.000000000000000000, 0.000000000000000000 ) ) ;
#72821 = CARTESIAN_POINT ( 'NONE',  ( 105.2318265017784000, -27.12228994480481248, 231.2270538473389649 ) ) ;
#72823 = DIRECTION ( 'NONE',  ( 0.000000000000000000, 1.000000000000000000, 0.000000000000000000 ) ) ;
#72825 = EDGE_CURVE ( 'NONE', #73315, #4973, #84053, .T. ) ;
#72824 = DIRECTION ( 'NONE',  ( 0.000000000000000000, -1.000000000000000000, 0.000000000000000000 ) ) ;
#72826 = CARTESIAN_POINT ( 'NONE',  ( -41.60202597009397607, 40.59999999999997300, 54.66767516814134353 ) ) ;
#72827 = CARTESIAN_POINT ( 'NONE',  ( -0.8299567123207916008, 69.87023232701913855, 118.5538273271561707 ) ) ;
#72828 = PLANE ( 'NONE',  #84105 ) ;
#72829 = DIRECTION ( 'NONE',  ( 0.000000000000000000, 1.000000000000000000, 0.000000000000000000 ) ) ;
#72830 = CARTESIAN_POINT ( 'NONE',  ( 117.7567108552515265, -34.01230579303179979, 169.0365776568629599 ) ) ;
#72831 = ORIENTED_EDGE ( 'NONE', *, *, #44117, .T. ) ;
#72832 = AXIS2_PLACEMENT_3D ( 'NONE', #80501, #39148, #60020 ) ;
#72833 = EDGE_LOOP ( 'NONE', ( #33836, #84912 ) ) ;
#72834 = AXIS2_PLACEMENT_3D ( 'NONE', #37991, #29403, #37107 ) ;
#72835 = CYLINDRICAL_SURFACE ( 'NONE', #25554, 9.525000000000000355 ) ;
#72836 = CARTESIAN_POINT ( 'NONE',  ( 145.9076452860354891, -68.98966598118471438, 247.3116641508191549 ) ) ;
#72837 = CARTESIAN_POINT ( 'NONE',  ( 138.8167039024479834, -57.40094715994099772, 35.51780685541480409 ) ) ;
#72838 = CARTESIAN_POINT ( 'NONE',  ( 97.81169951533574647, -40.51743117454552134, 102.6356342116286413 ) ) ;
#72839 = ADVANCED_FACE ( 'NONE', ( #50854 ), #35427, .F. ) ;
#72840 = CARTESIAN_POINT ( 'NONE',  ( 141.9629299006807344, -9.772340378754462265, -5.074374724088959177 ) ) ;
#72841 = CARTESIAN_POINT ( 'NONE',  ( 103.5423316596719445, -26.88027146080960961, 190.3499109901969746 ) ) ;
#72842 = CARTESIAN_POINT ( 'NONE',  ( 136.3179110785846149, -38.31136518418494319, 7.339178645749313112 ) ) ;
#72843 = ORIENTED_EDGE ( 'NONE', *, *, #6641, .F. ) ;
#72845 = ORIENTED_EDGE ( 'NONE', *, *, #17301, .T. ) ;
#72844 = EDGE_LOOP ( 'NONE', ( #3241, #87612, #7252, #77634 ) ) ;
#72846 = CARTESIAN_POINT ( 'NONE',  ( 6.802569982901797644E-16, 69.84999999999999432, 118.5560000000000116 ) ) ;
#72847 = CARTESIAN_POINT ( 'NONE',  ( 130.5667039024479834, -36.72944715994100306, 239.5838068554162987 ) ) ;
#72848 = CARTESIAN_POINT ( 'NONE',  ( 132.2214349158019502, -34.68812225915852565, 7.662832107304482498 ) ) ;
#72849 = CARTESIAN_POINT ( 'NONE',  ( 110.4041361119612930, -44.93847832680074106, 279.3158690201827881 ) ) ;
#72850 = EDGE_CURVE ( 'NONE', #8395, #8413, #69968, .T. ) ;
#72851 = CARTESIAN_POINT ( 'NONE',  ( 50.97905606905900555, -31.62489322948711035, -5.074374724088000832 ) ) ;
#72852 = ORIENTED_EDGE ( 'NONE', *, *, #55628, .F. ) ;
#72853 = VECTOR ( 'NONE', #50219, 999.9999999999998863 ) ;
#72854 = DIRECTION ( 'NONE',  ( 0.000000000000000000, -1.000000000000000000, 0.000000000000000000 ) ) ;
#72855 = CARTESIAN_POINT ( 'NONE',  ( 70.06670390244707392, -137.6784471599409869, 55.21780685541800437 ) ) ;
#72856 = VERTEX_POINT ( 'NONE', #28166 ) ;
#72857 = ORIENTED_EDGE ( 'NONE', *, *, #37347, .F. ) ;
#72858 = CIRCLE ( 'NONE', #48197, 1.000000000000000888 ) ;
#72859 = CARTESIAN_POINT ( 'NONE',  ( -3.174999999999664979, 24.56180297284579694, 31.75000000000000000 ) ) ;
#72860 = ORIENTED_EDGE ( 'NONE', *, *, #2836, .T. ) ;
#72861 = ORIENTED_EDGE ( 'NONE', *, *, #3650, .F. ) ;
#72862 = CARTESIAN_POINT ( 'NONE',  ( 102.0657985602879592, -27.97123491610240720, 156.4896842834733661 ) ) ;
#72863 = CARTESIAN_POINT ( 'NONE',  ( 98.56159230830689921, -41.41319107723295900, 26.14956268521895311 ) ) ;
#72864 = CARTESIAN_POINT ( 'NONE',  ( 99.06899620534126427, -29.95238561887155981, 215.7670538473399517 ) ) ;
#72865 = CARTESIAN_POINT ( 'NONE',  ( 102.6254653968535990, -46.82603978519644272, 132.2346728949579528 ) ) ;
#72866 = DIRECTION ( 'NONE',  ( 0.000000000000000000, 0.000000000000000000, 1.000000000000000000 ) ) ;
#72867 = CARTESIAN_POINT ( 'NONE',  ( 105.7763715259175257, -26.38449191207581634, 266.1756252759109884 ) ) ;
#72868 = CARTESIAN_POINT ( 'NONE',  ( 109.6431669551641477, -46.48004783680506335, 98.78305064256221613 ) ) ;
#72869 = EDGE_CURVE ( 'NONE', #628, #59432, #27638, .T. ) ;
#72870 = DIRECTION ( 'NONE',  ( 0.000000000000000000, 1.000000000000000000, 0.000000000000000000 ) ) ;
#72871 = ORIENTED_EDGE ( 'NONE', *, *, #29909, .T. ) ;
#72872 = CIRCLE ( 'NONE', #77232, 9.571100913904354357 ) ;
#72873 = VERTEX_POINT ( 'NONE', #28621 ) ;
#72874 = AXIS2_PLACEMENT_3D ( 'NONE', #56435, #15121, #84628 ) ;
#72875 = CARTESIAN_POINT ( 'NONE',  ( 115.2864439380202271, -30.18849607537921997, 244.3613395616249875 ) ) ;
#72876 = ORIENTED_EDGE ( 'NONE', *, *, #67127, .T. ) ;
#72877 = CARTESIAN_POINT ( 'NONE',  ( 108.0069521509713297, -26.34547698190780451, 155.0041967044819557 ) ) ;
#72878 = DIRECTION ( 'NONE',  ( -7.136255983449500255E-16, 0.000000000000000000, -1.000000000000000000 ) ) ;
#72879 = DIRECTION ( 'NONE',  ( -1.000000000000000000, -1.000000000000000078E-15, 0.000000000000000000 ) ) ;
#72880 = FACE_OUTER_BOUND ( 'NONE', #47116, .T. ) ;
#72881 = CARTESIAN_POINT ( 'NONE',  ( 143.8111385288040651, -140.2566682859662706, 246.7635256640583918 ) ) ;
#72884 = CARTESIAN_POINT ( 'NONE',  ( 111.7292870705843342, -27.42961193919087748, 275.7070538473395800 ) ) ;
#72883 = CARTESIAN_POINT ( 'NONE',  ( 144.5667039024470171, -90.27844715994091018, 45.21780685541799727 ) ) ;
#72882 = DIRECTION ( 'NONE',  ( 0.7071067811865473507, 0.7071067811865476838, 0.000000000000000000 ) ) ;
#72885 = DIRECTION ( 'NONE',  ( 0.000000000000000000, 0.000000000000000000, -1.000000000000000000 ) ) ;
#72886 = LINE ( 'NONE', #31990, #72940 ) ;
#72887 = AXIS2_PLACEMENT_3D ( 'NONE', #7094, #34788, #22521 ) ;
#72888 = LINE ( 'NONE', #38360, #39733 ) ;
#72889 = ADVANCED_FACE ( 'NONE', ( #64497, #43131, #921, #84955, #29081, #71320 ), #42678, .T. ) ;
#72890 = DIRECTION ( 'NONE',  ( 5.512527431108029424E-15, -1.000000000000000000, 0.000000000000000000 ) ) ;
#72891 = EDGE_CURVE ( 'NONE', #34937, #29192, #29975, .T. ) ;
#72892 = CARTESIAN_POINT ( 'NONE',  ( 45.66030316258350297, 82.54999999999999716, 346.9005000000000223 ) ) ;
#72893 = CARTESIAN_POINT ( 'NONE',  ( 107.0664832912739968, -36.72944715994100306, 287.6356252759109680 ) ) ;
#72895 = VERTEX_POINT ( 'NONE', #8644 ) ;
#72894 = CARTESIAN_POINT ( 'NONE',  ( 98.65276261104773425, -37.10273558558598239, 195.5838068554173788 ) ) ;
#72896 = DIRECTION ( 'NONE',  ( -1.000000000000000000, -1.734723475976808672E-15, 0.000000000000000000 ) ) ;
#72897 = CARTESIAN_POINT ( 'NONE',  ( 96.03049237414208505, -35.77952841945960216, 186.2461014663869889 ) ) ;
#72898 = CARTESIAN_POINT ( 'NONE',  ( 111.9288574835248511, -27.50774424443475397, 55.68991099019693536 ) ) ;
#72899 = CARTESIAN_POINT ( 'NONE',  ( 99.72256515790628839, -29.26889448616327982, 221.6956252759109702 ) ) ;
#72900 = DIRECTION ( 'NONE',  ( 1.000000000000000078E-15, -1.000000000000000083E-30, -1.000000000000000000 ) ) ;
#72901 = CARTESIAN_POINT ( 'NONE',  ( 53.56670390244828184, -48.82844715994055917, 300.4678068554150059 ) ) ;
#72903 = CARTESIAN_POINT ( 'NONE',  ( 117.0747869972543782, -37.01281407854411043, 39.80368068565672246 ) ) ;
#72902 = DIRECTION ( 'NONE',  ( 0.000000000000000000, 1.000000000000000000, 0.000000000000000000 ) ) ;
#72904 = FACE_BOUND ( 'NONE', #25370, .T. ) ;
#72905 = DIRECTION ( 'NONE',  ( -0.7071067812159698152, -0.7071067811571253303, -7.071067812159691855E-16 ) ) ;
#72906 = CARTESIAN_POINT ( 'NONE',  ( 36.23715912545429063, -47.82818131006125384, 237.4678068554150059 ) ) ;
#72907 = VERTEX_POINT ( 'NONE', #70418 ) ;
#72908 = EDGE_LOOP ( 'NONE', ( #84718, #46143, #26160, #14768, #87249, #39067 ) ) ;
#72909 = CARTESIAN_POINT ( 'NONE',  ( 109.5993548714604060, -44.88669505861042808, 97.23813411379100557 ) ) ;
#72911 = ORIENTED_EDGE ( 'NONE', *, *, #23651, .F. ) ;
#72910 = CARTESIAN_POINT ( 'NONE',  ( 173.9900000000000091, 28.98850000000000193, -7.937500000000000000 ) ) ;
#72912 = CARTESIAN_POINT ( 'NONE',  ( 103.2867953297129873, -47.09177226061134292, 93.28610146638693834 ) ) ;
#72913 = DIRECTION ( 'NONE',  ( 1.000000000000000078E-15, -1.000000000000000000, 0.000000000000000000 ) ) ;
#72914 = LINE ( 'NONE', #10682, #32617 ) ;
#72915 = CARTESIAN_POINT ( 'NONE',  ( 108.4174892645027910, -26.73503592953050045, 175.9689586082560027 ) ) ;
#72916 = CARTESIAN_POINT ( 'NONE',  ( 97.00695627739551696, -39.24785929248557892, 16.53372051400697629 ) ) ;
#72917 = VERTEX_POINT ( 'NONE', #49947 ) ;
#72918 = VERTEX_POINT ( 'NONE', #8188 ) ;
#72919 = ORIENTED_EDGE ( 'NONE', *, *, #39135, .F. ) ;
#72920 = VECTOR ( 'NONE', #2369, 1000.000000000000000 ) ;
#72921 = CARTESIAN_POINT ( 'NONE',  ( 124.9629318080292393, -56.47944715994101728, -5.074374724089012467 ) ) ;
#72922 = CARTESIAN_POINT ( 'NONE',  ( 107.0664832912748068, -36.72944715993923381, -5.074374724089029343 ) ) ;
#72923 = DIRECTION ( 'NONE',  ( -0.000000000000000000, 1.000000000000000000, -0.000000000000000000 ) ) ;
#72924 = DIRECTION ( 'NONE',  ( -1.000000000000000000, -4.299999999999999979E-14, -1.000000000000000078E-15 ) ) ;
#72925 = LINE ( 'NONE', #72048, #46107 ) ;
#72926 = CARTESIAN_POINT ( 'NONE',  ( 4.084841600441663445, 70.51762400537137410, -130.4926920574403937 ) ) ;
#72927 = LINE ( 'NONE', #38403, #76480 ) ;
#72928 = CARTESIAN_POINT ( 'NONE',  ( -8.592341146638979410, 91.91841160240160491, 130.2735359644163395 ) ) ;
#72929 = CARTESIAN_POINT ( 'NONE',  ( 99.31004196827748842, -43.71529311364911763, 56.90991099019593236 ) ) ;
#72930 = ORIENTED_EDGE ( 'NONE', *, *, #27074, .F. ) ;
#72931 = ORIENTED_EDGE ( 'NONE', *, *, #83144, .F. ) ;
#72932 = CARTESIAN_POINT ( 'NONE',  ( 8.391680458684335875, 92.11847147219766896, 130.2873503055691344 ) ) ;
#72933 = FACE_OUTER_BOUND ( 'NONE', #60727, .T. ) ;
#72934 = CARTESIAN_POINT ( 'NONE',  ( 106.6465955684521418, -26.33791012980835333, 322.9014499992877631 ) ) ;
#72935 = CARTESIAN_POINT ( 'NONE',  ( 115.4711811475381467, -34.66499115051416169, 161.8242808457819706 ) ) ;
#72936 = CIRCLE ( 'NONE', #35267, 2.750000000000002665 ) ;
#72937 = EDGE_CURVE ( 'NONE', #23005, #5529, #35880, .T. ) ;
#72938 = EDGE_CURVE ( 'NONE', #15987, #16664, #36341, .T. ) ;
#72939 = B_SPLINE_CURVE_WITH_KNOTS ( 'NONE', 3,
 ( #46229, #67595, #76997, #4923, #53936, #73964, #11742, #88942, #81694, #47127, #14779, #83817, #39440, #88051, #80795, #21134, #21591, #87596 ),
 .UNSPECIFIED., .F., .F.,
 ( 4, 2, 2, 2, 2, 2, 2, 2, 4 ),
 ( 0.4999639890268276488, 0.5624684903984742412, 0.6249729917701207782, 0.6874774931417673152, 0.7499819945134138521, 0.8124864958850603891, 0.8749909972567069261, 0.9374954986283534630, 1.000000000000000000 ),
 .UNSPECIFIED. ) ;
#72940 = VECTOR ( 'NONE', #17042, 1000.000000000000000 ) ;
#72941 = CARTESIAN_POINT ( 'NONE',  ( 87.31648329127403940, -54.62589567669624557, -5.074374724089048883 ) ) ;
#72942 = ORIENTED_EDGE ( 'NONE', *, *, #60384, .T. ) ;
#72943 = ORIENTED_EDGE ( 'NONE', *, *, #84881, .T. ) ;
#72944 = EDGE_CURVE ( 'NONE', #83829, #15300, #42239, .T. ) ;
#72945 = DIRECTION ( 'NONE',  ( 1.000000000000000078E-15, 1.000000000000000083E-30, -1.000000000000000000 ) ) ;
#72946 = ORIENTED_EDGE ( 'NONE', *, *, #42702, .T. ) ;
#72947 = VERTEX_POINT ( 'NONE', #29528 ) ;
#72948 = CARTESIAN_POINT ( 'NONE',  ( 0.000000000000000000, 101.5999999999999943, 0.000000000000000000 ) ) ;
#72949 = EDGE_CURVE ( 'NONE', #16561, #36943, #13128, .T. ) ;
#72950 = CARTESIAN_POINT ( 'NONE',  ( 116.1725082674369816, -34.41496348756209755, 165.4682499725639957 ) ) ;
#72951 = EDGE_CURVE ( 'NONE', #51499, #14684, #20392, .T. ) ;
#72952 = CARTESIAN_POINT ( 'NONE',  ( 136.8164832912740110, -36.72944715994100306, -5.074374724088999145 ) ) ;
#72953 = CARTESIAN_POINT ( 'NONE',  ( 97.81170242524891023, -40.51743837274789684, 121.6354095930283137 ) ) ;
#72954 = EDGE_CURVE ( 'NONE', #78791, #71161, #87105, .T. ) ;
#72955 = CARTESIAN_POINT ( 'NONE',  ( 97.92338993004062786, -40.78105876605869184, 16.65841519439857876 ) ) ;
#72956 = ORIENTED_EDGE ( 'NONE', *, *, #77502, .F. ) ;
#72957 = AXIS2_PLACEMENT_3D ( 'NONE', #59033, #71801, #30463 ) ;
#72958 = ORIENTED_EDGE ( 'NONE', *, *, #50031, .F. ) ;
#72959 = ORIENTED_EDGE ( 'NONE', *, *, #76438, .F. ) ;
#72960 = EDGE_CURVE ( 'NONE', #53086, #10966, #21369, .T. ) ;
#72961 = CARTESIAN_POINT ( 'NONE',  ( 100.8178804068425904, -31.43438811971037339, 213.5852332267339762 ) ) ;
#72963 = CARTESIAN_POINT ( 'NONE',  ( 103.2708046866033129, -47.13561192255075838, 97.28610146638693834 ) ) ;
#72962 = AXIS2_PLACEMENT_3D ( 'NONE', #21544, #49668, #34705 ) ;
#72964 = CARTESIAN_POINT ( 'NONE',  ( 110.3650187231686743, -47.25482062520524096, 52.80610146638697699 ) ) ;
#72965 = CARTESIAN_POINT ( 'NONE',  ( 112.7690144390553257, -28.67084679305116524, 249.5838068554166682 ) ) ;
#72966 = CARTESIAN_POINT ( 'NONE',  ( -465.6921742093550165, 47.62500000000000000, -3.174999999999999822 ) ) ;
#72967 = LINE ( 'NONE', #23511, #12723 ) ;
#72968 = CARTESIAN_POINT ( 'NONE',  ( 98.09065366798802188, -42.10120877535955231, 157.7556252759109725 ) ) ;
#72969 = EDGE_CURVE ( 'NONE', #52054, #49269, #36334, .T. ) ;
#72970 = DIRECTION ( 'NONE',  ( 0.7071067811865160424, 0.7071067811865791031, 0.000000000000000000 ) ) ;
#72971 = ORIENTED_EDGE ( 'NONE', *, *, #26899, .T. ) ;
#72972 = FACE_OUTER_BOUND ( 'NONE', #79793, .T. ) ;
#72973 = ORIENTED_EDGE ( 'NONE', *, *, #35833, .T. ) ;
#72974 = EDGE_LOOP ( 'NONE', ( #705, #53899, #13858, #36131 ) ) ;
#72975 = CARTESIAN_POINT ( 'NONE',  ( 68.69171528984767860, -139.3034585473416769, 245.6607614303540004 ) ) ;
#72976 = FACE_BOUND ( 'NONE', #13735, .T. ) ;
#72977 = ORIENTED_EDGE ( 'NONE', *, *, #69580, .T. ) ;
#72978 = AXIS2_PLACEMENT_3D ( 'NONE', #28807, #49674, #41073 ) ;
#72979 = DIRECTION ( 'NONE',  ( 2.900000000000000265E-14, -2.000000000000000155E-15, 1.000000000000000000 ) ) ;
#72980 = VERTEX_POINT ( 'NONE', #38555 ) ;
#72981 = CARTESIAN_POINT ( 'NONE',  ( 105.9042722318897063, -26.76946864612742871, 131.1688829675021850 ) ) ;
#72982 = CARTESIAN_POINT ( 'NONE',  ( 100.9409889914183225, -46.87433776650586736, 52.14419670448194921 ) ) ;
#72983 = LINE ( 'NONE', #67066, #73613 ) ;
#72984 = CARTESIAN_POINT ( 'NONE',  ( 164.9190312289458120, -35.91149509760592906, 237.4678068554150059 ) ) ;
#72985 = LINE ( 'NONE', #79382, #28152 ) ;
#72986 = CARTESIAN_POINT ( 'NONE',  ( 98.65123886609826798, -31.74476095556097377, 85.90133956162593165 ) ) ;
#72988 = CARTESIAN_POINT ( 'NONE',  ( 117.0473132972741013, -39.66401662079133672, 179.5984824187679294 ) ) ;
#72987 = CARTESIAN_POINT ( 'NONE',  ( 72.06648329127401098, -45.72944715994106701, 14.67562527591093513 ) ) ;
#72989 = CARTESIAN_POINT ( 'NONE',  ( 104.4871046023747141, -26.97959138088134168, 60.28169211698992314 ) ) ;
#72990 = CARTESIAN_POINT ( 'NONE',  ( 51.56670390244899949, -32.29483332968430886, 342.9256252759109884 ) ) ;
#72991 = EDGE_LOOP ( 'NONE', ( #35590, #28586 ) ) ;
#72992 = CARTESIAN_POINT ( 'NONE',  ( 19.56670390244824631, -47.82844715994191631, 300.4678068554150059 ) ) ;
#72993 = EDGE_CURVE ( 'NONE', #79585, #19595, #18114, .T. ) ;
#72994 = DIRECTION ( 'NONE',  ( -1.175184669632759901E-16, 1.000000000000000000, 2.000000000000003705E-15 ) ) ;
#72995 = EDGE_CURVE ( 'NONE', #28990, #65875, #62451, .T. ) ;
#72996 = FACE_OUTER_BOUND ( 'NONE', #15745, .T. ) ;
#72997 = EDGE_CURVE ( 'NONE', #42899, #88172, #44918, .T. ) ;
#72998 = CARTESIAN_POINT ( 'NONE',  ( 48.16670390244701139, -26.71338133339251542, -5.074374724088000832 ) ) ;
#73000 = ORIENTED_EDGE ( 'NONE', *, *, #22707, .F. ) ;
#72999 = CARTESIAN_POINT ( 'NONE',  ( 117.2706010548463667, -41.09852764615815346, 213.5165776568629781 ) ) ;
#73001 = CARTESIAN_POINT ( 'NONE',  ( 97.81070293921875702, -40.51501671228320589, 146.6354177189882932 ) ) ;
#73002 = CARTESIAN_POINT ( 'NONE',  ( 97.20328444759655895, -40.27860260594448505, 262.6013395616254797 ) ) ;
#73003 = CARTESIAN_POINT ( 'NONE',  ( 108.9928688995437653, -47.66043690685247469, 118.7032443235299723 ) ) ;
#73004 = EDGE_CURVE ( 'NONE', #57751, #75328, #10415, .T. ) ;
#73005 = CARTESIAN_POINT ( 'NONE',  ( 113.2492937776126922, -28.76157751642139360, 250.5554876614661737 ) ) ;
#73006 = CARTESIAN_POINT ( 'NONE',  ( 82.56634656606027534, -37.87725565066433120, 7.080220459961196866 ) ) ;
#73007 = DIRECTION ( 'NONE',  ( 8.538276166416950255E-16, -1.000000000000000000, 3.100000000000000044E-14 ) ) ;
#73008 = LINE ( 'NONE', #79852, #3229 ) ;
#73009 = ORIENTED_EDGE ( 'NONE', *, *, #41909, .F. ) ;
#73010 = CIRCLE ( 'NONE', #3442, 7.937500000000000000 ) ;
#73011 = VECTOR ( 'NONE', #79146, 1000.000000000000000 ) ;
#73012 = ORIENTED_EDGE ( 'NONE', *, *, #78679, .T. ) ;
#73013 = ORIENTED_EDGE ( 'NONE', *, *, #38150, .T. ) ;
#73014 = ORIENTED_EDGE ( 'NONE', *, *, #37541, .T. ) ;
#73015 = CARTESIAN_POINT ( 'NONE',  ( 113.1782937634553576, -44.75186859869646838, 73.09395860846349535 ) ) ;
#73016 = CARTESIAN_POINT ( 'NONE',  ( 116.3171286962602267, -41.53660429022799150, 284.4441967044824082 ) ) ;
#73017 = LINE ( 'NONE', #3098, #57717 ) ;
#73018 = CARTESIAN_POINT ( 'NONE',  ( 132.9420963948878125, -34.21971364483388811, 1.822997995688940165 ) ) ;
#73020 = CARTESIAN_POINT ( 'NONE',  ( 80.59807192910871265, 70.66242608954391358, 86.94609723791424472 ) ) ;
#73019 = CARTESIAN_POINT ( 'NONE',  ( 80.06648329127399677, 0.2215528400590013880, 293.6356252759119911 ) ) ;
#73021 = CARTESIAN_POINT ( 'NONE',  ( 103.9834678596679538, -28.76382429851063449, 214.7924198280769872 ) ) ;
#73022 = ORIENTED_EDGE ( 'NONE', *, *, #74527, .F. ) ;
#73023 = ORIENTED_EDGE ( 'NONE', *, *, #22766, .F. ) ;
#73024 = ORIENTED_EDGE ( 'NONE', *, *, #424, .T. ) ;
#73025 = CARTESIAN_POINT ( 'NONE',  ( 107.0664832912739968, -18.82844715994099971, 168.9256252759119832 ) ) ;
#73026 = VECTOR ( 'NONE', #53438, 1000.000000000000000 ) ;
#73027 = DIRECTION ( 'NONE',  ( 0.7071067811989676377, 0.7071067811741275078, 7.071067811989670636E-16 ) ) ;
#73028 = CYLINDRICAL_SURFACE ( 'NONE', #62012, 2.117000000000007987 ) ;
#73029 = CARTESIAN_POINT ( 'NONE',  ( 98.59875070808803343, -39.34206841476268579, 17.99586902018296541 ) ) ;
#73030 = CARTESIAN_POINT ( 'NONE',  ( 117.9438598201575843, 86.63388195152280957, -12.03269986015406445 ) ) ;
#73031 = VECTOR ( 'NONE', #15062, 1000.000000000000000 ) ;
#73032 = CARTESIAN_POINT ( 'NONE',  ( 50.97905606903279363, -31.62489322948217918, 193.9678068554150911 ) ) ;
#73033 = FACE_OUTER_BOUND ( 'NONE', #45657, .T. ) ;
#73034 = VERTEX_POINT ( 'NONE', #58549 ) ;
#73035 = CYLINDRICAL_SURFACE ( 'NONE', #9827, 0.4999999999999933387 ) ;
#73036 = ORIENTED_EDGE ( 'NONE', *, *, #52215, .F. ) ;
#73037 = LINE ( 'NONE', #30379, #72750 ) ;
#73038 = CARTESIAN_POINT ( 'NONE',  ( 106.6371065190374452, -28.08557299187883061, 42.94618560768698501 ) ) ;
#73039 = AXIS2_PLACEMENT_3D ( 'NONE', #54375, #82144, #19442 ) ;
#73040 = CARTESIAN_POINT ( 'NONE',  ( 135.6272734918656511, -16.46583755400462579, 7.833212107638488853 ) ) ;
#73041 = EDGE_CURVE ( 'NONE', #52002, #15093, #8305, .T. ) ;
#73042 = CYLINDRICAL_SURFACE ( 'NONE', #69354, 0.5000000000000197620 ) ;
#73043 = CARTESIAN_POINT ( 'NONE',  ( -11.75180001297214183, 87.41805222750765836, 117.9724353609281593 ) ) ;
#73044 = ORIENTED_EDGE ( 'NONE', *, *, #49056, .F. ) ;
#73045 = LINE ( 'NONE', #66682, #52265 ) ;
#73046 = ADVANCED_FACE ( 'NONE', ( #58984 ), #84202, .F. ) ;
#73047 = CARTESIAN_POINT ( 'NONE',  ( 119.7028791468282947, 54.86242404270847572, -52.11625092004412352 ) ) ;
#73048 = VERTEX_POINT ( 'NONE', #85849 ) ;
#73049 = CARTESIAN_POINT ( 'NONE',  ( 113.9865487620526920, -28.11017913222394071, 119.5261014663869474 ) ) ;
#73050 = EDGE_LOOP ( 'NONE', ( #71403, #24309, #56474, #87011 ) ) ;
#73051 = CARTESIAN_POINT ( 'NONE',  ( 98.78342310422263495, -33.06835657602663758, 55.40575316140994033 ) ) ;
#73052 = EDGE_CURVE ( 'NONE', #79236, #4014, #52160, .T. ) ;
#73053 = FACE_OUTER_BOUND ( 'NONE', #48376, .T. ) ;
#73054 = CARTESIAN_POINT ( 'NONE',  ( 97.10642131522254772, -35.22350214559244819, 67.63872616303994789 ) ) ;
#73055 = CARTESIAN_POINT ( 'NONE',  ( -22.91010569159546151, 50.47404986067924426, 30.44291311365987340 ) ) ;
#73056 = EDGE_CURVE ( 'NONE', #26477, #57212, #73078, .T. ) ;
#73057 = CARTESIAN_POINT ( 'NONE',  ( 72.96458098368701428, 127.0000000000000000, -72.96458098368670164 ) ) ;
#73058 = CYLINDRICAL_SURFACE ( 'NONE', #13530, 0.5000000000000004441 ) ;
#73059 = CARTESIAN_POINT ( 'NONE',  ( 116.7902211891048694, -31.42528581690661582, 20.21181575210195902 ) ) ;
#73061 = ADVANCED_FACE ( 'NONE', ( #66250 ), #16792, .F. ) ;
#73060 = CARTESIAN_POINT ( 'NONE',  ( 3.968750000000050182, 120.6499999999999915, -100.8961411191535973 ) ) ;
#73062 = ORIENTED_EDGE ( 'NONE', *, *, #72057, .T. ) ;
#73063 = VECTOR ( 'NONE', #43725, 1000.000000000000000 ) ;
#73064 = CARTESIAN_POINT ( 'NONE',  ( 25.56670390244797275, -62.87844715994099687, 178.0928068554149775 ) ) ;
#73065 = ORIENTED_EDGE ( 'NONE', *, *, #24099, .T. ) ;
#73066 = CARTESIAN_POINT ( 'NONE',  ( -118.1052048222230155, 75.15251084995274766, 10.33146714902738061 ) ) ;
#73067 = AXIS2_PLACEMENT_3D ( 'NONE', #29090, #71768, #77687 ) ;
#73068 = VERTEX_POINT ( 'NONE', #4042 ) ;
#73069 = ORIENTED_EDGE ( 'NONE', *, *, #25378, .F. ) ;
#73070 = ADVANCED_FACE ( 'NONE', ( #62132 ), #6726, .T. ) ;
#73071 = DIRECTION ( 'NONE',  ( 0.000000000000000000, 0.000000000000000000, 1.000000000000000000 ) ) ;
#73072 = VERTEX_POINT ( 'NONE', #11759 ) ;
#73073 = CARTESIAN_POINT ( 'NONE',  ( 101.0349934672010903, -27.38958028709080139, 220.5327681330539633 ) ) ;
#73074 = DIRECTION ( 'NONE',  ( 0.000000000000000000, 0.000000000000000000, -1.000000000000000000 ) ) ;
#73075 = CARTESIAN_POINT ( 'NONE',  ( 112.7812478461076040, -67.87844715994094713, 245.8358747327640117 ) ) ;
#73076 = CARTESIAN_POINT ( 'NONE',  ( 106.5180998683148488, -25.68982506017174927, 41.12800622829193742 ) ) ;
#73077 = ADVANCED_FACE ( 'NONE', ( #27615 ), #47145, .T. ) ;
#73078 = LINE ( 'NONE', #79027, #61017 ) ;
#73079 = ORIENTED_EDGE ( 'NONE', *, *, #25606, .T. ) ;
#73080 = CARTESIAN_POINT ( 'NONE',  ( 103.2795865501787773, -27.47421004149664014, 171.3855331769660495 ) ) ;
#73081 = CARTESIAN_POINT ( 'NONE',  ( 90.44969454456439450, -53.34645651782491882, 249.5838068554174640 ) ) ;
#73083 = ORIENTED_EDGE ( 'NONE', *, *, #80691, .F. ) ;
#73082 = ADVANCED_FACE ( 'NONE', ( #67156 ), #10195, .T. ) ;
#73084 = DIRECTION ( 'NONE',  ( 0.4999999999999998890, -0.8660254037844387076, 0.000000000000000000 ) ) ;
#73085 = VECTOR ( 'NONE', #65215, 1000.000000000000000 ) ;
#73086 = CARTESIAN_POINT ( 'NONE',  ( 72.06648329127399677, -9.729447159941065237, -4.824374724089063982 ) ) ;
#73087 = CARTESIAN_POINT ( 'NONE',  ( 112.4005920293390233, -46.38403708128156921, 252.9661014663871583 ) ) ;
#73088 = DIRECTION ( 'NONE',  ( 1.000000000000000078E-15, -1.000000000000000083E-30, -1.000000000000000000 ) ) ;
#73089 = AXIS2_PLACEMENT_3D ( 'NONE', #39362, #17585, #3065 ) ;
#73090 = CARTESIAN_POINT ( 'NONE',  ( 188.5667039024479834, -62.87844715994099687, 298.0928068554150627 ) ) ;
#73091 = CARTESIAN_POINT ( 'NONE',  ( 77.40046754268347229, -37.42701295173601039, 2.979899338979277612 ) ) ;
#73092 = CARTESIAN_POINT ( 'NONE',  ( 116.1125752699382048, -36.30413522796790460, 268.2743245899816884 ) ) ;
#73094 = CARTESIAN_POINT ( 'NONE',  ( 117.9659426345831719, -38.42225801833666310, 64.69181575210097890 ) ) ;
#73093 = CARTESIAN_POINT ( 'NONE',  ( 143.0664832912740110, -18.82844715994099971, -5.074374724088000832 ) ) ;
#73095 = CARTESIAN_POINT ( 'NONE',  ( 112.5527812704730337, 67.77553021976281400, 66.15876282107061002 ) ) ;
#73096 = CARTESIAN_POINT ( 'NONE',  ( 95.73117830242222226, -40.35431382354642693, 131.5727681330539554 ) ) ;
#73097 = EDGE_LOOP ( 'NONE', ( #20293, #47893 ) ) ;
#73098 = CARTESIAN_POINT ( 'NONE',  ( 1.166476076187854022E-15, 125.7300000000000040, -9.525000000000000355 ) ) ;
#73099 = ORIENTED_EDGE ( 'NONE', *, *, #7749, .F. ) ;
#73100 = LINE ( 'NONE', #36006, #49655 ) ;
#73101 = VECTOR ( 'NONE', #28012, 1000.000000000000000 ) ;
#73102 = DIRECTION ( 'NONE',  ( 1.000000000000000000, 8.673617379883546378E-16, 9.757819552368989676E-16 ) ) ;
#73103 = PLANE ( 'NONE',  #19513 ) ;
#73104 = ORIENTED_EDGE ( 'NONE', *, *, #85933, .T. ) ;
#73105 = EDGE_CURVE ( 'NONE', #74526, #55378, #5870, .T. ) ;
#73106 = DIRECTION ( 'NONE',  ( 0.000000000000000000, 1.000000000000000000, 0.000000000000000000 ) ) ;
#73108 = ORIENTED_EDGE ( 'NONE', *, *, #31325, .F. ) ;
#73107 = CARTESIAN_POINT ( 'NONE',  ( 101.7334424669833339, -26.99437863453528408, 100.4632443235299633 ) ) ;
#73109 = CARTESIAN_POINT ( 'NONE',  ( 3.174999999999879918, 8.255000000000000782, -33.98325472291465132 ) ) ;
#73110 = EDGE_CURVE ( 'NONE', #47557, #60931, #79859, .T. ) ;
#73111 = DIRECTION ( 'NONE',  ( -1.000000000000000000, 0.000000000000000000, 0.000000000000000000 ) ) ;
#73112 = DIRECTION ( 'NONE',  ( 0.000000000000000000, 0.000000000000000000, 1.000000000000000000 ) ) ;
#73113 = ORIENTED_EDGE ( 'NONE', *, *, #23367, .T. ) ;
#73114 = CARTESIAN_POINT ( 'NONE',  ( 108.0362122550155135, -25.69517931502184993, 109.9946728949589811 ) ) ;
#73115 = FACE_OUTER_BOUND ( 'NONE', #43460, .T. ) ;
#73116 = DIRECTION ( 'NONE',  ( 0.000000000000000000, 0.000000000000000000, -1.000000000000000000 ) ) ;
#73117 = ORIENTED_EDGE ( 'NONE', *, *, #47105, .F. ) ;
#73118 = ORIENTED_EDGE ( 'NONE', *, *, #30789, .T. ) ;
#73119 = DIRECTION ( 'NONE',  ( 1.000000000000000000, 0.000000000000000000, 0.000000000000000000 ) ) ;
#73120 = DIRECTION ( 'NONE',  ( -0.7071067811865470176, 0.000000000000000000, -0.7071067811865480168 ) ) ;
#73121 = DIRECTION ( 'NONE',  ( 0.000000000000000000, 1.000000000000000000, 0.000000000000000000 ) ) ;
#73123 = DIRECTION ( 'NONE',  ( -1.000000000000000000, -0.000000000000000000, -0.000000000000000000 ) ) ;
#73122 = DIRECTION ( 'NONE',  ( -0.7071067811865175967, -0.7071067811865774377, -7.071067811865168663E-16 ) ) ;
#73124 = CARTESIAN_POINT ( 'NONE',  ( 138.8167039024479834, -50.82844715994100682, 60.91780685541480267 ) ) ;
#73126 = EDGE_CURVE ( 'NONE', #834, #35753, #1523, .T. ) ;
#73125 = VECTOR ( 'NONE', #14387, 1000.000000000000000 ) ;
#73127 = ORIENTED_EDGE ( 'NONE', *, *, #82576, .T. ) ;
#73128 = VECTOR ( 'NONE', #84077, 1000.000000000000000 ) ;
#73129 = PLANE ( 'NONE',  #20118 ) ;
#73130 = CARTESIAN_POINT ( 'NONE',  ( 96.72778144249465981, -35.92320320382071230, 187.2765776568629406 ) ) ;
#73132 = ORIENTED_EDGE ( 'NONE', *, *, #23752, .T. ) ;
#73131 = CARTESIAN_POINT ( 'NONE',  ( 255.9983484187079910, 65.43750000000000000, 10.66800000000000104 ) ) ;
#73133 = CARTESIAN_POINT ( 'NONE',  ( 101.5072281473882612, -27.97539281467255279, 61.51467289495899138 ) ) ;
#73134 = CARTESIAN_POINT ( 'NONE',  ( 99.50486818388880295, -43.30594552113949192, 51.89608593702373440 ) ) ;
#73135 = CARTESIAN_POINT ( 'NONE',  ( 3.968749999999215294, 120.6499999999999915, 105.4788588808464027 ) ) ;
#73136 = CARTESIAN_POINT ( 'NONE',  ( 116.3201356630459884, -32.94258242523766711, 69.13562527591093954 ) ) ;
#73137 = ORIENTED_EDGE ( 'NONE', *, *, #60123, .F. ) ;
#73138 = CYLINDRICAL_SURFACE ( 'NONE', #67499, 11.45913725231036118 ) ;
#73139 = ORIENTED_EDGE ( 'NONE', *, *, #47418, .T. ) ;
#73140 = ORIENTED_EDGE ( 'NONE', *, *, #30594, .T. ) ;
#73141 = EDGE_CURVE ( 'NONE', #50262, #38273, #55298, .T. ) ;
#73142 = CARTESIAN_POINT ( 'NONE',  ( 100.4550560919867479, -30.82882778563945791, 187.1787261630399541 ) ) ;
#73143 = CARTESIAN_POINT ( 'NONE',  ( 117.0614819080372655, -38.07633510806910948, 54.71886380986607890 ) ) ;
#73144 = AXIS2_PLACEMENT_3D ( 'NONE', #49827, #28494, #48464 ) ;
#73145 = CARTESIAN_POINT ( 'NONE',  ( -86.19179098795268601, 92.11674985319540099, 98.06216817836288158 ) ) ;
#73146 = AXIS2_PLACEMENT_3D ( 'NONE', #21626, #42037, #1631 ) ;
#73147 = EDGE_CURVE ( 'NONE', #13607, #20681, #11518, .T. ) ;
#73148 = ADVANCED_FACE ( 'NONE', ( #5847 ), #33536, .F. ) ;
#73149 = DIRECTION ( 'NONE',  ( 0.000000000000000000, 1.000000000000000000, 0.000000000000000000 ) ) ;
#73150 = CARTESIAN_POINT ( 'NONE',  ( -487.2989999999999782, 86.51875000000001137, 94.61194598552339130 ) ) ;
#73151 = CIRCLE ( 'NONE', #33994, 6.349999999999999645 ) ;
#73152 = VERTEX_POINT ( 'NONE', #40792 ) ;
#73153 = LINE ( 'NONE', #32261, #63871 ) ;
#73155 = EDGE_CURVE ( 'NONE', #31941, #47853, #61235, .T. ) ;
#73154 = AXIS2_PLACEMENT_3D ( 'NONE', #26554, #27447, #46971 ) ;
#73156 = CARTESIAN_POINT ( 'NONE',  ( 97.31317918327525263, -38.96105433417827157, 37.50518654075179370 ) ) ;
#73157 = ORIENTED_EDGE ( 'NONE', *, *, #55287, .F. ) ;
#73158 = CARTESIAN_POINT ( 'NONE',  ( 101.6088808140983417, -47.24878093606274376, 17.19562527591095247 ) ) ;
#73159 = CARTESIAN_POINT ( 'NONE',  ( 12.61763483057320911, 84.21901225747508590, 117.8827707503577074 ) ) ;
#73160 = ORIENTED_EDGE ( 'NONE', *, *, #26429, .F. ) ;
#73161 = ADVANCED_FACE ( 'NONE', ( #53500 ), #81266, .T. ) ;
#73162 = CARTESIAN_POINT ( 'NONE',  ( 131.3179999999999836, 44.45000000000000284, 32.49205688096009936 ) ) ;
#73163 = CARTESIAN_POINT ( 'NONE',  ( -31.75000000000000000, 17.78000000000000114, 3.175000000000219647 ) ) ;
#73164 = CARTESIAN_POINT ( 'NONE',  ( 46.48091746482045750, -49.32844715994088602, 180.4678068554150911 ) ) ;
#73165 = CARTESIAN_POINT ( 'NONE',  ( 101.3252678580387709, -46.22870732629148449, 198.1318157521009482 ) ) ;
#73166 = DIRECTION ( 'NONE',  ( 0.000000000000000000, 1.000000000000000000, 5.463695987328529395E-16 ) ) ;
#73167 = EDGE_CURVE ( 'NONE', #82506, #32225, #68513, .T. ) ;
#73168 = ORIENTED_EDGE ( 'NONE', *, *, #12658, .F. ) ;
#73169 = CARTESIAN_POINT ( 'NONE',  ( 107.8717034087400322, -26.29179415218835913, 66.01562527591097762 ) ) ;
#73170 = CARTESIAN_POINT ( 'NONE',  ( 87.31648329127401098, -46.47944715994105280, 14.92562527591095112 ) ) ;
#73171 = ORIENTED_EDGE ( 'NONE', *, *, #45905, .F. ) ;
#73172 = ORIENTED_EDGE ( 'NONE', *, *, #38401, .F. ) ;
#73173 = EDGE_CURVE ( 'NONE', #26208, #71209, #63959, .T. ) ;
#73174 = CARTESIAN_POINT ( 'NONE',  ( 78.26014418490360924, -38.80290789369995252, 7.687431601936923542 ) ) ;
#73175 = CARTESIAN_POINT ( 'NONE',  ( 107.0664832912748068, -36.72944715993923381, -5.074374724089029343 ) ) ;
#73176 = DIRECTION ( 'NONE',  ( 3.999999999999999995E-14, -1.000000000000000000, 4.100000000000000342E-29 ) ) ;
#73177 = CARTESIAN_POINT ( 'NONE',  ( 111.7725766154891431, -30.05993356141850015, 127.4052332267339693 ) ) ;
#73178 = CARTESIAN_POINT ( 'NONE',  ( 95.27050013873164858, -38.09949539013453546, 232.4184824187679794 ) ) ;
#73179 = EDGE_CURVE ( 'NONE', #38559, #39595, #69856, .T. ) ;
#73180 = FACE_OUTER_BOUND ( 'NONE', #80983, .T. ) ;
#73181 = ORIENTED_EDGE ( 'NONE', *, *, #60837, .F. ) ;
#73182 = CARTESIAN_POINT ( 'NONE',  ( 135.9140641843650315, -38.77438500682884381, 2.186796636972260011 ) ) ;
#73183 = ORIENTED_EDGE ( 'NONE', *, *, #43442, .T. ) ;
#73184 = ORIENTED_EDGE ( 'NONE', *, *, #39381, .T. ) ;
#73185 = AXIS2_PLACEMENT_3D ( 'NONE', #68781, #13812, #56010 ) ;
#73186 = DIRECTION ( 'NONE',  ( -1.000000000000000078E-15, 1.000000000000000083E-30, 1.000000000000000000 ) ) ;
#73187 = ORIENTED_EDGE ( 'NONE', *, *, #54204, .F. ) ;
#73188 = VERTEX_POINT ( 'NONE', #14452 ) ;
#73189 = CARTESIAN_POINT ( 'NONE',  ( 59.67079009362632291, -0.9310397146383332379, 396.9756252759102040 ) ) ;
#73190 = AXIS2_PLACEMENT_3D ( 'NONE', #27642, #55322, #63052 ) ;
#73191 = PLANE ( 'NONE',  #12379 ) ;
#73192 = CARTESIAN_POINT ( 'NONE',  ( 77.31648329127399677, -18.72944715994106346, -5.074374724089059541 ) ) ;
#73193 = CARTESIAN_POINT ( 'NONE',  ( 102.0031328989874027, -44.23578847709845263, 151.5143245899819817 ) ) ;
#73194 = CARTESIAN_POINT ( 'NONE',  ( 96.79018504364255193, -38.90877927100929412, 31.49276813305495892 ) ) ;
#73195 = ORIENTED_EDGE ( 'NONE', *, *, #30979, .T. ) ;
#73196 = DIRECTION ( 'NONE',  ( 1.147230458779309805E-16, 3.204747427460360459E-31, 1.000000000000000000 ) ) ;
#73197 = VERTEX_POINT ( 'NONE', #21716 ) ;
#73198 = FACE_OUTER_BOUND ( 'NONE', #60429, .T. ) ;
#73199 = ORIENTED_EDGE ( 'NONE', *, *, #68336, .T. ) ;
#73200 = CARTESIAN_POINT ( 'NONE',  ( 97.79399791629339234, -40.47395449460485395, 167.6321610181374524 ) ) ;
#73201 = DIRECTION ( 'NONE',  ( 0.000000000000000000, 0.000000000000000000, -1.000000000000000000 ) ) ;
#73202 = EDGE_CURVE ( 'NONE', #65108, #78132, #70754, .T. ) ;
#73203 = CARTESIAN_POINT ( 'NONE',  ( 97.81847504816714434, -40.53396937462733973, 131.6370481833811255 ) ) ;
#73205 = AXIS2_PLACEMENT_3D ( 'NONE', #1666, #64771, #29366 ) ;
#73204 = DIRECTION ( 'NONE',  ( 1.000000000000000000, 1.000000000000000078E-15, 0.000000000000000000 ) ) ;
#73206 = ORIENTED_EDGE ( 'NONE', *, *, #3076, .T. ) ;
#73207 = CARTESIAN_POINT ( 'NONE',  ( 96.81178581975444786, -38.90419831550661911, 31.49276813305495892 ) ) ;
#73208 = CIRCLE ( 'NONE', #22401, 2.517500000000005844 ) ;
#73209 = CARTESIAN_POINT ( 'NONE',  ( 100.4377198651835101, -44.85950937921091253, 8.032768133053981074 ) ) ;
#73210 = VECTOR ( 'NONE', #77622, 1000.000000000000000 ) ;
#73211 = VECTOR ( 'NONE', #53606, 1000.000000000000000 ) ;
#73213 = CARTESIAN_POINT ( 'NONE',  ( 107.0664832912750057, -36.72944715993903486, 9.125625275910969947 ) ) ;
#73212 = CARTESIAN_POINT ( 'NONE',  ( -46.60773131249376178, 91.07499999999996021, -44.42500552774628630 ) ) ;
#73214 = CARTESIAN_POINT ( 'NONE',  ( 184.5667039024483813, -48.82844715993448403, 249.9678068554149775 ) ) ;
#73215 = DIRECTION ( 'NONE',  ( 0.000000000000000000, -1.000000000000000000, 0.000000000000000000 ) ) ;
#73216 = FACE_OUTER_BOUND ( 'NONE', #40767, .T. ) ;
#73217 = AXIS2_PLACEMENT_3D ( 'NONE', #86427, #65517, #16044 ) ;
#73218 = CARTESIAN_POINT ( 'NONE',  ( 152.5667039024469602, -23.42844715993586036, 300.4678068554149490 ) ) ;
#73219 = CARTESIAN_POINT ( 'NONE',  ( 145.7544960090152983, -67.86889861335799878, 247.4138443563959981 ) ) ;
#73220 = EDGE_CURVE ( 'NONE', #36065, #2851, #50281, .T. ) ;
#73221 = CARTESIAN_POINT ( 'NONE',  ( 106.5157732221739195, -25.64298685704507363, 45.12800622829193742 ) ) ;
#73222 = CARTESIAN_POINT ( 'NONE',  ( 97.76247233159546113, -41.51031662465626937, 192.7041967044819728 ) ) ;
#73223 = CARTESIAN_POINT ( 'NONE',  ( 114.8356066511136504, -43.71357066064707197, 34.24419670448197905 ) ) ;
#73225 = CARTESIAN_POINT ( 'NONE',  ( 110.0667047667142953, -70.87844715994094713, 173.2178068554179902 ) ) ;
#73224 = DIRECTION ( 'NONE',  ( 1.000000000000000000, 4.299999999999999979E-14, 1.000000000000000078E-15 ) ) ;
#73226 = CARTESIAN_POINT ( 'NONE',  ( 107.0664832912739968, -36.72944715994100306, 9.635625275910941312 ) ) ;
#73227 = EDGE_CURVE ( 'NONE', #61431, #65795, #53798, .T. ) ;
#73228 = AXIS2_PLACEMENT_3D ( 'NONE', #6090, #26518, #61472 ) ;
#73229 = ORIENTED_EDGE ( 'NONE', *, *, #21601, .T. ) ;
#73230 = LINE ( 'NONE', #66870, #63554 ) ;
#73231 = VERTEX_POINT ( 'NONE', #69409 ) ;
#73232 = CARTESIAN_POINT ( 'NONE',  ( 102.0418483691416895, -28.29933337693059414, 81.50419670448194154 ) ) ;
#73234 = ORIENTED_EDGE ( 'NONE', *, *, #34101, .T. ) ;
#73233 = DIRECTION ( 'NONE',  ( 0.000000000000000000, 0.000000000000000000, 1.000000000000000000 ) ) ;
#73235 = DIRECTION ( 'NONE',  ( 0.000000000000000000, 0.000000000000000000, -1.000000000000000000 ) ) ;
#73236 = CARTESIAN_POINT ( 'NONE',  ( 109.3321198358311932, -26.57584895156214699, 220.9013395616249795 ) ) ;
#73237 = CARTESIAN_POINT ( 'NONE',  ( 103.1875000000000000, 117.4749999999999943, -5.041899999999640336 ) ) ;
#73238 = CARTESIAN_POINT ( 'NONE',  ( 116.3221839001005264, -32.94216875276463696, 149.1356252759109680 ) ) ;
#73239 = FACE_OUTER_BOUND ( 'NONE', #88647, .T. ) ;
#73240 = CARTESIAN_POINT ( 'NONE',  ( 78.13314995793999174, 12.92155284005730387, 358.9756252759109998 ) ) ;
#73241 = PRODUCT_RELATED_PRODUCT_CATEGORY ( 'part', '', ( #60498 ) ) ;
#73242 = CARTESIAN_POINT ( 'NONE',  ( 131.7155263566431813, -38.16021090637521951, 2.608895778950927724 ) ) ;
#73243 = CARTESIAN_POINT ( 'NONE',  ( -83.89393544538295089, 76.91670260214422683, 100.0338904447229993 ) ) ;
#73244 = CARTESIAN_POINT ( 'NONE',  ( 104.0088209277215583, -27.43890701233894092, 165.3299109901969643 ) ) ;
#73245 = ORIENTED_EDGE ( 'NONE', *, *, #61698, .T. ) ;
#73246 = VERTEX_POINT ( 'NONE', #42128 ) ;
#73247 = VECTOR ( 'NONE', #20923, 1000.000000000000000 ) ;
#73248 = CARTESIAN_POINT ( 'NONE',  ( 101.3137116872897820, -44.99844491211269570, 83.52444044875394979 ) ) ;
#73249 = LINE ( 'NONE', #78319, #10965 ) ;
#73251 = CARTESIAN_POINT ( 'NONE',  ( 1.145694247088684285E-22, 95.25000000000000000, 118.5560000000000116 ) ) ;
#73250 = CARTESIAN_POINT ( 'NONE',  ( 97.67678136301130110, -41.13084272647604678, 207.6632443235299661 ) ) ;
#73252 = CARTESIAN_POINT ( 'NONE',  ( 0.000000000000000000, 238.7999999999999829, 154.6557476874258441 ) ) ;
#73253 = DIRECTION ( 'NONE',  ( 0.000000000000000000, 1.000000000000000000, 0.000000000000000000 ) ) ;
#73254 = EDGE_CURVE ( 'NONE', #4351, #25758, #36226, .T. ) ;
#73255 = DIRECTION ( 'NONE',  ( -0.000000000000000000, 1.000000000000000000, -0.000000000000000000 ) ) ;
#73256 = CARTESIAN_POINT ( 'NONE',  ( -254.0000000000000000, 93.66249999999999432, 6.350000000000409983 ) ) ;
#73257 = CARTESIAN_POINT ( 'NONE',  ( 177.0371591254543659, -48.62818131005480637, 237.4678068554150059 ) ) ;
#73258 = EDGE_CURVE ( 'NONE', #58668, #32600, #43638, .T. ) ;
#73259 = DIRECTION ( 'NONE',  ( -0.9254794337955620787, -0.3787978585227822492, 0.000000000000000000 ) ) ;
#73260 = CARTESIAN_POINT ( 'NONE',  ( 102.9757002774701959, -26.48594595611781344, 175.3908633711489813 ) ) ;
#73261 = EDGE_CURVE ( 'NONE', #67802, #66826, #3072, .T. ) ;
#73262 = EDGE_LOOP ( 'NONE', ( #79317, #3479, #71604, #76796 ) ) ;
#73263 = ORIENTED_EDGE ( 'NONE', *, *, #60978, .F. ) ;
#73264 = ADVANCED_FACE ( 'NONE', ( #8984 ), #808, .T. ) ;
#73265 = CARTESIAN_POINT ( 'NONE',  ( 80.58723842074230959, -73.69558419411040973, 248.4067532124560103 ) ) ;
#73266 = CARTESIAN_POINT ( 'NONE',  ( 97.31584368152388720, -39.30597586568408985, 152.5314585983696531 ) ) ;
#73267 = CARTESIAN_POINT ( 'NONE',  ( 51.06648329127400388, 19.62155284005901024, 336.6506252759110112 ) ) ;
#73268 = CARTESIAN_POINT ( 'NONE',  ( 59.56670390244700997, -79.67844715994098692, 190.2178068554179902 ) ) ;
#73269 = CIRCLE ( 'NONE', #84916, 1.000000000000000888 ) ;
#73271 = ORIENTED_EDGE ( 'NONE', *, *, #74707, .F. ) ;
#73270 = ADVANCED_FACE ( 'NONE', ( #29418 ), #56192, .F. ) ;
#73272 = VECTOR ( 'NONE', #69456, 1000.000000000000000 ) ;
#73273 = CARTESIAN_POINT ( 'NONE',  ( 141.8164832912740110, -9.833000550534297446, -5.074374724088994704 ) ) ;
#73274 = CIRCLE ( 'NONE', #38451, 3.600000000000000089 ) ;
#73275 = AXIS2_PLACEMENT_3D ( 'NONE', #25480, #10953, #25936 ) ;
#73276 = CARTESIAN_POINT ( 'NONE',  ( 117.7793243111075157, -34.00655811778471360, 169.0365776568629599 ) ) ;
#73277 = CARTESIAN_POINT ( 'NONE',  ( 135.1909174281129538, -39.23916151080251069, 8.028235474617126499 ) ) ;
#73278 = EDGE_LOOP ( 'NONE', ( #29869, #33809, #15330, #33077, #73350, #59429 ) ) ;
#73280 = ORIENTED_EDGE ( 'NONE', *, *, #10308, .T. ) ;
#73279 = VERTEX_POINT ( 'NONE', #83945 ) ;
#73281 = EDGE_CURVE ( 'NONE', #2341, #71979, #75559, .T. ) ;
#73282 = AXIS2_PLACEMENT_3D ( 'NONE', #51658, #66637, #45288 ) ;
#73283 = CARTESIAN_POINT ( 'NONE',  ( -9.568977433314790559, 74.15890990428199814, 118.1706578929490377 ) ) ;
#73284 = CARTESIAN_POINT ( 'NONE',  ( 95.35945913470564506, -35.72541260001472097, 298.1356252759109680 ) ) ;
#73285 = DIRECTION ( 'NONE',  ( 0.000000000000000000, 1.000000000000000000, 0.000000000000000000 ) ) ;
#73286 = CARTESIAN_POINT ( 'NONE',  ( 116.2008526694824582, -35.09873344310054932, 46.78523322673494533 ) ) ;
#73287 = AXIS2_PLACEMENT_3D ( 'NONE', #14501, #77617, #856 ) ;
#73288 = LINE ( 'NONE', #11977, #71036 ) ;
#73289 = ORIENTED_EDGE ( 'NONE', *, *, #20358, .T. ) ;
#73290 = AXIS2_PLACEMENT_3D ( 'NONE', #35141, #48306, #21540 ) ;
#73291 = DIRECTION ( 'NONE',  ( 0.000000000000000000, 1.000000000000000000, 0.000000000000000000 ) ) ;
#73292 = DIRECTION ( 'NONE',  ( 0.000000000000000000, 0.000000000000000000, 1.000000000000000000 ) ) ;
#73293 = ORIENTED_EDGE ( 'NONE', *, *, #85717, .T. ) ;
#73294 = ORIENTED_EDGE ( 'NONE', *, *, #47910, .T. ) ;
#73295 = DIRECTION ( 'NONE',  ( 1.000000000000000000, 4.163336342344347755E-14, 0.000000000000000000 ) ) ;
#73296 = ORIENTED_EDGE ( 'NONE', *, *, #51566, .T. ) ;
#73297 = ORIENTED_EDGE ( 'NONE', *, *, #67633, .T. ) ;
#73298 = DIRECTION ( 'NONE',  ( 1.000000000000000000, 0.000000000000000000, 0.000000000000000000 ) ) ;
#73299 = AXIS2_PLACEMENT_3D ( 'NONE', #58261, #58693, #30117 ) ;
#73300 = CARTESIAN_POINT ( 'NONE',  ( 102.4109068130577356, -29.56832019646944687, 24.95813411379099733 ) ) ;
#73301 = CARTESIAN_POINT ( 'NONE',  ( 117.2137812332333766, -41.17104435167765075, 208.4861014663869696 ) ) ;
#73302 = CARTESIAN_POINT ( 'NONE',  ( 96.06973772670281164, -35.87188691900273341, 191.2765776568629690 ) ) ;
#73303 = DIRECTION ( 'NONE',  ( 0.000000000000000000, 0.000000000000000000, -1.000000000000000000 ) ) ;
#73304 = CARTESIAN_POINT ( 'NONE',  ( 99.33320739591177073, -28.83195234130426243, 266.7051490854347549 ) ) ;
#73305 = DIRECTION ( 'NONE',  ( 0.000000000000000000, 1.000000000000000000, 0.000000000000000000 ) ) ;
#73306 = CYLINDRICAL_SURFACE ( 'NONE', #46789, 2.117000000000000881 ) ;
#73307 = VERTEX_POINT ( 'NONE', #35765 ) ;
#73308 = ORIENTED_EDGE ( 'NONE', *, *, #45338, .F. ) ;
#73309 = B_SPLINE_CURVE_WITH_KNOTS ( 'NONE', 3,
 ( #16985, #36975, #85597, #31482, #80115, #23376, #71955, #37424, #51045, #16537, #34166, #20114, #26473, #74178, #39642, #47343, #11505, #75071, #55040, #39199, #82804, #60989, #88716, #26031, #74618, #88273, #68267, #6048, #32373, #66909 ),
 .UNSPECIFIED., .F., .F.,
 ( 4, 2, 2, 2, 1, 2, 2, 2, 2, 2, 2, 2, 1, 2, 2, 4 ),
 ( 0.000000000000000000, 0.1249999999999997780, 0.1875000000000007772, 0.2187500000000001110, 0.2343749999999997780, 0.2421874999999996392, 0.2499999999999995282, 0.3749999999999976685, 0.4374999999999936717, 0.4999999999999896749, 0.6249999999999764633, 0.6874999999999692468, 0.7187499999999694689, 0.7343749999999699130, 0.7499999999999704681, 1.000000000000000000 ),
 .UNSPECIFIED. ) ;
#73310 = EDGE_CURVE ( 'NONE', #11858, #26048, #14679, .T. ) ;
#73311 = B_SPLINE_CURVE_WITH_KNOTS ( 'NONE', 3,
 ( #54190, #89205, #76009, #13784, #81953, #26971, #54638, #20162, #68752, #39688, #5183, #6522, #41470, #32877, #60577, #64620, #35111, #43717 ),
 .UNSPECIFIED., .F., .F.,
 ( 4, 2, 2, 2, 2, 2, 2, 2, 4 ),
 ( 0.000000000000000000, 0.06250000025565728701, 0.1250000005113145740, 0.1875000007669718749, 0.2500000010226291480, 0.3125000012782864212, 0.3750000015339437498, 0.4375000017896010229, 0.5000000020452582961 ),
 .UNSPECIFIED. ) ;
#73312 = CIRCLE ( 'NONE', #19636, 3.249999999999975131 ) ;
#73313 = CARTESIAN_POINT ( 'NONE',  ( 97.81362638013557387, -40.52215668197012377, 111.6360318040896829 ) ) ;
#73314 = CARTESIAN_POINT ( 'NONE',  ( 106.8507020815961397, -47.82747951245497831, 227.5489586092439538 ) ) ;
#73315 = VERTEX_POINT ( 'NONE', #49834 ) ;
#73316 = CARTESIAN_POINT ( 'NONE',  ( 117.9487373648833426, -34.79150140969374405, 198.9546728949589749 ) ) ;
#73317 = FACE_OUTER_BOUND ( 'NONE', #81760, .T. ) ;
#73318 = AXIS2_PLACEMENT_3D ( 'NONE', #61040, #88771, #26529 ) ;
#73319 = CYLINDRICAL_SURFACE ( 'NONE', #4235, 1.000000000002049694 ) ;
#73320 = EDGE_CURVE ( 'NONE', #23215, #87708, #5924, .T. ) ;
#73321 = CARTESIAN_POINT ( 'NONE',  ( 31.78666935232998725, -36.02818131005891189, -5.074374724088000832 ) ) ;
#73322 = CARTESIAN_POINT ( 'NONE',  ( 143.5504647578642050, -139.6982893664599885, 247.2544030524684615 ) ) ;
#73325 = CARTESIAN_POINT ( 'NONE',  ( 96.55902551080276908, -40.08462249002850086, 277.5603871806729899 ) ) ;
#73324 = CARTESIAN_POINT ( 'NONE',  ( 1.451892259197136103E-14, 61.59999999999999432, -118.5560000000000116 ) ) ;
#73323 = CARTESIAN_POINT ( 'NONE',  ( 154.5667039024469886, -67.87844715994090450, 85.21780685541799016 ) ) ;
#73326 = CARTESIAN_POINT ( 'NONE',  ( 63.03715912545646205, -24.89890238295017255, 129.9678068554150911 ) ) ;
#73327 = CARTESIAN_POINT ( 'NONE',  ( 182.5667039024459939, -22.48495420874030515, -5.074374724088000832 ) ) ;
#73328 = PLANE ( 'NONE',  #81844 ) ;
#73329 = CARTESIAN_POINT ( 'NONE',  ( 1.598849865763559337E-14, 95.25000000000000000, -130.5560000000000116 ) ) ;
#73330 = CARTESIAN_POINT ( 'NONE',  ( 21.03715912545829170, -47.82818131006186491, 249.9678068554150059 ) ) ;
#73331 = DIRECTION ( 'NONE',  ( -0.9254794337955620787, -0.3787978585227822492, 0.000000000000000000 ) ) ;
#73333 = VERTEX_POINT ( 'NONE', #15791 ) ;
#73332 = CARTESIAN_POINT ( 'NONE',  ( -11.89031456967464706, 87.03148351030580443, -117.9583453772440151 ) ) ;
#73334 = CARTESIAN_POINT ( 'NONE',  ( 136.4105765916308144, -20.17027654743777276, 7.249284792654901111 ) ) ;
#73335 = CARTESIAN_POINT ( 'NONE',  ( 109.3633609874958523, -25.89340572475189006, 184.9222919425779708 ) ) ;
#73336 = CARTESIAN_POINT ( 'NONE',  ( 106.0764678730365063, -48.53853201145131635, 108.5099109901969712 ) ) ;
#73337 = CARTESIAN_POINT ( 'NONE',  ( 95.24589774366052097, -38.10235284316662074, 232.4184824187679794 ) ) ;
#73338 = CARTESIAN_POINT ( 'NONE',  ( 63.56670390244828184, -47.82844715994016127, 249.9678068554150343 ) ) ;
#73339 = LINE ( 'NONE', #11112, #21400 ) ;
#73341 = CARTESIAN_POINT ( 'NONE',  ( 97.82515122448313605, -40.55016472165671360, 37.63815125684190832 ) ) ;
#73340 = DIRECTION ( 'NONE',  ( -1.000000000000000000, -3.360405532702990443E-14, 0.000000000000000000 ) ) ;
#73342 = CARTESIAN_POINT ( 'NONE',  ( -479.3614999999999782, 3.174999999999999822, -1.387778780781445991E-14 ) ) ;
#73343 = DIRECTION ( 'NONE',  ( 1.000000000000000000, 4.163336342344333240E-14, 0.000000000000000000 ) ) ;
#73344 = DIRECTION ( 'NONE',  ( 0.000000000000000000, 0.000000000000000000, 1.000000000000000000 ) ) ;
#73345 = AXIS2_PLACEMENT_3D ( 'NONE', #32249, #5458, #59945 ) ;
#73346 = EDGE_CURVE ( 'NONE', #41277, #86596, #33240, .T. ) ;
#73347 = AXIS2_PLACEMENT_3D ( 'NONE', #44639, #3329, #16958 ) ;
#73348 = CIRCLE ( 'NONE', #3712, 5.499999999999999112 ) ;
#73349 = VECTOR ( 'NONE', #37227, 1000.000000000000000 ) ;
#73350 = ORIENTED_EDGE ( 'NONE', *, *, #74356, .F. ) ;
#73351 = ORIENTED_EDGE ( 'NONE', *, *, #35302, .T. ) ;
#73352 = VECTOR ( 'NONE', #67417, 1000.000000000000000 ) ;
#73353 = CARTESIAN_POINT ( 'NONE',  ( 103.9632409301644316, -45.23724106753869734, 96.70861030426696914 ) ) ;
#73355 = ORIENTED_EDGE ( 'NONE', *, *, #86284, .T. ) ;
#73354 = CARTESIAN_POINT ( 'NONE',  ( -8.391680458684334099, 92.11847147219766896, -130.2873503055691629 ) ) ;
#73356 = CARTESIAN_POINT ( 'NONE',  ( 117.2009162446674395, -42.82382785266563019, 124.3956252759109731 ) ) ;
#73357 = CARTESIAN_POINT ( 'NONE',  ( 122.2221484686745470, -111.9799080603168022, -11.78219314458175937 ) ) ;
#73358 = CIRCLE ( 'NONE', #2123, 4.762500000000002842 ) ;
#73359 = CARTESIAN_POINT ( 'NONE',  ( 78.80082187617267664, -16.28157759251482517, 7.978179524063404138 ) ) ;
#73360 = CARTESIAN_POINT ( 'NONE',  ( 165.9667039024459996, -28.27351298637401200, 117.4678068554150485 ) ) ;
#73361 = DIRECTION ( 'NONE',  ( 0.000000000000000000, -1.000000000000000000, 0.000000000000000000 ) ) ;
#73363 = CARTESIAN_POINT ( 'NONE',  ( 101.3216544293209864, -28.81361639883581205, 75.57562527591093726 ) ) ;
#73362 = AXIS2_PLACEMENT_3D ( 'NONE', #38175, #57722, #9583 ) ;
#73364 = EDGE_LOOP ( 'NONE', ( #78518, #54247, #18395, #48028 ) ) ;
#73365 = ORIENTED_EDGE ( 'NONE', *, *, #58117, .F. ) ;
#73366 = ORIENTED_EDGE ( 'NONE', *, *, #80409, .T. ) ;
#73367 = DIRECTION ( 'NONE',  ( -1.000000000000000078E-15, 1.000000000000000083E-30, 1.000000000000000000 ) ) ;
#73369 = CARTESIAN_POINT ( 'NONE',  ( 51.56670390244772761, -33.35206098992764367, 237.4678068554150059 ) ) ;
#73368 = CARTESIAN_POINT ( 'NONE',  ( 117.2073019650708261, -38.89799087863979565, 104.6708633711489824 ) ) ;
#73370 = CIRCLE ( 'NONE', #55970, 2.117000000000007987 ) ;
#73371 = DIRECTION ( 'NONE',  ( 0.000000000000000000, 0.000000000000000000, 1.000000000000000000 ) ) ;
#73372 = CARTESIAN_POINT ( 'NONE',  ( 8.690912999409459161, 73.28018275885442279, -130.2667388509219677 ) ) ;
#73373 = ADVANCED_FACE ( 'NONE', ( #87062, #52494, #38440, #2609 ), #73415, .F. ) ;
#73374 = DIRECTION ( 'NONE',  ( -0.7071067708032375831, -0.0001211784769794317250, 0.7071067811865434649 ) ) ;
#73375 = CARTESIAN_POINT ( 'NONE',  ( 74.87617104506175281, 86.64222086580517157, 91.91945768840264464 ) ) ;
#73376 = CARTESIAN_POINT ( 'NONE',  ( 62.03715912545754207, -47.82818131006020934, 129.9678068554150911 ) ) ;
#73377 = CARTESIAN_POINT ( 'NONE',  ( 110.4495079430909641, -47.22796928374267367, 57.83657765686300678 ) ) ;
#73378 = ORIENTED_EDGE ( 'NONE', *, *, #29306, .F. ) ;
#73379 = EDGE_CURVE ( 'NONE', #33481, #56709, #59774, .T. ) ;
#73380 = ORIENTED_EDGE ( 'NONE', *, *, #88385, .F. ) ;
#73381 = EDGE_CURVE ( 'NONE', #58445, #61346, #86617, .T. ) ;
#73382 = LINE ( 'NONE', #4354, #86526 ) ;
#73383 = CARTESIAN_POINT ( 'NONE',  ( 31.78666935232898894, -29.62846900982320264, 342.9256252759119548 ) ) ;
#73384 = LINE ( 'NONE', #11154, #55466 ) ;
#73385 = CARTESIAN_POINT ( 'NONE',  ( 115.3759468638744181, -39.14889752855258820, 136.4071379886389650 ) ) ;
#73386 = VECTOR ( 'NONE', #57989, 1000.000000000000000 ) ;
#73387 = DIRECTION ( 'NONE',  ( 1.000000000000000000, 0.000000000000000000, 0.000000000000000000 ) ) ;
#73388 = ORIENTED_EDGE ( 'NONE', *, *, #76901, .F. ) ;
#73389 = ORIENTED_EDGE ( 'NONE', *, *, #89579, .T. ) ;
#73390 = ADVANCED_FACE ( 'NONE', ( #45682 ), #78478, .T. ) ;
#73391 = CARTESIAN_POINT ( 'NONE',  ( 27.27158787008327678, 184.0000000000000000, 101.0189074266571794 ) ) ;
#73392 = ORIENTED_EDGE ( 'NONE', *, *, #48067, .F. ) ;
#73393 = ORIENTED_EDGE ( 'NONE', *, *, #9489, .T. ) ;
#73394 = EDGE_CURVE ( 'NONE', #53017, #12546, #16679, .T. ) ;
#73395 = CYLINDRICAL_SURFACE ( 'NONE', #73853, 130.5560000000000116 ) ;
#73396 = CARTESIAN_POINT ( 'NONE',  ( 115.5247806442692422, -34.08644044406323559, 170.4987261630399473 ) ) ;
#73397 = PLANE ( 'NONE',  #32720 ) ;
#73398 = AXIS2_PLACEMENT_3D ( 'NONE', #33296, #49482, #42223 ) ;
#73399 = FACE_OUTER_BOUND ( 'NONE', #56097, .T. ) ;
#73400 = CARTESIAN_POINT ( 'NONE',  ( 183.5150000000000148, 14.63749999999999929, -9.525000000000000355 ) ) ;
#73401 = AXIS2_PLACEMENT_3D ( 'NONE', #60632, #53351, #11614 ) ;
#73402 = ORIENTED_EDGE ( 'NONE', *, *, #54319, .T. ) ;
#73403 = ORIENTED_EDGE ( 'NONE', *, *, #75078, .F. ) ;
#73404 = AXIS2_PLACEMENT_3D ( 'NONE', #34029, #89468, #27226 ) ;
#73405 = AXIS2_PLACEMENT_3D ( 'NONE', #31367, #17750, #79995 ) ;
#73406 = ORIENTED_EDGE ( 'NONE', *, *, #13000, .T. ) ;
#73407 = VERTEX_POINT ( 'NONE', #86171 ) ;
#73408 = CARTESIAN_POINT ( 'NONE',  ( 115.1674193411231784, -35.52216783720512439, 216.7623760838769726 ) ) ;
#73409 = CARTESIAN_POINT ( 'NONE',  ( 103.1971861921166038, -46.47197777470199753, 117.2756252759109543 ) ) ;
#73410 = CARTESIAN_POINT ( 'NONE',  ( 99.31004196827748842, -43.71529311364911763, 56.90991099019593236 ) ) ;
#73411 = CARTESIAN_POINT ( 'NONE',  ( 105.7135912305062391, -46.72357220724894233, 252.4691331623911594 ) ) ;
#73412 = FACE_OUTER_BOUND ( 'NONE', #13847, .T. ) ;
#73413 = CARTESIAN_POINT ( 'NONE',  ( 107.5312500490845053, -25.27893178259700591, 323.2150800290978623 ) ) ;
#73414 = CARTESIAN_POINT ( 'NONE',  ( 102.8440116971490852, -46.26114276377411016, 173.2441967044829596 ) ) ;
#73415 = CYLINDRICAL_SURFACE ( 'NONE', #8856, 118.5560000000000116 ) ;
#73416 = ORIENTED_EDGE ( 'NONE', *, *, #37508, .F. ) ;
#73417 = DIRECTION ( 'NONE',  ( 0.000000000000000000, 0.000000000000000000, 1.000000000000000000 ) ) ;
#73418 = ORIENTED_EDGE ( 'NONE', *, *, #50310, .T. ) ;
#73419 = ORIENTED_EDGE ( 'NONE', *, *, #13852, .T. ) ;
#73420 = CARTESIAN_POINT ( 'NONE',  ( 128.0667039024480118, -50.82844715994100682, 310.9178068554150514 ) ) ;
#73421 = LINE ( 'NONE', #2164, #37267 ) ;
#73422 = VECTOR ( 'NONE', #58068, 1000.000000000000000 ) ;
#73423 = EDGE_LOOP ( 'NONE', ( #65316, #55513, #51846, #16502, #88833, #13199, #23936, #71230, #50438, #36835, #61059, #72845, #53185, #61184 ) ) ;
#73424 = FACE_OUTER_BOUND ( 'NONE', #18878, .T. ) ;
#73425 = VERTEX_POINT ( 'NONE', #43916 ) ;
#73426 = CARTESIAN_POINT ( 'NONE',  ( 110.4252027303417663, -27.27630697421929540, 130.8049591708739854 ) ) ;
#73427 = CARTESIAN_POINT ( 'NONE',  ( 104.4906584979394211, -46.86803844812923359, 47.37848241876796607 ) ) ;
#73428 = CARTESIAN_POINT ( 'NONE',  ( 46.83715912545343940, -47.82818131006086304, 129.9678068554150911 ) ) ;
#73429 = VECTOR ( 'NONE', #44751, 999.9999999999998863 ) ;
#73430 = ADVANCED_FACE ( 'NONE', ( #59334 ), #24390, .F. ) ;
#73431 = CARTESIAN_POINT ( 'NONE',  ( 63.50000000000000000, 66.67499999999999716, 219.0749999999999886 ) ) ;
#73432 = FACE_OUTER_BOUND ( 'NONE', #47636, .T. ) ;
#73433 = CARTESIAN_POINT ( 'NONE',  ( 114.1038288540493539, -43.56973530630605751, 98.21276813305496489 ) ) ;
#73435 = CARTESIAN_POINT ( 'NONE',  ( 95.43233898611183008, -38.84956357215551037, 197.4699109901969791 ) ) ;
#73434 = CARTESIAN_POINT ( 'NONE',  ( 107.0667039024470313, -104.2784471599414502, 0.2178068554180012661 ) ) ;
#73436 = CARTESIAN_POINT ( 'NONE',  ( 115.0858478210553102, -30.61367454548772926, 59.34435376945771168 ) ) ;
#73437 = DIRECTION ( 'NONE',  ( 0.7071067811869283792, -0.7071067811861665442, 7.071067811869291448E-16 ) ) ;
#73438 = ORIENTED_EDGE ( 'NONE', *, *, #50801, .T. ) ;
#73439 = DIRECTION ( 'NONE',  ( 1.000000000000000000, 0.000000000000000000, 0.000000000000000000 ) ) ;
#73440 = DIRECTION ( 'NONE',  ( -4.299999999999999979E-14, 1.000000000000000000, -4.400000000000000367E-29 ) ) ;
#73441 = LINE ( 'NONE', #31660, #69138 ) ;
#73442 = DIRECTION ( 'NONE',  ( -0.000000000000000000, 1.000000000000000000, 0.000000000000000000 ) ) ;
#73444 = ORIENTED_EDGE ( 'NONE', *, *, #76242, .T. ) ;
#73443 = CARTESIAN_POINT ( 'NONE',  ( 116.4168962126584717, -41.43863437684461104, 203.4556252759109611 ) ) ;
#73445 = CARTESIAN_POINT ( 'NONE',  ( 97.70664662319364879, -40.25154480828024361, 146.6128751502485841 ) ) ;
#73446 = CARTESIAN_POINT ( 'NONE',  ( 100.4653332305737905, -44.82571634032018437, 8.032768133053981074 ) ) ;
#73447 = CARTESIAN_POINT ( 'NONE',  ( 102.2824096876565108, -27.37794169069978523, 116.4527681330539650 ) ) ;
#73448 = CARTESIAN_POINT ( 'NONE',  ( -48.02966122971774610, 91.07499999999996021, -43.00307561052233751 ) ) ;
#73449 = CARTESIAN_POINT ( 'NONE',  ( 82.80376803119651186, -37.00431460296900354, 6.768845908774068221 ) ) ;
#73450 = FACE_OUTER_BOUND ( 'NONE', #30391, .T. ) ;
#73451 = CYLINDRICAL_SURFACE ( 'NONE', #45217, 3.000000000000002665 ) ;
#73452 = ORIENTED_EDGE ( 'NONE', *, *, #43429, .T. ) ;
#73453 = ADVANCED_FACE ( 'NONE', ( #23945 ), #18002, .F. ) ;
#73454 = ORIENTED_EDGE ( 'NONE', *, *, #81140, .F. ) ;
#73455 = ORIENTED_EDGE ( 'NONE', *, *, #34723, .T. ) ;
#73456 = VERTEX_POINT ( 'NONE', #23514 ) ;
#73457 = CARTESIAN_POINT ( 'NONE',  ( 115.0372575016916556, -42.90846257304766453, 73.30229194195298703 ) ) ;
#73458 = CARTESIAN_POINT ( 'NONE',  ( 115.3234718241651535, -45.22984455807579707, 264.1899109901965517 ) ) ;
#73459 = DIRECTION ( 'NONE',  ( 6.524622321627019585E-16, 3.741823817616790462E-31, 1.000000000000000000 ) ) ;
#73460 = CARTESIAN_POINT ( 'NONE',  ( 129.9696172393100539, -140.6784471630960240, 245.6313762643000018 ) ) ;
#73461 = EDGE_CURVE ( 'NONE', #8926, #31809, #10305, .T. ) ;
#73462 = ADVANCED_FACE ( 'NONE', ( #72093 ), #32077, .T. ) ;
#73464 = CARTESIAN_POINT ( 'NONE',  ( 69.55244702860527184, -138.4431012436765798, 247.5929369389089914 ) ) ;
#73463 = DIRECTION ( 'NONE',  ( -2.195856868753399715E-16, -1.000000000000000000, 0.000000000000000000 ) ) ;
#73465 = AXIS2_PLACEMENT_3D ( 'NONE', #86500, #85172, #65148 ) ;
#73466 = CARTESIAN_POINT ( 'NONE',  ( 102.4446420578519934, -44.51733865501087450, 206.5848007804579538 ) ) ;
#73467 = ORIENTED_EDGE ( 'NONE', *, *, #1151, .F. ) ;
#73468 = ORIENTED_EDGE ( 'NONE', *, *, #24278, .T. ) ;
#73469 = CIRCLE ( 'NONE', #69136, 3.299999999999997158 ) ;
#73470 = VERTEX_POINT ( 'NONE', #51623 ) ;
#73471 = TOROIDAL_SURFACE ( 'NONE', #34305, 15.69999999999999929, 0.2999999999999999889 ) ;
#73472 = VECTOR ( 'NONE', #66450, 1000.000000000000000 ) ;
#73473 = DIRECTION ( 'NONE',  ( 1.000000000000000078E-15, -1.000000000000000083E-30, -1.000000000000000000 ) ) ;
#73474 = AXIS2_PLACEMENT_3D ( 'NONE', #70951, #35962, #36425 ) ;
#73476 = ADVANCED_FACE ( 'NONE', ( #65272 ), #3052, .T. ) ;
#73475 = DIRECTION ( 'NONE',  ( -4.237773401492740281E-14, 1.000000000000000000, 0.000000000000000000 ) ) ;
#73477 = LINE ( 'NONE', #38071, #22882 ) ;
#73478 = CARTESIAN_POINT ( 'NONE',  ( 100.3180865808431719, -43.26669944020724756, 38.38253568684996253 ) ) ;
#73479 = FACE_OUTER_BOUND ( 'NONE', #22077, .T. ) ;
#73480 = CARTESIAN_POINT ( 'NONE',  ( 113.2433229834693975, -28.75700906242621357, 174.5525078777224621 ) ) ;
#73481 = EDGE_CURVE ( 'NONE', #8582, #18961, #3486, .T. ) ;
#73482 = DIRECTION ( 'NONE',  ( 0.000000000000000000, 0.000000000000000000, -1.000000000000000000 ) ) ;
#73483 = ORIENTED_EDGE ( 'NONE', *, *, #26131, .T. ) ;
#73484 = CARTESIAN_POINT ( 'NONE',  ( 110.2707404709723846, -27.22220358462151779, 55.81764542590168077 ) ) ;
#73485 = VERTEX_POINT ( 'NONE', #17568 ) ;
#73486 = AXIS2_PLACEMENT_3D ( 'NONE', #10526, #11876, #80034 ) ;
#73487 = DIRECTION ( 'NONE',  ( -1.000000000000000000, -4.299999999999999979E-14, -9.351236661543306751E-17 ) ) ;
#73488 = CARTESIAN_POINT ( 'NONE',  ( 106.7065939435451440, -28.08240114970028856, 37.91570941720995336 ) ) ;
#73489 = CLOSED_SHELL ( 'NONE', ( #47727, #16369, #24698, #48115, #81105, #53124, #25832, #75275, #2120, #2417 ) ) ;
#73490 = CARTESIAN_POINT ( 'NONE',  ( 136.0678963113202258, -16.84294903903614937, 7.549690073078446417 ) ) ;
#73491 = B_SPLINE_CURVE_WITH_KNOTS ( 'NONE', 3,
 ( #841, #43050, #70791, #83976, #83515, #83087, #62163, #21749, #77154, #76248, #41707, #69439, #27650, #7215, #8561, #34904, #42598, #63511, #36261, #13571, #70334, #8110, #89439, #21288, #35797, #76702, #27200, #54875, #20402, #75806, #62615, #68989, #89898, #41261, #28085, #6758, #50318, #57587, #71245, #10769, #79400, #44394, #51207, #30346, #58043, #58913, #23544, #17164 ),
 .UNSPECIFIED., .F., .F.,
 ( 4, 2, 2, 2, 2, 2, 2, 2, 2, 1, 2, 2, 2, 2, 2, 2, 2, 2, 2, 2, 2, 1, 2, 2, 4 ),
 ( 0.05959919981814692375, 0.06208168506169063627, 0.06332292768346249601, 0.06456417030523434186, 0.06704665554877808908, 0.06828789817054996270, 0.06952914079232185018, 0.07201162603586555577, 0.07325286865763741551, 0.07449411127940928912, 0.07573535390118114885, 0.07697659652295302246, 0.07945908176649678356, 0.08194156701004054466, 0.08318280963181240439, 0.08442405225358426413, 0.08690653749712799747, 0.08814778011889984333, 0.08938902274067170306, 0.09187150798421539477, 0.09311275060598722675, 0.09435399322775908648, 0.09559523584953094621, 0.09683647847130277819, 0.09931896371484646990 ),
 .UNSPECIFIED. ) ;
#73492 = CARTESIAN_POINT ( 'NONE',  ( 107.0664832912739541, -36.72944715994095333, 305.0306255462182321 ) ) ;
#73493 = LINE ( 'NONE', #53467, #74972 ) ;
#73494 = ORIENTED_EDGE ( 'NONE', *, *, #7351, .F. ) ;
#73495 = CARTESIAN_POINT ( 'NONE',  ( 72.96458098368701428, 127.0000000000000000, -78.00648098368678518 ) ) ;
#73496 = ADVANCED_FACE ( 'NONE', ( #45250 ), #10736, .T. ) ;
#73497 = PLANE ( 'NONE',  #39685 ) ;
#73498 = VERTEX_POINT ( 'NONE', #51177 ) ;
#73499 = CARTESIAN_POINT ( 'NONE',  ( 117.2223540064780991, -42.83671953415140621, 128.3956252759109873 ) ) ;
#73500 = ORIENTED_EDGE ( 'NONE', *, *, #7131, .F. ) ;
#73501 = EDGE_CURVE ( 'NONE', #62421, #74897, #32034, .T. ) ;
#73502 = CARTESIAN_POINT ( 'NONE',  ( 107.2750367832685043, -27.67576416532946126, 74.46861030426799744 ) ) ;
#73503 = EDGE_CURVE ( 'NONE', #71292, #79308, #72643, .T. ) ;
#73504 = CARTESIAN_POINT ( 'NONE',  ( 162.7131505118539962, -33.70561438052111214, -5.074374724088000832 ) ) ;
#73505 = CARTESIAN_POINT ( 'NONE',  ( 115.5559677222042154, -32.70388140663459353, 60.62253568684894134 ) ) ;
#73506 = DIRECTION ( 'NONE',  ( -0.8660254037844381525, -0.5000000000000007772, 1.549999999999999706E-14 ) ) ;
#73507 = ADVANCED_FACE ( 'NONE', ( #25717 ), #12095, .T. ) ;
#73508 = CARTESIAN_POINT ( 'NONE',  ( 74.68590548172718968, -67.87844715994097555, 245.5622121550900090 ) ) ;
#73509 = CARTESIAN_POINT ( 'NONE',  ( 117.4061096064183971, -38.22256018827695101, 24.71276813305395237 ) ) ;
#73510 = VECTOR ( 'NONE', #71458, 1000.000000000000000 ) ;
#73511 = LINE ( 'NONE', #3580, #28015 ) ;
#73512 = ORIENTED_EDGE ( 'NONE', *, *, #65156, .F. ) ;
#73513 = CARTESIAN_POINT ( 'NONE',  ( 113.1781050883711544, -44.75200969554006747, 258.0938408987704520 ) ) ;
#73514 = ORIENTED_EDGE ( 'NONE', *, *, #87758, .T. ) ;
#73515 = CARTESIAN_POINT ( 'NONE',  ( -118.4716181662680583, 70.66242608954391358, -4.488731742999155117 ) ) ;
#73516 = VERTEX_POINT ( 'NONE', #13001 ) ;
#73517 = VERTEX_POINT ( 'NONE', #32976 ) ;
#73518 = VERTEX_POINT ( 'NONE', #52929 ) ;
#73519 = CARTESIAN_POINT ( 'NONE',  ( 104.0204373342842388, -47.42213563049719482, 217.3556252759109668 ) ) ;
#73520 = DIRECTION ( 'NONE',  ( -0.000000000000000000, -0.000000000000000000, -1.000000000000000000 ) ) ;
#73521 = DIRECTION ( 'NONE',  ( -1.000000000000000000, -1.000000000000000078E-15, 0.000000000000000000 ) ) ;
#73522 = B_SPLINE_CURVE_WITH_KNOTS ( 'NONE', 3,
 ( #385, #26743, #5422, #12684, #61701, #6308, #61263, #41256, #47622, #14015, #68089, #89434, #5875, #33117, #62609, #82185, #19941, #34898 ),
 .UNSPECIFIED., .F., .F.,
 ( 4, 2, 2, 2, 2, 2, 2, 2, 4 ),
 ( 0.4999434485927969907, 0.5624505175186973460, 0.6249575864445977569, 0.6874646553704981677, 0.7499717242963985786, 0.8124787932222989895, 0.8749858621481992893, 0.9374929310740995891, 1.000000000000000000 ),
 .UNSPECIFIED. ) ;
#73523 = CARTESIAN_POINT ( 'NONE',  ( 99.29379691555868703, -43.72992423520055638, 52.90991099019698396 ) ) ;
#73524 = CARTESIAN_POINT ( 'NONE',  ( 116.3212776292295842, -32.94146857471309886, 45.13562527591097506 ) ) ;
#73525 = EDGE_LOOP ( 'NONE', ( #63994, #54651 ) ) ;
#73526 = CARTESIAN_POINT ( 'NONE',  ( 115.8256479356252555, -31.73037971375361366, 114.2402245575558055 ) ) ;
#73527 = VECTOR ( 'NONE', #19521, 1000.000000000000000 ) ;
#73528 = DIRECTION ( 'NONE',  ( 0.000000000000000000, 1.000000000000000000, 0.000000000000000000 ) ) ;
#73529 = ORIENTED_EDGE ( 'NONE', *, *, #79906, .T. ) ;
#73530 = AXIS2_PLACEMENT_3D ( 'NONE', #50544, #78734, #8332 ) ;
#73531 = DIRECTION ( 'NONE',  ( -4.299999999999999979E-14, 1.000000000000000000, -4.400000000000000367E-29 ) ) ;
#73532 = AXIS2_PLACEMENT_3D ( 'NONE', #74959, #12743, #54482 ) ;
#73533 = CARTESIAN_POINT ( 'NONE',  ( 108.3314314236784384, -46.73508782468640277, 113.6779012139213449 ) ) ;
#73534 = CARTESIAN_POINT ( 'NONE',  ( 103.9458437887065827, -26.80522050874817808, 250.3184824187678714 ) ) ;
#73535 = LINE ( 'NONE', #44930, #12439 ) ;
#73536 = CONICAL_SURFACE ( 'NONE', #8259, 1.258750000000002922, 1.029744258676650093 ) ;
#73537 = EDGE_CURVE ( 'NONE', #42076, #34742, #20442, .T. ) ;
#73538 = CARTESIAN_POINT ( 'NONE',  ( 163.0664832912739826, 19.62155284005901024, 339.0006252759110339 ) ) ;
#73539 = CARTESIAN_POINT ( 'NONE',  ( 83.56670559755329464, -36.73837296219065252, 239.5838068554176914 ) ) ;
#73540 = CARTESIAN_POINT ( 'NONE',  ( 115.6071762752661130, -36.01623928086704041, 253.3152769709339793 ) ) ;
#73542 = CARTESIAN_POINT ( 'NONE',  ( 101.7220374796297335, -27.76276858577408291, 81.50419670448295051 ) ) ;
#73541 = CARTESIAN_POINT ( 'NONE',  ( -487.2989999999999782, 101.9113919710471947, 11.11250000000054072 ) ) ;
#73543 = CARTESIAN_POINT ( 'NONE',  ( 120.9980108323096317, 74.55612360026276519, 49.04309508044801191 ) ) ;
#73544 = CARTESIAN_POINT ( 'NONE',  ( 97.53097521295029537, -31.04728477963730171, 130.9108633711489915 ) ) ;
#73545 = ORIENTED_EDGE ( 'NONE', *, *, #59881, .T. ) ;
#73546 = DIRECTION ( 'NONE',  ( -0.8660254037844387076, -0.4999999999999998890, 0.000000000000000000 ) ) ;
#73547 = ORIENTED_EDGE ( 'NONE', *, *, #46780, .T. ) ;
#73548 = DIRECTION ( 'NONE',  ( 1.000000000000000000, 0.000000000000000000, -2.544367396927093851E-16 ) ) ;
#73549 = CARTESIAN_POINT ( 'NONE',  ( -50.03799999999999670, 0.000000000000000000, 191.3008000794699797 ) ) ;
#73550 = PRODUCT ( 'Workpiece Locating V-Block', 'Workpiece Locating V-Block', '', ( #80852 ) ) ;
#73551 = CARTESIAN_POINT ( 'NONE',  ( 135.7052281011855541, -34.51875982969371393, 2.060081176883824305 ) ) ;
#73552 = ORIENTED_EDGE ( 'NONE', *, *, #89069, .T. ) ;
#73553 = CARTESIAN_POINT ( 'NONE',  ( 164.9212702847357548, -29.73316016638997894, 313.9678068554149490 ) ) ;
#73555 = EDGE_LOOP ( 'NONE', ( #28308, #36557 ) ) ;
#73554 = CARTESIAN_POINT ( 'NONE',  ( 97.18391573584769105, -31.67496972499959895, 95.96229194257799122 ) ) ;
#73556 = CARTESIAN_POINT ( 'NONE',  ( 72.96458098368701428, 117.4749999999999943, -67.92268098368680285 ) ) ;
#73557 = CARTESIAN_POINT ( 'NONE',  ( -130.0919229099370398, 88.91113633199481114, -10.99998730946133918 ) ) ;
#73558 = AXIS2_PLACEMENT_3D ( 'NONE', #85858, #45805, #58992 ) ;
#73559 = DIRECTION ( 'NONE',  ( -0.8571673007021084478, -0.5150380749100604838, -8.571673007021083688E-16 ) ) ;
#73560 = VERTEX_POINT ( 'NONE', #40231 ) ;
#73561 = AXIS2_PLACEMENT_3D ( 'NONE', #46882, #34162, #81010 ) ;
#73562 = CARTESIAN_POINT ( 'NONE',  ( 109.5136938427377373, -46.88609643433851915, 132.7641967044819751 ) ) ;
#73563 = EDGE_CURVE ( 'NONE', #10086, #74993, #68850, .T. ) ;
#73564 = APPLICATION_PROTOCOL_DEFINITION ( 'draft international standard', 'automotive_design', 1998, #14364 ) ;
#73565 = DIRECTION ( 'NONE',  ( -0.7071067812162665778, -0.7071067811568285677, -6.612322856132800227E-17 ) ) ;
#73566 = EDGE_CURVE ( 'NONE', #59106, #24430, #5280, .T. ) ;
#73567 = DIRECTION ( 'NONE',  ( 0.000000000000000000, 0.000000000000000000, 1.000000000000000000 ) ) ;
#73568 = ORIENTED_EDGE ( 'NONE', *, *, #60600, .F. ) ;
#73569 = EDGE_CURVE ( 'NONE', #54266, #66028, #61130, .T. ) ;
#73570 = ORIENTED_EDGE ( 'NONE', *, *, #4979, .F. ) ;
#73571 = FACE_OUTER_BOUND ( 'NONE', #62461, .T. ) ;
#73572 = LINE ( 'NONE', #44963, #51231 ) ;
#73573 = DIRECTION ( 'NONE',  ( 0.000000000000000000, 0.000000000000000000, -1.000000000000000000 ) ) ;
#73574 = EDGE_CURVE ( 'NONE', #83432, #58568, #37413, .T. ) ;
#73575 = ADVANCED_FACE ( 'NONE', ( #18448, #74326 ), #60216, .T. ) ;
#73577 = DIRECTION ( 'NONE',  ( 0.000000000000000000, 0.000000000000000000, 1.000000000000000000 ) ) ;
#73576 = FACE_OUTER_BOUND ( 'NONE', #32337, .T. ) ;
#73578 = CARTESIAN_POINT ( 'NONE',  ( 90.44969454456416713, -50.82895651782500579, 219.5838068554169809 ) ) ;
#73579 = VECTOR ( 'NONE', #78951, 1000.000000000000000 ) ;
#73580 = ADVANCED_FACE ( 'NONE', ( #11652 ), #46136, .F. ) ;
#73581 = ORIENTED_EDGE ( 'NONE', *, *, #14142, .F. ) ;
#73583 = EDGE_CURVE ( 'NONE', #3527, #27939, #40726, .T. ) ;
#73582 = DIRECTION ( 'NONE',  ( 0.000000000000000000, 0.000000000000000000, -1.000000000000000000 ) ) ;
#73584 = CARTESIAN_POINT ( 'NONE',  ( 115.8019334949657804, -41.12891815432276843, 199.4556252759109611 ) ) ;
#73586 = VERTEX_POINT ( 'NONE', #47031 ) ;
#73585 = CARTESIAN_POINT ( 'NONE',  ( 107.0664832912750057, -36.72944715993903486, 0.4256252759109709349 ) ) ;
#73587 = CARTESIAN_POINT ( 'NONE',  ( 113.0644005321300227, -46.09090919705343481, 64.02991099019594401 ) ) ;
#73588 = CARTESIAN_POINT ( 'NONE',  ( 110.8542690866539004, -45.98432040429123902, 52.88560783171133295 ) ) ;
#73589 = DIRECTION ( 'NONE',  ( 0.5000000000000003331, 0.000000000000000000, 0.8660254037844383745 ) ) ;
#73590 = EDGE_CURVE ( 'NONE', #83707, #34621, #21176, .T. ) ;
#73591 = DIRECTION ( 'NONE',  ( -1.000000000000000000, -4.012088370409549976E-14, 0.000000000000000000 ) ) ;
#73592 = ORIENTED_EDGE ( 'NONE', *, *, #57401, .T. ) ;
#73593 = FACE_OUTER_BOUND ( 'NONE', #48542, .T. ) ;
#73594 = VECTOR ( 'NONE', #19357, 1000.000000000000000 ) ;
#73595 = VERTEX_POINT ( 'NONE', #20261 ) ;
#73596 = ORIENTED_EDGE ( 'NONE', *, *, #52522, .T. ) ;
#73597 = CARTESIAN_POINT ( 'NONE',  ( 110.9273191204289191, -44.70580129652318391, 244.3672975916109635 ) ) ;
#73598 = VECTOR ( 'NONE', #72789, 1000.000000000000000 ) ;
#73599 = LINE ( 'NONE', #82233, #80687 ) ;
#73600 = VECTOR ( 'NONE', #45333, 1000.000000000000114 ) ;
#73601 = CARTESIAN_POINT ( 'NONE',  ( -117.9898589647455083, 87.79588542099531878, -11.57341593931141155 ) ) ;
#73602 = CARTESIAN_POINT ( 'NONE',  ( -44.45000000000000284, 114.2999999999999972, 206.3750000000000000 ) ) ;
#73603 = DIRECTION ( 'NONE',  ( -0.9254794337955620787, -0.3787978585227822492, 0.000000000000000000 ) ) ;
#73604 = EDGE_LOOP ( 'NONE', ( #6235, #8937, #30817, #66827, #57216, #6582, #34337, #79138 ) ) ;
#73605 = CARTESIAN_POINT ( 'NONE',  ( 0.000000000000000000, 92.07499999999998863, 0.000000000000000000 ) ) ;
#73606 = PLANE ( 'NONE',  #19789 ) ;
#73607 = ORIENTED_EDGE ( 'NONE', *, *, #35385, .T. ) ;
#73608 = CARTESIAN_POINT ( 'NONE',  ( 116.7272869458707305, -31.35841744470506498, 29.24229194257799236 ) ) ;
#73609 = ORIENTED_EDGE ( 'NONE', *, *, #34266, .F. ) ;
#73610 = ORIENTED_EDGE ( 'NONE', *, *, #85477, .T. ) ;
#73611 = CARTESIAN_POINT ( 'NONE',  ( 106.0563433008199752, -28.62948770221197137, 267.9938046553056665 ) ) ;
#73612 = EDGE_CURVE ( 'NONE', #18423, #20334, #74766, .T. ) ;
#73613 = VECTOR ( 'NONE', #31647, 1000.000000000000000 ) ;
#73614 = FACE_OUTER_BOUND ( 'NONE', #10384, .T. ) ;
#73615 = CARTESIAN_POINT ( 'NONE',  ( 23.05726497218590154, 77.84977045057786427, 303.6782364904642009 ) ) ;
#73616 = CARTESIAN_POINT ( 'NONE',  ( 37.56670390244716629, -48.82844715994106366, 180.4678068554150911 ) ) ;
#73617 = VECTOR ( 'NONE', #81891, 1000.000000000000000 ) ;
#73619 = ADVANCED_FACE ( 'NONE', ( #75219 ), #26612, .T. ) ;
#73618 = DIRECTION ( 'NONE',  ( 0.000000000000000000, 1.000000000000000000, 0.000000000000000000 ) ) ;
#73620 = VECTOR ( 'NONE', #1725, 1000.000000000000000 ) ;
#73621 = CARTESIAN_POINT ( 'NONE',  ( 116.8983464293968524, -40.32492306460803633, 214.5470538473389581 ) ) ;
#73622 = CARTESIAN_POINT ( 'NONE',  ( 182.5667039024480118, -32.29483332968450782, 117.4678068554150627 ) ) ;
#73623 = AXIS2_PLACEMENT_3D ( 'NONE', #32135, #10798, #52557 ) ;
#73624 = ORIENTED_EDGE ( 'NONE', *, *, #16518, .T. ) ;
#73625 = CARTESIAN_POINT ( 'NONE',  ( 110.1708544452211100, -46.72723989065711692, 93.81562527591097478 ) ) ;
#73626 = CARTESIAN_POINT ( 'NONE',  ( 255.9983484187079910, 40.03750000000000142, -2.032000000000000028 ) ) ;
#73627 = VERTEX_POINT ( 'NONE', #7520 ) ;
#73628 = EDGE_LOOP ( 'NONE', ( #76941, #76409, #80492, #42166 ) ) ;
#73629 = ORIENTED_EDGE ( 'NONE', *, *, #2548, .T. ) ;
#73630 = FACE_OUTER_BOUND ( 'NONE', #79359, .T. ) ;
#73631 = PLANE ( 'NONE',  #73275 ) ;
#73632 = CARTESIAN_POINT ( 'NONE',  ( 117.0724204941129472, -35.46684028317002202, 153.9277302053984897 ) ) ;
#73633 = CARTESIAN_POINT ( 'NONE',  ( 99.66770068389166681, -32.23957622922084454, 123.6985665600679738 ) ) ;
#73634 = CARTESIAN_POINT ( 'NONE',  ( 104.3186933571878399, -25.99935600364358024, 241.2880062282919482 ) ) ;
#73635 = DIRECTION ( 'NONE',  ( 0.000000000000000000, -0.4999999999999998890, 0.8660254037844387076 ) ) ;
#73636 = VERTEX_POINT ( 'NONE', #35209 ) ;
#73637 = CARTESIAN_POINT ( 'NONE',  ( 136.6144450028905055, -37.76411817600060772, 2.828498113172214445 ) ) ;
#73638 = ORIENTED_EDGE ( 'NONE', *, *, #12175, .F. ) ;
#73640 = ORIENTED_EDGE ( 'NONE', *, *, #35530, .F. ) ;
#73639 = AXIS2_PLACEMENT_3D ( 'NONE', #47410, #76481, #55109 ) ;
#73641 = CARTESIAN_POINT ( 'NONE',  ( 83.56670390244799762, -36.72944715994108122, 239.5838068554169809 ) ) ;
#73642 = ORIENTED_EDGE ( 'NONE', *, *, #74185, .T. ) ;
#73643 = ORIENTED_EDGE ( 'NONE', *, *, #49136, .F. ) ;
#73644 = DIRECTION ( 'NONE',  ( 1.047445008332813989E-14, 0.000000000000000000, -1.000000000000000000 ) ) ;
#73645 = FACE_OUTER_BOUND ( 'NONE', #15226, .T. ) ;
#73646 = PLANE ( 'NONE',  #67824 ) ;
#73647 = CARTESIAN_POINT ( 'NONE',  ( 112.3908963168805712, -43.44530362507355647, 167.5324198280769963 ) ) ;
#73648 = CARTESIAN_POINT ( 'NONE',  ( 96.61485869678695337, -32.99094118449985302, 26.06514908543494613 ) ) ;
#73649 = LINE ( 'NONE', #60001, #39369 ) ;
#73650 = ORIENTED_EDGE ( 'NONE', *, *, #35254, .F. ) ;
#73651 = CARTESIAN_POINT ( 'NONE',  ( 141.0667039024479834, -58.72944715994110254, 310.9178068554150514 ) ) ;
#73652 = VERTEX_POINT ( 'NONE', #42464 ) ;
#73653 = DIRECTION ( 'NONE',  ( 1.000000000000000078E-15, -1.000000000000000083E-30, -1.000000000000000000 ) ) ;
#73654 = EDGE_LOOP ( 'NONE', ( #15513, #76861, #28695, #1271 ) ) ;
#73655 = DIRECTION ( 'NONE',  ( -1.000000000000000000, -2.756263715554006823E-15, 0.000000000000000000 ) ) ;
#73656 = VECTOR ( 'NONE', #70887, 1000.000000000000000 ) ;
#73657 = CARTESIAN_POINT ( 'NONE',  ( 105.9716693386988311, -11.55321978063677690, 320.5359728645732389 ) ) ;
#73658 = DIRECTION ( 'NONE',  ( -2.900000000000000265E-14, 2.000000000000000155E-15, -1.000000000000000000 ) ) ;
#73659 = EDGE_CURVE ( 'NONE', #72873, #8213, #34772, .T. ) ;
#73661 = FACE_OUTER_BOUND ( 'NONE', #51939, .T. ) ;
#73660 = AXIS2_PLACEMENT_3D ( 'NONE', #58924, #29913, #64429 ) ;
#73662 = ORIENTED_EDGE ( 'NONE', *, *, #67522, .F. ) ;
#73663 = VECTOR ( 'NONE', #70127, 1000.000000000000000 ) ;
#73664 = CARTESIAN_POINT ( 'NONE',  ( 96.32141381413643444, -39.41948438522342713, 16.53372051400597798 ) ) ;
#73665 = CARTESIAN_POINT ( 'NONE',  ( 107.6091111025649809, -48.61711588689897212, 38.61276813305397582 ) ) ;
#73666 =( LENGTH_UNIT ( ) NAMED_UNIT ( * ) SI_UNIT ( .MILLI., .METRE. ) );
#73667 = EDGE_CURVE ( 'NONE', #54028, #73279, #8425, .T. ) ;
#73669 = CYLINDRICAL_SURFACE ( 'NONE', #76082, 9.524999999999998579 ) ;
#73668 = CARTESIAN_POINT ( 'NONE',  ( 183.5150000000000148, 36.86249999999999716, -53.61543552338530105 ) ) ;
#73670 = CARTESIAN_POINT ( 'NONE',  ( 97.06107015462058030, -37.99640499814212546, 147.4278258600957940 ) ) ;
#73671 = EDGE_CURVE ( 'NONE', #22054, #18083, #48372, .T. ) ;
#73672 = PLANE ( 'NONE',  #23501 ) ;
#73673 = CARTESIAN_POINT ( 'NONE',  ( 132.8222787434396253, -39.18254450372684516, 7.982620440119482019 ) ) ;
#73675 = EDGE_CURVE ( 'NONE', #29586, #62958, #48826, .T. ) ;
#73674 = VECTOR ( 'NONE', #41637, 1000.000000000000000 ) ;
#73676 = DIRECTION ( 'NONE',  ( 0.000000000000000000, 1.000000000000000000, 0.000000000000000000 ) ) ;
#73677 = VECTOR ( 'NONE', #49961, 1000.000000000000000 ) ;
#73678 = FACE_OUTER_BOUND ( 'NONE', #88521, .T. ) ;
#73679 = EDGE_CURVE ( 'NONE', #23550, #40647, #27955, .T. ) ;
#73680 = EDGE_LOOP ( 'NONE', ( #75006, #69809, #8067, #4968 ) ) ;
#73681 = CARTESIAN_POINT ( 'NONE',  ( 97.03298259997053776, -33.74021148472603215, 31.09562527591097592 ) ) ;
#73682 = CARTESIAN_POINT ( 'NONE',  ( 101.4046705256369734, -45.52519664383009257, 218.1213395616249784 ) ) ;
#73683 = CARTESIAN_POINT ( 'NONE',  ( 110.3788355960759162, -47.29890920647816444, 48.80610146638797175 ) ) ;
#73684 = VECTOR ( 'NONE', #79891, 1000.000000000000000 ) ;
#73685 = VECTOR ( 'NONE', #20939, 1000.000000000000000 ) ;
#73687 = CARTESIAN_POINT ( 'NONE',  ( 188.5667039024479834, -48.82844715994099971, 137.2178068554150059 ) ) ;
#73686 = CARTESIAN_POINT ( 'NONE',  ( 117.0715322531006990, -35.45947498896153860, 173.9259864712019521 ) ) ;
#73688 = DIRECTION ( 'NONE',  ( -3.100000000000000258E-29, 3.100000000000000044E-14, 1.000000000000000000 ) ) ;
#73690 = ADVANCED_FACE ( 'NONE', ( #35664 ), #1159, .F. ) ;
#73689 = VECTOR ( 'NONE', #59728, 1000.000000000000000 ) ;
#73691 = ORIENTED_EDGE ( 'NONE', *, *, #43620, .F. ) ;
#73692 = DIRECTION ( 'NONE',  ( 0.000000000000000000, 1.000000000000000000, 0.000000000000000000 ) ) ;
#73693 = ORIENTED_EDGE ( 'NONE', *, *, #74004, .F. ) ;
#73694 = ADVANCED_FACE ( 'NONE', ( #76106 ), #1660, .T. ) ;
#73695 = CARTESIAN_POINT ( 'NONE',  ( 103.4440497394146092, -45.85039829771042719, 113.2756252759109827 ) ) ;
#73696 = AXIS2_PLACEMENT_3D ( 'NONE', #76328, #26827, #62697 ) ;
#73698 = VERTEX_POINT ( 'NONE', #43364 ) ;
#73697 = CARTESIAN_POINT ( 'NONE',  ( 10.51819778680380146, 89.66744784449326744, 130.1316157236187507 ) ) ;
#73699 = CARTESIAN_POINT ( 'NONE',  ( 106.3035372762157493, -47.10473409126645805, 218.5184824187679453 ) ) ;
#73700 = CARTESIAN_POINT ( 'NONE',  ( 107.7702177616926065, 120.6499999999999915, 4.179089330879380409E-13 ) ) ;
#73701 = DIRECTION ( 'NONE',  ( 0.000000000000000000, 0.000000000000000000, -1.000000000000000000 ) ) ;
#73702 = LINE ( 'NONE', #2885, #3710 ) ;
#73703 = LINE ( 'NONE', #74593, #61546 ) ;
#73704 = EDGE_CURVE ( 'NONE', #11193, #4142, #85817, .T. ) ;
#73705 = DIRECTION ( 'NONE',  ( -0.7071067811865774377, 0.7071067811865175967, -7.071067811865782003E-16 ) ) ;
#73706 = DIRECTION ( 'NONE',  ( 0.9217329428042198014, 0.3878251953515564066, -1.214306433183767175E-14 ) ) ;
#73707 = CARTESIAN_POINT ( 'NONE',  ( 116.4020974974656042, -33.81230083437810663, 174.0670538473399347 ) ) ;
#73708 = EDGE_LOOP ( 'NONE', ( #59479, #22174, #73160, #71281 ) ) ;
#73709 = ORIENTED_EDGE ( 'NONE', *, *, #1907, .F. ) ;
#73710 = AXIS2_PLACEMENT_3D ( 'NONE', #23184, #78591, #16343 ) ;
#73711 = CARTESIAN_POINT ( 'NONE',  ( 103.7583319442197052, -28.50847317404091186, 126.8130118773259625 ) ) ;
#73712 = CARTESIAN_POINT ( 'NONE',  ( 41.56670390244801894, -27.57844715994070484, -5.074374724088000832 ) ) ;
#73714 = DIRECTION ( 'NONE',  ( 1.000000000000000000, 0.000000000000000000, 0.000000000000000000 ) ) ;
#73713 = CARTESIAN_POINT ( 'NONE',  ( 101.2327472597882263, -44.62129728587211730, 253.0699109901961492 ) ) ;
#73715 = DIRECTION ( 'NONE',  ( -1.000000000000000000, 0.000000000000000000, 0.000000000000000000 ) ) ;
#73716 = DIRECTION ( 'NONE',  ( 3.100000000000000258E-29, -3.100000000000000044E-14, -1.000000000000000000 ) ) ;
#73717 = DIRECTION ( 'NONE',  ( 1.000000000000000078E-15, -1.000000000000000083E-30, -1.000000000000000000 ) ) ;
#73718 = DIRECTION ( 'NONE',  ( 0.000000000000000000, 0.000000000000000000, -1.000000000000000000 ) ) ;
#73719 = PLANE ( 'NONE',  #66693 ) ;
#73720 = LINE ( 'NONE', #74170, #56011 ) ;
#73721 = CARTESIAN_POINT ( 'NONE',  ( 117.3921119255897452, -35.46056622170122097, 193.9241967044829664 ) ) ;
#73722 = ORIENTED_EDGE ( 'NONE', *, *, #33186, .F. ) ;
#73723 = ORIENTED_EDGE ( 'NONE', *, *, #20775, .F. ) ;
#73724 = CARTESIAN_POINT ( 'NONE',  ( 133.3679539845121269, -80.39464238368842075, 249.3134381260879877 ) ) ;
#73725 = CARTESIAN_POINT ( 'NONE',  ( 147.0242276106250756, -67.91655684465823128, 245.8961201463810085 ) ) ;
#73726 = CARTESIAN_POINT ( 'NONE',  ( -48.02966122971776741, 93.07500000000001705, 75.53254848357481421 ) ) ;
#73728 = ADVANCED_FACE ( 'NONE', ( #62920 ), #22066, .T. ) ;
#73727 = CYLINDRICAL_SURFACE ( 'NONE', #49133, 5.041900000000001825 ) ;
#73729 = VECTOR ( 'NONE', #30573, 1000.000000000000114 ) ;
#73730 = ORIENTED_EDGE ( 'NONE', *, *, #43504, .T. ) ;
#73731 = VECTOR ( 'NONE', #78621, 1000.000000000000000 ) ;
#73732 = CARTESIAN_POINT ( 'NONE',  ( 117.0604406654448582, -38.08365174049107083, 63.71870391512912590 ) ) ;
#73733 = CARTESIAN_POINT ( 'NONE',  ( 106.9404395787681352, -47.78219344473501451, 232.5794347997199907 ) ) ;
#73734 = CARTESIAN_POINT ( 'NONE',  ( 107.0664832912739968, -36.72944715994100306, 287.6356252759109680 ) ) ;
#73735 = ORIENTED_EDGE ( 'NONE', *, *, #88496, .T. ) ;
#73736 = EDGE_LOOP ( 'NONE', ( #22765, #13343, #12931, #26664 ) ) ;
#73737 = CARTESIAN_POINT ( 'NONE',  ( -10.09446275336743781, 74.79825716961998694, 118.1263904669630733 ) ) ;
#73738 = CARTESIAN_POINT ( 'NONE',  ( 86.06670390244796920, -48.82844715994099971, 250.9178068554150514 ) ) ;
#73739 = CARTESIAN_POINT ( 'NONE',  ( 104.8541313898159757, -44.58662387026339502, 20.17666179816296435 ) ) ;
#73740 = VECTOR ( 'NONE', #73822, 1000.000000000000000 ) ;
#73741 = DIRECTION ( 'NONE',  ( 1.000000000000000000, 0.000000000000000000, 0.000000000000000000 ) ) ;
#73742 = VERTEX_POINT ( 'NONE', #55184 ) ;
#73743 = ADVANCED_FACE ( 'NONE', ( #84743 ), #28864, .T. ) ;
#73744 = VECTOR ( 'NONE', #37086, 1000.000000000000114 ) ;
#73745 = AXIS2_PLACEMENT_3D ( 'NONE', #55763, #27195, #55325 ) ;
#73746 = CARTESIAN_POINT ( 'NONE',  ( 186.6899999999999977, 59.08750000000000568, -38.10000000000000142 ) ) ;
#73747 = CARTESIAN_POINT ( 'NONE',  ( 81.36335724985904960, -16.30134337669397127, 7.962481652680392763 ) ) ;
#73748 = EDGE_LOOP ( 'NONE', ( #83519, #62028, #38883, #58573 ) ) ;
#73749 = ORIENTED_EDGE ( 'NONE', *, *, #37152, .T. ) ;
#73750 = ADVANCED_FACE ( 'NONE', ( #82945 ), #28400, .T. ) ;
#73751 = DIRECTION ( 'NONE',  ( 1.000000000000000078E-15, -1.000000000000000083E-30, -1.000000000000000000 ) ) ;
#73752 = VERTEX_POINT ( 'NONE', #71108 ) ;
#73753 = VERTEX_POINT ( 'NONE', #13885 ) ;
#73754 = CARTESIAN_POINT ( 'NONE',  ( 163.5667039024460223, -18.82844715994111340, -5.074374724088000832 ) ) ;
#73755 = AXIS2_PLACEMENT_3D ( 'NONE', #20373, #89414, #27172 ) ;
#73756 = CARTESIAN_POINT ( 'NONE',  ( 113.0365282982730264, -42.83802263516175657, 72.61527697093394806 ) ) ;
#73757 = CARTESIAN_POINT ( 'NONE',  ( 98.41658590534017037, -29.81029140585139814, 195.7775300378159784 ) ) ;
#73758 = CARTESIAN_POINT ( 'NONE',  ( 109.8501361970267425, -26.70547878262030395, 174.8613395616249591 ) ) ;
#73760 = CARTESIAN_POINT ( 'NONE',  ( 106.8364377494367403, -47.15199802307920152, 268.5584824187679374 ) ) ;
#73759 = CARTESIAN_POINT ( 'NONE',  ( 101.1175715082527660, -44.88412347719182804, 22.07575109432372074 ) ) ;
#73761 = CARTESIAN_POINT ( 'NONE',  ( 128.0667039024480118, -50.82844715994100682, 10.91780685541499807 ) ) ;
#73762 = CARTESIAN_POINT ( 'NONE',  ( 92.81551872686563343, -113.5468731908971307, -11.78219314458173272 ) ) ;
#73763 = ORIENTED_EDGE ( 'NONE', *, *, #82972, .T. ) ;
#73764 = ORIENTED_EDGE ( 'NONE', *, *, #31026, .F. ) ;
#73765 = CIRCLE ( 'NONE', #21532, 3.250000000000002665 ) ;
#73766 = AXIS2_PLACEMENT_3D ( 'NONE', #78979, #52996, #31698 ) ;
#73767 = CARTESIAN_POINT ( 'NONE',  ( -487.2989999999999782, 21.43125000000035030, 6.988054014476359654 ) ) ;
#73768 = CARTESIAN_POINT ( 'NONE',  ( 117.5184129516626257, -36.12626193255995588, 228.8727681330539667 ) ) ;
#73769 = ORIENTED_EDGE ( 'NONE', *, *, #9684, .F. ) ;
#73770 = CARTESIAN_POINT ( 'NONE',  ( 98.26116833961376074, -42.31097554054522902, 186.7756252759109543 ) ) ;
#73771 = CARTESIAN_POINT ( 'NONE',  ( 172.5664832912729878, -18.82844715994071194, 18.92562527591200094 ) ) ;
#73772 = CARTESIAN_POINT ( 'NONE',  ( -20.24703904125878040, 63.07654896400417499, 32.27577670923775344 ) ) ;
#73773 = CARTESIAN_POINT ( 'NONE',  ( 177.8371591254543489, -47.82818131005478079, 237.4678068554150059 ) ) ;
#73774 = CARTESIAN_POINT ( 'NONE',  ( 80.06648329127399677, -18.72944715994105991, -5.074374724089057764 ) ) ;
#73775 = EDGE_CURVE ( 'NONE', #56608, #84350, #49286, .T. ) ;
#73777 = DIRECTION ( 'NONE',  ( 0.000000000000000000, 1.000000000000000000, 0.000000000000000000 ) ) ;
#73776 = CARTESIAN_POINT ( 'NONE',  ( 110.8744162906118333, -29.68297622160992688, 277.6356252759108543 ) ) ;
#73778 = CARTESIAN_POINT ( 'NONE',  ( 97.81170986510684884, -40.51745644794008427, 172.6354259520616097 ) ) ;
#73779 = EDGE_CURVE ( 'NONE', #32950, #41217, #62573, .T. ) ;
#73780 = CARTESIAN_POINT ( 'NONE',  ( 75.61066417432020614, 101.5999999999999943, 177.0380000000000109 ) ) ;
#73781 = DIRECTION ( 'NONE',  ( 0.7071067811869283792, -0.7071067811861665442, 7.071067811868979848E-16 ) ) ;
#73782 = ADVANCED_FACE ( 'NONE', ( #70193 ), #7966, .F. ) ;
#73783 = CARTESIAN_POINT ( 'NONE',  ( 53.35959712126227572, -48.62134037875156878, 300.4678068554150059 ) ) ;
#73784 = CARTESIAN_POINT ( 'NONE',  ( 144.0667039024470739, -137.6784471599409017, 55.21780685541800437 ) ) ;
#73785 = CARTESIAN_POINT ( 'NONE',  ( 69.15045923641616810, -139.7622024939100811, 245.5930228695460187 ) ) ;
#73787 = ORIENTED_EDGE ( 'NONE', *, *, #89495, .T. ) ;
#73786 = DIRECTION ( 'NONE',  ( -1.000000000000000078E-15, 1.000000000000000083E-30, 1.000000000000000000 ) ) ;
#73788 = AXIS2_PLACEMENT_3D ( 'NONE', #77930, #8896, #72882 ) ;
#73789 = EDGE_CURVE ( 'NONE', #85398, #73516, #16833, .T. ) ;
#73790 = DIRECTION ( 'NONE',  ( 0.7071067811865779928, -0.7071067811865171526, 7.071067811865786933E-16 ) ) ;
#73791 = CARTESIAN_POINT ( 'NONE',  ( 112.4658351597014843, -45.71473303307890035, 238.0070538473389377 ) ) ;
#73792 = CARTESIAN_POINT ( 'NONE',  ( 98.20239980326637408, -43.33262854484335946, 107.8480062282919647 ) ) ;
#73793 = CARTESIAN_POINT ( 'NONE',  ( 113.1252749404788034, -46.02936877844707197, 219.0480062282919960 ) ) ;
#73794 = DIRECTION ( 'NONE',  ( 0.000000000000000000, 1.000000000000000000, 0.000000000000000000 ) ) ;
#73795 = DIRECTION ( 'NONE',  ( 0.000000000000000000, 0.000000000000000000, -1.000000000000000000 ) ) ;
#73797 = DIRECTION ( 'NONE',  ( -3.100000000000000258E-29, 3.100000000000000044E-14, 1.000000000000000000 ) ) ;
#73796 = CARTESIAN_POINT ( 'NONE',  ( 188.5667039024479834, -67.87844715994100397, 293.2178068554150627 ) ) ;
#73798 = LINE ( 'NONE', #65203, #36364 ) ;
#73799 = CARTESIAN_POINT ( 'NONE',  ( 132.9844404253379366, -21.25772566032916799, 1.807989669955668122 ) ) ;
#73800 = AXIS2_PLACEMENT_3D ( 'NONE', #80076, #4652, #32338 ) ;
#73801 = AXIS2_PLACEMENT_3D ( 'NONE', #2807, #85494, #84595 ) ;
#73802 = VERTEX_POINT ( 'NONE', #71990 ) ;
#73803 = ORIENTED_EDGE ( 'NONE', *, *, #58531, .T. ) ;
#73804 = EDGE_CURVE ( 'NONE', #12675, #20444, #73649, .T. ) ;
#73805 = CARTESIAN_POINT ( 'NONE',  ( 102.9824767429641525, -29.22764064321736299, 144.8952769709339634 ) ) ;
#73806 = AXIS2_PLACEMENT_3D ( 'NONE', #14982, #20896, #49474 ) ;
#73808 = ORIENTED_EDGE ( 'NONE', *, *, #43712, .T. ) ;
#73807 = CARTESIAN_POINT ( 'NONE',  ( -465.6921742093539933, 60.32499999999999574, 3.174999999999999822 ) ) ;
#73809 = CARTESIAN_POINT ( 'NONE',  ( 113.2453749487971209, -28.75857822357426130, 89.55142878775579618 ) ) ;
#73810 = CARTESIAN_POINT ( 'NONE',  ( 109.0680860650138300, -47.57644715601873742, 123.7337205140059666 ) ) ;
#73811 = CYLINDRICAL_SURFACE ( 'NONE', #17858, 5.041900000000000048 ) ;
#73812 = CARTESIAN_POINT ( 'NONE',  ( 79.41328093382365694, -16.05633243510679264, 8.161687850942282552 ) ) ;
#73813 = DIRECTION ( 'NONE',  ( 0.000000000000000000, 0.000000000000000000, 1.000000000000000000 ) ) ;
#73814 = CARTESIAN_POINT ( 'NONE',  ( 152.0368932755770288, -23.42844715993588522, 313.9678068554149490 ) ) ;
#73815 = AXIS2_PLACEMENT_3D ( 'NONE', #25741, #62944, #50206 ) ;
#73816 = CARTESIAN_POINT ( 'NONE',  ( 116.0809032858471852, -32.84949784884745583, 79.14991099019697174 ) ) ;
#73817 = VERTEX_POINT ( 'NONE', #85636 ) ;
#73818 = ORIENTED_EDGE ( 'NONE', *, *, #32996, .F. ) ;
#73819 = EDGE_LOOP ( 'NONE', ( #67922, #72693 ) ) ;
#73820 = DIRECTION ( 'NONE',  ( 1.000000000000000000, 0.000000000000000000, 0.000000000000000000 ) ) ;
#73822 = DIRECTION ( 'NONE',  ( 1.000000000000000000, 0.000000000000000000, 6.982966722218760189E-15 ) ) ;
#73821 = CARTESIAN_POINT ( 'NONE',  ( 103.2980200187117816, -27.06831524915196141, 166.3603871806719496 ) ) ;
#73823 = CARTESIAN_POINT ( 'NONE',  ( 96.06648329127393993, -36.72944715994093912, 312.6356252759112522 ) ) ;
#73824 = CARTESIAN_POINT ( 'NONE',  ( -479.3614999999999782, 104.7749999999999915, -1.387778780781445991E-14 ) ) ;
#73825 = VECTOR ( 'NONE', #5405, 1000.000000000000000 ) ;
#73826 = LINE ( 'NONE', #67008, #54849 ) ;
#73827 = DIRECTION ( 'NONE',  ( 0.000000000000000000, 0.000000000000000000, -1.000000000000000000 ) ) ;
#73828 = CARTESIAN_POINT ( 'NONE',  ( 67.06796439462205228, -67.87878520888916967, 245.5492565716537001 ) ) ;
#73829 = CARTESIAN_POINT ( 'NONE',  ( 97.28692064948100438, -31.62807703868913833, 90.93181575210196854 ) ) ;
#73830 = EDGE_LOOP ( 'NONE', ( #65059, #12721, #50386, #38231 ) ) ;
#73831 = VERTEX_POINT ( 'NONE', #86073 ) ;
#73832 = CARTESIAN_POINT ( 'NONE',  ( 11.41209158312316774, 88.18445188672593815, 130.0566639163489810 ) ) ;
#73833 = PLANE ( 'NONE',  #67837 ) ;
#73835 = EDGE_CURVE ( 'NONE', #76109, #82989, #84392, .T. ) ;
#73834 = DIRECTION ( 'NONE',  ( -4.237773401492740281E-14, 1.000000000000000000, 0.000000000000000000 ) ) ;
#73836 = CARTESIAN_POINT ( 'NONE',  ( 108.3793409795780036, -28.17508408765456096, 142.7614237029239632 ) ) ;
#73837 = CIRCLE ( 'NONE', #34662, 8.928099999999993486 ) ;
#73838 = EDGE_CURVE ( 'NONE', #56630, #23079, #36582, .T. ) ;
#73839 = CARTESIAN_POINT ( 'NONE',  ( -254.0000000000000000, 14.28749999999982201, 85.72499999999999432 ) ) ;
#73840 = ORIENTED_EDGE ( 'NONE', *, *, #35071, .F. ) ;
#73841 = VERTEX_POINT ( 'NONE', #2506 ) ;
#73842 = DIRECTION ( 'NONE',  ( 0.000000000000000000, 0.000000000000000000, 1.000000000000000000 ) ) ;
#73843 = ORIENTED_EDGE ( 'NONE', *, *, #31602, .F. ) ;
#73844 = ORIENTED_EDGE ( 'NONE', *, *, #57285, .T. ) ;
#73845 = LINE ( 'NONE', #26591, #73927 ) ;
#73846 = CARTESIAN_POINT ( 'NONE',  ( 114.9579445475069264, -42.99008164810605592, 194.7244404487539668 ) ) ;
#73847 = AXIS2_PLACEMENT_3D ( 'NONE', #26424, #5993, #26862 ) ;
#73848 = LINE ( 'NONE', #39327, #26413 ) ;
#73849 = DIRECTION ( 'NONE',  ( -3.100000000000000258E-29, 3.100000000000000044E-14, 1.000000000000000000 ) ) ;
#73850 = CARTESIAN_POINT ( 'NONE',  ( -109.9641975813423329, 60.51899751744934974, 70.37584683824053400 ) ) ;
#73851 = AXIS2_PLACEMENT_3D ( 'NONE', #47092, #12608, #74830 ) ;
#73852 = VERTEX_POINT ( 'NONE', #18688 ) ;
#73854 = ORIENTED_EDGE ( 'NONE', *, *, #15423, .F. ) ;
#73853 = AXIS2_PLACEMENT_3D ( 'NONE', #77659, #4370, #70853 ) ;
#73855 = EDGE_CURVE ( 'NONE', #71100, #1395, #49537, .T. ) ;
#73856 = ORIENTED_EDGE ( 'NONE', *, *, #60966, .F. ) ;
#73857 = ORIENTED_EDGE ( 'NONE', *, *, #81140, .T. ) ;
#73858 = CARTESIAN_POINT ( 'NONE',  ( 113.6383730011278601, -31.09817814777808564, 227.2204713219719565 ) ) ;
#73859 = AXIS2_PLACEMENT_3D ( 'NONE', #2716, #15896, #85843 ) ;
#73860 = CARTESIAN_POINT ( 'NONE',  ( 117.8983839226775387, -39.04577396070462214, 108.6708633711489824 ) ) ;
#73861 = CARTESIAN_POINT ( 'NONE',  ( 98.73996931189270754, -42.96625968561445319, 66.83848241876793850 ) ) ;
#73862 = CARTESIAN_POINT ( 'NONE',  ( 116.3186249068845939, -32.94868901192853627, 254.1356252759109395 ) ) ;
#73863 = CARTESIAN_POINT ( 'NONE',  ( 193.0371591254586292, -47.82818131005411999, 180.4678068554150343 ) ) ;
#73864 = CARTESIAN_POINT ( 'NONE',  ( 36.65249034007530327, -49.32844715994124130, 300.4678068554150059 ) ) ;
#73865 = MECHANICAL_DESIGN_GEOMETRIC_PRESENTATION_REPRESENTATION (  '', ( #8802 ), #1534 ) ;
#73866 = CARTESIAN_POINT ( 'NONE',  ( 99.10138041440774259, -45.50374834597938900, 152.9899109901969894 ) ) ;
#73867 = CARTESIAN_POINT ( 'NONE',  ( 107.8173249548519692, -46.71069529603006032, 277.6356222035115024 ) ) ;
#73868 = ORIENTED_EDGE ( 'NONE', *, *, #46506, .F. ) ;
#73869 = DIRECTION ( 'NONE',  ( -1.000000000000000078E-15, 0.000000000000000000, -1.000000000000000000 ) ) ;
#73870 = ORIENTED_EDGE ( 'NONE', *, *, #37087, .F. ) ;
#73871 = ORIENTED_EDGE ( 'NONE', *, *, #52036, .T. ) ;
#73872 = AXIS2_PLACEMENT_3D ( 'NONE', #49191, #55998, #83297 ) ;
#73873 = CARTESIAN_POINT ( 'NONE',  ( 134.0664832912740110, -8.350947159940998787, 308.6356252759119911 ) ) ;
#73874 = CARTESIAN_POINT ( 'NONE',  ( 90.44969454456413871, -50.82895651782494895, 239.5838068554169809 ) ) ;
#73875 = ORIENTED_EDGE ( 'NONE', *, *, #25159, .F. ) ;
#73876 = CARTESIAN_POINT ( 'NONE',  ( 52.06670390244699576, -67.87844715994100397, 55.21780685541800437 ) ) ;
#73877 = ORIENTED_EDGE ( 'NONE', *, *, #84789, .F. ) ;
#73878 = CARTESIAN_POINT ( 'NONE',  ( 115.0372574989604288, -42.90846257669011976, 178.3022919417056471 ) ) ;
#73879 = CARTESIAN_POINT ( 'NONE',  ( 108.5379876179846264, -26.40851185940291046, 104.9641967044819779 ) ) ;
#73880 = CARTESIAN_POINT ( 'NONE',  ( -3.842181601977885830, 70.44325810012327338, 130.4994487452559611 ) ) ;
#73881 = CARTESIAN_POINT ( 'NONE',  ( 180.2143765759489895, -35.91149509761070391, -5.074374724088000832 ) ) ;
#73882 = DIRECTION ( 'NONE',  ( 0.000000000000000000, 0.000000000000000000, -1.000000000000000000 ) ) ;
#73883 = CARTESIAN_POINT ( 'NONE',  ( 109.5220866130624984, -46.80460460589471694, 87.75467289495897205 ) ) ;
#73885 = CARTESIAN_POINT ( 'NONE',  ( 109.8501361970267425, -26.70547878262040342, 170.8613395616249591 ) ) ;
#73884 = LINE ( 'NONE', #24408, #29005 ) ;
#73886 = CARTESIAN_POINT ( 'NONE',  ( 97.06115785756830405, -37.99686386286577999, 61.42732787508487036 ) ) ;
#73887 = EDGE_CURVE ( 'NONE', #63654, #25238, #3126, .T. ) ;
#73888 = CARTESIAN_POINT ( 'NONE',  ( 50.03799999999999670, 0.000000000000000000, 206.3750000000000000 ) ) ;
#73889 = ORIENTED_EDGE ( 'NONE', *, *, #18534, .T. ) ;
#73890 = AXIS2_PLACEMENT_3D ( 'NONE', #67168, #74441, #86737 ) ;
#73891 = CARTESIAN_POINT ( 'NONE',  ( 177.4809174648213741, -49.32844715993478957, 300.4678068554149490 ) ) ;
#73892 = EDGE_CURVE ( 'NONE', #61198, #61470, #51514, .T. ) ;
#73893 = LINE ( 'NONE', #46162, #65928 ) ;
#73894 = ADVANCED_FACE ( 'NONE', ( #44256 ), #6041, .F. ) ;
#73895 = CARTESIAN_POINT ( 'NONE',  ( 115.8270178786686841, -31.73274795042722829, 134.2399272767322884 ) ) ;
#73896 = CARTESIAN_POINT ( 'NONE',  ( -487.2989999999999782, 10.16305401447644030, 97.63125000000000853 ) ) ;
#73898 = ORIENTED_EDGE ( 'NONE', *, *, #119, .F. ) ;
#73897 = CARTESIAN_POINT ( 'NONE',  ( 117.3784280654263341, -34.92100556036569259, 243.9641967044819637 ) ) ;
#73899 = EDGE_CURVE ( 'NONE', #13532, #43158, #14123, .T. ) ;
#73900 = CARTESIAN_POINT ( 'NONE',  ( 102.0668330567940387, -27.97062182092777149, 145.4898119003854902 ) ) ;
#73901 = CARTESIAN_POINT ( 'NONE',  ( 106.8359569501641744, -47.17378133968975362, 268.5584824187679374 ) ) ;
#73902 = CARTESIAN_POINT ( 'NONE',  ( 108.7502231993919395, -25.75847702231262204, 140.9432443235299672 ) ) ;
#73903 = PLANE ( 'NONE',  #81020 ) ;
#73904 = CARTESIAN_POINT ( 'NONE',  ( 10.09777173618929069, 90.29655250510941755, -130.1657284840294437 ) ) ;
#73905 = CIRCLE ( 'NONE', #27477, 16.72999999999999332 ) ;
#73906 = DIRECTION ( 'NONE',  ( 1.000000000000000000, 0.000000000000000000, 0.000000000000000000 ) ) ;
#73907 = CARTESIAN_POINT ( 'NONE',  ( 116.8174729601854835, -34.15427434069496115, 265.0316169617216815 ) ) ;
#73908 = ORIENTED_EDGE ( 'NONE', *, *, #33170, .T. ) ;
#73909 = B_SPLINE_CURVE_WITH_KNOTS ( 'NONE', 3,
 ( #19477, #13122, #40806, #68076, #54411, #40362, #20386, #48056, #74445, #19027, #68528, #76230, #48488, #82174, #12671, #47160, #34439, #41242, #7198, #19929, #6740, #67625, #82625, #46714, #12220, #26288, #13557, #89424, #6296, #68973, #14004 ),
 .UNSPECIFIED., .F., .F.,
 ( 4, 2, 2, 2, 2, 2, 2, 2, 2, 2, 2, 2, 1, 1, 1, 2, 4 ),
 ( 0.000000000000000000, 0.03125570353835087356, 0.06251140707670174712, 0.09376711061505262068, 0.1250228141534034942, 0.1875342212301058242, 0.2500456283068081542, 0.3125570353835104842, 0.3750684424602129807, 0.4375798495369154217, 0.4688355530752666422, 0.4844634048444423358, 0.4922773307290300160, 0.4961842936713238839, 0.4981377751424709288, 0.4991145158780446733, 0.5000912566136184179 ),
 .UNSPECIFIED. ) ;
#73910 = VERTEX_POINT ( 'NONE', #75001 ) ;
#73911 = ORIENTED_EDGE ( 'NONE', *, *, #31923, .F. ) ;
#73912 = ADVANCED_FACE ( 'NONE', ( #48167 ), #33218, .T. ) ;
#73913 = CONICAL_SURFACE ( 'NONE', #76831, 1.258750000000002922, 1.029744258676650093 ) ;
#73914 = ORIENTED_EDGE ( 'NONE', *, *, #84383, .F. ) ;
#73915 = DIRECTION ( 'NONE',  ( 0.000000000000000000, 0.000000000000000000, 1.000000000000000000 ) ) ;
#73916 = CARTESIAN_POINT ( 'NONE',  ( 117.4658636684176543, -37.01502254527064650, 39.80419670448193159 ) ) ;
#73917 = FACE_OUTER_BOUND ( 'NONE', #36814, .T. ) ;
#73918 = EDGE_CURVE ( 'NONE', #31858, #87649, #5998, .T. ) ;
#73919 = FACE_OUTER_BOUND ( 'NONE', #13846, .T. ) ;
#73920 = AXIS2_PLACEMENT_3D ( 'NONE', #12582, #68886, #290 ) ;
#73922 = CARTESIAN_POINT ( 'NONE',  ( 116.3181333158508295, -32.94392590426259204, 50.13562527591097506 ) ) ;
#73921 = CARTESIAN_POINT ( 'NONE',  ( 41.56648329127399677, -18.82844715994099971, 138.9256252759119832 ) ) ;
#73923 = CARTESIAN_POINT ( 'NONE',  ( 115.1439687268531600, -40.82418761129420659, 247.8876579233149755 ) ) ;
#73924 = VERTEX_POINT ( 'NONE', #48607 ) ;
#73925 = ORIENTED_EDGE ( 'NONE', *, *, #3859, .F. ) ;
#73926 = CIRCLE ( 'NONE', #65242, 9.425000000000000711 ) ;
#73928 = VERTEX_POINT ( 'NONE', #62711 ) ;
#73927 = VECTOR ( 'NONE', #18430, 1000.000000000000000 ) ;
#73929 = DIRECTION ( 'NONE',  ( 1.000000000000000000, 0.000000000000000000, 0.000000000000000000 ) ) ;
#73930 = CARTESIAN_POINT ( 'NONE',  ( 109.6431719188696263, -46.48004672784288260, 102.7812855322859917 ) ) ;
#73931 = DIRECTION ( 'NONE',  ( 1.000000000000000000, 0.000000000000000000, 0.000000000000000000 ) ) ;
#73932 = CARTESIAN_POINT ( 'NONE',  ( 107.0664832912739541, -22.72944715994095688, 312.1356252759112522 ) ) ;
#73933 = CARTESIAN_POINT ( 'NONE',  ( 102.2363890476183599, -29.29987999758196793, 21.96729759161197748 ) ) ;
#73934 = CARTESIAN_POINT ( 'NONE',  ( 118.1932448497438628, 91.23868085022584751, -9.271905035164968112 ) ) ;
#73935 = CONICAL_SURFACE ( 'NONE', #34764, 5.799999999999998934, 0.7853981633974369547 ) ;
#73936 = CARTESIAN_POINT ( 'NONE',  ( 105.7976179630505413, -26.72429355889029168, 175.1774430963942848 ) ) ;
#73937 = PRESENTATION_LAYER_ASSIGNMENT (  '', '', ( #55034 ) ) ;
#73938 = CARTESIAN_POINT ( 'NONE',  ( 116.7002268312856188, -35.03994406823839114, 243.9641967044829585 ) ) ;
#73939 = CARTESIAN_POINT ( 'NONE',  ( 34.92499999999999716, 77.96728223830740490, 310.8325000000000387 ) ) ;
#73940 = ORIENTED_EDGE ( 'NONE', *, *, #60133, .T. ) ;
#73941 = DIRECTION ( 'NONE',  ( 4.299999999999999979E-14, -1.000000000000000000, 0.000000000000000000 ) ) ;
#73942 = CIRCLE ( 'NONE', #43451, 15.99999999999999822 ) ;
#73944 = ADVANCED_FACE ( 'NONE', ( #89085 ), #83621, .T. ) ;
#73943 = LINE ( 'NONE', #60294, #69967 ) ;
#73945 = CARTESIAN_POINT ( 'NONE',  ( 109.0838521367681864, -44.63893190664380484, 45.59380465530593796 ) ) ;
#73946 = CARTESIAN_POINT ( 'NONE',  ( 226.4410000000000025, 52.73749999999999716, -32.00399999999999778 ) ) ;
#73947 = EDGE_CURVE ( 'NONE', #79544, #88157, #344, .T. ) ;
#73948 = DIRECTION ( 'NONE',  ( 0.000000000000000000, 1.000000000000000000, 0.000000000000000000 ) ) ;
#73949 = CIRCLE ( 'NONE', #43530, 7.873999999999991672 ) ;
#73950 = CARTESIAN_POINT ( 'NONE',  ( -12.70000000000000107, 82.54999999999999716, 117.8738102209307641 ) ) ;
#73951 = ORIENTED_EDGE ( 'NONE', *, *, #66702, .T. ) ;
#73952 = LINE ( 'NONE', #32157, #63922 ) ;
#73953 = CARTESIAN_POINT ( 'NONE',  ( 121.2641460698858396, 59.64250688777392639, -48.37286511902529895 ) ) ;
#73954 = ORIENTED_EDGE ( 'NONE', *, *, #25365, .T. ) ;
#73955 = CARTESIAN_POINT ( 'NONE',  ( 96.02342237304465300, -37.20891875426686823, 116.3489586092439652 ) ) ;
#73956 = VERTEX_POINT ( 'NONE', #13669 ) ;
#73957 = CARTESIAN_POINT ( 'NONE',  ( 100.1685590971342776, -42.59726720982692427, 76.32194363760098099 ) ) ;
#73958 = LINE ( 'NONE', #25348, #79407 ) ;
#73959 = CARTESIAN_POINT ( 'NONE',  ( 113.4424924140864590, -42.92691738999312889, 94.64444044875396855 ) ) ;
#73960 = LINE ( 'NONE', #74412, #31422 ) ;
#73961 = CARTESIAN_POINT ( 'NONE',  ( 131.8286707874590036, -67.87844715994091871, 245.6137563247699802 ) ) ;
#73962 = AXIS2_PLACEMENT_3D ( 'NONE', #74610, #18300, #12389 ) ;
#73963 = CARTESIAN_POINT ( 'NONE',  ( 115.4621199703947241, -43.00579008905405232, 24.31562527591096767 ) ) ;
#73964 = CARTESIAN_POINT ( 'NONE',  ( 98.34995908937969489, -31.65640510623499893, 181.9069259909072969 ) ) ;
#73965 = ORIENTED_EDGE ( 'NONE', *, *, #87736, .F. ) ;
#73966 = CARTESIAN_POINT ( 'NONE',  ( 85.06670390244700286, -71.37844715994096134, 55.21780685541800437 ) ) ;
#73967 = ORIENTED_EDGE ( 'NONE', *, *, #22866, .T. ) ;
#73968 = EDGE_CURVE ( 'NONE', #4351, #31932, #41354, .T. ) ;
#73969 = CARTESIAN_POINT ( 'NONE',  ( -118.4231949783269613, 71.15456258041351134, 5.621971333130180604 ) ) ;
#73970 = ORIENTED_EDGE ( 'NONE', *, *, #61069, .F. ) ;
#73971 = VERTEX_POINT ( 'NONE', #13230 ) ;
#73972 = DIRECTION ( 'NONE',  ( 0.000000000000000000, 1.000000000000000000, 2.000000000000000155E-15 ) ) ;
#73973 = ORIENTED_EDGE ( 'NONE', *, *, #14668, .T. ) ;
#73974 = CARTESIAN_POINT ( 'NONE',  ( 116.7002268312856188, -35.03994406823839114, 243.9641967044829585 ) ) ;
#73975 = CARTESIAN_POINT ( 'NONE',  ( 112.0074966433228099, -27.97083403899759801, 124.6671618762774187 ) ) ;
#73976 = CARTESIAN_POINT ( 'NONE',  ( 101.9936208482194075, -45.44607148560456267, 188.1564586008105664 ) ) ;
#73977 = CARTESIAN_POINT ( 'NONE',  ( 105.9884228536615609, -26.36024887173286757, 46.15848241876796720 ) ) ;
#73978 = CARTESIAN_POINT ( 'NONE',  ( 112.1429027457822656, -28.01486178590806730, 95.65578064394281910 ) ) ;
#73979 = ORIENTED_EDGE ( 'NONE', *, *, #61756, .F. ) ;
#73980 = CARTESIAN_POINT ( 'NONE',  ( 50.11670390244700712, -75.72844715994099829, 55.21780685541800437 ) ) ;
#73981 = CIRCLE ( 'NONE', #58034, 17.33514202138210081 ) ;
#73982 = EDGE_CURVE ( 'NONE', #10572, #49269, #40477, .T. ) ;
#73983 = CARTESIAN_POINT ( 'NONE',  ( 71.24025061656124080, 8.642044024269685210, 542.9756252759101471 ) ) ;
#73984 = EDGE_LOOP ( 'NONE', ( #45238, #58337, #22898, #30334 ) ) ;
#73985 = AXIS2_PLACEMENT_3D ( 'NONE', #85079, #50072, #49621 ) ;
#73986 = CARTESIAN_POINT ( 'NONE',  ( 134.0664832912740110, 0.2215528400590013880, 296.1531252759119752 ) ) ;
#73987 = CARTESIAN_POINT ( 'NONE',  ( 0.000000000000000000, 127.0000000000000000, -95.25000000000000000 ) ) ;
#73988 = CARTESIAN_POINT ( 'NONE',  ( 109.9831304889623027, -26.74336511273919115, 259.8499109901965767 ) ) ;
#73989 = DIRECTION ( 'NONE',  ( 0.000000000000000000, -1.000000000000000000, 0.000000000000000000 ) ) ;
#73990 = CARTESIAN_POINT ( 'NONE',  ( 72.31648329127396835, -9.833000550534366724, 14.92562527591093691 ) ) ;
#73991 = CARTESIAN_POINT ( 'NONE',  ( 78.80082187616059741, -39.17731672735968118, 1.873071027762776453 ) ) ;
#73992 = CARTESIAN_POINT ( 'NONE',  ( 106.3060546692423145, -45.75354925581387278, 261.9200388756959796 ) ) ;
#73994 = CARTESIAN_POINT ( 'NONE',  ( 116.1047473792919504, -29.10330858331350612, 70.38419670448192278 ) ) ;
#73993 = CARTESIAN_POINT ( 'NONE',  ( 63.03715912545740707, -46.82818131006017381, 117.4678068554150485 ) ) ;
#73995 = CARTESIAN_POINT ( 'NONE',  ( 119.4810000828223906, 74.54169681208188081, 52.62745965564226225 ) ) ;
#73996 = CARTESIAN_POINT ( 'NONE',  ( 117.6255004633147507, -33.30599276614662330, 134.0880062282919880 ) ) ;
#73997 = EDGE_LOOP ( 'NONE', ( #58123, #35588, #3040, #17975 ) ) ;
#73998 = DIRECTION ( 'NONE',  ( 0.000000000000000000, 1.000000000000000000, 0.000000000000000000 ) ) ;
#73999 = ORIENTED_EDGE ( 'NONE', *, *, #34297, .T. ) ;
#74000 = CARTESIAN_POINT ( 'NONE',  ( 57.56670390244747892, -48.82844715994040286, 137.2178068554150911 ) ) ;
#74001 = DIRECTION ( 'NONE',  ( 1.000000000000000078E-15, -1.000000000000000000, 0.000000000000000000 ) ) ;
#74002 = AXIS2_PLACEMENT_3D ( 'NONE', #9566, #78180, #57704 ) ;
#74003 = FACE_OUTER_BOUND ( 'NONE', #85531, .T. ) ;
#74005 = ORIENTED_EDGE ( 'NONE', *, *, #82547, .T. ) ;
#74004 = EDGE_CURVE ( 'NONE', #6945, #35850, #56733, .T. ) ;
#74006 = CARTESIAN_POINT ( 'NONE',  ( 97.80412552530029302, -40.49889735345233532, 51.63403232301700996 ) ) ;
#74008 = ORIENTED_EDGE ( 'NONE', *, *, #515, .T. ) ;
#74007 = CARTESIAN_POINT ( 'NONE',  ( 108.0109225731970213, -26.30163847990888826, 155.0041967044819557 ) ) ;
#74009 = DIRECTION ( 'NONE',  ( 0.7071067811864656383, 0.7071067811866295072, 7.071067811864650974E-16 ) ) ;
#74010 = VECTOR ( 'NONE', #24518, 1000.000000000000000 ) ;
#74011 = CARTESIAN_POINT ( 'NONE',  ( -130.3279567413622715, 92.64985122628465319, -7.743850073003764933 ) ) ;
#74012 = DIRECTION ( 'NONE',  ( 0.000000000000000000, 0.000000000000000000, -1.000000000000000000 ) ) ;
#74013 = CARTESIAN_POINT ( 'NONE',  ( 170.2205283966864897, 20.32000000000000028, -71.37400000000000944 ) ) ;
#74014 = ORIENTED_EDGE ( 'NONE', *, *, #31407, .T. ) ;
#74015 = CARTESIAN_POINT ( 'NONE',  ( 103.1663722902654001, -27.03741444506403724, 130.3813395616259925 ) ) ;
#74016 = PRODUCT_CONTEXT ( 'NONE', #44601, 'mechanical' ) ;
#74017 = DIRECTION ( 'NONE',  ( 1.000000000000000000, -0.000000000000000000, -0.000000000000000000 ) ) ;
#74018 = CARTESIAN_POINT ( 'NONE',  ( 154.5667039024469886, -67.87844715994090450, 85.21780685541799016 ) ) ;
#74019 = EDGE_LOOP ( 'NONE', ( #32390, #4605, #49609, #70762 ) ) ;
#74020 = VECTOR ( 'NONE', #26079, 1000.000000000000000 ) ;
#74021 = EDGE_CURVE ( 'NONE', #44052, #73924, #40917, .T. ) ;
#74022 = VERTEX_POINT ( 'NONE', #27295 ) ;
#74023 = CARTESIAN_POINT ( 'NONE',  ( 32.24491389930098251, -32.11662333284611748, -5.074374724088000832 ) ) ;
#74024 = CARTESIAN_POINT ( 'NONE',  ( 84.91247172076084837, 90.28418055714726620, -99.17062120112620960 ) ) ;
#74025 = EDGE_CURVE ( 'NONE', #53911, #37008, #54969, .T. ) ;
#74026 = CARTESIAN_POINT ( 'NONE',  ( 116.7951252645493128, -39.38782981807234052, 158.6147919403088906 ) ) ;
#74027 = CARTESIAN_POINT ( 'NONE',  ( 162.5667039024470171, -33.35206098992711077, -5.074374724088000832 ) ) ;
#74029 = LINE ( 'NONE', #12708, #79078 ) ;
#74028 = LINE ( 'NONE', #87219, #53714 ) ;
#74030 = DIRECTION ( 'NONE',  ( 0.000000000000000000, -0.8660254037844387076, 0.4999999999999998890 ) ) ;
#74031 = VECTOR ( 'NONE', #9059, 1000.000000000000000 ) ;
#74032 = EDGE_LOOP ( 'NONE', ( #21908, #31135, #78749, #78972 ) ) ;
#74033 = CARTESIAN_POINT ( 'NONE',  ( 59.67079009362632291, -0.9310397146383332379, 540.9756252759101471 ) ) ;
#74034 = CARTESIAN_POINT ( 'NONE',  ( 98.33750497493211640, -41.21483588869658377, 192.7041967044819728 ) ) ;
#74036 = VERTEX_POINT ( 'NONE', #82736 ) ;
#74035 = PLANE ( 'NONE',  #25447 ) ;
#74037 = CARTESIAN_POINT ( 'NONE',  ( 117.2535196871929770, -41.18324016912737306, 54.49848241876692612 ) ) ;
#74038 = CARTESIAN_POINT ( 'NONE',  ( 112.0515904353014065, -45.40454050051200596, 52.99152818533465137 ) ) ;
#74039 = FACE_OUTER_BOUND ( 'NONE', #62371, .T. ) ;
#74040 = CARTESIAN_POINT ( 'NONE',  ( 97.80782893958210877, -40.50798467304517914, 22.63481380566990708 ) ) ;
#74041 = AXIS2_PLACEMENT_3D ( 'NONE', #36041, #63755, #7888 ) ;
#74042 = ORIENTED_EDGE ( 'NONE', *, *, #34828, .F. ) ;
#74043 = CARTESIAN_POINT ( 'NONE',  ( 154.5667039024469886, -67.87844715994090450, 85.21780685541799016 ) ) ;
#74044 = ORIENTED_EDGE ( 'NONE', *, *, #18301, .F. ) ;
#74045 = ORIENTED_EDGE ( 'NONE', *, *, #55977, .T. ) ;
#74046 = CARTESIAN_POINT ( 'NONE',  ( 114.7070687854681807, -41.21829243659817621, 234.8358690201829404 ) ) ;
#74047 = VECTOR ( 'NONE', #6861, 1000.000000000000000 ) ;
#74048 = CARTESIAN_POINT ( 'NONE',  ( 164.7830935719599381, -29.99615139350823867, 342.9256252759109884 ) ) ;
#74049 = DIRECTION ( 'NONE',  ( 1.000000000000000000, 0.000000000000000000, 0.000000000000000000 ) ) ;
#74050 = CARTESIAN_POINT ( 'NONE',  ( -105.4788588808462038, 120.6499999999999915, -3.968750000001139977 ) ) ;
#74051 = AXIS2_PLACEMENT_3D ( 'NONE', #33089, #67610, #54844 ) ;
#74052 = DIRECTION ( 'NONE',  ( 0.000000000000000000, 0.000000000000000000, -1.000000000000000000 ) ) ;
#74053 = EDGE_LOOP ( 'NONE', ( #88994, #26652, #37154, #22964 ) ) ;
#74054 = DIRECTION ( 'NONE',  ( 0.000000000000000000, 1.000000000000000000, 0.000000000000000000 ) ) ;
#74055 = CARTESIAN_POINT ( 'NONE',  ( -487.2989999999999782, 7.143750000000280487, 15.23694598552305024 ) ) ;
#74056 = ORIENTED_EDGE ( 'NONE', *, *, #51290, .T. ) ;
#74057 = CARTESIAN_POINT ( 'NONE',  ( 97.10456541990245682, -39.80308206185652864, 21.56419670448195092 ) ) ;
#74058 = ORIENTED_EDGE ( 'NONE', *, *, #5522, .F. ) ;
#74059 = EDGE_LOOP ( 'NONE', ( #17627, #27568 ) ) ;
#74060 = CARTESIAN_POINT ( 'NONE',  ( 114.2324904129858112, -40.69568343359240714, 261.2423760838772182 ) ) ;
#74061 = CARTESIAN_POINT ( 'NONE',  ( 28.57499999999999929, 77.96728223830740490, 310.8325000000000387 ) ) ;
#74062 = CARTESIAN_POINT ( 'NONE',  ( 48.45959712129000252, -28.98061976758940617, 237.4678068554150059 ) ) ;
#74063 = AXIS2_PLACEMENT_3D ( 'NONE', #75576, #46492, #68307 ) ;
#74064 = DIRECTION ( 'NONE',  ( 1.000000000000000078E-15, -1.000000000000000083E-30, -1.000000000000000000 ) ) ;
#74065 = FACE_OUTER_BOUND ( 'NONE', #29642, .T. ) ;
#74066 = CARTESIAN_POINT ( 'NONE',  ( 96.81585423491817721, -34.60398634006848795, 212.1641967044819808 ) ) ;
#74067 = CARTESIAN_POINT ( 'NONE',  ( 92.07164801315056479, 85.85031469618033384, -74.68844285250138171 ) ) ;
#74068 = VERTEX_POINT ( 'NONE', #55427 ) ;
#74069 = CARTESIAN_POINT ( 'NONE',  ( 106.6586400085135438, -26.26872808310278629, 81.10705384733896040 ) ) ;
#74070 = EDGE_CURVE ( 'NONE', #18008, #28336, #20501, .T. ) ;
#74071 = FACE_OUTER_BOUND ( 'NONE', #24644, .T. ) ;
#74072 = ORIENTED_EDGE ( 'NONE', *, *, #5625, .T. ) ;
#74074 = ADVANCED_FACE ( 'NONE', ( #34553, #20935, #76344 ), #69536, .F. ) ;
#74073 = EDGE_LOOP ( 'NONE', ( #76519, #63930, #41785, #54727 ) ) ;
#74075 = ORIENTED_EDGE ( 'NONE', *, *, #27222, .F. ) ;
#74076 = AXIS2_PLACEMENT_3D ( 'NONE', #84937, #78574, #23163 ) ;
#74077 = ADVANCED_FACE ( 'NONE', ( #21388 ), #12329, .T. ) ;
#74078 = VECTOR ( 'NONE', #69672, 1000.000000000000000 ) ;
#74079 = LINE ( 'NONE', #48141, #20195 ) ;
#74080 = CARTESIAN_POINT ( 'NONE',  ( 72.96458098368701428, 117.4749999999999943, -72.96458098368670164 ) ) ;
#74081 = CARTESIAN_POINT ( 'NONE',  ( 115.7813752605596420, -41.80523413302275770, 153.4069233405687100 ) ) ;
#74082 = CARTESIAN_POINT ( 'NONE',  ( 112.8963470814680932, -31.01156847455079912, 147.2623760838769726 ) ) ;
#74083 = CARTESIAN_POINT ( 'NONE',  ( 118.0636334930051987, -35.40736804548507877, 234.9337205140059552 ) ) ;
#74084 = EDGE_CURVE ( 'NONE', #34812, #72137, #19583, .T. ) ;
#74085 = CARTESIAN_POINT ( 'NONE',  ( 44.45000000000000284, 66.67499999999999716, 257.1750000000000114 ) ) ;
#74086 = VERTEX_POINT ( 'NONE', #35903 ) ;
#74087 =( NAMED_UNIT ( * ) SI_UNIT ( $, .STERADIAN. ) SOLID_ANGLE_UNIT ( ) );
#74088 = EDGE_CURVE ( 'NONE', #12758, #2876, #2295, .T. ) ;
#74089 = CARTESIAN_POINT ( 'NONE',  ( 141.3509999999999991, 101.5999999999999943, 141.3509999999999991 ) ) ;
#74090 = ORIENTED_EDGE ( 'NONE', *, *, #72390, .F. ) ;
#74091 = VERTEX_POINT ( 'NONE', #43152 ) ;
#74092 = EDGE_CURVE ( 'NONE', #36659, #60843, #8210, .T. ) ;
#74093 = EDGE_CURVE ( 'NONE', #80239, #34761, #69985, .T. ) ;
#74094 = AXIS2_PLACEMENT_3D ( 'NONE', #16894, #64152, #10079 ) ;
#74095 = DIRECTION ( 'NONE',  ( -1.000000000000000078E-15, 0.000000000000000000, 1.000000000000000000 ) ) ;
#74096 = ORIENTED_EDGE ( 'NONE', *, *, #76222, .F. ) ;
#74097 = ORIENTED_EDGE ( 'NONE', *, *, #22939, .F. ) ;
#74098 = DIRECTION ( 'NONE',  ( 1.000000000000000000, 0.000000000000000000, 0.000000000000000000 ) ) ;
#74099 = CARTESIAN_POINT ( 'NONE',  ( 67.65734841870819594, 69.84999999999999432, 346.9005000000000223 ) ) ;
#74100 = ADVANCED_FACE ( 'NONE', ( #43600 ), #1847, .T. ) ;
#74101 = CARTESIAN_POINT ( 'NONE',  ( 162.0667039024469886, -67.87844715994089029, 55.21780685541800437 ) ) ;
#74102 = CARTESIAN_POINT ( 'NONE',  ( 115.3083805796901373, -34.38525866856544866, 148.4695626852189605 ) ) ;
#74103 = CARTESIAN_POINT ( 'NONE',  ( 98.38709084977145380, -42.09077886617859576, 11.76800622829193799 ) ) ;
#74104 = CARTESIAN_POINT ( 'NONE',  ( 74.76629182358846037, -133.7001020459428844, 248.3919653347779786 ) ) ;
#74105 = ORIENTED_EDGE ( 'NONE', *, *, #14312, .T. ) ;
#74106 = EDGE_CURVE ( 'NONE', #29846, #19430, #15022, .T. ) ;
#74107 = CARTESIAN_POINT ( 'NONE',  ( -185.9961463128564958, 20.32000000000000028, -3.174999999999514877 ) ) ;
#74109 = ORIENTED_EDGE ( 'NONE', *, *, #54678, .F. ) ;
#74108 = EDGE_CURVE ( 'NONE', #12759, #84665, #36807, .T. ) ;
#74110 = CIRCLE ( 'NONE', #42191, 2.500000000000002220 ) ;
#74111 = DIRECTION ( 'NONE',  ( 0.000000000000000000, 0.000000000000000000, -1.000000000000000000 ) ) ;
#74112 = ORIENTED_EDGE ( 'NONE', *, *, #27466, .F. ) ;
#74113 = CARTESIAN_POINT ( 'NONE',  ( 119.2637946045970097, -42.39761235918182791, 6.826283056785802827 ) ) ;
#74114 = PLANE ( 'NONE',  #86523 ) ;
#74115 = CARTESIAN_POINT ( 'NONE',  ( 33.98325472291465132, 8.255000000000000782, -3.174999999999999822 ) ) ;
#74116 = B_SPLINE_CURVE_WITH_KNOTS ( 'NONE', 3,
 ( #13377, #82435, #66987, #12483, #4769, #60608, #6554, #26109, #53779, #20196, #40164, #67884, #28326, #49664 ),
 .UNSPECIFIED., .F., .F.,
 ( 4, 2, 2, 2, 2, 2, 4 ),
 ( 0.008390848235266742949, 0.01104543637615772525, 0.01237273044660322160, 0.01370002451704871449, 0.01635461265793970720, 0.01768190672838519661, 0.01900920079883068256 ),
 .UNSPECIFIED. ) ;
#74117 = CIRCLE ( 'NONE', #52355, 7.143750000000004263 ) ;
#74118 = CYLINDRICAL_SURFACE ( 'NONE', #66952, 16.09746158385918946 ) ;
#74119 = EDGE_LOOP ( 'NONE', ( #62795, #54635 ) ) ;
#74120 = CARTESIAN_POINT ( 'NONE',  ( 106.2504075017224210, -26.27849585604564098, 25.13848241876792855 ) ) ;
#74121 = CARTESIAN_POINT ( 'NONE',  ( 98.55462967347544634, -43.85305904914448405, 67.86895860924497015 ) ) ;
#74122 = FILL_AREA_STYLE_COLOUR ( '', #52120 ) ;
#74124 = CARTESIAN_POINT ( 'NONE',  ( 184.5664832912740110, 15.62155284005900491, 323.8756252759109202 ) ) ;
#74123 = CARTESIAN_POINT ( 'NONE',  ( 29.00000000000001421, 172.0000000000000000, 113.8826257785461280 ) ) ;
#74125 = CARTESIAN_POINT ( 'NONE',  ( 115.0889146834008585, -30.61764965368201175, 145.3442830127359571 ) ) ;
#74126 = CARTESIAN_POINT ( 'NONE',  ( 105.8444747722200674, -25.33565403619829226, 322.4846826458744431 ) ) ;
#74127 = CARTESIAN_POINT ( 'NONE',  ( 34.33598329127499227, -36.32844715994100682, -5.074374724088000832 ) ) ;
#74128 = VECTOR ( 'NONE', #14344, 1000.000000000000000 ) ;
#74129 = EDGE_CURVE ( 'NONE', #51804, #79942, #26332, .T. ) ;
#74130 = DIRECTION ( 'NONE',  ( -1.000000000000000000, -6.055337108828351666E-16, 0.000000000000000000 ) ) ;
#74131 = EDGE_CURVE ( 'NONE', #3441, #53911, #15483, .T. ) ;
#74132 = CIRCLE ( 'NONE', #82840, 5.562600000000000655 ) ;
#74133 = EDGE_CURVE ( 'NONE', #76782, #28502, #69847, .T. ) ;
#74134 = FACE_BOUND ( 'NONE', #17535, .T. ) ;
#74135 = ORIENTED_EDGE ( 'NONE', *, *, #64575, .F. ) ;
#74136 = CARTESIAN_POINT ( 'NONE',  ( 112.7657546104280044, -27.20415503536211688, 54.65943479971996055 ) ) ;
#74137 = CARTESIAN_POINT ( 'NONE',  ( 110.0520154068402263, -26.08705182471624795, 215.8708633711489711 ) ) ;
#74138 = CARTESIAN_POINT ( 'NONE',  ( 101.6996507173639088, -27.72520905039313632, 81.50419670448295051 ) ) ;
#74139 = ADVANCED_FACE ( 'NONE', ( #63161 ), #49516, .F. ) ;
#74141 = DIRECTION ( 'NONE',  ( 1.000000000000000000, 0.000000000000000000, 0.000000000000000000 ) ) ;
#74140 = CYLINDRICAL_SURFACE ( 'NONE', #39218, 9.525000000000000355 ) ;
#74142 = LINE ( 'NONE', #11916, #82859 ) ;
#74143 = DIRECTION ( 'NONE',  ( 0.5000000000000061062, 0.8660254037844351549, 0.000000000000000000 ) ) ;
#74144 = ORIENTED_EDGE ( 'NONE', *, *, #19955, .F. ) ;
#74145 = CARTESIAN_POINT ( 'NONE',  ( 102.8368274790083490, -27.91052165842139487, 91.43276813305296002 ) ) ;
#74147 = ORIENTED_EDGE ( 'NONE', *, *, #5807, .T. ) ;
#74146 = CARTESIAN_POINT ( 'NONE',  ( 9.685063450406051544, 90.77563096578916202, 130.1966975709476628 ) ) ;
#74148 = VECTOR ( 'NONE', #63192, 1000.000000000000000 ) ;
#74149 = CARTESIAN_POINT ( 'NONE',  ( 98.95962429139169103, -30.20966935044063462, 236.7870538473399336 ) ) ;
#74150 = CARTESIAN_POINT ( 'NONE',  ( 48.45959712127301344, -26.00627455219131789, -5.074374724088000832 ) ) ;
#74151 = LINE ( 'NONE', #18279, #31856 ) ;
#74152 = PLANE ( 'NONE',  #37056 ) ;
#74153 = CARTESIAN_POINT ( 'NONE',  ( 104.4899544671745844, -26.97880758085721808, 81.28145860801052436 ) ) ;
#74154 = CARTESIAN_POINT ( 'NONE',  ( 0.000000000000000000, 20.32000000000000028, 0.000000000000000000 ) ) ;
#74155 = FACE_BOUND ( 'NONE', #23306, .T. ) ;
#74156 = B_SPLINE_CURVE_WITH_KNOTS ( 'NONE', 3,
 ( #89559, #40940, #47748, #76372, #48635, #49090, #27319, #14147, #48190, #68664, #76820, #83199, #62735, #20524, #41383, #54994, #61826, #13692, #41824, #55448, #54547, #89111, #82310, #75024, #6431 ),
 .UNSPECIFIED., .F., .F.,
 ( 4, 2, 2, 2, 2, 2, 2, 2, 2, 1, 2, 2, 4 ),
 ( 0.05960646776571127542, 0.06208810814592213845, 0.06332892833602757343, 0.06456974852613300841, 0.06705138890634392002, 0.06829220909644936888, 0.06953302928655483162, 0.07201466966676572934, 0.07325548985687117820, 0.07449631004697662706, 0.07573713023708206205, 0.07697795042718751091, 0.07945959080739838087 ),
 .UNSPECIFIED. ) ;
#74157 = CARTESIAN_POINT ( 'NONE',  ( 116.2045471004838078, -43.06251688283441581, 163.3441967044829823 ) ) ;
#74158 = VERTEX_POINT ( 'NONE', #77252 ) ;
#74159 = EDGE_LOOP ( 'NONE', ( #74588, #47721, #51746, #27300 ) ) ;
#74160 = CARTESIAN_POINT ( 'NONE',  ( 113.5773531717103282, -42.74084067657960162, 119.6644404487539646 ) ) ;
#74161 = AXIS2_PLACEMENT_3D ( 'NONE', #3160, #71317, #9085 ) ;
#74162 = CARTESIAN_POINT ( 'NONE',  ( 41.56648329127398966, -18.82844715994071194, 78.92562527591199739 ) ) ;
#74164 = CARTESIAN_POINT ( 'NONE',  ( 194.5664832912739826, 12.92155284005902516, 333.4006252759108975 ) ) ;
#74163 = CARTESIAN_POINT ( 'NONE',  ( 114.5610390845466071, -30.44493693613353358, 265.3813395616247135 ) ) ;
#74165 = CARTESIAN_POINT ( 'NONE',  ( 130.5667039024480118, -36.72944715994093912, 218.8274735512161158 ) ) ;
#74166 = FACE_OUTER_BOUND ( 'NONE', #84280, .T. ) ;
#74167 = CARTESIAN_POINT ( 'NONE',  ( 116.3212776292297406, -32.94146857471347545, 140.1356252759109680 ) ) ;
#74168 = DIRECTION ( 'NONE',  ( -1.314511288311335947E-16, 1.000000000000000000, 0.000000000000000000 ) ) ;
#74169 = CARTESIAN_POINT ( 'NONE',  ( 29.56648329127298069, -81.37844715994266664, 361.9756252759109998 ) ) ;
#74170 = CARTESIAN_POINT ( 'NONE',  ( 110.7536356736639078, -102.7271463785358492, -19.78219314458207378 ) ) ;
#74171 = B_SPLINE_SURFACE_WITH_KNOTS ( 'NONE', 3, 3, ( 
 ( #87364, #24243, #45108, #3356 ),
 ( #31046, #73265, #24683, #65126 ),
 ( #2909, #57862, #72401, #37874 ),
 ( #86038, #9720, #39198, #17864 ),
 ( #3794, #65574, #38306, #30161 ),
 ( #31481, #80552, #85596, #25124 ),
 ( #2466, #52350, #73724, #51913 ) ),
 .UNSPECIFIED., .F., .F., .F.,
 ( 4, 1, 1, 1, 4 ),
 ( 4, 4 ),
 ( -0.0007720614341078669424, 0.2857142857142860315, 0.5714285714285709528, 0.8571428571428569843, 1.000772061434110016 ),
 ( 0.09408714780213320306, 1.000772061434110016 ),
 .UNSPECIFIED. ) ;
#74172 = CARTESIAN_POINT ( 'NONE',  ( 117.9257662994440494, -34.79559216868040039, 198.9546728949589749 ) ) ;
#74173 = DIRECTION ( 'NONE',  ( 0.000000000000000000, 0.000000000000000000, 1.000000000000000000 ) ) ;
#74174 = EDGE_LOOP ( 'NONE', ( #82138, #29257 ) ) ;
#74175 = ORIENTED_EDGE ( 'NONE', *, *, #74964, .T. ) ;
#74176 = VECTOR ( 'NONE', #55691, 1000.000000000000000 ) ;
#74177 = CARTESIAN_POINT ( 'NONE',  ( -100.4327019155584964, 78.46683822716998691, -83.41556370846515733 ) ) ;
#74178 = CARTESIAN_POINT ( 'NONE',  ( 77.66889017811094220, -17.37024878619161683, 2.654395752941510978 ) ) ;
#74179 = LINE ( 'NONE', #53247, #38875 ) ;
#74180 = LINE ( 'NONE', #86924, #56343 ) ;
#74181 = AXIS2_PLACEMENT_3D ( 'NONE', #19385, #68880, #46621 ) ;
#74182 = CARTESIAN_POINT ( 'NONE',  ( 108.4139369173698242, -26.73458070908401041, 94.96924584189345353 ) ) ;
#74183 = VERTEX_POINT ( 'NONE', #29100 ) ;
#74184 = CARTESIAN_POINT ( 'NONE',  ( -11.32175285073831894, 88.14108913799663014, 117.8136741508921261 ) ) ;
#74185 = EDGE_CURVE ( 'NONE', #18386, #87456, #22745, .T. ) ;
#74186 = CARTESIAN_POINT ( 'NONE',  ( 107.2431713256043224, -47.18863871633809026, 212.5899109901969837 ) ) ;
#74187 = EDGE_CURVE ( 'NONE', #15780, #73586, #24381, .T. ) ;
#74188 = CARTESIAN_POINT ( 'NONE',  ( 98.06670458790040357, -71.37844715994094713, 55.21780685541800437 ) ) ;
#74189 = VERTEX_POINT ( 'NONE', #73098 ) ;
#74190 = VERTEX_POINT ( 'NONE', #79943 ) ;
#74191 = AXIS2_PLACEMENT_3D ( 'NONE', #489, #28180, #55870 ) ;
#74192 = ADVANCED_FACE ( 'NONE', ( #4063 ), #79046, .F. ) ;
#74193 = CARTESIAN_POINT ( 'NONE',  ( -12.59999999999999964, 82.54999999999999716, 117.8845415480757595 ) ) ;
#74194 = DIRECTION ( 'NONE',  ( 1.000000000000000000, 0.000000000000000000, 0.000000000000000000 ) ) ;
#74195 = DIRECTION ( 'NONE',  ( -1.000000000000000000, 0.000000000000000000, -1.000000000000000078E-15 ) ) ;
#74196 = AXIS2_PLACEMENT_3D ( 'NONE', #88874, #40703, #61149 ) ;
#74197 = CARTESIAN_POINT ( 'NONE',  ( 99.45988105884268293, -33.69262468827373169, 38.84237608387697094 ) ) ;
#74198 = CARTESIAN_POINT ( 'NONE',  ( 111.8040564975826356, -25.84011059577494152, 130.7499109901969518 ) ) ;
#74199 = EDGE_CURVE ( 'NONE', #19039, #25006, #17259, .T. ) ;
#74200 = LINE ( 'NONE', #32849, #76797 ) ;
#74201 = ORIENTED_EDGE ( 'NONE', *, *, #70688, .T. ) ;
#74202 = EDGE_CURVE ( 'NONE', #67042, #15378, #17699, .T. ) ;
#74203 = FACE_OUTER_BOUND ( 'NONE', #43650, .T. ) ;
#74204 = CARTESIAN_POINT ( 'NONE',  ( 80.06648329127401098, -33.97944715994105991, 1.625625275910943746 ) ) ;
#74205 = ORIENTED_EDGE ( 'NONE', *, *, #36461, .F. ) ;
#74206 = ORIENTED_EDGE ( 'NONE', *, *, #80515, .F. ) ;
#74207 = EDGE_CURVE ( 'NONE', #8128, #27831, #10876, .T. ) ;
#74208 = DIRECTION ( 'NONE',  ( -4.237773401492740281E-14, 1.000000000000000000, 0.000000000000000000 ) ) ;
#74209 = VERTEX_POINT ( 'NONE', #31762 ) ;
#74210 = ORIENTED_EDGE ( 'NONE', *, *, #22350, .T. ) ;
#74211 = PLANE ( 'NONE',  #58651 ) ;
#74212 = EDGE_CURVE ( 'NONE', #38962, #48829, #59458, .T. ) ;
#74213 = CARTESIAN_POINT ( 'NONE',  ( 114.9961339231967798, -33.55505389859023069, 53.55241982807695678 ) ) ;
#74214 = CARTESIAN_POINT ( 'NONE',  ( 117.7991783922927738, -31.64581934375353711, 214.1784824187679419 ) ) ;
#74215 = CIRCLE ( 'NONE', #43726, 6.571100913904396990 ) ;
#74216 = CARTESIAN_POINT ( 'NONE',  ( 113.5515132932711566, -44.90922781482916548, 168.1099109901969939 ) ) ;
#74218 = CARTESIAN_POINT ( 'NONE',  ( 115.4270991047690558, -42.97960947038945534, 24.31562527591096767 ) ) ;
#74217 = CARTESIAN_POINT ( 'NONE',  ( 104.8309510432842444, -46.56975234077351189, 22.39971745899171651 ) ) ;
#74219 = PLANE ( 'NONE',  #62277 ) ;
#74220 = DIRECTION ( 'NONE',  ( -3.100000000000000258E-29, 3.100000000000000044E-14, 1.000000000000000000 ) ) ;
#74221 = ORIENTED_EDGE ( 'NONE', *, *, #80774, .T. ) ;
#74222 = VERTEX_POINT ( 'NONE', #72669 ) ;
#74223 = AXIS2_PLACEMENT_3D ( 'NONE', #57701, #23648, #36376 ) ;
#74224 = EDGE_CURVE ( 'NONE', #20434, #30630, #66922, .T. ) ;
#74225 = AXIS2_PLACEMENT_3D ( 'NONE', #68404, #27951, #77456 ) ;
#74226 = CARTESIAN_POINT ( 'NONE',  ( 69.94616667561825807, -138.0587426493221699, 247.6570821721479945 ) ) ;
#74227 = CARTESIAN_POINT ( 'NONE',  ( 107.5119097530387933, -47.18928756557821202, 237.6099109901969655 ) ) ;
#74228 = EDGE_LOOP ( 'NONE', ( #68182, #75407, #68507, #37052, #6149, #62924 ) ) ;
#74229 = CARTESIAN_POINT ( 'NONE',  ( 98.53748378420890219, -30.73418253943381728, 205.8384824187679669 ) ) ;
#74230 = DIRECTION ( 'NONE',  ( 1.000000000000000000, 3.999999999999999995E-14, 1.000000000000000078E-15 ) ) ;
#74231 = DIRECTION ( 'NONE',  ( -0.7071067811865171526, -0.7071067811865779928, 2.899137802864853973E-29 ) ) ;
#74232 = DIRECTION ( 'NONE',  ( 0.000000000000000000, 1.000000000000000000, 0.000000000000000000 ) ) ;
#74234 = CARTESIAN_POINT ( 'NONE',  ( 144.4532657278588204, -72.54451140298851897, 540.9756252759101471 ) ) ;
#74233 = CARTESIAN_POINT ( 'NONE',  ( 111.9228550121644190, -44.05463541751552725, 277.6356252759109680 ) ) ;
#74235 = PLANE ( 'NONE',  #39433 ) ;
#74236 = DIRECTION ( 'NONE',  ( -1.000000000000000000, 7.570719237730541270E-15, 0.000000000000000000 ) ) ;
#74237 = DIRECTION ( 'NONE',  ( 6.982966722218758611E-15, 0.000000000000000000, -1.000000000000000000 ) ) ;
#74238 = LINE ( 'NONE', #164, #84965 ) ;
#74239 = CARTESIAN_POINT ( 'NONE',  ( 180.2121375201597573, -29.73316016638934300, 237.4678068554150059 ) ) ;
#74240 = DIRECTION ( 'NONE',  ( -2.999999999999999839E-15, 1.000000000000000000, -2.999999999999999900E-30 ) ) ;
#74241 = AXIS2_PLACEMENT_3D ( 'NONE', #37412, #30153, #65116 ) ;
#74242 = ADVANCED_FACE ( 'NONE', ( #53063 ), #18133, .T. ) ;
#74244 = ORIENTED_EDGE ( 'NONE', *, *, #70371, .T. ) ;
#74243 = CARTESIAN_POINT ( 'NONE',  ( -9.549789689180773422, 90.93251752167839186, -118.1710524764278887 ) ) ;
#74245 = DIRECTION ( 'NONE',  ( 1.000000000000000078E-15, 0.000000000000000000, 1.000000000000000000 ) ) ;
#74246 = CARTESIAN_POINT ( 'NONE',  ( 97.89977465614410335, -41.74121498826879417, 221.7241967044819546 ) ) ;
#74247 = CARTESIAN_POINT ( 'NONE',  ( 109.2549746569086437, -46.95841770046993702, 103.7441967044829880 ) ) ;
#74248 = CARTESIAN_POINT ( 'NONE',  ( 117.4559332992660075, -35.18111149946130922, 214.9441967044829767 ) ) ;
#74249 = CARTESIAN_POINT ( 'NONE',  ( 152.0368932755772562, -23.42844715993587812, 193.9678068554149775 ) ) ;
#74250 = EDGE_CURVE ( 'NONE', #77633, #54044, #30739, .T. ) ;
#74251 = CARTESIAN_POINT ( 'NONE',  ( 226.4410000000000025, 52.73749999999999716, -44.45000000000000284 ) ) ;
#74253 = LINE ( 'NONE', #12027, #73352 ) ;
#74252 = PLANE ( 'NONE',  #82691 ) ;
#74254 = CARTESIAN_POINT ( 'NONE',  ( 46.83715912545344651, -47.82818131006087015, 117.4678068554150485 ) ) ;
#74255 = AXIS2_PLACEMENT_3D ( 'NONE', #402, #7226, #69450 ) ;
#74256 = FACE_OUTER_BOUND ( 'NONE', #41527, .T. ) ;
#74257 = VECTOR ( 'NONE', #86708, 1000.000000000000000 ) ;
#74258 = ORIENTED_EDGE ( 'NONE', *, *, #17102, .F. ) ;
#74259 = ORIENTED_EDGE ( 'NONE', *, *, #87339, .F. ) ;
#74260 = CARTESIAN_POINT ( 'NONE',  ( 112.6791402994794709, -29.62235551608389628, 123.9790864947439815 ) ) ;
#74262 = ORIENTED_EDGE ( 'NONE', *, *, #87532, .F. ) ;
#74261 = CARTESIAN_POINT ( 'NONE',  ( 180.3521107875639871, -35.65087443492551245, 117.4678068554150627 ) ) ;
#74263 = CARTESIAN_POINT ( 'NONE',  ( 97.06107483254703538, -37.99643385399256346, 91.42643104473111748 ) ) ;
#74264 = CARTESIAN_POINT ( 'NONE',  ( 103.1828028919049984, -27.07824557232550688, 126.3813395616259783 ) ) ;
#74265 = CARTESIAN_POINT ( 'NONE',  ( 25.56670390244797275, -62.87844715994099687, 290.4678068554150627 ) ) ;
#74266 = AXIS2_PLACEMENT_3D ( 'NONE', #51862, #30110, #31431 ) ;
#74267 = DIRECTION ( 'NONE',  ( 1.000000000000000000, 0.000000000000000000, 0.000000000000000000 ) ) ;
#74268 = ADVANCED_FACE ( 'NONE', ( #18582 ), #46262, .F. ) ;
#74269 = CARTESIAN_POINT ( 'NONE',  ( 177.1649999999999920, 25.81350000000000477, -7.937500000000000000 ) ) ;
#74270 = AXIS2_PLACEMENT_3D ( 'NONE', #77545, #36208, #43899 ) ;
#74271 = CARTESIAN_POINT ( 'NONE',  ( 100.8874678906910418, -44.70022137984270927, 108.0522919431911788 ) ) ;
#74272 = CARTESIAN_POINT ( 'NONE',  ( 103.6990349130722251, -26.13358598113143216, 55.32133956162594046 ) ) ;
#74273 = ORIENTED_EDGE ( 'NONE', *, *, #50225, .F. ) ;
#74274 = VERTEX_POINT ( 'NONE', #32655 ) ;
#74275 = VERTEX_POINT ( 'NONE', #60351 ) ;
#74276 = EDGE_CURVE ( 'NONE', #18505, #40389, #56804, .T. ) ;
#74277 = CARTESIAN_POINT ( 'NONE',  ( 177.8371591254543489, -47.82818131005477369, 249.9678068554149775 ) ) ;
#74279 = DIRECTION ( 'NONE',  ( 0.7071067811865473507, 0.000000000000000000, -0.7071067811865476838 ) ) ;
#74278 = CARTESIAN_POINT ( 'NONE',  ( 116.2045471004837083, -43.06251688283437318, 159.3441967044819592 ) ) ;
#74280 = CARTESIAN_POINT ( 'NONE',  ( 163.1543517358360020, -31.62489322948790971, -5.074374724088000832 ) ) ;
#74281 = CARTESIAN_POINT ( 'NONE',  ( -76.76779673090611311, 55.97500000000000142, 30.90025125786759830 ) ) ;
#74282 = DIRECTION ( 'NONE',  ( 0.000000000000000000, 1.000000000000000000, 0.000000000000000000 ) ) ;
#74283 = CARTESIAN_POINT ( 'NONE',  ( 118.5256205435843526, -36.72944715994100306, 311.6356252759112522 ) ) ;
#74284 = CARTESIAN_POINT ( 'NONE',  ( 99.04403034142228535, -42.84121029749736920, 177.8439541681125036 ) ) ;
#74285 = CARTESIAN_POINT ( 'NONE',  ( 117.9791962420231073, -38.33460093242097599, 73.72229194257801055 ) ) ;
#74286 = VERTEX_POINT ( 'NONE', #44493 ) ;
#74287 = ORIENTED_EDGE ( 'NONE', *, *, #21524, .T. ) ;
#74288 = CYLINDRICAL_SURFACE ( 'NONE', #47327, 130.5560000000000116 ) ;
#74289 = CARTESIAN_POINT ( 'NONE',  ( -84.21071524772774808, 88.91113633199476851, -99.76704648670025222 ) ) ;
#74290 = VECTOR ( 'NONE', #43501, 1000.000000000000000 ) ;
#74291 = DIRECTION ( 'NONE',  ( 0.000000000000000000, 0.000000000000000000, 1.000000000000000000 ) ) ;
#74292 = CARTESIAN_POINT ( 'NONE',  ( 98.91056109567942656, -37.06209505544900651, 159.1766617981629679 ) ) ;
#74293 = EDGE_CURVE ( 'NONE', #89909, #61092, #9996, .T. ) ;
#74294 = ADVANCED_FACE ( 'NONE', ( #58567 ), #86297, .T. ) ;
#74295 = EDGE_CURVE ( 'NONE', #67028, #14919, #69427, .T. ) ;
#74296 = CARTESIAN_POINT ( 'NONE',  ( 1.154229608196380665E-15, 1.270000000000000018, 9.425000000000000711 ) ) ;
#74297 = ORIENTED_EDGE ( 'NONE', *, *, #59139, .F. ) ;
#74298 = ORIENTED_EDGE ( 'NONE', *, *, #55400, .T. ) ;
#74299 = CARTESIAN_POINT ( 'NONE',  ( 0.000000000000000000, 12.27000000000000313, 0.000000000000000000 ) ) ;
#74300 = EDGE_CURVE ( 'NONE', #61315, #72685, #48060, .T. ) ;
#74301 = VERTEX_POINT ( 'NONE', #88539 ) ;
#74302 = PRODUCT_DEFINITION_SHAPE ( 'NONE', 'NONE',  #57145 ) ;
#74303 = VERTEX_POINT ( 'NONE', #61693 ) ;
#74304 = DIRECTION ( 'NONE',  ( -0.04216478779797398074, 0.9991106698809455455, 0.000000000000000000 ) ) ;
#74305 = AXIS2_PLACEMENT_3D ( 'NONE', #44782, #52024, #3014 ) ;
#74306 = CARTESIAN_POINT ( 'NONE',  ( 109.9841060568515729, -28.36190534590500434, 206.2415833058969667 ) ) ;
#74307 = EDGE_CURVE ( 'NONE', #41305, #25889, #20827, .T. ) ;
#74308 = CARTESIAN_POINT ( 'NONE',  ( 51.56670390244676128, -33.35206098992666313, 193.9678068554150911 ) ) ;
#74309 = CARTESIAN_POINT ( 'NONE',  ( 116.3216177720312317, -32.94249360885015676, 184.1356252759109680 ) ) ;
#74310 = CYLINDRICAL_SURFACE ( 'NONE', #66253, 3.299999999999999822 ) ;
#74311 = ORIENTED_EDGE ( 'NONE', *, *, #69162, .T. ) ;
#74312 = EDGE_LOOP ( 'NONE', ( #8630, #5713, #88620, #79301 ) ) ;
#74313 = EDGE_CURVE ( 'NONE', #42339, #4876, #38002, .T. ) ;
#74314 = AXIS2_PLACEMENT_3D ( 'NONE', #54290, #73869, #52931 ) ;
#74315 = VERTEX_POINT ( 'NONE', #41692 ) ;
#74316 = ORIENTED_EDGE ( 'NONE', *, *, #80354, .T. ) ;
#74317 = EDGE_CURVE ( 'NONE', #66479, #5006, #14008, .T. ) ;
#74318 = AXIS2_PLACEMENT_3D ( 'NONE', #77934, #1636, #15258 ) ;
#74319 = CARTESIAN_POINT ( 'NONE',  ( 114.4736784013144586, -40.22460793573437599, 226.2938046553059621 ) ) ;
#74320 = CARTESIAN_POINT ( 'NONE',  ( 107.6042850712483698, -26.26048674992130572, 95.03562527591097364 ) ) ;
#74321 = CARTESIAN_POINT ( 'NONE',  ( 96.94236579736387682, -32.35154040576531997, 61.01372051400599616 ) ) ;
#74322 = CARTESIAN_POINT ( 'NONE',  ( 109.4816866186930326, -44.79096458540936254, 249.5838068554168672 ) ) ;
#74323 = FACE_OUTER_BOUND ( 'NONE', #83985, .T. ) ;
#74324 = CYLINDRICAL_SURFACE ( 'NONE', #57643, 0.2500000000000002220 ) ;
#74325 = CARTESIAN_POINT ( 'NONE',  ( 117.9325828832643026, -34.70414220975756336, 199.9851490854349549 ) ) ;
#74326 = FACE_OUTER_BOUND ( 'NONE', #58447, .T. ) ;
#74327 = ORIENTED_EDGE ( 'NONE', *, *, #27845, .T. ) ;
#74328 = LINE ( 'NONE', #33430, #85941 ) ;
#74329 = VERTEX_POINT ( 'NONE', #68532 ) ;
#74330 = VERTEX_POINT ( 'NONE', #47614 ) ;
#74331 = DIRECTION ( 'NONE',  ( -6.524622321627019585E-16, -4.013151879589939944E-16, -1.000000000000000000 ) ) ;
#74332 = EDGE_LOOP ( 'NONE', ( #77790, #61771 ) ) ;
#74333 = CARTESIAN_POINT ( 'NONE',  ( 87.17003668186750076, -46.62589376934784013, -5.074374724089000033 ) ) ;
#74334 = CARTESIAN_POINT ( 'NONE',  ( 116.7951252695739868, -39.38782979763659853, 178.6147919420326673 ) ) ;
#74335 = CARTESIAN_POINT ( 'NONE',  ( 117.3389957193927131, -32.64844533837379004, 99.13943479972098771 ) ) ;
#74336 = DIRECTION ( 'NONE',  ( 0.000000000000000000, 0.000000000000000000, 1.000000000000000000 ) ) ;
#74337 = CARTESIAN_POINT ( 'NONE',  ( -24.79284581386642827, 127.0000000000000000, 0.000000000000000000 ) ) ;
#74338 = PLANE ( 'NONE',  #35413 ) ;
#74341 = CARTESIAN_POINT ( 'NONE',  ( 98.18688568738953393, -31.30898482519909365, 166.8899109901969950 ) ) ;
#74340 = FACE_OUTER_BOUND ( 'NONE', #78677, .T. ) ;
#74339 = DIRECTION ( 'NONE',  ( -4.299999999999999979E-14, 1.000000000000000000, -4.400000000000000367E-29 ) ) ;
#74342 = PLANE ( 'NONE',  #74196 ) ;
#74343 = FACE_OUTER_BOUND ( 'NONE', #53884, .T. ) ;
#74344 = VERTEX_POINT ( 'NONE', #27636 ) ;
#74345 = FACE_OUTER_BOUND ( 'NONE', #67786, .T. ) ;
#74346 = AXIS2_PLACEMENT_3D ( 'NONE', #52983, #46640, #88907 ) ;
#74347 = DIRECTION ( 'NONE',  ( 1.000000000000000000, 0.000000000000000000, 2.671820169801660301E-13 ) ) ;
#74348 = CARTESIAN_POINT ( 'NONE',  ( 97.07198307494437017, -35.37891590512482054, 136.2191293735547788 ) ) ;
#74349 = LINE ( 'NONE', #19382, #23076 ) ;
#74351 = VERTEX_POINT ( 'NONE', #74450 ) ;
#74350 = CARTESIAN_POINT ( 'NONE',  ( 96.97388998173752839, -33.94624283173551049, 251.1127681330538337 ) ) ;
#74352 = CARTESIAN_POINT ( 'NONE',  ( 114.7884511584987024, -30.33054135350295866, 194.3769663851998928 ) ) ;
#74353 = CARTESIAN_POINT ( 'NONE',  ( 111.0012107362514939, -46.40699640104500645, 278.8841967044824059 ) ) ;
#74354 = CARTESIAN_POINT ( 'NONE',  ( 95.98172161192206886, -37.30002307145830542, 117.3794347997199594 ) ) ;
#74355 = DIRECTION ( 'NONE',  ( 0.000000000000000000, -1.000000000000000000, 5.463695987328529395E-16 ) ) ;
#74356 = EDGE_CURVE ( 'NONE', #49237, #1627, #6057, .T. ) ;
#74357 = CARTESIAN_POINT ( 'NONE',  ( 3.298961202091078793, 94.84210650921833974, -130.5168528568578097 ) ) ;
#74359 = FACE_OUTER_BOUND ( 'NONE', #70172, .T. ) ;
#74358 = CARTESIAN_POINT ( 'NONE',  ( 4.665904304751416087E-15, 95.00619999999999266, -38.10000000000000142 ) ) ;
#74360 = CARTESIAN_POINT ( 'NONE',  ( 108.4174892948216211, -26.73503593412567625, 189.9689586058460122 ) ) ;
#74361 = LINE ( 'NONE', #75261, #21909 ) ;
#74362 = ORIENTED_EDGE ( 'NONE', *, *, #28451, .F. ) ;
#74363 = AXIS2_PLACEMENT_3D ( 'NONE', #15552, #43227, #32947 ) ;
#74364 = EDGE_LOOP ( 'NONE', ( #77218, #31964, #59153, #7951 ) ) ;
#74365 = ORIENTED_EDGE ( 'NONE', *, *, #18307, .F. ) ;
#74366 = EDGE_LOOP ( 'NONE', ( #78452, #78306, #53226, #81593, #20770, #1491 ) ) ;
#74367 = FACE_BOUND ( 'NONE', #80075, .T. ) ;
#74368 = CARTESIAN_POINT ( 'NONE',  ( 96.36668125800727580, -39.40815171121896299, 12.53372051400597442 ) ) ;
#74369 = FACE_OUTER_BOUND ( 'NONE', #39069, .T. ) ;
#74370 = CARTESIAN_POINT ( 'NONE',  ( 133.6895842087618291, -33.97944715994099596, 1.625625275910995704 ) ) ;
#74371 = VECTOR ( 'NONE', #26475, 1000.000000000000114 ) ;
#74372 = CARTESIAN_POINT ( 'NONE',  ( 144.9304472658408258, -138.7995020472562828, 247.3025957270601225 ) ) ;
#74374 = CARTESIAN_POINT ( 'NONE',  ( -3.968749999999935163, 127.0000000000000000, -100.8961411191535973 ) ) ;
#74373 = CARTESIAN_POINT ( 'NONE',  ( 131.0667039024480118, -58.72944715994093201, 207.5838068554149913 ) ) ;
#74375 = CARTESIAN_POINT ( 'NONE',  ( 99.32305605351064060, -40.33436967443800825, 256.0952769709339236 ) ) ;
#74376 = ORIENTED_EDGE ( 'NONE', *, *, #9279, .F. ) ;
#74377 = ORIENTED_EDGE ( 'NONE', *, *, #84383, .T. ) ;
#74378 = ORIENTED_EDGE ( 'NONE', *, *, #46897, .T. ) ;
#74380 = ADVANCED_FACE ( 'NONE', ( #13561 ), #19032, .F. ) ;
#74379 = VECTOR ( 'NONE', #72870, 1000.000000000000000 ) ;
#74381 = FACE_OUTER_BOUND ( 'NONE', #28570, .T. ) ;
#74382 = CARTESIAN_POINT ( 'NONE',  ( 20.03715912545644073, -24.42818131006202265, 129.9678068554150627 ) ) ;
#74383 = CARTESIAN_POINT ( 'NONE',  ( 25.56670390244719115, -42.82844715994178131, 173.2178068554150627 ) ) ;
#74384 = CARTESIAN_POINT ( 'NONE',  ( 116.3114837287122754, -32.94280867712679850, 274.1356252759109680 ) ) ;
#74385 = CARTESIAN_POINT ( 'NONE',  ( 97.95230308628410398, -39.01119097033267025, 12.96539282970593554 ) ) ;
#74386 = VECTOR ( 'NONE', #47844, 1000.000000000000000 ) ;
#74387 = CARTESIAN_POINT ( 'NONE',  ( 117.9898589647454799, 87.79588542099538984, 11.57341593931223223 ) ) ;
#74388 = CARTESIAN_POINT ( 'NONE',  ( 99.09505096938842428, -30.55130953284144724, 175.8023783150660790 ) ) ;
#74389 = CARTESIAN_POINT ( 'NONE',  ( 105.9660763718858618, -46.48152545022894344, 282.4870538473400643 ) ) ;
#74390 = CARTESIAN_POINT ( 'NONE',  ( 51.06648329127400388, 12.92155284005902516, 333.4006252759110112 ) ) ;
#74391 = ORIENTED_EDGE ( 'NONE', *, *, #29560, .F. ) ;
#74392 = CARTESIAN_POINT ( 'NONE',  ( 21.56670390244696733, -23.42844715994183957, 300.4678068554150059 ) ) ;
#74393 = DIRECTION ( 'NONE',  ( 0.9068632946707807507, -0.4214249218767881500, 1.031805784967618114E-15 ) ) ;
#74394 = CARTESIAN_POINT ( 'NONE',  ( 115.6184857618795121, -38.05767108254817543, 66.50999513149596964 ) ) ;
#74395 = CARTESIAN_POINT ( 'NONE',  ( 136.5456844410148278, -17.53793914064988257, 7.103892432643784005 ) ) ;
#74396 = DIRECTION ( 'NONE',  ( 0.000000000000000000, 0.000000000000000000, -1.000000000000000000 ) ) ;
#74397 = EDGE_CURVE ( 'NONE', #89511, #28842, #23504, .T. ) ;
#74398 = CARTESIAN_POINT ( 'NONE',  ( 112.0658116054833897, -45.48845209930474454, 193.9897506056947236 ) ) ;
#74399 = ORIENTED_EDGE ( 'NONE', *, *, #17869, .F. ) ;
#74400 = CARTESIAN_POINT ( 'NONE',  ( 161.4809174648185603, -48.32844715993547169, 180.4678068554150059 ) ) ;
#74401 = DIRECTION ( 'NONE',  ( -0.7071067811865274777, 0.7071067811865675568, -7.071067811865283048E-16 ) ) ;
#74402 = VECTOR ( 'NONE', #5221, 1000.000000000000000 ) ;
#74403 = EDGE_CURVE ( 'NONE', #74329, #74526, #25852, .T. ) ;
#74404 = ORIENTED_EDGE ( 'NONE', *, *, #33890, .F. ) ;
#74405 = CARTESIAN_POINT ( 'NONE',  ( 96.69902036285651548, -37.82614351231516281, 126.4099109901969626 ) ) ;
#74406 = ORIENTED_EDGE ( 'NONE', *, *, #76995, .F. ) ;
#74407 = EDGE_CURVE ( 'NONE', #26268, #9288, #19934, .T. ) ;
#74408 = CARTESIAN_POINT ( 'NONE',  ( 116.0152812585483275, -38.11929796734737863, 68.11432458998100969 ) ) ;
#74409 = DIRECTION ( 'NONE',  ( -0.7071067811865526798, 0.7071067811865423547, 2.102802400022928177E-16 ) ) ;
#74410 = CARTESIAN_POINT ( 'NONE',  ( 111.9416332874190090, -45.54441269975540507, 99.41015473446796591 ) ) ;
#74411 = EDGE_CURVE ( 'NONE', #4573, #79978, #7543, .T. ) ;
#74412 = CARTESIAN_POINT ( 'NONE',  ( -64.09238476222100189, 53.97500000000000142, 58.69734786913941349 ) ) ;
#74413 = LINE ( 'NONE', #83038, #65775 ) ;
#74414 = CARTESIAN_POINT ( 'NONE',  ( 97.60264960697516301, -32.22222542080420027, 71.97276813305397525 ) ) ;
#74415 = CARTESIAN_POINT ( 'NONE',  ( 70.63919639214310564, 91.07499999999996021, 53.63573739454427880 ) ) ;
#74416 = AXIS2_PLACEMENT_3D ( 'NONE', #3585, #31281, #58539 ) ;
#74417 = CARTESIAN_POINT ( 'NONE',  ( 108.3332793974000765, -46.73487859761686991, 257.6771670143646702 ) ) ;
#74418 = ORIENTED_EDGE ( 'NONE', *, *, #77656, .F. ) ;
#74419 = DIRECTION ( 'NONE',  ( 1.000000000000000078E-15, -1.000000000000000083E-30, -1.000000000000000000 ) ) ;
#74420 = ORIENTED_EDGE ( 'NONE', *, *, #2165, .T. ) ;
#74421 = ORIENTED_EDGE ( 'NONE', *, *, #25265, .T. ) ;
#74422 = EDGE_CURVE ( 'NONE', #64746, #65669, #5414, .T. ) ;
#74423 = LINE ( 'NONE', #60778, #597 ) ;
#74424 = ORIENTED_EDGE ( 'NONE', *, *, #18201, .F. ) ;
#74425 = CARTESIAN_POINT ( 'NONE',  ( 101.2327472597881552, -44.62129728587218835, 257.0699109901973998 ) ) ;
#74426 = CARTESIAN_POINT ( 'NONE',  ( 113.8576076518026383, -28.74447221003411812, 135.5156252759109634 ) ) ;
#74427 = DIRECTION ( 'NONE',  ( 0.000000000000000000, -1.000000000000000000, 0.000000000000000000 ) ) ;
#74428 = CARTESIAN_POINT ( 'NONE',  ( 107.0664832912739968, 19.62155284005901024, 333.4006252759110112 ) ) ;
#74429 = CARTESIAN_POINT ( 'NONE',  ( 104.7595845749942782, -46.89609389129499561, 68.39848241876794077 ) ) ;
#74430 = CARTESIAN_POINT ( 'NONE',  ( 115.8279189686416828, -31.73432177683753608, 95.23967231875141692 ) ) ;
#74431 = ORIENTED_EDGE ( 'NONE', *, *, #13406, .T. ) ;
#74432 = CARTESIAN_POINT ( 'NONE',  ( 72.96458098368701428, 127.0000000000000000, -65.82083098368670449 ) ) ;
#74433 = CARTESIAN_POINT ( 'NONE',  ( 105.7157274140183603, -46.72389631486497308, 158.4687971658879349 ) ) ;
#74434 = EDGE_LOOP ( 'NONE', ( #13578, #54834, #21498 ) ) ;
#74435 = AXIS2_PLACEMENT_3D ( 'NONE', #25855, #81290, #4961 ) ;
#74436 = DIRECTION ( 'NONE',  ( 0.000000000000000000, 1.000000000000000000, 0.000000000000000000 ) ) ;
#74437 = LINE ( 'NONE', #54854, #33913 ) ;
#74438 = CARTESIAN_POINT ( 'NONE',  ( 105.1635383257858507, -47.00901688944614421, 12.42991099019596923 ) ) ;
#74439 = CARTESIAN_POINT ( 'NONE',  ( 194.0371591254573218, -24.42818131005417825, 249.9678068554149775 ) ) ;
#74440 = CIRCLE ( 'NONE', #33845, 0.5000000000000197620 ) ;
#74441 = DIRECTION ( 'NONE',  ( 1.000000000000000078E-15, -1.000000000000000000, 0.000000000000000000 ) ) ;
#74442 = CARTESIAN_POINT ( 'NONE',  ( 79.32178306375476495, -39.37853523628606212, 1.709393643967942245 ) ) ;
#74443 = CARTESIAN_POINT ( 'NONE',  ( 99.27767200979357654, -42.52643314540505060, 261.2581341137909590 ) ) ;
#74446 = CARTESIAN_POINT ( 'NONE',  ( 116.2124334422529870, -31.77159869865918296, 65.22133956162595325 ) ) ;
#74445 = CARTESIAN_POINT ( 'NONE',  ( 110.6885610099060244, -27.38152249298925867, 99.78298386793977670 ) ) ;
#74444 = TOROIDAL_SURFACE ( 'NONE', #9160, 11.75000000000000000, 2.125000000000000000 ) ;
#74447 = LINE ( 'NONE', #25849, #8862 ) ;
#74448 = CARTESIAN_POINT ( 'NONE',  ( 111.4357194830650002, -47.79916136671457849, 172.8756252759109771 ) ) ;
#74449 = EDGE_LOOP ( 'NONE', ( #65124, #69079 ) ) ;
#74450 = CARTESIAN_POINT ( 'NONE',  ( 241.3336515812914911, 65.43750000000000000, -2.032000000000000028 ) ) ;
#74451 = EDGE_LOOP ( 'NONE', ( #35287, #46676, #48451, #68128, #73723 ) ) ;
#74452 = CARTESIAN_POINT ( 'NONE',  ( 41.56648329127499153, -32.07844715994070839, 83.67562527591201160 ) ) ;
#74453 = CARTESIAN_POINT ( 'NONE',  ( 1.387778780781445676E-14, 238.5000000000000000, 97.27542076772557778 ) ) ;
#74454 = CARTESIAN_POINT ( 'NONE',  ( 131.0667039024480118, -61.87844715994100397, 231.5838068554150198 ) ) ;
#74455 = ORIENTED_EDGE ( 'NONE', *, *, #42203, .T. ) ;
#74456 = DIRECTION ( 'NONE',  ( 0.000000000000000000, 0.000000000000000000, -1.000000000000000000 ) ) ;
#74458 = ORIENTED_EDGE ( 'NONE', *, *, #6065, .F. ) ;
#74457 = CARTESIAN_POINT ( 'NONE',  ( 95.73117830242222226, -40.35431382354642693, 131.5727681330539554 ) ) ;
#74460 = DIRECTION ( 'NONE',  ( -4.554376769437570034E-14, 1.000000000000000000, 0.000000000000000000 ) ) ;
#74459 = UNCERTAINTY_MEASURE_WITH_UNIT (LENGTH_MEASURE( 1.000000000000000082E-05 ), #1574, 'distance_accuracy_value', 'NONE');
#74461 = CARTESIAN_POINT ( 'NONE',  ( -129.9528072873947337, 84.62817240485475168, -12.53569626682267568 ) ) ;
#74462 = EDGE_CURVE ( 'NONE', #47225, #64699, #53970, .T. ) ;
#74463 = DIRECTION ( 'NONE',  ( 0.000000000000000000, 0.000000000000000000, 1.000000000000000000 ) ) ;
#74464 = DIRECTION ( 'NONE',  ( -3.999999999999999995E-14, 1.000000000000000000, -4.100000000000000342E-29 ) ) ;
#74465 = ORIENTED_EDGE ( 'NONE', *, *, #41697, .F. ) ;
#74466 =( LENGTH_UNIT ( ) NAMED_UNIT ( * ) SI_UNIT ( .MILLI., .METRE. ) );
#74467 = VECTOR ( 'NONE', #70460, 1000.000000000000000 ) ;
#74468 = ADVANCED_FACE ( 'NONE', ( #60806 ), #54416, .T. ) ;
#74469 = DIRECTION ( 'NONE',  ( -2.900000000000000265E-14, 2.000000000000000155E-15, -1.000000000000000000 ) ) ;
#74470 = CARTESIAN_POINT ( 'NONE',  ( -27.27158787008326968, 127.0000000000000000, 90.32146847885337593 ) ) ;
#74471 = ORIENTED_EDGE ( 'NONE', *, *, #74921, .F. ) ;
#74472 = AXIS2_PLACEMENT_3D ( 'NONE', #70934, #29139, #37743 ) ;
#74473 = ORIENTED_EDGE ( 'NONE', *, *, #78649, .F. ) ;
#74474 = CARTESIAN_POINT ( 'NONE',  ( 257.5940999999999690, 52.73749999999999716, -2.903194600000015502 ) ) ;
#74475 = CARTESIAN_POINT ( 'NONE',  ( 87.44839512528858450, 93.33885111288435610, -96.94208673522955166 ) ) ;
#74476 = CARTESIAN_POINT ( 'NONE',  ( 97.81170669197712186, -40.51744871389600178, 156.6352702525290681 ) ) ;
#74477 = LINE ( 'NONE', #31344, #28443 ) ;
#74479 = CARTESIAN_POINT ( 'NONE',  ( -11.89159109876203146, 78.07192968827520474, -117.9582163940502966 ) ) ;
#74478 = DIRECTION ( 'NONE',  ( -0.7071067811866279529, 0.7071067811864671926, -7.071067811866286874E-16 ) ) ;
#74480 = LINE ( 'NONE', #33140, #12415 ) ;
#74481 = AXIS2_PLACEMENT_3D ( 'NONE', #83322, #76952, #56489 ) ;
#74482 = ORIENTED_EDGE ( 'NONE', *, *, #12159, .T. ) ;
#74483 = ADVANCED_FACE ( 'NONE', ( #27189 ), #12676, .F. ) ;
#74484 = DIRECTION ( 'NONE',  ( 0.7071067811865453523, 0.000000000000000000, 0.7071067811865496822 ) ) ;
#74485 = CARTESIAN_POINT ( 'NONE',  ( 116.5710038106514759, -34.42130396933982439, 205.0156252759109634 ) ) ;
#74487 = ORIENTED_EDGE ( 'NONE', *, *, #62322, .F. ) ;
#74486 = DIRECTION ( 'NONE',  ( -1.000000000000000078E-15, 1.000000000000000083E-30, 1.000000000000000000 ) ) ;
#74488 = CARTESIAN_POINT ( 'NONE',  ( 115.1932381579439948, -43.17108053757041830, 44.30514908543392494 ) ) ;
#74489 = CARTESIAN_POINT ( 'NONE',  ( 111.2436683438683644, -45.81674569873502634, 52.91934373813153769 ) ) ;
#74490 = CARTESIAN_POINT ( 'NONE',  ( 107.0667039024470313, -104.2784471599420755, -19.78219314458201694 ) ) ;
#74491 = DIRECTION ( 'NONE',  ( 0.000000000000000000, 0.000000000000000000, 1.000000000000000000 ) ) ;
#74492 = VERTEX_POINT ( 'NONE', #89885 ) ;
#74493 = CARTESIAN_POINT ( 'NONE',  ( 116.3148031259206192, -32.94054721833379062, 24.13562527591095375 ) ) ;
#74494 = VERTEX_POINT ( 'NONE', #20390 ) ;
#74495 = ORIENTED_EDGE ( 'NONE', *, *, #87316, .T. ) ;
#74496 = CARTESIAN_POINT ( 'NONE',  ( 100.8499323319230854, -30.41416626502819298, 222.1272975916109544 ) ) ;
#74497 = VECTOR ( 'NONE', #79283, 1000.000000000000000 ) ;
#74498 = DIRECTION ( 'NONE',  ( -0.7071067811734105257, 0.7071067811996846197, 0.000000000000000000 ) ) ;
#74499 = CARTESIAN_POINT ( 'NONE',  ( -83.22850972642717693, 85.83513192049080942, 100.5877680347024068 ) ) ;
#74500 = AXIS2_PLACEMENT_3D ( 'NONE', #934, #50863, #29535 ) ;
#74501 = CARTESIAN_POINT ( 'NONE',  ( 107.0667039024470171, -89.08784823670062281, -21.78219314458248945 ) ) ;
#74502 = CARTESIAN_POINT ( 'NONE',  ( 82.74959284958354999, -37.33856210725883784, 3.004220725470468256 ) ) ;
#74503 = ORIENTED_EDGE ( 'NONE', *, *, #24082, .T. ) ;
#74504 = CARTESIAN_POINT ( 'NONE',  ( 0.000000000000000000, 100.5999999999999659, 0.000000000000000000 ) ) ;
#74505 = CARTESIAN_POINT ( 'NONE',  ( 4.665904304751416087E-15, 65.60000000000000853, -38.10000000000000142 ) ) ;
#74506 = ORIENTED_EDGE ( 'NONE', *, *, #4765, .F. ) ;
#74507 = CARTESIAN_POINT ( 'NONE',  ( 115.4447846419100472, -42.99283068281499709, 28.31562527591097123 ) ) ;
#74508 = ORIENTED_EDGE ( 'NONE', *, *, #58271, .T. ) ;
#74510 = ORIENTED_EDGE ( 'NONE', *, *, #4655, .T. ) ;
#74509 = EDGE_CURVE ( 'NONE', #67629, #23399, #6119, .T. ) ;
#74511 = CARTESIAN_POINT ( 'NONE',  ( 114.7858077920586908, -40.64262416812939449, 246.2833284648299639 ) ) ;
#74512 = FACE_OUTER_BOUND ( 'NONE', #69760, .T. ) ;
#74513 = CARTESIAN_POINT ( 'NONE',  ( 108.2029444874846007, -47.03713394308636708, 157.6518157521019532 ) ) ;
#74514 = DIRECTION ( 'NONE',  ( 0.000000000000000000, 0.000000000000000000, -1.000000000000000000 ) ) ;
#74515 = CARTESIAN_POINT ( 'NONE',  ( 151.0371591254585724, -46.82818131005582529, 180.4678068554149775 ) ) ;
#74516 = LINE ( 'NONE', #12296, #46282 ) ;
#74517 = CARTESIAN_POINT ( 'NONE',  ( 115.8125398181975783, -30.97623284308500757, 250.2899109901966028 ) ) ;
#74518 = CARTESIAN_POINT ( 'NONE',  ( 4.788368984666157546E-15, 92.07499999999998863, -39.10000000000005116 ) ) ;
#74519 = ORIENTED_EDGE ( 'NONE', *, *, #12279, .T. ) ;
#74520 = CIRCLE ( 'NONE', #87562, 11.57110091390434192 ) ;
#74521 = CARTESIAN_POINT ( 'NONE',  ( 104.0301208637212369, -47.40549519127628031, 63.36800622829197494 ) ) ;
#74522 = DIRECTION ( 'NONE',  ( 0.000000000000000000, 0.000000000000000000, 1.000000000000000000 ) ) ;
#74523 = VECTOR ( 'NONE', #76612, 1000.000000000000000 ) ;
#74524 = ORIENTED_EDGE ( 'NONE', *, *, #65899, .T. ) ;
#74525 = EDGE_LOOP ( 'NONE', ( #71278, #68644, #22277, #88463 ) ) ;
#74526 = VERTEX_POINT ( 'NONE', #2181 ) ;
#74527 = EDGE_CURVE ( 'NONE', #11232, #27146, #43034, .T. ) ;
#74528 = CIRCLE ( 'NONE', #78897, 0.5000000000000197620 ) ;
#74529 = DIRECTION ( 'NONE',  ( 1.000000000000000078E-15, -1.000000000000000000, 0.000000000000000000 ) ) ;
#74531 = EDGE_CURVE ( 'NONE', #20097, #36440, #14918, .T. ) ;
#74530 = CYLINDRICAL_SURFACE ( 'NONE', #21033, 2.517499999999998739 ) ;
#74532 = CARTESIAN_POINT ( 'NONE',  ( -479.3614999999999782, 104.7749999999999915, -1.387778780781445991E-14 ) ) ;
#74533 = CARTESIAN_POINT ( 'NONE',  ( 108.9785397593094132, -44.66504833944034658, 130.5823760838769658 ) ) ;
#74534 = CARTESIAN_POINT ( 'NONE',  ( 98.92566635982139189, -30.18235936901480443, 236.7870538473399336 ) ) ;
#74535 = CARTESIAN_POINT ( 'NONE',  ( 188.5667039024484097, -48.82844715993431350, 254.7178068554150059 ) ) ;
#74536 = ORIENTED_EDGE ( 'NONE', *, *, #5053, .F. ) ;
#74537 = CARTESIAN_POINT ( 'NONE',  ( 130.5559693845970344, 95.24968527363472504, -0.8339068267389735389 ) ) ;
#74538 = CARTESIAN_POINT ( 'NONE',  ( 41.56648329127399677, -9.303447159940999356, 318.9256252759120116 ) ) ;
#74539 = ORIENTED_EDGE ( 'NONE', *, *, #89462, .T. ) ;
#74540 = ORIENTED_EDGE ( 'NONE', *, *, #86610, .F. ) ;
#74541 = PLANE ( 'NONE',  #37321 ) ;
#74542 = ORIENTED_EDGE ( 'NONE', *, *, #7445, .F. ) ;
#74543 = ORIENTED_EDGE ( 'NONE', *, *, #64708, .T. ) ;
#74544 = DIRECTION ( 'NONE',  ( 1.000000000000000000, 0.000000000000000000, 0.000000000000000000 ) ) ;
#74545 = DIRECTION ( 'NONE',  ( -1.000000000000000078E-15, 1.000000000000000083E-30, 1.000000000000000000 ) ) ;
#74546 = DIRECTION ( 'NONE',  ( 0.000000000000000000, 0.000000000000000000, 1.000000000000000000 ) ) ;
#74547 = CARTESIAN_POINT ( 'NONE',  ( 110.6311418553464279, -45.76071711580824086, 172.2981341137909794 ) ) ;
#74548 = CARTESIAN_POINT ( 'NONE',  ( 103.9442172157761917, -47.38141121271982570, 62.33753003781600199 ) ) ;
#74549 = CARTESIAN_POINT ( 'NONE',  ( 78.94219608136785382, -124.1415542323586720, 249.3055308415380011 ) ) ;
#74550 = VERTEX_POINT ( 'NONE', #21273 ) ;
#74551 = CARTESIAN_POINT ( 'NONE',  ( 107.0620278373210539, -36.73691869758540207, 394.9756252759100903 ) ) ;
#74552 = ORIENTED_EDGE ( 'NONE', *, *, #88719, .T. ) ;
#74553 = DIRECTION ( 'NONE',  ( 0.000000000000000000, -1.000000000000000000, 0.000000000000000000 ) ) ;
#74554 = ORIENTED_EDGE ( 'NONE', *, *, #13852, .F. ) ;
#74555 = DIRECTION ( 'NONE',  ( 0.000000000000000000, 0.000000000000000000, 1.000000000000000000 ) ) ;
#74556 = CARTESIAN_POINT ( 'NONE',  ( 86.61913848402866734, -135.9065445298735710, 248.4142799812389910 ) ) ;
#74557 = CARTESIAN_POINT ( 'NONE',  ( 104.4073079673720343, -46.45785698206038461, 132.3648020700444761 ) ) ;
#74558 = VECTOR ( 'NONE', #22411, 1000.000000000000000 ) ;
#74559 = DIRECTION ( 'NONE',  ( 0.000000000000000000, 0.000000000000000000, -1.000000000000000000 ) ) ;
#74560 = EDGE_LOOP ( 'NONE', ( #24253, #33455, #4670, #64694 ) ) ;
#74561 = CARTESIAN_POINT ( 'NONE',  ( 111.3322245453084918, -27.19268589797737334, 24.74133956162494030 ) ) ;
#74562 = CARTESIAN_POINT ( 'NONE',  ( 112.7653987728015323, -27.20474975302890996, 50.65943479972101215 ) ) ;
#74563 =( NAMED_UNIT ( * ) SI_UNIT ( $, .STERADIAN. ) SOLID_ANGLE_UNIT ( ) );
#74564 = CIRCLE ( 'NONE', #26699, 3.968749999999992895 ) ;
#74567 = EDGE_CURVE ( 'NONE', #64576, #15070, #29890, .T. ) ;
#74566 = CARTESIAN_POINT ( 'NONE',  ( 194.0371591254585155, -46.82818131005407736, 117.4678068554150627 ) ) ;
#74565 = DIRECTION ( 'NONE',  ( 0.000000000000000000, 1.000000000000000000, 0.000000000000000000 ) ) ;
#74568 = CARTESIAN_POINT ( 'NONE',  ( 99.09571505209436282, -30.55042394618130785, 146.8027630058878401 ) ) ;
#74569 = CARTESIAN_POINT ( 'NONE',  ( 149.4409906032288404, -0.9156555935619370423, 361.9756252759100335 ) ) ;
#74570 = CARTESIAN_POINT ( 'NONE',  ( 51.56670390244899238, -32.29483332968450782, -5.074374724088000832 ) ) ;
#74571 = FACE_OUTER_BOUND ( 'NONE', #73736, .T. ) ;
#74572 = ORIENTED_EDGE ( 'NONE', *, *, #70755, .F. ) ;
#74573 = CARTESIAN_POINT ( 'NONE',  ( 99.03195499373370581, -44.38837911315224716, 36.92038718067297509 ) ) ;
#74574 = CARTESIAN_POINT ( 'NONE',  ( 106.3019393658184129, -47.12646404140136269, 218.5184824187679453 ) ) ;
#74575 = CARTESIAN_POINT ( 'NONE',  ( 116.1426067713721437, -29.07136428874337142, 70.38419670448192278 ) ) ;
#74577 = CARTESIAN_POINT ( 'NONE',  ( 85.24325998657074877, -58.55267046464445002, -5.074374724089052435 ) ) ;
#74576 = CARTESIAN_POINT ( 'NONE',  ( 127.5252020268926003, 0.000000000000000000, 177.0380000000000109 ) ) ;
#74578 = DIRECTION ( 'NONE',  ( 0.000000000000000000, 0.000000000000000000, -1.000000000000000000 ) ) ;
#74579 = VECTOR ( 'NONE', #43437, 999.9999999999998863 ) ;
#74580 = EDGE_CURVE ( 'NONE', #3629, #60265, #42584, .T. ) ;
#74581 = VECTOR ( 'NONE', #72027, 1000.000000000000000 ) ;
#74582 = CIRCLE ( 'NONE', #87622, 0.5000000000000004441 ) ;
#74583 = CARTESIAN_POINT ( 'NONE',  ( 165.3359832912740046, -36.32844715994100682, -5.074374724088000832 ) ) ;
#74584 = ORIENTED_EDGE ( 'NONE', *, *, #75637, .T. ) ;
#74585 = CARTESIAN_POINT ( 'NONE',  ( 98.75024281215311817, -42.92452016420547523, 107.8480062282919647 ) ) ;
#74586 = ADVANCED_FACE ( 'NONE', ( #36246 ), #8974, .T. ) ;
#74588 = ORIENTED_EDGE ( 'NONE', *, *, #59617, .T. ) ;
#74587 = CARTESIAN_POINT ( 'NONE',  ( 10.55034476490975770, 89.61967029530742934, 130.1290104682496462 ) ) ;
#74589 = CARTESIAN_POINT ( 'NONE',  ( 103.9458437887066111, -26.80522050874827755, 246.3184824187679567 ) ) ;
#74590 = CARTESIAN_POINT ( 'NONE',  ( 108.3324760767353609, -46.73498777622212685, 253.6793502017058586 ) ) ;
#74591 = CARTESIAN_POINT ( 'NONE',  ( 107.0664832912739968, -36.72944715994100306, 293.2242906452868851 ) ) ;
#74592 = DIRECTION ( 'NONE',  ( 0.000000000000000000, -1.000000000000000000, 0.000000000000000000 ) ) ;
#74593 = CARTESIAN_POINT ( 'NONE',  ( 34.92499999999999716, 77.96728223830730542, 294.9574999999999818 ) ) ;
#74594 = ADVANCED_FACE ( 'NONE', ( #83962, #64403 ), #37146, .F. ) ;
#74595 = EDGE_CURVE ( 'NONE', #47865, #27915, #57573, .T. ) ;
#74596 = DIRECTION ( 'NONE',  ( -3.555032108465730541E-16, 1.000000000000000000, 0.000000000000000000 ) ) ;
#74597 = DIRECTION ( 'NONE',  ( 0.000000000000000000, 1.000000000000000000, 0.000000000000000000 ) ) ;
#74598 = CARTESIAN_POINT ( 'NONE',  ( 114.0663967180213803, -29.08153105160599949, 154.4746728949589851 ) ) ;
#74599 = ORIENTED_EDGE ( 'NONE', *, *, #86162, .T. ) ;
#74600 = ORIENTED_EDGE ( 'NONE', *, *, #71650, .T. ) ;
#74601 = EDGE_CURVE ( 'NONE', #52429, #89126, #84459, .T. ) ;
#74602 = CARTESIAN_POINT ( 'NONE',  ( 108.1315353547809224, -45.52682987947058280, 114.1044404487549571 ) ) ;
#74603 = DIRECTION ( 'NONE',  ( 1.000000000000000078E-15, -1.000000000000000083E-30, -1.000000000000000000 ) ) ;
#74605 = CYLINDRICAL_SURFACE ( 'NONE', #36083, 2.116999999999980009 ) ;
#74604 = CARTESIAN_POINT ( 'NONE',  ( 112.1541913332956284, -45.76570811864959154, 253.9965776568629110 ) ) ;
#74606 = FACE_OUTER_BOUND ( 'NONE', #37165, .T. ) ;
#74607 = ADVANCED_FACE ( 'NONE', ( #9002 ), #8548, .F. ) ;
#74608 = DIRECTION ( 'NONE',  ( -9.073094938289460781E-13, -1.000000000000000000, 0.000000000000000000 ) ) ;
#74609 = CARTESIAN_POINT ( 'NONE',  ( 107.0664832912739968, -36.72944715994100306, 287.6356252759109680 ) ) ;
#74610 = CARTESIAN_POINT ( 'NONE',  ( 134.0664832912740110, -36.72944715994100306, -5.074374724089001809 ) ) ;
#74611 = LINE ( 'NONE', #33730, #80683 ) ;
#74612 = CARTESIAN_POINT ( 'NONE',  ( 112.7681627534586681, -45.43114336468926950, 178.0384824187679556 ) ) ;
#74613 = DIRECTION ( 'NONE',  ( 0.000000000000000000, 1.000000000000000000, 0.000000000000000000 ) ) ;
#74614 = EDGE_LOOP ( 'NONE', ( #42827, #86712, #62681, #54544 ) ) ;
#74616 = VERTEX_POINT ( 'NONE', #15369 ) ;
#74615 = EDGE_CURVE ( 'NONE', #47600, #34651, #62643, .T. ) ;
#74617 = CARTESIAN_POINT ( 'NONE',  ( -94.62072105690063495, 70.27892663483460467, -89.95524642164077989 ) ) ;
#74618 = CARTESIAN_POINT ( 'NONE',  ( 78.88305248757605170, -16.24700279812641668, 1.845048209621644952 ) ) ;
#74619 = CARTESIAN_POINT ( 'NONE',  ( 107.0664832912739541, -23.08981143457874197, 302.6356252759109680 ) ) ;
#74620 = DIRECTION ( 'NONE',  ( 0.000000000000000000, 0.000000000000000000, 1.000000000000000000 ) ) ;
#74621 = VECTOR ( 'NONE', #57707, 1000.000000000000000 ) ;
#74622 = LINE ( 'NONE', #12400, #42661 ) ;
#74623 = ORIENTED_EDGE ( 'NONE', *, *, #55826, .T. ) ;
#74624 = CARTESIAN_POINT ( 'NONE',  ( 112.0640814316657412, -45.48941673008675224, 62.98962639481060677 ) ) ;
#74625 =( BOUNDED_CURVE ( )  B_SPLINE_CURVE ( 2, ( #13194, #82697, #63120 ),
 .UNSPECIFIED., .F., .T. ) 
 B_SPLINE_CURVE_WITH_KNOTS ( ( 3, 3 ),
 ( 0.000000000000000000, 0.5053286420056740669 ),
 .UNSPECIFIED. ) 
 CURVE ( )  GEOMETRIC_REPRESENTATION_ITEM ( )  RATIONAL_B_SPLINE_CURVE ( ( 1.000000000000000000, 1.009299002520649857, 1.000420656333769864 ) ) 
 REPRESENTATION_ITEM ( '' )  );
#74626 = AXIS2_PLACEMENT_3D ( 'NONE', #72675, #52186, #10440 ) ;
#74627 = CARTESIAN_POINT ( 'NONE',  ( 110.1375194624030769, -26.11116931986236267, 214.8403871806729342 ) ) ;
#74628 = DIRECTION ( 'NONE',  ( 0.000000000000000000, 0.000000000000000000, 1.000000000000000000 ) ) ;
#74629 = ORIENTED_EDGE ( 'NONE', *, *, #8697, .F. ) ;
#74630 = ADVANCED_FACE ( 'NONE', ( #21733 ), #85317, .F. ) ;
#74631 = DIRECTION ( 'NONE',  ( 3.999999999999999995E-14, -1.000000000000000000, 4.100000000000000342E-29 ) ) ;
#74633 = ADVANCED_FACE ( 'NONE', ( #28518 ), #70776, .F. ) ;
#74632 = DIRECTION ( 'NONE',  ( 0.000000000000000000, 1.000000000000000000, 0.000000000000000000 ) ) ;
#74634 = CARTESIAN_POINT ( 'NONE',  ( 72.06648329127386887, -9.729447159941003065, 14.82207188531764430 ) ) ;
#74635 = EDGE_CURVE ( 'NONE', #13404, #36163, #49405, .T. ) ;
#74636 = CARTESIAN_POINT ( 'NONE',  ( 114.3647906391003630, -33.01227106732497418, 42.01951894101996032 ) ) ;
#74637 = CARTESIAN_POINT ( 'NONE',  ( 108.2792189108890568, -26.31750842948725122, 125.9841967044819597 ) ) ;
#74638 = CARTESIAN_POINT ( 'NONE',  ( 19.56670390244739721, -25.42844715994192129, 249.9678068554150059 ) ) ;
#74639 = VERTEX_POINT ( 'NONE', #84862 ) ;
#74640 = EDGE_CURVE ( 'NONE', #42455, #52237, #71229, .T. ) ;
#74641 = DIRECTION ( 'NONE',  ( 0.000000000000000000, 0.000000000000000000, -1.000000000000000000 ) ) ;
#74642 = CARTESIAN_POINT ( 'NONE',  ( 82.67897566168218759, -17.84952872353950681, 6.945088388038879401 ) ) ;
#74643 = ORIENTED_EDGE ( 'NONE', *, *, #86485, .F. ) ;
#74644 = EDGE_LOOP ( 'NONE', ( #34900, #19889, #32932, #13659 ) ) ;
#74645 = AXIS2_PLACEMENT_3D ( 'NONE', #52690, #18208, #38648 ) ;
#74646 = AXIS2_PLACEMENT_3D ( 'NONE', #25531, #53204, #80973 ) ;
#74647 = DIRECTION ( 'NONE',  ( -1.000000000000000000, 0.000000000000000000, 1.047445008332813989E-14 ) ) ;
#74648 = AXIS2_PLACEMENT_3D ( 'NONE', #63538, #42622, #84901 ) ;
#74649 = VERTEX_POINT ( 'NONE', #28072 ) ;
#74650 = ORIENTED_EDGE ( 'NONE', *, *, #79577, .F. ) ;
#74651 = CARTESIAN_POINT ( 'NONE',  ( 146.0667039024470171, -86.77844715994089597, 55.21780685541800437 ) ) ;
#74652 = AXIS2_PLACEMENT_3D ( 'NONE', #41473, #81514, #13349 ) ;
#74653 = CARTESIAN_POINT ( 'NONE',  ( 107.7234663162357151, -28.21331511381966806, 69.43813411379096578 ) ) ;
#74655 = CARTESIAN_POINT ( 'NONE',  ( 113.0381276193345883, -46.05869713813741129, 218.0175300378159591 ) ) ;
#74654 = AXIS2_PLACEMENT_3D ( 'NONE', #10550, #3740, #31430 ) ;
#74656 = AXIS2_PLACEMENT_3D ( 'NONE', #11366, #12719, #18175 ) ;
#74657 = CARTESIAN_POINT ( 'NONE',  ( 98.02603654163375779, -30.41010087969369735, 160.8289586092449497 ) ) ;
#74659 = CARTESIAN_POINT ( 'NONE',  ( 105.3240584539683482, -26.47319898023377149, 11.20991099019697046 ) ) ;
#74658 = DIRECTION ( 'NONE',  ( -0.7071067812162665778, -0.7071067811568285677, 2.899137802742881592E-29 ) ) ;
#74660 = DIRECTION ( 'NONE',  ( 0.000000000000000000, -1.000000000000000000, 0.000000000000000000 ) ) ;
#74661 = CARTESIAN_POINT ( 'NONE',  ( 193.0371591254582881, -47.82818131005411999, 300.4678068554149490 ) ) ;
#74662 = ORIENTED_EDGE ( 'NONE', *, *, #34507, .F. ) ;
#74663 = ORIENTED_EDGE ( 'NONE', *, *, #41356, .T. ) ;
#74664 = CARTESIAN_POINT ( 'NONE',  ( 97.81192379525968761, -40.51799951135461697, 111.6356742260152402 ) ) ;
#74665 = CARTESIAN_POINT ( 'NONE',  ( 96.72907894039983034, -34.86132901292410224, 241.1841967044819626 ) ) ;
#74666 = ORIENTED_EDGE ( 'NONE', *, *, #68415, .F. ) ;
#74667 = CARTESIAN_POINT ( 'NONE',  ( 99.08584233156592802, -29.96666100724374715, 215.7670538473399517 ) ) ;
#74668 = PLANE ( 'NONE',  #37010 ) ;
#74669 = CARTESIAN_POINT ( 'NONE',  ( -22.56126763944003244, 58.71304942578738917, 30.70258120403678248 ) ) ;
#74670 = FACE_OUTER_BOUND ( 'NONE', #79394, .T. ) ;
#74671 = CARTESIAN_POINT ( 'NONE',  ( 46.83715912545339677, -47.82818131006086304, 180.4678068554150911 ) ) ;
#74672 = VECTOR ( 'NONE', #1056, 1000.000000000000000 ) ;
#74674 = LINE ( 'NONE', #46496, #670 ) ;
#74673 = CARTESIAN_POINT ( 'NONE',  ( 98.00685971283303388, -38.32702420013065137, 277.6356252759115932 ) ) ;
#74675 = CARTESIAN_POINT ( 'NONE',  ( 122.2221484686747317, -96.68314769832136335, -21.78219314458224076 ) ) ;
#74676 = CARTESIAN_POINT ( 'NONE',  ( 115.0439452383992318, -109.4614598618342853, -19.78219314458184996 ) ) ;
#74677 = LINE ( 'NONE', #40599, #45483 ) ;
#74678 = LINE ( 'NONE', #41043, #10948 ) ;
#74679 = DIRECTION ( 'NONE',  ( -0.9825752044165969590, -0.1858654558159821002, 0.000000000000000000 ) ) ;
#74680 = LINE ( 'NONE', #6535, #68043 ) ;
#74682 = EDGE_LOOP ( 'NONE', ( #57078, #65224, #42161, #8669, #14843, #22714, #76658, #43749, #1622, #70972, #74572, #64604 ) ) ;
#74681 = CARTESIAN_POINT ( 'NONE',  ( 0.000000000000000000, 17.78000000000000114, -154.1697486074984909 ) ) ;
#74683 = LINE ( 'NONE', #12464, #35008 ) ;
#74684 = CARTESIAN_POINT ( 'NONE',  ( 95.27000809083011745, -38.09955253919518015, 236.4184824187679510 ) ) ;
#74685 = CARTESIAN_POINT ( 'NONE',  ( 107.6031410145815528, -26.28275719304336633, 91.03562527591097364 ) ) ;
#74686 = CARTESIAN_POINT ( 'NONE',  ( 95.18190931754610062, -37.33608887137841492, 267.3670538473396618 ) ) ;
#74687 = CARTESIAN_POINT ( 'NONE',  ( 49.21437657594998427, -35.91149509761070391, -5.074374724088000832 ) ) ;
#74688 = PLANE ( 'NONE',  #46063 ) ;
#74690 = CARTESIAN_POINT ( 'NONE',  ( 116.3214877775586018, -32.94188667902410117, 30.13562527591096085 ) ) ;
#74689 = CARTESIAN_POINT ( 'NONE',  ( 28.57499999999999929, 87.13271776169258942, 310.8325000000000387 ) ) ;
#74691 = DIRECTION ( 'NONE',  ( -1.000000000000000000, 0.000000000000000000, 0.000000000000000000 ) ) ;
#74692 = VECTOR ( 'NONE', #40158, 1000.000000000000000 ) ;
#74693 = CARTESIAN_POINT ( 'NONE',  ( 133.0080215814340647, -21.26771232012911383, 1.799893082727315186 ) ) ;
#74694 = ADVANCED_FACE ( 'NONE', ( #55755 ), #83502, .F. ) ;
#74695 = CIRCLE ( 'NONE', #35517, 0.4999999999999932832 ) ;
#74696 = EDGE_LOOP ( 'NONE', ( #22914, #58934, #38795, #14952, #54232 ) ) ;
#74697 = EDGE_CURVE ( 'NONE', #2616, #32576, #45273, .T. ) ;
#74698 = ORIENTED_EDGE ( 'NONE', *, *, #64785, .T. ) ;
#74699 = CARTESIAN_POINT ( 'NONE',  ( 108.3628298334300268, -27.77214277553820665, 149.3962293518869444 ) ) ;
#74700 = EDGE_CURVE ( 'NONE', #24432, #21921, #17647, .T. ) ;
#74702 = VERTEX_POINT ( 'NONE', #18469 ) ;
#74701 = LINE ( 'NONE', #19294, #69102 ) ;
#74703 = LINE ( 'NONE', #61505, #12662 ) ;
#74704 = CARTESIAN_POINT ( 'NONE',  ( 116.7751801856527152, -32.99181816784840748, 135.1184824187679396 ) ) ;
#74705 = CYLINDRICAL_SURFACE ( 'NONE', #30901, 9.999999999999998224 ) ;
#74706 = CARTESIAN_POINT ( 'NONE',  ( -47.06748920650090184, 92.32491709964729409, 74.53227049051039899 ) ) ;
#74707 = EDGE_CURVE ( 'NONE', #73595, #55433, #3070, .T. ) ;
#74708 = EDGE_CURVE ( 'NONE', #52316, #6564, #19142, .T. ) ;
#74709 = CARTESIAN_POINT ( 'NONE',  ( 21.03689327557613709, -23.42844715994197813, 193.9678068554150627 ) ) ;
#74710 = CARTESIAN_POINT ( 'NONE',  ( 108.3334481003509779, -46.73485935324176666, 108.6772919430070914 ) ) ;
#74711 = CARTESIAN_POINT ( 'NONE',  ( 112.4079628628857677, -28.49644221148687251, 69.61848241876894861 ) ) ;
#74712 = ORIENTED_EDGE ( 'NONE', *, *, #76438, .T. ) ;
#74713 = ORIENTED_EDGE ( 'NONE', *, *, #62063, .T. ) ;
#74714 = ORIENTED_EDGE ( 'NONE', *, *, #62831, .F. ) ;
#74715 = ADVANCED_FACE ( 'NONE', ( #58025 ), #59794, .T. ) ;
#74716 = CIRCLE ( 'NONE', #34112, 8.999999999999994671 ) ;
#74717 = DIRECTION ( 'NONE',  ( 0.000000000000000000, 0.000000000000000000, -1.000000000000000000 ) ) ;
#74718 = VECTOR ( 'NONE', #17953, 1000.000000000000227 ) ;
#74720 = DIRECTION ( 'NONE',  ( 1.000000000000000000, 0.000000000000000000, 0.000000000000000000 ) ) ;
#74719 = CARTESIAN_POINT ( 'NONE',  ( 108.6395843534182291, -26.47938140272626484, 140.9432443235289725 ) ) ;
#74721 = VECTOR ( 'NONE', #7829, 1000.000000000000000 ) ;
#74722 = CARTESIAN_POINT ( 'NONE',  ( 0.000000000000000000, 103.1240000000000236, 0.000000000000000000 ) ) ;
#74723 = ADVANCED_FACE ( 'NONE', ( #24411 ), #45706, .F. ) ;
#74724 = CARTESIAN_POINT ( 'NONE',  ( 70.06670417066790435, -71.37844715994097555, 55.21780685541800437 ) ) ;
#74726 = DIRECTION ( 'NONE',  ( 1.000000000000000000, 0.000000000000000000, 0.000000000000000000 ) ) ;
#74725 = VECTOR ( 'NONE', #22101, 1000.000000000000000 ) ;
#74727 = CARTESIAN_POINT ( 'NONE',  ( 142.8687636814963184, 5.654319119531125537, 543.8623766218582887 ) ) ;
#74728 = CARTESIAN_POINT ( 'NONE',  ( 59.67056972692184758, -130.5939552371641810, 126.9238073910411941 ) ) ;
#74729 = CARTESIAN_POINT ( 'NONE',  ( 96.66103594285301881, -37.56076609107802255, 101.3899109901969524 ) ) ;
#74730 = ORIENTED_EDGE ( 'NONE', *, *, #43477, .F. ) ;
#74732 = ORIENTED_EDGE ( 'NONE', *, *, #13978, .F. ) ;
#74731 = ADVANCED_FACE ( 'NONE', ( #58900 ), #24908, .F. ) ;
#74733 = FACE_OUTER_BOUND ( 'NONE', #8064, .T. ) ;
#74734 = CARTESIAN_POINT ( 'NONE',  ( -83.40142812120586768, 86.64186789594792515, -100.4448767513720639 ) ) ;
#74735 = CARTESIAN_POINT ( 'NONE',  ( 204.2160000000000082, 52.73749999999999716, -47.62500000000000000 ) ) ;
#74737 = CARTESIAN_POINT ( 'NONE',  ( 105.6960798208838384, -45.90617939248504342, 145.2766617981629622 ) ) ;
#74736 = AXIS2_PLACEMENT_3D ( 'NONE', #42287, #62744, #77283 ) ;
#74738 = AXIS2_PLACEMENT_3D ( 'NONE', #16937, #44616, #64198 ) ;
#74739 = PLANE ( 'NONE',  #57654 ) ;
#74740 = VERTEX_POINT ( 'NONE', #52075 ) ;
#74741 = ORIENTED_EDGE ( 'NONE', *, *, #62631, .T. ) ;
#74742 = DIRECTION ( 'NONE',  ( -0.000000000000000000, -0.000000000000000000, -1.000000000000000000 ) ) ;
#74743 = CARTESIAN_POINT ( 'NONE',  ( 136.6493805748345380, -19.67376371870151175, 2.871651383882735331 ) ) ;
#74744 = ORIENTED_EDGE ( 'NONE', *, *, #3845, .T. ) ;
#74745 = ORIENTED_EDGE ( 'NONE', *, *, #89621, .T. ) ;
#74746 = LINE ( 'NONE', #12524, #54958 ) ;
#74747 = EDGE_CURVE ( 'NONE', #65614, #43245, #64090, .T. ) ;
#74748 = CARTESIAN_POINT ( 'NONE',  ( 109.2250051346758113, -28.10373483931914151, 196.3130118773259767 ) ) ;
#74749 = EDGE_CURVE ( 'NONE', #65895, #85412, #72561, .T. ) ;
#74750 = LINE ( 'NONE', #67036, #21143 ) ;
#74751 = COLOUR_RGB ( '', 0.31764706, 0.68627451, 0.89019608) ;
#74752 = CARTESIAN_POINT ( 'NONE',  ( 134.0664832912740110, -46.72944715994100306, 4.925625275910997303 ) ) ;
#74753 = VERTEX_POINT ( 'NONE', #79835 ) ;
#74754 = ORIENTED_EDGE ( 'NONE', *, *, #30409, .T. ) ;
#74755 = CARTESIAN_POINT ( 'NONE',  ( 0.000000000000000000, 61.59999999999999432, 0.000000000000000000 ) ) ;
#74756 = VECTOR ( 'NONE', #12457, 1000.000000000000000 ) ;
#74757 = VERTEX_POINT ( 'NONE', #4411 ) ;
#74758 = EDGE_LOOP ( 'NONE', ( #61868, #50610, #16657, #86946 ) ) ;
#74759 = CARTESIAN_POINT ( 'NONE',  ( 100.7056284991137289, -31.61385801203766377, 238.6052332267339580 ) ) ;
#74760 = CARTESIAN_POINT ( 'NONE',  ( 95.46334413863738177, -34.19939227723602926, 106.1556252759109640 ) ) ;
#74761 = CARTESIAN_POINT ( 'NONE',  ( 109.9050689397999889, -46.77468768478704675, 72.79562527591099297 ) ) ;
#74762 = CARTESIAN_POINT ( 'NONE',  ( 101.0001179910210141, -41.97448653419763787, 249.5838068554172366 ) ) ;
#74763 = CARTESIAN_POINT ( 'NONE',  ( 131.4524275574068497, -17.85322059724320454, 6.943211687812105737 ) ) ;
#74764 = CARTESIAN_POINT ( 'NONE',  ( 188.5667039024484950, -42.82844715993430640, 139.7178068554150059 ) ) ;
#74765 = CARTESIAN_POINT ( 'NONE',  ( 114.8139851684208992, -29.70110827795256014, 205.4127681330539872 ) ) ;
#74766 = LINE ( 'NONE', #13440, #50905 ) ;
#74767 = VERTEX_POINT ( 'NONE', #78937 ) ;
#74768 = CARTESIAN_POINT ( 'NONE',  ( 129.9368274816652047, 81.71102547120854354, -12.69999999999864038 ) ) ;
#74769 = VERTEX_POINT ( 'NONE', #10328 ) ;
#74770 = ORIENTED_EDGE ( 'NONE', *, *, #27357, .T. ) ;
#74771 = DIRECTION ( 'NONE',  ( 0.000000000000000000, 0.000000000000000000, -1.000000000000000000 ) ) ;
#74772 = ORIENTED_EDGE ( 'NONE', *, *, #40750, .F. ) ;
#74773 = VECTOR ( 'NONE', #16305, 1000.000000000000000 ) ;
#74774 = DIRECTION ( 'NONE',  ( 0.7071067811864656383, 0.7071067811866295072, 7.071067811864650974E-16 ) ) ;
#74775 = CIRCLE ( 'NONE', #58815, 36.57600000000000051 ) ;
#74776 = CIRCLE ( 'NONE', #55884, 3.814291549405317117 ) ;
#74777 = CARTESIAN_POINT ( 'NONE',  ( 100.9531696234827933, -28.70820207419374626, 91.59410946087238869 ) ) ;
#74778 = CARTESIAN_POINT ( 'NONE',  ( 97.93239114460148187, -31.63098981178377755, 110.9213395616259703 ) ) ;
#74779 = CARTESIAN_POINT ( 'NONE',  ( 115.8281814637101377, -31.73477629227051366, 254.2397833965958114 ) ) ;
#74780 = DIRECTION ( 'NONE',  ( -1.000000000000000000, -4.299999999999999979E-14, -1.000000000000000078E-15 ) ) ;
#74781 = DIRECTION ( 'NONE',  ( 0.000000000000000000, 0.000000000000000000, 1.000000000000000000 ) ) ;
#74784 = CARTESIAN_POINT ( 'NONE',  ( 117.7539631054256972, -31.66723592997637482, 210.1784824187679703 ) ) ;
#74783 = DIRECTION ( 'NONE',  ( 0.7071067811865491270, -0.7071067811865459074, 7.071067811865492096E-16 ) ) ;
#74782 = CARTESIAN_POINT ( 'NONE',  ( 112.0659116166449536, -45.48839626399238512, 143.9897919420481287 ) ) ;
#74785 = CARTESIAN_POINT ( 'NONE',  ( 154.5667039024470171, -79.67844715994088745, 85.21780685541799016 ) ) ;
#74786 = CARTESIAN_POINT ( 'NONE',  ( -487.2989999999999782, 93.66249999999999432, 6.350000000000409983 ) ) ;
#74787 = VERTEX_POINT ( 'NONE', #72990 ) ;
#74788 = CARTESIAN_POINT ( 'NONE',  ( 9.261585182541617556, 239.0000000000000000, 152.5407914452011653 ) ) ;
#74789 = AXIS2_PLACEMENT_3D ( 'NONE', #16171, #49321, #43850 ) ;
#74790 = FACE_OUTER_BOUND ( 'NONE', #60772, .T. ) ;
#74791 = DIRECTION ( 'NONE',  ( 0.000000000000000000, -1.000000000000000000, 0.000000000000000000 ) ) ;
#74792 = VECTOR ( 'NONE', #72595, 1000.000000000000000 ) ;
#74793 = DIRECTION ( 'NONE',  ( 0.000000000000000000, 1.000000000000000000, 0.000000000000000000 ) ) ;
#74795 = VERTEX_POINT ( 'NONE', #11674 ) ;
#74794 = CARTESIAN_POINT ( 'NONE',  ( 105.6259887305572676, -47.09919361126699044, 257.4670538473392298 ) ) ;
#74796 = CARTESIAN_POINT ( 'NONE',  ( 59.56670390244699576, -67.87844715994098976, 190.2178068554179902 ) ) ;
#74797 = CARTESIAN_POINT ( 'NONE',  ( 105.1635842947561343, -47.00881719185149876, 8.429910990196965770 ) ) ;
#74798 = CARTESIAN_POINT ( 'NONE',  ( 103.7937703862009613, -26.78548768338485075, 161.3299109901969643 ) ) ;
#74799 = DIRECTION ( 'NONE',  ( 1.000000000000000078E-15, -1.000000000000000083E-30, -1.000000000000000000 ) ) ;
#74800 = DIRECTION ( 'NONE',  ( 1.000000000000000078E-15, 1.000000000000000083E-30, -1.000000000000000000 ) ) ;
#74801 = AXIS2_PLACEMENT_3D ( 'NONE', #22675, #36743, #29933 ) ;
#74802 = EDGE_CURVE ( 'NONE', #54909, #22054, #71419, .T. ) ;
#74804 = DIRECTION ( 'NONE',  ( 0.000000000000000000, 1.000000000000000000, 0.000000000000000000 ) ) ;
#74803 = CARTESIAN_POINT ( 'NONE',  ( 33.98325472291465132, 8.255000000000000782, 3.174999999999999822 ) ) ;
#74805 = DIRECTION ( 'NONE',  ( -1.000000000000000078E-15, 0.000000000000000000, 1.000000000000000000 ) ) ;
#74806 = DIRECTION ( 'NONE',  ( 1.071939472051879986E-15, 0.000000000000000000, 1.000000000000000000 ) ) ;
#74807 = ORIENTED_EDGE ( 'NONE', *, *, #4865, .F. ) ;
#74808 = VECTOR ( 'NONE', #72698, 1000.000000000000000 ) ;
#74809 = EDGE_CURVE ( 'NONE', #47917, #32414, #38463, .T. ) ;
#74810 = VERTEX_POINT ( 'NONE', #18023 ) ;
#74811 = EDGE_CURVE ( 'NONE', #25056, #55605, #3954, .T. ) ;
#74812 = ORIENTED_EDGE ( 'NONE', *, *, #46078, .F. ) ;
#74813 = EDGE_CURVE ( 'NONE', #2544, #66251, #69982, .T. ) ;
#74814 = ORIENTED_EDGE ( 'NONE', *, *, #6531, .F. ) ;
#74815 = DIRECTION ( 'NONE',  ( 0.000000000000000000, -1.000000000000000000, 0.000000000000000000 ) ) ;
#74816 = CARTESIAN_POINT ( 'NONE',  ( 115.4270991047690558, -42.97960947038945534, 24.31562527591096767 ) ) ;
#74817 = DIRECTION ( 'NONE',  ( 1.000000000000000078E-15, 1.000000000000000083E-30, -1.000000000000000000 ) ) ;
#74818 = CARTESIAN_POINT ( 'NONE',  ( 145.3840438162638407, -139.2490617783571167, 246.2187065265057413 ) ) ;
#74819 = EDGE_CURVE ( 'NONE', #77225, #71373, #30811, .T. ) ;
#74821 = CARTESIAN_POINT ( 'NONE',  ( 70.10184668782046913, -140.7135899453143963, 245.8512780488630085 ) ) ;
#74820 = CARTESIAN_POINT ( 'NONE',  ( 194.5667039024482960, -47.82844715993405771, 300.4678068554149490 ) ) ;
#74822 = CARTESIAN_POINT ( 'NONE',  ( 106.6575247680289777, -45.29010455595041407, 246.9609912566479579 ) ) ;
#74823 = ORIENTED_EDGE ( 'NONE', *, *, #5508, .F. ) ;
#74824 = VERTEX_POINT ( 'NONE', #73888 ) ;
#74825 = AXIS2_PLACEMENT_3D ( 'NONE', #58996, #86736, #24507 ) ;
#74826 = ORIENTED_EDGE ( 'NONE', *, *, #2141, .T. ) ;
#74827 = EDGE_CURVE ( 'NONE', #61623, #15987, #80280, .T. ) ;
#74828 = DIRECTION ( 'NONE',  ( -1.000000000000000000, -4.299999999999999979E-14, -1.000000000000000078E-15 ) ) ;
#74829 = VECTOR ( 'NONE', #47367, 999.9999999999998863 ) ;
#74830 = DIRECTION ( 'NONE',  ( 0.000000000000000000, 1.000000000000000000, 1.056314557550181068E-14 ) ) ;
#74831 = CARTESIAN_POINT ( 'NONE',  ( 50.96943157743500308, -34.03355364505722491, 342.9256252759109884 ) ) ;
#74832 = DIRECTION ( 'NONE',  ( 0.000000000000000000, 0.000000000000000000, 1.000000000000000000 ) ) ;
#74833 = CARTESIAN_POINT ( 'NONE',  ( 110.0319707555399447, -45.11204900458633915, 34.27872616304095033 ) ) ;
#74834 = ADVANCED_FACE ( 'NONE', ( #11210 ), #32097, .F. ) ;
#74835 = CARTESIAN_POINT ( 'NONE',  ( 118.3663208563465190, 93.33902940301965145, 6.712516165663437562 ) ) ;
#74836 = DIRECTION ( 'NONE',  ( 0.000000000000000000, 0.000000000000000000, 1.000000000000000000 ) ) ;
#74837 = CARTESIAN_POINT ( 'NONE',  ( 112.3177584634463244, -44.98096486020163098, 263.0270538473400279 ) ) ;
#74838 = DIRECTION ( 'NONE',  ( 0.000000000000000000, 0.000000000000000000, 1.000000000000000000 ) ) ;
#74840 = ORIENTED_EDGE ( 'NONE', *, *, #65811, .F. ) ;
#74839 = ADVANCED_FACE ( 'NONE', ( #60691 ), #5304, .F. ) ;
#74841 = LINE ( 'NONE', #26678, #73674 ) ;
#74842 = CARTESIAN_POINT ( 'NONE',  ( 180.3521107875639871, -35.65087443492551245, 193.9678068554150059 ) ) ;
#74843 = CARTESIAN_POINT ( 'NONE',  ( 102.2704046875766579, -44.67259270758150080, 49.96237608387698970 ) ) ;
#74844 = CIRCLE ( 'NONE', #25550, 9.571100913904325935 ) ;
#74845 = CIRCLE ( 'NONE', #70508, 9.571100913904340146 ) ;
#74846 = AXIS2_PLACEMENT_3D ( 'NONE', #10047, #79098, #71827 ) ;
#74847 = CARTESIAN_POINT ( 'NONE',  ( 136.7727304466921510, -18.23917853420268287, 6.814128304789858426 ) ) ;
#74848 = AXIS2_PLACEMENT_3D ( 'NONE', #82345, #74168, #11948 ) ;
#74849 = CYLINDRICAL_SURFACE ( 'NONE', #65002, 12.99999999999999822 ) ;
#74850 = CARTESIAN_POINT ( 'NONE',  ( 177.4809174648214309, -49.32844715993478957, 249.9678068554149775 ) ) ;
#74851 = ORIENTED_EDGE ( 'NONE', *, *, #26180, .T. ) ;
#74852 = CARTESIAN_POINT ( 'NONE',  ( 25.56670390244745050, -48.82844715994178841, 170.7178068554150627 ) ) ;
#74853 = ORIENTED_EDGE ( 'NONE', *, *, #60442, .T. ) ;
#74854 = CARTESIAN_POINT ( 'NONE',  ( 101.5007711604877159, -27.91412646590841362, 110.5241967044819944 ) ) ;
#74855 = VERTEX_POINT ( 'NONE', #26190 ) ;
#74856 = CARTESIAN_POINT ( 'NONE',  ( 106.7337219657603100, -28.19449539544314476, 84.52956268522000016 ) ) ;
#74857 = CARTESIAN_POINT ( 'NONE',  ( 97.81171347387959258, -40.51745984142272761, 22.63530404563221410 ) ) ;
#74858 = CARTESIAN_POINT ( 'NONE',  ( 102.5524010923236915, -28.48932656383806972, 96.89491663923000431 ) ) ;
#74859 = CARTESIAN_POINT ( 'NONE',  ( 167.7413838386819123, -48.33240602328260849, 180.4678068554150059 ) ) ;
#74860 = ADVANCED_FACE ( 'NONE', ( #53859 ), #55206, .F. ) ;
#74861 = DIRECTION ( 'NONE',  ( 0.000000000000000000, 0.000000000000000000, 1.000000000000000000 ) ) ;
#74862 = CIRCLE ( 'NONE', #6707, 4.750000000000004441 ) ;
#74863 = CARTESIAN_POINT ( 'NONE',  ( 117.9472974416529638, -41.48656121291797660, 54.49848241876792088 ) ) ;
#74864 = DIRECTION ( 'NONE',  ( 0.000000000000000000, 0.000000000000000000, -1.000000000000000000 ) ) ;
#74865 = CARTESIAN_POINT ( 'NONE',  ( 117.0719393226367515, -35.46284531538225337, 258.9272565253700122 ) ) ;
#74866 = VERTEX_POINT ( 'NONE', #62042 ) ;
#74867 = CARTESIAN_POINT ( 'NONE',  ( 77.31651901074906164, -18.90078909148962083, 3.101427792080710955 ) ) ;
#74868 = EDGE_LOOP ( 'NONE', ( #5506, #34149, #41395, #1449, #60055, #73418 ) ) ;
#74869 = CIRCLE ( 'NONE', #35704, 7.143750000000004263 ) ;
#74870 = VERTEX_POINT ( 'NONE', #61587 ) ;
#74871 = FACE_OUTER_BOUND ( 'NONE', #26137, .T. ) ;
#74872 = ORIENTED_EDGE ( 'NONE', *, *, #65498, .F. ) ;
#74873 = CARTESIAN_POINT ( 'NONE',  ( 96.02263050233423769, -38.01213896886783061, 236.4184824187689458 ) ) ;
#74874 = CARTESIAN_POINT ( 'NONE',  ( 98.83948440537673719, -30.29086274794821065, 151.7984824187679465 ) ) ;
#74875 = CARTESIAN_POINT ( 'NONE',  ( 0.000000000000000000, 65.60000000000000853, 38.10000000000000142 ) ) ;
#74876 = CARTESIAN_POINT ( 'NONE',  ( 113.1762138295820961, -44.75342279309901983, 129.0937539895759869 ) ) ;
#74877 = CARTESIAN_POINT ( 'NONE',  ( 96.65662162753720565, -37.29271227441797265, 72.36991099019596163 ) ) ;
#74878 = DIRECTION ( 'NONE',  ( -1.000000000000000000, 0.000000000000000000, 0.000000000000000000 ) ) ;
#74879 = ORIENTED_EDGE ( 'NONE', *, *, #26338, .T. ) ;
#74880 = DIRECTION ( 'NONE',  ( 0.000000000000000000, 0.000000000000000000, -1.000000000000000000 ) ) ;
#74881 = EDGE_CURVE ( 'NONE', #66717, #51052, #32993, .T. ) ;
#74882 = CARTESIAN_POINT ( 'NONE',  ( 116.7952875727523576, -39.38725125411153272, 159.6146818031017744 ) ) ;
#74883 = CIRCLE ( 'NONE', #9651, 9.524999999999998579 ) ;
#74884 = VERTEX_POINT ( 'NONE', #81627 ) ;
#74885 = EDGE_CURVE ( 'NONE', #59669, #71638, #88876, .T. ) ;
#74886 = DIRECTION ( 'NONE',  ( 0.000000000000000000, 0.000000000000000000, -1.000000000000000000 ) ) ;
#74887 = LINE ( 'NONE', #88528, #68735 ) ;
#74888 = CARTESIAN_POINT ( 'NONE',  ( 117.4080659314679025, -35.59792815749687378, 278.9127681330539872 ) ) ;
#74889 = CARTESIAN_POINT ( 'NONE',  ( 162.0667039024469886, -68.87844715994089029, 96.96780685541800437 ) ) ;
#74890 = DIRECTION ( 'NONE',  ( -0.4999999999999998890, 0.8660254037844387076, 0.000000000000000000 ) ) ;
#74891 = DIRECTION ( 'NONE',  ( 0.000000000000000000, 0.000000000000000000, 1.000000000000000000 ) ) ;
#74892 = CARTESIAN_POINT ( 'NONE',  ( 101.4801710200817126, -30.26808144278882651, 260.0667055423624561 ) ) ;
#74894 = CARTESIAN_POINT ( 'NONE',  ( 114.0075736764522389, -28.98025818340847692, 110.4956252759109816 ) ) ;
#74893 = PLANE ( 'NONE',  #55021 ) ;
#74895 = CARTESIAN_POINT ( 'NONE',  ( 110.2536356736639220, -106.6957733451327215, -19.78219314458193168 ) ) ;
#74896 = CARTESIAN_POINT ( 'NONE',  ( 114.3747829841801149, -29.18355094256887838, 174.4641967044819637 ) ) ;
#74897 = VERTEX_POINT ( 'NONE', #74786 ) ;
#74898 = DIRECTION ( 'NONE',  ( 0.000000000000000000, 0.000000000000000000, -1.000000000000000000 ) ) ;
#74899 = ORIENTED_EDGE ( 'NONE', *, *, #60728, .T. ) ;
#74900 = FACE_OUTER_BOUND ( 'NONE', #75196, .T. ) ;
#74901 = CARTESIAN_POINT ( 'NONE',  ( 141.0664832912740394, -46.72944715994099596, 14.67562527591100441 ) ) ;
#74902 = CARTESIAN_POINT ( 'NONE',  ( -479.3614999999999782, 104.7749999999999915, -1.387778780781445991E-14 ) ) ;
#74903 = ORIENTED_EDGE ( 'NONE', *, *, #75245, .T. ) ;
#74904 = FACE_OUTER_BOUND ( 'NONE', #70181, .T. ) ;
#74906 = EDGE_LOOP ( 'NONE', ( #66997, #80436, #4902, #2127 ) ) ;
#74905 = CARTESIAN_POINT ( 'NONE',  ( 113.8721965385452677, -28.72731865945801744, 139.5156252759109634 ) ) ;
#74907 = DIRECTION ( 'NONE',  ( 0.000000000000000000, 1.000000000000000000, 0.000000000000000000 ) ) ;
#74908 = VECTOR ( 'NONE', #60534, 1000.000000000000000 ) ;
#74909 = CARTESIAN_POINT ( 'NONE',  ( -130.2266700119015184, 91.23859726994547259, 9.271983876140998504 ) ) ;
#74910 = DIRECTION ( 'NONE',  ( -3.100000000000000258E-29, 3.100000000000000044E-14, 1.000000000000000000 ) ) ;
#74912 = AXIS2_PLACEMENT_3D ( 'NONE', #40981, #49121, #75519 ) ;
#74911 = CARTESIAN_POINT ( 'NONE',  ( -0.8023776826656670025, 53.97499999999997300, -4.197052493943455254 ) ) ;
#74913 = ORIENTED_EDGE ( 'NONE', *, *, #76995, .T. ) ;
#74914 = CIRCLE ( 'NONE', #28475, 9.524999999999998579 ) ;
#74915 = CIRCLE ( 'NONE', #37180, 3.814291549405317117 ) ;
#74916 = APPLICATION_PROTOCOL_DEFINITION ( 'draft international standard', 'automotive_design', 1998, #9218 ) ;
#74917 = AXIS2_PLACEMENT_3D ( 'NONE', #3676, #65013, #31370 ) ;
#74918 = EDGE_CURVE ( 'NONE', #17548, #72419, #19824, .T. ) ;
#74919 = FACE_OUTER_BOUND ( 'NONE', #36179, .T. ) ;
#74920 = ORIENTED_EDGE ( 'NONE', *, *, #7369, .T. ) ;
#74921 = EDGE_CURVE ( 'NONE', #49976, #6901, #4852, .T. ) ;
#74922 = ADVANCED_FACE ( 'NONE', ( #6203 ), #82074, .T. ) ;
#74923 = ORIENTED_EDGE ( 'NONE', *, *, #44066, .T. ) ;
#74924 = LINE ( 'NONE', #48973, #45232 ) ;
#74925 = CARTESIAN_POINT ( 'NONE',  ( 87.71605664019014625, 93.55484823631826430, -96.70003673985416981 ) ) ;
#74926 = CARTESIAN_POINT ( 'NONE',  ( 105.7154772392229063, -46.72385838064575125, 157.4689586019844683 ) ) ;
#74927 = CARTESIAN_POINT ( 'NONE',  ( 72.96458098368650269, 127.0000000000000000, 72.96458098368729850 ) ) ;
#74928 = EDGE_CURVE ( 'NONE', #18950, #84106, #67514, .T. ) ;
#74930 = CARTESIAN_POINT ( 'NONE',  ( -0.8391700603252211232, 69.85000000000000853, -118.5560000000000400 ) ) ;
#74929 = CARTESIAN_POINT ( 'NONE',  ( 100.9545475257521332, -28.70712375422630558, 105.5939711813188495 ) ) ;
#74931 = CARTESIAN_POINT ( 'NONE',  ( 97.07202417197602529, -35.37877911891951044, 181.2189852412958260 ) ) ;
#74932 = VERTEX_POINT ( 'NONE', #34336 ) ;
#74933 = DIRECTION ( 'NONE',  ( 1.000000000000000000, 0.000000000000000000, 0.000000000000000000 ) ) ;
#74934 = DIRECTION ( 'NONE',  ( 1.000000000000000078E-15, -1.000000000000000083E-30, -1.000000000000000000 ) ) ;
#74935 = CARTESIAN_POINT ( 'NONE',  ( 98.96845470676157674, -30.25173782105014197, 191.7775300378149836 ) ) ;
#74936 = EDGE_CURVE ( 'NONE', #37298, #42164, #46610, .T. ) ;
#74938 = ORIENTED_EDGE ( 'NONE', *, *, #37476, .F. ) ;
#74937 = CARTESIAN_POINT ( 'NONE',  ( 31.56670390244700641, -22.48495420874110806, 342.9256252759109884 ) ) ;
#74939 = CARTESIAN_POINT ( 'NONE',  ( 103.2241971045484519, -45.72390501747104707, 88.25562527591095829 ) ) ;
#74940 = DIRECTION ( 'NONE',  ( 0.9242245927363033076, 0.3818493186865918321, 0.000000000000000000 ) ) ;
#74941 = LINE ( 'NONE', #67218, #83358 ) ;
#74942 = FACE_OUTER_BOUND ( 'NONE', #48528, .T. ) ;
#74943 = ORIENTED_EDGE ( 'NONE', *, *, #55940, .F. ) ;
#74944 = CYLINDRICAL_SURFACE ( 'NONE', #39945, 29.00000000000000000 ) ;
#74945 = EDGE_LOOP ( 'NONE', ( #26596, #10641 ) ) ;
#74946 = VERTEX_POINT ( 'NONE', #40704 ) ;
#74947 = CARTESIAN_POINT ( 'NONE',  ( 114.0241607691103809, -31.19294522270855907, 240.7930118773259665 ) ) ;
#74948 = CARTESIAN_POINT ( 'NONE',  ( 101.9940466514257622, -45.44635550110415068, 53.15612750292554267 ) ) ;
#74949 = CARTESIAN_POINT ( 'NONE',  ( -118.4232034889089533, 93.94553785444267646, -5.621872244391297180 ) ) ;
#74950 = CARTESIAN_POINT ( 'NONE',  ( -12.70000000000000107, 82.54999999999999716, -117.8738102209307641 ) ) ;
#74951 = CARTESIAN_POINT ( 'NONE',  ( 81.91406418435974501, -38.77438500683208389, 2.186796636968284080 ) ) ;
#74952 = ORIENTED_EDGE ( 'NONE', *, *, #41999, .T. ) ;
#74953 = DIRECTION ( 'NONE',  ( 0.000000000000000000, 0.000000000000000000, 1.000000000000000000 ) ) ;
#74954 = CARTESIAN_POINT ( 'NONE',  ( 147.0667039024469886, -67.87844715994090450, 222.2178068554179902 ) ) ;
#74955 = ORIENTED_EDGE ( 'NONE', *, *, #54848, .T. ) ;
#74956 = CARTESIAN_POINT ( 'NONE',  ( 97.79211192542227593, -40.52543860420435351, 11.63562527591094309 ) ) ;
#74957 = ORIENTED_EDGE ( 'NONE', *, *, #89170, .F. ) ;
#74958 = CARTESIAN_POINT ( 'NONE',  ( 102.1978417368446657, -43.31572210571547998, 254.8880903695915947 ) ) ;
#74959 = CARTESIAN_POINT ( 'NONE',  ( 184.5667039024480118, -48.82844715994099971, 300.9178068554150514 ) ) ;
#74960 = CARTESIAN_POINT ( 'NONE',  ( 116.2961327041338535, -39.96626766897450977, 133.5584824187689605 ) ) ;
#74961 = CARTESIAN_POINT ( 'NONE',  ( 107.0667039024470313, -104.2784471599409528, 222.2178068554179902 ) ) ;
#74962 = LINE ( 'NONE', #25923, #15760 ) ;
#74963 = CIRCLE ( 'NONE', #72060, 11.45913725231036118 ) ;
#74964 = EDGE_CURVE ( 'NONE', #51227, #70326, #20640, .T. ) ;
#74965 = CARTESIAN_POINT ( 'NONE',  ( 10.20674285154820460, 74.98125221267765994, 130.1568226710593592 ) ) ;
#74966 = CARTESIAN_POINT ( 'NONE',  ( 107.5118819425545951, -47.18863449879560079, 233.6099109901969655 ) ) ;
#74967 = DIRECTION ( 'NONE',  ( -1.000000000000000000, 0.000000000000000000, 0.000000000000000000 ) ) ;
#74968 = VERTEX_POINT ( 'NONE', #33891 ) ;
#74969 = AXIS2_PLACEMENT_3D ( 'NONE', #13798, #75586, #68319 ) ;
#74970 = CARTESIAN_POINT ( 'NONE',  ( 117.0955297935745705, -31.97384786926005873, 60.19086337114898555 ) ) ;
#74971 = CARTESIAN_POINT ( 'NONE',  ( 172.5664832912740110, -32.07844715994070839, 134.1756252759119832 ) ) ;
#74972 = VECTOR ( 'NONE', #69829, 1000.000000000000114 ) ;
#74973 = ADVANCED_FACE ( 'NONE', ( #74343 ), #27087, .F. ) ;
#74974 = VERTEX_POINT ( 'NONE', #89776 ) ;
#74975 = ORIENTED_EDGE ( 'NONE', *, *, #26423, .F. ) ;
#74976 = ORIENTED_EDGE ( 'NONE', *, *, #66675, .T. ) ;
#74977 = CARTESIAN_POINT ( 'NONE',  ( 108.4153923495580898, -26.73476988454487469, 159.9688923623228050 ) ) ;
#74978 = CARTESIAN_POINT ( 'NONE',  ( 141.0235900724605074, -8.833000550534283235, -5.074374724088999145 ) ) ;
#74979 = DIRECTION ( 'NONE',  ( -0.7071067811865453523, -0.7071067811865496822, -7.071067811865460542E-16 ) ) ;
#74980 = FACE_OUTER_BOUND ( 'NONE', #67082, .T. ) ;
#74981 = CARTESIAN_POINT ( 'NONE',  ( 112.4302714532559548, -29.93748856177429118, 122.3747570362579751 ) ) ;
#74982 = CARTESIAN_POINT ( 'NONE',  ( 115.3407290770031324, -45.24761053976980918, 264.1899109901965517 ) ) ;
#74983 = CARTESIAN_POINT ( 'NONE',  ( 41.56648329127381203, -27.82844715994070484, 261.9256252759120116 ) ) ;
#74984 = ORIENTED_EDGE ( 'NONE', *, *, #54097, .F. ) ;
#74985 = CARTESIAN_POINT ( 'NONE',  ( 130.0420937742006231, 87.79544278253750633, 11.57361518220490737 ) ) ;
#74986 = CIRCLE ( 'NONE', #35816, 5.599999999999994316 ) ;
#74987 = CARTESIAN_POINT ( 'NONE',  ( 97.80889870804310249, -40.51851473143300097, 41.63518016758125384 ) ) ;
#74988 = ORIENTED_EDGE ( 'NONE', *, *, #78941, .T. ) ;
#74989 = ORIENTED_EDGE ( 'NONE', *, *, #71469, .F. ) ;
#74990 = CLOSED_SHELL ( 'NONE', ( #15845, #49879, #79401, #50732, #31870, #68031, #88147, #39431, #40744, #55704, #20123, #61066, #67231, #25253, #2893, #12640, #67033, #75825, #64415, #83362, #9693, #33506, #74723, #83341, #59433, #14505, #60604, #84259, #27798, #34129, #56427, #73507, #60751, #33062, #40880, #34015, #58507, #18979, #29392, #66280, #56256, #19139, #30823, #89915, #20487, #35956, #38352, #78382, #15673, #6612, #54564, #89803, #43230, #31125, #24643, #72612, #55516, #75248, #77576 ) ) ;
#74991 = EDGE_CURVE ( 'NONE', #74036, #68275, #29337, .T. ) ;
#74992 = FACE_OUTER_BOUND ( 'NONE', #69909, .T. ) ;
#74993 = VERTEX_POINT ( 'NONE', #13458 ) ;
#74994 = ORIENTED_EDGE ( 'NONE', *, *, #9797, .F. ) ;
#74995 = PLANE ( 'NONE',  #457 ) ;
#74996 = DIRECTION ( 'NONE',  ( 0.000000000000000000, 0.000000000000000000, 1.000000000000000000 ) ) ;
#74997 = CARTESIAN_POINT ( 'NONE',  ( 177.0371591254546217, -48.62818131005479927, 117.4678068554150485 ) ) ;
#74998 = CYLINDRICAL_SURFACE ( 'NONE', #80880, 2.030000000001311644 ) ;
#74999 = CARTESIAN_POINT ( 'NONE',  ( 115.4591718486505698, -35.14231982251399700, 158.3981341137909737 ) ) ;
#75000 = CARTESIAN_POINT ( 'NONE',  ( 96.91385697446291658, -32.24201331651869396, 55.98324432352897162 ) ) ;
#75001 = CARTESIAN_POINT ( 'NONE',  ( 181.9694315774339941, -34.03355364505720360, 117.4678068554150627 ) ) ;
#75002 = ORIENTED_EDGE ( 'NONE', *, *, #57479, .F. ) ;
#75003 = CARTESIAN_POINT ( 'NONE',  ( -90.81844170390323256, 75.15251084995277608, -76.20754074253689225 ) ) ;
#75004 = ORIENTED_EDGE ( 'NONE', *, *, #61297, .F. ) ;
#75005 = CARTESIAN_POINT ( 'NONE',  ( -46.60773131249376178, 91.07499999999996021, -44.42500552774628630 ) ) ;
#75006 = ORIENTED_EDGE ( 'NONE', *, *, #61025, .F. ) ;
#75007 = DIRECTION ( 'NONE',  ( -1.000000000000000000, 0.000000000000000000, 1.821231995776179916E-16 ) ) ;
#75008 = DIRECTION ( 'NONE',  ( 1.000000000000000000, 0.000000000000000000, 0.000000000000000000 ) ) ;
#75009 = CARTESIAN_POINT ( 'NONE',  ( 98.38052710835017933, -41.69545545435574496, 131.7398046494048742 ) ) ;
#75010 = AXIS2_PLACEMENT_3D ( 'NONE', #60818, #74910, #12693 ) ;
#75011 = FACE_OUTER_BOUND ( 'NONE', #27889, .T. ) ;
#75012 = VERTEX_POINT ( 'NONE', #41144 ) ;
#75013 = CARTESIAN_POINT ( 'NONE',  ( 117.5190927476815119, -36.54584727635032237, 288.8413395616252615 ) ) ;
#75014 = CARTESIAN_POINT ( 'NONE',  ( 117.4907998085504062, -37.69205034685562339, 74.75276813305397638 ) ) ;
#75016 = DIRECTION ( 'NONE',  ( 0.000000000000000000, 1.000000000000000000, 0.000000000000000000 ) ) ;
#75015 = CARTESIAN_POINT ( 'NONE',  ( 86.06670390244796920, -58.72944715994110254, 10.91780685541499807 ) ) ;
#75017 = CARTESIAN_POINT ( 'NONE',  ( 97.81219807385008380, -40.51719912245609123, 147.6362401243850115 ) ) ;
#75018 = DIRECTION ( 'NONE',  ( 0.000000000000000000, 0.000000000000000000, 1.000000000000000000 ) ) ;
#75019 = ORIENTED_EDGE ( 'NONE', *, *, #66024, .T. ) ;
#75020 = EDGE_CURVE ( 'NONE', #56128, #15112, #53990, .T. ) ;
#75021 = CARTESIAN_POINT ( 'NONE',  ( 0.000000000000000000, 92.07499999999998863, 0.000000000000000000 ) ) ;
#75022 = EDGE_CURVE ( 'NONE', #23386, #28274, #32538, .T. ) ;
#75023 = CARTESIAN_POINT ( 'NONE',  ( 147.0667039024470739, -137.6786872052068134, 246.0480660933869785 ) ) ;
#75024 = CARTESIAN_POINT ( 'NONE',  ( 0.8391700603252211232, 69.85000000000000853, 118.5560000000000400 ) ) ;
#75025 = ORIENTED_EDGE ( 'NONE', *, *, #61073, .F. ) ;
#75026 = CARTESIAN_POINT ( 'NONE',  ( 107.1959452681378053, -26.26092741545045328, 35.06705384733893283 ) ) ;
#75027 = CARTESIAN_POINT ( 'NONE',  ( 97.52247766716473620, -32.48101032970659219, 96.99276813305395706 ) ) ;
#75028 = EDGE_CURVE ( 'NONE', #55721, #63478, #25736, .T. ) ;
#75029 = CIRCLE ( 'NONE', #85169, 3.250000000000002665 ) ;
#75030 = VECTOR ( 'NONE', #33603, 1000.000000000000000 ) ;
#75032 = LINE ( 'NONE', #40505, #76074 ) ;
#75031 = CARTESIAN_POINT ( 'NONE',  ( 97.81480632908598238, -40.51613010894325839, 171.6358981596145270 ) ) ;
#75033 = LINE ( 'NONE', #32334, #6016 ) ;
#75034 = VECTOR ( 'NONE', #8687, 1000.000000000000000 ) ;
#75035 = AXIS2_PLACEMENT_3D ( 'NONE', #188, #15167, #21996 ) ;
#75036 = AXIS2_PLACEMENT_3D ( 'NONE', #33846, #68377, #70162 ) ;
#75037 = CARTESIAN_POINT ( 'NONE',  ( 145.5844531081931166, -75.99209099266981582, 247.4783998280190076 ) ) ;
#75038 = ORIENTED_EDGE ( 'NONE', *, *, #70995, .F. ) ;
#75039 = CARTESIAN_POINT ( 'NONE',  ( 101.8448680821487642, -28.45912855063591351, 106.5241967044819944 ) ) ;
#75040 = EDGE_CURVE ( 'NONE', #28033, #78353, #27970, .T. ) ;
#75042 = VERTEX_POINT ( 'NONE', #70214 ) ;
#75041 = CARTESIAN_POINT ( 'NONE',  ( 11.59753438770549039, 87.72719248967439398, 130.0398859535097245 ) ) ;
#75043 = CARTESIAN_POINT ( 'NONE',  ( 99.76842024043818924, -29.31547782932927859, 221.6956252759109702 ) ) ;
#75044 = DIRECTION ( 'NONE',  ( 9.912705577010326536E-16, 1.000000000000000000, 0.000000000000000000 ) ) ;
#75045 = DIRECTION ( 'NONE',  ( -0.000000000000000000, -1.000000000000000000, -0.000000000000000000 ) ) ;
#75046 = ADVANCED_FACE ( 'NONE', ( #42042, #22977 ), #14815, .T. ) ;
#75047 = CARTESIAN_POINT ( 'NONE',  ( 19.56648329127400032, 0.2215528400590083269, 323.8756252759109202 ) ) ;
#75048 = CARTESIAN_POINT ( 'NONE',  ( 116.3212776292295842, -32.94146857471309886, 45.13562527591097506 ) ) ;
#75049 = CIRCLE ( 'NONE', #5421, 2.999999999999947153 ) ;
#75050 = FACE_OUTER_BOUND ( 'NONE', #29294, .T. ) ;
#75051 = CARTESIAN_POINT ( 'NONE',  ( -82.89895571708295563, 82.54999999999999716, 100.8594679592209644 ) ) ;
#75052 = VECTOR ( 'NONE', #64675, 1000.000000000000000 ) ;
#75053 = CARTESIAN_POINT ( 'NONE',  ( 108.8290724220007348, -27.07506712556656936, 164.9327681330539690 ) ) ;
#75054 = ORIENTED_EDGE ( 'NONE', *, *, #24046, .T. ) ;
#75055 = ORIENTED_EDGE ( 'NONE', *, *, #27144, .T. ) ;
#75056 = CARTESIAN_POINT ( 'NONE',  ( 103.0662520580798116, -44.63681263099613972, 123.6358690201829802 ) ) ;
#75057 = AXIS2_PLACEMENT_3D ( 'NONE', #83841, #62480, #42030 ) ;
#75058 = PLANE ( 'NONE',  #52941 ) ;
#75060 = CARTESIAN_POINT ( 'NONE',  ( 52.65249034007741358, -48.32844715994062312, 180.4678068554151196 ) ) ;
#75059 = CARTESIAN_POINT ( 'NONE',  ( 95.96284676697312932, -37.29622633765301032, 267.3670538473388092 ) ) ;
#75061 = CARTESIAN_POINT ( 'NONE',  ( 0.000000000000000000, 210.0000000000000000, 164.6557476874258441 ) ) ;
#75062 = CARTESIAN_POINT ( 'NONE',  ( 226.4410000000000025, 52.73749999999999716, -44.45000000000000284 ) ) ;
#75063 = PLANE ( 'NONE',  #74848 ) ;
#75064 = DIRECTION ( 'NONE',  ( 0.000000000000000000, -1.000000000000000000, 0.000000000000000000 ) ) ;
#75065 = LINE ( 'NONE', #66446, #26997 ) ;
#75066 = CARTESIAN_POINT ( 'NONE',  ( 116.3579325164319869, -41.40893824611053020, 203.4556252759109611 ) ) ;
#75067 = DIRECTION ( 'NONE',  ( 1.639958061481212836E-42, -4.100000000000000342E-29, -1.000000000000000000 ) ) ;
#75068 = ORIENTED_EDGE ( 'NONE', *, *, #71842, .T. ) ;
#75069 = ORIENTED_EDGE ( 'NONE', *, *, #15350, .F. ) ;
#75070 = CARTESIAN_POINT ( 'NONE',  ( -96.94335780202320052, 71.76234181793741129, -87.44698480207792102 ) ) ;
#75071 = CARTESIAN_POINT ( 'NONE',  ( 78.02982435611156120, -16.87939921900763096, 2.327894594457669886 ) ) ;
#75072 = CARTESIAN_POINT ( 'NONE',  ( 97.33789672108279944, -34.07083907252764021, 186.1152661070771046 ) ) ;
#75073 = DIRECTION ( 'NONE',  ( 1.000000000000000000, 4.163336342344333240E-14, 0.000000000000000000 ) ) ;
#75074 = AXIS2_PLACEMENT_3D ( 'NONE', #74251, #17931, #12025 ) ;
#75075 = CARTESIAN_POINT ( 'NONE',  ( 68.91674821478504498, 82.54999999999999716, -68.91674821478385127 ) ) ;
#75076 = ORIENTED_EDGE ( 'NONE', *, *, #89848, .F. ) ;
#75077 = DIRECTION ( 'NONE',  ( -1.000000000000000000, 0.000000000000000000, 0.000000000000000000 ) ) ;
#75078 = EDGE_CURVE ( 'NONE', #43367, #57559, #55425, .T. ) ;
#75079 = CARTESIAN_POINT ( 'NONE',  ( 113.0255487838780937, -46.03904575001691768, 218.0175300378159591 ) ) ;
#75080 = EDGE_LOOP ( 'NONE', ( #15060, #46562 ) ) ;
#75081 = CARTESIAN_POINT ( 'NONE',  ( -12.70000000000000107, 82.54999999999999716, 117.8738102209307641 ) ) ;
#75082 = FACE_OUTER_BOUND ( 'NONE', #44801, .T. ) ;
#75083 = CARTESIAN_POINT ( 'NONE',  ( -71.77848634863190114, 120.6499999999999915, 77.39114642429879609 ) ) ;
#75084 = CARTESIAN_POINT ( 'NONE',  ( 115.2453386458995652, -37.16432389609550313, 16.60237608387699026 ) ) ;
#75085 = CARTESIAN_POINT ( 'NONE',  ( 97.40507707138063154, -42.14631300639911160, 177.7451490854349743 ) ) ;
#75086 = DIRECTION ( 'NONE',  ( -4.237773401492740281E-14, 1.000000000000000000, 0.000000000000000000 ) ) ;
#75087 = VERTEX_POINT ( 'NONE', #35684 ) ;
#75088 = VECTOR ( 'NONE', #18238, 1000.000000000000000 ) ;
#75089 = PLANE ( 'NONE',  #65397 ) ;
#75090 = CARTESIAN_POINT ( 'NONE',  ( 109.3070416278940797, -46.56271945438447801, 67.75589170717483967 ) ) ;
#75091 = ORIENTED_EDGE ( 'NONE', *, *, #38001, .F. ) ;
#75092 = ORIENTED_EDGE ( 'NONE', *, *, #39639, .F. ) ;
#75093 = CONICAL_SURFACE ( 'NONE', #47528, 16.25000000000000000, 0.5235987755982992597 ) ;
#75094 = VECTOR ( 'NONE', #13821, 1000.000000000000000 ) ;
#75095 = CARTESIAN_POINT ( 'NONE',  ( 33.91903122894498779, -35.91149509761220315, -5.074374724088000832 ) ) ;
#75096 = ORIENTED_EDGE ( 'NONE', *, *, #59724, .T. ) ;
#75097 = ORIENTED_EDGE ( 'NONE', *, *, #63727, .T. ) ;
#75098 = PLANE ( 'NONE',  #6292 ) ;
#75099 = CARTESIAN_POINT ( 'NONE',  ( 106.9524907322914089, -28.15978509997144741, 59.50956268521995440 ) ) ;
#75100 = CARTESIAN_POINT ( 'NONE',  ( 99.52336843529489840, -29.45003914207232754, 250.7156252759109520 ) ) ;
#75101 = VECTOR ( 'NONE', #49355, 1000.000000000000000 ) ;
#75102 = CARTESIAN_POINT ( 'NONE',  ( 98.68348088377346983, -30.50934295487596515, 180.8184824187679567 ) ) ;
#75104 = CARTESIAN_POINT ( 'NONE',  ( 97.81168895331678925, -40.51742574516946860, 7.635625275910939536 ) ) ;
#75103 = CARTESIAN_POINT ( 'NONE',  ( 116.3148031259206192, -32.94054721833379062, 24.13562527591095375 ) ) ;
#75105 = CARTESIAN_POINT ( 'NONE',  ( 183.5150000000000148, 52.73749999999999716, -62.78087104677060637 ) ) ;
#75106 = DIRECTION ( 'NONE',  ( 2.999999999999999839E-15, -1.000000000000000000, 2.999999999999999900E-30 ) ) ;
#75107 = AXIS2_PLACEMENT_3D ( 'NONE', #68739, #50869, #37250 ) ;
#75108 = ADVANCED_FACE ( 'NONE', ( #62494 ), #8901, .T. ) ;
#75109 = VERTEX_POINT ( 'NONE', #7541 ) ;
#75110 = AXIS2_PLACEMENT_3D ( 'NONE', #1455, #539, #29152 ) ;
#75111 = CIRCLE ( 'NONE', #86729, 9.571100913904423635 ) ;
#75112 = AXIS2_PLACEMENT_3D ( 'NONE', #47762, #35039, #21885 ) ;
#75113 = DIRECTION ( 'NONE',  ( 0.9242245927363033076, 0.3818493186865917766, 0.000000000000000000 ) ) ;
#75114 = CARTESIAN_POINT ( 'NONE',  ( 118.1283360304583994, -32.34034571477864262, 249.1270538473389706 ) ) ;
#75115 = ORIENTED_EDGE ( 'NONE', *, *, #86746, .T. ) ;
#75116 = CARTESIAN_POINT ( 'NONE',  ( 110.1375194624030769, -26.11116931986236267, 214.8403871806729342 ) ) ;
#75117 = DIRECTION ( 'NONE',  ( 0.9999999853157766072, 0.0001713722456127401463, -9.999999853157767620E-16 ) ) ;
#75118 = CARTESIAN_POINT ( 'NONE',  ( -23.22008070988836792, 55.36727740576814938, 30.20659996360767252 ) ) ;
#75119 = EDGE_CURVE ( 'NONE', #31809, #9455, #42396, .T. ) ;
#75120 = CARTESIAN_POINT ( 'NONE',  ( 97.81280325506480722, -40.52014819707925852, 22.63585978562170453 ) ) ;
#75121 = CARTESIAN_POINT ( 'NONE',  ( -47.02966122971773189, 92.07499999999998863, -8.565507749926084753E-15 ) ) ;
#75123 = LINE ( 'NONE', #34224, #41304 ) ;
#75122 = CARTESIAN_POINT ( 'NONE',  ( 110.8530203762849169, -44.87085336317501572, 277.6356252759111953 ) ) ;
#75124 = CARTESIAN_POINT ( 'NONE',  ( 116.8171287662699456, -34.15293273489836423, 175.0314573698340439 ) ) ;
#75125 = DIRECTION ( 'NONE',  ( 0.9999999853157766072, 0.0001713722456127401463, -9.999999853157767620E-16 ) ) ;
#75126 = LINE ( 'NONE', #46048, #46978 ) ;
#75127 = CARTESIAN_POINT ( 'NONE',  ( 188.5667039024479834, -62.87844715994099687, 293.2178068554150627 ) ) ;
#75128 = CARTESIAN_POINT ( 'NONE',  ( 97.80889870804310249, -40.51851473143300097, 41.63518016758125384 ) ) ;
#75129 = ADVANCED_FACE ( 'NONE', ( #56106 ), #50652, .T. ) ;
#75130 = CARTESIAN_POINT ( 'NONE',  ( 112.1393456453461681, -28.01282278345784604, 75.65645860890421659 ) ) ;
#75132 = ORIENTED_EDGE ( 'NONE', *, *, #20417, .T. ) ;
#75131 = CARTESIAN_POINT ( 'NONE',  ( -12.61753767970230200, 84.21537865765682795, -117.8827776564338734 ) ) ;
#75133 = CARTESIAN_POINT ( 'NONE',  ( 136.8037680012526494, -19.00431460297267350, 6.768845952120934761 ) ) ;
#75134 = CARTESIAN_POINT ( 'NONE',  ( 100.6426946765138695, -44.96845825347062231, 232.0499109901969632 ) ) ;
#75135 = CARTESIAN_POINT ( 'NONE',  ( 117.3638278218041364, -38.35646377537064211, 109.7013395616249767 ) ) ;
#75136 = CARTESIAN_POINT ( 'NONE',  ( 99.30088202768328642, -28.79894053213705973, 266.7051490854347549 ) ) ;
#75137 = CARTESIAN_POINT ( 'NONE',  ( 51.23005224011598102, -33.89581943344511217, -5.074374724088000832 ) ) ;
#75138 = PLANE ( 'NONE',  #21463 ) ;
#75139 = VECTOR ( 'NONE', #68268, 1000.000000000000000 ) ;
#75141 = CARTESIAN_POINT ( 'NONE',  ( 89.10937460273895283, -56.62589376934769092, -5.074374724089016020 ) ) ;
#75140 = LINE ( 'NONE', #6544, #68148 ) ;
#75142 = PLANE ( 'NONE',  #39260 ) ;
#75143 = AXIS2_PLACEMENT_3D ( 'NONE', #82870, #34240, #60596 ) ;
#75144 = CARTESIAN_POINT ( 'NONE',  ( 131.5441285970359218, -19.82508440162534669, 2.797770139039466031 ) ) ;
#75145 = ORIENTED_EDGE ( 'NONE', *, *, #65870, .F. ) ;
#75146 = VERTEX_POINT ( 'NONE', #49751 ) ;
#75147 = CARTESIAN_POINT ( 'NONE',  ( 103.4202683135912650, -45.01906637089264507, 131.6571817328389784 ) ) ;
#75148 = EDGE_CURVE ( 'NONE', #57314, #38623, #13905, .T. ) ;
#75150 = ORIENTED_EDGE ( 'NONE', *, *, #15855, .T. ) ;
#75149 = CARTESIAN_POINT ( 'NONE',  ( 97.81252181335722184, -40.51708140359354360, 276.6353344664656220 ) ) ;
#75151 = CARTESIAN_POINT ( 'NONE',  ( 99.09566894039866725, -30.55048508729688095, 90.80073160410523769 ) ) ;
#75152 = CARTESIAN_POINT ( 'NONE',  ( 113.9719413768824126, -28.12837331961977938, 115.5261014663869474 ) ) ;
#75153 = CARTESIAN_POINT ( 'NONE',  ( 138.8664832912739939, -71.52944715994085811, 361.9756252759100335 ) ) ;
#75154 = ADVANCED_FACE ( 'NONE', ( #85211 ), #48844, .F. ) ;
#75155 = EDGE_CURVE ( 'NONE', #87961, #74344, #63397, .T. ) ;
#75156 = FACE_OUTER_BOUND ( 'NONE', #19875, .T. ) ;
#75157 = FACE_OUTER_BOUND ( 'NONE', #3011, .T. ) ;
#75158 = DIRECTION ( 'NONE',  ( 1.000000000000000078E-15, 1.000000000000000083E-30, -1.000000000000000000 ) ) ;
#75159 = EDGE_CURVE ( 'NONE', #30367, #71324, #14876, .T. ) ;
#75160 = AXIS2_PLACEMENT_3D ( 'NONE', #44486, #85424, #16804 ) ;
#75161 = CARTESIAN_POINT ( 'NONE',  ( 114.5308976578478735, -43.10096916487051288, 63.26419670448296984 ) ) ;
#75162 = ORIENTED_EDGE ( 'NONE', *, *, #52906, .F. ) ;
#75163 = VERTEX_POINT ( 'NONE', #77476 ) ;
#75164 = ORIENTED_EDGE ( 'NONE', *, *, #72850, .F. ) ;
#75165 = AXIS2_PLACEMENT_3D ( 'NONE', #61951, #69677, #35136 ) ;
#75166 = AXIS2_PLACEMENT_3D ( 'NONE', #59470, #2753, #51311 ) ;
#75167 = CARTESIAN_POINT ( 'NONE',  ( 114.0075790447407087, -33.88846322102013175, 9.635625275910941312 ) ) ;
#75168 =( BOUNDED_CURVE ( )  B_SPLINE_CURVE ( 2, ( #7895, #48762, #21083 ),
 .UNSPECIFIED., .F., .T. ) 
 B_SPLINE_CURVE_WITH_KNOTS ( ( 3, 3 ),
 ( 0.000000000000000000, 0.5053286420056790629 ),
 .UNSPECIFIED. ) 
 CURVE ( )  GEOMETRIC_REPRESENTATION_ITEM ( )  RATIONAL_B_SPLINE_CURVE ( ( 1.000000000000000000, 1.009299002520649857, 1.000420656333769864 ) ) 
 REPRESENTATION_ITEM ( '' )  );
#75170 = CARTESIAN_POINT ( 'NONE',  ( -479.3614999999999782, 104.7749999999999915, 101.5999999999999943 ) ) ;
#75169 = CARTESIAN_POINT ( 'NONE',  ( 113.8091913586853821, -43.81457933525486936, 154.1813395616249807 ) ) ;
#75171 = FACE_BOUND ( 'NONE', #21456, .T. ) ;
#75172 = DIRECTION ( 'NONE',  ( 0.000000000000000000, 0.000000000000000000, 1.000000000000000000 ) ) ;
#75173 = LINE ( 'NONE', #33832, #18433 ) ;
#75174 = AXIS2_PLACEMENT_3D ( 'NONE', #49241, #62881, #43779 ) ;
#75175 = CARTESIAN_POINT ( 'NONE',  ( 92.12450916458644201, 85.43299024555680887, 74.62309654709238771 ) ) ;
#75176 = DIRECTION ( 'NONE',  ( 0.000000000000000000, 0.000000000000000000, -1.000000000000000000 ) ) ;
#75177 = CARTESIAN_POINT ( 'NONE',  ( 108.5348814579965904, -26.43029805172848867, 104.9641967044819779 ) ) ;
#75178 = ORIENTED_EDGE ( 'NONE', *, *, #31166, .F. ) ;
#75179 = EDGE_LOOP ( 'NONE', ( #24122, #1887, #44358, #1434 ) ) ;
#75180 = ORIENTED_EDGE ( 'NONE', *, *, #62433, .T. ) ;
#75181 = AXIS2_PLACEMENT_3D ( 'NONE', #69251, #76057, #35613 ) ;
#75182 = CARTESIAN_POINT ( 'NONE',  ( 226.4410000000000025, 40.03750000000000142, 10.66800000000000104 ) ) ;
#75183 = CARTESIAN_POINT ( 'NONE',  ( 61.00843881761244347, 49.07499999999999574, -53.97512327982435210 ) ) ;
#75184 = AXIS2_PLACEMENT_3D ( 'NONE', #74050, #47222, #11831 ) ;
#75185 = AXIS2_PLACEMENT_3D ( 'NONE', #59015, #87199, #31771 ) ;
#75186 = CARTESIAN_POINT ( 'NONE',  ( 0.000000000000000000, 8.255000000000000782, 0.000000000000000000 ) ) ;
#75187 = CARTESIAN_POINT ( 'NONE',  ( 100.9764986820135420, -31.29420903488464845, 188.5652332267349607 ) ) ;
#75188 = EDGE_CURVE ( 'NONE', #60315, #81504, #56863, .T. ) ;
#75189 = CARTESIAN_POINT ( 'NONE',  ( 100.9551459015743262, -28.70665567104044058, 26.59337149677223877 ) ) ;
#75190 = ORIENTED_EDGE ( 'NONE', *, *, #81443, .F. ) ;
#75192 = ORIENTED_EDGE ( 'NONE', *, *, #33758, .T. ) ;
#75191 = ORIENTED_EDGE ( 'NONE', *, *, #52062, .F. ) ;
#75193 = CIRCLE ( 'NONE', #36029, 0.5000000000000004441 ) ;
#75194 = DIRECTION ( 'NONE',  ( 1.000000000000000000, 4.163336342344333240E-14, 0.000000000000000000 ) ) ;
#75195 = CARTESIAN_POINT ( 'NONE',  ( 136.6235172543038630, -19.74149216370141247, 2.839569540204845310 ) ) ;
#75196 = EDGE_LOOP ( 'NONE', ( #57980, #53225, #88922, #65656 ) ) ;
#75197 = ORIENTED_EDGE ( 'NONE', *, *, #37003, .F. ) ;
#75198 = CARTESIAN_POINT ( 'NONE',  ( 164.7812970173289955, -35.65087443492610930, -5.074374724088000832 ) ) ;
#75199 = CARTESIAN_POINT ( 'NONE',  ( 100.8499323319230854, -30.41416626502819298, 222.1272975916109544 ) ) ;
#75200 = CIRCLE ( 'NONE', #50552, 5.599999999999994316 ) ;
#75201 = FACE_OUTER_BOUND ( 'NONE', #58228, .T. ) ;
#75202 = CIRCLE ( 'NONE', #60655, 0.5000000000000004441 ) ;
#75203 = CARTESIAN_POINT ( 'NONE',  ( -121.5826742282154385, 74.35825521121780923, 47.56630412473074188 ) ) ;
#75204 = EDGE_LOOP ( 'NONE', ( #24170, #1116, #22150 ) ) ;
#75205 = ORIENTED_EDGE ( 'NONE', *, *, #28775, .F. ) ;
#75206 = EDGE_CURVE ( 'NONE', #47018, #27791, #62936, .T. ) ;
#75207 = CARTESIAN_POINT ( 'NONE',  ( 20.03715912545739997, -46.82818131006202123, 129.9678068554150627 ) ) ;
#75208 = VERTEX_POINT ( 'NONE', #69320 ) ;
#75209 = ORIENTED_EDGE ( 'NONE', *, *, #191, .F. ) ;
#75210 = EDGE_CURVE ( 'NONE', #66199, #10278, #23573, .T. ) ;
#75211 = CARTESIAN_POINT ( 'NONE',  ( 101.3402310731127329, -30.91225182618282830, 223.5138046553059894 ) ) ;
#75212 = EDGE_CURVE ( 'NONE', #83920, #76533, #3265, .T. ) ;
#75213 = CARTESIAN_POINT ( 'NONE',  ( 113.8578909311569305, -28.74413913138208088, 139.5156252759109634 ) ) ;
#75214 = CARTESIAN_POINT ( 'NONE',  ( 99.51750086509213133, -43.88776608678593760, 81.92991099019597812 ) ) ;
#75215 = CARTESIAN_POINT ( 'NONE',  ( 104.5384893572752958, -28.65942663403409441, 249.5838068554171514 ) ) ;
#75216 = CARTESIAN_POINT ( 'NONE',  ( 132.6459363690132705, -16.36767598606458307, 7.908804215160404993 ) ) ;
#75217 = FACE_OUTER_BOUND ( 'NONE', #5527, .T. ) ;
#75218 = CARTESIAN_POINT ( 'NONE',  ( 100.0081584303796944, -27.21027357624165788, 181.5841967044829630 ) ) ;
#75219 = FACE_OUTER_BOUND ( 'NONE', #52019, .T. ) ;
#75220 = VERTEX_POINT ( 'NONE', #70668 ) ;
#75221 = DIRECTION ( 'NONE',  ( 0.7071067811865969777, -0.7071067811864980568, 0.000000000000000000 ) ) ;
#75223 = VERTEX_POINT ( 'NONE', #84758 ) ;
#75222 = EDGE_CURVE ( 'NONE', #19595, #3377, #76583, .T. ) ;
#75224 = AXIS2_PLACEMENT_3D ( 'NONE', #37590, #38460, #80277 ) ;
#75225 = ADVANCED_FACE ( 'NONE', ( #14365 ), #24738, .F. ) ;
#75226 = ORIENTED_EDGE ( 'NONE', *, *, #68961, .F. ) ;
#75227 = DIRECTION ( 'NONE',  ( 0.000000000000000000, -1.000000000000000000, 0.000000000000000000 ) ) ;
#75228 = ORIENTED_EDGE ( 'NONE', *, *, #21279, .F. ) ;
#75229 = EDGE_CURVE ( 'NONE', #48612, #1618, #16594, .T. ) ;
#75230 = AXIS2_PLACEMENT_3D ( 'NONE', #15510, #77280, #35934 ) ;
#75231 = FACE_OUTER_BOUND ( 'NONE', #82673, .T. ) ;
#75232 = AXIS2_PLACEMENT_3D ( 'NONE', #28714, #62775, #62332 ) ;
#75233 = CARTESIAN_POINT ( 'NONE',  ( 112.5143773164265184, -27.84083190490108706, 94.63848241876793566 ) ) ;
#75234 = CARTESIAN_POINT ( 'NONE',  ( -8.597104536545209896, 73.19917002513419391, 130.2727017199365775 ) ) ;
#75235 = EDGE_CURVE ( 'NONE', #64226, #11834, #10653, .T. ) ;
#75236 = CARTESIAN_POINT ( 'NONE',  ( 0.000000000000000000, 20.32000000000000028, 0.000000000000000000 ) ) ;
#75237 = DIRECTION ( 'NONE',  ( 0.000000000000000000, 0.000000000000000000, 1.000000000000000000 ) ) ;
#75240 = CARTESIAN_POINT ( 'NONE',  ( 117.4525030917817645, -36.13006561810995976, 224.8727681330539667 ) ) ;
#75239 = CYLINDRICAL_SURFACE ( 'NONE', #70260, 4.762500000000002842 ) ;
#75238 = CARTESIAN_POINT ( 'NONE',  ( 98.30753418359370244, -41.72887547895405902, 142.7397919414705427 ) ) ;
#75241 = LINE ( 'NONE', #47947, #42278 ) ;
#75242 = CARTESIAN_POINT ( 'NONE',  ( 140.0667039024470455, -118.2784471599408960, 45.21780685541799727 ) ) ;
#75243 = VERTEX_POINT ( 'NONE', #51095 ) ;
#75244 = AXIS2_PLACEMENT_3D ( 'NONE', #8622, #83138, #69943 ) ;
#75245 = EDGE_CURVE ( 'NONE', #78242, #28246, #4300, .T. ) ;
#75246 = LINE ( 'NONE', #47952, #50038 ) ;
#75247 = CARTESIAN_POINT ( 'NONE',  ( 88.17226027475679473, -58.72944715994100306, 239.5838068554174924 ) ) ;
#75248 = ADVANCED_FACE ( 'NONE', ( #66511, #80169 ), #44722, .F. ) ;
#75249 = CIRCLE ( 'NONE', #60763, 4.750000000000004441 ) ;
#75250 = CARTESIAN_POINT ( 'NONE',  ( 48.85858412958099706, -30.08671355700241179, -5.074374724088000832 ) ) ;
#75252 = VERTEX_POINT ( 'NONE', #65183 ) ;
#75251 = CARTESIAN_POINT ( 'NONE',  ( 107.2500105196458549, -24.83007258495691616, 230.0641967044819580 ) ) ;
#75253 = CARTESIAN_POINT ( 'NONE',  ( 102.3835747273358550, -27.86123704493403963, 195.4630013769998982 ) ) ;
#75254 = CARTESIAN_POINT ( 'NONE',  ( 99.76212870471702843, -44.21728614272981872, 17.96133956162493206 ) ) ;
#75255 = CARTESIAN_POINT ( 'NONE',  ( 101.9507351169249887, -46.57965624409947480, 163.1832443235299763 ) ) ;
#75256 = CARTESIAN_POINT ( 'NONE',  ( 179.1667039024473809, -26.71338133338671739, 313.9678068554149490 ) ) ;
#75257 = CARTESIAN_POINT ( 'NONE',  ( 97.70650136287245857, -40.25115876428171191, 102.6128377541471650 ) ) ;
#75259 = CARTESIAN_POINT ( 'NONE',  ( 152.0368932755770857, -23.42844715993588522, 249.9678068554149490 ) ) ;
#75258 = CYLINDRICAL_SURFACE ( 'NONE', #78289, 7.937500000000000000 ) ;
#75260 = FACE_OUTER_BOUND ( 'NONE', #31213, .T. ) ;
#75261 = CARTESIAN_POINT ( 'NONE',  ( -15.89999999999999680, 53.97500000000000142, 30.79999999999999361 ) ) ;
#75262 = VERTEX_POINT ( 'NONE', #37481 ) ;
#75263 = EDGE_LOOP ( 'NONE', ( #28116, #65891, #19635, #83266 ) ) ;
#75264 = EDGE_LOOP ( 'NONE', ( #73640, #3669, #53419, #88652 ) ) ;
#75265 = AXIS2_PLACEMENT_3D ( 'NONE', #72652, #73528, #24501 ) ;
#75266 = EDGE_CURVE ( 'NONE', #36163, #89471, #36603, .T. ) ;
#75267 = ORIENTED_EDGE ( 'NONE', *, *, #56966, .F. ) ;
#75268 = CARTESIAN_POINT ( 'NONE',  ( 130.5667039024470455, -104.2784471599409386, 24.21780685541800082 ) ) ;
#75269 = CARTESIAN_POINT ( 'NONE',  ( 99.08262072259969955, -44.34008189452608661, 32.92038718067297509 ) ) ;
#75270 = CARTESIAN_POINT ( 'NONE',  ( 112.3535505598876654, -140.6782308490354296, 246.2059492953349888 ) ) ;
#75271 = EDGE_CURVE ( 'NONE', #5447, #74330, #78834, .T. ) ;
#75272 = ADVANCED_FACE ( 'NONE', ( #2962 ), #58362, .T. ) ;
#75273 = CARTESIAN_POINT ( 'NONE',  ( 145.4199999577330402, -139.2838544871431168, 246.0004081004534555 ) ) ;
#75275 = ADVANCED_FACE ( 'NONE', ( #45163 ), #56993, .F. ) ;
#75274 = CARTESIAN_POINT ( 'NONE',  ( 107.0664832912750057, -36.72944715993903486, 0.4256252759109709349 ) ) ;
#75276 = CARTESIAN_POINT ( 'NONE',  ( 114.8173571680961231, -40.38677627709480333, 227.8981341137909453 ) ) ;
#75277 = ORIENTED_EDGE ( 'NONE', *, *, #73503, .F. ) ;
#75278 = EDGE_LOOP ( 'NONE', ( #22390, #57781, #88130, #21443 ) ) ;
#75279 = VERTEX_POINT ( 'NONE', #71570 ) ;
#75280 = DIRECTION ( 'NONE',  ( -2.999999999999999839E-15, 1.000000000000000000, -2.999999999999999900E-30 ) ) ;
#75281 = CARTESIAN_POINT ( 'NONE',  ( 101.9936758543545636, -45.44610597658563478, 102.1565380991941652 ) ) ;
#75282 = LINE ( 'NONE', #47991, #9185 ) ;
#75283 = FACE_OUTER_BOUND ( 'NONE', #64079, .T. ) ;
#75284 = CARTESIAN_POINT ( 'NONE',  ( 184.5667039024485518, -48.82844715993447693, 180.4678068554150343 ) ) ;
#75285 = DIRECTION ( 'NONE',  ( 1.000000000000000000, 4.163336342344333240E-14, 0.000000000000000000 ) ) ;
#75286 = CARTESIAN_POINT ( 'NONE',  ( 109.8085987287837497, -27.34093086507531112, 259.8499109901970314 ) ) ;
#75287 = DIRECTION ( 'NONE',  ( 0.000000000000000000, 1.000000000000000000, 0.000000000000000000 ) ) ;
#75288 = EDGE_LOOP ( 'NONE', ( #15151, #15830, #38882, #70407 ) ) ;
#75289 = AXIS2_PLACEMENT_3D ( 'NONE', #88662, #39587, #32781 ) ;
#75290 = CARTESIAN_POINT ( 'NONE',  ( 194.0371591254584587, -46.82818131005407736, 193.9678068554150343 ) ) ;
#75291 = B_SPLINE_CURVE_WITH_KNOTS ( 'NONE', 3,
 ( #56590, #22540, #50671, #43852, #42061, #14834 ),
 .UNSPECIFIED., .F., .F.,
 ( 4, 2, 4 ),
 ( -0.009166911786111989549, -0.004585838005518491980, 0.000000000000000000 ),
 .UNSPECIFIED. ) ;
#75292 = DIRECTION ( 'NONE',  ( -0.000000000000000000, -0.000000000000000000, 1.000000000000000000 ) ) ;
#75293 = CARTESIAN_POINT ( 'NONE',  ( 113.4874516948114547, -42.53221286317273098, 81.07189989340096758 ) ) ;
#75294 = AXIS2_PLACEMENT_3D ( 'NONE', #32134, #73475, #58940 ) ;
#75295 = VECTOR ( 'NONE', #15883, 1000.000000000000000 ) ;
#75296 = CARTESIAN_POINT ( 'NONE',  ( 109.7231921452033276, -27.00035804852990751, 129.8649303482066273 ) ) ;
#75297 = CARTESIAN_POINT ( 'NONE',  ( 165.6738106836207578, -26.00627455218829809, 313.9678068554149490 ) ) ;
#75298 = CARTESIAN_POINT ( 'NONE',  ( 115.0889047237290157, -30.61763667965946212, 44.34395860927426014 ) ) ;
#75299 = ORIENTED_EDGE ( 'NONE', *, *, #21739, .F. ) ;
#75300 = CIRCLE ( 'NONE', #85506, 1.999999999999995781 ) ;
#75301 = CARTESIAN_POINT ( 'NONE',  ( 91.06648329127391150, -36.72944715993925513, -4.074374724089044442 ) ) ;
#75302 = EDGE_LOOP ( 'NONE', ( #19797, #62062, #80136, #49006, #53615, #67472 ) ) ;
#75303 = CARTESIAN_POINT ( 'NONE',  ( 96.67071733825032709, -35.94615501309311156, 146.2670538473399517 ) ) ;
#75304 = VERTEX_POINT ( 'NONE', #65624 ) ;
#75305 = LINE ( 'NONE', #25807, #72133 ) ;
#75306 = CARTESIAN_POINT ( 'NONE',  ( 108.9267623252842441, -45.42435897675616019, 104.1758690201829722 ) ) ;
#75307 = CARTESIAN_POINT ( 'NONE',  ( -44.45000000000000284, 50.79999999999999716, 257.1750000000000114 ) ) ;
#75308 = VECTOR ( 'NONE', #48738, 1000.000000000000000 ) ;
#75309 = CARTESIAN_POINT ( 'NONE',  ( -31.75000000000000000, 104.3431970271541900, 3.174999999999779998 ) ) ;
#75310 = CARTESIAN_POINT ( 'NONE',  ( 96.93562038266055936, -32.25163268508860881, 51.98324432352996638 ) ) ;
#75311 = DIRECTION ( 'NONE',  ( -1.000000000000000078E-15, 0.000000000000000000, 1.000000000000000000 ) ) ;
#75312 = EDGE_LOOP ( 'NONE', ( #17171, #16948, #84947, #8972 ) ) ;
#75313 = CARTESIAN_POINT ( 'NONE',  ( -118.2594037030539198, 73.00424585431356661, -8.387096233283337199 ) ) ;
#75314 = EDGE_LOOP ( 'NONE', ( #23605, #31879, #73468, #18455, #4140, #74421 ) ) ;
#75316 = EDGE_CURVE ( 'NONE', #85451, #52659, #72886, .T. ) ;
#75315 = VERTEX_POINT ( 'NONE', #38807 ) ;
#75317 = ADVANCED_FACE ( 'NONE', ( #59684 ), #87416, .T. ) ;
#75318 = VECTOR ( 'NONE', #7307, 1000.000000000000000 ) ;
#75319 = EDGE_CURVE ( 'NONE', #4943, #64884, #52403, .T. ) ;
#75320 = FACE_BOUND ( 'NONE', #625, .T. ) ;
#75321 = ORIENTED_EDGE ( 'NONE', *, *, #35, .F. ) ;
#75322 = CARTESIAN_POINT ( 'NONE',  ( 109.7813264909552515, -47.51098736074730766, 242.7727681330539724 ) ) ;
#75323 = CARTESIAN_POINT ( 'NONE',  ( 97.98816800684205930, -30.38363046389439859, 156.8289586092439549 ) ) ;
#75324 = CARTESIAN_POINT ( 'NONE',  ( -6.802569982901797644E-16, 69.84999999999999432, -118.5560000000000116 ) ) ;
#75325 = PLANE ( 'NONE',  #66323 ) ;
#75326 = CARTESIAN_POINT ( 'NONE',  ( 101.7559735582952953, -27.03550746236556890, 96.46324432352997746 ) ) ;
#75327 = DIRECTION ( 'NONE',  ( -1.000000000000000000, -4.510281037539694659E-14, 0.000000000000000000 ) ) ;
#75328 = VERTEX_POINT ( 'NONE', #57916 ) ;
#75329 = DIRECTION ( 'NONE',  ( 0.7071067811873675835, 0.7071067811857274510, 7.071067811873668640E-16 ) ) ;
#75330 = EDGE_CURVE ( 'NONE', #56272, #84121, #37924, .T. ) ;
#75331 = PRODUCT ( 'Pneumatic Workpiece Fixture Plate', 'Pneumatic Workpiece Fixture Plate', '', ( #82197 ) ) ;
#75332 = LINE ( 'NONE', #40351, #78198 ) ;
#75334 = ORIENTED_EDGE ( 'NONE', *, *, #27032, .F. ) ;
#75333 = CONICAL_SURFACE ( 'NONE', #36177, 9.571100913904395213, 0.7853981633974522758 ) ;
#75335 = EDGE_CURVE ( 'NONE', #78380, #31104, #86537, .T. ) ;
#75336 = FACE_OUTER_BOUND ( 'NONE', #22042, .T. ) ;
#75337 = CARTESIAN_POINT ( 'NONE',  ( 87.06648329127403940, -46.72944715994105280, -4.824374724089049771 ) ) ;
#75338 = CARTESIAN_POINT ( 'NONE',  ( 111.7637953458032172, -46.71243375810367837, 287.9146728949587555 ) ) ;
#75339 = DIRECTION ( 'NONE',  ( -0.7071067811578587436, 0.7071067812152364018, 0.000000000000000000 ) ) ;
#75340 = CARTESIAN_POINT ( 'NONE',  ( 33.96670390244661775, -28.27351298637442056, 117.4678068554150485 ) ) ;
#75341 = CARTESIAN_POINT ( 'NONE',  ( 108.3355664562415939, -46.73461849300061743, 92.67825729137430812 ) ) ;
#75342 = CARTESIAN_POINT ( 'NONE',  ( 111.8651074766111861, -28.16866562884735004, 34.66991099019695355 ) ) ;
#75344 = CARTESIAN_POINT ( 'NONE',  ( 117.8527506973082524, -39.03601561205230297, 104.6708633711489824 ) ) ;
#75343 = DIRECTION ( 'NONE',  ( 0.000000000000000000, 0.000000000000000000, -1.000000000000000000 ) ) ;
#75345 = DIRECTION ( 'NONE',  ( 0.7071067811865067165, 0.7071067811865883179, 7.071067811865061181E-16 ) ) ;
#75346 = CARTESIAN_POINT ( 'NONE',  ( 116.7015053437751959, -40.82493444377960401, 168.5070538473399608 ) ) ;
#75347 = CARTESIAN_POINT ( 'NONE',  ( 125.0664851986225159, -56.47944715994101728, 14.92562527591098842 ) ) ;
#75348 = VERTEX_POINT ( 'NONE', #38359 ) ;
#75349 = FACE_OUTER_BOUND ( 'NONE', #45014, .T. ) ;
#75350 = CARTESIAN_POINT ( 'NONE',  ( 107.0664832912739968, 0.2215528400590013880, 168.9256252759119832 ) ) ;
#75351 = CARTESIAN_POINT ( 'NONE',  ( 136.1684221027065576, -34.94667169167191645, 2.376609173399411912 ) ) ;
#75352 = VERTEX_POINT ( 'NONE', #66059 ) ;
#75353 = EDGE_CURVE ( 'NONE', #3666, #47532, #40977, .T. ) ;
#75354 = VECTOR ( 'NONE', #48182, 1000.000000000000000 ) ;
#75355 = DIRECTION ( 'NONE',  ( -0.7071067811869841124, 0.7071067811861110330, 0.000000000000000000 ) ) ;
#75357 = EDGE_LOOP ( 'NONE', ( #67724, #54116, #29371, #40448 ) ) ;
#75356 = CARTESIAN_POINT ( 'NONE',  ( 117.7240352459720043, -39.83258586197658246, 138.5889586092439743 ) ) ;
#75358 = CARTESIAN_POINT ( 'NONE',  ( 141.0667039024479834, -58.35344715994099829, 310.9178068554150514 ) ) ;
#75359 = CARTESIAN_POINT ( 'NONE',  ( -130.5461193570662317, 95.14808745951974345, -1.659440300507330157 ) ) ;
#75360 = LINE ( 'NONE', #68096, #18396 ) ;
#75361 = EDGE_CURVE ( 'NONE', #47693, #49032, #12013, .T. ) ;
#75363 = DIRECTION ( 'NONE',  ( 0.000000000000000000, -1.000000000000000000, 0.000000000000000000 ) ) ;
#75362 = VECTOR ( 'NONE', #7411, 1000.000000000000000 ) ;
#75364 = VERTEX_POINT ( 'NONE', #75582 ) ;
#75365 = VECTOR ( 'NONE', #29295, 1000.000000000000000 ) ;
#75366 = SHAPE_DEFINITION_REPRESENTATION ( #40083, #14421 ) ;
#75367 = VERTEX_POINT ( 'NONE', #19271 ) ;
#75368 = ORIENTED_EDGE ( 'NONE', *, *, #48277, .F. ) ;
#75369 = VECTOR ( 'NONE', #77521, 1000.000000000000000 ) ;
#75370 = ORIENTED_EDGE ( 'NONE', *, *, #83229, .F. ) ;
#75371 = CARTESIAN_POINT ( 'NONE',  ( 106.1656040943334602, -121.2545485715093463, -19.18411693322849487 ) ) ;
#75372 = LINE ( 'NONE', #12246, #15654 ) ;
#75373 = CARTESIAN_POINT ( 'NONE',  ( 107.0664832912739968, -36.72944715994100306, 287.6356252759109680 ) ) ;
#75374 = COLOUR_RGB ( '', 0.08235294, 0.09019608, 0.10196078) ;
#75375 = CARTESIAN_POINT ( 'NONE',  ( 63.03715912545736444, -24.42818131006027826, 237.4678068554150059 ) ) ;
#75376 = CIRCLE ( 'NONE', #29019, 118.5560000000000116 ) ;
#75379 = EDGE_CURVE ( 'NONE', #54417, #6675, #40140, .T. ) ;
#75378 = CARTESIAN_POINT ( 'NONE',  ( 19.56670390244796920, -67.87844715994100397, 310.9178068554150514 ) ) ;
#75377 = FACE_OUTER_BOUND ( 'NONE', #12462, .T. ) ;
#75380 = CARTESIAN_POINT ( 'NONE',  ( 97.79833369891507289, -40.48465503131496490, 181.6328088241103274 ) ) ;
#75381 = ORIENTED_EDGE ( 'NONE', *, *, #34304, .F. ) ;
#75382 = ORIENTED_EDGE ( 'NONE', *, *, #2430, .F. ) ;
#75383 = AXIS2_PLACEMENT_3D ( 'NONE', #66878, #46416, #11477 ) ;
#75384 = DIRECTION ( 'NONE',  ( 4.299999999999999979E-14, -1.000000000000000000, 4.400000000000000367E-29 ) ) ;
#75385 = DIRECTION ( 'NONE',  ( 9.351236661543306751E-17, -3.725950533538267725E-29, -1.000000000000000000 ) ) ;
#75386 = CARTESIAN_POINT ( 'NONE',  ( 101.0525363619397581, -44.44280425155404401, 228.0499109901959400 ) ) ;
#75387 = VECTOR ( 'NONE', #46152, 1000.000000000000000 ) ;
#75389 = ORIENTED_EDGE ( 'NONE', *, *, #24879, .F. ) ;
#75388 = DIRECTION ( 'NONE',  ( 0.000000000000000000, 0.000000000000000000, -1.000000000000000000 ) ) ;
#75390 = B_SPLINE_CURVE_WITH_KNOTS ( 'NONE', 3,
 ( #1462, #545, #55937, #28244, #83682, #43666, #70046, #63677, #35504, #63226, #28707, #77760, #15083, #21907, #49575, #56842, #84588, #70955, #8728, #1902, #59518, #30941, #30055, #2801, #36864, #38201 ),
 .UNSPECIFIED., .F., .F.,
 ( 4, 2, 2, 2, 2, 2, 2, 2, 2, 2, 2, 2, 4 ),
 ( 0.01971520310360850431, 0.02094683101846679663, 0.02217845893332509241, 0.02464171476304167704, 0.02587334267789997283, 0.02710497059275826515, 0.02956822642247482896, 0.03203148225219139278, 0.03326311016704969203, 0.03449473808190799129, 0.03695799391162458980, 0.03818962182648288906, 0.03942124974134118831 ),
 .UNSPECIFIED. ) ;
#75391 = CARTESIAN_POINT ( 'NONE',  ( 99.36524671511907059, -42.81259845621065807, 87.85848241876792031 ) ) ;
#75392 = PLANE ( 'NONE',  #53004 ) ;
#75393 = FACE_OUTER_BOUND ( 'NONE', #85834, .T. ) ;
#75394 = CARTESIAN_POINT ( 'NONE',  ( 103.2777341875169554, -27.47496823152900802, 21.38569241147085620 ) ) ;
#75395 = ORIENTED_EDGE ( 'NONE', *, *, #72266, .T. ) ;
#75396 = EDGE_CURVE ( 'NONE', #46111, #296, #25628, .T. ) ;
#75397 = DIRECTION ( 'NONE',  ( 0.000000000000000000, 1.000000000000000000, 2.000000000000000155E-15 ) ) ;
#75398 = EDGE_LOOP ( 'NONE', ( #83190, #30988, #7314, #72151 ) ) ;
#75399 = VERTEX_POINT ( 'NONE', #82408 ) ;
#75400 = CIRCLE ( 'NONE', #79762, 218.1859999999999786 ) ;
#75401 = CARTESIAN_POINT ( 'NONE',  ( 106.6421946519922983, -45.61100719954815474, 243.9701547344679682 ) ) ;
#75402 = ADVANCED_FACE ( 'NONE', ( #46945 ), #54645, .F. ) ;
#75403 = DIRECTION ( 'NONE',  ( 1.000000000000000000, 4.163336342344333240E-14, 0.000000000000000000 ) ) ;
#75404 = CARTESIAN_POINT ( 'NONE',  ( 115.0885484784128465, -30.61717473208839735, 139.3440046732524138 ) ) ;
#75405 = DIRECTION ( 'NONE',  ( 0.000000000000000000, 1.000000000000000000, 0.000000000000000000 ) ) ;
#75406 = CARTESIAN_POINT ( 'NONE',  ( 81.36878785332568498, -39.15209318185590348, 1.893168666199420924 ) ) ;
#75407 = ORIENTED_EDGE ( 'NONE', *, *, #51162, .T. ) ;
#75408 = VECTOR ( 'NONE', #18295, 1000.000000000000000 ) ;
#75409 = DIRECTION ( 'NONE',  ( 0.000000000000000000, -1.000000000000000000, 0.000000000000000000 ) ) ;
#75410 = CARTESIAN_POINT ( 'NONE',  ( 115.7817158473913253, -41.80465924930165755, 184.4068246429673366 ) ) ;
#75411 = EDGE_LOOP ( 'NONE', ( #8115, #64259 ) ) ;
#75412 = CARTESIAN_POINT ( 'NONE',  ( 109.6430426817424433, -46.83134659365198615, 47.77562527591094721 ) ) ;
#75413 = ORIENTED_EDGE ( 'NONE', *, *, #51140, .T. ) ;
#75414 = CARTESIAN_POINT ( 'NONE',  ( 113.5315931691687439, -43.38514287343249265, 266.0080903695914003 ) ) ;
#75415 = VECTOR ( 'NONE', #89677, 1000.000000000000000 ) ;
#75416 = CARTESIAN_POINT ( 'NONE',  ( 274.0659999999999741, 40.03750000000000142, -58.73749999999999716 ) ) ;
#75417 = CARTESIAN_POINT ( 'NONE',  ( 117.0231039428183522, -39.62849705588583760, 138.5889586092449690 ) ) ;
#75418 = CARTESIAN_POINT ( 'NONE',  ( 23.75871628398702384, 82.54999999999999716, 307.6575000000000273 ) ) ;
#75419 = DIRECTION ( 'NONE',  ( 0.000000000000000000, 0.000000000000000000, -1.000000000000000000 ) ) ;
#75420 = DIRECTION ( 'NONE',  ( -4.237773401492740281E-14, 1.000000000000000000, 0.000000000000000000 ) ) ;
#75421 = CARTESIAN_POINT ( 'NONE',  ( 7.208983637501106934, 72.09427944926730447, 130.3568028842946092 ) ) ;
#75422 = CARTESIAN_POINT ( 'NONE',  ( 117.5342389965484386, -35.85531600229182914, 249.8927681330537780 ) ) ;
#75423 = FACE_OUTER_BOUND ( 'NONE', #85638, .T. ) ;
#75424 = AXIS2_PLACEMENT_3D ( 'NONE', #79378, #37136, #58451 ) ;
#75425 = EDGE_LOOP ( 'NONE', ( #50342, #45130, #35520, #57192 ) ) ;
#75426 = CARTESIAN_POINT ( 'NONE',  ( 113.9455412938869330, -28.01876065682782624, 120.5565776568639507 ) ) ;
#75427 = CARTESIAN_POINT ( 'NONE',  ( 120.3165253744671759, 47.81691361759333603, -50.68368231966687887 ) ) ;
#75428 = EDGE_LOOP ( 'NONE', ( #40126, #77003, #22475, #52655 ) ) ;
#75430 = EDGE_CURVE ( 'NONE', #15550, #82481, #68763, .T. ) ;
#75429 = ORIENTED_EDGE ( 'NONE', *, *, #57171, .F. ) ;
#75432 = ORIENTED_EDGE ( 'NONE', *, *, #63647, .F. ) ;
#75431 = ADVANCED_FACE ( 'NONE', ( #81069 ), #19709, .F. ) ;
#75433 = CIRCLE ( 'NONE', #81288, 1.000000000000000888 ) ;
#75434 = EDGE_CURVE ( 'NONE', #85626, #29697, #54048, .T. ) ;
#75435 = DIRECTION ( 'NONE',  ( 0.000000000000000000, 0.000000000000000000, 1.000000000000000000 ) ) ;
#75436 = CYLINDRICAL_SURFACE ( 'NONE', #16694, 3.968749999999992895 ) ;
#75437 =( GEOMETRIC_REPRESENTATION_CONTEXT ( 3 ) GLOBAL_UNCERTAINTY_ASSIGNED_CONTEXT ( ( #15133 ) ) GLOBAL_UNIT_ASSIGNED_CONTEXT ( ( #74466, #33128, #31781 ) ) REPRESENTATION_CONTEXT ( 'NONE', 'WORKASPACE' ) );
#75438 = LINE ( 'NONE', #84049, #180 ) ;
#75439 = FACE_OUTER_BOUND ( 'NONE', #27511, .T. ) ;
#75440 = CARTESIAN_POINT ( 'NONE',  ( 112.8577109034250583, -30.29807625619018197, 157.3233284648299559 ) ) ;
#75441 = CARTESIAN_POINT ( 'NONE',  ( 97.54012738755939438, -43.81963713510241121, 257.8356252759109566 ) ) ;
#75442 = CARTESIAN_POINT ( 'NONE',  ( 99.50452936416800753, -43.30555000397543353, 57.89599405887542360 ) ) ;
#75443 = ORIENTED_EDGE ( 'NONE', *, *, #10316, .T. ) ;
#75444 = EDGE_CURVE ( 'NONE', #80913, #32309, #18817, .T. ) ;
#75445 = AXIS2_PLACEMENT_3D ( 'NONE', #18586, #46266, #74001 ) ;
#75446 = DIRECTION ( 'NONE',  ( 0.000000000000000000, 0.000000000000000000, -1.000000000000000000 ) ) ;
#75447 = ORIENTED_EDGE ( 'NONE', *, *, #62105, .T. ) ;
#75448 = ORIENTED_EDGE ( 'NONE', *, *, #75637, .F. ) ;
#75449 = EDGE_CURVE ( 'NONE', #39918, #14767, #6530, .T. ) ;
#75450 = CARTESIAN_POINT ( 'NONE',  ( 173.9900000000000091, 52.73749999999999716, -62.78087104677060637 ) ) ;
#75451 = ORIENTED_EDGE ( 'NONE', *, *, #76222, .T. ) ;
#75452 = ORIENTED_EDGE ( 'NONE', *, *, #36168, .T. ) ;
#75453 = DIRECTION ( 'NONE',  ( -2.999999999999999839E-15, 1.000000000000000000, -2.999999999999999900E-30 ) ) ;
#75454 = DIRECTION ( 'NONE',  ( 1.000000000000000078E-15, -1.000000000000000083E-30, -1.000000000000000000 ) ) ;
#75455 = LINE ( 'NONE', #49509, #84017 ) ;
#75456 = DIRECTION ( 'NONE',  ( -1.000000000000000078E-15, 0.000000000000000000, -1.000000000000000000 ) ) ;
#75457 = ADVANCED_FACE ( 'NONE', ( #88768 ), #32885, .T. ) ;
#75458 = VECTOR ( 'NONE', #87409, 1000.000000000000000 ) ;
#75459 = CARTESIAN_POINT ( 'NONE',  ( 98.52747904795083400, -36.52563780154032003, 195.7295626852199462 ) ) ;
#75460 = CARTESIAN_POINT ( 'NONE',  ( 117.1340566916381789, -32.05431620389533265, 59.16038718067295576 ) ) ;
#75461 = DIRECTION ( 'NONE',  ( 1.000000000000000000, 0.000000000000000000, 0.000000000000000000 ) ) ;
#75462 = ORIENTED_EDGE ( 'NONE', *, *, #30467, .F. ) ;
#75463 = CARTESIAN_POINT ( 'NONE',  ( -79.20758933349353015, 71.53193882405241766, -88.21655330423251939 ) ) ;
#75464 = EDGE_LOOP ( 'NONE', ( #73184, #45581, #33761, #19769, #61265 ) ) ;
#75465 = CARTESIAN_POINT ( 'NONE',  ( 87.17003668186664811, -54.68655584847640228, 14.92562527591100618 ) ) ;
#75466 = ORIENTED_EDGE ( 'NONE', *, *, #50855, .T. ) ;
#75467 = CARTESIAN_POINT ( 'NONE',  ( 115.5207272689788027, -31.29719706063076856, 165.2807688001713018 ) ) ;
#75468 = CARTESIAN_POINT ( 'NONE',  ( 124.4804366973139622, -125.9844606681579364, 250.2203867545810283 ) ) ;
#75469 = FACE_OUTER_BOUND ( 'NONE', #80458, .T. ) ;
#75470 = CIRCLE ( 'NONE', #36301, 2.500000000000002220 ) ;
#75471 = CARTESIAN_POINT ( 'NONE',  ( -487.2989999999999782, 89.53805401447711176, 3.968750000000410338 ) ) ;
#75472 = ORIENTED_EDGE ( 'NONE', *, *, #578, .T. ) ;
#75473 = CARTESIAN_POINT ( 'NONE',  ( 112.7537747436706184, -27.22417719680832704, 54.65943479971996055 ) ) ;
#75475 = DIRECTION ( 'NONE',  ( 1.000000000000000000, 0.000000000000000000, -0.000000000000000000 ) ) ;
#75474 = DIRECTION ( 'NONE',  ( 1.000000000000000000, 0.000000000000000000, 0.000000000000000000 ) ) ;
#75476 = FACE_OUTER_BOUND ( 'NONE', #55046, .T. ) ;
#75477 = CARTESIAN_POINT ( 'NONE',  ( 131.5918432679227408, -17.51852171454203244, 2.740177351677692830 ) ) ;
#75478 = ORIENTED_EDGE ( 'NONE', *, *, #26118, .F. ) ;
#75479 = AXIS2_PLACEMENT_3D ( 'NONE', #6908, #84128, #77300 ) ;
#75480 = CARTESIAN_POINT ( 'NONE',  ( 97.06871944863306112, -35.59214294076518570, 122.2351737579207054 ) ) ;
#75481 = DIRECTION ( 'NONE',  ( -0.7071067811865490160, 0.7071067811865461294, 0.000000000000000000 ) ) ;
#75483 = DIRECTION ( 'NONE',  ( -1.000000000000000000, -3.360405532702990443E-14, 0.000000000000000000 ) ) ;
#75482 = VECTOR ( 'NONE', #62397, 1000.000000000000000 ) ;
#75484 = ORIENTED_EDGE ( 'NONE', *, *, #34458, .F. ) ;
#75485 = CARTESIAN_POINT ( 'NONE',  ( 113.3277443033378376, -28.32255675095946046, 100.5670538473389684 ) ) ;
#75488 = EDGE_CURVE ( 'NONE', #18807, #5538, #34226, .T. ) ;
#75487 = DIRECTION ( 'NONE',  ( 4.299999999999999979E-14, -1.000000000000000000, 4.400000000000000367E-29 ) ) ;
#75486 = CARTESIAN_POINT ( 'NONE',  ( 0.000000000000000000, 92.07499999999998863, 0.000000000000000000 ) ) ;
#75489 = CARTESIAN_POINT ( 'NONE',  ( 28.57499999999999929, 87.13271776169258942, 310.8325000000000387 ) ) ;
#75490 = VECTOR ( 'NONE', #50882, 1000.000000000000114 ) ;
#75491 = DIRECTION ( 'NONE',  ( 0.000000000000000000, 0.000000000000000000, -1.000000000000000000 ) ) ;
#75492 = VERTEX_POINT ( 'NONE', #39257 ) ;
#75493 = CARTESIAN_POINT ( 'NONE',  ( 107.9488082096507213, -26.98745991040269487, 151.0041967044819557 ) ) ;
#75494 = VECTOR ( 'NONE', #56767, 1000.000000000000000 ) ;
#75496 = ORIENTED_EDGE ( 'NONE', *, *, #67321, .F. ) ;
#75495 = DIRECTION ( 'NONE',  ( -0.7071067811865453523, -0.7071067811865496822, 0.000000000000000000 ) ) ;
#75497 = CARTESIAN_POINT ( 'NONE',  ( 99.41296134609930846, -28.78668791560525975, 261.6746728949588032 ) ) ;
#75498 = CARTESIAN_POINT ( 'NONE',  ( 156.5667039024483813, -48.82844715993569196, 257.2178068554149490 ) ) ;
#75499 = CARTESIAN_POINT ( 'NONE',  ( -31.27367473141074683, 54.97499999999996589, 74.45358409497265484 ) ) ;
#75500 = CARTESIAN_POINT ( 'NONE',  ( 90.44969454456439450, -53.34645651782491882, 249.5838068554174640 ) ) ;
#75501 = FACE_OUTER_BOUND ( 'NONE', #2477, .T. ) ;
#75502 = CARTESIAN_POINT ( 'NONE',  ( 68.80307738653738170, -139.4148206440312947, 246.0960064844549890 ) ) ;
#75503 = CARTESIAN_POINT ( 'NONE',  ( -100.8082743238001200, 80.89704698943971550, 82.96136257730093178 ) ) ;
#75504 = MECHANICAL_DESIGN_GEOMETRIC_PRESENTATION_REPRESENTATION (  '', ( #2820 ), #85704 ) ;
#75505 = CARTESIAN_POINT ( 'NONE',  ( 103.9298229712113653, -26.84510867568817716, 205.3089586092449679 ) ) ;
#75506 = ORIENTED_EDGE ( 'NONE', *, *, #68136, .F. ) ;
#75507 = ORIENTED_EDGE ( 'NONE', *, *, #56785, .F. ) ;
#75508 = CARTESIAN_POINT ( 'NONE',  ( 98.25403324269851169, -37.66165033158306130, 122.8415833058969469 ) ) ;
#75509 = ADVANCED_FACE ( 'NONE', ( #52839 ), #46498, .T. ) ;
#75510 = CARTESIAN_POINT ( 'NONE',  ( 160.0667039024470171, -79.67844715994088745, 96.96780685541800437 ) ) ;
#75512 = LINE ( 'NONE', #5581, #4175 ) ;
#75511 = CARTESIAN_POINT ( 'NONE',  ( 115.2782656938782821, -32.16401669718150202, 25.67396425827794815 ) ) ;
#75513 = DIRECTION ( 'NONE',  ( -1.042183321081676705E-15, -1.000000000000000000, 0.000000000000000000 ) ) ;
#75514 = VECTOR ( 'NONE', #16771, 1000.000000000000000 ) ;
#75515 = PLANE ( 'NONE',  #69284 ) ;
#75516 = CARTESIAN_POINT ( 'NONE',  ( 33.91903122894498779, -35.91149509761220315, -5.074374724088000832 ) ) ;
#75517 = AXIS2_PLACEMENT_3D ( 'NONE', #75489, #13260, #40946 ) ;
#75518 = CARTESIAN_POINT ( 'NONE',  ( 100.9546728069516917, -28.70702573053221585, 106.5939586096738054 ) ) ;
#75519 = DIRECTION ( 'NONE',  ( -0.9254794337955620787, -0.3787978585227822492, 0.000000000000000000 ) ) ;
#75520 = CARTESIAN_POINT ( 'NONE',  ( 96.69582475441069391, -35.54038568221476879, 206.2356252759109623 ) ) ;
#75521 = DIRECTION ( 'NONE',  ( -1.825781832977094422E-16, 0.4999999999999998890, 0.8660254037844387076 ) ) ;
#75522 = ORIENTED_EDGE ( 'NONE', *, *, #10565, .F. ) ;
#75523 = ORIENTED_EDGE ( 'NONE', *, *, #89219, .T. ) ;
#75524 = CARTESIAN_POINT ( 'NONE',  ( -91.12742965731001732, 69.93364840292896645, -93.49502539975229354 ) ) ;
#75525 = FACE_OUTER_BOUND ( 'NONE', #84729, .T. ) ;
#75526 = CARTESIAN_POINT ( 'NONE',  ( 116.7956972015441863, -39.38580969979880564, 124.6137336630641812 ) ) ;
#75527 = CARTESIAN_POINT ( 'NONE',  ( 248.6659999999999968, 52.73749999999999716, 10.66800000000000104 ) ) ;
#75528 = VECTOR ( 'NONE', #29493, 1000.000000000000000 ) ;
#75529 = DIRECTION ( 'NONE',  ( -0.7071067811865794361, 0.7071067811865157093, -7.071067811865803697E-16 ) ) ;
#75530 = ORIENTED_EDGE ( 'NONE', *, *, #55309, .F. ) ;
#75531 = CARTESIAN_POINT ( 'NONE',  ( 104.4070190479019118, -46.45777198906507977, 62.36470280596612525 ) ) ;
#75532 = CARTESIAN_POINT ( 'NONE',  ( 112.2051334037466432, -45.80035149650004200, 212.9870538473389558 ) ) ;
#75534 = ORIENTED_EDGE ( 'NONE', *, *, #3664, .T. ) ;
#75533 = EDGE_CURVE ( 'NONE', #67060, #37287, #88326, .T. ) ;
#75535 = EDGE_CURVE ( 'NONE', #49587, #87146, #54198, .T. ) ;
#75536 = CARTESIAN_POINT ( 'NONE',  ( -4.446177000103011423, 94.34669717174053005, 118.4732138684817215 ) ) ;
#75537 = DIRECTION ( 'NONE',  ( 0.000000000000000000, 0.000000000000000000, -1.000000000000000000 ) ) ;
#75538 = ADVANCED_FACE ( 'NONE', ( #87863 ), #61480, .F. ) ;
#75539 = CARTESIAN_POINT ( 'NONE',  ( 115.9631861912839241, -41.36764275679356473, 168.4441829924387264 ) ) ;
#75540 = CIRCLE ( 'NONE', #36389, 6.647542495715439870 ) ;
#75541 = CARTESIAN_POINT ( 'NONE',  ( 116.2870986197744969, -35.69205421237206366, 81.73380465530594563 ) ) ;
#75542 = CARTESIAN_POINT ( 'NONE',  ( 114.9815172128508465, -29.91112648151817410, 180.3927681330539770 ) ) ;
#75543 = VECTOR ( 'NONE', #88567, 1000.000000000000000 ) ;
#75544 = CIRCLE ( 'NONE', #11935, 10.00000000000000888 ) ;
#75545 = CARTESIAN_POINT ( 'NONE',  ( 80.06648281188265059, -39.47944715903999224, 8.225259175037734849 ) ) ;
#75546 = ORIENTED_EDGE ( 'NONE', *, *, #55726, .F. ) ;
#75547 = EDGE_CURVE ( 'NONE', #11858, #87811, #68314, .T. ) ;
#75548 = FACE_OUTER_BOUND ( 'NONE', #37551, .T. ) ;
#75549 = CARTESIAN_POINT ( 'NONE',  ( 105.4091548812398855, -46.67577557997189786, 67.44613915122781123 ) ) ;
#75550 = VERTEX_POINT ( 'NONE', #26979 ) ;
#75552 = ORIENTED_EDGE ( 'NONE', *, *, #31463, .F. ) ;
#75551 = CIRCLE ( 'NONE', #88656, 9.525000000000000355 ) ;
#75553 = CARTESIAN_POINT ( 'NONE',  ( 12.37521547983011239, 85.43365698736771208, 117.9083787315452270 ) ) ;
#75554 = EDGE_LOOP ( 'NONE', ( #8838, #62449, #79681, #62233 ) ) ;
#75555 = VERTEX_POINT ( 'NONE', #61931 ) ;
#75556 = DIRECTION ( 'NONE',  ( 0.000000000000000000, -1.000000000000000000, 0.000000000000000000 ) ) ;
#75557 = EDGE_CURVE ( 'NONE', #19483, #21921, #80613, .T. ) ;
#75558 = CARTESIAN_POINT ( 'NONE',  ( 114.4871815801477624, -30.46814820527590228, 73.80670554236196779 ) ) ;
#75559 = CIRCLE ( 'NONE', #36402, 4.762500000000002842 ) ;
#75560 = CARTESIAN_POINT ( 'NONE',  ( 116.9463234969885974, -41.73785994705047386, 248.4651490854349731 ) ) ;
#75561 = CARTESIAN_POINT ( 'NONE',  ( 115.3705510513157861, -30.46277945167181045, 219.3413395616249773 ) ) ;
#75563 = CARTESIAN_POINT ( 'NONE',  ( 113.7560087186648730, -29.08427257552855494, 285.5032443235299979 ) ) ;
#75562 = CYLINDRICAL_SURFACE ( 'NONE', #49014, 3.000000000000002665 ) ;
#75564 = DIRECTION ( 'NONE',  ( 0.000000000000000000, 0.000000000000000000, -1.000000000000000000 ) ) ;
#75565 = CARTESIAN_POINT ( 'NONE',  ( -141.3509999999999991, 0.000000000000000000, 132.7150000000000034 ) ) ;
#75566 = CARTESIAN_POINT ( 'NONE',  ( 181.8884939055940038, -32.11662333284530746, -5.074374724088000832 ) ) ;
#75567 = VECTOR ( 'NONE', #88974, 1000.000000000000000 ) ;
#75568 = EDGE_LOOP ( 'NONE', ( #18740, #553 ) ) ;
#75569 = ORIENTED_EDGE ( 'NONE', *, *, #79631, .T. ) ;
#75570 = CARTESIAN_POINT ( 'NONE',  ( 114.7041265136728612, -43.74408836545399737, 78.22324432353094892 ) ) ;
#75571 = CARTESIAN_POINT ( 'NONE',  ( 96.74811198265052781, -38.50085326290480481, 91.46133956162493917 ) ) ;
#75572 = CARTESIAN_POINT ( 'NONE',  ( 97.18209604296552584, -40.28622700274314639, 266.6013395616253661 ) ) ;
#75573 = ORIENTED_EDGE ( 'NONE', *, *, #9397, .F. ) ;
#75574 = CARTESIAN_POINT ( 'NONE',  ( 116.8576245982602870, -40.31003124190988274, 218.5470538473399529 ) ) ;
#75575 = CARTESIAN_POINT ( 'NONE',  ( 172.5664832912740110, -32.07844715994070839, 198.9256252759119832 ) ) ;
#75576 = CARTESIAN_POINT ( 'NONE',  ( 141.8664832912729992, -71.52944715994142655, 352.4506252759077825 ) ) ;
#75577 = CARTESIAN_POINT ( 'NONE',  ( 118.5256205435843100, -36.72944715994100306, 309.2406250056037038 ) ) ;
#75578 = CARTESIAN_POINT ( 'NONE',  ( 100.8961411191535973, 127.0000000000000000, 3.968750000000400124 ) ) ;
#75580 = FACE_BOUND ( 'NONE', #13871, .T. ) ;
#75579 = CARTESIAN_POINT ( 'NONE',  ( 111.6409576225383802, -30.15385841292844304, 277.6356252759107974 ) ) ;
#75581 = CARTESIAN_POINT ( 'NONE',  ( 112.0657623353423560, -45.48848379642200257, 173.9897783938763780 ) ) ;
#75582 = CARTESIAN_POINT ( 'NONE',  ( 160.5667039024426970, -48.82844715994099971, 249.9678068554149775 ) ) ;
#75583 = DIRECTION ( 'NONE',  ( 1.000000000000000000, 0.000000000000000000, 0.000000000000000000 ) ) ;
#75584 = CIRCLE ( 'NONE', #24804, 2.517499999999998739 ) ;
#75585 = LINE ( 'NONE', #82860, #3696 ) ;
#75586 = DIRECTION ( 'NONE',  ( 1.907762142705490052E-15, 7.167082501179359715E-16, -1.000000000000000000 ) ) ;
#75587 = VECTOR ( 'NONE', #74806, 1000.000000000000000 ) ;
#75588 = DIRECTION ( 'NONE',  ( 0.000000000000000000, 0.000000000000000000, 1.000000000000000000 ) ) ;
#75590 = VERTEX_POINT ( 'NONE', #42819 ) ;
#75589 = CARTESIAN_POINT ( 'NONE',  ( -9.261585182541612227, 239.0000000000000000, 152.5407914452011369 ) ) ;
#75591 = DIRECTION ( 'NONE',  ( 0.9999999853157766072, 0.0001713722456134972175, 0.000000000000000000 ) ) ;
#75592 = CARTESIAN_POINT ( 'NONE',  ( 100.8099727397313217, -45.87009904342127697, 242.1108633711489517 ) ) ;
#75593 = CARTESIAN_POINT ( 'NONE',  ( 117.5808906079046352, -33.32045621506634347, 130.0880062282919880 ) ) ;
#75594 = CARTESIAN_POINT ( 'NONE',  ( 97.18271318096459765, -40.28600493293344442, 262.6013395616255934 ) ) ;
#75595 = B_SPLINE_CURVE_WITH_KNOTS ( 'NONE', 3,
 ( #61856, #9480, #22680, #37192, #64007, #29482, #50353, #57165, #85808, #70825, #64896, #30377, #9050, #36749, #36297, #57622, #78092, #15859, #43982, #15417, #64448, #89593, #78982, #72162, #41412, #51241, #8600, #82790, #6907, #84468 ),
 .UNSPECIFIED., .F., .F.,
 ( 4, 2, 2, 2, 1, 2, 2, 2, 2, 2, 2, 2, 1, 2, 2, 4 ),
 ( 0.000000000000000000, 0.1250000000000416889, 0.1875000000000625333, 0.2187500000000721367, 0.2343750000000751343, 0.2421875000000783817, 0.2500000000000816014, 0.3750000000000487943, 0.4375000000000323630, 0.5000000000000159872, 0.6249999999999775735, 0.6874999999999630296, 0.7187499999999547029, 0.7343749999999505951, 0.7499999999999464873, 1.000000000000000000 ),
 .UNSPECIFIED. ) ;
#75596 = CARTESIAN_POINT ( 'NONE',  ( 180.2143765759489895, -35.91149509761070391, 342.9256252759119548 ) ) ;
#75597 = AXIS2_PLACEMENT_3D ( 'NONE', #8776, #22853, #15130 ) ;
#75600 = ADVANCED_FACE ( 'NONE', ( #28302 ), #49187, .T. ) ;
#75599 = CARTESIAN_POINT ( 'NONE',  ( 83.73314995794039817, 12.92155284005802685, 349.2756252759109543 ) ) ;
#75598 = DIRECTION ( 'NONE',  ( -1.000000000000000000, 0.000000000000000000, -3.491483361109379305E-15 ) ) ;
#75601 = PLANE ( 'NONE',  #33490 ) ;
#75602 = CYLINDRICAL_SURFACE ( 'NONE', #89232, 2.030000000001807248 ) ;
#75603 = CIRCLE ( 'NONE', #20488, 12.99999999999999822 ) ;
#75604 = EDGE_CURVE ( 'NONE', #14208, #37970, #59837, .T. ) ;
#75605 = ORIENTED_EDGE ( 'NONE', *, *, #56651, .T. ) ;
#75606 = ORIENTED_EDGE ( 'NONE', *, *, #72673, .F. ) ;
#75607 = CARTESIAN_POINT ( 'NONE',  ( 97.43556672503765981, -37.99919831760565359, 150.8524198280769895 ) ) ;
#75609 = ORIENTED_EDGE ( 'NONE', *, *, #19345, .T. ) ;
#75608 = CARTESIAN_POINT ( 'NONE',  ( -71.09939861440099662, 0.000000000000000000, 177.8662485265279827 ) ) ;
#75610 = CARTESIAN_POINT ( 'NONE',  ( 115.0888006782553248, -30.61750168745167855, 89.34348336381457045 ) ) ;
#75611 = CARTESIAN_POINT ( 'NONE',  ( 114.4473569665853603, -28.53271593493113301, 155.5051490854349652 ) ) ;
#75612 = FACE_OUTER_BOUND ( 'NONE', #23591, .T. ) ;
#75613 = CARTESIAN_POINT ( 'NONE',  ( -55.89999999999999858, 55.97500000000000142, 70.79999999999999716 ) ) ;
#75614 = CIRCLE ( 'NONE', #8908, 2.117000000000007987 ) ;
#75615 = CARTESIAN_POINT ( 'NONE',  ( -78.16952835488679341, 72.45860812971083931, 89.13771950014329093 ) ) ;
#75616 = CARTESIAN_POINT ( 'NONE',  ( 48.85858412958099706, -30.08671355700241179, -5.074374724088000832 ) ) ;
#75617 = CARTESIAN_POINT ( 'NONE',  ( 106.1376555893193228, -47.80867374849579221, 112.5099109901969712 ) ) ;
#75618 = ORIENTED_EDGE ( 'NONE', *, *, #53482, .T. ) ;
#75619 = EDGE_LOOP ( 'NONE', ( #24048, #81123, #54246, #13966 ) ) ;
#75621 = VERTEX_POINT ( 'NONE', #83293 ) ;
#75620 = CIRCLE ( 'NONE', #6051, 1.000000000000000888 ) ;
#75622 = EDGE_CURVE ( 'NONE', #52976, #1304, #26527, .T. ) ;
#75623 = CARTESIAN_POINT ( 'NONE',  ( 46.48091746482131015, -48.32844715994084339, 249.9678068554150343 ) ) ;
#75625 = CARTESIAN_POINT ( 'NONE',  ( 70.06695561434436570, -140.6784471599409869, 245.4721420304120159 ) ) ;
#75624 = CARTESIAN_POINT ( 'NONE',  ( 98.64540312569894809, -41.76920806142280185, 157.7556252759109725 ) ) ;
#75626 = CARTESIAN_POINT ( 'NONE',  ( 63.06670390244794078, -40.32844715994017548, 300.4678068554150627 ) ) ;
#75627 = CYLINDRICAL_SURFACE ( 'NONE', #4544, 5.499999999999999112 ) ;
#75628 = VECTOR ( 'NONE', #81393, 1000.000000000000000 ) ;
#75629 = DIRECTION ( 'NONE',  ( -0.9254794337955620787, -0.3787978585227822492, 0.000000000000000000 ) ) ;
#75630 = DIRECTION ( 'NONE',  ( 3.999999999999999995E-14, -1.000000000000000000, 4.100000000000000342E-29 ) ) ;
#75631 = LINE ( 'NONE', #88373, #42919 ) ;
#75632 = CARTESIAN_POINT ( 'NONE',  ( 100.3128846869252726, -46.43702735306955276, 87.09276813305393716 ) ) ;
#75633 = EDGE_LOOP ( 'NONE', ( #43072, #39473, #31295, #33649, #21586, #65448 ) ) ;
#75634 = VERTEX_POINT ( 'NONE', #41925 ) ;
#75635 = CIRCLE ( 'NONE', #65503, 4.750000000000004441 ) ;
#75636 = VERTEX_POINT ( 'NONE', #83741 ) ;
#75637 = EDGE_CURVE ( 'NONE', #14474, #10702, #86005, .T. ) ;
#75638 = CARTESIAN_POINT ( 'NONE',  ( 107.0667039024479834, -36.72944715994099596, 239.5838068554170093 ) ) ;
#75639 = CARTESIAN_POINT ( 'NONE',  ( -91.13664476550682991, 95.14808745951974345, -93.48344774443309291 ) ) ;
#75640 = FACE_OUTER_BOUND ( 'NONE', #18790, .T. ) ;
#75641 = CARTESIAN_POINT ( 'NONE',  ( 115.2258025850914862, -39.61500320815195408, 176.3861856076869685 ) ) ;
#75642 = CARTESIAN_POINT ( 'NONE',  ( 25.56670390244748248, -48.82844715994178841, 137.2178068554150627 ) ) ;
#75643 = ORIENTED_EDGE ( 'NONE', *, *, #28796, .F. ) ;
#75645 = ORIENTED_EDGE ( 'NONE', *, *, #28736, .T. ) ;
#75644 = EDGE_LOOP ( 'NONE', ( #56342, #23340, #66081, #45485 ) ) ;
#75646 = FACE_OUTER_BOUND ( 'NONE', #30009, .T. ) ;
#75647 = VECTOR ( 'NONE', #44956, 1000.000000000000000 ) ;
#75648 = PLANE ( 'NONE',  #4170 ) ;
#75649 = ORIENTED_EDGE ( 'NONE', *, *, #64093, .T. ) ;
#75650 = EDGE_LOOP ( 'NONE', ( #14272, #64762, #68051, #67498 ) ) ;
#75651 = DIRECTION ( 'NONE',  ( 0.000000000000000000, 0.000000000000000000, -1.000000000000000000 ) ) ;
#75652 = ADVANCED_FACE ( 'NONE', ( #35117 ), #55094, .T. ) ;
#75653 = CARTESIAN_POINT ( 'NONE',  ( 106.4165995140572250, -45.56720307917569102, 218.9501547344689527 ) ) ;
#75654 = VERTEX_POINT ( 'NONE', #76467 ) ;
#75655 = AXIS2_PLACEMENT_3D ( 'NONE', #40489, #13242, #6865 ) ;
#75656 = DIRECTION ( 'NONE',  ( 0.8660254037844392627, -0.4999999999999990008, 1.549999999999999706E-14 ) ) ;
#75657 = CARTESIAN_POINT ( 'NONE',  ( -115.3679503581490309, 71.85924980799624961, 61.11881860259094879 ) ) ;
#75658 = ORIENTED_EDGE ( 'NONE', *, *, #3684, .T. ) ;
#75659 = ORIENTED_EDGE ( 'NONE', *, *, #33890, .T. ) ;
#75660 = CARTESIAN_POINT ( 'NONE',  ( 213.4642805167760002, 52.73749999999999716, -44.45000000000000284 ) ) ;
#75661 = ORIENTED_EDGE ( 'NONE', *, *, #61345, .F. ) ;
#75662 = VERTEX_POINT ( 'NONE', #20615 ) ;
#75663 = ADVANCED_FACE ( 'NONE', ( #84646 ), #62380, .T. ) ;
#75664 = CARTESIAN_POINT ( 'NONE',  ( 97.84965203270614609, -37.79993896977983070, 234.2366617981629702 ) ) ;
#75665 = CARTESIAN_POINT ( 'NONE',  ( 102.3504518276437523, -46.05175434220414132, 127.2041967044829960 ) ) ;
#75666 = CARTESIAN_POINT ( 'NONE',  ( 116.9011659702704264, -33.23038410113876040, 114.0984824187679720 ) ) ;
#75667 = CARTESIAN_POINT ( 'NONE',  ( 105.8091682078810294, -28.24967526344544311, 249.5838068554170377 ) ) ;
#75668 = ADVANCED_FACE ( 'NONE', ( #28773 ), #21972, .T. ) ;
#75669 = DIRECTION ( 'NONE',  ( 1.000000000000000000, 4.299999999999999979E-14, 1.000000000000000078E-15 ) ) ;
#75670 = CARTESIAN_POINT ( 'NONE',  ( 107.5657681238088941, -47.77139876010166830, 188.6003871806729535 ) ) ;
#75671 = CARTESIAN_POINT ( 'NONE',  ( 106.1656040943334318, -87.30234574837474781, -19.18411693322955003 ) ) ;
#75672 = ORIENTED_EDGE ( 'NONE', *, *, #84160, .F. ) ;
#75673 = CARTESIAN_POINT ( 'NONE',  ( 130.3267157422428113, 72.47310549519059464, 7.740869983443941393 ) ) ;
#75674 = EDGE_LOOP ( 'NONE', ( #64018, #57937, #68853, #3912 ) ) ;
#75675 = CIRCLE ( 'NONE', #35061, 2.517500000000000071 ) ;
#75676 = ORIENTED_EDGE ( 'NONE', *, *, #20497, .T. ) ;
#75677 = CARTESIAN_POINT ( 'NONE',  ( 188.5667039024483245, -42.82844715993430640, 170.7178068554150059 ) ) ;
#75678 = VERTEX_POINT ( 'NONE', #69656 ) ;
#75679 = AXIS2_PLACEMENT_3D ( 'NONE', #53088, #12245, #85551 ) ;
#75680 = DIRECTION ( 'NONE',  ( 1.000000000000000000, 8.953411488912556626E-16, 0.000000000000000000 ) ) ;
#75681 = CARTESIAN_POINT ( 'NONE',  ( 97.26623355869948284, -31.61728591124570542, 90.93181575210196854 ) ) ;
#75682 = CARTESIAN_POINT ( 'NONE',  ( -10.07588608733909119, 74.81633509576083441, 130.1668266806610177 ) ) ;
#75683 = CARTESIAN_POINT ( 'NONE',  ( 107.0664832912739968, 12.92155284005902516, 336.6506252759110112 ) ) ;
#75684 = CARTESIAN_POINT ( 'NONE',  ( -40.89999999999999858, 53.97500000000000142, 60.79999999999999716 ) ) ;
#75687 = CARTESIAN_POINT ( 'NONE',  ( 98.05565822401628395, -44.38798742045805312, 222.8870538473399563 ) ) ;
#75686 = DIRECTION ( 'NONE',  ( 0.000000000000000000, 1.000000000000000000, 0.000000000000000000 ) ) ;
#75685 = DIRECTION ( 'NONE',  ( -0.4999999999999932832, 0.8660254037844424824, 0.000000000000000000 ) ) ;
#75688 = DIRECTION ( 'NONE',  ( 0.000000000000000000, 1.000000000000000000, 0.000000000000000000 ) ) ;
#75689 = DIRECTION ( 'NONE',  ( 5.512527431108029424E-15, -1.000000000000000000, 0.000000000000000000 ) ) ;
#75690 = VERTEX_POINT ( 'NONE', #48283 ) ;
#75691 = AXIS2_PLACEMENT_3D ( 'NONE', #65724, #52515, #79387 ) ;
#75692 = CARTESIAN_POINT ( 'NONE',  ( 107.0667039024467186, -36.72944715994091069, 195.5838068554169809 ) ) ;
#75693 = DIRECTION ( 'NONE',  ( 0.7071067811864661934, 0.7071067811866289521, 7.071067811864966518E-16 ) ) ;
#75694 = CARTESIAN_POINT ( 'NONE',  ( 82.81648329127399677, -18.72944715994105636, -5.074374724089055100 ) ) ;
#75695 = VECTOR ( 'NONE', #6202, 1000.000000000000000 ) ;
#75696 = LINE ( 'NONE', #12573, #56360 ) ;
#75698 = VERTEX_POINT ( 'NONE', #7425 ) ;
#75697 = CARTESIAN_POINT ( 'NONE',  ( 95.24515967180828113, -38.10243856675759133, 236.4184824187679510 ) ) ;
#75699 = CARTESIAN_POINT ( 'NONE',  ( 72.06648329127401098, -45.72944715994106701, 14.92562527591093691 ) ) ;
#75700 = CARTESIAN_POINT ( 'NONE',  ( 99.66888285774223277, -46.01973906766702527, 122.0413395616249659 ) ) ;
#75701 = CARTESIAN_POINT ( 'NONE',  ( 105.9884228536615609, -26.36024887173286757, 46.15848241876796720 ) ) ;
#75702 = CARTESIAN_POINT ( 'NONE',  ( 117.8238795360118445, -33.99523349031771602, 165.0365776568629315 ) ) ;
#75703 = FACE_OUTER_BOUND ( 'NONE', #74758, .T. ) ;
#75704 = DIRECTION ( 'NONE',  ( 1.000000000000000000, 0.000000000000000000, -9.299908063537909262E-17 ) ) ;
#75706 = CARTESIAN_POINT ( 'NONE',  ( 23.75871628398702384, 82.54999999999999716, 307.6575000000000273 ) ) ;
#75705 = CARTESIAN_POINT ( 'NONE',  ( -186.2398777604659870, 0.000000000000000000, 107.9500000000000028 ) ) ;
#75707 = DIRECTION ( 'NONE',  ( 4.299999999999999979E-14, -1.000000000000000000, 4.400000000000000367E-29 ) ) ;
#75708 = CARTESIAN_POINT ( 'NONE',  ( 44.45000000000000284, 50.79999999999999716, 275.4630000000000223 ) ) ;
#75709 = VERTEX_POINT ( 'NONE', #14700 ) ;
#75710 = ORIENTED_EDGE ( 'NONE', *, *, #12679, .T. ) ;
#75711 = VERTEX_POINT ( 'NONE', #77364 ) ;
#75712 = AXIS2_PLACEMENT_3D ( 'NONE', #73342, #51985, #10670 ) ;
#75713 = ORIENTED_EDGE ( 'NONE', *, *, #82913, .F. ) ;
#75714 = DIRECTION ( 'NONE',  ( 0.000000000000000000, 0.000000000000000000, 1.000000000000000000 ) ) ;
#75715 = CARTESIAN_POINT ( 'NONE',  ( 99.16013801855510224, -43.49098322490559809, 27.88991099019694175 ) ) ;
#75716 = DIRECTION ( 'NONE',  ( 4.299999999999999979E-14, -1.000000000000000000, 4.400000000000000367E-29 ) ) ;
#75717 = LINE ( 'NONE', #13487, #16630 ) ;
#75718 = CARTESIAN_POINT ( 'NONE',  ( 110.7536356736639220, -105.8297479413476054, 2.217806855418058554 ) ) ;
#75719 = VECTOR ( 'NONE', #52636, 1000.000000000000000 ) ;
#75720 = CARTESIAN_POINT ( 'NONE',  ( 104.8198721574821803, -27.95645401395800533, 244.7105150661719790 ) ) ;
#75721 = VERTEX_POINT ( 'NONE', #21517 ) ;
#75722 = VERTEX_POINT ( 'NONE', #64191 ) ;
#75723 = ORIENTED_EDGE ( 'NONE', *, *, #32291, .T. ) ;
#75724 = EDGE_CURVE ( 'NONE', #73753, #41873, #45373, .T. ) ;
#75725 = LINE ( 'NONE', #26666, #26859 ) ;
#75726 = CARTESIAN_POINT ( 'NONE',  ( 115.0374107822371030, -42.90826833801408213, 103.3020634734001391 ) ) ;
#75727 = CARTESIAN_POINT ( 'NONE',  ( 165.2725846195380086, -35.55794170701810941, 342.9256252759119548 ) ) ;
#75728 = DIRECTION ( 'NONE',  ( 0.000000000000000000, -1.000000000000000000, 0.000000000000000000 ) ) ;
#75729 = CARTESIAN_POINT ( 'NONE',  ( 104.0667030381800942, -67.87844715994094713, 155.9678077345870122 ) ) ;
#75730 = LINE ( 'NONE', #83009, #79228 ) ;
#75731 = ADVANCED_FACE ( 'NONE', ( #36027 ), #30877, .F. ) ;
#75732 = CARTESIAN_POINT ( 'NONE',  ( 104.4882414327378939, -26.97927861161949181, 175.2815989661729077 ) ) ;
#75733 = CARTESIAN_POINT ( 'NONE',  ( 110.5064767540468296, -26.94654216138279068, 254.8194347997213640 ) ) ;
#75734 = FACE_OUTER_BOUND ( 'NONE', #31187, .T. ) ;
#75735 = EDGE_CURVE ( 'NONE', #83669, #28614, #82855, .T. ) ;
#75737 = VERTEX_POINT ( 'NONE', #84199 ) ;
#75736 = CIRCLE ( 'NONE', #22136, 2.517500000000005844 ) ;
#75738 = EDGE_CURVE ( 'NONE', #12019, #21182, #81667, .T. ) ;
#75739 = DIRECTION ( 'NONE',  ( 0.000000000000000000, 0.000000000000000000, -1.000000000000000000 ) ) ;
#75740 = DIRECTION ( 'NONE',  ( 0.000000000000000000, 0.000000000000000000, 1.000000000000000000 ) ) ;
#75741 = CARTESIAN_POINT ( 'NONE',  ( 101.7674321979440606, -44.34626990135510738, 84.91094751244793315 ) ) ;
#75742 = VECTOR ( 'NONE', #46742, 999.9999999999998863 ) ;
#75743 = EDGE_CURVE ( 'NONE', #40273, #87723, #42456, .T. ) ;
#75744 = CIRCLE ( 'NONE', #72819, 1.999999999999995781 ) ;
#75745 = EDGE_CURVE ( 'NONE', #56522, #623, #77821, .T. ) ;
#75746 = DIRECTION ( 'NONE',  ( 1.000000000000000000, 1.000000000000000078E-15, 0.000000000000000000 ) ) ;
#75747 = AXIS2_PLACEMENT_3D ( 'NONE', #16156, #64740, #9777 ) ;
#75748 = LINE ( 'NONE', #13516, #61925 ) ;
#75749 = ORIENTED_EDGE ( 'NONE', *, *, #13399, .F. ) ;
#75750 = CARTESIAN_POINT ( 'NONE',  ( 107.0664832912739399, -36.72944715994095333, 293.1356252759106837 ) ) ;
#75751 = VERTEX_POINT ( 'NONE', #72786 ) ;
#75752 = CARTESIAN_POINT ( 'NONE',  ( 117.0333688383452397, -30.31836458025946968, 144.2813395616249750 ) ) ;
#75753 = ORIENTED_EDGE ( 'NONE', *, *, #40782, .T. ) ;
#75754 = VECTOR ( 'NONE', #72345, 1000.000000000000000 ) ;
#75755 = EDGE_CURVE ( 'NONE', #46083, #78070, #75813, .T. ) ;
#75756 = CARTESIAN_POINT ( 'NONE',  ( 98.30753422232200478, -41.72887554593309289, 67.73979194757066580 ) ) ;
#75757 = CARTESIAN_POINT ( 'NONE',  ( 100.7916921807572379, -44.60965664144636378, 118.4730118773259733 ) ) ;
#75758 = DIRECTION ( 'NONE',  ( 1.000000000000000000, 0.000000000000000000, 0.000000000000000000 ) ) ;
#75759 = LINE ( 'NONE', #63814, #13594 ) ;
#75760 = CARTESIAN_POINT ( 'NONE',  ( 110.3609615670502535, -25.32029891922833897, 60.85276813305395649 ) ) ;
#75761 = DIRECTION ( 'NONE',  ( 0.7071067811865295871, -0.7071067811865655584, 7.071067811865303756E-16 ) ) ;
#75762 = EDGE_LOOP ( 'NONE', ( #28321, #82879, #1251, #6538 ) ) ;
#75763 = DIRECTION ( 'NONE',  ( 0.000000000000000000, 1.000000000000000000, 0.000000000000000000 ) ) ;
#75764 = ORIENTED_EDGE ( 'NONE', *, *, #82516, .F. ) ;
#75765 = VERTEX_POINT ( 'NONE', #23757 ) ;
#75766 = EDGE_CURVE ( 'NONE', #38579, #15522, #64627, .T. ) ;
#75768 = LINE ( 'NONE', #62574, #45504 ) ;
#75767 = CIRCLE ( 'NONE', #14891, 4.874999999999990230 ) ;
#75769 = ORIENTED_EDGE ( 'NONE', *, *, #58686, .F. ) ;
#75770 = CARTESIAN_POINT ( 'NONE',  ( 99.44473759953881142, -30.59981194223813361, 240.7870538473399620 ) ) ;
#75771 = CARTESIAN_POINT ( 'NONE',  ( 114.4782738979392747, -28.49838154746453256, 155.5051490854349652 ) ) ;
#75772 = ADVANCED_FACE ( 'NONE', ( #58687 ), #51424, .T. ) ;
#75773 = CARTESIAN_POINT ( 'NONE',  ( 107.0664832912750057, -36.72944715993903486, 6.826283056785790393 ) ) ;
#75774 = DIRECTION ( 'NONE',  ( 0.7071067811865295871, -0.7071067811865655584, 7.071067811864992156E-16 ) ) ;
#75775 = CARTESIAN_POINT ( 'NONE',  ( 99.50169031327072844, -43.90275843488763741, 77.92991099019597812 ) ) ;
#75777 = EDGE_CURVE ( 'NONE', #66733, #43936, #30558, .T. ) ;
#75776 = CARTESIAN_POINT ( 'NONE',  ( 97.31576093318726350, -39.30577132596791046, 97.53168462105917058 ) ) ;
#75778 = ORIENTED_EDGE ( 'NONE', *, *, #58636, .T. ) ;
#75779 = CARTESIAN_POINT ( 'NONE',  ( 179.7974245136200011, -36.32844715994040996, -5.074374724088000832 ) ) ;
#75780 = ADVANCED_FACE ( 'NONE', ( #16046 ), #50989, .T. ) ;
#75781 = CARTESIAN_POINT ( 'NONE',  ( 108.3337614075856692, -46.73482379084396143, 158.6771398271995679 ) ) ;
#75782 = ORIENTED_EDGE ( 'NONE', *, *, #88496, .F. ) ;
#75783 = VECTOR ( 'NONE', #9392, 1000.000000000000000 ) ;
#75784 = DIRECTION ( 'NONE',  ( 0.000000000000000000, -1.000000000000000000, 0.000000000000000000 ) ) ;
#75785 = CARTESIAN_POINT ( 'NONE',  ( 0.000000000000000000, 101.5999999999999943, 0.000000000000000000 ) ) ;
#75786 = CARTESIAN_POINT ( 'NONE',  ( 97.24442698086039627, -40.26379795196659472, 266.6013395616254797 ) ) ;
#75787 = CARTESIAN_POINT ( 'NONE',  ( 37.35959712144330780, -48.62134037893607541, 129.9678068554150911 ) ) ;
#75788 = CARTESIAN_POINT ( 'NONE',  ( 31.78666935232867630, -29.62846900982351528, 117.4678068554150485 ) ) ;
#75789 = CARTESIAN_POINT ( 'NONE',  ( 105.7171716027695112, -46.72411491083433077, 92.46978268234177278 ) ) ;
#75790 = CARTESIAN_POINT ( 'NONE',  ( 97.33063403691424753, -33.15845143124434458, 21.03467289495897319 ) ) ;
#75792 = CARTESIAN_POINT ( 'NONE',  ( 108.2741602056595269, -26.36093993100608657, 125.9841967044819597 ) ) ;
#75791 = DIRECTION ( 'NONE',  ( 0.0001713722456120069274, -0.9999999853157766072, 0.000000000000000000 ) ) ;
#75793 = CARTESIAN_POINT ( 'NONE',  ( 122.2189888861419433, -111.9861225405538221, -11.78219314458175937 ) ) ;
#75794 = CARTESIAN_POINT ( 'NONE',  ( 102.0297551351921044, -46.62107256275958633, 172.2137205140059564 ) ) ;
#75795 = DIRECTION ( 'NONE',  ( 1.000000000000000078E-15, -1.000000000000000000, 0.000000000000000000 ) ) ;
#75796 = EDGE_LOOP ( 'NONE', ( #29677, #3415, #7568, #34661 ) ) ;
#75797 = CARTESIAN_POINT ( 'NONE',  ( 107.0664832912739968, -36.72944715994100306, 287.6356252759109680 ) ) ;
#75798 = CYLINDRICAL_SURFACE ( 'NONE', #29085, 2.117000000000000881 ) ;
#75799 = CARTESIAN_POINT ( 'NONE',  ( 136.6805397534846520, -35.85322261660486731, 2.908039740961550823 ) ) ;
#75800 = ORIENTED_EDGE ( 'NONE', *, *, #12782, .T. ) ;
#75801 = CIRCLE ( 'NONE', #45299, 25.39999999999999858 ) ;
#75802 = CARTESIAN_POINT ( 'NONE',  ( 163.1543517358360020, -31.62489322948790971, -5.074374724088000832 ) ) ;
#75804 = ORIENTED_EDGE ( 'NONE', *, *, #47415, .F. ) ;
#75803 = CARTESIAN_POINT ( 'NONE',  ( 108.5962597759698127, -47.12230983477568458, 142.6927681330539883 ) ) ;
#75805 = CARTESIAN_POINT ( 'NONE',  ( 122.2221484686747459, -108.0760968907524955, -21.78219314458190681 ) ) ;
#75806 = CARTESIAN_POINT ( 'NONE',  ( 89.08909376919952194, 70.66229531820914644, 95.43663006862890086 ) ) ;
#75807 = CARTESIAN_POINT ( 'NONE',  ( 144.0667052733537901, -83.77844715994091018, 222.2178068554179902 ) ) ;
#75808 = CARTESIAN_POINT ( 'NONE',  ( 205.0097499999990305, 52.73749999999999716, -44.45000000000000284 ) ) ;
#75809 = ORIENTED_EDGE ( 'NONE', *, *, #64146, .T. ) ;
#75810 = CIRCLE ( 'NONE', #35194, 2.750000000000002665 ) ;
#75811 = ORIENTED_EDGE ( 'NONE', *, *, #19643, .F. ) ;
#75812 = VERTEX_POINT ( 'NONE', #2858 ) ;
#75813 = CIRCLE ( 'NONE', #36656, 14.00000000000000888 ) ;
#75814 = ORIENTED_EDGE ( 'NONE', *, *, #53027, .F. ) ;
#75815 = CYLINDRICAL_SURFACE ( 'NONE', #6113, 2.030000000001872529 ) ;
#75816 = CARTESIAN_POINT ( 'NONE',  ( 85.52787878288724244, 91.23859726994545838, -98.64044413062958938 ) ) ;
#75817 = CARTESIAN_POINT ( 'NONE',  ( 73.17003668186733023, -46.47944715994106701, -5.074374724089063982 ) ) ;
#75819 = CARTESIAN_POINT ( 'NONE',  ( 177.0371591254543091, -48.62818131005480637, 313.9678068554149490 ) ) ;
#75818 = DIRECTION ( 'NONE',  ( 1.000000000000000000, 0.000000000000000000, 0.000000000000000000 ) ) ;
#75820 = CARTESIAN_POINT ( 'NONE',  ( 188.5667039024480971, -42.82844715993431350, 290.7178068554150059 ) ) ;
#75821 = ORIENTED_EDGE ( 'NONE', *, *, #88767, .T. ) ;
#75822 = ORIENTED_EDGE ( 'NONE', *, *, #82236, .T. ) ;
#75823 = LINE ( 'NONE', #13597, #664 ) ;
#75824 = DIRECTION ( 'NONE',  ( 1.000000000000000000, 1.261617073437676668E-15, 1.261617073437676668E-15 ) ) ;
#75825 = ADVANCED_FACE ( 'NONE', ( #10552 ), #16487, .T. ) ;
#75826 = CARTESIAN_POINT ( 'NONE',  ( 118.0655259830058270, -38.35211242607483939, 219.7099109901959935 ) ) ;
#75827 = DIRECTION ( 'NONE',  ( -4.237773401492740281E-14, 1.000000000000000000, 0.000000000000000000 ) ) ;
#75828 = ADVANCED_FACE ( 'NONE', ( #71903 ), #74444, .T. ) ;
#75829 = AXIS2_PLACEMENT_3D ( 'NONE', #24766, #52436, #4330 ) ;
#75830 = CARTESIAN_POINT ( 'NONE',  ( 107.2219638487720488, -26.36052190073626988, 76.07657765686298035 ) ) ;
#75831 = DIRECTION ( 'NONE',  ( 0.000000000000000000, 0.000000000000000000, -1.000000000000000000 ) ) ;
#75832 = CARTESIAN_POINT ( 'NONE',  ( 115.7800367298386419, -31.78559340308600412, 20.23709803735599877 ) ) ;
#75833 = ADVANCED_FACE ( 'NONE', ( #85095 ), #22864, .F. ) ;
#75834 = ORIENTED_EDGE ( 'NONE', *, *, #53019, .F. ) ;
#75835 = CARTESIAN_POINT ( 'NONE',  ( 127.1498166246070269, 12.92155284005802685, 336.5756252759110225 ) ) ;
#75836 = ADVANCED_FACE ( 'NONE', ( #85986 ), #72346, .F. ) ;
#75837 = VERTEX_POINT ( 'NONE', #3304 ) ;
#75838 = EDGE_LOOP ( 'NONE', ( #59764, #878, #32117, #74482 ) ) ;
#75839 = LINE ( 'NONE', #24673, #61134 ) ;
#75840 = CARTESIAN_POINT ( 'NONE',  ( 104.4082965424966147, -28.27590814835049926, 246.7501547344679693 ) ) ;
#75841 = ADVANCED_FACE ( 'NONE', ( #37370 ), #65076, .T. ) ;
#75842 = VECTOR ( 'NONE', #51268, 1000.000000000000000 ) ;
#75843 = CYLINDRICAL_SURFACE ( 'NONE', #53005, 7.499999999999996447 ) ;
#75844 = CARTESIAN_POINT ( 'NONE',  ( -118.1932448497438202, 91.23868085022589014, 9.271905035165794118 ) ) ;
#75845 = EDGE_CURVE ( 'NONE', #51458, #10458, #31432, .T. ) ;
#75846 = CYLINDRICAL_SURFACE ( 'NONE', #11240, 2.116999999999993776 ) ;
#75847 = CARTESIAN_POINT ( 'NONE',  ( 90.32738470895340299, 74.16215221268208779, -76.79083731950171909 ) ) ;
#75848 = EDGE_LOOP ( 'NONE', ( #24692, #16869, #50268, #36378, #43156 ) ) ;
#75849 = CYLINDRICAL_SURFACE ( 'NONE', #60928, 7.873999999999991672 ) ;
#75850 = DIRECTION ( 'NONE',  ( 0.000000000000000000, 0.000000000000000000, 1.000000000000000000 ) ) ;
#75851 = VERTEX_POINT ( 'NONE', #9226 ) ;
#75852 = CARTESIAN_POINT ( 'NONE',  ( 97.77227622453175115, -32.00665715170008951, 50.95276813305294183 ) ) ;
#75853 = VERTEX_POINT ( 'NONE', #38257 ) ;
#75854 = CARTESIAN_POINT ( 'NONE',  ( 115.1807610290764075, -35.84162759104140150, 276.7309475124485516 ) ) ;
#75855 = ADVANCED_FACE ( 'NONE', ( #65954 ), #55540, .T. ) ;
#75856 = CARTESIAN_POINT ( 'NONE',  ( 97.81286927418427979, -40.51761286958078756, 126.6352223400343746 ) ) ;
#75857 = CARTESIAN_POINT ( 'NONE',  ( 102.6819511611810753, -27.33185899950643005, 135.4118157521019441 ) ) ;
#75858 = PLANE ( 'NONE',  #88285 ) ;
#75859 = CARTESIAN_POINT ( 'NONE',  ( 131.0667039024480118, -58.72944715994093201, 207.5838068554149913 ) ) ;
#75860 = LINE ( 'NONE', #54486, #70967 ) ;
#75861 = CARTESIAN_POINT ( 'NONE',  ( 7.161806819047721540, 72.06186804431776238, 130.3594151003946138 ) ) ;
#75862 = ADVANCED_FACE ( 'NONE', ( #78282 ), #2411, .F. ) ;
#75864 = B_SPLINE_CURVE_WITH_KNOTS ( 'NONE', 3,
 ( #80660, #53801, #81567, #73828, #39306, #67011, #87911, #81121, #15189, #28354, #55141, #50134, #22457, #42869, #56046, #76969, #83791, #77413, #20663, #77870, #29269, #62875, #651, #14753, #61977, #41087, #70604, #8378, #28823, #89715, #7920, #82903, #1567, #211, #48329, #35164, #21111, #68809, #21565, #35620, #13843, #62432, #27912, #41525, #42422 ),
 .UNSPECIFIED., .F., .F.,
 ( 4, 1, 1, 2, 2, 2, 1, 2, 2, 2, 2, 2, 1, 2, 2, 2, 2, 1, 1, 2, 2, 2, 1, 2, 2, 4 ),
 ( 0.000000000000000000, 0.007812499999944476706, 0.01171874999991686685, 0.01367187499991590408, 0.01562499999991493957, 0.02343749999997512753, 0.02734375000000554071, 0.02929687500002081321, 0.03125000000003608919, 0.06249999999996937172, 0.09374999999990264732, 0.1249999999998359368, 0.1874999999997302436, 0.2187499999996694866, 0.2499999999996087019, 0.3749999999993610111, 0.4374999999992401634, 0.4687499999991869282, 0.4843749999991663890, 0.4921874999991687205, 0.4999999999991709965, 0.6249999999993580690, 0.6874999999994604316, 0.7187499999995111688, 0.7499999999995617950, 1.000000000000000000 ),
 .UNSPECIFIED. ) ;
#75863 = CARTESIAN_POINT ( 'NONE',  ( 97.12841500021716001, -40.02000613830777098, 237.5813395616249579 ) ) ;
#75865 = CARTESIAN_POINT ( 'NONE',  ( 162.5667039024470171, -33.35206098992711077, 193.9678068554150059 ) ) ;
#75866 = ORIENTED_EDGE ( 'NONE', *, *, #79068, .F. ) ;
#75867 = AXIS2_PLACEMENT_3D ( 'NONE', #80386, #3618, #11324 ) ;
#75868 = ORIENTED_EDGE ( 'NONE', *, *, #18105, .F. ) ;
#75869 = CARTESIAN_POINT ( 'NONE',  ( 114.8035609388329021, -44.68778416175712920, 114.2022919425779719 ) ) ;
#75870 = CARTESIAN_POINT ( 'NONE',  ( 123.4442068678753799, 45.02545161509468130, -42.50497980019686395 ) ) ;
#75871 = VECTOR ( 'NONE', #20592, 1000.000000000000000 ) ;
#75872 = ORIENTED_EDGE ( 'NONE', *, *, #13962, .F. ) ;
#75873 = ORIENTED_EDGE ( 'NONE', *, *, #41022, .F. ) ;
#75874 = ORIENTED_EDGE ( 'NONE', *, *, #13603, .T. ) ;
#75875 = AXIS2_PLACEMENT_3D ( 'NONE', #78731, #73215, #51863 ) ;
#75876 = DIRECTION ( 'NONE',  ( 0.000000000000000000, 0.000000000000000000, -1.000000000000000000 ) ) ;
#75877 = FACE_OUTER_BOUND ( 'NONE', #49102, .T. ) ;
#75878 = FACE_OUTER_BOUND ( 'NONE', #80296, .T. ) ;
#75879 = DIRECTION ( 'NONE',  ( -0.7071067811865613395, 0.7071067811865336949, -7.071067811865620286E-16 ) ) ;
#75880 = CARTESIAN_POINT ( 'NONE',  ( 98.91056109567942656, -37.06209505544900651, 159.1766617981629679 ) ) ;
#75881 = CARTESIAN_POINT ( 'NONE',  ( 106.1364166314141499, -47.76666518589912869, 258.4975300378158636 ) ) ;
#75883 = EDGE_CURVE ( 'NONE', #39354, #33468, #57808, .T. ) ;
#75882 = CYLINDRICAL_SURFACE ( 'NONE', #8790, 0.5000000000000004441 ) ;
#75884 = ORIENTED_EDGE ( 'NONE', *, *, #24103, .T. ) ;
#75885 = CARTESIAN_POINT ( 'NONE',  ( 130.3273610158207418, 92.64237678566784950, -7.754451942556684685 ) ) ;
#75886 = EDGE_CURVE ( 'NONE', #22170, #86967, #52739, .T. ) ;
#75887 = CARTESIAN_POINT ( 'NONE',  ( 107.0664832912739399, -36.72944715994095333, 293.6356252759106837 ) ) ;
#75888 = ORIENTED_EDGE ( 'NONE', *, *, #64992, .T. ) ;
#75889 = ORIENTED_EDGE ( 'NONE', *, *, #19350, .T. ) ;
#75890 = DIRECTION ( 'NONE',  ( 1.000000000000000078E-15, -1.000000000000000083E-30, -1.000000000000000000 ) ) ;
#75891 = VECTOR ( 'NONE', #60595, 1000.000000000000000 ) ;
#75892 = ORIENTED_EDGE ( 'NONE', *, *, #57852, .F. ) ;
#75893 = LINE ( 'NONE', #68633, #65741 ) ;
#75894 = CARTESIAN_POINT ( 'NONE',  ( 115.0888988976580976, -30.61762792753790663, 14.34395942819159941 ) ) ;
#75895 = B_SPLINE_CURVE_WITH_KNOTS ( 'NONE', 3,
 ( #70115, #63756, #29239, #56923, #15613, #71026, #24207, #31005, #65962, #10561, #86439, #30125, #51437, #51874, #17385, #10125, #52748, #59150 ),
 .UNSPECIFIED., .F., .F.,
 ( 4, 2, 2, 2, 2, 2, 2, 2, 4 ),
 ( 0.5000000000719210247, 0.5625000000629308827, 0.6250000000539407408, 0.6875000000449507098, 0.7500000000359605679, 0.8125000000269704259, 0.8750000000179802839, 0.9375000000089901420, 1.000000000000000000 ),
 .UNSPECIFIED. ) ;
#75896 = DIRECTION ( 'NONE',  ( 1.907762142705490052E-15, 7.167082501179359715E-16, -1.000000000000000000 ) ) ;
#75897 = LINE ( 'NONE', #6849, #89627 ) ;
#75898 = CARTESIAN_POINT ( 'NONE',  ( 113.5483862797134549, -30.40508126489656604, 193.8762293518859678 ) ) ;
#75899 = CARTESIAN_POINT ( 'NONE',  ( 109.9230826530363743, -46.83843495353658426, 72.79562527591099297 ) ) ;
#75900 = DIRECTION ( 'NONE',  ( 0.000000000000000000, 0.000000000000000000, -1.000000000000000000 ) ) ;
#75901 = ORIENTED_EDGE ( 'NONE', *, *, #80925, .T. ) ;
#75902 = AXIS2_PLACEMENT_3D ( 'NONE', #26887, #61399, #89575 ) ;
#75903 = LINE ( 'NONE', #82290, #89100 ) ;
#75904 = ORIENTED_EDGE ( 'NONE', *, *, #1538, .T. ) ;
#75905 = CARTESIAN_POINT ( 'NONE',  ( 112.1380301845968290, -28.01206920712143500, 260.6564718618365646 ) ) ;
#75906 = VERTEX_POINT ( 'NONE', #18259 ) ;
#75907 = DIRECTION ( 'NONE',  ( 0.000000000000000000, 1.000000000000000000, 0.000000000000000000 ) ) ;
#75908 = CARTESIAN_POINT ( 'NONE',  ( 102.9783262188089594, -135.0490206179280506, 249.3173333679100097 ) ) ;
#75909 = CIRCLE ( 'NONE', #81695, 17.00000000000090239 ) ;
#75910 = EDGE_CURVE ( 'NONE', #72232, #89279, #12554, .T. ) ;
#75911 = DIRECTION ( 'NONE',  ( 1.000000000000000000, 4.272717921125132861E-14, 0.000000000000000000 ) ) ;
#75912 = ORIENTED_EDGE ( 'NONE', *, *, #60973, .T. ) ;
#75913 = CARTESIAN_POINT ( 'NONE',  ( 96.89953391513134306, -32.33301889150666142, 61.01372051400599616 ) ) ;
#75914 =( NAMED_UNIT ( * ) PLANE_ANGLE_UNIT ( ) SI_UNIT ( $, .RADIAN. ) );
#75916 = CARTESIAN_POINT ( 'NONE',  ( 98.26026929335873206, 73.28356282573679437, -85.96437953530649168 ) ) ;
#75915 = CYLINDRICAL_SURFACE ( 'NONE', #81138, 88.90000000000000568 ) ;
#75917 = CARTESIAN_POINT ( 'NONE',  ( 68.49979375445622054, -104.6923134067608743, 247.6412730378945639 ) ) ;
#75918 = CARTESIAN_POINT ( 'NONE',  ( 131.4450127212694781, -17.89730640218637703, 2.921034946745714844 ) ) ;
#75919 = EDGE_LOOP ( 'NONE', ( #30130, #30735, #9645, #40837 ) ) ;
#75920 = CARTESIAN_POINT ( 'NONE',  ( 71.77848634863140376, 120.6499999999999915, -77.39114642429929347 ) ) ;
#75921 = CARTESIAN_POINT ( 'NONE',  ( 69.56670390244705970, -123.2784471599409812, 55.21780685541800437 ) ) ;
#75922 = DIRECTION ( 'NONE',  ( 1.000000000000000000, 0.000000000000000000, 0.000000000000000000 ) ) ;
#75923 = ORIENTED_EDGE ( 'NONE', *, *, #12697, .F. ) ;
#75924 = CARTESIAN_POINT ( 'NONE',  ( 98.31807308660266642, -42.43931386104045345, 97.78705384733993355 ) ) ;
#75926 = DIRECTION ( 'NONE',  ( 1.000000000000000078E-15, -1.000000000000000083E-30, -1.000000000000000000 ) ) ;
#75925 = PLANE ( 'NONE',  #76974 ) ;
#75927 = LINE ( 'NONE', #13698, #29154 ) ;
#75928 = EDGE_CURVE ( 'NONE', #89348, #67268, #11905, .T. ) ;
#75929 =( REPRESENTATION_RELATIONSHIP ('NONE','NONE', #82876, #885 ) REPRESENTATION_RELATIONSHIP_WITH_TRANSFORMATION ( #84437 )SHAPE_REPRESENTATION_RELATIONSHIP( ) );
#75930 = AXIS2_PLACEMENT_3D ( 'NONE', #37242, #57219, #43589 ) ;
#75931 = EDGE_CURVE ( 'NONE', #69462, #60854, #51029, .T. ) ;
#75932 = CARTESIAN_POINT ( 'NONE',  ( 135.2338238997143378, -107.2609675061132180, 250.2191008560389776 ) ) ;
#75933 = VERTEX_POINT ( 'NONE', #59576 ) ;
#75934 = EDGE_CURVE ( 'NONE', #43691, #228, #87479, .T. ) ;
#75935 = CARTESIAN_POINT ( 'NONE',  ( 116.5042510202518571, -34.04512512578506289, 145.0470538473389581 ) ) ;
#75937 = ORIENTED_EDGE ( 'NONE', *, *, #1029, .T. ) ;
#75936 = DIRECTION ( 'NONE',  ( -1.000000000000000000, -4.554376769437570034E-14, 0.000000000000000000 ) ) ;
#75938 = EDGE_CURVE ( 'NONE', #85611, #83342, #25522, .T. ) ;
#75939 = CARTESIAN_POINT ( 'NONE',  ( 109.2074818670226222, -48.35976665079980563, 273.7213395616252569 ) ) ;
#75940 = DIRECTION ( 'NONE',  ( -4.299999999999999979E-14, 1.000000000000000000, -4.400000000000000367E-29 ) ) ;
#75941 = PLANE ( 'NONE',  #64944 ) ;
#75942 = DIRECTION ( 'NONE',  ( 0.000000000000000000, 0.000000000000000000, -1.000000000000000000 ) ) ;
#75943 = CARTESIAN_POINT ( 'NONE',  ( 95.56670390244703128, -104.2784471599408818, 19.21780685541799016 ) ) ;
#75944 = DIRECTION ( 'NONE',  ( 1.639958061481212836E-42, -4.100000000000000342E-29, -1.000000000000000000 ) ) ;
#75945 = ADVANCED_FACE ( 'NONE', ( #31885 ), #73672, .F. ) ;
#75946 = CARTESIAN_POINT ( 'NONE',  ( -87.44698480207762259, 71.76234181793739708, 96.94335780202351316 ) ) ;
#75947 = CARTESIAN_POINT ( 'NONE',  ( 104.0204373342842388, -47.42213563049719482, 217.3556252759109668 ) ) ;
#75948 = ORIENTED_EDGE ( 'NONE', *, *, #11129, .T. ) ;
#75949 = ORIENTED_EDGE ( 'NONE', *, *, #77825, .F. ) ;
#75950 = CARTESIAN_POINT ( 'NONE',  ( 115.5247806442692422, -34.08644044406323559, 170.4987261630399473 ) ) ;
#75951 = EDGE_CURVE ( 'NONE', #34761, #15433, #65364, .T. ) ;
#75952 = DIRECTION ( 'NONE',  ( 0.000000000000000000, 0.000000000000000000, 1.000000000000000000 ) ) ;
#75954 = CARTESIAN_POINT ( 'NONE',  ( 97.80396793100808850, -40.49851008571629762, 57.63399943843067774 ) ) ;
#75953 = CARTESIAN_POINT ( 'NONE',  ( 114.1881255536272022, -42.05338753103387717, 24.74729759161198217 ) ) ;
#75955 = CIRCLE ( 'NONE', #7805, 4.500000000000003553 ) ;
#75956 = CARTESIAN_POINT ( 'NONE',  ( 23.74939270293513616, 83.17752536574882072, 298.1637491577495780 ) ) ;
#75957 = EDGE_CURVE ( 'NONE', #70274, #63468, #86258, .T. ) ;
#75958 = CYLINDRICAL_SURFACE ( 'NONE', #41706, 38.10000000000000142 ) ;
#75959 = LINE ( 'NONE', #83232, #6633 ) ;
#75960 = VECTOR ( 'NONE', #28756, 1000.000000000000000 ) ;
#75961 = LINE ( 'NONE', #27801, #15950 ) ;
#75962 = CARTESIAN_POINT ( 'NONE',  ( 152.0368932755773130, -23.42844715993587812, 129.9678068554149775 ) ) ;
#75963 = CARTESIAN_POINT ( 'NONE',  ( 98.95962429139160577, -30.20966935044058488, 240.7870538473399620 ) ) ;
#75964 = CARTESIAN_POINT ( 'NONE',  ( 109.7260104821493485, -27.00109994382369649, 169.8639692407531925 ) ) ;
#75965 = ORIENTED_EDGE ( 'NONE', *, *, #57993, .T. ) ;
#75966 = ORIENTED_EDGE ( 'NONE', *, *, #36997, .T. ) ;
#75967 = ADVANCED_FACE ( 'NONE', ( #30844 ), #4025, .T. ) ;
#75968 = CARTESIAN_POINT ( 'NONE',  ( 72.96458098368650269, 127.0000000000000000, 72.96458098368729850 ) ) ;
#75969 = CARTESIAN_POINT ( 'NONE',  ( -87.71185091857921634, 93.94641470820117490, -79.76397050720419202 ) ) ;
#75970 = DIRECTION ( 'NONE',  ( 0.000000000000000000, 0.4999999999999897304, 0.8660254037844445918 ) ) ;
#75971 = CYLINDRICAL_SURFACE ( 'NONE', #21620, 16.00000000000090239 ) ;
#75972 = DIRECTION ( 'NONE',  ( 1.000000000000000000, 0.000000000000000000, 0.000000000000000000 ) ) ;
#75973 = VERTEX_POINT ( 'NONE', #24924 ) ;
#75974 = CYLINDRICAL_SURFACE ( 'NONE', #29166, 5.041900000000001825 ) ;
#75975 = CARTESIAN_POINT ( 'NONE',  ( 101.6505379212622699, -45.63756515480785225, 247.1413395616249602 ) ) ;
#75976 = EDGE_LOOP ( 'NONE', ( #43187, #19904 ) ) ;
#75977 = CARTESIAN_POINT ( 'NONE',  ( -68.91674821478409285, 82.54999999999999716, -68.91674821478481761 ) ) ;
#75978 = CARTESIAN_POINT ( 'NONE',  ( 107.3864418959535527, -26.30668689864625875, 322.4523926293242653 ) ) ;
#75979 = CARTESIAN_POINT ( 'NONE',  ( 109.6422649569531416, -46.48027517605736136, 167.7814222378137288 ) ) ;
#75980 = CARTESIAN_POINT ( 'NONE',  ( 114.9159532999967723, -33.08434830970520579, 56.97856656006794651 ) ) ;
#75981 = CARTESIAN_POINT ( 'NONE',  ( 97.93745859118190822, -30.45679909449765432, 161.8594347997199918 ) ) ;
#75982 = LINE ( 'NONE', #55505, #60892 ) ;
#75983 = ORIENTED_EDGE ( 'NONE', *, *, #13090, .T. ) ;
#75984 = ADVANCED_FACE ( 'NONE', ( #23604 ), #30401, .F. ) ;
#75985 = DIRECTION ( 'NONE',  ( 0.7071067811861728725, -0.7071067811869222730, 0.000000000000000000 ) ) ;
#75986 = ORIENTED_EDGE ( 'NONE', *, *, #62317, .F. ) ;
#75987 = ORIENTED_EDGE ( 'NONE', *, *, #38964, .F. ) ;
#75988 = AXIS2_PLACEMENT_3D ( 'NONE', #18710, #88666, #72787 ) ;
#75989 = DIRECTION ( 'NONE',  ( -1.000000000000000000, 0.000000000000000000, -6.982966722218760189E-15 ) ) ;
#75990 = ORIENTED_EDGE ( 'NONE', *, *, #33598, .F. ) ;
#75991 = ORIENTED_EDGE ( 'NONE', *, *, #24068, .F. ) ;
#75992 = FACE_OUTER_BOUND ( 'NONE', #54912, .T. ) ;
#75993 = AXIS2_PLACEMENT_3D ( 'NONE', #77343, #14682, #55975 ) ;
#75994 = CARTESIAN_POINT ( 'NONE',  ( 99.58293739761768393, -32.55228987500129278, 110.3438483995049495 ) ) ;
#75995 = CARTESIAN_POINT ( 'NONE',  ( 115.5353962700893788, -29.58991257470437120, 224.3718157521009573 ) ) ;
#75996 = CARTESIAN_POINT ( 'NONE',  ( 104.4591861284129948, -26.65816784528755790, 200.2784824187679362 ) ) ;
#75997 = CARTESIAN_POINT ( 'NONE',  ( 117.3629797429380659, -38.21633193987522503, 24.71276813305395237 ) ) ;
#75998 = CARTESIAN_POINT ( 'NONE',  ( 48.45959712128969699, -28.98061976758959801, 193.9678068554150911 ) ) ;
#75999 = CARTESIAN_POINT ( 'NONE',  ( 98.30745363658094504, -41.72867870133166690, 92.73977502107145199 ) ) ;
#76000 = EDGE_CURVE ( 'NONE', #25675, #10962, #58533, .T. ) ;
#76001 = ORIENTED_EDGE ( 'NONE', *, *, #76557, .F. ) ;
#76002 = CARTESIAN_POINT ( 'NONE',  ( 112.7054497023526807, -28.73785826246136921, 129.5870538473399449 ) ) ;
#76003 = EDGE_CURVE ( 'NONE', #43910, #52044, #67171, .T. ) ;
#76004 = CARTESIAN_POINT ( 'NONE',  ( 104.7497970125497204, -46.93922829031851762, 72.39848241876795498 ) ) ;
#76006 = AXIS2_PLACEMENT_3D ( 'NONE', #50824, #78994, #29050 ) ;
#76005 = CARTESIAN_POINT ( 'NONE',  ( 101.6276731664663089, -45.67517298127779668, 247.1413395616249602 ) ) ;
#76007 = ORIENTED_EDGE ( 'NONE', *, *, #55333, .T. ) ;
#76008 = CARTESIAN_POINT ( 'NONE',  ( 115.2518872279481030, -30.21599423016839836, 244.3613395616249875 ) ) ;
#76009 = CARTESIAN_POINT ( 'NONE',  ( 115.0889047178942661, -30.61763667089422469, 34.34395861009651441 ) ) ;
#76010 = CARTESIAN_POINT ( 'NONE',  ( 41.56648329127499153, -27.82844715994070484, 23.67562527591200094 ) ) ;
#76012 = LINE ( 'NONE', #34221, #60916 ) ;
#76011 = AXIS2_PLACEMENT_3D ( 'NONE', #75684, #88424, #39792 ) ;
#76013 = CARTESIAN_POINT ( 'NONE',  ( -254.0000000000000000, 104.7749999999999915, -41.27499999999999858 ) ) ;
#76015 = DIRECTION ( 'NONE',  ( -3.999999999999999995E-14, 1.000000000000000000, -4.100000000000000342E-29 ) ) ;
#76014 = DIRECTION ( 'NONE',  ( 0.7071067811571405404, 0.7071067812159546051, 0.000000000000000000 ) ) ;
#76016 = PLANE ( 'NONE',  #84463 ) ;
#76017 = DIRECTION ( 'NONE',  ( 0.000000000000000000, 0.000000000000000000, 1.000000000000000000 ) ) ;
#76018 = CARTESIAN_POINT ( 'NONE',  ( 46.83715912545343940, -47.82818131006086304, 129.9678068554150911 ) ) ;
#76019 = CIRCLE ( 'NONE', #38336, 8.999999999999994671 ) ;
#76020 = CARTESIAN_POINT ( 'NONE',  ( 63.06670390244700997, -79.67844715994098692, 190.2178068554179902 ) ) ;
#76021 = DIRECTION ( 'NONE',  ( 0.000000000000000000, 0.000000000000000000, -1.000000000000000000 ) ) ;
#76022 = CYLINDRICAL_SURFACE ( 'NONE', #78253, 3.299999999999999822 ) ;
#76024 = ORIENTED_EDGE ( 'NONE', *, *, #38346, .T. ) ;
#76023 = CARTESIAN_POINT ( 'NONE',  ( 97.31584372647238013, -39.30597603972135801, 261.5314586125417122 ) ) ;
#76025 = FACE_OUTER_BOUND ( 'NONE', #53491, .T. ) ;
#76026 = CARTESIAN_POINT ( 'NONE',  ( 111.8742750991676758, -46.04467666623092015, 272.9556252759110180 ) ) ;
#76027 = CARTESIAN_POINT ( 'NONE',  ( 100.8865061632069882, -45.89117093204367137, 148.0918157521009562 ) ) ;
#76028 = CARTESIAN_POINT ( 'NONE',  ( 117.5342389965484386, -35.85531600229182914, 249.8927681330537780 ) ) ;
#76029 = LINE ( 'NONE', #33801, #35975 ) ;
#76031 = DIRECTION ( 'NONE',  ( 0.000000000000000000, 1.000000000000000000, 0.000000000000000000 ) ) ;
#76030 = CARTESIAN_POINT ( 'NONE',  ( 196.2150000000000034, 43.68799999999999528, 57.14999999999999858 ) ) ;
#76032 = PLANE ( 'NONE',  #42167 ) ;
#76033 = FACE_OUTER_BOUND ( 'NONE', #8301, .T. ) ;
#76034 = ORIENTED_EDGE ( 'NONE', *, *, #31086, .T. ) ;
#76035 = CARTESIAN_POINT ( 'NONE',  ( 128.0667039024480118, -58.72944715994112386, 198.9178068554149945 ) ) ;
#76036 = ORIENTED_EDGE ( 'NONE', *, *, #17476, .T. ) ;
#76037 = EDGE_CURVE ( 'NONE', #80917, #82312, #38986, .T. ) ;
#76038 = CARTESIAN_POINT ( 'NONE',  ( 112.4311324297980406, -44.02555639339375659, 182.4914674471249612 ) ) ;
#76040 = ORIENTED_EDGE ( 'NONE', *, *, #80627, .T. ) ;
#76039 = DIRECTION ( 'NONE',  ( 0.9130365726098601531, 0.000000000000000000, 0.4078776986755214828 ) ) ;
#76041 = DIRECTION ( 'NONE',  ( 0.000000000000000000, 0.000000000000000000, -1.000000000000000000 ) ) ;
#76042 = EDGE_CURVE ( 'NONE', #12758, #17652, #65794, .T. ) ;
#76043 = CARTESIAN_POINT ( 'NONE',  ( 108.2752786314947286, -47.69320359391959840, 153.6518157521009584 ) ) ;
#76044 = DIRECTION ( 'NONE',  ( 0.000000000000000000, 0.000000000000000000, -1.000000000000000000 ) ) ;
#76045 = DIRECTION ( 'NONE',  ( -1.000000000000000000, -1.000000000000000078E-15, 0.000000000000000000 ) ) ;
#76046 = CARTESIAN_POINT ( 'NONE',  ( -77.01855645442535092, 73.86197090048098346, 90.13186587200978295 ) ) ;
#76047 = EDGE_CURVE ( 'NONE', #12839, #15555, #66695, .T. ) ;
#76048 = CARTESIAN_POINT ( 'NONE',  ( 97.81168895331838087, -40.51742574516882200, 287.6356252759109680 ) ) ;
#76049 = CARTESIAN_POINT ( 'NONE',  ( 108.8666348730871221, -46.34312957481634498, 82.72419670448294937 ) ) ;
#76050 = ORIENTED_EDGE ( 'NONE', *, *, #44856, .F. ) ;
#76051 = ORIENTED_EDGE ( 'NONE', *, *, #76054, .T. ) ;
#76052 = ORIENTED_EDGE ( 'NONE', *, *, #62679, .F. ) ;
#76053 = CIRCLE ( 'NONE', #15179, 13.99999999999999822 ) ;
#76054 = EDGE_CURVE ( 'NONE', #48698, #19610, #9962, .T. ) ;
#76055 = CYLINDRICAL_SURFACE ( 'NONE', #21103, 10.04999999999999361 ) ;
#76057 = DIRECTION ( 'NONE',  ( 0.000000000000000000, 0.000000000000000000, -1.000000000000000000 ) ) ;
#76056 = CARTESIAN_POINT ( 'NONE',  ( 109.4488926988246504, -27.20905326525217660, 195.8813395616249977 ) ) ;
#76058 = AXIS2_PLACEMENT_3D ( 'NONE', #46267, #65837, #4521 ) ;
#76059 = CARTESIAN_POINT ( 'NONE',  ( 3.110602869834275287E-15, -71.84204896855320044, -25.39999999999999858 ) ) ;
#76060 = DIRECTION ( 'NONE',  ( 0.000000000000000000, 1.000000000000000000, 0.000000000000000000 ) ) ;
#76061 = EDGE_CURVE ( 'NONE', #35213, #26343, #10399, .T. ) ;
#76062 = DIRECTION ( 'NONE',  ( 0.000000000000000000, 0.000000000000000000, 1.000000000000000000 ) ) ;
#76063 = FACE_OUTER_BOUND ( 'NONE', #32525, .T. ) ;
#76064 = DIRECTION ( 'NONE',  ( 9.299908063537919123E-17, 0.000000000000000000, 1.000000000000000000 ) ) ;
#76065 = CARTESIAN_POINT ( 'NONE',  ( 102.4028819069269218, -26.73371583578772004, 135.4118157521009493 ) ) ;
#76066 = EDGE_LOOP ( 'NONE', ( #74297, #25145, #74175, #63566, #71321, #40262 ) ) ;
#76067 = EDGE_LOOP ( 'NONE', ( #76778, #294, #12536, #79451 ) ) ;
#76068 = ORIENTED_EDGE ( 'NONE', *, *, #5223, .T. ) ;
#76069 = DIRECTION ( 'NONE',  ( 4.825893423866870279E-33, 0.000000000000000000, -1.000000000000000000 ) ) ;
#76070 = CARTESIAN_POINT ( 'NONE',  ( -94.33669211993698411, 94.92443974548201879, -90.25311968877646507 ) ) ;
#76071 = DIRECTION ( 'NONE',  ( 0.000000000000000000, 0.000000000000000000, -1.000000000000000000 ) ) ;
#76072 = CARTESIAN_POINT ( 'NONE',  ( 108.3259390676978455, -28.66449228317154763, 187.7709475124489700 ) ) ;
#76073 = CIRCLE ( 'NONE', #55682, 2.517500000000005844 ) ;
#76074 = VECTOR ( 'NONE', #6435, 1000.000000000000000 ) ;
#76075 = LINE ( 'NONE', #42881, #21857 ) ;
#76076 = AXIS2_PLACEMENT_3D ( 'NONE', #13158, #74933, #34928 ) ;
#76077 = CIRCLE ( 'NONE', #2115, 3.249999999999975131 ) ;
#76078 = LINE ( 'NONE', #27038, #15594 ) ;
#76079 = ORIENTED_EDGE ( 'NONE', *, *, #24991, .F. ) ;
#76081 = ORIENTED_EDGE ( 'NONE', *, *, #40397, .F. ) ;
#76080 = VERTEX_POINT ( 'NONE', #38104 ) ;
#76082 = AXIS2_PLACEMENT_3D ( 'NONE', #26425, #5081, #88219 ) ;
#76083 = CIRCLE ( 'NONE', #66091, 3.500000000000003109 ) ;
#76084 = CARTESIAN_POINT ( 'NONE',  ( 144.1872411114284773, -138.0587426716868151, 247.6570821702239869 ) ) ;
#76085 = ORIENTED_EDGE ( 'NONE', *, *, #86846, .F. ) ;
#76086 = VERTEX_POINT ( 'NONE', #71740 ) ;
#76087 = CARTESIAN_POINT ( 'NONE',  ( 77.76764265987219460, -20.23887630717950259, 7.293197373621064905 ) ) ;
#76088 = CARTESIAN_POINT ( 'NONE',  ( 106.2775494337459037, -46.09182447052010190, 258.9292023535161889 ) ) ;
#76089 = ORIENTED_EDGE ( 'NONE', *, *, #33476, .F. ) ;
#76090 = EDGE_CURVE ( 'NONE', #70, #43353, #73511, .T. ) ;
#76091 = DIRECTION ( 'NONE',  ( 0.000000000000000000, 0.000000000000000000, 1.000000000000000000 ) ) ;
#76092 = CARTESIAN_POINT ( 'NONE',  ( -123.5099984066448684, 72.79992482915794483, 42.31500800594746181 ) ) ;
#76093 = ORIENTED_EDGE ( 'NONE', *, *, #83241, .F. ) ;
#76094 = ORIENTED_EDGE ( 'NONE', *, *, #46308, .T. ) ;
#76095 = DIRECTION ( 'NONE',  ( 1.639958061481212836E-42, -4.100000000000000342E-29, -1.000000000000000000 ) ) ;
#76096 = VERTEX_POINT ( 'NONE', #85833 ) ;
#76097 = VERTEX_POINT ( 'NONE', #4482 ) ;
#76098 = EDGE_CURVE ( 'NONE', #64699, #28622, #17664, .T. ) ;
#76099 = CARTESIAN_POINT ( 'NONE',  ( 98.84295822536005005, -39.42912807745279480, 284.4090427505438470 ) ) ;
#76100 = CARTESIAN_POINT ( 'NONE',  ( 102.2921677216391174, -27.39701587636625391, 120.4527681330539792 ) ) ;
#76101 = CARTESIAN_POINT ( 'NONE',  ( 102.9796410358629828, -46.29638950891627047, 92.25562527591097250 ) ) ;
#76102 = CARTESIAN_POINT ( 'NONE',  ( 108.5950374404567071, -44.93858127607868624, 249.5838068554168387 ) ) ;
#76103 = CARTESIAN_POINT ( 'NONE',  ( 131.5325842222575830, -17.66080143920384771, 7.039723185229114222 ) ) ;
#76104 = CARTESIAN_POINT ( 'NONE',  ( 113.7506423937859807, -44.72972868871420360, 189.1299109901969757 ) ) ;
#76105 = DIRECTION ( 'NONE',  ( 0.000000000000000000, 0.000000000000000000, 1.000000000000000000 ) ) ;
#76106 = FACE_OUTER_BOUND ( 'NONE', #82646, .T. ) ;
#76107 = ORIENTED_EDGE ( 'NONE', *, *, #64014, .F. ) ;
#76108 = LINE ( 'NONE', #77019, #17769 ) ;
#76109 = VERTEX_POINT ( 'NONE', #31277 ) ;
#76110 = ORIENTED_EDGE ( 'NONE', *, *, #17093, .T. ) ;
#76111 = CARTESIAN_POINT ( 'NONE',  ( 51.34673845256598668, -36.02818131005800950, -5.074374724088000832 ) ) ;
#76112 = AXIS2_PLACEMENT_3D ( 'NONE', #46519, #32448, #66982 ) ;
#76113 = PLANE ( 'NONE',  #70792 ) ;
#76114 = ADVANCED_FACE ( 'NONE', ( #78576 ), #52587, .F. ) ;
#76115 = CARTESIAN_POINT ( 'NONE',  ( 97.98636869442889008, -41.85180495037556625, 136.7356252759109623 ) ) ;
#76116 = CARTESIAN_POINT ( 'NONE',  ( -7.038238517017752827, 71.97865724765921414, 130.3661473682803376 ) ) ;
#76117 = VECTOR ( 'NONE', #23431, 1000.000000000000000 ) ;
#76118 = LINE ( 'NONE', #61144, #39128 ) ;
#76119 = CARTESIAN_POINT ( 'NONE',  ( 168.3664380525673607, -48.62818131005418110, 300.4678068554149490 ) ) ;
#76122 = CARTESIAN_POINT ( 'NONE',  ( 118.7655994573050577, -38.45539276985793720, 219.7099109901969882 ) ) ;
#76121 = FACE_OUTER_BOUND ( 'NONE', #68978, .T. ) ;
#76120 = DIRECTION ( 'NONE',  ( 1.000000000000000078E-15, -1.000000000000000083E-30, -1.000000000000000000 ) ) ;
#76123 = DIRECTION ( 'NONE',  ( 0.000000000000000000, 0.000000000000000000, -1.000000000000000000 ) ) ;
#76124 = DIRECTION ( 'NONE',  ( -0.000000000000000000, -0.000000000000000000, -1.000000000000000000 ) ) ;
#76125 = ORIENTED_EDGE ( 'NONE', *, *, #29283, .F. ) ;
#76126 = DIRECTION ( 'NONE',  ( 1.000000000000000078E-15, -1.000000000000000000, 0.000000000000000000 ) ) ;
#76127 = DIRECTION ( 'NONE',  ( -2.108231265501709878E-16, 0.000000000000000000, 1.000000000000000000 ) ) ;
#76128 = CARTESIAN_POINT ( 'NONE',  ( 107.0664832912739968, -36.72944715994100306, 294.6356252759106837 ) ) ;
#76129 = CARTESIAN_POINT ( 'NONE',  ( -3.968750000000754508, 120.6499999999999915, 100.8961411191535973 ) ) ;
#76131 = VERTEX_POINT ( 'NONE', #58971 ) ;
#76130 = CARTESIAN_POINT ( 'NONE',  ( 106.5394234437989667, -24.24056378642895737, 322.0356252759110021 ) ) ;
#76132 = DIRECTION ( 'NONE',  ( -1.000000000000000078E-15, 1.000000000000000083E-30, 1.000000000000000000 ) ) ;
#76133 = CARTESIAN_POINT ( 'NONE',  ( 96.64877318785802629, -35.94450158219160585, 146.2670538473399517 ) ) ;
#76134 = CARTESIAN_POINT ( 'NONE',  ( 111.3231501057927346, -27.21297328954094041, 20.74133956162494030 ) ) ;
#76135 = CARTESIAN_POINT ( 'NONE',  ( 103.0329776526464087, -26.38883157761164000, 166.3603871806729444 ) ) ;
#76136 = DIRECTION ( 'NONE',  ( 0.000000000000000000, 0.000000000000000000, -1.000000000000000000 ) ) ;
#76137 = CARTESIAN_POINT ( 'NONE',  ( 194.5664832912739826, -18.82844715994099971, 342.9256252759119548 ) ) ;
#76139 = DIRECTION ( 'NONE',  ( 1.000000000000000000, 3.083952846180989689E-15, 1.541976423090494844E-15 ) ) ;
#76138 = DIRECTION ( 'NONE',  ( 0.000000000000000000, 1.000000000000000000, 0.000000000000000000 ) ) ;
#76140 = DIRECTION ( 'NONE',  ( 1.387778780781444413E-14, -1.000000000000000000, 0.000000000000000000 ) ) ;
#76141 = FACE_OUTER_BOUND ( 'NONE', #75848, .T. ) ;
#76142 = EDGE_LOOP ( 'NONE', ( #13952, #58232, #77553, #67255 ) ) ;
#76143 = CIRCLE ( 'NONE', #661, 32.50000000000001421 ) ;
#76144 = VECTOR ( 'NONE', #19064, 1000.000000000000000 ) ;
#76145 = CIRCLE ( 'NONE', #45695, 1.000000000000000888 ) ;
#76146 = CIRCLE ( 'NONE', #34115, 7.937500000000000000 ) ;
#76147 = ORIENTED_EDGE ( 'NONE', *, *, #18724, .T. ) ;
#76148 = ORIENTED_EDGE ( 'NONE', *, *, #50054, .T. ) ;
#76149 = EDGE_CURVE ( 'NONE', #56141, #77917, #18094, .T. ) ;
#76150 = TOROIDAL_SURFACE ( 'NONE', #68897, 7.799999999999999822, 0.2999999999999999889 ) ;
#76151 = VECTOR ( 'NONE', #27785, 1000.000000000000000 ) ;
#76152 = EDGE_LOOP ( 'NONE', ( #25858, #20587, #27835, #26123, #28523, #80703 ) ) ;
#76153 = CARTESIAN_POINT ( 'NONE',  ( 83.06670390244796920, -61.87844715994100397, 231.5838068554150198 ) ) ;
#76154 = CARTESIAN_POINT ( 'NONE',  ( 99.51750086509218818, -43.88776608678588786, 77.92991099019597812 ) ) ;
#76155 = CARTESIAN_POINT ( 'NONE',  ( 138.8167039024479834, -57.40094715994099772, 63.03480685541479289 ) ) ;
#76156 = ADVANCED_FACE ( 'NONE', ( #38541, #64919 ), #57646, .T. ) ;
#76157 = CARTESIAN_POINT ( 'NONE',  ( 145.3822798034300945, -139.2473393705360536, 246.2271668860497300 ) ) ;
#76158 = CARTESIAN_POINT ( 'NONE',  ( 117.5007279078441655, -40.51415819784174488, 169.5375300378159693 ) ) ;
#76159 = EDGE_CURVE ( 'NONE', #65225, #81285, #35188, .T. ) ;
#76160 = DIRECTION ( 'NONE',  ( 0.000000000000000000, 0.000000000000000000, 1.000000000000000000 ) ) ;
#76162 = CARTESIAN_POINT ( 'NONE',  ( 110.9972015515846238, -44.34532242709460093, 272.3781341137911909 ) ) ;
#76161 = VECTOR ( 'NONE', #76381, 1000.000000000000000 ) ;
#76163 = ORIENTED_EDGE ( 'NONE', *, *, #13072, .F. ) ;
#76164 = ORIENTED_EDGE ( 'NONE', *, *, #3636, .T. ) ;
#76165 = VERTEX_POINT ( 'NONE', #28382 ) ;
#76166 = DIRECTION ( 'NONE',  ( 4.299999999999999979E-14, -1.000000000000000000, 0.000000000000000000 ) ) ;
#76167 = CARTESIAN_POINT ( 'NONE',  ( 126.0667039024479550, -14.72944715994094977, 199.5838068554170093 ) ) ;
#76168 = DIRECTION ( 'NONE',  ( 1.000000000000000000, 0.000000000000000000, 0.000000000000000000 ) ) ;
#76169 = VECTOR ( 'NONE', #23421, 1000.000000000000114 ) ;
#76170 = DIRECTION ( 'NONE',  ( -1.000000000000000078E-15, 1.000000000000000083E-30, 1.000000000000000000 ) ) ;
#76171 = LINE ( 'NONE', #75729, #69775 ) ;
#76172 = CARTESIAN_POINT ( 'NONE',  ( -135.2444258376732193, 0.000000000000000000, -147.4575741623275746 ) ) ;
#76173 = EDGE_CURVE ( 'NONE', #54590, #32962, #14325, .T. ) ;
#76174 = CARTESIAN_POINT ( 'NONE',  ( 208.9149999999999920, 30.98800000000000310, 57.14999999999999858 ) ) ;
#76175 = ADVANCED_FACE ( 'NONE', ( #82147 ), #68046, .F. ) ;
#76176 = CARTESIAN_POINT ( 'NONE',  ( 106.2538455105912050, -26.32252419718678027, 25.13848241876792855 ) ) ;
#76177 = CARTESIAN_POINT ( 'NONE',  ( 71.24076473329810710, 5.642044068322332961, 394.9756252759101471 ) ) ;
#76178 = ORIENTED_EDGE ( 'NONE', *, *, #63517, .T. ) ;
#76179 = CARTESIAN_POINT ( 'NONE',  ( 97.81136857581559241, -40.51756142658395987, 157.6353372204761456 ) ) ;
#76180 = DIRECTION ( 'NONE',  ( 0.000000000000000000, 0.000000000000000000, -1.000000000000000000 ) ) ;
#76181 = CARTESIAN_POINT ( 'NONE',  ( 97.89197038913195570, -35.34227587553755257, 69.02523322673498285 ) ) ;
#76182 = VECTOR ( 'NONE', #31406, 1000.000000000000000 ) ;
#76183 = AXIS2_PLACEMENT_3D ( 'NONE', #2966, #72454, #51971 ) ;
#76184 = CYLINDRICAL_SURFACE ( 'NONE', #35409, 5.041900000000000048 ) ;
#76185 = CARTESIAN_POINT ( 'NONE',  ( 51.06648329127400388, 12.92155284005902516, 333.4006252759110112 ) ) ;
#76186 = ORIENTED_EDGE ( 'NONE', *, *, #85613, .F. ) ;
#76187 = VERTEX_POINT ( 'NONE', #49264 ) ;
#76188 = CARTESIAN_POINT ( 'NONE',  ( 78.80082187618229739, -34.28157759250729697, 7.978179524066798756 ) ) ;
#76189 = EDGE_LOOP ( 'NONE', ( #109, #84506, #30924, #67272 ) ) ;
#76190 = CARTESIAN_POINT ( 'NONE',  ( 98.85647153018690858, -30.30415715074617111, 155.7984824187679465 ) ) ;
#76191 = ORIENTED_EDGE ( 'NONE', *, *, #40466, .F. ) ;
#76192 = CARTESIAN_POINT ( 'NONE',  ( 100.8874679282520788, -44.70022140857566484, 68.05229194691942496 ) ) ;
#76193 = CARTESIAN_POINT ( 'NONE',  ( 99.18485448662231363, -41.84413841198986006, 143.2282499725629634 ) ) ;
#76194 = CARTESIAN_POINT ( 'NONE',  ( -47.11752803141011015, 100.5999999999999659, 108.7909173056707317 ) ) ;
#76195 = DIRECTION ( 'NONE',  ( 1.000000000000000078E-15, -1.000000000000000083E-30, -1.000000000000000000 ) ) ;
#76196 = CARTESIAN_POINT ( 'NONE',  ( 117.4762281475856724, -37.96087228405902181, 49.73276813305393773 ) ) ;
#76197 = LINE ( 'NONE', #83041, #29978 ) ;
#76198 = AXIS2_PLACEMENT_3D ( 'NONE', #29144, #71385, #57275 ) ;
#76199 = ORIENTED_EDGE ( 'NONE', *, *, #56454, .F. ) ;
#76200 = CARTESIAN_POINT ( 'NONE',  ( 48.79742451361987321, -36.32844715994078655, 193.9678068554150911 ) ) ;
#76201 = AXIS2_PLACEMENT_3D ( 'NONE', #65989, #2895, #16085 ) ;
#76202 = AXIS2_PLACEMENT_3D ( 'NONE', #65379, #9974, #71316 ) ;
#76203 = EDGE_LOOP ( 'NONE', ( #5709, #4250, #51086, #59372 ) ) ;
#76204 = ORIENTED_EDGE ( 'NONE', *, *, #24160, .T. ) ;
#76205 = ADVANCED_FACE ( 'NONE', ( #81251 ), #80226, .T. ) ;
#76206 = AXIS2_PLACEMENT_3D ( 'NONE', #13037, #26646, #41159 ) ;
#76207 = CARTESIAN_POINT ( 'NONE',  ( 107.0664832912739968, -36.72944715994100306, 287.6356252759109680 ) ) ;
#76208 = ORIENTED_EDGE ( 'NONE', *, *, #78565, .F. ) ;
#76209 = CARTESIAN_POINT ( 'NONE',  ( 100.4593435015893164, -29.47291325643525184, 285.6641967044828334 ) ) ;
#76210 = CARTESIAN_POINT ( 'NONE',  ( 97.96758126215280527, -41.86240348953004542, 132.7356252759109623 ) ) ;
#76211 = LINE ( 'NONE', #88954, #64059 ) ;
#76212 = DIRECTION ( 'NONE',  ( 0.000000000000000000, 0.000000000000000000, 1.000000000000000000 ) ) ;
#76213 = CARTESIAN_POINT ( 'NONE',  ( 113.5060836576900272, -28.53103057085638383, 75.54705384733995288 ) ) ;
#76214 = CARTESIAN_POINT ( 'NONE',  ( 104.4081006910507341, -46.45808914803028955, 262.3647919450149288 ) ) ;
#76215 = ORIENTED_EDGE ( 'NONE', *, *, #37483, .F. ) ;
#76216 = AXIS2_PLACEMENT_3D ( 'NONE', #37626, #71701, #29466 ) ;
#76217 = DIRECTION ( 'NONE',  ( 3.100000000000000258E-29, -3.100000000000000044E-14, -1.000000000000000000 ) ) ;
#76218 = CARTESIAN_POINT ( 'NONE',  ( 109.6433497169441722, -46.48000174799164341, 158.7813111578553844 ) ) ;
#76219 = CONICAL_SURFACE ( 'NONE', #79163, 1.624999999999987566, 1.029744258676650093 ) ;
#76220 = VERTEX_POINT ( 'NONE', #678 ) ;
#76221 = CARTESIAN_POINT ( 'NONE',  ( 0.000000000000000000, 65.60000000000000853, 0.000000000000000000 ) ) ;
#76222 = EDGE_CURVE ( 'NONE', #29668, #36866, #72939, .T. ) ;
#76223 = DIRECTION ( 'NONE',  ( -4.237773401492740281E-14, 1.000000000000000000, 0.000000000000000000 ) ) ;
#76224 = CARTESIAN_POINT ( 'NONE',  ( 100.4109522542116650, -28.70505079160765760, 40.62705384733894221 ) ) ;
#76225 = DIRECTION ( 'NONE',  ( 0.000000000000000000, 1.000000000000000000, 0.000000000000000000 ) ) ;
#76226 = VECTOR ( 'NONE', #3309, 1000.000000000000000 ) ;
#76227 = DIRECTION ( 'NONE',  ( 9.351236661543306751E-17, -3.725950533538267725E-29, -1.000000000000000000 ) ) ;
#76228 = CARTESIAN_POINT ( 'NONE',  ( 115.0393671692859101, -42.90578492219520967, 93.30325341284572005 ) ) ;
#76229 = CARTESIAN_POINT ( 'NONE',  ( 115.3963617111076445, -41.85549503053864839, 18.38705384734096171 ) ) ;
#76231 = CARTESIAN_POINT ( 'NONE',  ( 107.3333893024683903, -26.32957087652229689, 116.0556252759109555 ) ) ;
#76230 = CARTESIAN_POINT ( 'NONE',  ( 104.5295158156824584, -26.96092172908695161, 100.2802235910898787 ) ) ;
#76232 = CARTESIAN_POINT ( 'NONE',  ( 109.2774118001976120, 53.97500000000000142, 71.43750000000000000 ) ) ;
#76233 = CARTESIAN_POINT ( 'NONE',  ( 101.7470617766046956, -45.74667603143129924, 162.1527681330539679 ) ) ;
#76234 = DIRECTION ( 'NONE',  ( 1.000000000000000000, 1.000000000000000078E-15, 1.000000000000000078E-15 ) ) ;
#76235 = ORIENTED_EDGE ( 'NONE', *, *, #82838, .F. ) ;
#76236 = DIRECTION ( 'NONE',  ( 0.000000000000000000, 0.000000000000000000, -1.000000000000000000 ) ) ;
#76237 = CARTESIAN_POINT ( 'NONE',  ( 12.70000000000000107, 82.54999999999999716, -97.46299999999996544 ) ) ;
#76238 = CARTESIAN_POINT ( 'NONE',  ( 107.5667039024470455, -113.7784471599413791, 2.217806855418308132 ) ) ;
#76239 = CIRCLE ( 'NONE', #16789, 3.174999999999983391 ) ;
#76240 = VERTEX_POINT ( 'NONE', #26695 ) ;
#76241 = EDGE_CURVE ( 'NONE', #76131, #78184, #5373, .T. ) ;
#76242 = EDGE_CURVE ( 'NONE', #1472, #56709, #69733, .T. ) ;
#76243 = FACE_BOUND ( 'NONE', #38365, .T. ) ;
#76245 = ORIENTED_EDGE ( 'NONE', *, *, #45683, .F. ) ;
#76244 = CARTESIAN_POINT ( 'NONE',  ( 117.0593108693811786, -33.60693806652478344, 174.0670538473389399 ) ) ;
#76246 = DIRECTION ( 'NONE',  ( 0.000000000000000000, 0.000000000000000000, 1.000000000000000000 ) ) ;
#76247 = CARTESIAN_POINT ( 'NONE',  ( 106.9401787849546537, -47.80506239865356122, 228.5794347997199907 ) ) ;
#76248 = CARTESIAN_POINT ( 'NONE',  ( 99.33321048326423863, 75.15271101351808625, 84.72210942532007039 ) ) ;
#76249 = DIRECTION ( 'NONE',  ( 0.7071067811865590080, 0.000000000000000000, 0.7071067811865361374 ) ) ;
#76250 = AXIS2_PLACEMENT_3D ( 'NONE', #35894, #9541, #49956 ) ;
#76251 = CARTESIAN_POINT ( 'NONE',  ( 52.38749999999999574, 94.53880000000000905, 225.4249999999999829 ) ) ;
#76252 = ORIENTED_EDGE ( 'NONE', *, *, #78750, .T. ) ;
#76253 = EDGE_CURVE ( 'NONE', #4135, #14684, #46685, .T. ) ;
#76254 = VERTEX_POINT ( 'NONE', #48805 ) ;
#76255 = ORIENTED_EDGE ( 'NONE', *, *, #34196, .T. ) ;
#76256 = ORIENTED_EDGE ( 'NONE', *, *, #52240, .T. ) ;
#76257 = DIRECTION ( 'NONE',  ( 1.000000000000000000, 3.999999999999999995E-14, 1.000000000000000078E-15 ) ) ;
#76258 = CARTESIAN_POINT ( 'NONE',  ( 97.16978355702093495, -40.00630874038032658, 237.5813395616249579 ) ) ;
#76259 = DIRECTION ( 'NONE',  ( 0.3552177606235679130, 0.000000000000000000, -0.9347835805883507598 ) ) ;
#76260 = CARTESIAN_POINT ( 'NONE',  ( 107.0667039024470313, -104.2784471599409528, 222.2178068554179902 ) ) ;
#76261 = ADVANCED_FACE ( 'NONE', ( #39874 ), #13503, .F. ) ;
#76263 = CARTESIAN_POINT ( 'NONE',  ( 92.12448541806557500, 79.66685870724428753, 74.62312585591683955 ) ) ;
#76262 = DIRECTION ( 'NONE',  ( -1.000000000000000078E-15, -1.000000000000000083E-30, 1.000000000000000000 ) ) ;
#76264 = CARTESIAN_POINT ( 'NONE',  ( 33.92127028473601769, -29.73316016639540749, -5.074374724088000832 ) ) ;
#76265 = CARTESIAN_POINT ( 'NONE',  ( 104.7307148508592007, -47.55717207929887991, 32.41943479972098174 ) ) ;
#76266 = VERTEX_POINT ( 'NONE', #12639 ) ;
#76267 = AXIS2_PLACEMENT_3D ( 'NONE', #33605, #27230, #61300 ) ;
#76268 = EDGE_LOOP ( 'NONE', ( #72314, #40951, #48425, #46327 ) ) ;
#76269 = CIRCLE ( 'NONE', #50187, 8.999999999999994671 ) ;
#76270 = VECTOR ( 'NONE', #15527, 1000.000000000000000 ) ;
#76271 = FACE_OUTER_BOUND ( 'NONE', #10494, .T. ) ;
#76272 = AXIS2_PLACEMENT_3D ( 'NONE', #58301, #49802, #80545 ) ;
#76273 = CARTESIAN_POINT ( 'NONE',  ( -240.5296158183964792, 14.28750000000026077, 11.11249999999970051 ) ) ;
#76274 = CARTESIAN_POINT ( 'NONE',  ( 116.3159835831961857, -41.41832011455023377, 244.4651490854349731 ) ) ;
#76275 = CARTESIAN_POINT ( 'NONE',  ( 31.56670390244800117, -32.29483332968611364, 342.9256252759109884 ) ) ;
#76276 = ADVANCED_FACE ( 'NONE', ( #32613 ), #40325, .T. ) ;
#76277 = CARTESIAN_POINT ( 'NONE',  ( 102.0418483691416895, -28.29933337693059414, 81.50419670448194154 ) ) ;
#76279 = EDGE_CURVE ( 'NONE', #1004, #79764, #53486, .T. ) ;
#76278 = CARTESIAN_POINT ( 'NONE',  ( 177.0371591254543091, -48.62818131005480637, 313.9678068554149490 ) ) ;
#76280 = EDGE_CURVE ( 'NONE', #67362, #4351, #82954, .T. ) ;
#76281 = CARTESIAN_POINT ( 'NONE',  ( -76.76779673090611311, 55.97500000000000142, 30.90025125786759830 ) ) ;
#76282 = ORIENTED_EDGE ( 'NONE', *, *, #38037, .T. ) ;
#76283 = CARTESIAN_POINT ( 'NONE',  ( 177.0664832912730162, 12.92155284005730387, 361.9756252759109998 ) ) ;
#76284 = EDGE_CURVE ( 'NONE', #32868, #32236, #61221, .T. ) ;
#76285 = ORIENTED_EDGE ( 'NONE', *, *, #73982, .T. ) ;
#76286 = ORIENTED_EDGE ( 'NONE', *, *, #42615, .T. ) ;
#76287 = AXIS2_PLACEMENT_3D ( 'NONE', #68469, #7141, #19870 ) ;
#76288 = CARTESIAN_POINT ( 'NONE',  ( -92.22587532767808227, 84.62843115047674303, 74.49778344313872935 ) ) ;
#76289 = CARTESIAN_POINT ( 'NONE',  ( 116.4516747918435300, -36.28819209217700603, 265.2834880678017839 ) ) ;
#76290 = DIRECTION ( 'NONE',  ( 1.000000000000000000, 4.237773401492740281E-14, 0.000000000000000000 ) ) ;
#76291 = CARTESIAN_POINT ( 'NONE',  ( -118.5108459337403843, 94.82191660594813243, 3.295896443149240351 ) ) ;
#76292 = CIRCLE ( 'NONE', #54470, 0.5000000000000004441 ) ;
#76293 = CARTESIAN_POINT ( 'NONE',  ( 98.34985892274558239, -31.65658479228161681, 85.90645860766178998 ) ) ;
#76294 = CARTESIAN_POINT ( 'NONE',  ( 79.21825297796463872, 71.54629894495526798, -88.20503424218246380 ) ) ;
#76295 = ORIENTED_EDGE ( 'NONE', *, *, #76740, .F. ) ;
#76296 = CARTESIAN_POINT ( 'NONE',  ( -126.4481529151155996, 44.45000000000000284, 32.49205688096009936 ) ) ;
#76297 = CARTESIAN_POINT ( 'NONE',  ( 104.4070256631273850, -46.45777391140720169, 183.3652439674835932 ) ) ;
#76298 = EDGE_LOOP ( 'NONE', ( #12687, #60908, #44841, #14031, #40345, #36689 ) ) ;
#76299 = CARTESIAN_POINT ( 'NONE',  ( 106.6068369155051698, -25.68554329116653534, 40.09753003781596448 ) ) ;
#76300 = VERTEX_POINT ( 'NONE', #46701 ) ;
#76301 = CARTESIAN_POINT ( 'NONE',  ( 99.09762411907954061, -31.97621503831505407, 278.7166617981628178 ) ) ;
#76302 = CARTESIAN_POINT ( 'NONE',  ( 115.7840093042128018, -41.80077732092177456, 128.4066342822487456 ) ) ;
#76303 = CARTESIAN_POINT ( 'NONE',  ( 113.1634500054122583, -44.41975088505045477, 168.1099109901969939 ) ) ;
#76304 = DIRECTION ( 'NONE',  ( -1.000000000000000000, -8.953411488912552682E-16, 0.000000000000000000 ) ) ;
#76305 = LINE ( 'NONE', #1355, #62164 ) ;
#76306 = LINE ( 'NONE', #40877, #17273 ) ;
#76307 = CARTESIAN_POINT ( 'NONE',  ( 4.872201249568272274, 70.82175023847671014, 130.4650562613408908 ) ) ;
#76308 = CARTESIAN_POINT ( 'NONE',  ( 116.0926836276447460, -42.03234139191665975, 234.4041967044819899 ) ) ;
#76309 = CARTESIAN_POINT ( 'NONE',  ( 79.76397050720444781, 93.94641470820114648, -87.71185091857894633 ) ) ;
#76310 = ORIENTED_EDGE ( 'NONE', *, *, #88777, .F. ) ;
#76311 = CARTESIAN_POINT ( 'NONE',  ( 136.5146477271286187, -37.98222059078806012, 7.138441653514234098 ) ) ;
#76312 = ORIENTED_EDGE ( 'NONE', *, *, #86270, .T. ) ;
#76313 = CARTESIAN_POINT ( 'NONE',  ( 117.1483892680215888, -39.54869380112744892, 94.60991099019693706 ) ) ;
#76314 = CARTESIAN_POINT ( 'NONE',  ( 123.9297970803746267, 45.55335027554141192, -41.06498388075110739 ) ) ;
#76315 = VERTEX_POINT ( 'NONE', #19912 ) ;
#76316 = VERTEX_POINT ( 'NONE', #53502 ) ;
#76317 = ORIENTED_EDGE ( 'NONE', *, *, #86522, .F. ) ;
#76318 = DIRECTION ( 'NONE',  ( 1.000000000000000000, 1.000000000000000078E-15, 0.000000000000000000 ) ) ;
#76319 = CARTESIAN_POINT ( 'NONE',  ( -487.2989999999999782, 10.16305401447645984, 83.34375000000000000 ) ) ;
#76320 = FACE_OUTER_BOUND ( 'NONE', #21199, .T. ) ;
#76321 = DIRECTION ( 'NONE',  ( 1.000000000000000000, 0.000000000000000000, 0.000000000000000000 ) ) ;
#76322 = CARTESIAN_POINT ( 'NONE',  ( 100.6382899380647871, -31.69863749346629689, 153.6166617981629656 ) ) ;
#76323 = CARTESIAN_POINT ( 'NONE',  ( 112.6753912189806073, -45.54292608213916793, 259.0270538473393458 ) ) ;
#76324 = CARTESIAN_POINT ( 'NONE',  ( 97.82520644204963389, -40.55030899666594024, 57.63845489205286299 ) ) ;
#76325 = ORIENTED_EDGE ( 'NONE', *, *, #10608, .F. ) ;
#76326 = CARTESIAN_POINT ( 'NONE',  ( 6.123233995736769241E-16, 223.9999999999999716, 149.6557476874258441 ) ) ;
#76327 = AXIS2_PLACEMENT_3D ( 'NONE', #29961, #59428, #23169 ) ;
#76328 = CARTESIAN_POINT ( 'NONE',  ( 107.0664832912739968, -18.82844715994099971, 168.9256252759119832 ) ) ;
#76329 = VERTEX_POINT ( 'NONE', #39003 ) ;
#76330 = ORIENTED_EDGE ( 'NONE', *, *, #41989, .T. ) ;
#76331 = CIRCLE ( 'NONE', #19728, 9.999999999999994671 ) ;
#76332 = CIRCLE ( 'NONE', #77901, 2.750000000000002665 ) ;
#76333 = DIRECTION ( 'NONE',  ( 1.000000000000000078E-15, -1.000000000000000083E-30, -1.000000000000000000 ) ) ;
#76335 = EDGE_CURVE ( 'NONE', #54231, #82906, #88522, .T. ) ;
#76334 = CIRCLE ( 'NONE', #40074, 5.041900000000000048 ) ;
#76336 = DIRECTION ( 'NONE',  ( 0.000000000000000000, 0.000000000000000000, -1.000000000000000000 ) ) ;
#76337 = CARTESIAN_POINT ( 'NONE',  ( 97.80833607050627165, -40.50923396610764371, 16.63492042907981272 ) ) ;
#76338 = AXIS2_PLACEMENT_3D ( 'NONE', #16423, #64568, #4119 ) ;
#76339 = EDGE_CURVE ( 'NONE', #53860, #59559, #68515, .T. ) ;
#76340 = CARTESIAN_POINT ( 'NONE',  ( 162.7131505118539962, -33.70561438052090608, -5.074374724088000832 ) ) ;
#76341 = DIRECTION ( 'NONE',  ( -1.000000000000000078E-15, 1.000000000000000083E-30, 1.000000000000000000 ) ) ;
#76342 = CARTESIAN_POINT ( 'NONE',  ( 98.15635076299318484, -32.87196533591951919, 210.4238483995049762 ) ) ;
#76343 = CARTESIAN_POINT ( 'NONE',  ( 104.0299312746664526, -47.40616179873944702, 67.36800622829191809 ) ) ;
#76344 = FACE_BOUND ( 'NONE', #66763, .T. ) ;
#76345 = ORIENTED_EDGE ( 'NONE', *, *, #20696, .T. ) ;
#76346 = EDGE_CURVE ( 'NONE', #30351, #58675, #53986, .T. ) ;
#76347 = CARTESIAN_POINT ( 'NONE',  ( -86.67734222162535218, 70.52090377575436264, -80.88709205069426389 ) ) ;
#76348 = ORIENTED_EDGE ( 'NONE', *, *, #40259, .F. ) ;
#76349 = ADVANCED_FACE ( 'NONE', ( #32184 ), #67612, .T. ) ;
#76350 = EDGE_CURVE ( 'NONE', #34574, #53327, #81594, .T. ) ;
#76351 = FACE_OUTER_BOUND ( 'NONE', #44411, .T. ) ;
#76352 = ORIENTED_EDGE ( 'NONE', *, *, #361, .F. ) ;
#76353 = CARTESIAN_POINT ( 'NONE',  ( 116.3175913315759402, -32.94491325663879877, 165.1356252759109680 ) ) ;
#76354 = FACE_OUTER_BOUND ( 'NONE', #8355, .T. ) ;
#76355 = CARTESIAN_POINT ( 'NONE',  ( 97.81252181392954981, -40.51708140501057187, 272.6353344860016819 ) ) ;
#76356 = VECTOR ( 'NONE', #37792, 1000.000000000000000 ) ;
#76357 = EDGE_CURVE ( 'NONE', #16796, #11319, #75744, .T. ) ;
#76358 = CARTESIAN_POINT ( 'NONE',  ( 83.06670390244796920, -61.87844715994100397, 213.1838068554149856 ) ) ;
#76359 = VERTEX_POINT ( 'NONE', #26277 ) ;
#76360 = CARTESIAN_POINT ( 'NONE',  ( 118.0120547386033678, -38.42941975617429762, 68.69181575210198787 ) ) ;
#76361 =( NAMED_UNIT ( * ) PLANE_ANGLE_UNIT ( ) SI_UNIT ( $, .RADIAN. ) );
#76362 = VECTOR ( 'NONE', #78420, 1000.000000000000000 ) ;
#76363 = EDGE_CURVE ( 'NONE', #43607, #14882, #7600, .T. ) ;
#76365 = CARTESIAN_POINT ( 'NONE',  ( 86.19129576945162796, 72.98383416765814502, -98.06260288352355303 ) ) ;
#76364 = CARTESIAN_POINT ( 'NONE',  ( 91.42390633313587500, -35.38788608837992911, 293.9356252759109793 ) ) ;
#76366 = CARTESIAN_POINT ( 'NONE',  ( 163.0959832912772356, -23.42844715993520310, 193.9678068554149775 ) ) ;
#76367 = CARTESIAN_POINT ( 'NONE',  ( 117.8738102209306362, 82.54999999999999716, 12.70000000000123386 ) ) ;
#76368 = ORIENTED_EDGE ( 'NONE', *, *, #71960, .F. ) ;
#76369 = LINE ( 'NONE', #21867, #35865 ) ;
#76370 = EDGE_CURVE ( 'NONE', #36669, #3392, #67158, .T. ) ;
#76371 = LINE ( 'NONE', #28202, #31283 ) ;
#76372 = CARTESIAN_POINT ( 'NONE',  ( 12.37563412544579045, 79.66819247178165142, 117.9083347083516173 ) ) ;
#76373 = ORIENTED_EDGE ( 'NONE', *, *, #21621, .F. ) ;
#76374 = CARTESIAN_POINT ( 'NONE',  ( 98.18387371117843543, -43.34642931133835475, 107.8480062282919647 ) ) ;
#76376 = DIRECTION ( 'NONE',  ( 0.000000000000000000, 0.5000000000000007772, -0.8660254037844381525 ) ) ;
#76375 = CARTESIAN_POINT ( 'NONE',  ( 0.000000000000000000, 82.54999999999999716, 89.46299999999996544 ) ) ;
#76377 = CARTESIAN_POINT ( 'NONE',  ( 130.5667039024480118, -36.72944715994093912, 219.5838068554170093 ) ) ;
#76378 = CARTESIAN_POINT ( 'NONE',  ( 133.3763278023386647, -128.2462349309375043, 249.3055338466990065 ) ) ;
#76379 = ORIENTED_EDGE ( 'NONE', *, *, #34478, .T. ) ;
#76380 = CARTESIAN_POINT ( 'NONE',  ( 98.98846131648984681, -42.30253745798191289, 122.8070538473389490 ) ) ;
#76382 = ORIENTED_EDGE ( 'NONE', *, *, #54848, .F. ) ;
#76381 = DIRECTION ( 'NONE',  ( 0.7071067811864980568, 0.7071067811865969777, 0.000000000000000000 ) ) ;
#76383 = CARTESIAN_POINT ( 'NONE',  ( 100.2615012876618295, -45.41023301258249489, 273.0594347997205773 ) ) ;
#76384 = CARTESIAN_POINT ( 'NONE',  ( 97.81455683053849270, -40.52442650171994387, 252.6361864024953547 ) ) ;
#76385 = CARTESIAN_POINT ( 'NONE',  ( 131.0667039024480118, -42.21678055153905262, 231.5838068554170093 ) ) ;
#76386 = LINE ( 'NONE', #15964, #89377 ) ;
#76387 = FACE_OUTER_BOUND ( 'NONE', #49024, .T. ) ;
#76388 = EDGE_CURVE ( 'NONE', #51056, #84701, #61677, .T. ) ;
#76389 = CARTESIAN_POINT ( 'NONE',  ( 131.0667039024480118, -58.72944715994098175, 231.5838068554150198 ) ) ;
#76390 = CARTESIAN_POINT ( 'NONE',  ( 180.1667039024460166, -28.27351298637340093, -5.074374724088000832 ) ) ;
#76391 = EDGE_CURVE ( 'NONE', #19911, #68206, #52603, .T. ) ;
#76392 = AXIS2_PLACEMENT_3D ( 'NONE', #87833, #4264, #3816 ) ;
#76393 = CARTESIAN_POINT ( 'NONE',  ( 117.2610056464983899, -34.82931580038571440, 203.9851490854349549 ) ) ;
#76394 = ORIENTED_EDGE ( 'NONE', *, *, #85582, .T. ) ;
#76395 = EDGE_LOOP ( 'NONE', ( #83275, #54167, #82178, #35492 ) ) ;
#76396 = CARTESIAN_POINT ( 'NONE',  ( 115.9244277637092040, -39.86207309682762912, 174.9996785439919904 ) ) ;
#76397 = AXIS2_PLACEMENT_3D ( 'NONE', #33344, #82412, #61041 ) ;
#76398 = LINE ( 'NONE', #7803, #63241 ) ;
#76399 = VECTOR ( 'NONE', #16536, 1000.000000000000000 ) ;
#76400 = CARTESIAN_POINT ( 'NONE',  ( 116.7892270756567967, -35.66563809766837778, 274.9127681330532482 ) ) ;
#76401 = CIRCLE ( 'NONE', #88013, 3.000000000000002665 ) ;
#76402 = CARTESIAN_POINT ( 'NONE',  ( 134.0664832912740110, -8.729447159940999512, 296.1531252759119752 ) ) ;
#76403 = CARTESIAN_POINT ( 'NONE',  ( 112.0652091731003139, -45.48878794064455633, 267.9899078305007833 ) ) ;
#76404 = CARTESIAN_POINT ( 'NONE',  ( 121.3178890780284434, -113.5468731908973439, -19.18411693322874356 ) ) ;
#76405 = CARTESIAN_POINT ( 'NONE',  ( 0.000000000000000000, -71.84204896855320044, 0.000000000000000000 ) ) ;
#76406 = CARTESIAN_POINT ( 'NONE',  ( 163.1543517358360020, -31.62489322948790971, -5.074374724088000832 ) ) ;
#76407 = CARTESIAN_POINT ( 'NONE',  ( 114.5897159479186342, -29.54407062678533791, 234.4327681330539690 ) ) ;
#76408 = CARTESIAN_POINT ( 'NONE',  ( 32.24491389929970353, -32.11662333284649407, 193.9678068554150911 ) ) ;
#76409 = ORIENTED_EDGE ( 'NONE', *, *, #89164, .T. ) ;
#76410 = ORIENTED_EDGE ( 'NONE', *, *, #78014, .T. ) ;
#76411 = LINE ( 'NONE', #14188, #44480 ) ;
#76412 = CARTESIAN_POINT ( 'NONE',  ( -92.32962665258509105, 83.38952084682850341, -74.36911441044763649 ) ) ;
#76413 = DIRECTION ( 'NONE',  ( 0.000000000000000000, -1.000000000000000000, 0.000000000000000000 ) ) ;
#76414 = LINE ( 'NONE', #89608, #18679 ) ;
#76415 = VECTOR ( 'NONE', #77335, 1000.000000000000000 ) ;
#76416 = LINE ( 'NONE', #47793, #28147 ) ;
#76417 = CLOSED_SHELL ( 'NONE', ( #34398, #65164, #52398, #8682 ) ) ;
#76418 = ORIENTED_EDGE ( 'NONE', *, *, #18499, .F. ) ;
#76419 = CARTESIAN_POINT ( 'NONE',  ( 116.5137666388868780, -32.21926627522912412, 15.18133956162492915 ) ) ;
#76420 = CARTESIAN_POINT ( 'NONE',  ( 100.1386363970297992, -44.51995214173314963, 266.9984824187679919 ) ) ;
#76421 = EDGE_LOOP ( 'NONE', ( #75834, #2929, #18644, #85054, #33752, #21158 ) ) ;
#76422 = CARTESIAN_POINT ( 'NONE',  ( 77.55551418447849699, -37.85480617631969835, 7.067502061087529874 ) ) ;
#76423 = DIRECTION ( 'NONE',  ( -0.7071067811985215501, 0.7071067811745735954, 0.000000000000000000 ) ) ;
#76424 = CARTESIAN_POINT ( 'NONE',  ( 41.56648329127499153, -32.07844715994070839, 14.17562527591199917 ) ) ;
#76425 = CARTESIAN_POINT ( 'NONE',  ( 114.6445280793269603, -33.69580855137893138, 51.94809036959197357 ) ) ;
#76426 = CARTESIAN_POINT ( 'NONE',  ( 117.0891209002388678, -39.67630891660421355, 179.5984824187679294 ) ) ;
#76427 = DIRECTION ( 'NONE',  ( 1.000000000000000000, 1.000000000000000078E-15, 0.000000000000000000 ) ) ;
#76428 = ORIENTED_EDGE ( 'NONE', *, *, #20201, .T. ) ;
#76429 = CARTESIAN_POINT ( 'NONE',  ( 37.03715912545433042, -48.62818131006122258, 249.9678068554150343 ) ) ;
#76430 = EDGE_LOOP ( 'NONE', ( #53068, #3507, #44906, #67372 ) ) ;
#76432 = ORIENTED_EDGE ( 'NONE', *, *, #27705, .T. ) ;
#76431 = CIRCLE ( 'NONE', #89478, 5.041900000000001825 ) ;
#76433 = PLANE ( 'NONE',  #34324 ) ;
#76434 = ORIENTED_EDGE ( 'NONE', *, *, #4468, .T. ) ;
#76435 = EDGE_LOOP ( 'NONE', ( #86694, #8922 ) ) ;
#76436 = CARTESIAN_POINT ( 'NONE',  ( 0.000000000000000000, 101.5999999999999943, 0.000000000000000000 ) ) ;
#76437 = EDGE_CURVE ( 'NONE', #38582, #11954, #12654, .T. ) ;
#76438 = EDGE_CURVE ( 'NONE', #39122, #33219, #80364, .T. ) ;
#76439 = CARTESIAN_POINT ( 'NONE',  ( 103.3727720482000620, -29.02797788616916108, 94.85527697093499455 ) ) ;
#76440 = CARTESIAN_POINT ( 'NONE',  ( 106.5662725644766908, -47.20027100765710060, 247.5384824187679556 ) ) ;
#76441 = EDGE_CURVE ( 'NONE', #6854, #82398, #18116, .T. ) ;
#76442 = CARTESIAN_POINT ( 'NONE',  ( 112.1942863616536386, -45.78120396183496155, 212.9870538473389558 ) ) ;
#76443 = CARTESIAN_POINT ( 'NONE',  ( 117.0705705820183482, -32.08379757587637471, 55.16038718067301261 ) ) ;
#76444 = LINE ( 'NONE', #14227, #62962 ) ;
#76445 = PLANE ( 'NONE',  #36653 ) ;
#76446 = EDGE_CURVE ( 'NONE', #72723, #76939, #13110, .T. ) ;
#76447 = EDGE_LOOP ( 'NONE', ( #49406, #89176, #34965, #25477 ) ) ;
#76448 = CARTESIAN_POINT ( 'NONE',  ( 108.3334480733278866, -46.73485935691606841, 177.6772919410516351 ) ) ;
#76449 = AXIS2_PLACEMENT_3D ( 'NONE', #29033, #56718, #12651 ) ;
#76450 = CARTESIAN_POINT ( 'NONE',  ( -187.8075999999999794, 20.32000000000000028, -9.525000000000000355 ) ) ;
#76451 = CARTESIAN_POINT ( 'NONE',  ( 181.9790560690580037, -31.62489322948711035, 117.4678068554150627 ) ) ;
#76452 = EDGE_CURVE ( 'NONE', #50846, #1932, #54399, .T. ) ;
#76453 = CARTESIAN_POINT ( 'NONE',  ( 104.2906771502715628, -46.10805769451172864, 107.3470538473399500 ) ) ;
#76454 = CARTESIAN_POINT ( 'NONE',  ( 103.8276485124378183, -46.72253193893131140, 82.32705384733995402 ) ) ;
#76456 = CARTESIAN_POINT ( 'NONE',  ( 100.1483249706684546, -45.40999835672980112, 272.0289586092442278 ) ) ;
#76455 = CIRCLE ( 'NONE', #43115, 7.999999999999992895 ) ;
#76457 = ORIENTED_EDGE ( 'NONE', *, *, #55731, .F. ) ;
#76458 = AXIS2_PLACEMENT_3D ( 'NONE', #73504, #32607, #80789 ) ;
#76459 = CARTESIAN_POINT ( 'NONE',  ( 97.16957671423683962, -40.00637722736999535, 241.5813395616249863 ) ) ;
#76460 = CARTESIAN_POINT ( 'NONE',  ( 29.56670390244743629, -48.82844715994161078, 180.4678068554150911 ) ) ;
#76461 = VECTOR ( 'NONE', #5707, 1000.000000000000000 ) ;
#76462 = CARTESIAN_POINT ( 'NONE',  ( 98.54762029648411215, -41.97692828339373960, 22.76579877019573672 ) ) ;
#76463 = DIRECTION ( 'NONE',  ( 0.000000000000000000, 0.000000000000000000, 1.000000000000000000 ) ) ;
#76465 = CARTESIAN_POINT ( 'NONE',  ( 7.661254700127833495, 82.54999999999999716, 275.4630000000000223 ) ) ;
#76464 = CARTESIAN_POINT ( 'NONE',  ( -17.13243906362141900, 54.97499999999995879, 42.79834678115690849 ) ) ;
#76466 = DIRECTION ( 'NONE',  ( -1.000000000000000078E-15, 1.000000000000000000, 0.000000000000000000 ) ) ;
#76468 = EDGE_CURVE ( 'NONE', #76300, #83795, #43481, .T. ) ;
#76467 = CARTESIAN_POINT ( 'NONE',  ( -186.2398777604655038, 0.000000000000000000, -6.349999999999999645 ) ) ;
#76469 = FACE_OUTER_BOUND ( 'NONE', #26796, .T. ) ;
#76470 = FACE_OUTER_BOUND ( 'NONE', #56676, .T. ) ;
#76471 = DIRECTION ( 'NONE',  ( -6.982966722218760189E-15, 0.000000000000000000, 1.000000000000000000 ) ) ;
#76472 = CARTESIAN_POINT ( 'NONE',  ( 92.81551872686561921, -95.01002112898675023, -19.18411693322930134 ) ) ;
#76473 = EDGE_CURVE ( 'NONE', #38611, #22233, #42130, .T. ) ;
#76475 = ORIENTED_EDGE ( 'NONE', *, *, #70431, .F. ) ;
#76474 = CARTESIAN_POINT ( 'NONE',  ( 102.0670549394996840, -27.97049807078126094, 260.4897919444414924 ) ) ;
#76476 = PLANE ( 'NONE',  #23498 ) ;
#76477 = CARTESIAN_POINT ( 'NONE',  ( 100.1240125862563275, -44.53639691489608765, 266.9984824187678782 ) ) ;
#76478 = CARTESIAN_POINT ( 'NONE',  ( 96.01412018463531695, -36.58377574468403282, 152.3280062282919971 ) ) ;
#76479 = CARTESIAN_POINT ( 'NONE',  ( 106.8354761508916226, -47.19556465630029862, 268.5584824187679374 ) ) ;
#76480 = VECTOR ( 'NONE', #66108, 1000.000000000000000 ) ;
#76481 = DIRECTION ( 'NONE',  ( 0.000000000000000000, 1.000000000000000000, 0.000000000000000000 ) ) ;
#76482 = AXIS2_PLACEMENT_3D ( 'NONE', #88637, #47263, #48598 ) ;
#76484 = DIRECTION ( 'NONE',  ( 1.000000000000000000, 1.271620792853953879E-14, 0.000000000000000000 ) ) ;
#76483 = LINE ( 'NONE', #43285, #75482 ) ;
#76485 = CARTESIAN_POINT ( 'NONE',  ( 97.81939108931598525, -40.53620304804683627, 137.6372407434755019 ) ) ;
#76486 = CARTESIAN_POINT ( 'NONE',  ( 142.8821648370247885, -72.54478064608022692, 361.9756252759100335 ) ) ;
#76487 = VECTOR ( 'NONE', #66339, 1000.000000000000000 ) ;
#76488 = ORIENTED_EDGE ( 'NONE', *, *, #578, .F. ) ;
#76489 = LINE ( 'NONE', #59820, #67897 ) ;
#76490 = ORIENTED_EDGE ( 'NONE', *, *, #5919, .T. ) ;
#76491 = CARTESIAN_POINT ( 'NONE',  ( 115.4591718486505698, -35.14231982251399700, 158.3981341137909737 ) ) ;
#76493 = ORIENTED_EDGE ( 'NONE', *, *, #87131, .F. ) ;
#76492 = DIRECTION ( 'NONE',  ( -1.000000000000000000, 0.000000000000000000, 0.000000000000000000 ) ) ;
#76494 = CYLINDRICAL_SURFACE ( 'NONE', #15655, 9.999999999999998224 ) ;
#76495 = CARTESIAN_POINT ( 'NONE',  ( 108.0049669398584911, -26.36739623290736390, 151.0041967044829505 ) ) ;
#76496 = PLANE ( 'NONE',  #54079 ) ;
#76497 = CARTESIAN_POINT ( 'NONE',  ( 70.06174462629407174, -138.9592723264546521, 247.5160078862170110 ) ) ;
#76498 = CARTESIAN_POINT ( 'NONE',  ( 100.4979874790370644, -29.16083011470633224, 86.64560808839608796 ) ) ;
#76499 = DIRECTION ( 'NONE',  ( -1.000000000000000078E-15, 1.000000000000000083E-30, 1.000000000000000000 ) ) ;
#76500 = DIRECTION ( 'NONE',  ( 0.000000000000000000, 0.000000000000000000, -1.000000000000000000 ) ) ;
#76501 = EDGE_CURVE ( 'NONE', #9140, #33432, #20810, .T. ) ;
#76502 = CARTESIAN_POINT ( 'NONE',  ( 104.0406618471960201, -46.06530165129709076, 82.32705384733995402 ) ) ;
#76503 = ORIENTED_EDGE ( 'NONE', *, *, #53550, .F. ) ;
#76504 = VERTEX_POINT ( 'NONE', #83948 ) ;
#76506 = VERTEX_POINT ( 'NONE', #62135 ) ;
#76505 = AXIS2_PLACEMENT_3D ( 'NONE', #44735, #38371, #66071 ) ;
#76507 = CARTESIAN_POINT ( 'NONE',  ( 104.0154917791352744, -27.12933488216606648, 51.75301187732594599 ) ) ;
#76508 = DIRECTION ( 'NONE',  ( -3.100000000000000258E-29, 3.100000000000000044E-14, 1.000000000000000000 ) ) ;
#76510 = FACE_OUTER_BOUND ( 'NONE', #80550, .T. ) ;
#76509 = CARTESIAN_POINT ( 'NONE',  ( 99.07755742602716964, -44.46178485432842109, 187.9384824187679612 ) ) ;
#76511 = CYLINDRICAL_SURFACE ( 'NONE', #69773, 5.041900000000001825 ) ;
#76512 = DIRECTION ( 'NONE',  ( 0.000000000000000000, 1.000000000000000000, 0.000000000000000000 ) ) ;
#76513 = CARTESIAN_POINT ( 'NONE',  ( 116.3212776292296127, -32.94146857471318413, 287.6356252759109680 ) ) ;
#76514 = CARTESIAN_POINT ( 'NONE',  ( 163.0822201311030142, 101.5999999999999943, 75.92468371870748456 ) ) ;
#76515 = DIRECTION ( 'NONE',  ( 0.000000000000000000, 1.000000000000000000, 0.000000000000000000 ) ) ;
#76516 = CARTESIAN_POINT ( 'NONE',  ( 114.6914383512288254, -44.69963429152232237, 113.1718157521009687 ) ) ;
#76517 = ORIENTED_EDGE ( 'NONE', *, *, #69111, .F. ) ;
#76518 = ORIENTED_EDGE ( 'NONE', *, *, #37865, .T. ) ;
#76519 = ORIENTED_EDGE ( 'NONE', *, *, #9559, .T. ) ;
#76520 = ADVANCED_FACE ( 'NONE', ( #13992 ), #69412, .T. ) ;
#76521 = CARTESIAN_POINT ( 'NONE',  ( 6.720195294977327372, 71.76561749959921599, 130.3833905926466628 ) ) ;
#76522 = CARTESIAN_POINT ( 'NONE',  ( 145.5835616515379627, -69.28104898940431156, 247.4312010763500211 ) ) ;
#76523 = VECTOR ( 'NONE', #55866, 1000.000000000000000 ) ;
#76524 = CARTESIAN_POINT ( 'NONE',  ( 183.5150000000000148, 52.73749999999999716, -26.11912895322935313 ) ) ;
#76525 = CARTESIAN_POINT ( 'NONE',  ( 106.9948502263972188, -44.89183619263916825, 185.3880903695919642 ) ) ;
#76526 = EDGE_CURVE ( 'NONE', #1241, #77970, #32219, .T. ) ;
#76527 = CIRCLE ( 'NONE', #72188, 4.500000000000003553 ) ;
#76528 = VECTOR ( 'NONE', #47871, 999.9999999999998863 ) ;
#76529 = CYLINDRICAL_SURFACE ( 'NONE', #18911, 2.517499999999998739 ) ;
#76530 = DIRECTION ( 'NONE',  ( 0.7071067811865157093, 0.7071067811865794361, 7.071067811865148942E-16 ) ) ;
#76531 = ORIENTED_EDGE ( 'NONE', *, *, #8377, .F. ) ;
#76533 = VERTEX_POINT ( 'NONE', #41229 ) ;
#76532 = EDGE_LOOP ( 'NONE', ( #48984, #5895, #36205, #38249 ) ) ;
#76534 = VECTOR ( 'NONE', #65239, 1000.000000000000000 ) ;
#76535 = CARTESIAN_POINT ( 'NONE',  ( 136.6144450028906192, -19.76411817599922216, 2.828498113172279727 ) ) ;
#76536 = VERTEX_POINT ( 'NONE', #14901 ) ;
#76537 = ORIENTED_EDGE ( 'NONE', *, *, #72472, .T. ) ;
#76538 = CARTESIAN_POINT ( 'NONE',  ( 34.67381068360452900, -28.98061976759034764, 237.4678068554150059 ) ) ;
#76539 = CARTESIAN_POINT ( 'NONE',  ( 98.10010861879410982, -32.13871408278030373, 242.3815833058969815 ) ) ;
#76540 = AXIS2_PLACEMENT_3D ( 'NONE', #3497, #11203, #65286 ) ;
#76541 = DIRECTION ( 'NONE',  ( -0.7071067811865474617, 0.7071067811865474617, 0.000000000000000000 ) ) ;
#76542 = VERTEX_POINT ( 'NONE', #812 ) ;
#76543 = VECTOR ( 'NONE', #77755, 1000.000000000000000 ) ;
#76544 = AXIS2_PLACEMENT_3D ( 'NONE', #84408, #36692, #28978 ) ;
#76545 = DIRECTION ( 'NONE',  ( 0.000000000000000000, 0.000000000000000000, -1.000000000000000000 ) ) ;
#76546 = CARTESIAN_POINT ( 'NONE',  ( -123.2955287385074143, 73.06768973456320282, 42.93641881194006515 ) ) ;
#76547 = ORIENTED_EDGE ( 'NONE', *, *, #9703, .F. ) ;
#76548 = ORIENTED_EDGE ( 'NONE', *, *, #11947, .F. ) ;
#76549 = CIRCLE ( 'NONE', #28698, 34.13125000000000142 ) ;
#76550 = CARTESIAN_POINT ( 'NONE',  ( 0.000000000000000000, 125.7300000000000040, 9.525000000000000355 ) ) ;
#76551 = ORIENTED_EDGE ( 'NONE', *, *, #22638, .T. ) ;
#76552 = ORIENTED_EDGE ( 'NONE', *, *, #17586, .T. ) ;
#76553 = EDGE_CURVE ( 'NONE', #37760, #45213, #7628, .T. ) ;
#76554 = EDGE_CURVE ( 'NONE', #84986, #28006, #34874, .T. ) ;
#76555 = CARTESIAN_POINT ( 'NONE',  ( 115.2503885696571047, -36.58558574821132936, 286.6595189410200533 ) ) ;
#76556 = CARTESIAN_POINT ( 'NONE',  ( 109.5136938427377373, -46.88609643433851915, 132.7641967044819751 ) ) ;
#76557 = EDGE_CURVE ( 'NONE', #51377, #79343, #15348, .T. ) ;
#76558 = CARTESIAN_POINT ( 'NONE',  ( 114.7552509866192452, -44.63809267644818135, 118.2022919425779719 ) ) ;
#76559 = DIRECTION ( 'NONE',  ( 0.000000000000000000, 1.000000000000000000, 0.000000000000000000 ) ) ;
#76560 = CARTESIAN_POINT ( 'NONE',  ( 52.65249034007746332, -49.32844715994061602, 180.4678068554151196 ) ) ;
#76561 = CARTESIAN_POINT ( 'NONE',  ( 117.4742555207853059, -36.12881027634428222, 224.8727681330539667 ) ) ;
#76562 = DIRECTION ( 'NONE',  ( -0.7071067811567173234, 0.7071067812163779331, 0.000000000000000000 ) ) ;
#76563 = DIRECTION ( 'NONE',  ( -0.8660254037844379305, 0.000000000000000000, 0.5000000000000011102 ) ) ;
#76564 = VERTEX_POINT ( 'NONE', #43019 ) ;
#76565 = CARTESIAN_POINT ( 'NONE',  ( 130.5149182481443688, 70.27892663483460467, -3.298988752045384221 ) ) ;
#76566 = ORIENTED_EDGE ( 'NONE', *, *, #6590, .F. ) ;
#76567 = EDGE_CURVE ( 'NONE', #86245, #52932, #28503, .T. ) ;
#76568 = EDGE_LOOP ( 'NONE', ( #84749, #7605, #74244, #85716 ) ) ;
#76569 = CARTESIAN_POINT ( 'NONE',  ( 241.3336515812914911, 65.43750000000000000, 10.66800000000000104 ) ) ;
#76570 = VECTOR ( 'NONE', #24371, 1000.000000000000000 ) ;
#76571 = VECTOR ( 'NONE', #41780, 1000.000000000000000 ) ;
#76572 = CARTESIAN_POINT ( 'NONE',  ( 97.39130545576651343, -39.27856786311136261, 137.5314412799998536 ) ) ;
#76573 = ADVANCED_FACE ( 'NONE', ( #70757 ), #56194, .F. ) ;
#76574 = EDGE_LOOP ( 'NONE', ( #56509, #82269 ) ) ;
#76575 = CARTESIAN_POINT ( 'NONE',  ( 99.05404782812107101, -43.39937282746017644, 116.8784824187679732 ) ) ;
#76576 = CARTESIAN_POINT ( 'NONE',  ( -10.55536724279236616, 75.48783127733061349, 130.1286031690422078 ) ) ;
#76577 = CARTESIAN_POINT ( 'NONE',  ( 138.8167039024479834, -67.87844715994100397, 33.40080685541480676 ) ) ;
#76578 = CARTESIAN_POINT ( 'NONE',  ( -72.96458098368751166, 127.0000000000000000, 72.96458098368620426 ) ) ;
#76581 = CARTESIAN_POINT ( 'NONE',  ( 104.1918496689535090, -26.69446299336411599, 221.2984824187679465 ) ) ;
#76580 = DIRECTION ( 'NONE',  ( -0.9825752044165969590, -0.1858654558159821002, 0.000000000000000000 ) ) ;
#76579 = FACE_BOUND ( 'NONE', #26360, .T. ) ;
#76582 = CYLINDRICAL_SURFACE ( 'NONE', #4559, 9.525000000000000355 ) ;
#76584 = ADVANCED_FACE ( 'NONE', ( #63938 ), #34425, .T. ) ;
#76583 = LINE ( 'NONE', #273, #58363 ) ;
#76585 = ORIENTED_EDGE ( 'NONE', *, *, #29017, .F. ) ;
#76586 = DIRECTION ( 'NONE',  ( 0.000000000000000000, 1.000000000000000000, 0.000000000000000000 ) ) ;
#76587 = LINE ( 'NONE', #62498, #79061 ) ;
#76588 = CARTESIAN_POINT ( 'NONE',  ( 107.0664832912750057, -36.72944715993903486, 0.7256252759109708128 ) ) ;
#76589 = DIRECTION ( 'NONE',  ( -0.9834602067153815907, -0.1811243269341220596, 0.000000000000000000 ) ) ;
#76591 = ORIENTED_EDGE ( 'NONE', *, *, #28357, .T. ) ;
#76590 = CARTESIAN_POINT ( 'NONE',  ( 104.5776654613874683, -26.56013282928604724, 285.2670538473396391 ) ) ;
#76592 = DIRECTION ( 'NONE',  ( 0.000000000000000000, -0.8660254037844387076, 0.4999999999999998890 ) ) ;
#76593 = CARTESIAN_POINT ( 'NONE',  ( 97.72652769937234041, -42.68433437468970482, 141.7661014663869707 ) ) ;
#76594 = CARTESIAN_POINT ( 'NONE',  ( 99.98074987894446508, -44.37633341885192095, 42.98133956162492098 ) ) ;
#76595 = CARTESIAN_POINT ( 'NONE',  ( 102.6652156630552355, -27.23093027504711117, 176.4213395616249898 ) ) ;
#76596 = AXIS2_PLACEMENT_3D ( 'NONE', #29538, #23200, #35896 ) ;
#76597 = DIRECTION ( 'NONE',  ( -2.900000000000000265E-14, 2.000000000000000155E-15, -1.000000000000000000 ) ) ;
#76598 = CARTESIAN_POINT ( 'NONE',  ( 97.75828880830677292, -40.38464125964823381, 102.6242338216369774 ) ) ;
#76600 = DIRECTION ( 'NONE',  ( 0.000000000000000000, 0.000000000000000000, 1.000000000000000000 ) ) ;
#76599 = CARTESIAN_POINT ( 'NONE',  ( 182.0667039024469886, -33.35206098992630075, 342.9256252759119548 ) ) ;
#76601 = DIRECTION ( 'NONE',  ( -1.000000000000000078E-15, 1.000000000000000083E-30, 1.000000000000000000 ) ) ;
#76602 = DIRECTION ( 'NONE',  ( -0.7071067811865441310, 0.000000000000000000, -0.7071067811865510144 ) ) ;
#76603 = ORIENTED_EDGE ( 'NONE', *, *, #46536, .F. ) ;
#76604 = DIRECTION ( 'NONE',  ( 0.000000000000000000, 0.000000000000000000, -1.000000000000000000 ) ) ;
#76605 = AXIS2_PLACEMENT_3D ( 'NONE', #24877, #80304, #18053 ) ;
#76606 = CIRCLE ( 'NONE', #37431, 1.000000000000000888 ) ;
#76607 = VERTEX_POINT ( 'NONE', #68960 ) ;
#76608 = ORIENTED_EDGE ( 'NONE', *, *, #58820, .F. ) ;
#76609 = AXIS2_PLACEMENT_3D ( 'NONE', #74961, #68152, #39540 ) ;
#76610 = ORIENTED_EDGE ( 'NONE', *, *, #60747, .T. ) ;
#76611 = CARTESIAN_POINT ( 'NONE',  ( 96.36089708107968477, -41.75325360632972149, 57.67562527591096710 ) ) ;
#76612 = DIRECTION ( 'NONE',  ( -1.000000000000000078E-15, 1.000000000000000000, 0.000000000000000000 ) ) ;
#76613 = AXIS2_PLACEMENT_3D ( 'NONE', #25847, #72664, #59453 ) ;
#76614 = CYLINDRICAL_SURFACE ( 'NONE', #12272, 9.999999999999998224 ) ;
#76615 = CARTESIAN_POINT ( 'NONE',  ( 101.9507351169249887, -46.57965624409947480, 163.1832443235299763 ) ) ;
#76616 = VECTOR ( 'NONE', #53920, 1000.000000000000000 ) ;
#76617 = EDGE_CURVE ( 'NONE', #1814, #79502, #8078, .T. ) ;
#76618 = CARTESIAN_POINT ( 'NONE',  ( 116.3037889147421424, -33.73884459347697629, 283.4981341137910249 ) ) ;
#76619 = VERTEX_POINT ( 'NONE', #65274 ) ;
#76620 = ORIENTED_EDGE ( 'NONE', *, *, #86499, .T. ) ;
#76621 = ORIENTED_EDGE ( 'NONE', *, *, #57003, .F. ) ;
#76622 = DIRECTION ( 'NONE',  ( 2.900000000000000265E-14, -2.000000000000000155E-15, 1.000000000000000000 ) ) ;
#76623 = DIRECTION ( 'NONE',  ( 1.000000000000000078E-15, -1.000000000000000083E-30, -1.000000000000000000 ) ) ;
#76624 = CARTESIAN_POINT ( 'NONE',  ( 156.5667039024483529, -48.82844715993569196, 295.7178068554149490 ) ) ;
#76625 = CARTESIAN_POINT ( 'NONE',  ( 98.35015076301363024, -31.65606670507391840, 20.90547850657702611 ) ) ;
#76626 = CARTESIAN_POINT ( 'NONE',  ( 86.68005309089053867, 92.64985122628469583, 97.63151088911791931 ) ) ;
#76627 = DIRECTION ( 'NONE',  ( 1.825781832977096147E-16, 0.5000000000000003331, -0.8660254037844384856 ) ) ;
#76628 = DIRECTION ( 'NONE',  ( 1.000000000000000000, 0.000000000000000000, 2.671820169801660301E-13 ) ) ;
#76629 = CIRCLE ( 'NONE', #12827, 8.636000000000004562 ) ;
#76630 = CARTESIAN_POINT ( 'NONE',  ( 87.06648329127403940, -56.72944715994104570, -5.074374724089050659 ) ) ;
#76631 = CARTESIAN_POINT ( 'NONE',  ( 99.77739493559400330, -44.20163642594134501, 21.96133956162593748 ) ) ;
#76632 = CARTESIAN_POINT ( 'NONE',  ( 29.56648329127298069, -71.37844715994266664, 361.9756252759109998 ) ) ;
#76633 = VERTEX_POINT ( 'NONE', #51179 ) ;
#76634 = CARTESIAN_POINT ( 'NONE',  ( 181.8764988495240118, -33.54226604284930602, -5.074374724088000832 ) ) ;
#76635 = AXIS2_PLACEMENT_3D ( 'NONE', #37876, #65576, #3358 ) ;
#76636 = LINE ( 'NONE', #43433, #26449 ) ;
#76637 = CARTESIAN_POINT ( 'NONE',  ( 107.2657893863845260, -28.07721033202879113, 72.86428084578200526 ) ) ;
#76638 = EDGE_CURVE ( 'NONE', #38934, #7104, #57554, .T. ) ;
#76639 = DIRECTION ( 'NONE',  ( 1.000000000000000078E-15, 0.000000000000000000, 1.000000000000000000 ) ) ;
#76640 = PLANE ( 'NONE',  #58997 ) ;
#76641 = ORIENTED_EDGE ( 'NONE', *, *, #35434, .F. ) ;
#76642 = ORIENTED_EDGE ( 'NONE', *, *, #38096, .T. ) ;
#76643 = DIRECTION ( 'NONE',  ( 1.000000000000000078E-15, 0.000000000000000000, 1.000000000000000000 ) ) ;
#76644 = ORIENTED_EDGE ( 'NONE', *, *, #28247, .F. ) ;
#76645 = ORIENTED_EDGE ( 'NONE', *, *, #51403, .F. ) ;
#76646 = PRODUCT_DEFINITION ( 'UNKNOWN', '', #58056, #22399 ) ;
#76647 = CARTESIAN_POINT ( 'NONE',  ( 115.0372575196810061, -42.90846254905609669, 69.30229194431436213 ) ) ;
#76648 = CARTESIAN_POINT ( 'NONE',  ( 108.0961452412413166, -46.06846630830715128, 154.0834880678019374 ) ) ;
#76649 = VECTOR ( 'NONE', #79721, 1000.000000000000000 ) ;
#76650 = CARTESIAN_POINT ( 'NONE',  ( -7.746212673614270905, 92.64801822704207268, 118.3046725678181872 ) ) ;
#76651 = CARTESIAN_POINT ( 'NONE',  ( 116.6182342972125809, -29.67350615900649657, 105.3327681330539463 ) ) ;
#76652 = LINE ( 'NONE', #28490, #22724 ) ;
#76653 = AXIS2_PLACEMENT_3D ( 'NONE', #44629, #18725, #51441 ) ;
#76654 = ORIENTED_EDGE ( 'NONE', *, *, #67021, .T. ) ;
#76655 = VECTOR ( 'NONE', #16271, 1000.000000000000000 ) ;
#76656 = DIRECTION ( 'NONE',  ( -1.000000000000000000, 0.000000000000000000, 0.000000000000000000 ) ) ;
#76657 = VERTEX_POINT ( 'NONE', #51625 ) ;
#76658 = ORIENTED_EDGE ( 'NONE', *, *, #25364, .T. ) ;
#76659 = EDGE_CURVE ( 'NONE', #18961, #43071, #9416, .T. ) ;
#76660 = VECTOR ( 'NONE', #86935, 999.9999999999998863 ) ;
#76661 = DIRECTION ( 'NONE',  ( 0.000000000000000000, 1.000000000000000000, 0.000000000000000000 ) ) ;
#76662 = ORIENTED_EDGE ( 'NONE', *, *, #57972, .F. ) ;
#76663 = ADVANCED_FACE ( 'NONE', ( #72972 ), #85296, .T. ) ;
#76664 = CARTESIAN_POINT ( 'NONE',  ( 113.3428377330624954, -29.55695056567750711, 289.5032443235305664 ) ) ;
#76665 = CARTESIAN_POINT ( 'NONE',  ( 98.41694670496758590, -29.81058001376278099, 191.7775300378159784 ) ) ;
#76666 = DIRECTION ( 'NONE',  ( -4.299999999999999979E-14, 1.000000000000000000, -4.400000000000000367E-29 ) ) ;
#76667 = LINE ( 'NONE', #14450, #30038 ) ;
#76668 = EDGE_CURVE ( 'NONE', #14129, #73307, #37128, .T. ) ;
#76669 = CARTESIAN_POINT ( 'NONE',  ( 96.64197643737422538, -36.61924597882073584, 107.3184824187679567 ) ) ;
#76670 = CARTESIAN_POINT ( 'NONE',  ( 116.7951252736160086, -39.38782978119709810, 263.6147919432945059 ) ) ;
#76671 = EDGE_LOOP ( 'NONE', ( #31823, #22709 ) ) ;
#76672 = AXIS2_PLACEMENT_3D ( 'NONE', #61519, #61969, #60172 ) ;
#76673 = CARTESIAN_POINT ( 'NONE',  ( 97.33763774114136424, -34.07177809286157810, 116.1163881612916384 ) ) ;
#76674 = ADVANCED_FACE ( 'NONE', ( #8986, #24392, #85743, #64386, #64829, #15795, #50745, #38015, #65708, #71654 ), #38442, .T. ) ;
#76675 = VECTOR ( 'NONE', #21281, 1000.000000000000000 ) ;
#76676 = DIRECTION ( 'NONE',  ( -0.000000000000000000, 0.000000000000000000, -1.000000000000000000 ) ) ;
#76677 = ORIENTED_EDGE ( 'NONE', *, *, #39846, .T. ) ;
#76678 = CARTESIAN_POINT ( 'NONE',  ( 162.0667039024469886, -67.87844715994089029, 222.2178068554179902 ) ) ;
#76679 = CARTESIAN_POINT ( 'NONE',  ( 89.33314995793998037, 12.92155284005730387, 358.9756252759109998 ) ) ;
#76680 = CARTESIAN_POINT ( 'NONE',  ( 102.7552189479022928, -25.69072042043729098, 20.37276813305294354 ) ) ;
#76681 = DIRECTION ( 'NONE',  ( 0.000000000000000000, 0.000000000000000000, -1.000000000000000000 ) ) ;
#76682 = CARTESIAN_POINT ( 'NONE',  ( 141.0664832912739826, -8.729447159940995959, 14.67562527591100441 ) ) ;
#76683 = CARTESIAN_POINT ( 'NONE',  ( 45.76696975232854925, -48.62818131006066835, 300.4678068554150059 ) ) ;
#76684 = CARTESIAN_POINT ( 'NONE',  ( 111.1466539572802787, -45.61852150023370456, 27.91848241876893155 ) ) ;
#76686 = CARTESIAN_POINT ( 'NONE',  ( 98.47671751366520709, -30.86049585540216711, 116.8499109901969604 ) ) ;
#76685 = CARTESIAN_POINT ( 'NONE',  ( 97.78504508517835347, -40.45176323166522536, 111.6299858404451300 ) ) ;
#76687 = DIRECTION ( 'NONE',  ( 0.000000000000000000, 0.8660254037844387076, 0.4999999999999998890 ) ) ;
#76689 = ADVANCED_FACE ( 'NONE', ( #37575 ), #78480, .T. ) ;
#76688 = DIRECTION ( 'NONE',  ( -4.299999999999999979E-14, 1.000000000000000000, -4.400000000000000367E-29 ) ) ;
#76690 = ORIENTED_EDGE ( 'NONE', *, *, #52841, .T. ) ;
#76691 = LINE ( 'NONE', #43036, #33772 ) ;
#76692 = CARTESIAN_POINT ( 'NONE',  ( 109.2774118001976120, 53.97500000000000142, 71.43750000000000000 ) ) ;
#76693 = EDGE_CURVE ( 'NONE', #3831, #71161, #10739, .T. ) ;
#76694 = DIRECTION ( 'NONE',  ( 0.9068632946707805287, -0.4214249218767880389, 9.068632946707802473E-16 ) ) ;
#76695 = ORIENTED_EDGE ( 'NONE', *, *, #56459, .F. ) ;
#76696 = DIRECTION ( 'NONE',  ( 1.000000000000000000, 0.000000000000000000, 0.000000000000000000 ) ) ;
#76698 = ORIENTED_EDGE ( 'NONE', *, *, #74885, .T. ) ;
#76697 = CARTESIAN_POINT ( 'NONE',  ( 102.0297551351921044, -46.62107256275958633, 172.2137205140059564 ) ) ;
#76699 = CYLINDRICAL_SURFACE ( 'NONE', #5986, 2.030000000002086580 ) ;
#76700 = CARTESIAN_POINT ( 'NONE',  ( 117.7987307161850907, -31.64603138916173464, 210.1784824187679703 ) ) ;
#76701 = CARTESIAN_POINT ( 'NONE',  ( 110.4707641138770668, -47.29393344369797347, 53.83657765686300678 ) ) ;
#76702 = CARTESIAN_POINT ( 'NONE',  ( 91.12742965730937783, 69.93364840292896645, 93.49502539975293303 ) ) ;
#76703 = DIRECTION ( 'NONE',  ( 0.5773502691896202910, 0.5773502691896288397, -0.5773502691896282846 ) ) ;
#76704 = VECTOR ( 'NONE', #45315, 1000.000000000000000 ) ;
#76705 = DIRECTION ( 'NONE',  ( 0.000000000000000000, 0.000000000000000000, -1.000000000000000000 ) ) ;
#76706 = VERTEX_POINT ( 'NONE', #3054 ) ;
#76707 = ORIENTED_EDGE ( 'NONE', *, *, #76874, .F. ) ;
#76708 = ORIENTED_EDGE ( 'NONE', *, *, #86010, .T. ) ;
#76709 = VERTEX_POINT ( 'NONE', #78920 ) ;
#76710 = FACE_OUTER_BOUND ( 'NONE', #35715, .T. ) ;
#76711 = CARTESIAN_POINT ( 'NONE',  ( 116.5266666817545627, -41.19333145446972821, 224.4756252759109714 ) ) ;
#76712 = DIRECTION ( 'NONE',  ( 0.000000000000000000, 0.000000000000000000, -1.000000000000000000 ) ) ;
#76713 = DIRECTION ( 'NONE',  ( 1.000000000000000000, 0.000000000000000000, 0.000000000000000000 ) ) ;
#76714 = AXIS2_PLACEMENT_3D ( 'NONE', #78279, #51860, #59129 ) ;
#76716 = CARTESIAN_POINT ( 'NONE',  ( 41.56648329127398966, -27.57844715994070484, 135.9256252759119832 ) ) ;
#76715 = FACE_OUTER_BOUND ( 'NONE', #21145, .T. ) ;
#76717 = DIRECTION ( 'NONE',  ( 0.000000000000000000, 0.000000000000000000, 1.000000000000000000 ) ) ;
#76718 = EDGE_CURVE ( 'NONE', #68380, #47694, #22076, .T. ) ;
#76719 = CARTESIAN_POINT ( 'NONE',  ( 106.5169308145888607, -25.66629059357601506, 45.12800622829193742 ) ) ;
#76720 = VERTEX_POINT ( 'NONE', #3488 ) ;
#76721 = VECTOR ( 'NONE', #82320, 1000.000000000000000 ) ;
#76723 = EDGE_LOOP ( 'NONE', ( #79911, #26121, #45629, #5775 ) ) ;
#76722 = CIRCLE ( 'NONE', #67960, 7.937500000000000000 ) ;
#76724 = DIRECTION ( 'NONE',  ( -3.100000000000000258E-29, 3.100000000000000044E-14, 1.000000000000000000 ) ) ;
#76725 = EDGE_CURVE ( 'NONE', #78995, #19810, #30805, .T. ) ;
#76726 = CARTESIAN_POINT ( 'NONE',  ( 116.2779988688839552, -41.49250982992358416, 239.4346728949579699 ) ) ;
#76727 = CARTESIAN_POINT ( 'NONE',  ( 182.4202572930400095, -33.70561438051981185, -5.074374724088000832 ) ) ;
#76728 = VECTOR ( 'NONE', #89165, 1000.000000000000000 ) ;
#76729 = CARTESIAN_POINT ( 'NONE',  ( 116.7343647603065619, -32.97833357388816466, 90.10895860924395606 ) ) ;
#76730 = DIRECTION ( 'NONE',  ( 0.000000000000000000, 0.000000000000000000, -1.000000000000000000 ) ) ;
#76731 = AXIS2_PLACEMENT_3D ( 'NONE', #71503, #23361, #10588 ) ;
#76732 = CARTESIAN_POINT ( 'NONE',  ( -76.71224887342795284, 55.42750769018135060, 30.85235132533246372 ) ) ;
#76733 = ORIENTED_EDGE ( 'NONE', *, *, #89297, .F. ) ;
#76734 = CARTESIAN_POINT ( 'NONE',  ( 172.5664832912740110, -18.82844715994099971, 141.0426252759120018 ) ) ;
#76735 = ORIENTED_EDGE ( 'NONE', *, *, #55345, .T. ) ;
#76736 = EDGE_LOOP ( 'NONE', ( #3939, #45307 ) ) ;
#76737 = CARTESIAN_POINT ( 'NONE',  ( -105.4788588808464027, 120.6499999999999915, 3.968749999998844924 ) ) ;
#76738 = CARTESIAN_POINT ( 'NONE',  ( 114.4699299399979395, -31.85941057575024971, 250.7215833058968997 ) ) ;
#76739 = CARTESIAN_POINT ( 'NONE',  ( -215.9000000000000057, 101.5999999999999943, 146.9389999999999930 ) ) ;
#76740 = EDGE_CURVE ( 'NONE', #74351, #12839, #43468, .T. ) ;
#76741 = CARTESIAN_POINT ( 'NONE',  ( 99.09558145272080765, -30.55060196207903900, 140.8023086913604232 ) ) ;
#76742 = DIRECTION ( 'NONE',  ( -1.000000000000000078E-15, 0.000000000000000000, -1.000000000000000000 ) ) ;
#76743 = CARTESIAN_POINT ( 'NONE',  ( 83.24493215373414046, 69.84937538953985836, -84.41866557162641982 ) ) ;
#76744 = VERTEX_POINT ( 'NONE', #84841 ) ;
#76745 = CARTESIAN_POINT ( 'NONE',  ( 114.6444261855608175, -117.4034471599418055, -11.78219314458159239 ) ) ;
#76746 = FACE_OUTER_BOUND ( 'NONE', #10627, .T. ) ;
#76747 = ORIENTED_EDGE ( 'NONE', *, *, #26265, .F. ) ;
#76748 = CARTESIAN_POINT ( 'NONE',  ( 95.25894796463062164, -35.71821259427313322, 36.25848241876794731 ) ) ;
#76749 = ORIENTED_EDGE ( 'NONE', *, *, #27585, .T. ) ;
#76750 = CARTESIAN_POINT ( 'NONE',  ( 99.16797791762762415, -38.78938375721887155, 274.3480903695913184 ) ) ;
#76751 = CARTESIAN_POINT ( 'NONE',  ( 97.81168895331838087, -40.51742574516882200, 287.6356252759109680 ) ) ;
#76752 = CARTESIAN_POINT ( 'NONE',  ( 114.4888877093246293, -29.48743791597849651, 194.4537205140069318 ) ) ;
#76753 = LINE ( 'NONE', #55829, #14298 ) ;
#76754 = CARTESIAN_POINT ( 'NONE',  ( 0.000000000000000000, 124.5870000000000033, 0.000000000000000000 ) ) ;
#76755 = DIRECTION ( 'NONE',  ( 0.000000000000000000, 0.000000000000000000, 1.000000000000000000 ) ) ;
#76756 = CARTESIAN_POINT ( 'NONE',  ( 7.108806956920044051, 72.02595942673482909, 130.3623174704088115 ) ) ;
#76757 = VECTOR ( 'NONE', #21564, 1000.000000000000000 ) ;
#76758 = CARTESIAN_POINT ( 'NONE',  ( 105.3167593786310903, -26.43023667424511913, 11.20991099019697046 ) ) ;
#76759 = LINE ( 'NONE', #34964, #45631 ) ;
#76760 = ORIENTED_EDGE ( 'NONE', *, *, #62995, .T. ) ;
#76761 = CARTESIAN_POINT ( 'NONE',  ( 147.9173672921288869, -72.54391775211570348, 542.9756252759101471 ) ) ;
#76762 = ORIENTED_EDGE ( 'NONE', *, *, #26702, .F. ) ;
#76763 = CARTESIAN_POINT ( 'NONE',  ( 116.9629591039797845, -33.20839883953882321, 110.0984824187679578 ) ) ;
#76764 = CARTESIAN_POINT ( 'NONE',  ( 124.1536575006588379, 45.91621576730522492, -40.38304405550843512 ) ) ;
#76765 = ORIENTED_EDGE ( 'NONE', *, *, #15989, .F. ) ;
#76766 = LINE ( 'NONE', #37109, #12446 ) ;
#76767 = EDGE_LOOP ( 'NONE', ( #67484, #11837, #13646, #82194, #74643, #53429, #45256, #11175, #44634, #38332, #25592, #25460, #49, #42441, #72931, #12074 ) ) ;
#76768 = ORIENTED_EDGE ( 'NONE', *, *, #79758, .F. ) ;
#76769 = CARTESIAN_POINT ( 'NONE',  ( 62.03742497533659872, -23.42844715994045401, 117.4678068554150485 ) ) ;
#76770 = CARTESIAN_POINT ( 'NONE',  ( -77.39114642430010349, 120.6499999999999915, 71.77848634863050847 ) ) ;
#76771 = LINE ( 'NONE', #14558, #5079 ) ;
#76772 = DIRECTION ( 'NONE',  ( -0.7071067811865475727, 0.000000000000000000, -0.7071067811865475727 ) ) ;
#76773 = CARTESIAN_POINT ( 'NONE',  ( 0.000000000000000000, 210.0000000000000000, 154.6557476874258441 ) ) ;
#76774 = EDGE_CURVE ( 'NONE', #52430, #7253, #52056, .T. ) ;
#76775 = CARTESIAN_POINT ( 'NONE',  ( 108.9290709455192570, -28.27771998284391231, 177.7099951314959583 ) ) ;
#76776 = CARTESIAN_POINT ( 'NONE',  ( 97.59563580048326514, -41.13856347273024738, 252.6727681330536655 ) ) ;
#76777 = CARTESIAN_POINT ( 'NONE',  ( 188.5667039024479834, -65.37844715994100397, 288.3428068554150059 ) ) ;
#76778 = ORIENTED_EDGE ( 'NONE', *, *, #74021, .F. ) ;
#76779 = FACE_OUTER_BOUND ( 'NONE', #15664, .T. ) ;
#76780 = VECTOR ( 'NONE', #77051, 1000.000000000000000 ) ;
#76781 = DIRECTION ( 'NONE',  ( 0.000000000000000000, 0.000000000000000000, -1.000000000000000000 ) ) ;
#76782 = VERTEX_POINT ( 'NONE', #29420 ) ;
#76783 = VERTEX_POINT ( 'NONE', #57098 ) ;
#76784 = AXIS2_PLACEMENT_3D ( 'NONE', #10367, #44875, #9929 ) ;
#76785 = AXIS2_PLACEMENT_3D ( 'NONE', #21807, #447, #76755 ) ;
#76786 = DIRECTION ( 'NONE',  ( 0.000000000000000000, 0.000000000000000000, -1.000000000000000000 ) ) ;
#76787 = CARTESIAN_POINT ( 'NONE',  ( 162.9033555647770015, -33.89581943344391135, -5.074374724088000832 ) ) ;
#76788 = CARTESIAN_POINT ( 'NONE',  ( 7.661254700127833495, 69.45253841614081125, 317.6630000000000109 ) ) ;
#76789 = DIRECTION ( 'NONE',  ( -1.000000000000000000, 0.000000000000000000, 0.000000000000000000 ) ) ;
#76790 = CARTESIAN_POINT ( 'NONE',  ( 149.4430470701762772, -12.91565541735124256, 394.9756252759100903 ) ) ;
#76791 = CARTESIAN_POINT ( 'NONE',  ( 107.9802517323619355, -45.22186489331556203, 202.0838483995049728 ) ) ;
#76792 = CARTESIAN_POINT ( 'NONE',  ( 103.3467460430879612, -47.18776626161088927, 102.3165776568629752 ) ) ;
#76793 = ORIENTED_EDGE ( 'NONE', *, *, #56252, .T. ) ;
#76795 = ADVANCED_FACE ( 'NONE', ( #50283 ), #11937, .F. ) ;
#76794 = CARTESIAN_POINT ( 'NONE',  ( 131.4622572338305986, -19.61690131752980903, 6.952852217890792552 ) ) ;
#76796 = ORIENTED_EDGE ( 'NONE', *, *, #17170, .F. ) ;
#76797 = VECTOR ( 'NONE', #51932, 1000.000000000000000 ) ;
#76798 = ADVANCED_FACE ( 'NONE', ( #2161, #29871 ), #87955, .F. ) ;
#76799 = CARTESIAN_POINT ( 'NONE',  ( 130.0664832912740110, -18.82844715994099971, 199.5838068554170093 ) ) ;
#76800 = EDGE_LOOP ( 'NONE', ( #76001, #65370 ) ) ;
#76801 = CARTESIAN_POINT ( 'NONE',  ( 99.09532346176355588, -30.55094594719723133, 261.8023343508735366 ) ) ;
#76802 = ORIENTED_EDGE ( 'NONE', *, *, #13308, .F. ) ;
#76803 = DIRECTION ( 'NONE',  ( -0.000000000000000000, 1.000000000000000000, -0.000000000000000000 ) ) ;
#76804 = AXIS2_PLACEMENT_3D ( 'NONE', #67406, #47851, #66969 ) ;
#76805 = FACE_BOUND ( 'NONE', #69973, .T. ) ;
#76806 = CARTESIAN_POINT ( 'NONE',  ( 73.06648329127358465, -8.729447159940534107, -4.970821333494978234 ) ) ;
#76807 = DIRECTION ( 'NONE',  ( -1.087812297297669405E-15, 1.000000000000000000, -3.100000000000000044E-14 ) ) ;
#76808 = ORIENTED_EDGE ( 'NONE', *, *, #81057, .F. ) ;
#76809 = CARTESIAN_POINT ( 'NONE',  ( 96.90545716317438973, -39.15842060370329847, 56.51276813305394597 ) ) ;
#76810 =( NAMED_UNIT ( * ) SI_UNIT ( $, .STERADIAN. ) SOLID_ANGLE_UNIT ( ) );
#76812 = CARTESIAN_POINT ( 'NONE',  ( 96.71266027437765445, 71.53177522571071734, -87.70409100286326520 ) ) ;
#76811 = LINE ( 'NONE', #6423, #75354 ) ;
#76813 = CARTESIAN_POINT ( 'NONE',  ( -487.2989999999999782, 7.143750000000280487, 15.23694598552305024 ) ) ;
#76814 = CARTESIAN_POINT ( 'NONE',  ( 103.1875000000000000, 127.0000000000000000, -7.143749999999640110 ) ) ;
#76815 = ORIENTED_EDGE ( 'NONE', *, *, #20878, .F. ) ;
#76816 = VECTOR ( 'NONE', #32987, 1000.000000000000000 ) ;
#76817 = LINE ( 'NONE', #43172, #63432 ) ;
#76818 = DIRECTION ( 'NONE',  ( 1.075267683398002218E-15, -1.000000000000000000, 3.100000000000000044E-14 ) ) ;
#76819 = DIRECTION ( 'NONE',  ( 0.9999999853157766072, 0.0001713722456127291416, -9.999999853157765648E-16 ) ) ;
#76820 = CARTESIAN_POINT ( 'NONE',  ( 10.08473622792051039, 74.81935728795534146, 118.1266015380916912 ) ) ;
#76821 = CARTESIAN_POINT ( 'NONE',  ( 99.03746950336261534, -43.41317339962571253, 112.8784824187679732 ) ) ;
#76823 = CARTESIAN_POINT ( 'NONE',  ( 76.06670390244703128, -104.2784471599409812, 45.21780685541799727 ) ) ;
#76822 = LINE ( 'NONE', #69563, #11680 ) ;
#76824 = DIRECTION ( 'NONE',  ( -4.237773401492740281E-14, 1.000000000000000000, 0.000000000000000000 ) ) ;
#76825 = AXIS2_PLACEMENT_3D ( 'NONE', #26466, #60518, #25562 ) ;
#76826 = VERTEX_POINT ( 'NONE', #39781 ) ;
#76827 = CARTESIAN_POINT ( 'NONE',  ( 74.06670390244701707, -90.27844715994098124, 230.7030882296565721 ) ) ;
#76828 = CARTESIAN_POINT ( 'NONE',  ( 97.31342953368671544, -35.99458159538090030, 142.2670538473389570 ) ) ;
#76830 = ORIENTED_EDGE ( 'NONE', *, *, #12658, .T. ) ;
#76829 = CYLINDRICAL_SURFACE ( 'NONE', #2197, 9.999999999999998224 ) ;
#76831 = AXIS2_PLACEMENT_3D ( 'NONE', #74165, #6035, #47331 ) ;
#76832 = CARTESIAN_POINT ( 'NONE',  ( 100.1919508713739759, -45.35525880799009713, 268.0289586092443415 ) ) ;
#76833 = CARTESIAN_POINT ( 'NONE',  ( 213.1962561210690126, 52.73749999999999716, -47.62500000000000000 ) ) ;
#76834 = FACE_OUTER_BOUND ( 'NONE', #82917, .T. ) ;
#76835 = CARTESIAN_POINT ( 'NONE',  ( 82.81648064515530905, -18.72944715939135207, 6.749772901088279653 ) ) ;
#76836 = DIRECTION ( 'NONE',  ( 1.047445008332813989E-14, 0.000000000000000000, -1.000000000000000000 ) ) ;
#76837 = CIRCLE ( 'NONE', #88457, 11.57110091390439699 ) ;
#76838 = CARTESIAN_POINT ( 'NONE',  ( 69.57145439714845736, -138.4421226178978941, 247.5996244233720063 ) ) ;
#76839 = FACE_OUTER_BOUND ( 'NONE', #49528, .T. ) ;
#76840 = CARTESIAN_POINT ( 'NONE',  ( 115.7764676695378512, -43.63945112744040955, 198.2927681330539542 ) ) ;
#76841 = ORIENTED_EDGE ( 'NONE', *, *, #36867, .F. ) ;
#76842 = VERTEX_POINT ( 'NONE', #53392 ) ;
#76843 = VECTOR ( 'NONE', #69870, 1000.000000000000000 ) ;
#76844 = CARTESIAN_POINT ( 'NONE',  ( 117.1402439185659006, -36.89830975172036887, 150.2444404487539487 ) ) ;
#76845 = CIRCLE ( 'NONE', #49270, 7.937500000000000000 ) ;
#76846 = DIRECTION ( 'NONE',  ( -2.900000000000000265E-14, 2.000000000000000155E-15, -1.000000000000000000 ) ) ;
#76847 = EDGE_CURVE ( 'NONE', #53694, #29605, #32978, .T. ) ;
#76848 = CARTESIAN_POINT ( 'NONE',  ( 116.8725690376871569, -36.55701438716827312, 284.8413395616245793 ) ) ;
#76849 = CARTESIAN_POINT ( 'NONE',  ( 37.36643805256671413, -48.62818131006081046, 300.4678068554150059 ) ) ;
#76850 = EDGE_CURVE ( 'NONE', #73636, #59995, #59336, .T. ) ;
#76851 = CARTESIAN_POINT ( 'NONE',  ( 117.0720588755466025, -35.46383719571640825, 268.9274440218657105 ) ) ;
#76853 = EDGE_CURVE ( 'NONE', #37391, #86124, #81611, .T. ) ;
#76852 = CIRCLE ( 'NONE', #30444, 2.117000000000007987 ) ;
#76854 = LINE ( 'NONE', #35500, #40077 ) ;
#76855 = CYLINDRICAL_SURFACE ( 'NONE', #82676, 7.499999999999996447 ) ;
#76856 = CARTESIAN_POINT ( 'NONE',  ( 90.44969454456408187, -53.34645651782490461, 239.5838068554174356 ) ) ;
#76858 = CARTESIAN_POINT ( 'NONE',  ( 97.07914014679025172, -41.41098531455293141, 211.6632443235299945 ) ) ;
#76857 = AXIS2_PLACEMENT_3D ( 'NONE', #81307, #53987, #19952 ) ;
#76859 = DIRECTION ( 'NONE',  ( 1.000000000000000000, 4.163336342344333240E-14, 0.000000000000000000 ) ) ;
#76860 = ORIENTED_EDGE ( 'NONE', *, *, #68466, .F. ) ;
#76861 = ORIENTED_EDGE ( 'NONE', *, *, #62829, .T. ) ;
#76862 = EDGE_CURVE ( 'NONE', #50856, #2257, #3259, .T. ) ;
#76863 = ADVANCED_FACE ( 'NONE', ( #67054 ), #24830, .F. ) ;
#76864 = DIRECTION ( 'NONE',  ( 1.000000000000000000, 0.000000000000000000, -9.299908063537909262E-17 ) ) ;
#76865 = CARTESIAN_POINT ( 'NONE',  ( -80.04418453221599350, 94.12556101775332706, -87.45628510944642642 ) ) ;
#76866 = AXIS2_PLACEMENT_3D ( 'NONE', #69292, #61556, #89293 ) ;
#76867 = DIRECTION ( 'NONE',  ( 0.000000000000000000, 0.000000000000000000, 1.000000000000000000 ) ) ;
#76868 = DIRECTION ( 'NONE',  ( 3.100000000000000258E-29, -3.100000000000000044E-14, -1.000000000000000000 ) ) ;
#76869 = EDGE_CURVE ( 'NONE', #66435, #42743, #11654, .T. ) ;
#76870 = CARTESIAN_POINT ( 'NONE',  ( 165.6738106836199904, -26.00627455219321860, -5.074374724088000832 ) ) ;
#76871 = EDGE_CURVE ( 'NONE', #17132, #19112, #81160, .T. ) ;
#76872 = ORIENTED_EDGE ( 'NONE', *, *, #66652, .F. ) ;
#76873 = DIRECTION ( 'NONE',  ( -1.000000000000000000, 0.000000000000000000, -1.748382715945130038E-14 ) ) ;
#76874 = EDGE_CURVE ( 'NONE', #48829, #38962, #55417, .T. ) ;
#76875 = CARTESIAN_POINT ( 'NONE',  ( 118.0818320075808856, -32.35879749485835788, 249.1270538473389706 ) ) ;
#76876 = EDGE_LOOP ( 'NONE', ( #16217, #10329, #80094, #49378, #34630, #61573 ) ) ;
#76877 = CIRCLE ( 'NONE', #7242, 2.517500000000005844 ) ;
#76878 = CARTESIAN_POINT ( 'NONE',  ( 176.7669697523282935, -48.62818131005432321, 300.4678068554149490 ) ) ;
#76879 = CARTESIAN_POINT ( 'NONE',  ( 29.56670390244828184, -48.82844715994152551, 300.4678068554150059 ) ) ;
#76880 = DIRECTION ( 'NONE',  ( 0.000000000000000000, 0.000000000000000000, -1.000000000000000000 ) ) ;
#76881 = ADVANCED_FACE ( 'NONE', ( #4834 ), #80258, .T. ) ;
#76882 = CARTESIAN_POINT ( 'NONE',  ( 115.5682441604615178, -40.44643428488449644, 56.31666179816296847 ) ) ;
#76883 = CARTESIAN_POINT ( 'NONE',  ( 102.8351866564443924, -46.28106417705388509, 173.2441967044829596 ) ) ;
#76884 = CARTESIAN_POINT ( 'NONE',  ( 67.65734841870819594, 69.84999999999999432, 346.9005000000000223 ) ) ;
#76885 = ORIENTED_EDGE ( 'NONE', *, *, #89380, .F. ) ;
#76886 = FACE_BOUND ( 'NONE', #87694, .T. ) ;
#76887 = VECTOR ( 'NONE', #38196, 1000.000000000000000 ) ;
#76888 = EDGE_LOOP ( 'NONE', ( #70469, #77005, #35137, #33232, #41891, #40069, #27770, #47376, #21690, #62771, #79777, #65005, #77747, #48030, #87695, #49012 ) ) ;
#76889 = EDGE_LOOP ( 'NONE', ( #26845, #67631, #73875, #52720 ) ) ;
#76890 = CARTESIAN_POINT ( 'NONE',  ( 6.710838307577478012, 93.34022857041041732, 118.3664257206621357 ) ) ;
#76891 = ORIENTED_EDGE ( 'NONE', *, *, #59421, .F. ) ;
#76892 = ORIENTED_EDGE ( 'NONE', *, *, #30816, .F. ) ;
#76893 = CARTESIAN_POINT ( 'NONE',  ( -72.96458098368600531, 117.4749999999999943, -72.96458098368781009 ) ) ;
#76894 = LINE ( 'NONE', #12093, #73594 ) ;
#76895 = CARTESIAN_POINT ( 'NONE',  ( 98.06318007301436523, -37.70576754076741821, 80.82289601855296723 ) ) ;
#76896 = CARTESIAN_POINT ( 'NONE',  ( 96.75420216176078725, -40.77324476150559462, 246.6118157521009664 ) ) ;
#76897 = EDGE_CURVE ( 'NONE', #84365, #17889, #18906, .T. ) ;
#76898 = CARTESIAN_POINT ( 'NONE',  ( 117.2062538965840304, -41.07097622818930915, 213.5165776568629781 ) ) ;
#76899 = DIRECTION ( 'NONE',  ( 0.000000000000000000, 1.000000000000000000, 0.000000000000000000 ) ) ;
#76900 = DIRECTION ( 'NONE',  ( 0.7071067811865491270, -0.7071067811865459074, 7.071067811865492096E-16 ) ) ;
#76901 = EDGE_CURVE ( 'NONE', #14672, #46763, #26391, .T. ) ;
#76902 = AXIS2_PLACEMENT_3D ( 'NONE', #70919, #29128, #35468 ) ;
#76903 = VERTEX_POINT ( 'NONE', #3935 ) ;
#76904 = DIRECTION ( 'NONE',  ( 0.7071067811571405404, 0.7071067812159546051, 0.000000000000000000 ) ) ;
#76905 = EDGE_CURVE ( 'NONE', #86581, #29066, #74328, .T. ) ;
#76906 = DIRECTION ( 'NONE',  ( -0.7967329428042217998, 0.6043315462976631691, -1.908195823574488750E-14 ) ) ;
#76907 = FACE_OUTER_BOUND ( 'NONE', #14933, .T. ) ;
#76908 = AXIS2_PLACEMENT_3D ( 'NONE', #3290, #44594, #50526 ) ;
#76909 = CARTESIAN_POINT ( 'NONE',  ( 114.2951562036313646, -44.16484043540982185, 118.2022919425779719 ) ) ;
#76910 = CARTESIAN_POINT ( 'NONE',  ( 97.24697957573494023, -33.09846756419045022, 66.04419670448297097 ) ) ;
#76911 = CARTESIAN_POINT ( 'NONE',  ( 105.7708979221677197, -26.34060099707374292, 270.1756252759109884 ) ) ;
#76912 = ORIENTED_EDGE ( 'NONE', *, *, #26557, .T. ) ;
#76913 = CARTESIAN_POINT ( 'NONE',  ( 114.6056301357651819, -29.52887111919123697, 234.4327681330539690 ) ) ;
#76914 = CARTESIAN_POINT ( 'NONE',  ( 107.0664832912739399, -48.47944715994096043, 307.1356252759109680 ) ) ;
#76915 = SURFACE_STYLE_USAGE ( .BOTH. , #56904 ) ;
#76916 = CARTESIAN_POINT ( 'NONE',  ( 116.3244028009478797, -32.94573790848593120, 95.13562527591096796 ) ) ;
#76917 = CARTESIAN_POINT ( 'NONE',  ( 62.03715912545739286, -47.82818131006020934, 180.4678068554151196 ) ) ;
#76919 = CARTESIAN_POINT ( 'NONE',  ( 68.71165106495583075, -139.2855573909722011, 245.9906543998875748 ) ) ;
#76918 = CARTESIAN_POINT ( 'NONE',  ( 126.0667039024479266, -14.72944715994094977, 239.5838068554170377 ) ) ;
#76920 = DIRECTION ( 'NONE',  ( 1.000000000000000000, 0.000000000000000000, 0.000000000000000000 ) ) ;
#76921 = CARTESIAN_POINT ( 'NONE',  ( 107.0667039024470313, -104.2784471599409528, 55.21780685541800437 ) ) ;
#76922 = CARTESIAN_POINT ( 'NONE',  ( 5.624880194777466258, 93.94404932077411274, -118.4230601929072435 ) ) ;
#76923 = VECTOR ( 'NONE', #63703, 1000.000000000000000 ) ;
#76924 = CARTESIAN_POINT ( 'NONE',  ( -11.00078833628931818, 88.90974477516434149, 130.0918550420129236 ) ) ;
#76925 = PRODUCT_DEFINITION_FORMATION_WITH_SPECIFIED_SOURCE ( 'ANY', '', #1904, .NOT_KNOWN. ) ;
#76926 = CARTESIAN_POINT ( 'NONE',  ( 98.34985888773255169, -31.65658485141074152, 11.90645861297915076 ) ) ;
#76927 = DIRECTION ( 'NONE',  ( 0.000000000000000000, 0.000000000000000000, 1.000000000000000000 ) ) ;
#76929 = EDGE_LOOP ( 'NONE', ( #22067, #8382, #68215, #59801, #13203 ) ) ;
#76928 = CARTESIAN_POINT ( 'NONE',  ( 116.3135889066590636, -32.94480564983713577, 259.1356252759109680 ) ) ;
#76930 = CARTESIAN_POINT ( 'NONE',  ( -105.4788588808462038, 127.0000000000000000, -3.968750000001139977 ) ) ;
#76931 = CARTESIAN_POINT ( 'NONE',  ( 101.2817000042767148, -26.35783695576231267, 255.4813395616251626 ) ) ;
#76932 = CARTESIAN_POINT ( 'NONE',  ( 113.0769238478409449, -28.21140209294909695, 125.5870538473399591 ) ) ;
#76933 = CARTESIAN_POINT ( 'NONE',  ( 104.7308122791112908, -47.55672043936114335, 28.41943479971997988 ) ) ;
#76934 = VECTOR ( 'NONE', #18136, 1000.000000000000000 ) ;
#76935 = DIRECTION ( 'NONE',  ( 0.000000000000000000, -1.000000000000000000, 0.000000000000000000 ) ) ;
#76937 = CARTESIAN_POINT ( 'NONE',  ( 82.79786375350262517, -36.40984252624630102, 6.777538624683718815 ) ) ;
#76936 = CARTESIAN_POINT ( 'NONE',  ( 113.7762091862918226, -33.98316268565083220, -2.114374724089040924 ) ) ;
#76938 = LINE ( 'NONE', #28790, #58139 ) ;
#76939 = VERTEX_POINT ( 'NONE', #18004 ) ;
#76940 = CARTESIAN_POINT ( 'NONE',  ( 124.7998166246059810, 12.92155284005730387, 361.9756252759109998 ) ) ;
#76941 = ORIENTED_EDGE ( 'NONE', *, *, #80928, .F. ) ;
#76942 = CIRCLE ( 'NONE', #58067, 130.5560000000000116 ) ;
#76943 = CARTESIAN_POINT ( 'NONE',  ( 99.77605516222793369, -32.27907757783855658, 170.3124198280769974 ) ) ;
#76945 = EDGE_LOOP ( 'NONE', ( #59431, #55143, #48834, #88886 ) ) ;
#76944 = CARTESIAN_POINT ( 'NONE',  ( -50.35902679310718355, 64.60000000000000853, 27.95514712793348977 ) ) ;
#76946 = LINE ( 'NONE', #7454, #37361 ) ;
#76947 = CARTESIAN_POINT ( 'NONE',  ( 117.4654710391979222, -40.40706546494229201, 174.5680062282919778 ) ) ;
#76948 = CARTESIAN_POINT ( 'NONE',  ( 223.2659999999999911, 52.73749999999999716, -56.89600000000000080 ) ) ;
#76949 = CARTESIAN_POINT ( 'NONE',  ( 99.09591451443299093, -30.55015794387348649, 150.8027366674846235 ) ) ;
#76950 = DIRECTION ( 'NONE',  ( 0.000000000000000000, 1.000000000000000000, 0.000000000000000000 ) ) ;
#76951 = CARTESIAN_POINT ( 'NONE',  ( -84.43201024598403137, 69.85063172184841562, 83.23139715273285333 ) ) ;
#76952 = DIRECTION ( 'NONE',  ( 1.000000000000000000, 0.000000000000000000, 0.000000000000000000 ) ) ;
#76953 = CARTESIAN_POINT ( 'NONE',  ( 113.4367438382844284, -44.15125393826594546, 108.1413395616259692 ) ) ;
#76954 = VERTEX_POINT ( 'NONE', #87064 ) ;
#76955 = VECTOR ( 'NONE', #46672, 1000.000000000000000 ) ;
#76956 = VERTEX_POINT ( 'NONE', #45685 ) ;
#76957 = VERTEX_POINT ( 'NONE', #11189 ) ;
#76958 = CARTESIAN_POINT ( 'NONE',  ( 111.1996377132626748, -28.89074107182586815, 56.12158330589694799 ) ) ;
#76959 = CARTESIAN_POINT ( 'NONE',  ( 45.76696975232782449, -48.62818131005837330, 249.9678068554150343 ) ) ;
#76961 = DIRECTION ( 'NONE',  ( 0.000000000000000000, 1.000000000000000000, 0.000000000000000000 ) ) ;
#76960 = CARTESIAN_POINT ( 'NONE',  ( 101.7740290765682829, -45.64733444449320388, 203.1622919425769567 ) ) ;
#76962 = CARTESIAN_POINT ( 'NONE',  ( -103.1875000000000000, 117.4749999999999943, -7.937500000001080913 ) ) ;
#76963 = EDGE_CURVE ( 'NONE', #6159, #29190, #84710, .T. ) ;
#76964 = CARTESIAN_POINT ( 'NONE',  ( 188.5667039024479834, -48.82844715994099971, 137.2178068554150059 ) ) ;
#76965 = ADVANCED_FACE ( 'NONE', ( #47933 ), #48374, .F. ) ;
#76966 = CARTESIAN_POINT ( 'NONE',  ( 107.0667039024470313, -104.2784471599413934, 2.217806855418003043 ) ) ;
#76967 = EDGE_CURVE ( 'NONE', #34717, #28582, #88790, .T. ) ;
#76968 = DIRECTION ( 'NONE',  ( 0.000000000000000000, 0.000000000000000000, 1.000000000000000000 ) ) ;
#76969 = CARTESIAN_POINT ( 'NONE',  ( 67.07577529756494528, -67.88575619384793924, 245.6832122914381387 ) ) ;
#76970 = CARTESIAN_POINT ( 'NONE',  ( 95.69905522618344662, -33.46911247776736786, 141.1041967044829732 ) ) ;
#76971 = EDGE_LOOP ( 'NONE', ( #65965, #85522, #82600, #31674, #62263, #53275 ) ) ;
#76972 = ORIENTED_EDGE ( 'NONE', *, *, #80664, .F. ) ;
#76973 = VERTEX_POINT ( 'NONE', #70195 ) ;
#76974 = AXIS2_PLACEMENT_3D ( 'NONE', #77275, #1870, #35925 ) ;
#76975 = EDGE_CURVE ( 'NONE', #48113, #10930, #76108, .T. ) ;
#76976 = EDGE_CURVE ( 'NONE', #4752, #82826, #56090, .T. ) ;
#76977 = SURFACE_SIDE_STYLE ('',( #42429 ) ) ;
#76978 = LINE ( 'NONE', #56052, #47584 ) ;
#76979 = CARTESIAN_POINT ( 'NONE',  ( 116.3254862984629909, -32.93730789470958342, 129.1356252759109680 ) ) ;
#76980 = DIRECTION ( 'NONE',  ( -0.7071067811865774377, 0.7071067811865175967, -7.071067811865782003E-16 ) ) ;
#76981 = CARTESIAN_POINT ( 'NONE',  ( 107.5268921225462719, -45.37172398690709230, 195.4490427505439811 ) ) ;
#76982 = VECTOR ( 'NONE', #46379, 1000.000000000000000 ) ;
#76983 = EDGE_CURVE ( 'NONE', #30351, #5575, #14799, .T. ) ;
#76984 = FACE_OUTER_BOUND ( 'NONE', #6777, .T. ) ;
#76985 = EDGE_CURVE ( 'NONE', #8401, #82562, #26130, .T. ) ;
#76986 = CARTESIAN_POINT ( 'NONE',  ( 97.81193178031652735, -40.51732023384165160, 27.63604381180012837 ) ) ;
#76987 = VERTEX_POINT ( 'NONE', #29764 ) ;
#76989 = ORIENTED_EDGE ( 'NONE', *, *, #87449, .F. ) ;
#76988 = EDGE_LOOP ( 'NONE', ( #6268, #22529, #63354, #18607 ) ) ;
#76990 = AXIS2_PLACEMENT_3D ( 'NONE', #64936, #9978, #30420 ) ;
#76991 = CARTESIAN_POINT ( 'NONE',  ( 150.5667039024473866, -25.42844715993594562, 249.9678068554149490 ) ) ;
#76992 = EDGE_LOOP ( 'NONE', ( #28265, #16174, #28447, #69358, #2613 ) ) ;
#76993 = VERTEX_POINT ( 'NONE', #37464 ) ;
#76994 = LINE ( 'NONE', #36099, #79713 ) ;
#76995 = EDGE_CURVE ( 'NONE', #15725, #89539, #40971, .T. ) ;
#76996 = CARTESIAN_POINT ( 'NONE',  ( 111.6101215911791087, -44.95330735676063938, 249.3977737820869720 ) ) ;
#76997 = CARTESIAN_POINT ( 'NONE',  ( 97.06105994701182738, -37.99635423742223850, 182.4277913507199003 ) ) ;
#76998 = ORIENTED_EDGE ( 'NONE', *, *, #3471, .T. ) ;
#76999 = DIRECTION ( 'NONE',  ( 6.831565154159360295E-14, -1.000000000000000000, 0.000000000000000000 ) ) ;
#77000 = EDGE_CURVE ( 'NONE', #83000, #52485, #72434, .T. ) ;
#77001 = CARTESIAN_POINT ( 'NONE',  ( -116.2551261185419236, 72.73974665673414108, 59.41428421001764093 ) ) ;
#77002 = ORIENTED_EDGE ( 'NONE', *, *, #46310, .F. ) ;
#77003 = ORIENTED_EDGE ( 'NONE', *, *, #32415, .T. ) ;
#77004 = FACE_OUTER_BOUND ( 'NONE', #2202, .T. ) ;
#77005 = ORIENTED_EDGE ( 'NONE', *, *, #8690, .T. ) ;
#77006 = VERTEX_POINT ( 'NONE', #15239 ) ;
#77007 = AXIS2_PLACEMENT_3D ( 'NONE', #82823, #48252, #75985 ) ;
#77008 = CARTESIAN_POINT ( 'NONE',  ( 110.8229109585819003, -44.00762958608321895, 270.7738046553057529 ) ) ;
#77009 = CARTESIAN_POINT ( 'NONE',  ( 108.5930441862165026, -47.10046404026961397, 142.6927681330539883 ) ) ;
#77010 = AXIS2_PLACEMENT_3D ( 'NONE', #73226, #31896, #66413 ) ;
#77011 = CARTESIAN_POINT ( 'NONE',  ( 117.3173117416417739, -32.65705981835808558, 99.13943479972098771 ) ) ;
#77012 = DIRECTION ( 'NONE',  ( 0.000000000000000000, 0.000000000000000000, -1.000000000000000000 ) ) ;
#77013 =( NAMED_UNIT ( * ) SI_UNIT ( $, .STERADIAN. ) SOLID_ANGLE_UNIT ( ) );
#77014 = CARTESIAN_POINT ( 'NONE',  ( 100.6376613383881704, -26.77430457650146423, 216.5327681330539633 ) ) ;
#77015 = FACE_OUTER_BOUND ( 'NONE', #19196, .T. ) ;
#77016 = VECTOR ( 'NONE', #3520, 1000.000000000000000 ) ;
#77017 = CARTESIAN_POINT ( 'NONE',  ( 0.000000000000000000, 50.79999999999999716, 265.5569999999999595 ) ) ;
#77018 = ORIENTED_EDGE ( 'NONE', *, *, #1095, .F. ) ;
#77019 = CARTESIAN_POINT ( 'NONE',  ( 116.3212776292296127, -32.94146857471318413, 287.6356252759109680 ) ) ;
#77020 = ORIENTED_EDGE ( 'NONE', *, *, #73501, .T. ) ;
#77021 = EDGE_CURVE ( 'NONE', #71887, #40190, #80155, .T. ) ;
#77022 = ORIENTED_EDGE ( 'NONE', *, *, #49924, .F. ) ;
#77023 = DIRECTION ( 'NONE',  ( 0.000000000000000000, 0.000000000000000000, 1.000000000000000000 ) ) ;
#77024 = EDGE_CURVE ( 'NONE', #1670, #14963, #64287, .T. ) ;
#77025 = AXIS2_PLACEMENT_3D ( 'NONE', #53184, #32776, #53636 ) ;
#77026 = CARTESIAN_POINT ( 'NONE',  ( 97.33776833833610453, -34.07136034921212797, 137.1147412179166736 ) ) ;
#77027 = CIRCLE ( 'NONE', #52333, 2.116999999999993776 ) ;
#77028 = ORIENTED_EDGE ( 'NONE', *, *, #82648, .F. ) ;
#77029 = CARTESIAN_POINT ( 'NONE',  ( 114.1752211786757414, -45.19379553418442441, 148.1203871806719405 ) ) ;
#77030 = DIRECTION ( 'NONE',  ( 1.000000000000000078E-15, 1.000000000000000083E-30, -1.000000000000000000 ) ) ;
#77031 = CARTESIAN_POINT ( 'NONE',  ( 0.000000000000000000, 101.5999999999999943, 0.000000000000000000 ) ) ;
#77032 = CARTESIAN_POINT ( 'NONE',  ( 80.06648329127399677, -15.97944715994105813, 1.625625275910943746 ) ) ;
#77035 = CARTESIAN_POINT ( 'NONE',  ( 115.8883252675856994, -30.10835006627626953, 260.3508633711493871 ) ) ;
#77034 = LINE ( 'NONE', #77473, #7876 ) ;
#77033 = DIRECTION ( 'NONE',  ( 1.821299053822143307E-16, 0.000000000000000000, -1.000000000000000000 ) ) ;
#77036 = FACE_OUTER_BOUND ( 'NONE', #57457, .T. ) ;
#77037 = DIRECTION ( 'NONE',  ( 0.000000000000000000, 0.000000000000000000, -1.000000000000000000 ) ) ;
#77038 = CARTESIAN_POINT ( 'NONE',  ( 0.000000000000000000, 223.9999999999999716, 154.6557476874258441 ) ) ;
#77039 = FACE_OUTER_BOUND ( 'NONE', #46110, .T. ) ;
#77040 = CARTESIAN_POINT ( 'NONE',  ( 109.6430121502607733, -46.48008672978578204, 258.7814586108584081 ) ) ;
#77041 = DIRECTION ( 'NONE',  ( 0.000000000000000000, -1.000000000000000000, 0.000000000000000000 ) ) ;
#77042 = AXIS2_PLACEMENT_3D ( 'NONE', #24875, #45729, #60268 ) ;
#77044 = ORIENTED_EDGE ( 'NONE', *, *, #50630, .F. ) ;
#77043 = CARTESIAN_POINT ( 'NONE',  ( 112.8265051076421770, -28.69573459919405067, 195.5838068554226368 ) ) ;
#77045 = CARTESIAN_POINT ( 'NONE',  ( 51.56670390244699576, -19.82844715994031048, -5.074374724088000832 ) ) ;
#77046 = CARTESIAN_POINT ( 'NONE',  ( 97.93707779058323126, -30.45653744243544736, 165.8594347997199634 ) ) ;
#77047 = CARTESIAN_POINT ( 'NONE',  ( 111.4154404335798745, -46.20410067450679037, 23.91848241876792969 ) ) ;
#77048 = CARTESIAN_POINT ( 'NONE',  ( 110.7114656039092893, -48.05751922203765503, 203.8241967044819489 ) ) ;
#77049 = DIRECTION ( 'NONE',  ( 0.000000000000000000, 0.000000000000000000, 1.000000000000000000 ) ) ;
#77050 = CARTESIAN_POINT ( 'NONE',  ( 0.000000000000000000, 127.0000000000000000, 0.000000000000000000 ) ) ;
#77052 = DIRECTION ( 'NONE',  ( 0.000000000000000000, 0.000000000000000000, 1.000000000000000000 ) ) ;
#77051 = DIRECTION ( 'NONE',  ( 1.000000000000000000, 0.000000000000000000, 0.000000000000000000 ) ) ;
#77053 = DIRECTION ( 'NONE',  ( 0.000000000000000000, 0.000000000000000000, -1.000000000000000000 ) ) ;
#77054 = LINE ( 'NONE', #22103, #84295 ) ;
#77055 = ORIENTED_EDGE ( 'NONE', *, *, #20921, .F. ) ;
#77056 = CIRCLE ( 'NONE', #39296, 9.425000000000000711 ) ;
#77057 = EDGE_CURVE ( 'NONE', #4931, #55131, #63839, .T. ) ;
#77058 = FACE_BOUND ( 'NONE', #85362, .T. ) ;
#77059 = ORIENTED_EDGE ( 'NONE', *, *, #28715, .F. ) ;
#77060 = VERTEX_POINT ( 'NONE', #84745 ) ;
#77061 = VECTOR ( 'NONE', #89411, 1000.000000000000114 ) ;
#77063 = VERTEX_POINT ( 'NONE', #57901 ) ;
#77062 = FACE_OUTER_BOUND ( 'NONE', #46070, .T. ) ;
#77064 = CARTESIAN_POINT ( 'NONE',  ( 101.9712125536871383, -27.65933791914800111, 56.48419670448296159 ) ) ;
#77065 = LINE ( 'NONE', #13935, #74523 ) ;
#77066 = VECTOR ( 'NONE', #79386, 1000.000000000000114 ) ;
#77067 = CARTESIAN_POINT ( 'NONE',  ( 48.79742451362098166, -36.32844715994040996, 237.4678068554150059 ) ) ;
#77068 = CARTESIAN_POINT ( 'NONE',  ( 113.5922599384962552, -44.96062289245586641, 164.1099109901969655 ) ) ;
#77069 = CARTESIAN_POINT ( 'NONE',  ( 105.4627246288800109, -27.81649992262058646, 274.6286103042674540 ) ) ;
#77070 = VERTEX_POINT ( 'NONE', #22504 ) ;
#77071 = ADVANCED_FACE ( 'NONE', ( #50636 ), #70036, .F. ) ;
#77072 = ORIENTED_EDGE ( 'NONE', *, *, #20083, .F. ) ;
#77073 = ORIENTED_EDGE ( 'NONE', *, *, #87977, .T. ) ;
#77074 = VERTEX_POINT ( 'NONE', #44257 ) ;
#77075 = CARTESIAN_POINT ( 'NONE',  ( 125.0664851986225443, -56.72944715994101728, -4.824374724089012467 ) ) ;
#77076 = PLANE ( 'NONE',  #56479 ) ;
#77077 = DIRECTION ( 'NONE',  ( 0.7071067812164788524, -0.7071067811566160710, 0.000000000000000000 ) ) ;
#77078 = CARTESIAN_POINT ( 'NONE',  ( 100.9546728043249573, -28.70702573249558753, 75.59395860993166139 ) ) ;
#77079 = CARTESIAN_POINT ( 'NONE',  ( 100.6521573293557452, 85.43248893795416166, 83.15057989155073415 ) ) ;
#77080 = EDGE_CURVE ( 'NONE', #37453, #14129, #9761, .T. ) ;
#77081 = DIRECTION ( 'NONE',  ( 1.000000000000000000, 0.000000000000000000, 0.000000000000000000 ) ) ;
#77082 = EDGE_CURVE ( 'NONE', #18243, #88352, #38786, .T. ) ;
#77083 = PLANE ( 'NONE',  #83423 ) ;
#77084 = VECTOR ( 'NONE', #23234, 1000.000000000000000 ) ;
#77085 = EDGE_CURVE ( 'NONE', #70326, #66434, #60566, .T. ) ;
#77086 = DIRECTION ( 'NONE',  ( 0.000000000000000000, -1.000000000000000000, 0.000000000000000000 ) ) ;
#77087 = CARTESIAN_POINT ( 'NONE',  ( 115.4270991047691410, -42.97960947038953350, 28.31562527591097123 ) ) ;
#77088 = DIRECTION ( 'NONE',  ( -1.000000000000000000, 0.000000000000000000, 0.000000000000000000 ) ) ;
#77089 = ORIENTED_EDGE ( 'NONE', *, *, #81503, .F. ) ;
#77090 = EDGE_CURVE ( 'NONE', #78558, #47032, #45144, .T. ) ;
#77091 = CARTESIAN_POINT ( 'NONE',  ( 188.5667039024479834, -62.87844715994099687, 173.2178068554149775 ) ) ;
#77092 = VECTOR ( 'NONE', #76807, 1000.000000000000000 ) ;
#77093 = CYLINDRICAL_SURFACE ( 'NONE', #58347, 0.9999999999999800160 ) ;
#77094 = CARTESIAN_POINT ( 'NONE',  ( 109.2937122495728772, -44.61120707852311540, 70.61380465530497474 ) ) ;
#77095 = EDGE_CURVE ( 'NONE', #7923, #50110, #45580, .T. ) ;
#77096 = AXIS2_PLACEMENT_3D ( 'NONE', #49495, #85408, #36338 ) ;
#77097 = CYLINDRICAL_SURFACE ( 'NONE', #86208, 3.174999999999983391 ) ;
#77098 = EDGE_CURVE ( 'NONE', #73753, #70996, #67383, .T. ) ;
#77099 = FACE_OUTER_BOUND ( 'NONE', #3708, .T. ) ;
#77100 = ORIENTED_EDGE ( 'NONE', *, *, #14236, .T. ) ;
#77101 = VERTEX_POINT ( 'NONE', #73762 ) ;
#77102 = DIRECTION ( 'NONE',  ( 0.000000000000000000, 0.000000000000000000, -1.000000000000000000 ) ) ;
#77103 = ORIENTED_EDGE ( 'NONE', *, *, #56743, .T. ) ;
#77104 = ORIENTED_EDGE ( 'NONE', *, *, #8261, .F. ) ;
#77105 = AXIS2_PLACEMENT_3D ( 'NONE', #61522, #76512, #14296 ) ;
#77106 = CARTESIAN_POINT ( 'NONE',  ( 108.3613424580152724, -45.52634895430261253, 139.1244404487539725 ) ) ;
#77107 = LINE ( 'NONE', #6263, #54744 ) ;
#77108 = CARTESIAN_POINT ( 'NONE',  ( 101.6669702799278525, -27.05833217848093497, 101.4937205140059575 ) ) ;
#77109 = AXIS2_PLACEMENT_3D ( 'NONE', #723, #27982, #49312 ) ;
#77110 = PLANE ( 'NONE',  #63359 ) ;
#77111 = ORIENTED_EDGE ( 'NONE', *, *, #69816, .F. ) ;
#77112 = ORIENTED_EDGE ( 'NONE', *, *, #43289, .T. ) ;
#77113 = ORIENTED_EDGE ( 'NONE', *, *, #21687, .F. ) ;
#77114 = AXIS2_PLACEMENT_3D ( 'NONE', #1396, #57230, #35445 ) ;
#77115 = DIRECTION ( 'NONE',  ( 0.000000000000000000, 0.000000000000000000, -1.000000000000000000 ) ) ;
#77116 = ORIENTED_EDGE ( 'NONE', *, *, #73461, .F. ) ;
#77117 = CARTESIAN_POINT ( 'NONE',  ( 101.4562478665867928, -44.74122718545263666, 282.0899109901972110 ) ) ;
#77118 = CARTESIAN_POINT ( 'NONE',  ( 117.8014899757583578, -34.00092425788908912, 165.0365776568629315 ) ) ;
#77119 = CARTESIAN_POINT ( 'NONE',  ( 107.0664832912739968, -8.729447159940999512, 17.92562527591199739 ) ) ;
#77120 = CARTESIAN_POINT ( 'NONE',  ( -109.7273655885044974, 48.66981474652848050, 70.74444168010853673 ) ) ;
#77121 = CARTESIAN_POINT ( 'NONE',  ( 117.1635299909640082, -34.13481127188234865, 120.0270538473389479 ) ) ;
#77122 = CIRCLE ( 'NONE', #23458, 8.999999999999994671 ) ;
#77123 = CARTESIAN_POINT ( 'NONE',  ( 0.000000000000000000, 127.0000000000000000, 0.000000000000000000 ) ) ;
#77124 = VERTEX_POINT ( 'NONE', #53735 ) ;
#77125 = DIRECTION ( 'NONE',  ( 0.7071067811868710917, -0.7071067811862240537, 0.000000000000000000 ) ) ;
#77126 = EDGE_LOOP ( 'NONE', ( #44804, #67182, #88934, #85318 ) ) ;
#77127 = DIRECTION ( 'NONE',  ( -2.170915417798913418E-16, 0.000000000000000000, -1.000000000000000000 ) ) ;
#77128 = EDGE_CURVE ( 'NONE', #36943, #16561, #75810, .T. ) ;
#77129 = ORIENTED_EDGE ( 'NONE', *, *, #49317, .F. ) ;
#77130 = DIRECTION ( 'NONE',  ( -1.000000000000000000, 0.000000000000000000, 0.000000000000000000 ) ) ;
#77131 = APPLICATION_CONTEXT ( 'automotive_design' ) ;
#77132 = CARTESIAN_POINT ( 'NONE',  ( 34.27258461953793045, -35.55794170701850732, 117.4678068554150485 ) ) ;
#77133 = CARTESIAN_POINT ( 'NONE',  ( 114.0907319755898186, -46.27410096495736269, 33.08133956162495792 ) ) ;
#77134 = CARTESIAN_POINT ( 'NONE',  ( 72.96458098368701428, 101.5999999999999943, -67.92268098368680285 ) ) ;
#77135 = CARTESIAN_POINT ( 'NONE',  ( 234.0013031625829854, 52.73749999999999716, 10.66800000000000104 ) ) ;
#77136 = DIRECTION ( 'NONE',  ( 0.000000000000000000, 0.000000000000000000, 1.000000000000000000 ) ) ;
#77137 = CARTESIAN_POINT ( 'NONE',  ( 114.5003125304781122, -32.48770244606883040, 288.6609912566482308 ) ) ;
#77139 = CARTESIAN_POINT ( 'NONE',  ( 107.6517678568360452, -47.10594642807011923, 148.6213395616249784 ) ) ;
#77138 = CARTESIAN_POINT ( 'NONE',  ( 97.81169822462854313, -40.51742973538109993, 111.6355314416972391 ) ) ;
#77140 = FACE_BOUND ( 'NONE', #15021, .T. ) ;
#77141 = DIRECTION ( 'NONE',  ( 0.7071067811869279351, -0.7071067811861670993, 2.899137802863401107E-29 ) ) ;
#77142 = VERTEX_POINT ( 'NONE', #59667 ) ;
#77143 = DIRECTION ( 'NONE',  ( 1.000000000000000000, 0.000000000000000000, 0.000000000000000000 ) ) ;
#77144 = VECTOR ( 'NONE', #28198, 1000.000000000000000 ) ;
#77145 = FACE_OUTER_BOUND ( 'NONE', #23043, .T. ) ;
#77146 = FACE_OUTER_BOUND ( 'NONE', #22950, .T. ) ;
#77147 = VERTEX_POINT ( 'NONE', #11994 ) ;
#77148 = LINE ( 'NONE', #11216, #5683 ) ;
#77150 = VERTEX_POINT ( 'NONE', #17464 ) ;
#77149 = CARTESIAN_POINT ( 'NONE',  ( 118.9274366748948069, -37.70237179777471681, 188.7613395616259595 ) ) ;
#77151 = DIRECTION ( 'NONE',  ( 1.000000000000000000, 0.000000000000000000, 0.000000000000000000 ) ) ;
#77152 = CARTESIAN_POINT ( 'NONE',  ( 96.10234264863321130, -35.15692507338371087, 222.2251490854349640 ) ) ;
#77153 = CARTESIAN_POINT ( 'NONE',  ( 110.8100519147795922, -46.50588177123592715, 58.86705384733998159 ) ) ;
#77154 = CARTESIAN_POINT ( 'NONE',  ( 99.78212687779678447, 76.18750001922980175, 84.19388261208071356 ) ) ;
#77155 = AXIS2_PLACEMENT_3D ( 'NONE', #34006, #81745, #54879 ) ;
#77156 = CARTESIAN_POINT ( 'NONE',  ( 115.5439452383992176, -108.5954344580491551, 2.217806855418142042 ) ) ;
#77157 = CARTESIAN_POINT ( 'NONE',  ( 113.1782937761293653, -44.75186858878011265, 78.09395860973531001 ) ) ;
#77158 = ORIENTED_EDGE ( 'NONE', *, *, #44959, .F. ) ;
#77159 = AXIS2_PLACEMENT_3D ( 'NONE', #62020, #41124, #75669 ) ;
#77160 = EDGE_CURVE ( 'NONE', #62011, #41091, #86957, .T. ) ;
#77161 = CONTEXT_DEPENDENT_SHAPE_REPRESENTATION ( #81092, #19188 ) ;
#77162 = ORIENTED_EDGE ( 'NONE', *, *, #43007, .T. ) ;
#77163 = ORIENTED_EDGE ( 'NONE', *, *, #39832, .T. ) ;
#77164 = ORIENTED_EDGE ( 'NONE', *, *, #10823, .F. ) ;
#77165 = CARTESIAN_POINT ( 'NONE',  ( 12.70000000000000107, 82.54999999999999716, 92.46299999999996544 ) ) ;
#77166 = CARTESIAN_POINT ( 'NONE',  ( 106.9404422130490815, -47.78196244520037084, 228.5794347997199907 ) ) ;
#77167 = CARTESIAN_POINT ( 'NONE',  ( 93.91125933621933086, -96.68314769832107913, -11.78219314458223188 ) ) ;
#77168 = DIRECTION ( 'NONE',  ( 1.000000000000000000, 1.122464679914735423E-15, 0.000000000000000000 ) ) ;
#77169 = AXIS2_PLACEMENT_3D ( 'NONE', #85587, #58297, #79661 ) ;
#77171 = CARTESIAN_POINT ( 'NONE',  ( 56.06670390244699576, -67.87844715994098976, 85.21780685541799016 ) ) ;
#77170 = LINE ( 'NONE', #49886, #13397 ) ;
#77172 = CARTESIAN_POINT ( 'NONE',  ( 25.56670390244734747, -48.82844715994178841, 139.7178068554150627 ) ) ;
#77173 = CARTESIAN_POINT ( 'NONE',  ( 101.1290945223330198, -28.09024711436062915, 50.55562527591095545 ) ) ;
#77174 = ORIENTED_EDGE ( 'NONE', *, *, #66395, .F. ) ;
#77175 = VECTOR ( 'NONE', #43510, 1000.000000000000000 ) ;
#77176 = VERTEX_POINT ( 'NONE', #46927 ) ;
#77177 = FACE_OUTER_BOUND ( 'NONE', #14457, .T. ) ;
#77178 = CARTESIAN_POINT ( 'NONE',  ( 98.35016245627538467, -31.65604021423551373, 16.90910402984798111 ) ) ;
#77179 = CARTESIAN_POINT ( 'NONE',  ( 100.2051353121705546, -29.75912871662447756, 221.6956252759109702 ) ) ;
#77180 = EDGE_CURVE ( 'NONE', #59590, #69306, #61023, .T. ) ;
#77181 = AXIS2_PLACEMENT_3D ( 'NONE', #7645, #43935, #1283 ) ;
#77182 = CYLINDRICAL_SURFACE ( 'NONE', #58830, 3.000000000000002665 ) ;
#77183 = CARTESIAN_POINT ( 'NONE',  ( 114.2526777242400726, -43.36435822665418982, 119.2327681330529714 ) ) ;
#77184 = ADVANCED_FACE ( 'NONE', ( #66947, #53284 ), #4729, .T. ) ;
#77185 = CYLINDRICAL_SURFACE ( 'NONE', #18289, 9.999999999999998224 ) ;
#77186 = EDGE_CURVE ( 'NONE', #52268, #78070, #45308, .T. ) ;
#77187 = AXIS2_PLACEMENT_3D ( 'NONE', #52738, #67756, #53644 ) ;
#77188 = CARTESIAN_POINT ( 'NONE',  ( -76.30649458666536589, 54.70491969191439807, 30.81302321914488473 ) ) ;
#77189 = EDGE_LOOP ( 'NONE', ( #57697, #71053, #17059, #8271 ) ) ;
#77190 = DIRECTION ( 'NONE',  ( -0.7071067811865794361, 0.7071067811865157093, -7.071067811865803697E-16 ) ) ;
#77192 = EDGE_CURVE ( 'NONE', #42534, #73518, #48216, .T. ) ;
#77191 = VECTOR ( 'NONE', #87488, 1000.000000000000000 ) ;
#77193 = ORIENTED_EDGE ( 'NONE', *, *, #62567, .F. ) ;
#77194 = ORIENTED_EDGE ( 'NONE', *, *, #4797, .T. ) ;
#77195 = CARTESIAN_POINT ( 'NONE',  ( -74.70172715947499853, 85.83559868056558173, 92.06080542007487111 ) ) ;
#77196 = CARTESIAN_POINT ( 'NONE',  ( 105.9698521113164844, -27.93594508925886188, 266.6072975916113705 ) ) ;
#77197 = CARTESIAN_POINT ( 'NONE',  ( 116.8171228685551313, -34.15291832559168483, 194.0314586088195199 ) ) ;
#77198 = CARTESIAN_POINT ( 'NONE',  ( -118.3041687469093830, 92.64232203292144163, 7.754495127085286654 ) ) ;
#77199 = CARTESIAN_POINT ( 'NONE',  ( 100.9546728245577469, -28.70702571737296793, 85.59395860794109012 ) ) ;
#77200 = ADVANCED_FACE ( 'NONE', ( #5633 ), #18799, .F. ) ;
#77201 = CARTESIAN_POINT ( 'NONE',  ( 74.89042153202936447, 78.46643079253871633, -91.90737012895618818 ) ) ;
#77202 = VERTEX_POINT ( 'NONE', #88309 ) ;
#77203 = DIRECTION ( 'NONE',  ( 0.000000000000000000, 0.000000000000000000, 1.000000000000000000 ) ) ;
#77204 = CARTESIAN_POINT ( 'NONE',  ( 95.56670390244703128, -104.2784471599411660, 7.717806855417980394 ) ) ;
#77205 = ORIENTED_EDGE ( 'NONE', *, *, #83663, .F. ) ;
#77206 = CARTESIAN_POINT ( 'NONE',  ( 99.06573214631099233, -44.35618096740151373, 36.92038718067297509 ) ) ;
#77207 = VERTEX_POINT ( 'NONE', #88751 ) ;
#77208 = CARTESIAN_POINT ( 'NONE',  ( 110.5540359372802328, -28.93245362646326768, 24.16384839950497110 ) ) ;
#77209 = DIRECTION ( 'NONE',  ( 0.000000000000000000, 0.000000000000000000, -1.000000000000000000 ) ) ;
#77210 = CARTESIAN_POINT ( 'NONE',  ( 114.4768422515204946, -30.34587328852055066, 184.3927681330539770 ) ) ;
#77211 = CARTESIAN_POINT ( 'NONE',  ( 23.74939251434799203, 81.92209703240837371, 298.1637470768533831 ) ) ;
#77212 = LINE ( 'NONE', #20897, #11396 ) ;
#77213 = DIRECTION ( 'NONE',  ( 0.9254794337955621897, 0.3787978585227821382, 0.000000000000000000 ) ) ;
#77214 = CIRCLE ( 'NONE', #22115, 17.00000000000000000 ) ;
#77215 = CARTESIAN_POINT ( 'NONE',  ( 167.2371591254544967, -47.82818131005522133, 180.4678068554150059 ) ) ;
#77216 = CARTESIAN_POINT ( 'NONE',  ( 118.3880299729056276, -33.06406546148816261, 280.0756252759109657 ) ) ;
#77217 = CARTESIAN_POINT ( 'NONE',  ( 98.06462366603227565, -41.13538585706373851, 116.6892862011573584 ) ) ;
#77218 = ORIENTED_EDGE ( 'NONE', *, *, #15228, .F. ) ;
#77219 = CARTESIAN_POINT ( 'NONE',  ( 57.14999999999999858, 60.86974387893089755, 329.4379999999999882 ) ) ;
#77220 = ORIENTED_EDGE ( 'NONE', *, *, #41619, .F. ) ;
#77221 = CARTESIAN_POINT ( 'NONE',  ( 108.5441076757828398, -26.36558658937538269, 100.9641967044829727 ) ) ;
#77222 = CARTESIAN_POINT ( 'NONE',  ( 173.9900000000000091, 36.86249999999999716, -35.28456447661465489 ) ) ;
#77223 = ORIENTED_EDGE ( 'NONE', *, *, #20593, .F. ) ;
#77224 = ORIENTED_EDGE ( 'NONE', *, *, #63000, .T. ) ;
#77225 = VERTEX_POINT ( 'NONE', #10639 ) ;
#77226 = CARTESIAN_POINT ( 'NONE',  ( 108.3334479865492455, -46.73485936871515634, 122.6772919339558143 ) ) ;
#77227 = CARTESIAN_POINT ( 'NONE',  ( 41.56648329127381203, -18.82844715994071194, 81.92562527591194055 ) ) ;
#77228 = PLANE ( 'NONE',  #50129 ) ;
#77229 = CARTESIAN_POINT ( 'NONE',  ( 144.2411641744344593, -140.0674981546435163, 246.8991607896899723 ) ) ;
#77230 = DIRECTION ( 'NONE',  ( 0.000000000000000000, 0.000000000000000000, 1.000000000000000000 ) ) ;
#77231 = CARTESIAN_POINT ( 'NONE',  ( 114.8194029112656551, -43.69900416259703491, 34.24419670448197905 ) ) ;
#77232 = AXIS2_PLACEMENT_3D ( 'NONE', #83913, #21683, #49357 ) ;
#77233 = CARTESIAN_POINT ( 'NONE',  ( 121.2221484686747459, -113.6057974291316839, -19.26696060647573105 ) ) ;
#77234 = EDGE_LOOP ( 'NONE', ( #36176, #65596 ) ) ;
#77235 = DIRECTION ( 'NONE',  ( 0.7071067811865671127, 0.7071067811865279218, 7.071067811865664660E-16 ) ) ;
#77236 = CARTESIAN_POINT ( 'NONE',  ( 116.7951261054197118, -39.38782728827160895, 43.61448311080118856 ) ) ;
#77237 = EDGE_CURVE ( 'NONE', #42340, #45263, #38343, .T. ) ;
#77238 = ORIENTED_EDGE ( 'NONE', *, *, #73155, .T. ) ;
#77239 = VERTEX_POINT ( 'NONE', #26509 ) ;
#77240 = VECTOR ( 'NONE', #83274, 1000.000000000000000 ) ;
#77241 = CARTESIAN_POINT ( 'NONE',  ( 82.68803181460158669, -19.56139158947832613, 2.921136715972032505 ) ) ;
#77242 = CARTESIAN_POINT ( 'NONE',  ( 105.8881231706732962, -26.36991942434103819, 322.4846826458744431 ) ) ;
#77243 = LINE ( 'NONE', #1838, #79189 ) ;
#77244 = ADVANCED_FACE ( 'NONE', ( #79709 ), #73306, .F. ) ;
#77245 = FACE_BOUND ( 'NONE', #5324, .T. ) ;
#77246 = CARTESIAN_POINT ( 'NONE',  ( 70.63919639214310564, 100.5999999999999659, 0.000000000000000000 ) ) ;
#77247 = CARTESIAN_POINT ( 'NONE',  ( 99.44356389104279970, -40.64648710652873831, 196.1267055423629699 ) ) ;
#77248 = CARTESIAN_POINT ( 'NONE',  ( -74.36911441044668436, 82.54999999999999716, -92.32962665258587265 ) ) ;
#77249 = CARTESIAN_POINT ( 'NONE',  ( 125.8424616898026756, 66.98845471270220742, 34.76731936747097507 ) ) ;
#77250 = CARTESIAN_POINT ( 'NONE',  ( 96.74811198265052781, -38.50085326290480481, 91.46133956162493917 ) ) ;
#77251 = ORIENTED_EDGE ( 'NONE', *, *, #34064, .F. ) ;
#77252 = CARTESIAN_POINT ( 'NONE',  ( 84.06648329127399677, -18.82844715994099971, 284.9256252759119548 ) ) ;
#77253 = ORIENTED_EDGE ( 'NONE', *, *, #56454, .T. ) ;
#77254 = FACE_OUTER_BOUND ( 'NONE', #45105, .T. ) ;
#77255 = ORIENTED_EDGE ( 'NONE', *, *, #11939, .T. ) ;
#77256 = DIRECTION ( 'NONE',  ( 1.000000000000000000, 0.000000000000000000, 0.000000000000000000 ) ) ;
#77257 = ORIENTED_EDGE ( 'NONE', *, *, #54903, .T. ) ;
#77258 = DIRECTION ( 'NONE',  ( 1.000000000000000000, 4.299999999999999979E-14, 1.000000000000000078E-15 ) ) ;
#77259 = FACE_OUTER_BOUND ( 'NONE', #46139, .T. ) ;
#77260 = LINE ( 'NONE', #29109, #4096 ) ;
#77261 = LINE ( 'NONE', #84984, #33566 ) ;
#77262 = ORIENTED_EDGE ( 'NONE', *, *, #50413, .T. ) ;
#77263 = EDGE_CURVE ( 'NONE', #9455, #53584, #59228, .T. ) ;
#77264 = CARTESIAN_POINT ( 'NONE',  ( 110.3789737648050107, -47.29935009229100729, 52.80610146638697699 ) ) ;
#77266 = CARTESIAN_POINT ( 'NONE',  ( 47.62500000000000000, 66.67499999999999716, 292.1000000000000227 ) ) ;
#77265 = CARTESIAN_POINT ( 'NONE',  ( 84.06648329127399677, -18.82844715994099971, 284.9256252759119548 ) ) ;
#77267 = DIRECTION ( 'NONE',  ( 1.000000000000000078E-15, -1.000000000000000083E-30, -1.000000000000000000 ) ) ;
#77268 = CARTESIAN_POINT ( 'NONE',  ( 25.56670390244797275, -62.87844715994099687, 134.4678068554150059 ) ) ;
#77269 = EDGE_LOOP ( 'NONE', ( #55350, #54596, #55132, #54342 ) ) ;
#77270 = VECTOR ( 'NONE', #12597, 1000.000000000000000 ) ;
#77271 = CARTESIAN_POINT ( 'NONE',  ( 179.8608231853567645, -35.55794170701179269, 313.9678068554149490 ) ) ;
#77272 = FACE_OUTER_BOUND ( 'NONE', #22289, .T. ) ;
#77273 = CARTESIAN_POINT ( 'NONE',  ( 25.56670390244731550, -42.82844715994178131, 175.7178068554150627 ) ) ;
#77274 = CARTESIAN_POINT ( 'NONE',  ( 118.9284187910711665, -36.16665333732972698, 114.8641967044819694 ) ) ;
#77276 = FACE_BOUND ( 'NONE', #39606, .T. ) ;
#77275 = CARTESIAN_POINT ( 'NONE',  ( 41.56670390244689628, -36.32844715994109208, 180.4678068554150911 ) ) ;
#77277 = CARTESIAN_POINT ( 'NONE',  ( 80.54920390244805617, -51.22944715994108833, 207.5838068554169809 ) ) ;
#77278 = AXIS2_PLACEMENT_3D ( 'NONE', #71416, #9179, #36878 ) ;
#77279 = ORIENTED_EDGE ( 'NONE', *, *, #84511, .F. ) ;
#77280 = DIRECTION ( 'NONE',  ( 0.000000000000000000, 0.000000000000000000, 1.000000000000000000 ) ) ;
#77281 = CARTESIAN_POINT ( 'NONE',  ( 109.3575602964533289, -46.23809593081413993, 128.7641967044819751 ) ) ;
#77282 = EDGE_CURVE ( 'NONE', #64418, #29598, #16351, .T. ) ;
#77284 = ORIENTED_EDGE ( 'NONE', *, *, #61910, .T. ) ;
#77283 = DIRECTION ( 'NONE',  ( -1.000000000000000000, -2.756263715554006823E-15, 0.000000000000000000 ) ) ;
#77285 = CARTESIAN_POINT ( 'NONE',  ( 104.5933598291445605, -26.62426044571802208, 281.2670538473395823 ) ) ;
#77286 = FACE_OUTER_BOUND ( 'NONE', #62504, .T. ) ;
#77287 = DIRECTION ( 'NONE',  ( 1.000000000000000078E-15, -1.000000000000000083E-30, -1.000000000000000000 ) ) ;
#77288 = DIRECTION ( 'NONE',  ( 0.4999999999999998890, -0.8660254037844387076, 0.000000000000000000 ) ) ;
#77289 = EDGE_CURVE ( 'NONE', #56771, #76956, #48265, .T. ) ;
#77290 = CARTESIAN_POINT ( 'NONE',  ( 226.4410000000000025, 40.03750000000000142, 10.66800000000000104 ) ) ;
#77291 = PLANE ( 'NONE',  #41847 ) ;
#77292 = CARTESIAN_POINT ( 'NONE',  ( 116.3289480479917017, -32.94026123176625731, 29.13562527591096085 ) ) ;
#77293 = CARTESIAN_POINT ( 'NONE',  ( 101.7025241355416796, -45.60450926735023813, 202.1318157521019430 ) ) ;
#77294 = ORIENTED_EDGE ( 'NONE', *, *, #38203, .T. ) ;
#77295 = ORIENTED_EDGE ( 'NONE', *, *, #43370, .F. ) ;
#77296 = CARTESIAN_POINT ( 'NONE',  ( 102.5639289776614191, -44.36196183098122958, 158.5844404487539805 ) ) ;
#77297 = VECTOR ( 'NONE', #33555, 1000.000000000000000 ) ;
#77298 = DIRECTION ( 'NONE',  ( -1.000000000000000000, 0.000000000000000000, 1.821231995776179916E-16 ) ) ;
#77299 = CARTESIAN_POINT ( 'NONE',  ( 116.8454820155364331, -34.32316206775963963, 10.45015473446897403 ) ) ;
#77300 = DIRECTION ( 'NONE',  ( 0.000000000000000000, 0.000000000000000000, -1.000000000000000000 ) ) ;
#77301 = AXIS2_PLACEMENT_3D ( 'NONE', #81518, #81961, #40598 ) ;
#77302 = CARTESIAN_POINT ( 'NONE',  ( -71.09939861440099662, 0.000000000000000000, 177.8662485265279827 ) ) ;
#77303 = EDGE_CURVE ( 'NONE', #20681, #14785, #32711, .T. ) ;
#77304 = CARTESIAN_POINT ( 'NONE',  ( 61.00843881761244347, 49.07499999999999574, -53.97512327982435210 ) ) ;
#77305 = CARTESIAN_POINT ( 'NONE',  ( 102.0670549556952409, -27.97049806174883813, 106.4897919429764244 ) ) ;
#77306 = DIRECTION ( 'NONE',  ( 0.000000000000000000, 1.000000000000000000, 0.000000000000000000 ) ) ;
#77307 = ADVANCED_FACE ( 'NONE', ( #63266 ), #55976, .F. ) ;
#77308 = CARTESIAN_POINT ( 'NONE',  ( 103.8265608274144256, -48.10271009292828381, 217.3556252759109668 ) ) ;
#77309 = CARTESIAN_POINT ( 'NONE',  ( 97.31322288428147260, -38.96126826842726132, 171.5055204312964747 ) ) ;
#77310 = ORIENTED_EDGE ( 'NONE', *, *, #52726, .F. ) ;
#77311 = ORIENTED_EDGE ( 'NONE', *, *, #23231, .T. ) ;
#77312 = CARTESIAN_POINT ( 'NONE',  ( 109.6430121157968074, -46.48008673925917833, 87.78145860803415701 ) ) ;
#77313 = CARTESIAN_POINT ( 'NONE',  ( -79.21650378603835918, 93.55239623846826191, -88.20661029664601926 ) ) ;
#77314 = CARTESIAN_POINT ( 'NONE',  ( 115.7840308798700022, -41.80076151575822507, 124.4051493520911720 ) ) ;
#77315 = LINE ( 'NONE', #15089, #51988 ) ;
#77316 = CARTESIAN_POINT ( 'NONE',  ( 99.61812512063050917, -43.94476044465307751, 37.95086337114900488 ) ) ;
#77317 = CARTESIAN_POINT ( 'NONE',  ( 50.42303506447345285, 91.07499999999996021, -73.21698938693724301 ) ) ;
#77318 = EDGE_LOOP ( 'NONE', ( #25820, #47723, #4431, #7032 ) ) ;
#77319 = PLANE ( 'NONE',  #58207 ) ;
#77320 = DIRECTION ( 'NONE',  ( 0.000000000000000000, 1.000000000000000000, 0.000000000000000000 ) ) ;
#77321 = CARTESIAN_POINT ( 'NONE',  ( 115.7763152052227156, -31.00006163510664337, 254.2899109901966028 ) ) ;
#77322 = EDGE_LOOP ( 'NONE', ( #47679, #53146, #32800, #44779 ) ) ;
#77323 = CIRCLE ( 'NONE', #55497, 10.00000000000000711 ) ;
#77324 = CARTESIAN_POINT ( 'NONE',  ( 0.000000000000000000, 127.0000000000000000, 101.0189074266571794 ) ) ;
#77325 = DIRECTION ( 'NONE',  ( -1.000000000000000000, 0.000000000000000000, 0.000000000000000000 ) ) ;
#77326 = LINE ( 'NONE', #76424, #70139 ) ;
#77327 = CARTESIAN_POINT ( 'NONE',  ( 99.67188489287487130, -33.20771423803368094, 73.79094751244896599 ) ) ;
#77328 = CARTESIAN_POINT ( 'NONE',  ( 97.03730526165486481, -41.43059529571826261, 207.6632443235299661 ) ) ;
#77329 = CARTESIAN_POINT ( 'NONE',  ( 0.000000000000000000, 60.82030000000000314, 265.5569999999999595 ) ) ;
#77330 = ORIENTED_EDGE ( 'NONE', *, *, #42997, .F. ) ;
#77331 = DIRECTION ( 'NONE',  ( 0.000000000000000000, 0.000000000000000000, 1.000000000000000000 ) ) ;
#77332 = ORIENTED_EDGE ( 'NONE', *, *, #25532, .T. ) ;
#77333 = ORIENTED_EDGE ( 'NONE', *, *, #26510, .F. ) ;
#77334 = AXIS2_PLACEMENT_3D ( 'NONE', #21245, #68943, #48917 ) ;
#77335 = DIRECTION ( 'NONE',  ( -1.000000000000000000, 0.000000000000000000, -7.067626426349370916E-15 ) ) ;
#77336 = EDGE_LOOP ( 'NONE', ( #11745, #4082, #45630, #79630 ) ) ;
#77337 = EDGE_LOOP ( 'NONE', ( #38900, #14316 ) ) ;
#77338 = FACE_OUTER_BOUND ( 'NONE', #55338, .T. ) ;
#77339 = EDGE_CURVE ( 'NONE', #60265, #89871, #35098, .T. ) ;
#77340 = CARTESIAN_POINT ( 'NONE',  ( 105.8444747722200674, -25.33565403619829226, 322.4846826458744431 ) ) ;
#77341 = CARTESIAN_POINT ( 'NONE',  ( 107.5061752250017264, -28.17031325930595642, 94.45813411379100444 ) ) ;
#77342 = CARTESIAN_POINT ( 'NONE',  ( 100.0090739042524604, -28.97838942479177149, 285.6641967044823787 ) ) ;
#77343 = CARTESIAN_POINT ( 'NONE',  ( 141.0667039024479834, -48.82844715994099971, 250.9178068554160461 ) ) ;
#77344 = LINE ( 'NONE', #38141, #6237 ) ;
#77345 = ORIENTED_EDGE ( 'NONE', *, *, #88046, .T. ) ;
#77346 = ORIENTED_EDGE ( 'NONE', *, *, #3130, .F. ) ;
#77347 = DIRECTION ( 'NONE',  ( 0.000000000000000000, 1.000000000000000000, 1.047445008332813989E-14 ) ) ;
#77348 = DIRECTION ( 'NONE',  ( 0.000000000000000000, 1.000000000000000000, 0.000000000000000000 ) ) ;
#77349 = DIRECTION ( 'NONE',  ( 0.000000000000000000, 1.000000000000000000, 0.000000000000000000 ) ) ;
#77350 = CARTESIAN_POINT ( 'NONE',  ( 116.5825849560772411, -39.12894369053753252, 123.6299109901969615 ) ) ;
#77351 = AXIS2_PLACEMENT_3D ( 'NONE', #72992, #58463, #58027 ) ;
#77352 = CARTESIAN_POINT ( 'NONE',  ( 113.4422559937560777, -27.64306140573813408, 84.57753003781698453 ) ) ;
#77353 = CARTESIAN_POINT ( 'NONE',  ( 3.968750000000050182, 120.6499999999999915, -100.8961411191535973 ) ) ;
#77354 = VERTEX_POINT ( 'NONE', #61912 ) ;
#77355 = ADVANCED_FACE ( 'NONE', ( #14228 ), #76445, .F. ) ;
#77356 = CARTESIAN_POINT ( 'NONE',  ( 103.9392425780951754, -26.78422740453794404, 250.3184824187678714 ) ) ;
#77357 = CARTESIAN_POINT ( 'NONE',  ( 131.0667039024480118, -58.35344715994099829, 207.5838068554149913 ) ) ;
#77358 = VECTOR ( 'NONE', #70075, 1000.000000000000000 ) ;
#77359 = CARTESIAN_POINT ( 'NONE',  ( 12.03847361652802306, 78.49881328697941285, 129.9999214341232232 ) ) ;
#77360 = DIRECTION ( 'NONE',  ( 1.000000000000000000, 4.299999999999999979E-14, 1.000000000000000078E-15 ) ) ;
#77362 = DIRECTION ( 'NONE',  ( 4.299999999999999979E-14, -1.000000000000000000, 4.400000000000000367E-29 ) ) ;
#77361 = LINE ( 'NONE', #76464, #20178 ) ;
#77363 = DIRECTION ( 'NONE',  ( 0.000000000000000000, 0.000000000000000000, 1.000000000000000000 ) ) ;
#77364 = CARTESIAN_POINT ( 'NONE',  ( 143.0664832912740110, -8.729447159940999512, 323.8756252759120002 ) ) ;
#77365 = CARTESIAN_POINT ( 'NONE',  ( 5.244287019405557082, 94.12413552026931995, -118.4405785268131552 ) ) ;
#77366 = DIRECTION ( 'NONE',  ( 0.000000000000000000, -1.000000000000000000, 0.000000000000000000 ) ) ;
#77367 = CARTESIAN_POINT ( 'NONE',  ( 154.5667039024469886, -67.87844715994090450, 120.2178068554179902 ) ) ;
#77368 = ADVANCED_FACE ( 'NONE', ( #47375 ), #27941, .F. ) ;
#77369 = LINE ( 'NONE', #41929, #56419 ) ;
#77371 = ORIENTED_EDGE ( 'NONE', *, *, #36129, .T. ) ;
#77370 = CARTESIAN_POINT ( 'NONE',  ( 31.71315051185499811, -33.70561438052090608, -5.074374724088000832 ) ) ;
#77372 = EDGE_CURVE ( 'NONE', #12421, #39347, #52554, .T. ) ;
#77373 = LINE ( 'NONE', #70564, #24905 ) ;
#77374 = CARTESIAN_POINT ( 'NONE',  ( 105.6290166497307581, -47.07739640705644035, 257.4670538473392298 ) ) ;
#77375 = CARTESIAN_POINT ( 'NONE',  ( 108.7432144037193922, -25.80414517310806488, 140.9432443235299672 ) ) ;
#77376 = CARTESIAN_POINT ( 'NONE',  ( 104.2350475155005114, -46.78530274442771031, 18.35848241876792031 ) ) ;
#77377 = B_SPLINE_CURVE_WITH_KNOTS ( 'NONE', 3,
 ( #88468, #22123, #35720, #43420, #8025, #84355, #71165, #63435, #49791, #48883, #63896, #21211, #77973, #70707, #9370, #15747, #77519, #1221 ),
 .UNSPECIFIED., .F., .F.,
 ( 4, 2, 2, 2, 2, 2, 2, 2, 4 ),
 ( 0.4999969828548403439, 0.5624973599979853356, 0.6249977371411302718, 0.6874981142842752080, 0.7499984914274202552, 0.8124988685705651914, 0.8749992457137101276, 0.9374996228568550638, 1.000000000000000000 ),
 .UNSPECIFIED. ) ;
#77378 = FACE_BOUND ( 'NONE', #47570, .T. ) ;
#77380 = DIRECTION ( 'NONE',  ( 1.000000000000000078E-15, 0.000000000000000000, -1.000000000000000000 ) ) ;
#77379 = FACE_OUTER_BOUND ( 'NONE', #28383, .T. ) ;
#77381 = CARTESIAN_POINT ( 'NONE',  ( 115.0372256488966087, -42.90850505318414321, 139.3022878054204909 ) ) ;
#77382 = VECTOR ( 'NONE', #42277, 1000.000000000000000 ) ;
#77383 = EDGE_CURVE ( 'NONE', #88283, #84681, #40582, .T. ) ;
#77384 = ORIENTED_EDGE ( 'NONE', *, *, #16078, .F. ) ;
#77385 = CARTESIAN_POINT ( 'NONE',  ( 97.81286927418427979, -40.51761286958078756, 126.6352223400343746 ) ) ;
#77386 = ORIENTED_EDGE ( 'NONE', *, *, #78657, .T. ) ;
#77387 = CARTESIAN_POINT ( 'NONE',  ( 108.6057327191364976, -28.29838476132584191, 164.3552769709339714 ) ) ;
#77389 = ORIENTED_EDGE ( 'NONE', *, *, #51404, .T. ) ;
#77388 = FACE_OUTER_BOUND ( 'NONE', #64885, .T. ) ;
#77390 = VECTOR ( 'NONE', #43298, 1000.000000000000000 ) ;
#77391 = LINE ( 'NONE', #50111, #33017 ) ;
#77392 = CARTESIAN_POINT ( 'NONE',  ( 107.9164806882189254, -47.13338536194948603, 173.6413395616249886 ) ) ;
#77393 = CARTESIAN_POINT ( 'NONE',  ( 115.7812633450314053, -41.80542298390999179, 149.4069061460392049 ) ) ;
#77394 = PLANE ( 'NONE',  #21101 ) ;
#77395 = EDGE_CURVE ( 'NONE', #40665, #58734, #33721, .T. ) ;
#77396 = CARTESIAN_POINT ( 'NONE',  ( 49.21213752015946596, -29.73316016639569526, 313.9678068554150059 ) ) ;
#77397 = DIRECTION ( 'NONE',  ( 0.000000000000000000, 1.000000000000000000, 0.000000000000000000 ) ) ;
#77398 = DIRECTION ( 'NONE',  ( -1.000000000000000078E-15, 1.000000000000000083E-30, 1.000000000000000000 ) ) ;
#77399 = CARTESIAN_POINT ( 'NONE',  ( 101.8448680821487073, -28.45912855063583891, 110.5241967044829892 ) ) ;
#77400 = ORIENTED_EDGE ( 'NONE', *, *, #51084, .F. ) ;
#77401 = ORIENTED_EDGE ( 'NONE', *, *, #58581, .F. ) ;
#77402 = ORIENTED_EDGE ( 'NONE', *, *, #60323, .T. ) ;
#77403 = CIRCLE ( 'NONE', #41133, 5.500000000000000888 ) ;
#77404 = CARTESIAN_POINT ( 'NONE',  ( 102.7262891916532084, -29.00345248032369483, 56.91586902018297423 ) ) ;
#77405 = DIRECTION ( 'NONE',  ( -1.092739197465703932E-16, 1.000000000000000000, 0.000000000000000000 ) ) ;
#77407 = LINE ( 'NONE', #7913, #21570 ) ;
#77406 = CARTESIAN_POINT ( 'NONE',  ( 116.7860849611260647, -31.33117650353040062, 175.2299109901959753 ) ) ;
#77408 = CARTESIAN_POINT ( 'NONE',  ( 38.10000000000000142, 95.25000000000000000, 346.9005000000000223 ) ) ;
#77409 = DIRECTION ( 'NONE',  ( 0.000000000000000000, 0.000000000000000000, 1.000000000000000000 ) ) ;
#77410 = CARTESIAN_POINT ( 'NONE',  ( 3.110602869834275287E-15, 124.5870000000000033, 25.39999999999999858 ) ) ;
#77411 = ADVANCED_FACE ( 'NONE', ( #27397 ), #68300, .F. ) ;
#77412 = FACE_OUTER_BOUND ( 'NONE', #67604, .T. ) ;
#77413 = CARTESIAN_POINT ( 'NONE',  ( 67.08803875813310924, -67.89720537647744436, 245.7828803018591657 ) ) ;
#77414 = EDGE_CURVE ( 'NONE', #12239, #83014, #69638, .T. ) ;
#77415 = CARTESIAN_POINT ( 'NONE',  ( 104.9672558511365992, -25.09151557957600076, 125.2184824187689856 ) ) ;
#77416 = EDGE_LOOP ( 'NONE', ( #574, #51080, #40106, #81423 ) ) ;
#77417 = ORIENTED_EDGE ( 'NONE', *, *, #5307, .T. ) ;
#77418 = ORIENTED_EDGE ( 'NONE', *, *, #4004, .T. ) ;
#77419 = ADVANCED_FACE ( 'NONE', ( #61462 ), #55076, .F. ) ;
#77420 = CARTESIAN_POINT ( 'NONE',  ( 12.70000000000000107, 82.54999999999999716, 129.9368274816650910 ) ) ;
#77421 = CARTESIAN_POINT ( 'NONE',  ( -100.6521573293563279, 85.43248893795414745, -83.15057989155002360 ) ) ;
#77422 = EDGE_CURVE ( 'NONE', #66156, #71950, #86300, .T. ) ;
#77423 = CARTESIAN_POINT ( 'NONE',  ( 115.7831076670964876, -41.80230951558946373, 79.40645860876814766 ) ) ;
#77424 = DIRECTION ( 'NONE',  ( 0.000000000000000000, 0.000000000000000000, 1.000000000000000000 ) ) ;
#77425 = CARTESIAN_POINT ( 'NONE',  ( 99.49937927431119533, -39.79027430526630127, 204.4509475124479536 ) ) ;
#77426 = VECTOR ( 'NONE', #53413, 1000.000000000000000 ) ;
#77427 = CARTESIAN_POINT ( 'NONE',  ( 177.4809174648215730, -49.32844715993478246, 180.4678068554150059 ) ) ;
#77428 = CONICAL_SURFACE ( 'NONE', #36778, 16.25000000000000000, 0.5235987755982992597 ) ;
#77429 = DIRECTION ( 'NONE',  ( -1.907762142705490052E-15, -7.167082501179359715E-16, 1.000000000000000000 ) ) ;
#77430 = ORIENTED_EDGE ( 'NONE', *, *, #10985, .F. ) ;
#77432 = ORIENTED_EDGE ( 'NONE', *, *, #54677, .F. ) ;
#77431 = VERTEX_POINT ( 'NONE', #10878 ) ;
#77433 = LINE ( 'NONE', #56975, #51992 ) ;
#77434 = ORIENTED_EDGE ( 'NONE', *, *, #56129, .F. ) ;
#77435 = EDGE_LOOP ( 'NONE', ( #48179, #28491, #75672, #9855, #40147 ) ) ;
#77436 = B_SPLINE_CURVE_WITH_KNOTS ( 'NONE', 3,
 ( #17125, #4829, #38887, #17565, #87949, #10302 ),
 .UNSPECIFIED., .F., .F.,
 ( 4, 1, 1, 4 ),
 ( -7.513558482637090030, -5.399388959130909882, -4.342301322120899698, -0.1139565347578015420 ),
 .UNSPECIFIED. ) ;
#77437 = B_SPLINE_CURVE_WITH_KNOTS ( 'NONE', 3,
 ( #2661, #23117, #52544, #31230, #51221, #17178, #23996, #44861, #43513, #16282, #65749, #31682, #2208, #59378, #58055, #71258, #3535, #87110, #58926, #86664, #24438, #79865, #85785, #29914, #23556, #45298, #73018, #24878, #74370, #67547 ),
 .UNSPECIFIED., .F., .F.,
 ( 4, 2, 2, 2, 1, 2, 2, 2, 2, 2, 2, 2, 1, 2, 2, 4 ),
 ( 0.000000000000000000, 0.1249999999999328315, 0.1874999999998993028, 0.2187499999998844258, 0.2343749999998752109, 0.2421874999998733236, 0.2499999999998714362, 0.3749999999998946953, 0.4374999999999019118, 0.4999999999999091838, 0.6249999999999314992, 0.6874999999999480416, 0.7187499999999479305, 0.7343749999999469313, 0.7499999999999458211, 1.000000000000000000 ),
 .UNSPECIFIED. ) ;
#77438 = CARTESIAN_POINT ( 'NONE',  ( 0.000000000000000000, -71.84204896855320044, 25.39999999999999858 ) ) ;
#77439 = CARTESIAN_POINT ( 'NONE',  ( 110.2543409660563043, -27.89122963701645830, 246.2206309249449703 ) ) ;
#77440 = DIRECTION ( 'NONE',  ( 0.0001713722456120069274, -0.9999999853157766072, -0.000000000000000000 ) ) ;
#77441 = VERTEX_POINT ( 'NONE', #45381 ) ;
#77442 = DIRECTION ( 'NONE',  ( 1.000000000000000000, 0.000000000000000000, 0.000000000000000000 ) ) ;
#77443 = CARTESIAN_POINT ( 'NONE',  ( 188.5667039024486087, -48.82844715993430640, 137.2178068554150059 ) ) ;
#77444 = EDGE_LOOP ( 'NONE', ( #16736, #44923, #24902, #53883, #76208, #34558, #6388, #78209 ) ) ;
#77445 = ORIENTED_EDGE ( 'NONE', *, *, #34718, .F. ) ;
#77446 = AXIS2_PLACEMENT_3D ( 'NONE', #3131, #2244, #85377 ) ;
#77447 = CARTESIAN_POINT ( 'NONE',  ( 98.38059522467183626, -41.69557667784989974, 111.7398153013165540 ) ) ;
#77448 = VECTOR ( 'NONE', #71698, 1000.000000000000000 ) ;
#77449 = ORIENTED_EDGE ( 'NONE', *, *, #26965, .F. ) ;
#77450 = ORIENTED_EDGE ( 'NONE', *, *, #2132, .T. ) ;
#77451 = CARTESIAN_POINT ( 'NONE',  ( 110.5225122084979574, -28.79501634926980458, 282.5557094172103803 ) ) ;
#77453 = CARTESIAN_POINT ( 'NONE',  ( 98.83914123113804351, -30.29059417415423638, 155.7984824187679465 ) ) ;
#77452 = AXIS2_PLACEMENT_3D ( 'NONE', #85693, #16198, #64783 ) ;
#77454 = CARTESIAN_POINT ( 'NONE',  ( 114.7100688122353063, -43.78666090992615523, 123.2327681330539519 ) ) ;
#77455 = CARTESIAN_POINT ( 'NONE',  ( 116.3463703120535513, -39.80474152520470454, 249.5838068554169524 ) ) ;
#77456 = DIRECTION ( 'NONE',  ( -1.000000000000000000, 0.000000000000000000, 2.775557561562892929E-14 ) ) ;
#77457 = CARTESIAN_POINT ( 'NONE',  ( 105.1109661324377811, -26.48940614006117755, 231.2270538473399597 ) ) ;
#77458 = CARTESIAN_POINT ( 'NONE',  ( -12.70000000000000107, 82.54999999999999716, -97.46299999999996544 ) ) ;
#77459 = DIRECTION ( 'NONE',  ( -1.045284632676476099E-16, -0.1045284632676476005, -0.9945218953682739560 ) ) ;
#77460 = EDGE_LOOP ( 'NONE', ( #4549, #70864, #28148, #50151 ) ) ;
#77461 = CARTESIAN_POINT ( 'NONE',  ( 129.9368274816649489, 82.54999999999999716, 12.70000000000136176 ) ) ;
#77462 = ORIENTED_EDGE ( 'NONE', *, *, #82656, .F. ) ;
#77463 = VERTEX_POINT ( 'NONE', #56886 ) ;
#77464 = DIRECTION ( 'NONE',  ( -0.7071067811864697461, -0.7071067811866252883, -7.071067811864691403E-16 ) ) ;
#77465 = ORIENTED_EDGE ( 'NONE', *, *, #43633, .T. ) ;
#77466 = EDGE_CURVE ( 'NONE', #30868, #54369, #44942, .T. ) ;
#77467 = CARTESIAN_POINT ( 'NONE',  ( 103.1745875910851851, -27.05783000869472588, 130.3813395616259925 ) ) ;
#77468 = CARTESIAN_POINT ( 'NONE',  ( 223.2659999999999911, 52.73749999999999716, -44.45000000000000284 ) ) ;
#77469 = CARTESIAN_POINT ( 'NONE',  ( 135.5068622967102385, -34.38644903112312079, 7.895285856723117668 ) ) ;
#77470 = CARTESIAN_POINT ( 'NONE',  ( -187.8075999999999794, 101.5999999999999943, 114.2999999999999972 ) ) ;
#77471 = EDGE_CURVE ( 'NONE', #20143, #40854, #73100, .T. ) ;
#77474 = CARTESIAN_POINT ( 'NONE',  ( 106.1402962346845982, -47.72062544595559785, 258.4975300378158636 ) ) ;
#77473 = CARTESIAN_POINT ( 'NONE',  ( 47.62500000000000000, 69.84999999999999432, 257.1750000000000114 ) ) ;
#77472 = CARTESIAN_POINT ( 'NONE',  ( 259.3340000000000032, 52.73749999999999716, 10.66800000000000104 ) ) ;
#77475 = DIRECTION ( 'NONE',  ( 0.000000000000000000, 0.000000000000000000, 1.000000000000000000 ) ) ;
#77476 = CARTESIAN_POINT ( 'NONE',  ( -34.93928583487483763, 53.97499999999997300, 35.93880153443800651 ) ) ;
#77477 = CARTESIAN_POINT ( 'NONE',  ( -103.1875000000000000, 117.4749999999999943, -1.080832317973422076E-12 ) ) ;
#77478 = EDGE_CURVE ( 'NONE', #1599, #73197, #38576, .T. ) ;
#77479 = LINE ( 'NONE', #22524, #45671 ) ;
#77480 = PLANE ( 'NONE',  #30043 ) ;
#77481 = EDGE_CURVE ( 'NONE', #11825, #65478, #395, .T. ) ;
#77482 = DIRECTION ( 'NONE',  ( 1.000000000000000000, 1.000000000000000078E-15, 1.000000000000000078E-15 ) ) ;
#77484 = ORIENTED_EDGE ( 'NONE', *, *, #15787, .T. ) ;
#77483 = CARTESIAN_POINT ( 'NONE',  ( 115.9443088281525149, -30.06633247050010382, 264.3508633711492735 ) ) ;
#77485 = EDGE_CURVE ( 'NONE', #26619, #62403, #17261, .T. ) ;
#77486 = PLANE ( 'NONE',  #4548 ) ;
#77487 = CARTESIAN_POINT ( 'NONE',  ( 117.8235219141173218, -34.08718286818967158, 164.0061014663869798 ) ) ;
#77488 = CARTESIAN_POINT ( 'NONE',  ( 116.7699407904022451, -31.43634848722146202, 20.21181575210195902 ) ) ;
#77489 = CARTESIAN_POINT ( 'NONE',  ( 104.5521338839504608, -48.36083399734661725, 178.4070538473399665 ) ) ;
#77490 = DIRECTION ( 'NONE',  ( -0.000000000000000000, 1.000000000000000000, 0.000000000000000000 ) ) ;
#77491 = CARTESIAN_POINT ( 'NONE',  ( 20.03715912545641231, -24.95799193693202156, 180.4678068554150911 ) ) ;
#77493 = CARTESIAN_POINT ( 'NONE',  ( 164.9667039024476196, -26.71338133338732135, 193.9678068554149775 ) ) ;
#77492 = CARTESIAN_POINT ( 'NONE',  ( 186.6899999999999977, 46.38749999999999574, -50.79999999999999716 ) ) ;
#77494 = CARTESIAN_POINT ( 'NONE',  ( 97.33784131618190827, -34.07106451174902162, 71.11479194109409718 ) ) ;
#77495 = LINE ( 'NONE', #15275, #17745 ) ;
#77496 = ADVANCED_FACE ( 'NONE', ( #31765 ), #72671, .F. ) ;
#77497 = ORIENTED_EDGE ( 'NONE', *, *, #29306, .T. ) ;
#77498 = ADVANCED_FACE ( 'NONE', ( #65406 ), #66735, .T. ) ;
#77499 = AXIS2_PLACEMENT_3D ( 'NONE', #68764, #55995, #41926 ) ;
#77500 = DIRECTION ( 'NONE',  ( -1.000000000000000000, -4.299999999999999979E-14, -1.000000000000000078E-15 ) ) ;
#77501 = CIRCLE ( 'NONE', #22382, 3.174999999999983391 ) ;
#77502 = EDGE_CURVE ( 'NONE', #79692, #50744, #77344, .T. ) ;
#77503 = ORIENTED_EDGE ( 'NONE', *, *, #38089, .F. ) ;
#77504 = ORIENTED_EDGE ( 'NONE', *, *, #6503, .T. ) ;
#77506 = VERTEX_POINT ( 'NONE', #21951 ) ;
#77505 = CARTESIAN_POINT ( 'NONE',  ( -479.3614999999999782, 86.51875000000001137, 86.36305401447658880 ) ) ;
#77507 = CARTESIAN_POINT ( 'NONE',  ( 100.9560042165379770, -28.30978499293933126, 71.57562527591099411 ) ) ;
#77508 = CARTESIAN_POINT ( 'NONE',  ( 34.92499999999999716, 82.54999999999999716, 315.3410000000000082 ) ) ;
#77509 = EDGE_CURVE ( 'NONE', #12725, #23895, #58477, .T. ) ;
#77510 = CARTESIAN_POINT ( 'NONE',  ( 71.24189083761808661, -0.9290567490904538817, 542.9756252759101471 ) ) ;
#77511 = CARTESIAN_POINT ( 'NONE',  ( 102.8263616157396854, -46.30098559033366001, 173.2441967044829596 ) ) ;
#77512 = CARTESIAN_POINT ( 'NONE',  ( 114.8253727231603136, -41.39981172478538696, 277.8057531614101663 ) ) ;
#77513 = ORIENTED_EDGE ( 'NONE', *, *, #30932, .T. ) ;
#77514 = ORIENTED_EDGE ( 'NONE', *, *, #68047, .T. ) ;
#77515 = EDGE_LOOP ( 'NONE', ( #41392, #48702, #15034, #86660 ) ) ;
#77516 = VECTOR ( 'NONE', #62333, 1000.000000000000000 ) ;
#77517 = ORIENTED_EDGE ( 'NONE', *, *, #12052, .T. ) ;
#77518 = AXIS2_PLACEMENT_3D ( 'NONE', #86878, #87323, #58268 ) ;
#77519 = CARTESIAN_POINT ( 'NONE',  ( 116.8171228664334365, -34.15291832040662712, 109.0314586092652576 ) ) ;
#77520 = AXIS2_PLACEMENT_3D ( 'NONE', #37051, #23446, #9793 ) ;
#77521 = DIRECTION ( 'NONE',  ( -1.000000000000000078E-15, 1.000000000000000083E-30, 1.000000000000000000 ) ) ;
#77522 = CARTESIAN_POINT ( 'NONE',  ( 180.2143765759500127, -35.91149509760546010, 313.9678068554149490 ) ) ;
#77523 = CARTESIAN_POINT ( 'NONE',  ( 108.4186602322921829, -26.73518583127572512, 19.96809642925226669 ) ) ;
#77524 = CARTESIAN_POINT ( 'NONE',  ( 82.89895571708156297, 82.54999999999999716, 100.8594679592221155 ) ) ;
#77525 = CYLINDRICAL_SURFACE ( 'NONE', #72699, 12.44600000000001216 ) ;
#77526 = CARTESIAN_POINT ( 'NONE',  ( 147.0665874381622018, -67.87844715994090450, 245.5130140176639770 ) ) ;
#77527 = AXIS2_PLACEMENT_3D ( 'NONE', #53219, #88247, #89578 ) ;
#77528 = DIRECTION ( 'NONE',  ( 0.7071067811865506814, -0.7071067811865443531, 7.071067811865500971E-16 ) ) ;
#77529 = CARTESIAN_POINT ( 'NONE',  ( 104.2468583329775669, -46.74335657891444384, 22.35848241876792031 ) ) ;
#77530 = CARTESIAN_POINT ( 'NONE',  ( -11.57414189257196568, 77.30572722422043341, 117.9897876170239073 ) ) ;
#77531 = VERTEX_POINT ( 'NONE', #28749 ) ;
#77532 = ADVANCED_FACE ( 'NONE', ( #84178 ), #18135, .F. ) ;
#77533 = DIRECTION ( 'NONE',  ( 1.000000000000000000, 0.000000000000000000, 0.000000000000000000 ) ) ;
#77534 = ADVANCED_FACE ( 'NONE', ( #31314, #59009, #79945 ), #86748, .T. ) ;
#77535 = CARTESIAN_POINT ( 'NONE',  ( 50.96943157740508923, -34.03355364506504799, 117.4678068554150485 ) ) ;
#77536 = CARTESIAN_POINT ( 'NONE',  ( 112.4302714532559548, -29.93748856177429118, 122.3747570362579751 ) ) ;
#77537 = PLANE ( 'NONE',  #7860 ) ;
#77538 = CARTESIAN_POINT ( 'NONE',  ( 176.7738106835696499, -48.62134037881071436, 129.9678068554150059 ) ) ;
#77539 = ORIENTED_EDGE ( 'NONE', *, *, #32609, .F. ) ;
#77540 = ORIENTED_EDGE ( 'NONE', *, *, #87, .F. ) ;
#77541 = CARTESIAN_POINT ( 'NONE',  ( 116.7952593538610131, -39.38735379887159382, 138.6131012738933634 ) ) ;
#77542 = ORIENTED_EDGE ( 'NONE', *, *, #3393, .T. ) ;
#77543 = ORIENTED_EDGE ( 'NONE', *, *, #49083, .T. ) ;
#77544 = CARTESIAN_POINT ( 'NONE',  ( 102.5639289776614191, -44.36196183098122958, 158.5844404487539805 ) ) ;
#77545 = CARTESIAN_POINT ( 'NONE',  ( -7.205548786489490269E-13, 117.4749999999999943, 103.1875000000000000 ) ) ;
#77546 = CARTESIAN_POINT ( 'NONE',  ( 97.91349202876114077, -31.62044072442156306, 106.9213395616259703 ) ) ;
#77547 = AXIS2_PLACEMENT_3D ( 'NONE', #59027, #86766, #47182 ) ;
#77548 = CYLINDRICAL_SURFACE ( 'NONE', #41547, 0.2500000000000002220 ) ;
#77549 = ORIENTED_EDGE ( 'NONE', *, *, #49985, .T. ) ;
#77550 =( BOUNDED_CURVE ( )  B_SPLINE_CURVE ( 3, ( #60999, #74634, #5149, #11521 ),
 .UNSPECIFIED., .F., .T. ) 
 B_SPLINE_CURVE_WITH_KNOTS ( ( 4, 4 ),
 ( 1.488040654385104793E-11, 1.570796326813557631 ),
 .UNSPECIFIED. ) 
 CURVE ( )  GEOMETRIC_REPRESENTATION_ITEM ( )  RATIONAL_B_SPLINE_CURVE ( ( 1.000000000000000000, 0.8047378541234737614, 0.8047378541234737614, 1.000000000000000000 ) ) 
 REPRESENTATION_ITEM ( '' )  );
#77551 = VECTOR ( 'NONE', #63962, 1000.000000000000000 ) ;
#77552 = EDGE_LOOP ( 'NONE', ( #34099, #56844, #25743, #62436 ) ) ;
#77553 = ORIENTED_EDGE ( 'NONE', *, *, #17531, .T. ) ;
#77554 = CARTESIAN_POINT ( 'NONE',  ( 115.5918606122963439, -42.76801532637115599, 53.33562527591095659 ) ) ;
#77555 = VERTEX_POINT ( 'NONE', #45819 ) ;
#77556 = CARTESIAN_POINT ( 'NONE',  ( 118.5467753794659842, -33.90456151647278205, 14.01848241876796308 ) ) ;
#77557 = CARTESIAN_POINT ( 'NONE',  ( 96.72156277063432128, -35.27346698316355145, 177.2156252759109805 ) ) ;
#77558 = CARTESIAN_POINT ( 'NONE',  ( 12.03133265694088294, 78.46222587235902779, -117.9439990761035943 ) ) ;
#77559 = CARTESIAN_POINT ( 'NONE',  ( -109.9591342944440697, 47.45097955103868514, 70.38379434518259359 ) ) ;
#77560 = CARTESIAN_POINT ( 'NONE',  ( 118.9036788419121962, -36.16782713317093112, 114.8641967044819694 ) ) ;
#77561 = DIRECTION ( 'NONE',  ( 0.000000000000000000, 0.000000000000000000, 1.000000000000000000 ) ) ;
#77562 = ORIENTED_EDGE ( 'NONE', *, *, #51455, .F. ) ;
#77563 = CARTESIAN_POINT ( 'NONE',  ( 97.53211280107056780, -39.74980392530692086, 116.5710736105993135 ) ) ;
#77564 = VERTEX_POINT ( 'NONE', #49618 ) ;
#77565 = CARTESIAN_POINT ( 'NONE',  ( 98.54769938335446966, -41.97705865527272096, 132.7663827518260575 ) ) ;
#77566 = ORIENTED_EDGE ( 'NONE', *, *, #57648, .F. ) ;
#77568 = ORIENTED_EDGE ( 'NONE', *, *, #77940, .F. ) ;
#77567 = EDGE_CURVE ( 'NONE', #55635, #42534, #42799, .T. ) ;
#77569 = CARTESIAN_POINT ( 'NONE',  ( 137.8897065959776000, -5.906223855237799469, -4.824374724088998256 ) ) ;
#77570 = CIRCLE ( 'NONE', #64480, 2.116999999999993776 ) ;
#77571 = CIRCLE ( 'NONE', #6498, 2.500000000000002220 ) ;
#77572 = DIRECTION ( 'NONE',  ( -0.7071067811865470176, 0.000000000000000000, -0.7071067811865480168 ) ) ;
#77573 = CARTESIAN_POINT ( 'NONE',  ( 118.2087526870871415, -40.76557371769158777, 23.54991099019593292 ) ) ;
#77574 = CARTESIAN_POINT ( 'NONE',  ( 1.385076594094139635, 70.24203434096087051, 38.10000000000000142 ) ) ;
#77575 = CIRCLE ( 'NONE', #665, 88.90000000000000568 ) ;
#77576 = ADVANCED_FACE ( 'NONE', ( #30885 ), #41026, .T. ) ;
#77577 = FACE_OUTER_BOUND ( 'NONE', #13574, .T. ) ;
#77578 = CARTESIAN_POINT ( 'NONE',  ( 188.5667039024479834, -65.37844715994100397, 298.0928068554150627 ) ) ;
#77579 = EDGE_CURVE ( 'NONE', #77633, #19525, #8308, .T. ) ;
#77580 = CARTESIAN_POINT ( 'NONE',  ( 97.95204982468527533, -33.09064556074055474, 41.02419670448293232 ) ) ;
#77582 = CARTESIAN_POINT ( 'NONE',  ( 95.69905522618357452, -33.46911247776740339, 137.1041967044819501 ) ) ;
#77581 = CARTESIAN_POINT ( 'NONE',  ( 102.0667094465962919, -27.97069076498398132, 110.4898230829296466 ) ) ;
#77583 = CYLINDRICAL_SURFACE ( 'NONE', #36412, 2.500000000000002220 ) ;
#77584 = CARTESIAN_POINT ( 'NONE',  ( 172.5664832912740110, -9.303447159940999356, 318.9256252759120116 ) ) ;
#77585 = ORIENTED_EDGE ( 'NONE', *, *, #13962, .T. ) ;
#77586 = DIRECTION ( 'NONE',  ( 0.7071067811865535679, -0.7071067811865415775, 7.071067811865543372E-16 ) ) ;
#77588 = ADVANCED_FACE ( 'NONE', ( #67179 ), #1889, .F. ) ;
#77587 = AXIS2_PLACEMENT_3D ( 'NONE', #49107, #41841, #13716 ) ;
#77589 = CARTESIAN_POINT ( 'NONE',  ( -11.41071036765134750, 68.71936554549954224, 36.35710361961175607 ) ) ;
#77590 = DIRECTION ( 'NONE',  ( -3.100000000000000258E-29, 3.100000000000000044E-14, 1.000000000000000000 ) ) ;
#77591 = EDGE_LOOP ( 'NONE', ( #1080, #18252, #21691, #5181 ) ) ;
#77592 = EDGE_CURVE ( 'NONE', #58734, #40665, #55527, .T. ) ;
#77593 = CARTESIAN_POINT ( 'NONE',  ( 107.0667039024470313, -104.2784471599421323, -21.78219314458201694 ) ) ;
#77595 = ORIENTED_EDGE ( 'NONE', *, *, #73667, .T. ) ;
#77594 = CARTESIAN_POINT ( 'NONE',  ( 117.8461808354131080, -34.08161713018977679, 164.0061014663869798 ) ) ;
#77596 = CARTESIAN_POINT ( 'NONE',  ( 71.25443513191777356, -74.12815658812309039, 540.9756252759101471 ) ) ;
#77597 = CARTESIAN_POINT ( 'NONE',  ( 117.2133579748808927, -41.17085908628773439, 204.4861014663869696 ) ) ;
#77598 = CARTESIAN_POINT ( 'NONE',  ( 106.6586400085135438, -26.26872808310278629, 81.10705384733896040 ) ) ;
#77599 = CARTESIAN_POINT ( 'NONE',  ( 31.56670390244700641, -22.48495420874110806, 342.9256252759119548 ) ) ;
#77600 = DIRECTION ( 'NONE',  ( 0.000000000000000000, 0.000000000000000000, -1.000000000000000000 ) ) ;
#77601 = CARTESIAN_POINT ( 'NONE',  ( 117.0718954850710389, -35.46248235502250168, 78.92729194267583637 ) ) ;
#77602 = EDGE_LOOP ( 'NONE', ( #54921, #69629, #22915, #57491 ) ) ;
#77603 = EDGE_CURVE ( 'NONE', #56720, #65259, #16416, .T. ) ;
#77604 = ITEM_DEFINED_TRANSFORMATION ( 'NONE', 'NONE', #69598,  #50656 ) ;
#77605 = AXIS2_PLACEMENT_3D ( 'NONE', #155, #55085, #82848 ) ;
#77606 = VERTEX_POINT ( 'NONE', #53520 ) ;
#77607 = EDGE_CURVE ( 'NONE', #9436, #9318, #88542, .T. ) ;
#77608 = ORIENTED_EDGE ( 'NONE', *, *, #23771, .T. ) ;
#77609 = ORIENTED_EDGE ( 'NONE', *, *, #38923, .T. ) ;
#77610 = LINE ( 'NONE', #16724, #77175 ) ;
#77611 = CARTESIAN_POINT ( 'NONE',  ( 109.9892391005685255, -26.72245031140752758, 255.8499109901966051 ) ) ;
#77612 = DIRECTION ( 'NONE',  ( 0.000000000000000000, 0.000000000000000000, 1.000000000000000000 ) ) ;
#77613 = CARTESIAN_POINT ( 'NONE',  ( 136.5183630979287557, -17.48272428402880863, 2.716753546994847834 ) ) ;
#77614 = EDGE_CURVE ( 'NONE', #46964, #89573, #6302, .T. ) ;
#77616 = DIRECTION ( 'NONE',  ( 0.000000000000000000, 0.000000000000000000, 1.000000000000000000 ) ) ;
#77615 = CARTESIAN_POINT ( 'NONE',  ( 24.79284581386643183, 184.0000000000000000, 90.32146847885336172 ) ) ;
#77617 = DIRECTION ( 'NONE',  ( 1.000000000000000000, 0.000000000000000000, -7.723290606088049820E-15 ) ) ;
#77618 = CARTESIAN_POINT ( 'NONE',  ( 116.4074703635738075, -31.97189281592868682, 44.20133956162491984 ) ) ;
#77619 = ORIENTED_EDGE ( 'NONE', *, *, #76284, .T. ) ;
#77620 = VECTOR ( 'NONE', #30683, 1000.000000000000000 ) ;
#77621 = VERTEX_POINT ( 'NONE', #87635 ) ;
#77622 = DIRECTION ( 'NONE',  ( -4.237773401492740281E-14, 1.000000000000000000, 0.000000000000000000 ) ) ;
#77623 = VECTOR ( 'NONE', #47055, 1000.000000000000000 ) ;
#77624 = FACE_OUTER_BOUND ( 'NONE', #6379, .T. ) ;
#77625 = CARTESIAN_POINT ( 'NONE',  ( 109.0793648129487678, -47.66380996059997699, 273.7213395616246885 ) ) ;
#77626 = PLANE ( 'NONE',  #3730 ) ;
#77627 = CARTESIAN_POINT ( 'NONE',  ( 98.99072789581764198, -31.21169308021403310, 116.8499109901959514 ) ) ;
#77628 = CARTESIAN_POINT ( 'NONE',  ( 33.96670390244745619, -26.71338133339334320, 237.4678068554150059 ) ) ;
#77629 = LINE ( 'NONE', #43979, #25681 ) ;
#77630 = ORIENTED_EDGE ( 'NONE', *, *, #42075, .T. ) ;
#77631 = DIRECTION ( 'NONE',  ( 0.000000000000000000, 0.000000000000000000, -1.000000000000000000 ) ) ;
#77632 = CARTESIAN_POINT ( 'NONE',  ( 97.39134470890573425, -39.27871236491387918, 57.53145266978995664 ) ) ;
#77633 = VERTEX_POINT ( 'NONE', #47617 ) ;
#77634 = ORIENTED_EDGE ( 'NONE', *, *, #56255, .F. ) ;
#77635 = EDGE_CURVE ( 'NONE', #43132, #29159, #48062, .T. ) ;
#77636 = CARTESIAN_POINT ( 'NONE',  ( -91.50010255991617214, 88.17653575778739139, 75.38763434846499933 ) ) ;
#77637 = CARTESIAN_POINT ( 'NONE',  ( 116.4478251454372923, -36.21277458701120366, 270.3139642582781335 ) ) ;
#77638 = VECTOR ( 'NONE', #3773, 1000.000000000000114 ) ;
#77639 = CARTESIAN_POINT ( 'NONE',  ( 147.0667039024469886, -67.87844715994090450, 222.2178068554179902 ) ) ;
#77640 = VECTOR ( 'NONE', #56704, 1000.000000000000000 ) ;
#77641 = VECTOR ( 'NONE', #74828, 1000.000000000000000 ) ;
#77642 = CYLINDRICAL_SURFACE ( 'NONE', #2922, 5.599999999999994316 ) ;
#77643 = VECTOR ( 'NONE', #16004, 1000.000000000000000 ) ;
#77644 = DIRECTION ( 'NONE',  ( 0.000000000000000000, -1.000000000000000000, 0.000000000000000000 ) ) ;
#77645 = CARTESIAN_POINT ( 'NONE',  ( 75.37281393334508550, 76.91656954603719498, -91.51265874544250778 ) ) ;
#77646 = VECTOR ( 'NONE', #58, 1000.000000000000000 ) ;
#77647 = ORIENTED_EDGE ( 'NONE', *, *, #79178, .T. ) ;
#77648 = CARTESIAN_POINT ( 'NONE',  ( 0.000000000000000000, 95.00619999999999266, 0.000000000000000000 ) ) ;
#77649 = CARTESIAN_POINT ( 'NONE',  ( 107.0664832912739968, -0.7548456658612000547, 333.4006252759120343 ) ) ;
#77650 = ORIENTED_EDGE ( 'NONE', *, *, #49686, .F. ) ;
#77651 = CARTESIAN_POINT ( 'NONE',  ( 116.6749405801447921, -32.59381477748385691, 79.14991099019697174 ) ) ;
#77652 = ORIENTED_EDGE ( 'NONE', *, *, #61511, .F. ) ;
#77653 = CARTESIAN_POINT ( 'NONE',  ( 101.0492827672293714, -31.21374014463884805, 273.5538046553056688 ) ) ;
#77654 = CARTESIAN_POINT ( 'NONE',  ( 98.30786778252010549, -41.72947753537307847, 126.7394794444259247 ) ) ;
#77655 = CARTESIAN_POINT ( 'NONE',  ( 116.8431970675092515, -40.18699730018606431, 178.5680062282919778 ) ) ;
#77656 = EDGE_CURVE ( 'NONE', #54421, #25056, #81716, .T. ) ;
#77657 = CARTESIAN_POINT ( 'NONE',  ( 134.0664832912739826, -8.729447159941003065, 1.325625275910988554 ) ) ;
#77658 = PLANE ( 'NONE',  #70485 ) ;
#77659 = CARTESIAN_POINT ( 'NONE',  ( 0.000000000000000000, 61.59999999999999432, 0.000000000000000000 ) ) ;
#77660 = CARTESIAN_POINT ( 'NONE',  ( 147.1762241153655282, -83.77844715994089597, 222.2178068554179902 ) ) ;
#77661 = CARTESIAN_POINT ( 'NONE',  ( 97.18271318096459765, -40.28600493293344442, 262.6013395616255934 ) ) ;
#77662 = CARTESIAN_POINT ( 'NONE',  ( 88.44409384119012429, 93.33902940301966566, -78.95116244206050737 ) ) ;
#77663 = EDGE_LOOP ( 'NONE', ( #53064, #50795, #46645 ) ) ;
#77664 = EDGE_CURVE ( 'NONE', #42594, #9140, #45364, .T. ) ;
#77665 = CARTESIAN_POINT ( 'NONE',  ( 128.8167039024470455, -104.2784471599409244, 19.21780685541800437 ) ) ;
#77666 = VERTEX_POINT ( 'NONE', #46265 ) ;
#77667 = CARTESIAN_POINT ( 'NONE',  ( 113.3575164265628672, -45.09699625868619677, 139.0899109901969553 ) ) ;
#77668 = CARTESIAN_POINT ( 'NONE',  ( 79.05226586199776762, -21.28573230649618608, 1.785258109343569100 ) ) ;
#77669 = ORIENTED_EDGE ( 'NONE', *, *, #47690, .F. ) ;
#77670 = AXIS2_PLACEMENT_3D ( 'NONE', #1515, #29217, #56903 ) ;
#77671 = ORIENTED_EDGE ( 'NONE', *, *, #25886, .F. ) ;
#77672 = ORIENTED_EDGE ( 'NONE', *, *, #51917, .F. ) ;
#77673 = DIRECTION ( 'NONE',  ( 1.000000000000000078E-15, 1.000000000000000083E-30, -1.000000000000000000 ) ) ;
#77674 = LINE ( 'NONE', #70868, #62260 ) ;
#77675 = FACE_OUTER_BOUND ( 'NONE', #63340, .T. ) ;
#77676 = DIRECTION ( 'NONE',  ( 0.000000000000000000, 0.000000000000000000, 1.000000000000000000 ) ) ;
#77677 = CARTESIAN_POINT ( 'NONE',  ( 168.0371591254546217, -48.62818131005519007, 129.9678068554150059 ) ) ;
#77678 = CARTESIAN_POINT ( 'NONE',  ( 112.1812230000633832, -27.60471316448668588, 30.66991099019694644 ) ) ;
#77679 = DIRECTION ( 'NONE',  ( 0.000000000000000000, 1.000000000000000000, 0.000000000000000000 ) ) ;
#77680 = EDGE_LOOP ( 'NONE', ( #71052, #80739, #89502, #61749 ) ) ;
#77681 = CARTESIAN_POINT ( 'NONE',  ( 126.9629299006806775, -54.68655584847609674, -5.074374724088952959 ) ) ;
#77682 = DIRECTION ( 'NONE',  ( -0.7071067811855900054, -0.7071067811875051401, 0.000000000000000000 ) ) ;
#77683 = ORIENTED_EDGE ( 'NONE', *, *, #89055, .F. ) ;
#77684 = ORIENTED_EDGE ( 'NONE', *, *, #64682, .F. ) ;
#77685 = AXIS2_PLACEMENT_3D ( 'NONE', #17351, #72760, #63373 ) ;
#77686 = CARTESIAN_POINT ( 'NONE',  ( 82.46407580265253046, -20.08864647352212174, 2.654395117675909965 ) ) ;
#77687 = DIRECTION ( 'NONE',  ( -1.000000000000000000, -8.163404592832032979E-16, 0.000000000000000000 ) ) ;
#77688 = CIRCLE ( 'NONE', #32676, 2.517499999999998739 ) ;
#77689 = DIRECTION ( 'NONE',  ( 0.000000000000000000, 0.000000000000000000, -1.000000000000000000 ) ) ;
#77690 = ADVANCED_FACE ( 'NONE', ( #82181 ), #27191, .F. ) ;
#77691 = DIRECTION ( 'NONE',  ( -1.000000000000000000, 0.000000000000000000, -2.108231265501709878E-16 ) ) ;
#77692 = CARTESIAN_POINT ( 'NONE',  ( 106.5667039024470171, -94.77844715994137914, 2.217806855417697953 ) ) ;
#77693 = ADVANCED_FACE ( 'NONE', ( #75349 ), #82631, .T. ) ;
#77694 = CARTESIAN_POINT ( 'NONE',  ( 97.42200983434074146, -37.84960760947268454, 235.8409912566479818 ) ) ;
#77695 = CARTESIAN_POINT ( 'NONE',  ( 20.03715912545730760, -24.42818131006189830, 300.4678068554150059 ) ) ;
#77696 = CARTESIAN_POINT ( 'NONE',  ( 126.9809554502671887, 56.79209779858037876, 30.34323007394005600 ) ) ;
#77697 = CARTESIAN_POINT ( 'NONE',  ( 96.59500279541983048, -37.56604165528066375, 101.3899109901969524 ) ) ;
#77698 = ORIENTED_EDGE ( 'NONE', *, *, #74108, .F. ) ;
#77699 = CARTESIAN_POINT ( 'NONE',  ( 173.9900000000000091, 28.98850000000000193, -7.937500000000000000 ) ) ;
#77700 = ORIENTED_EDGE ( 'NONE', *, *, #10620, .T. ) ;
#77701 = ADVANCED_FACE ( 'NONE', ( #46722, #33112 ), #19484, .F. ) ;
#77702 = CARTESIAN_POINT ( 'NONE',  ( 97.81169160209351787, -40.51741184665055329, 67.63577596198375375 ) ) ;
#77703 = DIRECTION ( 'NONE',  ( 0.8660254037844382635, 0.5000000000000008882, -1.550000000000000022E-14 ) ) ;
#77704 = ORIENTED_EDGE ( 'NONE', *, *, #29802, .T. ) ;
#77705 = DIRECTION ( 'NONE',  ( 0.000000000000000000, 1.000000000000000000, 0.000000000000000000 ) ) ;
#77706 = EDGE_CURVE ( 'NONE', #40317, #24929, #22202, .T. ) ;
#77707 = ORIENTED_EDGE ( 'NONE', *, *, #19754, .F. ) ;
#77708 = DIRECTION ( 'NONE',  ( 1.000000000000000078E-15, 0.000000000000000000, -1.000000000000000000 ) ) ;
#77709 = CARTESIAN_POINT ( 'NONE',  ( 115.7844980097995062, -41.79996075137723466, 274.4062243839134112 ) ) ;
#77711 = AXIS2_PLACEMENT_3D ( 'NONE', #22679, #85363, #78091 ) ;
#77710 = DIRECTION ( 'NONE',  ( -0.000000000000000000, 1.000000000000000000, 0.000000000000000000 ) ) ;
#77712 = VERTEX_POINT ( 'NONE', #33993 ) ;
#77713 = CARTESIAN_POINT ( 'NONE',  ( 117.3753987692272602, -38.63066374137464720, 88.68133956162493803 ) ) ;
#77714 = VECTOR ( 'NONE', #21999, 1000.000000000000000 ) ;
#77715 = CIRCLE ( 'NONE', #80560, 8.999999999999994671 ) ;
#77716 = SURFACE_STYLE_USAGE ( .BOTH. , #8679 ) ;
#77717 = AXIS2_PLACEMENT_3D ( 'NONE', #15457, #9524, #78138 ) ;
#77719 = CARTESIAN_POINT ( 'NONE',  ( 95.43663006862857401, 70.66229531820914644, -89.08909376919980616 ) ) ;
#77718 = CARTESIAN_POINT ( 'NONE',  ( 25.56670390244797275, -62.87844715994099687, 137.2178068554150059 ) ) ;
#77720 = CARTESIAN_POINT ( 'NONE',  ( 83.56670559755329464, -33.43837296219065536, 239.5838068554176914 ) ) ;
#77721 = CARTESIAN_POINT ( 'NONE',  ( -8.616376681309702690, 73.34747254003858075, 118.0423040787594005 ) ) ;
#77722 = VERTEX_POINT ( 'NONE', #26296 ) ;
#77723 = EDGE_CURVE ( 'NONE', #4807, #24603, #28007, .T. ) ;
#77724 = CONICAL_SURFACE ( 'NONE', #28350, 161.5439999999999827, 0.08726646259971625186 ) ;
#77725 = DIRECTION ( 'NONE',  ( 1.000000000000000000, 4.163336342344333240E-14, 0.000000000000000000 ) ) ;
#77726 = CARTESIAN_POINT ( 'NONE',  ( 25.56670390244797275, -58.35344715994099829, 137.2178068554150059 ) ) ;
#77727 = CIRCLE ( 'NONE', #42874, 0.4999999999999989453 ) ;
#77728 = CARTESIAN_POINT ( 'NONE',  ( 46.03715912545343514, -48.62818131006090283, 180.4678068554150911 ) ) ;
#77729 = CARTESIAN_POINT ( 'NONE',  ( 97.55141575199942849, -31.05946519635597269, 126.9108633711489915 ) ) ;
#77731 = DIRECTION ( 'NONE',  ( -1.000000000000000078E-15, 1.000000000000000083E-30, 1.000000000000000000 ) ) ;
#77730 = CARTESIAN_POINT ( 'NONE',  ( 163.0959832912742797, -23.42844715993517113, 117.4678068554150485 ) ) ;
#77732 = CARTESIAN_POINT ( 'NONE',  ( 127.5252020268926003, 101.5999999999999943, 177.0380000000000109 ) ) ;
#77733 = TOROIDAL_SURFACE ( 'NONE', #89341, 11.75000000000000000, 2.550000000000000266 ) ;
#77734 = ORIENTED_EDGE ( 'NONE', *, *, #50920, .T. ) ;
#77735 = AXIS2_PLACEMENT_3D ( 'NONE', #1424, #37276, #44069 ) ;
#77736 = CARTESIAN_POINT ( 'NONE',  ( 181.9694315774339941, -34.03355364505720360, -5.074374724088000832 ) ) ;
#77737 = CARTESIAN_POINT ( 'NONE',  ( 103.2980200187117816, -27.06831524915196141, 166.3603871806719496 ) ) ;
#77739 = ORIENTED_EDGE ( 'NONE', *, *, #4282, .T. ) ;
#77738 = DIRECTION ( 'NONE',  ( 0.000000000000000000, 0.000000000000000000, 1.000000000000000000 ) ) ;
#77740 = CARTESIAN_POINT ( 'NONE',  ( 117.3951115944450123, -37.65585020919950665, 29.74324432352998215 ) ) ;
#77741 = CARTESIAN_POINT ( 'NONE',  ( 50.03799999999999670, 0.000000000000000000, 191.3008000794699797 ) ) ;
#77742 = DIRECTION ( 'NONE',  ( 0.000000000000000000, 1.000000000000000000, 0.000000000000000000 ) ) ;
#77743 = CARTESIAN_POINT ( 'NONE',  ( 38.10000000000000142, 95.25000000000000000, 346.9005000000000223 ) ) ;
#77744 = CARTESIAN_POINT ( 'NONE',  ( -72.96458098368600531, 127.0000000000000000, -72.96458098368781009 ) ) ;
#77745 = CARTESIAN_POINT ( 'NONE',  ( 46.03715912545427358, -48.62818131006086020, 300.4678068554150059 ) ) ;
#77746 = CARTESIAN_POINT ( 'NONE',  ( 113.3831382903590992, -27.58002901871518020, 239.5956252759109759 ) ) ;
#77747 = ORIENTED_EDGE ( 'NONE', *, *, #34405, .T. ) ;
#77748 = ORIENTED_EDGE ( 'NONE', *, *, #27242, .T. ) ;
#77749 = ADVANCED_FACE ( 'NONE', ( #74900 ), #68534, .T. ) ;
#77750 = CARTESIAN_POINT ( 'NONE',  ( 115.7125814391468737, -38.67428926243481158, 145.0815833058969702 ) ) ;
#77751 = FACE_OUTER_BOUND ( 'NONE', #7265, .T. ) ;
#77752 = CARTESIAN_POINT ( 'NONE',  ( 97.02995690277612084, -35.86988738539728416, 32.69015473446795994 ) ) ;
#77753 = FACE_OUTER_BOUND ( 'NONE', #63884, .T. ) ;
#77754 = EDGE_CURVE ( 'NONE', #593, #17048, #40370, .T. ) ;
#77755 = DIRECTION ( 'NONE',  ( 0.000000000000000000, 0.000000000000000000, -1.000000000000000000 ) ) ;
#77756 = FACE_BOUND ( 'NONE', #28851, .T. ) ;
#77757 = CARTESIAN_POINT ( 'NONE',  ( 170.2205283966864897, 20.32000000000000028, 71.37400000000000944 ) ) ;
#77758 = DIRECTION ( 'NONE',  ( 0.000000000000000000, 0.000000000000000000, 1.000000000000000000 ) ) ;
#77759 = CARTESIAN_POINT ( 'NONE',  ( 114.3996560367811810, -27.45190519937920470, 274.5441967044824878 ) ) ;
#77760 = CARTESIAN_POINT ( 'NONE',  ( 7.685743261040695273, 92.56811239613027453, 118.1081662844706557 ) ) ;
#77761 = ORIENTED_EDGE ( 'NONE', *, *, #69032, .T. ) ;
#77762 = ORIENTED_EDGE ( 'NONE', *, *, #80984, .F. ) ;
#77763 = CARTESIAN_POINT ( 'NONE',  ( -83.15048135366454574, 79.66749569656610674, -100.6522392491101954 ) ) ;
#77764 = CARTESIAN_POINT ( 'NONE',  ( 82.67951041502472265, -19.60592655296214204, 6.943955837755186877 ) ) ;
#77765 = DIRECTION ( 'NONE',  ( 0.000000000000000000, 1.000000000000000000, 0.000000000000000000 ) ) ;
#77766 = CARTESIAN_POINT ( 'NONE',  ( 142.0294495518149915, -69.53963562688741717, 247.5178273157324327 ) ) ;
#77767 = AXIS2_PLACEMENT_3D ( 'NONE', #41769, #28146, #55837 ) ;
#77768 = CARTESIAN_POINT ( 'NONE',  ( 97.35451824726690973, -37.88753622196094284, 37.42133956162496844 ) ) ;
#77770 = CARTESIAN_POINT ( 'NONE',  ( 71.77848634863079269, 120.6499999999999915, 77.39114642429989033 ) ) ;
#77769 = CIRCLE ( 'NONE', #38587, 2.517499999999998739 ) ;
#77771 = ORIENTED_EDGE ( 'NONE', *, *, #5094, .T. ) ;
#77772 = EDGE_CURVE ( 'NONE', #80239, #84598, #32657, .T. ) ;
#77773 = VECTOR ( 'NONE', #87300, 1000.000000000000000 ) ;
#77774 = CARTESIAN_POINT ( 'NONE',  ( -3.266173478975160638, 94.72629918563912099, 118.3115834712042584 ) ) ;
#77775 = CIRCLE ( 'NONE', #12477, 4.500000000000003553 ) ;
#77776 = DIRECTION ( 'NONE',  ( -9.437404618277395057E-08, 0.000000000000000000, -0.9999999999999955591 ) ) ;
#77777 = VECTOR ( 'NONE', #14181, 1000.000000000000114 ) ;
#77778 = CARTESIAN_POINT ( 'NONE',  ( 107.5100371804366688, -47.14531440222233272, 237.6099109901969655 ) ) ;
#77779 = ORIENTED_EDGE ( 'NONE', *, *, #89703, .F. ) ;
#77780 = DIRECTION ( 'NONE',  ( 1.000000000000000000, 0.000000000000000000, -0.000000000000000000 ) ) ;
#77781 = CARTESIAN_POINT ( 'NONE',  ( 182.6664832912729821, 12.92155284005730387, 361.9756252759109998 ) ) ;
#77782 = FACE_OUTER_BOUND ( 'NONE', #21793, .T. ) ;
#77783 = CARTESIAN_POINT ( 'NONE',  ( 100.6253115865833365, -30.05058211904245624, 113.5052332267339779 ) ) ;
#77784 = CARTESIAN_POINT ( 'NONE',  ( 114.9943830143096335, -28.99422824087939432, 190.4537205140059655 ) ) ;
#77785 = CARTESIAN_POINT ( 'NONE',  ( -33.98325472291460159, 111.1250000000000000, -3.175000000000234746 ) ) ;
#77786 = ORIENTED_EDGE ( 'NONE', *, *, #27173, .T. ) ;
#77787 = AXIS2_PLACEMENT_3D ( 'NONE', #59235, #25615, #19260 ) ;
#77788 = DIRECTION ( 'NONE',  ( 0.000000000000000000, -1.000000000000000000, 0.000000000000000000 ) ) ;
#77789 = VERTEX_POINT ( 'NONE', #22633 ) ;
#77790 = ORIENTED_EDGE ( 'NONE', *, *, #18924, .T. ) ;
#77791 = CYLINDRICAL_SURFACE ( 'NONE', #51690, 2.517500000000005844 ) ;
#77792 = ORIENTED_EDGE ( 'NONE', *, *, #36957, .F. ) ;
#77793 = ORIENTED_EDGE ( 'NONE', *, *, #21092, .T. ) ;
#77794 = CARTESIAN_POINT ( 'NONE',  ( 25.56670390244797275, -62.87844715994099687, 259.9678068554150059 ) ) ;
#77795 = VECTOR ( 'NONE', #23888, 1000.000000000000000 ) ;
#77796 = CARTESIAN_POINT ( 'NONE',  ( 116.3148031259206192, -32.94054721833379062, 24.13562527591095375 ) ) ;
#77797 = ADVANCED_FACE ( 'NONE', ( #379 ), #830, .F. ) ;
#77798 = CARTESIAN_POINT ( 'NONE',  ( 99.91372553312717741, -41.39787175238471661, 101.2095626852199644 ) ) ;
#77799 = CARTESIAN_POINT ( 'NONE',  ( 105.0173152498862947, -25.84384494483574102, 280.2365776568630622 ) ) ;
#77800 = ADVANCED_FACE ( 'NONE', ( #28520 ), #56213, .F. ) ;
#77801 = DIRECTION ( 'NONE',  ( -0.9963424814100680926, 0.08544974978095698503, 0.000000000000000000 ) ) ;
#77802 = EDGE_CURVE ( 'NONE', #12424, #86245, #34445, .T. ) ;
#77803 = DIRECTION ( 'NONE',  ( -1.000000000000000000, 0.000000000000000000, 1.784063995862374817E-16 ) ) ;
#77804 = ORIENTED_EDGE ( 'NONE', *, *, #24195, .F. ) ;
#77805 = EDGE_CURVE ( 'NONE', #58818, #43667, #84864, .T. ) ;
#77806 = ORIENTED_EDGE ( 'NONE', *, *, #12387, .F. ) ;
#77807 = DIRECTION ( 'NONE',  ( 0.000000000000000000, 0.000000000000000000, -1.000000000000000000 ) ) ;
#77808 = PLANE ( 'NONE',  #63758 ) ;
#77809 = CARTESIAN_POINT ( 'NONE',  ( 70.82666682523679924, -139.1379245046460085, 247.4850519812006553 ) ) ;
#77810 = CARTESIAN_POINT ( 'NONE',  ( 97.57695254711111943, -30.97082841205668657, 125.8803871806719599 ) ) ;
#77811 = DIRECTION ( 'NONE',  ( 1.000000000000000078E-15, -1.000000000000000083E-30, -1.000000000000000000 ) ) ;
#77812 = EDGE_LOOP ( 'NONE', ( #49677, #86489, #5821, #26872 ) ) ;
#77813 = PRODUCT_DEFINITION_CONTEXT ( 'detailed design', #30700, 'design' ) ;
#77814 = CARTESIAN_POINT ( 'NONE',  ( 111.7391504816189212, -27.40993963462091543, 279.7070538473396937 ) ) ;
#77815 = CARTESIAN_POINT ( 'NONE',  ( 83.56670390244799762, -36.72944715994108122, 239.5838068554169809 ) ) ;
#77816 = DIRECTION ( 'NONE',  ( 0.000000000000000000, 1.000000000000000000, 0.000000000000000000 ) ) ;
#77817 = DIRECTION ( 'NONE',  ( 1.000000000000000000, 1.000000000000000078E-15, 0.000000000000000000 ) ) ;
#77819 = CARTESIAN_POINT ( 'NONE',  ( 68.73082703990547770, -139.2670877096359447, 246.1201790234991620 ) ) ;
#77818 = CARTESIAN_POINT ( 'NONE',  ( -77.39114642429849766, 120.6499999999999915, -71.77848634863219957 ) ) ;
#77820 = DIRECTION ( 'NONE',  ( 0.000000000000000000, 1.000000000000000000, 0.000000000000000000 ) ) ;
#77821 = LINE ( 'NONE', #15599, #25036 ) ;
#77822 = CARTESIAN_POINT ( 'NONE',  ( 132.4924365228324916, -38.98954602992306917, 7.829737527538009445 ) ) ;
#77823 = ADVANCED_FACE ( 'NONE', ( #22188 ), #83965, .F. ) ;
#77824 = CYLINDRICAL_SURFACE ( 'NONE', #5121, 179.8898777604655095 ) ;
#77825 = EDGE_CURVE ( 'NONE', #18276, #37103, #70321, .T. ) ;
#77826 = CARTESIAN_POINT ( 'NONE',  ( 140.0667039024470171, -90.27844715994091018, 51.21780685541800437 ) ) ;
#77827 = DIRECTION ( 'NONE',  ( -0.8660254037844389297, 0.4999999999999993894, -1.550000000000000968E-14 ) ) ;
#77829 = VERTEX_POINT ( 'NONE', #35786 ) ;
#77828 = CARTESIAN_POINT ( 'NONE',  ( 107.0664832912739399, -36.72944715994095333, 302.4856252759109907 ) ) ;
#77830 = CARTESIAN_POINT ( 'NONE',  ( 86.72755763596096301, -122.7870702624433648, 250.2178068554179902 ) ) ;
#77831 = CARTESIAN_POINT ( 'NONE',  ( 115.9788024870550061, -30.15175701148841725, 259.3203871806730945 ) ) ;
#77832 = CARTESIAN_POINT ( 'NONE',  ( 107.9182609186041333, -47.15517531916538019, 173.6413395616249886 ) ) ;
#77833 = CARTESIAN_POINT ( 'NONE',  ( 99.99465048579469340, -28.96254792738658779, 281.6641967044822650 ) ) ;
#77834 = AXIS2_PLACEMENT_3D ( 'NONE', #87049, #31616, #53824 ) ;
#77836 = CARTESIAN_POINT ( 'NONE',  ( 80.43833865489237667, -33.97944715994105991, 8.225625275910944723 ) ) ;
#77835 = CARTESIAN_POINT ( 'NONE',  ( 63.56670390244714497, -40.82844715994014706, 129.9678068554150911 ) ) ;
#77837 = CARTESIAN_POINT ( 'NONE',  ( 113.1782416917127705, -44.75190934023923006, 139.0939534517803793 ) ) ;
#77838 = VECTOR ( 'NONE', #14183, 1000.000000000000000 ) ;
#77839 = AXIS2_PLACEMENT_3D ( 'NONE', #87742, #5984, #12336 ) ;
#77840 =( GEOMETRIC_REPRESENTATION_CONTEXT ( 3 ) GLOBAL_UNCERTAINTY_ASSIGNED_CONTEXT ( ( #74459 ) ) GLOBAL_UNIT_ASSIGNED_CONTEXT ( ( #1574, #22916, #29275 ) ) REPRESENTATION_CONTEXT ( 'NONE', 'WORKASPACE' ) );
#77841 = CIRCLE ( 'NONE', #38654, 2.030000000001869864 ) ;
#77842 = VERTEX_POINT ( 'NONE', #14010 ) ;
#77843 = DIRECTION ( 'NONE',  ( 1.000000000000000000, 4.299999999999999979E-14, 1.000000000000000078E-15 ) ) ;
#77844 = VERTEX_POINT ( 'NONE', #15814 ) ;
#77845 = CARTESIAN_POINT ( 'NONE',  ( 98.53214291706959216, -37.07752924029257713, 160.7809912566479511 ) ) ;
#77847 = ORIENTED_EDGE ( 'NONE', *, *, #72993, .F. ) ;
#77846 = CARTESIAN_POINT ( 'NONE',  ( 117.0727434263538669, -35.46952932352849075, 188.9273346943833758 ) ) ;
#77848 = CARTESIAN_POINT ( 'NONE',  ( 37.35959712144463651, -48.62134037893550698, 249.9678068554150343 ) ) ;
#77849 = CARTESIAN_POINT ( 'NONE',  ( 98.39792771585426578, -29.90889243069713288, 196.8080062282919869 ) ) ;
#77850 = LINE ( 'NONE', #71042, #43977 ) ;
#77851 = CARTESIAN_POINT ( 'NONE',  ( 29.56648329127298069, -81.37844715994266664, 342.9256252759109884 ) ) ;
#77852 = CARTESIAN_POINT ( 'NONE',  ( 108.4238121438592231, -26.80045362567452472, 85.96918707036505225 ) ) ;
#77853 = CARTESIAN_POINT ( 'NONE',  ( 146.4789389236947557, -138.2662121386931062, 245.5138901987649831 ) ) ;
#77854 = CARTESIAN_POINT ( 'NONE',  ( 97.81360741897486832, -40.52211042289001597, 96.63602782802603031 ) ) ;
#77856 = CARTESIAN_POINT ( 'NONE',  ( 108.4956486572523744, -46.43878675094428843, 142.6927681330539883 ) ) ;
#77855 = VECTOR ( 'NONE', #5621, 1000.000000000000000 ) ;
#77857 = VERTEX_POINT ( 'NONE', #7204 ) ;
#77858 = EDGE_LOOP ( 'NONE', ( #27661, #71340, #87634, #42511 ) ) ;
#77859 = EDGE_CURVE ( 'NONE', #63478, #46794, #68979, .T. ) ;
#77860 = CARTESIAN_POINT ( 'NONE',  ( 111.9059958850653800, -29.27014106345288624, 66.05015473446795227 ) ) ;
#77861 = VECTOR ( 'NONE', #88416, 1000.000000000000000 ) ;
#77862 = FACE_BOUND ( 'NONE', #45325, .T. ) ;
#77864 = LINE ( 'NONE', #69702, #12814 ) ;
#77863 = CARTESIAN_POINT ( 'NONE',  ( 99.76930146980372172, -30.21680002102814555, 186.7470538473389752 ) ) ;
#77865 = LINE ( 'NONE', #21106, #59558 ) ;
#77867 = EDGE_CURVE ( 'NONE', #71530, #64390, #6747, .T. ) ;
#77866 = DIRECTION ( 'NONE',  ( 1.000000000000000078E-15, -1.000000000000000000, 0.000000000000000000 ) ) ;
#77868 = PLANE ( 'NONE',  #50334 ) ;
#77869 = CARTESIAN_POINT ( 'NONE',  ( -215.9000000000000057, 0.000000000000000000, -45.33899999999999864 ) ) ;
#77870 = CARTESIAN_POINT ( 'NONE',  ( 67.10568820078560748, -67.91409804406747242, 245.8838271276815988 ) ) ;
#77871 = CARTESIAN_POINT ( 'NONE',  ( 117.1882713363357169, -39.28166824301213467, 123.6299109901969615 ) ) ;
#77872 = ORIENTED_EDGE ( 'NONE', *, *, #20769, .F. ) ;
#77873 = ORIENTED_EDGE ( 'NONE', *, *, #25032, .T. ) ;
#77874 = ORIENTED_EDGE ( 'NONE', *, *, #10203, .F. ) ;
#77875 = DIRECTION ( 'NONE',  ( 0.000000000000000000, -1.000000000000000000, 0.000000000000000000 ) ) ;
#77876 = CARTESIAN_POINT ( 'NONE',  ( 0.000000000000000000, 238.5000000000000000, 164.6557476874258441 ) ) ;
#77877 = FACE_OUTER_BOUND ( 'NONE', #11694, .T. ) ;
#77878 = CARTESIAN_POINT ( 'NONE',  ( 99.25992742994408502, -40.46556956555936324, 214.5118998934009653 ) ) ;
#77879 = VECTOR ( 'NONE', #76703, 1000.000000000000114 ) ;
#77880 = EDGE_CURVE ( 'NONE', #25134, #60085, #69875, .T. ) ;
#77881 = DIRECTION ( 'NONE',  ( 0.000000000000000000, 0.000000000000000000, 1.000000000000000000 ) ) ;
#77882 = CARTESIAN_POINT ( 'NONE',  ( 114.1752211786757414, -45.19379553418442441, 148.1203871806719405 ) ) ;
#77883 = CARTESIAN_POINT ( 'NONE',  ( 134.0664832912740110, -8.729447159940999512, 308.6356252759119911 ) ) ;
#77884 = VERTEX_POINT ( 'NONE', #8551 ) ;
#77886 = ORIENTED_EDGE ( 'NONE', *, *, #5701, .F. ) ;
#77885 = EDGE_LOOP ( 'NONE', ( #85711, #20246, #5244, #25912, #83325 ) ) ;
#77887 = DIRECTION ( 'NONE',  ( 4.299999999999999979E-14, -1.000000000000000000, 0.000000000000000000 ) ) ;
#77888 = ORIENTED_EDGE ( 'NONE', *, *, #86615, .T. ) ;
#77889 = ORIENTED_EDGE ( 'NONE', *, *, #65217, .T. ) ;
#77890 = DIRECTION ( 'NONE',  ( -1.000000000000000000, -6.193183223602000661E-14, -1.000000000000000078E-15 ) ) ;
#77891 = FACE_OUTER_BOUND ( 'NONE', #84725, .T. ) ;
#77892 = CARTESIAN_POINT ( 'NONE',  ( 101.9834712436270507, -43.98831800240917289, 278.5215833058970247 ) ) ;
#77893 = EDGE_CURVE ( 'NONE', #35637, #24486, #72936, .T. ) ;
#77894 = CARTESIAN_POINT ( 'NONE',  ( 112.0659110422256930, -45.48839660081501535, 272.9897918895903217 ) ) ;
#77895 = VERTEX_POINT ( 'NONE', #83075 ) ;
#77896 = VECTOR ( 'NONE', #78021, 1000.000000000000000 ) ;
#77897 = CARTESIAN_POINT ( 'NONE',  ( 115.4645620972963513, -40.57776935811419605, 9.635625275910941312 ) ) ;
#77898 = CYLINDRICAL_SURFACE ( 'NONE', #27117, 2.500000000000002220 ) ;
#77899 = EDGE_LOOP ( 'NONE', ( #17592, #71687, #11289, #82935 ) ) ;
#77900 = ORIENTED_EDGE ( 'NONE', *, *, #31846, .T. ) ;
#77901 = AXIS2_PLACEMENT_3D ( 'NONE', #279, #27977, #55652 ) ;
#77902 = CIRCLE ( 'NONE', #73532, 10.00000000000002487 ) ;
#77903 = CARTESIAN_POINT ( 'NONE',  ( 98.15101777340095168, -41.26169252765487272, 111.7007443023918825 ) ) ;
#77904 = CIRCLE ( 'NONE', #66263, 9.571100913904423635 ) ;
#77905 = ORIENTED_EDGE ( 'NONE', *, *, #29504, .F. ) ;
#77906 = ORIENTED_EDGE ( 'NONE', *, *, #75229, .T. ) ;
#77907 = ADVANCED_FACE ( 'NONE', ( #20829 ), #62603, .F. ) ;
#77908 = CARTESIAN_POINT ( 'NONE',  ( 105.5338363264665986, -28.21170577469638729, 273.0242808457819592 ) ) ;
#77909 = CARTESIAN_POINT ( 'NONE',  ( 97.93707779058323126, -30.45653744243544736, 165.8594347997199634 ) ) ;
#77910 = CARTESIAN_POINT ( 'NONE',  ( 99.43809884604145566, -27.69271567064627604, 150.6356252759109680 ) ) ;
#77911 = FILL_AREA_STYLE ('',( #55627 ) ) ;
#77912 = FACE_OUTER_BOUND ( 'NONE', #33015, .T. ) ;
#77913 = CARTESIAN_POINT ( 'NONE',  ( 110.1374552785425323, -26.11139123911904036, 210.8403871806729626 ) ) ;
#77914 = CYLINDRICAL_SURFACE ( 'NONE', #66021, 4.762500000000001066 ) ;
#77915 = ADVANCED_FACE ( 'NONE', ( #35336 ), #63499, .F. ) ;
#77916 = DIRECTION ( 'NONE',  ( -0.7071067811864671926, -0.7071067811866279529, -6.612322855854137577E-17 ) ) ;
#77917 = VERTEX_POINT ( 'NONE', #49857 ) ;
#77918 = CARTESIAN_POINT ( 'NONE',  ( -130.4363378768870234, 71.14122173980734942, -5.641126054320938721 ) ) ;
#77919 = VERTEX_POINT ( 'NONE', #7647 ) ;
#77920 = ORIENTED_EDGE ( 'NONE', *, *, #29310, .T. ) ;
#77921 = VECTOR ( 'NONE', #9267, 1000.000000000000000 ) ;
#77922 = AXIS2_PLACEMENT_3D ( 'NONE', #31750, #37691, #44927 ) ;
#77923 = VECTOR ( 'NONE', #34323, 1000.000000000000000 ) ;
#77924 = CARTESIAN_POINT ( 'NONE',  ( 96.00724586008001893, -35.77752748456175169, 186.2461014663869889 ) ) ;
#77925 = ORIENTED_EDGE ( 'NONE', *, *, #37926, .F. ) ;
#77926 = CARTESIAN_POINT ( 'NONE',  ( 113.9170494572507266, -28.05483877344520849, 124.5565776568629559 ) ) ;
#77927 = DIRECTION ( 'NONE',  ( 0.9659258262890688673, 0.000000000000000000, -0.2588190451025189631 ) ) ;
#77928 = CARTESIAN_POINT ( 'NONE',  ( -72.96458098368751166, 127.0000000000000000, 72.96458098368620426 ) ) ;
#77929 = DIRECTION ( 'NONE',  ( -0.9659258262890675351, 0.000000000000000000, -0.2588190451025234595 ) ) ;
#77932 = CARTESIAN_POINT ( 'NONE',  ( 96.27200394136428940, -34.46162041542912391, 257.1737205140064475 ) ) ;
#77931 = CARTESIAN_POINT ( 'NONE',  ( 116.9441839019826261, -38.62175960871475411, 58.67575922383635145 ) ) ;
#77930 = CARTESIAN_POINT ( 'NONE',  ( 184.5664832912740110, 15.62155284005900491, 323.8756252759109202 ) ) ;
#77933 = DIRECTION ( 'NONE',  ( 1.000000000000000000, 0.000000000000000000, -1.224646799147353207E-16 ) ) ;
#77934 = CARTESIAN_POINT ( 'NONE',  ( 188.5667039024485518, -48.82844715993430640, 173.2178068554150059 ) ) ;
#77935 = CARTESIAN_POINT ( 'NONE',  ( -15.89999999999999680, 53.97500000000000142, 30.79999999999999361 ) ) ;
#77936 = EDGE_CURVE ( 'NONE', #1366, #20465, #14920, .T. ) ;
#77937 = CARTESIAN_POINT ( 'NONE',  ( 90.44969454456403923, -20.11243780205715481, 239.5838068554169809 ) ) ;
#77938 = EDGE_CURVE ( 'NONE', #69845, #13929, #48948, .T. ) ;
#77939 = CARTESIAN_POINT ( 'NONE',  ( 99.09570906053022554, -30.55043177293176981, 256.8022919445643879 ) ) ;
#77940 = EDGE_CURVE ( 'NONE', #46193, #5603, #76691, .T. ) ;
#77941 = CARTESIAN_POINT ( 'NONE',  ( 172.5664832912729878, -27.82844715994070484, 198.9256252759119832 ) ) ;
#77943 = ORIENTED_EDGE ( 'NONE', *, *, #61297, .T. ) ;
#77942 = CARTESIAN_POINT ( 'NONE',  ( 99.30039714715974242, -28.79844535499942637, 270.7051490854347549 ) ) ;
#77944 = FACE_OUTER_BOUND ( 'NONE', #76298, .T. ) ;
#77945 = CARTESIAN_POINT ( 'NONE',  ( 108.8526476014722277, -47.02293932800507292, 167.7127681330539701 ) ) ;
#77946 = CARTESIAN_POINT ( 'NONE',  ( 99.50169031327072844, -43.90275843488763741, 77.92991099019597812 ) ) ;
#77947 = CARTESIAN_POINT ( 'NONE',  ( 113.1808386317757282, -26.52034477659904610, 200.6470538473399756 ) ) ;
#77948 = ADVANCED_FACE ( 'NONE', ( #50766 ), #16704, .T. ) ;
#77949 = FACE_OUTER_BOUND ( 'NONE', #53942, .T. ) ;
#77950 = CARTESIAN_POINT ( 'NONE',  ( 163.1639762274590169, -34.03355364505800651, -5.074374724088000832 ) ) ;
#77952 = CARTESIAN_POINT ( 'NONE',  ( 146.0667039024470171, -94.02844715994091018, 45.21780685541799727 ) ) ;
#77951 = LINE ( 'NONE', #729, #69579 ) ;
#77953 = CARTESIAN_POINT ( 'NONE',  ( 112.1393456458850579, -28.01282278379046886, 69.65645860885391016 ) ) ;
#77954 = PLANE ( 'NONE',  #68517 ) ;
#77955 = EDGE_LOOP ( 'NONE', ( #87558, #81926, #9637, #88584 ) ) ;
#77956 = AXIS2_PLACEMENT_3D ( 'NONE', #63409, #71584, #43398 ) ;
#77957 = PLANE ( 'NONE',  #45543 ) ;
#77958 = ORIENTED_EDGE ( 'NONE', *, *, #80192, .F. ) ;
#77959 = ORIENTED_EDGE ( 'NONE', *, *, #21042, .T. ) ;
#77961 = ORIENTED_EDGE ( 'NONE', *, *, #67538, .F. ) ;
#77960 = LINE ( 'NONE', #77505, #63261 ) ;
#77962 = CARTESIAN_POINT ( 'NONE',  ( 96.97787942770426639, -32.27031107066119375, 51.98324432352996638 ) ) ;
#77963 = CARTESIAN_POINT ( 'NONE',  ( 25.56670390244797275, -62.87844715994099687, 257.2178068554150059 ) ) ;
#77964 = DIRECTION ( 'NONE',  ( 0.7071067811865449082, 0.7071067811865501263, 7.071067811865448709E-16 ) ) ;
#77965 = DIRECTION ( 'NONE',  ( 1.000000000000000000, 0.000000000000000000, 0.000000000000000000 ) ) ;
#77966 = CIRCLE ( 'NONE', #14079, 23.50000000000000711 ) ;
#77967 = CARTESIAN_POINT ( 'NONE',  ( 113.6113952709150396, -31.24125447920927101, 268.8038483995053411 ) ) ;
#77968 = ORIENTED_EDGE ( 'NONE', *, *, #73202, .F. ) ;
#77969 = VERTEX_POINT ( 'NONE', #52517 ) ;
#77970 = VERTEX_POINT ( 'NONE', #45275 ) ;
#77971 = VECTOR ( 'NONE', #80506, 1000.000000000000000 ) ;
#77972 = AXIS2_PLACEMENT_3D ( 'NONE', #60610, #88353, #62853 ) ;
#77973 = CARTESIAN_POINT ( 'NONE',  ( 115.7831076709258582, -41.80230950872173423, 108.4064586093909384 ) ) ;
#77974 = DIRECTION ( 'NONE',  ( -1.147230458779309805E-16, 0.000000000000000000, -1.000000000000000000 ) ) ;
#77975 = VECTOR ( 'NONE', #89728, 1000.000000000000000 ) ;
#77976 = CARTESIAN_POINT ( 'NONE',  ( 112.1388153513013037, -28.01251898142565011, 160.6565068732068937 ) ) ;
#77977 = CARTESIAN_POINT ( 'NONE',  ( 97.07211725179735140, -35.37804438830692533, 21.21817328746602982 ) ) ;
#77978 = CARTESIAN_POINT ( 'NONE',  ( 99.33304294513213506, 89.94765885072628464, 84.72230615113687691 ) ) ;
#77980 = EDGE_CURVE ( 'NONE', #66368, #6493, #4804, .T. ) ;
#77979 = CARTESIAN_POINT ( 'NONE',  ( 4.481506956522084195, 70.65969245518890318, -130.4796279538066983 ) ) ;
#77981 = DIRECTION ( 'NONE',  ( -1.000000000000000000, 0.000000000000000000, 0.000000000000000000 ) ) ;
#77982 = DIRECTION ( 'NONE',  ( 1.705911707540438309E-29, 0.7071067811865391350, -0.7071067811865560104 ) ) ;
#77983 = CARTESIAN_POINT ( 'NONE',  ( 116.4547782460827250, -32.24742764444978604, 19.18133956162493092 ) ) ;
#77984 = ORIENTED_EDGE ( 'NONE', *, *, #12162, .T. ) ;
#77985 = VECTOR ( 'NONE', #55308, 1000.000000000000000 ) ;
#77986 = CARTESIAN_POINT ( 'NONE',  ( 98.34985944185039841, -31.65658391562952545, 270.9064585273550847 ) ) ;
#77987 = VECTOR ( 'NONE', #17752, 1000.000000000000000 ) ;
#77988 = AXIS2_PLACEMENT_3D ( 'NONE', #9422, #72979, #52938 ) ;
#77989 = DIRECTION ( 'NONE',  ( -0.0001713722456120069274, 0.9999999853157766072, 0.000000000000000000 ) ) ;
#77990 = CARTESIAN_POINT ( 'NONE',  ( 115.0182259351703777, -41.51125854152899564, 126.2138046553059638 ) ) ;
#77991 = VECTOR ( 'NONE', #14351, 1000.000000000000000 ) ;
#77992 = EDGE_CURVE ( 'NONE', #19337, #9633, #37596, .T. ) ;
#77993 = EDGE_CURVE ( 'NONE', #81147, #65492, #72114, .T. ) ;
#77994 = CARTESIAN_POINT ( 'NONE',  ( 116.3229784443844324, -32.93528945216412041, 94.13562527591096796 ) ) ;
#77995 = CARTESIAN_POINT ( 'NONE',  ( -254.0000000000000000, 53.97500000000000142, 50.79999999999999716 ) ) ;
#77996 = ORIENTED_EDGE ( 'NONE', *, *, #70981, .F. ) ;
#77997 = ORIENTED_EDGE ( 'NONE', *, *, #65167, .T. ) ;
#77998 = EDGE_CURVE ( 'NONE', #15487, #20374, #54110, .T. ) ;
#77999 = CARTESIAN_POINT ( 'NONE',  ( 109.6432586217883909, -46.48002561855553694, 137.7791137709158988 ) ) ;
#78000 = VERTEX_POINT ( 'NONE', #71233 ) ;
#78001 = ORIENTED_EDGE ( 'NONE', *, *, #16409, .F. ) ;
#78002 = EDGE_CURVE ( 'NONE', #46484, #87166, #10331, .T. ) ;
#78003 = CARTESIAN_POINT ( 'NONE',  ( 103.0256836488564716, -28.24720316769774797, 136.8739642582779652 ) ) ;
#78004 = ADVANCED_FACE ( 'NONE', ( #3508 ), #31205, .T. ) ;
#78005 = CARTESIAN_POINT ( 'NONE',  ( 107.5667039024470313, -100.3098201933451605, -19.78219314458212708 ) ) ;
#78006 = CARTESIAN_POINT ( 'NONE',  ( 103.2709630098024576, -47.13517786649186547, 93.28610146638693834 ) ) ;
#78007 = VECTOR ( 'NONE', #7440, 1000.000000000000114 ) ;
#78008 = EDGE_CURVE ( 'NONE', #48239, #47446, #26513, .T. ) ;
#78009 = CARTESIAN_POINT ( 'NONE',  ( 113.6855641942755142, -44.25381336270734067, 18.15052713635613557 ) ) ;
#78010 = VERTEX_POINT ( 'NONE', #58902 ) ;
#78011 = EDGE_CURVE ( 'NONE', #89277, #48723, #9004, .T. ) ;
#78012 = ORIENTED_EDGE ( 'NONE', *, *, #83933, .T. ) ;
#78013 = VERTEX_POINT ( 'NONE', #85764 ) ;
#78014 = EDGE_CURVE ( 'NONE', #64725, #4573, #86640, .T. ) ;
#78015 = CARTESIAN_POINT ( 'NONE',  ( 103.8344565422589767, -46.70152647745319996, 82.32705384733995402 ) ) ;
#78016 = ORIENTED_EDGE ( 'NONE', *, *, #83207, .T. ) ;
#78017 = CARTESIAN_POINT ( 'NONE',  ( 97.37192905580960200, -32.85904099757679830, 41.02419670448193045 ) ) ;
#78018 = CARTESIAN_POINT ( 'NONE',  ( 98.24294948823698803, -42.32252413779357170, 182.7756252759109543 ) ) ;
#78019 = EDGE_CURVE ( 'NONE', #50313, #54435, #36705, .T. ) ;
#78020 = CARTESIAN_POINT ( 'NONE',  ( 92.82872956494375671, -30.11307588647346023, 0.7256252759109567130 ) ) ;
#78021 = DIRECTION ( 'NONE',  ( 0.000000000000000000, -1.000000000000000000, 0.000000000000000000 ) ) ;
#78022 = CARTESIAN_POINT ( 'NONE',  ( 99.05421528594702352, -43.39923342774125814, 112.8784824187679732 ) ) ;
#78023 = EDGE_CURVE ( 'NONE', #3353, #296, #79837, .T. ) ;
#78024 = CARTESIAN_POINT ( 'NONE',  ( -446.0240000000000009, 14.28749999999982201, 90.48749999999999716 ) ) ;
#78025 = ORIENTED_EDGE ( 'NONE', *, *, #71346, .T. ) ;
#78026 = CARTESIAN_POINT ( 'NONE',  ( 130.3998166246070127, 12.92155284005802685, 335.5992267699912190 ) ) ;
#78027 = AXIS2_PLACEMENT_3D ( 'NONE', #39569, #19580, #33215 ) ;
#78028 = VERTEX_POINT ( 'NONE', #51646 ) ;
#78029 = CARTESIAN_POINT ( 'NONE',  ( 22.49563609058250435, -67.87844715994100397, 13.84673904354932361 ) ) ;
#78030 = VERTEX_POINT ( 'NONE', #17151 ) ;
#78031 = ORIENTED_EDGE ( 'NONE', *, *, #41875, .F. ) ;
#78032 = VECTOR ( 'NONE', #9915, 1000.000000000000000 ) ;
#78033 = CARTESIAN_POINT ( 'NONE',  ( 99.53451269431035087, -109.2045100507364737, 2.217806855418169576 ) ) ;
#78034 = AXIS2_PLACEMENT_3D ( 'NONE', #46381, #66847, #81407 ) ;
#78035 = LINE ( 'NONE', #83491, #66718 ) ;
#78036 = CARTESIAN_POINT ( 'NONE',  ( 112.1173730388400287, -26.89747643418222722, 19.71086337114896736 ) ) ;
#78037 = LINE ( 'NONE', #57108, #32954 ) ;
#78038 = DIRECTION ( 'NONE',  ( 0.4999999999999998890, -0.8660254037844387076, 0.000000000000000000 ) ) ;
#78039 = CARTESIAN_POINT ( 'NONE',  ( 60.32499999999999574, 82.54999999999999716, 335.3740053999999304 ) ) ;
#78040 = CARTESIAN_POINT ( 'NONE',  ( 101.3196941207356758, -46.24713579373447914, 52.14419670448295108 ) ) ;
#78042 = CARTESIAN_POINT ( 'NONE',  ( 103.8142050530422864, -26.84757730287823563, 161.3299109901969643 ) ) ;
#78041 = CARTESIAN_POINT ( 'NONE',  ( 97.79845349656991971, -40.48495068833381083, 111.6328342125843989 ) ) ;
#78043 = CARTESIAN_POINT ( 'NONE',  ( 112.1393456392507630, -28.01282277969801626, 70.65645860946722223 ) ) ;
#78044 = CARTESIAN_POINT ( 'NONE',  ( 27.27158787008325902, 184.0000000000000000, -5.920431057502157584E-15 ) ) ;
#78045 = EDGE_LOOP ( 'NONE', ( #39760, #7190, #54067, #56598 ) ) ;
#78046 = DIRECTION ( 'NONE',  ( 3.100000000000000258E-29, -3.100000000000000044E-14, -1.000000000000000000 ) ) ;
#78047 = EDGE_CURVE ( 'NONE', #22553, #32339, #2183, .T. ) ;
#78048 = VECTOR ( 'NONE', #61636, 1000.000000000000000 ) ;
#78049 = DIRECTION ( 'NONE',  ( 0.000000000000000000, 0.000000000000000000, -1.000000000000000000 ) ) ;
#78050 = LINE ( 'NONE', #1741, #28195 ) ;
#78051 = EDGE_CURVE ( 'NONE', #29424, #61339, #30985, .T. ) ;
#78052 = ORIENTED_EDGE ( 'NONE', *, *, #75449, .F. ) ;
#78053 = ADVANCED_FACE ( 'NONE', ( #3956 ), #51197, .T. ) ;
#78054 = AXIS2_PLACEMENT_3D ( 'NONE', #88748, #87395, #25155 ) ;
#78055 = LINE ( 'NONE', #36255, #66472 ) ;
#78057 = ORIENTED_EDGE ( 'NONE', *, *, #52928, .T. ) ;
#78056 = CARTESIAN_POINT ( 'NONE',  ( 114.3747829841801149, -29.18355094256887838, 174.4641967044819637 ) ) ;
#78058 = PLANE ( 'NONE',  #29191 ) ;
#78059 = CARTESIAN_POINT ( 'NONE',  ( 107.2435369062854420, -47.21027956138831883, 208.5899109901969837 ) ) ;
#78060 = CARTESIAN_POINT ( 'NONE',  ( 112.8257383337702606, -47.14300054286279362, 98.97848241876793907 ) ) ;
#78061 = AXIS2_PLACEMENT_3D ( 'NONE', #2685, #31259, #9056 ) ;
#78062 = EDGE_CURVE ( 'NONE', #23208, #86726, #38034, .T. ) ;
#78063 = CARTESIAN_POINT ( 'NONE',  ( 7.620115932400929327E-15, 67.86880000000000734, 221.5895999999999901 ) ) ;
#78064 = VECTOR ( 'NONE', #88651, 1000.000000000000000 ) ;
#78065 = CARTESIAN_POINT ( 'NONE',  ( 156.5667039024483245, -42.82844715993568485, 170.7178068554149775 ) ) ;
#78066 = DIRECTION ( 'NONE',  ( 1.000000000000000078E-15, -1.000000000000000000, 0.000000000000000000 ) ) ;
#78067 = ORIENTED_EDGE ( 'NONE', *, *, #77706, .F. ) ;
#78068 = VECTOR ( 'NONE', #38953, 1000.000000000000000 ) ;
#78069 = ORIENTED_EDGE ( 'NONE', *, *, #82638, .F. ) ;
#78070 = VERTEX_POINT ( 'NONE', #9437 ) ;
#78071 = VERTEX_POINT ( 'NONE', #37148 ) ;
#78072 = PLANE ( 'NONE',  #51083 ) ;
#78073 = CARTESIAN_POINT ( 'NONE',  ( 118.0406971908402340, -35.41012545131285094, 234.9337205140059552 ) ) ;
#78074 = CYLINDRICAL_SURFACE ( 'NONE', #86711, 12.70000000000000107 ) ;
#78075 = DIRECTION ( 'NONE',  ( -0.8660254037844382635, -0.5000000000000008882, 1.550000000000000022E-14 ) ) ;
#78077 = LINE ( 'NONE', #15838, #18101 ) ;
#78076 = CARTESIAN_POINT ( 'NONE',  ( 25.56670390244797275, -67.87844715994100397, 173.2178068554149775 ) ) ;
#78078 = DIRECTION ( 'NONE',  ( -7.980413499659419871E-32, -1.000000000000000000, 3.785359618865284342E-16 ) ) ;
#78079 = CARTESIAN_POINT ( 'NONE',  ( 101.3720933679328482, -27.97043537882594322, 25.53562527591096654 ) ) ;
#78080 = ORIENTED_EDGE ( 'NONE', *, *, #43934, .F. ) ;
#78081 = VECTOR ( 'NONE', #62396, 1000.000000000000000 ) ;
#78082 = VERTEX_POINT ( 'NONE', #64849 ) ;
#78083 = ORIENTED_EDGE ( 'NONE', *, *, #66917, .T. ) ;
#78084 = LINE ( 'NONE', #36738, #35475 ) ;
#78085 = DIRECTION ( 'NONE',  ( 0.000000000000000000, 0.000000000000000000, -1.000000000000000000 ) ) ;
#78086 = CARTESIAN_POINT ( 'NONE',  ( 111.4826097991074079, -46.11499196468592743, 283.9146728949579597 ) ) ;
#78087 = PLANE ( 'NONE',  #70468 ) ;
#78088 = CARTESIAN_POINT ( 'NONE',  ( 114.2951562036312936, -44.16484043540973659, 114.2022919425769771 ) ) ;
#78089 = CARTESIAN_POINT ( 'NONE',  ( 77.06670390244701707, -90.27844715994098124, 222.2178068554179902 ) ) ;
#78090 = ORIENTED_EDGE ( 'NONE', *, *, #16458, .F. ) ;
#78091 = DIRECTION ( 'NONE',  ( 0.000000000000000000, 0.000000000000000000, -1.000000000000000000 ) ) ;
#78092 = CARTESIAN_POINT ( 'NONE',  ( 77.96925277058818438, -34.94806367530411251, 2.376725340801996378 ) ) ;
#78093 = EDGE_LOOP ( 'NONE', ( #42467, #16981, #34009, #73139 ) ) ;
#78094 = CARTESIAN_POINT ( 'NONE',  ( -74.36911441044735227, 83.38952084682851762, 92.32962665258540369 ) ) ;
#78095 = CARTESIAN_POINT ( 'NONE',  ( 111.0839405624553251, -29.06298261359865975, 12.49856656006798161 ) ) ;
#78096 = VECTOR ( 'NONE', #7449, 1000.000000000000000 ) ;
#78097 = VECTOR ( 'NONE', #28189, 1000.000000000000000 ) ;
#78098 =( BOUNDED_CURVE ( )  B_SPLINE_CURVE ( 3, ( #66143, #11649, #31627, #45679 ),
 .UNSPECIFIED., .F., .F. ) 
 B_SPLINE_CURVE_WITH_KNOTS ( ( 4, 4 ),
 ( 5.813027347256380040, 6.283185307179586232 ),
 .UNSPECIFIED. ) 
 CURVE ( )  GEOMETRIC_REPRESENTATION_ITEM ( )  RATIONAL_B_SPLINE_CURVE ( ( 1.000000000000000000, 0.9816639655796099984, 0.9816639655796099984, 1.000000000000000000 ) ) 
 REPRESENTATION_ITEM ( '' )  );
#78099 = CARTESIAN_POINT ( 'NONE',  ( 107.0667039024479834, -36.72944715994100306, 239.5838068554170093 ) ) ;
#78100 = EDGE_CURVE ( 'NONE', #67129, #85840, #52670, .T. ) ;
#78101 = EDGE_CURVE ( 'NONE', #31104, #71751, #81181, .T. ) ;
#78102 = FACE_OUTER_BOUND ( 'NONE', #41104, .T. ) ;
#78103 = CARTESIAN_POINT ( 'NONE',  ( 91.50401754987822756, 76.93600387762165838, -75.38287938184973314 ) ) ;
#78104 = ORIENTED_EDGE ( 'NONE', *, *, #19410, .F. ) ;
#78105 = DIRECTION ( 'NONE',  ( 0.000000000000000000, 1.000000000000000000, 0.000000000000000000 ) ) ;
#78107 = EDGE_CURVE ( 'NONE', #22201, #38380, #33893, .T. ) ;
#78106 = VECTOR ( 'NONE', #3795, 1000.000000000000000 ) ;
#78108 = DIRECTION ( 'NONE',  ( 1.000000000000000000, 4.299999999999999979E-14, 1.000000000000000078E-15 ) ) ;
#78109 = ORIENTED_EDGE ( 'NONE', *, *, #73775, .T. ) ;
#78110 = CARTESIAN_POINT ( 'NONE',  ( 100.9430784815160251, -28.29197455274081463, 75.57562527591093726 ) ) ;
#78111 = B_SPLINE_CURVE_WITH_KNOTS ( 'NONE', 3,
 ( #45777, #4475, #68934, #55715, #34856, #48909, #76647, #69388, #14433, #33951, #42110, #69836, #83034, #68494, #76192, #27596, #75756, #20788 ),
 .UNSPECIFIED., .F., .F.,
 ( 4, 2, 2, 2, 2, 2, 2, 2, 4 ),
 ( 0.000000000000000000, 0.06249999986974735799, 0.1249999997394947160, 0.1874999996092420740, 0.2499999994789894320, 0.3124999993487367900, 0.3749999992184841480, 0.4374999990882315060, 0.4999999989579788640 ),
 .UNSPECIFIED. ) ;
#78112 = VERTEX_POINT ( 'NONE', #46614 ) ;
#78113 = CARTESIAN_POINT ( 'NONE',  ( 111.8977291718574065, -29.68564172797395528, 44.02099125664899049 ) ) ;
#78114 = VECTOR ( 'NONE', #20213, 1000.000000000000000 ) ;
#78115 = ADVANCED_FACE ( 'NONE', ( #12116 ), #61391, .T. ) ;
#78116 = LINE ( 'NONE', #58527, #66329 ) ;
#78117 = CARTESIAN_POINT ( 'NONE',  ( 111.1483613326457913, -47.07112276671761464, 172.8756252759109771 ) ) ;
#78118 = CARTESIAN_POINT ( 'NONE',  ( -21.75527563292445521, 47.22364764115523172, 31.28221943681005257 ) ) ;
#78119 = FACE_OUTER_BOUND ( 'NONE', #20938, .T. ) ;
#78120 = AXIS2_PLACEMENT_3D ( 'NONE', #80658, #11611, #24787 ) ;
#78121 = FACE_OUTER_BOUND ( 'NONE', #21814, .T. ) ;
#78122 = AXIS2_PLACEMENT_3D ( 'NONE', #63165, #64521, #44499 ) ;
#78123 = LINE ( 'NONE', #15884, #27658 ) ;
#78124 = CARTESIAN_POINT ( 'NONE',  ( 96.51983850151567879, -40.19180362902228865, 282.5908633711491120 ) ) ;
#78125 = EDGE_CURVE ( 'NONE', #19557, #27791, #73010, .T. ) ;
#78126 = VERTEX_POINT ( 'NONE', #74788 ) ;
#78127 = LINE ( 'NONE', #71305, #85041 ) ;
#78128 = ORIENTED_EDGE ( 'NONE', *, *, #82554, .T. ) ;
#78129 = CARTESIAN_POINT ( 'NONE',  ( 98.24414503606394078, -31.02815815664761345, 141.8699109901969564 ) ) ;
#78130 = CARTESIAN_POINT ( 'NONE',  ( 116.3212776292296127, -32.94146857471318413, 287.6356252759109680 ) ) ;
#78131 = ORIENTED_EDGE ( 'NONE', *, *, #69822, .T. ) ;
#78132 = VERTEX_POINT ( 'NONE', #47054 ) ;
#78133 = EDGE_CURVE ( 'NONE', #86269, #66733, #47507, .T. ) ;
#78134 = ORIENTED_EDGE ( 'NONE', *, *, #31285, .T. ) ;
#78135 = CIRCLE ( 'NONE', #38936, 0.5000000000000004441 ) ;
#78136 = FACE_OUTER_BOUND ( 'NONE', #77552, .T. ) ;
#78137 = DIRECTION ( 'NONE',  ( 9.299908063537919123E-17, 0.000000000000000000, 1.000000000000000000 ) ) ;
#78138 = DIRECTION ( 'NONE',  ( 0.000000000000000000, 0.000000000000000000, -1.000000000000000000 ) ) ;
#78139 = PLANE ( 'NONE',  #78599 ) ;
#78140 = DIRECTION ( 'NONE',  ( 0.000000000000000000, 0.000000000000000000, -1.000000000000000000 ) ) ;
#78141 = CARTESIAN_POINT ( 'NONE',  ( 97.79230575738172604, -40.52535926896634777, 7.635625275910939536 ) ) ;
#78142 = ADVANCED_FACE ( 'NONE', ( #74345 ), #32540, .F. ) ;
#78143 = DIRECTION ( 'NONE',  ( 0.000000000000000000, 1.000000000000000000, 0.000000000000000000 ) ) ;
#78144 = VERTEX_POINT ( 'NONE', #40706 ) ;
#78145 = CARTESIAN_POINT ( 'NONE',  ( 108.6169522717627700, -26.81698160835030365, 170.9531425218682159 ) ) ;
#78146 = AXIS2_PLACEMENT_3D ( 'NONE', #78231, #44108, #32726 ) ;
#78147 = CARTESIAN_POINT ( 'NONE',  ( 109.2774118001976120, 53.97500000000000142, 71.43750000000000000 ) ) ;
#78148 = ORIENTED_EDGE ( 'NONE', *, *, #23886, .F. ) ;
#78151 = ORIENTED_EDGE ( 'NONE', *, *, #86425, .F. ) ;
#78150 = EDGE_CURVE ( 'NONE', #12059, #41030, #88963, .T. ) ;
#78149 = VECTOR ( 'NONE', #27009, 1000.000000000000000 ) ;
#78152 = CARTESIAN_POINT ( 'NONE',  ( 90.44969454456413871, -53.34645651782494724, 239.5838068554169809 ) ) ;
#78153 = DIRECTION ( 'NONE',  ( 1.000000000000000000, 0.000000000000000000, 0.000000000000000000 ) ) ;
#78154 = PLANE ( 'NONE',  #76250 ) ;
#78155 = DIRECTION ( 'NONE',  ( 1.000000000000000000, 1.000000000000000078E-15, 0.000000000000000000 ) ) ;
#78156 = LINE ( 'NONE', #79039, #59187 ) ;
#78157 = CARTESIAN_POINT ( 'NONE',  ( 113.9904334582008545, -30.89236017996071837, 223.7943245899819829 ) ) ;
#78159 = CARTESIAN_POINT ( 'NONE',  ( 105.9906760191434358, -26.38192068051327510, 46.15848241876796720 ) ) ;
#78158 = DIRECTION ( 'NONE',  ( 0.000000000000000000, 0.000000000000000000, -1.000000000000000000 ) ) ;
#78160 = CARTESIAN_POINT ( 'NONE',  ( 125.5854509285793910, 68.02811073279640652, 35.68229276901666225 ) ) ;
#78161 = CARTESIAN_POINT ( 'NONE',  ( 115.2418052506917832, -44.23790868596334747, 78.22324432352995416 ) ) ;
#78162 = ORIENTED_EDGE ( 'NONE', *, *, #89792, .T. ) ;
#78163 = DIRECTION ( 'NONE',  ( -0.7071067812159675947, -0.7071067811571274397, -7.071067812159669175E-16 ) ) ;
#78164 = ORIENTED_EDGE ( 'NONE', *, *, #27687, .F. ) ;
#78165 = CARTESIAN_POINT ( 'NONE',  ( 104.4899544225926604, -26.97880759208219104, 66.28145861163227437 ) ) ;
#78166 = CARTESIAN_POINT ( 'NONE',  ( 103.2772504383587915, -27.47516629124199383, 276.3857340133070011 ) ) ;
#78167 = EDGE_LOOP ( 'NONE', ( #66884, #27031, #24446, #48996 ) ) ;
#78168 = EDGE_CURVE ( 'NONE', #54510, #22506, #62885, .T. ) ;
#78169 = AXIS2_PLACEMENT_3D ( 'NONE', #35226, #83850, #42038 ) ;
#78170 = LINE ( 'NONE', #8670, #47597 ) ;
#78171 = ORIENTED_EDGE ( 'NONE', *, *, #71952, .T. ) ;
#78172 = DIRECTION ( 'NONE',  ( 0.000000000000000000, 1.000000000000000000, 0.000000000000000000 ) ) ;
#78173 = EDGE_CURVE ( 'NONE', #36895, #49620, #18471, .T. ) ;
#78174 = DIRECTION ( 'NONE',  ( 0.000000000000000000, 0.000000000000000000, -1.000000000000000000 ) ) ;
#78176 = DIRECTION ( 'NONE',  ( -1.000000000000000000, 6.036837696399408848E-13, 0.000000000000000000 ) ) ;
#78175 = VECTOR ( 'NONE', #29573, 1000.000000000000000 ) ;
#78177 = VERTEX_POINT ( 'NONE', #67075 ) ;
#78178 = CIRCLE ( 'NONE', #14354, 20.00000000000000355 ) ;
#78179 = CARTESIAN_POINT ( 'NONE',  ( 117.4695374193713775, -37.69008693337416815, 78.75276813305399060 ) ) ;
#78180 = DIRECTION ( 'NONE',  ( 0.000000000000000000, 0.000000000000000000, 1.000000000000000000 ) ) ;
#78181 = CARTESIAN_POINT ( 'NONE',  ( 97.31309759000943416, -38.96071495204963497, 166.5054468050763603 ) ) ;
#78182 = CARTESIAN_POINT ( 'NONE',  ( 152.0368932755772562, -23.42844715993587812, 180.4678068554149775 ) ) ;
#78183 = DIRECTION ( 'NONE',  ( 1.000000000000000000, 0.000000000000000000, 0.000000000000000000 ) ) ;
#78184 = VERTEX_POINT ( 'NONE', #11212 ) ;
#78185 = VECTOR ( 'NONE', #37661, 1000.000000000000000 ) ;
#78186 = LINE ( 'NONE', #36828, #31507 ) ;
#78187 = CARTESIAN_POINT ( 'NONE',  ( 24.79284581386643183, 127.0000000000000000, -0.000000000000000000 ) ) ;
#78188 = CARTESIAN_POINT ( 'NONE',  ( 116.3201495438094923, -32.94088975182634726, 124.1356252759109537 ) ) ;
#78189 = ADVANCED_FACE ( 'NONE', ( #6205 ), #87528, .T. ) ;
#78190 = AXIS2_PLACEMENT_3D ( 'NONE', #84319, #27979, #76589 ) ;
#78192 = CARTESIAN_POINT ( 'NONE',  ( 83.96770390244806492, -18.82844715994099971, 168.9256252759119548 ) ) ;
#78191 = CARTESIAN_POINT ( 'NONE',  ( 6.938893903907229955E-15, 67.86880000000000734, 216.0269999999999868 ) ) ;
#78193 = DIRECTION ( 'NONE',  ( 0.000000000000000000, 0.000000000000000000, 1.000000000000000000 ) ) ;
#78194 = ADVANCED_FACE ( 'NONE', ( #5306 ), #87976, .T. ) ;
#78195 = VERTEX_POINT ( 'NONE', #81630 ) ;
#78196 = DIRECTION ( 'NONE',  ( -0.7071067811865439090, 0.000000000000000000, -0.7071067811865512365 ) ) ;
#78197 = CARTESIAN_POINT ( 'NONE',  ( 100.4443968677459935, -27.79860430499269697, 181.5841967044819683 ) ) ;
#78198 = VECTOR ( 'NONE', #61238, 1000.000000000000000 ) ;
#78200 = EDGE_LOOP ( 'NONE', ( #55938, #7993 ) ) ;
#78199 = DIRECTION ( 'NONE',  ( 1.000000000000000078E-15, 1.000000000000000083E-30, -1.000000000000000000 ) ) ;
#78201 = CARTESIAN_POINT ( 'NONE',  ( 105.2810544170623359, -46.37316503544239765, 8.429910990195965681 ) ) ;
#78202 = LINE ( 'NONE', #79088, #33866 ) ;
#78203 = CARTESIAN_POINT ( 'NONE',  ( 107.0667039024470313, -104.2784471599409102, 17.71780685541799016 ) ) ;
#78204 = FACE_OUTER_BOUND ( 'NONE', #8239, .T. ) ;
#78205 = FACE_OUTER_BOUND ( 'NONE', #78611, .T. ) ;
#78206 = CARTESIAN_POINT ( 'NONE',  ( 105.8005514283656225, -26.72389458433680076, 30.17743840264089528 ) ) ;
#78207 = CARTESIAN_POINT ( 'NONE',  ( 106.5981863181247462, -46.53222597210214673, 247.5384824187689787 ) ) ;
#78208 = ORIENTED_EDGE ( 'NONE', *, *, #27281, .T. ) ;
#78209 = ORIENTED_EDGE ( 'NONE', *, *, #75604, .T. ) ;
#78210 = VECTOR ( 'NONE', #1444, 1000.000000000000000 ) ;
#78211 = CARTESIAN_POINT ( 'NONE',  ( 97.82234778274722942, -32.72736474536957019, 207.4330118773259528 ) ) ;
#78212 = DIRECTION ( 'NONE',  ( 0.000000000000000000, 1.000000000000000000, 0.000000000000000000 ) ) ;
#78213 = CARTESIAN_POINT ( 'NONE',  ( 97.82387236378413320, -38.41783952554947490, 47.91396425827898753 ) ) ;
#78214 = CARTESIAN_POINT ( 'NONE',  ( -92.89936586971981569, 95.23006786499111342, 91.73195104381176179 ) ) ;
#78215 = EDGE_CURVE ( 'NONE', #46288, #78417, #54758, .T. ) ;
#78216 = EDGE_CURVE ( 'NONE', #56160, #30248, #18025, .T. ) ;
#78217 = DIRECTION ( 'NONE',  ( 0.000000000000000000, 0.000000000000000000, -1.000000000000000000 ) ) ;
#78218 = DIRECTION ( 'NONE',  ( 0.000000000000000000, 0.4999999999999998890, -0.8660254037844387076 ) ) ;
#78219 = VERTEX_POINT ( 'NONE', #32995 ) ;
#78220 = CARTESIAN_POINT ( 'NONE',  ( 4.163101094985349692E-14, 120.6499999999999915, -98.60478223830740774 ) ) ;
#78221 = EDGE_CURVE ( 'NONE', #38949, #14757, #60693, .T. ) ;
#78222 = DIRECTION ( 'NONE',  ( 1.639958061481212836E-42, -4.100000000000000342E-29, -1.000000000000000000 ) ) ;
#78223 = CARTESIAN_POINT ( 'NONE',  ( 115.0380569359702463, -30.04493676975920380, 269.3813395616251682 ) ) ;
#78224 = CARTESIAN_POINT ( 'NONE',  ( 106.0667039024470171, -87.35579742913164125, -19.26696060647653397 ) ) ;
#78225 = VERTEX_POINT ( 'NONE', #26192 ) ;
#78226 = VERTEX_POINT ( 'NONE', #19379 ) ;
#78227 = VECTOR ( 'NONE', #19601, 1000.000000000000000 ) ;
#78228 = EDGE_CURVE ( 'NONE', #87676, #37352, #61153, .T. ) ;
#78229 = DIRECTION ( 'NONE',  ( 1.000000000000000078E-15, -1.000000000000000000, 0.000000000000000000 ) ) ;
#78230 = LINE ( 'NONE', #65466, #1204 ) ;
#78231 = CARTESIAN_POINT ( 'NONE',  ( 163.0664832912739826, 19.62155284005901024, 333.4006252759110112 ) ) ;
#78232 = DIRECTION ( 'NONE',  ( 0.000000000000000000, 0.000000000000000000, -1.000000000000000000 ) ) ;
#78233 = CARTESIAN_POINT ( 'NONE',  ( 97.69287098190334007, -33.93680905855630670, 27.09562527591097236 ) ) ;
#78235 = CARTESIAN_POINT ( 'NONE',  ( 61.67078992371376245, -0.9290567490904538817, 542.9756252759101471 ) ) ;
#78234 = VECTOR ( 'NONE', #26330, 1000.000000000000000 ) ;
#78236 = AXIS2_PLACEMENT_3D ( 'NONE', #8167, #45228, #86597 ) ;
#78237 = EDGE_CURVE ( 'NONE', #47917, #1770, #70158, .T. ) ;
#78238 = ORIENTED_EDGE ( 'NONE', *, *, #14013, .T. ) ;
#78239 = CARTESIAN_POINT ( 'NONE',  ( 96.13205292066136565, -38.63620640773733328, 42.45181575210199298 ) ) ;
#78240 = CARTESIAN_POINT ( 'NONE',  ( 72.06648329127256147, -9.729447159940422196, -4.970821333494543026 ) ) ;
#78241 = CARTESIAN_POINT ( 'NONE',  ( 118.5953454549360231, -33.89261193510051839, 14.01848241876796308 ) ) ;
#78242 = VERTEX_POINT ( 'NONE', #48392 ) ;
#78243 = EDGE_CURVE ( 'NONE', #85401, #6767, #59949, .T. ) ;
#78244 = AXIS2_PLACEMENT_3D ( 'NONE', #68717, #40997, #34636 ) ;
#78245 = CARTESIAN_POINT ( 'NONE',  ( 199.3900000000000148, 52.73749999999999716, -41.27499999999999858 ) ) ;
#78246 = CARTESIAN_POINT ( 'NONE',  ( 82.81648329127399677, -18.72944715994105636, -5.074374724089055100 ) ) ;
#78247 =( GEOMETRIC_REPRESENTATION_CONTEXT ( 3 ) GLOBAL_UNCERTAINTY_ASSIGNED_CONTEXT ( ( #36914 ) ) GLOBAL_UNIT_ASSIGNED_CONTEXT ( ( #36918, #10990, #37365 ) ) REPRESENTATION_CONTEXT ( 'NONE', 'WORKASPACE' ) );
#78248 = LINE ( 'NONE', #23288, #39334 ) ;
#78249 = CARTESIAN_POINT ( 'NONE',  ( 100.2308834438963174, -41.19087078291441628, 99.60523322673398638 ) ) ;
#78250 = CARTESIAN_POINT ( 'NONE',  ( 96.16865940696823145, -32.01143006853777706, 207.0013395616249738 ) ) ;
#78251 = DIRECTION ( 'NONE',  ( 1.000000000000000000, 1.132880637372608296E-15, 0.000000000000000000 ) ) ;
#78252 = ORIENTED_EDGE ( 'NONE', *, *, #36168, .F. ) ;
#78253 = AXIS2_PLACEMENT_3D ( 'NONE', #39263, #12915, #89668 ) ;
#78254 = FACE_OUTER_BOUND ( 'NONE', #45896, .T. ) ;
#78255 = VERTEX_POINT ( 'NONE', #41589 ) ;
#78256 = ORIENTED_EDGE ( 'NONE', *, *, #16404, .T. ) ;
#78257 = PLANE ( 'NONE',  #79296 ) ;
#78258 = VERTEX_POINT ( 'NONE', #276 ) ;
#78259 = ORIENTED_EDGE ( 'NONE', *, *, #85969, .T. ) ;
#78260 = DIRECTION ( 'NONE',  ( 0.7071067811865535679, -0.7071067811865415775, 7.071067811865230786E-16 ) ) ;
#78261 = CARTESIAN_POINT ( 'NONE',  ( 114.7326334688429483, -30.28293645095888209, 40.38281810511883663 ) ) ;
#78262 = AXIS2_PLACEMENT_3D ( 'NONE', #27291, #75896, #13664 ) ;
#78263 = CARTESIAN_POINT ( 'NONE',  ( 115.3871705984363984, -41.73312485046139386, 127.8181341137909470 ) ) ;
#78264 = CARTESIAN_POINT ( 'NONE',  ( 96.89273651078235616, -34.20293982824353662, 276.1327681330536734 ) ) ;
#78265 = DIRECTION ( 'NONE',  ( 0.000000000000000000, 0.000000000000000000, -1.000000000000000000 ) ) ;
#78266 = ORIENTED_EDGE ( 'NONE', *, *, #46994, .F. ) ;
#78267 = EDGE_LOOP ( 'NONE', ( #43094, #30787 ) ) ;
#78268 = FACE_OUTER_BOUND ( 'NONE', #8158, .T. ) ;
#78269 = FACE_OUTER_BOUND ( 'NONE', #52918, .T. ) ;
#78270 = EDGE_CURVE ( 'NONE', #75751, #4284, #55208, .T. ) ;
#78271 = PLANE ( 'NONE',  #61483 ) ;
#78272 = AXIS2_PLACEMENT_3D ( 'NONE', #8492, #48435, #49800 ) ;
#78273 = CARTESIAN_POINT ( 'NONE',  ( 113.8852007176727028, -44.67373811025045427, 108.1413395616249744 ) ) ;
#78274 = CARTESIAN_POINT ( 'NONE',  ( 63.50000000000000000, 69.84999999999999432, 219.0749999999999886 ) ) ;
#78275 = VERTEX_POINT ( 'NONE', #28885 ) ;
#78276 = CARTESIAN_POINT ( 'NONE',  ( 100.8483124575627414, -45.14135884264823773, 257.0699109901967745 ) ) ;
#78277 = CARTESIAN_POINT ( 'NONE',  ( 61.68306511546570903, -72.55869591834560595, 542.9756252759101471 ) ) ;
#78278 = FACE_BOUND ( 'NONE', #73525, .T. ) ;
#78280 = PLANE ( 'NONE',  #16640 ) ;
#78279 = CARTESIAN_POINT ( 'NONE',  ( 140.0667039024470171, -90.27844715994091018, 222.2178068554179902 ) ) ;
#78281 = DIRECTION ( 'NONE',  ( 1.175184669632759901E-16, -1.000000000000000000, -2.000000000000003705E-15 ) ) ;
#78282 = FACE_OUTER_BOUND ( 'NONE', #8063, .T. ) ;
#78283 = CARTESIAN_POINT ( 'NONE',  ( 131.4622572338342934, -37.61690131753618971, 6.952852217895568288 ) ) ;
#78284 = VECTOR ( 'NONE', #2570, 1000.000000000000114 ) ;
#78285 = DIRECTION ( 'NONE',  ( 1.000000000000000078E-15, 0.000000000000000000, -1.000000000000000000 ) ) ;
#78286 = PLANE ( 'NONE',  #73530 ) ;
#78287 = FACE_BOUND ( 'NONE', #6663, .T. ) ;
#78288 = FACE_OUTER_BOUND ( 'NONE', #37982, .T. ) ;
#78289 = AXIS2_PLACEMENT_3D ( 'NONE', #48405, #76138, #33461 ) ;
#78290 = CARTESIAN_POINT ( 'NONE',  ( 63.56670390244828184, -47.82844715994016127, 249.9678068554150343 ) ) ;
#78291 = CARTESIAN_POINT ( 'NONE',  ( 116.8111099997371554, -31.41389126640522989, 24.21181575210196257 ) ) ;
#78292 = CARTESIAN_POINT ( 'NONE',  ( 96.05396905170981370, -35.78154916559406473, 182.2461014663869889 ) ) ;
#78293 = CARTESIAN_POINT ( 'NONE',  ( 117.5626006132557535, -36.54510529939036445, 284.8413395616253752 ) ) ;
#78295 = DIRECTION ( 'NONE',  ( 0.000000000000000000, 0.000000000000000000, -1.000000000000000000 ) ) ;
#78294 = CARTESIAN_POINT ( 'NONE',  ( 85.06670390244701707, -80.35669973212957018, 55.21780685541800437 ) ) ;
#78296 = CARTESIAN_POINT ( 'NONE',  ( 101.9935118427002152, -45.44600903161029493, 138.1564489287590334 ) ) ;
#78297 = VECTOR ( 'NONE', #56208, 1000.000000000000000 ) ;
#78298 = AXIS2_PLACEMENT_3D ( 'NONE', #2033, #57428, #3809 ) ;
#78299 = EDGE_CURVE ( 'NONE', #73456, #39861, #69322, .T. ) ;
#78300 = ORIENTED_EDGE ( 'NONE', *, *, #10249, .T. ) ;
#78301 = DIRECTION ( 'NONE',  ( 0.000000000000000000, 1.000000000000000000, 0.000000000000000000 ) ) ;
#78302 = ORIENTED_EDGE ( 'NONE', *, *, #88661, .F. ) ;
#78303 = CARTESIAN_POINT ( 'NONE',  ( 118.1148702536303290, -35.48641528967803538, 79.91562527591095488 ) ) ;
#78304 = VECTOR ( 'NONE', #44688, 1000.000000000000000 ) ;
#78306 = ORIENTED_EDGE ( 'NONE', *, *, #6008, .T. ) ;
#78305 = CARTESIAN_POINT ( 'NONE',  ( 6.719641267068065638, 93.32766509845849612, 130.3830046867565500 ) ) ;
#78307 = DIRECTION ( 'NONE',  ( -1.000000000000000078E-15, 1.000000000000000000, 0.000000000000000000 ) ) ;
#78308 = CARTESIAN_POINT ( 'NONE',  ( 101.2129617469313132, -45.32973500739954886, 193.1013395616249682 ) ) ;
#78309 = LINE ( 'NONE', #71489, #88998 ) ;
#78310 = CARTESIAN_POINT ( 'NONE',  ( -59.93649209371488951, 82.54999999999999716, -77.89700433585392148 ) ) ;
#78311 = FACE_OUTER_BOUND ( 'NONE', #41962, .T. ) ;
#78312 = CARTESIAN_POINT ( 'NONE',  ( 110.8029255159877806, -27.45356875239903971, 85.77192066089217803 ) ) ;
#78313 = PLANE ( 'NONE',  #43350 ) ;
#78314 = CARTESIAN_POINT ( 'NONE',  ( -72.96458098368751166, 127.0000000000000000, 67.92268098368620599 ) ) ;
#78315 = CARTESIAN_POINT ( 'NONE',  ( 99.54941199951403519, -42.98700854487248080, 116.8784824187689679 ) ) ;
#78316 = ORIENTED_EDGE ( 'NONE', *, *, #40174, .F. ) ;
#78317 = ORIENTED_EDGE ( 'NONE', *, *, #47000, .F. ) ;
#78318 = CARTESIAN_POINT ( 'NONE',  ( 99.53176374547611260, -42.34233651421938305, 108.2796785439919773 ) ) ;
#78320 = CIRCLE ( 'NONE', #11587, 4.762500000000002842 ) ;
#78319 = CARTESIAN_POINT ( 'NONE',  ( -7.205548786489490269E-13, 127.0000000000000000, 96.04375000000000284 ) ) ;
#78322 = CARTESIAN_POINT ( 'NONE',  ( 73.06670390244801183, -58.72944715994110254, 250.9178068554160461 ) ) ;
#78321 = CARTESIAN_POINT ( 'NONE',  ( 117.3624379696766198, -35.49166588079122420, 234.9337205140059552 ) ) ;
#78323 = LINE ( 'NONE', #85586, #28992 ) ;
#78324 = CARTESIAN_POINT ( 'NONE',  ( 97.07206919424615421, -35.37846131109193948, 112.2194697797737462 ) ) ;
#78325 = EDGE_CURVE ( 'NONE', #61270, #6171, #6286, .T. ) ;
#78326 = AXIS2_PLACEMENT_3D ( 'NONE', #34782, #82957, #62487 ) ;
#78327 = FACE_OUTER_BOUND ( 'NONE', #12522, .T. ) ;
#78328 = CARTESIAN_POINT ( 'NONE',  ( 0.000000000000000000, 0.000000000000000000, 0.000000000000000000 ) ) ;
#78329 = EDGE_CURVE ( 'NONE', #43857, #74189, #47950, .T. ) ;
#78330 = CARTESIAN_POINT ( 'NONE',  ( 97.81219835445369881, -40.51719899421586746, 151.6362400511890769 ) ) ;
#78331 = CARTESIAN_POINT ( 'NONE',  ( 108.7397100058831541, -25.82697924850565840, 144.9432443235299672 ) ) ;
#78332 = ORIENTED_EDGE ( 'NONE', *, *, #83309, .T. ) ;
#78333 = EDGE_CURVE ( 'NONE', #29833, #23923, #21177, .T. ) ;
#78334 = VERTEX_POINT ( 'NONE', #20286 ) ;
#78335 = VERTEX_POINT ( 'NONE', #48846 ) ;
#78336 = EDGE_CURVE ( 'NONE', #79343, #64560, #42570, .T. ) ;
#78337 = CARTESIAN_POINT ( 'NONE',  ( 0.8390482630167189759, 69.85000000000000853, 130.5560000000000400 ) ) ;
#78338 = CARTESIAN_POINT ( 'NONE',  ( 51.03742451361318189, -23.42844715994068849, 117.4678068554150485 ) ) ;
#78339 = CARTESIAN_POINT ( 'NONE',  ( 105.7980258636739279, -26.72423388751797546, 130.1774127513859867 ) ) ;
#78340 = CARTESIAN_POINT ( 'NONE',  ( 99.50448107662171537, -43.30550302426849640, 102.8959900338089994 ) ) ;
#78341 = CARTESIAN_POINT ( 'NONE',  ( 105.5353399150147737, -28.71163411781831698, 233.0452332267339841 ) ) ;
#78342 = VECTOR ( 'NONE', #20557, 1000.000000000000114 ) ;
#78343 = CYLINDRICAL_SURFACE ( 'NONE', #88633, 2.500000000000002220 ) ;
#78344 = CARTESIAN_POINT ( 'NONE',  ( 108.2778356434855027, -47.71639565607667066, 157.6518157521019532 ) ) ;
#78345 = DIRECTION ( 'NONE',  ( 0.000000000000000000, 0.000000000000000000, -1.000000000000000000 ) ) ;
#78346 = ORIENTED_EDGE ( 'NONE', *, *, #51122, .T. ) ;
#78348 = ORIENTED_EDGE ( 'NONE', *, *, #65582, .T. ) ;
#78347 = ORIENTED_EDGE ( 'NONE', *, *, #68176, .F. ) ;
#78349 = EDGE_CURVE ( 'NONE', #67882, #88995, #57051, .T. ) ;
#78350 = CIRCLE ( 'NONE', #68140, 2.030000000001311644 ) ;
#78351 = DIRECTION ( 'NONE',  ( 1.000000000000000000, 4.299999999999999979E-14, 1.000000000000000078E-15 ) ) ;
#78352 = VERTEX_POINT ( 'NONE', #27530 ) ;
#78353 = VERTEX_POINT ( 'NONE', #15259 ) ;
#78354 = CARTESIAN_POINT ( 'NONE',  ( 116.3263622980238097, -32.93962144782776846, 195.1356252759109680 ) ) ;
#78355 = DIRECTION ( 'NONE',  ( 0.7071067811862279395, -0.7071067811868672059, 7.071067811862286363E-16 ) ) ;
#78356 = CARTESIAN_POINT ( 'NONE',  ( 115.1162204959661466, -41.57488383322457537, 274.8149166392303755 ) ) ;
#78357 = AXIS2_PLACEMENT_3D ( 'NONE', #50553, #176, #21533 ) ;
#78358 = DIRECTION ( 'NONE',  ( 0.000000000000000000, -1.000000000000000000, 0.000000000000000000 ) ) ;
#78359 = VERTEX_POINT ( 'NONE', #1179 ) ;
#78360 = CARTESIAN_POINT ( 'NONE',  ( 114.9151178457587577, -41.28570029556458820, 9.635625275910941312 ) ) ;
#78361 = DIRECTION ( 'NONE',  ( 0.000000000000000000, 0.000000000000000000, -1.000000000000000000 ) ) ;
#78362 = ORIENTED_EDGE ( 'NONE', *, *, #14863, .F. ) ;
#78364 = ORIENTED_EDGE ( 'NONE', *, *, #18313, .F. ) ;
#78363 = VECTOR ( 'NONE', #86181, 1000.000000000000000 ) ;
#78365 = CARTESIAN_POINT ( 'NONE',  ( 105.7155658375387333, -46.72387182276721518, 112.4690335037959557 ) ) ;
#78366 = ORIENTED_EDGE ( 'NONE', *, *, #44750, .F. ) ;
#78367 = ORIENTED_EDGE ( 'NONE', *, *, #86918, .F. ) ;
#78368 = CARTESIAN_POINT ( 'NONE',  ( 99.98530978427844218, -41.10337153935440568, 11.19051506617196878 ) ) ;
#78369 = AXIS2_PLACEMENT_3D ( 'NONE', #68283, #20583, #6063 ) ;
#78370 = CARTESIAN_POINT ( 'NONE',  ( 108.2803926554762626, -47.73958771823362213, 157.6518157521019532 ) ) ;
#78371 = CARTESIAN_POINT ( 'NONE',  ( 96.72090476913461998, -37.82382852467500811, 126.4099109901969626 ) ) ;
#78372 = DIRECTION ( 'NONE',  ( 0.000000000000000000, 0.000000000000000000, 1.000000000000000000 ) ) ;
#78373 = PRODUCT_DEFINITION_FORMATION_WITH_SPECIFIED_SOURCE ( 'ANY', '', #60498, .NOT_KNOWN. ) ;
#78374 = CARTESIAN_POINT ( 'NONE',  ( 117.7763469108053869, -31.65663365956905650, 210.1784824187679703 ) ) ;
#78375 = FACE_OUTER_BOUND ( 'NONE', #8480, .T. ) ;
#78376 = CARTESIAN_POINT ( 'NONE',  ( 74.25553510437300986, -77.53446767201269552, 248.3919653347779786 ) ) ;
#78377 = ORIENTED_EDGE ( 'NONE', *, *, #53976, .F. ) ;
#78378 = CARTESIAN_POINT ( 'NONE',  ( -130.4354319819074703, 71.15434825076370373, 5.621545387653513970 ) ) ;
#78379 = ORIENTED_EDGE ( 'NONE', *, *, #44343, .T. ) ;
#78380 = VERTEX_POINT ( 'NONE', #35232 ) ;
#78381 = AXIS2_PLACEMENT_3D ( 'NONE', #38142, #2745, #70895 ) ;
#78382 = ADVANCED_FACE ( 'NONE', ( #41146 ), #17887, .T. ) ;
#78383 = CARTESIAN_POINT ( 'NONE',  ( 117.3348906646497909, -34.51323323996641079, 183.9956252759109532 ) ) ;
#78384 = EDGE_LOOP ( 'NONE', ( #44043, #3858, #1569, #3022 ) ) ;
#78385 = CARTESIAN_POINT ( 'NONE',  ( 101.9719236373881444, -46.53885842731235556, 167.1832443235299763 ) ) ;
#78386 = CARTESIAN_POINT ( 'NONE',  ( 34.92499999999999716, 66.67499999999999716, 295.2750000000000341 ) ) ;
#78387 = EDGE_CURVE ( 'NONE', #82724, #36938, #23745, .T. ) ;
#78388 = DIRECTION ( 'NONE',  ( 1.000000000000000000, 4.299999999999999979E-14, 9.351236661543306751E-17 ) ) ;
#78389 = CARTESIAN_POINT ( 'NONE',  ( 172.5667039024480687, -36.32844715993499563, 129.9678068554150059 ) ) ;
#78392 = CARTESIAN_POINT ( 'NONE',  ( 109.9831304889622743, -26.74336511273928707, 255.8499109901966051 ) ) ;
#78391 = CARTESIAN_POINT ( 'NONE',  ( 98.46045456725896372, -41.84421156295625366, 56.75289356703274990 ) ) ;
#78390 = CARTESIAN_POINT ( 'NONE',  ( 183.5150000000000148, 21.46300000000000097, 41.63456447661474868 ) ) ;
#78393 = CARTESIAN_POINT ( 'NONE',  ( 51.06648329127400388, 19.62155284005901024, 333.4006252759110112 ) ) ;
#78394 = CARTESIAN_POINT ( 'NONE',  ( 131.3179999999999836, 53.97500000000000142, 30.16249999999999787 ) ) ;
#78395 = AXIS2_PLACEMENT_3D ( 'NONE', #77928, #64297, #43377 ) ;
#78396 = CARTESIAN_POINT ( 'NONE',  ( 25.56670390244797275, -48.82844715994099971, 290.4678068554150627 ) ) ;
#78397 = CARTESIAN_POINT ( 'NONE',  ( -446.0240000000000009, 53.97500000000000142, 50.79999999999999716 ) ) ;
#78398 = DIRECTION ( 'NONE',  ( -0.9999999853157766072, -0.0001713722456127401463, 9.999999853157767620E-16 ) ) ;
#78399 = DIRECTION ( 'NONE',  ( 0.7071067811865614505, -0.7071067811865336949, 0.000000000000000000 ) ) ;
#78401 = ORIENTED_EDGE ( 'NONE', *, *, #83461, .T. ) ;
#78400 = CARTESIAN_POINT ( 'NONE',  ( 98.90717908043868078, -38.42765120644578047, 195.5838068554173788 ) ) ;
#78402 = DIRECTION ( 'NONE',  ( 0.000000000000000000, 0.000000000000000000, -1.000000000000000000 ) ) ;
#78403 = CARTESIAN_POINT ( 'NONE',  ( 112.7922847239315161, -45.46795744031502551, 178.0384824187679556 ) ) ;
#78404 = CARTESIAN_POINT ( 'NONE',  ( 96.92116189526866776, -32.34237133930066221, 57.01372051400599616 ) ) ;
#78405 = CARTESIAN_POINT ( 'NONE',  ( 99.97865438147567829, -27.17048309217152990, 181.5841967044829630 ) ) ;
#78406 = PLANE ( 'NONE',  #57583 ) ;
#78407 = LINE ( 'NONE', #86550, #61965 ) ;
#78408 = CIRCLE ( 'NONE', #65280, 3.700000000000001954 ) ;
#78410 = DIRECTION ( 'NONE',  ( 0.000000000000000000, 0.000000000000000000, -1.000000000000000000 ) ) ;
#78409 = CARTESIAN_POINT ( 'NONE',  ( -7.205548786489490269E-13, 117.4749999999999943, 111.1250000000000000 ) ) ;
#78411 = PLANE ( 'NONE',  #85841 ) ;
#78412 = DIRECTION ( 'NONE',  ( 0.000000000000000000, 0.000000000000000000, 1.000000000000000000 ) ) ;
#78413 = VERTEX_POINT ( 'NONE', #717 ) ;
#78414 = DIRECTION ( 'NONE',  ( 1.000000000000000078E-15, 1.000000000000000083E-30, -1.000000000000000000 ) ) ;
#78415 = EDGE_CURVE ( 'NONE', #79965, #33432, #68672, .T. ) ;
#78416 = ORIENTED_EDGE ( 'NONE', *, *, #22118, .F. ) ;
#78417 = VERTEX_POINT ( 'NONE', #70215 ) ;
#78418 = CARTESIAN_POINT ( 'NONE',  ( 108.6382307137633205, -45.64809506003439310, 122.1257531614099747 ) ) ;
#78419 = CIRCLE ( 'NONE', #56596, 2.029999999999997140 ) ;
#78421 = VERTEX_POINT ( 'NONE', #7985 ) ;
#78420 = DIRECTION ( 'NONE',  ( -0.7349399772593263602, 0.6687953793059858709, 0.1121426343770439427 ) ) ;
#78422 = CARTESIAN_POINT ( 'NONE',  ( 98.22092589535434115, -43.31882777834836418, 107.8480062282919647 ) ) ;
#78423 = CARTESIAN_POINT ( 'NONE',  ( 107.0664832912739968, -0.2185775633790978945, 333.4006252759120343 ) ) ;
#78425 = CARTESIAN_POINT ( 'NONE',  ( 20.03715912545824906, -46.82818131006190043, 249.9678068554150059 ) ) ;
#78424 = VECTOR ( 'NONE', #34583, 1000.000000000000000 ) ;
#78426 = EDGE_CURVE ( 'NONE', #40553, #6056, #9215, .T. ) ;
#78427 = CARTESIAN_POINT ( 'NONE',  ( 105.7995185030575982, -26.72403496415040891, 176.1772919413423040 ) ) ;
#78428 = CARTESIAN_POINT ( 'NONE',  ( 95.98894198207682393, -35.78073158428679790, 36.25848241876794731 ) ) ;
#78429 = ORIENTED_EDGE ( 'NONE', *, *, #22105, .T. ) ;
#78430 = EDGE_LOOP ( 'NONE', ( #14302, #78347, #87886, #62050 ) ) ;
#78432 = ORIENTED_EDGE ( 'NONE', *, *, #4790, .F. ) ;
#78431 = CIRCLE ( 'NONE', #31961, 2.030000000001807248 ) ;
#78433 = DIRECTION ( 'NONE',  ( 0.000000000000000000, 0.000000000000000000, 1.000000000000000000 ) ) ;
#78434 = PLANE ( 'NONE',  #49211 ) ;
#78435 = CARTESIAN_POINT ( 'NONE',  ( 0.000000000000000000, 101.6000000000000227, 0.000000000000000000 ) ) ;
#78436 = LINE ( 'NONE', #31141, #52759 ) ;
#78437 = CYLINDRICAL_SURFACE ( 'NONE', #62083, 1.000000000000000888 ) ;
#78438 = CARTESIAN_POINT ( 'NONE',  ( 97.60783471073349915, -39.98226673208375104, 52.58976314850144718 ) ) ;
#78439 = VECTOR ( 'NONE', #1829, 1000.000000000000114 ) ;
#78440 = CARTESIAN_POINT ( 'NONE',  ( 31.75000000000000000, 17.78000000000000114, -3.174999999999999822 ) ) ;
#78441 = CARTESIAN_POINT ( 'NONE',  ( -10.77377455544796625, 89.27589758714826473, 130.1107393577912035 ) ) ;
#78442 = CARTESIAN_POINT ( 'NONE',  ( 118.7081646409642133, -34.65111545711807395, 48.96705384733895983 ) ) ;
#78443 = EDGE_CURVE ( 'NONE', #81124, #14889, #42932, .T. ) ;
#78444 = ORIENTED_EDGE ( 'NONE', *, *, #31412, .F. ) ;
#78445 = CARTESIAN_POINT ( 'NONE',  ( 99.09570968012857861, -30.55043098681969838, 270.8022918655054241 ) ) ;
#78446 = COLOUR_RGB ( '', 0.40784314, 0.44705882, 0.49803922) ;
#78447 = LINE ( 'NONE', #78886, #32210 ) ;
#78448 = CARTESIAN_POINT ( 'NONE',  ( 102.8475555715194361, -29.17288882023929730, 103.3118998934009767 ) ) ;
#78449 = DIRECTION ( 'NONE',  ( 0.000000000000000000, 1.000000000000000000, 0.000000000000000000 ) ) ;
#78450 = VECTOR ( 'NONE', #63360, 1000.000000000000000 ) ;
#78451 = CARTESIAN_POINT ( 'NONE',  ( 12.70000000000000107, 82.54999999999999716, -129.9368274816650910 ) ) ;
#78452 = ORIENTED_EDGE ( 'NONE', *, *, #46305, .T. ) ;
#78453 = EDGE_LOOP ( 'NONE', ( #86833, #45040, #23455, #30802 ) ) ;
#78454 = ADVANCED_FACE ( 'NONE', ( #70669 ), #28061, .F. ) ;
#78455 = CARTESIAN_POINT ( 'NONE',  ( -50.03799999999999670, 101.5999999999999943, 206.3750000000000000 ) ) ;
#78456 = VECTOR ( 'NONE', #60034, 1000.000000000000000 ) ;
#78457 = ORIENTED_EDGE ( 'NONE', *, *, #30139, .F. ) ;
#78458 = VERTEX_POINT ( 'NONE', #29338 ) ;
#78459 = EDGE_CURVE ( 'NONE', #34522, #36080, #52920, .T. ) ;
#78460 = CARTESIAN_POINT ( 'NONE',  ( 97.69936372639945432, -35.99897019620807725, 187.7082499725639764 ) ) ;
#78461 = CARTESIAN_POINT ( 'NONE',  ( -76.20505178924278766, 120.6499999999999915, -76.20505178924469192 ) ) ;
#78462 = AXIS2_PLACEMENT_3D ( 'NONE', #64459, #8611, #23150 ) ;
#78463 = CARTESIAN_POINT ( 'NONE',  ( 117.8789659794968543, -39.13265831612300616, 99.64038718067195077 ) ) ;
#78464 = DIRECTION ( 'NONE',  ( 0.000000000000000000, -0.4999999999999998890, -0.8660254037844387076 ) ) ;
#78465 = CARTESIAN_POINT ( 'NONE',  ( 97.81168921572486852, -40.51740600946125426, 16.63579259794490284 ) ) ;
#78466 = ORIENTED_EDGE ( 'NONE', *, *, #22766, .T. ) ;
#78467 = ORIENTED_EDGE ( 'NONE', *, *, #33692, .F. ) ;
#78468 = VERTEX_POINT ( 'NONE', #71572 ) ;
#78469 = CARTESIAN_POINT ( 'NONE',  ( 108.0840670587429599, -45.32394831497818899, 160.5004713219719861 ) ) ;
#78470 = CARTESIAN_POINT ( 'NONE',  ( 99.27722696178533113, -43.74484797918319856, 56.90991099019593236 ) ) ;
#78471 = VERTEX_POINT ( 'NONE', #78396 ) ;
#78472 = CARTESIAN_POINT ( 'NONE',  ( 107.6057229598026339, -48.54288983744056907, 42.61276813305398292 ) ) ;
#78473 = CARTESIAN_POINT ( 'NONE',  ( 103.0413726597163446, -26.41035368485499646, 166.3603871806729444 ) ) ;
#78474 = CARTESIAN_POINT ( 'NONE',  ( 68.06670390244701707, -86.77844715994098124, 45.21780685541799727 ) ) ;
#78475 = CARTESIAN_POINT ( 'NONE',  ( -109.7874373783072457, 48.32589523802096210, 70.65122087376927595 ) ) ;
#78476 = CARTESIAN_POINT ( 'NONE',  ( 99.68461964852595258, -45.99997598619422234, 118.0413395616259606 ) ) ;
#78477 = AXIS2_PLACEMENT_3D ( 'NONE', #73823, #60173, #87907 ) ;
#78478 = PLANE ( 'NONE',  #37885 ) ;
#78479 = VERTEX_POINT ( 'NONE', #16596 ) ;
#78480 = CYLINDRICAL_SURFACE ( 'NONE', #24971, 3.700000000000001954 ) ;
#78481 = VECTOR ( 'NONE', #64427, 1000.000000000000000 ) ;
#78482 = ORIENTED_EDGE ( 'NONE', *, *, #62799, .F. ) ;
#78483 = CARTESIAN_POINT ( 'NONE',  ( 115.7836371542223901, -41.80142107029080734, 134.4074412807795795 ) ) ;
#78484 = DIRECTION ( 'NONE',  ( 0.000000000000000000, 0.000000000000000000, -1.000000000000000000 ) ) ;
#78485 = ORIENTED_EDGE ( 'NONE', *, *, #53180, .F. ) ;
#78486 = AXIS2_PLACEMENT_3D ( 'NONE', #29445, #22643, #50314 ) ;
#78487 = DIRECTION ( 'NONE',  ( 0.000000000000000000, 0.000000000000000000, -1.000000000000000000 ) ) ;
#78488 = LINE ( 'NONE', #43474, #84186 ) ;
#78489 = CARTESIAN_POINT ( 'NONE',  ( 113.5062182464826748, -28.53085922249196216, 79.54705384733995288 ) ) ;
#78490 = DIRECTION ( 'NONE',  ( 0.000000000000000000, 0.000000000000000000, 1.000000000000000000 ) ) ;
#78491 = B_SPLINE_CURVE_WITH_KNOTS ( 'NONE', 3,
 ( #46311, #67676, #74040, #81769, #11822, #67219, #5002, #83554, #28112, #14054, #47661, #69021, #41736, #34935, #42190, #82670, #14513, #422, #19979, #6786, #872, #20869, #7687, #75394, #48991, #54461, #14962, #69922, #62648, #28569, #13165, #13606, #34030, #89469, #40849, #34485, #62196, #68579, #48099, #61735, #1330, #20429, #6342, #55798, #89930, #27228, #27681, #75832, #63089, #35377 ),
 .UNSPECIFIED., .F., .F.,
 ( 4, 2, 1, 1, 1, 1, 1, 2, 2, 2, 2, 2, 2, 2, 1, 1, 1, 1, 1, 1, 1, 2, 2, 2, 2, 2, 2, 2, 2, 2, 4 ),
 ( 0.5000148422006782667, 0.5002589755784957459, 0.5005031089563133362, 0.5009913757119484057, 0.5019679092232189888, 0.5039209762457607100, 0.5078271102908441526, 0.5156393783810113707, 0.5312639145613456959, 0.5625129869220144574, 0.6250111316433523134, 0.6875092763646900584, 0.7500074210860279145, 0.7500684544304828671, 0.7501294877749378198, 0.7502515544638449496, 0.7504956878416844113, 0.7509839545973868713, 0.7519604881087729176, 0.7539135551315454542, 0.7578196891770798693, 0.7656319572681415941, 0.7812564934502654879, 0.8125055658145132753, 0.8437546381787610628, 0.8750037105430088502, 0.9062527829072566377, 0.9375018552715044251, 0.9687509276357521015, 0.9843754638178759953, 1.000000000000000000 ),
 .UNSPECIFIED. ) ;
#78492 = ADVANCED_FACE ( 'NONE', ( #23430 ), #17043, .F. ) ;
#78493 = DIRECTION ( 'NONE',  ( 1.821299053822143307E-16, 0.000000000000000000, -1.000000000000000000 ) ) ;
#78494 = DIRECTION ( 'NONE',  ( -1.000000000000000000, 1.122464679914735423E-15, 0.000000000000000000 ) ) ;
#78495 = CARTESIAN_POINT ( 'NONE',  ( 106.6352542858682284, -26.36832623700835398, 40.09753003781596448 ) ) ;
#78497 = CARTESIAN_POINT ( 'NONE',  ( 96.62907006607247240, -36.88702529232762828, 132.3384824187679669 ) ) ;
#78496 = CARTESIAN_POINT ( 'NONE',  ( 41.56648329127499153, -36.32844715994070839, 78.92562527591199739 ) ) ;
#78498 = DIRECTION ( 'NONE',  ( -1.000000000000000000, 0.000000000000000000, -7.723290606088049820E-15 ) ) ;
#78499 = CARTESIAN_POINT ( 'NONE',  ( 164.9190312289447888, -35.91149509760580116, 237.4678068554150059 ) ) ;
#78500 = ORIENTED_EDGE ( 'NONE', *, *, #23594, .F. ) ;
#78501 = VECTOR ( 'NONE', #65705, 1000.000000000000000 ) ;
#78502 = DIRECTION ( 'NONE',  ( -4.299999999999999979E-14, 1.000000000000000000, -4.400000000000000367E-29 ) ) ;
#78503 = DIRECTION ( 'NONE',  ( 1.000000000000000000, 0.000000000000000000, 0.000000000000000000 ) ) ;
#78504 = VERTEX_POINT ( 'NONE', #66060 ) ;
#78505 = AXIS2_PLACEMENT_3D ( 'NONE', #64512, #13332, #21843 ) ;
#78506 = FACE_OUTER_BOUND ( 'NONE', #4595, .T. ) ;
#78508 = EDGE_LOOP ( 'NONE', ( #88737, #27161, #29908 ) ) ;
#78507 = CARTESIAN_POINT ( 'NONE',  ( 117.8217860357262481, -31.63511105064214490, 214.1784824187679419 ) ) ;
#78509 = FACE_OUTER_BOUND ( 'NONE', #81787, .T. ) ;
#78510 = CARTESIAN_POINT ( 'NONE',  ( 106.5662934289835988, -47.19983425457502335, 243.5384824187679556 ) ) ;
#78511 = CARTESIAN_POINT ( 'NONE',  ( 97.18453276023305420, -31.67528530451021851, 91.96229194257693962 ) ) ;
#78512 = DIRECTION ( 'NONE',  ( -1.000000000000000000, 0.000000000000000000, 0.000000000000000000 ) ) ;
#78513 = DIRECTION ( 'NONE',  ( -0.9254794337955620787, -0.3787978585227822492, 0.000000000000000000 ) ) ;
#78514 = CARTESIAN_POINT ( 'NONE',  ( 115.0372575094445295, -42.90846256270808823, 78.30229194297042739 ) ) ;
#78515 = EDGE_LOOP ( 'NONE', ( #26157, #32578, #59924, #24241 ) ) ;
#78516 = EDGE_CURVE ( 'NONE', #28761, #89263, #78835, .T. ) ;
#78517 = EDGE_LOOP ( 'NONE', ( #2262, #41608 ) ) ;
#78518 = ORIENTED_EDGE ( 'NONE', *, *, #63926, .T. ) ;
#78519 = EDGE_CURVE ( 'NONE', #60004, #67149, #85212, .T. ) ;
#78520 = AXIS2_PLACEMENT_3D ( 'NONE', #64541, #85006, #22773 ) ;
#78521 = ORIENTED_EDGE ( 'NONE', *, *, #54565, .T. ) ;
#78522 = CARTESIAN_POINT ( 'NONE',  ( 129.9368274816649489, 82.54999999999999716, 12.70000000000136176 ) ) ;
#78523 = CARTESIAN_POINT ( 'NONE',  ( 111.8640475646460857, -46.02486053542493494, 268.9556252759110180 ) ) ;
#78524 = CARTESIAN_POINT ( 'NONE',  ( 194.0371591254575492, -24.42818131005417115, 129.9678068554150343 ) ) ;
#78525 = CARTESIAN_POINT ( 'NONE',  ( -458.3598257906459708, 60.32499999999999574, 3.174999999999999822 ) ) ;
#78526 = EDGE_CURVE ( 'NONE', #35491, #39283, #37035, .T. ) ;
#78527 = EDGE_CURVE ( 'NONE', #6249, #82562, #58794, .T. ) ;
#78529 = FACE_OUTER_BOUND ( 'NONE', #51116, .T. ) ;
#78528 = PLANE ( 'NONE',  #350 ) ;
#78530 = DIRECTION ( 'NONE',  ( 0.000000000000000000, 0.000000000000000000, -1.000000000000000000 ) ) ;
#78531 = AXIS2_PLACEMENT_3D ( 'NONE', #66916, #6479, #81021 ) ;
#78532 = CARTESIAN_POINT ( 'NONE',  ( 111.9487353400944158, -44.35678517904902662, 217.4400388756959615 ) ) ;
#78533 = ORIENTED_EDGE ( 'NONE', *, *, #49361, .T. ) ;
#78534 = EDGE_CURVE ( 'NONE', #9292, #87042, #58535, .T. ) ;
#78535 = EDGE_LOOP ( 'NONE', ( #82545, #12098 ) ) ;
#78536 = ORIENTED_EDGE ( 'NONE', *, *, #48644, .T. ) ;
#78537 = AXIS2_PLACEMENT_3D ( 'NONE', #5502, #73176, #10516 ) ;
#78538 = DIRECTION ( 'NONE',  ( -4.237773401492740281E-14, 1.000000000000000000, 0.000000000000000000 ) ) ;
#78540 = ADVANCED_FACE ( 'NONE', ( #23862 ), #51970, .T. ) ;
#78539 = CARTESIAN_POINT ( 'NONE',  ( 109.6427193709274519, -46.48016071713966113, 182.7814590059388138 ) ) ;
#78541 = CARTESIAN_POINT ( 'NONE',  ( 98.14754276252335785, -43.36755551587071977, 257.8356252759109566 ) ) ;
#78542 = CARTESIAN_POINT ( 'NONE',  ( -19.89663890320305839, 44.45000000000000284, 32.49205688096009936 ) ) ;
#78543 = CARTESIAN_POINT ( 'NONE',  ( 97.25364341294459791, -36.87759583893578963, 132.3384824187679669 ) ) ;
#78544 = ADVANCED_FACE ( 'NONE', ( #86539 ), #24304, .F. ) ;
#78545 = DIRECTION ( 'NONE',  ( -0.9254794337955620787, -0.3787978585227822492, 0.000000000000000000 ) ) ;
#78547 = ORIENTED_EDGE ( 'NONE', *, *, #62008, .F. ) ;
#78546 = CIRCLE ( 'NONE', #5980, 121.3994834559399862 ) ;
#78548 = DIRECTION ( 'NONE',  ( 0.000000000000000000, -1.000000000000000000, 0.000000000000000000 ) ) ;
#78549 = CYLINDRICAL_SURFACE ( 'NONE', #7100, 11.57110091390434903 ) ;
#78550 = VERTEX_POINT ( 'NONE', #17483 ) ;
#78551 = CARTESIAN_POINT ( 'NONE',  ( -74.15067561874160162, 127.0000000000000000, -68.53801554307528932 ) ) ;
#78552 = CARTESIAN_POINT ( 'NONE',  ( 97.82153671710952381, -35.93768077729445309, 34.07666179816293095 ) ) ;
#78553 = VECTOR ( 'NONE', #64311, 1000.000000000000000 ) ;
#78554 = CARTESIAN_POINT ( 'NONE',  ( 123.6837132603318423, -17.59493780205705704, 239.5838068554170377 ) ) ;
#78555 = LINE ( 'NONE', #79442, #4109 ) ;
#78556 = AXIS2_PLACEMENT_3D ( 'NONE', #45817, #73546, #32204 ) ;
#78557 = CARTESIAN_POINT ( 'NONE',  ( 115.7830320273964304, -41.80243732865377382, 194.4064425540411776 ) ) ;
#78558 = VERTEX_POINT ( 'NONE', #45164 ) ;
#78559 = DIRECTION ( 'NONE',  ( -0.7071067811865475727, 0.7071067811865475727, 0.000000000000000000 ) ) ;
#78560 = EDGE_CURVE ( 'NONE', #89089, #62710, #72888, .T. ) ;
#78561 = DIRECTION ( 'NONE',  ( 1.000000000000000078E-15, -1.000000000000000083E-30, -1.000000000000000000 ) ) ;
#78562 = ORIENTED_EDGE ( 'NONE', *, *, #25147, .T. ) ;
#78563 = CARTESIAN_POINT ( 'NONE',  ( 113.4596546395850680, -46.70781606211470205, 68.02991099019695298 ) ) ;
#78564 = ORIENTED_EDGE ( 'NONE', *, *, #58899, .F. ) ;
#78565 = EDGE_CURVE ( 'NONE', #67868, #53581, #84759, .T. ) ;
#78567 = VECTOR ( 'NONE', #79281, 1000.000000000000000 ) ;
#78566 = CARTESIAN_POINT ( 'NONE',  ( 116.0925701722734686, -37.46594287791281630, 38.19622935188693447 ) ) ;
#78568 = ADVANCED_FACE ( 'NONE', ( #15709 ), #43384, .F. ) ;
#78569 = DIRECTION ( 'NONE',  ( 1.000000000000000000, 0.000000000000000000, -3.491483361109380094E-15 ) ) ;
#78570 = CARTESIAN_POINT ( 'NONE',  ( 114.8570798905637673, -32.50631050113013742, 65.65301187732598009 ) ) ;
#78571 = DIRECTION ( 'NONE',  ( 0.000000000000000000, 1.000000000000000000, 0.000000000000000000 ) ) ;
#78572 = CARTESIAN_POINT ( 'NONE',  ( 6.812220284937080487E-16, 67.86880000000000734, 271.1195999999999913 ) ) ;
#78573 = EDGE_CURVE ( 'NONE', #23208, #43944, #32427, .T. ) ;
#78574 = DIRECTION ( 'NONE',  ( 0.000000000000000000, -1.000000000000000000, -0.000000000000000000 ) ) ;
#78575 = CARTESIAN_POINT ( 'NONE',  ( 110.9086127847465377, -26.95314644129561543, 265.7784824187680783 ) ) ;
#78576 = FACE_OUTER_BOUND ( 'NONE', #82812, .T. ) ;
#78577 = ORIENTED_EDGE ( 'NONE', *, *, #971, .T. ) ;
#78578 = DIRECTION ( 'NONE',  ( 0.000000000000000000, 0.000000000000000000, 1.000000000000000000 ) ) ;
#78579 = ORIENTED_EDGE ( 'NONE', *, *, #2118, .T. ) ;
#78580 = CARTESIAN_POINT ( 'NONE',  ( 102.8960693947464051, -27.08911147246314499, 151.4013395616249511 ) ) ;
#78581 = LINE ( 'NONE', #15891, #54017 ) ;
#78582 = ORIENTED_EDGE ( 'NONE', *, *, #29520, .T. ) ;
#78583 = ORIENTED_EDGE ( 'NONE', *, *, #1527, .F. ) ;
#78584 = ORIENTED_EDGE ( 'NONE', *, *, #8262, .F. ) ;
#78585 = VECTOR ( 'NONE', #10455, 1000.000000000000000 ) ;
#78586 = PLANE ( 'NONE',  #56559 ) ;
#78587 = PLANE ( 'NONE',  #15925 ) ;
#78588 = CARTESIAN_POINT ( 'NONE',  ( 118.0655259830059265, -38.35211242607485360, 223.7099109901979546 ) ) ;
#78589 = CARTESIAN_POINT ( 'NONE',  ( 94.86917197795301604, -31.06128196069623471, 9.425625275910958223 ) ) ;
#78590 = CARTESIAN_POINT ( 'NONE',  ( 107.0664832912739968, 0.2215528400590083269, 333.4006252759110112 ) ) ;
#78591 = DIRECTION ( 'NONE',  ( -1.000000000000000000, 0.000000000000000000, 0.000000000000000000 ) ) ;
#78592 = CARTESIAN_POINT ( 'NONE',  ( 116.1583077856502086, -43.02023234939740348, 9.356577656862985037 ) ) ;
#78593 = CARTESIAN_POINT ( 'NONE',  ( 199.3900000000000148, 52.73749999999999716, -44.45000000000000284 ) ) ;
#78594 = VERTEX_POINT ( 'NONE', #11567 ) ;
#78595 = CARTESIAN_POINT ( 'NONE',  ( 105.9988973700097574, -26.77423969884217669, 171.1614530458196271 ) ) ;
#78596 = CARTESIAN_POINT ( 'NONE',  ( 77.06670390244703128, -118.2784471599409812, 222.2178068554179902 ) ) ;
#78597 = AXIS2_PLACEMENT_3D ( 'NONE', #35912, #22757, #9560 ) ;
#78598 = ORIENTED_EDGE ( 'NONE', *, *, #1624, .F. ) ;
#78599 = AXIS2_PLACEMENT_3D ( 'NONE', #33085, #74427, #66707 ) ;
#78600 = CARTESIAN_POINT ( 'NONE',  ( 82.72805595269750256, -19.42731094490102706, 2.974216770161542289 ) ) ;
#78601 = CARTESIAN_POINT ( 'NONE',  ( -7.661254700127833495, 66.45253841614081125, 317.6630000000000109 ) ) ;
#78602 = CARTESIAN_POINT ( 'NONE',  ( 117.3910620576583312, -35.19077923515891371, 218.9441967044829482 ) ) ;
#78603 = CARTESIAN_POINT ( 'NONE',  ( 70.99299999999999500, 82.54999999999999716, 358.0130000000000337 ) ) ;
#78604 = FACE_BOUND ( 'NONE', #7159, .T. ) ;
#78605 = DIRECTION ( 'NONE',  ( 0.000000000000000000, 0.000000000000000000, 1.000000000000000000 ) ) ;
#78606 = CARTESIAN_POINT ( 'NONE',  ( 109.5125757112413822, -28.00996883845181173, 219.2933722090289734 ) ) ;
#78608 = CARTESIAN_POINT ( 'NONE',  ( 99.99555918775628527, -44.36035129061379934, 42.98133956162492098 ) ) ;
#78607 = DIRECTION ( 'NONE',  ( 0.2588190451025236261, 0.000000000000000000, -0.9659258262890675351 ) ) ;
#78609 = DIRECTION ( 'NONE',  ( -8.252657816380299978E-16, -2.773339119917620066E-31, -1.000000000000000000 ) ) ;
#78610 = CARTESIAN_POINT ( 'NONE',  ( 109.2642598482130154, -47.00181652296804913, 107.7441967044829880 ) ) ;
#78611 = EDGE_LOOP ( 'NONE', ( #2937, #21387, #66730, #42316, #29738, #21745, #65771, #41165, #65878, #7222, #2216, #50071, #13414 ) ) ;
#78612 = CARTESIAN_POINT ( 'NONE',  ( 131.7606268095719031, -20.22815166919999896, 7.286367513304471188 ) ) ;
#78613 = VERTEX_POINT ( 'NONE', #4747 ) ;
#78614 = DIRECTION ( 'NONE',  ( 1.000000000000000078E-15, -1.000000000000000000, 0.000000000000000000 ) ) ;
#78615 = CARTESIAN_POINT ( 'NONE',  ( 116.3185006702053244, -32.93849971620830530, 275.1356252759109680 ) ) ;
#78616 = ORIENTED_EDGE ( 'NONE', *, *, #56331, .F. ) ;
#78617 = VECTOR ( 'NONE', #73487, 1000.000000000000000 ) ;
#78618 = DIRECTION ( 'NONE',  ( 0.000000000000000000, 0.000000000000000000, 1.000000000000000000 ) ) ;
#78619 = ORIENTED_EDGE ( 'NONE', *, *, #27446, .F. ) ;
#78620 = DIRECTION ( 'NONE',  ( 0.8660254037844382635, 0.5000000000000008882, -1.550000000000000022E-14 ) ) ;
#78621 = DIRECTION ( 'NONE',  ( 0.000000000000000000, 0.000000000000000000, -1.000000000000000000 ) ) ;
#78622 = AXIS2_PLACEMENT_3D ( 'NONE', #8337, #83300, #50095 ) ;
#78623 = CARTESIAN_POINT ( 'NONE',  ( 29.56670390244743629, -48.82844715994161078, 180.4678068554150911 ) ) ;
#78624 = EDGE_LOOP ( 'NONE', ( #39973, #17573, #44579, #5598 ) ) ;
#78625 = VECTOR ( 'NONE', #4189, 1000.000000000000000 ) ;
#78626 = CARTESIAN_POINT ( 'NONE',  ( 109.6894323871380976, -47.49121184687970754, 87.75467289495897205 ) ) ;
#78627 = EDGE_CURVE ( 'NONE', #64886, #66793, #71660, .T. ) ;
#78628 = CARTESIAN_POINT ( 'NONE',  ( 0.000000000000000000, 0.000000000000000000, 0.000000000000000000 ) ) ;
#78629 = DIRECTION ( 'NONE',  ( 0.000000000000000000, 1.000000000000000000, 0.000000000000000000 ) ) ;
#78630 = CYLINDRICAL_SURFACE ( 'NONE', #225, 2.750000000000002665 ) ;
#78631 = EDGE_CURVE ( 'NONE', #57079, #85514, #75126, .T. ) ;
#78632 = CARTESIAN_POINT ( 'NONE',  ( -7.669759969481850348, 72.54466164532334460, 118.1076662423914883 ) ) ;
#78633 = ORIENTED_EDGE ( 'NONE', *, *, #20083, .T. ) ;
#78634 = VECTOR ( 'NONE', #76234, 1000.000000000000000 ) ;
#78635 = EDGE_CURVE ( 'NONE', #83511, #397, #45596, .T. ) ;
#78636 = CARTESIAN_POINT ( 'NONE',  ( 100.5986936721446341, 85.85000629251469206, -83.21537498883944295 ) ) ;
#78637 = CARTESIAN_POINT ( 'NONE',  ( 85.58420390244802434, -43.72944715994107412, 207.5838068554169809 ) ) ;
#78638 = AXIS2_PLACEMENT_3D ( 'NONE', #66510, #31989, #72885 ) ;
#78639 = DIRECTION ( 'NONE',  ( 3.100000000000000258E-29, -3.100000000000000044E-14, -1.000000000000000000 ) ) ;
#78640 = EDGE_CURVE ( 'NONE', #49287, #88413, #59685, .T. ) ;
#78641 = EDGE_CURVE ( 'NONE', #2091, #70138, #54199, .T. ) ;
#78643 = LINE ( 'NONE', #46297, #29725 ) ;
#78642 = CARTESIAN_POINT ( 'NONE',  ( 142.0664832912739826, -9.729447159940995959, 14.67562527591100441 ) ) ;
#78644 = CARTESIAN_POINT ( 'NONE',  ( 194.0667039024479834, -40.32844715993407902, 300.4678068554149490 ) ) ;
#78645 = ADVANCED_FACE ( 'NONE', ( #4301 ), #88327, .F. ) ;
#78646 = EDGE_LOOP ( 'NONE', ( #76235, #62227, #58509, #8610 ) ) ;
#78647 =( BOUNDED_CURVE ( )  B_SPLINE_CURVE ( 3, ( #63108, #89485, #84020, #71290 ),
 .UNSPECIFIED., .F., .T. ) 
 B_SPLINE_CURVE_WITH_KNOTS ( ( 4, 4 ),
 ( 3.141592653599576401, 4.712388980396665872 ),
 .UNSPECIFIED. ) 
 CURVE ( )  GEOMETRIC_REPRESENTATION_ITEM ( )  RATIONAL_B_SPLINE_CURVE ( ( 1.000000000000000000, 0.8047378541238481287, 0.8047378541238481287, 1.000000000000000000 ) ) 
 REPRESENTATION_ITEM ( '' )  );
#78649 = EDGE_CURVE ( 'NONE', #8827, #58352, #74677, .T. ) ;
#78648 = CARTESIAN_POINT ( 'NONE',  ( 208.9149999999999920, 37.33800000000000097, 41.27499999999999858 ) ) ;
#78650 = CARTESIAN_POINT ( 'NONE',  ( 103.1049807579881588, -45.67203811392940338, 173.2441967044819648 ) ) ;
#78652 = ORIENTED_EDGE ( 'NONE', *, *, #55199, .F. ) ;
#78651 = CARTESIAN_POINT ( 'NONE',  ( 59.56670390244699576, -67.87844715994098976, 120.2178068554179902 ) ) ;
#78653 = CARTESIAN_POINT ( 'NONE',  ( 100.9534786964906345, -28.35269599622561643, 26.56610146638693948 ) ) ;
#78654 = DIRECTION ( 'NONE',  ( 0.000000000000000000, 0.000000000000000000, 1.000000000000000000 ) ) ;
#78655 = CARTESIAN_POINT ( 'NONE',  ( 97.81556188947165253, -40.52687520453045522, 51.63643775176898032 ) ) ;
#78656 = DIRECTION ( 'NONE',  ( 0.000000000000000000, 0.000000000000000000, -1.000000000000000000 ) ) ;
#78657 = EDGE_CURVE ( 'NONE', #30791, #84622, #25178, .T. ) ;
#78658 = LINE ( 'NONE', #2785, #57318 ) ;
#78659 = CARTESIAN_POINT ( 'NONE',  ( 101.0349934672010903, -27.38958028709080139, 220.5327681330539633 ) ) ;
#78660 = ORIENTED_EDGE ( 'NONE', *, *, #35756, .F. ) ;
#78661 = AXIS2_PLACEMENT_3D ( 'NONE', #31326, #86760, #69444 ) ;
#78662 = ORIENTED_EDGE ( 'NONE', *, *, #28715, .T. ) ;
#78663 = EDGE_CURVE ( 'NONE', #35463, #2140, #80171, .T. ) ;
#78664 = CARTESIAN_POINT ( 'NONE',  ( 98.29135092237498839, -35.49440443996801520, 177.6472975916109647 ) ) ;
#78665 = AXIS2_PLACEMENT_3D ( 'NONE', #47028, #67946, #21151 ) ;
#78666 = B_SPLINE_CURVE_WITH_KNOTS ( 'NONE', 3,
 ( #36581, #43813, #23410, #37462, #86515, #71553, #72433, #29761, #64284, #72868, #86072, #9315, #58775, #80148, #59227, #65608, #24284, #24721 ),
 .UNSPECIFIED., .F., .F.,
 ( 4, 2, 2, 2, 2, 2, 2, 2, 4 ),
 ( 0.000000000000000000, 0.06249238452393977850, 0.1249847690478795570, 0.1874771535718193216, 0.2499695380957591140, 0.3124619226196989064, 0.3749543071436386432, 0.4374466916675784356, 0.4999390761915182280 ),
 .UNSPECIFIED. ) ;
#78667 = CARTESIAN_POINT ( 'NONE',  ( 47.62500000000000000, 69.84999999999999432, 260.3500000000000227 ) ) ;
#78668 = CARTESIAN_POINT ( 'NONE',  ( 116.4309197881342612, -37.49355097060504249, 35.20539282970796791 ) ) ;
#78669 = CARTESIAN_POINT ( 'NONE',  ( 23.68747463269394160, 84.09014500043505791, 307.4123016622365299 ) ) ;
#78670 = DIRECTION ( 'NONE',  ( 1.000000000000000078E-15, -1.000000000000000083E-30, -1.000000000000000000 ) ) ;
#78671 = CARTESIAN_POINT ( 'NONE',  ( 61.56670390244639890, -23.42844715994043270, 129.9678068554150911 ) ) ;
#78672 = VERTEX_POINT ( 'NONE', #81962 ) ;
#78673 = LINE ( 'NONE', #15535, #33374 ) ;
#78674 = DIRECTION ( 'NONE',  ( 1.000000000000000000, 8.953411488912556626E-16, 0.000000000000000000 ) ) ;
#78675 = CARTESIAN_POINT ( 'NONE',  ( 97.57986484199619781, -43.79006170206860560, 261.8356252759109566 ) ) ;
#78676 = DIRECTION ( 'NONE',  ( 0.000000000000000000, 0.000000000000000000, 1.000000000000000000 ) ) ;
#78677 = EDGE_LOOP ( 'NONE', ( #9467, #38327, #70440, #7219 ) ) ;
#78678 = ORIENTED_EDGE ( 'NONE', *, *, #24695, .T. ) ;
#78679 = EDGE_CURVE ( 'NONE', #22201, #64265, #53753, .T. ) ;
#78680 = CARTESIAN_POINT ( 'NONE',  ( 97.81169409577289287, -40.51741657705139232, 81.63570706759205109 ) ) ;
#78681 = LINE ( 'NONE', #31828, #57787 ) ;
#78682 = DIRECTION ( 'NONE',  ( 0.000000000000000000, 0.000000000000000000, 1.000000000000000000 ) ) ;
#78684 = ADVANCED_FACE ( 'NONE', ( #17917 ), #73328, .F. ) ;
#78683 = CARTESIAN_POINT ( 'NONE',  ( 179.1667039024460166, -26.71338133339251542, 117.4678068554150627 ) ) ;
#78685 = AXIS2_PLACEMENT_3D ( 'NONE', #89351, #5328, #12140 ) ;
#78686 = CARTESIAN_POINT ( 'NONE',  ( 106.3024736416176950, -26.94527301088420046, 21.13848241876792144 ) ) ;
#78687 = CARTESIAN_POINT ( 'NONE',  ( 7.674859615925401002, 72.54855685995774195, 118.1073353992515393 ) ) ;
#78688 = ORIENTED_EDGE ( 'NONE', *, *, #73563, .T. ) ;
#78689 = AXIS2_PLACEMENT_3D ( 'NONE', #32517, #75221, #47033 ) ;
#78690 = CARTESIAN_POINT ( 'NONE',  ( 96.67145939589113368, -37.96898657530446997, 37.42133956162496844 ) ) ;
#78691 = CARTESIAN_POINT ( 'NONE',  ( 85.58420390244803855, -51.22944715994107412, 231.5838068554169524 ) ) ;
#78692 = CARTESIAN_POINT ( 'NONE',  ( 100.0239399080498544, -28.99471651683304785, 285.6641967044823787 ) ) ;
#78693 = EDGE_LOOP ( 'NONE', ( #6391, #21175, #47713, #24171 ) ) ;
#78694 = CARTESIAN_POINT ( 'NONE',  ( 97.81168895331838087, -40.51742574516882200, 287.6356252759109680 ) ) ;
#78695 = CARTESIAN_POINT ( 'NONE',  ( 97.86658600797379393, -40.64924548183623898, 17.64667790301706063 ) ) ;
#78696 = LINE ( 'NONE', #57769, #58152 ) ;
#78697 = CARTESIAN_POINT ( 'NONE',  ( 99.02147155855831784, -38.11057432192225747, 89.27951894101998676 ) ) ;
#78698 = CARTESIAN_POINT ( 'NONE',  ( 103.5350399278988078, -26.85989278392735002, 186.3499109901969746 ) ) ;
#78699 = DIRECTION ( 'NONE',  ( 0.000000000000000000, 1.000000000000000000, 0.000000000000000000 ) ) ;
#78700 = ORIENTED_EDGE ( 'NONE', *, *, #67919, .T. ) ;
#78701 = DIRECTION ( 'NONE',  ( 0.000000000000000000, 0.000000000000000000, 1.000000000000000000 ) ) ;
#78702 = ORIENTED_EDGE ( 'NONE', *, *, #4149, .F. ) ;
#78703 = EDGE_LOOP ( 'NONE', ( #16645, #13335, #39651, #25406 ) ) ;
#78704 = EDGE_CURVE ( 'NONE', #68783, #3990, #13613, .T. ) ;
#78705 = FACE_BOUND ( 'NONE', #57378, .T. ) ;
#78706 = ORIENTED_EDGE ( 'NONE', *, *, #66281, .T. ) ;
#78707 = VERTEX_POINT ( 'NONE', #39696 ) ;
#78708 = CARTESIAN_POINT ( 'NONE',  ( -33.98325472291460159, 17.78000000000000114, 3.175000000000234746 ) ) ;
#78709 = CARTESIAN_POINT ( 'NONE',  ( 115.1037186944613921, -30.74792710411506391, 40.33566342910106783 ) ) ;
#78710 = CARTESIAN_POINT ( 'NONE',  ( 99.62716111080935377, -40.92618603589043147, 136.1581341137909646 ) ) ;
#78711 = CARTESIAN_POINT ( 'NONE',  ( 116.2381414160656874, -41.80576965393662903, 263.4241967044824833 ) ) ;
#78712 = AXIS2_PLACEMENT_3D ( 'NONE', #20853, #35813, #407 ) ;
#78713 = DIRECTION ( 'NONE',  ( 0.000000000000000000, -1.000000000000000000, 0.000000000000000000 ) ) ;
#78714 = ORIENTED_EDGE ( 'NONE', *, *, #21605, .F. ) ;
#78715 = CARTESIAN_POINT ( 'NONE',  ( 105.9338276561856560, -26.78157160042634644, 136.1666567892166881 ) ) ;
#78716 = ORIENTED_EDGE ( 'NONE', *, *, #14198, .F. ) ;
#78717 = CARTESIAN_POINT ( 'NONE',  ( 83.06670390244796920, -58.35344715994099829, 204.3338068554149913 ) ) ;
#78718 = DIRECTION ( 'NONE',  ( -0.000000000000000000, 1.000000000000000000, 0.000000000000000000 ) ) ;
#78719 = PLANE ( 'NONE',  #64989 ) ;
#78720 = EDGE_CURVE ( 'NONE', #75399, #60225, #67401, .T. ) ;
#78721 = CARTESIAN_POINT ( 'NONE',  ( 116.1780915764957740, -31.53023347274874055, 289.2384824187680579 ) ) ;
#78722 = EDGE_LOOP ( 'NONE', ( #36794, #27554 ) ) ;
#78723 = CARTESIAN_POINT ( 'NONE',  ( 97.01631923850186467, -33.95794342121210718, 251.1127681330538337 ) ) ;
#78724 = CARTESIAN_POINT ( 'NONE',  ( 97.44667640776515327, -32.59970075057101724, 12.00419670448293985 ) ) ;
#78725 = CARTESIAN_POINT ( 'NONE',  ( 115.7831076684064300, -41.80230951324009681, 119.4064586089808699 ) ) ;
#78726 = EDGE_CURVE ( 'NONE', #41047, #9127, #32886, .T. ) ;
#78728 = CARTESIAN_POINT ( 'NONE',  ( 69.36306272520799610, -138.6409717137631503, 247.3638974706309455 ) ) ;
#78727 = CARTESIAN_POINT ( 'NONE',  ( 165.6738106836030227, -28.98061976758901892, -5.074374724088000832 ) ) ;
#78729 = DIRECTION ( 'NONE',  ( 0.000000000000000000, 0.000000000000000000, -1.000000000000000000 ) ) ;
#78730 = ADVANCED_FACE ( 'NONE', ( #81520 ), #19273, .T. ) ;
#78731 = CARTESIAN_POINT ( 'NONE',  ( 0.000000000000000000, 198.8420489685532004, 0.000000000000000000 ) ) ;
#78732 = DIRECTION ( 'NONE',  ( 1.000000000000000000, 0.000000000000000000, 0.000000000000000000 ) ) ;
#78733 = EDGE_CURVE ( 'NONE', #88193, #9096, #69232, .T. ) ;
#78734 = DIRECTION ( 'NONE',  ( -4.237773401492740281E-14, 1.000000000000000000, 0.000000000000000000 ) ) ;
#78735 = FACE_BOUND ( 'NONE', #17105, .T. ) ;
#78736 = AXIS2_PLACEMENT_3D ( 'NONE', #85599, #23378, #78783 ) ;
#78737 = PLANE ( 'NONE',  #71899 ) ;
#78738 = CARTESIAN_POINT ( 'NONE',  ( 172.5664832912740110, -9.303447159940999356, 76.80862527591200717 ) ) ;
#78739 = CARTESIAN_POINT ( 'NONE',  ( 117.5411534933602837, -36.54545762053501079, 288.8413395616251478 ) ) ;
#78740 = CARTESIAN_POINT ( 'NONE',  ( 103.0497676667862947, -26.43187579209836002, 166.3603871806729444 ) ) ;
#78741 = CARTESIAN_POINT ( 'NONE',  ( 110.2908372810403819, -46.66631795110420455, 8.827053847339950465 ) ) ;
#78743 = CARTESIAN_POINT ( 'NONE',  ( 55.48342271751659638, 101.5999999999999943, 171.1197181046785261 ) ) ;
#78742 = DIRECTION ( 'NONE',  ( 1.000000000000000000, 4.299999999999999979E-14, 1.000000000000000078E-15 ) ) ;
#78744 = DIRECTION ( 'NONE',  ( 1.000000000000000000, 0.000000000000000000, 9.462128050782575008E-16 ) ) ;
#78745 = EDGE_CURVE ( 'NONE', #18287, #71147, #65860, .T. ) ;
#78746 = VECTOR ( 'NONE', #26067, 1000.000000000000000 ) ;
#78747 = ORIENTED_EDGE ( 'NONE', *, *, #55286, .T. ) ;
#78748 = DIRECTION ( 'NONE',  ( 1.000000000000000000, 0.000000000000000000, 0.000000000000000000 ) ) ;
#78749 = ORIENTED_EDGE ( 'NONE', *, *, #31010, .T. ) ;
#78750 = EDGE_CURVE ( 'NONE', #70047, #76240, #27413, .T. ) ;
#78751 = VECTOR ( 'NONE', #13353, 1000.000000000000000 ) ;
#78752 = CARTESIAN_POINT ( 'NONE',  ( 110.5640613610537883, -45.86347053068958246, 58.86705384733897972 ) ) ;
#78754 = ORIENTED_EDGE ( 'NONE', *, *, #63125, .T. ) ;
#78753 = CARTESIAN_POINT ( 'NONE',  ( 3.944304526105059924E-28, 95.25000000000000000, 130.5560000000000116 ) ) ;
#78755 = DIRECTION ( 'NONE',  ( -4.194175870806139918E-14, 1.000000000000000000, 0.000000000000000000 ) ) ;
#78756 = CARTESIAN_POINT ( 'NONE',  ( 113.0097079652340000, -45.31096836313445664, 199.0584824187679374 ) ) ;
#78757 = DIRECTION ( 'NONE',  ( 1.000000000000000078E-15, -1.000000000000000083E-30, -1.000000000000000000 ) ) ;
#78758 = CARTESIAN_POINT ( 'NONE',  ( 193.0371591254585155, -47.82818131005411999, 180.4678068554150343 ) ) ;
#78759 = CARTESIAN_POINT ( 'NONE',  ( 193.0371591254586576, -47.82818131005411999, 129.9678068554150343 ) ) ;
#78760 = CARTESIAN_POINT ( 'NONE',  ( 110.7536356736639220, -105.8297479413482733, -19.78219314458196010 ) ) ;
#78761 = ADVANCED_FACE ( 'NONE', ( #605, #28774 ), #61482, .F. ) ;
#78762 = DIRECTION ( 'NONE',  ( -0.000000000000000000, 1.000000000000000000, 0.000000000000000000 ) ) ;
#78763 = CARTESIAN_POINT ( 'NONE',  ( 115.1877794388830836, -42.61991029308448020, 98.32696653269469778 ) ) ;
#78764 = CARTESIAN_POINT ( 'NONE',  ( 116.6093774848466325, -38.87601340171674025, 148.6499109901969859 ) ) ;
#78765 = ORIENTED_EDGE ( 'NONE', *, *, #57996, .F. ) ;
#78766 = EDGE_LOOP ( 'NONE', ( #63092, #31371, #89400, #28825 ) ) ;
#78767 = CARTESIAN_POINT ( 'NONE',  ( 111.9416332874190090, -45.54441269975540507, 99.41015473446796591 ) ) ;
#78768 = PLANE ( 'NONE',  #57395 ) ;
#78770 = CARTESIAN_POINT ( 'NONE',  ( 31.90335556477799628, -33.89581943344391135, -5.074374724088000832 ) ) ;
#78769 = CARTESIAN_POINT ( 'NONE',  ( 107.4826147187165333, -46.50135945624614209, 233.6099109901959707 ) ) ;
#78771 = DIRECTION ( 'NONE',  ( -0.9419738712670564507, -0.000000000000000000, -0.3356862014592719157 ) ) ;
#78772 = LINE ( 'NONE', #36962, #46659 ) ;
#78773 = CARTESIAN_POINT ( 'NONE',  ( 37.03715912545425937, -48.62818131006122258, 313.9678068554150059 ) ) ;
#78774 = AXIS2_PLACEMENT_3D ( 'NONE', #17512, #64770, #3435 ) ;
#78775 = DIRECTION ( 'NONE',  ( 0.000000000000000000, 0.000000000000000000, 1.000000000000000000 ) ) ;
#78776 = CARTESIAN_POINT ( 'NONE',  ( 0.000000000000000000, 210.0000000000000000, 154.6557476874258441 ) ) ;
#78777 = CARTESIAN_POINT ( 'NONE',  ( 117.2886123466743271, -34.79635738071011986, 158.9756252759109714 ) ) ;
#78778 = ORIENTED_EDGE ( 'NONE', *, *, #12052, .F. ) ;
#78779 = ORIENTED_EDGE ( 'NONE', *, *, #25487, .T. ) ;
#78780 = CARTESIAN_POINT ( 'NONE',  ( 181.9790560690336463, -31.62489322947673642, 237.4678068554150059 ) ) ;
#78781 = DIRECTION ( 'NONE',  ( 0.000000000000000000, 1.000000000000000000, 0.000000000000000000 ) ) ;
#78782 = CARTESIAN_POINT ( 'NONE',  ( 19.56670390244796920, -67.87844715994100397, 20.91780685541479912 ) ) ;
#78784 = EDGE_CURVE ( 'NONE', #914, #34504, #13354, .T. ) ;
#78783 = DIRECTION ( 'NONE',  ( 0.0001713722455994998422, -0.9999999853157766072, 0.000000000000000000 ) ) ;
#78785 = CARTESIAN_POINT ( 'NONE',  ( 107.4137727038933150, -44.88475929872373626, 235.4280903695919562 ) ) ;
#78786 = AXIS2_PLACEMENT_3D ( 'NONE', #85943, #16887, #23713 ) ;
#78787 = FACE_OUTER_BOUND ( 'NONE', #53011, .T. ) ;
#78788 = CARTESIAN_POINT ( 'NONE',  ( 101.2005795642084820, -45.34792753215401007, 197.1013395616249966 ) ) ;
#78789 = DIRECTION ( 'NONE',  ( 3.999999999999999995E-14, -1.000000000000000000, 4.100000000000000342E-29 ) ) ;
#78790 = VERTEX_POINT ( 'NONE', #56455 ) ;
#78792 = EDGE_LOOP ( 'NONE', ( #63339, #45585, #76677, #68197 ) ) ;
#78791 = VERTEX_POINT ( 'NONE', #89214 ) ;
#78793 = CARTESIAN_POINT ( 'NONE',  ( 98.27464689803356634, -41.50197325149740379, 62.72272253483316007 ) ) ;
#78794 = ORIENTED_EDGE ( 'NONE', *, *, #7846, .F. ) ;
#78795 = LINE ( 'NONE', #85612, #20245 ) ;
#78796 = DIRECTION ( 'NONE',  ( 0.000000000000000000, 0.000000000000000000, -1.000000000000000000 ) ) ;
#78797 = CARTESIAN_POINT ( 'NONE',  ( 116.4516747918435300, -36.28819209217700603, 265.2834880678017839 ) ) ;
#78798 = PLANE ( 'NONE',  #47781 ) ;
#78799 = EDGE_LOOP ( 'NONE', ( #74938, #62890, #30185, #928 ) ) ;
#78800 = EDGE_CURVE ( 'NONE', #71390, #58180, #42372, .T. ) ;
#78801 = CARTESIAN_POINT ( 'NONE',  ( 103.7043515502224551, -44.10458127404638873, 9.635625275910941312 ) ) ;
#78802 = CARTESIAN_POINT ( 'NONE',  ( 103.1875000000000000, 117.4749999999999943, -7.143749999999640110 ) ) ;
#78803 = VERTEX_POINT ( 'NONE', #28303 ) ;
#78804 = ORIENTED_EDGE ( 'NONE', *, *, #34231, .F. ) ;
#78806 = ADVANCED_FACE ( 'NONE', ( #76469 ), #13795, .T. ) ;
#78805 = AXIS2_PLACEMENT_3D ( 'NONE', #54867, #89430, #67632 ) ;
#78807 = CARTESIAN_POINT ( 'NONE',  ( 110.8545879224105306, -45.98418990642309012, 112.8856352535895837 ) ) ;
#78808 = EDGE_LOOP ( 'NONE', ( #25653, #25150, #13517, #56621 ) ) ;
#78809 = ORIENTED_EDGE ( 'NONE', *, *, #75845, .F. ) ;
#78810 = AXIS2_PLACEMENT_3D ( 'NONE', #10092, #86395, #80037 ) ;
#78811 = VECTOR ( 'NONE', #46392, 1000.000000000000000 ) ;
#78812 = CARTESIAN_POINT ( 'NONE',  ( 99.21763626795888058, -33.35996782468227195, 15.42670554236297242 ) ) ;
#78813 = CARTESIAN_POINT ( 'NONE',  ( 111.4265353497823128, -47.77589283047310431, 172.8756252759109771 ) ) ;
#78814 = CARTESIAN_POINT ( 'NONE',  ( 113.9025887763448566, -28.07314977735658701, 124.5565776568629559 ) ) ;
#78815 = CARTESIAN_POINT ( 'NONE',  ( 34.33598329127472937, -36.32844715994134788, 313.9678068554150059 ) ) ;
#78816 = CARTESIAN_POINT ( 'NONE',  ( 96.51815522165868799, -31.32876289826797134, 241.9499109901969689 ) ) ;
#78817 = LINE ( 'NONE', #16577, #69020 ) ;
#78818 = CARTESIAN_POINT ( 'NONE',  ( 99.09513708517808084, -30.55119466390278049, 126.8023670118761714 ) ) ;
#78819 = DIRECTION ( 'NONE',  ( 0.000000000000000000, 0.000000000000000000, 1.000000000000000000 ) ) ;
#78820 = ORIENTED_EDGE ( 'NONE', *, *, #48847, .T. ) ;
#78821 = ORIENTED_EDGE ( 'NONE', *, *, #84282, .T. ) ;
#78822 = CARTESIAN_POINT ( 'NONE',  ( 101.3249093792229871, -46.22930045566884871, 202.1318157521019430 ) ) ;
#78823 = VERTEX_POINT ( 'NONE', #41042 ) ;
#78824 = CARTESIAN_POINT ( 'NONE',  ( 116.6609997163256764, -40.80771701747383418, 168.5070538473399608 ) ) ;
#78825 = CARTESIAN_POINT ( 'NONE',  ( 32.56670390244700997, -18.82844715994111340, -5.074374724088000832 ) ) ;
#78826 = VECTOR ( 'NONE', #3642, 1000.000000000000000 ) ;
#78827 = CARTESIAN_POINT ( 'NONE',  ( 135.3633572498488888, -34.30134337669387889, 7.962481652684965105 ) ) ;
#78828 = CARTESIAN_POINT ( 'NONE',  ( 143.5397427877413747, -139.6742706447616058, 247.2684776741174062 ) ) ;
#78831 = CARTESIAN_POINT ( 'NONE',  ( 115.9412561796927577, -30.17946786548973748, 255.3203871806729524 ) ) ;
#78830 = DIRECTION ( 'NONE',  ( -0.6537961156249219030, 0.7071067811865322517, 0.2693522585644778089 ) ) ;
#78829 = CARTESIAN_POINT ( 'NONE',  ( 116.3212776292299253, -32.94146857471393730, 145.1356252759109680 ) ) ;
#78832 = DIRECTION ( 'NONE',  ( 0.7071067811868035902, 0.7071067811862914443, 7.071067811868029270E-16 ) ) ;
#78833 = EDGE_CURVE ( 'NONE', #73407, #84780, #70359, .T. ) ;
#78834 = LINE ( 'NONE', #73327, #80170 ) ;
#78835 = LINE ( 'NONE', #9332, #74497 ) ;
#78836 = CIRCLE ( 'NONE', #49815, 0.5000000000000004441 ) ;
#78837 = EDGE_CURVE ( 'NONE', #81882, #71705, #49842, .T. ) ;
#78838 = DIRECTION ( 'NONE',  ( -1.000000000000000000, 0.000000000000000000, 0.000000000000000000 ) ) ;
#78839 = CARTESIAN_POINT ( 'NONE',  ( 104.4081006870482184, -46.45808914696898739, 258.3647919446885339 ) ) ;
#78840 = DIRECTION ( 'NONE',  ( 0.000000000000000000, 0.000000000000000000, -1.000000000000000000 ) ) ;
#78842 = ORIENTED_EDGE ( 'NONE', *, *, #40170, .T. ) ;
#78841 = CARTESIAN_POINT ( 'NONE',  ( 113.8796460939257287, -30.53604272315569546, 195.5838068554168103 ) ) ;
#78843 = ADVANCED_FACE ( 'NONE', ( #62828 ), #21061, .F. ) ;
#78844 = CARTESIAN_POINT ( 'NONE',  ( 188.5667039024479834, -48.82844715994099971, 175.9678068554150059 ) ) ;
#78845 = CARTESIAN_POINT ( 'NONE',  ( 104.4481554933880716, -26.61555950438322427, 200.2784824187679362 ) ) ;
#78846 = CARTESIAN_POINT ( 'NONE',  ( 107.8683515708180636, -26.33524229811608919, 66.01562527591097762 ) ) ;
#78847 = CARTESIAN_POINT ( 'NONE',  ( 97.38492667529318680, -42.15761073986299579, 177.7451490854349743 ) ) ;
#78848 = CARTESIAN_POINT ( 'NONE',  ( -68.53801554307499089, 120.6499999999999915, 74.15067561874188584 ) ) ;
#78849 = DIRECTION ( 'NONE',  ( 0.000000000000000000, 1.000000000000000000, -0.000000000000000000 ) ) ;
#78851 = CARTESIAN_POINT ( 'NONE',  ( 101.6336199742765984, -45.20051650499360107, 38.12198527528386194 ) ) ;
#78850 = PLANE ( 'NONE',  #13048 ) ;
#78852 = CARTESIAN_POINT ( 'NONE',  ( 46.03715912545427358, -48.62818131006086020, 300.4678068554150059 ) ) ;
#78853 = CARTESIAN_POINT ( 'NONE',  ( 71.25416588882602298, -72.55705569728901594, 396.9756252759102040 ) ) ;
#78854 = EDGE_LOOP ( 'NONE', ( #9247, #45523 ) ) ;
#78855 = AXIS2_PLACEMENT_3D ( 'NONE', #7903, #84233, #13385 ) ;
#78856 = DIRECTION ( 'NONE',  ( 0.000000000000000000, 0.000000000000000000, -1.000000000000000000 ) ) ;
#78857 = ADVANCED_FACE ( 'NONE', ( #33788 ), #20616, .F. ) ;
#78858 = ORIENTED_EDGE ( 'NONE', *, *, #10406, .T. ) ;
#78859 = EDGE_LOOP ( 'NONE', ( #26516, #12192, #34554, #31551 ) ) ;
#78860 = EDGE_CURVE ( 'NONE', #15500, #5714, #72347, .T. ) ;
#78861 = CARTESIAN_POINT ( 'NONE',  ( 113.2121186763659040, -42.70299450126940144, 97.63527697093398672 ) ) ;
#78863 = ORIENTED_EDGE ( 'NONE', *, *, #45260, .T. ) ;
#78862 = CARTESIAN_POINT ( 'NONE',  ( -4.867771054587870516, 94.30191638479371363, -130.4669033451686175 ) ) ;
#78864 = CARTESIAN_POINT ( 'NONE',  ( 113.8422018911646774, -44.62364141802220985, 104.1413395616249744 ) ) ;
#78865 = CARTESIAN_POINT ( 'NONE',  ( 57.56670390244744340, -48.82844715994040286, 173.2178068554150911 ) ) ;
#78866 = LINE ( 'NONE', #32018, #26854 ) ;
#78867 = DIRECTION ( 'NONE',  ( -1.000000000000000078E-15, 1.000000000000000000, 0.000000000000000000 ) ) ;
#78868 = B_SPLINE_CURVE_WITH_KNOTS ( 'NONE', 3,
 ( #51481, #43784, #66008, #64690, #71522, #9281, #79677, #31488, #37879, #85601, #3361, #24688, #80118, #31050, #66457, #4245, #50601, #85154 ),
 .UNSPECIFIED., .F., .F.,
 ( 4, 2, 2, 2, 2, 2, 2, 2, 4 ),
 ( 0.000000000000000000, 0.06250004591115866648, 0.1250000918223173330, 0.1875001377334760133, 0.2500001836446346659, 0.3125002295557933185, 0.3750002754669520266, 0.4375003213781106792, 0.5000003672892693318 ),
 .UNSPECIFIED. ) ;
#78869 = CARTESIAN_POINT ( 'NONE',  ( 100.4186822966649828, -43.90371905523902996, 46.98133956162492098 ) ) ;
#78870 = VERTEX_POINT ( 'NONE', #43273 ) ;
#78871 = VERTEX_POINT ( 'NONE', #30112 ) ;
#78872 = EDGE_LOOP ( 'NONE', ( #48797, #3149, #25215, #49712 ) ) ;
#78873 = AXIS2_PLACEMENT_3D ( 'NONE', #8444, #36141, #63856 ) ;
#78874 = LINE ( 'NONE', #40180, #63099 ) ;
#78875 = CARTESIAN_POINT ( 'NONE',  ( 89.60916260784479448, 223.9999999999999716, 134.1927865330827103 ) ) ;
#78877 = VECTOR ( 'NONE', #42685, 999.9999999999998863 ) ;
#78876 = DIRECTION ( 'NONE',  ( 0.000000000000000000, 0.000000000000000000, -1.000000000000000000 ) ) ;
#78878 = CARTESIAN_POINT ( 'NONE',  ( 177.0664832912740110, 12.92155284005802685, 349.2756252759111248 ) ) ;
#78879 = CARTESIAN_POINT ( 'NONE',  ( 34.33598329127499227, -36.32844715994100682, -5.074374724088000832 ) ) ;
#78880 = DIRECTION ( 'NONE',  ( -0.8660254037844380415, -0.5000000000000012212, 1.550000000000001284E-14 ) ) ;
#78881 = DIRECTION ( 'NONE',  ( -3.100000000000000258E-29, 3.100000000000000044E-14, 1.000000000000000000 ) ) ;
#78882 = CARTESIAN_POINT ( 'NONE',  ( -6.301391689584750821, 93.58422381887211827, 130.4043053684175106 ) ) ;
#78883 = CARTESIAN_POINT ( 'NONE',  ( 111.9186950350130303, -27.52701776748434170, 59.68991099019693536 ) ) ;
#78884 = ORIENTED_EDGE ( 'NONE', *, *, #67596, .T. ) ;
#78885 = LINE ( 'NONE', #66565, #28681 ) ;
#78887 = EDGE_CURVE ( 'NONE', #60920, #45127, #57809, .T. ) ;
#78886 = CARTESIAN_POINT ( 'NONE',  ( 77.06670390244703128, -118.2784471599409812, 230.7030882296565721 ) ) ;
#78888 = CARTESIAN_POINT ( 'NONE',  ( 115.5296723907996039, -38.53924143319417794, 106.4890427505429642 ) ) ;
#78889 = AXIS2_PLACEMENT_3D ( 'NONE', #19995, #6357, #61751 ) ;
#78890 = AXIS2_PLACEMENT_3D ( 'NONE', #21201, #84343, #22112 ) ;
#78891 = EDGE_CURVE ( 'NONE', #6718, #85945, #33912, .T. ) ;
#78892 = DIRECTION ( 'NONE',  ( -0.7071067811865773267, 0.7071067811865178188, -7.071067811865781017E-16 ) ) ;
#78893 = FACE_OUTER_BOUND ( 'NONE', #12312, .T. ) ;
#78894 = ORIENTED_EDGE ( 'NONE', *, *, #66208, .T. ) ;
#78895 = EDGE_LOOP ( 'NONE', ( #25902, #57422, #7052, #44792 ) ) ;
#78896 = CARTESIAN_POINT ( 'NONE',  ( 116.8169691553371763, -34.15232147661988193, 139.0309223820618740 ) ) ;
#78897 = AXIS2_PLACEMENT_3D ( 'NONE', #75727, #39842, #33038 ) ;
#78898 = ORIENTED_EDGE ( 'NONE', *, *, #66482, .F. ) ;
#78899 = ORIENTED_EDGE ( 'NONE', *, *, #43782, .T. ) ;
#78900 = CARTESIAN_POINT ( 'NONE',  ( 113.2524973562852608, -30.34232264463288686, 170.8958690201829711 ) ) ;
#78901 = CARTESIAN_POINT ( 'NONE',  ( 97.81670390244700286, -68.87844715994096134, 55.21780685541800437 ) ) ;
#78902 = CARTESIAN_POINT ( 'NONE',  ( 97.59729452806701033, -30.98317272244041121, 121.8803871806729546 ) ) ;
#78903 = DIRECTION ( 'NONE',  ( 0.000000000000000000, 0.000000000000000000, 1.000000000000000000 ) ) ;
#78904 = AXIS2_PLACEMENT_3D ( 'NONE', #68279, #6060, #54157 ) ;
#78905 = CARTESIAN_POINT ( 'NONE',  ( 57.14999999999999858, 69.84999999999999432, 297.6879999999999882 ) ) ;
#78906 = ORIENTED_EDGE ( 'NONE', *, *, #26281, .T. ) ;
#78907 = ADVANCED_FACE ( 'NONE', ( #36488 ), #58688, .F. ) ;
#78908 = ORIENTED_EDGE ( 'NONE', *, *, #79778, .T. ) ;
#78909 = ORIENTED_EDGE ( 'NONE', *, *, #79559, .F. ) ;
#78910 = CARTESIAN_POINT ( 'NONE',  ( 102.4736563324128440, -43.47745920372498318, 194.9195189410199589 ) ) ;
#78911 = CARTESIAN_POINT ( 'NONE',  ( 107.2325596213128875, -25.65389481303129315, 80.07657765686299456 ) ) ;
#78912 = ORIENTED_EDGE ( 'NONE', *, *, #87326, .F. ) ;
#78913 = CARTESIAN_POINT ( 'NONE',  ( 100.4929927897290014, -27.87207479535954135, 35.59657765686397113 ) ) ;
#78914 = CARTESIAN_POINT ( 'NONE',  ( 112.3219919889560288, -28.66302566169128596, 249.5838068554155882 ) ) ;
#78915 = LINE ( 'NONE', #29415, #88701 ) ;
#78916 = DIRECTION ( 'NONE',  ( -8.252657816380299978E-16, -2.773339119917620066E-31, -1.000000000000000000 ) ) ;
#78917 = CARTESIAN_POINT ( 'NONE',  ( 114.2399097434533246, -45.14383888093294672, 149.1508633711489722 ) ) ;
#78918 = CARTESIAN_POINT ( 'NONE',  ( 36.74138383868169910, -48.33240602328862678, 249.9678068554150343 ) ) ;
#78919 = EDGE_LOOP ( 'NONE', ( #5016, #69898, #4488, #4576 ) ) ;
#78920 = CARTESIAN_POINT ( 'NONE',  ( -446.0240000000000009, 3.174999999999999822, 101.5999999999999943 ) ) ;
#78921 = ORIENTED_EDGE ( 'NONE', *, *, #1494, .T. ) ;
#78922 = PLANE ( 'NONE',  #72348 ) ;
#78923 = ORIENTED_EDGE ( 'NONE', *, *, #51847, .T. ) ;
#78924 = EDGE_LOOP ( 'NONE', ( #40984, #32672, #22816, #56245 ) ) ;
#78925 = VECTOR ( 'NONE', #45493, 1000.000000000000000 ) ;
#78926 = LINE ( 'NONE', #45692, #80908 ) ;
#78927 = CYLINDRICAL_SURFACE ( 'NONE', #37753, 3.499999999999996003 ) ;
#78928 = CARTESIAN_POINT ( 'NONE',  ( 118.7327907441706571, -34.64671908090114272, 48.96705384733895983 ) ) ;
#78929 = DIRECTION ( 'NONE',  ( 0.000000000000000000, 0.000000000000000000, 1.000000000000000000 ) ) ;
#78930 = CYLINDRICAL_SURFACE ( 'NONE', #69557, 3.249999999999975131 ) ;
#78931 = CARTESIAN_POINT ( 'NONE',  ( 80.06648329127398256, -9.029447159941060619, 8.225625275910942946 ) ) ;
#78932 = CARTESIAN_POINT ( 'NONE',  ( 103.6990349130722251, -26.13358598113143216, 55.32133956162594046 ) ) ;
#78934 = CARTESIAN_POINT ( 'NONE',  ( 114.2383551682309815, -44.26553795382356071, 154.1813395616249807 ) ) ;
#78933 = CARTESIAN_POINT ( 'NONE',  ( 107.0664832912739968, -36.72944715994100306, 287.6356252759109680 ) ) ;
#78935 = DIRECTION ( 'NONE',  ( 0.000000000000000000, 0.000000000000000000, 1.000000000000000000 ) ) ;
#78936 = EDGE_CURVE ( 'NONE', #52592, #65495, #35384, .T. ) ;
#78937 = CARTESIAN_POINT ( 'NONE',  ( 25.56670390244805446, -42.82844715994167473, 290.7178068554150059 ) ) ;
#78938 = ORIENTED_EDGE ( 'NONE', *, *, #8900, .F. ) ;
#78939 = CARTESIAN_POINT ( 'NONE',  ( -103.1875000000000000, 127.0000000000000000, 5.041899999998910253 ) ) ;
#78940 = DIRECTION ( 'NONE',  ( 1.000000000000000000, 0.000000000000000000, 0.000000000000000000 ) ) ;
#78941 = EDGE_CURVE ( 'NONE', #27915, #79779, #64192, .T. ) ;
#78942 = CARTESIAN_POINT ( 'NONE',  ( 82.81648329127402519, -36.72944715994107412, -5.074374724089055100 ) ) ;
#78943 = DIRECTION ( 'NONE',  ( 0.000000000000000000, 0.000000000000000000, 1.000000000000000000 ) ) ;
#78945 = ORIENTED_EDGE ( 'NONE', *, *, #57384, .T. ) ;
#78944 = CARTESIAN_POINT ( 'NONE',  ( 101.3249093792229871, -46.22930045566884871, 202.1318157521019430 ) ) ;
#78946 = ADVANCED_FACE ( 'NONE', ( #44612 ), #29662, .F. ) ;
#78947 = CARTESIAN_POINT ( 'NONE',  ( 97.53194275716850825, -39.74926679241858096, 146.5705568277559223 ) ) ;
#78948 = CARTESIAN_POINT ( 'NONE',  ( 100.2339645716073164, -28.82666620644582522, 256.6441967044821695 ) ) ;
#78949 = CARTESIAN_POINT ( 'NONE',  ( 118.8919219083537797, -35.39899076563189340, 79.91562527591095488 ) ) ;
#78950 = LINE ( 'NONE', #85774, #65048 ) ;
#78951 = DIRECTION ( 'NONE',  ( 0.000000000000000000, 1.000000000000000000, 0.000000000000000000 ) ) ;
#78952 = CARTESIAN_POINT ( 'NONE',  ( 97.80969226196111777, -40.51824922604903634, 262.6357212258262166 ) ) ;
#78953 = ORIENTED_EDGE ( 'NONE', *, *, #28288, .F. ) ;
#78954 = VECTOR ( 'NONE', #46894, 1000.000000000000000 ) ;
#78955 = VECTOR ( 'NONE', #13983, 1000.000000000000000 ) ;
#78956 = VECTOR ( 'NONE', #87078, 1000.000000000000000 ) ;
#78957 = VERTEX_POINT ( 'NONE', #71904 ) ;
#78958 = ORIENTED_EDGE ( 'NONE', *, *, #24995, .F. ) ;
#78959 = EDGE_CURVE ( 'NONE', #42534, #9271, #85096, .T. ) ;
#78960 = B_SPLINE_CURVE_WITH_KNOTS ( 'NONE', 3,
 ( #72846, #23820, #32384, #30623, #79239, #58323, #10611, #16998, #66017, #24696, #52363, #80126, #45552, #73283, #73737, #11059, #4255, #59642, #25136, #52796, #39214, #33746, #81915, #81475, #75081 ),
 .UNSPECIFIED., .F., .F.,
 ( 4, 2, 2, 2, 2, 2, 2, 2, 2, 1, 2, 2, 4 ),
 ( 6.610103225985008611E-19, 0.002483982529268030041, 0.003725973793902044844, 0.004967965058536060081, 0.007451947587804091423, 0.008693938852438104492, 0.009935930117072118428, 0.01241991264634014977, 0.01366190391097416197, 0.01490389517560817417, 0.01614588644024218464, 0.01738787770487619858, 0.01987186023414422298 ),
 .UNSPECIFIED. ) ;
#78961 = VECTOR ( 'NONE', #60688, 1000.000000000000000 ) ;
#78962 = ORIENTED_EDGE ( 'NONE', *, *, #26812, .F. ) ;
#78963 = DIRECTION ( 'NONE',  ( -0.7071067811865475727, 0.000000000000000000, -0.7071067811865475727 ) ) ;
#78964 = CARTESIAN_POINT ( 'NONE',  ( 117.4913186190917855, -36.80221964929349809, 259.8213395616249386 ) ) ;
#78965 = LINE ( 'NONE', #9460, #64987 ) ;
#78966 = EDGE_CURVE ( 'NONE', #19262, #62172, #22865, .T. ) ;
#78967 = DIRECTION ( 'NONE',  ( -0.7071067811865473507, -0.7071067811865477948, 0.000000000000000000 ) ) ;
#78969 = CARTESIAN_POINT ( 'NONE',  ( 90.13186587200897293, 73.86197090048096925, 77.01855645442628884 ) ) ;
#78968 = CARTESIAN_POINT ( 'NONE',  ( 34.27258461953873336, -35.55794170701842916, 313.9678068554150059 ) ) ;
#78970 = DIRECTION ( 'NONE',  ( 0.000000000000000000, 0.000000000000000000, 1.000000000000000000 ) ) ;
#78971 = CARTESIAN_POINT ( 'NONE',  ( 98.15635076299318484, -32.87196533591951919, 210.4238483995049762 ) ) ;
#78972 = ORIENTED_EDGE ( 'NONE', *, *, #61291, .F. ) ;
#78973 = ORIENTED_EDGE ( 'NONE', *, *, #33000, .F. ) ;
#78974 = ORIENTED_EDGE ( 'NONE', *, *, #30381, .F. ) ;
#78975 = CARTESIAN_POINT ( 'NONE',  ( 160.7738106836348777, -48.62134037874901082, 249.9678068554149490 ) ) ;
#78976 = CARTESIAN_POINT ( 'NONE',  ( 111.2449163426335303, -45.81617768730462359, 182.9194528165492954 ) ) ;
#78977 = CARTESIAN_POINT ( 'NONE',  ( 115.9511604134431195, -42.07746527072326614, 274.3832443235294249 ) ) ;
#78978 = CYLINDRICAL_SURFACE ( 'NONE', #16840, 9.999999999999998224 ) ;
#78979 = CARTESIAN_POINT ( 'NONE',  ( 156.5667039024483529, -42.82844715993568485, 137.2178068554149775 ) ) ;
#78980 = CARTESIAN_POINT ( 'NONE',  ( 162.5667039024470171, -32.29483332968611364, 237.4678068554150059 ) ) ;
#78981 = ORIENTED_EDGE ( 'NONE', *, *, #54255, .T. ) ;
#78982 = CARTESIAN_POINT ( 'NONE',  ( 78.76417807488600431, -34.30680158339610841, 1.893168945966681838 ) ) ;
#78983 = EDGE_LOOP ( 'NONE', ( #49389, #84024, #12290, #85519, #38512 ) ) ;
#78984 = FACE_OUTER_BOUND ( 'NONE', #89387, .T. ) ;
#78985 = CARTESIAN_POINT ( 'NONE',  ( 109.0595394021483742, -27.66723669546327358, 27.72237608387795404 ) ) ;
#78986 = VECTOR ( 'NONE', #14140, 1000.000000000000000 ) ;
#78987 = DIRECTION ( 'NONE',  ( 5.512527431108029424E-15, -1.000000000000000000, 0.000000000000000000 ) ) ;
#78988 = AXIS2_PLACEMENT_3D ( 'NONE', #71343, #9553, #86302 ) ;
#78989 = EDGE_CURVE ( 'NONE', #30803, #17437, #35591, .T. ) ;
#78990 = DIRECTION ( 'NONE',  ( 0.000000000000000000, 0.000000000000000000, 1.000000000000000000 ) ) ;
#78991 = FACE_OUTER_BOUND ( 'NONE', #30531, .T. ) ;
#78992 = ORIENTED_EDGE ( 'NONE', *, *, #27227, .F. ) ;
#78993 = CYLINDRICAL_SURFACE ( 'NONE', #42113, 9.525000000000000355 ) ;
#78994 = DIRECTION ( 'NONE',  ( 0.000000000000000000, 1.000000000000000000, 0.000000000000000000 ) ) ;
#78995 = VERTEX_POINT ( 'NONE', #67757 ) ;
#78996 = CARTESIAN_POINT ( 'NONE',  ( 104.2140152791992875, -25.22710339543701963, 90.26991099019693365 ) ) ;
#78997 = ORIENTED_EDGE ( 'NONE', *, *, #37087, .T. ) ;
#78998 = CARTESIAN_POINT ( 'NONE',  ( 104.2253390597007581, -44.78450961640034222, 56.72956268521994616 ) ) ;
#78999 = DIRECTION ( 'NONE',  ( 0.9834602067019598826, 0.1811243270069988198, 0.000000000000000000 ) ) ;
#79000 = CARTESIAN_POINT ( 'NONE',  ( 98.26727195740441800, -38.00851302551287603, 62.87301187732596475 ) ) ;
#79001 = CARTESIAN_POINT ( 'NONE',  ( 101.9932406875673081, -45.44583697117432308, 13.15642348592802691 ) ) ;
#79002 = LINE ( 'NONE', #16770, #13995 ) ;
#79003 = CARTESIAN_POINT ( 'NONE',  ( 68.82702071641912767, -69.48851445456057263, 247.4865261645284136 ) ) ;
#79004 = CARTESIAN_POINT ( 'NONE',  ( 112.9754938005188478, -28.11429459860147873, 40.59848241876795782 ) ) ;
#79005 = DIRECTION ( 'NONE',  ( 0.7071067811865536790, 0.000000000000000000, -0.7071067811865413555 ) ) ;
#79006 = VERTEX_POINT ( 'NONE', #65955 ) ;
#79007 = CARTESIAN_POINT ( 'NONE',  ( 172.5664832912740110, -9.303447159940999356, 316.8086252759120498 ) ) ;
#79008 = CIRCLE ( 'NONE', #87745, 0.2999999999999943823 ) ;
#79009 = ORIENTED_EDGE ( 'NONE', *, *, #58033, .T. ) ;
#79010 = CARTESIAN_POINT ( 'NONE',  ( 114.5587124134895731, -28.54364023664675187, 150.4746728949579619 ) ) ;
#79011 = ADVANCED_FACE ( 'NONE', ( #19165 ), #45058, .F. ) ;
#79012 = CARTESIAN_POINT ( 'NONE',  ( 0.000000000000000000, 50.79999999999999716, 259.9944000000000415 ) ) ;
#79013 = AXIS2_PLACEMENT_3D ( 'NONE', #82316, #40050, #66867 ) ;
#79014 = CIRCLE ( 'NONE', #3588, 12.70000000000000107 ) ;
#79015 = ORIENTED_EDGE ( 'NONE', *, *, #51778, .T. ) ;
#79016 = ORIENTED_EDGE ( 'NONE', *, *, #55706, .F. ) ;
#79017 = VECTOR ( 'NONE', #12452, 1000.000000000000000 ) ;
#79018 = DIRECTION ( 'NONE',  ( 0.000000000000000000, 0.000000000000000000, -1.000000000000000000 ) ) ;
#79019 = VECTOR ( 'NONE', #35041, 1000.000000000000000 ) ;
#79020 = DIRECTION ( 'NONE',  ( -0.0001713722455994998422, 0.9999999853157766072, 0.000000000000000000 ) ) ;
#79021 = CARTESIAN_POINT ( 'NONE',  ( 103.9298229712113653, -26.84510867568817716, 205.3089586092449679 ) ) ;
#79022 = LINE ( 'NONE', #64932, #73349 ) ;
#79023 = CARTESIAN_POINT ( 'NONE',  ( 51.56670390244671154, -32.29483332968566600, 193.9678068554150911 ) ) ;
#79024 = CARTESIAN_POINT ( 'NONE',  ( 36.23715912545422668, -47.82818131006125384, 313.9678068554150059 ) ) ;
#79025 = CARTESIAN_POINT ( 'NONE',  ( 117.3845446746782386, -38.21944606407609513, 24.71276813305395237 ) ) ;
#79026 = EDGE_CURVE ( 'NONE', #66874, #15321, #66400, .T. ) ;
#79027 = CARTESIAN_POINT ( 'NONE',  ( 51.42025729304100423, -33.70561438051981185, -5.074374724088000832 ) ) ;
#79028 = EDGE_LOOP ( 'NONE', ( #18912, #51132, #80403, #25144 ) ) ;
#79029 = CARTESIAN_POINT ( 'NONE',  ( 97.75828382342812972, -40.38462848611586509, 172.6242326989190872 ) ) ;
#79030 = EDGE_CURVE ( 'NONE', #55083, #22615, #68729, .T. ) ;
#79031 = LINE ( 'NONE', #29530, #86800 ) ;
#79032 = ORIENTED_EDGE ( 'NONE', *, *, #83123, .F. ) ;
#79033 = CARTESIAN_POINT ( 'NONE',  ( 154.5667039024470171, -79.67844715994088745, 120.2178068554179902 ) ) ;
#79034 = DIRECTION ( 'NONE',  ( 1.000000000000000000, 1.261617073437676668E-15, 9.462128050782575008E-16 ) ) ;
#79035 = CARTESIAN_POINT ( 'NONE',  ( 106.8520627977276831, -47.75749532952668375, 227.5489586092439538 ) ) ;
#79036 = DIRECTION ( 'NONE',  ( 1.000000000000000000, 0.000000000000000000, 0.000000000000000000 ) ) ;
#79037 = EDGE_CURVE ( 'NONE', #15093, #26765, #4190, .T. ) ;
#79038 = FACE_BOUND ( 'NONE', #76574, .T. ) ;
#79039 = CARTESIAN_POINT ( 'NONE',  ( -105.4788588808462038, 120.6499999999999915, -3.968750000001139977 ) ) ;
#79040 = CARTESIAN_POINT ( 'NONE',  ( 98.42407572851979580, -32.30458340910843162, 245.3724198280769428 ) ) ;
#79042 = CARTESIAN_POINT ( 'NONE',  ( 99.14404768239424470, -44.40400490628089614, 37.95086337114900488 ) ) ;
#79041 = CARTESIAN_POINT ( 'NONE',  ( 179.8608231853560255, -35.55794170701751256, 342.9256252759119548 ) ) ;
#79043 = CARTESIAN_POINT ( 'NONE',  ( 111.3497592566078964, 65.14957505911826274, 68.16382463248645251 ) ) ;
#79044 = CARTESIAN_POINT ( 'NONE',  ( 107.3350830925955961, -26.26357308316309869, 120.0556252759109555 ) ) ;
#79045 = ORIENTED_EDGE ( 'NONE', *, *, #10253, .T. ) ;
#79046 = CYLINDRICAL_SURFACE ( 'NONE', #50968, 3.174999999999983391 ) ;
#79047 = EDGE_LOOP ( 'NONE', ( #86517, #87996, #10911, #64807 ) ) ;
#79048 = CARTESIAN_POINT ( 'NONE',  ( 97.06107110448571973, -37.99641202366499471, 67.42729194735355236 ) ) ;
#79049 = CARTESIAN_POINT ( 'NONE',  ( 134.0664832912739826, -18.72944715994100306, -5.074374724089001809 ) ) ;
#79051 = EDGE_LOOP ( 'NONE', ( #6223, #56174, #8715, #41542 ) ) ;
#79050 = ADVANCED_FACE ( 'NONE', ( #73216 ), #59577, .F. ) ;
#79052 = CARTESIAN_POINT ( 'NONE',  ( 115.8254254363784810, -31.73000183497265425, 49.23979340379111136 ) ) ;
#79053 = ORIENTED_EDGE ( 'NONE', *, *, #48976, .F. ) ;
#79054 = LINE ( 'NONE', #71349, #56663 ) ;
#79055 = PLANE ( 'NONE',  #75166 ) ;
#79056 = AXIS2_PLACEMENT_3D ( 'NONE', #52426, #23882, #78856 ) ;
#79057 = LINE ( 'NONE', #45829, #55331 ) ;
#79058 = ORIENTED_EDGE ( 'NONE', *, *, #13447, .F. ) ;
#79059 = CARTESIAN_POINT ( 'NONE',  ( 102.9623509218069302, -46.33686416246144546, 92.25562527591097250 ) ) ;
#79060 = FILL_AREA_STYLE ('',( #10012 ) ) ;
#79061 = VECTOR ( 'NONE', #41590, 1000.000000000000000 ) ;
#79062 = CARTESIAN_POINT ( 'NONE',  ( 141.9629299006807628, -45.68655394112754919, -5.074374724088960953 ) ) ;
#79063 = DIRECTION ( 'NONE',  ( -3.100000000000000258E-29, 3.100000000000000044E-14, 1.000000000000000000 ) ) ;
#79064 = CYLINDRICAL_SURFACE ( 'NONE', #31115, 3.174999999999983391 ) ;
#79065 = ORIENTED_EDGE ( 'NONE', *, *, #50039, .F. ) ;
#79066 = EDGE_CURVE ( 'NONE', #15987, #39978, #17817, .T. ) ;
#79067 = CARTESIAN_POINT ( 'NONE',  ( 46.03715912545343514, -48.62818131006090283, 180.4678068554150911 ) ) ;
#79068 = EDGE_CURVE ( 'NONE', #29470, #80239, #87757, .T. ) ;
#79069 = CARTESIAN_POINT ( 'NONE',  ( 106.5667039024470171, -94.77844715994137914, 2.217806855417697953 ) ) ;
#79070 = ADVANCED_FACE ( 'NONE', ( #45939, #5546, #86869, #39592, #66857, #67298, #31433 ), #5084, .T. ) ;
#79071 = CARTESIAN_POINT ( 'NONE',  ( -240.5296158183964792, 14.28749999999982201, 95.25000000000000000 ) ) ;
#79072 = ADVANCED_FACE ( 'NONE', ( #39150 ), #32784, .F. ) ;
#79074 = DIRECTION ( 'NONE',  ( -1.000000000000000000, -8.953411488912552682E-16, 0.000000000000000000 ) ) ;
#79073 = CARTESIAN_POINT ( 'NONE',  ( 0.000000000000000000, 0.000000000000000000, -161.5439999999999827 ) ) ;
#79075 = CARTESIAN_POINT ( 'NONE',  ( 0.000000000000000000, 101.5999999999999943, -103.1875000000000000 ) ) ;
#79076 = VECTOR ( 'NONE', #63776, 1000.000000000000000 ) ;
#79077 = ORIENTED_EDGE ( 'NONE', *, *, #84371, .F. ) ;
#79078 = VECTOR ( 'NONE', #18160, 1000.000000000000000 ) ;
#79079 = CIRCLE ( 'NONE', #44219, 3.250000000000002665 ) ;
#79080 = AXIS2_PLACEMENT_3D ( 'NONE', #46797, #17777, #47249 ) ;
#79081 = CYLINDRICAL_SURFACE ( 'NONE', #7083, 0.5000000000000104361 ) ;
#79082 = CARTESIAN_POINT ( 'NONE',  ( 114.0056865186721922, -29.02320718445401226, 155.5051490854339704 ) ) ;
#79084 = VERTEX_POINT ( 'NONE', #54096 ) ;
#79083 = CARTESIAN_POINT ( 'NONE',  ( 151.0371591254572934, -24.42818131005592974, 313.9678068554149490 ) ) ;
#79085 = AXIS2_PLACEMENT_3D ( 'NONE', #39812, #62059, #20736 ) ;
#79086 = AXIS2_PLACEMENT_3D ( 'NONE', #63441, #49799, #16202 ) ;
#79087 = CARTESIAN_POINT ( 'NONE',  ( 116.1206117333611019, -31.56300607074032882, 285.2384824187680579 ) ) ;
#79088 = CARTESIAN_POINT ( 'NONE',  ( 51.42025729304100423, -33.70561438051981185, 342.9256252759119548 ) ) ;
#79089 = CARTESIAN_POINT ( 'NONE',  ( -492.0614999999999668, 93.66249999999999432, 15.87500000000039968 ) ) ;
#79090 = CARTESIAN_POINT ( 'NONE',  ( -44.45000000000000284, 114.2999999999999972, 257.1750000000000114 ) ) ;
#79091 = ORIENTED_EDGE ( 'NONE', *, *, #40841, .T. ) ;
#79092 = CARTESIAN_POINT ( 'NONE',  ( 97.07210237969420064, -35.37814555816738959, 31.21915939149969077 ) ) ;
#79093 = CARTESIAN_POINT ( 'NONE',  ( 96.80143343076635176, -35.25719154489700458, 226.2251490854349640 ) ) ;
#79094 = VERTEX_POINT ( 'NONE', #4638 ) ;
#79095 = ORIENTED_EDGE ( 'NONE', *, *, #76901, .T. ) ;
#79096 = VECTOR ( 'NONE', #35594, 1000.000000000000000 ) ;
#79097 = CARTESIAN_POINT ( 'NONE',  ( 112.2422220273998477, -28.08754728269216372, 201.0787261630399598 ) ) ;
#79098 = DIRECTION ( 'NONE',  ( 0.5000000000000012212, 0.000000000000000000, 0.8660254037844380415 ) ) ;
#79099 = CARTESIAN_POINT ( 'NONE',  ( 115.8966032383871436, -37.77400989437322210, 50.16444044875395747 ) ) ;
#79100 = CARTESIAN_POINT ( 'NONE',  ( -88.25806911646338904, 93.94653598907717651, 96.20559720633596612 ) ) ;
#79101 = AXIS2_PLACEMENT_3D ( 'NONE', #38261, #9665, #29667 ) ;
#79102 = ADVANCED_FACE ( 'NONE', ( #53646 ), #86178, .T. ) ;
#79103 = DIRECTION ( 'NONE',  ( 0.000000000000000000, 1.000000000000000000, 0.000000000000000000 ) ) ;
#79104 = CARTESIAN_POINT ( 'NONE',  ( 107.0664832912739541, -21.02944715994095759, 311.6356252759109680 ) ) ;
#79105 = ORIENTED_EDGE ( 'NONE', *, *, #68766, .T. ) ;
#79106 = DIRECTION ( 'NONE',  ( -1.000000000000000000, -8.843517682682131024E-16, -1.000000000000000078E-15 ) ) ;
#79107 = DIRECTION ( 'NONE',  ( -4.237773401492740281E-14, 1.000000000000000000, 0.000000000000000000 ) ) ;
#79108 = VERTEX_POINT ( 'NONE', #25523 ) ;
#79109 = CARTESIAN_POINT ( 'NONE',  ( 105.7790678824445081, -26.40611305247077567, 270.1756252759109884 ) ) ;
#79110 = CARTESIAN_POINT ( 'NONE',  ( 6.162975822039154730E-30, 95.25000000000000000, 118.5560000000000116 ) ) ;
#79111 = VERTEX_POINT ( 'NONE', #74569 ) ;
#79112 = DIRECTION ( 'NONE',  ( -0.7071067811865476838, -0.7071067811865473507, 0.000000000000000000 ) ) ;
#79113 = FACE_OUTER_BOUND ( 'NONE', #50290, .T. ) ;
#79114 = DIRECTION ( 'NONE',  ( 1.000000000000000000, 6.508581945447490214E-14, 1.000000000000000078E-15 ) ) ;
#79116 = CARTESIAN_POINT ( 'NONE',  ( 116.7468388360763925, -38.12735696270775065, 24.71276813305395237 ) ) ;
#79115 = CIRCLE ( 'NONE', #45738, 118.5560000000000116 ) ;
#79117 = CARTESIAN_POINT ( 'NONE',  ( 107.0667039024470313, -104.2784471599409528, 45.21780685541799727 ) ) ;
#79118 = ORIENTED_EDGE ( 'NONE', *, *, #82516, .T. ) ;
#79119 = CARTESIAN_POINT ( 'NONE',  ( 110.5697598356958764, -46.63222799359486714, 33.84705384733993583 ) ) ;
#79120 = ADVANCED_FACE ( 'NONE', ( #12351 ), #38258, .F. ) ;
#79121 = LINE ( 'NONE', #78691, #83120 ) ;
#79122 = CIRCLE ( 'NONE', #64641, 2.517500000000005844 ) ;
#79123 = CARTESIAN_POINT ( 'NONE',  ( 116.3173282457959345, -41.53670860177669510, 288.4441967044823514 ) ) ;
#79124 = EDGE_CURVE ( 'NONE', #17571, #42544, #12252, .T. ) ;
#79125 = ORIENTED_EDGE ( 'NONE', *, *, #10212, .T. ) ;
#79126 = EDGE_CURVE ( 'NONE', #14315, #72641, #20494, .T. ) ;
#79127 = CARTESIAN_POINT ( 'NONE',  ( 82.81648329127398256, -18.72944715994105636, 3.101481641215461327 ) ) ;
#79128 = CARTESIAN_POINT ( 'NONE',  ( 117.0611971830093410, -38.07833408437429767, 19.71924984274187054 ) ) ;
#79129 = CARTESIAN_POINT ( 'NONE',  ( -44.45000000000000284, 114.2999999999999972, 206.3750000000000000 ) ) ;
#79130 = CARTESIAN_POINT ( 'NONE',  ( 115.1291642039608547, -38.00337907228554712, 111.5195189410199674 ) ) ;
#79131 = CARTESIAN_POINT ( 'NONE',  ( 98.41694670496758590, -29.81058001376278099, 191.7775300378159784 ) ) ;
#79132 = CARTESIAN_POINT ( 'NONE',  ( 107.0667039024470171, -79.67844715994094429, 138.7178068554180186 ) ) ;
#79133 = EDGE_CURVE ( 'NONE', #18507, #7678, #63010, .T. ) ;
#79134 = DIRECTION ( 'NONE',  ( -1.000000000000000000, -0.000000000000000000, -0.000000000000000000 ) ) ;
#79135 = ORIENTED_EDGE ( 'NONE', *, *, #76693, .F. ) ;
#79136 = EDGE_CURVE ( 'NONE', #71312, #37218, #6871, .T. ) ;
#79137 = CARTESIAN_POINT ( 'NONE',  ( 57.56670390244722313, -42.82844715994040996, 137.2178068554150911 ) ) ;
#79138 = ORIENTED_EDGE ( 'NONE', *, *, #5615, .T. ) ;
#79139 = VERTEX_POINT ( 'NONE', #76367 ) ;
#79140 = ADVANCED_FACE ( 'NONE', ( #62278 ), #68659, .F. ) ;
#79141 = VECTOR ( 'NONE', #192, 1000.000000000000000 ) ;
#79142 = FACE_BOUND ( 'NONE', #63707, .T. ) ;
#79143 = VECTOR ( 'NONE', #13281, 1000.000000000000000 ) ;
#79144 = ORIENTED_EDGE ( 'NONE', *, *, #86305, .T. ) ;
#79145 = ORIENTED_EDGE ( 'NONE', *, *, #84269, .F. ) ;
#79146 = DIRECTION ( 'NONE',  ( -0.000000000000000000, 1.000000000000000000, -0.000000000000000000 ) ) ;
#79147 = AXIS2_PLACEMENT_3D ( 'NONE', #64046, #84951, #37679 ) ;
#79148 = EDGE_CURVE ( 'NONE', #51120, #57891, #55890, .T. ) ;
#79149 = CARTESIAN_POINT ( 'NONE',  ( 103.2786526221089645, -27.47459228116735375, 41.38561342082059724 ) ) ;
#79150 = CARTESIAN_POINT ( 'NONE',  ( 100.0140161817732860, -31.91085406740108610, 120.2724198280769912 ) ) ;
#79152 = CARTESIAN_POINT ( 'NONE',  ( 115.6474790210939290, -28.48352029850561706, 39.43562527591099354 ) ) ;
#79151 = VECTOR ( 'NONE', #18268, 1000.000000000000000 ) ;
#79153 = EDGE_CURVE ( 'NONE', #3395, #18115, #61380, .T. ) ;
#79154 = DIRECTION ( 'NONE',  ( 0.000000000000000000, 0.4999999999999998890, 0.8660254037844387076 ) ) ;
#79156 = ORIENTED_EDGE ( 'NONE', *, *, #88312, .F. ) ;
#79155 = ADVANCED_FACE ( 'NONE', ( #69555 ), #62729, .F. ) ;
#79157 = VECTOR ( 'NONE', #89919, 999.9999999999998863 ) ;
#79158 = CARTESIAN_POINT ( 'NONE',  ( 115.1113848037478391, -30.75858365065169764, 135.3346201298422216 ) ) ;
#79159 = VERTEX_POINT ( 'NONE', #40496 ) ;
#79160 = DIRECTION ( 'NONE',  ( 0.000000000000000000, 1.000000000000000000, 0.000000000000000000 ) ) ;
#79161 = LINE ( 'NONE', #73657, #29926 ) ;
#79162 = CARTESIAN_POINT ( 'NONE',  ( 84.06648329127399677, -18.82844715994099971, 17.92562527591199739 ) ) ;
#79163 = AXIS2_PLACEMENT_3D ( 'NONE', #16846, #44524, #77738 ) ;
#79164 = CARTESIAN_POINT ( 'NONE',  ( 112.3606361654194075, -28.17110760307337713, 289.6356252759109680 ) ) ;
#79165 = ORIENTED_EDGE ( 'NONE', *, *, #48328, .F. ) ;
#79166 = CARTESIAN_POINT ( 'NONE',  ( 115.9069864544413662, -30.09434420101750973, 264.3508633711492735 ) ) ;
#79167 = CARTESIAN_POINT ( 'NONE',  ( 97.03360904796217312, -33.74039811955494628, 27.09562527591097236 ) ) ;
#79168 = CARTESIAN_POINT ( 'NONE',  ( 101.9936209330291064, -45.44607153419508450, 118.1564586085293627 ) ) ;
#79169 = VECTOR ( 'NONE', #2320, 1000.000000000000000 ) ;
#79171 = CARTESIAN_POINT ( 'NONE',  ( 69.38693536744452217, -138.6172649514752777, 247.3844049223929176 ) ) ;
#79170 = CARTESIAN_POINT ( 'NONE',  ( 123.6837132603318707, -20.11243780205705534, 219.5838068554170093 ) ) ;
#79172 = CARTESIAN_POINT ( 'NONE',  ( 105.8602753772252498, -25.33367152814009771, 323.3526086649692957 ) ) ;
#79173 = CARTESIAN_POINT ( 'NONE',  ( 163.0959832912774914, -23.42844715993537719, 117.4678068554150485 ) ) ;
#79174 = CARTESIAN_POINT ( 'NONE',  ( 131.5555141844853040, -37.85480617634013356, 7.067502061095533250 ) ) ;
#79175 = LINE ( 'NONE', #65522, #60488 ) ;
#79176 = VECTOR ( 'NONE', #86453, 999.9999999999998863 ) ;
#79177 = DIRECTION ( 'NONE',  ( -0.000000000000000000, 0.8660254037844340447, 0.5000000000000081046 ) ) ;
#79178 = EDGE_CURVE ( 'NONE', #30549, #31278, #46524, .T. ) ;
#79179 = LINE ( 'NONE', #71018, #23987 ) ;
#79180 = LINE ( 'NONE', #78738, #19129 ) ;
#79181 = CARTESIAN_POINT ( 'NONE',  ( 111.0631195717115673, -47.08511319755631774, 17.85753003781598380 ) ) ;
#79182 = CARTESIAN_POINT ( 'NONE',  ( 97.38209261381841486, -42.05735084626116560, 172.7146728949589942 ) ) ;
#79183 = CARTESIAN_POINT ( 'NONE',  ( 105.4175444341163939, -47.04536977979798706, 33.44991099019695469 ) ) ;
#79184 = EDGE_CURVE ( 'NONE', #29469, #80801, #3558, .T. ) ;
#79186 = CARTESIAN_POINT ( 'NONE',  ( 72.26648329127297643, -71.52944715994141234, 361.9756252759109998 ) ) ;
#79185 = CARTESIAN_POINT ( 'NONE',  ( -240.5296158183964792, 14.28749999999982201, 90.48749999999999716 ) ) ;
#79187 = CARTESIAN_POINT ( 'NONE',  ( 172.5664832912740110, -36.32844715994070839, 14.17562527591199917 ) ) ;
#79188 = VECTOR ( 'NONE', #20455, 1000.000000000000000 ) ;
#79189 = VECTOR ( 'NONE', #70885, 1000.000000000000000 ) ;
#79190 = CIRCLE ( 'NONE', #11005, 7.999999999999992895 ) ;
#79191 = ORIENTED_EDGE ( 'NONE', *, *, #45548, .T. ) ;
#79192 = CARTESIAN_POINT ( 'NONE',  ( 109.7248659590922273, -27.00080519083036990, 185.8647919394705070 ) ) ;
#79193 = ORIENTED_EDGE ( 'NONE', *, *, #89740, .F. ) ;
#79194 = CARTESIAN_POINT ( 'NONE',  ( 113.0644005321300227, -46.09090919705343481, 64.02991099019594401 ) ) ;
#79196 = ORIENTED_EDGE ( 'NONE', *, *, #6008, .F. ) ;
#79195 = CARTESIAN_POINT ( 'NONE',  ( 4.684674336965106711, 94.35461990771972296, 130.4719347088314123 ) ) ;
#79197 = DIRECTION ( 'NONE',  ( 3.999999999999999995E-14, -1.000000000000000000, 4.100000000000000342E-29 ) ) ;
#79198 = CARTESIAN_POINT ( 'NONE',  ( 104.4591861284130232, -26.65816784528765382, 196.2784824187679362 ) ) ;
#79199 = DIRECTION ( 'NONE',  ( 1.000000000000000078E-15, -1.000000000000000083E-30, -1.000000000000000000 ) ) ;
#79200 = CARTESIAN_POINT ( 'NONE',  ( 97.83900604915858423, -40.58358724573557197, 146.6413223322464603 ) ) ;
#79201 = FACE_OUTER_BOUND ( 'NONE', #83996, .T. ) ;
#79202 = LINE ( 'NONE', #65104, #64489 ) ;
#79203 = LINE ( 'NONE', #30142, #20156 ) ;
#79204 = FACE_OUTER_BOUND ( 'NONE', #33526, .T. ) ;
#79205 = CARTESIAN_POINT ( 'NONE',  ( 98.54774150848822956, -41.53511815344526070, 136.7356252759109623 ) ) ;
#79206 = VERTEX_POINT ( 'NONE', #10015 ) ;
#79207 = ORIENTED_EDGE ( 'NONE', *, *, #61811, .T. ) ;
#79208 = CARTESIAN_POINT ( 'NONE',  ( 108.3172770934737628, -27.95654607328577868, 101.3958690201829711 ) ) ;
#79209 = AXIS2_PLACEMENT_3D ( 'NONE', #59941, #75831, #74940 ) ;
#79210 = CARTESIAN_POINT ( 'NONE',  ( 191.6375511031394865, 22.69262065192448219, 323.8756252759109202 ) ) ;
#79211 = VECTOR ( 'NONE', #46319, 1000.000000000000000 ) ;
#79213 = DIRECTION ( 'NONE',  ( 0.000000000000000000, 0.000000000000000000, -1.000000000000000000 ) ) ;
#79212 = CARTESIAN_POINT ( 'NONE',  ( 103.5361331145923032, -27.60804031003073788, 211.3699109901959616 ) ) ;
#79214 = AXIS2_PLACEMENT_3D ( 'NONE', #48224, #84584, #8724 ) ;
#79215 = DIRECTION ( 'NONE',  ( 0.000000000000000000, -1.000000000000000000, 0.000000000000000000 ) ) ;
#79216 = PLANE ( 'NONE',  #66906 ) ;
#79217 = CARTESIAN_POINT ( 'NONE',  ( 118.4716181662679872, 70.66242608954388515, 4.488731742999982011 ) ) ;
#79218 = CARTESIAN_POINT ( 'NONE',  ( -28.99999999999997513, 172.0000000000000000, 183.8826257785461280 ) ) ;
#79219 = DIRECTION ( 'NONE',  ( 0.000000000000000000, 1.000000000000000000, 0.000000000000000000 ) ) ;
#79220 = DIRECTION ( 'NONE',  ( 0.000000000000000000, -1.000000000000000000, 0.000000000000000000 ) ) ;
#79221 = CARTESIAN_POINT ( 'NONE',  ( 96.64068249873260186, -36.21262657180042766, 171.2870538473399620 ) ) ;
#79222 = EDGE_LOOP ( 'NONE', ( #50525, #84060, #4764, #82865 ) ) ;
#79223 = VERTEX_POINT ( 'NONE', #9571 ) ;
#79224 = FACE_OUTER_BOUND ( 'NONE', #255, .T. ) ;
#79225 = CARTESIAN_POINT ( 'NONE',  ( 147.0183410955044678, -67.92213675950819152, 245.9229835953497911 ) ) ;
#79226 = CARTESIAN_POINT ( 'NONE',  ( -492.0614999999999668, 14.28750000000029985, 6.349999999999710099 ) ) ;
#79227 = CARTESIAN_POINT ( 'NONE',  ( 41.56648329127398966, -27.57844715994070484, 318.9256252759120116 ) ) ;
#79228 = VECTOR ( 'NONE', #48890, 999.9999999999998863 ) ;
#79229 = DIRECTION ( 'NONE',  ( 0.7071067811865614505, -0.7071067811865336949, 0.000000000000000000 ) ) ;
#79230 = AXIS2_PLACEMENT_3D ( 'NONE', #70691, #36166, #83885 ) ;
#79231 = EDGE_CURVE ( 'NONE', #12340, #35953, #37272, .T. ) ;
#79232 = CARTESIAN_POINT ( 'NONE',  ( 97.38189020833135601, -42.05746220039552696, 176.7146728949589658 ) ) ;
#79233 = EDGE_CURVE ( 'NONE', #14667, #76506, #61516, .T. ) ;
#79234 = DIRECTION ( 'NONE',  ( 0.000000000000000000, 0.000000000000000000, -1.000000000000000000 ) ) ;
#79235 = ORIENTED_EDGE ( 'NONE', *, *, #12162, .F. ) ;
#79237 = EDGE_LOOP ( 'NONE', ( #26663, #9023, #15757, #33058 ) ) ;
#79236 = VERTEX_POINT ( 'NONE', #44511 ) ;
#79238 = ADVANCED_FACE ( 'NONE', ( #84993 ), #70280, .T. ) ;
#79239 = CARTESIAN_POINT ( 'NONE',  ( -3.286821707691937711, 70.27560252132435892, 118.5111027017741776 ) ) ;
#79240 = DIRECTION ( 'NONE',  ( 0.7071067811865344721, 8.659560562355082002E-17, 0.7071067811865604513 ) ) ;
#79241 = CARTESIAN_POINT ( 'NONE',  ( 133.0522658620028835, -34.17316201338590531, 8.065992442480034441 ) ) ;
#79242 = CARTESIAN_POINT ( 'NONE',  ( 98.30854254679421445, -35.37787306724802505, 262.6358690201826676 ) ) ;
#79243 = ADVANCED_FACE ( 'NONE', ( #9126 ), #15941, .T. ) ;
#79244 = DIRECTION ( 'NONE',  ( 0.7071067811868056996, 0.7071067811862893349, 7.071067811868050964E-16 ) ) ;
#79245 = VERTEX_POINT ( 'NONE', #85886 ) ;
#79246 = CARTESIAN_POINT ( 'NONE',  ( 115.1222891817772620, -41.02565380217686908, 9.635625275910943088 ) ) ;
#79247 = DIRECTION ( 'NONE',  ( 1.000000000000000078E-15, -1.000000000000000083E-30, -1.000000000000000000 ) ) ;
#79248 = ORIENTED_EDGE ( 'NONE', *, *, #85795, .F. ) ;
#79249 = ORIENTED_EDGE ( 'NONE', *, *, #14313, .T. ) ;
#79250 = EDGE_CURVE ( 'NONE', #49393, #13709, #64534, .T. ) ;
#79251 = FACE_OUTER_BOUND ( 'NONE', #13263, .T. ) ;
#79252 = ORIENTED_EDGE ( 'NONE', *, *, #15565, .F. ) ;
#79253 = EDGE_LOOP ( 'NONE', ( #36034, #1083, #81592, #31778 ) ) ;
#79254 = ADVANCED_FACE ( 'NONE', ( #85450 ), #79064, .F. ) ;
#79255 = CARTESIAN_POINT ( 'NONE',  ( 114.5155466417691912, -41.88356374938643256, 12.77908649474396263 ) ) ;
#79256 = CARTESIAN_POINT ( 'NONE',  ( 109.3633609874958523, -25.89340572475189006, 184.9222919425779708 ) ) ;
#79257 = CARTESIAN_POINT ( 'NONE',  ( 102.4028819069269218, -26.73371583578772004, 135.4118157521009493 ) ) ;
#79258 = CARTESIAN_POINT ( 'NONE',  ( 51.34673845256495639, -36.02818131005847135, 117.4678068554150485 ) ) ;
#79259 = CARTESIAN_POINT ( 'NONE',  ( 109.9892391005685255, -26.72245031140752758, 255.8499109901966051 ) ) ;
#79260 = CARTESIAN_POINT ( 'NONE',  ( 0.000000000000000000, 82.54999999999999716, -179.8908777604655143 ) ) ;
#79261 = CARTESIAN_POINT ( 'NONE',  ( 73.74475183977565962, -128.3542712181327943, 248.3919653347779786 ) ) ;
#79262 = CARTESIAN_POINT ( 'NONE',  ( -130.1658077747427171, 74.80151635532865839, -10.09693588310369350 ) ) ;
#79263 = VERTEX_POINT ( 'NONE', #77268 ) ;
#79264 = EDGE_CURVE ( 'NONE', #52443, #59735, #55028, .T. ) ;
#79265 = ORIENTED_EDGE ( 'NONE', *, *, #58271, .F. ) ;
#79266 = CIRCLE ( 'NONE', #40066, 3.249999999999975131 ) ;
#79267 = AXIS2_PLACEMENT_3D ( 'NONE', #20997, #48673, #78674 ) ;
#79269 = CARTESIAN_POINT ( 'NONE',  ( 116.3896376309502045, -44.12590514183388990, 198.2927681330539542 ) ) ;
#79268 = AXIS2_PLACEMENT_3D ( 'NONE', #2637, #16708, #51199 ) ;
#79270 = ORIENTED_EDGE ( 'NONE', *, *, #55736, .F. ) ;
#79271 = CONICAL_SURFACE ( 'NONE', #28476, 5.562600000000000655, 1.029744258676653645 ) ;
#79272 = CARTESIAN_POINT ( 'NONE',  ( 96.01388918828124019, -36.58377270012555726, 156.3280062282919687 ) ) ;
#79273 = FACE_OUTER_BOUND ( 'NONE', #61787, .T. ) ;
#79274 = AXIS2_PLACEMENT_3D ( 'NONE', #34614, #29153, #14636 ) ;
#79275 = B_SPLINE_CURVE_WITH_KNOTS ( 'NONE', 3,
 ( #59368, #52970, #4864, #45719, #66635, #46173, #67531, #33010, #87990, #4426, #32112, #73904, #65736, #32553, #60706, #11688, #60258, #39382, #25748, #88442, #74357, #12127, #39809, #26203, #44846, #89340 ),
 .UNSPECIFIED., .F., .F.,
 ( 4, 2, 2, 2, 2, 2, 2, 2, 2, 2, 2, 2, 4 ),
 ( 0.01986933033599076748, 0.02111058882927464853, 0.02235184732255853304, 0.02483436430912634024, 0.02607562280241026292, 0.02731688129569418561, 0.02979939828226199974, 0.03228191526882981388, 0.03352317376211371575, 0.03476443225539761761, 0.03724694924196542134, 0.03848820773524931627, 0.03972946622853321813 ),
 .UNSPECIFIED. ) ;
#79276 = LINE ( 'NONE', #73773, #71126 ) ;
#79277 = CARTESIAN_POINT ( 'NONE',  ( 143.7785205373602082, -140.1898562409545548, 246.8437313719147994 ) ) ;
#79280 = CARTESIAN_POINT ( 'NONE',  ( 98.95751068421678553, -41.73716824282166016, 7.768006228290936122 ) ) ;
#79279 = DIRECTION ( 'NONE',  ( -0.9254794337955620787, -0.3787978585227822492, 0.000000000000000000 ) ) ;
#79278 = DIRECTION ( 'NONE',  ( -0.8571673007021084478, -0.5150380749100604838, -8.571673007021083688E-16 ) ) ;
#79281 = DIRECTION ( 'NONE',  ( 0.7071067811865426878, -0.000000000000000000, -0.7071067811865524577 ) ) ;
#79282 = DIRECTION ( 'NONE',  ( 0.9963424814100680926, -0.08544974978095691565, 0.000000000000000000 ) ) ;
#79283 = DIRECTION ( 'NONE',  ( -0.4999999999999998890, -0.8660254037844387076, 0.000000000000000000 ) ) ;
#79284 = CARTESIAN_POINT ( 'NONE',  ( 67.97654527815089409, -137.2003834803944926, 247.1835444442183984 ) ) ;
#79285 = DIRECTION ( 'NONE',  ( -0.8571673007021110013, 1.917331853055865018E-16, 0.5150380749100563760 ) ) ;
#79286 = DIRECTION ( 'NONE',  ( -0.8473160576754937834, 0.4185024680272297348, 0.3269727552264514725 ) ) ;
#79288 = ORIENTED_EDGE ( 'NONE', *, *, #73855, .F. ) ;
#79287 = CARTESIAN_POINT ( 'NONE',  ( 99.35013961165397234, -39.68856579947961194, 195.5838068554172651 ) ) ;
#79289 = CARTESIAN_POINT ( 'NONE',  ( 135.9139897988289079, -20.77444411305278749, 7.664507283848439378 ) ) ;
#79290 = CARTESIAN_POINT ( 'NONE',  ( 96.62214413241265731, -36.48016117738031738, 196.3070538473399438 ) ) ;
#79291 = CARTESIAN_POINT ( 'NONE',  ( 117.2667774650794428, -38.88269731149204489, 59.66133956162595098 ) ) ;
#79292 = CARTESIAN_POINT ( 'NONE',  ( 98.90868739403623522, -30.16870437830188934, 236.7870538473399336 ) ) ;
#79293 = CARTESIAN_POINT ( 'NONE',  ( 120.1849926298398685, -37.85453553205689303, 293.6356252759106837 ) ) ;
#79294 = EDGE_CURVE ( 'NONE', #34565, #36668, #31783, .T. ) ;
#79295 = CARTESIAN_POINT ( 'NONE',  ( 172.5664832912729878, -27.82844715994070484, 318.9256252759120116 ) ) ;
#79296 = AXIS2_PLACEMENT_3D ( 'NONE', #1033, #37343, #85959 ) ;
#79298 = CARTESIAN_POINT ( 'NONE',  ( 112.9469377066634905, -44.85846281290874771, 39.07437081555113423 ) ) ;
#79297 = CARTESIAN_POINT ( 'NONE',  ( 50.97905606905900555, -31.62489322948711035, 237.4678068554150059 ) ) ;
#79299 = DIRECTION ( 'NONE',  ( 0.000000000000000000, 0.000000000000000000, -1.000000000000000000 ) ) ;
#79300 = CARTESIAN_POINT ( 'NONE',  ( 20.03715912545735023, -46.82818131006192175, 180.4678068554150911 ) ) ;
#79301 = ORIENTED_EDGE ( 'NONE', *, *, #27908, .T. ) ;
#79302 = CARTESIAN_POINT ( 'NONE',  ( 97.31306429104051858, -38.96057676328502595, 66.50610887445193953 ) ) ;
#79303 = VECTOR ( 'NONE', #33136, 1000.000000000000000 ) ;
#79304 = EDGE_LOOP ( 'NONE', ( #12102, #67280, #25295, #63162 ) ) ;
#79305 = ORIENTED_EDGE ( 'NONE', *, *, #66090, .T. ) ;
#79306 = CARTESIAN_POINT ( 'NONE',  ( 113.3268105416314171, -43.27322076882862945, 112.5943245899819516 ) ) ;
#79308 = VERTEX_POINT ( 'NONE', #11799 ) ;
#79307 = CARTESIAN_POINT ( 'NONE',  ( -0.8293186434173683841, 95.24999999999997158, -130.5560000000000116 ) ) ;
#79309 = CARTESIAN_POINT ( 'NONE',  ( 114.5517459224756038, -44.00510994954048982, 94.21276813305395592 ) ) ;
#79310 = DIRECTION ( 'NONE',  ( 0.000000000000000000, 1.000000000000000000, 0.000000000000000000 ) ) ;
#79311 = CARTESIAN_POINT ( 'NONE',  ( 80.06648329127398256, -15.97944715994105813, 8.225625275910942946 ) ) ;
#79312 = EDGE_CURVE ( 'NONE', #10387, #67090, #79964, .T. ) ;
#79313 = DIRECTION ( 'NONE',  ( -3.100000000000000258E-29, 3.100000000000000044E-14, 1.000000000000000000 ) ) ;
#79314 = CARTESIAN_POINT ( 'NONE',  ( 116.1702204290647984, -31.76348745297265808, 24.21181575210196257 ) ) ;
#79315 = VERTEX_POINT ( 'NONE', #88113 ) ;
#79316 = ORIENTED_EDGE ( 'NONE', *, *, #89398, .T. ) ;
#79317 = ORIENTED_EDGE ( 'NONE', *, *, #72281, .F. ) ;
#79318 = EDGE_CURVE ( 'NONE', #45792, #34396, #54295, .T. ) ;
#79319 = CARTESIAN_POINT ( 'NONE',  ( 62.56670390244663338, -48.82844715994099971, 180.4678068554151196 ) ) ;
#79320 = DIRECTION ( 'NONE',  ( -3.999999999999999995E-14, 1.000000000000000000, -4.100000000000000342E-29 ) ) ;
#79321 = CARTESIAN_POINT ( 'NONE',  ( 97.81170255947417047, -40.51743869465033754, 117.6354096206635518 ) ) ;
#79322 = PLANE ( 'NONE',  #16508 ) ;
#79323 = DIRECTION ( 'NONE',  ( 0.9130365726098601531, 0.000000000000000000, 0.4078776986755215384 ) ) ;
#79324 = CARTESIAN_POINT ( 'NONE',  ( 1.665555919329872792, 69.93248702128259708, -130.5479027315182066 ) ) ;
#79325 = CARTESIAN_POINT ( 'NONE',  ( 107.0667039024470313, -104.2784471599420755, -19.78219314458201694 ) ) ;
#79326 = CARTESIAN_POINT ( 'NONE',  ( -7.206242203287891002, 93.00761057503720508, 130.3569541155684988 ) ) ;
#79327 = CARTESIAN_POINT ( 'NONE',  ( 97.37192905580960200, -32.85904099757679830, 41.02419670448193045 ) ) ;
#79328 = ORIENTED_EDGE ( 'NONE', *, *, #31436, .T. ) ;
#79329 = ORIENTED_EDGE ( 'NONE', *, *, #41535, .T. ) ;
#79330 = CARTESIAN_POINT ( 'NONE',  ( 116.3221839001005264, -32.94216875276463696, 149.1356252759109680 ) ) ;
#79331 = CARTESIAN_POINT ( 'NONE',  ( 41.56648329127398966, -27.82844715994070484, 255.9256252759120116 ) ) ;
#79332 = VECTOR ( 'NONE', #5261, 1000.000000000000000 ) ;
#79333 = DIRECTION ( 'NONE',  ( -0.000000000000000000, 1.000000000000000000, 0.000000000000000000 ) ) ;
#79334 = CARTESIAN_POINT ( 'NONE',  ( 100.3267271402381624, -32.12451360540737255, 118.6680903695919653 ) ) ;
#79335 = AXIS2_PLACEMENT_3D ( 'NONE', #61485, #88329, #12914 ) ;
#79336 = VECTOR ( 'NONE', #26030, 1000.000000000000000 ) ;
#79337 = VECTOR ( 'NONE', #57974, 1000.000000000000000 ) ;
#79338 = EDGE_CURVE ( 'NONE', #88268, #41446, #47040, .T. ) ;
#79339 = DIRECTION ( 'NONE',  ( 0.000000000000000000, 1.000000000000000000, 0.000000000000000000 ) ) ;
#79340 = ADVANCED_FACE ( 'NONE', ( #46287 ), #87212, .F. ) ;
#79341 = DIRECTION ( 'NONE',  ( -0.9825752044165969590, -0.1858654558159821002, 0.000000000000000000 ) ) ;
#79342 = ORIENTED_EDGE ( 'NONE', *, *, #62188, .F. ) ;
#79343 = VERTEX_POINT ( 'NONE', #72692 ) ;
#79344 = DIRECTION ( 'NONE',  ( 4.299999999999999979E-14, -1.000000000000000000, 4.400000000000000367E-29 ) ) ;
#79345 = ADVANCED_FACE ( 'NONE', ( #59478 ), #32678, .F. ) ;
#79346 = ORIENTED_EDGE ( 'NONE', *, *, #58210, .T. ) ;
#79347 = VERTEX_POINT ( 'NONE', #10893 ) ;
#79348 = CARTESIAN_POINT ( 'NONE',  ( 111.6733053606431412, -27.77132819582071122, 166.1301547344679932 ) ) ;
#79349 = EDGE_CURVE ( 'NONE', #36478, #55038, #7909, .T. ) ;
#79350 = DIRECTION ( 'NONE',  ( 3.100000000000000258E-29, -3.100000000000000044E-14, -1.000000000000000000 ) ) ;
#79351 = AXIS2_PLACEMENT_3D ( 'NONE', #66719, #73531, #39462 ) ;
#79352 = CARTESIAN_POINT ( 'NONE',  ( 102.3028228262999164, -26.72980997527264790, 136.4422919425779526 ) ) ;
#79353 = CARTESIAN_POINT ( 'NONE',  ( 132.3254539024480039, -42.97311385573998876, 231.5838068554170093 ) ) ;
#79354 = CARTESIAN_POINT ( 'NONE',  ( 110.8543047535783330, -45.98430580984275906, 17.88561088277840838 ) ) ;
#79355 = ORIENTED_EDGE ( 'NONE', *, *, #58478, .F. ) ;
#79357 = EDGE_CURVE ( 'NONE', #56828, #56526, #46447, .T. ) ;
#79356 = AXIS2_PLACEMENT_3D ( 'NONE', #46596, #82507, #61574 ) ;
#79358 = ORIENTED_EDGE ( 'NONE', *, *, #66622, .F. ) ;
#79359 = EDGE_LOOP ( 'NONE', ( #9151, #2331, #42211, #54962 ) ) ;
#79360 = EDGE_CURVE ( 'NONE', #21659, #51663, #42706, .T. ) ;
#79361 = B_SPLINE_CURVE_WITH_KNOTS ( 'NONE', 1,
 ( #20692, #42453 ),
 .UNSPECIFIED., .F., .F.,
 ( 2, 2 ),
 ( 0.000000000000000000, 0.003789203591536580672 ),
 .UNSPECIFIED. ) ;
#79362 = CARTESIAN_POINT ( 'NONE',  ( 100.9764986820135420, -31.29420903488464845, 188.5652332267349607 ) ) ;
#79363 = CARTESIAN_POINT ( 'NONE',  ( 110.3610989901968651, -25.31982300743893077, 64.85276813305395649 ) ) ;
#79364 = ORIENTED_EDGE ( 'NONE', *, *, #33753, .F. ) ;
#79365 = CARTESIAN_POINT ( 'NONE',  ( 96.85498737197825392, -38.89503640450125488, 31.49276813305495892 ) ) ;
#79366 = DIRECTION ( 'NONE',  ( -0.7071067708032359178, -0.0001211784769794170747, 0.7071067811865451302 ) ) ;
#79367 = DIRECTION ( 'NONE',  ( 0.000000000000000000, 1.000000000000000000, 0.000000000000000000 ) ) ;
#79368 = CARTESIAN_POINT ( 'NONE',  ( 112.4860951546057919, -26.19083136796355404, 165.6984824187679521 ) ) ;
#79369 = CARTESIAN_POINT ( 'NONE',  ( 116.3259679314843282, -32.93868236591013243, 264.1356252759109680 ) ) ;
#79370 = ORIENTED_EDGE ( 'NONE', *, *, #75434, .F. ) ;
#79371 = DIRECTION ( 'NONE',  ( 1.000000000000000000, 6.831565154159360295E-14, 0.000000000000000000 ) ) ;
#79372 = ORIENTED_EDGE ( 'NONE', *, *, #40964, .F. ) ;
#79373 = DIRECTION ( 'NONE',  ( -1.000000000000000000, -1.000000000000000078E-15, 0.000000000000000000 ) ) ;
#79374 = DIRECTION ( 'NONE',  ( 0.000000000000000000, -1.000000000000000000, 0.000000000000000000 ) ) ;
#79375 = VERTEX_POINT ( 'NONE', #59919 ) ;
#79376 = VECTOR ( 'NONE', #842, 1000.000000000000000 ) ;
#79377 = CARTESIAN_POINT ( 'NONE',  ( 270.8910000000000196, 65.43750000000000000, -2.032000000000000028 ) ) ;
#79378 = CARTESIAN_POINT ( 'NONE',  ( 194.5667039024479834, -67.87844715994100397, 310.9178068554150514 ) ) ;
#79379 = CARTESIAN_POINT ( 'NONE',  ( 98.58988425959138624, -43.82355431373886034, 71.86895860924397539 ) ) ;
#79380 = CARTESIAN_POINT ( 'NONE',  ( 31.75000000000000000, 124.5870000000000033, 3.174999999999999822 ) ) ;
#79381 = DIRECTION ( 'NONE',  ( 6.745093096447288888E-17, 1.000000000000000000, 0.000000000000000000 ) ) ;
#79382 = CARTESIAN_POINT ( 'NONE',  ( 182.5667039024480118, -32.29483332968450782, -5.074374724088000832 ) ) ;
#79383 = CARTESIAN_POINT ( 'NONE',  ( 100.8224265971272615, -29.20115443902020047, 40.62705384733994407 ) ) ;
#79385 = CARTESIAN_POINT ( 'NONE',  ( 99.30484619187392070, -29.80227926343066613, 186.7470538473389752 ) ) ;
#79384 = LINE ( 'NONE', #51640, #56472 ) ;
#79386 = DIRECTION ( 'NONE',  ( 0.9347835805883503157, 0.000000000000000000, -0.3552177606235690788 ) ) ;
#79387 = DIRECTION ( 'NONE',  ( 0.000000000000000000, -1.000000000000000000, 0.000000000000000000 ) ) ;
#79388 = ORIENTED_EDGE ( 'NONE', *, *, #5250, .F. ) ;
#79389 = CARTESIAN_POINT ( 'NONE',  ( 41.56648329127398966, -27.82844715994070484, 138.9256252759119832 ) ) ;
#79390 = CARTESIAN_POINT ( 'NONE',  ( 102.3035641816324102, -119.0284471599421181, -21.78219314458157285 ) ) ;
#79391 = CARTESIAN_POINT ( 'NONE',  ( 86.71802151318415497, -122.7425185119399629, 250.2203867545810283 ) ) ;
#79392 = DIRECTION ( 'NONE',  ( 0.7071067812123270624, 0.7071067811607679721, 0.000000000000000000 ) ) ;
#79394 = EDGE_LOOP ( 'NONE', ( #12591, #60461, #80390, #79191, #67146, #55952 ) ) ;
#79393 = CARTESIAN_POINT ( 'NONE',  ( 107.6569944592711607, -47.81385874506208467, 197.6308633711489620 ) ) ;
#79395 = CIRCLE ( 'NONE', #6810, 7.999999999999992895 ) ;
#79396 = CARTESIAN_POINT ( 'NONE',  ( 115.8254250420262252, -31.73000087149041448, 144.2397934866363016 ) ) ;
#79397 = CARTESIAN_POINT ( 'NONE',  ( 109.9953477121747767, -26.70153551007575388, 255.8499109901966051 ) ) ;
#79398 = CARTESIAN_POINT ( 'NONE',  ( 101.6884573362309823, -27.70642928270265060, 81.50419670448295051 ) ) ;
#79399 = CONICAL_SURFACE ( 'NONE', #67765, 5.562599999999973122, 1.029744258676653645 ) ;
#79400 = CARTESIAN_POINT ( 'NONE',  ( 83.90387289223293976, 76.93632333215535368, 100.0252357601330004 ) ) ;
#79401 = ADVANCED_FACE ( 'NONE', ( #19053 ), #89156, .T. ) ;
#79402 = PLANE ( 'NONE',  #51775 ) ;
#79403 = CARTESIAN_POINT ( 'NONE',  ( 100.8082743238007595, 80.89704698943972971, -82.96136257730026387 ) ) ;
#79404 = FACE_OUTER_BOUND ( 'NONE', #29641, .T. ) ;
#79405 = ORIENTED_EDGE ( 'NONE', *, *, #72041, .F. ) ;
#79406 = AXIS2_PLACEMENT_3D ( 'NONE', #26868, #68217, #74130 ) ;
#79407 = VECTOR ( 'NONE', #81689, 1000.000000000000000 ) ;
#79408 = VECTOR ( 'NONE', #76530, 999.9999999999998863 ) ;
#79409 = EDGE_LOOP ( 'NONE', ( #60889, #39196, #40620, #31150 ) ) ;
#79410 = ORIENTED_EDGE ( 'NONE', *, *, #17976, .T. ) ;
#79411 = ORIENTED_EDGE ( 'NONE', *, *, #86926, .T. ) ;
#79412 = CARTESIAN_POINT ( 'NONE',  ( 89.60916260784479448, 223.9999999999999716, 134.1927865330827103 ) ) ;
#79413 = CARTESIAN_POINT ( 'NONE',  ( 97.22385571422852024, -40.27120027895552568, 262.6013395616254797 ) ) ;
#79414 = CARTESIAN_POINT ( 'NONE',  ( 193.0374249753376432, -23.42844715993431848, 180.4678068554150343 ) ) ;
#79415 = CARTESIAN_POINT ( 'NONE',  ( 138.0667039024479266, -14.72944715994091069, 239.5838068554170377 ) ) ;
#79416 = AXIS2_PLACEMENT_3D ( 'NONE', #43027, #8540, #29429 ) ;
#79417 = AXIS2_PLACEMENT_3D ( 'NONE', #81565, #48783, #75629 ) ;
#79419 = CARTESIAN_POINT ( 'NONE',  ( 75.10852726169315474, 77.68452076096552616, 91.72954497613159219 ) ) ;
#79418 = CARTESIAN_POINT ( 'NONE',  ( 134.0664832912740110, -46.72944715994100306, 8.225625275910998013 ) ) ;
#79420 = LINE ( 'NONE', #23562, #83485 ) ;
#79421 = CIRCLE ( 'NONE', #5428, 13.49999999999999822 ) ;
#79422 = CARTESIAN_POINT ( 'NONE',  ( 106.4400806841681231, -45.24788313703638210, 221.9409912566479477 ) ) ;
#79423 = ORIENTED_EDGE ( 'NONE', *, *, #41478, .F. ) ;
#79424 = VERTEX_POINT ( 'NONE', #74470 ) ;
#79425 = ORIENTED_EDGE ( 'NONE', *, *, #7364, .F. ) ;
#79426 = AXIS2_PLACEMENT_3D ( 'NONE', #68703, #53241, #68262 ) ;
#79427 = EDGE_CURVE ( 'NONE', #34489, #1069, #76053, .T. ) ;
#79428 = DIRECTION ( 'NONE',  ( -0.9999999853157766072, -0.0001713722456143218888, 0.000000000000000000 ) ) ;
#79429 = CARTESIAN_POINT ( 'NONE',  ( -41.60202597009397607, 40.59999999999997300, 50.85338361873603219 ) ) ;
#79430 = CARTESIAN_POINT ( 'NONE',  ( 100.6687104580203567, -44.89077600156390702, 273.0594347997199520 ) ) ;
#79431 = FACE_OUTER_BOUND ( 'NONE', #79028, .T. ) ;
#79432 = CARTESIAN_POINT ( 'NONE',  ( 116.3149231129805941, -32.94053081170188335, 174.1356252759109680 ) ) ;
#79433 = CARTESIAN_POINT ( 'NONE',  ( 98.30750624414157812, -41.72880715729390744, 26.73978606779152756 ) ) ;
#79434 = ORIENTED_EDGE ( 'NONE', *, *, #59617, .F. ) ;
#79435 = CARTESIAN_POINT ( 'NONE',  ( 103.2943085291411478, -27.46819606563682470, 56.38426792498484730 ) ) ;
#79436 = ORIENTED_EDGE ( 'NONE', *, *, #65994, .F. ) ;
#79437 = CIRCLE ( 'NONE', #19967, 13.16666666666670160 ) ;
#79438 = LINE ( 'NONE', #78551, #33582 ) ;
#79439 = CARTESIAN_POINT ( 'NONE',  ( 115.1548909598205057, -41.51005587062507374, 279.8453928297065545 ) ) ;
#79440 = AXIS2_PLACEMENT_3D ( 'NONE', #4316, #66526, #32003 ) ;
#79441 = LINE ( 'NONE', #58953, #53647 ) ;
#79442 = CARTESIAN_POINT ( 'NONE',  ( 192.5667039024474434, -23.42844715993433624, 180.4678068554150343 ) ) ;
#79443 = EDGE_CURVE ( 'NONE', #8508, #85887, #79516, .T. ) ;
#79444 = LINE ( 'NONE', #51696, #9678 ) ;
#79445 = ORIENTED_EDGE ( 'NONE', *, *, #87182, .T. ) ;
#79446 = CARTESIAN_POINT ( 'NONE',  ( 72.96458098368701428, 127.0000000000000000, -80.10833098368678407 ) ) ;
#79447 = FACE_OUTER_BOUND ( 'NONE', #61342, .T. ) ;
#79448 = ADVANCED_FACE ( 'NONE', ( #67654 ), #5435, .F. ) ;
#79449 = VERTEX_POINT ( 'NONE', #51767 ) ;
#79450 = CARTESIAN_POINT ( 'NONE',  ( 113.4154522487949919, -27.68126056648907252, 84.57753003781698453 ) ) ;
#79451 = ORIENTED_EDGE ( 'NONE', *, *, #16283, .F. ) ;
#79452 = EDGE_CURVE ( 'NONE', #23895, #12725, #20944, .T. ) ;
#79453 = CARTESIAN_POINT ( 'NONE',  ( 106.1832117796525807, -28.23380338452170335, 49.58099125664799800 ) ) ;
#79454 = CARTESIAN_POINT ( 'NONE',  ( 116.7800429006774436, -34.22024395345221137, 90.02721173792870957 ) ) ;
#79455 = CARTESIAN_POINT ( 'NONE',  ( 117.0765951205083439, -35.60322954364740156, 80.34729759161096752 ) ) ;
#79456 = PLANE ( 'NONE',  #31714 ) ;
#79457 = ADVANCED_FACE ( 'NONE', ( #65851 ), #31338, .T. ) ;
#79458 = CARTESIAN_POINT ( 'NONE',  ( 31.75000000000000000, 24.56180297284579694, -3.174999999999999822 ) ) ;
#79459 = VECTOR ( 'NONE', #58440, 1000.000000000000000 ) ;
#79460 = CARTESIAN_POINT ( 'NONE',  ( 61.00843881761244347, 49.07499999999999574, -33.74458626278666884 ) ) ;
#79461 = CARTESIAN_POINT ( 'NONE',  ( 96.66758392153232649, -32.91525239269808623, 17.03467289495896964 ) ) ;
#79462 = CARTESIAN_POINT ( 'NONE',  ( 0.000000000000000000, 82.54999999999999716, 92.46299999999996544 ) ) ;
#79463 = ORIENTED_EDGE ( 'NONE', *, *, #9282, .T. ) ;
#79464 = CYLINDRICAL_SURFACE ( 'NONE', #15465, 1.999999999999995781 ) ;
#79465 = AXIS2_PLACEMENT_3D ( 'NONE', #23661, #86769, #37274 ) ;
#79466 = ORIENTED_EDGE ( 'NONE', *, *, #37990, .T. ) ;
#79467 = VECTOR ( 'NONE', #3293, 1000.000000000000000 ) ;
#79468 = CARTESIAN_POINT ( 'NONE',  ( 78.35735255114366282, -20.88611802719123389, 2.101554303218999831 ) ) ;
#79469 = ORIENTED_EDGE ( 'NONE', *, *, #28591, .F. ) ;
#79470 = ORIENTED_EDGE ( 'NONE', *, *, #19225, .T. ) ;
#79471 = EDGE_CURVE ( 'NONE', #2833, #4111, #60823, .T. ) ;
#79472 = DIRECTION ( 'NONE',  ( 0.000000000000000000, 1.000000000000000000, 0.000000000000000000 ) ) ;
#79473 = VECTOR ( 'NONE', #27583, 1000.000000000000000 ) ;
#79474 = CARTESIAN_POINT ( 'NONE',  ( 63.03715912545737865, -24.89890238295017966, 249.9678068554150343 ) ) ;
#79475 = CARTESIAN_POINT ( 'NONE',  ( 97.32398421004032230, -35.86507053846867166, 231.2556252759109725 ) ) ;
#79476 = DIRECTION ( 'NONE',  ( -0.000000000000000000, -0.000000000000000000, -1.000000000000000000 ) ) ;
#79477 = DIRECTION ( 'NONE',  ( 0.000000000000000000, 0.000000000000000000, 1.000000000000000000 ) ) ;
#79478 = CARTESIAN_POINT ( 'NONE',  ( 106.9273518165185948, -26.26990724610170247, 56.08705384733997334 ) ) ;
#79479 = CARTESIAN_POINT ( 'NONE',  ( 116.8171323280760276, -34.15294143710698904, 45.03145662157326967 ) ) ;
#79480 = ORIENTED_EDGE ( 'NONE', *, *, #42823, .F. ) ;
#79481 = CARTESIAN_POINT ( 'NONE',  ( 97.81170986510684884, -40.51745644794008427, 172.6354259520616097 ) ) ;
#79482 = CARTESIAN_POINT ( 'NONE',  ( 51.34673845256558167, -29.62846900982264842, 237.4678068554150059 ) ) ;
#79483 = EDGE_LOOP ( 'NONE', ( #44442, #26559 ) ) ;
#79484 = CIRCLE ( 'NONE', #35955, 3.000000000000002665 ) ;
#79485 = LINE ( 'NONE', #67163, #9697 ) ;
#79486 = CARTESIAN_POINT ( 'NONE',  ( 101.9927635143278621, -45.44554184246400297, 113.1570561696343447 ) ) ;
#79487 = CARTESIAN_POINT ( 'NONE',  ( 100.8363305107023251, -45.83159080358284854, 242.1108633711489517 ) ) ;
#79488 = CARTESIAN_POINT ( 'NONE',  ( 63.06670390244699576, -67.87844715994098976, 190.2178068554179902 ) ) ;
#79489 = CARTESIAN_POINT ( 'NONE',  ( 107.0667039024470313, -104.2784471599413791, 2.217806855418003043 ) ) ;
#79490 = CARTESIAN_POINT ( 'NONE',  ( 127.0667039024477560, -15.72944715994076681, 239.5838068554164408 ) ) ;
#79491 = CARTESIAN_POINT ( 'NONE',  ( 101.7992505034292350, -28.57304559719056058, 219.9552769709339657 ) ) ;
#79493 = CARTESIAN_POINT ( 'NONE',  ( 96.05879824974444148, -41.05137697672054742, 92.62419670448296927 ) ) ;
#79492 = CARTESIAN_POINT ( 'NONE',  ( 81.84766347661002328, -83.77844715994096703, 45.21780685541799727 ) ) ;
#79494 = CARTESIAN_POINT ( 'NONE',  ( 119.7619606472514135, 74.58858857478185200, 51.98495555578256955 ) ) ;
#79495 = CARTESIAN_POINT ( 'NONE',  ( 98.41978056949241704, -42.69487473605161654, 126.8070538473389490 ) ) ;
#79496 = VERTEX_POINT ( 'NONE', #14836 ) ;
#79497 = DIRECTION ( 'NONE',  ( 0.000000000000000000, 1.000000000000000000, 0.000000000000000000 ) ) ;
#79498 = ORIENTED_EDGE ( 'NONE', *, *, #32243, .F. ) ;
#79499 = CARTESIAN_POINT ( 'NONE',  ( 51.34673845256575930, -36.02818131005845004, 313.9678068554150059 ) ) ;
#79500 = FACE_OUTER_BOUND ( 'NONE', #42324, .T. ) ;
#79501 = CARTESIAN_POINT ( 'NONE',  ( 135.1485260852069530, -34.20116861175128520, 1.807989644435019416 ) ) ;
#79502 = VERTEX_POINT ( 'NONE', #49771 ) ;
#79503 = DIRECTION ( 'NONE',  ( 0.7071067811865774377, -0.7071067811865175967, 7.071067811865782003E-16 ) ) ;
#79504 = VERTEX_POINT ( 'NONE', #48867 ) ;
#79505 = DIRECTION ( 'NONE',  ( 7.570719237730591757E-15, 1.000000000000000000, 0.000000000000000000 ) ) ;
#79506 = DIRECTION ( 'NONE',  ( 0.7071067811575828532, -0.7071067812155121812, 0.000000000000000000 ) ) ;
#79507 = VECTOR ( 'NONE', #83244, 1000.000000000000000 ) ;
#79508 = EDGE_CURVE ( 'NONE', #77207, #14208, #7118, .T. ) ;
#79509 = CIRCLE ( 'NONE', #53320, 7.874000000000186184 ) ;
#79510 = LINE ( 'NONE', #25866, #69887 ) ;
#79511 = ORIENTED_EDGE ( 'NONE', *, *, #63136, .T. ) ;
#79512 = CARTESIAN_POINT ( 'NONE',  ( 96.06419827846988824, -38.01208726283962847, 86.43086337114897333 ) ) ;
#79514 = ADVANCED_FACE ( 'NONE', ( #56126, #36161 ), #81749, .T. ) ;
#79513 = CARTESIAN_POINT ( 'NONE',  ( 131.0667039024480118, -64.87844715994098976, 237.1838068554150141 ) ) ;
#79515 = DIRECTION ( 'NONE',  ( 1.000000000000000000, 0.000000000000000000, 0.000000000000000000 ) ) ;
#79516 = LINE ( 'NONE', #12242, #65923 ) ;
#79517 = ORIENTED_EDGE ( 'NONE', *, *, #58185, .F. ) ;
#79518 = VERTEX_POINT ( 'NONE', #8006 ) ;
#79519 = DIRECTION ( 'NONE',  ( 0.000000000000000000, 0.000000000000000000, -1.000000000000000000 ) ) ;
#79520 = CARTESIAN_POINT ( 'NONE',  ( -160.2664750769294812, 0.000000000000000000, -148.0533267522755807 ) ) ;
#79521 = CARTESIAN_POINT ( 'NONE',  ( -135.2444258376732193, 20.32000000000000028, -147.4575741623275746 ) ) ;
#79522 = CIRCLE ( 'NONE', #53335, 42.54500000000000171 ) ;
#79524 = LINE ( 'NONE', #65430, #28270 ) ;
#79523 = DIRECTION ( 'NONE',  ( 1.000000000000000078E-15, 0.000000000000000000, -1.000000000000000000 ) ) ;
#79525 = DIRECTION ( 'NONE',  ( 0.000000000000000000, 1.000000000000000000, 0.000000000000000000 ) ) ;
#79526 = VECTOR ( 'NONE', #9243, 1000.000000000000000 ) ;
#79527 = ORIENTED_EDGE ( 'NONE', *, *, #24465, .T. ) ;
#79529 = ADVANCED_FACE ( 'NONE', ( #29357 ), #77957, .F. ) ;
#79528 = AXIS2_PLACEMENT_3D ( 'NONE', #3969, #52969, #74799 ) ;
#79530 = PLANE ( 'NONE',  #37505 ) ;
#79531 = CARTESIAN_POINT ( 'NONE',  ( 117.1170091337236414, -34.17489915221372598, 165.0365776568629315 ) ) ;
#79533 = ORIENTED_EDGE ( 'NONE', *, *, #46360, .T. ) ;
#79532 = LINE ( 'NONE', #85012, #64616 ) ;
#79534 = VECTOR ( 'NONE', #70610, 1000.000000000000000 ) ;
#79535 = CARTESIAN_POINT ( 'NONE',  ( 114.3402351757609097, -43.26825200597433962, 34.24419670448197905 ) ) ;
#79536 = CARTESIAN_POINT ( 'NONE',  ( 160.5667039024483529, -48.82844715993552143, 300.4678068554149490 ) ) ;
#79537 = DIRECTION ( 'NONE',  ( 0.000000000000000000, 1.000000000000000000, 0.000000000000000000 ) ) ;
#79538 = DIRECTION ( 'NONE',  ( -4.237773401492740281E-14, 1.000000000000000000, 0.000000000000000000 ) ) ;
#79539 = AXIS2_PLACEMENT_3D ( 'NONE', #61082, #18860, #74279 ) ;
#79540 = VERTEX_POINT ( 'NONE', #22106 ) ;
#79541 = FACE_OUTER_BOUND ( 'NONE', #34083, .T. ) ;
#79542 = AXIS2_PLACEMENT_3D ( 'NONE', #55815, #6797, #888 ) ;
#79543 = CIRCLE ( 'NONE', #75185, 3.174999999999983391 ) ;
#79544 = VERTEX_POINT ( 'NONE', #15277 ) ;
#79545 = ORIENTED_EDGE ( 'NONE', *, *, #66302, .F. ) ;
#79546 = CARTESIAN_POINT ( 'NONE',  ( 113.7804517773139708, -30.94577135814159519, 180.8244404487539612 ) ) ;
#79547 = CARTESIAN_POINT ( 'NONE',  ( 91.91441891875203396, -96.57077177933014411, -21.78219314458226918 ) ) ;
#79548 = CARTESIAN_POINT ( 'NONE',  ( 105.0852382675896024, -45.91373775275845759, 28.85110711542093753 ) ) ;
#79549 = CARTESIAN_POINT ( 'NONE',  ( 23.04787079752263068, 87.28121659793244191, 303.5230764621404660 ) ) ;
#79550 = CARTESIAN_POINT ( 'NONE',  ( 99.09570908192057459, -30.55043174579301635, 80.80229194183452535 ) ) ;
#79551 = AXIS2_PLACEMENT_3D ( 'NONE', #79137, #71428, #8295 ) ;
#79552 = CARTESIAN_POINT ( 'NONE',  ( -103.1875000000000000, 117.4749999999999943, -1.080832317973422076E-12 ) ) ;
#79553 = ORIENTED_EDGE ( 'NONE', *, *, #70395, .T. ) ;
#79554 = PLANE ( 'NONE',  #55130 ) ;
#79555 = CARTESIAN_POINT ( 'NONE',  ( 50.88849390559467878, -32.11662333284566273, 237.4678068554150059 ) ) ;
#79556 = ORIENTED_EDGE ( 'NONE', *, *, #7078, .F. ) ;
#79557 = CARTESIAN_POINT ( 'NONE',  ( 100.1532602078032568, -44.50350736857021161, 266.9984824187679919 ) ) ;
#79558 = DIRECTION ( 'NONE',  ( 0.000000000000000000, -1.000000000000000000, 0.000000000000000000 ) ) ;
#79560 = ORIENTED_EDGE ( 'NONE', *, *, #4463, .T. ) ;
#79559 = EDGE_CURVE ( 'NONE', #50079, #74968, #57170, .T. ) ;
#79561 = FACE_BOUND ( 'NONE', #55561, .T. ) ;
#79562 = DIRECTION ( 'NONE',  ( -1.000000000000000000, 6.036837696399408848E-13, 0.000000000000000000 ) ) ;
#79563 = DIRECTION ( 'NONE',  ( 0.000000000000000000, 0.000000000000000000, 1.000000000000000000 ) ) ;
#79564 = CARTESIAN_POINT ( 'NONE',  ( 69.67078994678415427, -0.9293259921821603875, 540.9756252759101471 ) ) ;
#79565 = AXIS2_PLACEMENT_3D ( 'NONE', #23275, #51369, #71846 ) ;
#79566 = VECTOR ( 'NONE', #68348, 1000.000000000000000 ) ;
#79567 = CARTESIAN_POINT ( 'NONE',  ( 113.2457357650714727, -45.17988020286173878, 224.0784824187679476 ) ) ;
#79568 = CARTESIAN_POINT ( 'NONE',  ( 182.2420472961728137, -31.76306994223154589, 313.9678068554149490 ) ) ;
#79569 = ORIENTED_EDGE ( 'NONE', *, *, #73887, .T. ) ;
#79570 = CARTESIAN_POINT ( 'NONE',  ( 116.7853252867327996, -32.83880582269000570, 50.12991099019698282 ) ) ;
#79571 = FACE_OUTER_BOUND ( 'NONE', #57688, .T. ) ;
#79572 = CARTESIAN_POINT ( 'NONE',  ( 97.77253489752784787, -40.53345146323919579, 11.63562527591094309 ) ) ;
#79573 = VERTEX_POINT ( 'NONE', #53988 ) ;
#79574 = EDGE_CURVE ( 'NONE', #78870, #75109, #70687, .T. ) ;
#79575 = CARTESIAN_POINT ( 'NONE',  ( 80.25489464535442607, -15.97944715994106524, 1.625625275910945078 ) ) ;
#79577 = EDGE_CURVE ( 'NONE', #59850, #41003, #80411, .T. ) ;
#79576 = DIRECTION ( 'NONE',  ( 1.000000000000000000, 1.132880637372608296E-15, 0.000000000000000000 ) ) ;
#79578 = DIRECTION ( 'NONE',  ( -1.000000000000000078E-15, 1.000000000000000083E-30, 1.000000000000000000 ) ) ;
#79579 = CARTESIAN_POINT ( 'NONE',  ( 104.7498880507309451, -44.55652276380406818, 105.1652332267339602 ) ) ;
#79580 = CARTESIAN_POINT ( 'NONE',  ( 96.78746529907793672, -40.85582509469530521, 247.6422919425769749 ) ) ;
#79581 = LINE ( 'NONE', #32287, #14555 ) ;
#79582 = ORIENTED_EDGE ( 'NONE', *, *, #9319, .F. ) ;
#79583 = CIRCLE ( 'NONE', #62177, 7.143750000000001599 ) ;
#79584 = CARTESIAN_POINT ( 'NONE',  ( 136.3243469132048062, -38.30306751046402525, 2.518077574340959579 ) ) ;
#79585 = VERTEX_POINT ( 'NONE', #7566 ) ;
#79586 = ORIENTED_EDGE ( 'NONE', *, *, #4246, .F. ) ;
#79587 = VECTOR ( 'NONE', #72363, 1000.000000000000000 ) ;
#79588 = CONICAL_SURFACE ( 'NONE', #43310, 10.66800000000000992, 0.02993239667170383839 ) ;
#79589 = LINE ( 'NONE', #80933, #9631 ) ;
#79590 = ORIENTED_EDGE ( 'NONE', *, *, #60236, .F. ) ;
#79591 = EDGE_LOOP ( 'NONE', ( #88978, #70810, #49928, #69923 ) ) ;
#79592 = CARTESIAN_POINT ( 'NONE',  ( 99.04438571895173027, -42.84170729117609255, 167.8444702960626387 ) ) ;
#79593 = CARTESIAN_POINT ( 'NONE',  ( 107.0664832912739968, 0.2215528400590083269, 333.4006252759110112 ) ) ;
#79594 = CARTESIAN_POINT ( 'NONE',  ( 100.9546606413581458, -28.70703445851304991, 41.59391690566671684 ) ) ;
#79595 = CARTESIAN_POINT ( 'NONE',  ( 103.2107857629706018, -44.35110894017614669, 126.6267055423619610 ) ) ;
#79596 = CARTESIAN_POINT ( 'NONE',  ( 99.73113825573250324, -44.24905506706784308, 21.96133956162593748 ) ) ;
#79597 = VECTOR ( 'NONE', #69727, 1000.000000000000000 ) ;
#79598 = CARTESIAN_POINT ( 'NONE',  ( -8.690912999409459161, 73.28018275885442279, 130.2667388509219677 ) ) ;
#79599 = ORIENTED_EDGE ( 'NONE', *, *, #49028, .F. ) ;
#79600 = AXIS2_PLACEMENT_3D ( 'NONE', #27905, #55583, #49684 ) ;
#79601 = CARTESIAN_POINT ( 'NONE',  ( 176.7669697523291461, -48.62818131005361977, 249.9678068554149775 ) ) ;
#79602 = ORIENTED_EDGE ( 'NONE', *, *, #36074, .T. ) ;
#79603 = DIRECTION ( 'NONE',  ( 2.900000000000000265E-14, -2.000000000000000155E-15, 1.000000000000000000 ) ) ;
#79604 = AXIS2_PLACEMENT_3D ( 'NONE', #15263, #57476, #56577 ) ;
#79605 = CARTESIAN_POINT ( 'NONE',  ( 116.7945501114407278, -39.38987908835133567, 33.61483829906352838 ) ) ;
#79606 = CARTESIAN_POINT ( 'NONE',  ( 102.3035641816324102, -119.0284471599421181, -21.78219314458157285 ) ) ;
#79607 = DIRECTION ( 'NONE',  ( 0.7071067811865779928, -0.7071067811865171526, 7.071067811865785947E-16 ) ) ;
#79608 = ORIENTED_EDGE ( 'NONE', *, *, #85477, .F. ) ;
#79609 = CARTESIAN_POINT ( 'NONE',  ( 117.4915365000037042, -36.80222117025145678, 263.8213395616251660 ) ) ;
#79610 = CARTESIAN_POINT ( 'NONE',  ( 110.2975601020867202, -46.68703778808450267, 8.827053847339950465 ) ) ;
#79611 = SHAPE_REPRESENTATION_RELATIONSHIP ( 'NONE' , 'NONE' ,  #19449, #28324 ) ;
#79614 = ADVANCED_FACE ( 'NONE', ( #49325 ), #26316, .F. ) ;
#79613 = DIRECTION ( 'NONE',  ( -1.000000000000000000, 0.000000000000000000, 0.000000000000000000 ) ) ;
#79612 = DIRECTION ( 'NONE',  ( 0.000000000000000000, 0.000000000000000000, -1.000000000000000000 ) ) ;
#79615 = CARTESIAN_POINT ( 'NONE',  ( 105.6195873783703831, -25.36179723890650450, 323.1871736463168645 ) ) ;
#79616 = CARTESIAN_POINT ( 'NONE',  ( 49.21213752016101495, -29.73316016639650172, -5.074374724088000832 ) ) ;
#79617 = CARTESIAN_POINT ( 'NONE',  ( 131.6545875264125129, -38.05177997655169264, 7.178113714837632386 ) ) ;
#79618 = VECTOR ( 'NONE', #79927, 1000.000000000000000 ) ;
#79619 = DIRECTION ( 'NONE',  ( 1.000000000000000000, 0.000000000000000000, 0.000000000000000000 ) ) ;
#79620 = FACE_BOUND ( 'NONE', #47582, .T. ) ;
#79621 = CARTESIAN_POINT ( 'NONE',  ( 34.33598329127499227, -36.32844715994100682, -5.074374724088000832 ) ) ;
#79622 = CARTESIAN_POINT ( 'NONE',  ( 112.2192032947272509, -26.89661630634724432, 14.68038718067299442 ) ) ;
#79623 = CARTESIAN_POINT ( 'NONE',  ( 114.3439067968150624, -29.21543093042305728, 170.4641967044829585 ) ) ;
#79624 = CARTESIAN_POINT ( 'NONE',  ( 115.7467025339723250, -43.60978142820201242, 44.30514908543492680 ) ) ;
#79626 = DIRECTION ( 'NONE',  ( 1.000000000000000000, 3.999999999999999995E-14, 1.000000000000000078E-15 ) ) ;
#79625 = CARTESIAN_POINT ( 'NONE',  ( 167.2371591254545535, -47.82818131005522133, 129.9678068554149775 ) ) ;
#79627 = CYLINDRICAL_SURFACE ( 'NONE', #45016, 3.250000000000002665 ) ;
#79628 = VECTOR ( 'NONE', #17194, 1000.000000000000000 ) ;
#79629 = EDGE_CURVE ( 'NONE', #89037, #28914, #71145, .T. ) ;
#79630 = ORIENTED_EDGE ( 'NONE', *, *, #52956, .T. ) ;
#79631 = EDGE_CURVE ( 'NONE', #52525, #13042, #84777, .T. ) ;
#79632 = CARTESIAN_POINT ( 'NONE',  ( 108.4174892967461403, -26.73503593441724391, 185.9689586056932740 ) ) ;
#79633 = EDGE_LOOP ( 'NONE', ( #55818, #41168, #44890, #2675 ) ) ;
#79634 = CARTESIAN_POINT ( 'NONE',  ( 97.30000116515917341, -37.25789978020652171, 72.36991099019596163 ) ) ;
#79635 = EDGE_CURVE ( 'NONE', #39084, #27685, #32523, .T. ) ;
#79637 = VERTEX_POINT ( 'NONE', #69790 ) ;
#79636 = CARTESIAN_POINT ( 'NONE',  ( 4.851269734593515182, 94.28692116364298670, 130.4658362704004730 ) ) ;
#79638 = CARTESIAN_POINT ( 'NONE',  ( 105.7151186495713944, -46.72380402441561387, 48.46893004826933549 ) ) ;
#79639 = CARTESIAN_POINT ( 'NONE',  ( 103.3114313307234085, -27.02747569519259230, 211.3699109901969848 ) ) ;
#79640 = DIRECTION ( 'NONE',  ( 0.000000000000000000, 0.000000000000000000, 1.000000000000000000 ) ) ;
#79641 = CARTESIAN_POINT ( 'NONE',  ( 108.3332376935612871, -46.73488331510854010, 147.6773181741651513 ) ) ;
#79642 = DIRECTION ( 'NONE',  ( 3.100000000000000258E-29, -3.100000000000000044E-14, -1.000000000000000000 ) ) ;
#79643 = CARTESIAN_POINT ( 'NONE',  ( 151.0371591254575492, -24.95799193692592155, 180.4678068554149775 ) ) ;
#79644 = ADVANCED_FACE ( 'NONE', ( #74919 ), #40386, .T. ) ;
#79645 = AXIS2_PLACEMENT_3D ( 'NONE', #56450, #56907, #84643 ) ;
#79646 = ADVANCED_FACE ( 'NONE', ( #77058, #15726 ), #33130, .F. ) ;
#79647 = CARTESIAN_POINT ( 'NONE',  ( 145.3020554092476857, -139.4430956531403183, 245.6798494796449859 ) ) ;
#79648 = CARTESIAN_POINT ( 'NONE',  ( 107.0664832912739968, -36.72944715994100306, 287.6356252759109680 ) ) ;
#79649 = CARTESIAN_POINT ( 'NONE',  ( 113.6473777113568531, -44.00994186338857617, 133.1613395616259936 ) ) ;
#79650 = EDGE_LOOP ( 'NONE', ( #8116, #74814, #48077, #74903 ) ) ;
#79651 = ORIENTED_EDGE ( 'NONE', *, *, #48026, .F. ) ;
#79652 = EDGE_CURVE ( 'NONE', #52534, #7158, #65986, .T. ) ;
#79653 = VECTOR ( 'NONE', #314, 1000.000000000000000 ) ;
#79654 = CARTESIAN_POINT ( 'NONE',  ( 104.3250142303409831, -45.18796221723782480, 78.75872616303996665 ) ) ;
#79655 = AXIS2_PLACEMENT_3D ( 'NONE', #48126, #83140, #902 ) ;
#79656 = CARTESIAN_POINT ( 'NONE',  ( 107.0664832912739541, -23.22944715994095688, 315.6356252759111953 ) ) ;
#79658 = DIRECTION ( 'NONE',  ( 0.000000000000000000, 0.000000000000000000, -1.000000000000000000 ) ) ;
#79657 = CARTESIAN_POINT ( 'NONE',  ( 114.7458293810856418, -30.61868467657538062, 240.3613395616249875 ) ) ;
#79659 = CARTESIAN_POINT ( 'NONE',  ( -46.60773131249376888, 65.60000000000000853, -44.42500552774628630 ) ) ;
#79660 = EDGE_CURVE ( 'NONE', #22927, #31607, #34021, .T. ) ;
#79661 = DIRECTION ( 'NONE',  ( 1.000000000000000000, 0.000000000000000000, 0.000000000000000000 ) ) ;
#79662 = CARTESIAN_POINT ( 'NONE',  ( 118.4231949783269897, 71.15456258041355397, -5.621971333129370585 ) ) ;
#79663 = AXIS2_PLACEMENT_3D ( 'NONE', #559, #36882, #70060 ) ;
#79664 = DIRECTION ( 'NONE',  ( 0.000000000000000000, 0.000000000000000000, -1.000000000000000000 ) ) ;
#79665 = DIRECTION ( 'NONE',  ( -1.000000000000000000, -6.514610998690690188E-14, -1.000000000000000078E-15 ) ) ;
#79666 = FACE_OUTER_BOUND ( 'NONE', #41075, .T. ) ;
#79667 = CARTESIAN_POINT ( 'NONE',  ( 117.1049515565469221, -33.87427183379790563, 149.0470538473389581 ) ) ;
#79668 = ORIENTED_EDGE ( 'NONE', *, *, #52220, .F. ) ;
#79670 = ORIENTED_EDGE ( 'NONE', *, *, #84789, .T. ) ;
#79669 = ADVANCED_FACE ( 'NONE', ( #85671 ), #86556, .T. ) ;
#79671 = CIRCLE ( 'NONE', #1329, 2.030000000001310312 ) ;
#79672 = FACE_OUTER_BOUND ( 'NONE', #81460, .T. ) ;
#79673 = CARTESIAN_POINT ( 'NONE',  ( 115.8254323941762891, -31.73001883427092196, 150.2397919421048300 ) ) ;
#79674 = AXIS2_PLACEMENT_3D ( 'NONE', #70219, #7991, #78399 ) ;
#79675 = CARTESIAN_POINT ( 'NONE',  ( 194.0371591254572934, -24.89890238294407965, 300.4678068554149490 ) ) ;
#79676 = DIRECTION ( 'NONE',  ( 9.351236661543306751E-17, -3.725950533538267725E-29, -1.000000000000000000 ) ) ;
#79677 = CARTESIAN_POINT ( 'NONE',  ( 115.0372528418681242, -42.90846878759241179, 269.3022913304283747 ) ) ;
#79678 = CARTESIAN_POINT ( 'NONE',  ( 117.4575111195971857, -40.49848259682686802, 173.5375300378159693 ) ) ;
#79679 = CARTESIAN_POINT ( 'NONE',  ( 136.1600792929918953, -38.51483178663133344, 7.477467810854448338 ) ) ;
#79680 = VERTEX_POINT ( 'NONE', #16175 ) ;
#79682 = ORIENTED_EDGE ( 'NONE', *, *, #21315, .T. ) ;
#79681 = ORIENTED_EDGE ( 'NONE', *, *, #19324, .F. ) ;
#79683 = CIRCLE ( 'NONE', #21657, 11.45913725231036118 ) ;
#79684 = EDGE_CURVE ( 'NONE', #43506, #56405, #50673, .T. ) ;
#79685 = CARTESIAN_POINT ( 'NONE',  ( 100.1576839525979352, -44.03386264563039987, 62.97446275362836587 ) ) ;
#79687 = EDGE_CURVE ( 'NONE', #9211, #82640, #39856, .T. ) ;
#79686 = DIRECTION ( 'NONE',  ( 1.000000000000000078E-15, -1.000000000000000083E-30, -1.000000000000000000 ) ) ;
#79688 = CARTESIAN_POINT ( 'NONE',  ( 132.9844404253386472, -34.20116865955331065, 8.043260881866558520 ) ) ;
#79689 = EDGE_CURVE ( 'NONE', #1932, #59530, #10239, .T. ) ;
#79690 = CARTESIAN_POINT ( 'NONE',  ( 100.5340721669357009, -30.74146890971161739, 272.1672975916113160 ) ) ;
#79691 = DIRECTION ( 'NONE',  ( 0.000000000000000000, 1.000000000000000000, 0.000000000000000000 ) ) ;
#79692 = VERTEX_POINT ( 'NONE', #16614 ) ;
#79693 = ADVANCED_FACE ( 'NONE', ( #57938 ), #18073, .F. ) ;
#79694 = CARTESIAN_POINT ( 'NONE',  ( 114.6673900882561554, -41.57871802750004520, 9.635625275910941312 ) ) ;
#79695 = VECTOR ( 'NONE', #77528, 1000.000000000000000 ) ;
#79696 = CARTESIAN_POINT ( 'NONE',  ( 131.3179999999999836, 37.33800000000000097, 50.79999999999999716 ) ) ;
#79697 = VERTEX_POINT ( 'NONE', #22997 ) ;
#79698 = ORIENTED_EDGE ( 'NONE', *, *, #84700, .F. ) ;
#79699 = CARTESIAN_POINT ( 'NONE',  ( 116.3212776292296127, -32.94146857471318413, 287.6356252759109680 ) ) ;
#79700 = ORIENTED_EDGE ( 'NONE', *, *, #88459, .T. ) ;
#79701 = VERTEX_POINT ( 'NONE', #29797 ) ;
#79702 = CARTESIAN_POINT ( 'NONE',  ( 109.7226905202563501, -27.00022865876924172, 155.8647339722907645 ) ) ;
#79703 = CARTESIAN_POINT ( 'NONE',  ( 98.56427472769081533, -33.61093641167653345, 20.45718173283900398 ) ) ;
#79704 = CARTESIAN_POINT ( 'NONE',  ( 113.0348518357461955, -45.34727401701223926, 203.0584824187679374 ) ) ;
#79705 = CARTESIAN_POINT ( 'NONE',  ( 117.2167691715783064, -39.01263929987995027, 148.6499109901969859 ) ) ;
#79706 = PLANE ( 'NONE',  #32189 ) ;
#79707 = CARTESIAN_POINT ( 'NONE',  ( 99.38154727845876835, -29.68499927947409489, 271.7356252759109907 ) ) ;
#79708 = DIRECTION ( 'NONE',  ( -4.163336342344333240E-14, -1.000000000000000000, 0.000000000000000000 ) ) ;
#79709 = FACE_OUTER_BOUND ( 'NONE', #45092, .T. ) ;
#79710 = ORIENTED_EDGE ( 'NONE', *, *, #3984, .T. ) ;
#79711 = VECTOR ( 'NONE', #34803, 1000.000000000000000 ) ;
#79712 = VERTEX_POINT ( 'NONE', #86996 ) ;
#79713 = VECTOR ( 'NONE', #229, 1000.000000000000000 ) ;
#79714 = CARTESIAN_POINT ( 'NONE',  ( 97.72299786849482928, -41.53060059208619492, 196.7041967044819728 ) ) ;
#79715 = EDGE_LOOP ( 'NONE', ( #56061, #22968 ) ) ;
#79716 = CARTESIAN_POINT ( 'NONE',  ( 102.6834449319766378, -27.27027144519976787, 180.4213395616249898 ) ) ;
#79717 = CARTESIAN_POINT ( 'NONE',  ( 102.0662944402908749, -27.97094399341936821, 265.4898263988108624 ) ) ;
#79718 = DIRECTION ( 'NONE',  ( 0.000000000000000000, 0.000000000000000000, -1.000000000000000000 ) ) ;
#79719 = CARTESIAN_POINT ( 'NONE',  ( 100.1253875378072848, -39.57043109886186727, 9.635625275910941312 ) ) ;
#79720 = DIRECTION ( 'NONE',  ( 0.000000000000000000, -0.000000000000000000, 1.000000000000000000 ) ) ;
#79723 = CARTESIAN_POINT ( 'NONE',  ( 113.7419942178972576, -29.10023054337259296, 285.5032443235299979 ) ) ;
#79722 = DIRECTION ( 'NONE',  ( 0.000000000000000000, 0.000000000000000000, 1.000000000000000000 ) ) ;
#79721 = DIRECTION ( 'NONE',  ( -3.100000000000000258E-29, 3.100000000000000044E-14, 1.000000000000000000 ) ) ;
#79724 = CARTESIAN_POINT ( 'NONE',  ( 41.56648329127399677, 0.2215528400590013880, 16.80862527591200006 ) ) ;
#79725 = DIRECTION ( 'NONE',  ( -1.000000000000000000, 0.000000000000000000, 0.000000000000000000 ) ) ;
#79726 = CARTESIAN_POINT ( 'NONE',  ( 25.56670390244797275, -65.37844715994100397, 293.2178068554150627 ) ) ;
#79727 = CIRCLE ( 'NONE', #40534, 3.000000000000002665 ) ;
#79728 = CARTESIAN_POINT ( 'NONE',  ( 68.08801065749622694, -137.1506278873062286, 247.2512423094629810 ) ) ;
#79729 =( GEOMETRIC_REPRESENTATION_CONTEXT ( 3 ) GLOBAL_UNCERTAINTY_ASSIGNED_CONTEXT ( ( #56901 ) ) GLOBAL_UNIT_ASSIGNED_CONTEXT ( ( #69550, #21405, #76810 ) ) REPRESENTATION_CONTEXT ( 'NONE', 'WORKASPACE' ) );
#79730 = DIRECTION ( 'NONE',  ( -1.000000000000000000, 0.000000000000000000, 0.000000000000000000 ) ) ;
#79731 = CARTESIAN_POINT ( 'NONE',  ( 127.0664832912740394, -46.72944715994101017, -4.824374724089008915 ) ) ;
#79733 = ORIENTED_EDGE ( 'NONE', *, *, #46536, .T. ) ;
#79732 = CARTESIAN_POINT ( 'NONE',  ( 101.7839708215018106, -42.86206951696545531, 195.5838068554171798 ) ) ;
#79734 = CARTESIAN_POINT ( 'NONE',  ( 136.5146477271300682, -19.98222059078257473, 7.138441653512620277 ) ) ;
#79735 = CARTESIAN_POINT ( 'NONE',  ( 117.4357963365922615, -35.45519799489562729, 193.9241967044829664 ) ) ;
#79736 = CARTESIAN_POINT ( 'NONE',  ( 116.2315886754559386, -31.76121500512346074, 65.22133956162595325 ) ) ;
#79737 = CARTESIAN_POINT ( 'NONE',  ( 103.8062037941931095, -48.17417041148343060, 213.3556252759109668 ) ) ;
#79738 = DIRECTION ( 'NONE',  ( 1.000000000000000078E-15, -1.000000000000000083E-30, -1.000000000000000000 ) ) ;
#79739 = CIRCLE ( 'NONE', #31851, 7.143750000000004263 ) ;
#79740 = CARTESIAN_POINT ( 'NONE',  ( 83.06670390244804025, -42.97311385574013798, 207.5838068554169809 ) ) ;
#79742 = CARTESIAN_POINT ( 'NONE',  ( 109.7368013281214445, -46.41511743547308555, 38.79047438361208577 ) ) ;
#79741 = DIRECTION ( 'NONE',  ( 0.000000000000000000, 0.000000000000000000, 1.000000000000000000 ) ) ;
#79743 = FACE_OUTER_BOUND ( 'NONE', #531, .T. ) ;
#79744 = DIRECTION ( 'NONE',  ( 1.000000000000000000, 1.000000000000000078E-15, 0.000000000000000000 ) ) ;
#79745 = CARTESIAN_POINT ( 'NONE',  ( 104.4917770246300535, -26.97830201417560403, 65.28281118898505042 ) ) ;
#79746 = EDGE_LOOP ( 'NONE', ( #8482, #45618, #51727, #14441 ) ) ;
#79747 = EDGE_CURVE ( 'NONE', #61299, #37060, #71591, .T. ) ;
#79748 = EDGE_LOOP ( 'NONE', ( #34452, #18533, #34987, #18561, #42227 ) ) ;
#79749 = CIRCLE ( 'NONE', #33299, 3.968749999999992895 ) ;
#79750 = CARTESIAN_POINT ( 'NONE',  ( 112.1857315011839802, -29.85591823435125747, 103.9895626852199655 ) ) ;
#79751 = ADVANCED_FACE ( 'NONE', ( #64759 ), #31116, .T. ) ;
#79753 = ORIENTED_EDGE ( 'NONE', *, *, #47618, .T. ) ;
#79752 = CARTESIAN_POINT ( 'NONE',  ( -12.69999999999999929, 83.38939070830898004, -129.9368274816650342 ) ) ;
#79754 = CARTESIAN_POINT ( 'NONE',  ( 98.35456548258461851, -42.41549619454038123, 97.78705384733993355 ) ) ;
#79755 = LINE ( 'NONE', #51996, #22340 ) ;
#79756 = DIRECTION ( 'NONE',  ( -3.100000000000000258E-29, 3.100000000000000044E-14, 1.000000000000000000 ) ) ;
#79757 = EDGE_CURVE ( 'NONE', #63429, #36556, #23449, .T. ) ;
#79758 = EDGE_CURVE ( 'NONE', #44882, #2509, #13877, .T. ) ;
#79759 = CARTESIAN_POINT ( 'NONE',  ( 107.0667039024479834, -36.72944715994100306, 239.5838068554170093 ) ) ;
#79760 = CARTESIAN_POINT ( 'NONE',  ( 110.3395589168170972, -45.98151452052003663, 37.84705384733994293 ) ) ;
#79761 = ORIENTED_EDGE ( 'NONE', *, *, #69808, .F. ) ;
#79762 = AXIS2_PLACEMENT_3D ( 'NONE', #78328, #2458, #30602 ) ;
#79763 = EDGE_LOOP ( 'NONE', ( #86709, #65925, #22361, #47662 ) ) ;
#79764 = VERTEX_POINT ( 'NONE', #4762 ) ;
#79765 = ADVANCED_FACE ( 'NONE', ( #39277 ), #68334, .F. ) ;
#79766 = DIRECTION ( 'NONE',  ( 0.000000000000000000, 1.000000000000000000, 0.000000000000000000 ) ) ;
#79767 = CARTESIAN_POINT ( 'NONE',  ( 73.10937651008742932, -46.62589376934775487, -5.074374724089109279 ) ) ;
#79768 = DIRECTION ( 'NONE',  ( 0.000000000000000000, -1.000000000000000000, 0.000000000000000000 ) ) ;
#79769 = DIRECTION ( 'NONE',  ( 0.000000000000000000, 0.000000000000000000, 1.000000000000000000 ) ) ;
#79770 = CARTESIAN_POINT ( 'NONE',  ( 50.96943157743499597, -34.03355364505720360, -5.074374724088000832 ) ) ;
#79771 = EDGE_CURVE ( 'NONE', #61198, #11064, #60146, .T. ) ;
#79772 = CARTESIAN_POINT ( 'NONE',  ( 116.3181333158508295, -32.94392590426259204, 50.13562527591097506 ) ) ;
#79773 = DIRECTION ( 'NONE',  ( 1.000000000000000000, 4.163336342344333240E-14, 0.000000000000000000 ) ) ;
#79774 = CIRCLE ( 'NONE', #34744, 2.500000000000002220 ) ;
#79775 = CARTESIAN_POINT ( 'NONE',  ( -5.017381069699506924, 94.21703938470614048, 130.4595628991474143 ) ) ;
#79776 = CARTESIAN_POINT ( 'NONE',  ( 103.4847015977353379, -25.45917443855071838, 55.32133956162594046 ) ) ;
#79777 = ORIENTED_EDGE ( 'NONE', *, *, #41869, .T. ) ;
#79779 = VERTEX_POINT ( 'NONE', #6114 ) ;
#79778 = EDGE_CURVE ( 'NONE', #28741, #24002, #87881, .T. ) ;
#79780 = CIRCLE ( 'NONE', #2865, 4.875000000000017764 ) ;
#79781 = DIRECTION ( 'NONE',  ( 1.000000000000000000, 4.163336342344333240E-14, 0.000000000000000000 ) ) ;
#79782 = CARTESIAN_POINT ( 'NONE',  ( 163.0667039024466760, -32.29483332967941323, 237.4678068554150059 ) ) ;
#79783 = DIRECTION ( 'NONE',  ( 0.000000000000000000, -1.000000000000000000, 0.000000000000000000 ) ) ;
#79784 = CARTESIAN_POINT ( 'NONE',  ( 103.9214495108435017, -28.66658863671924706, 168.1785665600669688 ) ) ;
#79785 = ADVANCED_FACE ( 'NONE', ( #74256 ), #40618, .F. ) ;
#79786 = AXIS2_PLACEMENT_3D ( 'NONE', #51528, #44718, #86973 ) ;
#79787 = CIRCLE ( 'NONE', #40586, 3.499999999999996003 ) ;
#79788 = LINE ( 'NONE', #53363, #41627 ) ;
#79789 = ORIENTED_EDGE ( 'NONE', *, *, #70642, .T. ) ;
#79790 = VERTEX_POINT ( 'NONE', #18837 ) ;
#79791 = AXIS2_PLACEMENT_3D ( 'NONE', #42335, #22827, #50955 ) ;
#79792 = CARTESIAN_POINT ( 'NONE',  ( 127.0664832912740394, -54.72944906728950798, -5.074374724089008915 ) ) ;
#79793 = EDGE_LOOP ( 'NONE', ( #56735, #70507, #50575, #57735 ) ) ;
#79794 = VERTEX_POINT ( 'NONE', #89233 ) ;
#79795 = FACE_OUTER_BOUND ( 'NONE', #27509, .T. ) ;
#79796 = ADVANCED_FACE ( 'NONE', ( #12029 ), #5208, .F. ) ;
#79797 = CARTESIAN_POINT ( 'NONE',  ( 109.0147404159584568, -27.53810233378435157, 181.3539642582779550 ) ) ;
#79798 = LINE ( 'NONE', #81589, #51582 ) ;
#79799 = CIRCLE ( 'NONE', #15992, 15.00000000000000000 ) ;
#79800 = EDGE_CURVE ( 'NONE', #89348, #14315, #42014, .T. ) ;
#79801 = CARTESIAN_POINT ( 'NONE',  ( 164.7812970173289955, -35.65087443492610930, -5.074374724088000832 ) ) ;
#79802 = CARTESIAN_POINT ( 'NONE',  ( 100.8872678004313457, -44.70005588500947624, 17.05233985846918898 ) ) ;
#79803 = ORIENTED_EDGE ( 'NONE', *, *, #22516, .F. ) ;
#79804 = ORIENTED_EDGE ( 'NONE', *, *, #62778, .T. ) ;
#79805 = ORIENTED_EDGE ( 'NONE', *, *, #18652, .F. ) ;
#79806 = CIRCLE ( 'NONE', #68191, 8.928099999999993486 ) ;
#79807 = CARTESIAN_POINT ( 'NONE',  ( 104.1201707603140107, -29.11702517433068138, 213.1880903695919756 ) ) ;
#79808 = CARTESIAN_POINT ( 'NONE',  ( 117.3753987692272602, -38.63066374137464720, 88.68133956162493803 ) ) ;
#79809 = CARTESIAN_POINT ( 'NONE',  ( 117.4328057974123567, -37.95573561897359838, 53.73276813305394484 ) ) ;
#79810 = CARTESIAN_POINT ( 'NONE',  ( 101.9926078131534979, -45.44544624334183425, 252.1566658911062007 ) ) ;
#79811 = CARTESIAN_POINT ( 'NONE',  ( 134.5667039024480118, -50.82844715994100682, 104.9178068554150087 ) ) ;
#79812 = DIRECTION ( 'NONE',  ( 0.000000000000000000, 0.000000000000000000, -1.000000000000000000 ) ) ;
#79813 = CARTESIAN_POINT ( 'NONE',  ( 96.61884675261427446, -36.21154414529181764, 167.2870538473399620 ) ) ;
#79814 = DIRECTION ( 'NONE',  ( 1.000000000000000078E-15, -1.000000000000000083E-30, -1.000000000000000000 ) ) ;
#79815 = EDGE_LOOP ( 'NONE', ( #32393, #57049, #72237, #51054 ) ) ;
#79816 = DIRECTION ( 'NONE',  ( 0.000000000000000000, 0.000000000000000000, -1.000000000000000000 ) ) ;
#79817 = ORIENTED_EDGE ( 'NONE', *, *, #38592, .T. ) ;
#79818 = ORIENTED_EDGE ( 'NONE', *, *, #52082, .T. ) ;
#79819 = LINE ( 'NONE', #17574, #1285 ) ;
#79820 = CARTESIAN_POINT ( 'NONE',  ( 57.14999999999999858, 60.86974387893089755, 300.8629999999999995 ) ) ;
#79822 = EDGE_LOOP ( 'NONE', ( #51599, #48908, #1834, #85365, #89921, #23946, #26261, #5836 ) ) ;
#79821 = CIRCLE ( 'NONE', #37736, 118.5560000000000116 ) ;
#79823 = ADVANCED_FACE ( 'NONE', ( #20188 ), #52858, .F. ) ;
#79824 = CARTESIAN_POINT ( 'NONE',  ( 111.8298436232616240, -89.52844715994213232, -21.78219314458246103 ) ) ;
#79825 = ORIENTED_EDGE ( 'NONE', *, *, #48335, .T. ) ;
#79826 = CARTESIAN_POINT ( 'NONE',  ( 100.8874678597574785, -44.70022135617958980, 177.0522919403976232 ) ) ;
#79827 = CARTESIAN_POINT ( 'NONE',  ( 96.19295485998075890, -38.71576710077270889, 51.48229194257797303 ) ) ;
#79828 = FACE_BOUND ( 'NONE', #51158, .T. ) ;
#79829 = LINE ( 'NONE', #74337, #17354 ) ;
#79830 = CARTESIAN_POINT ( 'NONE',  ( 80.06648329127399677, 0.2215528400590013880, 306.1181252759120071 ) ) ;
#79831 = CARTESIAN_POINT ( 'NONE',  ( 104.3903674582245742, -25.93822912171379969, 90.26991099019693365 ) ) ;
#79833 = CARTESIAN_POINT ( 'NONE',  ( 103.0581626738562306, -26.45339789934171293, 166.3603871806729444 ) ) ;
#79832 = DIRECTION ( 'NONE',  ( -4.237773401492740281E-14, 1.000000000000000000, 0.000000000000000000 ) ) ;
#79834 = DIRECTION ( 'NONE',  ( 0.000000000000000000, -1.000000000000000000, 0.000000000000000000 ) ) ;
#79835 = CARTESIAN_POINT ( 'NONE',  ( -487.2989999999999782, 93.66249999999999432, 95.25000000000000000 ) ) ;
#79836 = VERTEX_POINT ( 'NONE', #11118 ) ;
#79837 = LINE ( 'NONE', #10760, #1952 ) ;
#79838 = AXIS2_PLACEMENT_3D ( 'NONE', #72616, #22687, #50359 ) ;
#79839 = DIRECTION ( 'NONE',  ( 0.000000000000000000, 1.000000000000000000, 0.000000000000000000 ) ) ;
#79840 = CARTESIAN_POINT ( 'NONE',  ( 97.80867505543230322, -40.51006205963207663, 136.6353762839628985 ) ) ;
#79841 = AXIS2_PLACEMENT_3D ( 'NONE', #34130, #81427, #20077 ) ;
#79842 = DIRECTION ( 'NONE',  ( 0.000000000000000000, 0.000000000000000000, -1.000000000000000000 ) ) ;
#79844 = ORIENTED_EDGE ( 'NONE', *, *, #32316, .F. ) ;
#79843 = CARTESIAN_POINT ( 'NONE',  ( 106.8507020815961397, -47.82747951245497831, 227.5489586092439538 ) ) ;
#79845 = DIRECTION ( 'NONE',  ( 1.000000000000000000, 0.000000000000000000, 1.047445008332812253E-14 ) ) ;
#79846 = CARTESIAN_POINT ( 'NONE',  ( 115.2688234373398046, -30.20251741173218818, 240.3613395616249875 ) ) ;
#79847 = CARTESIAN_POINT ( 'NONE',  ( 97.53157056845665807, -31.04763954905634193, 126.9108633711489915 ) ) ;
#79848 = CARTESIAN_POINT ( 'NONE',  ( 109.7287935134955035, -27.00184743278844124, 250.8695244108087365 ) ) ;
#79849 = CARTESIAN_POINT ( 'NONE',  ( 82.26793483429604237, -38.38027623202342653, 7.385026757020076715 ) ) ;
#79850 = EDGE_CURVE ( 'NONE', #4517, #18229, #18379, .T. ) ;
#79851 = DIRECTION ( 'NONE',  ( 0.000000000000000000, 1.000000000000000000, 0.000000000000000000 ) ) ;
#79852 = CARTESIAN_POINT ( 'NONE',  ( 177.3246001664174969, -48.34074026909178912, 180.4678068554150059 ) ) ;
#79853 = VERTEX_POINT ( 'NONE', #28318 ) ;
#79854 = VECTOR ( 'NONE', #4073, 1000.000000000000000 ) ;
#79855 = ADVANCED_FACE ( 'NONE', ( #76033 ), #6998, .T. ) ;
#79856 = VERTEX_POINT ( 'NONE', #34244 ) ;
#79857 = ADVANCED_FACE ( 'NONE', ( #21076 ), #75602, .F. ) ;
#79858 = EDGE_LOOP ( 'NONE', ( #26763, #9210, #49154, #5338, #452 ) ) ;
#79859 = CIRCLE ( 'NONE', #40661, 12.70000000000000107 ) ;
#79860 = EDGE_CURVE ( 'NONE', #40430, #70137, #27433, .T. ) ;
#79861 = EDGE_LOOP ( 'NONE', ( #9982, #71706, #57195, #40331 ) ) ;
#79862 = FACE_OUTER_BOUND ( 'NONE', #70250, .T. ) ;
#79863 = CARTESIAN_POINT ( 'NONE',  ( 105.1090458072749527, -25.85091697680629608, 271.2061014663872243 ) ) ;
#79864 = CARTESIAN_POINT ( 'NONE',  ( 167.6524903400755875, -49.32844715993520879, 180.4678068554150059 ) ) ;
#79865 = CARTESIAN_POINT ( 'NONE',  ( 132.6481957738560311, -34.37139167075012125, 1.944749297857192083 ) ) ;
#79866 = ADVANCED_FACE ( 'NONE', ( #69673 ), #48299, .F. ) ;
#79867 = AXIS2_PLACEMENT_3D ( 'NONE', #6303, #89431, #79718 ) ;
#79869 = CARTESIAN_POINT ( 'NONE',  ( 172.5664832912740110, -36.32844715994070839, 134.1756252759119832 ) ) ;
#79868 = CARTESIAN_POINT ( 'NONE',  ( 134.0664832912740110, -33.97944715994100306, 1.625625275910997480 ) ) ;
#79870 = CARTESIAN_POINT ( 'NONE',  ( 115.3626348109362425, -40.36077478062563983, 207.9086103042679667 ) ) ;
#79871 = ORIENTED_EDGE ( 'NONE', *, *, #72460, .T. ) ;
#79872 = ORIENTED_EDGE ( 'NONE', *, *, #53543, .F. ) ;
#79873 = EDGE_LOOP ( 'NONE', ( #8769, #9287, #66501, #2097 ) ) ;
#79874 = EDGE_CURVE ( 'NONE', #55592, #60004, #47109, .T. ) ;
#79875 = DIRECTION ( 'NONE',  ( -0.000000000000000000, -1.000000000000000000, -0.000000000000000000 ) ) ;
#79876 = CARTESIAN_POINT ( 'NONE',  ( 110.8542377207676992, -45.98433324150028767, 182.8856051340782471 ) ) ;
#79877 = CARTESIAN_POINT ( 'NONE',  ( -479.3614999999999782, 93.66249999999999432, 98.73639197104678544 ) ) ;
#79878 = CARTESIAN_POINT ( 'NONE',  ( 98.26720277155988015, -37.77870449121756025, 37.85301187732598294 ) ) ;
#79879 = EDGE_CURVE ( 'NONE', #51322, #3721, #7972, .T. ) ;
#79880 = VECTOR ( 'NONE', #83821, 1000.000000000000000 ) ;
#79881 = CARTESIAN_POINT ( 'NONE',  ( 118.3041687469094256, 92.64232203292141321, -7.754495127084455319 ) ) ;
#79882 = AXIS2_PLACEMENT_3D ( 'NONE', #4319, #11585, #39276 ) ;
#79883 = PLANE ( 'NONE',  #5636 ) ;
#79884 = FACE_OUTER_BOUND ( 'NONE', #76532, .T. ) ;
#79885 = ORIENTED_EDGE ( 'NONE', *, *, #64246, .T. ) ;
#79886 = CARTESIAN_POINT ( 'NONE',  ( 115.8361900164103275, -31.75800120241248337, 55.23740761269547761 ) ) ;
#79887 = EDGE_LOOP ( 'NONE', ( #38087, #87597, #86831, #50825 ) ) ;
#79888 = LINE ( 'NONE', #43984, #24897 ) ;
#79889 = CARTESIAN_POINT ( 'NONE',  ( 107.6943352634791182, -28.59092592337147209, 67.83380465530596837 ) ) ;
#79890 = LINE ( 'NONE', #24906, #20359 ) ;
#79891 = DIRECTION ( 'NONE',  ( 1.000000000000000000, 0.000000000000000000, 0.000000000000000000 ) ) ;
#79892 = FACE_OUTER_BOUND ( 'NONE', #33267, .T. ) ;
#79893 = VERTEX_POINT ( 'NONE', #7446 ) ;
#79894 = DIRECTION ( 'NONE',  ( 0.000000000000000000, 0.000000000000000000, -1.000000000000000000 ) ) ;
#79895 = CARTESIAN_POINT ( 'NONE',  ( 120.2489068914665182, 57.44811514648141326, -50.84382873326221386 ) ) ;
#79896 = ORIENTED_EDGE ( 'NONE', *, *, #38171, .F. ) ;
#79897 = CARTESIAN_POINT ( 'NONE',  ( 113.8565348333340665, -44.64034031543166492, 108.1413395616249744 ) ) ;
#79898 = ORIENTED_EDGE ( 'NONE', *, *, #77592, .T. ) ;
#79899 = CARTESIAN_POINT ( 'NONE',  ( 101.2610328325635010, -42.99465878394229179, 46.40384839950495177 ) ) ;
#79900 = AXIS2_PLACEMENT_3D ( 'NONE', #33830, #26128, #53796 ) ;
#79901 = VECTOR ( 'NONE', #43629, 1000.000000000000114 ) ;
#79902 = DIRECTION ( 'NONE',  ( 0.000000000000000000, 1.000000000000000000, 0.000000000000000000 ) ) ;
#79903 = CARTESIAN_POINT ( 'NONE',  ( 98.21780894689015895, -37.20823830323941905, 72.80158330589698323 ) ) ;
#79904 = FACE_OUTER_BOUND ( 'NONE', #71177, .T. ) ;
#79905 = DIRECTION ( 'NONE',  ( 9.351236661543306751E-17, -3.725950533538267725E-29, -1.000000000000000000 ) ) ;
#79906 = EDGE_CURVE ( 'NONE', #11120, #74275, #34690, .T. ) ;
#79907 = CARTESIAN_POINT ( 'NONE',  ( 89.90578320442969584, -68.21248437868196390, 247.0699965152190032 ) ) ;
#79908 = CARTESIAN_POINT ( 'NONE',  ( 114.1052656684236979, -46.29384956339717405, 29.08133956162595268 ) ) ;
#79909 = AXIS2_PLACEMENT_3D ( 'NONE', #29552, #49523, #77258 ) ;
#79910 = CARTESIAN_POINT ( 'NONE',  ( 37.35959712144378386, -48.62134037893557803, 129.9678068554150911 ) ) ;
#79911 = ORIENTED_EDGE ( 'NONE', *, *, #80952, .F. ) ;
#79912 = LINE ( 'NONE', #57649, #69070 ) ;
#79913 = ORIENTED_EDGE ( 'NONE', *, *, #68671, .F. ) ;
#79914 = FACE_OUTER_BOUND ( 'NONE', #78508, .T. ) ;
#79915 = VERTEX_POINT ( 'NONE', #62401 ) ;
#79916 = EDGE_LOOP ( 'NONE', ( #7790, #34644, #74135, #89385 ) ) ;
#79917 = AXIS2_PLACEMENT_3D ( 'NONE', #6621, #12545, #61568 ) ;
#79918 = CARTESIAN_POINT ( 'NONE',  ( -29.99999999999996092, 171.0000000000000000, 182.8826257785461280 ) ) ;
#79919 = ORIENTED_EDGE ( 'NONE', *, *, #12576, .F. ) ;
#79920 = CARTESIAN_POINT ( 'NONE',  ( 99.57924082623969753, -30.38476633542323313, 215.7670538473399517 ) ) ;
#79921 = CARTESIAN_POINT ( 'NONE',  ( 30.48091746481826192, -48.32844715994148999, 300.4678068554150059 ) ) ;
#79922 = CARTESIAN_POINT ( 'NONE',  ( 94.58945128933383728, -41.88441296220994303, 289.6356252759106837 ) ) ;
#79923 = CARTESIAN_POINT ( 'NONE',  ( 117.0915230934440103, -32.07406775014006683, 55.16038718067301261 ) ) ;
#79924 = CARTESIAN_POINT ( 'NONE',  ( 97.81200933032994271, -40.51820848727025037, 42.63569297931775282 ) ) ;
#79925 = EDGE_LOOP ( 'NONE', ( #73552, #3489, #26832, #37843, #23177 ) ) ;
#79926 = CARTESIAN_POINT ( 'NONE',  ( 102.0659925822678531, -27.97112074188683550, 171.4898645953594212 ) ) ;
#79927 = DIRECTION ( 'NONE',  ( 0.7071067811873671394, 0.7071067811857280061, 6.612322855862553737E-17 ) ) ;
#79928 = VERTEX_POINT ( 'NONE', #13370 ) ;
#79929 = EDGE_CURVE ( 'NONE', #29190, #6159, #54001, .T. ) ;
#79930 = CARTESIAN_POINT ( 'NONE',  ( 31.78666935232895341, -36.02818131005931690, 117.4678068554150485 ) ) ;
#79931 = CARTESIAN_POINT ( 'NONE',  ( 117.0603190384279912, -38.08450654926203072, 114.7195913024953313 ) ) ;
#79932 = CARTESIAN_POINT ( 'NONE',  ( 99.55514648348071205, -29.48070623161989801, 250.7156252759109520 ) ) ;
#79933 = LINE ( 'NONE', #72658, #83517 ) ;
#79934 = DIRECTION ( 'NONE',  ( 0.000000000000000000, 0.000000000000000000, -1.000000000000000000 ) ) ;
#79935 = CARTESIAN_POINT ( 'NONE',  ( 77.53592152231081513, -37.80596063775247728, 2.807537029279840279 ) ) ;
#79936 = AXIS2_PLACEMENT_3D ( 'NONE', #55060, #68285, #61442 ) ;
#79937 = CARTESIAN_POINT ( 'NONE',  ( 114.1034101198941215, -31.83723292758831747, 278.7324198280767860 ) ) ;
#79939 = CARTESIAN_POINT ( 'NONE',  ( 101.7670726180548542, -27.05576796868586698, 96.46324432352997746 ) ) ;
#79938 = LINE ( 'NONE', #73541, #67912 ) ;
#79940 = CARTESIAN_POINT ( 'NONE',  ( 110.1894008633096149, 61.51549208609898045, 70.02337478721381103 ) ) ;
#79941 = CARTESIAN_POINT ( 'NONE',  ( 102.3732866125132688, -26.67028275327534814, 135.4118157521009493 ) ) ;
#79942 = VERTEX_POINT ( 'NONE', #12313 ) ;
#79943 = CARTESIAN_POINT ( 'NONE',  ( 143.2522959336310748, -139.0102598546870922, 247.5112310255240118 ) ) ;
#79944 = ORIENTED_EDGE ( 'NONE', *, *, #72951, .T. ) ;
#79945 = FACE_BOUND ( 'NONE', #1984, .T. ) ;
#79946 = VECTOR ( 'NONE', #37279, 1000.000000000000000 ) ;
#79947 = DIRECTION ( 'NONE',  ( 0.000000000000000000, -1.000000000000000000, 0.000000000000000000 ) ) ;
#79948 = DIRECTION ( 'NONE',  ( -1.000000000000000078E-15, 1.000000000000000083E-30, 1.000000000000000000 ) ) ;
#79950 = ORIENTED_EDGE ( 'NONE', *, *, #87090, .T. ) ;
#79949 = AXIS2_PLACEMENT_3D ( 'NONE', #58475, #86206, #52533 ) ;
#79951 = CARTESIAN_POINT ( 'NONE',  ( 97.75843041625837770, -40.38500185162371992, 51.62426656411139447 ) ) ;
#79953 = ORIENTED_EDGE ( 'NONE', *, *, #62497, .T. ) ;
#79952 = CARTESIAN_POINT ( 'NONE',  ( 117.9021936627155895, -39.13782096276514721, 103.6403871806729455 ) ) ;
#79954 = DIRECTION ( 'NONE',  ( 0.000000000000000000, 0.000000000000000000, -1.000000000000000000 ) ) ;
#79955 = LINE ( 'NONE', #50883, #73731 ) ;
#79956 = CARTESIAN_POINT ( 'NONE',  ( 83.06670390244804025, -43.72944715994108122, 207.5838068554169809 ) ) ;
#79957 = VERTEX_POINT ( 'NONE', #33650 ) ;
#79958 = AXIS2_PLACEMENT_3D ( 'NONE', #69516, #13208, #34977 ) ;
#79959 = CARTESIAN_POINT ( 'NONE',  ( 106.0743573402139930, -48.56370683269541644, 112.5099109901969712 ) ) ;
#79960 = DIRECTION ( 'NONE',  ( 1.000000000000000000, 0.000000000000000000, 0.000000000000000000 ) ) ;
#79961 = DIRECTION ( 'NONE',  ( 0.7071067811865279218, -0.7071067811865670016, 6.612322855859973915E-17 ) ) ;
#79962 = LINE ( 'NONE', #4976, #63153 ) ;
#79963 = MANIFOLD_SOLID_BREP ( 'Stock-BR-Y-104-1', #63386 ) ;
#79964 = LINE ( 'NONE', #18604, #35454 ) ;
#79965 = VERTEX_POINT ( 'NONE', #76326 ) ;
#79966 = ADVANCED_FACE ( 'NONE', ( #41786 ), #54953, .T. ) ;
#79967 = EDGE_CURVE ( 'NONE', #62846, #33523, #57239, .T. ) ;
#79968 = ORIENTED_EDGE ( 'NONE', *, *, #48683, .T. ) ;
#79969 = DIRECTION ( 'NONE',  ( 0.000000000000000000, 0.000000000000000000, 1.000000000000000000 ) ) ;
#79970 = CARTESIAN_POINT ( 'NONE',  ( 47.62500000000000000, 111.1250000000000000, 219.0749999999999886 ) ) ;
#79971 = ADVANCED_FACE ( 'NONE', ( #7298 ), #15006, .T. ) ;
#79972 = DIRECTION ( 'NONE',  ( 0.000000000000000000, 0.000000000000000000, -1.000000000000000000 ) ) ;
#79973 = CIRCLE ( 'NONE', #14733, 2.116999999999980009 ) ;
#79974 = ADVANCED_FACE ( 'NONE', ( #1378 ), #70876, .F. ) ;
#79976 = CARTESIAN_POINT ( 'NONE',  ( 107.0664832912739399, -36.72944715994095333, 293.1356252759106837 ) ) ;
#79975 = CARTESIAN_POINT ( 'NONE',  ( 41.56648329127399677, -9.303447159940999356, 316.8086252759120498 ) ) ;
#79977 = CARTESIAN_POINT ( 'NONE',  ( 210.5660000000000025, 52.73749999999999716, -51.09754249571540186 ) ) ;
#79978 = VERTEX_POINT ( 'NONE', #69068 ) ;
#79979 = DIRECTION ( 'NONE',  ( 1.000000000000000078E-15, -1.000000000000000083E-30, -1.000000000000000000 ) ) ;
#79980 = CARTESIAN_POINT ( 'NONE',  ( 103.5361331145923032, -27.60804031003073788, 211.3699109901959616 ) ) ;
#79981 = EDGE_CURVE ( 'NONE', #29010, #11533, #5291, .T. ) ;
#79982 = VECTOR ( 'NONE', #69088, 1000.000000000000114 ) ;
#79984 = ORIENTED_EDGE ( 'NONE', *, *, #79652, .F. ) ;
#79983 = CARTESIAN_POINT ( 'NONE',  ( -194.1576000000000022, 101.5999999999999943, 114.2999999999999972 ) ) ;
#79985 = CARTESIAN_POINT ( 'NONE',  ( 110.1509004715571507, -26.04776408289600909, 60.85276813305296173 ) ) ;
#79986 = CARTESIAN_POINT ( 'NONE',  ( 98.04154294162555061, -41.04190759109129516, 51.68120649424626123 ) ) ;
#79987 = DIRECTION ( 'NONE',  ( 0.000000000000000000, 0.000000000000000000, 1.000000000000000000 ) ) ;
#79988 = AXIS2_PLACEMENT_3D ( 'NONE', #31202, #30770, #23532 ) ;
#79989 = CARTESIAN_POINT ( 'NONE',  ( 72.96458098368701428, 117.4749999999999943, -72.96458098368670164 ) ) ;
#79990 = EDGE_LOOP ( 'NONE', ( #21444, #22603, #52579, #71306 ) ) ;
#79991 = DIRECTION ( 'NONE',  ( 1.000000000000000000, 0.000000000000000000, 0.000000000000000000 ) ) ;
#79992 = ORIENTED_EDGE ( 'NONE', *, *, #46314, .F. ) ;
#79993 = ORIENTED_EDGE ( 'NONE', *, *, #53995, .T. ) ;
#79994 = CARTESIAN_POINT ( 'NONE',  ( 115.7580415341064111, -34.85356206270782309, 180.4272975916109374 ) ) ;
#79995 = DIRECTION ( 'NONE',  ( -0.1858654557293118459, 0.9825752044329915114, 0.000000000000000000 ) ) ;
#79996 = CARTESIAN_POINT ( 'NONE',  ( 23.75871628398702384, 82.54999999999999716, 307.6575000000000273 ) ) ;
#79997 = PLANE ( 'NONE',  #31597 ) ;
#79998 = DIRECTION ( 'NONE',  ( 0.000000000000000000, 1.000000000000000000, 0.000000000000000000 ) ) ;
#80000 = ORIENTED_EDGE ( 'NONE', *, *, #18263, .T. ) ;
#79999 = CIRCLE ( 'NONE', #59662, 2.500000000000002220 ) ;
#80001 = DIRECTION ( 'NONE',  ( -1.000000000000000000, 0.000000000000000000, 0.000000000000000000 ) ) ;
#80002 = CARTESIAN_POINT ( 'NONE',  ( 116.8180460095236981, -34.15649538984454381, 185.0317730482575769 ) ) ;
#80003 = ORIENTED_EDGE ( 'NONE', *, *, #24759, .F. ) ;
#80004 = CARTESIAN_POINT ( 'NONE',  ( 96.68578154376476164, -42.44622222083611263, 26.72705384733997747 ) ) ;
#80005 = CARTESIAN_POINT ( 'NONE',  ( 10.78439996481962915, 89.27017318066090468, 118.0647117534048647 ) ) ;
#80006 = ORIENTED_EDGE ( 'NONE', *, *, #4941, .F. ) ;
#80007 = SURFACE_STYLE_USAGE ( .BOTH. , #85934 ) ;
#80008 = CARTESIAN_POINT ( 'NONE',  ( 41.56648329127398966, -27.82844715994070484, 258.9256252759120116 ) ) ;
#80009 = CARTESIAN_POINT ( 'NONE',  ( 70.06670417066791856, -83.77844715994098124, 55.21780685541800437 ) ) ;
#80010 = CARTESIAN_POINT ( 'NONE',  ( 131.0667039024480118, -61.87844715994100397, 213.1838068554149856 ) ) ;
#80011 = AXIS2_PLACEMENT_3D ( 'NONE', #33231, #89548, #23219 ) ;
#80012 = ADVANCED_FACE ( 'NONE', ( #76779 ), #29083, .F. ) ;
#80013 = CARTESIAN_POINT ( 'NONE',  ( 107.2439061797007156, -47.23213900083308658, 208.5899109901969837 ) ) ;
#80014 = FACE_OUTER_BOUND ( 'NONE', #35667, .T. ) ;
#80015 = ORIENTED_EDGE ( 'NONE', *, *, #41981, .T. ) ;
#80016 = AXIS2_PLACEMENT_3D ( 'NONE', #70751, #71648, #16675 ) ;
#80017 = CARTESIAN_POINT ( 'NONE',  ( 100.5235407922616133, -27.76354498484767674, 26.56610146638793779 ) ) ;
#80018 = CARTESIAN_POINT ( 'NONE',  ( 150.5667039024485803, -47.82844715993594065, 129.9678068554149775 ) ) ;
#80019 = EDGE_CURVE ( 'NONE', #25675, #71030, #21861, .T. ) ;
#80020 = ORIENTED_EDGE ( 'NONE', *, *, #54600, .T. ) ;
#80021 = ORIENTED_EDGE ( 'NONE', *, *, #771, .T. ) ;
#80022 = CARTESIAN_POINT ( 'NONE',  ( 81.97596355239433308, -16.74831825238168648, 2.232988539019116647 ) ) ;
#80023 = DIRECTION ( 'NONE',  ( 0.000000000000000000, -1.000000000000000000, 0.000000000000000000 ) ) ;
#80024 = DIRECTION ( 'NONE',  ( 0.000000000000000000, 0.000000000000000000, -1.000000000000000000 ) ) ;
#80025 = CARTESIAN_POINT ( 'NONE',  ( 115.2991214174112002, -34.06025354975611918, 131.9061856076869788 ) ) ;
#80026 = CARTESIAN_POINT ( 'NONE',  ( 99.52368306943544951, -29.45034277662237443, 246.7156252759109520 ) ) ;
#80027 = AXIS2_PLACEMENT_3D ( 'NONE', #6348, #86907, #45983 ) ;
#80028 = DIRECTION ( 'NONE',  ( 0.000000000000000000, 1.000000000000000000, 0.000000000000000000 ) ) ;
#80029 = EDGE_LOOP ( 'NONE', ( #33915, #49503, #12122, #45582 ) ) ;
#80030 = CARTESIAN_POINT ( 'NONE',  ( 136.1031425115661193, -38.57949487819416134, 2.327894807233447327 ) ) ;
#80031 = EDGE_LOOP ( 'NONE', ( #82502, #78908, #81700 ) ) ;
#80032 = VERTEX_POINT ( 'NONE', #83604 ) ;
#80033 = EDGE_CURVE ( 'NONE', #28457, #76903, #71431, .T. ) ;
#80034 = DIRECTION ( 'NONE',  ( 0.000000000000000000, 0.000000000000000000, -1.000000000000000000 ) ) ;
#80035 = ORIENTED_EDGE ( 'NONE', *, *, #35366, .F. ) ;
#80036 = ORIENTED_EDGE ( 'NONE', *, *, #5807, .F. ) ;
#80037 = DIRECTION ( 'NONE',  ( 9.912705577010326536E-16, 1.000000000000000000, 0.000000000000000000 ) ) ;
#80038 = DIRECTION ( 'NONE',  ( 0.000000000000000000, 0.000000000000000000, 1.000000000000000000 ) ) ;
#80039 = CARTESIAN_POINT ( 'NONE',  ( 4.163336342344339551E-14, 127.0000000000000000, -107.7702177616926065 ) ) ;
#80040 = CARTESIAN_POINT ( 'NONE',  ( 105.3429517235655766, -27.17434032488695550, 124.6409912566479647 ) ) ;
#80041 = VECTOR ( 'NONE', #44833, 1000.000000000000000 ) ;
#80042 = CARTESIAN_POINT ( 'NONE',  ( 96.29878009220107060, -39.42515072222565209, 16.53372051400597798 ) ) ;
#80043 = VERTEX_POINT ( 'NONE', #27730 ) ;
#80044 = FACE_OUTER_BOUND ( 'NONE', #10001, .T. ) ;
#80045 = VECTOR ( 'NONE', #78832, 1000.000000000000000 ) ;
#80046 = EDGE_LOOP ( 'NONE', ( #85473, #77418, #62777, #19686 ) ) ;
#80047 = CARTESIAN_POINT ( 'NONE',  ( 41.56648329127399677, -9.303447159940999356, 321.0426252759119734 ) ) ;
#80048 = ORIENTED_EDGE ( 'NONE', *, *, #32770, .F. ) ;
#80049 = CARTESIAN_POINT ( 'NONE',  ( 97.54864246082097168, -39.81029565519295943, 167.5757964592916096 ) ) ;
#80050 = CARTESIAN_POINT ( 'NONE',  ( 115.0361479189475205, -42.90987010871590712, 33.30236611295504190 ) ) ;
#80051 = LINE ( 'NONE', #51409, #79467 ) ;
#80052 = CYLINDRICAL_SURFACE ( 'NONE', #49502, 2.750000000000002665 ) ;
#80053 = ORIENTED_EDGE ( 'NONE', *, *, #85437, .F. ) ;
#80054 = CARTESIAN_POINT ( 'NONE',  ( 97.46629803964546568, -32.60812463323921406, 16.00419670448194154 ) ) ;
#80055 = CARTESIAN_POINT ( 'NONE',  ( 112.2188834189205409, -26.89723471487287654, 10.68038718067299087 ) ) ;
#80057 = LINE ( 'NONE', #18257, #9377 ) ;
#80056 = DIRECTION ( 'NONE',  ( -1.821231995776179916E-16, 0.000000000000000000, -1.000000000000000000 ) ) ;
#80058 = CARTESIAN_POINT ( 'NONE',  ( -22.62762465138237644, 172.0000000000000000, 96.88262577854611379 ) ) ;
#80059 = DIRECTION ( 'NONE',  ( 0.9242245927363031965, 0.3818493186865917766, 0.000000000000000000 ) ) ;
#80060 = CARTESIAN_POINT ( 'NONE',  ( 134.0664828118826506, -39.47944715903992829, 8.225259175038003079 ) ) ;
#80061 = EDGE_CURVE ( 'NONE', #51500, #80913, #55410, .T. ) ;
#80062 = CIRCLE ( 'NONE', #1739, 2.116999999999980009 ) ;
#80063 = CARTESIAN_POINT ( 'NONE',  ( 139.9417039024470455, -127.9034471599408960, 55.21780685541800437 ) ) ;
#80064 = EDGE_CURVE ( 'NONE', #19911, #71480, #34562, .T. ) ;
#80065 = CARTESIAN_POINT ( 'NONE',  ( 113.1786937796897092, -44.75156961497670238, 163.0938295933654842 ) ) ;
#80066 = DIRECTION ( 'NONE',  ( -1.092739197465703932E-16, 0.000000000000000000, 1.000000000000000000 ) ) ;
#80067 = CARTESIAN_POINT ( 'NONE',  ( 105.0173152498862947, -25.84384494483574102, 280.2365776568630622 ) ) ;
#80068 = CARTESIAN_POINT ( 'NONE',  ( 116.3773924821832111, -41.41873894932305689, 199.4556252759109611 ) ) ;
#80069 = CARTESIAN_POINT ( 'NONE',  ( 118.1061288724552725, -37.63024191249119355, 34.77372051400695341 ) ) ;
#80070 = VECTOR ( 'NONE', #88990, 1000.000000000000000 ) ;
#80072 = DIRECTION ( 'NONE',  ( -0.000000000000000000, -0.000000000000000000, -1.000000000000000000 ) ) ;
#80071 = CARTESIAN_POINT ( 'NONE',  ( -7.205548786489490269E-13, 127.0000000000000000, 103.1875000000000000 ) ) ;
#80073 = CARTESIAN_POINT ( 'NONE',  ( 80.81118397279048793, -34.08035908359610033, 1.709393751551411045 ) ) ;
#80074 = COLOUR_RGB ( '', 0.09019608, 0.27058824, 0.51372549) ;
#80075 = EDGE_LOOP ( 'NONE', ( #79015, #9846 ) ) ;
#80076 = CARTESIAN_POINT ( 'NONE',  ( 83.73314995793998605, 12.92155284005730387, 361.9756252759109998 ) ) ;
#80077 = EDGE_LOOP ( 'NONE', ( #67354, #10282, #34068 ) ) ;
#80078 = CARTESIAN_POINT ( 'NONE',  ( 104.1495640007033501, -46.68084741754449851, 58.33753003781600199 ) ) ;
#80079 = EDGE_CURVE ( 'NONE', #70797, #52812, #80471, .T. ) ;
#80081 = VERTEX_POINT ( 'NONE', #85852 ) ;
#80080 = PLANE ( 'NONE',  #51495 ) ;
#80082 = LINE ( 'NONE', #37845, #56200 ) ;
#80083 = CARTESIAN_POINT ( 'NONE',  ( 100.8363305107023820, -45.83159080358277748, 238.1108633711489517 ) ) ;
#80084 = CARTESIAN_POINT ( 'NONE',  ( 49.21437657595017612, -35.91149509761089575, 342.9256252759109884 ) ) ;
#80085 = PRODUCT_DEFINITION_SHAPE ( 'NONE', 'NONE',  #89936 ) ;
#80086 = CARTESIAN_POINT ( 'NONE',  ( 104.4079568779007730, -46.45804709415482847, 147.3648544342418347 ) ) ;
#80087 = ADVANCED_FACE ( 'NONE', ( #4044 ), #87174, .F. ) ;
#80088 = DIRECTION ( 'NONE',  ( -0.000000000000000000, -0.000000000000000000, -1.000000000000000000 ) ) ;
#80089 = DIRECTION ( 'NONE',  ( 0.000000000000000000, 0.000000000000000000, 1.000000000000000000 ) ) ;
#80090 = AXIS2_PLACEMENT_3D ( 'NONE', #68477, #53461, #68021 ) ;
#80091 = CARTESIAN_POINT ( 'NONE',  ( 132.3573525511384048, -38.88611802718990873, 2.101554303222315845 ) ) ;
#80092 = CARTESIAN_POINT ( 'NONE',  ( -83.52520760052897231, 78.07027470200927155, 100.3415888741740503 ) ) ;
#80093 = CARTESIAN_POINT ( 'NONE',  ( 99.18511857479137461, -30.88155312011791409, 180.8184824187689799 ) ) ;
#80094 = ORIENTED_EDGE ( 'NONE', *, *, #16515, .T. ) ;
#80095 = ORIENTED_EDGE ( 'NONE', *, *, #83539, .F. ) ;
#80096 = CIRCLE ( 'NONE', #52479, 1.000000000000000888 ) ;
#80097 = CARTESIAN_POINT ( 'NONE',  ( 107.5226574059108202, -27.84946772507149504, 91.46729759161098627 ) ) ;
#80098 = VECTOR ( 'NONE', #11301, 1000.000000000000114 ) ;
#80099 = CARTESIAN_POINT ( 'NONE',  ( 118.5667039024470313, -104.2784471599411376, 7.717806855417980394 ) ) ;
#80101 = CARTESIAN_POINT ( 'NONE',  ( 116.3188053082936051, -32.94429434937755019, 19.13562527591095019 ) ) ;
#80100 = CARTESIAN_POINT ( 'NONE',  ( 106.3491918589965763, -46.48387837312645132, 218.5184824187679453 ) ) ;
#80102 = CARTESIAN_POINT ( 'NONE',  ( 141.0667039024479834, -48.82844715994099971, 10.91780685541499807 ) ) ;
#80103 = DIRECTION ( 'NONE',  ( 1.000000000000000000, 1.000000000000000078E-15, 0.000000000000000000 ) ) ;
#80104 = MANIFOLD_SOLID_BREP ( 'Stock-BR-Y-104-1', #15549 ) ;
#80105 = VECTOR ( 'NONE', #52952, 1000.000000000000000 ) ;
#80106 = CARTESIAN_POINT ( 'NONE',  ( 117.9083433361412290, 79.66725693986899159, 12.37555662352282226 ) ) ;
#80107 = CARTESIAN_POINT ( 'NONE',  ( -6.360108159902766012, 71.54942407907350344, 118.3858500351901029 ) ) ;
#80108 = CARTESIAN_POINT ( 'NONE',  ( 208.9149999999999920, 43.68799999999999528, 44.45000000000000284 ) ) ;
#80109 = CYLINDRICAL_SURFACE ( 'NONE', #45888, 9.999999999999998224 ) ;
#80110 = CARTESIAN_POINT ( 'NONE',  ( 117.0123300003821640, -30.33189756676010163, 144.2813395616249750 ) ) ;
#80111 = ORIENTED_EDGE ( 'NONE', *, *, #89908, .F. ) ;
#80112 = CIRCLE ( 'NONE', #4622, 2.517500000000005844 ) ;
#80113 = EDGE_LOOP ( 'NONE', ( #51687, #44752 ) ) ;
#80114 = CARTESIAN_POINT ( 'NONE',  ( 107.0667039024470313, -104.2784471599420755, -19.78219314458201694 ) ) ;
#80115 = CARTESIAN_POINT ( 'NONE',  ( 77.40501520703328708, -18.03131342367423073, 2.974074870387416691 ) ) ;
#80116 = CARTESIAN_POINT ( 'NONE',  ( 27.27158787008325902, 184.0000000000000000, -5.920431057502157584E-15 ) ) ;
#80117 = CARTESIAN_POINT ( 'NONE',  ( 172.5664832912729878, -18.82844715994071194, 18.92562527591200094 ) ) ;
#80118 = CARTESIAN_POINT ( 'NONE',  ( 104.4080847095425639, -46.45808491063921508, 268.3647906417609761 ) ) ;
#80119 = EDGE_CURVE ( 'NONE', #55858, #65321, #79115, .T. ) ;
#80120 = CARTESIAN_POINT ( 'NONE',  ( 116.6609997163256764, -40.80771701747383418, 168.5070538473399608 ) ) ;
#80121 = CARTESIAN_POINT ( 'NONE',  ( 31.90335556477799628, -33.89581943344391135, -5.074374724088000832 ) ) ;
#80122 = EDGE_LOOP ( 'NONE', ( #67143, #3116, #65921, #46771 ) ) ;
#80124 = EDGE_LOOP ( 'NONE', ( #62698, #75452, #47674, #6942, #39197 ) ) ;
#80123 = EDGE_LOOP ( 'NONE', ( #68533, #73889, #14326, #88615 ) ) ;
#80125 = AXIS2_PLACEMENT_3D ( 'NONE', #26659, #19854, #68002 ) ;
#80126 = CARTESIAN_POINT ( 'NONE',  ( -8.383266637423213652, 73.00087262779534569, 118.2596760195012848 ) ) ;
#80127 = DIRECTION ( 'NONE',  ( 0.000000000000000000, 0.000000000000000000, -1.000000000000000000 ) ) ;
#80128 = DIRECTION ( 'NONE',  ( -1.776356839400250465E-15, 0.000000000000000000, -1.000000000000000000 ) ) ;
#80129 = CARTESIAN_POINT ( 'NONE',  ( 105.0496896133374918, -44.66766052993097702, 45.19666179816294971 ) ) ;
#80130 = CARTESIAN_POINT ( 'NONE',  ( 183.5150000000000148, 37.33800000000000097, 69.13087104677069306 ) ) ;
#80131 = EDGE_LOOP ( 'NONE', ( #72677, #48317, #42853, #50169 ) ) ;
#80132 = AXIS2_PLACEMENT_3D ( 'NONE', #68889, #62061, #89796 ) ;
#80133 = CARTESIAN_POINT ( 'NONE',  ( 139.9417039024470171, -80.65344715994091018, 55.21780685541800437 ) ) ;
#80134 = CARTESIAN_POINT ( 'NONE',  ( 82.57621891717900553, -17.60488046387944294, 7.068409955839225489 ) ) ;
#80135 = ORIENTED_EDGE ( 'NONE', *, *, #87426, .F. ) ;
#80136 = ORIENTED_EDGE ( 'NONE', *, *, #29121, .F. ) ;
#80137 = VECTOR ( 'NONE', #71628, 1000.000000000000000 ) ;
#80138 = EDGE_CURVE ( 'NONE', #52412, #23079, #87058, .T. ) ;
#80139 = FACE_OUTER_BOUND ( 'NONE', #1201, .T. ) ;
#80140 = ORIENTED_EDGE ( 'NONE', *, *, #58795, .F. ) ;
#80141 = ORIENTED_EDGE ( 'NONE', *, *, #39206, .F. ) ;
#80142 = DIRECTION ( 'NONE',  ( 2.900000000000000265E-14, -2.000000000000000155E-15, 1.000000000000000000 ) ) ;
#80143 = CARTESIAN_POINT ( 'NONE',  ( 107.1721053552439713, -28.18866407513752392, 34.48956268521896362 ) ) ;
#80144 = CARTESIAN_POINT ( 'NONE',  ( 110.5061846383585475, -26.86461981176654845, 209.8099109901969541 ) ) ;
#80145 = CARTESIAN_POINT ( 'NONE',  ( 111.4081670832169237, -47.72935575799012753, 172.8756252759109771 ) ) ;
#80146 = CARTESIAN_POINT ( 'NONE',  ( 151.0371591254576060, -24.95799193692592155, 129.9678068554149775 ) ) ;
#80147 = CARTESIAN_POINT ( 'NONE',  ( 105.6320745483020147, -47.05538338894268691, 253.4670538473393719 ) ) ;
#80148 = CARTESIAN_POINT ( 'NONE',  ( 101.9936794628098369, -45.44610784961911065, 98.15771542624335666 ) ) ;
#80149 = CARTESIAN_POINT ( 'NONE',  ( -7.661254700127832606, 98.64746158385918307, 320.6630000000000109 ) ) ;
#80151 = ORIENTED_EDGE ( 'NONE', *, *, #49489, .F. ) ;
#80150 = ADVANCED_FACE ( 'NONE', ( #46132 ), #72537, .F. ) ;
#80152 = AXIS2_PLACEMENT_3D ( 'NONE', #16987, #22468, #10603 ) ;
#80153 = EDGE_CURVE ( 'NONE', #22550, #35335, #67061, .T. ) ;
#80154 = ORIENTED_EDGE ( 'NONE', *, *, #10860, .T. ) ;
#80155 = CIRCLE ( 'NONE', #43888, 17.00000000000090239 ) ;
#80156 = DIRECTION ( 'NONE',  ( 1.907762142705490052E-15, 7.167082501179359715E-16, -1.000000000000000000 ) ) ;
#80157 = CARTESIAN_POINT ( 'NONE',  ( 106.9399074540173871, -47.82885535071048366, 232.5794347997199907 ) ) ;
#80158 = ORIENTED_EDGE ( 'NONE', *, *, #39245, .T. ) ;
#80159 = CARTESIAN_POINT ( 'NONE',  ( 118.9178230750475649, -36.92810663041961305, 153.8127681330539644 ) ) ;
#80160 = CARTESIAN_POINT ( 'NONE',  ( 97.07203916561205403, -35.37876108150283017, 266.2190116188336901 ) ) ;
#80161 = DIRECTION ( 'NONE',  ( 1.000000000000000000, 0.000000000000000000, -0.000000000000000000 ) ) ;
#80162 = EDGE_CURVE ( 'NONE', #4014, #28273, #59769, .T. ) ;
#80163 = LINE ( 'NONE', #11560, #69614 ) ;
#80164 = DIRECTION ( 'NONE',  ( -1.000000000000000000, 0.000000000000000000, -2.108231265501709878E-16 ) ) ;
#80167 = CARTESIAN_POINT ( 'NONE',  ( 118.0799254396264786, -36.12288750354066735, 269.8822919425776945 ) ) ;
#80166 = CARTESIAN_POINT ( 'NONE',  ( 21.03689327557705369, -23.42844715994187155, 237.4678068554150059 ) ) ;
#80165 = DIRECTION ( 'NONE',  ( -0.000000000000000000, 1.000000000000000000, -0.000000000000000000 ) ) ;
#80168 = DIRECTION ( 'NONE',  ( -0.1811243269279065315, 0.9834602067165264527, 0.000000000000000000 ) ) ;
#80169 = FACE_OUTER_BOUND ( 'NONE', #9753, .T. ) ;
#80170 = VECTOR ( 'NONE', #24303, 1000.000000000000000 ) ;
#80171 = LINE ( 'NONE', #87864, #15109 ) ;
#80172 = CARTESIAN_POINT ( 'NONE',  ( 68.76053423562146349, -136.8603496727827746, 247.4879725229279757 ) ) ;
#80173 = DIRECTION ( 'NONE',  ( 0.000000000000000000, 0.000000000000000000, 1.000000000000000000 ) ) ;
#80174 = EDGE_CURVE ( 'NONE', #18741, #75087, #63150, .T. ) ;
#80175 = DIRECTION ( 'NONE',  ( 1.000000000000000000, 0.000000000000000000, 0.000000000000000000 ) ) ;
#80177 = VERTEX_POINT ( 'NONE', #66593 ) ;
#80176 = CARTESIAN_POINT ( 'NONE',  ( 106.7204202803107904, -44.74667865324451554, 195.5838068554169809 ) ) ;
#80178 = DIRECTION ( 'NONE',  ( 0.000000000000000000, 0.000000000000000000, 1.000000000000000000 ) ) ;
#80179 = CARTESIAN_POINT ( 'NONE',  ( 110.7040309646834970, -48.03441345040916843, 207.8241967044819489 ) ) ;
#80180 = CARTESIAN_POINT ( 'NONE',  ( 102.3023240427231570, -27.41686860022338124, 116.4527681330539650 ) ) ;
#80181 = CARTESIAN_POINT ( 'NONE',  ( 110.0644950372451945, -26.04256623378434554, 215.8708633711489711 ) ) ;
#80182 = CARTESIAN_POINT ( 'NONE',  ( 110.2536356736639220, -106.6957733451327215, -19.78219314458193168 ) ) ;
#80183 = DIRECTION ( 'NONE',  ( 0.000000000000000000, -0.000000000000000000, 1.000000000000000000 ) ) ;
#80185 = CARTESIAN_POINT ( 'NONE',  ( 116.6468703464407355, -39.65304199921658324, 39.59041423949068417 ) ) ;
#80184 = DIRECTION ( 'NONE',  ( 0.000000000000000000, 1.000000000000000000, 0.000000000000000000 ) ) ;
#80186 = LINE ( 'NONE', #72470, #34913 ) ;
#80187 = FACE_BOUND ( 'NONE', #18099, .T. ) ;
#80188 = CARTESIAN_POINT ( 'NONE',  ( 77.31648329127402519, -36.72944715994107412, -5.074374724089059541 ) ) ;
#80189 = EDGE_LOOP ( 'NONE', ( #27000, #15801, #52930, #28855 ) ) ;
#80190 = ORIENTED_EDGE ( 'NONE', *, *, #17993, .F. ) ;
#80191 = CARTESIAN_POINT ( 'NONE',  ( 98.02237212078092909, -37.19498283172546849, 120.8019436376009708 ) ) ;
#80192 = EDGE_CURVE ( 'NONE', #74330, #18892, #58438, .T. ) ;
#80194 = ORIENTED_EDGE ( 'NONE', *, *, #81496, .T. ) ;
#80193 = CARTESIAN_POINT ( 'NONE',  ( 45.77381068356938698, -48.62134037881676818, 249.9678068554150343 ) ) ;
#80195 = VECTOR ( 'NONE', #28330, 1000.000000000000000 ) ;
#80196 = CARTESIAN_POINT ( 'NONE',  ( 97.95167206076199307, -31.64175201202211341, 106.9213395616259703 ) ) ;
#80197 = LINE ( 'NONE', #17944, #4771 ) ;
#80198 = EDGE_CURVE ( 'NONE', #13914, #51337, #52489, .T. ) ;
#80199 = EDGE_CURVE ( 'NONE', #10583, #5137, #22582, .T. ) ;
#80200 = DIRECTION ( 'NONE',  ( 0.000000000000000000, 0.000000000000000000, 1.000000000000000000 ) ) ;
#80201 = CARTESIAN_POINT ( 'NONE',  ( -74.36911441044735227, 81.71068249639867531, 92.32962665258538948 ) ) ;
#80202 = CARTESIAN_POINT ( 'NONE',  ( 34.27258461953881152, -35.55794170701842916, 237.4678068554150059 ) ) ;
#80203 = EDGE_CURVE ( 'NONE', #4730, #15894, #1155, .T. ) ;
#80204 = CARTESIAN_POINT ( 'NONE',  ( 114.3402351757609665, -43.26825200597438226, 38.24419670448392594 ) ) ;
#80205 = EDGE_LOOP ( 'NONE', ( #81581, #79077, #72211, #41650 ) ) ;
#80206 = VERTEX_POINT ( 'NONE', #56084 ) ;
#80207 = EDGE_LOOP ( 'NONE', ( #87385, #38111 ) ) ;
#80208 = VECTOR ( 'NONE', #57197, 1000.000000000000000 ) ;
#80209 = CARTESIAN_POINT ( 'NONE',  ( 115.5439452383991892, -99.96145986183427112, -19.78219314458215550 ) ) ;
#80211 = CARTESIAN_POINT ( 'NONE',  ( 73.17003668186733023, -46.47944715994106701, -5.074374724089063982 ) ) ;
#80210 = CARTESIAN_POINT ( 'NONE',  ( 111.8077268321493278, -46.78591733285061594, 133.9270538473389536 ) ) ;
#80212 = DIRECTION ( 'NONE',  ( 0.000000000000000000, 0.000000000000000000, 1.000000000000000000 ) ) ;
#80213 = CARTESIAN_POINT ( 'NONE',  ( 0.000000000000000000, 117.4749999999999943, -103.1875000000000000 ) ) ;
#80214 = DIRECTION ( 'NONE',  ( 0.000000000000000000, -1.000000000000000000, 0.000000000000000000 ) ) ;
#80215 = CARTESIAN_POINT ( 'NONE',  ( -4.887181091293991031, 94.27201341476896346, 130.4644959256346795 ) ) ;
#80216 = LINE ( 'NONE', #43981, #37111 ) ;
#80217 = CARTESIAN_POINT ( 'NONE',  ( 110.3472192523918380, -25.36789009815977636, 64.85276813305395649 ) ) ;
#80218 = ORIENTED_EDGE ( 'NONE', *, *, #65498, .T. ) ;
#80219 = ORIENTED_EDGE ( 'NONE', *, *, #86004, .F. ) ;
#80220 = CARTESIAN_POINT ( 'NONE',  ( 11.89044713366393324, 87.03112570152838146, 130.0135071244502285 ) ) ;
#80221 = DIRECTION ( 'NONE',  ( 0.000000000000000000, 0.000000000000000000, -1.000000000000000000 ) ) ;
#80222 = DIRECTION ( 'NONE',  ( -4.237773401492740281E-14, 1.000000000000000000, 0.000000000000000000 ) ) ;
#80223 = CARTESIAN_POINT ( 'NONE',  ( 103.3443811052163568, -28.91619688769685936, 138.2604713219729717 ) ) ;
#80224 = B_SPLINE_CURVE_WITH_KNOTS ( 'NONE', 3,
 ( #84679, #30587, #77854, #36951, #57387, #1553, #44644, #51889, #72377, #58286, #10145, #29694, #9256, #2888, #37853, #64659, #2445, #45088, #16079, #71929, #17406, #30143, #15630, #50573, #57839, #64223, #85130, #50118, #85576, #23790, #8823, #9696, #22896, #23353, #3333, #43304, #10580, #37403, #86018, #51023, #36521, #78763, #1993, #65550, #16517, #31027, #44194, #58717, #86458 ),
 .UNSPECIFIED., .F., .F.,
 ( 4, 2, 1, 1, 1, 1, 1, 1, 2, 2, 2, 2, 2, 2, 2, 1, 1, 1, 1, 1, 1, 1, 2, 2, 2, 2, 2, 2, 2, 2, 4 ),
 ( 0.5000144601850410320, 0.5001365269672251035, 0.5002585937494091750, 0.5005027273137773181, 0.5009909944425138262, 0.5019675286999867314, 0.5039205972149323198, 0.5078267342448233856, 0.5156390083046059614, 0.5312635564241712238, 0.5625126526633018598, 0.6250108451415630206, 0.6875090376198240705, 0.7500072300980851203, 0.7500682634891768785, 0.7501292968802688588, 0.7502513636624523752, 0.7504954972268100821, 0.7509837643555183906, 0.7519602986129432232, 0.7539133671277988835, 0.7578195041575164215, 0.7656317782169517194, 0.7812563263358216492, 0.8125054225735615088, 0.8437545188113011463, 0.8750036150490410058, 0.9062527112867807544, 0.9375018075245205029, 0.9687509037622602515, 1.000000000000000000 ),
 .UNSPECIFIED. ) ;
#80225 = AXIS2_PLACEMENT_3D ( 'NONE', #16457, #64606, #44137 ) ;
#80226 = CONICAL_SURFACE ( 'NONE', #35275, 3.968750000000520473, 0.7853981633974667087 ) ;
#80227 = DIRECTION ( 'NONE',  ( 1.000000000000000000, 0.000000000000000000, 0.000000000000000000 ) ) ;
#80228 = ORIENTED_EDGE ( 'NONE', *, *, #79030, .F. ) ;
#80229 = ORIENTED_EDGE ( 'NONE', *, *, #18603, .T. ) ;
#80230 = CARTESIAN_POINT ( 'NONE',  ( 63.06670390244641311, -24.92844715994017335, 180.4678068554151196 ) ) ;
#80231 = EDGE_LOOP ( 'NONE', ( #52516, #48139, #88976, #54062, #50362, #3726 ) ) ;
#80232 = ORIENTED_EDGE ( 'NONE', *, *, #28736, .F. ) ;
#80233 = FACE_BOUND ( 'NONE', #17033, .T. ) ;
#80234 = CARTESIAN_POINT ( 'NONE',  ( 98.20738808897236538, -36.51799785534514342, 192.7387261630399564 ) ) ;
#80235 = DIRECTION ( 'NONE',  ( 0.000000000000000000, 0.000000000000000000, 1.000000000000000000 ) ) ;
#80236 = LINE ( 'NONE', #60198, #3757 ) ;
#80237 = CARTESIAN_POINT ( 'NONE',  ( -110.0726456481004050, 61.01229592318024686, 70.20625887764980178 ) ) ;
#80238 = ORIENTED_EDGE ( 'NONE', *, *, #1213, .F. ) ;
#80239 = VERTEX_POINT ( 'NONE', #63832 ) ;
#80240 = ADVANCED_FACE ( 'NONE', ( #43360 ), #64281, .T. ) ;
#80241 = VECTOR ( 'NONE', #59483, 1000.000000000000000 ) ;
#80242 = ORIENTED_EDGE ( 'NONE', *, *, #70020, .T. ) ;
#80243 = ORIENTED_EDGE ( 'NONE', *, *, #16458, .T. ) ;
#80244 = EDGE_CURVE ( 'NONE', #51011, #2099, #42460, .T. ) ;
#80245 = B_SPLINE_CURVE_WITH_KNOTS ( 'NONE', 3,
 ( #11584, #25193, #65202, #45179, #51110, #3868, #51984, #51547, #72903, #2979, #30679, #80185, #10668, #38373, #66979, #46061, #9791, #79298, #72025, #45609, #79742, #31559, #24753, #86993, #4760, #78851, #32444, #66073, #3423, #52421, #39275, #18377, #17933, #17499, #17056, #58377, #73341, #11115, #44737, #72469 ),
 .UNSPECIFIED., .F., .F.,
 ( 4, 2, 2, 2, 2, 2, 2, 2, 2, 2, 2, 2, 2, 2, 2, 2, 1, 1, 1, 1, 2, 4 ),
 ( 0.000000000000000000, 0.06250740735585620655, 0.1250148147117124131, 0.1562685183896407870, 0.1875222220675691609, 0.2187759257454975625, 0.2500296294234259364, 0.2812833331013543381, 0.3125370367792826842, 0.3437907404572110859, 0.3750444441351394320, 0.4062981478130678337, 0.4375518514909962353, 0.4688055551689245815, 0.4844324070078888655, 0.4922458329273708966, 0.4961525458871118288, 0.4981059023669823782, 0.4990825806069176251, 0.4995709197268851653, 0.4998150892868689077, 0.5000592588468526500 ),
 .UNSPECIFIED. ) ;
#80246 = MANIFOLD_SOLID_BREP ( 'Stock-BR-Y-104-1', #40159 ) ;
#80247 = CARTESIAN_POINT ( 'NONE',  ( 114.7326537306653762, -39.53293727251440970, 216.3652332267339773 ) ) ;
#80248 = EDGE_CURVE ( 'NONE', #73072, #44803, #70646, .T. ) ;
#80250 = CARTESIAN_POINT ( 'NONE',  ( 116.6186327310674500, -29.67321183330947321, 109.3327681330539605 ) ) ;
#80249 = CIRCLE ( 'NONE', #29477, 2.117000000000000881 ) ;
#80251 = CARTESIAN_POINT ( 'NONE',  ( 96.94826409162251935, -39.14818769109204055, 56.51276813305394597 ) ) ;
#80252 = DIRECTION ( 'NONE',  ( 0.000000000000000000, 1.000000000000000000, 0.000000000000000000 ) ) ;
#80253 = FACE_OUTER_BOUND ( 'NONE', #20903, .T. ) ;
#80254 = CARTESIAN_POINT ( 'NONE',  ( 106.8112376695022192, -25.27147963872677039, 323.5310614826137794 ) ) ;
#80255 = CARTESIAN_POINT ( 'NONE',  ( 108.3661019610163123, -47.70601195518164417, 158.6822919425779617 ) ) ;
#80256 = DIRECTION ( 'NONE',  ( 0.000000000000000000, 0.000000000000000000, 1.000000000000000000 ) ) ;
#80257 = EDGE_LOOP ( 'NONE', ( #81833, #1602, #14923, #18786 ) ) ;
#80258 = PLANE ( 'NONE',  #78689 ) ;
#80260 = ORIENTED_EDGE ( 'NONE', *, *, #32946, .T. ) ;
#80259 = ADVANCED_FACE ( 'NONE', ( #49281 ), #30973, .T. ) ;
#80261 = EDGE_CURVE ( 'NONE', #20221, #88467, #73312, .T. ) ;
#80262 = ORIENTED_EDGE ( 'NONE', *, *, #5272, .T. ) ;
#80263 = CARTESIAN_POINT ( 'NONE',  ( 147.0667039024469886, -67.87844716047348470, 245.4920193514540188 ) ) ;
#80264 = CARTESIAN_POINT ( 'NONE',  ( 176.7669697523293735, -48.62818131005361266, 129.9678068554150059 ) ) ;
#80265 = ORIENTED_EDGE ( 'NONE', *, *, #51455, .T. ) ;
#80266 = ADVANCED_FACE ( 'NONE', ( #56997 ), #36578, .F. ) ;
#80267 = VECTOR ( 'NONE', #67140, 1000.000000000000000 ) ;
#80268 = DIRECTION ( 'NONE',  ( -6.524622321627019585E-16, -4.013151879589939944E-16, -1.000000000000000000 ) ) ;
#80269 = ORIENTED_EDGE ( 'NONE', *, *, #63736, .T. ) ;
#80270 = CARTESIAN_POINT ( 'NONE',  ( 101.9270123149900513, -28.12399952947236059, 131.5047745096841254 ) ) ;
#80271 = CARTESIAN_POINT ( 'NONE',  ( 106.8411850752606966, -48.57806423327891565, 77.56133956162491927 ) ) ;
#80272 = CARTESIAN_POINT ( 'NONE',  ( 1.925672578516905147E-22, 69.84999999999999432, 130.5560000000000116 ) ) ;
#80273 = EDGE_CURVE ( 'NONE', #49695, #68284, #10530, .T. ) ;
#80274 = CARTESIAN_POINT ( 'NONE',  ( 20.03715912545644784, -24.42818131006202975, 117.4678068554150485 ) ) ;
#80275 = DIRECTION ( 'NONE',  ( 1.000000000000000000, 0.000000000000000000, 0.000000000000000000 ) ) ;
#80276 = CARTESIAN_POINT ( 'NONE',  ( 112.4079628628857677, -28.49644221148687251, 69.61848241876894861 ) ) ;
#80278 = CARTESIAN_POINT ( 'NONE',  ( 109.3536845750984128, -25.93905639472658819, 180.9222919425779708 ) ) ;
#80277 = DIRECTION ( 'NONE',  ( 0.000000000000000000, -1.000000000000000000, 0.000000000000000000 ) ) ;
#80279 = DIRECTION ( 'NONE',  ( 0.000000000000000000, 0.000000000000000000, -1.000000000000000000 ) ) ;
#80280 = LINE ( 'NONE', #87526, #68483 ) ;
#80281 = ORIENTED_EDGE ( 'NONE', *, *, #54541, .F. ) ;
#80282 = DIRECTION ( 'NONE',  ( 0.000000000000000000, 0.000000000000000000, 1.000000000000000000 ) ) ;
#80283 = CARTESIAN_POINT ( 'NONE',  ( 29.77381068363397887, -48.62134037875510018, 129.9678068554150627 ) ) ;
#80284 = CARTESIAN_POINT ( 'NONE',  ( 176.5667039024392579, -48.82844715994099971, 129.9678068554150343 ) ) ;
#80285 = EDGE_CURVE ( 'NONE', #21324, #48511, #44261, .T. ) ;
#80286 = CARTESIAN_POINT ( 'NONE',  ( 188.5667039024479834, -65.37844715994100397, 293.2178068554150627 ) ) ;
#80288 = EDGE_LOOP ( 'NONE', ( #20600, #17258, #4859 ) ) ;
#80287 = CARTESIAN_POINT ( 'NONE',  ( 116.3896376309502045, -44.12590514183388990, 198.2927681330539542 ) ) ;
#80289 = CARTESIAN_POINT ( 'NONE',  ( 97.81169536214920868, -40.51742132101362870, 146.6356105553879274 ) ) ;
#80290 = CARTESIAN_POINT ( 'NONE',  ( 109.2164500608077873, -48.40848361911378817, 273.7213395616253706 ) ) ;
#80291 = CARTESIAN_POINT ( 'NONE',  ( 117.4068710881028323, -38.36326476267787200, 109.7013395616249767 ) ) ;
#80292 = CARTESIAN_POINT ( 'NONE',  ( 48.85858412958051389, -30.08671355700274574, 313.9678068554150059 ) ) ;
#80293 = CARTESIAN_POINT ( 'NONE',  ( 82.72821098189017164, -37.44060378568480019, 6.877169033942653442 ) ) ;
#80294 = DIRECTION ( 'NONE',  ( 0.7071067811865449082, 0.7071067811865501263, 7.071067811865448709E-16 ) ) ;
#80295 = DIRECTION ( 'NONE',  ( -3.100000000000000258E-29, 3.100000000000000044E-14, 1.000000000000000000 ) ) ;
#80296 = EDGE_LOOP ( 'NONE', ( #6489, #66705, #51082, #1691 ) ) ;
#80297 = VECTOR ( 'NONE', #83857, 1000.000000000000000 ) ;
#80298 = AXIS2_PLACEMENT_3D ( 'NONE', #76893, #75556, #26951 ) ;
#80299 = VERTEX_POINT ( 'NONE', #7516 ) ;
#80300 = VERTEX_POINT ( 'NONE', #35205 ) ;
#80301 = ORIENTED_EDGE ( 'NONE', *, *, #31624, .T. ) ;
#80302 = LINE ( 'NONE', #65746, #23373 ) ;
#80303 = CARTESIAN_POINT ( 'NONE',  ( 105.1675567143510364, -46.98732170830142962, 8.429910990196965770 ) ) ;
#80304 = DIRECTION ( 'NONE',  ( 0.000000000000000000, -0.000000000000000000, 1.000000000000000000 ) ) ;
#80305 = CARTESIAN_POINT ( 'NONE',  ( 70.06684293446046752, -140.6784485900457753, 245.9352930260599805 ) ) ;
#80306 = EDGE_CURVE ( 'NONE', #1830, #66807, #66829, .T. ) ;
#80309 = ADVANCED_FACE ( 'NONE', ( #11424 ), #88196, .T. ) ;
#80308 = CARTESIAN_POINT ( 'NONE',  ( 28.57499999999999929, 82.54999999999999716, 302.8950000000000387 ) ) ;
#80307 = DIRECTION ( 'NONE',  ( -1.000000000000000000, 2.195856868753399715E-16, 0.000000000000000000 ) ) ;
#80310 = CARTESIAN_POINT ( 'NONE',  ( 99.99456525420680464, -31.07253584695887483, 195.2000388756959808 ) ) ;
#80311 = ORIENTED_EDGE ( 'NONE', *, *, #32428, .F. ) ;
#80312 = EDGE_LOOP ( 'NONE', ( #66448, #29272, #4958, #19943 ) ) ;
#80313 = ORIENTED_EDGE ( 'NONE', *, *, #8150, .F. ) ;
#80314 = DIRECTION ( 'NONE',  ( 1.000000000000000000, 1.261617073437676668E-15, 9.462128050782575008E-16 ) ) ;
#80315 = VECTOR ( 'NONE', #74817, 1000.000000000000000 ) ;
#80316 = CARTESIAN_POINT ( 'NONE',  ( 110.8973285702773950, -45.96660512525729558, 182.8893129469914811 ) ) ;
#80317 = DIRECTION ( 'NONE',  ( 0.000000000000000000, 0.8660254037844383745, -0.5000000000000003331 ) ) ;
#80318 = CARTESIAN_POINT ( 'NONE',  ( 105.6677623720644306, -45.47998190943052066, 33.88158330589596545 ) ) ;
#80319 = CARTESIAN_POINT ( 'NONE',  ( 118.0058645681208702, 88.18374315479978520, -11.41243735079784472 ) ) ;
#80320 = CIRCLE ( 'NONE', #13520, 4.749999999999976907 ) ;
#80321 = CARTESIAN_POINT ( 'NONE',  ( 115.0870674648954690, -30.61525487349474872, 174.3441961381653016 ) ) ;
#80322 = LINE ( 'NONE', #18067, #13837 ) ;
#80323 = ORIENTED_EDGE ( 'NONE', *, *, #73220, .T. ) ;
#80324 = CARTESIAN_POINT ( 'NONE',  ( 103.2767410102387231, -27.47537489543444877, 56.38577783829719436 ) ) ;
#80325 = EDGE_LOOP ( 'NONE', ( #25724, #28377, #78151, #72522, #86321, #12150, #76551, #25650, #72571, #42129, #16832, #33849, #8567, #29344, #22476, #47276, #38992, #78031 ) ) ;
#80326 = CARTESIAN_POINT ( 'NONE',  ( -71.77848634863029531, 120.6499999999999915, -77.39114642430038771 ) ) ;
#80327 = CARTESIAN_POINT ( 'NONE',  ( 111.5243040195562401, -29.85845577577017806, 67.43666179816293038 ) ) ;
#80328 = VECTOR ( 'NONE', #49598, 1000.000000000000000 ) ;
#80329 = CARTESIAN_POINT ( 'NONE',  ( 67.65734841870819594, 69.84999999999999432, 358.0130000000000337 ) ) ;
#80330 = DIRECTION ( 'NONE',  ( 0.000000000000000000, 0.000000000000000000, 1.000000000000000000 ) ) ;
#80331 = CARTESIAN_POINT ( 'NONE',  ( 109.6429171241200038, -46.48011071818258699, 193.7814046315215251 ) ) ;
#80332 = ORIENTED_EDGE ( 'NONE', *, *, #18313, .T. ) ;
#80333 = FACE_OUTER_BOUND ( 'NONE', #2747, .T. ) ;
#80334 = CARTESIAN_POINT ( 'NONE',  ( 124.7264490944447175, 58.08405409534557151, -38.57737657011050914 ) ) ;
#80335 = ORIENTED_EDGE ( 'NONE', *, *, #32889, .T. ) ;
#80336 = CARTESIAN_POINT ( 'NONE',  ( 97.61684652917979577, -30.99503764212949264, 125.8803871806719599 ) ) ;
#80337 = ORIENTED_EDGE ( 'NONE', *, *, #15852, .T. ) ;
#80338 = CARTESIAN_POINT ( 'NONE',  ( 112.3043975166656736, -44.90470753876829235, 67.45241982807698378 ) ) ;
#80339 = DIRECTION ( 'NONE',  ( -0.7071067811864980568, -0.7071067811865969777, 0.000000000000000000 ) ) ;
#80340 = CARTESIAN_POINT ( 'NONE',  ( 108.6974651445452764, -45.43968118700122005, 79.15586902018296200 ) ) ;
#80341 = CARTESIAN_POINT ( 'NONE',  ( 86.06670390244796920, -58.72944715994110254, 310.9178068554150514 ) ) ;
#80342 = CARTESIAN_POINT ( 'NONE',  ( 154.5667039024469886, -67.87844715994090450, 155.2178068554179902 ) ) ;
#80343 = ADVANCED_FACE ( 'NONE', ( #45470 ), #18237, .F. ) ;
#80344 = CARTESIAN_POINT ( 'NONE',  ( 96.66430309996448500, -42.45805065352005414, 22.72705384733997391 ) ) ;
#80345 = DIRECTION ( 'NONE',  ( 0.000000000000000000, -1.000000000000000000, 0.000000000000000000 ) ) ;
#80346 = ORIENTED_EDGE ( 'NONE', *, *, #4797, .F. ) ;
#80347 = DIRECTION ( 'NONE',  ( -2.900000000000000265E-14, 2.000000000000000155E-15, -1.000000000000000000 ) ) ;
#80348 = EDGE_LOOP ( 'NONE', ( #31731, #2279, #45117, #47296 ) ) ;
#80349 = CARTESIAN_POINT ( 'NONE',  ( -118.5214325610856605, 70.17658267799285454, 2.892017926150298734 ) ) ;
#80350 = AXIS2_PLACEMENT_3D ( 'NONE', #61244, #76223, #89875 ) ;
#80351 = VERTEX_POINT ( 'NONE', #45915 ) ;
#80353 = ADVANCED_FACE ( 'NONE', ( #39125 ), #81388, .T. ) ;
#80352 = ORIENTED_EDGE ( 'NONE', *, *, #67021, .F. ) ;
#80354 = EDGE_CURVE ( 'NONE', #8565, #37523, #55860, .T. ) ;
#80355 = B_SPLINE_CURVE_WITH_KNOTS ( 'NONE', 3,
 ( #61427, #89154, #26918, #20115, #75526, #77314, #1910, #550, #29164, #6923, #21915, #34625, #21460, #70502, #29608, #70051, #28250, #56400, #57297, #84143, #112, #69607, #22810, #7819, #1468, #62331, #27810, #35509 ),
 .UNSPECIFIED., .F., .F.,
 ( 4, 2, 2, 2, 2, 2, 2, 2, 2, 2, 1, 1, 1, 1, 2, 4 ),
 ( 0.000000000000000000, 0.06251150331641630586, 0.1250230066328326117, 0.1875345099492489176, 0.2500460132656652235, 0.3125575165820815848, 0.3750690198984978352, 0.4375805232149141411, 0.4688362748731219609, 0.4844641507022258153, 0.4922780886167778536, 0.4961850575740540670, 0.4981385420526921459, 0.4991152842920111299, 0.4996036554116704553, 0.5000920265313297808 ),
 .UNSPECIFIED. ) ;
#80356 = EDGE_CURVE ( 'NONE', #72283, #34034, #60453, .T. ) ;
#80357 = EDGE_LOOP ( 'NONE', ( #6710, #65599, #1945, #45897 ) ) ;
#80358 = CARTESIAN_POINT ( 'NONE',  ( 98.06605190618643064, -40.64173669134676459, 231.6527681330539679 ) ) ;
#80359 = CARTESIAN_POINT ( 'NONE',  ( 97.81286927418427979, -40.51761286958078756, 126.6352223400343746 ) ) ;
#80360 = CYLINDRICAL_SURFACE ( 'NONE', #31689, 0.4999999999999989453 ) ;
#80361 = CARTESIAN_POINT ( 'NONE',  ( 112.7598396812348369, -27.95408244994987967, 65.61848241876793963 ) ) ;
#80362 = DIRECTION ( 'NONE',  ( 4.299999999999999979E-14, -1.000000000000000000, 4.100000000000000342E-29 ) ) ;
#80363 = ORIENTED_EDGE ( 'NONE', *, *, #4650, .T. ) ;
#80364 = LINE ( 'NONE', #40347, #40906 ) ;
#80365 = EDGE_CURVE ( 'NONE', #56941, #84744, #59108, .T. ) ;
#80366 = CARTESIAN_POINT ( 'NONE',  ( 28.57499999999999929, 77.96728223830740490, 310.8325000000000387 ) ) ;
#80367 = ORIENTED_EDGE ( 'NONE', *, *, #2329, .T. ) ;
#80368 = EDGE_CURVE ( 'NONE', #65464, #27479, #32298, .T. ) ;
#80369 = VECTOR ( 'NONE', #24028, 1000.000000000000000 ) ;
#80370 = FACE_OUTER_BOUND ( 'NONE', #48153, .T. ) ;
#80371 = CIRCLE ( 'NONE', #20908, 0.5000000000000004441 ) ;
#80372 = LINE ( 'NONE', #18121, #10693 ) ;
#80373 = CARTESIAN_POINT ( 'NONE',  ( 110.7254274611716056, -26.32387412717027786, 254.8194347997205682 ) ) ;
#80374 = DIRECTION ( 'NONE',  ( 1.000000000000000078E-15, -1.000000000000000000, 0.000000000000000000 ) ) ;
#80375 = CARTESIAN_POINT ( 'NONE',  ( -185.9961463128564958, 20.32000000000000028, -9.525000000000000355 ) ) ;
#80376 = CARTESIAN_POINT ( 'NONE',  ( 77.55659459556547120, -37.85370728022186171, 2.783021134850681477 ) ) ;
#80377 = EDGE_CURVE ( 'NONE', #65034, #70844, #67274, .T. ) ;
#80378 = CARTESIAN_POINT ( 'NONE',  ( 99.32305605351064060, -40.33436967443800825, 256.0952769709339236 ) ) ;
#80380 = CARTESIAN_POINT ( 'NONE',  ( 106.8416606513710008, -48.55305329746386178, 73.56133956162497611 ) ) ;
#80379 = DIRECTION ( 'NONE',  ( 0.000000000000000000, 1.000000000000000000, 0.000000000000000000 ) ) ;
#80381 = CARTESIAN_POINT ( 'NONE',  ( 109.3721747360122691, 56.79532162893549696, 71.29316779583847108 ) ) ;
#80382 = CARTESIAN_POINT ( 'NONE',  ( 95.98102948456921979, -37.30005869795228080, 121.3794347997209684 ) ) ;
#80383 = ORIENTED_EDGE ( 'NONE', *, *, #79030, .T. ) ;
#80384 = CARTESIAN_POINT ( 'NONE',  ( 83.56670559755357885, -36.73837296219067383, 249.5838068554176630 ) ) ;
#80385 = EDGE_LOOP ( 'NONE', ( #84638, #56143, #63925, #57708 ) ) ;
#80386 = CARTESIAN_POINT ( 'NONE',  ( 72.26648329127297643, -1.929447159941394263, 361.9756252759109998 ) ) ;
#80387 = CIRCLE ( 'NONE', #70186, 2.117000000000007987 ) ;
#80388 = CARTESIAN_POINT ( 'NONE',  ( -24.79284581386642827, 184.0000000000000000, 101.0189074266571794 ) ) ;
#80389 = CARTESIAN_POINT ( 'NONE',  ( 135.3321452824027631, -34.28157797493338421, 1.873071231924423374 ) ) ;
#80390 = ORIENTED_EDGE ( 'NONE', *, *, #42084, .T. ) ;
#80391 = EDGE_CURVE ( 'NONE', #84281, #29010, #28317, .T. ) ;
#80392 = DIRECTION ( 'NONE',  ( 0.000000000000000000, 1.000000000000000000, 0.000000000000000000 ) ) ;
#80394 = ORIENTED_EDGE ( 'NONE', *, *, #48678, .F. ) ;
#80393 = CARTESIAN_POINT ( 'NONE',  ( 117.6400240572639575, -42.19104337252187520, 93.44705384733897802 ) ) ;
#80395 = DIRECTION ( 'NONE',  ( 0.000000000000000000, 0.000000000000000000, -1.000000000000000000 ) ) ;
#80396 = DIRECTION ( 'NONE',  ( 1.000000000000000000, 0.000000000000000000, 0.000000000000000000 ) ) ;
#80397 = LINE ( 'NONE', #74013, #30783 ) ;
#80398 = VERTEX_POINT ( 'NONE', #66373 ) ;
#80399 = CARTESIAN_POINT ( 'NONE',  ( 117.3857798876165788, -38.35993227889734669, 113.7013395616249767 ) ) ;
#80400 = CARTESIAN_POINT ( 'NONE',  ( 61.56670390244727287, -23.42844715994024085, 300.4678068554150627 ) ) ;
#80401 = CARTESIAN_POINT ( 'NONE',  ( 91.91125933621934507, -111.8737466215628160, -19.26696060647578435 ) ) ;
#80402 = VERTEX_POINT ( 'NONE', #38672 ) ;
#80403 = ORIENTED_EDGE ( 'NONE', *, *, #70336, .F. ) ;
#80404 = FACE_OUTER_BOUND ( 'NONE', #26488, .T. ) ;
#80405 = CARTESIAN_POINT ( 'NONE',  ( 194.0371591254575208, -24.42818131005417115, 180.4678068554150343 ) ) ;
#80406 = DIRECTION ( 'NONE',  ( 0.000000000000000000, 0.000000000000000000, 1.000000000000000000 ) ) ;
#80409 = EDGE_CURVE ( 'NONE', #69770, #61270, #86842, .T. ) ;
#80408 = CARTESIAN_POINT ( 'NONE',  ( -11.41378189430731993, 76.91903266065129685, -118.0057337156638653 ) ) ;
#80407 = PLANE ( 'NONE',  #8841 ) ;
#80410 = CARTESIAN_POINT ( 'NONE',  ( 108.4173540871620389, -26.73501544328009416, 179.9689693287395755 ) ) ;
#80411 = CIRCLE ( 'NONE', #41212, 2.500000000000002220 ) ;
#80412 = ORIENTED_EDGE ( 'NONE', *, *, #28415, .F. ) ;
#80413 = AXIS2_PLACEMENT_3D ( 'NONE', #53174, #25506, #26407 ) ;
#80414 = CARTESIAN_POINT ( 'NONE',  ( 105.7154775075611752, -46.72385841472092949, 33.46895862334973515 ) ) ;
#80415 = CARTESIAN_POINT ( 'NONE',  ( 99.76930146980372172, -30.21680002102814555, 186.7470538473389752 ) ) ;
#80417 = ORIENTED_EDGE ( 'NONE', *, *, #80669, .F. ) ;
#80416 = FACE_OUTER_BOUND ( 'NONE', #73423, .T. ) ;
#80418 = CARTESIAN_POINT ( 'NONE',  ( 102.2761128416349692, -28.20209198692217356, 56.48419670448195973 ) ) ;
#80419 = CARTESIAN_POINT ( 'NONE',  ( 110.8542252850209309, -45.98433833104029844, 52.88560406628666044 ) ) ;
#80420 = DIRECTION ( 'NONE',  ( -0.9217329428042198014, -0.3878251953515564066, 1.214306433183767175E-14 ) ) ;
#80421 = DIRECTION ( 'NONE',  ( 0.000000000000000000, -0.7071067811865321406, -0.7071067811865628938 ) ) ;
#80422 = ORIENTED_EDGE ( 'NONE', *, *, #32765, .T. ) ;
#80423 = ADVANCED_FACE ( 'NONE', ( #73645 ), #12324, .T. ) ;
#80424 = FACE_OUTER_BOUND ( 'NONE', #75425, .T. ) ;
#80425 = ORIENTED_EDGE ( 'NONE', *, *, #533, .T. ) ;
#80426 = ORIENTED_EDGE ( 'NONE', *, *, #56319, .F. ) ;
#80427 = CARTESIAN_POINT ( 'NONE',  ( 114.5371455856629694, -43.48665885088448135, 229.6730118773259619 ) ) ;
#80428 = EDGE_CURVE ( 'NONE', #16796, #87491, #31860, .T. ) ;
#80429 = LINE ( 'NONE', #67684, #15406 ) ;
#80430 = AXIS2_PLACEMENT_3D ( 'NONE', #19178, #8695, #41829 ) ;
#80431 =( GEOMETRIC_REPRESENTATION_CONTEXT ( 3 ) GLOBAL_UNCERTAINTY_ASSIGNED_CONTEXT ( ( #29649 ) ) GLOBAL_UNIT_ASSIGNED_CONTEXT ( ( #8131, #21772, #85796 ) ) REPRESENTATION_CONTEXT ( 'NONE', 'WORKASPACE' ) );
#80432 = CARTESIAN_POINT ( 'NONE',  ( -72.96458098368600531, 117.4749999999999943, -72.96458098368781009 ) ) ;
#80433 = AXIS2_PLACEMENT_3D ( 'NONE', #37029, #64735, #43378 ) ;
#80434 = LINE ( 'NONE', #10928, #25764 ) ;
#80435 = CARTESIAN_POINT ( 'NONE',  ( 80.81785596310795938, -39.40256188477532362, 1.690787648074149496 ) ) ;
#80436 = ORIENTED_EDGE ( 'NONE', *, *, #20016, .F. ) ;
#80437 = LINE ( 'NONE', #33169, #8754 ) ;
#80438 = VECTOR ( 'NONE', #2945, 1000.000000000000000 ) ;
#80439 = CARTESIAN_POINT ( 'NONE',  ( 98.34811578340129756, -31.65970814803674571, 36.90641431777298465 ) ) ;
#80440 = ORIENTED_EDGE ( 'NONE', *, *, #21315, .F. ) ;
#80441 = CARTESIAN_POINT ( 'NONE',  ( 96.91023542590092177, -30.67149048741783091, 280.8984824187682534 ) ) ;
#80442 = CARTESIAN_POINT ( 'NONE',  ( 12.37156061772173388, 85.44992509219818544, 117.9087631476423041 ) ) ;
#80443 = ORIENTED_EDGE ( 'NONE', *, *, #65811, .T. ) ;
#80444 = CARTESIAN_POINT ( 'NONE',  ( 104.1201707603140107, -29.11702517433068138, 213.1880903695919756 ) ) ;
#80445 = CARTESIAN_POINT ( 'NONE',  ( 21.03715912545829170, -47.82818131006186491, 249.9678068554150059 ) ) ;
#80446 = CARTESIAN_POINT ( 'NONE',  ( -71.77848634863029531, 127.0000000000000000, -77.39114642430038771 ) ) ;
#80447 = DIRECTION ( 'NONE',  ( 0.000000000000000000, 0.000000000000000000, -1.000000000000000000 ) ) ;
#80448 = PLANE ( 'NONE',  #15779 ) ;
#80449 = CARTESIAN_POINT ( 'NONE',  ( 97.05457585776278506, -41.52102392564493272, 212.6937205140059461 ) ) ;
#80450 = CARTESIAN_POINT ( 'NONE',  ( 194.5667039024483529, -47.82844715993405771, 249.9678068554149775 ) ) ;
#80451 = VERTEX_POINT ( 'NONE', #11880 ) ;
#80452 = CARTESIAN_POINT ( 'NONE',  ( 107.6053842629478794, -26.23908965751013156, 91.03562527591097364 ) ) ;
#80453 = CARTESIAN_POINT ( 'NONE',  ( 194.5664832912729878, -18.82844715994100326, 342.9256252759109884 ) ) ;
#80454 = ORIENTED_EDGE ( 'NONE', *, *, #25990, .F. ) ;
#80456 = ADVANCED_FACE ( 'NONE', ( #24609 ), #73191, .T. ) ;
#80455 = ORIENTED_EDGE ( 'NONE', *, *, #43340, .F. ) ;
#80458 = EDGE_LOOP ( 'NONE', ( #25135, #86003, #17671, #87193 ) ) ;
#80457 = EDGE_CURVE ( 'NONE', #70447, #59781, #7379, .T. ) ;
#80459 = EDGE_CURVE ( 'NONE', #3107, #14741, #8040, .T. ) ;
#80460 = CARTESIAN_POINT ( 'NONE',  ( 81.08070086926866793, -16.17316201338597992, 1.785258157649182165 ) ) ;
#80461 = CARTESIAN_POINT ( 'NONE',  ( 71.06648329127399677, -18.82844715994099971, 284.9256252759119548 ) ) ;
#80462 = DIRECTION ( 'NONE',  ( 0.000000000000000000, 1.000000000000000000, 0.000000000000000000 ) ) ;
#80463 = CARTESIAN_POINT ( 'NONE',  ( 104.0192455041231767, -29.15686055524244935, 128.1995189410199600 ) ) ;
#80464 = CARTESIAN_POINT ( 'NONE',  ( 118.8146046005060015, -38.46262239392275717, 219.7099109901969882 ) ) ;
#80465 = CARTESIAN_POINT ( 'NONE',  ( 116.8180029026503206, -34.15632288917988291, 60.03118074130109960 ) ) ;
#80466 = ORIENTED_EDGE ( 'NONE', *, *, #16391, .F. ) ;
#80467 = EDGE_CURVE ( 'NONE', #10437, #16028, #38, .T. ) ;
#80468 = CYLINDRICAL_SURFACE ( 'NONE', #60645, 8.636000000000004562 ) ;
#80469 = ORIENTED_EDGE ( 'NONE', *, *, #22683, .T. ) ;
#80470 = ORIENTED_EDGE ( 'NONE', *, *, #74928, .T. ) ;
#80471 = CIRCLE ( 'NONE', #81977, 0.5000000000000004441 ) ;
#80472 = DIRECTION ( 'NONE',  ( 0.000000000000000000, -1.000000000000000000, 0.000000000000000000 ) ) ;
#80473 = ORIENTED_EDGE ( 'NONE', *, *, #86809, .T. ) ;
#80474 = ORIENTED_EDGE ( 'NONE', *, *, #2635, .T. ) ;
#80475 = LINE ( 'NONE', #18236, #88968 ) ;
#80476 = VECTOR ( 'NONE', #69432, 1000.000000000000000 ) ;
#80477 = CARTESIAN_POINT ( 'NONE',  ( 135.5667039024470171, -90.27844715994091018, 45.21780685541799727 ) ) ;
#80478 = FACE_OUTER_BOUND ( 'NONE', #7495, .T. ) ;
#80479 = ADVANCED_FACE ( 'NONE', ( #482 ), #62703, .T. ) ;
#80481 = CARTESIAN_POINT ( 'NONE',  ( 99.77605516222793369, -32.27907757783855658, 170.3124198280769974 ) ) ;
#80480 = B_SPLINE_CURVE_WITH_KNOTS ( 'NONE', 3,
 ( #72790, #30115, #3307, #65081, #43730, #86872, #30562, #51866, #16490, #24198, #80065, #24633, #2863, #44169, #71467, #10118, #58260, #45063 ),
 .UNSPECIFIED., .F., .F.,
 ( 4, 2, 2, 2, 2, 2, 2, 2, 4 ),
 ( 0.4999681725817722855, 0.5624721510090507914, 0.6249761294363291864, 0.6874801078636076923, 0.7499840862908861983, 0.8124880647181645932, 0.8749920431454430991, 0.9374960215727214941, 1.000000000000000000 ),
 .UNSPECIFIED. ) ;
#80482 = CARTESIAN_POINT ( 'NONE',  ( 118.2557925370599179, -40.78261322564650015, 23.54991099019593292 ) ) ;
#80483 = ORIENTED_EDGE ( 'NONE', *, *, #19957, .F. ) ;
#80484 = PLANE ( 'NONE',  #55669 ) ;
#80485 = ORIENTED_EDGE ( 'NONE', *, *, #46600, .T. ) ;
#80486 = CYLINDRICAL_SURFACE ( 'NONE', #89648, 0.9999999999991942001 ) ;
#80487 = VERTEX_POINT ( 'NONE', #83614 ) ;
#80488 = CARTESIAN_POINT ( 'NONE',  ( 97.45633071946963355, -39.50260968302539055, 167.5502217315908808 ) ) ;
#80489 = CARTESIAN_POINT ( 'NONE',  ( 2.684158038187649039E-15, 69.84999999999999432, -130.5560000000000116 ) ) ;
#80490 = CARTESIAN_POINT ( 'NONE',  ( 123.6837132603318992, -53.34645651782490461, 239.5838068554164693 ) ) ;
#80491 = CARTESIAN_POINT ( 'NONE',  ( 25.56670390244805091, -42.82844715994167473, 293.2178068554150059 ) ) ;
#80492 = ORIENTED_EDGE ( 'NONE', *, *, #47258, .F. ) ;
#80493 = CARTESIAN_POINT ( 'NONE',  ( 116.4944971008961261, -32.22846566477972630, 19.18133956162493092 ) ) ;
#80494 = VECTOR ( 'NONE', #67205, 1000.000000000000000 ) ;
#80495 = CARTESIAN_POINT ( 'NONE',  ( 96.64260770218685082, -42.46999856532355011, 22.72705384733997391 ) ) ;
#80496 = VECTOR ( 'NONE', #34829, 1000.000000000000000 ) ;
#80497 =( NAMED_UNIT ( * ) SI_UNIT ( $, .STERADIAN. ) SOLID_ANGLE_UNIT ( ) );
#80498 = VECTOR ( 'NONE', #88180, 1000.000000000000000 ) ;
#80500 = DIRECTION ( 'NONE',  ( -3.100000000000000258E-29, 3.100000000000000044E-14, 1.000000000000000000 ) ) ;
#80499 = CARTESIAN_POINT ( 'NONE',  ( 150.5667039024476139, -25.42844715993593852, 129.9678068554149775 ) ) ;
#80501 = CARTESIAN_POINT ( 'NONE',  ( 172.5664832912729878, -27.82844715994070484, 138.9256252759119832 ) ) ;
#80502 = CARTESIAN_POINT ( 'NONE',  ( 144.0667052733537901, -71.37844715994090450, 55.21780685541800437 ) ) ;
#80503 = DIRECTION ( 'NONE',  ( 0.000000000000000000, 0.000000000000000000, 1.000000000000000000 ) ) ;
#80504 = AXIS2_PLACEMENT_3D ( 'NONE', #26977, #68312, #47842 ) ;
#80505 = AXIS2_PLACEMENT_3D ( 'NONE', #52662, #87234, #5905 ) ;
#80506 = DIRECTION ( 'NONE',  ( 0.000000000000000000, 1.000000000000000000, 0.000000000000000000 ) ) ;
#80507 = CARTESIAN_POINT ( 'NONE',  ( 173.9900000000000091, 20.32000000000000028, 71.37400000000000944 ) ) ;
#80508 = CARTESIAN_POINT ( 'NONE',  ( 95.20909952976953150, -35.71394341709248721, 36.25848241876794731 ) ) ;
#80509 = CARTESIAN_POINT ( 'NONE',  ( 103.8197751496740011, -48.12653019911325458, 213.3556252759109668 ) ) ;
#80510 = CARTESIAN_POINT ( 'NONE',  ( 107.8700274897790479, -26.31351822515222949, 66.01562527591097762 ) ) ;
#80513 = EDGE_CURVE ( 'NONE', #73956, #52482, #66044, .T. ) ;
#80512 = FACE_OUTER_BOUND ( 'NONE', #45538, .T. ) ;
#80511 = DIRECTION ( 'NONE',  ( 0.000000000000000000, 0.000000000000000000, -1.000000000000000000 ) ) ;
#80514 = CARTESIAN_POINT ( 'NONE',  ( 81.01407827912798609, -34.14703303315388183, 1.764000745016844007 ) ) ;
#80515 = EDGE_CURVE ( 'NONE', #65403, #33963, #36666, .T. ) ;
#80516 = VECTOR ( 'NONE', #10211, 1000.000000000000000 ) ;
#80517 = ORIENTED_EDGE ( 'NONE', *, *, #23231, .F. ) ;
#80518 = CARTESIAN_POINT ( 'NONE',  ( 32.09598329128129279, -23.42844715994118587, 313.9678068554150059 ) ) ;
#80519 = ORIENTED_EDGE ( 'NONE', *, *, #64697, .F. ) ;
#80520 = CARTESIAN_POINT ( 'NONE',  ( 116.7274023843878581, -38.25590632018514725, 109.7013395616249767 ) ) ;
#80522 = ORIENTED_EDGE ( 'NONE', *, *, #52956, .F. ) ;
#80521 = DIRECTION ( 'NONE',  ( 0.9999999853157766072, 0.0001713722456126751754, 0.000000000000000000 ) ) ;
#80523 = FACE_BOUND ( 'NONE', #61708, .T. ) ;
#80524 = CARTESIAN_POINT ( 'NONE',  ( 109.9541224118590321, -48.19721710984605068, 238.7727681330539724 ) ) ;
#80525 = LINE ( 'NONE', #4213, #61418 ) ;
#80526 = CARTESIAN_POINT ( 'NONE',  ( 31.56670390244800828, -33.35206098992711077, -5.074374724088000832 ) ) ;
#80527 = CARTESIAN_POINT ( 'NONE',  ( 234.0013031625829854, 52.73749999999999716, -2.032000000000000028 ) ) ;
#80528 = CARTESIAN_POINT ( 'NONE',  ( 108.0667039024470455, -121.2010968907524529, -19.26696060647547881 ) ) ;
#80529 = CARTESIAN_POINT ( 'NONE',  ( 194.5664832912739826, 0.2215528400590083269, 323.8756252759109202 ) ) ;
#80530 = FACE_OUTER_BOUND ( 'NONE', #38978, .T. ) ;
#80531 = CARTESIAN_POINT ( 'NONE',  ( 98.51953950620406886, -30.85675296092858844, 165.8594347997209582 ) ) ;
#80532 = ORIENTED_EDGE ( 'NONE', *, *, #14096, .F. ) ;
#80533 = ORIENTED_EDGE ( 'NONE', *, *, #78679, .F. ) ;
#80534 = VECTOR ( 'NONE', #23941, 1000.000000000000000 ) ;
#80535 = CARTESIAN_POINT ( 'NONE',  ( 116.0874278420761527, -39.35605806303598797, 135.0206309249449532 ) ) ;
#80536 = ADVANCED_FACE ( 'NONE', ( #34992 ), #7305, .F. ) ;
#80537 = FACE_OUTER_BOUND ( 'NONE', #73654, .T. ) ;
#80539 = CARTESIAN_POINT ( 'NONE',  ( 154.5667039024469886, -67.87844715994090450, 155.2178068554179902 ) ) ;
#80538 = CARTESIAN_POINT ( 'NONE',  ( 110.6561457788924230, -27.59554888373227755, 265.7784824187677941 ) ) ;
#80540 = CIRCLE ( 'NONE', #37027, 13.31747058675099815 ) ;
#80541 = DIRECTION ( 'NONE',  ( 3.999999999999999995E-14, -1.000000000000000000, 4.100000000000000342E-29 ) ) ;
#80542 = CARTESIAN_POINT ( 'NONE',  ( 188.5667039024486087, -48.82844715993430640, 134.7178068554150059 ) ) ;
#80543 = MANIFOLD_SOLID_BREP ( 'Stock-BR-Y-104-1', #74990 ) ;
#80544 = CARTESIAN_POINT ( 'NONE',  ( 118.3861417219090555, 71.54629894495526798, -6.354613972968428115 ) ) ;
#80545 = DIRECTION ( 'NONE',  ( 0.000000000000000000, 0.000000000000000000, -1.000000000000000000 ) ) ;
#80546 = FACE_OUTER_BOUND ( 'NONE', #49082, .T. ) ;
#80547 = CYLINDRICAL_SURFACE ( 'NONE', #18346, 4.874999999999990230 ) ;
#80548 = CARTESIAN_POINT ( 'NONE',  ( 114.7977927517518566, -29.71579763117545880, 209.4127681330539872 ) ) ;
#80549 = VERTEX_POINT ( 'NONE', #50410 ) ;
#80550 = EDGE_LOOP ( 'NONE', ( #70275, #6754, #2259, #82199 ) ) ;
#80551 = PRODUCT_DEFINITION ( 'UNKNOWN', '', #34839, #77813 ) ;
#80552 = CARTESIAN_POINT ( 'NONE',  ( 136.4247830841161999, -74.33686277290898659, 248.4067532124560103 ) ) ;
#80553 = CARTESIAN_POINT ( 'NONE',  ( 147.0665874381622018, -67.87844715994090450, 245.5130140176639770 ) ) ;
#80554 = PLANE ( 'NONE',  #1165 ) ;
#80555 = CARTESIAN_POINT ( 'NONE',  ( 106.1586424053105873, -87.30271670975442078, -11.78219314458253741 ) ) ;
#80556 = AXIS2_PLACEMENT_3D ( 'NONE', #35260, #21662, #84346 ) ;
#80557 = ORIENTED_EDGE ( 'NONE', *, *, #18030, .T. ) ;
#80558 = AXIS2_PLACEMENT_3D ( 'NONE', #88, #26002, #60963 ) ;
#80559 = CARTESIAN_POINT ( 'NONE',  ( 109.6412877908718713, -46.48052073322395472, 62.78131853186246047 ) ) ;
#80560 = AXIS2_PLACEMENT_3D ( 'NONE', #8369, #76508, #15637 ) ;
#80561 = VECTOR ( 'NONE', #20474, 1000.000000000000114 ) ;
#80562 = CARTESIAN_POINT ( 'NONE',  ( 98.03659727384791722, -44.40418782976336587, 226.8870538473399563 ) ) ;
#80563 = CARTESIAN_POINT ( 'NONE',  ( 136.2679348342933281, -38.38027623202234651, 7.385026757022528088 ) ) ;
#80564 = ORIENTED_EDGE ( 'NONE', *, *, #43669, .F. ) ;
#80566 = ORIENTED_EDGE ( 'NONE', *, *, #58631, .T. ) ;
#80565 = EDGE_CURVE ( 'NONE', #80780, #38663, #64639, .T. ) ;
#80567 = VECTOR ( 'NONE', #72128, 1000.000000000000000 ) ;
#80568 = ADVANCED_FACE ( 'NONE', ( #50865 ), #78154, .T. ) ;
#80569 = CARTESIAN_POINT ( 'NONE',  ( 116.9574880481188899, -38.55991405319311127, 64.68174541508243180 ) ) ;
#80570 = DIRECTION ( 'NONE',  ( 0.2011513310014971800, -0.7071067811865459074, 0.6778924265960850626 ) ) ;
#80571 = ADVANCED_FACE ( 'NONE', ( #15014, #3175 ), #22281, .T. ) ;
#80572 = CARTESIAN_POINT ( 'NONE',  ( 97.83899624421785290, -40.58356376421257750, 166.6413203159688976 ) ) ;
#80573 = CARTESIAN_POINT ( 'NONE',  ( 102.2704046875766579, -44.67259270758150080, 49.96237608387698970 ) ) ;
#80574 = AXIS2_PLACEMENT_3D ( 'NONE', #2665, #78970, #2211 ) ;
#80575 = CYLINDRICAL_SURFACE ( 'NONE', #68169, 0.2500000000000002220 ) ;
#80576 = ORIENTED_EDGE ( 'NONE', *, *, #89275, .F. ) ;
#80577 = EDGE_CURVE ( 'NONE', #38949, #52724, #16797, .T. ) ;
#80578 = AXIS2_PLACEMENT_3D ( 'NONE', #38275, #2879, #45511 ) ;
#80579 = CARTESIAN_POINT ( 'NONE',  ( 172.5667039024478129, -36.32844715993500273, 300.4678068554149490 ) ) ;
#80580 = CARTESIAN_POINT ( 'NONE',  ( 82.18073802037548603, -16.97076862298585453, 7.459445689451158934 ) ) ;
#80581 = VERTEX_POINT ( 'NONE', #43590 ) ;
#80582 = ORIENTED_EDGE ( 'NONE', *, *, #1203, .F. ) ;
#80583 = DIRECTION ( 'NONE',  ( 0.000000000000000000, -1.000000000000000000, 0.000000000000000000 ) ) ;
#80584 = ORIENTED_EDGE ( 'NONE', *, *, #20397, .F. ) ;
#80585 = VERTEX_POINT ( 'NONE', #15473 ) ;
#80586 = CARTESIAN_POINT ( 'NONE',  ( 108.4153923495623104, -26.73476988454542536, 155.9688923574878743 ) ) ;
#80587 = AXIS2_PLACEMENT_3D ( 'NONE', #21525, #8335, #15150 ) ;
#80588 = EDGE_CURVE ( 'NONE', #46935, #41326, #57220, .T. ) ;
#80589 = CARTESIAN_POINT ( 'NONE',  ( 99.48186602960301173, -30.66774701162068695, 45.21241982807700310 ) ) ;
#80590 = CARTESIAN_POINT ( 'NONE',  ( 101.1881973814857076, -45.36612005690837890, 197.1013395616249966 ) ) ;
#80591 = CARTESIAN_POINT ( 'NONE',  ( 116.7861719071672866, -43.46560779248406448, 163.3441967044829823 ) ) ;
#80592 = EDGE_CURVE ( 'NONE', #57125, #62710, #36798, .T. ) ;
#80594 = CARTESIAN_POINT ( 'NONE',  ( 96.76336351750784104, -35.13941245127819002, 262.2041967044821149 ) ) ;
#80593 = CARTESIAN_POINT ( 'NONE',  ( 99.18578730576537339, -42.92413673961824117, 21.85661952785993378 ) ) ;
#80595 = CARTESIAN_POINT ( 'NONE',  ( -187.8075999999999794, 101.5999999999999943, 114.2999999999999972 ) ) ;
#80596 = CARTESIAN_POINT ( 'NONE',  ( 31.71315051186898870, -31.94127993907790852, -5.074374724088000832 ) ) ;
#80597 = EDGE_LOOP ( 'NONE', ( #67425, #59828, #33415, #50164 ) ) ;
#80598 = ORIENTED_EDGE ( 'NONE', *, *, #79066, .F. ) ;
#80599 = CIRCLE ( 'NONE', #53286, 0.5000000000000004441 ) ;
#80600 = LINE ( 'NONE', #39246, #879 ) ;
#80601 = CARTESIAN_POINT ( 'NONE',  ( 109.9724474192709351, -48.26999177473817326, 242.7727681330539724 ) ) ;
#80602 = ORIENTED_EDGE ( 'NONE', *, *, #58424, .T. ) ;
#80603 = CARTESIAN_POINT ( 'NONE',  ( 103.5423316596719445, -26.88027146080960961, 190.3499109901969746 ) ) ;
#80604 = LINE ( 'NONE', #25621, #80516 ) ;
#80605 = CIRCLE ( 'NONE', #73318, 0.5000000000000129896 ) ;
#80606 = CARTESIAN_POINT ( 'NONE',  ( -19.19064667470416197, 64.29050366814337281, 32.91834566403962015 ) ) ;
#80607 = DIRECTION ( 'NONE',  ( -1.000000000000000078E-15, -1.000000000000000083E-30, 1.000000000000000000 ) ) ;
#80608 = CARTESIAN_POINT ( 'NONE',  ( 162.0667039024469886, -67.87844715994089029, 222.2178068554179902 ) ) ;
#80611 = CARTESIAN_POINT ( 'NONE',  ( 114.3996560367811099, -27.45190519937929707, 270.5441967044823741 ) ) ;
#80610 = CARTESIAN_POINT ( 'NONE',  ( 24.79284581386643183, 184.0000000000000000, 101.0189074266571794 ) ) ;
#80609 = CARTESIAN_POINT ( 'NONE',  ( 109.2954090318264377, -45.76736768674248168, 277.6356252759110816 ) ) ;
#80612 = CARTESIAN_POINT ( 'NONE',  ( 182.4202572930257134, -31.94127993907681073, 342.9256252759109884 ) ) ;
#80613 = LINE ( 'NONE', #62826, #32281 ) ;
#80614 = DIRECTION ( 'NONE',  ( 0.000000000000000000, 0.000000000000000000, 1.000000000000000000 ) ) ;
#80615 = CARTESIAN_POINT ( 'NONE',  ( 123.6837132603319560, -53.34645651782485487, 219.5838068554170093 ) ) ;
#80616 = PLANE ( 'NONE',  #67707 ) ;
#80617 = DIRECTION ( 'NONE',  ( 0.000000000000000000, 1.000000000000000000, 0.000000000000000000 ) ) ;
#80619 = ORIENTED_EDGE ( 'NONE', *, *, #7549, .F. ) ;
#80618 = CARTESIAN_POINT ( 'NONE',  ( -11.41184330286787052, 88.18497404666861428, -118.0059224074909707 ) ) ;
#80620 = CARTESIAN_POINT ( 'NONE',  ( 136.5939002653058196, -19.81452881268075572, 7.047625865513104770 ) ) ;
#80621 = CARTESIAN_POINT ( 'NONE',  ( 96.10188529952328906, -35.15685947849579662, 226.2251490854349640 ) ) ;
#80622 = CARTESIAN_POINT ( 'NONE',  ( 101.7559735582952953, -27.03550746236556890, 96.46324432352997746 ) ) ;
#80623 = CARTESIAN_POINT ( 'NONE',  ( 98.86476787746175887, -29.25085353348518424, 226.7261014663869503 ) ) ;
#80624 = DIRECTION ( 'NONE',  ( 0.000000000000000000, 0.000000000000000000, 1.000000000000000000 ) ) ;
#80627 = EDGE_CURVE ( 'NONE', #82808, #12675, #77243, .T. ) ;
#80626 = DIRECTION ( 'NONE',  ( 0.000000000000000000, -1.000000000000000000, 0.000000000000000000 ) ) ;
#80625 = CYLINDRICAL_SURFACE ( 'NONE', #33324, 3.250000000000002665 ) ;
#80628 = DIRECTION ( 'NONE',  ( 0.000000000000000000, -1.000000000000000000, 0.000000000000000000 ) ) ;
#80629 = DIRECTION ( 'NONE',  ( 0.000000000000000000, 1.000000000000000000, 0.000000000000000000 ) ) ;
#80630 = VECTOR ( 'NONE', #61737, 1000.000000000000000 ) ;
#80631 = VECTOR ( 'NONE', #77298, 1000.000000000000000 ) ;
#80632 = VECTOR ( 'NONE', #64125, 1000.000000000000000 ) ;
#80633 = EDGE_CURVE ( 'NONE', #13721, #33634, #2280, .T. ) ;
#80634 = ORIENTED_EDGE ( 'NONE', *, *, #80952, .T. ) ;
#80635 = EDGE_LOOP ( 'NONE', ( #17119, #75451, #32280, #16465 ) ) ;
#80636 = CARTESIAN_POINT ( 'NONE',  ( 110.9399543235443559, -27.82625392046294266, 134.1724198280769826 ) ) ;
#80638 = ORIENTED_EDGE ( 'NONE', *, *, #31867, .T. ) ;
#80637 = PLANE ( 'NONE',  #45848 ) ;
#80639 = CARTESIAN_POINT ( 'NONE',  ( 34.92499999999999716, 69.84999999999999432, 292.1000000000000227 ) ) ;
#80640 = CARTESIAN_POINT ( 'NONE',  ( 117.6812658759004222, -39.72780374360937827, 139.6194347997199827 ) ) ;
#80641 = LINE ( 'NONE', #18849, #67132 ) ;
#80642 = CIRCLE ( 'NONE', #42672, 4.875000000000017764 ) ;
#80643 = DIRECTION ( 'NONE',  ( -4.299999999999999979E-14, 1.000000000000000000, -4.400000000000000367E-29 ) ) ;
#80644 = DIRECTION ( 'NONE',  ( -0.4999999999999994449, -0.8660254037844390407, 2.684678751731759347E-14 ) ) ;
#80645 = DIRECTION ( 'NONE',  ( 0.000000000000000000, 1.000000000000000000, 0.000000000000000000 ) ) ;
#80647 = CARTESIAN_POINT ( 'NONE',  ( 97.35459460924916186, -38.14118110200430323, 66.44133956162595211 ) ) ;
#80646 = VECTOR ( 'NONE', #14958, 1000.000000000000000 ) ;
#80648 = ORIENTED_EDGE ( 'NONE', *, *, #39630, .T. ) ;
#80649 = ORIENTED_EDGE ( 'NONE', *, *, #64174, .F. ) ;
#80650 = ORIENTED_EDGE ( 'NONE', *, *, #29622, .T. ) ;
#80651 = ADVANCED_FACE ( 'NONE', ( #63607 ), #36351, .F. ) ;
#80652 = FACE_OUTER_BOUND ( 'NONE', #72586, .T. ) ;
#80654 = LINE ( 'NONE', #51135, #89721 ) ;
#80653 = CARTESIAN_POINT ( 'NONE',  ( 113.7357275853186280, -44.67049210939290305, 144.1203871806719690 ) ) ;
#80655 = CIRCLE ( 'NONE', #51576, 218.1859999999999786 ) ;
#80656 = DIRECTION ( 'NONE',  ( -1.000000000000000000, 0.000000000000000000, -2.108231265501709878E-16 ) ) ;
#80657 = DIRECTION ( 'NONE',  ( 0.000000000000000000, 0.000000000000000000, -1.000000000000000000 ) ) ;
#80658 = CARTESIAN_POINT ( 'NONE',  ( 141.8164832912739826, -8.729447159940995959, 14.67562527591100441 ) ) ;
#80659 = CARTESIAN_POINT ( 'NONE',  ( 92.32962665258456525, 83.38952084682853183, 74.36911441044827598 ) ) ;
#80660 = CARTESIAN_POINT ( 'NONE',  ( 67.06681736700808472, -67.87844715931913697, 245.5130139978070076 ) ) ;
#80661 = CARTESIAN_POINT ( 'NONE',  ( 100.9560042165379059, -28.30978499293925310, 75.57562527591093726 ) ) ;
#80662 = EDGE_LOOP ( 'NONE', ( #32014, #81299, #25982 ) ) ;
#80663 = ORIENTED_EDGE ( 'NONE', *, *, #1946, .T. ) ;
#80664 = EDGE_CURVE ( 'NONE', #3721, #51322, #87851, .T. ) ;
#80665 = CARTESIAN_POINT ( 'NONE',  ( 107.0667039024470313, -104.2784471599409528, 24.21780685541800082 ) ) ;
#80666 = DIRECTION ( 'NONE',  ( 0.9586846635221889512, 0.000000000000000000, -0.2844709403917162205 ) ) ;
#80667 = DIRECTION ( 'NONE',  ( -1.000000000000000000, 0.000000000000000000, 0.000000000000000000 ) ) ;
#80668 = CARTESIAN_POINT ( 'NONE',  ( 103.1394548971403680, -44.44173430692483606, 170.0318998934009755 ) ) ;
#80669 = EDGE_CURVE ( 'NONE', #75722, #10086, #85422, .T. ) ;
#80670 = CARTESIAN_POINT ( 'NONE',  ( 180.1667039024460166, -26.71338133339240528, -5.074374724088000832 ) ) ;
#80671 = ORIENTED_EDGE ( 'NONE', *, *, #11132, .F. ) ;
#80672 = ORIENTED_EDGE ( 'NONE', *, *, #28772, .F. ) ;
#80673 = DIRECTION ( 'NONE',  ( -3.100000000000000258E-29, 3.100000000000000044E-14, 1.000000000000000000 ) ) ;
#80674 = ORIENTED_EDGE ( 'NONE', *, *, #71783, .T. ) ;
#80675 = ORIENTED_EDGE ( 'NONE', *, *, #27463, .F. ) ;
#80676 = CARTESIAN_POINT ( 'NONE',  ( 77.40528906089566874, -19.42303004212691775, 6.877070700249886315 ) ) ;
#80677 = ADVANCED_FACE ( 'NONE', ( #44483 ), #37694, .T. ) ;
#80678 = CARTESIAN_POINT ( 'NONE',  ( 104.8455658278054017, -28.15064746346142144, 196.7101547344689720 ) ) ;
#80679 = CARTESIAN_POINT ( 'NONE',  ( 160.5667039024428391, -48.82844715994099971, 180.4678068554150059 ) ) ;
#80680 = AXIS2_PLACEMENT_3D ( 'NONE', #70399, #36326, #12407 ) ;
#80681 = PLANE ( 'NONE',  #61769 ) ;
#80682 = CARTESIAN_POINT ( 'NONE',  ( -111.5220324117239556, 65.55856874647801646, 67.88008701381139076 ) ) ;
#80683 = VECTOR ( 'NONE', #18302, 1000.000000000000000 ) ;
#80684 = ORIENTED_EDGE ( 'NONE', *, *, #6410, .T. ) ;
#80685 = ORIENTED_EDGE ( 'NONE', *, *, #14985, .T. ) ;
#80686 = AXIS2_PLACEMENT_3D ( 'NONE', #30775, #69545, #63168 ) ;
#80687 = VECTOR ( 'NONE', #12729, 1000.000000000000000 ) ;
#80688 = AXIS2_PLACEMENT_3D ( 'NONE', #68138, #39077, #68590 ) ;
#80689 = ORIENTED_EDGE ( 'NONE', *, *, #48222, .T. ) ;
#80690 = ORIENTED_EDGE ( 'NONE', *, *, #23157, .F. ) ;
#80691 = EDGE_CURVE ( 'NONE', #45550, #89277, #51737, .T. ) ;
#80692 = CARTESIAN_POINT ( 'NONE',  ( 114.1044565855118265, -40.86425766668616433, 236.2223760838769806 ) ) ;
#80693 = CARTESIAN_POINT ( 'NONE',  ( 102.5485826229696329, -27.30952478670668881, 95.43276813305395478 ) ) ;
#80694 = CARTESIAN_POINT ( 'NONE',  ( 113.4461594614341777, -46.68675298423774223, 68.02991099019695298 ) ) ;
#80695 = EDGE_CURVE ( 'NONE', #71968, #69308, #60280, .T. ) ;
#80696 = CARTESIAN_POINT ( 'NONE',  ( -3.968749999999949818, 120.6499999999999915, -105.4788588808462038 ) ) ;
#80697 = CARTESIAN_POINT ( 'NONE',  ( 114.3200451278417518, -29.78195214854387629, 195.4345394874663384 ) ) ;
#80698 = CARTESIAN_POINT ( 'NONE',  ( 113.5650955083461326, -44.92635950737134465, 164.1099109901969655 ) ) ;
#80699 = CARTESIAN_POINT ( 'NONE',  ( 106.7711676359460000, -46.77985028430433800, 277.5523465834128274 ) ) ;
#80700 = ORIENTED_EDGE ( 'NONE', *, *, #45505, .F. ) ;
#80701 = DIRECTION ( 'NONE',  ( -1.531877379624855416E-14, 0.000000000000000000, 1.000000000000000000 ) ) ;
#80702 = EDGE_LOOP ( 'NONE', ( #18327, #16656, #13005, #25798 ) ) ;
#80703 = ORIENTED_EDGE ( 'NONE', *, *, #71559, .F. ) ;
#80704 = FACE_BOUND ( 'NONE', #32288, .T. ) ;
#80705 = CYLINDRICAL_SURFACE ( 'NONE', #79356, 3.499999999999996003 ) ;
#80706 = AXIS2_PLACEMENT_3D ( 'NONE', #20764, #26073, #45583 ) ;
#80707 = ORIENTED_EDGE ( 'NONE', *, *, #83393, .T. ) ;
#80708 = CARTESIAN_POINT ( 'NONE',  ( -147.4575741623271767, 0.000000000000000000, -135.2444258376735888 ) ) ;
#80709 = EDGE_LOOP ( 'NONE', ( #54465, #35673, #3364, #43618, #30495 ) ) ;
#80710 = CARTESIAN_POINT ( 'NONE',  ( 103.8017946383473031, -27.25047886087329729, 131.3403327703989021 ) ) ;
#80711 = CARTESIAN_POINT ( 'NONE',  ( 115.2672674329477900, -44.14067019768319966, 83.25372051400698581 ) ) ;
#80712 = CARTESIAN_POINT ( 'NONE',  ( -1.594871763261194175, 69.92315485616694559, 130.5484598327008712 ) ) ;
#80713 = VECTOR ( 'NONE', #38383, 1000.000000000000000 ) ;
#80714 = LINE ( 'NONE', #73431, #28962 ) ;
#80715 = DIRECTION ( 'NONE',  ( 1.907762142705490052E-15, 7.167082501179359715E-16, -1.000000000000000000 ) ) ;
#80716 = CARTESIAN_POINT ( 'NONE',  ( 113.1080853710608238, -29.03773216254911915, 79.54705384733995288 ) ) ;
#80718 = CARTESIAN_POINT ( 'NONE',  ( 107.9164806882189254, -47.13338536194948603, 173.6413395616249886 ) ) ;
#80717 = CARTESIAN_POINT ( 'NONE',  ( 0.000000000000000000, 92.07499999999998863, 88.90000000000000568 ) ) ;
#80719 = CARTESIAN_POINT ( 'NONE',  ( 51.06648329127400388, 22.62155284005901024, 339.0006252759110339 ) ) ;
#80720 = CARTESIAN_POINT ( 'NONE',  ( 172.5667039024480687, -36.32844715993499563, 129.9678068554150059 ) ) ;
#80721 = VERTEX_POINT ( 'NONE', #5403 ) ;
#80722 = CARTESIAN_POINT ( 'NONE',  ( 188.5667039024483529, -48.82844715993431350, 293.2178068554150059 ) ) ;
#80723 = FACE_OUTER_BOUND ( 'NONE', #68503, .T. ) ;
#80724 = CARTESIAN_POINT ( 'NONE',  ( 21.03715912545738220, -47.82818131006197149, 193.9678068554150627 ) ) ;
#80725 = PLANE ( 'NONE',  #18697 ) ;
#80727 = EDGE_LOOP ( 'NONE', ( #28867, #7346, #52271, #20588 ) ) ;
#80726 = CARTESIAN_POINT ( 'NONE',  ( 118.0872578842352993, -35.40452791748241879, 238.9337205140059552 ) ) ;
#80728 = DIRECTION ( 'NONE',  ( 0.000000000000000000, -0.4999999999999990563, -0.8660254037844392627 ) ) ;
#80729 = CARTESIAN_POINT ( 'NONE',  ( 116.3364580279229301, -41.54664843801584340, 284.4441967044824082 ) ) ;
#80730 = CARTESIAN_POINT ( 'NONE',  ( 97.70743813507087339, -42.69650533217181021, 137.7661014663869992 ) ) ;
#80731 = FACE_OUTER_BOUND ( 'NONE', #19077, .T. ) ;
#80732 = CARTESIAN_POINT ( 'NONE',  ( 81.19091742811399115, -39.23916151080219095, 8.028235474616696621 ) ) ;
#80733 = CARTESIAN_POINT ( 'NONE',  ( 100.4321520267700265, 78.46444036551646661, -83.41622542100857629 ) ) ;
#80734 = CARTESIAN_POINT ( 'NONE',  ( 142.8821648370248170, -72.54478064608022692, 540.9756252759101471 ) ) ;
#80735 = ORIENTED_EDGE ( 'NONE', *, *, #75535, .F. ) ;
#80736 = EDGE_CURVE ( 'NONE', #85960, #44232, #4053, .T. ) ;
#80737 = EDGE_LOOP ( 'NONE', ( #41090, #2481 ) ) ;
#80738 = ORIENTED_EDGE ( 'NONE', *, *, #63709, .F. ) ;
#80739 = ORIENTED_EDGE ( 'NONE', *, *, #33616, .T. ) ;
#80740 = CARTESIAN_POINT ( 'NONE',  ( 126.0667039024479550, -14.72944715994094977, 199.5838068554170093 ) ) ;
#80741 = CARTESIAN_POINT ( 'NONE',  ( 107.6057229598026197, -48.54288983744045538, 38.61276813305397582 ) ) ;
#80742 = CARTESIAN_POINT ( 'NONE',  ( 31.71315051186898870, -31.94127993907790852, -5.074374724088000832 ) ) ;
#80743 = CARTESIAN_POINT ( 'NONE',  ( 125.5177273812784193, -99.45575754528751133, 55.21780685541800437 ) ) ;
#80745 = CARTESIAN_POINT ( 'NONE',  ( 70.45481371026527029, -138.5762527540429971, 247.5817532094160072 ) ) ;
#80744 = CARTESIAN_POINT ( 'NONE',  ( 63.03715912545639100, -24.42818131006026761, 180.4678068554151196 ) ) ;
#80746 = CIRCLE ( 'NONE', #15520, 4.749999999999976907 ) ;
#80747 = CARTESIAN_POINT ( 'NONE',  ( 109.6796103444932129, -28.56711482602328900, 234.2524198280769951 ) ) ;
#80748 = ORIENTED_EDGE ( 'NONE', *, *, #46892, .F. ) ;
#80749 = EDGE_LOOP ( 'NONE', ( #66850, #26949, #2264, #14094 ) ) ;
#80750 = VECTOR ( 'NONE', #64127, 1000.000000000000000 ) ;
#80751 = ORIENTED_EDGE ( 'NONE', *, *, #85437, .T. ) ;
#80752 = VECTOR ( 'NONE', #50090, 1000.000000000000000 ) ;
#80754 = ADVANCED_FACE ( 'NONE', ( #17249 ), #87181, .T. ) ;
#80753 = AXIS2_PLACEMENT_3D ( 'NONE', #75638, #55147, #13849 ) ;
#80755 = CARTESIAN_POINT ( 'NONE',  ( 141.3509999999999991, 0.000000000000000000, 141.3509999999999991 ) ) ;
#80756 = AXIS2_PLACEMENT_3D ( 'NONE', #2135, #23485, #57073 ) ;
#80757 = CARTESIAN_POINT ( 'NONE',  ( -7.205548786489490269E-13, 127.0000000000000000, 103.1875000000000000 ) ) ;
#80758 = CARTESIAN_POINT ( 'NONE',  ( 188.5667039024479834, -48.82844715994099971, 295.9678068554150059 ) ) ;
#80759 = EDGE_CURVE ( 'NONE', #14739, #24467, #66262, .T. ) ;
#80760 = CARTESIAN_POINT ( 'NONE',  ( 103.4018642804673789, -27.34641595622759169, 16.80444044875395448 ) ) ;
#80761 = DIRECTION ( 'NONE',  ( 0.000000000000000000, 0.000000000000000000, 1.000000000000000000 ) ) ;
#80762 = EDGE_CURVE ( 'NONE', #18491, #16965, #73535, .T. ) ;
#80763 = CARTESIAN_POINT ( 'NONE',  ( 100.9535969414460794, -28.70786762247625035, 175.5940665755088048 ) ) ;
#80764 = CARTESIAN_POINT ( 'NONE',  ( 104.3638673426610666, -27.29495504168057707, 225.2984824187689981 ) ) ;
#80765 = FACE_OUTER_BOUND ( 'NONE', #20689, .T. ) ;
#80766 = EDGE_CURVE ( 'NONE', #12989, #55881, #79933, .T. ) ;
#80767 = ORIENTED_EDGE ( 'NONE', *, *, #81168, .T. ) ;
#80768 = EDGE_CURVE ( 'NONE', #85840, #3395, #5178, .T. ) ;
#80769 = LINE ( 'NONE', #18520, #50454 ) ;
#80770 = AXIS2_PLACEMENT_3D ( 'NONE', #3276, #53617, #25048 ) ;
#80771 = CARTESIAN_POINT ( 'NONE',  ( 156.5667039024483813, -48.82844715993569196, 259.7178068554149490 ) ) ;
#80772 = CARTESIAN_POINT ( 'NONE',  ( 111.6835086010359532, -29.99796862204811987, 42.41666179816294857 ) ) ;
#80773 = EDGE_CURVE ( 'NONE', #18895, #59994, #38129, .T. ) ;
#80774 = EDGE_CURVE ( 'NONE', #7579, #23174, #65822, .T. ) ;
#80775 = VECTOR ( 'NONE', #54293, 1000.000000000000000 ) ;
#80776 = CARTESIAN_POINT ( 'NONE',  ( 136.1807380203812272, -16.97076862299123334, 7.459445689446392969 ) ) ;
#80777 = EDGE_CURVE ( 'NONE', #41770, #35035, #39988, .T. ) ;
#80778 = CARTESIAN_POINT ( 'NONE',  ( 100.4020455594773580, -99.85325460238202311, -19.78219314458215550 ) ) ;
#80779 = DIRECTION ( 'NONE',  ( 1.000000000000000000, 0.000000000000000000, 0.000000000000000000 ) ) ;
#80780 = VERTEX_POINT ( 'NONE', #32194 ) ;
#80781 = CARTESIAN_POINT ( 'NONE',  ( -487.2989999999999782, 97.78694598552380057, 3.968750000000479616 ) ) ;
#80782 = CARTESIAN_POINT ( 'NONE',  ( 125.3303947399734568, 53.81125057877675744, -36.56738695590195931 ) ) ;
#80783 = EDGE_CURVE ( 'NONE', #25445, #60868, #24063, .T. ) ;
#80784 = ORIENTED_EDGE ( 'NONE', *, *, #11675, .F. ) ;
#80785 = CARTESIAN_POINT ( 'NONE',  ( 98.20221454234541625, -43.33276655250838871, 111.8480062282919647 ) ) ;
#80786 = VERTEX_POINT ( 'NONE', #80823 ) ;
#80787 = CARTESIAN_POINT ( 'NONE',  ( 114.4871815801477624, -30.46814820527590228, 73.80670554236196779 ) ) ;
#80788 = EDGE_CURVE ( 'NONE', #7841, #41944, #57370, .T. ) ;
#80789 = DIRECTION ( 'NONE',  ( -0.7071067811874389708, 0.7071067811856560636, 0.000000000000000000 ) ) ;
#80790 = CARTESIAN_POINT ( 'NONE',  ( 110.4802244392091950, -27.25226000720831721, 96.23301187732596418 ) ) ;
#80791 = DIRECTION ( 'NONE',  ( 1.000000000000000000, 4.299999999999999979E-14, 9.351236661543306751E-17 ) ) ;
#80792 = DIRECTION ( 'NONE',  ( 0.9963424814100680926, -0.08544974978095698503, 0.000000000000000000 ) ) ;
#80793 = CARTESIAN_POINT ( 'NONE',  ( 97.08395347075709481, -39.80944164022105980, 17.56419670448195092 ) ) ;
#80794 = AXIS2_PLACEMENT_3D ( 'NONE', #84195, #36023, #58681 ) ;
#80795 = CARTESIAN_POINT ( 'NONE',  ( 113.2459685721311047, -28.75903239629483465, 180.5526760553944996 ) ) ;
#80796 = EDGE_LOOP ( 'NONE', ( #10376, #10347 ) ) ;
#80797 = CARTESIAN_POINT ( 'NONE',  ( 117.0608477614241707, -38.08078333794142623, 258.7188941364966581 ) ) ;
#80798 = EDGE_LOOP ( 'NONE', ( #38687, #65536, #60279, #71195 ) ) ;
#80799 = DIRECTION ( 'NONE',  ( 1.000000000000000000, 6.145690160522480771E-16, 0.000000000000000000 ) ) ;
#80800 = VERTEX_POINT ( 'NONE', #31753 ) ;
#80801 = VERTEX_POINT ( 'NONE', #18572 ) ;
#80802 = EDGE_CURVE ( 'NONE', #35086, #1484, #60341, .T. ) ;
#80803 = CARTESIAN_POINT ( 'NONE',  ( -77.39114642429849766, 120.6499999999999915, -71.77848634863219957 ) ) ;
#80804 = ORIENTED_EDGE ( 'NONE', *, *, #75020, .F. ) ;
#80805 = CARTESIAN_POINT ( 'NONE',  ( 111.3277751695583078, -45.53312973143663811, 247.9356252759109509 ) ) ;
#80806 = EDGE_CURVE ( 'NONE', #66670, #38273, #80599, .T. ) ;
#80807 = CARTESIAN_POINT ( 'NONE',  ( 110.9910846855449478, -27.45570243918006170, 124.7564986738925796 ) ) ;
#80808 = DIRECTION ( 'NONE',  ( 1.000000000000000078E-15, -1.000000000000000083E-30, -1.000000000000000000 ) ) ;
#80809 = CARTESIAN_POINT ( 'NONE',  ( 118.7325469213664633, -34.64676260937859098, 44.96705384733895272 ) ) ;
#80811 = ADVANCED_FACE ( 'NONE', ( #45808 ), #25386, .T. ) ;
#80810 = CARTESIAN_POINT ( 'NONE',  ( 97.86649994386787910, -40.64904342295498907, 42.64697140597041880 ) ) ;
#80812 = VERTEX_POINT ( 'NONE', #11768 ) ;
#80813 = CARTESIAN_POINT ( 'NONE',  ( 104.4897322876167323, -26.97885769723445648, 115.2836109755910030 ) ) ;
#80814 = VECTOR ( 'NONE', #84327, 1000.000000000000000 ) ;
#80815 = EDGE_CURVE ( 'NONE', #41588, #77431, #39465, .T. ) ;
#80816 = VECTOR ( 'NONE', #10918, 1000.000000000000000 ) ;
#80817 = DIRECTION ( 'NONE',  ( -2.900000000000000265E-14, 2.000000000000000155E-15, -1.000000000000000000 ) ) ;
#80818 = EDGE_LOOP ( 'NONE', ( #76552, #11046 ) ) ;
#80819 = VECTOR ( 'NONE', #20173, 1000.000000000000000 ) ;
#80820 = PLANE ( 'NONE',  #69223 ) ;
#80821 = DIRECTION ( 'NONE',  ( 0.000000000000000000, 1.000000000000000000, 0.000000000000000000 ) ) ;
#80822 = CARTESIAN_POINT ( 'NONE',  ( 118.0844448206164827, -36.21142561920247971, 268.8518157521015723 ) ) ;
#80823 = CARTESIAN_POINT ( 'NONE',  ( 32.56670390244700997, -18.82844715994112050, 342.9256252759109884 ) ) ;
#80824 = AXIS2_PLACEMENT_3D ( 'NONE', #34395, #62106, #89838 ) ;
#80825 = PLANE ( 'NONE',  #20216 ) ;
#80826 = LINE ( 'NONE', #59893, #14210 ) ;
#80827 = CARTESIAN_POINT ( 'NONE',  ( 115.1439687268531600, -40.82418761129420659, 247.8876579233149755 ) ) ;
#80829 = CARTESIAN_POINT ( 'NONE',  ( 109.7644292386349889, -47.42453529627113085, 88.78514908543493789 ) ) ;
#80828 = CARTESIAN_POINT ( 'NONE',  ( 0.000000000000000000, 20.32000000000000028, 0.000000000000000000 ) ) ;
#80830 = CARTESIAN_POINT ( 'NONE',  ( 113.2217361175605532, 68.94557673950741616, 65.00547801876621179 ) ) ;
#80831 = CARTESIAN_POINT ( 'NONE',  ( 116.8367917427482467, -32.96809911012589112, 139.1184824187679396 ) ) ;
#80832 = ORIENTED_EDGE ( 'NONE', *, *, #44877, .F. ) ;
#80833 = DIRECTION ( 'NONE',  ( -1.000000000000000000, -8.163404592832032979E-16, 0.000000000000000000 ) ) ;
#80834 = ORIENTED_EDGE ( 'NONE', *, *, #55799, .F. ) ;
#80835 = CARTESIAN_POINT ( 'NONE',  ( 32.15435173583699680, -31.62489322948790971, -5.074374724088000832 ) ) ;
#80836 = CARTESIAN_POINT ( 'NONE',  ( 107.0664832912748068, -36.72944715993923381, -4.074374724089028454 ) ) ;
#80837 = PRODUCT_DEFINITION_SHAPE ( 'NONE', 'NONE',  #89934 ) ;
#80838 = CARTESIAN_POINT ( 'NONE',  ( 25.56670390244820368, -48.82844715994168183, 259.7178068554150059 ) ) ;
#80839 = ORIENTED_EDGE ( 'NONE', *, *, #52464, .T. ) ;
#80840 = CARTESIAN_POINT ( 'NONE',  ( 100.9544648868430414, -28.70718114071191351, 50.59397893232809906 ) ) ;
#80842 = ORIENTED_EDGE ( 'NONE', *, *, #567, .T. ) ;
#80841 = CARTESIAN_POINT ( 'NONE',  ( 114.0157635323931515, -28.07379075743241259, 119.5261014663869474 ) ) ;
#80843 = DIRECTION ( 'NONE',  ( -0.000000000000000000, -1.000000000000000000, -0.000000000000000000 ) ) ;
#80844 = VECTOR ( 'NONE', #60176, 1000.000000000000000 ) ;
#80845 = PLANE ( 'NONE',  #20057 ) ;
#80846 = CIRCLE ( 'NONE', #85197, 10.00000000000000178 ) ;
#80847 = CARTESIAN_POINT ( 'NONE',  ( 107.0664832912739399, -36.72944715994095333, 290.1356252759106837 ) ) ;
#80848 = DIRECTION ( 'NONE',  ( 0.000000000000000000, 0.000000000000000000, -1.000000000000000000 ) ) ;
#80849 = ORIENTED_EDGE ( 'NONE', *, *, #22016, .T. ) ;
#80850 = AXIS2_PLACEMENT_3D ( 'NONE', #25018, #79558, #85487 ) ;
#80851 = CARTESIAN_POINT ( 'NONE',  ( 107.9474950258210413, -25.68774170017952940, 115.0251490854349612 ) ) ;
#80852 = PRODUCT_CONTEXT ( 'NONE', #39967, 'mechanical' ) ;
#80853 = CARTESIAN_POINT ( 'NONE',  ( 107.0664832912739968, -0.2185775633790978945, 333.4006252759120343 ) ) ;
#80854 = CARTESIAN_POINT ( 'NONE',  ( 91.91125933621934507, -111.9108492392177396, -19.23816774841976951 ) ) ;
#80855 = EDGE_LOOP ( 'NONE', ( #64605, #55159, #82599, #8243 ) ) ;
#80856 = ORIENTED_EDGE ( 'NONE', *, *, #74356, .T. ) ;
#80857 = CYLINDRICAL_SURFACE ( 'NONE', #53916, 8.928099999999993486 ) ;
#80858 = CARTESIAN_POINT ( 'NONE',  ( 98.05663017059093534, 92.12504059357191011, -86.19814306825418271 ) ) ;
#80859 = FACE_OUTER_BOUND ( 'NONE', #59183, .T. ) ;
#80860 = CARTESIAN_POINT ( 'NONE',  ( 57.14999999999999858, 69.84999999999999432, 326.2630000000000337 ) ) ;
#80862 = FACE_OUTER_BOUND ( 'NONE', #27360, .T. ) ;
#80861 = CARTESIAN_POINT ( 'NONE',  ( 20.03715912545729338, -24.42818131006189830, 313.9678068554150059 ) ) ;
#80863 = CARTESIAN_POINT ( 'NONE',  ( 183.5150000000000148, 53.21300000000000097, 59.96543552338529537 ) ) ;
#80864 = ORIENTED_EDGE ( 'NONE', *, *, #29449, .T. ) ;
#80865 = EDGE_CURVE ( 'NONE', #61274, #47365, #64938, .T. ) ;
#80866 = CARTESIAN_POINT ( 'NONE',  ( 109.6430122704383763, -46.48008669675207472, 33.78145862070494587 ) ) ;
#80867 = ADVANCED_FACE ( 'NONE', ( #54856 ), #40802, .F. ) ;
#80868 = CARTESIAN_POINT ( 'NONE',  ( 97.28849942844340148, -36.49606577720026479, 192.3070538473389490 ) ) ;
#80870 = ORIENTED_EDGE ( 'NONE', *, *, #37294, .F. ) ;
#80869 = DIRECTION ( 'NONE',  ( 1.000000000000000078E-15, 1.000000000000000083E-30, -1.000000000000000000 ) ) ;
#80871 = EDGE_CURVE ( 'NONE', #89072, #1768, #54720, .T. ) ;
#80872 = CARTESIAN_POINT ( 'NONE',  ( 109.7352083718000131, -46.17358189742679286, 68.79562527591099297 ) ) ;
#80873 = CARTESIAN_POINT ( 'NONE',  ( 21.03715912545830591, -47.82818131006186491, 237.4678068554150059 ) ) ;
#80874 = CARTESIAN_POINT ( 'NONE',  ( 138.8167039024479834, -67.87844715994100397, 35.51780685541480409 ) ) ;
#80875 = PLANE ( 'NONE',  #34368 ) ;
#80876 = EDGE_CURVE ( 'NONE', #58384, #18192, #6736, .T. ) ;
#80877 = VERTEX_POINT ( 'NONE', #69866 ) ;
#80878 = LINE ( 'NONE', #25444, #50122 ) ;
#80879 = EDGE_CURVE ( 'NONE', #1571, #11233, #19940, .T. ) ;
#80880 = AXIS2_PLACEMENT_3D ( 'NONE', #17791, #74546, #5060 ) ;
#80881 = EDGE_LOOP ( 'NONE', ( #60463, #53826, #72379, #45023 ) ) ;
#80882 = ORIENTED_EDGE ( 'NONE', *, *, #43757, .F. ) ;
#80883 = CARTESIAN_POINT ( 'NONE',  ( 112.7895289397446561, -28.43984804668171051, 236.0272975916119549 ) ) ;
#80884 = ADVANCED_FACE ( 'NONE', ( #83065 ), #13552, .T. ) ;
#80885 = AXIS2_PLACEMENT_3D ( 'NONE', #75021, #33689, #12352 ) ;
#80886 = LINE ( 'NONE', #18639, #79211 ) ;
#80887 = AXIS2_PLACEMENT_3D ( 'NONE', #15435, #69941, #34956 ) ;
#80888 = VECTOR ( 'NONE', #69272, 1000.000000000000227 ) ;
#80889 = CARTESIAN_POINT ( 'NONE',  ( -82.96293804092792357, 84.21449860606323057, 100.8069756963044341 ) ) ;
#80890 = ADVANCED_FACE ( 'NONE', ( #61684 ), #7636, .F. ) ;
#80891 = DIRECTION ( 'NONE',  ( 0.000000000000000000, 1.000000000000000000, 0.000000000000000000 ) ) ;
#80892 = CARTESIAN_POINT ( 'NONE',  ( 194.0371591254573218, -24.42818131005417825, 249.9678068554149775 ) ) ;
#80893 = EDGE_LOOP ( 'NONE', ( #9951, #77997, #73294, #51350 ) ) ;
#80894 = DIRECTION ( 'NONE',  ( 0.000000000000000000, 0.000000000000000000, -1.000000000000000000 ) ) ;
#80895 = CARTESIAN_POINT ( 'NONE',  ( 97.06391965937397970, -37.34326081457973601, 37.37502593264307649 ) ) ;
#80896 = ORIENTED_EDGE ( 'NONE', *, *, #19678, .F. ) ;
#80897 = CARTESIAN_POINT ( 'NONE',  ( 100.5506404981706510, -27.80068015945615656, 30.56610146638794134 ) ) ;
#80898 = ORIENTED_EDGE ( 'NONE', *, *, #54892, .T. ) ;
#80899 = VERTEX_POINT ( 'NONE', #47156 ) ;
#80900 = CARTESIAN_POINT ( 'NONE',  ( 99.31750181266291122, -39.29518527230509051, 239.3995189410199487 ) ) ;
#80901 = EDGE_CURVE ( 'NONE', #9938, #3093, #33544, .T. ) ;
#80902 = AXIS2_PLACEMENT_3D ( 'NONE', #57909, #15249, #57461 ) ;
#80903 = CARTESIAN_POINT ( 'NONE',  ( 80.55084967033837984, -151.1625929292324884, 73.15139425023529895 ) ) ;
#80904 = CARTESIAN_POINT ( 'NONE',  ( 0.000000000000000000, 101.5999999999999943, 0.000000000000000000 ) ) ;
#80905 = CARTESIAN_POINT ( 'NONE',  ( 177.8371591254543489, -47.82818131005477369, 249.9678068554149775 ) ) ;
#80906 = CIRCLE ( 'NONE', #14170, 1.000000000000000888 ) ;
#80907 = CARTESIAN_POINT ( 'NONE',  ( 172.5664832912729878, -27.82844715994070484, 78.92562527591199739 ) ) ;
#80908 = VECTOR ( 'NONE', #80268, 1000.000000000000000 ) ;
#80909 = ADVANCED_FACE ( 'NONE', ( #82619 ), #68968, .F. ) ;
#80910 = CARTESIAN_POINT ( 'NONE',  ( 117.2345208925008109, -41.18012235578145663, 204.4861014663869696 ) ) ;
#80911 = LINE ( 'NONE', #74518, #20964 ) ;
#80912 = AXIS2_PLACEMENT_3D ( 'NONE', #70935, #65759, #3547 ) ;
#80913 = VERTEX_POINT ( 'NONE', #48052 ) ;
#80914 = CARTESIAN_POINT ( 'NONE',  ( 104.2021517265174992, -25.17926459036136322, 86.26991099019699050 ) ) ;
#80915 = FACE_OUTER_BOUND ( 'NONE', #70514, .T. ) ;
#80916 = EDGE_LOOP ( 'NONE', ( #56000, #7482, #36553, #89683 ) ) ;
#80917 = VERTEX_POINT ( 'NONE', #75787 ) ;
#80918 = ORIENTED_EDGE ( 'NONE', *, *, #24943, .T. ) ;
#80919 = CARTESIAN_POINT ( 'NONE',  ( 97.81136857603131318, -40.51756142711754194, 161.6353372277744143 ) ) ;
#80920 = DIRECTION ( 'NONE',  ( 0.000000000000000000, 0.000000000000000000, 1.000000000000000000 ) ) ;
#80921 = FACE_OUTER_BOUND ( 'NONE', #30757, .T. ) ;
#80922 = CARTESIAN_POINT ( 'NONE',  ( 103.3817498881349906, -44.01315952142851984, 125.0223760838769778 ) ) ;
#80923 = CARTESIAN_POINT ( 'NONE',  ( 96.75463230179867935, -40.77307608890721013, 242.6118157521009664 ) ) ;
#80925 = EDGE_CURVE ( 'NONE', #81025, #36469, #51809, .T. ) ;
#80924 = DIRECTION ( 'NONE',  ( 0.000000000000000000, 1.000000000000000000, 0.000000000000000000 ) ) ;
#80926 = ORIENTED_EDGE ( 'NONE', *, *, #57521, .F. ) ;
#80927 =( LENGTH_UNIT ( ) NAMED_UNIT ( * ) SI_UNIT ( .MILLI., .METRE. ) );
#80928 = EDGE_CURVE ( 'NONE', #67043, #87073, #26284, .T. ) ;
#80929 = DIRECTION ( 'NONE',  ( 0.000000000000000000, 0.000000000000000000, -1.000000000000000000 ) ) ;
#80930 = EDGE_LOOP ( 'NONE', ( #6999, #18936, #84297, #16036 ) ) ;
#80932 = VERTEX_POINT ( 'NONE', #62144 ) ;
#80931 = AXIS2_PLACEMENT_3D ( 'NONE', #8642, #9527, #2720 ) ;
#80933 = CARTESIAN_POINT ( 'NONE',  ( -487.2989999999999782, 18.41194598552320016, 97.63125000000000853 ) ) ;
#80934 = ORIENTED_EDGE ( 'NONE', *, *, #20404, .F. ) ;
#80935 = EDGE_LOOP ( 'NONE', ( #25872, #78067, #57578, #1936 ) ) ;
#80936 = DIRECTION ( 'NONE',  ( 0.000000000000000000, 0.000000000000000000, 1.000000000000000000 ) ) ;
#80937 = CARTESIAN_POINT ( 'NONE',  ( -103.1875000000000000, 127.0000000000000000, 7.143749999998919797 ) ) ;
#80938 = DIRECTION ( 'NONE',  ( 1.561055996379579722E-16, -1.000000000000000000, 0.000000000000000000 ) ) ;
#80939 = CARTESIAN_POINT ( 'NONE',  ( 113.0289883941274525, -30.57309799635150682, 173.8867055423629608 ) ) ;
#80940 = CARTESIAN_POINT ( 'NONE',  ( 112.1386966202503430, -26.85596833298010111, 19.71086337114896736 ) ) ;
#80941 = CARTESIAN_POINT ( 'NONE',  ( 113.2436075868320984, -28.75722666126760529, 125.5524796337008979 ) ) ;
#80942 = ORIENTED_EDGE ( 'NONE', *, *, #49709, .F. ) ;
#80943 = DIRECTION ( 'NONE',  ( 0.000000000000000000, 0.000000000000000000, -1.000000000000000000 ) ) ;
#80944 = ORIENTED_EDGE ( 'NONE', *, *, #20206, .T. ) ;
#80945 = EDGE_CURVE ( 'NONE', #73072, #13477, #89877, .T. ) ;
#80946 = DIRECTION ( 'NONE',  ( 0.000000000000000000, 0.000000000000000000, -1.000000000000000000 ) ) ;
#80947 = ORIENTED_EDGE ( 'NONE', *, *, #22130, .T. ) ;
#80948 = CARTESIAN_POINT ( 'NONE',  ( 101.2924984490993836, -28.53423124992686155, 166.5645102773719373 ) ) ;
#80949 = CIRCLE ( 'NONE', #69332, 2.116999999999980009 ) ;
#80950 = CARTESIAN_POINT ( 'NONE',  ( -5.203389996554649066, 71.06717806059110387, 118.4423725322968011 ) ) ;
#80951 = CARTESIAN_POINT ( 'NONE',  ( 111.2955958668267584, -45.79294333952354634, 132.9238878757940938 ) ) ;
#80952 = EDGE_CURVE ( 'NONE', #54341, #15887, #40357, .T. ) ;
#80954 = DIRECTION ( 'NONE',  ( -1.000000000000000078E-15, 1.000000000000000083E-30, 1.000000000000000000 ) ) ;
#80953 = AXIS2_PLACEMENT_3D ( 'NONE', #79864, #17618, #30795 ) ;
#80955 = ORIENTED_EDGE ( 'NONE', *, *, #87405, .F. ) ;
#80956 = VECTOR ( 'NONE', #1547, 1000.000000000000000 ) ;
#80957 = CARTESIAN_POINT ( 'NONE',  ( 98.40533970481327231, -42.07952101345657780, 11.76800622829193799 ) ) ;
#80958 = CARTESIAN_POINT ( 'NONE',  ( 104.0301208637212369, -47.40549519127628031, 63.36800622829197494 ) ) ;
#80960 = CARTESIAN_POINT ( 'NONE',  ( 98.60478223830740774, 120.6499999999999915, 3.859079674607175002E-13 ) ) ;
#80959 = DIRECTION ( 'NONE',  ( -1.000000000000000000, 1.011922027653136551E-15, 0.000000000000000000 ) ) ;
#80961 = LINE ( 'NONE', #33684, #49599 ) ;
#80962 = DIRECTION ( 'NONE',  ( 1.000000000000000078E-15, -1.000000000000000000, 0.000000000000000000 ) ) ;
#80963 = DIRECTION ( 'NONE',  ( 4.649954031768951549E-17, -0.8660254037844387076, 0.4999999999999998890 ) ) ;
#80964 = DIRECTION ( 'NONE',  ( -1.000000000000000000, -4.299999999999999979E-14, -1.000000000000000078E-15 ) ) ;
#80965 = CIRCLE ( 'NONE', #41757, 2.999999999999947153 ) ;
#80966 = CARTESIAN_POINT ( 'NONE',  ( 146.7395179759399184, -101.1118038811399913, 247.0601187889650134 ) ) ;
#80967 = ORIENTED_EDGE ( 'NONE', *, *, #51616, .F. ) ;
#80968 = CARTESIAN_POINT ( 'NONE',  ( 107.6091449839925929, -48.61785814739364042, 42.61276813305398292 ) ) ;
#80969 = CARTESIAN_POINT ( 'NONE',  ( 99.08600912489498569, -29.96680234772274787, 211.7670538473399517 ) ) ;
#80970 = CARTESIAN_POINT ( 'NONE',  ( 101.1293421793351968, -28.09060746778665418, 46.55562527591094835 ) ) ;
#80971 = AXIS2_PLACEMENT_3D ( 'NONE', #45765, #19427, #87581 ) ;
#80973 = DIRECTION ( 'NONE',  ( -0.9254794337955620787, -0.3787978585227823602, 0.000000000000000000 ) ) ;
#80972 = CARTESIAN_POINT ( 'NONE',  ( 109.6444706913881930, -46.47971972121219864, 172.7775026101618039 ) ) ;
#80974 = CARTESIAN_POINT ( 'NONE',  ( 172.5664832912740110, 0.2215528400590013880, 16.80862527591200006 ) ) ;
#80975 = ADVANCED_FACE ( 'NONE', ( #20818 ), #68072, .F. ) ;
#80976 = EDGE_CURVE ( 'NONE', #9481, #88962, #5859, .T. ) ;
#80977 = DIRECTION ( 'NONE',  ( 1.000000000000000000, 4.163336342344347755E-14, 0.000000000000000000 ) ) ;
#80978 = ORIENTED_EDGE ( 'NONE', *, *, #76869, .F. ) ;
#80979 = EDGE_CURVE ( 'NONE', #78000, #27916, #9832, .T. ) ;
#80980 = CARTESIAN_POINT ( 'NONE',  ( 99.54941199951412045, -42.98700854487240974, 112.8784824187679732 ) ) ;
#80981 = CIRCLE ( 'NONE', #2656, 16.33514202138213633 ) ;
#80983 = EDGE_LOOP ( 'NONE', ( #15324, #56917, #16585, #81311 ) ) ;
#80982 = CARTESIAN_POINT ( 'NONE',  ( 142.8690268918515471, 4.118420757222291506, 542.9756252759101471 ) ) ;
#80984 = EDGE_CURVE ( 'NONE', #18119, #27695, #75049, .T. ) ;
#80985 = CARTESIAN_POINT ( 'NONE',  ( 105.1150531980676561, -26.51080800785444680, 231.2270538473399597 ) ) ;
#80986 = CARTESIAN_POINT ( 'NONE',  ( 37.56670390244801183, -48.82844715994119866, 300.4678068554150059 ) ) ;
#80987 = DIRECTION ( 'NONE',  ( 0.000000000000000000, 1.000000000000000000, 0.000000000000000000 ) ) ;
#80988 = CARTESIAN_POINT ( 'NONE',  ( 142.8698897858160706, -0.9167816978817300289, 542.9756252759101471 ) ) ;
#80989 = CARTESIAN_POINT ( 'NONE',  ( -7.661254700127832606, 98.64746158385918307, 317.6630000000000109 ) ) ;
#80990 = CARTESIAN_POINT ( 'NONE',  ( 131.4524275574069350, -37.60567372263788144, 2.908038864009826252 ) ) ;
#80991 = EDGE_CURVE ( 'NONE', #41462, #13431, #23525, .T. ) ;
#80992 = CARTESIAN_POINT ( 'NONE',  ( -3.968749999999949818, 120.6499999999999915, -105.4788588808462038 ) ) ;
#80993 = CARTESIAN_POINT ( 'NONE',  ( 108.7386892141029477, -46.36620816325537930, 167.7127681330539701 ) ) ;
#80994 = AXIS2_PLACEMENT_3D ( 'NONE', #4129, #58634, #2359 ) ;
#80995 = ORIENTED_EDGE ( 'NONE', *, *, #28378, .F. ) ;
#80996 = EDGE_LOOP ( 'NONE', ( #2265, #84618 ) ) ;
#80997 = CARTESIAN_POINT ( 'NONE',  ( 99.03419491772403660, -31.85514013008181777, 122.3120594963729673 ) ) ;
#80998 = EDGE_CURVE ( 'NONE', #9798, #19996, #78037, .T. ) ;
#80999 = DIRECTION ( 'NONE',  ( 1.000000000000000078E-15, -1.000000000000000000, 0.000000000000000000 ) ) ;
#81001 = CARTESIAN_POINT ( 'NONE',  ( -46.60773131249376178, 65.60000000000000853, -44.42500552774628630 ) ) ;
#81000 = CARTESIAN_POINT ( 'NONE',  ( 112.0813997088635432, -45.80630777137064058, 248.9661014663869878 ) ) ;
#81002 = CARTESIAN_POINT ( 'NONE',  ( 0.000000000000000000, 127.0000000000000000, -103.1875000000000000 ) ) ;
#81003 = PLANE ( 'NONE',  #16219 ) ;
#81004 = EDGE_CURVE ( 'NONE', #56941, #22696, #86665, .T. ) ;
#81005 = CARTESIAN_POINT ( 'NONE',  ( 162.0667039024469886, -67.87844715994089029, 222.2178068554179902 ) ) ;
#81006 = DIRECTION ( 'NONE',  ( 1.000000000000000000, 0.000000000000000000, 0.000000000000000000 ) ) ;
#81007 = LINE ( 'NONE', #11949, #47809 ) ;
#81008 = CARTESIAN_POINT ( 'NONE',  ( 0.000000000000000000, 184.0000000000000000, 90.32146847885336172 ) ) ;
#81009 = CARTESIAN_POINT ( 'NONE',  ( 102.6926969729869938, -27.29023857175969781, 180.4213395616249898 ) ) ;
#81010 = DIRECTION ( 'NONE',  ( 8.673617379884035472E-16, 1.000000000000000000, 0.000000000000000000 ) ) ;
#81011 = ORIENTED_EDGE ( 'NONE', *, *, #17537, .T. ) ;
#81012 = ORIENTED_EDGE ( 'NONE', *, *, #31518, .F. ) ;
#81013 = CARTESIAN_POINT ( 'NONE',  ( -100.6520717229718542, 79.66695435136416847, -83.15068351451320439 ) ) ;
#81014 = CARTESIAN_POINT ( 'NONE',  ( 82.53070037945653326, -19.95069274174520402, 7.120636252911432429 ) ) ;
#81015 = DIRECTION ( 'NONE',  ( 0.000000000000000000, 0.000000000000000000, -1.000000000000000000 ) ) ;
#81016 = DIRECTION ( 'NONE',  ( 0.000000000000000000, 1.000000000000000000, 0.000000000000000000 ) ) ;
#81018 = PLANE ( 'NONE',  #26717 ) ;
#81017 = AXIS2_PLACEMENT_3D ( 'NONE', #21991, #49659, #43744 ) ;
#81019 = ORIENTED_EDGE ( 'NONE', *, *, #37073, .F. ) ;
#81020 = AXIS2_PLACEMENT_3D ( 'NONE', #39808, #11687, #74355 ) ;
#81021 = DIRECTION ( 'NONE',  ( 0.000000000000000000, 0.000000000000000000, -1.000000000000000000 ) ) ;
#81022 =( BOUNDED_CURVE ( )  B_SPLINE_CURVE ( 3, ( #72987, #66164, #3950, #87080 ),
 .UNSPECIFIED., .F., .T. ) 
 B_SPLINE_CURVE_WITH_KNOTS ( ( 4, 4 ),
 ( 7.227822158068946767E-12, 1.570796326804053678 ),
 .UNSPECIFIED. ) 
 CURVE ( )  GEOMETRIC_REPRESENTATION_ITEM ( )  RATIONAL_B_SPLINE_CURVE ( ( 1.000000000000000000, 0.8047378541239101901, 0.8047378541239101901, 1.000000000000000000 ) ) 
 REPRESENTATION_ITEM ( '' )  );
#81023 = CARTESIAN_POINT ( 'NONE',  ( 114.6056301357651819, -29.52887111919123697, 234.4327681330539690 ) ) ;
#81024 = CARTESIAN_POINT ( 'NONE',  ( 4.665904304751416087E-15, 44.45000000000000284, -38.10000000000000142 ) ) ;
#81025 = VERTEX_POINT ( 'NONE', #77134 ) ;
#81026 = ORIENTED_EDGE ( 'NONE', *, *, #20593, .T. ) ;
#81027 = CIRCLE ( 'NONE', #11362, 1.000000000000000888 ) ;
#81028 = CARTESIAN_POINT ( 'NONE',  ( -12.52017803906219129, 84.19101337647619232, 117.8931578309348964 ) ) ;
#81029 = LINE ( 'NONE', #82364, #66657 ) ;
#81030 = CARTESIAN_POINT ( 'NONE',  ( 99.50478645252971432, -43.30584932723667890, 166.8960762454959195 ) ) ;
#81031 = CARTESIAN_POINT ( 'NONE',  ( 97.82153671710952381, -35.93768077729445309, 34.07666179816293095 ) ) ;
#81033 = CARTESIAN_POINT ( 'NONE',  ( 102.6884963789050289, -46.90384819475383438, 133.2651490854349561 ) ) ;
#81032 = VECTOR ( 'NONE', #37078, 1000.000000000000000 ) ;
#81034 = CARTESIAN_POINT ( 'NONE',  ( 96.20012047777625241, -115.5046222945369436, -21.78219314458165812 ) ) ;
#81035 = ORIENTED_EDGE ( 'NONE', *, *, #40506, .F. ) ;
#81036 = VECTOR ( 'NONE', #37260, 1000.000000000000000 ) ;
#81037 = EDGE_CURVE ( 'NONE', #17490, #5834, #89765, .T. ) ;
#81038 = CARTESIAN_POINT ( 'NONE',  ( 84.40120044323725779, -147.4828892783847607, 72.80491794383669912 ) ) ;
#81039 = CARTESIAN_POINT ( 'NONE',  ( -492.0614999999999668, 93.66249999999999432, 6.350000000000409983 ) ) ;
#81040 = EDGE_LOOP ( 'NONE', ( #68835, #47814, #28267, #11981 ) ) ;
#81041 = EDGE_LOOP ( 'NONE', ( #23868, #3183, #4095, #58990 ) ) ;
#81042 = DIRECTION ( 'NONE',  ( 0.000000000000000000, -0.000000000000000000, -1.000000000000000000 ) ) ;
#81043 = ORIENTED_EDGE ( 'NONE', *, *, #41883, .F. ) ;
#81044 = EDGE_LOOP ( 'NONE', ( #78090, #21361, #3775, #41979 ) ) ;
#81045 = CARTESIAN_POINT ( 'NONE',  ( 183.6524903400785718, -49.32844715993451956, 180.4678068554150343 ) ) ;
#81046 = CIRCLE ( 'NONE', #59290, 11.45913725231036118 ) ;
#81047 = CARTESIAN_POINT ( 'NONE',  ( 100.6982016950751699, -42.46504578929962292, 56.33241982807696502 ) ) ;
#81048 = CARTESIAN_POINT ( 'NONE',  ( 106.4823715260129688, -24.86804634255730662, 195.1156252759109861 ) ) ;
#81049 = CARTESIAN_POINT ( 'NONE',  ( 117.2886123466743271, -34.79635738071011986, 158.9756252759109714 ) ) ;
#81051 = CARTESIAN_POINT ( 'NONE',  ( 96.70769389551976758, -42.43415482991306220, 22.72705384733997391 ) ) ;
#81050 = CARTESIAN_POINT ( 'NONE',  ( 127.0667052882549797, -69.62844715994097555, 55.21780685541800437 ) ) ;
#81052 = DIRECTION ( 'NONE',  ( -1.000000000000000000, -4.163336342344275811E-14, 0.000000000000000000 ) ) ;
#81053 = DIRECTION ( 'NONE',  ( -0.3818493186865920541, 0.9242245927363033076, 0.000000000000000000 ) ) ;
#81054 = EDGE_LOOP ( 'NONE', ( #24805, #47358, #79145, #69788 ) ) ;
#81055 = EDGE_LOOP ( 'NONE', ( #59295, #32788 ) ) ;
#81056 = CIRCLE ( 'NONE', #57824, 5.000000000000004441 ) ;
#81057 = EDGE_CURVE ( 'NONE', #11825, #53364, #22621, .T. ) ;
#81058 = DIRECTION ( 'NONE',  ( 0.000000000000000000, 0.000000000000000000, -1.000000000000000000 ) ) ;
#81059 = CARTESIAN_POINT ( 'NONE',  ( 106.2986956077118208, -47.17057584017531724, 222.5184824187679453 ) ) ;
#81060 = ORIENTED_EDGE ( 'NONE', *, *, #23659, .T. ) ;
#81061 = CARTESIAN_POINT ( 'NONE',  ( 113.0222799004901333, -45.32912119007338703, 203.0584824187679374 ) ) ;
#81062 = CYLINDRICAL_SURFACE ( 'NONE', #73228, 9.999999999999998224 ) ;
#81063 =( LENGTH_UNIT ( ) NAMED_UNIT ( * ) SI_UNIT ( .MILLI., .METRE. ) );
#81064 = CARTESIAN_POINT ( 'NONE',  ( 53.56670390244749314, -48.82844715994058049, 129.9678068554150911 ) ) ;
#81065 = CARTESIAN_POINT ( 'NONE',  ( 34.33598329127499227, -36.32844715994100682, 237.4678068554150059 ) ) ;
#81067 = DIRECTION ( 'NONE',  ( 0.000000000000000000, 1.000000000000000000, 0.000000000000000000 ) ) ;
#81066 = CARTESIAN_POINT ( 'NONE',  ( 112.5738672296349705, -43.44503014251905171, 277.6356252759110248 ) ) ;
#81068 = CARTESIAN_POINT ( 'NONE',  ( 113.1781702599491979, -44.75196522829472912, 174.0939462851112580 ) ) ;
#81069 = FACE_OUTER_BOUND ( 'NONE', #75428, .T. ) ;
#81070 = CARTESIAN_POINT ( 'NONE',  ( -7.205548786489490269E-13, 127.0000000000000000, 103.1875000000000000 ) ) ;
#81071 = LINE ( 'NONE', #32888, #31240 ) ;
#81072 = CARTESIAN_POINT ( 'NONE',  ( 223.2659999999999911, 52.73749999999999716, -44.45000000000000284 ) ) ;
#81073 = CARTESIAN_POINT ( 'NONE',  ( -492.0614999999999668, 14.28750000000026077, 11.11249999999970051 ) ) ;
#81075 = ORIENTED_EDGE ( 'NONE', *, *, #8791, .T. ) ;
#81074 = DIRECTION ( 'NONE',  ( -3.100000000000000258E-29, 3.100000000000000044E-14, 1.000000000000000000 ) ) ;
#81076 = AXIS2_PLACEMENT_3D ( 'NONE', #42368, #34671, #7870 ) ;
#81077 = DIRECTION ( 'NONE',  ( 0.000000000000000000, 1.000000000000000000, 0.000000000000000000 ) ) ;
#81078 = CARTESIAN_POINT ( 'NONE',  ( 97.07499705966343129, -41.51125058752681696, 216.6937205140059461 ) ) ;
#81079 = CARTESIAN_POINT ( 'NONE',  ( 108.5379568639253449, -26.40872756427751611, 100.9641967044829727 ) ) ;
#81080 = CARTESIAN_POINT ( 'NONE',  ( 104.3129624051631907, -25.97697669550431243, 241.2880062282919482 ) ) ;
#81081 = LINE ( 'NONE', #74249, #16439 ) ;
#81082 = CARTESIAN_POINT ( 'NONE',  ( 162.0667039024469886, -67.87844715994089029, 222.2178068554179902 ) ) ;
#81084 = CARTESIAN_POINT ( 'NONE',  ( 69.68306499799194853, -72.55732494037970071, 540.9756252759101471 ) ) ;
#81083 = CARTESIAN_POINT ( 'NONE',  ( 116.3212776292296127, -32.94146857471318413, 287.6356252759109680 ) ) ;
#81085 = CARTESIAN_POINT ( 'NONE',  ( 173.9900000000000091, 28.98850000000000193, -58.73749999999999716 ) ) ;
#81086 = DIRECTION ( 'NONE',  ( 1.000000000000000078E-15, -1.000000000000000000, 0.000000000000000000 ) ) ;
#81087 = VECTOR ( 'NONE', #6010, 1000.000000000000000 ) ;
#81088 = CIRCLE ( 'NONE', #8517, 3.600000000000000089 ) ;
#81089 = VERTEX_POINT ( 'NONE', #22179 ) ;
#81090 = VERTEX_POINT ( 'NONE', #14911 ) ;
#81091 = EDGE_CURVE ( 'NONE', #83626, #14127, #43476, .T. ) ;
#81092 =( REPRESENTATION_RELATIONSHIP ('NONE','NONE', #82876, #87903 ) REPRESENTATION_RELATIONSHIP_WITH_TRANSFORMATION ( #77604 )SHAPE_REPRESENTATION_RELATIONSHIP( ) );
#81093 = CARTESIAN_POINT ( 'NONE',  ( 115.3083805796901373, -34.38525866856544866, 148.4695626852189605 ) ) ;
#81094 = AXIS2_PLACEMENT_3D ( 'NONE', #35400, #69495, #7272 ) ;
#81096 = VERTEX_POINT ( 'NONE', #2173 ) ;
#81095 = LINE ( 'NONE', #33812, #53100 ) ;
#81097 = DIRECTION ( 'NONE',  ( -1.000000000000000078E-15, 1.000000000000000083E-30, 1.000000000000000000 ) ) ;
#81098 = EDGE_CURVE ( 'NONE', #11575, #75698, #25763, .T. ) ;
#81099 = CARTESIAN_POINT ( 'NONE',  ( 114.0662423116485229, -44.47333502991302367, 129.1613395616249704 ) ) ;
#81100 = CARTESIAN_POINT ( 'NONE',  ( 142.0664832912739826, -9.729447159940995959, 14.92562527591100618 ) ) ;
#81101 = EDGE_CURVE ( 'NONE', #32858, #61827, #50399, .T. ) ;
#81102 = AXIS2_PLACEMENT_3D ( 'NONE', #34721, #84242, #62425 ) ;
#81103 = CARTESIAN_POINT ( 'NONE',  ( 0.000000000000000000, 215.0000000000000000, 159.6557476874258441 ) ) ;
#81104 = CARTESIAN_POINT ( 'NONE',  ( -74.89042153202872498, 78.46643079253875896, 91.90737012895671398 ) ) ;
#81105 = ADVANCED_FACE ( 'NONE', ( #1276 ), #46030, .T. ) ;
#81106 = CARTESIAN_POINT ( 'NONE',  ( 115.7831076713507343, -41.80230950795940714, 109.4064586094590652 ) ) ;
#81107 = VECTOR ( 'NONE', #26637, 1000.000000000000000 ) ;
#81108 = CARTESIAN_POINT ( 'NONE',  ( 115.5638989210038119, -29.55965564860105843, 74.38419670448293175 ) ) ;
#81109 = ORIENTED_EDGE ( 'NONE', *, *, #64976, .F. ) ;
#81110 = ORIENTED_EDGE ( 'NONE', *, *, #52130, .T. ) ;
#81111 = VERTEX_POINT ( 'NONE', #57564 ) ;
#81112 = CARTESIAN_POINT ( 'NONE',  ( 145.6286013927122553, -101.3636183722299222, 247.6387710704172491 ) ) ;
#81114 = DIRECTION ( 'NONE',  ( 1.000000000000000000, 0.000000000000000000, -9.299908063537909262E-17 ) ) ;
#81113 = CARTESIAN_POINT ( 'NONE',  ( 98.36735121233628831, -42.37464764417345719, 142.7965776568629508 ) ) ;
#81115 = LINE ( 'NONE', #46983, #17513 ) ;
#81116 = LINE ( 'NONE', #47439, #49520 ) ;
#81117 = EDGE_CURVE ( 'NONE', #24603, #4807, #63447, .T. ) ;
#81118 = CIRCLE ( 'NONE', #31799, 0.5000000000000004441 ) ;
#81119 = FACE_OUTER_BOUND ( 'NONE', #64240, .T. ) ;
#81120 = CARTESIAN_POINT ( 'NONE',  ( 89.13693605261661901, 92.64232203292139900, 78.17042387453797403 ) ) ;
#81121 = CARTESIAN_POINT ( 'NONE',  ( 67.06803645764867383, -67.87922922289656924, 245.5675989924858698 ) ) ;
#81122 = CARTESIAN_POINT ( 'NONE',  ( 106.6611865629619018, -26.33404432545455265, 85.10705384733896040 ) ) ;
#81123 = ORIENTED_EDGE ( 'NONE', *, *, #73892, .T. ) ;
#81124 = VERTEX_POINT ( 'NONE', #87517 ) ;
#81125 = CARTESIAN_POINT ( 'NONE',  ( 0.000000000000000000, 44.45000000000000284, 0.000000000000000000 ) ) ;
#81126 = DIRECTION ( 'NONE',  ( 1.000000000000000000, 1.276118419109374860E-15, 0.000000000000000000 ) ) ;
#81127 = CARTESIAN_POINT ( 'NONE',  ( 57.14999999999999858, 95.25000000000000000, 280.2255000000000109 ) ) ;
#81128 = CARTESIAN_POINT ( 'NONE',  ( 114.8623915286450199, -39.24071799505598079, 156.3966617981629668 ) ) ;
#81129 = AXIS2_PLACEMENT_3D ( 'NONE', #60289, #47554, #75285 ) ;
#81130 = DIRECTION ( 'NONE',  ( 0.7071067811575898476, -0.7071067812155052978, 0.000000000000000000 ) ) ;
#81131 = ORIENTED_EDGE ( 'NONE', *, *, #6962, .T. ) ;
#81132 = ORIENTED_EDGE ( 'NONE', *, *, #40241, .F. ) ;
#81133 = DIRECTION ( 'NONE',  ( 0.7759704746411385523, -0.6307692307692301936, 0.000000000000000000 ) ) ;
#81134 = ORIENTED_EDGE ( 'NONE', *, *, #80945, .F. ) ;
#81135 = ORIENTED_EDGE ( 'NONE', *, *, #50376, .T. ) ;
#81136 = DIRECTION ( 'NONE',  ( -1.000000000000000000, -8.953411488912552682E-16, 0.000000000000000000 ) ) ;
#81137 = CARTESIAN_POINT ( 'NONE',  ( 109.6768956016245227, -27.70380185851407973, 211.2720594963729752 ) ) ;
#81138 = AXIS2_PLACEMENT_3D ( 'NONE', #6868, #27760, #41815 ) ;
#81139 = LINE ( 'NONE', #32956, #44324 ) ;
#81140 = EDGE_CURVE ( 'NONE', #76300, #8047, #66159, .T. ) ;
#81141 = PLANE ( 'NONE',  #47244 ) ;
#81142 = DIRECTION ( 'NONE',  ( 0.000000000000000000, 1.000000000000000000, 0.000000000000000000 ) ) ;
#81143 = CONICAL_SURFACE ( 'NONE', #37630, 6.858000000000003205, 0.02993239667170383839 ) ;
#81144 = ORIENTED_EDGE ( 'NONE', *, *, #365, .F. ) ;
#81146 = ORIENTED_EDGE ( 'NONE', *, *, #70927, .T. ) ;
#81145 = AXIS2_PLACEMENT_3D ( 'NONE', #5938, #35402, #55831 ) ;
#81147 = VERTEX_POINT ( 'NONE', #79380 ) ;
#81148 = ORIENTED_EDGE ( 'NONE', *, *, #16815, .F. ) ;
#81149 = ADVANCED_FACE ( 'NONE', ( #18917 ), #65717, .F. ) ;
#81150 = CARTESIAN_POINT ( 'NONE',  ( 109.9373871219287082, -28.56496087843131448, 252.6376141791152747 ) ) ;
#81151 = VECTOR ( 'NONE', #58218, 1000.000000000000000 ) ;
#81152 = CARTESIAN_POINT ( 'NONE',  ( 104.2079940790944477, -25.20282339889105927, 90.26991099019693365 ) ) ;
#81153 = CARTESIAN_POINT ( 'NONE',  ( 101.7220374796296909, -27.76276858577399409, 85.50419670448295051 ) ) ;
#81154 = CARTESIAN_POINT ( 'NONE',  ( 108.0208457958009234, -27.96381440099374416, 249.5838068554170377 ) ) ;
#81155 = DIRECTION ( 'NONE',  ( -0.4214249218767880945, -0.9068632946707806397, -4.214249218767889924E-16 ) ) ;
#81156 = CARTESIAN_POINT ( 'NONE',  ( 72.31648329127402519, -45.62589376934781882, -5.074374724089063982 ) ) ;
#81157 = CARTESIAN_POINT ( 'NONE',  ( 103.5424053135282634, -26.88047730603072694, 186.3499109901969746 ) ) ;
#81158 = CARTESIAN_POINT ( 'NONE',  ( 100.9173739041163174, -44.68471384580785610, 277.0520784369447824 ) ) ;
#81159 = ORIENTED_EDGE ( 'NONE', *, *, #18517, .F. ) ;
#81160 = LINE ( 'NONE', #67494, #3200 ) ;
#81161 = ORIENTED_EDGE ( 'NONE', *, *, #31686, .F. ) ;
#81162 = ORIENTED_EDGE ( 'NONE', *, *, #72049, .T. ) ;
#81163 = AXIS2_PLACEMENT_3D ( 'NONE', #32891, #55101, #53758 ) ;
#81164 = CARTESIAN_POINT ( 'NONE',  ( 51.42025729302698522, -31.94127993907710206, -5.074374724088000832 ) ) ;
#81165 = CYLINDRICAL_SURFACE ( 'NONE', #41577, 0.5000000000000031086 ) ;
#81166 = ORIENTED_EDGE ( 'NONE', *, *, #51185, .T. ) ;
#81167 = CARTESIAN_POINT ( 'NONE',  ( 107.0664832912739399, -36.72944715994095333, 302.6356252759109680 ) ) ;
#81168 = EDGE_CURVE ( 'NONE', #31479, #45956, #15604, .T. ) ;
#81169 = CARTESIAN_POINT ( 'NONE',  ( 97.07199446366847440, -35.37919910817579705, 92.21901894701355218 ) ) ;
#81170 = CARTESIAN_POINT ( 'NONE',  ( 117.5955728976552166, -42.16808282502534411, 93.44705384733897802 ) ) ;
#81171 = CARTESIAN_POINT ( 'NONE',  ( 116.3212776292296127, -32.94146857471318413, 287.6356252759109680 ) ) ;
#81172 = DIRECTION ( 'NONE',  ( 1.000000000000000078E-15, -1.000000000000000083E-30, -1.000000000000000000 ) ) ;
#81173 = CARTESIAN_POINT ( 'NONE',  ( 116.3191775144681515, -32.94222376661483764, 89.13562527591095375 ) ) ;
#81176 = CARTESIAN_POINT ( 'NONE',  ( 107.6532706963292441, -47.74396045468172645, 193.6308633711489620 ) ) ;
#81175 = DIRECTION ( 'NONE',  ( 1.000000000000000000, 0.000000000000000000, 9.462128050782575008E-16 ) ) ;
#81174 = CARTESIAN_POINT ( 'NONE',  ( 32.24491389930059881, -32.11662333284641591, 313.9678068554150059 ) ) ;
#81177 = CARTESIAN_POINT ( 'NONE',  ( 83.06670390244796920, -58.35344715994099829, 231.5838068554150198 ) ) ;
#81178 = DIRECTION ( 'NONE',  ( 1.000000000000000000, 0.000000000000000000, 0.000000000000000000 ) ) ;
#81179 = VERTEX_POINT ( 'NONE', #3946 ) ;
#81180 = AXIS2_PLACEMENT_3D ( 'NONE', #14462, #69867, #61247 ) ;
#81181 = LINE ( 'NONE', #19826, #4869 ) ;
#81182 = LINE ( 'NONE', #18930, #5058 ) ;
#81183 = CARTESIAN_POINT ( 'NONE',  ( 98.34988348865829266, -31.65649366854221469, 135.9064676967609842 ) ) ;
#81184 = EDGE_CURVE ( 'NONE', #14045, #18758, #17142, .T. ) ;
#81185 = FACE_OUTER_BOUND ( 'NONE', #31414, .T. ) ;
#81187 = ORIENTED_EDGE ( 'NONE', *, *, #85707, .F. ) ;
#81186 = CARTESIAN_POINT ( 'NONE',  ( 115.8130859178907599, -30.97587361506452197, 254.2899109901966028 ) ) ;
#81188 = FACE_OUTER_BOUND ( 'NONE', #3680, .T. ) ;
#81189 = CARTESIAN_POINT ( 'NONE',  ( 105.7736751693905148, -26.36287077168075754, 266.1756252759109884 ) ) ;
#81190 = CARTESIAN_POINT ( 'NONE',  ( 97.75552660847078812, -42.77168409777202385, 142.7965776568629508 ) ) ;
#81191 = CARTESIAN_POINT ( 'NONE',  ( 53.97500000000000142, 95.25000000000000000, 283.4005000000000223 ) ) ;
#81192 = CARTESIAN_POINT ( 'NONE',  ( 82.77032304066686663, -37.23127003359135756, 6.817519769820709286 ) ) ;
#81193 = CIRCLE ( 'NONE', #18783, 0.5000000000000004441 ) ;
#81194 = CARTESIAN_POINT ( 'NONE',  ( 100.8594679592218171, 82.54999999999999716, -82.89895571708191824 ) ) ;
#81195 = CARTESIAN_POINT ( 'NONE',  ( 188.5667039024479834, -58.35344715994099829, 137.2178068554150059 ) ) ;
#81196 = LINE ( 'NONE', #12131, #33695 ) ;
#81197 = ORIENTED_EDGE ( 'NONE', *, *, #68486, .F. ) ;
#81198 = ORIENTED_EDGE ( 'NONE', *, *, #16812, .T. ) ;
#81199 = ORIENTED_EDGE ( 'NONE', *, *, #89384, .F. ) ;
#81200 = CIRCLE ( 'NONE', #41994, 1.000000000000000888 ) ;
#81201 = ORIENTED_EDGE ( 'NONE', *, *, #87574, .F. ) ;
#81202 = CARTESIAN_POINT ( 'NONE',  ( 20.03715912545824906, -46.82818131006190043, 249.9678068554150059 ) ) ;
#81203 = CARTESIAN_POINT ( 'NONE',  ( 118.0525141433397636, -37.71481444994962118, 29.74324432352998215 ) ) ;
#81204 = CARTESIAN_POINT ( 'NONE',  ( -24.20305689751608824, 54.97499999999995879, 58.62596543806478877 ) ) ;
#81205 = CARTESIAN_POINT ( 'NONE',  ( 87.67246433899146041, -140.4240802520271529, 246.9378847324709909 ) ) ;
#81206 = EDGE_CURVE ( 'NONE', #5947, #14550, #87966, .T. ) ;
#81207 = AXIS2_PLACEMENT_3D ( 'NONE', #24752, #72024, #86103 ) ;
#81209 = CARTESIAN_POINT ( 'NONE',  ( 172.5664832912740110, -27.82844715994070484, 203.6756252759119832 ) ) ;
#81208 = DIRECTION ( 'NONE',  ( -1.000000000000000078E-15, 1.000000000000000083E-30, 1.000000000000000000 ) ) ;
#81210 = CARTESIAN_POINT ( 'NONE',  ( 104.5043403851385904, -28.58134581971437882, 249.7409912566480727 ) ) ;
#81211 = VERTEX_POINT ( 'NONE', #58891 ) ;
#81212 = ORIENTED_EDGE ( 'NONE', *, *, #20741, .F. ) ;
#81213 = AXIS2_PLACEMENT_3D ( 'NONE', #39908, #62148, #75343 ) ;
#81215 = VERTEX_POINT ( 'NONE', #73428 ) ;
#81214 = AXIS2_PLACEMENT_3D ( 'NONE', #53260, #40557, #74194 ) ;
#81216 = DIRECTION ( 'NONE',  ( 0.9999999853157766072, 0.0001713722456127291416, -9.999999853157765648E-16 ) ) ;
#81217 = CARTESIAN_POINT ( 'NONE',  ( 111.4712670676476307, -45.71312987848808973, 182.9392243914140295 ) ) ;
#81218 = DIRECTION ( 'NONE',  ( 0.000000000000000000, 0.000000000000000000, -1.000000000000000000 ) ) ;
#81219 = DIRECTION ( 'NONE',  ( 0.000000000000000000, 0.000000000000000000, -1.000000000000000000 ) ) ;
#81220 = B_SPLINE_CURVE_WITH_KNOTS ( 'NONE', 3,
 ( #13590, #69006, #34473, #76263, #21304, #9919, #44407, #65324, #37625, #17622, #1764, #45302, #78969, #43966, #3101, #52103, #58928, #72145, #30362, #29917, #9033, #23561, #86668, #24440, #37171, #23120, #57606, #44865, #51669, #73020, #64880, #17180, #51224, #50792, #10790, #23998, #31233, #30799, #58492, #2664, #86221, #79419, #84893, #71261, #72594, #10357, #58058, #63989 ),
 .UNSPECIFIED., .F., .F.,
 ( 4, 2, 2, 2, 2, 2, 2, 2, 2, 1, 2, 2, 2, 2, 2, 2, 2, 2, 2, 2, 2, 1, 2, 2, 4 ),
 ( 0.05960646776571133093, 0.06208927922045071046, 0.06333068494782040370, 0.06457209067519009693, 0.06705490212992951116, 0.06829630785729923215, 0.06953771358466893926, 0.07202052503940842287, 0.07326193076677815774, 0.07450333649414789261, 0.07574474222151762748, 0.07698614794888736235, 0.07946895940362684596, 0.08195177085836631570, 0.08319317658573605057, 0.08443458231310579931, 0.08691739376784528293, 0.08815879949521501779, 0.08940020522258475266, 0.09188301667732420852, 0.09312442240469395727, 0.09436582813206367826, 0.09560723385943342700, 0.09684863958680314799, 0.09933145104154265936 ),
 .UNSPECIFIED. ) ;
#81221 = CARTESIAN_POINT ( 'NONE',  ( 101.5279499456468528, -29.13990343739101974, 26.99777378208800727 ) ) ;
#81222 = CARTESIAN_POINT ( 'NONE',  ( 117.8759966127888674, 83.38015080693121206, 12.67975824297127296 ) ) ;
#81223 = ADVANCED_FACE ( 'NONE', ( #38903 ), #8334, .T. ) ;
#81224 = CIRCLE ( 'NONE', #2878, 4.874999999999990230 ) ;
#81225 = CARTESIAN_POINT ( 'NONE',  ( 0.000000000000000000, 223.9999999999999716, 154.6557476874258441 ) ) ;
#81226 = ADVANCED_FACE ( 'NONE', ( #53403 ), #25729, .T. ) ;
#81227 = CARTESIAN_POINT ( 'NONE',  ( 113.9608400058234849, -28.00707201207230668, 274.5441967044828857 ) ) ;
#81228 = CARTESIAN_POINT ( 'NONE',  ( -487.2989999999999782, 14.28750000000026077, 11.11249999999970051 ) ) ;
#81229 = ORIENTED_EDGE ( 'NONE', *, *, #70350, .T. ) ;
#81230 = CARTESIAN_POINT ( 'NONE',  ( 103.5010607639055706, -27.38617375340112403, 56.36656921207620741 ) ) ;
#81231 = VECTOR ( 'NONE', #77673, 1000.000000000000000 ) ;
#81232 = DIRECTION ( 'NONE',  ( -0.8758084860610321210, -0.03696114963002913867, -0.4812414873652411940 ) ) ;
#81233 = CARTESIAN_POINT ( 'NONE',  ( 98.96126485936372319, -37.90763323093077020, 64.25951894101994810 ) ) ;
#81234 = DIRECTION ( 'NONE',  ( -2.999999999999999839E-15, 1.000000000000000000, -2.999999999999999900E-30 ) ) ;
#81235 = CARTESIAN_POINT ( 'NONE',  ( 130.0664832912740110, -18.82844715994099971, 239.5838068554170377 ) ) ;
#81236 = VECTOR ( 'NONE', #45589, 1000.000000000000000 ) ;
#81237 = CARTESIAN_POINT ( 'NONE',  ( -7.399411900505344697, 92.88009567113228115, 118.3253705404784739 ) ) ;
#81238 = ORIENTED_EDGE ( 'NONE', *, *, #81762, .F. ) ;
#81239 = LINE ( 'NONE', #53012, #88570 ) ;
#81240 = CARTESIAN_POINT ( 'NONE',  ( 121.8072289635121166, 60.27442714569195914, -46.99064742675564332 ) ) ;
#81241 = ORIENTED_EDGE ( 'NONE', *, *, #81919, .T. ) ;
#81242 = CARTESIAN_POINT ( 'NONE',  ( 113.9170494572507266, -28.05483877344520849, 124.5565776568629559 ) ) ;
#81243 = ORIENTED_EDGE ( 'NONE', *, *, #21100, .F. ) ;
#81244 = CARTESIAN_POINT ( 'NONE',  ( 101.5215670198552544, -44.69967496328137457, 86.51527697093396796 ) ) ;
#81245 = PLANE ( 'NONE',  #76458 ) ;
#81246 = CARTESIAN_POINT ( 'NONE',  ( 109.6943014565619450, -45.19247559555673632, 94.24729759161093057 ) ) ;
#81247 = CARTESIAN_POINT ( 'NONE',  ( 97.81168895331838087, -40.51742574516882200, 287.6356252759109680 ) ) ;
#81248 = CARTESIAN_POINT ( 'NONE',  ( 107.0664832912739399, -36.72944715994095333, 293.9356252759109793 ) ) ;
#81249 = AXIS2_PLACEMENT_3D ( 'NONE', #14067, #21335, #62212 ) ;
#81250 = CARTESIAN_POINT ( 'NONE',  ( 103.4696982656617479, -25.41196563057017244, 51.32133956162493149 ) ) ;
#81251 = FACE_OUTER_BOUND ( 'NONE', #77416, .T. ) ;
#81252 = ORIENTED_EDGE ( 'NONE', *, *, #67526, .F. ) ;
#81253 = CARTESIAN_POINT ( 'NONE',  ( 116.3214902495786873, -32.94210931476069248, 180.1356252759109680 ) ) ;
#81254 = ORIENTED_EDGE ( 'NONE', *, *, #7986, .T. ) ;
#81255 = CARTESIAN_POINT ( 'NONE',  ( 77.53258422225754032, -19.79809288067777118, 2.811527366592890154 ) ) ;
#81256 = ORIENTED_EDGE ( 'NONE', *, *, #28557, .F. ) ;
#81257 = VERTEX_POINT ( 'NONE', #30764 ) ;
#81258 = ADVANCED_FACE ( 'NONE', ( #79828, #10750 ), #10320, .T. ) ;
#81259 = AXIS2_PLACEMENT_3D ( 'NONE', #7698, #13615, #35387 ) ;
#81260 = LINE ( 'NONE', #53943, #33929 ) ;
#81261 = ORIENTED_EDGE ( 'NONE', *, *, #89798, .T. ) ;
#81262 = CARTESIAN_POINT ( 'NONE',  ( 98.14754276252327259, -43.36755551587079083, 261.8356252759109566 ) ) ;
#81263 = CARTESIAN_POINT ( 'NONE',  ( 248.6659999999999968, 52.73749999999999716, -10.97647784993501396 ) ) ;
#81264 = CARTESIAN_POINT ( 'NONE',  ( 154.4409905298078058, -0.9147987323338667709, 396.9756252759102040 ) ) ;
#81265 = CARTESIAN_POINT ( 'NONE',  ( 117.9246037767874498, -41.47663949653230020, 54.49848241876792088 ) ) ;
#81266 = CYLINDRICAL_SURFACE ( 'NONE', #88667, 1.000000000000000888 ) ;
#81267 = ORIENTED_EDGE ( 'NONE', *, *, #40200, .F. ) ;
#81268 = DIRECTION ( 'NONE',  ( 0.5000000000000015543, -0.8660254037844377084, 2.688821387764056676E-14 ) ) ;
#81269 = AXIS2_PLACEMENT_3D ( 'NONE', #8344, #55552, #7442 ) ;
#81270 = DIRECTION ( 'NONE',  ( 0.000000000000000000, 0.000000000000000000, 1.000000000000000000 ) ) ;
#81271 = ORIENTED_EDGE ( 'NONE', *, *, #7946, .T. ) ;
#81272 = AXIS2_PLACEMENT_3D ( 'NONE', #87074, #38452, #24840 ) ;
#81273 = CYLINDRICAL_SURFACE ( 'NONE', #35887, 7.143750000000004263 ) ;
#81274 = ADVANCED_FACE ( 'NONE', ( #32091 ), #4846, .F. ) ;
#81275 = CARTESIAN_POINT ( 'NONE',  ( 80.54920390244805617, -58.72944715994108833, 231.5838068554169524 ) ) ;
#81276 = CARTESIAN_POINT ( 'NONE',  ( 112.3272512417296980, -28.22507648531173530, 289.6356252759109680 ) ) ;
#81277 = DIRECTION ( 'NONE',  ( 1.000000000000000000, 4.163336342344333240E-14, 0.000000000000000000 ) ) ;
#81278 = CARTESIAN_POINT ( 'NONE',  ( 107.0664832912739541, -36.72944715994095333, 309.2406250056037038 ) ) ;
#81279 = CARTESIAN_POINT ( 'NONE',  ( 99.04430456227140667, -42.84162139839268235, 91.84393114961771687 ) ) ;
#81280 = CARTESIAN_POINT ( 'NONE',  ( 98.21912858861395534, -34.79631884261151242, 255.5657531614102709 ) ) ;
#81282 = CARTESIAN_POINT ( 'NONE',  ( 117.3319688044106925, -38.62265419183309945, 84.68133956162593279 ) ) ;
#81281 = DIRECTION ( 'NONE',  ( 0.000000000000000000, -1.000000000000000000, 0.000000000000000000 ) ) ;
#81283 = FACE_OUTER_BOUND ( 'NONE', #55546, .T. ) ;
#81284 = CARTESIAN_POINT ( 'NONE',  ( 103.7935660395325073, -26.78486678718983072, 165.3299109901969643 ) ) ;
#81285 = VERTEX_POINT ( 'NONE', #39360 ) ;
#81286 = CARTESIAN_POINT ( 'NONE',  ( 146.0667039024470171, -83.77844715994089597, 55.21780685541800437 ) ) ;
#81287 = ORIENTED_EDGE ( 'NONE', *, *, #24893, .F. ) ;
#81289 = EDGE_CURVE ( 'NONE', #17437, #47694, #72983, .T. ) ;
#81288 = AXIS2_PLACEMENT_3D ( 'NONE', #14207, #62347, #128 ) ;
#81290 = DIRECTION ( 'NONE',  ( 0.8660254037844432595, 0.4999999999999921174, 0.000000000000000000 ) ) ;
#81291 = CARTESIAN_POINT ( 'NONE',  ( 57.56670390244832447, -48.82844715994039575, 257.2178068554150627 ) ) ;
#81292 = CARTESIAN_POINT ( 'NONE',  ( 110.9303245704231102, -101.4704344580498514, -19.78219314458209865 ) ) ;
#81293 = DIRECTION ( 'NONE',  ( -4.237773401492740281E-14, 1.000000000000000000, 0.000000000000000000 ) ) ;
#81294 = ORIENTED_EDGE ( 'NONE', *, *, #46236, .F. ) ;
#81295 = ADVANCED_FACE ( 'NONE', ( #59787 ), #59347, .T. ) ;
#81296 = EDGE_CURVE ( 'NONE', #22712, #85960, #8347, .T. ) ;
#81297 = CARTESIAN_POINT ( 'NONE',  ( 97.81066791858781073, -40.51493114651297134, 51.63541036076257740 ) ) ;
#81299 = ORIENTED_EDGE ( 'NONE', *, *, #11010, .T. ) ;
#81298 = CARTESIAN_POINT ( 'NONE',  ( 98.41978056949241704, -42.69487473605161654, 126.8070538473389490 ) ) ;
#81300 = LINE ( 'NONE', #81742, #33520 ) ;
#81301 = AXIS2_PLACEMENT_3D ( 'NONE', #35787, #88980, #55760 ) ;
#81302 = CARTESIAN_POINT ( 'NONE',  ( -130.4016766882983234, 93.55256755804781221, -6.356666657630320572 ) ) ;
#81303 = FACE_OUTER_BOUND ( 'NONE', #58183, .T. ) ;
#81304 = EDGE_CURVE ( 'NONE', #35335, #75906, #23482, .T. ) ;
#81305 = CARTESIAN_POINT ( 'NONE',  ( 142.0664832912740394, -46.47944715994099596, 14.67562527591100441 ) ) ;
#81306 = ORIENTED_EDGE ( 'NONE', *, *, #41872, .F. ) ;
#81307 = CARTESIAN_POINT ( 'NONE',  ( -107.0569861830068845, 79.12155284005903866, -223.2310704183842347 ) ) ;
#81308 = EDGE_CURVE ( 'NONE', #4456, #26477, #30116, .T. ) ;
#81309 = DIRECTION ( 'NONE',  ( 0.7071067811989784069, -0.7071067811741166276, 7.071067811989791923E-16 ) ) ;
#81310 = CARTESIAN_POINT ( 'NONE',  ( -141.3509999999999991, 20.32000000000000028, 141.3509999999999991 ) ) ;
#81311 = ORIENTED_EDGE ( 'NONE', *, *, #29177, .F. ) ;
#81312 = AXIS2_PLACEMENT_3D ( 'NONE', #27051, #7058, #77442 ) ;
#81313 = ORIENTED_EDGE ( 'NONE', *, *, #58084, .F. ) ;
#81314 = DIRECTION ( 'NONE',  ( -0.1811243269278930978, 0.9834602067165288952, 0.000000000000000000 ) ) ;
#81315 = CARTESIAN_POINT ( 'NONE',  ( 85.31607583734475497, 90.93081950567957961, -98.82361644294707048 ) ) ;
#81316 = DIRECTION ( 'NONE',  ( -0.000000000000000000, -0.000000000000000000, 1.000000000000000000 ) ) ;
#81317 = EDGE_CURVE ( 'NONE', #13444, #50715, #43824, .T. ) ;
#81318 = FACE_OUTER_BOUND ( 'NONE', #66835, .T. ) ;
#81320 = CARTESIAN_POINT ( 'NONE',  ( 123.4696824136382105, 0.000000000000000000, -179.8898777604649979 ) ) ;
#81319 = CARTESIAN_POINT ( 'NONE',  ( 97.31584970183817518, -39.30599062596471072, 106.5314598669042425 ) ) ;
#81321 = CARTESIAN_POINT ( 'NONE',  ( 97.12557807017356026, -37.99703648465538208, 181.4273212068781902 ) ) ;
#81322 = VECTOR ( 'NONE', #17210, 1000.000000000000000 ) ;
#81323 = VERTEX_POINT ( 'NONE', #29329 ) ;
#81324 = CARTESIAN_POINT ( 'NONE',  ( 6.938893903907229955E-15, 50.79999999999999716, 216.0269999999999868 ) ) ;
#81325 = CARTESIAN_POINT ( 'NONE',  ( 113.6884830475838442, -29.53135334845051574, 195.4841967044819739 ) ) ;
#81327 = ORIENTED_EDGE ( 'NONE', *, *, #34321, .F. ) ;
#81326 = CARTESIAN_POINT ( 'NONE',  ( -29.99999999999998224, 127.0000000000000000, 114.8826257785461280 ) ) ;
#81328 = AXIS2_PLACEMENT_3D ( 'NONE', #16986, #51476, #85598 ) ;
#81329 = ADVANCED_FACE ( 'NONE', ( #42474 ), #14808, .T. ) ;
#81330 = CARTESIAN_POINT ( 'NONE',  ( 104.6499073705539473, -46.24122592705968771, 43.37848241876795896 ) ) ;
#81332 = EDGE_CURVE ( 'NONE', #51305, #33391, #57009, .T. ) ;
#81331 = DIRECTION ( 'NONE',  ( 0.000000000000000000, 0.000000000000000000, -1.000000000000000000 ) ) ;
#81333 = CARTESIAN_POINT ( 'NONE',  ( 147.0667039024471592, -67.87844715994090450, 245.4990136654952835 ) ) ;
#81334 = EDGE_CURVE ( 'NONE', #28440, #43956, #7976, .T. ) ;
#81335 = DIRECTION ( 'NONE',  ( 1.639958061481212836E-42, -4.100000000000000342E-29, -1.000000000000000000 ) ) ;
#81336 = VECTOR ( 'NONE', #24639, 1000.000000000000114 ) ;
#81337 = ORIENTED_EDGE ( 'NONE', *, *, #32838, .T. ) ;
#81338 = CARTESIAN_POINT ( 'NONE',  ( 97.81413651554109379, -40.51640884438177181, 97.63607350422876152 ) ) ;
#81339 = EDGE_CURVE ( 'NONE', #66434, #77147, #21056, .T. ) ;
#81340 = ORIENTED_EDGE ( 'NONE', *, *, #82015, .F. ) ;
#81341 = ORIENTED_EDGE ( 'NONE', *, *, #81117, .T. ) ;
#81342 = CARTESIAN_POINT ( 'NONE',  ( 106.8838381269920745, -46.12323054477403161, 223.9806309249449612 ) ) ;
#81343 = AXIS2_PLACEMENT_3D ( 'NONE', #9557, #37262, #22297 ) ;
#81344 = DIRECTION ( 'NONE',  ( 0.000000000000000000, 1.000000000000000000, 0.000000000000000000 ) ) ;
#81345 = DIRECTION ( 'NONE',  ( 1.907762142705490052E-15, 7.167082501179359715E-16, -1.000000000000000000 ) ) ;
#81346 = DIRECTION ( 'NONE',  ( -3.100000000000000258E-29, 3.100000000000000044E-14, 1.000000000000000000 ) ) ;
#81347 = VECTOR ( 'NONE', #56307, 1000.000000000000000 ) ;
#81348 = DIRECTION ( 'NONE',  ( 1.000000000000000000, 0.000000000000000000, 0.000000000000000000 ) ) ;
#81349 = ORIENTED_EDGE ( 'NONE', *, *, #43205, .F. ) ;
#81350 = DIRECTION ( 'NONE',  ( 0.9963424814100680926, -0.08544974978095712381, 0.000000000000000000 ) ) ;
#81351 = CARTESIAN_POINT ( 'NONE',  ( 177.1649999999999920, 5.112500000000000711, -58.73749999999999716 ) ) ;
#81352 = VERTEX_POINT ( 'NONE', #8435 ) ;
#81353 = CARTESIAN_POINT ( 'NONE',  ( 104.5933598291445463, -26.62426044571792616, 285.2670538473396391 ) ) ;
#81354 = ORIENTED_EDGE ( 'NONE', *, *, #45351, .T. ) ;
#81355 = ORIENTED_EDGE ( 'NONE', *, *, #70057, .T. ) ;
#81356 = CARTESIAN_POINT ( 'NONE',  ( 101.6421866332951396, -42.82917926744636361, 264.8166617981626700 ) ) ;
#81357 = CARTESIAN_POINT ( 'NONE',  ( -194.1576000000000022, 101.5999999999999943, -9.525000000000000355 ) ) ;
#81358 = CARTESIAN_POINT ( 'NONE',  ( 116.2045471004838078, -43.06251688283441581, 163.3441967044829823 ) ) ;
#81359 = DIRECTION ( 'NONE',  ( -0.000000000000000000, -1.000000000000000000, -0.000000000000000000 ) ) ;
#81360 = CARTESIAN_POINT ( 'NONE',  ( 130.1657039024480014, -18.82844715994099971, 239.5838068554170377 ) ) ;
#81361 = DIRECTION ( 'NONE',  ( 0.000000000000000000, 0.000000000000000000, 1.000000000000000000 ) ) ;
#81362 = CARTESIAN_POINT ( 'NONE',  ( 115.4227270478554317, -30.42340481720227885, 215.3413395616249773 ) ) ;
#81363 = CARTESIAN_POINT ( 'NONE',  ( 92.32962665258612844, 82.54999999999999716, -74.36911441044637172 ) ) ;
#81364 = VERTEX_POINT ( 'NONE', #707 ) ;
#81365 = CARTESIAN_POINT ( 'NONE',  ( 109.6947933286257353, -47.51320739032397000, 83.75467289495897205 ) ) ;
#81366 = DIRECTION ( 'NONE',  ( 1.000000000000000078E-15, 0.000000000000000000, 1.000000000000000000 ) ) ;
#81367 = ORIENTED_EDGE ( 'NONE', *, *, #35609, .T. ) ;
#81368 = VERTEX_POINT ( 'NONE', #85203 ) ;
#81369 = ORIENTED_EDGE ( 'NONE', *, *, #12050, .F. ) ;
#81370 = CIRCLE ( 'NONE', #61037, 87.89999999999997726 ) ;
#81371 = CARTESIAN_POINT ( 'NONE',  ( 45.77381068350460680, -48.62134037888156968, 300.4678068554150059 ) ) ;
#81372 = DIRECTION ( 'NONE',  ( 0.000000000000000000, -1.000000000000000000, 0.000000000000000000 ) ) ;
#81373 = DIRECTION ( 'NONE',  ( -0.9254794337955620787, -0.3787978585227822492, 0.000000000000000000 ) ) ;
#81374 = CARTESIAN_POINT ( 'NONE',  ( 103.4072989863811074, -28.88653346237834185, 133.2299951314959685 ) ) ;
#81375 = CARTESIAN_POINT ( 'NONE',  ( 98.01791376823749147, -44.42006743888428133, 222.8870538473399563 ) ) ;
#81376 = CARTESIAN_POINT ( 'NONE',  ( -3.174999999999644995, 24.56180297284579694, 33.98325472291465132 ) ) ;
#81377 = ORIENTED_EDGE ( 'NONE', *, *, #37597, .T. ) ;
#81378 = SURFACE_SIDE_STYLE ('',( #54059 ) ) ;
#81379 = CARTESIAN_POINT ( 'NONE',  ( 136.8005346357622614, -37.07423037058595838, 3.076719480830206077 ) ) ;
#81380 = AXIS2_PLACEMENT_3D ( 'NONE', #16475, #30548, #84189 ) ;
#81381 = VERTEX_POINT ( 'NONE', #51088 ) ;
#81382 = EDGE_LOOP ( 'NONE', ( #9717, #35343 ) ) ;
#81383 = CARTESIAN_POINT ( 'NONE',  ( 31.56670390244700641, -19.82844715994111340, -5.074374724088000832 ) ) ;
#81384 = EDGE_CURVE ( 'NONE', #29549, #4973, #71118, .T. ) ;
#81385 = EDGE_LOOP ( 'NONE', ( #46930, #69403, #70367, #32241, #14617 ) ) ;
#81386 = ORIENTED_EDGE ( 'NONE', *, *, #61861, .T. ) ;
#81387 = DIRECTION ( 'NONE',  ( -1.000200923085726652E-15, -1.000000000000000000, 0.000000000000000000 ) ) ;
#81388 = CYLINDRICAL_SURFACE ( 'NONE', #84961, 10.00000000000000711 ) ;
#81389 = ADVANCED_FACE ( 'NONE', ( #28876 ), #48582, .T. ) ;
#81390 = CARTESIAN_POINT ( 'NONE',  ( 97.31589562384981207, -39.30610287545482606, 26.53146951830015610 ) ) ;
#81391 = CARTESIAN_POINT ( 'NONE',  ( 102.8925193805077498, -44.76628084087394654, 166.6057531614099503 ) ) ;
#81392 = CARTESIAN_POINT ( 'NONE',  ( 96.14704956656235879, -38.72415284237285960, 51.48229194257797303 ) ) ;
#81393 = DIRECTION ( 'NONE',  ( -1.000000000000000000, -0.000000000000000000, -0.000000000000000000 ) ) ;
#81394 = ORIENTED_EDGE ( 'NONE', *, *, #82021, .F. ) ;
#81395 = EDGE_CURVE ( 'NONE', #14785, #11421, #71563, .T. ) ;
#81396 = DIRECTION ( 'NONE',  ( 0.000000000000000000, 0.000000000000000000, -1.000000000000000000 ) ) ;
#81397 = CONICAL_SURFACE ( 'NONE', #55212, 190.5000000000000000, 0.7853981633974300713 ) ;
#81398 = EDGE_LOOP ( 'NONE', ( #1258, #41773, #8209, #6027 ) ) ;
#81399 = EDGE_CURVE ( 'NONE', #1134, #24776, #22079, .T. ) ;
#81400 = AXIS2_PLACEMENT_3D ( 'NONE', #22129, #70713, #42973 ) ;
#81401 = EDGE_CURVE ( 'NONE', #69984, #1742, #14357, .T. ) ;
#81402 = CARTESIAN_POINT ( 'NONE',  ( 97.80969226196111777, -40.51824922604903634, 262.6357212258262166 ) ) ;
#81403 = ORIENTED_EDGE ( 'NONE', *, *, #76967, .T. ) ;
#81404 = B_SPLINE_CURVE_WITH_KNOTS ( 'NONE', 3,
 ( #77420, #55594, #8385, #56511, #56051, #49698, #69716, #35169, #84702, #42875, #70609, #71515, #50595, #14306, #83796, #76521, #50140, #84254, #41982, #71070, #21572, #36084, #2015, #78337, #63796 ),
 .UNSPECIFIED., .F., .F.,
 ( 4, 2, 2, 2, 2, 2, 2, 2, 2, 1, 2, 2, 4 ),
 ( 0.05959919981814688211, 0.06208050401323544909, 0.06332115611077974993, 0.06456180820832406464, 0.06704311240341262468, 0.06828376450095689776, 0.06952441659850118472, 0.07200572079358977251, 0.07324637289113407335, 0.07448702498867838806, 0.07572767708622268890, 0.07696832918376700361, 0.07944963337885561916 ),
 .UNSPECIFIED. ) ;
#81405 = CARTESIAN_POINT ( 'NONE',  ( 152.4532656103850172, -72.54314042502360849, 542.9756252759101471 ) ) ;
#81406 = CARTESIAN_POINT ( 'NONE',  ( -12.59999999999999964, 82.54999999999999716, 117.8845415480757595 ) ) ;
#81407 = DIRECTION ( 'NONE',  ( -0.9254794337955621897, -0.3787978585227819717, 0.000000000000000000 ) ) ;
#81408 = AXIS2_PLACEMENT_3D ( 'NONE', #14479, #50774, #71681 ) ;
#81409 = EDGE_CURVE ( 'NONE', #72980, #26828, #50192, .T. ) ;
#81410 = CARTESIAN_POINT ( 'NONE',  ( 25.56670390244797275, -58.35344715994099829, 173.2178068554149775 ) ) ;
#81411 = ORIENTED_EDGE ( 'NONE', *, *, #72352, .T. ) ;
#81412 = CARTESIAN_POINT ( 'NONE',  ( 117.5344697633125577, -37.28603910398157240, 18.78419670448294809 ) ) ;
#81413 = CARTESIAN_POINT ( 'NONE',  ( 96.91449086013869874, -32.24229349230230923, 51.98324432352996638 ) ) ;
#81414 = ADVANCED_FACE ( 'NONE', ( #15701 ), #43375, .T. ) ;
#81416 = CYLINDRICAL_SURFACE ( 'NONE', #83357, 4.500000000000003553 ) ;
#81415 = CARTESIAN_POINT ( 'NONE',  ( 135.5667039024470171, -90.27844715994091018, 45.21780685541799727 ) ) ;
#81417 = CARTESIAN_POINT ( 'NONE',  ( 31.71315051185421297, -33.70561438052095582, 193.9678068554150911 ) ) ;
#81418 = CARTESIAN_POINT ( 'NONE',  ( 133.3151861768211006, -39.40257939794550879, 8.160477455076955877 ) ) ;
#81419 = CARTESIAN_POINT ( 'NONE',  ( -75.61066417432020614, 20.32000000000000028, 189.7379999999999995 ) ) ;
#81420 = VECTOR ( 'NONE', #61252, 1000.000000000000000 ) ;
#81421 = EDGE_CURVE ( 'NONE', #78184, #76706, #22970, .T. ) ;
#81422 = CARTESIAN_POINT ( 'NONE',  ( 146.6554688966711808, -67.87104837875700980, 246.9811635433789831 ) ) ;
#81423 = ORIENTED_EDGE ( 'NONE', *, *, #68762, .F. ) ;
#81424 = CARTESIAN_POINT ( 'NONE',  ( 109.6539202653692087, -46.87399426414072678, 47.77562527591094721 ) ) ;
#81425 = CARTESIAN_POINT ( 'NONE',  ( 104.4537254180046375, -26.63707460721619213, 196.2784824187679362 ) ) ;
#81426 = CARTESIAN_POINT ( 'NONE',  ( 98.62975546523678361, -43.90627301359564427, 72.89943479972099283 ) ) ;
#81427 = DIRECTION ( 'NONE',  ( -1.000000000000000078E-15, 1.000000000000000000, 0.000000000000000000 ) ) ;
#81428 = DIRECTION ( 'NONE',  ( 0.000000000000000000, 1.000000000000000000, 0.000000000000000000 ) ) ;
#81429 = DIRECTION ( 'NONE',  ( 0.000000000000000000, -1.000000000000000000, 0.000000000000000000 ) ) ;
#81430 = ORIENTED_EDGE ( 'NONE', *, *, #43012, .F. ) ;
#81431 = CARTESIAN_POINT ( 'NONE',  ( 109.1197153606379828, -46.32621810461552059, 103.7441967044819791 ) ) ;
#81433 = ORIENTED_EDGE ( 'NONE', *, *, #39314, .T. ) ;
#81432 = CARTESIAN_POINT ( 'NONE',  ( 7.047591375350159559, 93.11510580299035666, 130.3656419271163998 ) ) ;
#81434 = VECTOR ( 'NONE', #30906, 1000.000000000000000 ) ;
#81435 = CARTESIAN_POINT ( 'NONE',  ( 97.03753386688410387, -33.96379371595042329, 247.1127681330539758 ) ) ;
#81436 = CARTESIAN_POINT ( 'NONE',  ( 113.1776502951240388, -44.75236549504541728, 254.0960424504467596 ) ) ;
#81437 = FACE_OUTER_BOUND ( 'NONE', #75411, .T. ) ;
#81438 = CARTESIAN_POINT ( 'NONE',  ( 179.1667039024460166, -28.27351298637280408, -5.074374724088000832 ) ) ;
#81439 = DIRECTION ( 'NONE',  ( -0.000000000000000000, -0.000000000000000000, 1.000000000000000000 ) ) ;
#81440 = EDGE_CURVE ( 'NONE', #14322, #26947, #64732, .T. ) ;
#81441 = DIRECTION ( 'NONE',  ( -3.100000000000000258E-29, 3.100000000000000044E-14, 1.000000000000000000 ) ) ;
#81442 = DIRECTION ( 'NONE',  ( 0.000000000000000000, 0.000000000000000000, -1.000000000000000000 ) ) ;
#81443 = EDGE_CURVE ( 'NONE', #31184, #3831, #6526, .T. ) ;
#81444 = CARTESIAN_POINT ( 'NONE',  ( 113.8941270090217444, -29.67983328691845557, 174.4641967044829585 ) ) ;
#81445 = ORIENTED_EDGE ( 'NONE', *, *, #89926, .F. ) ;
#81446 = CIRCLE ( 'NONE', #37912, 0.9999999999999800160 ) ;
#81447 = ORIENTED_EDGE ( 'NONE', *, *, #74991, .T. ) ;
#81448 = CARTESIAN_POINT ( 'NONE',  ( 116.1082436049511415, -39.28347229878176705, 140.0511071154209617 ) ) ;
#81449 = CIRCLE ( 'NONE', #23417, 2.116999999999993776 ) ;
#81450 = CARTESIAN_POINT ( 'NONE',  ( 113.5448393278429364, -34.07786215028152554, -2.364374724089013391 ) ) ;
#81452 = CARTESIAN_POINT ( 'NONE',  ( 172.5664832912740110, -36.32844715994070839, 74.17562527591199739 ) ) ;
#81451 = CARTESIAN_POINT ( 'NONE',  ( 100.6687104580203567, -44.89077600156390702, 273.0594347997199520 ) ) ;
#81453 = LINE ( 'NONE', #5582, #87020 ) ;
#81454 = LINE ( 'NONE', #81005, #44621 ) ;
#81455 = FACE_OUTER_BOUND ( 'NONE', #12148, .T. ) ;
#81456 = DIRECTION ( 'NONE',  ( 0.000000000000000000, 0.000000000000000000, -1.000000000000000000 ) ) ;
#81457 = DIRECTION ( 'NONE',  ( 1.000000000000000000, 0.000000000000000000, 0.000000000000000000 ) ) ;
#81458 = CARTESIAN_POINT ( 'NONE',  ( 113.7366723824214887, -44.71300795807898965, 193.1299109901969757 ) ) ;
#81459 = DIRECTION ( 'NONE',  ( -4.012088370409549976E-14, 1.000000000000000000, 0.000000000000000000 ) ) ;
#81460 = EDGE_LOOP ( 'NONE', ( #34444, #67997, #26138, #24775 ) ) ;
#81461 = ORIENTED_EDGE ( 'NONE', *, *, #9230, .T. ) ;
#81462 = AXIS2_PLACEMENT_3D ( 'NONE', #43425, #23022, #15752 ) ;
#81463 = CARTESIAN_POINT ( 'NONE',  ( -86.19613171056677459, 73.00415124681445889, -98.05713019660817054 ) ) ;
#81464 = DIRECTION ( 'NONE',  ( -1.000000000000000000, -1.734723475976808672E-15, 0.000000000000000000 ) ) ;
#81465 = CARTESIAN_POINT ( 'NONE',  ( 156.5667039024485803, -48.82844715993568485, 134.7178068554149775 ) ) ;
#81466 = CARTESIAN_POINT ( 'NONE',  ( 28.57499999999999929, 87.13271776169258942, 310.8325000000000387 ) ) ;
#81467 = AXIS2_PLACEMENT_3D ( 'NONE', #10228, #31552, #23437 ) ;
#81468 = CARTESIAN_POINT ( 'NONE',  ( 270.8910000000000196, 40.03750000000000142, -67.11950000000000216 ) ) ;
#81469 = EDGE_LOOP ( 'NONE', ( #70897, #81146, #78109, #45818, #31222, #52802, #27269, #63065, #8865, #49856, #61806, #56216, #6134, #39351, #28020, #84466, #39991, #71873, #73014, #89630, #6271, #38092, #73355, #82241, #85957, #49428, #31124, #52095, #27061, #43113, #23014, #44869, #12043, #82964, #69806, #61558, #70685, #38180, #53028, #28077, #39368, #59654, #50576, #65205, #54880, #15797, #82723, #54153 ) ) ;
#81470 = CARTESIAN_POINT ( 'NONE',  ( -10.00075923923900589, 90.22574527804057709, 117.9330208250991490 ) ) ;
#81471 = CARTESIAN_POINT ( 'NONE',  ( 97.91908366271991326, -41.73065806300744640, 221.7241967044819546 ) ) ;
#81472 = DIRECTION ( 'NONE',  ( 0.000000000000000000, 0.000000000000000000, 1.000000000000000000 ) ) ;
#81473 = ORIENTED_EDGE ( 'NONE', *, *, #79184, .T. ) ;
#81474 = VECTOR ( 'NONE', #2742, 1000.000000000000000 ) ;
#81475 = CARTESIAN_POINT ( 'NONE',  ( -12.70000000000000284, 81.72078997525719046, 117.8738102209307641 ) ) ;
#81476 = CARTESIAN_POINT ( 'NONE',  ( 184.5664832912729878, -71.37844715994266664, 342.9256252759109884 ) ) ;
#81477 = PLANE ( 'NONE',  #28104 ) ;
#81478 = AXIS2_PLACEMENT_3D ( 'NONE', #40252, #54755, #33889 ) ;
#81479 = CARTESIAN_POINT ( 'NONE',  ( 101.9647735066782843, -29.73848997801458083, 28.38428084578198352 ) ) ;
#81480 = CARTESIAN_POINT ( 'NONE',  ( 102.6068629045982021, -46.86833229348674479, 128.2346728949589760 ) ) ;
#81481 = CARTESIAN_POINT ( 'NONE',  ( 33.96670390244647564, -26.71338133339342136, 193.9678068554150911 ) ) ;
#81482 = ORIENTED_EDGE ( 'NONE', *, *, #62438, .F. ) ;
#81483 = DIRECTION ( 'NONE',  ( 0.7071067811865496822, -0.7071067811865453523, 0.000000000000000000 ) ) ;
#81484 = EDGE_CURVE ( 'NONE', #50121, #75621, #2201, .T. ) ;
#81485 = CARTESIAN_POINT ( 'NONE',  ( 82.77273044669111357, -18.23917853419690971, 6.814128304791288393 ) ) ;
#81486 = ORIENTED_EDGE ( 'NONE', *, *, #799, .F. ) ;
#81487 = ORIENTED_EDGE ( 'NONE', *, *, #65864, .T. ) ;
#81488 = DIRECTION ( 'NONE',  ( 6.982966722218760189E-15, 0.000000000000000000, -1.000000000000000000 ) ) ;
#81489 = VERTEX_POINT ( 'NONE', #66049 ) ;
#81490 = VERTEX_POINT ( 'NONE', #17472 ) ;
#81491 = CARTESIAN_POINT ( 'NONE',  ( 75.31670390244798341, -50.82844715994100682, 60.91780685541480267 ) ) ;
#81492 = EDGE_CURVE ( 'NONE', #61827, #75223, #83439, .T. ) ;
#81493 = CARTESIAN_POINT ( 'NONE',  ( 99.45175552060571533, -32.86007347668476086, 50.37527697093396739 ) ) ;
#81494 = CARTESIAN_POINT ( 'NONE',  ( 96.02321403599634664, -35.86825885766610611, 191.2765776568629690 ) ) ;
#81495 = AXIS2_PLACEMENT_3D ( 'NONE', #63180, #84549, #49534 ) ;
#81496 = EDGE_CURVE ( 'NONE', #15404, #81489, #5038, .T. ) ;
#81497 = CARTESIAN_POINT ( 'NONE',  ( 117.7782040715257921, -34.09831434418944696, 164.0061014663869798 ) ) ;
#81499 = CARTESIAN_POINT ( 'NONE',  ( 96.88896422860915436, -30.65880273170215276, 276.8984824187680829 ) ) ;
#81498 = CARTESIAN_POINT ( 'NONE',  ( 113.5781282841511484, -44.42724326460464823, 23.13510136712798371 ) ) ;
#81500 = CARTESIAN_POINT ( 'NONE',  ( 188.5667039024486087, -48.82844715993430640, 134.7178068554150059 ) ) ;
#81501 = DIRECTION ( 'NONE',  ( 0.000000000000000000, -1.000000000000000000, 0.000000000000000000 ) ) ;
#81502 = ORIENTED_EDGE ( 'NONE', *, *, #71171, .F. ) ;
#81503 = EDGE_CURVE ( 'NONE', #30378, #67525, #80604, .T. ) ;
#81504 = VERTEX_POINT ( 'NONE', #58783 ) ;
#81505 = VECTOR ( 'NONE', #63171, 1000.000000000000000 ) ;
#81506 = ADVANCED_FACE ( 'NONE', ( #86969 ), #3840, .T. ) ;
#81507 = CIRCLE ( 'NONE', #56830, 38.10000000000000142 ) ;
#81508 = DIRECTION ( 'NONE',  ( 1.000000000000000000, 0.000000000000000000, 0.000000000000000000 ) ) ;
#81509 = CARTESIAN_POINT ( 'NONE',  ( 114.6374585114582771, -29.49847210400304576, 234.4327681330539690 ) ) ;
#81510 = VERTEX_POINT ( 'NONE', #24730 ) ;
#81511 = CARTESIAN_POINT ( 'NONE',  ( 117.1924066864372520, -41.16168844948898453, 208.4861014663869696 ) ) ;
#81512 = DIRECTION ( 'NONE',  ( 0.000000000000000000, 0.000000000000000000, 1.000000000000000000 ) ) ;
#81513 = CARTESIAN_POINT ( 'NONE',  ( 99.08956014417853453, -42.79550325639331732, 22.84392096656654658 ) ) ;
#81514 = DIRECTION ( 'NONE',  ( 4.299999999999999979E-14, -1.000000000000000000, 4.400000000000000367E-29 ) ) ;
#81516 = DIRECTION ( 'NONE',  ( -0.7071067811567173234, 0.7071067812163779331, 0.000000000000000000 ) ) ;
#81515 = CARTESIAN_POINT ( 'NONE',  ( 99.29589592323129921, -33.18472740410275179, 277.6356252759111953 ) ) ;
#81517 = CARTESIAN_POINT ( 'NONE',  ( 97.81399931465544739, -40.51646775427786196, 252.6355816051047896 ) ) ;
#81519 = EDGE_CURVE ( 'NONE', #48806, #51052, #31982, .T. ) ;
#81518 = CARTESIAN_POINT ( 'NONE',  ( 0.000000000000000000, 92.07499999999998863, 0.000000000000000000 ) ) ;
#81520 = FACE_OUTER_BOUND ( 'NONE', #83923, .T. ) ;
#81521 = DIRECTION ( 'NONE',  ( -3.406823656978775284E-15, 0.000000000000000000, -1.000000000000000000 ) ) ;
#81522 = CARTESIAN_POINT ( 'NONE',  ( 62.03715912545754207, -47.82818131006020934, 129.9678068554150911 ) ) ;
#81523 = CYLINDRICAL_SURFACE ( 'NONE', #8601, 2.517500000000005844 ) ;
#81525 = EDGE_CURVE ( 'NONE', #86596, #5327, #19102, .T. ) ;
#81524 = VECTOR ( 'NONE', #23140, 1000.000000000000000 ) ;
#81527 = ORIENTED_EDGE ( 'NONE', *, *, #38935, .T. ) ;
#81526 = CARTESIAN_POINT ( 'NONE',  ( -2.883928177975681351, 94.92528396209723951, -118.5216277020858797 ) ) ;
#81528 = PLANE ( 'NONE',  #23448 ) ;
#81529 = CARTESIAN_POINT ( 'NONE',  ( 96.16820482414080118, -32.01123326506838396, 211.0013395616249738 ) ) ;
#81530 = CARTESIAN_POINT ( 'NONE',  ( 102.5581934769535906, -27.32956362888499768, 91.43276813305395478 ) ) ;
#81531 = CARTESIAN_POINT ( 'NONE',  ( 115.6911734784272170, -30.73338764459478867, 275.3099109901965562 ) ) ;
#81532 = CARTESIAN_POINT ( 'NONE',  ( 97.81168895331838087, -40.51742574516882200, 287.6356252759109680 ) ) ;
#81533 = CARTESIAN_POINT ( 'NONE',  ( 48.16670390244654953, -26.71338133339281029, 117.4678068554150485 ) ) ;
#81535 = DIRECTION ( 'NONE',  ( 1.000000000000000000, 1.000000000000000078E-15, 0.000000000000000000 ) ) ;
#81534 = FACE_OUTER_BOUND ( 'NONE', #85271, .T. ) ;
#81536 = FACE_OUTER_BOUND ( 'NONE', #89904, .T. ) ;
#81537 = CIRCLE ( 'NONE', #49584, 2.116999999999980009 ) ;
#81538 = CARTESIAN_POINT ( 'NONE',  ( 133.1188885517742619, -21.31186128672819535, 1.764000668899316837 ) ) ;
#81539 = AXIS2_PLACEMENT_3D ( 'NONE', #37215, #66236, #2704 ) ;
#81540 = ORIENTED_EDGE ( 'NONE', *, *, #45663, .T. ) ;
#81541 = VERTEX_POINT ( 'NONE', #37473 ) ;
#81542 = AXIS2_PLACEMENT_3D ( 'NONE', #81286, #26293, #75795 ) ;
#81543 = CARTESIAN_POINT ( 'NONE',  ( 113.1668408875787435, -30.74627054922163438, 148.8667055423629790 ) ) ;
#81545 = ORIENTED_EDGE ( 'NONE', *, *, #61807, .T. ) ;
#81544 = DIRECTION ( 'NONE',  ( 0.9347835805883506488, 0.000000000000000000, 0.3552177606235679130 ) ) ;
#81546 = DIRECTION ( 'NONE',  ( -1.000000000000000000, 1.011922027653136551E-15, 0.000000000000000000 ) ) ;
#81547 = CARTESIAN_POINT ( 'NONE',  ( 111.7842945758856246, -25.88553347519915349, 130.7499109901969518 ) ) ;
#81548 = DIRECTION ( 'NONE',  ( 0.000000000000000000, 0.000000000000000000, -1.000000000000000000 ) ) ;
#81549 = VECTOR ( 'NONE', #12350, 1000.000000000000000 ) ;
#81550 = CARTESIAN_POINT ( 'NONE',  ( 74.38348329127296665, -1.929447159941392931, 352.4506252759079530 ) ) ;
#81551 = DIRECTION ( 'NONE',  ( 1.000000000000000000, 0.000000000000000000, 0.000000000000000000 ) ) ;
#81552 = CIRCLE ( 'NONE', #65573, 2.999999999999919176 ) ;
#81553 = CARTESIAN_POINT ( 'NONE',  ( 162.8913605087219878, -31.76306994223740432, -5.074374724088000832 ) ) ;
#81554 = EDGE_CURVE ( 'NONE', #87657, #84035, #45154, .T. ) ;
#81555 = CARTESIAN_POINT ( 'NONE',  ( 96.75683229781650141, -37.84742820979680289, 81.40038718067398804 ) ) ;
#81556 = ORIENTED_EDGE ( 'NONE', *, *, #1949, .F. ) ;
#81557 = ORIENTED_EDGE ( 'NONE', *, *, #63878, .F. ) ;
#81558 = VERTEX_POINT ( 'NONE', #44265 ) ;
#81559 = DIRECTION ( 'NONE',  ( 0.000000000000000000, 1.000000000000000000, 0.000000000000000000 ) ) ;
#81560 =( BOUNDED_CURVE ( )  B_SPLINE_CURVE ( 3, ( #71359, #79062, #43167, #44508 ),
 .UNSPECIFIED., .F., .T. ) 
 B_SPLINE_CURVE_WITH_KNOTS ( ( 4, 4 ),
 ( 1.570796326805116383, 3.141592653598081153 ),
 .UNSPECIFIED. ) 
 CURVE ( )  GEOMETRIC_REPRESENTATION_ITEM ( )  RATIONAL_B_SPLINE_CURVE ( ( 1.000000000000000000, 0.8047378541248202399, 0.8047378541248202399, 1.000000000000000000 ) ) 
 REPRESENTATION_ITEM ( '' )  );
#81562 = DIRECTION ( 'NONE',  ( 0.000000000000000000, 0.000000000000000000, 1.000000000000000000 ) ) ;
#81561 = CARTESIAN_POINT ( 'NONE',  ( 113.1634500054121872, -44.41975088505036240, 164.1099109901959707 ) ) ;
#81563 = CARTESIAN_POINT ( 'NONE',  ( 0.000000000000000000, 93.07500000000001705, 88.90000000000000568 ) ) ;
#81564 = DIRECTION ( 'NONE',  ( 3.100000000000000258E-29, -3.100000000000000044E-14, -1.000000000000000000 ) ) ;
#81565 = CARTESIAN_POINT ( 'NONE',  ( 107.0664832912739968, -36.72944715994100306, 287.6356252759109680 ) ) ;
#81566 = CARTESIAN_POINT ( 'NONE',  ( 89.55756476669434107, 92.11680164986010766, 77.68727430815062007 ) ) ;
#81567 = CARTESIAN_POINT ( 'NONE',  ( 67.06770054697865646, -67.87853365652237869, 245.5343369445640462 ) ) ;
#81568 = CARTESIAN_POINT ( 'NONE',  ( 107.6020193903983824, -26.30459096080988246, 95.03562527591097364 ) ) ;
#81569 = ORIENTED_EDGE ( 'NONE', *, *, #34202, .F. ) ;
#81570 = ORIENTED_EDGE ( 'NONE', *, *, #31708, .T. ) ;
#81571 = EDGE_CURVE ( 'NONE', #3896, #25804, #65964, .T. ) ;
#81572 = PLANE ( 'NONE',  #2428 ) ;
#81573 = FACE_OUTER_BOUND ( 'NONE', #10184, .T. ) ;
#81574 = CONICAL_SURFACE ( 'NONE', #59740, 1.258750000000002922, 1.029744258676650093 ) ;
#81575 = DIRECTION ( 'NONE',  ( 0.000000000000000000, 0.8660254037844390407, -0.4999999999999995004 ) ) ;
#81576 = CARTESIAN_POINT ( 'NONE',  ( 112.6937225954192172, -42.64246220573352275, 155.9995189410199714 ) ) ;
#81577 = AXIS2_PLACEMENT_3D ( 'NONE', #67027, #18425, #51597 ) ;
#81578 = ADVANCED_FACE ( 'NONE', ( #73317 ), #66958, .T. ) ;
#81579 = DIRECTION ( 'NONE',  ( 0.000000000000000000, 1.000000000000000000, 0.000000000000000000 ) ) ;
#81580 = VERTEX_POINT ( 'NONE', #38797 ) ;
#81581 = ORIENTED_EDGE ( 'NONE', *, *, #30094, .F. ) ;
#81582 = LINE ( 'NONE', #56407, #17749 ) ;
#81583 = CARTESIAN_POINT ( 'NONE',  ( 135.3687878533466176, -21.15209318184243514, 1.893168666208430162 ) ) ;
#81584 = VERTEX_POINT ( 'NONE', #23853 ) ;
#81585 = ORIENTED_EDGE ( 'NONE', *, *, #37643, .T. ) ;
#81586 = CARTESIAN_POINT ( 'NONE',  ( 77.72936414032787411, -20.17925173418399964, 7.255518600576354338 ) ) ;
#81587 = AXIS2_PLACEMENT_3D ( 'NONE', #14417, #7598, #41639 ) ;
#81588 = CARTESIAN_POINT ( 'NONE',  ( 97.77711562652216060, -35.32084007268648662, 217.6263452106589682 ) ) ;
#81589 = CARTESIAN_POINT ( 'NONE',  ( 219.9639999999999986, 40.03750000000000142, -58.73749999999999716 ) ) ;
#81590 = DIRECTION ( 'NONE',  ( -0.7071067811864980568, -0.7071067811865969777, 0.000000000000000000 ) ) ;
#81591 = CARTESIAN_POINT ( 'NONE',  ( -110.3182612653083794, 61.98564117580777122, 69.81941546282760669 ) ) ;
#81592 = ORIENTED_EDGE ( 'NONE', *, *, #69895, .T. ) ;
#81593 = ORIENTED_EDGE ( 'NONE', *, *, #71148, .F. ) ;
#81594 = CIRCLE ( 'NONE', #29325, 3.968749999999992895 ) ;
#81595 = LINE ( 'NONE', #72195, #88482 ) ;
#81596 = ORIENTED_EDGE ( 'NONE', *, *, #77993, .T. ) ;
#81597 = ORIENTED_EDGE ( 'NONE', *, *, #59651, .T. ) ;
#81598 = EDGE_CURVE ( 'NONE', #62770, #69306, #65175, .T. ) ;
#81599 = ADVANCED_FACE ( 'NONE', ( #79273 ), #74668, .T. ) ;
#81600 = VECTOR ( 'NONE', #20720, 1000.000000000000000 ) ;
#81601 = CARTESIAN_POINT ( 'NONE',  ( 112.9694095044039841, -31.09161174735247002, 232.2509475124489597 ) ) ;
#81602 = CARTESIAN_POINT ( 'NONE',  ( 109.6894323871380976, -47.49121184687970754, 87.75467289495897205 ) ) ;
#81603 = EDGE_CURVE ( 'NONE', #66915, #63598, #44180, .T. ) ;
#81604 = CARTESIAN_POINT ( 'NONE',  ( 112.7479404651554376, -27.97242311821432992, 69.61848241876793963 ) ) ;
#81605 = CARTESIAN_POINT ( 'NONE',  ( 99.23474689667037296, -34.85485995268171422, 249.5838068554169809 ) ) ;
#81606 = CARTESIAN_POINT ( 'NONE',  ( 131.5867845949885009, -17.53883969337127979, 7.103318745424658687 ) ) ;
#81607 = CARTESIAN_POINT ( 'NONE',  ( 126.8164832912740110, -46.72944715994101017, 14.67562527591099020 ) ) ;
#81608 = CARTESIAN_POINT ( 'NONE',  ( 117.4137378716304738, -35.45790868367866722, 189.9241967044829664 ) ) ;
#81609 = CARTESIAN_POINT ( 'NONE',  ( 105.7140747251564079, -46.69282035222812510, 277.4689685590014960 ) ) ;
#81610 = ORIENTED_EDGE ( 'NONE', *, *, #66454, .F. ) ;
#81611 = LINE ( 'NONE', #59776, #43820 ) ;
#81612 = ORIENTED_EDGE ( 'NONE', *, *, #14885, .T. ) ;
#81613 = EDGE_CURVE ( 'NONE', #66251, #2544, #16650, .T. ) ;
#81614 = EDGE_LOOP ( 'NONE', ( #27381, #5477, #22161, #65571 ) ) ;
#81615 = CARTESIAN_POINT ( 'NONE',  ( 71.24189083761808661, -0.9290567490904538817, 542.9756252759101471 ) ) ;
#81616 = ORIENTED_EDGE ( 'NONE', *, *, #68486, .T. ) ;
#81617 = CARTESIAN_POINT ( 'NONE',  ( 97.78478039248422249, -40.45110315034128234, 137.6299286654718230 ) ) ;
#81618 = CARTESIAN_POINT ( 'NONE',  ( -446.0240000000000009, 53.97500000000000142, 50.79999999999999716 ) ) ;
#81619 = CARTESIAN_POINT ( 'NONE',  ( 117.1066318038510303, -39.53701698219273908, 98.60991099019594230 ) ) ;
#81620 = CARTESIAN_POINT ( 'NONE',  ( -4.504857172154159706, 70.67494150456570878, 130.4783009322840996 ) ) ;
#81621 = FACE_OUTER_BOUND ( 'NONE', #55616, .T. ) ;
#81622 = DIRECTION ( 'NONE',  ( -1.000000000000000078E-15, 0.000000000000000000, 1.000000000000000000 ) ) ;
#81625 = CARTESIAN_POINT ( 'NONE',  ( 113.0874441278155160, -45.97130050132138024, 219.0480062282919960 ) ) ;
#81624 = CARTESIAN_POINT ( 'NONE',  ( 107.0664832912739968, -36.72944715994100306, 287.6356252759109680 ) ) ;
#81623 = CARTESIAN_POINT ( 'NONE',  ( 117.0608945233090878, -38.08045312323447007, 144.7189586090517253 ) ) ;
#81626 = LINE ( 'NONE', #33446, #75695 ) ;
#81628 = EDGE_CURVE ( 'NONE', #29668, #11890, #40591, .T. ) ;
#81627 = CARTESIAN_POINT ( 'NONE',  ( -44.45000000000000284, 50.79999999999999716, 206.3750000000000000 ) ) ;
#81629 = ORIENTED_EDGE ( 'NONE', *, *, #25990, .T. ) ;
#81630 = CARTESIAN_POINT ( 'NONE',  ( 131.0667039024480118, -61.87844715994100397, 210.8338068554149913 ) ) ;
#81631 = AXIS2_PLACEMENT_3D ( 'NONE', #78968, #58927, #3538 ) ;
#81632 = DIRECTION ( 'NONE',  ( -0.9659258262890686453, 0.000000000000000000, 0.2588190451025194072 ) ) ;
#81633 = CARTESIAN_POINT ( 'NONE',  ( 97.53214211805510558, -39.74989731879190202, 136.5709469236470284 ) ) ;
#81634 = CARTESIAN_POINT ( 'NONE',  ( 20.03715912545741418, -46.82818131006202123, 117.4678068554150485 ) ) ;
#81636 = ORIENTED_EDGE ( 'NONE', *, *, #80577, .T. ) ;
#81635 = CARTESIAN_POINT ( 'NONE',  ( 112.4344423749254531, -46.44530527459760805, 252.9661014663871015 ) ) ;
#81637 = DIRECTION ( 'NONE',  ( -1.000000000000000078E-15, 1.000000000000000083E-30, 1.000000000000000000 ) ) ;
#81638 = CARTESIAN_POINT ( 'NONE',  ( 111.0462345608747796, -47.04136251952688497, 13.85753003781498016 ) ) ;
#81639 = CARTESIAN_POINT ( 'NONE',  ( 114.5587124134895731, -28.54364023664675187, 150.4746728949579619 ) ) ;
#81640 = CARTESIAN_POINT ( 'NONE',  ( 183.5150000000000148, 52.73749999999999716, -62.78087104677060637 ) ) ;
#81642 = DIRECTION ( 'NONE',  ( 0.7071067811865475727, -0.7071067811865475727, 0.000000000000000000 ) ) ;
#81641 = CARTESIAN_POINT ( 'NONE',  ( 151.5667039024486087, -48.82844715993590512, 129.9678068554149775 ) ) ;
#81643 = CARTESIAN_POINT ( 'NONE',  ( 188.5667039024481255, -42.82844715993431350, 257.2178068554150059 ) ) ;
#81644 = DIRECTION ( 'NONE',  ( -1.000000000000000000, 0.000000000000000000, 0.000000000000000000 ) ) ;
#81645 = ORIENTED_EDGE ( 'NONE', *, *, #54163, .T. ) ;
#81646 = AXIS2_PLACEMENT_3D ( 'NONE', #39993, #61327, #67251 ) ;
#81647 = ORIENTED_EDGE ( 'NONE', *, *, #33623, .T. ) ;
#81648 = ORIENTED_EDGE ( 'NONE', *, *, #30413, .T. ) ;
#81649 = EDGE_LOOP ( 'NONE', ( #81569, #69382, #10884, #29099 ) ) ;
#81650 = LINE ( 'NONE', #6227, #8842 ) ;
#81651 = CARTESIAN_POINT ( 'NONE',  ( 96.68076663292312389, -33.01451620012166899, 22.06514908543494258 ) ) ;
#81652 = CARTESIAN_POINT ( 'NONE',  ( 121.3140869715381456, -113.5527167097541508, -11.78219314458173272 ) ) ;
#81653 = CARTESIAN_POINT ( 'NONE',  ( 145.4069151017104105, -139.2712999699453462, 246.0952024083894401 ) ) ;
#81655 = FACE_OUTER_BOUND ( 'NONE', #4965, .T. ) ;
#81654 = PLANE ( 'NONE',  #70005 ) ;
#81656 = EDGE_CURVE ( 'NONE', #53327, #34574, #52897, .T. ) ;
#81657 = CARTESIAN_POINT ( 'NONE',  ( 103.8089036935402021, -45.87596577953674881, 251.7267055423626516 ) ) ;
#81658 = ORIENTED_EDGE ( 'NONE', *, *, #23094, .F. ) ;
#81659 = ORIENTED_EDGE ( 'NONE', *, *, #24366, .T. ) ;
#81660 = EDGE_LOOP ( 'NONE', ( #21309, #63028, #73454, #19970 ) ) ;
#81661 = CARTESIAN_POINT ( 'NONE',  ( 0.000000000000000000, 65.60000000000000853, 0.000000000000000000 ) ) ;
#81662 = LINE ( 'NONE', #89363, #10066 ) ;
#81663 = ADVANCED_FACE ( 'NONE', ( #47837 ), #5641, .T. ) ;
#81664 = CARTESIAN_POINT ( 'NONE',  ( 123.6837132603319702, -55.86395651782485317, 229.5838068554170093 ) ) ;
#81665 = LINE ( 'NONE', #46653, #89649 ) ;
#81666 = CARTESIAN_POINT ( 'NONE',  ( 98.36824592180721538, -38.57411413555575308, 27.92444044875497156 ) ) ;
#81667 = CIRCLE ( 'NONE', #29393, 5.599999999999994316 ) ;
#81668 = CARTESIAN_POINT ( 'NONE',  ( 118.3048154812336179, 92.64969027323469675, 7.744053933099116271 ) ) ;
#81669 = DIRECTION ( 'NONE',  ( 0.000000000000000000, 0.000000000000000000, -1.000000000000000000 ) ) ;
#81670 = CARTESIAN_POINT ( 'NONE',  ( 111.2075918398242038, -27.22220237496667394, 284.7375300378162706 ) ) ;
#81671 = DIRECTION ( 'NONE',  ( 0.000000000000000000, 0.000000000000000000, 1.000000000000000000 ) ) ;
#81672 = ORIENTED_EDGE ( 'NONE', *, *, #46236, .T. ) ;
#81673 = CARTESIAN_POINT ( 'NONE',  ( 164.7830935719630361, -29.99615139349950965, -5.074374724088000832 ) ) ;
#81674 = LINE ( 'NONE', #82577, #32144 ) ;
#81675 = CARTESIAN_POINT ( 'NONE',  ( 115.0531750927473951, -38.41541278395968817, 61.47951894101993986 ) ) ;
#81676 = ADVANCED_FACE ( 'NONE', ( #67854 ), #69201, .F. ) ;
#81677 = CARTESIAN_POINT ( 'NONE',  ( 136.2652213604061160, -17.07517613921647026, 7.387586420629034478 ) ) ;
#81678 = DIRECTION ( 'NONE',  ( 0.9217329428042198014, 0.3878251953515564066, -1.214306433183767175E-14 ) ) ;
#81679 = CARTESIAN_POINT ( 'NONE',  ( 116.3212776292296127, -32.94146857471318413, 287.6356252759109680 ) ) ;
#81680 = ORIENTED_EDGE ( 'NONE', *, *, #53750, .T. ) ;
#81681 = CARTESIAN_POINT ( 'NONE',  ( 83.06670390244796920, -61.87844715994100397, 210.8338068554149913 ) ) ;
#81682 = CARTESIAN_POINT ( 'NONE',  ( 107.0667039024470313, -104.2784471599409528, 24.21780685541800082 ) ) ;
#81683 = AXIS2_PLACEMENT_3D ( 'NONE', #36630, #29811, #50683 ) ;
#81684 = ORIENTED_EDGE ( 'NONE', *, *, #70350, .F. ) ;
#81685 = CARTESIAN_POINT ( 'NONE',  ( 107.9456392385311005, -25.71100025151098478, 115.0251490854349612 ) ) ;
#81686 = ORIENTED_EDGE ( 'NONE', *, *, #31763, .T. ) ;
#81687 = CARTESIAN_POINT ( 'NONE',  ( 107.2022627278996652, -27.67438038655213006, 79.49908649474396327 ) ) ;
#81688 = ORIENTED_CLOSED_SHELL ( 'NONE', *, #89461, .F. );
#81689 = DIRECTION ( 'NONE',  ( -4.237773401492740281E-14, 1.000000000000000000, 0.000000000000000000 ) ) ;
#81690 = CARTESIAN_POINT ( 'NONE',  ( 107.5226574059108202, -27.84946772507149504, 91.46729759161098627 ) ) ;
#81691 = CARTESIAN_POINT ( 'NONE',  ( 144.0667039024470455, -124.7784471599409102, 222.2178068554179902 ) ) ;
#81692 = CARTESIAN_POINT ( 'NONE',  ( 107.0664832912739399, -36.72944715994095333, 302.6356252759109680 ) ) ;
#81693 = CARTESIAN_POINT ( 'NONE',  ( 115.2842354651272814, -44.15600456922878436, 79.25372051400697160 ) ) ;
#81694 = CARTESIAN_POINT ( 'NONE',  ( 102.0673354423506396, -27.97033358461368735, 181.4902337030571289 ) ) ;
#81695 = AXIS2_PLACEMENT_3D ( 'NONE', #54228, #75158, #66544 ) ;
#81696 = CARTESIAN_POINT ( 'NONE',  ( -41.60202597009397607, 65.59999999999998010, 47.15338361873602935 ) ) ;
#81697 = ORIENTED_EDGE ( 'NONE', *, *, #66795, .T. ) ;
#81698 = DIRECTION ( 'NONE',  ( 0.000000000000000000, -1.000000000000000000, 0.000000000000000000 ) ) ;
#81699 = VERTEX_POINT ( 'NONE', #20608 ) ;
#81700 = ORIENTED_EDGE ( 'NONE', *, *, #86908, .F. ) ;
#81701 = ADVANCED_FACE ( 'NONE', ( #33333 ), #12005, .F. ) ;
#81702 = FACE_OUTER_BOUND ( 'NONE', #63547, .T. ) ;
#81703 = ORIENTED_EDGE ( 'NONE', *, *, #22866, .F. ) ;
#81704 = CARTESIAN_POINT ( 'NONE',  ( 109.8085987287837497, -27.34093086507531112, 259.8499109901970314 ) ) ;
#81705 = CARTESIAN_POINT ( 'NONE',  ( 109.2058805625337925, -26.50397703278076733, 135.9127681330539872 ) ) ;
#81706 = CARTESIAN_POINT ( 'NONE',  ( 168.0371591254543091, -48.62818131005519717, 313.9678068554149490 ) ) ;
#81707 = CARTESIAN_POINT ( 'NONE',  ( 97.06107109563198776, -37.99641195030216068, 142.4272919415186323 ) ) ;
#81708 = EDGE_CURVE ( 'NONE', #82549, #20374, #48274, .T. ) ;
#81709 = CARTESIAN_POINT ( 'NONE',  ( 98.09687384527185827, -31.41638835794072193, 81.90133956162493689 ) ) ;
#81710 = DIRECTION ( 'NONE',  ( -0.7071067812162686872, -0.7071067811568263473, -7.071067812162680651E-16 ) ) ;
#81711 = ORIENTED_EDGE ( 'NONE', *, *, #56134, .F. ) ;
#81712 = DIRECTION ( 'NONE',  ( -1.000000000000000078E-15, 1.000000000000000083E-30, 1.000000000000000000 ) ) ;
#81713 = EDGE_CURVE ( 'NONE', #61107, #20086, #70339, .T. ) ;
#81714 = CARTESIAN_POINT ( 'NONE',  ( 101.9937552062217776, -45.44615440094798942, 158.1562831739205990 ) ) ;
#81715 = EDGE_LOOP ( 'NONE', ( #69038, #43229 ) ) ;
#81716 = CIRCLE ( 'NONE', #19325, 1.000000000000000888 ) ;
#81717 = CARTESIAN_POINT ( 'NONE',  ( 162.5667039024478981, -32.29483332968042220, 117.4678068554150485 ) ) ;
#81718 = CARTESIAN_POINT ( 'NONE',  ( 0.000000000000000000, 95.25000000000000000, 0.000000000000000000 ) ) ;
#81719 = CARTESIAN_POINT ( 'NONE',  ( 115.8883252675857847, -30.10835006627621269, 264.3508633711492735 ) ) ;
#81720 = CARTESIAN_POINT ( 'NONE',  ( 168.3664380525675881, -48.62818131005417399, 180.4678068554150059 ) ) ;
#81721 = AXIS2_PLACEMENT_3D ( 'NONE', #41450, #69181, #26499 ) ;
#81722 = DIRECTION ( 'NONE',  ( 9.073094938289460781E-13, 1.000000000000000000, 0.000000000000000000 ) ) ;
#81723 = FACE_OUTER_BOUND ( 'NONE', #6236, .T. ) ;
#81724 = CARTESIAN_POINT ( 'NONE',  ( 116.1088647163993386, -36.23144265813309772, 273.3048007804578674 ) ) ;
#81726 = CARTESIAN_POINT ( 'NONE',  ( 98.22092589535434115, -43.31882777834836418, 107.8480062282919647 ) ) ;
#81725 = LINE ( 'NONE', #53965, #21685 ) ;
#81727 = DIRECTION ( 'NONE',  ( 0.000000000000000000, 0.000000000000000000, 1.000000000000000000 ) ) ;
#81728 = CARTESIAN_POINT ( 'NONE',  ( 108.6554276816787734, -25.75039326353942926, 149.9737205140059473 ) ) ;
#81729 = VERTEX_POINT ( 'NONE', #12445 ) ;
#81731 = ADVANCED_FACE ( 'NONE', ( #34218 ), #40133, .T. ) ;
#81730 = DIRECTION ( 'NONE',  ( -1.000000000000000000, -4.510281037539694659E-14, 0.000000000000000000 ) ) ;
#81732 = ORIENTED_EDGE ( 'NONE', *, *, #53865, .T. ) ;
#81733 = DIRECTION ( 'NONE',  ( -1.000000000000000000, -1.206764157201257538E-15, 0.000000000000000000 ) ) ;
#81734 = PLANE ( 'NONE',  #26153 ) ;
#81735 = ADVANCED_FACE ( 'NONE', ( #68306 ), #81062, .T. ) ;
#81736 = CARTESIAN_POINT ( 'NONE',  ( 51.06648329127400388, 0.2215528400590083269, 336.6506252759110112 ) ) ;
#81737 = EDGE_LOOP ( 'NONE', ( #47637, #73514, #88911, #67852 ) ) ;
#81738 = CARTESIAN_POINT ( 'NONE',  ( 141.0235900724605358, -46.62589376934771224, 14.92562527591103105 ) ) ;
#81740 = EDGE_LOOP ( 'NONE', ( #85792, #10889, #69294, #9025 ) ) ;
#81739 = CARTESIAN_POINT ( 'NONE',  ( 103.1581569894456294, -27.01699888143334860, 130.3813395616259925 ) ) ;
#81742 = CARTESIAN_POINT ( 'NONE',  ( 173.9900000000000091, 5.112500000000000711, -7.937500000000000000 ) ) ;
#81741 = UNCERTAINTY_MEASURE_WITH_UNIT (LENGTH_MEASURE( 1.000000000000000082E-05 ), #80927, 'distance_accuracy_value', 'NONE');
#81743 = CARTESIAN_POINT ( 'NONE',  ( -129.9388103550934090, 83.38002811471484677, -12.67976361810899988 ) ) ;
#81744 = FACE_OUTER_BOUND ( 'NONE', #84504, .T. ) ;
#81745 = DIRECTION ( 'NONE',  ( -1.000000000000000078E-15, 1.000000000000000000, 0.000000000000000000 ) ) ;
#81746 = ORIENTED_EDGE ( 'NONE', *, *, #63750, .F. ) ;
#81747 = SHAPE_DEFINITION_REPRESENTATION ( #48474, #42769 ) ;
#81748 = AXIS2_PLACEMENT_3D ( 'NONE', #37731, #16835, #65426 ) ;
#81749 = PLANE ( 'NONE',  #33956 ) ;
#81750 = ORIENTED_EDGE ( 'NONE', *, *, #69003, .F. ) ;
#81751 = ORIENTED_EDGE ( 'NONE', *, *, #38105, .T. ) ;
#81752 = CYLINDRICAL_SURFACE ( 'NONE', #61202, 0.2500000000000002220 ) ;
#81753 = FACE_BOUND ( 'NONE', #4126, .T. ) ;
#81754 = CARTESIAN_POINT ( 'NONE',  ( 100.8874677930869552, -44.70022130517887149, 157.0522919335028007 ) ) ;
#81755 = DIRECTION ( 'NONE',  ( 0.5000000000000012212, -0.8660254037844379305, 2.684678751731759347E-14 ) ) ;
#81757 = CARTESIAN_POINT ( 'NONE',  ( -7.760001168987765929, 72.46196594926868784, -118.3038028359265894 ) ) ;
#81756 = LINE ( 'NONE', #19507, #47957 ) ;
#81758 = CARTESIAN_POINT ( 'NONE',  ( 181.9694315774057713, -34.03355364505798519, 313.9678068554149490 ) ) ;
#81759 = CIRCLE ( 'NONE', #25195, 88.90000000000000568 ) ;
#81760 = EDGE_LOOP ( 'NONE', ( #39166, #30455, #87737, #73999 ) ) ;
#81761 = CARTESIAN_POINT ( 'NONE',  ( 177.0664832912740110, 12.92155284005802685, 334.6228282640715292 ) ) ;
#81762 = EDGE_CURVE ( 'NONE', #9949, #58653, #73311, .T. ) ;
#81763 = CARTESIAN_POINT ( 'NONE',  ( 101.7545977962314652, -44.98157700518526525, 218.1213395616249784 ) ) ;
#81765 = EDGE_LOOP ( 'NONE', ( #47901, #23549, #77669, #68490 ) ) ;
#81764 = CARTESIAN_POINT ( 'NONE',  ( 162.7131505118679797, -31.94127993907790852, -5.074374724088000832 ) ) ;
#81766 = CARTESIAN_POINT ( 'NONE',  ( 116.4719273984280790, -32.36179259691363796, 55.16038718067301261 ) ) ;
#81767 = CARTESIAN_POINT ( 'NONE',  ( 116.5686728426965857, -33.54608030872165614, 54.08363974141789754 ) ) ;
#81768 = CARTESIAN_POINT ( 'NONE',  ( 88.24325903289653183, -55.55267141831875222, -5.074374724089048883 ) ) ;
#81769 = CARTESIAN_POINT ( 'NONE',  ( 97.80396990294123327, -40.49851493234764632, 22.63399986120327867 ) ) ;
#81770 = ORIENTED_EDGE ( 'NONE', *, *, #30409, .F. ) ;
#81771 = CARTESIAN_POINT ( 'NONE',  ( 41.56648329127499153, -32.07844715994070839, 138.9256252759119832 ) ) ;
#81772 = ORIENTED_EDGE ( 'NONE', *, *, #65783, .T. ) ;
#81773 = ORIENTED_EDGE ( 'NONE', *, *, #5088, .F. ) ;
#81774 = CARTESIAN_POINT ( 'NONE',  ( 104.6178464025351218, -28.18156397322882967, 221.7301547344689823 ) ) ;
#81775 = VECTOR ( 'NONE', #27972, 1000.000000000000000 ) ;
#81776 = LINE ( 'NONE', #39968, #9565 ) ;
#81777 = ADVANCED_FACE ( 'NONE', ( #69650, #27855 ), #83733, .T. ) ;
#81778 = LINE ( 'NONE', #11380, #62429 ) ;
#81779 = AXIS2_PLACEMENT_3D ( 'NONE', #30430, #10864, #24945 ) ;
#81780 = CARTESIAN_POINT ( 'NONE',  ( 107.0664832912739399, -36.72944715994095333, 311.6356252759109680 ) ) ;
#81781 = CARTESIAN_POINT ( 'NONE',  ( 156.5667039024483529, -42.82844715993568485, 137.2178068554149775 ) ) ;
#81782 = ORIENTED_EDGE ( 'NONE', *, *, #71557, .T. ) ;
#81783 = DIRECTION ( 'NONE',  ( 0.000000000000000000, 0.000000000000000000, -1.000000000000000000 ) ) ;
#81784 = CARTESIAN_POINT ( 'NONE',  ( -148.0533267522759786, 20.32000000000000028, -160.2664750769289697 ) ) ;
#81785 = VERTEX_POINT ( 'NONE', #42364 ) ;
#81786 = CARTESIAN_POINT ( 'NONE',  ( 101.0991643652557173, -45.25116564454923207, 282.0899109901967563 ) ) ;
#81787 = EDGE_LOOP ( 'NONE', ( #5654, #13294, #34102 ) ) ;
#81788 = CARTESIAN_POINT ( 'NONE',  ( 111.3125147634731462, -44.27080922411229835, 255.8147570362582712 ) ) ;
#81789 = EDGE_CURVE ( 'NONE', #60401, #7119, #61629, .T. ) ;
#81790 = FACE_BOUND ( 'NONE', #45227, .T. ) ;
#81791 = CARTESIAN_POINT ( 'NONE',  ( 97.25364341294451265, -36.87759583893578252, 136.3384824187689333 ) ) ;
#81792 = CARTESIAN_POINT ( 'NONE',  ( 23.18076855059904418, 78.27346916906378738, 305.0143276166587043 ) ) ;
#81793 = DIRECTION ( 'NONE',  ( -3.100000000000000258E-29, 3.100000000000000044E-14, 1.000000000000000000 ) ) ;
#81794 = FACE_OUTER_BOUND ( 'NONE', #4853, .T. ) ;
#81795 = CARTESIAN_POINT ( 'NONE',  ( 7.584119442562257341, 72.36170844776167144, 130.3354891464173306 ) ) ;
#81796 = CARTESIAN_POINT ( 'NONE',  ( 117.3777842326014706, -34.92111847156615312, 239.9641967044819637 ) ) ;
#81797 = DIRECTION ( 'NONE',  ( 1.000000000000000000, 0.000000000000000000, -0.000000000000000000 ) ) ;
#81798 = ORIENTED_EDGE ( 'NONE', *, *, #31355, .F. ) ;
#81799 = AXIS2_PLACEMENT_3D ( 'NONE', #9060, #49914, #36759 ) ;
#81800 = CARTESIAN_POINT ( 'NONE',  ( 96.74875621672018156, -38.50074266403909462, 87.46133956162493917 ) ) ;
#81801 = CARTESIAN_POINT ( 'NONE',  ( 63.03715912545729338, -24.42818131006027826, 313.9678068554150059 ) ) ;
#81802 = VECTOR ( 'NONE', #62526, 1000.000000000000000 ) ;
#81803 = ADVANCED_FACE ( 'NONE', ( #83284 ), #1957, .F. ) ;
#81804 = ORIENTED_EDGE ( 'NONE', *, *, #63054, .T. ) ;
#81805 = ORIENTED_EDGE ( 'NONE', *, *, #21789, .F. ) ;
#81806 = ORIENTED_EDGE ( 'NONE', *, *, #48565, .F. ) ;
#81807 = AXIS2_PLACEMENT_3D ( 'NONE', #23468, #85256, #51137 ) ;
#81808 = CARTESIAN_POINT ( 'NONE',  ( 188.5667039024479834, -58.35344715994099829, 293.2178068554150627 ) ) ;
#81809 = CARTESIAN_POINT ( 'NONE',  ( -179.8898777604649979, 101.5999999999999943, 122.9960808104842016 ) ) ;
#81810 = CYLINDRICAL_SURFACE ( 'NONE', #21922, 9.999999999999998224 ) ;
#81811 = CARTESIAN_POINT ( 'NONE',  ( -103.1875000000000000, 127.0000000000000000, 7.937499999998919087 ) ) ;
#81812 = EDGE_CURVE ( 'NONE', #37208, #27150, #43266, .T. ) ;
#81813 = CARTESIAN_POINT ( 'NONE',  ( 111.0233670443594463, -45.12224181339347240, 135.7452332267339443 ) ) ;
#81814 = CARTESIAN_POINT ( 'NONE',  ( 97.20328444759655895, -40.27860260594448505, 262.6013395616254797 ) ) ;
#81815 = DIRECTION ( 'NONE',  ( 1.000000000000000000, 4.299999999999999979E-14, 1.000000000000000078E-15 ) ) ;
#81816 = ORIENTED_EDGE ( 'NONE', *, *, #26112, .T. ) ;
#81817 = DIRECTION ( 'NONE',  ( -0.000000000000000000, -0.000000000000000000, -1.000000000000000000 ) ) ;
#81818 = ORIENTED_EDGE ( 'NONE', *, *, #18381, .T. ) ;
#81819 = VERTEX_POINT ( 'NONE', #57346 ) ;
#81820 = CARTESIAN_POINT ( 'NONE',  ( 30.48091746481741637, -48.32844715994156815, 180.4678068554150911 ) ) ;
#81821 = ORIENTED_EDGE ( 'NONE', *, *, #74580, .F. ) ;
#81822 = EDGE_LOOP ( 'NONE', ( #74201, #46856 ) ) ;
#81823 = DIRECTION ( 'NONE',  ( -0.7071067812162665778, -0.7071067811568285677, -6.612322856132800227E-17 ) ) ;
#81824 = CARTESIAN_POINT ( 'NONE',  ( 210.5660000000000025, 52.73749999999999716, -44.45000000000000284 ) ) ;
#81825 = B_SPLINE_CURVE_WITH_KNOTS ( 'NONE', 3,
 ( #10318, #38023, #52066, #79826, #40243, #60232, #87964, #76448, #67961, #67064, #39787, #73878, #4844, #74334, #32526, #41908, #12105, #7410 ),
 .UNSPECIFIED., .F., .F.,
 ( 4, 2, 2, 2, 2, 2, 2, 2, 4 ),
 ( 0.4999740858641279484, 0.5624773251311119271, 0.6249805643980959058, 0.6874838036650799955, 0.7499870429320639742, 0.8124902821990479529, 0.8749935214660320426, 0.9374967607330160213, 1.000000000000000000 ),
 .UNSPECIFIED. ) ;
#81826 = PLANE ( 'NONE',  #42303 ) ;
#81827 = FACE_OUTER_BOUND ( 'NONE', #18235, .T. ) ;
#81828 = CARTESIAN_POINT ( 'NONE',  ( 111.5068547175069824, -28.09499701576110198, 169.1209912566479545 ) ) ;
#81829 = CARTESIAN_POINT ( 'NONE',  ( 98.68712911129445331, -43.00583860492766064, 66.83848241876793850 ) ) ;
#81830 = ORIENTED_EDGE ( 'NONE', *, *, #22016, .F. ) ;
#81832 = ADVANCED_FACE ( 'NONE', ( #28764 ), #85087, .F. ) ;
#81831 = CARTESIAN_POINT ( 'NONE',  ( 162.8913605087224710, -31.76306994223275382, 193.9678068554149775 ) ) ;
#81833 = ORIENTED_EDGE ( 'NONE', *, *, #79631, .F. ) ;
#81834 = EDGE_CURVE ( 'NONE', #29924, #21942, #81957, .T. ) ;
#81835 = CARTESIAN_POINT ( 'NONE',  ( 48.79742451361987321, -36.32844715994078655, 193.9678068554150911 ) ) ;
#81836 = ORIENTED_EDGE ( 'NONE', *, *, #65969, .F. ) ;
#81837 = EDGE_CURVE ( 'NONE', #50690, #62285, #50534, .T. ) ;
#81838 = LINE ( 'NONE', #61808, #38860 ) ;
#81839 = ORIENTED_EDGE ( 'NONE', *, *, #3231, .T. ) ;
#81840 = CARTESIAN_POINT ( 'NONE',  ( 107.0667039024470313, -104.2784471599413934, 2.217806855418003043 ) ) ;
#81841 = EDGE_CURVE ( 'NONE', #52939, #82504, #41327, .T. ) ;
#81842 = CARTESIAN_POINT ( 'NONE',  ( -11.30434772722943926, 76.96944167614310572, 118.0159957117157745 ) ) ;
#81843 = CARTESIAN_POINT ( 'NONE',  ( 101.9931123694998973, -45.44575822371417928, 132.1564871734879318 ) ) ;
#81844 = AXIS2_PLACEMENT_3D ( 'NONE', #66966, #59248, #31992 ) ;
#81845 = DIRECTION ( 'NONE',  ( -1.000000000000000000, 6.036837696399451257E-13, 0.000000000000000000 ) ) ;
#81846 = ORIENTED_EDGE ( 'NONE', *, *, #53322, .F. ) ;
#81847 = CARTESIAN_POINT ( 'NONE',  ( 114.1055592783800137, -46.29424852498188869, 33.08133956162495792 ) ) ;
#81848 = CARTESIAN_POINT ( 'NONE',  ( 117.9699911065184637, -41.49648292930365301, 54.49848241876792088 ) ) ;
#81849 = VECTOR ( 'NONE', #12331, 1000.000000000000000 ) ;
#81851 = CYLINDRICAL_SURFACE ( 'NONE', #70379, 4.000000000000002665 ) ;
#81850 = CARTESIAN_POINT ( 'NONE',  ( 182.2738106836200132, -23.19206098993950604, -5.074374724088000832 ) ) ;
#81852 = DIRECTION ( 'NONE',  ( 1.000000000000000000, 0.000000000000000000, 2.108231265501709878E-16 ) ) ;
#81853 = CARTESIAN_POINT ( 'NONE',  ( 71.24189083761808661, -0.9290567490904538817, 396.9756252759102040 ) ) ;
#81854 = DIRECTION ( 'NONE',  ( 0.000000000000000000, -1.000000000000000000, 0.000000000000000000 ) ) ;
#81855 = FACE_OUTER_BOUND ( 'NONE', #45658, .T. ) ;
#81856 = CYLINDRICAL_SURFACE ( 'NONE', #77520, 9.999999999999998224 ) ;
#81857 = ORIENTED_EDGE ( 'NONE', *, *, #49043, .T. ) ;
#81858 = CARTESIAN_POINT ( 'NONE',  ( 103.4619715496438630, -25.38765309446003116, 55.32133956162594046 ) ) ;
#81859 = CARTESIAN_POINT ( 'NONE',  ( 104.2081133107797228, -25.20330419090194951, 86.26991099019699050 ) ) ;
#81861 = LINE ( 'NONE', #19614, #25305 ) ;
#81860 = CARTESIAN_POINT ( 'NONE',  ( 97.83900064082345693, -40.58357432020694233, 171.6415561560118590 ) ) ;
#81862 = CARTESIAN_POINT ( 'NONE',  ( 145.4416927396864878, -139.3034583227001804, 245.6607614918409865 ) ) ;
#81863 = AXIS2_PLACEMENT_3D ( 'NONE', #32836, #60530, #68712 ) ;
#81864 = AXIS2_PLACEMENT_3D ( 'NONE', #52856, #80626, #37940 ) ;
#81865 = CIRCLE ( 'NONE', #68753, 11.57110091390449469 ) ;
#81866 = VECTOR ( 'NONE', #31198, 1000.000000000000000 ) ;
#81867 = B_SPLINE_CURVE_WITH_KNOTS ( 'NONE', 3,
 ( #12641, #25356, #19002, #38988, #32171, #53937, #46686, #74417, #40776, #19897, #73513, #53029, #45785, #19446, #80797, #74865, #26260, #87599 ),
 .UNSPECIFIED., .F., .F.,
 ( 4, 2, 2, 2, 2, 2, 2, 2, 4 ),
 ( 0.4999998914591470833, 0.5624999050267537326, 0.6249999185943603264, 0.6874999321619669201, 0.7499999457295736249, 0.8124999592971802187, 0.8749999728647868125, 0.9374999864323934062, 1.000000000000000000 ),
 .UNSPECIFIED. ) ;
#81868 = CARTESIAN_POINT ( 'NONE',  ( 179.8585841295805210, -30.08671355699668837, 313.9678068554149490 ) ) ;
#81869 = ORIENTED_EDGE ( 'NONE', *, *, #74185, .F. ) ;
#81870 = CARTESIAN_POINT ( 'NONE',  ( 98.87588542518402335, -42.07524381596787322, 97.78705384733893879 ) ) ;
#81872 = ORIENTED_EDGE ( 'NONE', *, *, #89490, .T. ) ;
#81871 = CARTESIAN_POINT ( 'NONE',  ( 10.48278874474372380, 89.71962060600694144, 130.1344814326622554 ) ) ;
#81873 = VECTOR ( 'NONE', #6637, 1000.000000000000114 ) ;
#81874 = CARTESIAN_POINT ( 'NONE',  ( 97.93839266929580845, -41.72010113774604889, 217.7241967044829494 ) ) ;
#81875 = CARTESIAN_POINT ( 'NONE',  ( 121.3042370176062548, -43.34581843340460239, 9.125625275910984158 ) ) ;
#81876 = LINE ( 'NONE', #19189, #27517 ) ;
#81877 = FACE_OUTER_BOUND ( 'NONE', #24764, .T. ) ;
#81878 = CARTESIAN_POINT ( 'NONE',  ( 98.34985892484459669, -31.65658478873675108, 81.90645860733756933 ) ) ;
#81879 = CARTESIAN_POINT ( 'NONE',  ( 167.7413838386817702, -48.33240602328261559, 249.9678068554149775 ) ) ;
#81880 = DIRECTION ( 'NONE',  ( 0.000000000000000000, 0.000000000000000000, -1.000000000000000000 ) ) ;
#81881 = CARTESIAN_POINT ( 'NONE',  ( 112.1511370651177231, -26.84216853020813076, 169.6984824187689469 ) ) ;
#81882 = VERTEX_POINT ( 'NONE', #70092 ) ;
#81883 = ORIENTED_EDGE ( 'NONE', *, *, #57843, .T. ) ;
#81884 = CARTESIAN_POINT ( 'NONE',  ( 111.0851542815211985, -27.49251106464650007, 131.1815833058969645 ) ) ;
#81885 = DIRECTION ( 'NONE',  ( -0.7071067811865253683, 0.7071067811865696662, -7.071067811865261355E-16 ) ) ;
#81886 = EDGE_CURVE ( 'NONE', #76826, #67926, #7864, .T. ) ;
#81888 = DIRECTION ( 'NONE',  ( 1.000000000000000000, 2.106816776397999944E-14, 9.351236661543306751E-17 ) ) ;
#81887 = CARTESIAN_POINT ( 'NONE',  ( 111.3277751695582651, -45.53312973143654574, 243.9356252759109509 ) ) ;
#81889 = CARTESIAN_POINT ( 'NONE',  ( 182.3467384525660862, -36.02818131005237490, 117.4678068554150627 ) ) ;
#81890 = ADVANCED_FACE ( 'NONE', ( #35562 ), #54407, .T. ) ;
#81891 = DIRECTION ( 'NONE',  ( 0.000000000000000000, 0.000000000000000000, 1.000000000000000000 ) ) ;
#81892 = ADVANCED_FACE ( 'NONE', ( #36917 ), #55903, .T. ) ;
#81893 = CARTESIAN_POINT ( 'NONE',  ( 46.03715912545342093, -48.62818131006090283, 193.9678068554150911 ) ) ;
#81894 = DIRECTION ( 'NONE',  ( -1.047445008332813989E-14, 0.000000000000000000, 1.000000000000000000 ) ) ;
#81895 = CARTESIAN_POINT ( 'NONE',  ( 125.5177273812784762, -131.0330679306342461, 222.2178068554179902 ) ) ;
#81896 = CARTESIAN_POINT ( 'NONE',  ( 107.6532706963292725, -47.74396045468181882, 197.6308633711489620 ) ) ;
#81897 = FACE_OUTER_BOUND ( 'NONE', #78872, .T. ) ;
#81898 = ORIENTED_EDGE ( 'NONE', *, *, #9128, .F. ) ;
#81899 = VERTEX_POINT ( 'NONE', #21965 ) ;
#81900 = ADVANCED_FACE ( 'NONE', ( #70551 ), #41390, .F. ) ;
#81901 = EDGE_CURVE ( 'NONE', #11953, #74795, #8780, .T. ) ;
#81902 = CARTESIAN_POINT ( 'NONE',  ( -98.82395782888141866, 74.16976894168007561, -85.31568053864921808 ) ) ;
#81903 = FACE_OUTER_BOUND ( 'NONE', #60660, .T. ) ;
#81904 = DIRECTION ( 'NONE',  ( 1.000000000000000000, 0.000000000000000000, 0.000000000000000000 ) ) ;
#81905 = LINE ( 'NONE', #38751, #51145 ) ;
#81906 = ADVANCED_FACE ( 'NONE', ( #63733 ), #15305, .F. ) ;
#81907 = AXIS2_PLACEMENT_3D ( 'NONE', #74018, #39497, #38597 ) ;
#81908 = LINE ( 'NONE', #19658, #77516 ) ;
#81909 = ORIENTED_EDGE ( 'NONE', *, *, #58705, .F. ) ;
#81910 = CARTESIAN_POINT ( 'NONE',  ( -5.572224674611368833, 93.85841628716941898, 118.2253171978965867 ) ) ;
#81911 = CIRCLE ( 'NONE', #39790, 12.59999999999999964 ) ;
#81912 = ADVANCED_FACE ( 'NONE', ( #84640 ), #82203, .F. ) ;
#81913 = CARTESIAN_POINT ( 'NONE',  ( 99.75298236265237506, -29.29979477046331127, 225.6956252759109702 ) ) ;
#81914 = ORIENTED_EDGE ( 'NONE', *, *, #28481, .T. ) ;
#81915 = CARTESIAN_POINT ( 'NONE',  ( -12.61957378781718297, 80.89607376620493540, 117.8825615626982994 ) ) ;
#81916 = EDGE_CURVE ( 'NONE', #62559, #82107, #6591, .T. ) ;
#81917 = DIRECTION ( 'NONE',  ( 0.000000000000000000, 0.000000000000000000, -1.000000000000000000 ) ) ;
#81918 = DIRECTION ( 'NONE',  ( 0.9130365726098601531, 0.000000000000000000, 0.4078776986755215384 ) ) ;
#81919 = EDGE_CURVE ( 'NONE', #26048, #11858, #57350, .T. ) ;
#81920 = CARTESIAN_POINT ( 'NONE',  ( 115.1453852183930593, -37.89609606526670404, 26.53094751244894312 ) ) ;
#81921 = CARTESIAN_POINT ( 'NONE',  ( 102.0714078572591319, -27.55412165564507632, 141.4727681330539895 ) ) ;
#81922 = CARTESIAN_POINT ( 'NONE',  ( 50.87649884952384127, -33.54226604284969682, 117.4678068554150485 ) ) ;
#81923 = VERTEX_POINT ( 'NONE', #21640 ) ;
#81924 = DIRECTION ( 'NONE',  ( -4.649954031768947235E-17, 0.8660254037844387076, -0.4999999999999998890 ) ) ;
#81925 = CARTESIAN_POINT ( 'NONE',  ( 99.02771868422573220, -42.71062859073643381, 66.83645039813700350 ) ) ;
#81926 = ORIENTED_EDGE ( 'NONE', *, *, #85503, .T. ) ;
#81927 = ORIENTED_EDGE ( 'NONE', *, *, #45753, .T. ) ;
#81928 = AXIS2_PLACEMENT_3D ( 'NONE', #5942, #62226, #89046 ) ;
#81929 = CARTESIAN_POINT ( 'NONE',  ( 12.27452259663393086, 85.83635631587367243, 117.9189384461415813 ) ) ;
#81930 = AXIS2_PLACEMENT_3D ( 'NONE', #43972, #70812, #1773 ) ;
#81931 = ORIENTED_EDGE ( 'NONE', *, *, #21279, .T. ) ;
#81932 = EDGE_LOOP ( 'NONE', ( #49915, #16723, #4183, #12042 ) ) ;
#81933 = FACE_BOUND ( 'NONE', #46788, .T. ) ;
#81934 = AXIS2_PLACEMENT_3D ( 'NONE', #42926, #70663, #7535 ) ;
#81935 = CARTESIAN_POINT ( 'NONE',  ( 114.7034172354883168, -32.83980166744527196, 43.62384839950495063 ) ) ;
#81937 = CARTESIAN_POINT ( 'NONE',  ( 112.4231589263966526, -46.42488254349225940, 252.9661014663871015 ) ) ;
#81936 = CIRCLE ( 'NONE', #64552, 16.09746158385918946 ) ;
#81938 = EDGE_CURVE ( 'NONE', #42224, #69089, #9468, .T. ) ;
#81939 = VECTOR ( 'NONE', #29142, 1000.000000000000000 ) ;
#81940 = CARTESIAN_POINT ( 'NONE',  ( 116.9962961068553966, -33.62662860631126449, 174.0670538473389399 ) ) ;
#81943 = EDGE_CURVE ( 'NONE', #84780, #11327, #25701, .T. ) ;
#81942 = CARTESIAN_POINT ( 'NONE',  ( 112.1867106929447573, -26.95862322015898016, 10.68038718067299087 ) ) ;
#81941 = CARTESIAN_POINT ( 'NONE',  ( 98.42165055296780451, -41.76806737957761584, 21.74622857282093591 ) ) ;
#81944 = LINE ( 'NONE', #47824, #11514 ) ;
#81945 = DIRECTION ( 'NONE',  ( 0.7071067811571405404, 0.7071067812159546051, 0.000000000000000000 ) ) ;
#81946 = ADVANCED_FACE ( 'NONE', ( #33793 ), #47401, .T. ) ;
#81947 = ORIENTED_EDGE ( 'NONE', *, *, #86959, .F. ) ;
#81948 = ADVANCED_FACE ( 'NONE', ( #66970 ), #32434, .F. ) ;
#81949 = FACE_OUTER_BOUND ( 'NONE', #22168, .T. ) ;
#81950 = CARTESIAN_POINT ( 'NONE',  ( 116.5766284862631466, -42.45395780223795157, 278.3832443235297660 ) ) ;
#81951 = ORIENTED_EDGE ( 'NONE', *, *, #45978, .F. ) ;
#81952 = CARTESIAN_POINT ( 'NONE',  ( 117.9328099866778246, -34.70409988052399086, 203.9851490854349549 ) ) ;
#81953 = CARTESIAN_POINT ( 'NONE',  ( 112.1393456185932251, -28.01282276695584983, 34.65645861137475947 ) ) ;
#81954 = PRESENTATION_STYLE_ASSIGNMENT (( #54192 ) ) ;
#81955 = DIRECTION ( 'NONE',  ( -0.000000000000000000, -1.000000000000000000, -0.000000000000000000 ) ) ;
#81956 = FACE_BOUND ( 'NONE', #76736, .T. ) ;
#81957 = CIRCLE ( 'NONE', #29755, 2.999999999999988898 ) ;
#81959 = CARTESIAN_POINT ( 'NONE',  ( 179.4595971212905852, -28.98061976758350511, 313.9678068554149490 ) ) ;
#81958 = CARTESIAN_POINT ( 'NONE',  ( 115.1744752910655620, -38.35034237767378329, 277.6356252759110248 ) ) ;
#81960 = DIRECTION ( 'NONE',  ( 0.000000000000000000, 0.000000000000000000, 1.000000000000000000 ) ) ;
#81961 = DIRECTION ( 'NONE',  ( 0.000000000000000000, 1.000000000000000000, 0.000000000000000000 ) ) ;
#81962 = CARTESIAN_POINT ( 'NONE',  ( -487.2989999999999782, 89.53805401447711176, 3.968750000000410338 ) ) ;
#81963 = CARTESIAN_POINT ( 'NONE',  ( 131.5667039024470455, -104.2784471599409244, 22.21780685541800082 ) ) ;
#81964 = CARTESIAN_POINT ( 'NONE',  ( 97.31602727650306406, -39.30641804829839714, 41.53089032425290839 ) ) ;
#81965 = DIRECTION ( 'NONE',  ( -1.000000000000000000, 0.000000000000000000, 0.000000000000000000 ) ) ;
#81967 = VERTEX_POINT ( 'NONE', #31996 ) ;
#81966 = CARTESIAN_POINT ( 'NONE',  ( -10.33011338239548493, 89.94938708489701185, -118.1053235025621291 ) ) ;
#81968 = CARTESIAN_POINT ( 'NONE',  ( 0.000000000000000000, 114.2999999999999972, -9.525000000000000355 ) ) ;
#81969 = CARTESIAN_POINT ( 'NONE',  ( 106.3003094972131208, -47.14862859053906874, 222.5184824187679453 ) ) ;
#81970 = CARTESIAN_POINT ( 'NONE',  ( 96.64197643737422538, -36.61924597882073584, 107.3184824187679567 ) ) ;
#81971 = CARTESIAN_POINT ( 'NONE',  ( 115.9970180223098311, -30.13831313182449989, 255.3203871806730660 ) ) ;
#81972 = DIRECTION ( 'NONE',  ( 1.000000000000000000, 0.000000000000000000, 0.000000000000000000 ) ) ;
#81973 = FACE_OUTER_BOUND ( 'NONE', #47769, .T. ) ;
#81975 = CARTESIAN_POINT ( 'NONE',  ( 89.17003477451885374, -56.47944715994104570, -5.074374724089047106 ) ) ;
#81974 = CARTESIAN_POINT ( 'NONE',  ( 183.5150000000000148, 14.63749999999999929, -47.62500000000000000 ) ) ;
#81976 = DIRECTION ( 'NONE',  ( 0.000000000000000000, 0.000000000000000000, 1.000000000000000000 ) ) ;
#81977 = AXIS2_PLACEMENT_3D ( 'NONE', #43583, #58120, #52162 ) ;
#81978 = CARTESIAN_POINT ( 'NONE',  ( 131.6146038194058292, -19.97617057400509566, 2.716753174561010287 ) ) ;
#81979 = AXIS2_PLACEMENT_3D ( 'NONE', #77937, #15260, #71128 ) ;
#81980 = ORIENTED_EDGE ( 'NONE', *, *, #43746, .T. ) ;
#81981 = EDGE_LOOP ( 'NONE', ( #49112, #10204, #74044, #44947 ) ) ;
#81982 = CARTESIAN_POINT ( 'NONE',  ( 108.0589421777836492, -45.73103505524393597, 157.0743245899819556 ) ) ;
#81984 = ORIENTED_EDGE ( 'NONE', *, *, #7488, .T. ) ;
#81983 = FACE_OUTER_BOUND ( 'NONE', #85727, .T. ) ;
#81985 = DIRECTION ( 'NONE',  ( -0.7071067811865779928, 0.7071067811865171526, -7.071067811865785947E-16 ) ) ;
#81986 = CARTESIAN_POINT ( 'NONE',  ( 98.47430666977648173, -42.65725675464086919, 122.8070538473389490 ) ) ;
#81987 = CARTESIAN_POINT ( 'NONE',  ( 168.3664380525669912, -48.62818131005517586, 180.4678068554150059 ) ) ;
#81988 = CARTESIAN_POINT ( 'NONE',  ( 71.06670390244705970, -124.7784471599409812, 45.21780685541799727 ) ) ;
#81989 = DIRECTION ( 'NONE',  ( 3.100000000000000258E-29, -3.100000000000000044E-14, -1.000000000000000000 ) ) ;
#81990 = DIRECTION ( 'NONE',  ( 0.000000000000000000, -1.000000000000000000, 0.000000000000000000 ) ) ;
#81991 = CARTESIAN_POINT ( 'NONE',  ( 97.00151786184777336, -41.45262973156714992, 61.67562527591097421 ) ) ;
#81992 = ORIENTED_EDGE ( 'NONE', *, *, #31313, .T. ) ;
#81993 = ORIENTED_EDGE ( 'NONE', *, *, #72954, .T. ) ;
#81994 = VERTEX_POINT ( 'NONE', #60135 ) ;
#81995 = AXIS2_PLACEMENT_3D ( 'NONE', #79648, #29255, #56939 ) ;
#81996 = VECTOR ( 'NONE', #77616, 1000.000000000000000 ) ;
#81997 = CARTESIAN_POINT ( 'NONE',  ( 97.81168895331838087, -40.51742574516882200, 287.6356252759109680 ) ) ;
#81998 = AXIS2_PLACEMENT_3D ( 'NONE', #19412, #61186, #46649 ) ;
#82000 = LINE ( 'NONE', #40640, #34577 ) ;
#81999 = CARTESIAN_POINT ( 'NONE',  ( 108.7386892141029335, -46.36620816325528693, 163.7127681330539701 ) ) ;
#82001 = CIRCLE ( 'NONE', #42791, 10.00000000000000355 ) ;
#82002 = LINE ( 'NONE', #89257, #45039 ) ;
#82003 = EDGE_CURVE ( 'NONE', #82155, #38959, #42815, .T. ) ;
#82004 = CARTESIAN_POINT ( 'NONE',  ( 12.61959663417972521, 80.89626266586573422, -129.9447639770759508 ) ) ;
#82005 = EDGE_CURVE ( 'NONE', #64140, #41877, #46052, .T. ) ;
#82006 = DIRECTION ( 'NONE',  ( -1.000000000000000000, 0.000000000000000000, 0.000000000000000000 ) ) ;
#82007 = EDGE_CURVE ( 'NONE', #57667, #1571, #60589, .T. ) ;
#82008 = CARTESIAN_POINT ( 'NONE',  ( 87.71185091857864791, 93.94641470820116069, 79.76397050720474624 ) ) ;
#82009 = CARTESIAN_POINT ( 'NONE',  ( 115.0369792144555134, -42.90881563258641052, 179.3022564342772114 ) ) ;
#82010 = CARTESIAN_POINT ( 'NONE',  ( 117.8338636819851644, -39.12263375953642708, 103.6403871806729455 ) ) ;
#82011 = VERTEX_POINT ( 'NONE', #74681 ) ;
#82012 = EDGE_LOOP ( 'NONE', ( #81482, #59096, #82030, #4011 ) ) ;
#82013 = EDGE_LOOP ( 'NONE', ( #14317, #23897, #32315, #15370 ) ) ;
#82014 = VECTOR ( 'NONE', #56087, 1000.000000000000000 ) ;
#82015 = EDGE_CURVE ( 'NONE', #45804, #88820, #12461, .T. ) ;
#82016 = FACE_OUTER_BOUND ( 'NONE', #46127, .T. ) ;
#82017 = CARTESIAN_POINT ( 'NONE',  ( -82.89895571708225930, 82.54999999999999716, -100.8594679592215471 ) ) ;
#82018 = DIRECTION ( 'NONE',  ( 0.000000000000000000, -1.000000000000000000, 0.000000000000000000 ) ) ;
#82020 = CARTESIAN_POINT ( 'NONE',  ( 115.5744916924636954, -35.14366089088881751, 201.8033284648299457 ) ) ;
#82019 = VECTOR ( 'NONE', #8242, 1000.000000000000000 ) ;
#82021 = EDGE_CURVE ( 'NONE', #70182, #73152, #55842, .T. ) ;
#82022 = AXIS2_PLACEMENT_3D ( 'NONE', #55102, #21065, #35574 ) ;
#82023 = EDGE_CURVE ( 'NONE', #1995, #41277, #776, .T. ) ;
#82024 = CARTESIAN_POINT ( 'NONE',  ( 115.8261224330695569, -31.73121246411632512, 25.23977400646692715 ) ) ;
#82025 = ORIENTED_EDGE ( 'NONE', *, *, #19232, .T. ) ;
#82027 = ORIENTED_EDGE ( 'NONE', *, *, #68548, .T. ) ;
#82026 = ORIENTED_EDGE ( 'NONE', *, *, #48526, .F. ) ;
#82028 = DIRECTION ( 'NONE',  ( 0.000000000000000000, 0.000000000000000000, -1.000000000000000000 ) ) ;
#82029 = CARTESIAN_POINT ( 'NONE',  ( 144.1785682890445628, -138.0502943055581966, 247.6584922886219999 ) ) ;
#82030 = ORIENTED_EDGE ( 'NONE', *, *, #77754, .T. ) ;
#82031 = EDGE_LOOP ( 'NONE', ( #64239, #67815, #84734, #50058 ) ) ;
#82032 = CARTESIAN_POINT ( 'NONE',  ( 77.65458752641551143, -20.05177997656060995, 7.178113714840788973 ) ) ;
#82033 = EDGE_CURVE ( 'NONE', #23851, #78707, #27870, .T. ) ;
#82034 = CARTESIAN_POINT ( 'NONE',  ( 116.1701677112242237, -32.41741342456931818, 210.6101547344689777 ) ) ;
#82035 = DIRECTION ( 'NONE',  ( 3.100000000000000258E-29, -3.100000000000000044E-14, -1.000000000000000000 ) ) ;
#82036 = EDGE_CURVE ( 'NONE', #48953, #78000, #20176, .T. ) ;
#82037 = VECTOR ( 'NONE', #50174, 1000.000000000000000 ) ;
#82038 = CARTESIAN_POINT ( 'NONE',  ( -109.5132684488906705, 57.82504450241307126, 71.07540765708218089 ) ) ;
#82039 = ORIENTED_EDGE ( 'NONE', *, *, #58795, .T. ) ;
#82040 = ORIENTED_EDGE ( 'NONE', *, *, #30193, .T. ) ;
#82041 = DIRECTION ( 'NONE',  ( 0.000000000000000000, 1.000000000000000000, 0.000000000000000000 ) ) ;
#82042 = CIRCLE ( 'NONE', #15317, 2.749999999999974687 ) ;
#82043 = EDGE_LOOP ( 'NONE', ( #35433, #23237, #63069, #57825 ) ) ;
#82044 = VERTEX_POINT ( 'NONE', #14256 ) ;
#82045 = CARTESIAN_POINT ( 'NONE',  ( 115.6911714722407396, -33.30735935496929301, 246.9452332267339614 ) ) ;
#82046 = CARTESIAN_POINT ( 'NONE',  ( 114.5280328947845732, -29.41122550446140949, 149.4441967044819819 ) ) ;
#82047 = CARTESIAN_POINT ( 'NONE',  ( 106.9276426037745011, -26.29176787048580266, 60.08705384733897858 ) ) ;
#82048 = CARTESIAN_POINT ( 'NONE',  ( 99.79500342874349883, -40.09713400422746332, 249.5838068554171514 ) ) ;
#82049 = LINE ( 'NONE', #27066, #62678 ) ;
#82050 = CARTESIAN_POINT ( 'NONE',  ( 107.8711561831457857, -25.29845801491854473, 321.2571935114572739 ) ) ;
#82051 = CARTESIAN_POINT ( 'NONE',  ( 117.4872506282070503, -40.41476785070875621, 174.5680062282919778 ) ) ;
#82052 = DIRECTION ( 'NONE',  ( 1.000000000000000000, 4.299999999999999979E-14, 1.000000000000000078E-15 ) ) ;
#82053 = ORIENTED_EDGE ( 'NONE', *, *, #50743, .T. ) ;
#82054 = DIRECTION ( 'NONE',  ( 0.000000000000000000, 1.000000000000000000, 1.914177628664063178E-15 ) ) ;
#82055 = ORIENTED_EDGE ( 'NONE', *, *, #40112, .F. ) ;
#82056 = EDGE_LOOP ( 'NONE', ( #22334, #1846, #16721, #43640, #12777, #63145, #10949, #11081, #88138, #18012, #44971, #34164, #80417, #81267, #25237, #80383, #15659, #78057, #80533, #1874, #21797, #48651, #69991, #83360, #17297, #55063, #4441, #61182, #39519, #43006, #79590, #30513, #82253, #59067, #84007, #44853, #81187, #80842, #68796, #39529, #46928, #75076, #72715, #15970, #65266, #45222, #88191, #69882 ) ) ;
#82057 = FACE_OUTER_BOUND ( 'NONE', #29327, .T. ) ;
#82058 = EDGE_CURVE ( 'NONE', #3590, #52727, #36033, .T. ) ;
#82059 = ORIENTED_EDGE ( 'NONE', *, *, #42745, .T. ) ;
#82060 = CIRCLE ( 'NONE', #73345, 3.250000000000002665 ) ;
#82061 = CARTESIAN_POINT ( 'NONE',  ( 97.80395965993845664, -40.49850016457129698, 137.6339984679455313 ) ) ;
#82062 = VECTOR ( 'NONE', #30140, 1000.000000000000000 ) ;
#82063 = CONICAL_SURFACE ( 'NONE', #31256, 118.5560000000000116, 0.7853981633974346233 ) ;
#82064 = CARTESIAN_POINT ( 'NONE',  ( 105.7968630617233288, -26.72439637550503377, 91.17750313677824181 ) ) ;
#82065 = CARTESIAN_POINT ( 'NONE',  ( 116.5985118214053813, -29.68807528100325044, 109.3327681330539605 ) ) ;
#82066 = CARTESIAN_POINT ( 'NONE',  ( 104.4929461018149937, -26.97798581942615215, 255.2813983111578011 ) ) ;
#82067 = CIRCLE ( 'NONE', #61726, 0.5000000000000004441 ) ;
#82068 = CARTESIAN_POINT ( 'NONE',  ( 136.7302760451810286, -36.02416100034015756, 6.874390491355895527 ) ) ;
#82069 = CARTESIAN_POINT ( 'NONE',  ( 0.000000000000000000, 82.54999999999999716, 92.46299999999996544 ) ) ;
#82072 = CARTESIAN_POINT ( 'NONE',  ( 117.9098725419244005, -34.70837513311213485, 199.9851490854349549 ) ) ;
#82071 = DIRECTION ( 'NONE',  ( 0.000000000000000000, -5.300584669389750404E-15, 1.000000000000000000 ) ) ;
#82070 = CARTESIAN_POINT ( 'NONE',  ( 116.7951252707073024, -39.38782979302678910, 144.6147919423369785 ) ) ;
#82073 = LINE ( 'NONE', #20282, #82907 ) ;
#82074 = CYLINDRICAL_SURFACE ( 'NONE', #45313, 11.17600000000001970 ) ;
#82075 = ORIENTED_EDGE ( 'NONE', *, *, #1302, .F. ) ;
#82076 = DIRECTION ( 'NONE',  ( 0.000000000000000000, 0.000000000000000000, 1.000000000000000000 ) ) ;
#82077 = CIRCLE ( 'NONE', #81864, 5.599999999999994316 ) ;
#82078 = CARTESIAN_POINT ( 'NONE',  ( 75.31670390244798341, -57.40094715994099772, 33.40080685541480676 ) ) ;
#82079 = CARTESIAN_POINT ( 'NONE',  ( 125.9611475301391721, -14.72944715994100484, 239.5838068554164977 ) ) ;
#82080 = CIRCLE ( 'NONE', #41250, 0.5000000000000004441 ) ;
#82081 = CARTESIAN_POINT ( 'NONE',  ( -479.3614999999999782, 3.174999999999999822, -1.387778780781445991E-14 ) ) ;
#82082 = ADVANCED_FACE ( 'NONE', ( #89669 ), #41930, .F. ) ;
#82084 = ORIENTED_EDGE ( 'NONE', *, *, #51222, .F. ) ;
#82083 = CARTESIAN_POINT ( 'NONE',  ( 115.9975756407361018, -30.13790158448777845, 259.3203871806730945 ) ) ;
#82085 = CYLINDRICAL_SURFACE ( 'NONE', #74181, 16.00000000000090239 ) ;
#82086 = CARTESIAN_POINT ( 'NONE',  ( 104.5830001944168259, -26.58193179050359589, 281.2670538473395823 ) ) ;
#82087 = CARTESIAN_POINT ( 'NONE',  ( 97.63545021146504155, -41.27351965004424983, 167.6841967044829573 ) ) ;
#82088 = LINE ( 'NONE', #18481, #25883 ) ;
#82089 = CARTESIAN_POINT ( 'NONE',  ( 109.7248315322984524, -27.00080197363539725, 100.8648701262310823 ) ) ;
#82090 = VECTOR ( 'NONE', #29476, 1000.000000000000000 ) ;
#82092 = DIRECTION ( 'NONE',  ( 0.000000000000000000, 0.000000000000000000, 1.000000000000000000 ) ) ;
#82091 = CARTESIAN_POINT ( 'NONE',  ( 114.6444261855608175, -117.4034471599418055, -11.78219314458159239 ) ) ;
#82093 = DIRECTION ( 'NONE',  ( 1.000000000000000000, 0.000000000000000000, 0.000000000000000000 ) ) ;
#82094 = CARTESIAN_POINT ( 'NONE',  ( 34.92499999999999716, 87.13271776169270311, 294.9574999999999818 ) ) ;
#82095 = ORIENTED_EDGE ( 'NONE', *, *, #63457, .F. ) ;
#82096 = EDGE_CURVE ( 'NONE', #19571, #80402, #48289, .T. ) ;
#82097 = VECTOR ( 'NONE', #67, 1000.000000000000000 ) ;
#82098 = ORIENTED_EDGE ( 'NONE', *, *, #26914, .F. ) ;
#82099 = ORIENTED_EDGE ( 'NONE', *, *, #87436, .T. ) ;
#82100 = VERTEX_POINT ( 'NONE', #75589 ) ;
#82101 = CARTESIAN_POINT ( 'NONE',  ( -446.0240000000000009, 93.66249999999999432, 6.350000000000409983 ) ) ;
#82102 = CARTESIAN_POINT ( 'NONE',  ( 95.28387218206130171, -35.72034718286344912, 32.25848241876794020 ) ) ;
#82103 = CARTESIAN_POINT ( 'NONE',  ( 144.0731096511982798, -140.3870298840350017, 246.8745206071880034 ) ) ;
#82104 = DIRECTION ( 'NONE',  ( -0.0001713722456129692653, 0.9999999853157764962, 0.000000000000000000 ) ) ;
#82105 = CARTESIAN_POINT ( 'NONE',  ( 131.3164832912740110, -36.72944715994100306, -5.074374724089004474 ) ) ;
#82106 = CARTESIAN_POINT ( 'NONE',  ( 99.20650695390740736, -40.14600596985821568, 231.0752769709339418 ) ) ;
#82107 = VERTEX_POINT ( 'NONE', #27420 ) ;
#82108 = EDGE_LOOP ( 'NONE', ( #32131, #86366, #27621, #24350 ) ) ;
#82109 = VERTEX_POINT ( 'NONE', #7881 ) ;
#82110 = CARTESIAN_POINT ( 'NONE',  ( -47.11752803141010304, 65.60000000000000853, 108.7909173056707317 ) ) ;
#82111 = CIRCLE ( 'NONE', #5184, 10.00000000000000888 ) ;
#82112 = CARTESIAN_POINT ( 'NONE',  ( 99.50492789300037089, -43.30601609924293172, 101.8962887008209464 ) ) ;
#82113 = DIRECTION ( 'NONE',  ( 1.387778780781444492E-15, 0.000000000000000000, -1.000000000000000000 ) ) ;
#82114 = CARTESIAN_POINT ( 'NONE',  ( 102.0649443859605299, -27.97173592226543093, 275.4895552553568905 ) ) ;
#82115 = EDGE_CURVE ( 'NONE', #7119, #8522, #1528, .T. ) ;
#82116 = EDGE_CURVE ( 'NONE', #56525, #31932, #2263, .T. ) ;
#82117 = LINE ( 'NONE', #33933, #27011 ) ;
#82118 = EDGE_CURVE ( 'NONE', #9110, #73852, #60264, .T. ) ;
#82119 = CARTESIAN_POINT ( 'NONE',  ( 109.7226150969135716, -27.00020866801084196, 174.8649754870583308 ) ) ;
#82120 = CARTESIAN_POINT ( 'NONE',  ( 106.1957191385480570, -47.06291487533376028, 262.4975300378164320 ) ) ;
#82121 = LINE ( 'NONE', #768, #66135 ) ;
#82122 = ORIENTED_EDGE ( 'NONE', *, *, #36293, .T. ) ;
#82123 = EDGE_CURVE ( 'NONE', #72752, #19831, #52975, .T. ) ;
#82124 = DIRECTION ( 'NONE',  ( 1.000000000000000000, 4.272717921125132861E-14, 0.000000000000000000 ) ) ;
#82125 = CYLINDRICAL_SURFACE ( 'NONE', #59753, 5.000000000000004441 ) ;
#82126 = CARTESIAN_POINT ( 'NONE',  ( 98.90209562501077301, -37.38172185807169967, 99.20809036959194316 ) ) ;
#82127 = CIRCLE ( 'NONE', #21228, 3.174999999999983391 ) ;
#82128 = EDGE_CURVE ( 'NONE', #11434, #14889, #16720, .T. ) ;
#82129 = VECTOR ( 'NONE', #55358, 1000.000000000000000 ) ;
#82130 = AXIS2_PLACEMENT_3D ( 'NONE', #63669, #36420, #75952 ) ;
#82131 = FACE_OUTER_BOUND ( 'NONE', #45784, .T. ) ;
#82132 = AXIS2_PLACEMENT_3D ( 'NONE', #88262, #27354, #26022 ) ;
#82133 = CARTESIAN_POINT ( 'NONE',  ( 97.81170508561586985, -40.51744524251693491, 57.63550115181184452 ) ) ;
#82134 = EDGE_CURVE ( 'NONE', #4517, #27286, #19618, .T. ) ;
#82135 = DIRECTION ( 'NONE',  ( 1.000000000000000078E-15, -1.000000000000000083E-30, -1.000000000000000000 ) ) ;
#82136 = EDGE_LOOP ( 'NONE', ( #41117, #2743, #18789, #36111, #66462, #50943 ) ) ;
#82137 = CYLINDRICAL_SURFACE ( 'NONE', #65817, 3.000000000000002665 ) ;
#82138 = ORIENTED_EDGE ( 'NONE', *, *, #89002, .F. ) ;
#82139 = CARTESIAN_POINT ( 'NONE',  ( 116.8067323440835565, -43.47985705614018315, 163.3441967044829823 ) ) ;
#82140 = ORIENTED_EDGE ( 'NONE', *, *, #69912, .T. ) ;
#82141 = DIRECTION ( 'NONE',  ( -2.913971193241881161E-15, 0.000000000000000000, 1.000000000000000000 ) ) ;
#82142 = CARTESIAN_POINT ( 'NONE',  ( 108.1315353547809224, -45.52682987947058280, 114.1044404487549571 ) ) ;
#82143 = DIRECTION ( 'NONE',  ( 4.299999999999999979E-14, -1.000000000000000000, 4.400000000000000367E-29 ) ) ;
#82144 = DIRECTION ( 'NONE',  ( 0.000000000000000000, -1.000000000000000000, 0.000000000000000000 ) ) ;
#82145 = VECTOR ( 'NONE', #8416, 1000.000000000000000 ) ;
#82146 = CARTESIAN_POINT ( 'NONE',  ( 112.7717388973142647, -27.93574178168534061, 65.61848241876793963 ) ) ;
#82147 = FACE_OUTER_BOUND ( 'NONE', #77899, .T. ) ;
#82148 = DIRECTION ( 'NONE',  ( 1.000000000000000000, 4.299999999999999979E-14, 1.000000000000000078E-15 ) ) ;
#82149 = VERTEX_POINT ( 'NONE', #63291 ) ;
#82150 = CARTESIAN_POINT ( 'NONE',  ( -118.1261869548601453, 74.80137413886471620, -10.09682577435429529 ) ) ;
#82151 = ORIENTED_EDGE ( 'NONE', *, *, #4803, .F. ) ;
#82152 = AXIS2_PLACEMENT_3D ( 'NONE', #52432, #44300, #57943 ) ;
#82153 = VERTEX_POINT ( 'NONE', #84207 ) ;
#82154 = CARTESIAN_POINT ( 'NONE',  ( 183.5150000000000148, 68.61249999999999716, -35.28456447661459805 ) ) ;
#82155 = VERTEX_POINT ( 'NONE', #28307 ) ;
#82156 = CARTESIAN_POINT ( 'NONE',  ( 115.2378349030890945, -31.35427756934436871, 254.2899109901970292 ) ) ;
#82157 = CARTESIAN_POINT ( 'NONE',  ( 113.3444227873369243, -45.07958072982976461, 139.0899109901969553 ) ) ;
#82158 = CARTESIAN_POINT ( 'NONE',  ( -487.2989999999999782, 86.51875000000001137, 86.36305401447658880 ) ) ;
#82159 = CARTESIAN_POINT ( 'NONE',  ( 163.0664832912739826, 22.62155284005901024, 339.0006252759110339 ) ) ;
#82160 = CARTESIAN_POINT ( 'NONE',  ( 96.07767081433036083, -37.92107664550148627, 77.40038718067299328 ) ) ;
#82161 = CARTESIAN_POINT ( 'NONE',  ( 36.23715912545424089, -47.82818131006125384, 300.4678068554150059 ) ) ;
#82162 = ORIENTED_EDGE ( 'NONE', *, *, #79879, .T. ) ;
#82163 = CARTESIAN_POINT ( 'NONE',  ( 37.03715912545433753, -48.62818131006121547, 237.4678068554150059 ) ) ;
#82164 = CARTESIAN_POINT ( 'NONE',  ( 12.60000000000000142, 82.54999999999999716, 117.6834004267381744 ) ) ;
#82165 = EDGE_CURVE ( 'NONE', #86561, #55881, #28779, .T. ) ;
#82166 = ORIENTED_EDGE ( 'NONE', *, *, #79559, .T. ) ;
#82167 = CARTESIAN_POINT ( 'NONE',  ( 72.96458098368650269, 127.0000000000000000, 72.96458098368729850 ) ) ;
#82168 = DIRECTION ( 'NONE',  ( 0.000000000000000000, 0.000000000000000000, 1.000000000000000000 ) ) ;
#82169 = CARTESIAN_POINT ( 'NONE',  ( 97.23737678141878860, -33.32131919061083636, 286.0613395616252888 ) ) ;
#82170 = CARTESIAN_POINT ( 'NONE',  ( 85.24325998657074877, -58.55267046464445002, -4.824374724089051547 ) ) ;
#82171 = DIRECTION ( 'NONE',  ( -1.000000000000000078E-15, -1.000000000000000083E-30, 1.000000000000000000 ) ) ;
#82172 = DIRECTION ( 'NONE',  ( 0.000000000000000000, 0.7071067811865328068, 0.7071067811865622277 ) ) ;
#82173 = CARTESIAN_POINT ( 'NONE',  ( 115.3461623907574563, -31.52268719801062957, 34.27276813305396530 ) ) ;
#82175 = CARTESIAN_POINT ( 'NONE',  ( 108.9808406375926779, -47.59218431635552093, 118.7032443235299723 ) ) ;
#82174 = CARTESIAN_POINT ( 'NONE',  ( 100.9654861239525161, -28.69876604995092961, 100.5949546195926132 ) ) ;
#82176 = FACE_OUTER_BOUND ( 'NONE', #82492, .T. ) ;
#82177 = CARTESIAN_POINT ( 'NONE',  ( 108.7503283313270543, -25.75779200005056779, 144.9432443235299672 ) ) ;
#82178 = ORIENTED_EDGE ( 'NONE', *, *, #16145, .F. ) ;
#82179 = DIRECTION ( 'NONE',  ( 0.000000000000000000, 1.365923996832131856E-16, -1.000000000000000000 ) ) ;
#82180 = ORIENTED_EDGE ( 'NONE', *, *, #38089, .T. ) ;
#82181 = FACE_OUTER_BOUND ( 'NONE', #84899, .T. ) ;
#82182 = CARTESIAN_POINT ( 'NONE',  ( 109.4081066450106619, 51.07333133673250103, 71.23720173749269691 ) ) ;
#82183 = CARTESIAN_POINT ( 'NONE',  ( 136.8164832912740110, -36.72944715994100306, 3.101481641215515950 ) ) ;
#82184 = EDGE_LOOP ( 'NONE', ( #61446, #85903, #17559, #61131, #42966 ) ) ;
#82185 = CARTESIAN_POINT ( 'NONE',  ( 115.0909704615979763, -30.62031916169713597, 60.34404414507040570 ) ) ;
#82187 = ORIENTED_EDGE ( 'NONE', *, *, #22868, .F. ) ;
#82186 = CARTESIAN_POINT ( 'NONE',  ( 102.8958089960464690, -27.08850953439599962, 155.4013395616249795 ) ) ;
#82188 = CARTESIAN_POINT ( 'NONE',  ( 182.4202572930400095, -33.70561438051981185, -5.074374724088000832 ) ) ;
#82189 = AXIS2_PLACEMENT_3D ( 'NONE', #59636, #59196, #81472 ) ;
#82190 = CARTESIAN_POINT ( 'NONE',  ( -129.9449521816638935, 84.21449860606323057, 12.61764002986459765 ) ) ;
#82191 = CARTESIAN_POINT ( 'NONE',  ( 12.69999999999999929, 82.54999999999999716, 129.9368274816650057 ) ) ;
#82193 = VECTOR ( 'NONE', #66789, 1000.000000000000000 ) ;
#82192 = CARTESIAN_POINT ( 'NONE',  ( 105.7154773402737789, -46.72385839347782621, 77.46895861002991523 ) ) ;
#82194 = ORIENTED_EDGE ( 'NONE', *, *, #72361, .F. ) ;
#82195 = ADVANCED_FACE ( 'NONE', ( #2416 ), #65957, .F. ) ;
#82196 = AXIS2_PLACEMENT_3D ( 'NONE', #47282, #82295, #54977 ) ;
#82197 = PRODUCT_CONTEXT ( 'NONE', #12135, 'mechanical' ) ;
#82198 = CIRCLE ( 'NONE', #18294, 34.13125000000000142 ) ;
#82199 = ORIENTED_EDGE ( 'NONE', *, *, #64682, .T. ) ;
#82200 = ORIENTED_EDGE ( 'NONE', *, *, #75755, .F. ) ;
#82201 = ORIENTED_EDGE ( 'NONE', *, *, #84057, .T. ) ;
#82202 = FACE_OUTER_BOUND ( 'NONE', #10679, .T. ) ;
#82203 = B_SPLINE_SURFACE_WITH_KNOTS ( 'NONE', 3, 3, ( 
 ( #15593, #36480, #73209, #65513, #79610, #65948, #58678, #80055, #44604, #23317, #78724, #58251, #50983, #24625, #4185, #57802, #37364, #85539, #31427, #38251, #44156, #51416, #3298, #3735, #10989, #24189, #25070, #59127, #10109, #16478, #80495, #30990, #17811, #23749, #52293, #11448, #18254, #37817, #79167, #86422, #17369, #39145, #45051, #85980, #51858, #31881, #59571, #16928, #72341, #86864, #72781, #10548, #30105, #71896, #30552, #45487, #9655, #45932, #2406, #65071, #73665, #38689, #2853, #66394, #87306, #52734, #46834, #56224, #60014, #35346, #4632, #87749, #53639, #21748, #48960, #14929, #69885, #7658, #33234, #63060, #60933, #83975, #19598, #74562, #12804, #81413, #32779, #840, #28529, #76701, #81848, #39586, #5076, #40492, #66852, #68208, #49417, #32318, #77153, #19160, #11901, #89099, #55768, #12344, #25517, #60471, #53187, #80958, #18703, #46387, #14481, #88217, #40035, #25974, #67753, #74121, #5541, #26858, #42157, #83514, #61375, #88660, #67292, #26422, #54092, #21286, #5991, #47289, #75014, #33679, #8108, #23980, #43498, #50776, #51654, #49866, #71244, #8560, #78949, #36260, #77598, #79398, #58040, #1748, #37606, #23543, #63971, #29447, #70789, #57128, #72124, #50316, #2645, #16714, #85773, #37157, #84875, #42597, #35795, #15381, #30345, #78511, #29900, #51206, #65307, #63509, #70333, #9015, #16270, #1296, #43048, #36714, #22645, #44393, #78060, #15823, #29002, #9898, #64413, #2194, #56687, #71683, #43948, #84430, #57586, #85329, #9447, #3085, #23104, #30781, #64858, #58471, #22197, #86202, #80291, #4862, #38475, #67085, #26201, #5316, #24861, #66178, #18036, #4423, #53875, #59804, #10768, #73447, #46623, #74354, #31667, #73003, #52967, #3967, #11221, #44844, #3516, #45284, #32551, #72574, #60703, #17162, #24422, #33006, #52528, #65734, #39379, #79847, #45717, #87095, #88440, #10341, #12125, #38045, #31216, #59365, #58912, #87987, #86648, #18940, #39807, #38926, #67529, #66633, #52087, #87538, #32110, #80730, #25298, #18479, #17605, #46171, #25746, #73902, #11686, #60256, #53422, #81190, #55222, #35242, #19387, #62950, #6214, #26642, #13919, #69331, #27099, #42054, #19834, #28433, #81639, #47063, #33458, #13470, #5767, #54767, #7557, #54317, #62509, #82537, #68883, #82979, #47965, #7108, #33904, #12579, #67985, #47518, #40265, #41598, #83410, #74798, #41155, #13031, #75255, #20297, #6653, #40715, #75702, #61162, #76135, #88890, #61598, #82087, #68439, #34347, #34800, #89337, #27985, #726, #62054, #89788, #27542, #287, #55659, #20732, #48402, #21186, #48858, #76595, #14377, #69781, #78847, #77489, #70224, #22989, #1648, #84768, #37045, #78405, #7997, #50664, #43395, #57929, #22534, #65197, #49762, #36614, #49315, #85662, #16605, #22097, #70678, #29348, #23440, #8453, #35694, #57027, #72020, #64750, #30236, #51106, #36152, #64314, #2974, #56117, #29789, #44283, #2537, #50212, #84326, #83869, #9787, #15718, #37495, #77947, #71136, #8915, #2084, #21645, #57483, #77048, #14828, #85222, #16167, #43846, #71582, #9341, #42496, #63407, #63868, #1189, #28899, #56583, #15269, #42944, #31555, #66524, #17495, #79737, #44733, #32001, #74248, #87430, #80181, #24748, #51980, #59695, #18830, #32440, #73793, #45175, #46057, #59258, #4313, #72899, #10664, #72464, #25189, #12023, #52851, #17929, #52417, #38369, #80623, #46512, #60140, #10231, #45605, #37936, #66069, #39705, #3419, #11579, #3863, #73337, #18372, #86988, #39270, #11110, #51543, #17052, #86548, #79292, #66975, #87875, #86100, #38819, #4756, #24313, #25638, #53314, #81080, #67413, #30675, #58373, #23873, #65635, #31108, #58805, #40610, #55107, #26538, #41489, #21070, #68327, #54210, #61050, #76028, #82869, #48745, #6107, #48294, #47857, #6991, #34685, #13364, #27875, #81971, #19283, #61941, #33799, #61493, #13806, #27427, #46956, #89674, #82421, #62394, #89225, #14261, #88781, #75594, #88337, #173, #55550, #19719, #47407, #26989, #83303, #75136, #74686, #54655, #76479, #69219, #41936, #5203, #12922, #41051, #32897, #60594, #68776, #26096, #53765, #20182, #33351, #81531, #12467, #6542, #40151, #34237, #20626, #67872, #5659, #50998, #15155, #43736, #36934, #77833, #15610, #70567, #1975, #56921, #50098, #78293, #49650, #71024, #29672 ),
 ( #69667, #43283, #23332, #7439, #78741, #84212, #14711, #57366, #85106, #42831, #30121, #7886, #16496, #35128, #62839, #64635, #50551, #35579, #56466, #63296, #1073, #9235, #77376, #22876, #71474, #16056, #64203, #28785, #615, #28312, #42385, #2421, #8801, #84656, #57819, #85554, #56004, #83754, #8340, #36499, #21530, #76933, #36038, #21983, #49199, #63754, #70112, #1533, #29235, #22424, #79183, #37381, #73223, #80069, #85995, #3312, #17383, #45498, #25081, #65960, #66865, #11001, #51871, #9669, #32331, #45067, #31893, #65528, #4199, #53200, #60030, #79624, #31003, #72794, #31440, #80970, #86876, #37833, #10559, #73683, #11463, #58697, #10123, #17824, #86437, #38264, #71911, #30566, #72356, #59583, #65086, #87765, #44175, #51435, #25529, #3752, #2869, #66408, #16941, #59144, #24203, #58265, #23767, #39160, #44620, #24638, #52305, #38703, #52746, #87319, #45944, #4644, #80510, #18266, #12819, #6877, #61387, #88676, #54549, #5553, #74575, #20526, #41385, #27322, #33694, #81426, #46845, #82313, #18719, #20073, #62286, #46402, #71, #33246, #53655, #40942, #6433, #54105, #69115, #12357, #55450, #74138, #11912, #13695, #89561, #40047, #60944, #67763, #26434, #48193, #81859, #68667, #82765, #34128, #13257, #19612, #27771, #39598, #19174, #61828, #47750, #6004, #54996, #34581, #67305, #5093, #47302, #26873, #32791, #25985, #75027, #40503, #75924, #68223, #89113, #60481, #88230, #75485, #62737, #48638, #8234, #42720, #69562, #49091, #35467, #35923, #22313, #56359, #36394, #63642, #70011, #76374, #1869, #63189, #56808, #21417, #29126, #85002, #29567, #7780, #76821, #964, #21871, #22770, #77274, #83647, #28666, #70917, #8691, #14605, #55897, #70463, #42280, #84100, #20959, #41826, #28206, #84556, #14149, #57253, #83202, #49541, #7338, #15048, #1425, #43176, #49990, #77729, #15503, #35026, #64098, #512, #12200, #5385, #61231, #28051, #55293, #21253, #76210, #13986, #40786, #39888, #55730, #74426, #81705, #354, #19906, #33084, #6721, #47141, #82157, #54392, #62577, #67606, #41666, #60781, #88516, #88953, #83479, #83051, #26270, #69405, #7180, #68509, #34869, #6276, #53946, #27165, #47588, #20364, #26706, #40340, #19457, #74874, #20802, #89407, #12649, #68058, #48037, #5842, #75771, #33531, #75323, #13103, #33967, #61670, #34419, #62128, #54840, #82605, #13539, #41223, #68953, #89861, #27611, #48467, #14895, #35760, #77118, #42559, #78473, #56648, #8979, #23064, #64380, #43462, #70292, #30306, #14448, #21711, #36678, #84835, #36222, #2155, #43912, #42124, #58001, #49830, #57092, #85734, #56188, #77557, #8069, #85290, #63473, #83941, #48923, #29864, #1260, #49383, #69851, #78018, #22605, #803, #28966, #22163, #50277, #57548, #70749, #71647, #15786, #84396, #7622, #37122, #15342, #50737, #43011, #16236, #76665, #64823, #8524, #63932, #1711, #29414, #35308, #71203, #9410, #2605, #63021, #28497, #9092, #42596, #56223, #389, #21747, #49865, #21285, #70332, #1295, #8107, #27648, #41705, #77597, #7657, #68988, #55329, #69438, #56686, #6756, #84874, #78059, #48504, #57127, #76700, #89897, #63508, #14019, #48959, #14480, #29446, #34454, #8559, #62162, #83085, #28083, #22644, #22196, #41260, #43047, #70788, #35345, #36259, #63059, #50315, #83974, #42156, #77152, #55767, #7214, #63970, #1747, #15380, #49416, #34902, #62614, #14928, #20837, #35794, #76247, #83513, #69884, #839, #28528, #29001, #84429, #51205, #66177, #43947, #52527, #15822, #71243, #10767, #86647, #71682, #2644, #9446, #37156, #45283, #23542, #65733, #79846, #31215, #10340, #64857, #87094, #9014, #78510, #3515, #51653, #3084, #58911, #38474, #36713, #24860, #16713, #23979, #43497, #23103, #44392, #30344, #52086, #58039, #50775, #64412, #24421, #85772, #16269, #2193, #44843, #79397, #57585, #78948, #72123, #17161, #17604, #37605, #3966, #72573, #9897, #29899, #31666, #65306, #73002, #30780, #59364, #85328, #58470, #86201, #38044, #81189, #67528, #27098, #33005, #73901, #46622, #19833, #47517, #18035, #66632, #18478, #5766, #45716, #33903, #80290, #87537, #6213, #25745, #38925, #12578, #52966, #87986, #88439, #39806, #74353, #11685, #19386, #68438, #82086, #32109, #12124, #4422, #53421, #61597, #80729, #61161, #18939, #5315, #53874 ),
 ( #46170, #60702, #73446, #74797, #11220, #32550, #39378, #67084, #26200, #40264, #4861, #26641, #89336, #81638, #60255, #47062, #88889, #67984, #59803, #33457, #54316, #75254, #13030, #40714, #25297, #77488, #76134, #68882, #21644, #286, #83409, #35693, #77047, #6652, #49314, #42053, #56582, #21185, #63867, #48401, #35241, #47964, #84325, #15268, #20731, #69330, #27984, #22096, #7107, #34346, #55658, #70677, #63406, #28898, #49761, #34799, #62949, #1647, #54766, #28432, #42943, #1188, #48857, #82978, #82536, #8452, #14376, #36151, #76594, #69780, #7556, #725, #20296, #56116, #75701, #13469, #83868, #41154, #14827, #42495, #13918, #70223, #62053, #7996, #89787, #27541, #55221, #41597, #62508, #3418, #86547, #37494, #72898, #30674, #44282, #78404, #9786, #37935, #9340, #58372, #79291, #72463, #43845, #44732, #30235, #65196, #16166, #71581, #64313, #2083, #79736, #2973, #78846, #23439, #50663, #86099, #17494, #31107, #71135, #51105, #43394, #64749, #45174, #29788, #10230, #2536, #16604, #23872, #85661, #17051, #37044, #50211, #15717, #85221, #77946, #51542, #58804, #84767, #72019, #57928, #22988, #65634, #24312, #51979, #10663, #66068, #38368, #22533, #29347, #57482, #57026, #8914, #36613, #25188, #40150, #19718, #66974, #52850, #59694, #74685, #81530, #47406, #4755, #46955, #46511, #5658, #33350, #12022, #26537, #80622, #17928, #60593, #39269, #32439, #12466, #26095, #45604, #88336, #81079, #61049, #60139, #12921, #87429, #74247, #86987, #88780, #54209, #18371, #46056, #87874, #81970, #73792, #73336, #25637, #75135, #67871, #40609, #3862, #11578, #39704, #31554, #59257, #67412, #24747, #52416, #53313, #32000, #80180, #11109, #38818, #66523, #18829, #5202, #32896, #53764, #4312, #19282, #61940, #34684, #7885, #35578, #7438, #54654, #68775, #76932, #62393, #6106, #82420, #6541, #83753, #33798, #21982, #15154, #75593, #84211, #13805, #26988, #63295, #20625, #49198, #20181, #56465, #61492, #1072, #89224, #47856, #55106, #49649, #14710, #68326, #70111, #28784, #172, #77375, #27874, #13363, #21069, #48293, #14260, #82868, #34236, #41050, #89673, #42384, #83302, #27426, #76027, #41935, #41488, #69666, #69218, #6990, #55549, #48744, #76478, #614, #56003, #35127, #62838, #28311, #21529, #42830, #8339, #37832, #23766, #8800, #29671, #71023, #36498, #72355, #50550, #2868, #16940, #58264, #37380, #64202, #24202, #36037, #15609, #30565, #78740, #30120, #85994, #65527, #63753, #51870, #43735, #50997, #79623, #50097, #71473, #1974, #79182, #57365, #77832, #70566, #51434, #85105, #43282, #1532, #71910, #16495, #84655, #22875, #16055, #44174, #44619, #64634, #3311, #9668, #78292, #29234, #31002, #9234, #10122, #36933, #58696, #86436, #2420, #57818, #65085, #56920, #85553, #22423, #23331, #55341, #17382, #72793, #13584, #88229, #73222, #4198, #45497, #11000, #46844, #25080, #67304, #81425, #32790, #11911, #38702, #89911, #10558, #80068, #5092, #53199, #4643, #60480, #41271, #38263, #27663, #18265, #25528, #45066, #24637, #45943, #66407, #53654, #31892, #52304, #65959, #25984, #59582, #17823, #3751, #46401, #80969, #59143, #87318, #80509, #18718, #19173, #39159, #69001, #74137, #52745, #31439, #6769, #73682, #74574, #11462, #34469, #86875, #62174, #66864, #32330, #60029, #87764, #39597, #35810, #76711, #49430, #22657, #50330, #22208, #69451, #83529, #1759, #77166, #20850, #7227, #21299, #8572, #48516, #36727, #29912, #403, #9027, #28546, #41718, #78073, #35360, #63983, #34917, #71256, #76258, #15833, #14036, #62627, #69900, #64428, #29461, #83097, #84888, #43511, #14943, #2206, #42612, #28096, #63525, #63072, #29015, #7670, #48974, #55779, #14495, #57142, #8119, #42170, #851, #56699, #56237, #84443, #83987, #21760, #70344, #36272, #1307, #49882, #77611, #15392, #43061, #70800, #18052, #65747, #17176, #51665, #78964, #86662, #45730, #59376, #9459, #79413, #71696, #3097, #73458, #30356, #38488, #30794, #44859, #31228, #23993, #45296, #9914, #78523, #43961, #23554, #16280, #79863, #87108, #23115, #72588, #16725, #51219, #86216, #10352, #44403, #58486, #4435, #52098, #50787, #37619, #58053, #85783, #38058, #17617, #72139, #3982, #11235, #3533, #65318, #58923, #66188, #73016, #38939, #24436, #10785, #31680 ),
 ( #24876, #66646, #52542, #80303, #37167, #57600, #85343, #64875, #2659, #5329, #61616, #74368, #46182, #33023, #47980, #13046, #6228, #27113, #12141, #40282, #68901, #32122, #5782, #82552, #68453, #88455, #60269, #59819, #33919, #81651, #89352, #60718, #53889, #74816, #19401, #13485, #67545, #54787, #20311, #67999, #75715, #33473, #47082, #81203, #12593, #40729, #39828, #61176, #82102, #75269, #26212, #41170, #25760, #88904, #25313, #87552, #52980, #88000, #46636, #26656, #80741, #54336, #73916, #19850, #18494, #11698, #39391, #67097, #47536, #4878, #32569, #53436, #18955, #57042, #42959, #62967, #34816, #34361, #70693, #56132, #8471, #35257, #28448, #49330, #83887, #77962, #42068, #36169, #63885, #14844, #50228, #8015, #21660, #55674, #77064, #15287, #76611, #35710, #56599, #49779, #21200, #22111, #7571, #42512, #83425, #48872, #41612, #69348, #84786, #70240, #63422, #746, #27999, #1207, #22554, #1663, #48417, #28915, #20746, #69798, #15735, #7123, #77507, #84342, #29363, #43410, #6667, #62071, #14392, #27558, #82992, #62525, #55237, #89806, #76154, #13934, #300, #2554, #37065, #9805, #58389, #64769, #72035, #17943, #65650, #64329, #23456, #43864, #71597, #16621, #31126, #30254, #17510, #87002, #44302, #57945, #85679, #51995, #58825, #24765, #37515, #24327, #23890, #72912, #10680, #79309, #3878, #51123, #85237, #37950, #65214, #2990, #79754, #3434, #23006, #86562, #86117, #38385, #45191, #51562, #66088, #31569, #17067, #59274, #78864, #50682, #52434, #30691, #44753, #80196, #71153, #78422, #8931, #72480, #36629, #10246, #2100, #29810, #57500, #16184, #9358, #68343, #11595, #60155, #18848, #75152, #87892, #59712, #46529, #61506, #26552, #19741, #40627, #25655, #53782, #82438, #45622, #19298, #6125, #81986, #12036, #73810, #73356, #47425, #5220, #12938, #74264, #67430, #88354, #32912, #27006, #81099, #33816, #89241, #81547, #54674, #46969, #60611, #4773, #26113, #54224, #53329, #74704, #5677, #88799, #39721, #61067, #12486, #40167, #32457, #67887, #80640, #18388, #11127, #33367, #38834, #66540, #66990, #4329, #32015, #87446, #25204, #52866, #46073, #39285, #36054, #82884, #1090, #83317, #7455, #83772, #76495, #7898, #62410, #41067, #6557, #76043, #68790, #42401, #21997, #75611, #69685, #41506, #13822, #48765, #35144, #69238, #21087, #56934, #14728, #13380, #189, #20645, #48310, #55567, #70128, #7006, #56483, #63770, #14277, #34704, #27891, #28801, #35597, #1548, #41952, #62854, #630, #84228, #28329, #21543, #63314, #49667, #56023, #77392, #49215, #76947, #15168, #42845, #55122, #70584, #8357, #29249, #20199, #47872, #34256, #61957, #89692, #27444, #36513, #16510, #8816, #30136, #10574, #57380, #65543, #57832, #71923, #58279, #51014, #72369, #36945, #15625, #71041, #50566, #43297, #16955, #86451, #50112, #44188, #16072, #78308, #23347, #9688, #43751, #85569, #31455, #79198, #77849, #64651, #85123, #22890, #78756, #44636, #71488, #31020, #38279, #37396, #9250, #2438, #3326, #10137, #65975, #65099, #37846, #2882, #24218, #51883, #30581, #17398, #86011, #64217, #51447, #23783, #58710, #79639, #45080, #1987, #72807, #3766, #84672, #22436, #29686, #52760, #39611, #52319, #60960, #81874, #25097, #73699, #32343, #88688, #11475, #73236, #60046, #75043, #40058, #33257, #54117, #39173, #67317, #6018, #59160, #32801, #19624, #5565, #25539, #87334, #86888, #26444, #18731, #47311, #87777, #80985, #11923, #46414, #40514, #4658, #12830, #68235, #5106, #24653, #60496, #74149, #46857, #53214, #80083, #80524, #17837, #45515, #11016, #38720, #67776, #18277, #45962, #66876, #88243, #66423, #25999, #19186, #4212, #74589, #53668, #81435, #31906, #59598, #12368, #83658, #69573, #20978, #21430, #28682, #89129, #15061, #34593, #41837, #42735, #40957, #62297, #89574, #70023, #27334, #68679, #70475, #49103, #82776, #6447, #26886, #62746, #7347, #75497, #20537, #6890, #35037, #14618, #55461, #56371, #522, #41396, #54559, #21883, #84, #76832, #55009, #42290, #33707, #49552, #69125, #48204, #27781, #48652, #61398, #76383, #75939, #83214, #63201, #978, #28221, #20087, #34140, #7791, #14162, #82325, #47760, #61838, #35483, #13268, #77285, #13712, #55911, #84111, #43641, #56818, #3222, #50455, #79087, #84567, #86340 ),
 ( #71817, #64553, #85905, #78201, #29138, #22325, #64109, #50006, #30476, #10037, #63655, #57725, #29577, #1879, #36842, #85466, #57269, #9145, #44978, #2780, #30032, #30916, #9585, #15961, #1437, #24115, #71379, #23677, #85014, #58175, #17298, #51782, #2332, #22780, #23243, #50909, #8244, #78653, #16405, #44082, #37742, #65440, #37288, #77740, #8705, #16848, #64996, #35941, #15514, #36406, #51339, #43189, #79535, #70933, #44526, #72263, #58605, #31356, #67673, #24999, #53562, #59046, #60845, #65871, #39956, #10475, #3661, #59496, #26336, #81330, #19518, #74488, #12260, #39063, #5452, #66770, #88578, #25437, #52660, #18627, #87230, #38618, #33149, #54008, #19072, #87670, #45414, #10914, #46306, #72710, #74037, #81766, #38177, #86785, #80418, #17738, #4999, #60393, #18173, #24556, #66314, #52219, #79985, #73133, #4102, #46756, #31802, #45856, #73587, #11363, #4556, #32242, #32699, #59940, #88131, #67214, #53105, #80872, #11818, #39515, #25892, #83110, #34483, #34933, #42186, #12717, #28566, #48097, #55357, #56253, #54457, #75830, #13162, #83550, #40846, #82220, #84003, #62645, #6338, #19976, #40409, #76277, #20867, #89015, #34028, #20426, #48535, #28110, #47205, #14052, #7685, #21316, #13602, #75391, #74939, #48989, #6784, #76729, #41286, #69018, #89928, #62191, #68122, #82668, #14511, #69920, #41734, #870, #69469, #27678, #61732, #7244, #55796, #27224, #420, #35375, #63087, #89467, #5903, #33597, #61293, #54905, #26773, #47657, #68575, #73368, #29934, #71274, #15853, #43078, #50806, #11140, #24781, #63543, #43532, #35827, #57158, #38845, #84461, #3887, #84907, #9045, #85360, #78088, #9477, #64001, #42626, #8137, #77627, #70362, #43978, #52447, #77183, #36745, #70818, #15412, #50349, #64444, #8594, #22676, #59726, #16300, #14960, #1779, #22223, #49897, #2223, #71711, #36291, #59286, #66552, #57618, #29478, #23132, #31582, #37187, #4342, #78543, #66101, #87013, #80210, #17954, #45636, #32028, #21778, #1325, #49446, #29031, #56716, #68356, #19756, #39300, #54236, #74719, #89255, #53794, #6570, #81113, #67900, #80653, #27017, #20212, #53343, #12047, #60625, #54688, #39735, #11607, #88366, #13391, #6138, #61518, #82451, #67445, #5690, #34268, #47436, #75169, #32923, #47882, #25667, #87459, #25218, #52878, #75624, #33828, #18859, #74278, #46543, #5234, #41080, #26126, #12950, #68802, #40639, #81999, #81561, #18399, #46088, #60171, #73821, #33378, #12498, #67002, #4787, #32470, #87904, #19310, #61081, #46980, #40181, #88811, #26564, #8370, #55582, #69250, #8830, #77406, #21104, #7019, #55134, #1105, #7912, #13835, #48778, #35157, #63327, #42860, #83785, #84688, #28816, #69701, #27456, #50127, #62868, #49683, #83329, #22011, #71057, #77863, #7470, #76509, #644, #49228, #61968, #14745, #14293, #28344, #1561, #29262, #56498, #48321, #62424, #70598, #56038, #89707, #76056, #204, #15182, #82896, #15638, #20657, #34720, #43312, #21558, #41518, #56945, #41965, #36070, #27904, #76960, #42414, #22449, #70142, #35612, #84241, #63784, #17413, #73250, #38291, #65990, #2896, #3782, #30596, #24669, #79212, #16525, #72384, #23360, #2452, #31470, #59174, #45096, #51462, #9263, #64669, #10152, #36529, #37861, #80100, #64229, #17850, #51031, #71502, #9706, #24232, #57848, #86468, #45528, #52335, #44200, #85584, #37409, #23796, #2000, #16969, #30150, #58294, #86904, #29703, #65559, #22904, #36958, #72821, #86025, #57396, #50581, #78769, #51898, #85138, #78321, #16086, #43767, #71939, #65113, #44653, #3339, #31034, #10587, #58724, #79657, #4226, #68249, #38736, #31919, #87790, #54575, #81887, #47776, #12845, #40530, #67330, #6033, #5119, #89141, #53683, #81000, #46870, #25555, #66891, #33723, #61412, #19639, #26016, #73713, #39186, #74604, #11034, #12382, #82340, #66439, #20101, #53230, #45980, #33272, #88703, #46430, #26900, #4676, #59614, #87350, #25110, #52773, #47328, #32356, #18746, #60059, #74163, #80538, #11940, #60975, #75059, #26460, #5580, #39626, #18292, #11491, #32817, #54129, #40075, #88257, #60513, #81451, #19201, #67792, #76400, #83675, #56833, #82789, #14178, #41411, #21896, #69140, #20552, #22339, #995, #34609, #48218, #68693, #14631, #21448, #27349, #62313, #48668, #76848, #56387, #7360, #8258 ),
 ( #84127, #63215, #29150, #41851, #28700, #28233, #77299, #15074, #49116, #35958, #6906, #89592, #42305, #20991, #69590, #49567, #7804, #55025, #70038, #62761, #42748, #35051, #84580, #98, #55928, #6461, #70489, #63670, #27796, #55476, #536, #1453, #83226, #75953, #35496, #75511, #13282, #40973, #34153, #61855, #13726, #79548, #50017, #65009, #58617, #72278, #23255, #50471, #77752, #10048, #16418, #37755, #85479, #78668, #71829, #44092, #15529, #57740, #65453, #30929, #2793, #43203, #85920, #37303, #36854, #30491, #3235, #30046, #58188, #16861, #86355, #2344, #44541, #50922, #23690, #64565, #9596, #78213, #15975, #51797, #51354, #79099, #24125, #9156, #70947, #8720, #36421, #43655, #64122, #71394, #1892, #29590, #57282, #85025, #22795, #38098, #30839, #86702, #37659, #16768, #52582, #73505, #59419, #65789, #23598, #79000, #24479, #50832, #52141, #4476, #78570, #32165, #65357, #85828, #73054, #38535, #3574, #31271, #59859, #86253, #24918, #18089, #58965, #87591, #79903, #17658, #9955, #45334, #87152, #58528, #10830, #66230, #4019, #3139, #31722, #51705, #80340, #24035, #79455, #51257, #44448, #11277, #45778, #10393, #44898, #72179, #38982, #66690, #16322, #2697, #72628, #64912, #17219, #43999, #71735, #9504, #37211, #30394, #58092, #81690, #13084, #67590, #46224, #11737, #81246, #73959, #47572, #27152, #80790, #74858, #46680, #18997, #53932, #12633, #74410, #26254, #62113, #19891, #18538, #5368, #88045, #25808, #60765, #75306, #12185, #61651, #41208, #88500, #39869, #33064, #6262, #40771, #68935, #19439, #68495, #68040, #54824, #82590, #33515, #48019, #47123, #39435, #82142, #40320, #5827, #33952, #89390, #67138, #20348, #61216, #75757, #88938, #34404, #26691, #54372, #4918, #13526, #6704, #25349, #53021, #32608, #60309, #53480, #13972, #63005, #15772, #70737, #63920, #84822, #69837, #8053, #36663, #89846, #63462, #50263, #36207, #56175, #28037, #27597, #1697, #49370, #29401, #28486, #21697, #8965, #78003, #7610, #48910, #788, #77106, #55277, #42549, #83463, #83925, #57081, #22590, #28953, #76193, #338, #8510, #14883, #83035, #41652, #55716, #15325, #20789, #43449, #48454, #7167, #71190, #35293, #69389, #34857, #42111, #62563, #21239, #76648, #14434, #70276, #35748, #1246, #56635, #84382, #22152, #49818, #77544, #42996, #30730, #86152, #10284, #17983, #51600, #44342, #37989, #51159, #30287, #66126, #87046, #72950, #79348, #37106, #2592, #65686, #64366, #3473, #45664, #2142, #73396, #78900, #9396, #86598, #52037, #9848, #24810, #57984, #11167, #29848, #57536, #59312, #45229, #85718, #16658, #23494, #72076, #3915, #37552, #24369, #38425, #79797, #58862, #65253, #85276, #23045, #64809, #17552, #31164, #17110, #10721, #52476, #50722, #78460, #3029, #72523, #16220, #71632, #58425, #23927, #31611, #44794, #80234, #43898, #54269, #87929, #73846, #32060, #67930, #74748, #80678, #25696, #12078, #40209, #19784, #60651, #61551, #5717, #46569, #4371, #27049, #39763, #26592, #60196, #88840, #18431, #88391, #52907, #74306, #54719, #11633, #18886, #89286, #53373, #5258, #32953, #82034, #81137, #59755, #25244, #4814, #87487, #61110, #40668, #46117, #26151, #67475, #32500, #53820, #81588, #19339, #47015, #75653, #33411, #39325, #12525, #67034, #47468, #75199, #12980, #68389, #6166, #82484, #33855, #20238, #47911, #38873, #66577, #56981, #14324, #56528, #56067, #15216, #42892, #21590, #36101, #34750, #27487, #70170, #48804, #42000, #84274, #35644, #55162, #7945, #677, #70627, #69732, #22485, #7055, #83815, #6601, #8405, #63815, #69281, #27934, #76539, #1594, #55611, #82924, #7502, #29297, #22046, #77439, #84723, #83364, #49261, #50159, #13423, #76996, #41107, #49716, #35187, #41545, #68834, #34296, #62897, #62003, #28381, #14778, #42445, #63356, #89738, #1136, #20685, #48353, #28845, #76088, #13865, #62456, #230, #21133, #86495, #57881, #79242, #37890, #31060, #2484, #3371, #78797, #23823, #64705, #36998, #22937, #50614, #38322, #86053, #37442, #71974, #9295, #17002, #66020, #79690, #31497, #15669, #59205, #30182, #78356, #10181, #65588, #23394, #3811, #16118, #24701, #77892, #43346, #72849, #58754, #43795, #85615, #71533, #51059, #17443, #16554, #24260, #51930, #45125, #72417, #44235, #86939, #71088 ),
 ( #9738, #85166, #8863, #10617, #65143, #2926, #36560, #44686, #51492, #29744, #30628, #58326, #64262, #2036, #57430, #75084, #53712, #60089, #17879, #40560, #25589, #40103, #73739, #12413, #61438, #68280, #87825, #11522, #53262, #39659, #89168, #5150, #46006, #18777, #81920, #19673, #6061, #81479, #67359, #39217, #32847, #61001, #32387, #19230, #67819, #5610, #66929, #33303, #81031, #88289, #4709, #46460, #87380, #25139, #12874, #60542, #11975, #74197, #26045, #46906, #33749, #54158, #4258, #74636, #66467, #88730, #52367, #52799, #26485, #80129, #47355, #45556, #73286, #11062, #38764, #31954, #59648, #18325, #80573, #49145, #28728, #82366, #76425, #48248, #82817, #20130, #69168, #89622, #27377, #62345, #76882, #75980, #63250, #42777, #125, #13753, #20581, #7831, #14663, #70520, #27825, #70063, #69620, #56414, #84158, #35079, #49601, #41438, #41000, #83701, #55503, #83256, #35526, #42333, #68720, #21472, #14204, #21932, #21017, #35987, #6939, #7388, #47804, #77327, #15102, #34641, #48695, #41884, #8291, #62786, #6486, #563, #63700, #1025, #26938, #54606, #28262, #55957, #75541, #13314, #34184, #61890, #55056, #57770, #29623, #29181, #37784, #50952, #3269, #30076, #23289, #44123, #78697, #72748, #65483, #16896, #56869, #30960, #45020, #2822, #16446, #50503, #71862, #10080, #71424, #30519, #51381, #44575, #16006, #72307, #2376, #37333, #78249, #43687, #36449, #64154, #51828, #9627, #65038, #85511, #22825, #58221, #79579, #58647, #43234, #85950, #15561, #36886, #17340, #1927, #9189, #24158, #64595, #23721, #79130, #86382, #10517, #22369, #77783, #57311, #50046, #38222, #1481, #84611, #70976, #8749, #85058, #4601, #53153, #31847, #66816, #12765, #60438, #87274, #25938, #74981, #54054, #73633, #25040, #32285, #80922, #65915, #18670, #45457, #73177, #19119, #80463, #5044, #52260, #66360, #74533, #59983, #3702, #80025, #4147, #81374, #31395, #19564, #59092, #10955, #81813, #11409, #24597, #60898, #18222, #46800, #17779, #47252, #86828, #33197, #38660, #59540, #52703, #45902, #12309, #39107, #67717, #5503, #87713, #25482, #11865, #46351, #74082, #39557, #67260, #32742, #88182, #88627, #26381, #40002, #53608, #13211, #68621, #76322, #40454, #14101, #85285, #68174, #23059, #54949, #75440, #62692, #28163, #75880, #2151, #6385, #78469, #5956, #33645, #36672, #21367, #34074, #27274, #61779, #89518, #71199, #48145, #469, #14563, #55850, #34979, #82716, #50733, #61336, #40894, #83600, #41782, #27726, #49041, #64376, #89063, #26822, #41334, #48589, #54503, #47700, #69063, #20477, #76775, #13652, #6833, #82266, #42237, #34536, #62239, #20024, #69518, #7294, #26, #55405, #83160, #8975, #29860, #20918, #57544, #17561, #23937, #71642, #4383, #79362, #3926, #10296, #37563, #45241, #32070, #17994, #57997, #38003, #30300, #51613, #59766, #78910, #86163, #38884, #30741, #72533, #65695, #31622, #58433, #37118, #2601, #72085, #64819, #38433, #45675, #9406, #3480, #65263, #9858, #44805, #31174, #3043, #17120, #52921, #10729, #85730, #58873, #16669, #44356, #86608, #66139, #24382, #52486, #87496, #52045, #79807, #72961, #87055, #59326, #25254, #24821, #80247, #73408, #11180, #66588, #16232, #43907, #23505, #51169, #47479, #26164, #19351, #61561, #12992, #32508, #75211, #67942, #82495, #47024, #89750, #74319, #61122, #73858, #20252, #13434, #46580, #5271, #53832, #47923, #32968, #4824, #81601, #6614, #89298, #54732, #75664, #60663, #88851, #27499, #80692, #54281, #41119, #27062, #74759, #18897, #18442, #68844, #40223, #34311, #12537, #5729, #33421, #26603, #62016, #46129, #6178, #11644, #39338, #67045, #82045, #19798, #39772, #40678, #60208, #88401, #68399, #33865, #87944, #25709, #53383, #81150, #12087, #67485, #14337, #243, #27947, #15685, #63370, #14790, #21147, #69744, #28393, #84737, #7513, #69296, #56081, #71102, #36114, #29311, #50170, #35201, #1152, #2050, #55175, #28857, #43357, #1607, #21603, #83374, #82937, #56994, #42457, #22496, #83830, #77008, #7958, #70184, #36574, #77908, #70643, #20697, #8876, #64278, #56543, #35656, #42015, #84287, #63828, #62911, #22059, #15229, #8419, #689, #48364, #49277, #49729, #77451, #42906, #55623, #48819, #76099, #13878, #41560, #7067, #76555, #34763, #62467, #31516 ),
 ( #85628, #78368, #51945, #59222, #85182, #79255, #51072, #23404, #58338, #17017, #78812, #30640, #66485, #24279, #22954, #71984, #2500, #30198, #65155, #79703, #16570, #66035, #45572, #2938, #44250, #9754, #10632, #17457, #73300, #86067, #72863, #72428, #86951, #24715, #37901, #52379, #37457, #43809, #86509, #23838, #51507, #38335, #45137, #71548, #3824, #44700, #80143, #10194, #38779, #65602, #3384, #50627, #17893, #11074, #9310, #31076, #29756, #57893, #58770, #57441, #16131, #37011, #64716, #81935, #46476, #25152, #80589, #60105, #52815, #26502, #6074, #59660, #53728, #25603, #87841, #32860, #81493, #53278, #5166, #41014, #88744, #87392, #74213, #66940, #4723, #39674, #54175, #81047, #40575, #20146, #67376, #18792, #11988, #75099, #19689, #47818, #60558, #47369, #46920, #33763, #61455, #12428, #26953, #88303, #18336, #61016, #26060, #19247, #12888, #68294, #46022, #89188, #74653, #54621, #40117, #13326, #67835, #5627, #73756, #82381, #75558, #33316, #4273, #31967, #11537, #39233, #32402, #41898, #84625, #49615, #42794, #63716, #48710, #76895, #15577, #68736, #42347, #29200, #15118, #35093, #6953, #6505, #70536, #28278, #8304, #7402, #579, #21489, #55972, #50063, #36002, #84174, #34203, #1496, #22385, #70077, #83714, #27838, #49164, #77341, #76439, #7847, #28745, #21945, #83269, #56881, #69632, #14678, #55517, #21034, #13769, #41454, #77798, #35544, #63263, #62800, #139, #1037, #61904, #89637, #20594, #56431, #69183, #27391, #55069, #14222, #82832, #34655, #48260, #75994, #62357, #38236, #24175, #9206, #30090, #71439, #36899, #72763, #50967, #3282, #17355, #58663, #37799, #64608, #24612, #8763, #16021, #30975, #79150, #30536, #86401, #65931, #36464, #52276, #44140, #51398, #80040, #50520, #71878, #2392, #79595, #57785, #78263, #43248, #51841, #85528, #43702, #64170, #72324, #16911, #85073, #23302, #16461, #44588, #45035, #65055, #3718, #10095, #78710, #1940, #31409, #9642, #10533, #37349, #59111, #70991, #86844, #2838, #58236, #85964, #23735, #29637, #65499, #22839, #57328, #60917, #32301, #46814, #4167, #18239, #26401, #74102, #45473, #31863, #45917, #33216, #73193, #61353, #54522, #25054, #33663, #53170, #66376, #12783, #59999, #88644, #59554, #5974, #10972, #74999, #38674, #87290, #4616, #89082, #54074, #17793, #19581, #47273, #11882, #39570, #53624, #26839, #5061, #87730, #81391, #25502, #73647, #40475, #68192, #81828, #32761, #80481, #11427, #19141, #52718, #74547, #39129, #66831, #80939, #18686, #46368, #67277, #60456, #88198, #25957, #12327, #40020, #67735, #5523, #48605, #14120, #28177, #35898, #69533, #62256, #55867, #69086, #48164, #84069, #15017, #939, #7310, #54967, #20498, #83618, #82286, #21385, #63610, #20042, #1391, #6850, #27293, #14578, #69981, #27741, #42691, #75898, #29095, #47719, #75459, #77247, #63157, #13666, #34551, #41352, #42, #21841, #55424, #42253, #56322, #7750, #76791, #83175, #13228, #40914, #82734, #35441, #49059, #34995, #28636, #70432, #68637, #6402, #20933, #486, #34095, #89536, #76342, #41796, #49511, #62707, #8205, #61799, #72219, #15917, #1841, #49960, #85863, #2736, #8658, #43594, #29993, #58131, #37699, #78606, #79491, #23633, #64509, #22285, #44933, #57683, #44487, #78157, #16805, #65825, #72663, #2289, #71333, #85426, #44038, #3610, #9544, #36356, #64066, #9990, #9104, #51293, #43147, #57224, #65398, #23201, #84527, #70888, #84969, #3178, #77694, #10430, #56779, #29539, #38132, #50868, #15478, #51741, #36801, #30876, #22739, #50414, #16360, #71773, #58561, #37249, #64952, #30436, #79040, #86291, #24071, #17253, #86739, #80827, #52616, #87186, #59894, #18576, #24950, #32198, #68075, #25846, #24510, #73540, #4057, #31756, #66725, #81280, #80378, #67624, #47159, #4510, #18127, #45811, #12219, #19026, #74892, #87627, #74443, #73992, #33103, #60800, #39468, #53964, #11314, #45372, #88083, #25391, #53057, #39907, #53512, #73092, #46713, #46256, #88533, #11771, #40361, #39015, #67170, #52174, #26287, #81724, #4953, #32649, #60345, #19476, #5408, #10870, #12670, #31305, #59001, #79937, #17693, #38568, #66266, #59452, #42580, #69422, #56207, #42141, #62147, #33986, #33547, #69869, #55312, #7641, #34438, #27631, #48487, #83068, #77137, #35330, #21269 ),
 ( #41687, #82624, #54859, #40805, #68527, #83958, #14003, #20822, #89880, #27184, #34887, #21729, #63042, #47609, #76229, #19928, #41241, #49401, #6295, #75790, #28514, #20385, #7197, #28068, #83498, #68972, #14914, #61688, #5862, #61249, #88971, #824, #76684, #89423, #48055, #13556, #6739, #26727, #62597, #55751, #54410, #48942, #373, #14464, #82173, #75342, #13121, #30329, #16255, #57569, #58021, #65290, #35780, #51639, #71225, #78495, #79383, #77580, #8997, #36242, #16697, #63952, #15365, #17145, #85757, #29432, #43030, #63494, #9431, #43930, #22182, #57112, #43480, #71668, #51191, #2177, #3066, #37142, #78040, #1279, #58457, #36698, #23529, #1731, #78932, #70315, #86187, #15808, #84858, #64399, #85313, #8090, #23086, #49851, #70772, #44379, #22627, #64843, #56670, #8544, #72108, #29886, #28984, #84414, #50300, #9882, #50760, #23962, #2627, #37589, #30767, #80276, #3502, #41025, #87079, #26966, #31199, #34213, #38028, #13340, #72557, #65720, #31650, #89650, #54631, #82843, #47832, #75570, #11206, #66616, #80716, #27400, #32094, #24845, #18465, #59350, #10754, #68746, #6517, #82395, #59790, #17587, #72986, #46154, #44829, #73883, #55080, #10324, #58895, #52511, #79831, #4407, #38906, #66163, #11670, #61917, #86633, #24407, #87522, #52071, #18019, #45270, #38459, #45702, #3949, #73433, #25283, #52948, #33771, #39363, #67069, #6084, #61466, #89200, #20157, #70545, #48268, #21505, #48720, #21047, #589, #49175, #76453, #28291, #50076, #1048, #13779, #69645, #27850, #55526, #35105, #56443, #14237, #15128, #29212, #62812, #41913, #7413, #49626, #84187, #84634, #55982, #21960, #76909, #8316, #36015, #42358, #63728, #83726, #6969, #63273, #14688, #70086, #77350, #28758, #34663, #42807, #7857, #1510, #35557, #22394, #56896, #20603, #41465, #76002, #69194, #62368, #150, #83278, #41314, #54032, #25921, #74960, #27704, #82693, #75857, #6808, #81791, #20002, #48567, #11845, #75417, #62219, #48123, #68151, #39983, #39539, #13629, #61318, #69043, #40433, #33625, #54483, #89040, #83137, #34511, #27254, #67242, #4, #55381, #13191, #26802, #60876, #82246, #20453, #19544, #40874, #61758, #54929, #26363, #20895, #12744, #47682, #88607, #47233, #46782, #74513, #5026, #68602, #32724, #60417, #88162, #67698, #5935, #6363, #53589, #34054, #81358, #89493, #19097, #12293, #5481, #33178, #56282, #84489, #23159, #76303, #49920, #36766, #22699, #42650, #14536, #14074, #50370, #35854, #78117, #14981, #8164, #29056, #63572, #57639, #15880, #1804, #41760, #43558, #29955, #77655, #1353, #35399, #56745, #84932, #84027, #15436, #36317, #29502, #899, #57185, #77210, #22250, #63117, #28593, #21342, #49016, #64468, #43104, #70849, #70389, #7709, #8621, #2251, #71298, #28137, #64027, #444, #21804, #85384, #76752, #49473, #9066, #69494, #7271, #34957, #62668, #55828, #83578, #42215, #69942, #85844, #37226, #2717, #10411, #64491, #38114, #18109, #2268, #45793, #79021, #9523, #86720, #52156, #9973, #24933, #30415, #11294, #29970, #57661, #59436, #45353, #58112, #51274, #23616, #16785, #4038, #72198, #24494, #38551, #79920, #58980, #44466, #73519, #85406, #64931, #17674, #65805, #51721, #73073, #87167, #23181, #50849, #65378, #72645, #78588, #71756, #3158, #37678, #10851, #16340, #44018, #52597, #66246, #30855, #58545, #86274, #24053, #31739, #79475, #80358, #17235, #44914, #3594, #31287, #20363, #4493, #11753, #88952, #74873, #26269, #26705, #33966, #32178, #48036, #39887, #47140, #75770, #46239, #67605, #4934, #75322, #32629, #73974, #38997, #54391, #88062, #39450, #59874, #68057, #12648, #80805, #25826, #12199, #40339, #19905, #60780, #61669, #5841, #46694, #87607, #27164, #5384, #82156, #60327, #47587, #66706, #54839, #74425, #53496, #33083, #53945, #25371, #81704, #18556, #67152, #13102, #81262, #33530, #53039, #19011, #40785, #88515, #19456, #61230, #68508, #6275, #89406, #82604, #50276, #20801, #29413, #48922, #62127, #8523, #55729, #84395, #89860, #1710, #6720, #70748, #41222, #34418, #353, #57091, #22162, #13538, #15341, #43010, #69850, #35307, #49382, #84834, #802, #83478, #77117, #28050, #69404, #21252, #63020, #8068, #34868, #76209, #41665, #14894, #68952, #42558, #22604, #27610, #55292, #76664, #48466 ),
 ( #14447, #7179, #62576, #36221, #42123, #63472, #77556, #28965, #35759, #7621, #83050, #13985, #28496, #1259, #70291, #56187, #56647, #63931, #83940, #21710, #49829, #86166, #59329, #85289, #16673, #43911, #24385, #71646, #23063, #24823, #3482, #37121, #50736, #71202, #17123, #23940, #29863, #64822, #51172, #79365, #58875, #9861, #10731, #44809, #85733, #43461, #66141, #78913, #65699, #9409, #38006, #87057, #3928, #23508, #2604, #44359, #65267, #78017, #30744, #57547, #78472, #31176, #30305, #72536, #64379, #16235, #86611, #72088, #15785, #2154, #58000, #52048, #8978, #31625, #36677, #37567, #3046, #58437, #51617, #72964, #10300, #79809, #17563, #45244, #38435, #19800, #80251, #73410, #39340, #6180, #33423, #89300, #54283, #82047, #18899, #74321, #88404, #33868, #39774, #32510, #26166, #67047, #18444, #60211, #12090, #47026, #73861, #25257, #80694, #53834, #52488, #81604, #61564, #17996, #45677, #4827, #87499, #74761, #40226, #87946, #47481, #25711, #12539, #26607, #67944, #5732, #11647, #11182, #38886, #52923, #61124, #19354, #67487, #88853, #75214, #66592, #4385, #53385, #60665, #32072, #59768, #81153, #46131, #12995, #46583, #5274, #32970, #40681, #68401, #62018, #20256, #56083, #62914, #68846, #76101, #246, #28395, #7960, #48821, #49731, #83832, #34766, #82497, #15232, #27949, #14792, #48367, #77011, #36116, #42908, #62470, #13880, #55626, #14339, #63831, #69746, #6617, #34313, #70188, #41563, #21606, #13436, #27502, #35658, #83376, #54734, #41122, #55179, #42459, #47926, #70645, #27064, #89752, #8421, #21149, #75666, #22061, #69298, #63372, #82939, #20699, #7069, #84290, #76558, #42018, #7515, #35204, #1154, #691, #28859, #56547, #49280, #77454, #37459, #45140, #78814, #71551, #65158, #78371, #57443, #9313, #51074, #86069, #22956, #64280, #29758, #2941, #1611, #30643, #72865, #29313, #10634, #16134, #36577, #23841, #79257, #37013, #51947, #85185, #38339, #56996, #84739, #86512, #72430, #50629, #43811, #64718, #2502, #30201, #15687, #57895, #17460, #10198, #65604, #24281, #85631, #9756, #22498, #50173, #58340, #79705, #37904, #23407, #16574, #77910, #3386, #44252, #31079, #71986, #51510, #17019, #44702, #43359, #58772, #71105, #8879, #2053, #19691, #67379, #81049, #25154, #46479, #74657, #46024, #5168, #26063, #19249, #80591, #81497, #66943, #11990, #52819, #18338, #11076, #38781, #26505, #74216, #25605, #60109, #87394, #32862, #54177, #67838, #17895, #87843, #80145, #11541, #81940, #66488, #73758, #88747, #39236, #32404, #53280, #53731, #4725, #86953, #47371, #18795, #39676, #75102, #5629, #31519, #60561, #88305, #31969, #46922, #12430, #59663, #40119, #12890, #33319, #59224, #61019, #4276, #66037, #3826, #24718, #52382, #45575, #73302, #13773, #89640, #6508, #21493, #28282, #85421, #41457, #83716, #83271, #42349, #70079, #48712, #64505, #61907, #54623, #7404, #75996, #69185, #49166, #62802, #82384, #35095, #27840, #7849, #6957, #50864, #34205, #21038, #33765, #35547, #2283, #27393, #55072, #34657, #29988, #57677, #23198, #41901, #55519, #82835, #76442, #76898, #20596, #69635, #581, #14681, #48262, #55974, #62360, #14225, #142, #78602, #75561, #13329, #40578, #68296, #6076, #61458, #89192, #26956, #20148, #47821, #41016, #68738, #30431, #51736, #32193, #79035, #86286, #39010, #30872, #72657, #10425, #4052, #58558, #37243, #87620, #38128, #52169, #4505, #18122, #71769, #65821, #37693, #72215, #44929, #3605, #9986, #17248, #53053, #10865, #9539, #24066, #16800, #44482, #79487, #66261, #65392, #52609, #59888, #31299, #3174, #58995, #87180, #31752, #25385, #86735, #59448, #24506, #45807, #73534, #79932, #66721, #17687, #58126, #73087, #45367, #38562, #24946, #80373, #85860, #11310, #16355, #44033, #64948, #2730, #23629, #51288, #73988, #82618, #13551, #46709, #5402, #53959, #20379, #33099, #4948, #81719, #6735, #61683, #54855, #75786, #60796, #88966, #27625, #80822, #54405, #41237, #27179, #47155, #19022, #18571, #48051, #40356, #68967, #19471, #12664, #33543, #68071, #62143, #34433, #6290, #46252, #5858, #74888, #12214, #19923, #89876, #11767, #32642, #61245, #60340, #26283, #39464, #53508, #88529, #67165, #26722, #82169, #47603, #68522, #75338, #88078, #25842, #13117, #40801, #81276 ),
 ( #33981, #89419, #39903, #74438, #67618, #28509, #14460, #21265, #36238, #43026, #8994, #56203, #8539, #8085, #57107, #84853, #63489, #78036, #76680, #69418, #22178, #819, #83954, #63948, #77573, #7193, #49846, #42573, #22620, #21725, #64394, #48938, #35776, #48482, #50295, #15804, #42137, #69865, #49397, #43475, #7635, #34883, #77133, #71221, #1727, #29428, #36694, #35324, #1275, #2172, #55307, #28980, #83064, #20817, #14910, #83492, #76224, #13999, #70309, #41682, #56666, #84410, #15359, #70768, #62591, #368, #28064, #55747, #63037, #73427, #31194, #44825, #78928, #10319, #38453, #9878, #58890, #79827, #72982, #44374, #45265, #30763, #65716, #16692, #72104, #64839, #2621, #58017, #58452, #38024, #11202, #37137, #86182, #85753, #66158, #23524, #30324, #66612, #10749, #37583, #51187, #23082, #86629, #3496, #71663, #65285, #3062, #24403, #3945, #51634, #52505, #52067, #23957, #85308, #18014, #79379, #17581, #17141, #31646, #38902, #45697, #72551, #59346, #87075, #24841, #29881, #80271, #9426, #57563, #50756, #78489, #16251, #43926, #4845, #13009, #60683, #32090, #80711, #32527, #19816, #59786, #47940, #41136, #11666, #20274, #39788, #52943, #12106, #40244, #82512, #60233, #75681, #87516, #61578, #25277, #18460, #81170, #13449, #75233, #4402, #6195, #33882, #88420, #26182, #67962, #46150, #81619, #74335, #5748, #18916, #87965, #67503, #53850, #88867, #25728, #67065, #53402, #33438, #73879, #61142, #39359, #46602, #5294, #32985, #19369, #26623, #82065, #47043, #54748, #74778, #12556, #54298, #47496, #89315, #40696, #68418, #27079, #7086, #34780, #8434, #76575, #28875, #42922, #84307, #63388, #264, #50191, #34328, #41578, #56564, #14807, #56098, #22078, #63845, #62034, #77926, #42034, #70205, #49743, #706, #1628, #7975, #14356, #89768, #57008, #69761, #77467, #27962, #15248, #15700, #84750, #7532, #55640, #35221, #83846, #68859, #21623, #48381, #76115, #70660, #83389, #35675, #55197, #69312, #36132, #62928, #6631, #82955, #62485, #29328, #27518, #22511, #20712, #13895, #21165, #28412, #48835, #49296, #42473, #77029, #1170, #31535, #36593, #10644, #71117, #64294, #30216, #86968, #24294, #80159, #45153, #72877, #9769, #65174, #79272, #24729, #30656, #23420, #17034, #57908, #9323, #51087, #2954, #37916, #64731, #16148, #71562, #44714, #43374, #72442, #52393, #8892, #2066, #85643, #78385, #65615, #31089, #78824, #3839, #37025, #29770, #57460, #85202, #38349, #51960, #2515, #16586, #44264, #72001, #66048, #37472, #3396, #17471, #58782, #86527, #58353, #22969, #50644, #43823, #79716, #10210, #86080, #59238, #23852, #51523, #89204, #18808, #26076, #26970, #25166, #46490, #73770, #54189, #11557, #52830, #54637, #33332, #66957, #80603, #11091, #46936, #53741, #59675, #4737, #61471, #32416, #18352, #40132, #5640, #53295, #68305, #46038, #17906, #45586, #73316, #12901, #88758, #39249, #60121, #87855, #25620, #47384, #81061, #67853, #81952, #61029, #12444, #74229, #38796, #66502, #12004, #26517, #81511, #5182, #19700, #40590, #4291, #31981, #39687, #19263, #87406, #67390, #32876, #60576, #75116, #88317, #74667, #6089, #33776, #41469, #27405, #75574, #21510, #28295, #34217, #69200, #55531, #83732, #63278, #14241, #15134, #49179, #154, #47836, #70550, #83283, #70091, #13783, #42363, #1514, #8322, #27854, #6973, #21052, #69649, #29216, #35110, #61922, #89654, #35561, #34667, #76913, #68751, #82847, #1055, #48724, #20161, #6521, #20607, #7862, #13344, #36020, #82400, #55084, #63732, #76459, #41031, #41917, #55987, #48273, #76008, #62373, #7418, #49631, #62817, #595, #14692, #28763, #56447, #84192, #21964, #77356, #42811, #78723, #2852, #10547, #44154, #36915, #30551, #43716, #22856, #64619, #16477, #51414, #78276, #29650, #85086, #58250, #56902, #85979, #38250, #84639, #16038, #30104, #23748, #37816, #71895, #79609, #79166, #2405, #22400, #45050, #57801, #44603, #71456, #16927, #65946, #72780, #85538, #9219, #23316, #9654, #3734, #37363, #36479, #64184, #10108, #50982, #72340, #43265, #57345, #65512, #65070, #50080, #71005, #50533, #3297, #77814, #15592, #8779, #1956, #30989, #58676, #86421, #24188, #51857, #17368, #59570, #19596, #24624, #88659, #59126, #52292, #18253, #75013, #12342, #68207, #33233 ),
 ( #86863, #80957, #52733, #87305, #60013, #18702, #25069, #32317, #31426, #25973, #80054, #73664, #4184, #31880, #66851, #81412, #80493, #67752, #47288, #4631, #45931, #11447, #40034, #19159, #12803, #87747, #74561, #74120, #60932, #26421, #39585, #54091, #39144, #45486, #88216, #25516, #53186, #5540, #53638, #73207, #46833, #46386, #81847, #11900, #40491, #67291, #5074, #17810, #10988, #38688, #32778, #60470, #66393, #35457, #48180, #20058, #69101, #49077, #20514, #35011, #82301, #6420, #14593, #62273, #33678, #47738, #34111, #21404, #61374, #49529, #42709, #13244, #21860, #41369, #54536, #13680, #41814, #84088, #61817, #77264, #89098, #63174, #26856, #75473, #82752, #15035, #76809, #5990, #7769, #955, #56, #27759, #69549, #40930, #83191, #75913, #7326, #6867, #89550, #34567, #55439, #502, #27309, #68653, #54981, #62725, #20948, #28193, #48619, #76360, #14136, #55882, #83633, #42270, #69997, #28653, #56344, #8677, #17275, #70448, #35914, #65419, #51316, #36379, #57243, #64085, #1860, #10011, #78179, #30456, #44507, #85882, #64971, #29558, #51763, #63627, #43165, #58153, #16383, #57703, #23650, #3201, #1413, #79512, #71356, #78626, #8223, #77713, #9123, #84987, #16825, #22760, #15495, #29113, #79059, #50433, #70907, #56797, #9563, #44058, #22303, #15937, #43613, #71792, #72239, #2309, #30895, #37269, #36822, #84544, #58580, #64529, #37723, #30011, #86314, #49977, #24091, #85446, #23221, #50887, #2759, #82977, #87651, #24532, #52197, #72688, #31329, #73114, #60368, #10453, #89786, #44953, #79959, #62052, #80399, #3630, #52639, #80851, #34345, #10890, #27540, #38154, #13468, #65846, #59023, #31780, #55220, #27097, #86762, #47963, #75700, #11340, #66748, #18599, #17718, #32221, #24972, #46283, #59474, #38589, #18149, #4532, #39493, #66293, #45393, #4078, #74015, #87209, #11796, #45832, #73562, #39038, #59915, #25413, #67192, #32674, #53080, #6651, #4974, #89335, #54765, #82535, #41153, #20295, #68881, #7555, #48856, #76593, #50210, #28431, #70676, #84766, #36150, #15267, #42052, #2082, #76133, #83408, #8451, #56581, #7995, #63866, #15716, #13917, #29787, #21643, #28897, #57481, #27983, #49313, #14375, #57025, #69779, #55657, #20730, #1646, #35240, #21184, #41596, #49760, #84324, #62507, #62948, #83867, #22095, #29346, #42494, #43393, #77487, #56115, #69329, #8913, #77046, #22532, #724, #77945, #48400, #36612, #14826, #70222, #35692, #63405, #7106, #1187, #285, #42942, #71134, #64312, #34798, #71580, #85660, #3861, #51541, #44281, #30234, #78403, #24311, #31106, #37043, #72018, #58371, #86546, #66067, #17050, #17927, #51978, #2972, #50662, #73335, #86098, #72897, #16603, #45173, #4311, #11108, #30673, #9785, #23871, #72462, #31999, #37934, #64748, #2535, #38367, #37493, #79735, #9339, #23438, #31553, #79290, #22987, #57927, #51104, #10662, #16165, #38817, #85220, #78845, #66522, #44731, #43844, #10229, #58803, #65195, #65633, #3417, #17493, #52415, #59256, #86986, #24746, #80179, #45603, #6540, #61491, #89223, #26094, #81529, #5657, #13362, #46954, #39703, #33349, #46510, #25636, #67411, #19281, #54208, #81078, #32438, #87873, #61048, #59693, #88779, #41049, #87428, #68774, #74246, #4754, #81969, #47405, #5201, #20180, #53312, #25187, #52849, #80621, #54653, #40608, #18828, #12021, #32895, #60592, #26987, #88335, #19717, #33797, #75134, #12920, #53763, #18370, #46055, #60138, #68325, #26536, #74684, #6105, #82419, #73791, #11577, #12465, #67870, #39268, #66973, #40149, #47855, #75592, #27873, #41487, #71022, #49648, #7437, #50096, #15153, #8338, #29233, #14259, #42383, #34235, #61939, #7884, #84654, #70565, #613, #62392, #89672, #36036, #83752, #63752, #62837, #56002, #76931, #21528, #15608, #1531, #77374, #27425, #56919, #77831, #35577, #49197, #83301, #14709, #42829, #41934, #63294, #84210, #22422, #48743, #43281, #35126, #70110, #21068, #76477, #55105, #69665, #82867, #34683, #1071, #28310, #55548, #28783, #20624, #48292, #76026, #56464, #13804, #21981, #69217, #6989, #171, #31438, #23330, #65084, #2867, #86435, #50996, #29670, #80067, #30564, #44618, #86874, #10557, #64201, #58263, #30119, #64633, #37379, #85993, #2419, #9667, #45496, #3310, #1973, #78739, #71472, #9233, #44173 ),
 ( #16939, #59142, #57817, #22874, #65526, #71909, #23765, #79622, #31001, #50549, #58695, #51433, #38262, #79181, #17822, #85552, #72354, #57364, #65958, #24636, #16494, #10121, #37831, #3750, #24201, #78291, #51869, #17381, #52303, #36932, #8799, #36497, #85104, #16054, #45065, #72792, #43734, #45942, #73681, #60943, #60028, #19172, #5552, #46843, #53653, #11461, #75026, #10999, #80508, #74573, #32789, #11910, #12356, #88675, #38701, #12818, #53198, #5091, #47301, #52744, #80968, #39158, #67762, #66863, #18264, #73221, #33245, #32329, #4642, #31891, #81424, #25983, #87763, #25527, #18717, #40046, #26433, #39596, #19611, #54104, #46400, #59581, #66406, #74136, #81858, #67303, #4197, #87317, #25079, #60479, #88228, #41466, #34214, #14689, #89651, #42359, #83727, #33773, #7858, #21961, #69646, #83279, #27401, #48721, #76910, #48270, #7414, #28292, #21506, #82844, #49176, #69195, #14238, #55081, #20604, #56444, #76004, #61467, #68747, #27851, #62369, #13780, #35106, #84188, #70088, #20158, #151, #82396, #6970, #49627, #41028, #34664, #1050, #55528, #21049, #76454, #55984, #41914, #89201, #77352, #62814, #590, #15129, #35558, #26967, #63274, #28759, #61918, #68302, #6086, #54632, #47833, #75571, #13341, #6518, #8775, #80393, #64180, #18141, #59466, #8317, #73554, #87643, #45387, #59016, #1953, #24523, #52632, #22851, #73107, #4071, #87200, #57340, #24964, #43713, #79952, #29646, #85082, #32212, #50530, #36017, #43261, #3623, #38147, #78273, #10883, #59909, #45824, #84636, #65840, #56898, #16034, #25405, #15587, #71452, #66741, #10445, #31321, #86754, #31772, #52189, #63729, #53071, #17709, #38581, #80841, #11331, #1511, #66283, #39030, #36476, #4524, #42808, #70546, #29213, #22395, #50077, #77810, #71002, #81298, #19041, #53979, #68540, #39920, #54872, #34451, #81739, #67639, #74457, #89435, #6309, #62159, #19489, #61702, #61264, #20399, #48069, #26744, #41257, #5423, #32664, #75356, #47172, #74905, #27196, #40818, #60359, #13135, #5876, #75803, #12686, #27645, #12233, #88985, #11787, #13568, #68985, #33118, #60814, #40376, #6753, #88547, #88099, #68090, #89893, #82639, #55326, #18590, #26304, #54423, #46273, #74007, #82186, #39483, #67184, #33561, #46729, #4967, #25860, #19942, #53526, #47624, #34001, #28998, #69881, #48956, #836, #42593, #77594, #14477, #55764, #21282, #56683, #83082, #84426, #36710, #20834, #64409, #7654, #28080, #15377, #70785, #28525, #43494, #76697, #29896, #48501, #76244, #78056, #63967, #42153, #35342, #63056, #56220, #22640, #83971, #43044, #57124, #8556, #36256, #21744, #2190, #14016, #83510, #1744, #22193, #70329, #29443, #15819, #41702, #69435, #49413, #1292, #7211, #386, #77149, #14925, #84871, #8104, #35791, #34899, #50312, #63505, #49862, #62610, #71240, #9010, #9443, #16710, #30777, #58907, #38471, #79393, #80287, #86644, #65303, #23100, #45713, #58467, #45280, #78944, #17601, #66629, #73443, #3081, #44389, #50772, #65730, #37602, #66174, #37153, #64853, #10764, #72119, #24418, #43943, #58036, #3962, #23975, #85325, #71679, #85769, #72999, #78507, #11217, #4419, #2641, #38921, #86198, #16266, #51650, #3512, #57581, #23539, #30341, #51202, #24857, #9894, #17158, #44840, #72570, #31663, #10337, #59361, #87091, #38041, #31212, #52083, #79843, #52524, #18032, #11682, #39375, #75251, #46619, #61158, #18475, #32546, #40711, #88436, #59800, #46167, #60252, #47513, #87534, #75697, #68877, #67081, #47960, #67524, #80726, #39803, #67981, #20292, #87983, #13465, #25294, #89332, #52963, #73897, #18935, #41150, #13027, #32106, #33899, #61594, #26197, #53870, #5763, #4858, #19383, #12121, #33454, #74350, #25742, #5312, #81635, #26638, #53418, #81186, #33002, #88885, #60699, #54313, #47059, #74794, #12574, #40261, #82083, #19830, #68435, #6210, #82531, #27094, #54762, #6648, #62049, #1643, #77483, #62503, #83405, #34795, #282, #36147, #14372, #56578, #70673, #22092, #1184, #27980, #77942, #89783, #69326, #84321, #42490, #83863, #49757, #29343, #27536, #15713, #7551, #14822, #43390, #13913, #35237, #55654, #42939, #21181, #41593, #34342, #15264, #48852, #7103, #55217, #35689, #70220, #48397, #76590, #69776, #7992, #8448, #28428, #57022, #63402, #42049, #82974, #84763, #62945 ) ),
 .UNSPECIFIED., .F., .F., .F.,
 ( 4, 3, 1, 1, 1, 3, 4 ),
 ( 4, 1, 1, 1, 1, 1, 1, 1, 1, 1, 1, 1, 1, 1, 1, 1, 1, 1, 1, 1, 1, 1, 1, 1, 1, 1, 1, 1, 1, 1, 1, 1, 1, 1, 1, 1, 1, 1, 1, 1, 1, 1, 1, 1, 1, 1, 1, 1, 1, 1, 1, 1, 1, 1, 1, 1, 1, 1, 1, 1, 1, 1, 1, 1, 1, 1, 1, 1, 1, 1, 1, 1, 1, 1, 1, 1, 1, 1, 1, 1, 1, 1, 1, 1, 1, 1, 1, 1, 1, 1, 1, 1, 1, 1, 1, 1, 1, 1, 1, 1, 1, 1, 1, 1, 1, 1, 1, 1, 1, 1, 1, 1, 1, 1, 1, 1, 1, 1, 1, 1, 1, 1, 1, 1, 1, 1, 1, 1, 1, 1, 1, 1, 1, 1, 1, 1, 1, 1, 1, 1, 1, 1, 1, 1, 1, 1, 1, 1, 1, 1, 1, 1, 1, 1, 1, 1, 1, 1, 1, 1, 1, 1, 1, 1, 1, 1, 1, 1, 1, 1, 1, 1, 1, 1, 1, 1, 1, 1, 1, 1, 1, 1, 1, 1, 1, 1, 1, 1, 1, 1, 1, 1, 1, 1, 1, 1, 1, 1, 1, 1, 1, 1, 1, 1, 1, 1, 1, 1, 1, 1, 1, 1, 1, 1, 1, 1, 1, 1, 1, 1, 1, 1, 1, 1, 1, 1, 1, 1, 1, 1, 1, 1, 1, 1, 1, 1, 1, 1, 1, 1, 1, 1, 1, 1, 1, 1, 1, 1, 1, 1, 1, 1, 1, 1, 1, 1, 1, 1, 1, 1, 1, 1, 1, 1, 1, 1, 1, 1, 1, 1, 1, 1, 1, 1, 1, 1, 1, 1, 1, 1, 1, 1, 1, 1, 1, 1, 1, 1, 1, 1, 1, 1, 1, 1, 1, 1, 1, 1, 1, 1, 1, 1, 1, 1, 1, 1, 1, 1, 1, 1, 1, 1, 1, 1, 1, 1, 1, 1, 1, 1, 1, 1, 1, 1, 1, 1, 1, 1, 1, 1, 1, 1, 1, 1, 1, 1, 1, 1, 1, 1, 1, 1, 1, 1, 1, 1, 1, 1, 1, 1, 1, 1, 1, 1, 1, 1, 1, 1, 1, 1, 1, 1, 1, 1, 1, 1, 1, 1, 1, 1, 1, 1, 1, 1, 1, 1, 1, 1, 1, 1, 1, 1, 1, 1, 1, 1, 1, 1, 1, 1, 1, 1, 1, 1, 1, 1, 1, 1, 1, 1, 1, 1, 1, 1, 1, 1, 1, 1, 1, 1, 1, 1, 1, 1, 1, 1, 1, 1, 1, 1, 1, 1, 1, 1, 1, 1, 1, 1, 1, 1, 1, 1, 1, 1, 1, 1, 1, 1, 1, 1, 1, 1, 1, 1, 1, 1, 1, 1, 1, 1, 1, 1, 1, 1, 1, 1, 1, 1, 1, 1, 1, 1, 1, 1, 1, 1, 1, 1, 1, 1, 1, 1, 1, 1, 1, 1, 1, 1, 1, 1, 1, 1, 1, 1, 1, 1, 1, 1, 1, 1, 1, 1, 1, 1, 1, 1, 1, 1, 1, 1, 1, 1, 1, 1, 1, 1, 1, 1, 1, 1, 1, 1, 1, 1, 1, 1, 1, 1, 1, 1, 1, 1, 1, 1, 1, 4 ),
 ( -1.602212253331664948, -1.570796326795749875, -0.6731984257695950991, -0.2243994752565149908, 0.6731984257696440599, 1.570796326795800057, 1.602526412597075067 ),
 ( 0.000000000000000000, 0.4990644329702639825, 0.9981288659405289643, 1.497193298910790116, 1.996257731881059927, 2.994386597821590001, 3.992515463762110084, 4.491579896732379673, 4.990644329702639936, 5.489708762672909970, 5.988773195643170233, 6.986902061583700529, 7.985030927524229938, 8.484095360494489313, 8.983159793464759346, 9.482224226435020498, 9.981288659405290531, 10.97941752534580040, 11.97754639128630139, 12.47661082425659984, 12.97567525722690007, 13.47473969019709905, 13.97380412316740106, 14.97193298910790027, 15.97006185504850073, 16.46912628801869971, 16.96819072098899994, 17.46725515395930017, 17.96631958692950093, 18.96444845286999836, 19.96257731881059883, 20.46164175178079958, 20.96070618475109981, 21.45977061772140004, 21.95883505069160080, 22.95696391663220126, 23.95509278257270225, 24.45415721554289945, 24.95322164851319968, 25.45228608148349991, 25.95135051445370067, 26.94947938039430113, 27.94760824633480212, 28.44667267930509880, 28.94573711227529955, 29.44480154524559978, 29.94386597821590001, 30.94199484415640100, 31.94012371009690199, 32.43918814306720577, 32.93825257603739942, 33.43731700900769965, 33.93638144197799988, 34.93451030791850087, 35.93263917385900186, 36.43170360682930209, 36.93076803979960232, 37.42983247276980308, 37.92889690574009620, 38.92702577168060429, 39.92515463762109817, 40.42421907059139841, 40.92328350356169864, 41.42234793653189939, 41.92141236950219962, 42.91954123544270061, 43.91767010138330107, 44.41673453435349472, 44.91579896732380206, 45.41486340029400282, 45.91392783326430305, 46.91205669920479693, 47.91018556514539739, 48.40924999811559815, 48.90831443108589838, 49.40737886405619861, 49.90644329702639936, 50.90457216296699983, 51.90270102890750081, 52.40176546187770157, 52.90082989484799469, 53.39989432781830203, 53.89895876078850279, 54.89708762672909614, 55.89521649266960424, 56.39428092563989736, 56.89334535861009812, 57.39240979158039835, 57.89147422455069858, 58.88960309049119957, 59.88773195643170055, 60.38679638940200078, 60.88586082237220154, 61.38492525534249467, 61.88398968831280200, 62.88211855425329588, 63.88024742019380398, 64.37931185316409710, 64.87837628613441154, 65.37744071910459809, 65.87650515207489832, 66.87463401801539931, 67.87276288395590029, 68.37182731692620052, 68.87089174989650076, 69.36995618286670151, 69.86902061583700174, 70.86714948177750273, 71.86527834771810319, 72.36434278068828974, 72.86340721365860418, 73.36247164662880493, 73.86153607959910516, 74.85966494553959194, 75.85779381148019240, 76.35685824445040737, 76.85592267742069339, 77.35498711039100783, 77.85405154336119438, 78.85218040930179484, 79.85030927524229583, 80.34937370821249658, 80.84843814118279681, 81.34750257415311125, 81.84656700712329780, 82.84469587306389826, 83.84282473900439925, 84.34188917197469948, 84.84095360494490023, 85.34001803791520047, 85.83908247088550070, 86.83721133682600168, 87.83534020276650267, 88.33440463573680290, 88.83346906870698945, 89.33253350167728968, 89.83159793464760412, 90.82972680058810511, 91.82785566652860609, 92.32692009949890632, 92.82598453246910708, 93.32504896543939310, 93.82411339840969333, 94.82224226435020853, 95.82037113029070952, 96.31943556326099554, 96.81849999623130998, 97.31756442920149652, 97.81662886217179675, 98.81475772811229774, 99.81288659405289820, 100.3119510270229995, 100.8110154599930013, 101.3100798929639978, 101.8091443259339997, 102.8072731918740033, 103.8054020578150016, 104.3044664907849892, 104.8035309237550052, 105.3025953567259876, 105.8016597896960036, 106.7997886556370020, 107.7979175215769914, 108.2969819545470074, 108.7960463875180039, 109.2951108204880057, 109.7941752534579933, 110.7923041193989917, 111.7904329853389953, 112.2894974183089971, 112.7885618512799937, 113.2876262842500097, 113.7866907172199973, 114.7848195831609956, 115.7829484491009993, 116.2820128820720100, 116.7810773150420118, 117.2801417480119994, 117.7792061809820012, 118.7773350469229996, 119.7754639128630032, 120.2745283458339998, 120.7735927788040016, 121.2726572117740034, 121.7717216447440052, 122.7698505106850035, 123.7679793766259877, 124.2670438095959895, 124.7661082425660055, 125.2651726755359931, 125.7642371085070039, 126.7623659744470075, 127.7604948403880059, 128.2595592733580077, 128.7586237063279953, 129.2576881392979828, 129.7567525722689936, 130.7548814382089972, 131.7530103041499956, 132.2520747371200116, 132.7511391700899992, 133.2502036030609815, 133.7492680360309976, 134.7473969019710012, 135.7455257679119995, 136.2445902008820156, 136.7436546338520031, 137.2427190668229855, 137.7417834997930015, 138.7399123657329767, 139.7380412316740035, 140.2371056646440195, 140.7361700976149734, 141.2352345305849894, 141.7342989635550055, 142.7324278294960038, 143.7305566954360074, 144.2296211284059950, 144.7286855613770058, 145.2277499943469934, 145.7268144273169810, 146.7249432932580078, 147.7230721591979830, 148.2221365921679990, 148.7212010251390097, 149.2202654581089973, 149.7193298910789849, 150.7174587570200117, 151.7155876229599869, 152.2146520559309977, 152.7137164889010137, 153.2127809218710013, 153.7118453548409889, 154.7099742207820157, 155.7081030867219908, 156.2071675196930016, 156.7062319526630176, 157.2052963856329768, 157.7043608186039876, 158.7024896845440196, 159.7006185504849896, 160.1996829834550056, 160.6987474164249932, 161.1978118493950092, 161.6968762823659915, 162.6950051483059951, 163.6931340142469935, 164.1921984472169811, 164.6912628801869971, 165.1903273131570131, 165.6893917461279955, 166.6875206120679991, 167.6856494780089974, 168.1847139109789850, 168.6837783439490011, 169.1828427769200118, 169.6819072098899994, 170.6800360758300030, 171.6781649417710014, 172.1772293747409890, 172.6762938077110050, 173.1753582406820158, 173.6744226736520034, 174.6725515395920070, 175.6706804055330053, 176.6688092714740037, 177.1678737044439913, 177.6669381374140073, 178.6650670033550057, 179.6631958692950093, 180.1622603022650253, 180.6613247352360077, 181.1603891682059952, 181.6594536011760113, 182.6575824671170096, 183.6557113330570132, 184.1547757660279956, 184.6538401989979832, 185.1529046319679992, 185.6519690649380152, 186.6500979308789852, 187.6482267968190172, 188.1472912297899995, 188.6463556627599871, 189.1454200957300031, 189.6444845286999907, 190.6426133946409891, 191.6407422605809927, 192.1398066935519751, 192.6388711265219911, 193.1379355594920071, 193.6369999924630179, 194.6351288584029930, 195.6332577243439914, 196.1323221573140074, 196.6313865902839950, 197.1304510232539826, 197.6295154562249934, 198.6276443221649970, 199.6257731881059954, 200.1248376210760114, 200.6239020540459990, 201.1229664870159866, 201.6220309199869973, 202.6201597859270009, 203.6182886518679993, 204.1173530848380153, 204.6164175178080029, 205.1154819507789853, 205.6145463837490013, 206.6126752496890049, 207.6108041156300033, 208.1098685485999908, 208.6089329815700069, 209.1079974145409892, 209.6070618475110052, 210.6051907134520036, 211.6033195793920072, 212.1023840123619948, 212.6014484453330056, 213.1005128783029932, 213.5995773112729808, 214.5977061772140075, 215.5958350431539827, 216.0948994761239987, 216.5939639090950095, 217.0930283420649971, 217.5920927750350131, 218.5902216409760115, 219.5883505069159867, 220.0874149398869974, 220.5864793728569850, 221.0855438058270011, 221.5846082387970171, 222.5827371047380154, 223.5808659706779906, 224.0799304036490014, 224.5789948366189890, 225.0780592695890050, 225.5771237025589926, 226.5752525685000194, 227.5733814344410177, 228.0724458674109769, 228.5715103003809929, 229.0705747333509805, 229.5696391663219913, 230.5677680322619949, 231.5658968982030217, 232.0649613311730093, 232.5640257641429969, 233.0630901971129845, 233.5621546300839952, 234.5602834960239989, 235.5584123619649972, 236.0574767949350132, 236.5565412279050008, 237.0556056608760116, 237.5546700938459992, 238.5527989597860028, 239.5509278257270012, 240.0499922586970172, 240.5490566916670048, 241.0481211246380155, 241.5471855576080031, 242.5453144235479783, 243.5434432894890051, 244.0425077224589927, 244.5415721554290087, 245.0406365884000195, 245.5397010213700071, 246.5378298873109770, 247.5359587532509806, 248.0350231862209966, 248.5340876191920074, 249.0331520521619950, 249.5322164851320110, 250.5303453510730094, 251.5284742170129846, 252.0275386499830006, 252.5266030829539829, 253.0256675159239990, 253.5247319488940150, 254.5228608148350133, 255.5209896807749885, 256.0200541137460277, 256.5191185467160153, 257.0181829796860029, 257.5172474126559905, 258.5153762785969889, 259.5135051445370209, 260.0125695775079748, 260.5116340104780193, 261.0106984434480069, 261.5097628764180513, 262.5078917423589928, 263.5060206082999912, 264.0050850412700356, 264.5041494742399664, 265.0032139072100108, 265.5022783401809647, 266.5004072061209968, 267.4985360720619951, 267.9976005050319827, 268.4966649380020272, 268.9957293709719579, 269.4947938039430255, 270.4929226698830007, 271.4910515358239991, 271.9901159687939867, 272.4891804017639743, 272.9882448347349850, 273.4873092677049726, 274.4854381336450047, 275.4835669995860030, 275.9826314325560475, 276.4816958655259782, 276.9807602984969890, 277.4798247314670334, 278.4779535974070086, 279.4760824633480070, 279.9751468963179946, 280.4742113292880390, 280.9732757622589929, 281.4723401952289805, 282.4704690611699789, 283.4685979271100109, 283.9676623600799985, 284.4667267930510093, 284.9657912260209969, 285.4648556589909845, 286.4629845249319828, 287.4611133908720149, 287.9601778238429688, 288.4592422568130132, 288.9583066897830008, 289.4573711227530453, 290.4554999886939868, 291.4536288546339620, 291.9526932876050296, 292.4517577205749603, 292.9508221535450048, 293.4498865865149924, 294.4480154524559907, 295.4461443183960228, 295.9452087513669767, 296.4442731843370211, 296.9433376173070087, 297.4424020502780195, 298.4405309162180515, 299.4386597821589930, 299.9377242151289806, 300.4367886480989682, 300.9358530810690127, 301.4349175140399666, 302.4330463799799986, 303.4311752459209970, 303.9302396788909846, 304.4293041118610290, 304.9283685448309598, 305.4274329778020274, 306.4255618437420026, 307.4236907096830009, 307.9227551426529885, 308.4218195756230330, 308.9208840085939869, 309.4199484415639745, 310.4180773075040065, 311.4162061734450049, 311.9152706064150493, 312.4143350393849801, 312.9133994723560477, 313.4124639053259784, 314.4105927712660105, 315.4087216372070088, 315.9077860701769964, 316.4068505031480072, 316.9059149361179948, 317.4049793690880392, 318.4031082350289807, 319.4012371009689559, 319.9003015339390004, 320.3993659669100111, 320.8984303998799987, 321.3974948328499863, 322.3956236987909847, 323.3937525647310167, 323.8928169977019706, 324.3918814306720151, 324.8909458636420027, 325.3900102966119903, 326.3881391625530455, 327.3862680284929638, 327.8853324614640314, 328.3843968944339622, 328.8834613274040066, 329.3825257603739942, 330.3806546263149926, 331.3787834922550246, 331.8778479252259785, 332.3769123581960230, 332.8759767911659537, 333.3750412241370213, 334.3731700900769965, 335.3712989560180517, 335.8703633889879825, 336.3694278219579701, 336.8684922549280145, 337.3675566878989684, 338.3656855538390005, 339.3638144197799988, 339.8628788527500433, 340.3619432857199740, 340.8610077186899616, 341.3600721516610292, 342.3582010176010044, 343.3563298835420028, 343.8553943165119904, 344.3544587494820348, 344.8535231824529887, 345.3525876154230332, 346.3507164813629515, 347.3488453473040067, 347.8479097802739943, 348.3469742132439819, 348.8460386462150495, 349.3451030791849803 ),
 .UNSPECIFIED. ) ;
#82204 = CARTESIAN_POINT ( 'NONE',  ( 84.72230615113649321, 89.94765885072622780, -99.33304294513241928 ) ) ;
#82205 = CARTESIAN_POINT ( 'NONE',  ( -47.02966122971776741, 101.5999999999999943, 76.61736725193563302 ) ) ;
#82206 = CYLINDRICAL_SURFACE ( 'NONE', #79230, 3.174999999999997158 ) ;
#82207 = PRODUCT_RELATED_PRODUCT_CATEGORY ( 'part', '', ( #75331 ) ) ;
#82209 = DIRECTION ( 'NONE',  ( 0.000000000000000000, -1.000000000000000000, 0.000000000000000000 ) ) ;
#82208 = PLANE ( 'NONE',  #33452 ) ;
#82210 = CARTESIAN_POINT ( 'NONE',  ( 102.0668616197963985, -27.97060589024009047, 180.4898093164620718 ) ) ;
#82211 = CIRCLE ( 'NONE', #25641, 2.117000000000007987 ) ;
#82212 = ORIENTED_EDGE ( 'NONE', *, *, #61673, .F. ) ;
#82213 = ORIENTED_EDGE ( 'NONE', *, *, #60762, .F. ) ;
#82214 = CARTESIAN_POINT ( 'NONE',  ( 194.0371591254572650, -24.42818131005417825, 313.9678068554149490 ) ) ;
#82215 = PLANE ( 'NONE',  #88394 ) ;
#82216 = CARTESIAN_POINT ( 'NONE',  ( 96.80143343076643703, -35.25719154489702589, 222.2251490854339693 ) ) ;
#82217 = EDGE_CURVE ( 'NONE', #76316, #65852, #57815, .T. ) ;
#82219 = ORIENTED_EDGE ( 'NONE', *, *, #70246, .F. ) ;
#82218 = FACE_OUTER_BOUND ( 'NONE', #59829, .T. ) ;
#82220 = CARTESIAN_POINT ( 'NONE',  ( 104.0406618471960627, -46.06530165129700549, 78.32705384733895926 ) ) ;
#82221 = EDGE_CURVE ( 'NONE', #23005, #46468, #50546, .T. ) ;
#82222 = CARTESIAN_POINT ( 'NONE',  ( 110.8742435910063051, -45.97612887520801195, 52.88732575667828684 ) ) ;
#82223 = ADVANCED_FACE ( 'NONE', ( #10119 ), #78737, .F. ) ;
#82224 = CARTESIAN_POINT ( 'NONE',  ( 69.95046282694566742, -138.0544793580991723, 247.6577929086349741 ) ) ;
#82225 = CARTESIAN_POINT ( 'NONE',  ( -74.84259178415759095, 53.97499999999998010, 30.79999999999997939 ) ) ;
#82226 = EDGE_LOOP ( 'NONE', ( #43940, #82494, #88807, #16817 ) ) ;
#82227 = PLANE ( 'NONE',  #24017 ) ;
#82228 = ADVANCED_FACE ( 'NONE', ( #10556 ), #37081, .T. ) ;
#82229 = ORIENTED_EDGE ( 'NONE', *, *, #29104, .F. ) ;
#82230 = ORIENTED_EDGE ( 'NONE', *, *, #24163, .T. ) ;
#82231 = VECTOR ( 'NONE', #3576, 1000.000000000000000 ) ;
#82232 = CARTESIAN_POINT ( 'NONE',  ( 99.29109958770327182, -40.98052783126505005, 218.1558690201829620 ) ) ;
#82233 = CARTESIAN_POINT ( 'NONE',  ( 50.79999999999999716, 69.84999999999999432, 257.1750000000000114 ) ) ;
#82234 = CARTESIAN_POINT ( 'NONE',  ( 141.8164832912739826, -9.729447159940995959, 14.92562527591100618 ) ) ;
#82235 = LINE ( 'NONE', #19085, #22877 ) ;
#82236 = EDGE_CURVE ( 'NONE', #55559, #70423, #58769, .T. ) ;
#82237 = CARTESIAN_POINT ( 'NONE',  ( 81.55985452234320121, -39.04079274305795622, 1.981704437692578313 ) ) ;
#82238 = VERTEX_POINT ( 'NONE', #79621 ) ;
#82239 = CARTESIAN_POINT ( 'NONE',  ( 25.56670390244808289, -42.82844715994167473, 257.2178068554150059 ) ) ;
#82240 = CARTESIAN_POINT ( 'NONE',  ( 27.27158787008328389, 184.0000000000000000, 106.1020876358972629 ) ) ;
#82241 = ORIENTED_EDGE ( 'NONE', *, *, #62088, .F. ) ;
#82242 = CARTESIAN_POINT ( 'NONE',  ( 115.8917813183058740, -31.17956921574393903, 34.27276813305396530 ) ) ;
#82243 = ORIENTED_EDGE ( 'NONE', *, *, #86119, .F. ) ;
#82244 = CARTESIAN_POINT ( 'NONE',  ( 104.9194883499490061, -28.34545421100826346, 243.1061856076869958 ) ) ;
#82245 = DIRECTION ( 'NONE',  ( -0.000000000000000000, -1.000000000000000000, -0.000000000000000000 ) ) ;
#82246 = CARTESIAN_POINT ( 'NONE',  ( 108.5509251780138271, -26.47246927008487205, 149.9737205140069420 ) ) ;
#82247 = CARTESIAN_POINT ( 'NONE',  ( 67.65734841870819594, 69.84999999999999432, 358.0130000000000337 ) ) ;
#82248 = DIRECTION ( 'NONE',  ( 0.000000000000000000, 0.000000000000000000, -1.000000000000000000 ) ) ;
#82249 = CARTESIAN_POINT ( 'NONE',  ( 91.91125933621934507, -111.8737466215629013, -21.78219314458179667 ) ) ;
#82250 = CARTESIAN_POINT ( 'NONE',  ( 10.56149714719919075, 75.49700186538963464, 130.1281057863494652 ) ) ;
#82251 = CARTESIAN_POINT ( 'NONE',  ( 110.8324567285566076, -26.28842506301429083, 245.7889586092439629 ) ) ;
#82252 = CARTESIAN_POINT ( 'NONE',  ( 107.0664832912739399, -36.72944715994095333, 294.6356252759106837 ) ) ;
#82253 = ORIENTED_EDGE ( 'NONE', *, *, #6503, .F. ) ;
#82254 = AXIS2_PLACEMENT_3D ( 'NONE', #77826, #23326, #43729 ) ;
#82255 = CARTESIAN_POINT ( 'NONE',  ( 99.47006920962783738, -43.93274313109116491, 77.92991099019597812 ) ) ;
#82256 = VECTOR ( 'NONE', #20113, 1000.000000000000000 ) ;
#82257 = DIRECTION ( 'NONE',  ( 0.000000000000000000, 0.000000000000000000, 1.000000000000000000 ) ) ;
#82258 = CIRCLE ( 'NONE', #80824, 2.500000000000002220 ) ;
#82259 = ORIENTED_EDGE ( 'NONE', *, *, #37826, .F. ) ;
#82260 = VERTEX_POINT ( 'NONE', #23328 ) ;
#82261 = VERTEX_POINT ( 'NONE', #22871 ) ;
#82262 = DIRECTION ( 'NONE',  ( 0.000000000000000000, 0.000000000000000000, -1.000000000000000000 ) ) ;
#82263 = LINE ( 'NONE', #63139, #63101 ) ;
#82264 = LINE ( 'NONE', #27272, #62483 ) ;
#82265 = LINE ( 'NONE', #7293, #85279 ) ;
#82266 = CARTESIAN_POINT ( 'NONE',  ( 98.98344471881878803, -35.59181213353920725, 179.0338046553059712 ) ) ;
#82267 = CARTESIAN_POINT ( 'NONE',  ( 96.22678813199759418, -34.45212096497557042, 257.1737205140064475 ) ) ;
#82268 = CARTESIAN_POINT ( 'NONE',  ( 115.0357021915621090, -42.91043845286343128, 59.30209018972115587 ) ) ;
#82269 = ORIENTED_EDGE ( 'NONE', *, *, #73918, .T. ) ;
#82270 = CARTESIAN_POINT ( 'NONE',  ( 130.4016766882982949, 93.55256755804781221, 6.356666657631230066 ) ) ;
#82271 = AXIS2_PLACEMENT_3D ( 'NONE', #79325, #44774, #72498 ) ;
#82272 = AXIS2_PLACEMENT_3D ( 'NONE', #78152, #15912, #17685 ) ;
#82273 = LINE ( 'NONE', #54954, #89732 ) ;
#82274 = ADVANCED_FACE ( 'NONE', ( #31000 ), #9231, .T. ) ;
#82275 = ORIENTED_EDGE ( 'NONE', *, *, #70123, .F. ) ;
#82276 = ORIENTED_EDGE ( 'NONE', *, *, #41293, .T. ) ;
#82277 = VECTOR ( 'NONE', #25270, 1000.000000000000000 ) ;
#82278 = CARTESIAN_POINT ( 'NONE',  ( 123.6837132603318992, -56.64645651782490177, 239.5838068554164693 ) ) ;
#82279 = ORIENTED_EDGE ( 'NONE', *, *, #72049, .F. ) ;
#82280 = EDGE_LOOP ( 'NONE', ( #34, #16857, #58289, #8714 ) ) ;
#82281 = CARTESIAN_POINT ( 'NONE',  ( 59.56670390244699576, -67.87844715994098976, 155.2178068554179902 ) ) ;
#82282 = CARTESIAN_POINT ( 'NONE',  ( 116.3265979651016409, -32.94445627519164077, 14.13562527591094664 ) ) ;
#82283 = ADVANCED_FACE ( 'NONE', ( #36930 ), #24200, .T. ) ;
#82284 = DIRECTION ( 'NONE',  ( 0.000000000000000000, 0.000000000000000000, -1.000000000000000000 ) ) ;
#82285 = CARTESIAN_POINT ( 'NONE',  ( 72.31648329127402519, -36.72944715994106701, -5.074374724089063982 ) ) ;
#82286 = CARTESIAN_POINT ( 'NONE',  ( 116.7432888474544370, -37.52321155953265475, 188.1838483995059619 ) ) ;
#82287 = CARTESIAN_POINT ( 'NONE',  ( 117.3100546213214699, -38.89183298362549834, 63.66133956162494911 ) ) ;
#82288 = CARTESIAN_POINT ( 'NONE',  ( 141.0664832912740394, -46.72944715994099596, -4.824374724088994704 ) ) ;
#82289 = ORIENTED_EDGE ( 'NONE', *, *, #52340, .F. ) ;
#82290 = CARTESIAN_POINT ( 'NONE',  ( 73.06670390244801183, -58.72944715994112386, 198.9178068554149945 ) ) ;
#82291 = ORIENTED_EDGE ( 'NONE', *, *, #85284, .F. ) ;
#82292 = CARTESIAN_POINT ( 'NONE',  ( 113.2442291481427361, -28.75770190614504429, 260.5523025446513543 ) ) ;
#82293 = VERTEX_POINT ( 'NONE', #71907 ) ;
#82294 = LINE ( 'NONE', #26849, #1508 ) ;
#82295 = DIRECTION ( 'NONE',  ( -4.237773401492740281E-14, 1.000000000000000000, 0.000000000000000000 ) ) ;
#82296 = DIRECTION ( 'NONE',  ( 1.907762142705490052E-15, 7.167082501179359715E-16, -1.000000000000000000 ) ) ;
#82297 = CIRCLE ( 'NONE', #41607, 25.39999999999999858 ) ;
#82298 = CARTESIAN_POINT ( 'NONE',  ( -148.0533267522759786, 101.5999999999999943, -160.2664750769289697 ) ) ;
#82299 = ORIENTED_EDGE ( 'NONE', *, *, #77567, .T. ) ;
#82300 = EDGE_CURVE ( 'NONE', #33618, #11998, #67467, .T. ) ;
#82301 = CARTESIAN_POINT ( 'NONE',  ( 107.6080043092626113, -48.59286871074260006, 42.61276813305398292 ) ) ;
#82302 = SURFACE_STYLE_FILL_AREA ( #34114 ) ;
#82304 = CARTESIAN_POINT ( 'NONE',  ( 172.5664832912740110, 0.2215528400590013880, 258.9256252759120116 ) ) ;
#82303 = DIRECTION ( 'NONE',  ( 0.000000000000000000, 1.000000000000000000, 0.000000000000000000 ) ) ;
#82305 = CARTESIAN_POINT ( 'NONE',  ( 36.23715912545339535, -47.82818131006131779, 180.4678068554150911 ) ) ;
#82306 = CARTESIAN_POINT ( 'NONE',  ( 131.8086190314096484, -17.15582774929994869, 2.518078172612508769 ) ) ;
#82307 = VERTEX_POINT ( 'NONE', #37376 ) ;
#82308 = CARTESIAN_POINT ( 'NONE',  ( 97.01457192517754891, -36.67423255113659764, 122.3204556863920232 ) ) ;
#82309 = DIRECTION ( 'NONE',  ( 0.000000000000000000, 0.000000000000000000, -1.000000000000000000 ) ) ;
#82310 = CARTESIAN_POINT ( 'NONE',  ( 1.669011862100898913, 69.93236506402145380, 118.5470928879096562 ) ) ;
#82311 = ADVANCED_FACE ( 'NONE', ( #78288 ), #72351, .F. ) ;
#82312 = VERTEX_POINT ( 'NONE', #84651 ) ;
#82313 = CARTESIAN_POINT ( 'NONE',  ( 115.2242804385497976, -44.22181337150698255, 74.22324432352993995 ) ) ;
#82314 = AXIS2_PLACEMENT_3D ( 'NONE', #53948, #21255, #62580 ) ;
#82316 = CARTESIAN_POINT ( 'NONE',  ( 51.06648329127400388, 0.2215528400590083269, 333.4006252759110112 ) ) ;
#82315 = DIRECTION ( 'NONE',  ( 0.7071067811865779928, -0.7071067811865171526, 7.071067811865785947E-16 ) ) ;
#82317 = DIRECTION ( 'NONE',  ( -1.000000000000000000, -4.163336342344333240E-14, 0.000000000000000000 ) ) ;
#82318 = CIRCLE ( 'NONE', #56145, 9.524999999999998579 ) ;
#82319 = AXIS2_PLACEMENT_3D ( 'NONE', #86591, #52898, #18877 ) ;
#82320 = DIRECTION ( 'NONE',  ( 0.7071067811865443531, 6.205111755629953205E-16, 0.7071067811865506814 ) ) ;
#82321 = EDGE_LOOP ( 'NONE', ( #31980, #71116, #82915, #17545 ) ) ;
#82322 = CARTESIAN_POINT ( 'NONE',  ( 102.0112516875887678, -27.67497761899955933, 101.4937205140059575 ) ) ;
#82324 = ORIENTED_EDGE ( 'NONE', *, *, #84373, .F. ) ;
#82323 = DIRECTION ( 'NONE',  ( 0.000000000000000000, -1.000000000000000000, 0.000000000000000000 ) ) ;
#82325 = CARTESIAN_POINT ( 'NONE',  ( 105.8960369669305948, -47.10223136823062617, 278.4870538473395527 ) ) ;
#82326 = DIRECTION ( 'NONE',  ( 0.8861241255175470455, 0.000000000000000000, -0.4634479843259246556 ) ) ;
#82327 = LINE ( 'NONE', #63657, #67849 ) ;
#82328 = CARTESIAN_POINT ( 'NONE',  ( 33.78129701732328982, -35.65087443489905183, 193.9678068554150911 ) ) ;
#82329 = EDGE_CURVE ( 'NONE', #18476, #75636, #45064, .T. ) ;
#82330 = LINE ( 'NONE', #20092, #55759 ) ;
#82331 = VECTOR ( 'NONE', #52068, 1000.000000000000000 ) ;
#82332 = LINE ( 'NONE', #21437, #63666 ) ;
#82333 = CARTESIAN_POINT ( 'NONE',  ( -91.73035097708734042, 69.84937019662268654, 92.90380151375066475 ) ) ;
#82334 = VECTOR ( 'NONE', #73255, 1000.000000000000000 ) ;
#82335 = CARTESIAN_POINT ( 'NONE',  ( 96.72778144249456034, -35.92320320382069099, 191.2765776568639922 ) ) ;
#82336 = ORIENTED_EDGE ( 'NONE', *, *, #80766, .F. ) ;
#82337 = ORIENTED_EDGE ( 'NONE', *, *, #1209, .T. ) ;
#82338 = CARTESIAN_POINT ( 'NONE',  ( 115.6492561437540445, -34.52393389210755004, 120.4587261630399837 ) ) ;
#82339 = CARTESIAN_POINT ( 'NONE',  ( 107.0664832912739257, -52.72944715994095333, 357.5272416190308604 ) ) ;
#82341 = CARTESIAN_POINT ( 'NONE',  ( 80.06648329127398256, -8.729447159941058132, 1.325625275910934597 ) ) ;
#82340 = CARTESIAN_POINT ( 'NONE',  ( 109.8085987287837213, -27.34093086507540704, 255.8499109901960367 ) ) ;
#82342 = DIRECTION ( 'NONE',  ( 9.351236661543306751E-17, -3.725950533538267725E-29, -1.000000000000000000 ) ) ;
#82343 = CARTESIAN_POINT ( 'NONE',  ( 221.2791280605339921, 36.86249999999999716, -7.937500000000000000 ) ) ;
#82344 = EDGE_CURVE ( 'NONE', #80812, #86777, #79179, .T. ) ;
#82345 = CARTESIAN_POINT ( 'NONE',  ( 274.0659999999999741, 36.86249999999999716, -7.937500000000000000 ) ) ;
#82346 = CARTESIAN_POINT ( 'NONE',  ( 105.7995184837401155, -26.72403496634397868, 106.1772919428844091 ) ) ;
#82347 = FACE_OUTER_BOUND ( 'NONE', #71144, .T. ) ;
#82348 = ADVANCED_FACE ( 'NONE', ( #8795 ), #36494, .T. ) ;
#82349 = CARTESIAN_POINT ( 'NONE',  ( 109.4403364888817123, -25.95778788316468422, 179.8918157521019339 ) ) ;
#82350 = DIRECTION ( 'NONE',  ( 0.000000000000000000, 0.000000000000000000, 1.000000000000000000 ) ) ;
#82351 = ORIENTED_EDGE ( 'NONE', *, *, #28038, .F. ) ;
#82352 = VERTEX_POINT ( 'NONE', #37830 ) ;
#82353 = CARTESIAN_POINT ( 'NONE',  ( -96.70122665881181945, 71.54617234588346264, -87.71474477836304118 ) ) ;
#82354 = CYLINDRICAL_SURFACE ( 'NONE', #67906, 2.030000000001807248 ) ;
#82355 = CARTESIAN_POINT ( 'NONE',  ( 100.9550373873344569, -28.70674047333049117, 185.5943939165742336 ) ) ;
#82356 = FACE_OUTER_BOUND ( 'NONE', #39836, .T. ) ;
#82357 = AXIS2_PLACEMENT_3D ( 'NONE', #84770, #15271, #56585 ) ;
#82358 = DIRECTION ( 'NONE',  ( 0.000000000000000000, 0.000000000000000000, -1.000000000000000000 ) ) ;
#82359 = VERTEX_POINT ( 'NONE', #57360 ) ;
#82360 = CARTESIAN_POINT ( 'NONE',  ( -11.93750983681333899, 86.60304284441519940, 117.7525081508920408 ) ) ;
#82361 = CARTESIAN_POINT ( 'NONE',  ( 115.4600223225059494, -29.53725764737424342, 229.4022919425779605 ) ) ;
#82362 = ORIENTED_EDGE ( 'NONE', *, *, #11974, .F. ) ;
#82363 = CARTESIAN_POINT ( 'NONE',  ( -7.341132454938143148, 92.79876842313133523, 118.3289926826412710 ) ) ;
#82364 = CARTESIAN_POINT ( 'NONE',  ( 107.0664832912739257, -49.72944715994095333, 311.6343304127839815 ) ) ;
#82365 = DIRECTION ( 'NONE',  ( 0.000000000000000000, 0.000000000000000000, 1.000000000000000000 ) ) ;
#82366 = CARTESIAN_POINT ( 'NONE',  ( 115.2001725772484662, -37.69162533786680314, 51.55094751244793372 ) ) ;
#82367 = CARTESIAN_POINT ( 'NONE',  ( 102.6743760996991597, -27.25069970728465307, 176.4213395616249898 ) ) ;
#82368 = DIRECTION ( 'NONE',  ( 0.000000000000000000, 0.000000000000000000, -1.000000000000000000 ) ) ;
#82369 = EDGE_LOOP ( 'NONE', ( #79753, #54731, #65236, #40868 ) ) ;
#82370 = AXIS2_PLACEMENT_3D ( 'NONE', #25260, #51175, #31628 ) ;
#82371 = DIRECTION ( 'NONE',  ( 0.000000000000000000, 0.000000000000000000, 1.000000000000000000 ) ) ;
#82372 = CARTESIAN_POINT ( 'NONE',  ( 116.8390257611673917, -34.20685525486396728, 69.02717489141187457 ) ) ;
#82373 = ORIENTED_EDGE ( 'NONE', *, *, #3631, .F. ) ;
#82374 = ORIENTED_EDGE ( 'NONE', *, *, #65756, .T. ) ;
#82375 = AXIS2_PLACEMENT_3D ( 'NONE', #58487, #86217, #23555 ) ;
#82376 = VECTOR ( 'NONE', #21542, 999.9999999999998863 ) ;
#82377 = CARTESIAN_POINT ( 'NONE',  ( 11.89031456967465594, 87.03148351030577601, 117.9583453772440151 ) ) ;
#82378 = EDGE_LOOP ( 'NONE', ( #5700, #55120, #44536, #69486 ) ) ;
#82379 = ORIENTED_EDGE ( 'NONE', *, *, #87326, .T. ) ;
#82380 = CARTESIAN_POINT ( 'NONE',  ( 30.48091746481831166, -48.32844715994148999, 249.9678068554150059 ) ) ;
#82381 = CARTESIAN_POINT ( 'NONE',  ( 116.0261628859374383, -38.04732875056770780, 73.14480078045792766 ) ) ;
#82382 = CARTESIAN_POINT ( 'NONE',  ( 118.0640922190486890, -35.40731289736847032, 238.9337205140059552 ) ) ;
#82383 = VECTOR ( 'NONE', #69824, 1000.000000000000000 ) ;
#82384 = CARTESIAN_POINT ( 'NONE',  ( 108.1794352217186344, -47.07304438381573419, 202.6613395616249704 ) ) ;
#82386 = CARTESIAN_POINT ( 'NONE',  ( 116.7068942081671423, -31.36975501082244477, 25.24229194257798881 ) ) ;
#82385 = DIRECTION ( 'NONE',  ( -7.723290606088049820E-15, 0.000000000000000000, 1.000000000000000000 ) ) ;
#82387 = DIRECTION ( 'NONE',  ( 0.000000000000000000, 1.000000000000000000, 0.000000000000000000 ) ) ;
#82388 = CARTESIAN_POINT ( 'NONE',  ( 117.0602913923447090, -38.08470216738429315, 94.71862027038207543 ) ) ;
#82389 = AXIS2_PLACEMENT_3D ( 'NONE', #41017, #34206, #29994 ) ;
#82390 = VERTEX_POINT ( 'NONE', #85101 ) ;
#82391 = ORIENTED_EDGE ( 'NONE', *, *, #13796, .T. ) ;
#82392 = CIRCLE ( 'NONE', #37382, 12.44599999999999795 ) ;
#82393 = CIRCLE ( 'NONE', #40291, 179.8898777604655095 ) ;
#82394 = AXIS2_PLACEMENT_3D ( 'NONE', #36408, #56820, #46196 ) ;
#82395 = CARTESIAN_POINT ( 'NONE',  ( 113.0229309284916752, -28.24065945027244595, 84.57753003781698453 ) ) ;
#82396 = CARTESIAN_POINT ( 'NONE',  ( 115.2418052506917832, -44.23790868596334747, 78.22324432352995416 ) ) ;
#82397 = CARTESIAN_POINT ( 'NONE',  ( 105.0129988258793645, -25.82091521352475283, 280.2365776568630622 ) ) ;
#82398 = VERTEX_POINT ( 'NONE', #32326 ) ;
#82399 = EDGE_CURVE ( 'NONE', #82603, #17863, #60026, .T. ) ;
#82400 = CARTESIAN_POINT ( 'NONE',  ( 104.4105186412307944, -25.99981812482467092, 240.2575300378159682 ) ) ;
#82401 = DIRECTION ( 'NONE',  ( 3.999999999999999995E-14, -1.000000000000000000, 4.100000000000000342E-29 ) ) ;
#82402 = FACE_OUTER_BOUND ( 'NONE', #84909, .T. ) ;
#82403 = DIRECTION ( 'NONE',  ( 1.000000000000000000, 1.000000000000000078E-15, 1.000000000000000078E-15 ) ) ;
#82404 = DIRECTION ( 'NONE',  ( 1.000000000000000000, 1.261617073437676668E-15, 9.462128050782575008E-16 ) ) ;
#82406 = DIRECTION ( 'NONE',  ( -0.7071067811865460184, 0.000000000000000000, -0.7071067811865489050 ) ) ;
#82405 = CARTESIAN_POINT ( 'NONE',  ( 112.9946529305922667, -31.31372160417125627, 277.6356252759109680 ) ) ;
#82407 = CARTESIAN_POINT ( 'NONE',  ( 98.38041226088876101, -41.69525672787395365, 172.7397638099760684 ) ) ;
#82408 = CARTESIAN_POINT ( 'NONE',  ( 19.56670390244643443, -25.42844715994203852, 180.4678068554150911 ) ) ;
#82409 = CARTESIAN_POINT ( 'NONE',  ( 9.572570118836559061, 90.93799233918605296, -118.1704038715884337 ) ) ;
#82410 = EDGE_CURVE ( 'NONE', #58062, #69308, #58839, .T. ) ;
#82411 = DIRECTION ( 'NONE',  ( 0.000000000000000000, 0.000000000000000000, -1.000000000000000000 ) ) ;
#82412 = DIRECTION ( 'NONE',  ( -4.237773401492740281E-14, 1.000000000000000000, 0.000000000000000000 ) ) ;
#82413 = EDGE_CURVE ( 'NONE', #77919, #36708, #32780, .T. ) ;
#82414 = LINE ( 'NONE', #87869, #43397 ) ;
#82416 = ORIENTED_EDGE ( 'NONE', *, *, #67904, .T. ) ;
#82415 = CARTESIAN_POINT ( 'NONE',  ( 101.1598124200938571, -28.84337187651578915, 195.5838068554168672 ) ) ;
#82417 = ADVANCED_FACE ( 'NONE', ( #81855 ), #67601, .T. ) ;
#82418 = DIRECTION ( 'NONE',  ( -0.7071067811855900054, -0.7071067811875051401, 0.000000000000000000 ) ) ;
#82419 = CARTESIAN_POINT ( 'NONE',  ( 107.5109734667377239, -47.16730098390026882, 237.6099109901969655 ) ) ;
#82420 = CARTESIAN_POINT ( 'NONE',  ( 97.57126093554219892, -31.07129084365559279, 126.9108633711489915 ) ) ;
#82421 = CARTESIAN_POINT ( 'NONE',  ( 117.5348948014565593, -36.80252384088669260, 259.8213395616249386 ) ) ;
#82422 = CARTESIAN_POINT ( 'NONE',  ( 97.31584368291662202, -39.30597587107634894, 156.5314585988082285 ) ) ;
#82423 = CARTESIAN_POINT ( 'NONE',  ( 70.99299999999999500, 82.54999999999999716, 358.0130000000000337 ) ) ;
#82424 = VECTOR ( 'NONE', #57755, 1000.000000000000000 ) ;
#82426 = LINE ( 'NONE', #41054, #32698 ) ;
#82425 = DIRECTION ( 'NONE',  ( -1.000000000000000078E-15, 1.000000000000000083E-30, 1.000000000000000000 ) ) ;
#82427 = CARTESIAN_POINT ( 'NONE',  ( 120.2221484686747317, -111.8737466215628871, -21.78219314458179667 ) ) ;
#82428 = CIRCLE ( 'NONE', #43221, 2.999999999999919176 ) ;
#82429 = EDGE_CURVE ( 'NONE', #16666, #43971, #67760, .T. ) ;
#82430 = CARTESIAN_POINT ( 'NONE',  ( 131.3164832912739826, -18.72944715994100662, 3.101481641215524832 ) ) ;
#82431 = ADVANCED_FACE ( 'NONE', ( #60477 ), #52301, .F. ) ;
#82432 = EDGE_LOOP ( 'NONE', ( #74714, #7521, #47130, #3924 ) ) ;
#82433 = EDGE_LOOP ( 'NONE', ( #71781, #8117 ) ) ;
#82434 = CARTESIAN_POINT ( 'NONE',  ( 98.57243884988349691, -37.62796858414048273, 125.8324198280769650 ) ) ;
#82436 = VERTEX_POINT ( 'NONE', #31889 ) ;
#82435 = CARTESIAN_POINT ( 'NONE',  ( 20.42678914444644889, 45.07398772557888122, 32.16741729433402242 ) ) ;
#82437 = DIRECTION ( 'NONE',  ( -1.000000000000000078E-15, 1.000000000000000083E-30, 1.000000000000000000 ) ) ;
#82438 = CARTESIAN_POINT ( 'NONE',  ( 113.9025887763447997, -28.07314977735667938, 120.5565776568639507 ) ) ;
#82439 = CARTESIAN_POINT ( 'NONE',  ( 98.30745143774481676, -41.72867539435345208, 147.7403404978439880 ) ) ;
#82440 = EDGE_CURVE ( 'NONE', #69114, #84182, #46841, .T. ) ;
#82441 = CARTESIAN_POINT ( 'NONE',  ( -47.02966122971774610, 92.07499999999998863, 74.26049396966043048 ) ) ;
#82442 = CARTESIAN_POINT ( 'NONE',  ( -79.21825297796402765, 71.54629894495528220, 88.20503424218303223 ) ) ;
#82443 = DIRECTION ( 'NONE',  ( 0.1811243268507065352, -0.9834602067307444129, 0.000000000000000000 ) ) ;
#82444 = CARTESIAN_POINT ( 'NONE',  ( 109.7352083718000415, -46.17358189742688523, 72.79562527591099297 ) ) ;
#82445 = ORIENTED_EDGE ( 'NONE', *, *, #4315, .T. ) ;
#82446 = EDGE_LOOP ( 'NONE', ( #40387, #69584, #27277, #76645 ) ) ;
#82447 = ORIENTED_EDGE ( 'NONE', *, *, #16301, .T. ) ;
#82448 = VECTOR ( 'NONE', #82878, 1000.000000000000000 ) ;
#82449 = VECTOR ( 'NONE', #21399, 1000.000000000000114 ) ;
#82450 = CARTESIAN_POINT ( 'NONE',  ( 70.14948329127297200, -1.929447159941395817, 352.4506252759079530 ) ) ;
#82452 = CARTESIAN_POINT ( 'NONE',  ( 107.0664832912739683, -24.97944715994095333, 307.1356252759109680 ) ) ;
#82451 = CARTESIAN_POINT ( 'NONE',  ( 103.1701080265564912, -27.72257962874998327, 151.4013395616249511 ) ) ;
#82453 = LINE ( 'NONE', #75626, #27482 ) ;
#82454 = LINE ( 'NONE', #56501, #49449 ) ;
#82455 = B_SPLINE_CURVE_WITH_KNOTS ( 'NONE', 3,
 ( #84384, #8055, #56636, #27153, #55278, #28954, #22153, #41209, #40772, #34858, #14884, #28487, #48911, #83037, #76650, #49372, #48455, #55717, #21698, #68496, #62564, #63007, #62114, #82591, #41653, #789 ),
 .UNSPECIFIED., .F., .F.,
 ( 4, 2, 2, 2, 2, 2, 2, 2, 2, 2, 2, 2, 4 ),
 ( 0.01987186023414422298, 0.02111327400948154187, 0.02235468778481886076, 0.02483751533549349855, 0.02607892911083080009, 0.02732034288616810164, 0.02980317043684273595, 0.03228599798751737027, 0.03352741176285468222, 0.03476882553819198723, 0.03725165308886659726, 0.03849306686420389534, 0.03973448063954120035 ),
 .UNSPECIFIED. ) ;
#82456 = DIRECTION ( 'NONE',  ( 0.000000000000000000, 0.000000000000000000, 1.000000000000000000 ) ) ;
#82457 = EDGE_CURVE ( 'NONE', #27929, #27593, #47221, .T. ) ;
#82458 = AXIS2_PLACEMENT_3D ( 'NONE', #86368, #71845, #44555 ) ;
#82459 = CARTESIAN_POINT ( 'NONE',  ( 57.56670390244808289, -42.82844715994040286, 257.2178068554150627 ) ) ;
#82460 = DIRECTION ( 'NONE',  ( 0.000000000000000000, -0.4999999999999921174, -0.8660254037844431485 ) ) ;
#82461 = ADVANCED_FACE ( 'NONE', ( #74571 ), #66861, .F. ) ;
#82462 = CARTESIAN_POINT ( 'NONE',  ( 97.24623519876071498, -31.70684325556592853, 95.96229194257799122 ) ) ;
#82463 = EDGE_LOOP ( 'NONE', ( #27287, #15766, #11274, #83573 ) ) ;
#82464 = ORIENTED_EDGE ( 'NONE', *, *, #18573, .F. ) ;
#82465 = ORIENTED_EDGE ( 'NONE', *, *, #15464, .F. ) ;
#82466 = ADVANCED_FACE ( 'NONE', ( #73678 ), #45839, .F. ) ;
#82467 = DIRECTION ( 'NONE',  ( -1.000000000000000000, 0.000000000000000000, 0.000000000000000000 ) ) ;
#82468 = CARTESIAN_POINT ( 'NONE',  ( -92.90667244829720062, 95.24968527363475346, -91.72735010416646162 ) ) ;
#82469 = CIRCLE ( 'NONE', #54792, 2.750000000000002665 ) ;
#82470 = ADVANCED_FACE ( 'NONE', ( #74134, #5089 ), #87315, .T. ) ;
#82471 = AXIS2_PLACEMENT_3D ( 'NONE', #64852, #69880, #43942 ) ;
#82472 = DIRECTION ( 'NONE',  ( 0.000000000000000000, 0.000000000000000000, 1.000000000000000000 ) ) ;
#82473 = CARTESIAN_POINT ( 'NONE',  ( 115.5869623526398016, -35.21209367091628906, 196.7728522743529425 ) ) ;
#82474 = CARTESIAN_POINT ( 'NONE',  ( 122.2189888861420286, -96.57077177933004464, -19.18411693322927292 ) ) ;
#82475 = ORIENTED_EDGE ( 'NONE', *, *, #86857, .F. ) ;
#82477 = ORIENTED_EDGE ( 'NONE', *, *, #28024, .F. ) ;
#82476 = ORIENTED_EDGE ( 'NONE', *, *, #31763, .F. ) ;
#82478 = VECTOR ( 'NONE', #83606, 1000.000000000000000 ) ;
#82479 = DIRECTION ( 'NONE',  ( 1.000000000000000000, 3.999999999999999995E-14, 1.000000000000000078E-15 ) ) ;
#82480 = CARTESIAN_POINT ( 'NONE',  ( 136.4640758026638991, -20.08864647350496924, 2.654395117688020278 ) ) ;
#82481 = VERTEX_POINT ( 'NONE', #34125 ) ;
#82482 = ORIENTED_EDGE ( 'NONE', *, *, #21486, .T. ) ;
#82483 = CARTESIAN_POINT ( 'NONE',  ( 107.0667039024470313, -104.2784471599421323, -21.78219314458201694 ) ) ;
#82484 = CARTESIAN_POINT ( 'NONE',  ( 112.2971567814265512, -43.88265157833087926, 224.5101547344679886 ) ) ;
#82485 = AXIS2_PLACEMENT_3D ( 'NONE', #26365, #46784, #47235 ) ;
#82486 = CARTESIAN_POINT ( 'NONE',  ( 173.9900000000000091, 68.61249999999999716, -53.61543552338530105 ) ) ;
#82487 = AXIS2_PLACEMENT_3D ( 'NONE', #24331, #2558, #30259 ) ;
#82488 = CARTESIAN_POINT ( 'NONE',  ( -113.3591856336701937, 69.18138141856444179, 64.76768199333514531 ) ) ;
#82489 = EDGE_LOOP ( 'NONE', ( #34087, #84682 ) ) ;
#82490 = EDGE_LOOP ( 'NONE', ( #25398, #45294, #83090, #82558 ) ) ;
#82491 = DIRECTION ( 'NONE',  ( 0.9068632946707807507, -0.4214249218767881500, 1.031805784967618114E-15 ) ) ;
#82492 = EDGE_LOOP ( 'NONE', ( #62453, #21708, #64791, #47363 ) ) ;
#82493 = B_SPLINE_CURVE_WITH_KNOTS ( 'NONE', 3,
 ( #7559, #13921, #20299, #47065, #6216, #83412, #7111, #76598, #75257, #67988, #14381, #5769, #42056, #35244, #41157, #88892, #54320, #34802, #19836, #13472, #33460, #34350, #20734, #26644, #82089, #41600, #69783, #62953, #48404, #68885 ),
 .UNSPECIFIED., .F., .F.,
 ( 4, 2, 1, 1, 1, 1, 1, 1, 2, 2, 2, 2, 2, 2, 2, 2, 2, 4 ),
 ( 0.5000144061015490138, 0.5001364728969340812, 0.5002585396923192596, 0.5005026732830898384, 0.5009909404646311071, 0.5019674748277139775, 0.5039205435538794964, 0.5078266810062112002, 0.5156389559108744969, 0.5312635057202012012, 0.5625126053388546099, 0.6250108045761610942, 0.6875090038134675785, 0.7500072030507740628, 0.8125054022880805471, 0.8750036015253870314, 0.9375018007626936267, 1.000000000000000000 ),
 .UNSPECIFIED. ) ;
#82494 = ORIENTED_EDGE ( 'NONE', *, *, #83547, .T. ) ;
#82495 = CARTESIAN_POINT ( 'NONE',  ( 99.99635294717694478, -42.73853927783394369, 224.7052332267339807 ) ) ;
#82496 = CARTESIAN_POINT ( 'NONE',  ( 109.0765542020472907, -47.62233732142709641, 127.7337205140059382 ) ) ;
#82497 = CARTESIAN_POINT ( 'NONE',  ( 96.05879824974435621, -41.05137697672059716, 96.62419670448197451 ) ) ;
#82498 = CARTESIAN_POINT ( 'NONE',  ( 106.1381103904814012, -44.89503369465886351, 249.5838068554170377 ) ) ;
#82499 = CARTESIAN_POINT ( 'NONE',  ( 32.16397622746005425, -34.03355364505773650, 342.9256252759109884 ) ) ;
#82500 = CARTESIAN_POINT ( 'NONE',  ( 104.4537254180046375, -26.63707460721619213, 196.2784824187679362 ) ) ;
#82501 = DIRECTION ( 'NONE',  ( -0.02992792722492364568, 3.665114028111763974E-18, 0.9995520592605569021 ) ) ;
#82502 = ORIENTED_EDGE ( 'NONE', *, *, #2639, .F. ) ;
#82503 = CARTESIAN_POINT ( 'NONE',  ( -130.0566129357925433, 76.91670260214422683, 11.41267162807883118 ) ) ;
#82504 = VERTEX_POINT ( 'NONE', #963 ) ;
#82505 = CIRCLE ( 'NONE', #67954, 7.837499999999996803 ) ;
#82506 = VERTEX_POINT ( 'NONE', #21869 ) ;
#82507 = DIRECTION ( 'NONE',  ( 1.000000000000000078E-15, -1.000000000000000000, 0.000000000000000000 ) ) ;
#82508 = VERTEX_POINT ( 'NONE', #14603 ) ;
#82509 = TOROIDAL_SURFACE ( 'NONE', #75230, 13.50000000000000000, 0.5000000000000000000 ) ;
#82510 = CARTESIAN_POINT ( 'NONE',  ( 87.31648329127403940, -46.47944715994105280, -5.074374724089048883 ) ) ;
#82511 = VECTOR ( 'NONE', #35064, 1000.000000000000000 ) ;
#82512 = CARTESIAN_POINT ( 'NONE',  ( 113.3425240358415778, -27.63052414531908596, 89.60800622829195561 ) ) ;
#82513 = CARTESIAN_POINT ( 'NONE',  ( -7.575738673516524635, 72.34850935353102841, 130.3362775872886061 ) ) ;
#82514 = CARTESIAN_POINT ( 'NONE',  ( 136.7838203269360520, -36.30343833342887905, 6.798133076502122840 ) ) ;
#82515 = LINE ( 'NONE', #48385, #20909 ) ;
#82516 = EDGE_CURVE ( 'NONE', #50313, #66470, #22622, .T. ) ;
#82519 = CARTESIAN_POINT ( 'NONE',  ( 116.8369567342159456, -40.30247308064090817, 214.5470538473389581 ) ) ;
#82518 = DIRECTION ( 'NONE',  ( 0.000000000000000000, -1.000000000000000000, 0.000000000000000000 ) ) ;
#82517 = DIRECTION ( 'NONE',  ( 0.000000000000000000, 0.000000000000000000, -1.000000000000000000 ) ) ;
#82520 = FACE_OUTER_BOUND ( 'NONE', #50432, .T. ) ;
#82521 = CARTESIAN_POINT ( 'NONE',  ( 154.5667039024469886, -67.87844715994090450, 190.2178068554179902 ) ) ;
#82522 = ORIENTED_EDGE ( 'NONE', *, *, #74813, .F. ) ;
#82523 = CARTESIAN_POINT ( 'NONE',  ( 97.81252181392954981, -40.51708140501057187, 272.6353344860016819 ) ) ;
#82525 = EDGE_CURVE ( 'NONE', #12182, #65108, #21415, .T. ) ;
#82524 = AXIS2_PLACEMENT_3D ( 'NONE', #49710, #7941, #85609 ) ;
#82526 = DIRECTION ( 'NONE',  ( 1.000000000000000000, 0.000000000000000000, 2.108231265501709878E-16 ) ) ;
#82527 = CARTESIAN_POINT ( 'NONE',  ( 41.56648329127398966, -27.57844715994070484, 315.9256252759120116 ) ) ;
#82528 = VECTOR ( 'NONE', #52336, 1000.000000000000000 ) ;
#82529 = EDGE_CURVE ( 'NONE', #13668, #71916, #76371, .T. ) ;
#82530 = DIRECTION ( 'NONE',  ( -0.000000000000000000, 1.000000000000000000, -0.000000000000000000 ) ) ;
#82532 = ORIENTED_EDGE ( 'NONE', *, *, #3466, .T. ) ;
#82531 = CARTESIAN_POINT ( 'NONE',  ( 96.20350199017366322, -34.44722874799195722, 261.1737205140063338 ) ) ;
#82533 = ADVANCED_FACE ( 'NONE', ( #34578 ), #28664, .T. ) ;
#82534 = DIRECTION ( 'NONE',  ( -0.2588190451025281225, 0.000000000000000000, 0.9659258262890663138 ) ) ;
#82535 = CARTESIAN_POINT ( 'NONE',  ( 117.7016330746719035, -39.82606306527180351, 138.5889586092439743 ) ) ;
#82536 = CARTESIAN_POINT ( 'NONE',  ( 112.9631696212496905, -28.13226286662721165, 40.59848241876795782 ) ) ;
#82537 = CARTESIAN_POINT ( 'NONE',  ( 117.3528398777633299, -34.78421141941176842, 154.9756252759109714 ) ) ;
#82538 = LINE ( 'NONE', #7109, #80814 ) ;
#82539 = VECTOR ( 'NONE', #67980, 1000.000000000000000 ) ;
#82540 = LINE ( 'NONE', #47968, #8366 ) ;
#82542 = CYLINDRICAL_SURFACE ( 'NONE', #18172, 3.000000000000002665 ) ;
#82541 = PLANE ( 'NONE',  #31825 ) ;
#82543 = CARTESIAN_POINT ( 'NONE',  ( 97.06107108305931774, -37.99641184612347189, 191.4272919332322545 ) ) ;
#82544 = CARTESIAN_POINT ( 'NONE',  ( 107.0667039024470313, -104.2784471599418197, -11.78219314458200984 ) ) ;
#82545 = ORIENTED_EDGE ( 'NONE', *, *, #8262, .T. ) ;
#82546 = ADVANCED_FACE ( 'NONE', ( #70462 ), #41382, .F. ) ;
#82547 = EDGE_CURVE ( 'NONE', #73595, #89539, #83644, .T. ) ;
#82548 = VERTEX_POINT ( 'NONE', #35023 ) ;
#82549 = VERTEX_POINT ( 'NONE', #77273 ) ;
#82550 = ORIENTED_EDGE ( 'NONE', *, *, #84700, .T. ) ;
#82551 = DIRECTION ( 'NONE',  ( 0.000000000000000000, 0.000000000000000000, -1.000000000000000000 ) ) ;
#82552 = CARTESIAN_POINT ( 'NONE',  ( 111.1204619107249556, -46.98756979654999810, 18.88800622829195319 ) ) ;
#82553 = DIRECTION ( 'NONE',  ( 0.000000000000000000, 1.000000000000000000, 0.000000000000000000 ) ) ;
#82554 = EDGE_CURVE ( 'NONE', #34288, #40430, #7334, .T. ) ;
#82555 = CARTESIAN_POINT ( 'NONE',  ( 116.4921925463200552, -40.17707423577839876, 118.5492147079741585 ) ) ;
#82556 = DIRECTION ( 'NONE',  ( 0.000000000000000000, 0.4999999999999897304, 0.8660254037844445918 ) ) ;
#82557 = CARTESIAN_POINT ( 'NONE',  ( 107.4298862253102698, -45.26314917194000742, 237.0324198280769679 ) ) ;
#82558 = ORIENTED_EDGE ( 'NONE', *, *, #46986, .T. ) ;
#82560 = ADVANCED_FACE ( 'NONE', ( #49540 ), #6430, .T. ) ;
#82559 = AXIS2_PLACEMENT_3D ( 'NONE', #9695, #45087, #72812 ) ;
#82561 = ORIENTED_EDGE ( 'NONE', *, *, #86345, .T. ) ;
#82562 = VERTEX_POINT ( 'NONE', #55895 ) ;
#82563 = CARTESIAN_POINT ( 'NONE',  ( 125.9611475301394847, -14.72944715994102616, 249.5838068554164693 ) ) ;
#82564 = DIRECTION ( 'NONE',  ( 1.907762142705490052E-15, 7.167082501179359715E-16, -1.000000000000000000 ) ) ;
#82565 = CARTESIAN_POINT ( 'NONE',  ( 37.36643805256732520, -48.62818131006020650, 300.4678068554150059 ) ) ;
#82566 = DIRECTION ( 'NONE',  ( -0.2588190451025166317, 0.000000000000000000, -0.9659258262890694224 ) ) ;
#82567 = CARTESIAN_POINT ( 'NONE',  ( 7.661254700127822836, 98.64746158385918307, 320.6630000000000109 ) ) ;
#82568 = DIRECTION ( 'NONE',  ( 0.000000000000000000, 0.000000000000000000, 1.000000000000000000 ) ) ;
#82569 = DIRECTION ( 'NONE',  ( 0.04216478779797398074, -0.9991106698809455455, 0.000000000000000000 ) ) ;
#82570 = CARTESIAN_POINT ( 'NONE',  ( 99.85651329992167291, -30.12038005267077878, 275.7356252759109907 ) ) ;
#82571 = CARTESIAN_POINT ( 'NONE',  ( -141.3509999999999991, 20.32000000000000028, 132.7150000000000034 ) ) ;
#82572 = ORIENTED_EDGE ( 'NONE', *, *, #65994, .T. ) ;
#82573 = EDGE_CURVE ( 'NONE', #89203, #2756, #70010, .T. ) ;
#82574 = VECTOR ( 'NONE', #45591, 1000.000000000000000 ) ;
#82575 = DIRECTION ( 'NONE',  ( 0.7071067811869263808, -0.7071067811861687646, 7.071067811869270740E-16 ) ) ;
#82576 = EDGE_CURVE ( 'NONE', #89264, #9747, #20956, .T. ) ;
#82577 = CARTESIAN_POINT ( 'NONE',  ( 36.65249034007441509, -48.32844715994130524, 180.4678068554150911 ) ) ;
#82578 = CARTESIAN_POINT ( 'NONE',  ( 102.8730905416367278, -29.69395531543277400, 83.32237608387698913 ) ) ;
#82579 = AXIS2_PLACEMENT_3D ( 'NONE', #47198, #75385, #11812 ) ;
#82580 = CIRCLE ( 'NONE', #2811, 1.000000000000000888 ) ;
#82581 = DIRECTION ( 'NONE',  ( 0.000000000000000000, 0.000000000000000000, -1.000000000000000000 ) ) ;
#82582 = CARTESIAN_POINT ( 'NONE',  ( 97.06107109773994068, -37.99641196776861563, 46.42729194290728856 ) ) ;
#82583 = ORIENTED_EDGE ( 'NONE', *, *, #45449, .T. ) ;
#82584 = CIRCLE ( 'NONE', #15851, 0.5000000000000004441 ) ;
#82585 = DIRECTION ( 'NONE',  ( 0.000000000000000000, 1.000000000000000000, 0.000000000000000000 ) ) ;
#82586 = VERTEX_POINT ( 'NONE', #49089 ) ;
#82587 = CARTESIAN_POINT ( 'NONE',  ( 95.56927879810542947, -39.60255952144336078, 166.5213395616259788 ) ) ;
#82588 = ORIENTED_EDGE ( 'NONE', *, *, #9303, .T. ) ;
#82589 = CARTESIAN_POINT ( 'NONE',  ( 145.2166182285888851, -69.56242951228074389, 247.5001056298889921 ) ) ;
#82590 = CARTESIAN_POINT ( 'NONE',  ( 107.8137748826309377, -27.36365403737595159, 111.4568214011349738 ) ) ;
#82591 = CARTESIAN_POINT ( 'NONE',  ( -0.8301440424157360276, 95.22976080284065858, 118.5538265829301281 ) ) ;
#82592 = CIRCLE ( 'NONE', #50666, 5.041900000000001825 ) ;
#82593 = DIRECTION ( 'NONE',  ( 1.000000000000000078E-15, -1.000000000000000000, 0.000000000000000000 ) ) ;
#82594 = CARTESIAN_POINT ( 'NONE',  ( 109.9169591795599388, -46.81676508990216234, 68.79562527591099297 ) ) ;
#82595 = ADVANCED_FACE ( 'NONE', ( #68663 ), #509, .F. ) ;
#82596 = LINE ( 'NONE', #341, #61845 ) ;
#82597 = ORIENTED_EDGE ( 'NONE', *, *, #33681, .F. ) ;
#82598 = DIRECTION ( 'NONE',  ( -0.2588190451025219607, 0.000000000000000000, -0.9659258262890678681 ) ) ;
#82599 = ORIENTED_EDGE ( 'NONE', *, *, #71364, .T. ) ;
#82600 = ORIENTED_EDGE ( 'NONE', *, *, #21249, .F. ) ;
#82601 = VECTOR ( 'NONE', #87624, 1000.000000000000000 ) ;
#82602 = DIRECTION ( 'NONE',  ( -0.7071067811865460184, 0.000000000000000000, 0.7071067811865489050 ) ) ;
#82603 = VERTEX_POINT ( 'NONE', #27318 ) ;
#82604 = CARTESIAN_POINT ( 'NONE',  ( 106.2788006184939888, -47.06957971430152554, 267.5280062282925542 ) ) ;
#82605 = CARTESIAN_POINT ( 'NONE',  ( 113.6281748933624556, -28.60039662530314430, 160.5356252759109736 ) ) ;
#82606 = CARTESIAN_POINT ( 'NONE',  ( 163.2449138992999735, -32.11662333284611748, 342.9256252759119548 ) ) ;
#82607 = DIRECTION ( 'NONE',  ( 0.000000000000000000, -0.000000000000000000, 1.000000000000000000 ) ) ;
#82608 = CARTESIAN_POINT ( 'NONE',  ( 106.8411897839350786, -48.57781660025092663, 73.56133956162497611 ) ) ;
#82609 = DIRECTION ( 'NONE',  ( 0.000000000000000000, 0.000000000000000000, 1.000000000000000000 ) ) ;
#82610 = VERTEX_POINT ( 'NONE', #54546 ) ;
#82611 = CARTESIAN_POINT ( 'NONE',  ( 97.80792351950141494, -40.51905676813210988, 116.6359120812046939 ) ) ;
#82612 = DIRECTION ( 'NONE',  ( 0.7071067811865344721, 0.000000000000000000, 0.7071067811865604513 ) ) ;
#82615 = ORIENTED_EDGE ( 'NONE', *, *, #47744, .F. ) ;
#82614 = EDGE_CURVE ( 'NONE', #68568, #38559, #54993, .T. ) ;
#82613 = AXIS2_PLACEMENT_3D ( 'NONE', #1680, #64348, #48891 ) ;
#82616 = PLANE ( 'NONE',  #60571 ) ;
#82617 = CARTESIAN_POINT ( 'NONE',  ( 51.24204729617327558, -31.76306994223702418, 342.9256252759109884 ) ) ;
#82618 = CARTESIAN_POINT ( 'NONE',  ( 104.8459308146384643, -26.52976224399699134, 260.2470538473397710 ) ) ;
#82619 = FACE_OUTER_BOUND ( 'NONE', #85607, .T. ) ;
#82620 = EDGE_CURVE ( 'NONE', #89126, #52429, #73370, .T. ) ;
#82621 = LINE ( 'NONE', #6293, #71062 ) ;
#82622 = LINE ( 'NONE', #63041, #83287 ) ;
#82623 = ADVANCED_FACE ( 'NONE', ( #20070 ), #14146, .F. ) ;
#82624 = CARTESIAN_POINT ( 'NONE',  ( 98.95807093800334542, -41.73853705562144967, 11.76800622829293808 ) ) ;
#82626 = CARTESIAN_POINT ( 'NONE',  ( 116.5135284680787322, -32.37261310794437463, 100.1699109901969535 ) ) ;
#82625 = CARTESIAN_POINT ( 'NONE',  ( 97.44822407315507462, -39.47994946543299477, 101.5486323904540029 ) ) ;
#82627 = DIRECTION ( 'NONE',  ( 0.000000000000000000, 1.000000000000000000, 0.000000000000000000 ) ) ;
#82628 = CARTESIAN_POINT ( 'NONE',  ( 114.2703446987665643, -45.17953892438131192, 153.1508633711489722 ) ) ;
#82629 = DIRECTION ( 'NONE',  ( 1.000000000000000000, 4.163336342344333240E-14, 0.000000000000000000 ) ) ;
#82630 = ORIENTED_EDGE ( 'NONE', *, *, #43328, .F. ) ;
#82631 = PLANE ( 'NONE',  #32335 ) ;
#82632 = EDGE_CURVE ( 'NONE', #38380, #37957, #76292, .T. ) ;
#82633 = FACE_BOUND ( 'NONE', #30792, .T. ) ;
#82634 = CARTESIAN_POINT ( 'NONE',  ( 107.0667039024470313, -104.2784471599409528, 250.2178068554179902 ) ) ;
#82635 = VERTEX_POINT ( 'NONE', #86325 ) ;
#82636 = VECTOR ( 'NONE', #69336, 1000.000000000000000 ) ;
#82637 = LINE ( 'NONE', #48955, #63578 ) ;
#82638 = EDGE_CURVE ( 'NONE', #75737, #21876, #24104, .T. ) ;
#82640 = VERTEX_POINT ( 'NONE', #50441 ) ;
#82639 = CARTESIAN_POINT ( 'NONE',  ( 95.26177648276406273, -38.28579333248966776, 151.4299109901969871 ) ) ;
#82641 = LINE ( 'NONE', #69437, #132 ) ;
#82642 = DIRECTION ( 'NONE',  ( 0.000000000000000000, -1.000000000000000000, 0.000000000000000000 ) ) ;
#82643 = CYLINDRICAL_SURFACE ( 'NONE', #27107, 118.5560000000000116 ) ;
#82645 = CARTESIAN_POINT ( 'NONE',  ( 194.0667039024479834, -40.32844715993407902, 300.4678068554149490 ) ) ;
#82644 = AXIS2_PLACEMENT_3D ( 'NONE', #3002, #9821, #66103 ) ;
#82646 = EDGE_LOOP ( 'NONE', ( #51675, #14415, #65768, #49951 ) ) ;
#82647 = AXIS2_PLACEMENT_3D ( 'NONE', #68833, #67474, #39324 ) ;
#82648 = EDGE_CURVE ( 'NONE', #55378, #83168, #36391, .T. ) ;
#82649 = ORIENTED_EDGE ( 'NONE', *, *, #65760, .F. ) ;
#82650 = EDGE_CURVE ( 'NONE', #53265, #83626, #66104, .T. ) ;
#82651 = ORIENTED_EDGE ( 'NONE', *, *, #31190, .F. ) ;
#82652 = ORIENTED_EDGE ( 'NONE', *, *, #32316, .T. ) ;
#82653 = DIRECTION ( 'NONE',  ( 0.000000000000000000, 0.000000000000000000, -1.000000000000000000 ) ) ;
#82654 = CARTESIAN_POINT ( 'NONE',  ( 96.70275196374477389, 93.55256755804781221, -87.71306776503814717 ) ) ;
#82655 = CARTESIAN_POINT ( 'NONE',  ( 51.03742451361634380, -23.42844715994068849, 180.4678068554151196 ) ) ;
#82656 = EDGE_CURVE ( 'NONE', #78195, #17392, #67539, .T. ) ;
#82657 = AXIS2_PLACEMENT_3D ( 'NONE', #64044, #28158, #55845 ) ;
#82659 = LINE ( 'NONE', #49434, #89253 ) ;
#82658 = CARTESIAN_POINT ( 'NONE',  ( 5.562599999999999767, 60.82030000000000314, 216.0269999999999868 ) ) ;
#82660 = FACE_OUTER_BOUND ( 'NONE', #3652, .T. ) ;
#82661 = ORIENTED_EDGE ( 'NONE', *, *, #32450, .T. ) ;
#82662 = VERTEX_POINT ( 'NONE', #64981 ) ;
#82663 = CIRCLE ( 'NONE', #75383, 10.00000000000000711 ) ;
#82664 = CARTESIAN_POINT ( 'NONE',  ( 107.0664832912739399, -36.72944715994095333, 292.6356252759106837 ) ) ;
#82665 = CARTESIAN_POINT ( 'NONE',  ( 1.224646799147354440E-15, 215.0000000000000000, 144.6557476874258441 ) ) ;
#82666 = CARTESIAN_POINT ( 'NONE',  ( 115.9419818307743668, -40.91744192719421847, 224.4756252759109714 ) ) ;
#82667 = CARTESIAN_POINT ( 'NONE',  ( 115.0667039024470313, -104.2784471599420897, -21.78219314458201694 ) ) ;
#82668 = CARTESIAN_POINT ( 'NONE',  ( 103.5129713284350146, -46.47169217660395191, 93.28610146638693834 ) ) ;
#82669 = DIRECTION ( 'NONE',  ( 0.000000000000000000, 0.000000000000000000, -1.000000000000000000 ) ) ;
#82670 = CARTESIAN_POINT ( 'NONE',  ( 97.33772894284302879, -34.07151874822147875, 22.11475355860416769 ) ) ;
#82671 = ORIENTED_EDGE ( 'NONE', *, *, #46285, .F. ) ;
#82672 = DIRECTION ( 'NONE',  ( -0.8660254037844379305, 0.000000000000000000, 0.5000000000000011102 ) ) ;
#82673 = EDGE_LOOP ( 'NONE', ( #81818, #23266, #62334, #51413, #38891, #39921 ) ) ;
#82674 = ORIENTED_EDGE ( 'NONE', *, *, #59704, .T. ) ;
#82675 = EDGE_CURVE ( 'NONE', #52659, #83508, #31117, .T. ) ;
#82676 = AXIS2_PLACEMENT_3D ( 'NONE', #35963, #13289, #15080 ) ;
#82677 = CARTESIAN_POINT ( 'NONE',  ( 21.03689327557705369, -23.42844715994186089, 313.9678068554150059 ) ) ;
#82678 = CARTESIAN_POINT ( 'NONE',  ( 101.2699428795238106, -44.12381293138377458, 273.4911071154209594 ) ) ;
#82679 = FACE_OUTER_BOUND ( 'NONE', #62964, .T. ) ;
#82680 = CARTESIAN_POINT ( 'NONE',  ( -118.4577320646418599, 94.30044247306076954, 4.871303722669348524 ) ) ;
#82681 = CARTESIAN_POINT ( 'NONE',  ( 180.3521107875676250, -35.65087443490890706, 342.9256252759109884 ) ) ;
#82682 = CARTESIAN_POINT ( 'NONE',  ( 89.55259891852614373, 73.00424585431356661, -77.69145367648771128 ) ) ;
#82683 = ORIENTED_EDGE ( 'NONE', *, *, #57215, .T. ) ;
#82684 = VECTOR ( 'NONE', #37411, 1000.000000000000000 ) ;
#82685 = DIRECTION ( 'NONE',  ( 0.000000000000000000, 0.000000000000000000, -1.000000000000000000 ) ) ;
#82686 = DIRECTION ( 'NONE',  ( -4.237773401492740281E-14, 1.000000000000000000, 0.000000000000000000 ) ) ;
#82687 = ORIENTED_EDGE ( 'NONE', *, *, #38305, .F. ) ;
#82688 = CARTESIAN_POINT ( 'NONE',  ( 110.5552498863747246, -46.59121243395724576, 37.84705384733994293 ) ) ;
#82689 = ORIENTED_EDGE ( 'NONE', *, *, #43091, .F. ) ;
#82690 = CARTESIAN_POINT ( 'NONE',  ( 115.2503885696571047, -36.58558574821132936, 286.6595189410200533 ) ) ;
#82691 = AXIS2_PLACEMENT_3D ( 'NONE', #12026, #67416, #40155 ) ;
#82692 = CARTESIAN_POINT ( 'NONE',  ( 101.9944482998265158, -45.44656310684662515, 127.1564288467080530 ) ) ;
#82693 = CARTESIAN_POINT ( 'NONE',  ( 111.5019814087853831, -26.53443175268781218, 134.7499109901969518 ) ) ;
#82694 = EDGE_CURVE ( 'NONE', #68161, #73068, #10024, .T. ) ;
#82695 = CARTESIAN_POINT ( 'NONE',  ( -12.70000000000000107, 82.54999999999999716, -129.9368274816650910 ) ) ;
#82696 = DIRECTION ( 'NONE',  ( 4.299999999999999979E-14, -1.000000000000000000, 4.400000000000000367E-29 ) ) ;
#82697 = CARTESIAN_POINT ( 'NONE',  ( 122.2221484686747601, -109.6038751290258944, -21.02845593540793345 ) ) ;
#82698 = CARTESIAN_POINT ( 'NONE',  ( 10.56818871369674717, 75.50703187974120567, 130.1275625430741627 ) ) ;
#82699 = CARTESIAN_POINT ( 'NONE',  ( 104.8319786719434603, -26.46567573359534364, 256.2470538473397710 ) ) ;
#82700 = CARTESIAN_POINT ( 'NONE',  ( 140.0667039024470171, -90.27844715994091018, 45.21780685541799727 ) ) ;
#82701 = CIRCLE ( 'NONE', #63822, 2.517500000000005844 ) ;
#82702 = ORIENTED_EDGE ( 'NONE', *, *, #67092, .F. ) ;
#82703 = EDGE_CURVE ( 'NONE', #4611, #56634, #65427, .T. ) ;
#82704 = EDGE_LOOP ( 'NONE', ( #30102, #31088, #22156, #53050, #89014 ) ) ;
#82705 = CARTESIAN_POINT ( 'NONE',  ( 101.7337754387761635, -26.99498644972499051, 96.46324432352997746 ) ) ;
#82706 = CARTESIAN_POINT ( 'NONE',  ( 172.5664832912729878, -27.57844715994070484, 201.9256252759119832 ) ) ;
#82707 = ORIENTED_EDGE ( 'NONE', *, *, #30260, .F. ) ;
#82708 = ORIENTED_EDGE ( 'NONE', *, *, #7479, .F. ) ;
#82709 = ORIENTED_EDGE ( 'NONE', *, *, #55324, .T. ) ;
#82710 = AXIS2_PLACEMENT_3D ( 'NONE', #81922, #47357, #62788 ) ;
#82711 = CARTESIAN_POINT ( 'NONE',  ( 109.7226905202519873, -27.00022865876807643, 159.8647339765212791 ) ) ;
#82712 = FACE_OUTER_BOUND ( 'NONE', #12711, .T. ) ;
#82713 = AXIS2_PLACEMENT_3D ( 'NONE', #52198, #17719, #52640 ) ;
#82714 = CARTESIAN_POINT ( 'NONE',  ( -72.96458098368751166, 127.0000000000000000, 72.96458098368620426 ) ) ;
#82715 = DIRECTION ( 'NONE',  ( 0.7071067811868696484, 0.7071067811862253860, 7.071067811868689941E-16 ) ) ;
#82716 = CARTESIAN_POINT ( 'NONE',  ( 100.0993174663912697, -32.47640984694866262, 168.7080903695919858 ) ) ;
#82717 = CARTESIAN_POINT ( 'NONE',  ( 115.9252781128442535, -30.08061567962537453, 260.3508633711493871 ) ) ;
#82718 = CARTESIAN_POINT ( 'NONE',  ( 100.8868427626595690, -44.69971354075113368, 58.05222648633483118 ) ) ;
#82719 = ORIENTED_EDGE ( 'NONE', *, *, #77289, .F. ) ;
#82720 = CARTESIAN_POINT ( 'NONE',  ( 130.4018701889609133, 93.55484823631827851, -6.352633250517150110 ) ) ;
#82721 = CIRCLE ( 'NONE', #78381, 3.000000864267354572 ) ;
#82722 = PLANE ( 'NONE',  #4118 ) ;
#82723 = ORIENTED_EDGE ( 'NONE', *, *, #26955, .T. ) ;
#82724 = VERTEX_POINT ( 'NONE', #79521 ) ;
#82725 = FACE_BOUND ( 'NONE', #36585, .T. ) ;
#82726 = EDGE_LOOP ( 'NONE', ( #28573, #24938, #8662, #65812, #28285 ) ) ;
#82727 = ORIENTED_EDGE ( 'NONE', *, *, #67681, .T. ) ;
#82728 = CARTESIAN_POINT ( 'NONE',  ( 162.7866693523280048, -29.62846900982320264, -5.074374724088000832 ) ) ;
#82729 = DIRECTION ( 'NONE',  ( -4.237773401492740281E-14, 1.000000000000000000, 0.000000000000000000 ) ) ;
#82730 = FACE_OUTER_BOUND ( 'NONE', #26497, .T. ) ;
#82731 = LINE ( 'NONE', #20496, #33067 ) ;
#82732 = EDGE_CURVE ( 'NONE', #71111, #71979, #72247, .T. ) ;
#82733 = AXIS2_PLACEMENT_3D ( 'NONE', #1172, #85645, #16588 ) ;
#82734 = CARTESIAN_POINT ( 'NONE',  ( 112.0552156641497703, -28.39979068407086515, 204.0695626852199496 ) ) ;
#82735 = CARTESIAN_POINT ( 'NONE',  ( 110.3859512856231788, -47.32161482583386913, 52.80610146638697699 ) ) ;
#82736 = CARTESIAN_POINT ( 'NONE',  ( 123.6837132603319418, -50.82895651782485658, 219.5838068554170093 ) ) ;
#82737 = EDGE_LOOP ( 'NONE', ( #87280, #23534, #30190, #75534 ) ) ;
#82738 = ADVANCED_FACE ( 'NONE', ( #30464 ), #43174, .F. ) ;
#82739 = CARTESIAN_POINT ( 'NONE',  ( -78.17938156622513191, 72.47328848629021536, -89.12695577293565918 ) ) ;
#82740 = EDGE_CURVE ( 'NONE', #66312, #21358, #60320, .T. ) ;
#82741 = VERTEX_POINT ( 'NONE', #58161 ) ;
#82742 = CARTESIAN_POINT ( 'NONE',  ( 87.31648329127402519, -54.62589567669624557, 14.92562527591095112 ) ) ;
#82743 = EDGE_CURVE ( 'NONE', #48254, #19996, #85892, .T. ) ;
#82744 = EDGE_LOOP ( 'NONE', ( #9593, #40124, #36711, #19331 ) ) ;
#82745 = DIRECTION ( 'NONE',  ( 9.351236661543306751E-17, -3.725950533538267725E-29, -1.000000000000000000 ) ) ;
#82746 = CARTESIAN_POINT ( 'NONE',  ( -12.43699715260042993, 80.48827657640002542, 117.9018778621280887 ) ) ;
#82747 = CARTESIAN_POINT ( 'NONE',  ( 112.1253770014904205, -45.36205269762271541, 132.9982990853162903 ) ) ;
#82748 = AXIS2_PLACEMENT_3D ( 'NONE', #5471, #59065, #81783 ) ;
#82749 = DIRECTION ( 'NONE',  ( 0.000000000000000000, 1.000000000000000000, 0.000000000000000000 ) ) ;
#82750 = VERTEX_POINT ( 'NONE', #3211 ) ;
#82751 = ADVANCED_FACE ( 'NONE', ( #17286 ), #22769, .F. ) ;
#82752 = CARTESIAN_POINT ( 'NONE',  ( 103.4695482323410118, -25.41149354249025549, 55.32133956162594046 ) ) ;
#82754 = CARTESIAN_POINT ( 'NONE',  ( 87.71474477836335382, 71.54617234588344843, -96.70122665881150681 ) ) ;
#82753 = CARTESIAN_POINT ( 'NONE',  ( 113.2448793187668059, -28.75819631133450116, 164.5523540477198026 ) ) ;
#82755 = DIRECTION ( 'NONE',  ( 0.000000000000000000, 0.000000000000000000, 1.000000000000000000 ) ) ;
#82756 = CARTESIAN_POINT ( 'NONE',  ( 132.2189018279154595, -16.68450975841260941, 2.186797062529802105 ) ) ;
#82757 = ORIENTED_EDGE ( 'NONE', *, *, #27765, .T. ) ;
#82758 = EDGE_CURVE ( 'NONE', #77844, #63421, #71369, .T. ) ;
#82759 = AXIS2_PLACEMENT_3D ( 'NONE', #33502, #10815, #59404 ) ;
#82760 = CARTESIAN_POINT ( 'NONE',  ( 97.56637869462663559, -33.41331154858068686, 122.0570635727724209 ) ) ;
#82761 = CARTESIAN_POINT ( 'NONE',  ( 128.2504969244201618, -12.91928723231331588, 394.9756252759100903 ) ) ;
#82763 = DIRECTION ( 'NONE',  ( -1.907762142705490052E-15, -7.167082501179359715E-16, 1.000000000000000000 ) ) ;
#82762 = AXIS2_PLACEMENT_3D ( 'NONE', #4201, #25083, #52747 ) ;
#82764 = VERTEX_POINT ( 'NONE', #58590 ) ;
#82765 = CARTESIAN_POINT ( 'NONE',  ( 96.77023068570494502, -38.49705603518268049, 87.46133956162493917 ) ) ;
#82767 = LINE ( 'NONE', #88678, #662 ) ;
#82766 = CARTESIAN_POINT ( 'NONE',  ( 112.0674640741628707, -45.48753058403565319, 172.9858083296317375 ) ) ;
#82768 = DIRECTION ( 'NONE',  ( 0.000000000000000000, -1.000000000000000000, 0.000000000000000000 ) ) ;
#82769 = VECTOR ( 'NONE', #31323, 999.9999999999998863 ) ;
#82770 = FACE_OUTER_BOUND ( 'NONE', #73278, .T. ) ;
#82771 = ORIENTED_EDGE ( 'NONE', *, *, #84262, .T. ) ;
#82772 = CARTESIAN_POINT ( 'NONE',  ( 113.7357275853186280, -44.67049210939290305, 144.1203871806719690 ) ) ;
#82773 = AXIS2_PLACEMENT_3D ( 'NONE', #5046, #32745, #4150 ) ;
#82775 = ORIENTED_EDGE ( 'NONE', *, *, #31923, .T. ) ;
#82774 = CARTESIAN_POINT ( 'NONE',  ( 107.0667039024470313, -104.2784471599409528, 24.21780685541800082 ) ) ;
#82776 = CARTESIAN_POINT ( 'NONE',  ( 112.6519946835718144, -45.50616226388157770, 259.0270538473393458 ) ) ;
#82777 = LINE ( 'NONE', #76833, #30956 ) ;
#82778 = LINE ( 'NONE', #27336, #83825 ) ;
#82779 = CARTESIAN_POINT ( 'NONE',  ( -178.3658777604659917, 20.32000000000000028, 122.9960808104842016 ) ) ;
#82780 = CARTESIAN_POINT ( 'NONE',  ( 99.09570909016483142, -30.55043173533305989, 81.80229194078304999 ) ) ;
#82781 = CARTESIAN_POINT ( 'NONE',  ( 67.06670390123206005, -137.6784471587259873, 245.4218662566639750 ) ) ;
#82782 = CARTESIAN_POINT ( 'NONE',  ( -100.2530235599234203, 77.68489675156570229, 83.63178471058918717 ) ) ;
#82783 = CARTESIAN_POINT ( 'NONE',  ( 109.9476544338203325, -26.76763818355050262, 214.8403871806739289 ) ) ;
#82784 = VERTEX_POINT ( 'NONE', #78188 ) ;
#82785 = ORIENTED_EDGE ( 'NONE', *, *, #61906, .F. ) ;
#82786 = EDGE_CURVE ( 'NONE', #25323, #41091, #821, .T. ) ;
#82787 = CARTESIAN_POINT ( 'NONE',  ( 105.9222987080832752, -26.72137021301569959, 156.5987261630399701 ) ) ;
#82788 = CARTESIAN_POINT ( 'NONE',  ( -492.0614999999999668, 14.28749999999982201, 85.72499999999999432 ) ) ;
#82790 = CARTESIAN_POINT ( 'NONE',  ( 79.31510987520702827, -34.05633243510678199, 1.690787911858491421 ) ) ;
#82789 = CARTESIAN_POINT ( 'NONE',  ( 105.1480534186857483, -26.53835308478808130, 276.2365776568628917 ) ) ;
#82791 = CARTESIAN_POINT ( 'NONE',  ( 46.03715912545348488, -48.62818131006090283, 129.9678068554150911 ) ) ;
#82792 = EDGE_CURVE ( 'NONE', #40647, #55396, #22312, .T. ) ;
#82793 = VECTOR ( 'NONE', #84194, 1000.000000000000000 ) ;
#82794 = LINE ( 'NONE', #46875, #73617 ) ;
#82795 = CYLINDRICAL_SURFACE ( 'NONE', #73474, 4.500000000000003553 ) ;
#82796 = AXIS2_PLACEMENT_3D ( 'NONE', #82427, #32445, #32903 ) ;
#82797 = DIRECTION ( 'NONE',  ( 0.000000000000000000, 0.000000000000000000, 1.000000000000000000 ) ) ;
#82798 = CARTESIAN_POINT ( 'NONE',  ( 13.40680633928205268, 239.0000000000000000, 102.7987842159323009 ) ) ;
#82799 = CARTESIAN_POINT ( 'NONE',  ( 107.2427983594548948, -47.16656068249886857, 212.5899109901969837 ) ) ;
#82800 = LINE ( 'NONE', #26027, #31530 ) ;
#82801 = ORIENTED_EDGE ( 'NONE', *, *, #27023, .F. ) ;
#82802 = EDGE_LOOP ( 'NONE', ( #40215, #75096, #87237, #80036 ) ) ;
#82803 = CARTESIAN_POINT ( 'NONE',  ( 50.03799999999999670, 101.5999999999999943, 191.3008000794699797 ) ) ;
#82804 = CARTESIAN_POINT ( 'NONE',  ( 78.57311110805129317, -16.41810224486967584, 1.981704920694429495 ) ) ;
#82805 = CARTESIAN_POINT ( 'NONE',  ( 38.10000000000000142, 95.25000000000000000, 358.0130000000000337 ) ) ;
#82806 = LINE ( 'NONE', #63233, #82511 ) ;
#82807 = CARTESIAN_POINT ( 'NONE',  ( 27.27158787008328389, 127.0000000000000000, 106.1020876358972629 ) ) ;
#82808 = VERTEX_POINT ( 'NONE', #8689 ) ;
#82809 = EDGE_CURVE ( 'NONE', #83014, #2756, #80655, .T. ) ;
#82810 = CARTESIAN_POINT ( 'NONE',  ( 97.44667640776515327, -32.59970075057101724, 12.00419670448293985 ) ) ;
#82811 = CARTESIAN_POINT ( 'NONE',  ( 97.55979742750555772, -43.80499729575070234, 261.8356252759109566 ) ) ;
#82812 = EDGE_LOOP ( 'NONE', ( #69571, #10528, #49155, #68996 ) ) ;
#82813 = CARTESIAN_POINT ( 'NONE',  ( -0.8330786292759821965, 95.14999999999997726, 118.5559999999999974 ) ) ;
#82814 = CARTESIAN_POINT ( 'NONE',  ( 36.65249034007526063, -48.32844715994123419, 300.4678068554150059 ) ) ;
#82815 = CARTESIAN_POINT ( 'NONE',  ( 111.4977754997606780, -45.70022213410786094, 167.9415684329345879 ) ) ;
#82816 = VECTOR ( 'NONE', #71612, 1000.000000000000000 ) ;
#82817 = CARTESIAN_POINT ( 'NONE',  ( 104.2561231690431782, -27.88649476002280636, 53.13951894101997908 ) ) ;
#82818 = CARTESIAN_POINT ( 'NONE',  ( 117.3128790654603080, -34.51798396817098080, 179.9956252759109532 ) ) ;
#82819 = VECTOR ( 'NONE', #40395, 1000.000000000000000 ) ;
#82820 = AXIS2_PLACEMENT_3D ( 'NONE', #83904, #48889, #63901 ) ;
#82821 = CARTESIAN_POINT ( 'NONE',  ( -240.5296158183964792, 93.66249999999999432, 90.48749999999999716 ) ) ;
#82822 = ORIENTED_EDGE ( 'NONE', *, *, #11365, .T. ) ;
#82823 = CARTESIAN_POINT ( 'NONE',  ( 182.0667039024469886, -33.35206098992630075, -5.074374724088000832 ) ) ;
#82824 = ORIENTED_EDGE ( 'NONE', *, *, #61988, .T. ) ;
#82826 = VERTEX_POINT ( 'NONE', #25423 ) ;
#82825 = VECTOR ( 'NONE', #70331, 1000.000000000000000 ) ;
#82827 = CARTESIAN_POINT ( 'NONE',  ( 0.8293608286808564767, 95.25000000000000000, 118.5560000000000258 ) ) ;
#82828 = ORIENTED_EDGE ( 'NONE', *, *, #44334, .T. ) ;
#82829 = ORIENTED_EDGE ( 'NONE', *, *, #23034, .T. ) ;
#82830 = DIRECTION ( 'NONE',  ( 0.000000000000000000, 1.000000000000000000, 0.000000000000000000 ) ) ;
#82831 = EDGE_CURVE ( 'NONE', #14469, #51166, #45842, .T. ) ;
#82832 = CARTESIAN_POINT ( 'NONE',  ( 114.8760577754623569, -30.96046336120327069, 108.7552769709339771 ) ) ;
#82833 = VECTOR ( 'NONE', #38890, 1000.000000000000000 ) ;
#82834 = CARTESIAN_POINT ( 'NONE',  ( 113.2331319966886412, -45.16264392691098806, 228.0784824187679760 ) ) ;
#82835 = CARTESIAN_POINT ( 'NONE',  ( 107.2427983594548948, -47.16656068249886857, 212.5899109901969837 ) ) ;
#82836 = CARTESIAN_POINT ( 'NONE',  ( 105.0216744116726630, -25.86700170375123520, 276.2365776568634033 ) ) ;
#82837 = PLANE ( 'NONE',  #84778 ) ;
#82838 = EDGE_CURVE ( 'NONE', #38868, #51146, #24985, .T. ) ;
#82839 = DIRECTION ( 'NONE',  ( 0.000000000000000000, 0.000000000000000000, 1.000000000000000000 ) ) ;
#82840 = AXIS2_PLACEMENT_3D ( 'NONE', #44382, #3505, #80279 ) ;
#82841 = EDGE_CURVE ( 'NONE', #7668, #32579, #41451, .T. ) ;
#82842 = ORIENTED_EDGE ( 'NONE', *, *, #55309, .T. ) ;
#82843 = CARTESIAN_POINT ( 'NONE',  ( 99.16769444712198833, -43.44866735504071187, 76.89943479972100704 ) ) ;
#82844 = CARTESIAN_POINT ( 'NONE',  ( 118.0351107906133876, -38.43300062509310067, 68.69181575210198787 ) ) ;
#82845 = CARTESIAN_POINT ( 'NONE',  ( 118.1498169324930529, -36.11903826555217023, 273.8822919425775808 ) ) ;
#82846 = ORIENTED_EDGE ( 'NONE', *, *, #79231, .T. ) ;
#82847 = CARTESIAN_POINT ( 'NONE',  ( 105.1109252617814604, -26.48919212138316581, 235.2270538473399313 ) ) ;
#82848 = DIRECTION ( 'NONE',  ( 0.000000000000000000, 0.000000000000000000, 1.000000000000000000 ) ) ;
#82849 = CARTESIAN_POINT ( 'NONE',  ( -23.27731929905162289, 53.97500000000000142, 30.16249999999999076 ) ) ;
#82850 = CARTESIAN_POINT ( 'NONE',  ( 115.0365814371429991, -42.90932526432983707, 24.30220417310802716 ) ) ;
#82851 = CARTESIAN_POINT ( 'NONE',  ( 194.0667039024480118, -40.32844715993407902, 249.9678068554149775 ) ) ;
#82853 = CARTESIAN_POINT ( 'NONE',  ( 165.9667039024474491, -26.71338133338628751, 237.4678068554150059 ) ) ;
#82852 = DIRECTION ( 'NONE',  ( 0.000000000000000000, 0.000000000000000000, 1.000000000000000000 ) ) ;
#82854 = FACE_OUTER_BOUND ( 'NONE', #52204, .T. ) ;
#82855 = LINE ( 'NONE', #63741, #70040 ) ;
#82856 = VECTOR ( 'NONE', #7836, 1000.000000000000000 ) ;
#82857 = CARTESIAN_POINT ( 'NONE',  ( 12.70000000000000284, 82.96441223327236969, -117.8738102209307783 ) ) ;
#82858 = ADVANCED_FACE ( 'NONE', ( #86771 ), #4089, .F. ) ;
#82859 = VECTOR ( 'NONE', #39601, 1000.000000000000000 ) ;
#82860 = CARTESIAN_POINT ( 'NONE',  ( 41.56648329127398966, -27.57844715994070484, 75.92562527591199739 ) ) ;
#82861 = ADVANCED_FACE ( 'NONE', ( #81318 ), #19505, .T. ) ;
#82862 = CARTESIAN_POINT ( 'NONE',  ( -24.79284581386642827, 184.0000000000000000, 0.000000000000000000 ) ) ;
#82863 = DIRECTION ( 'NONE',  ( 0.6960018342484241005, 0.6960018342484289855, -0.1765301488291779741 ) ) ;
#82865 = ORIENTED_EDGE ( 'NONE', *, *, #1851, .F. ) ;
#82864 = DIRECTION ( 'NONE',  ( 0.000000000000000000, 0.000000000000000000, 1.000000000000000000 ) ) ;
#82866 = PLANE ( 'NONE',  #46664 ) ;
#82867 = CARTESIAN_POINT ( 'NONE',  ( 118.1310582692406257, -36.20923403681121044, 268.8518157521014587 ) ) ;
#82868 = CARTESIAN_POINT ( 'NONE',  ( 114.1750726078950890, -45.19361863149571690, 144.1203871806729637 ) ) ;
#82869 = CARTESIAN_POINT ( 'NONE',  ( 115.8125398181975783, -30.97623284308500757, 250.2899109901966028 ) ) ;
#82870 = CARTESIAN_POINT ( 'NONE',  ( 21.56670390244634561, -23.42844715994195326, 180.4678068554150911 ) ) ;
#82872 = DIRECTION ( 'NONE',  ( 0.000000000000000000, 0.000000000000000000, 1.000000000000000000 ) ) ;
#82871 = DIRECTION ( 'NONE',  ( -0.9825752044165969590, -0.1858654558159821002, 0.000000000000000000 ) ) ;
#82873 = CARTESIAN_POINT ( 'NONE',  ( 77.89700433585413464, 82.54999999999999716, -59.93649209371462661 ) ) ;
#82874 = DIRECTION ( 'NONE',  ( 1.000000000000000000, 0.000000000000000000, 6.878358445406130340E-15 ) ) ;
#82875 = CIRCLE ( 'NONE', #4531, 10.00000000000000888 ) ;
#82876 = SHAPE_REPRESENTATION ( 'BR-Y-104', ( #46417, #69598, #15927, #66667, #85572, #46349, #1460, #74002, #37711, #14560, #87043, #82713, #26088, #53671, #76857, #7291 ), #75437 ) ;
#82877 = ORIENTED_EDGE ( 'NONE', *, *, #30359, .T. ) ;
#82878 = DIRECTION ( 'NONE',  ( 0.000000000000000000, 0.000000000000000000, -1.000000000000000000 ) ) ;
#82879 = ORIENTED_EDGE ( 'NONE', *, *, #8465, .T. ) ;
#82880 = CARTESIAN_POINT ( 'NONE',  ( 103.7755263489600281, -28.29248842296361133, 169.7828960185539415 ) ) ;
#82882 = ORIENTED_EDGE ( 'NONE', *, *, #73310, .F. ) ;
#82881 = DIRECTION ( 'NONE',  ( 0.000000000000000000, 0.000000000000000000, 1.000000000000000000 ) ) ;
#82883 = LINE ( 'NONE', #49214, #63433 ) ;
#82884 = CARTESIAN_POINT ( 'NONE',  ( 100.8994224252809033, -45.87202276647009569, 148.0918157521009562 ) ) ;
#82885 = DIRECTION ( 'NONE',  ( 0.7071067811874264253, -0.7071067811856686092, 7.071067811874271132E-16 ) ) ;
#82886 = CARTESIAN_POINT ( 'NONE',  ( 20.56670390244743984, -48.82844715994200158, 180.4678068554150911 ) ) ;
#82887 = VECTOR ( 'NONE', #72387, 1000.000000000000000 ) ;
#82888 = DIRECTION ( 'NONE',  ( 0.000000000000000000, 0.000000000000000000, 1.000000000000000000 ) ) ;
#82889 = DIRECTION ( 'NONE',  ( 0.000000000000000000, 0.000000000000000000, -1.000000000000000000 ) ) ;
#82890 = CARTESIAN_POINT ( 'NONE',  ( 98.49710108934563380, -31.94619897774420636, 110.9213395616259703 ) ) ;
#82891 = EDGE_LOOP ( 'NONE', ( #53337, #9298, #32466, #75983, #15828 ) ) ;
#82892 = ORIENTED_EDGE ( 'NONE', *, *, #6009, .T. ) ;
#82894 = ORIENTED_EDGE ( 'NONE', *, *, #70412, .F. ) ;
#82893 = VECTOR ( 'NONE', #67527, 1000.000000000000000 ) ;
#82895 = DIRECTION ( 'NONE',  ( 0.000000000000000000, 0.000000000000000000, 1.000000000000000000 ) ) ;
#82897 = LINE ( 'NONE', #46089, #83947 ) ;
#82896 = CARTESIAN_POINT ( 'NONE',  ( 96.12852455334832769, -38.72269610271986551, 197.4699109901959844 ) ) ;
#82898 = DIRECTION ( 'NONE',  ( 0.7071067811865753283, -0.7071067811865197061, 7.071067811865760309E-16 ) ) ;
#82900 = EDGE_CURVE ( 'NONE', #4612, #42888, #25518, .T. ) ;
#82899 = CARTESIAN_POINT ( 'NONE',  ( 162.0667039024470171, -79.67844715994088745, 222.2178068554179902 ) ) ;
#82901 = CARTESIAN_POINT ( 'NONE',  ( 152.0371591254582881, -47.82818131005588214, 300.4678068554149490 ) ) ;
#82902 = FACE_OUTER_BOUND ( 'NONE', #283, .T. ) ;
#82903 = CARTESIAN_POINT ( 'NONE',  ( 67.62649790207950673, -68.41612585961607351, 246.8806801031981877 ) ) ;
#82904 = CARTESIAN_POINT ( 'NONE',  ( 114.0662423116486082, -44.47333502991310183, 133.1613395616249989 ) ) ;
#82905 = VERTEX_POINT ( 'NONE', #66758 ) ;
#82906 = VERTEX_POINT ( 'NONE', #26323 ) ;
#82907 = VECTOR ( 'NONE', #41143, 1000.000000000000000 ) ;
#82908 = ORIENTED_EDGE ( 'NONE', *, *, #74819, .F. ) ;
#82909 = DIRECTION ( 'NONE',  ( 0.000000000000000000, -1.000000000000000000, 0.000000000000000000 ) ) ;
#82910 = DIRECTION ( 'NONE',  ( 1.000000000000000000, 4.163336342344333240E-14, 0.000000000000000000 ) ) ;
#82911 = CARTESIAN_POINT ( 'NONE',  ( 92.82872956494375671, -30.11307588647346023, 9.125625275910955736 ) ) ;
#82912 = CARTESIAN_POINT ( 'NONE',  ( 112.2491357751623582, -43.66061143999345262, 185.9176141791149917 ) ) ;
#82913 = EDGE_CURVE ( 'NONE', #53871, #6226, #10898, .T. ) ;
#82914 = CARTESIAN_POINT ( 'NONE',  ( 97.31582012341550580, -39.30591678905398112, 27.53171479399969712 ) ) ;
#82915 = ORIENTED_EDGE ( 'NONE', *, *, #67742, .F. ) ;
#82917 = EDGE_LOOP ( 'NONE', ( #11082, #78317, #22257, #18394, #56074, #66549 ) ) ;
#82916 = ORIENTED_EDGE ( 'NONE', *, *, #36415, .F. ) ;
#82918 = VECTOR ( 'NONE', #36620, 1000.000000000000000 ) ;
#82919 = PLANE ( 'NONE',  #53414 ) ;
#82920 = ORIENTED_EDGE ( 'NONE', *, *, #68658, .T. ) ;
#82921 = EDGE_LOOP ( 'NONE', ( #3185, #669, #56796, #44512 ) ) ;
#82922 = FACE_OUTER_BOUND ( 'NONE', #39622, .T. ) ;
#82923 = ADVANCED_FACE ( 'NONE', ( #31790 ), #52650, .F. ) ;
#82924 = CARTESIAN_POINT ( 'NONE',  ( 106.6421946519922983, -45.61100719954815474, 243.9701547344679682 ) ) ;
#82925 = EDGE_CURVE ( 'NONE', #16856, #4380, #86424, .T. ) ;
#82926 = ORIENTED_EDGE ( 'NONE', *, *, #7652, .F. ) ;
#82927 = VECTOR ( 'NONE', #50885, 1000.000000000000000 ) ;
#82928 = CARTESIAN_POINT ( 'NONE',  ( 51.56670390244799762, -33.35206098992650681, -5.074374724088000832 ) ) ;
#82929 = CARTESIAN_POINT ( 'NONE',  ( -125.9554655030170949, 66.44187932044889067, 34.35260500423783725 ) ) ;
#82930 = ORIENTED_EDGE ( 'NONE', *, *, #32572, .T. ) ;
#82931 = ORIENTED_EDGE ( 'NONE', *, *, #53008, .F. ) ;
#82932 = AXIS2_PLACEMENT_3D ( 'NONE', #58003, #43013, #1712 ) ;
#82933 = DIRECTION ( 'NONE',  ( -1.000000000000000078E-15, 1.000000000000000083E-30, 1.000000000000000000 ) ) ;
#82934 = ORIENTED_EDGE ( 'NONE', *, *, #49606, .T. ) ;
#82935 = ORIENTED_EDGE ( 'NONE', *, *, #40224, .T. ) ;
#82936 = EDGE_CURVE ( 'NONE', #52812, #20444, #38166, .T. ) ;
#82937 = CARTESIAN_POINT ( 'NONE',  ( 106.0563433008199752, -28.62948770221197137, 267.9938046553056665 ) ) ;
#82938 = CARTESIAN_POINT ( 'NONE',  ( 108.2792694979413568, -26.31707411447196421, 129.9841967044819739 ) ) ;
#82939 = CARTESIAN_POINT ( 'NONE',  ( 96.04673288144547882, -37.20790665022158805, 116.3489586092439652 ) ) ;
#82940 = CARTESIAN_POINT ( 'NONE',  ( 103.4004682572699920, -43.97339471306070635, 249.5838068554171514 ) ) ;
#82941 = CARTESIAN_POINT ( 'NONE',  ( 131.6729728819767047, -17.37149612621589156, 7.198162082950363860 ) ) ;
#82942 = CARTESIAN_POINT ( 'NONE',  ( 98.66592356458792779, -30.49631559909255074, 176.8184824187679567 ) ) ;
#82943 = CARTESIAN_POINT ( 'NONE',  ( 107.0667039024470313, -104.2784471599409528, 25.71780685541800437 ) ) ;
#82944 = EDGE_CURVE ( 'NONE', #35045, #56594, #65856, .T. ) ;
#82945 = FACE_OUTER_BOUND ( 'NONE', #83261, .T. ) ;
#82946 = ORIENTED_EDGE ( 'NONE', *, *, #28911, .F. ) ;
#82947 = CARTESIAN_POINT ( 'NONE',  ( 129.9368274816649489, 81.72130195885949888, 12.70000000000135643 ) ) ;
#82948 = ORIENTED_EDGE ( 'NONE', *, *, #36462, .F. ) ;
#82949 = VECTOR ( 'NONE', #12621, 1000.000000000000000 ) ;
#82950 = ORIENTED_EDGE ( 'NONE', *, *, #9625, .F. ) ;
#82951 = LINE ( 'NONE', #35216, #69228 ) ;
#82952 = AXIS2_PLACEMENT_3D ( 'NONE', #5438, #60828, #14035 ) ;
#82953 = LINE ( 'NONE', #4842, #37447 ) ;
#82954 = CIRCLE ( 'NONE', #25091, 4.000000000000002665 ) ;
#82955 = CARTESIAN_POINT ( 'NONE',  ( 97.74620163809125017, -42.67179083687646823, 141.7661014663869707 ) ) ;
#82956 = CARTESIAN_POINT ( 'NONE',  ( -10.54081325544818704, 75.46611757261116793, 130.1297836194693218 ) ) ;
#82957 = DIRECTION ( 'NONE',  ( 9.351236661543306751E-17, -3.725950533538267725E-29, -1.000000000000000000 ) ) ;
#82958 = DIRECTION ( 'NONE',  ( 0.000000000000000000, -1.000000000000000000, 0.000000000000000000 ) ) ;
#82961 = CARTESIAN_POINT ( 'NONE',  ( 96.21411768969888101, -32.03111041547180804, 207.0013395616249738 ) ) ;
#82960 = CYLINDRICAL_SURFACE ( 'NONE', #61545, 9.999999999999998224 ) ;
#82959 = CARTESIAN_POINT ( 'NONE',  ( 38.10000000000000142, 69.84999999999999432, 283.4005000000000223 ) ) ;
#82962 = CARTESIAN_POINT ( 'NONE',  ( 151.0371591254573787, -24.95799193692592866, 249.9678068554149490 ) ) ;
#82963 = DIRECTION ( 'NONE',  ( 1.000000000000000000, 0.000000000000000000, 0.000000000000000000 ) ) ;
#82964 = ORIENTED_EDGE ( 'NONE', *, *, #62995, .F. ) ;
#82965 = VECTOR ( 'NONE', #50764, 999.9999999999998863 ) ;
#82966 = CARTESIAN_POINT ( 'NONE',  ( 123.0079629938350223, -38.09664315643626509, 247.7440089327910755 ) ) ;
#82967 = ADVANCED_FACE ( 'NONE', ( #59928 ), #19062, .F. ) ;
#82968 = CYLINDRICAL_SURFACE ( 'NONE', #39858, 5.562599999999973122 ) ;
#82969 = EDGE_CURVE ( 'NONE', #47477, #44015, #25876, .T. ) ;
#82970 = DIRECTION ( 'NONE',  ( 1.175184669632759901E-16, -1.000000000000000000, -2.000000000000003705E-15 ) ) ;
#82971 = CIRCLE ( 'NONE', #55359, 3.500000000000003109 ) ;
#82972 = EDGE_CURVE ( 'NONE', #79496, #49561, #74477, .T. ) ;
#82973 = CARTESIAN_POINT ( 'NONE',  ( 51.56670390244678970, -32.29483332968566600, 117.4678068554150485 ) ) ;
#82975 = EDGE_LOOP ( 'NONE', ( #33639, #27218, #59344, #17436, #59362 ) ) ;
#82974 = CARTESIAN_POINT ( 'NONE',  ( 116.1780915764957740, -31.53023347274874055, 289.2384824187680579 ) ) ;
#82976 = LINE ( 'NONE', #12123, #24836 ) ;
#82977 = CARTESIAN_POINT ( 'NONE',  ( 98.13060510664840308, -43.27509626496242134, 106.8175300378159704 ) ) ;
#82978 = CARTESIAN_POINT ( 'NONE',  ( 116.3875994391314634, -31.98201348113981268, 40.20133956162496958 ) ) ;
#82979 = CARTESIAN_POINT ( 'NONE',  ( 105.7148016331714757, -24.90641244965552659, 156.1670538473399574 ) ) ;
#82980 = ADVANCED_FACE ( 'NONE', ( #59035 ), #11806, .T. ) ;
#82981 = DIRECTION ( 'NONE',  ( 0.000000000000000000, 0.000000000000000000, -1.000000000000000000 ) ) ;
#82982 = FACE_BOUND ( 'NONE', #7728, .T. ) ;
#82984 = CARTESIAN_POINT ( 'NONE',  ( 107.0667039024480260, -36.72944715994100306, 199.5838068554169809 ) ) ;
#82983 = LINE ( 'NONE', #74803, #8647 ) ;
#82985 = CARTESIAN_POINT ( 'NONE',  ( 112.1393456646557212, -28.01282279536882669, 189.6564586071203564 ) ) ;
#82986 = DIRECTION ( 'NONE',  ( 1.000000000000000078E-15, -1.000000000000000000, 0.000000000000000000 ) ) ;
#82987 = ORIENTED_EDGE ( 'NONE', *, *, #38990, .F. ) ;
#82988 = ORIENTED_EDGE ( 'NONE', *, *, #461, .T. ) ;
#82989 = VERTEX_POINT ( 'NONE', #52207 ) ;
#82990 = ORIENTED_EDGE ( 'NONE', *, *, #17970, .F. ) ;
#82991 = CARTESIAN_POINT ( 'NONE',  ( -126.4481529151155996, 44.45000000000000284, 32.49205688096009936 ) ) ;
#82992 = CARTESIAN_POINT ( 'NONE',  ( 113.4926247784320452, -28.54816540729044405, 75.54705384733995288 ) ) ;
#82993 = CARTESIAN_POINT ( 'NONE',  ( 63.03715912545637678, -24.42818131006026761, 193.9678068554150911 ) ) ;
#82994 = CARTESIAN_POINT ( 'NONE',  ( 145.3961078426698066, -139.2608187703180249, 246.1574457750005251 ) ) ;
#82995 = CARTESIAN_POINT ( 'NONE',  ( 115.0109179074633374, -28.97809521412381883, 190.4537205140059655 ) ) ;
#82996 = DIRECTION ( 'NONE',  ( 0.9068632946707805287, -0.4214249218767882055, 9.081056412856297650E-16 ) ) ;
#82997 = AXIS2_PLACEMENT_3D ( 'NONE', #58578, #51760, #44951 ) ;
#82998 = CARTESIAN_POINT ( 'NONE',  ( 108.8243102715920685, -46.27830423087877421, 277.1438483995053161 ) ) ;
#82999 = ORIENTED_EDGE ( 'NONE', *, *, #3257, .T. ) ;
#83000 = VERTEX_POINT ( 'NONE', #4985 ) ;
#83001 = ORIENTED_EDGE ( 'NONE', *, *, #16064, .F. ) ;
#83002 =( GEOMETRIC_REPRESENTATION_CONTEXT ( 3 ) GLOBAL_UNCERTAINTY_ASSIGNED_CONTEXT ( ( #16037 ) ) GLOBAL_UNIT_ASSIGNED_CONTEXT ( ( #48823, #16135, #77013 ) ) REPRESENTATION_CONTEXT ( 'NONE', 'WORKASPACE' ) );
#83003 = DIRECTION ( 'NONE',  ( 0.000000000000000000, 0.000000000000000000, -1.000000000000000000 ) ) ;
#83004 = CARTESIAN_POINT ( 'NONE',  ( 98.34974946644537397, -31.65678111301215836, 161.9064763829012463 ) ) ;
#83005 = CYLINDRICAL_SURFACE ( 'NONE', #23781, 2.000000000000001776 ) ;
#83006 = CARTESIAN_POINT ( 'NONE',  ( 113.2419700359208434, -28.75597482910771419, 274.5522191157403995 ) ) ;
#83008 = EDGE_CURVE ( 'NONE', #37391, #27515, #56040, .T. ) ;
#83007 = CARTESIAN_POINT ( 'NONE',  ( 57.56670390244832447, -48.82844715994039575, 254.7178068554150627 ) ) ;
#83009 = CARTESIAN_POINT ( 'NONE',  ( -71.77848634863190114, 127.0000000000000000, 77.39114642429879609 ) ) ;
#83010 = DIRECTION ( 'NONE',  ( 1.346944695195362088E-15, -1.000000000000000000, 3.469446951953620425E-31 ) ) ;
#83011 = CARTESIAN_POINT ( 'NONE',  ( 97.60228370312334789, -39.19771807597653179, 276.5299109901972088 ) ) ;
#83012 = FACE_BOUND ( 'NONE', #3677, .T. ) ;
#83014 = VERTEX_POINT ( 'NONE', #61281 ) ;
#83013 = CONICAL_SURFACE ( 'NONE', #16284, 11.57110091390439699, 0.7853981633974452814 ) ;
#83015 = CARTESIAN_POINT ( 'NONE',  ( 107.0664832912739257, -49.72944715994096043, 312.6356252759112522 ) ) ;
#83016 = CARTESIAN_POINT ( 'NONE',  ( 142.8821648370248170, -72.54478064608022692, 396.9756252759102040 ) ) ;
#83017 = CARTESIAN_POINT ( 'NONE',  ( 102.2720406957515991, -30.12315877573194101, 73.39380465530592801 ) ) ;
#83018 = CIRCLE ( 'NONE', #16290, 3.000000000000002665 ) ;
#83019 = VECTOR ( 'NONE', #360, 1000.000000000000000 ) ;
#83020 = EDGE_CURVE ( 'NONE', #87481, #8418, #34270, .T. ) ;
#83021 = EDGE_CURVE ( 'NONE', #54444, #58766, #66160, .T. ) ;
#83022 = CARTESIAN_POINT ( 'NONE',  ( 193.5667039024483529, -48.82844715993410034, 300.4678068554149490 ) ) ;
#83023 = VECTOR ( 'NONE', #50201, 1000.000000000000000 ) ;
#83024 = CARTESIAN_POINT ( 'NONE',  ( 113.2454986974503015, -28.75867294428107002, 44.55229194263754522 ) ) ;
#83025 = ORIENTED_EDGE ( 'NONE', *, *, #26512, .F. ) ;
#83026 = ORIENTED_EDGE ( 'NONE', *, *, #11762, .T. ) ;
#83027 = EDGE_CURVE ( 'NONE', #39332, #72160, #77960, .T. ) ;
#83028 = CYLINDRICAL_SURFACE ( 'NONE', #67249, 3.000000000000002665 ) ;
#83029 = ORIENTED_EDGE ( 'NONE', *, *, #61069, .T. ) ;
#83030 = CARTESIAN_POINT ( 'NONE',  ( 116.9043533071046568, -40.17956947857189220, 133.5584824187679658 ) ) ;
#83031 = ORIENTED_EDGE ( 'NONE', *, *, #62807, .T. ) ;
#83032 = VECTOR ( 'NONE', #25073, 1000.000000000000000 ) ;
#83033 = EDGE_CURVE ( 'NONE', #33210, #29629, #19758, .T. ) ;
#83034 = CARTESIAN_POINT ( 'NONE',  ( 104.4081007064180824, -46.45808915210482581, 68.36479194626816991 ) ) ;
#83035 = CARTESIAN_POINT ( 'NONE',  ( 115.6173342623064713, -34.29738501013303420, 145.4787261630399371 ) ) ;
#83036 = EDGE_CURVE ( 'NONE', #46741, #48304, #71150, .T. ) ;
#83037 = CARTESIAN_POINT ( 'NONE',  ( -8.387180980836955513, 92.12328101316225570, 118.2604483546762424 ) ) ;
#83038 = CARTESIAN_POINT ( 'NONE',  ( 90.06670420047028358, -137.6784471599409585, 55.21780685541800437 ) ) ;
#83039 = CARTESIAN_POINT ( 'NONE',  ( 96.63486483157898022, -37.29388950852173679, 72.36991099019596163 ) ) ;
#83040 = ADVANCED_FACE ( 'NONE', ( #77062 ), #15285, .F. ) ;
#83041 = CARTESIAN_POINT ( 'NONE',  ( -179.8898777604655095, 20.32000000000000028, 114.2999999999999972 ) ) ;
#83042 = VERTEX_POINT ( 'NONE', #75375 ) ;
#83043 = LINE ( 'NONE', #28044, #16453 ) ;
#83044 = ORIENTED_EDGE ( 'NONE', *, *, #79026, .T. ) ;
#83045 = ORIENTED_EDGE ( 'NONE', *, *, #80788, .T. ) ;
#83046 = EDGE_CURVE ( 'NONE', #38663, #26848, #57040, .T. ) ;
#83048 = CARTESIAN_POINT ( 'NONE',  ( 71.23990787207000608, 10.64204399490126463, 540.9756252759101471 ) ) ;
#83047 = AXIS2_PLACEMENT_3D ( 'NONE', #44864, #72593, #10356 ) ;
#83049 = ORIENTED_EDGE ( 'NONE', *, *, #54264, .F. ) ;
#83050 = CARTESIAN_POINT ( 'NONE',  ( 97.50674219252212538, -32.62548708300529654, 16.00419670448194154 ) ) ;
#83051 = CARTESIAN_POINT ( 'NONE',  ( 114.1899296859532171, -45.21130890035909999, 144.1203871806729637 ) ) ;
#83052 = CARTESIAN_POINT ( 'NONE',  ( 7.400192735666117905, 72.22046014531929359, -118.3253218772466511 ) ) ;
#83053 = LINE ( 'NONE', #48039, #5394 ) ;
#83054 = CARTESIAN_POINT ( 'NONE',  ( 101.6782318212999314, -27.07850282373152950, 101.4937205140059575 ) ) ;
#83055 = ADVANCED_FACE ( 'NONE', ( #8469 ), #42957, .T. ) ;
#83056 = CARTESIAN_POINT ( 'NONE',  ( 97.33810157587271306, -34.07000700935488169, 97.11433392722962310 ) ) ;
#83057 = EDGE_LOOP ( 'NONE', ( #53790, #73062 ) ) ;
#83058 = CARTESIAN_POINT ( 'NONE',  ( 97.79857776613020803, -40.48525735399483949, 116.6331486142001808 ) ) ;
#83059 = CARTESIAN_POINT ( 'NONE',  ( 104.4083119130582702, -46.45815109594069980, 158.3646258352321752 ) ) ;
#83060 = ORIENTED_EDGE ( 'NONE', *, *, #15228, .T. ) ;
#83061 = AXIS2_PLACEMENT_3D ( 'NONE', #31606, #80673, #37984 ) ;
#83062 = DIRECTION ( 'NONE',  ( 0.000000000000000000, 1.000000000000000000, 0.000000000000000000 ) ) ;
#83063 = CARTESIAN_POINT ( 'NONE',  ( 122.2221484686747317, -101.0284471599423171, -21.78219314458213063 ) ) ;
#83064 = CARTESIAN_POINT ( 'NONE',  ( 114.8195649486642225, -43.69914982757761379, 38.24419670448192221 ) ) ;
#83065 = FACE_OUTER_BOUND ( 'NONE', #48375, .T. ) ;
#83066 = CARTESIAN_POINT ( 'NONE',  ( 69.55653269757553403, 92.18234976669049274, 53.91899401579343731 ) ) ;
#83067 = DIRECTION ( 'NONE',  ( 0.000000000000000000, 0.000000000000000000, 1.000000000000000000 ) ) ;
#83068 = CARTESIAN_POINT ( 'NONE',  ( 115.6302422591030137, -36.57899571384957937, 288.2638483995053775 ) ) ;
#83070 = CARTESIAN_POINT ( 'NONE',  ( 114.7552509866191599, -44.63809267644810319, 114.2022919425779719 ) ) ;
#83069 = DIRECTION ( 'NONE',  ( 3.100000000000000258E-29, -3.100000000000000044E-14, -1.000000000000000000 ) ) ;
#83071 = DIRECTION ( 'NONE',  ( 0.7071067811864666375, 0.7071067811866283970, 7.071067811864659848E-16 ) ) ;
#83072 = CARTESIAN_POINT ( 'NONE',  ( 114.2052324763531743, -45.22952987728847063, 148.1203871806719405 ) ) ;
#83073 = DIRECTION ( 'NONE',  ( 1.000000000000000000, 4.299999999999999979E-14, 1.000000000000000078E-15 ) ) ;
#83074 = VERTEX_POINT ( 'NONE', #35708 ) ;
#83075 = CARTESIAN_POINT ( 'NONE',  ( 105.7995771162975416, -24.27178701759104840, 322.4846826458744431 ) ) ;
#83076 = FACE_OUTER_BOUND ( 'NONE', #30316, .T. ) ;
#83077 = PLANE ( 'NONE',  #20949 ) ;
#83078 = ORIENTED_EDGE ( 'NONE', *, *, #33941, .T. ) ;
#83079 = AXIS2_PLACEMENT_3D ( 'NONE', #82911, #49701, #21576 ) ;
#83080 = ADVANCED_FACE ( 'NONE', ( #84340 ), #68110, .T. ) ;
#83081 = DIRECTION ( 'NONE',  ( 0.7071067811873675835, 0.7071067811857274510, 7.071067811873668640E-16 ) ) ;
#83083 = ORIENTED_EDGE ( 'NONE', *, *, #42362, .T. ) ;
#83082 = CARTESIAN_POINT ( 'NONE',  ( 95.52074050172029729, -39.61468907688732344, 166.5213395616259788 ) ) ;
#83084 = DIRECTION ( 'NONE',  ( 7.076552332833900719E-16, -1.000000000000000000, 3.100000000000000044E-14 ) ) ;
#83085 = CARTESIAN_POINT ( 'NONE',  ( 115.4053350490088548, -30.43652969535880359, 215.3413395616249773 ) ) ;
#83086 = ADVANCED_FACE ( 'NONE', ( #35255 ), #82206, .T. ) ;
#83087 = CARTESIAN_POINT ( 'NONE',  ( 100.4327019155579137, 78.46683822717001533, 83.41556370846579682 ) ) ;
#83088 = DIRECTION ( 'NONE',  ( 0.000000000000000000, 1.000000000000000000, 0.000000000000000000 ) ) ;
#83089 = LINE ( 'NONE', #48507, #46704 ) ;
#83090 = ORIENTED_EDGE ( 'NONE', *, *, #9001, .T. ) ;
#83091 = VECTOR ( 'NONE', #73548, 1000.000000000000000 ) ;
#83092 = ORIENTED_EDGE ( 'NONE', *, *, #14837, .T. ) ;
#83093 = ORIENTED_EDGE ( 'NONE', *, *, #28078, .F. ) ;
#83094 = VECTOR ( 'NONE', #53304, 1000.000000000000000 ) ;
#83095 = EDGE_LOOP ( 'NONE', ( #85355, #20306, #81610, #85839 ) ) ;
#83096 = LINE ( 'NONE', #20849, #65554 ) ;
#83097 = CARTESIAN_POINT ( 'NONE',  ( 104.3244243092125032, -26.02173531178284804, 241.2880062282919482 ) ) ;
#83098 = DIRECTION ( 'NONE',  ( -0.000000000000000000, 0.000000000000000000, -1.000000000000000000 ) ) ;
#83099 = CARTESIAN_POINT ( 'NONE',  ( 135.0807008692694922, -16.17316201338588399, 1.785258157649496136 ) ) ;
#83101 = PLANE ( 'NONE',  #48548 ) ;
#83100 = FACE_OUTER_BOUND ( 'NONE', #20835, .T. ) ;
#83102 = CARTESIAN_POINT ( 'NONE',  ( 107.0664832912739968, -36.72944715994100306, 287.6356252759109680 ) ) ;
#83103 = ORIENTED_EDGE ( 'NONE', *, *, #67059, .F. ) ;
#83104 = ORIENTED_EDGE ( 'NONE', *, *, #42102, .F. ) ;
#83105 = DIRECTION ( 'NONE',  ( 0.000000000000000000, 1.000000000000000000, 0.000000000000000000 ) ) ;
#83106 = CARTESIAN_POINT ( 'NONE',  ( -33.98325472291465132, 17.78000000000000114, -3.174999999999764899 ) ) ;
#83107 = CARTESIAN_POINT ( 'NONE',  ( 116.7002268312855051, -35.03994406823841246, 239.9641967044819637 ) ) ;
#83108 = FACE_OUTER_BOUND ( 'NONE', #12567, .T. ) ;
#83109 = AXIS2_PLACEMENT_3D ( 'NONE', #17068, #24328, #45192 ) ;
#83110 = CARTESIAN_POINT ( 'NONE',  ( 107.3052971647831697, -26.36210646096938959, 71.04610146638695767 ) ) ;
#83111 = CARTESIAN_POINT ( 'NONE',  ( 41.56648329127399677, 0.2215528400590013880, 321.0426252759119734 ) ) ;
#83112 = DIRECTION ( 'NONE',  ( 0.6893610196960207048, -0.7071067811865335839, 0.1574210421884009170 ) ) ;
#83113 = ORIENTED_EDGE ( 'NONE', *, *, #69895, .F. ) ;
#83114 = DIRECTION ( 'NONE',  ( -0.8660254037844380415, -0.5000000000000012212, 1.550000000000001284E-14 ) ) ;
#83115 = ORIENTED_EDGE ( 'NONE', *, *, #69032, .F. ) ;
#83116 = ORIENTED_EDGE ( 'NONE', *, *, #8900, .T. ) ;
#83117 = ADVANCED_FACE ( 'NONE', ( #63883 ), #49328, .F. ) ;
#83118 = CARTESIAN_POINT ( 'NONE',  ( 84.06648329127399677, -18.82844715994099971, 239.5838068554169809 ) ) ;
#83119 = CARTESIAN_POINT ( 'NONE',  ( 101.9834712436270507, -43.98831800240917289, 278.5215833058970247 ) ) ;
#83120 = VECTOR ( 'NONE', #45011, 1000.000000000000000 ) ;
#83121 = LINE ( 'NONE', #41744, #44351 ) ;
#83122 = DIRECTION ( 'NONE',  ( 1.000000000000000000, 4.443626637970152463E-14, 0.000000000000000000 ) ) ;
#83123 = EDGE_CURVE ( 'NONE', #3990, #68783, #74869, .T. ) ;
#83124 = ADVANCED_FACE ( 'NONE', ( #62965 ), #33580, .F. ) ;
#83125 = CARTESIAN_POINT ( 'NONE',  ( 113.2454987016537302, -28.75867294776266903, 84.55229194220528655 ) ) ;
#83126 = CARTESIAN_POINT ( 'NONE',  ( 78.16952835488746132, 72.45860812971083931, -89.13771950014273671 ) ) ;
#83127 = ORIENTED_EDGE ( 'NONE', *, *, #80377, .F. ) ;
#83128 = CARTESIAN_POINT ( 'NONE',  ( 45.76696975232854925, -48.62818131006087441, 300.4678068554150059 ) ) ;
#83129 = EDGE_CURVE ( 'NONE', #72194, #13679, #27019, .T. ) ;
#83130 = DIRECTION ( 'NONE',  ( 1.000000000000000000, 4.443626637970137948E-14, 0.000000000000000000 ) ) ;
#83131 = VERTEX_POINT ( 'NONE', #1661 ) ;
#83132 = CARTESIAN_POINT ( 'NONE',  ( 96.71451373887593661, -37.96385262316839260, 41.42133956162496844 ) ) ;
#83133 = EDGE_LOOP ( 'NONE', ( #38947, #19150, #29769, #60166 ) ) ;
#83134 = CARTESIAN_POINT ( 'NONE',  ( 103.5342718762226895, -27.68543744656516026, 19.79527697093397265 ) ) ;
#83135 = ADVANCED_FACE ( 'NONE', ( #28446 ), #1205, .T. ) ;
#83136 = CARTESIAN_POINT ( 'NONE',  ( 90.44969454456405344, -20.11243780205715481, 218.0711402470150801 ) ) ;
#83137 = CARTESIAN_POINT ( 'NONE',  ( 102.3899016914588458, -28.13915478247111679, 145.4727681330539610 ) ) ;
#83138 = DIRECTION ( 'NONE',  ( 9.351236661543306751E-17, -3.725950533538267725E-29, -1.000000000000000000 ) ) ;
#83139 = CARTESIAN_POINT ( 'NONE',  ( 32.56670390244700997, -18.82844715994111340, -5.074374724088000832 ) ) ;
#83140 = DIRECTION ( 'NONE',  ( 1.000000000000000078E-15, -1.000000000000000083E-30, -1.000000000000000000 ) ) ;
#83141 = CARTESIAN_POINT ( 'NONE',  ( 6.301291950802956343, 71.51565506672721995, 130.4043135987251674 ) ) ;
#83142 = CARTESIAN_POINT ( 'NONE',  ( 106.1344768297789329, -47.78968505587090476, 258.4975300378158636 ) ) ;
#83143 = CARTESIAN_POINT ( 'NONE',  ( 99.97047271725682549, -43.84442383188222436, 116.9535692024431057 ) ) ;
#83144 = EDGE_CURVE ( 'NONE', #24254, #28103, #86114, .T. ) ;
#83145 = EDGE_LOOP ( 'NONE', ( #40763, #18343, #38138, #38042, #16429, #477 ) ) ;
#83146 = AXIS2_PLACEMENT_3D ( 'NONE', #63048, #78046, #14470 ) ;
#83147 = CARTESIAN_POINT ( 'NONE',  ( 180.1667039024476651, -26.71338133338667120, 117.4678068554150627 ) ) ;
#83148 = ORIENTED_EDGE ( 'NONE', *, *, #24870, .F. ) ;
#83149 = CARTESIAN_POINT ( 'NONE',  ( 114.5987772146603731, -44.05082428708011832, 94.21276813305395592 ) ) ;
#83150 = DIRECTION ( 'NONE',  ( -3.100000000000000258E-29, 3.100000000000000044E-14, 1.000000000000000000 ) ) ;
#83151 = AXIS2_PLACEMENT_3D ( 'NONE', #64167, #1938, #1492 ) ;
#83152 = ORIENTED_EDGE ( 'NONE', *, *, #81834, .F. ) ;
#83153 = ORIENTED_EDGE ( 'NONE', *, *, #67338, .F. ) ;
#83154 = ORIENTED_EDGE ( 'NONE', *, *, #77414, .F. ) ;
#83155 = EDGE_CURVE ( 'NONE', #1627, #61361, #59272, .T. ) ;
#83156 = FACE_OUTER_BOUND ( 'NONE', #49124, .T. ) ;
#83157 = PLANE ( 'NONE',  #41371 ) ;
#83158 = DIRECTION ( 'NONE',  ( 1.000000000000000000, 0.000000000000000000, 0.000000000000000000 ) ) ;
#83159 = DIRECTION ( 'NONE',  ( 0.000000000000000000, -1.000000000000000000, 0.000000000000000000 ) ) ;
#83160 = CARTESIAN_POINT ( 'NONE',  ( 98.44383420958352815, -35.98725590436672661, 184.0642808457819797 ) ) ;
#83161 = CARTESIAN_POINT ( 'NONE',  ( 104.5830001944168259, -26.58193179050359589, 281.2670538473395823 ) ) ;
#83162 = EDGE_CURVE ( 'NONE', #27981, #58550, #11124, .T. ) ;
#83163 = CARTESIAN_POINT ( 'NONE',  ( 97.81311576760518278, -40.52091172574487388, 57.63592544568884790 ) ) ;
#83164 = ORIENTED_EDGE ( 'NONE', *, *, #42865, .F. ) ;
#83165 = CARTESIAN_POINT ( 'NONE',  ( 148.0533267522752112, 101.5999999999999943, 160.2664750769284865 ) ) ;
#83166 = DIRECTION ( 'NONE',  ( 1.000000000000000000, 4.299999999999999979E-14, 1.000000000000000078E-15 ) ) ;
#83167 = ORIENTED_EDGE ( 'NONE', *, *, #41193, .T. ) ;
#83168 = VERTEX_POINT ( 'NONE', #85677 ) ;
#83169 = LINE ( 'NONE', #27735, #1011 ) ;
#83170 = CIRCLE ( 'NONE', #3398, 7.874000000000227928 ) ;
#83171 = DIRECTION ( 'NONE',  ( 0.1811243268507098381, -0.9834602067307437467, 0.000000000000000000 ) ) ;
#83172 = CARTESIAN_POINT ( 'NONE',  ( 97.70652731244065592, -40.25122769212212859, 16.61284818632429250 ) ) ;
#83173 = DIRECTION ( 'NONE',  ( 1.000000000000000000, 1.000000000000000078E-15, 1.000000000000000078E-15 ) ) ;
#83174 = DIRECTION ( 'NONE',  ( -1.000000000000000078E-15, 1.000000000000000000, 0.000000000000000000 ) ) ;
#83175 = CARTESIAN_POINT ( 'NONE',  ( 111.9460571495898620, -43.77514521526708080, 202.4809912566479397 ) ) ;
#83176 = CARTESIAN_POINT ( 'NONE',  ( 101.1158648436187235, -27.35912039304959009, 65.51467289495799662 ) ) ;
#83177 = DIRECTION ( 'NONE',  ( 0.7071067811865789920, -0.7071067811865159314, 0.000000000000000000 ) ) ;
#83178 = EDGE_LOOP ( 'NONE', ( #63895, #62611, #37345, #75180 ) ) ;
#83179 = CIRCLE ( 'NONE', #7756, 7.874000000000227928 ) ;
#83180 = LINE ( 'NONE', #20937, #6421 ) ;
#83181 = ORIENTED_EDGE ( 'NONE', *, *, #79124, .T. ) ;
#83182 = CARTESIAN_POINT ( 'NONE',  ( 116.3259296754763028, -32.93870509136930025, 260.1356252759109680 ) ) ;
#83183 = ORIENTED_EDGE ( 'NONE', *, *, #83036, .F. ) ;
#83184 = CARTESIAN_POINT ( 'NONE',  ( 113.5222875812157071, -29.01406153566750845, 165.5214312225362789 ) ) ;
#83185 = CARTESIAN_POINT ( 'NONE',  ( 151.0667039024469886, -67.87844715994090450, 155.2178068554179902 ) ) ;
#83186 = EDGE_CURVE ( 'NONE', #8752, #34742, #43861, .T. ) ;
#83187 = CARTESIAN_POINT ( 'NONE',  ( 117.0613444152393754, -38.07727497758394009, 274.7187601539478692 ) ) ;
#83188 = AXIS2_PLACEMENT_3D ( 'NONE', #58976, #40330, #74419 ) ;
#83189 = CARTESIAN_POINT ( 'NONE',  ( 177.3246001664173264, -48.34074026909179622, 249.9678068554149775 ) ) ;
#83190 = ORIENTED_EDGE ( 'NONE', *, *, #49696, .T. ) ;
#83191 = CARTESIAN_POINT ( 'NONE',  ( 101.9496561033292039, -27.62096520655628851, 60.48419670448296159 ) ) ;
#83193 = CARTESIAN_POINT ( 'NONE',  ( 194.0667039024480118, -40.32844715993407902, 249.9678068554149775 ) ) ;
#83192 = CARTESIAN_POINT ( 'NONE',  ( -27.27158787008326968, 184.0000000000000000, 111.9860621927989826 ) ) ;
#83194 = LINE ( 'NONE', #48184, #4688 ) ;
#83195 = DIRECTION ( 'NONE',  ( 0.000000000000000000, 0.000000000000000000, 1.000000000000000000 ) ) ;
#83196 = ORIENTED_EDGE ( 'NONE', *, *, #68094, .T. ) ;
#83197 = CARTESIAN_POINT ( 'NONE',  ( 69.72411017813010403, 120.6499999999999915, -69.72411017812979139 ) ) ;
#83198 = CARTESIAN_POINT ( 'NONE',  ( 107.0667039024470313, -104.2784471599409528, 19.21780685541800437 ) ) ;
#83199 = CARTESIAN_POINT ( 'NONE',  ( 9.554550254943340093, 74.17292945273928240, 118.1706666865833455 ) ) ;
#83200 = ORIENTED_EDGE ( 'NONE', *, *, #49092, .T. ) ;
#83201 = EDGE_CURVE ( 'NONE', #24899, #12759, #23004, .T. ) ;
#83202 = CARTESIAN_POINT ( 'NONE',  ( 102.3506485400807975, -46.05136549539959390, 123.2041967044829818 ) ) ;
#83204 = CARTESIAN_POINT ( 'NONE',  ( 52.65249034007835149, -49.32844715994059470, 249.9678068554150343 ) ) ;
#83203 = CARTESIAN_POINT ( 'NONE',  ( 219.9639999999999986, 40.03750000000000142, -7.937500000000000000 ) ) ;
#83205 = CARTESIAN_POINT ( 'NONE',  ( -479.3614999999999782, 89.53805401447711176, 3.968750000000410338 ) ) ;
#83207 = EDGE_CURVE ( 'NONE', #19003, #62636, #3802, .T. ) ;
#83206 = AXIS2_PLACEMENT_3D ( 'NONE', #62044, #49752, #89778 ) ;
#83208 = VECTOR ( 'NONE', #57676, 1000.000000000000000 ) ;
#83209 = CARTESIAN_POINT ( 'NONE',  ( 139.3670970868850532, -133.7001840312377396, 248.3919668373590071 ) ) ;
#83210 = VERTEX_POINT ( 'NONE', #58386 ) ;
#83211 = CARTESIAN_POINT ( 'NONE',  ( 108.8662857618680846, -46.94215964495589333, 118.7032443235299723 ) ) ;
#83213 = ORIENTED_EDGE ( 'NONE', *, *, #68041, .F. ) ;
#83212 = CARTESIAN_POINT ( 'NONE',  ( 141.0667039024479834, -58.72944715994110254, 198.9178068554149945 ) ) ;
#83214 = CARTESIAN_POINT ( 'NONE',  ( 116.5166575185068467, -42.41785904284974862, 274.3832443235299365 ) ) ;
#83215 = CARTESIAN_POINT ( 'NONE',  ( 34.92499999999999716, 91.71543552338529537, 302.8950000000000387 ) ) ;
#83216 = CARTESIAN_POINT ( 'NONE',  ( 105.1589286322272585, -76.77844715994095282, 250.2178068554180470 ) ) ;
#83217 = CARTESIAN_POINT ( 'NONE',  ( -72.96458098368751166, 127.0000000000000000, 72.96458098368620426 ) ) ;
#83218 = CARTESIAN_POINT ( 'NONE',  ( 67.77264411201586825, -137.9410731809939819, 246.8967413324789959 ) ) ;
#83219 = CARTESIAN_POINT ( 'NONE',  ( -94.33955404248663967, 70.17666187254641841, 90.25011051337732226 ) ) ;
#83220 = CARTESIAN_POINT ( 'NONE',  ( 109.2168187703261282, -26.58475186820026792, 184.9222919425779708 ) ) ;
#83221 = ORIENTED_EDGE ( 'NONE', *, *, #8041, .T. ) ;
#83222 = VERTEX_POINT ( 'NONE', #24763 ) ;
#83223 = CARTESIAN_POINT ( 'NONE',  ( 116.1908163682739712, -34.48822628859398520, 160.4377737820879588 ) ) ;
#83224 = CIRCLE ( 'NONE', #59971, 14.00000000000000888 ) ;
#83225 = DIRECTION ( 'NONE',  ( 0.000000000000000000, 1.000000000000000000, 0.000000000000000000 ) ) ;
#83226 = CARTESIAN_POINT ( 'NONE',  ( 110.7632188227358512, -44.78316835090528514, 24.35015473446894418 ) ) ;
#83227 = AXIS2_PLACEMENT_3D ( 'NONE', #51667, #64877, #78967 ) ;
#83228 = LINE ( 'NONE', #55930, #17375 ) ;
#83229 = EDGE_CURVE ( 'NONE', #60182, #78082, #10244, .T. ) ;
#83230 = EDGE_CURVE ( 'NONE', #75851, #82261, #47291, .T. ) ;
#83231 = CARTESIAN_POINT ( 'NONE',  ( 105.7149878756584798, -46.72378413123163199, 267.4690543908536711 ) ) ;
#83232 = CARTESIAN_POINT ( 'NONE',  ( -3.968749999999949818, 120.6499999999999915, -105.4788588808462038 ) ) ;
#83233 = CIRCLE ( 'NONE', #44046, 2.750000000000002665 ) ;
#83234 = CARTESIAN_POINT ( 'NONE',  ( 115.8254323917787332, -31.73001882841382937, 105.2397919426083206 ) ) ;
#83235 = EDGE_CURVE ( 'NONE', #77441, #59415, #31350, .T. ) ;
#83236 = CARTESIAN_POINT ( 'NONE',  ( 188.5667039024479834, -48.82844715994099971, 170.4678068554149775 ) ) ;
#83237 = CARTESIAN_POINT ( 'NONE',  ( 102.2473430764596714, -45.94923854148477460, 212.1927681330539599 ) ) ;
#83238 = CARTESIAN_POINT ( 'NONE',  ( 97.80895962946385680, -40.51075741989382095, 171.6353300661548928 ) ) ;
#83239 = VERTEX_POINT ( 'NONE', #80193 ) ;
#83240 = ORIENTED_EDGE ( 'NONE', *, *, #52645, .T. ) ;
#83241 = EDGE_CURVE ( 'NONE', #27698, #76097, #11053, .T. ) ;
#83242 = CARTESIAN_POINT ( 'NONE',  ( 56.06670390244699576, -67.87844715994098976, 155.2178068554179902 ) ) ;
#83243 = CARTESIAN_POINT ( 'NONE',  ( -86.13037352894129128, 94.82191660594813243, -81.46927207886268718 ) ) ;
#83244 = DIRECTION ( 'NONE',  ( 0.2884130866282269556, 0.7071067811865447972, -0.6456143519637576045 ) ) ;
#83245 = CARTESIAN_POINT ( 'NONE',  ( -7.661254700127832606, 95.64746158385918307, 320.6630000000000109 ) ) ;
#83246 = VECTOR ( 'NONE', #27154, 1000.000000000000000 ) ;
#83247 = CYLINDRICAL_SURFACE ( 'NONE', #18043, 1.999999999999995781 ) ;
#83248 = ORIENTED_EDGE ( 'NONE', *, *, #6824, .T. ) ;
#83249 = CARTESIAN_POINT ( 'NONE',  ( 104.2291421067619694, -46.80627582718438617, 18.35848241876792031 ) ) ;
#83250 = CARTESIAN_POINT ( 'NONE',  ( 116.2188219837490522, -41.79507674895632618, 263.4241967044824833 ) ) ;
#83251 = ORIENTED_EDGE ( 'NONE', *, *, #32927, .T. ) ;
#83252 = EDGE_CURVE ( 'NONE', #24268, #70447, #29723, .T. ) ;
#83253 = CARTESIAN_POINT ( 'NONE',  ( 107.0664832912739968, 19.62155284005901024, 333.4006252759110112 ) ) ;
#83254 = DIRECTION ( 'NONE',  ( 0.000000000000000000, 1.000000000000000000, 0.000000000000000000 ) ) ;
#83255 = LINE ( 'NONE', #70062, #80328 ) ;
#83256 = CARTESIAN_POINT ( 'NONE',  ( 111.5243040195562401, -29.85845577577017806, 67.43666179816293038 ) ) ;
#83257 = CARTESIAN_POINT ( 'NONE',  ( 117.0378900095125942, -33.61363155034663208, 170.0670538473399631 ) ) ;
#83258 = LINE ( 'NONE', #35081, #87039 ) ;
#83259 = ORIENTED_EDGE ( 'NONE', *, *, #72769, .F. ) ;
#83260 = DIRECTION ( 'NONE',  ( 0.000000000000000000, 0.000000000000000000, 1.000000000000000000 ) ) ;
#83261 = EDGE_LOOP ( 'NONE', ( #6186, #71798, #85488, #42940 ) ) ;
#83262 = ORIENTED_EDGE ( 'NONE', *, *, #34931, .T. ) ;
#83263 = VECTOR ( 'NONE', #12014, 1000.000000000000000 ) ;
#83264 = CARTESIAN_POINT ( 'NONE',  ( 52.99265158129170317, 95.25000000000000000, 346.9005000000000223 ) ) ;
#83265 = ORIENTED_EDGE ( 'NONE', *, *, #82648, .T. ) ;
#83266 = ORIENTED_EDGE ( 'NONE', *, *, #50284, .T. ) ;
#83267 = CARTESIAN_POINT ( 'NONE',  ( 163.0664832912739826, 19.62155284005901024, 333.4006252759110112 ) ) ;
#83268 = AXIS2_PLACEMENT_3D ( 'NONE', #30539, #37351, #77801 ) ;
#83269 = CARTESIAN_POINT ( 'NONE',  ( 109.5993548714604060, -44.88669505861042808, 97.23813411379100557 ) ) ;
#83270 = CARTESIAN_POINT ( 'NONE',  ( 117.3567523603254159, -34.92480690411444044, 243.9641967044819637 ) ) ;
#83271 = CARTESIAN_POINT ( 'NONE',  ( 96.66614461754329568, -36.48121138304695421, 196.3070538473399438 ) ) ;
#83272 = CARTESIAN_POINT ( 'NONE',  ( 110.5478855402367913, -46.57039549162846015, 33.84705384733993583 ) ) ;
#83273 = LINE ( 'NONE', #27396, #46982 ) ;
#83274 = DIRECTION ( 'NONE',  ( 1.000000000000000000, 1.314511288311335947E-16, 0.000000000000000000 ) ) ;
#83275 = ORIENTED_EDGE ( 'NONE', *, *, #64143, .F. ) ;
#83276 = ADVANCED_FACE ( 'NONE', ( #3432 ), #17508, .T. ) ;
#83277 = CARTESIAN_POINT ( 'NONE',  ( -479.3614999999999782, 97.78694598552380057, 3.968750000000479616 ) ) ;
#83278 = CARTESIAN_POINT ( 'NONE',  ( 96.47668441219802560, -40.11591174724604514, 131.5727681330539554 ) ) ;
#83279 = CARTESIAN_POINT ( 'NONE',  ( 117.0961560025638306, -31.97355093185684538, 64.19086337114899266 ) ) ;
#83281 = AXIS2_PLACEMENT_3D ( 'NONE', #8279, #1013, #29168 ) ;
#83280 = CARTESIAN_POINT ( 'NONE',  ( 115.3585040474263508, -45.26590950091470233, 268.1899109901965517 ) ) ;
#83282 = ORIENTED_EDGE ( 'NONE', *, *, #36377, .T. ) ;
#83283 = CARTESIAN_POINT ( 'NONE',  ( 99.75298236265237506, -29.29979477046331127, 225.6956252759109702 ) ) ;
#83284 = FACE_OUTER_BOUND ( 'NONE', #87484, .T. ) ;
#83285 = VECTOR ( 'NONE', #53494, 1000.000000000000000 ) ;
#83286 = FILL_AREA_STYLE ('',( #21512 ) ) ;
#83288 = CARTESIAN_POINT ( 'NONE',  ( 97.92323840168593563, -40.78071684388427087, 22.65838076743288454 ) ) ;
#83287 = VECTOR ( 'NONE', #47607, 1000.000000000000000 ) ;
#83289 = CARTESIAN_POINT ( 'NONE',  ( 97.82830680173087501, -40.55783747296570851, 27.63952666306597195 ) ) ;
#83291 = LINE ( 'NONE', #1519, #15209 ) ;
#83290 = DIRECTION ( 'NONE',  ( 1.000000000000000000, 0.000000000000000000, 0.000000000000000000 ) ) ;
#83292 = CARTESIAN_POINT ( 'NONE',  ( 105.8903942048936386, -25.33046657390624290, 320.7024103198550051 ) ) ;
#83293 = CARTESIAN_POINT ( 'NONE',  ( 180.3503142329376487, -29.99615139351623583, 237.4678068554150059 ) ) ;
#83294 = CARTESIAN_POINT ( 'NONE',  ( 6.359675246477851651, 93.55082578214791056, -118.3858732848555206 ) ) ;
#83295 = DIRECTION ( 'NONE',  ( -0.1858654557293118459, 0.9825752044329915114, 0.000000000000000000 ) ) ;
#83296 = FACE_OUTER_BOUND ( 'NONE', #40165, .T. ) ;
#83297 = DIRECTION ( 'NONE',  ( 0.000000000000000000, 0.000000000000000000, 1.000000000000000000 ) ) ;
#83299 = ORIENTED_EDGE ( 'NONE', *, *, #14198, .T. ) ;
#83298 = DIRECTION ( 'NONE',  ( 0.000000000000000000, 0.000000000000000000, 1.000000000000000000 ) ) ;
#83300 = DIRECTION ( 'NONE',  ( 0.000000000000000000, -1.000000000000000000, 0.000000000000000000 ) ) ;
#83301 = CARTESIAN_POINT ( 'NONE',  ( 100.2336795655629089, -28.82633655636628589, 260.6441967044821695 ) ) ;
#83302 = CARTESIAN_POINT ( 'NONE',  ( 99.42212199502026237, -27.67378918447352731, 146.6356252759109395 ) ) ;
#83303 = CARTESIAN_POINT ( 'NONE',  ( 105.7709788128635182, -26.34124963128569163, 266.1756252759109884 ) ) ;
#83304 = CARTESIAN_POINT ( 'NONE',  ( 184.5664832912729878, -71.37844715994266664, 361.9756252759109998 ) ) ;
#83306 = LINE ( 'NONE', #42388, #44298 ) ;
#83305 = CARTESIAN_POINT ( 'NONE',  ( 107.0667039024470313, -104.2784471599420755, -19.78219314458201694 ) ) ;
#83307 = CARTESIAN_POINT ( 'NONE',  ( 105.7153723085520056, -46.72384505539759658, 138.4689504240039071 ) ) ;
#83308 = CARTESIAN_POINT ( 'NONE',  ( 129.9368274816649489, 82.54999999999999716, 12.70000000000136176 ) ) ;
#83309 = EDGE_CURVE ( 'NONE', #52469, #67042, #5674, .T. ) ;
#83310 = ORIENTED_EDGE ( 'NONE', *, *, #68142, .F. ) ;
#83311 = DIRECTION ( 'NONE',  ( 0.0001713722456127401463, -0.9999999853157766072, -1.713722456137401502E-19 ) ) ;
#83312 = ORIENTED_EDGE ( 'NONE', *, *, #54370, .T. ) ;
#83313 = CARTESIAN_POINT ( 'NONE',  ( 100.0898434420045788, -43.48201142159524579, 191.3609912566489584 ) ) ;
#83315 = VERTEX_POINT ( 'NONE', #18845 ) ;
#83314 = CARTESIAN_POINT ( 'NONE',  ( 115.0340621167422626, -42.91251456256151897, 188.3024629498006846 ) ) ;
#83316 = FACE_OUTER_BOUND ( 'NONE', #6674, .T. ) ;
#83317 = CARTESIAN_POINT ( 'NONE',  ( 114.2249171546290967, -45.12625265263328345, 149.1508633711489722 ) ) ;
#83318 = DIRECTION ( 'NONE',  ( 0.000000000000000000, 0.000000000000000000, 1.000000000000000000 ) ) ;
#83319 = CARTESIAN_POINT ( 'NONE',  ( 70.57087804374656059, -139.4754646311776867, 247.4327973477450087 ) ) ;
#83320 = CARTESIAN_POINT ( 'NONE',  ( 110.1700060600548312, -27.22182654212957331, 85.82575214445022027 ) ) ;
#83321 = CARTESIAN_POINT ( 'NONE',  ( -41.60202597009397607, 65.59999999999998010, 54.55338361873603503 ) ) ;
#83322 = CARTESIAN_POINT ( 'NONE',  ( 183.5150000000000148, 52.73749999999999716, -44.45000000000000284 ) ) ;
#83323 = CARTESIAN_POINT ( 'NONE',  ( 117.2073019650709256, -38.89799087863980276, 108.6708633711499772 ) ) ;
#83324 = ORIENTED_EDGE ( 'NONE', *, *, #39995, .F. ) ;
#83325 = ORIENTED_EDGE ( 'NONE', *, *, #6716, .F. ) ;
#83326 = ORIENTED_EDGE ( 'NONE', *, *, #15782, .T. ) ;
#83327 = CARTESIAN_POINT ( 'NONE',  ( 104.8770057419572908, -45.34735396192071732, 43.81015473446897346 ) ) ;
#83328 = CARTESIAN_POINT ( 'NONE',  ( 133.3245970085671388, -112.6232539059702731, 250.2178068554180470 ) ) ;
#83330 = CARTESIAN_POINT ( 'NONE',  ( 70.88111044991026688, -139.0101909505960691, 247.5112285516309782 ) ) ;
#83329 = CARTESIAN_POINT ( 'NONE',  ( 114.5468542906242391, -29.54732804739400365, 185.4232443235299570 ) ) ;
#83331 = VECTOR ( 'NONE', #38143, 1000.000000000000000 ) ;
#83332 = FACE_OUTER_BOUND ( 'NONE', #16903, .T. ) ;
#83333 = DIRECTION ( 'NONE',  ( 0.000000000000000000, 1.000000000000000000, 0.000000000000000000 ) ) ;
#83334 = EDGE_CURVE ( 'NONE', #7646, #65744, #6121, .T. ) ;
#83335 = CARTESIAN_POINT ( 'NONE',  ( 20.03715912545639100, -24.42818131006202265, 180.4678068554150911 ) ) ;
#83336 = CARTESIAN_POINT ( 'NONE',  ( 22.49541547940750519, -78.44951497180814215, 361.9756252759109998 ) ) ;
#83337 = EDGE_CURVE ( 'NONE', #1545, #78613, #8149, .T. ) ;
#83338 = CARTESIAN_POINT ( 'NONE',  ( 95.56670390244703128, -104.2784471599408818, 19.21780685541799016 ) ) ;
#83339 = CARTESIAN_POINT ( 'NONE',  ( 113.0643619202157879, -28.22920495858469891, 129.5870538473399449 ) ) ;
#83340 = VERTEX_POINT ( 'NONE', #46966 ) ;
#83341 = ADVANCED_FACE ( 'NONE', ( #81983 ), #80637, .T. ) ;
#83342 = VERTEX_POINT ( 'NONE', #25652 ) ;
#83343 = EDGE_LOOP ( 'NONE', ( #42885, #8516 ) ) ;
#83344 = EDGE_CURVE ( 'NONE', #11013, #15725, #53326, .T. ) ;
#83345 = DIRECTION ( 'NONE',  ( 2.900000000000000265E-14, -2.000000000000000155E-15, 1.000000000000000000 ) ) ;
#83346 = CARTESIAN_POINT ( 'NONE',  ( 145.5337519030156557, -69.32260879017363209, 247.4441250540085946 ) ) ;
#83347 = DIRECTION ( 'NONE',  ( -1.000000000000000000, 0.000000000000000000, -2.108231265501709878E-16 ) ) ;
#83348 = CARTESIAN_POINT ( 'NONE',  ( 100.3081386793954408, -31.32336695771306623, 193.5957094172099744 ) ) ;
#83349 = VECTOR ( 'NONE', #1211, 1000.000000000000000 ) ;
#83350 = DIRECTION ( 'NONE',  ( 0.000000000000000000, 0.000000000000000000, 1.000000000000000000 ) ) ;
#83351 = VECTOR ( 'NONE', #83105, 1000.000000000000000 ) ;
#83352 = DIRECTION ( 'NONE',  ( 0.000000000000000000, 0.000000000000000000, 1.000000000000000000 ) ) ;
#83353 = ORIENTED_EDGE ( 'NONE', *, *, #30199, .F. ) ;
#83355 = EDGE_LOOP ( 'NONE', ( #65907, #27208 ) ) ;
#83354 = ORIENTED_EDGE ( 'NONE', *, *, #60023, .T. ) ;
#83356 = EDGE_CURVE ( 'NONE', #77060, #9798, #74701, .T. ) ;
#83357 = AXIS2_PLACEMENT_3D ( 'NONE', #11452, #39147, #54094 ) ;
#83358 = VECTOR ( 'NONE', #69817, 1000.000000000000000 ) ;
#83359 = DIRECTION ( 'NONE',  ( 1.000000000000000000, 0.000000000000000000, 0.000000000000000000 ) ) ;
#83360 = ORIENTED_EDGE ( 'NONE', *, *, #60188, .T. ) ;
#83361 = ORIENTED_EDGE ( 'NONE', *, *, #31128, .F. ) ;
#83362 = ADVANCED_FACE ( 'NONE', ( #18385 ), #5217, .F. ) ;
#83363 = CARTESIAN_POINT ( 'NONE',  ( 78.92327517541272641, -21.23064218986597851, 8.021355262920510043 ) ) ;
#83364 = CARTESIAN_POINT ( 'NONE',  ( 100.6682639674293114, -30.55490919580550013, 247.1472975916109647 ) ) ;
#83365 = ORIENTED_EDGE ( 'NONE', *, *, #76003, .F. ) ;
#83366 = PLANE ( 'NONE',  #30514 ) ;
#83367 = CARTESIAN_POINT ( 'NONE',  ( -119.9082588554310576, 74.59549379520217371, 51.64190430363700557 ) ) ;
#83368 = ORIENTED_EDGE ( 'NONE', *, *, #55726, .T. ) ;
#83369 = ORIENTED_EDGE ( 'NONE', *, *, #39119, .T. ) ;
#83370 = FACE_OUTER_BOUND ( 'NONE', #64273, .T. ) ;
#83371 = ORIENTED_EDGE ( 'NONE', *, *, #34709, .T. ) ;
#83372 = ORIENTED_EDGE ( 'NONE', *, *, #13761, .T. ) ;
#83373 = AXIS2_PLACEMENT_3D ( 'NONE', #30657, #11092, #58354 ) ;
#83374 = CARTESIAN_POINT ( 'NONE',  ( 110.0622958990556839, -29.10660024649327227, 267.5966617981628701 ) ) ;
#83375 = CARTESIAN_POINT ( 'NONE',  ( 114.7424063621565722, -43.81651770963347303, 123.2327681330539519 ) ) ;
#83376 = CARTESIAN_POINT ( 'NONE',  ( 113.8422018911647484, -44.62364141802228090, 108.1413395616249744 ) ) ;
#83377 = CARTESIAN_POINT ( 'NONE',  ( 131.5441285970350691, -17.63380991825878397, 7.053480412781381048 ) ) ;
#83378 = CARTESIAN_POINT ( 'NONE',  ( 98.89890862997502552, -29.28198419350761483, 226.7261014663869503 ) ) ;
#83379 = CYLINDRICAL_SURFACE ( 'NONE', #67521, 27.99999999999999645 ) ;
#83380 = DIRECTION ( 'NONE',  ( -0.5000000000000012212, 0.000000000000000000, -0.8660254037844380415 ) ) ;
#83381 = EDGE_LOOP ( 'NONE', ( #56382, #6700, #11376, #63691 ) ) ;
#83382 = CARTESIAN_POINT ( 'NONE',  ( 130.5477899301573359, 69.93364840292898066, 1.674143004590020523 ) ) ;
#83383 = ORIENTED_EDGE ( 'NONE', *, *, #87016, .T. ) ;
#83384 = ORIENTED_EDGE ( 'NONE', *, *, #5734, .T. ) ;
#83385 = DIRECTION ( 'NONE',  ( 1.000000000000000000, 0.000000000000000000, 9.868649107779159826E-16 ) ) ;
#83386 = EDGE_CURVE ( 'NONE', #1363, #55007, #81095, .T. ) ;
#83387 = VECTOR ( 'NONE', #66531, 1000.000000000000000 ) ;
#83388 = DIRECTION ( 'NONE',  ( 2.301579500234999682E-14, 0.000000000000000000, -1.000000000000000000 ) ) ;
#83389 = CARTESIAN_POINT ( 'NONE',  ( 112.1201679527454047, -47.44862423305024635, 137.9270538473389820 ) ) ;
#83390 = CARTESIAN_POINT ( 'NONE',  ( -10.55295613787796327, 75.48422888499150929, 130.1287987652872857 ) ) ;
#83391 = B_SPLINE_CURVE_WITH_KNOTS ( 'NONE', 3,
 ( #64794, #86585, #37975, #50707, #3901, #17968, #31599, #37542, #58849, #29835, #59299, #52465, #58412, #16209, #9384, #24357, #37093, #30717 ),
 .UNSPECIFIED., .F., .F.,
 ( 4, 2, 2, 2, 2, 2, 2, 2, 4 ),
 ( 0.000000000000000000, 0.1250000000000000000, 0.2500000000000000000, 0.3750000000000000000, 0.5000000000000000000, 0.6250000000000000000, 0.7500000000000000000, 0.8750000000000000000, 1.000000000000000000 ),
 .UNSPECIFIED. ) ;
#83392 = AXIS2_PLACEMENT_3D ( 'NONE', #40707, #82526, #76127 ) ;
#83393 = EDGE_CURVE ( 'NONE', #26931, #30738, #25578, .T. ) ;
#83394 = LINE ( 'NONE', #21168, #62340 ) ;
#83397 = CARTESIAN_POINT ( 'NONE',  ( 96.69582475441080760, -35.54038568221479011, 202.2356252759109623 ) ) ;
#83396 = DIRECTION ( 'NONE',  ( 0.000000000000000000, 0.000000000000000000, 1.000000000000000000 ) ) ;
#83395 = DIRECTION ( 'NONE',  ( 0.000000000000000000, 0.000000000000000000, 1.000000000000000000 ) ) ;
#83398 = PLANE ( 'NONE',  #52437 ) ;
#83399 = DIRECTION ( 'NONE',  ( 0.000000000000000000, 0.000000000000000000, 1.000000000000000000 ) ) ;
#83400 = ORIENTED_EDGE ( 'NONE', *, *, #68567, .T. ) ;
#83401 = DIRECTION ( 'NONE',  ( 0.000000000000000000, 1.000000000000000000, 0.000000000000000000 ) ) ;
#83402 = CARTESIAN_POINT ( 'NONE',  ( 74.15067561874209900, 120.6499999999999915, 68.53801554307469246 ) ) ;
#83403 = FACE_OUTER_BOUND ( 'NONE', #80312, .T. ) ;
#83404 = CARTESIAN_POINT ( 'NONE',  ( 147.0667039024470739, -137.6624395622106078, 245.7309020619233593 ) ) ;
#83406 = ORIENTED_EDGE ( 'NONE', *, *, #31602, .T. ) ;
#83405 = CARTESIAN_POINT ( 'NONE',  ( 99.36439196449877898, -28.73628302914087840, 265.6746728949588032 ) ) ;
#83407 = CARTESIAN_POINT ( 'NONE',  ( 114.0075790447407087, -33.88846322102013175, 9.635625275910941312 ) ) ;
#83408 = CARTESIAN_POINT ( 'NONE',  ( 97.77451808712464754, -42.75935979880518545, 146.7965776568629508 ) ) ;
#83409 = CARTESIAN_POINT ( 'NONE',  ( 96.68599849774213340, -42.44610274171655817, 22.72705384733997391 ) ) ;
#83410 = CARTESIAN_POINT ( 'NONE',  ( 108.9530382828359052, -26.39605832486118331, 160.9327681330539690 ) ) ;
#83411 = CARTESIAN_POINT ( 'NONE',  ( 113.2454986637468011, -28.75867291636540912, 30.55229194610398480 ) ) ;
#83412 = CARTESIAN_POINT ( 'NONE',  ( 97.79820142046531828, -40.48432854127982239, 102.6327809001923157 ) ) ;
#83414 = PLANE ( 'NONE',  #60175 ) ;
#83413 = CARTESIAN_POINT ( 'NONE',  ( -179.8898777604649979, 20.32000000000000028, 122.9960808104842016 ) ) ;
#83415 = CARTESIAN_POINT ( 'NONE',  ( 102.0670549713190667, -27.97049805303531045, 70.48979194156258643 ) ) ;
#83416 = CARTESIAN_POINT ( 'NONE',  ( 103.1875000000000000, 127.0000000000000000, -7.937499999999639400 ) ) ;
#83417 = VERTEX_POINT ( 'NONE', #52863 ) ;
#83418 = DIRECTION ( 'NONE',  ( 1.000000000000000000, 0.000000000000000000, 0.000000000000000000 ) ) ;
#83419 = AXIS2_PLACEMENT_3D ( 'NONE', #39054, #88121, #4988 ) ;
#83420 = ORIENTED_EDGE ( 'NONE', *, *, #80945, .T. ) ;
#83421 = VERTEX_POINT ( 'NONE', #74261 ) ;
#83422 = AXIS2_PLACEMENT_3D ( 'NONE', #85226, #15273, #77052 ) ;
#83423 = AXIS2_PLACEMENT_3D ( 'NONE', #72052, #22131, #29829 ) ;
#83424 = EDGE_LOOP ( 'NONE', ( #4429, #85064 ) ) ;
#83425 = CARTESIAN_POINT ( 'NONE',  ( 97.30890135812539654, -33.12136451854836849, 62.04419670448196911 ) ) ;
#83426 = DIRECTION ( 'NONE',  ( -1.000000000000000000, -4.299999999999999979E-14, -1.000000000000000078E-15 ) ) ;
#83427 = CARTESIAN_POINT ( 'NONE',  ( 116.9216359643101839, -34.79311186879120044, 118.9822785838860710 ) ) ;
#83428 = ADVANCED_FACE ( 'NONE', ( #54671 ), #41062, .F. ) ;
#83429 = CARTESIAN_POINT ( 'NONE',  ( 102.0300696065151982, -46.62045497284175610, 168.2137205140059564 ) ) ;
#83431 = CARTESIAN_POINT ( 'NONE',  ( 115.6302422591030137, -36.57899571384957937, 288.2638483995053775 ) ) ;
#83430 = AXIS2_PLACEMENT_3D ( 'NONE', #12033, #32454, #19738 ) ;
#83432 = VERTEX_POINT ( 'NONE', #75149 ) ;
#83433 = ORIENTED_EDGE ( 'NONE', *, *, #23070, .F. ) ;
#83434 = ORIENTED_EDGE ( 'NONE', *, *, #46905, .F. ) ;
#83435 = DIRECTION ( 'NONE',  ( -0.7396053187813123042, -0.6730408400909958511, 0.000000000000000000 ) ) ;
#83436 = CARTESIAN_POINT ( 'NONE',  ( 151.5667039024483245, -48.82844715993591223, 300.4678068554149490 ) ) ;
#83437 = DIRECTION ( 'NONE',  ( 0.000000000000000000, 0.000000000000000000, -1.000000000000000000 ) ) ;
#83438 = LINE ( 'NONE', #21214, #73101 ) ;
#83439 = CIRCLE ( 'NONE', #35498, 2.030000000002086580 ) ;
#83440 = CARTESIAN_POINT ( 'NONE',  ( 84.90178614994185580, 90.29814575435200652, 99.18048580889484356 ) ) ;
#83441 = CARTESIAN_POINT ( 'NONE',  ( 72.06648329127401098, -46.72944715994106701, 14.67562527591093513 ) ) ;
#83442 = CARTESIAN_POINT ( 'NONE',  ( 51.56670390244699576, -19.82844715994031048, 342.9256252759109884 ) ) ;
#83443 = CARTESIAN_POINT ( 'NONE',  ( 128.0667039024480118, -58.35344715994099829, 310.9178068554150514 ) ) ;
#83444 = CARTESIAN_POINT ( 'NONE',  ( 118.5467753794659842, -33.90456151647278205, 14.01848241876796308 ) ) ;
#83445 = EDGE_CURVE ( 'NONE', #13645, #66334, #40624, .T. ) ;
#83446 = CYLINDRICAL_SURFACE ( 'NONE', #85051, 4.000000000000006217 ) ;
#83447 = ORIENTED_EDGE ( 'NONE', *, *, #83547, .F. ) ;
#83448 = LINE ( 'NONE', #68020, #11291 ) ;
#83449 = DIRECTION ( 'NONE',  ( 0.000000000000000000, 0.000000000000000000, -1.000000000000000000 ) ) ;
#83450 = CARTESIAN_POINT ( 'NONE',  ( 109.4870457054322941, -44.52499740455228761, 95.63380465530596553 ) ) ;
#83451 = COLOUR_RGB ( '', 0.66274510, 0.83137255, 0.94901961) ;
#83452 = AXIS2_PLACEMENT_3D ( 'NONE', #67863, #33343, #89216 ) ;
#83453 = DIRECTION ( 'NONE',  ( 1.000000000000000000, 4.299999999999999979E-14, 1.000000000000000078E-15 ) ) ;
#83454 = DIRECTION ( 'NONE',  ( 0.7071067811862279395, -0.7071067811868672059, 7.071067811862286363E-16 ) ) ;
#83455 = ORIENTED_EDGE ( 'NONE', *, *, #51616, .T. ) ;
#83456 = ORIENTED_EDGE ( 'NONE', *, *, #76897, .F. ) ;
#83457 = ADVANCED_FACE ( 'NONE', ( #68787 ), #54221, .T. ) ;
#83458 = CARTESIAN_POINT ( 'NONE',  ( 141.8545562996767444, -1.932463243632623229, 361.9756252759100335 ) ) ;
#83459 = VERTEX_POINT ( 'NONE', #11592 ) ;
#83460 = ORIENTED_EDGE ( 'NONE', *, *, #55169, .F. ) ;
#83461 = EDGE_CURVE ( 'NONE', #378, #17490, #74116, .T. ) ;
#83462 = FACE_OUTER_BOUND ( 'NONE', #55284, .T. ) ;
#83463 = CARTESIAN_POINT ( 'NONE',  ( 115.5384384484689804, -31.27996107247446744, 140.7130118773259539 ) ) ;
#83464 = CARTESIAN_POINT ( 'NONE',  ( 41.56670390244783420, -36.32844715994104234, 249.9678068554150343 ) ) ;
#83465 = CARTESIAN_POINT ( 'NONE',  ( 98.84076182955313072, -43.22688528923472262, 87.85848241876792031 ) ) ;
#83466 = LINE ( 'NONE', #6709, #986 ) ;
#83467 = CIRCLE ( 'NONE', #32689, 0.5000000000000004441 ) ;
#83468 = ORIENTED_EDGE ( 'NONE', *, *, #78047, .T. ) ;
#83469 = DIRECTION ( 'NONE',  ( 0.000000000000000000, 1.000000000000000000, 0.000000000000000000 ) ) ;
#83470 = CIRCLE ( 'NONE', #24018, 7.873999999999991672 ) ;
#83471 = AXIS2_PLACEMENT_3D ( 'NONE', #54573, #46429, #20100 ) ;
#83472 = AXIS2_PLACEMENT_3D ( 'NONE', #17636, #3552, #11258 ) ;
#83473 = ORIENTED_EDGE ( 'NONE', *, *, #78966, .T. ) ;
#83474 = EDGE_LOOP ( 'NONE', ( #78016, #87505, #15334, #22147 ) ) ;
#83475 = VECTOR ( 'NONE', #26101, 1000.000000000000000 ) ;
#83476 = CARTESIAN_POINT ( 'NONE',  ( 107.0667039024479834, -36.72944715994099596, 239.5838068554170093 ) ) ;
#83477 = ORIENTED_EDGE ( 'NONE', *, *, #27423, .F. ) ;
#83478 = CARTESIAN_POINT ( 'NONE',  ( 97.18779033502694631, -39.88384928074078317, 281.5603871806734446 ) ) ;
#83479 = CARTESIAN_POINT ( 'NONE',  ( 105.3125989252256147, -48.47411034989094958, 143.4584824187689662 ) ) ;
#83480 = CARTESIAN_POINT ( 'NONE',  ( 71.77848634863140376, 120.6499999999999915, -77.39114642429929347 ) ) ;
#83481 = FACE_OUTER_BOUND ( 'NONE', #70530, .T. ) ;
#83482 = CARTESIAN_POINT ( 'NONE',  ( 117.8753414029365842, -39.04084647772175032, 104.6708633711489824 ) ) ;
#83483 = CARTESIAN_POINT ( 'NONE',  ( 115.0372575151875054, -42.90846255504887097, 263.3022919437246401 ) ) ;
#83484 = VERTEX_POINT ( 'NONE', #62850 ) ;
#83485 = VECTOR ( 'NONE', #70805, 1000.000000000000000 ) ;
#83486 = CARTESIAN_POINT ( 'NONE',  ( 97.81072293460368883, -40.51506560680811475, 116.6357015805674706 ) ) ;
#83487 = DIRECTION ( 'NONE',  ( 0.000000000000000000, 1.000000000000000000, 0.000000000000000000 ) ) ;
#83488 = ORIENTED_EDGE ( 'NONE', *, *, #3216, .T. ) ;
#83489 = DIRECTION ( 'NONE',  ( 0.000000000000000000, 1.000000000000000000, 0.000000000000000000 ) ) ;
#83490 =( REPRESENTATION_RELATIONSHIP ('NONE','NONE', #82876, #28740 ) REPRESENTATION_RELATIONSHIP_WITH_TRANSFORMATION ( #6316 )SHAPE_REPRESENTATION_RELATIONSHIP( ) );
#83491 = CARTESIAN_POINT ( 'NONE',  ( 194.5664832912729878, -81.37844715994266664, 342.9256252759109884 ) ) ;
#83492 = CARTESIAN_POINT ( 'NONE',  ( 106.6068369155051698, -25.68554329116653534, 40.09753003781596448 ) ) ;
#83493 = DIRECTION ( 'NONE',  ( 1.000000000000000000, 0.000000000000000000, 0.000000000000000000 ) ) ;
#83494 = AXIS2_PLACEMENT_3D ( 'NONE', #76130, #56112, #63862 ) ;
#83495 = ADVANCED_FACE ( 'NONE', ( #56480, #7452 ), #15622, .T. ) ;
#83496 = CARTESIAN_POINT ( 'NONE',  ( 69.13171461148455421, 92.73732945906610325, 55.35424314442764882 ) ) ;
#83497 = CYLINDRICAL_SURFACE ( 'NONE', #60616, 9.999999999999998224 ) ;
#83498 = CARTESIAN_POINT ( 'NONE',  ( 117.5198883494731632, -40.51604253578042858, 23.54991099019792955 ) ) ;
#83500 = CARTESIAN_POINT ( 'NONE',  ( 97.63679352021421209, -31.00714225716596673, 121.8803871806729546 ) ) ;
#83499 = CARTESIAN_POINT ( 'NONE',  ( 179.7974245136207685, -36.32844715993469720, 313.9678068554149490 ) ) ;
#83501 = CARTESIAN_POINT ( 'NONE',  ( 97.81170008160388818, -40.51743097690945916, 72.63551179937353197 ) ) ;
#83502 = PLANE ( 'NONE',  #20575 ) ;
#83503 = VERTEX_POINT ( 'NONE', #49212 ) ;
#83504 = CARTESIAN_POINT ( 'NONE',  ( 53.56670390244749314, -48.82844715994058049, 129.9678068554150911 ) ) ;
#83505 = CARTESIAN_POINT ( 'NONE',  ( 109.6365420697629531, 49.23178009149190615, 70.88510413816129585 ) ) ;
#83506 = DIRECTION ( 'NONE',  ( 1.000000000000000078E-15, 1.000000000000000083E-30, -1.000000000000000000 ) ) ;
#83507 = AXIS2_PLACEMENT_3D ( 'NONE', #59162, #10576, #71490 ) ;
#83508 = VERTEX_POINT ( 'NONE', #56019 ) ;
#83509 = DIRECTION ( 'NONE',  ( 0.000000000000000000, 1.000000000000000000, 0.000000000000000000 ) ) ;
#83511 = VERTEX_POINT ( 'NONE', #43294 ) ;
#83510 = CARTESIAN_POINT ( 'NONE',  ( 104.5519768891453651, -48.36156025571956718, 182.4070538473399665 ) ) ;
#83512 = CARTESIAN_POINT ( 'NONE',  ( 0.000000000000000000, 239.0000000000000000, 154.6557476874258441 ) ) ;
#83513 = CARTESIAN_POINT ( 'NONE',  ( 115.8735763837842256, -44.69546008661756531, 229.2413395616249545 ) ) ;
#83514 = CARTESIAN_POINT ( 'NONE',  ( 118.0477628396966310, -38.34468641101997122, 69.72229194257801055 ) ) ;
#83515 = CARTESIAN_POINT ( 'NONE',  ( 100.5877059554732824, 79.26455342200333121, 83.22858459372999107 ) ) ;
#83516 = FACE_OUTER_BOUND ( 'NONE', #3707, .T. ) ;
#83517 = VECTOR ( 'NONE', #10426, 1000.000000000000000 ) ;
#83518 = DIRECTION ( 'NONE',  ( 1.639958061481212836E-42, -4.100000000000000342E-29, -1.000000000000000000 ) ) ;
#83519 = ORIENTED_EDGE ( 'NONE', *, *, #82743, .T. ) ;
#83520 = EDGE_CURVE ( 'NONE', #75367, #39978, #8354, .T. ) ;
#83521 = VECTOR ( 'NONE', #19341, 1000.000000000000000 ) ;
#83522 = EDGE_CURVE ( 'NONE', #54219, #81211, #75168, .T. ) ;
#83523 = ORIENTED_EDGE ( 'NONE', *, *, #66494, .T. ) ;
#83524 = ORIENTED_EDGE ( 'NONE', *, *, #61620, .T. ) ;
#83525 = ADVANCED_BREP_SHAPE_REPRESENTATION ( '', ( #50495, #50656 ), #10078 ) ;
#83526 = ADVANCED_FACE ( 'NONE', ( #77388 ), #56931, .T. ) ;
#83527 = ORIENTED_EDGE ( 'NONE', *, *, #32941, .F. ) ;
#83528 = DIRECTION ( 'NONE',  ( 1.000000000000000078E-15, -1.000000000000000083E-30, -1.000000000000000000 ) ) ;
#83529 = CARTESIAN_POINT ( 'NONE',  ( 97.47313694375068849, -40.89946378256092174, 227.6527681330539679 ) ) ;
#83530 = LINE ( 'NONE', #55342, #44598 ) ;
#83531 = DIRECTION ( 'NONE',  ( 0.000000000000000000, 0.000000000000000000, -1.000000000000000000 ) ) ;
#83532 = EDGE_CURVE ( 'NONE', #55523, #69100, #55119, .T. ) ;
#83533 = EDGE_CURVE ( 'NONE', #84299, #47032, #18182, .T. ) ;
#83535 = CYLINDRICAL_SURFACE ( 'NONE', #5075, 81.91591158490091118 ) ;
#83534 = DIRECTION ( 'NONE',  ( -1.365069428641121829E-15, 0.000000000000000000, -1.000000000000000000 ) ) ;
#83536 = DIRECTION ( 'NONE',  ( 0.000000000000000000, 0.000000000000000000, -1.000000000000000000 ) ) ;
#83537 = CARTESIAN_POINT ( 'NONE',  ( 115.6294417704117734, -28.50085323451786579, 39.43562527591099354 ) ) ;
#83538 = ORIENTED_EDGE ( 'NONE', *, *, #44176, .F. ) ;
#83539 = EDGE_CURVE ( 'NONE', #1472, #56124, #20642, .T. ) ;
#83540 = EDGE_CURVE ( 'NONE', #25056, #49045, #37001, .T. ) ;
#83541 = ORIENTED_EDGE ( 'NONE', *, *, #87422, .F. ) ;
#83542 = CIRCLE ( 'NONE', #67576, 0.5000000000000004441 ) ;
#83543 = VECTOR ( 'NONE', #28578, 1000.000000000000000 ) ;
#83544 = LINE ( 'NONE', #82214, #87683 ) ;
#83545 = AXIS2_PLACEMENT_3D ( 'NONE', #20105, #19645, #19206 ) ;
#83547 = EDGE_CURVE ( 'NONE', #49587, #81729, #89689, .T. ) ;
#83546 = DIRECTION ( 'NONE',  ( -0.7071067811567310901, 0.7071067812163639443, 0.000000000000000000 ) ) ;
#83548 = CARTESIAN_POINT ( 'NONE',  ( 116.0161715043949471, -40.67488961668902192, 249.4956252759109532 ) ) ;
#83549 = DIRECTION ( 'NONE',  ( 0.000000000000000000, 0.000000000000000000, 1.000000000000000000 ) ) ;
#83550 = CARTESIAN_POINT ( 'NONE',  ( 96.75683229781660089, -37.84742820979678868, 77.40038718067299328 ) ) ;
#83551 = ADVANCED_FACE ( 'NONE', ( #36050 ), #70124, .F. ) ;
#83552 = LINE ( 'NONE', #63544, #86465 ) ;
#83553 = EDGE_CURVE ( 'NONE', #28392, #8532, #70581, .T. ) ;
#83554 = CARTESIAN_POINT ( 'NONE',  ( 97.70650013186612171, -40.25115521776017857, 22.61283738089579742 ) ) ;
#83555 = ORIENTED_EDGE ( 'NONE', *, *, #20008, .T. ) ;
#83556 = DIRECTION ( 'NONE',  ( 0.000000000000000000, 0.000000000000000000, 1.000000000000000000 ) ) ;
#83557 = VERTEX_POINT ( 'NONE', #28798 ) ;
#83558 = ORIENTED_EDGE ( 'NONE', *, *, #35842, .F. ) ;
#83559 = AXIS2_PLACEMENT_3D ( 'NONE', #32139, #4896, #32585 ) ;
#83560 = CARTESIAN_POINT ( 'NONE',  ( -87.71311422381535294, 93.94553785444269067, 79.76258624986857626 ) ) ;
#83561 = CARTESIAN_POINT ( 'NONE',  ( 116.4296429186904049, -33.01435002197194279, 245.5587261630399780 ) ) ;
#83562 = CARTESIAN_POINT ( 'NONE',  ( 115.7831076517189928, -41.80230954316925818, 193.4064586062707463 ) ) ;
#83563 = CARTESIAN_POINT ( 'NONE',  ( -117.8738102209307925, 82.54999999999999716, 12.69999999999959073 ) ) ;
#83564 = AXIS2_PLACEMENT_3D ( 'NONE', #83198, #35466, #62282 ) ;
#83565 = CARTESIAN_POINT ( 'NONE',  ( 71.25502878279074537, -77.59225815239315693, 542.9756252759101471 ) ) ;
#83566 = CARTESIAN_POINT ( 'NONE',  ( 82.65143893653623763, 69.93120980984942037, -84.99964240976891006 ) ) ;
#83567 = ORIENTED_EDGE ( 'NONE', *, *, #56884, .T. ) ;
#83568 = CARTESIAN_POINT ( 'NONE',  ( 24.79284581386643183, 184.0000000000000000, 90.32146847885336172 ) ) ;
#83569 = EDGE_CURVE ( 'NONE', #85174, #64215, #5916, .T. ) ;
#83570 = CARTESIAN_POINT ( 'NONE',  ( 6.123233995736764310E-16, 239.0000000000000000, 149.6557476874258441 ) ) ;
#83571 = EDGE_LOOP ( 'NONE', ( #65938, #44709, #65150, #55193 ) ) ;
#83572 = CARTESIAN_POINT ( 'NONE',  ( 116.3877942521162936, -31.98191425893181261, 44.20133956162491984 ) ) ;
#83573 = ORIENTED_EDGE ( 'NONE', *, *, #37807, .F. ) ;
#83574 = ADVANCED_FACE ( 'NONE', ( #24650 ), #57377, .F. ) ;
#83575 = CARTESIAN_POINT ( 'NONE',  ( 116.4921678451845111, -34.41013889705870099, 13.44099125664899219 ) ) ;
#83576 = EDGE_CURVE ( 'NONE', #56843, #70, #38478, .T. ) ;
#83577 = DIRECTION ( 'NONE',  ( -1.000000000000000000, -4.299999999999999979E-14, -1.000000000000000078E-15 ) ) ;
#83578 = CARTESIAN_POINT ( 'NONE',  ( 117.2759483237920080, -34.91131378075001379, 198.9546728949589749 ) ) ;
#83579 = CARTESIAN_POINT ( 'NONE',  ( 20.03715912545729338, -24.42818131006189830, 313.9678068554150059 ) ) ;
#83580 = CARTESIAN_POINT ( 'NONE',  ( 172.5664832912729878, -18.82844715994071194, 78.92562527591199739 ) ) ;
#83582 = EDGE_CURVE ( 'NONE', #1742, #8767, #71485, .T. ) ;
#83581 = CARTESIAN_POINT ( 'NONE',  ( 183.6524903400785433, -48.32844715993451956, 180.4678068554150343 ) ) ;
#83583 = CARTESIAN_POINT ( 'NONE',  ( 107.0667039024470313, -104.2784471599418197, -11.78219314458200984 ) ) ;
#83584 = CARTESIAN_POINT ( 'NONE',  ( 103.0738860297313266, -47.93972279484852095, 248.3041967044829619 ) ) ;
#83585 = CARTESIAN_POINT ( 'NONE',  ( 75.37293521528361850, 88.18374315479975678, -91.51255889651554298 ) ) ;
#83586 = ORIENTED_EDGE ( 'NONE', *, *, #53939, .T. ) ;
#83587 = LINE ( 'NONE', #76761, #41490 ) ;
#83588 = EDGE_LOOP ( 'NONE', ( #57776, #84517, #65063, #88362 ) ) ;
#83589 = CARTESIAN_POINT ( 'NONE',  ( 95.73188602939242742, -40.35408750269280631, 127.5727681330539554 ) ) ;
#83590 = CARTESIAN_POINT ( 'NONE',  ( 119.5843592605237120, 52.73749999999999716, -52.38749999999991758 ) ) ;
#83591 = VERTEX_POINT ( 'NONE', #65096 ) ;
#83592 = CARTESIAN_POINT ( 'NONE',  ( 6.938893903907229955E-15, 60.82030000000000314, 216.0269999999999868 ) ) ;
#83593 = EDGE_LOOP ( 'NONE', ( #50928, #12096, #63807 ) ) ;
#83594 = VERTEX_POINT ( 'NONE', #2435 ) ;
#83595 = CARTESIAN_POINT ( 'NONE',  ( 100.8874677604249115, -44.70022128019346752, 122.0522919302606795 ) ) ;
#83596 = CARTESIAN_POINT ( 'NONE',  ( 172.5664832912740110, -9.303447159940999356, 198.9256252759119832 ) ) ;
#83597 = LINE ( 'NONE', #35423, #80561 ) ;
#83598 = CARTESIAN_POINT ( 'NONE',  ( 57.56670390244819657, -42.82844715994040286, 259.7178068554150627 ) ) ;
#83599 = CARTESIAN_POINT ( 'NONE',  ( -254.0000000000000000, 14.28750000000026077, 11.11249999999970051 ) ) ;
#83600 = CARTESIAN_POINT ( 'NONE',  ( 110.4730825863185260, -45.36026475776040456, 170.6938046553059678 ) ) ;
#83601 = CARTESIAN_POINT ( 'NONE',  ( 100.8354465997397540, -45.15876371340904427, 253.0699109901969450 ) ) ;
#83602 = DIRECTION ( 'NONE',  ( 0.000000000000000000, 0.000000000000000000, -1.000000000000000000 ) ) ;
#83603 = VERTEX_POINT ( 'NONE', #52315 ) ;
#83604 = CARTESIAN_POINT ( 'NONE',  ( 123.6837132603319560, -53.34645651782485487, 218.0711402470151370 ) ) ;
#83605 = CONICAL_SURFACE ( 'NONE', #28471, 1.624999999999987566, 1.029744258676650093 ) ;
#83606 = DIRECTION ( 'NONE',  ( 1.907762142705490052E-15, 7.167082501179359715E-16, -1.000000000000000000 ) ) ;
#83607 = ORIENTED_EDGE ( 'NONE', *, *, #28485, .T. ) ;
#83608 = EDGE_LOOP ( 'NONE', ( #19305, #22419 ) ) ;
#83609 = VECTOR ( 'NONE', #72829, 1000.000000000000000 ) ;
#83610 = AXIS2_PLACEMENT_3D ( 'NONE', #20289, #13463, #13024 ) ;
#83611 = LINE ( 'NONE', #62251, #53223 ) ;
#83612 = STYLED_ITEM ( 'NONE', ( #7925 ), #50041 ) ;
#83613 = FACE_OUTER_BOUND ( 'NONE', #30352, .T. ) ;
#83614 = CARTESIAN_POINT ( 'NONE',  ( 80.06648329127399677, -8.729447159940999512, 2.408125275911999097 ) ) ;
#83615 = VECTOR ( 'NONE', #60863, 1000.000000000000000 ) ;
#83616 = CARTESIAN_POINT ( 'NONE',  ( 29.56670390244828184, -48.82844715994152551, 300.4678068554150059 ) ) ;
#83617 = CARTESIAN_POINT ( 'NONE',  ( 141.8545562996768012, -1.932463243632623229, 394.9756252759100903 ) ) ;
#83618 = CARTESIAN_POINT ( 'NONE',  ( 112.4896002948435410, -43.98220334580144453, 187.5219436376009696 ) ) ;
#83619 = CARTESIAN_POINT ( 'NONE',  ( 117.6400240572639575, -42.19104337252187520, 93.44705384733897802 ) ) ;
#83620 = ORIENTED_EDGE ( 'NONE', *, *, #82399, .T. ) ;
#83621 = CYLINDRICAL_SURFACE ( 'NONE', #43703, 11.45913725231036118 ) ;
#83622 = ORIENTED_EDGE ( 'NONE', *, *, #72338, .F. ) ;
#83623 = CARTESIAN_POINT ( 'NONE',  ( -74.62294912200651709, 79.66725693986896317, -92.12462914090781396 ) ) ;
#83624 = ORIENTED_EDGE ( 'NONE', *, *, #68372, .T. ) ;
#83625 = CYLINDRICAL_SURFACE ( 'NONE', #33156, 4.500000000000003553 ) ;
#83626 = VERTEX_POINT ( 'NONE', #57829 ) ;
#83627 = CARTESIAN_POINT ( 'NONE',  ( 0.000000000000000000, 65.60000000000000853, 118.5560000000000116 ) ) ;
#83628 = CARTESIAN_POINT ( 'NONE',  ( 37.06648329127298780, 12.92155284005730387, 358.9756252759109998 ) ) ;
#83629 = CARTESIAN_POINT ( 'NONE',  ( 67.35034461891076774, -127.7125575906254937, 246.8833065113800274 ) ) ;
#83630 = CIRCLE ( 'NONE', #6775, 13.44999999999999396 ) ;
#83631 = DIRECTION ( 'NONE',  ( 0.000000000000000000, 0.000000000000000000, 1.000000000000000000 ) ) ;
#83632 = ORIENTED_EDGE ( 'NONE', *, *, #65061, .T. ) ;
#83633 = CARTESIAN_POINT ( 'NONE',  ( 107.8700610081582738, -26.31308374369285730, 70.01562527591099183 ) ) ;
#83634 = VECTOR ( 'NONE', #80406, 1000.000000000000000 ) ;
#83635 = EDGE_CURVE ( 'NONE', #31632, #11502, #23983, .T. ) ;
#83637 = CARTESIAN_POINT ( 'NONE',  ( 84.72210942531978617, 75.15271101351807204, -99.33321048326455127 ) ) ;
#83636 = DIRECTION ( 'NONE',  ( 0.7071067811865453523, 0.7071067811865496822, 0.000000000000000000 ) ) ;
#83638 = DIRECTION ( 'NONE',  ( 0.7071067811865279218, -0.7071067811865670016, 6.612322855859973915E-17 ) ) ;
#83639 = ADVANCED_FACE ( 'NONE', ( #36942 ), #68403, .T. ) ;
#83640 = CARTESIAN_POINT ( 'NONE',  ( 132.9233478419694165, -16.22821065591804768, 1.829869330583287157 ) ) ;
#83641 = ORIENTED_EDGE ( 'NONE', *, *, #21898, .T. ) ;
#83642 = ADVANCED_FACE ( 'NONE', ( #31015 ), #23779, .F. ) ;
#83643 = CARTESIAN_POINT ( 'NONE',  ( 192.5667039024472444, -23.42844715993434335, 300.4678068554149490 ) ) ;
#83644 = LINE ( 'NONE', #89110, #5236 ) ;
#83645 = DIRECTION ( 'NONE',  ( -0.1811243269279065315, 0.9834602067165264527, 0.000000000000000000 ) ) ;
#83646 = ADVANCED_FACE ( 'NONE', ( #51010 ), #51444, .T. ) ;
#83648 = ADVANCED_FACE ( 'NONE', ( #30577 ), #80080, .T. ) ;
#83647 = CARTESIAN_POINT ( 'NONE',  ( 114.0008668920709738, -28.09234522576677762, 115.5261014663869474 ) ) ;
#83650 = DIRECTION ( 'NONE',  ( 1.000000000000000078E-15, -1.000000000000000083E-30, -1.000000000000000000 ) ) ;
#83649 = CYLINDRICAL_SURFACE ( 'NONE', #30541, 3.174999999999983391 ) ;
#83651 = LINE ( 'NONE', #63646, #21974 ) ;
#83652 = EDGE_CURVE ( 'NONE', #77712, #40497, #9139, .T. ) ;
#83654 = EDGE_CURVE ( 'NONE', #42800, #13980, #18729, .T. ) ;
#83653 = CARTESIAN_POINT ( 'NONE',  ( -47.02966122971771767, 65.60000000000000853, -44.00307561052230199 ) ) ;
#83655 = CARTESIAN_POINT ( 'NONE',  ( 116.2961327041337825, -39.96626766897446714, 129.5584824187679658 ) ) ;
#83657 = EDGE_LOOP ( 'NONE', ( #782, #41204, #10036, #1218 ) ) ;
#83656 = DIRECTION ( 'NONE',  ( 1.000000000000000078E-15, 0.000000000000000000, -1.000000000000000000 ) ) ;
#83658 = CARTESIAN_POINT ( 'NONE',  ( 116.5858064714420976, -40.92601143571967270, 249.4956252759109532 ) ) ;
#83659 = DIRECTION ( 'NONE',  ( 0.000000000000000000, 0.000000000000000000, -1.000000000000000000 ) ) ;
#83660 = CARTESIAN_POINT ( 'NONE',  ( 130.0664832912740110, -14.47844715994100007, 284.9256252759119548 ) ) ;
#83661 = DIRECTION ( 'NONE',  ( 0.000000000000000000, -1.000000000000000000, 0.000000000000000000 ) ) ;
#83662 = DIRECTION ( 'NONE',  ( -1.000000000000000000, 0.000000000000000000, 5.463695987328529395E-16 ) ) ;
#83663 = EDGE_CURVE ( 'NONE', #19584, #37970, #60957, .T. ) ;
#83664 = CARTESIAN_POINT ( 'NONE',  ( 142.8698897858160706, -0.9167816978817300289, 540.9756252759101471 ) ) ;
#83665 = LINE ( 'NONE', #27341, #39876 ) ;
#83666 = AXIS2_PLACEMENT_3D ( 'NONE', #8868, #79247, #57434 ) ;
#83667 = CARTESIAN_POINT ( 'NONE',  ( 113.2764755850018048, -45.03455287549805774, 188.0994347997209672 ) ) ;
#83668 = ORIENTED_EDGE ( 'NONE', *, *, #46792, .T. ) ;
#83669 = VERTEX_POINT ( 'NONE', #18275 ) ;
#83670 = EDGE_CURVE ( 'NONE', #28502, #36969, #40056, .T. ) ;
#83671 = CARTESIAN_POINT ( 'NONE',  ( 109.4376220470258119, -28.19094731436911871, 171.2930118773249717 ) ) ;
#83672 = VECTOR ( 'NONE', #79285, 1000.000000000000000 ) ;
#83673 = FACE_OUTER_BOUND ( 'NONE', #26028, .T. ) ;
#83674 = AXIS2_PLACEMENT_3D ( 'NONE', #35507, #21003, #84592 ) ;
#83675 = CARTESIAN_POINT ( 'NONE',  ( 115.1244435615320612, -31.12738976831575144, 275.3099109901961015 ) ) ;
#83676 = CARTESIAN_POINT ( 'NONE',  ( 75.31670390244798341, -67.87844715994100397, 35.51780685541480409 ) ) ;
#83677 = CARTESIAN_POINT ( 'NONE',  ( 115.0366439558389544, -42.90924087293481648, 268.3024198942891871 ) ) ;
#83678 = CARTESIAN_POINT ( 'NONE',  ( 165.6738106836030227, -28.98061976758901892, 193.9678068554150059 ) ) ;
#83679 = CARTESIAN_POINT ( 'NONE',  ( 98.34985890914866502, -31.65658481524367929, 106.9064586097658207 ) ) ;
#83680 = DIRECTION ( 'NONE',  ( 0.000000000000000000, 0.000000000000000000, -1.000000000000000000 ) ) ;
#83681 = CARTESIAN_POINT ( 'NONE',  ( 97.49318720818078532, -40.89074837367932957, 231.6527681330539679 ) ) ;
#83682 = CARTESIAN_POINT ( 'NONE',  ( 2.061567565891823328, 94.98702740777858367, 118.3387339768891593 ) ) ;
#83683 = ORIENTED_EDGE ( 'NONE', *, *, #25200, .F. ) ;
#83684 = VERTEX_POINT ( 'NONE', #87775 ) ;
#83685 = EDGE_CURVE ( 'NONE', #77202, #21144, #25996, .T. ) ;
#83686 = CARTESIAN_POINT ( 'NONE',  ( -84.90151352399661278, 74.80151635532862997, -99.18073718829371899 ) ) ;
#83687 = CARTESIAN_POINT ( 'NONE',  ( -92.32962665258507684, 82.54999999999999716, -74.36911441044765070 ) ) ;
#83688 = DIRECTION ( 'NONE',  ( 0.000000000000000000, 0.000000000000000000, -1.000000000000000000 ) ) ;
#83690 = ADVANCED_FACE ( 'NONE', ( #59594 ), #87331, .F. ) ;
#83689 = FACE_OUTER_BOUND ( 'NONE', #7261, .T. ) ;
#83691 = VECTOR ( 'NONE', #62701, 1000.000000000000000 ) ;
#83692 = CARTESIAN_POINT ( 'NONE',  ( 80.06648329127399677, -8.350947159940998787, 296.1531252759119752 ) ) ;
#83693 = CLOSED_SHELL ( 'NONE', ( #47605, #46929, #58758, #48332 ) ) ;
#83694 = ORIENTED_EDGE ( 'NONE', *, *, #8054, .F. ) ;
#83695 = CARTESIAN_POINT ( 'NONE',  ( 181.5667039024459939, -18.82844715994031048, -5.074374724088000832 ) ) ;
#83696 = CARTESIAN_POINT ( 'NONE',  ( 110.7331673686684610, -26.30186281216086996, 254.8194347997205682 ) ) ;
#83697 = ORIENTED_EDGE ( 'NONE', *, *, #7956, .F. ) ;
#83698 = CARTESIAN_POINT ( 'NONE',  ( 77.38816033347453072, -37.35482103167625212, 6.853567712192049299 ) ) ;
#83699 = LINE ( 'NONE', #29179, #86332 ) ;
#83700 = CARTESIAN_POINT ( 'NONE',  ( 110.9691608666757219, -45.93657765348226718, 167.8955081847088309 ) ) ;
#83701 = CARTESIAN_POINT ( 'NONE',  ( 115.6184857618795121, -38.05767108254817543, 66.50999513149596964 ) ) ;
#83702 = CARTESIAN_POINT ( 'NONE',  ( 112.4974222397575545, -26.16880547358812947, 165.6984824187679521 ) ) ;
#83703 = DIRECTION ( 'NONE',  ( 1.000000000000000078E-15, -1.000000000000000083E-30, -1.000000000000000000 ) ) ;
#83704 = EDGE_LOOP ( 'NONE', ( #71252, #52874, #89105, #71109 ) ) ;
#83705 = CARTESIAN_POINT ( 'NONE',  ( 107.0664832912739399, -36.72944715994095333, 293.6369201390379544 ) ) ;
#83706 = VERTEX_POINT ( 'NONE', #45959 ) ;
#83707 = VERTEX_POINT ( 'NONE', #46412 ) ;
#83708 = EDGE_CURVE ( 'NONE', #7908, #87146, #12366, .T. ) ;
#83709 = DIRECTION ( 'NONE',  ( 0.7071067811868657627, 0.7071067811862293828, 7.071067811868650498E-16 ) ) ;
#83710 = ORIENTED_EDGE ( 'NONE', *, *, #14096, .T. ) ;
#83711 = ORIENTED_EDGE ( 'NONE', *, *, #28563, .T. ) ;
#83712 = DIRECTION ( 'NONE',  ( -1.000000000000000000, 0.000000000000000000, 0.000000000000000000 ) ) ;
#83713 = CARTESIAN_POINT ( 'NONE',  ( 92.81551872686563343, -113.5468731908974291, -21.78219314458173983 ) ) ;
#83714 = CARTESIAN_POINT ( 'NONE',  ( 115.6929481903037100, -41.18531195142565338, 92.86956268521994673 ) ) ;
#83715 = CARTESIAN_POINT ( 'NONE',  ( 109.9663390834669912, -48.24573355310754152, 242.7727681330539724 ) ) ;
#83716 = CARTESIAN_POINT ( 'NONE',  ( 98.45302666770167832, -29.83944080489365902, 195.7775300378159784 ) ) ;
#83717 = PLANE ( 'NONE',  #58599 ) ;
#83718 = CARTESIAN_POINT ( 'NONE',  ( 173.9900000000000091, 28.98850000000000193, -7.937500000000000000 ) ) ;
#83719 = VECTOR ( 'NONE', #84769, 1000.000000000000000 ) ;
#83720 = ORIENTED_EDGE ( 'NONE', *, *, #16535, .F. ) ;
#83721 = CARTESIAN_POINT ( 'NONE',  ( 59.56670390244700997, -79.67844715994098692, 155.2178068554179902 ) ) ;
#83722 = CIRCLE ( 'NONE', #9743, 16.09746158385918946 ) ;
#83723 = CARTESIAN_POINT ( 'NONE',  ( 72.96458098368650269, 117.4749999999999943, 72.96458098368729850 ) ) ;
#83724 = CARTESIAN_POINT ( 'NONE',  ( 70.86177220334050730, -139.0548940191880263, 247.5038799219895225 ) ) ;
#83725 = EDGE_CURVE ( 'NONE', #81584, #18119, #33255, .T. ) ;
#83726 = CARTESIAN_POINT ( 'NONE',  ( 98.99072789581755671, -31.21169308021397981, 120.8499109901969604 ) ) ;
#83727 = CARTESIAN_POINT ( 'NONE',  ( 96.29295924727914269, -41.78513476824832651, 61.67562527591097421 ) ) ;
#83729 = CARTESIAN_POINT ( 'NONE',  ( 105.1007409166104054, -25.80476224416663200, 275.2061014663870537 ) ) ;
#83728 = CIRCLE ( 'NONE', #25753, 7.999999999999992895 ) ;
#83730 = VERTEX_POINT ( 'NONE', #63199 ) ;
#83731 = AXIS2_PLACEMENT_3D ( 'NONE', #64026, #14535, #28136 ) ;
#83732 = CARTESIAN_POINT ( 'NONE',  ( 97.91908366271991326, -41.73065806300744640, 221.7241967044819546 ) ) ;
#83733 = PLANE ( 'NONE',  #13788 ) ;
#83734 = VECTOR ( 'NONE', #64802, 1000.000000000000000 ) ;
#83735 = CARTESIAN_POINT ( 'NONE',  ( 107.0667039024470313, -104.2784471599418197, -11.78219314458200984 ) ) ;
#83736 = ADVANCED_FACE ( 'NONE', ( #29136 ), #27332, .F. ) ;
#83738 = DIRECTION ( 'NONE',  ( 1.000000000000000000, 4.163336342344333240E-14, 0.000000000000000000 ) ) ;
#83737 = CARTESIAN_POINT ( 'NONE',  ( 107.9576737208367518, -46.48113836195031467, 277.6356252759107974 ) ) ;
#83739 = CARTESIAN_POINT ( 'NONE',  ( 105.5702964725068114, -25.36820327604221248, 320.9276179173060086 ) ) ;
#83740 = EDGE_CURVE ( 'NONE', #49393, #16580, #31219, .T. ) ;
#83741 = CARTESIAN_POINT ( 'NONE',  ( 97.81168895331838087, -40.51742574516882200, 9.635625275910941312 ) ) ;
#83742 = CARTESIAN_POINT ( 'NONE',  ( 12.05172457139580899, 86.64129263485732224, -117.9422889837464794 ) ) ;
#83743 = EDGE_CURVE ( 'NONE', #74068, #67267, #15059, .T. ) ;
#83744 = CARTESIAN_POINT ( 'NONE',  ( 130.0664832912740110, -18.72922654876698090, 199.5838068554170093 ) ) ;
#83745 = DIRECTION ( 'NONE',  ( 2.050609665440986486E-14, 0.7071067811865465735, 0.7071067811865484609 ) ) ;
#83746 = CARTESIAN_POINT ( 'NONE',  ( 0.000000000000000000, 95.25000000000000000, 0.000000000000000000 ) ) ;
#83747 = VECTOR ( 'NONE', #76681, 1000.000000000000000 ) ;
#83749 = ORIENTED_EDGE ( 'NONE', *, *, #34291, .T. ) ;
#83748 = DIRECTION ( 'NONE',  ( 0.000000000000000000, 1.000000000000000000, 0.000000000000000000 ) ) ;
#83750 = ADVANCED_FACE ( 'NONE', ( #41835 ), #82, .T. ) ;
#83751 = CARTESIAN_POINT ( 'NONE',  ( 110.8821949118858612, -131.5792096921222196, 250.2178068554180470 ) ) ;
#83752 = CARTESIAN_POINT ( 'NONE',  ( 116.6260796636124155, -40.94376574832517690, 253.4956252759109532 ) ) ;
#83753 = CARTESIAN_POINT ( 'NONE',  ( 102.6161641507259219, -46.84718603934155823, 128.2346728949589760 ) ) ;
#83754 = CARTESIAN_POINT ( 'NONE',  ( 100.5371587349295055, -27.78220587661078156, 26.56610146638793779 ) ) ;
#83755 = AXIS2_PLACEMENT_3D ( 'NONE', #18863, #39304, #52451 ) ;
#83756 = LINE ( 'NONE', #36039, #78007 ) ;
#83757 = VECTOR ( 'NONE', #44823, 1000.000000000000000 ) ;
#83759 = DIRECTION ( 'NONE',  ( -3.100000000000000258E-29, 3.100000000000000044E-14, 1.000000000000000000 ) ) ;
#83758 = DIRECTION ( 'NONE',  ( 2.279500465453769633E-16, -3.481761372429950061E-31, -1.000000000000000000 ) ) ;
#83760 = CARTESIAN_POINT ( 'NONE',  ( 97.83894798970808893, -40.58344824236100834, 137.6413097730125230 ) ) ;
#83761 = DIRECTION ( 'NONE',  ( -1.000000000000000000, 0.000000000000000000, 0.000000000000000000 ) ) ;
#83763 = EDGE_CURVE ( 'NONE', #18132, #1382, #27778, .T. ) ;
#83762 = VECTOR ( 'NONE', #40085, 1000.000000000000000 ) ;
#83764 = EDGE_LOOP ( 'NONE', ( #72362, #58274 ) ) ;
#83765 = CARTESIAN_POINT ( 'NONE',  ( 34.67381068360400320, -28.98061976758901892, 313.9678068554150059 ) ) ;
#83766 = VERTEX_POINT ( 'NONE', #68677 ) ;
#83767 = EDGE_CURVE ( 'NONE', #85398, #62066, #55459, .T. ) ;
#83768 = CARTESIAN_POINT ( 'NONE',  ( 103.7078221352084881, -28.31921139840152435, 174.8133722090289552 ) ) ;
#83770 = VERTEX_POINT ( 'NONE', #42731 ) ;
#83769 = DIRECTION ( 'NONE',  ( -1.000000000000000078E-15, 1.000000000000000000, 0.000000000000000000 ) ) ;
#83771 = LINE ( 'NONE', #8356, #80956 ) ;
#83772 = CARTESIAN_POINT ( 'NONE',  ( 114.5119312840559473, -28.59475203354334027, 150.4746728949579619 ) ) ;
#83773 = CARTESIAN_POINT ( 'NONE',  ( 107.0664832912750057, -36.72944715993903486, 4.925625275910970657 ) ) ;
#83774 = CARTESIAN_POINT ( 'NONE',  ( 80.06648329127399677, -33.97944715994105991, 8.225625275910942946 ) ) ;
#83775 = DIRECTION ( 'NONE',  ( 0.000000000000000000, 0.000000000000000000, 1.000000000000000000 ) ) ;
#83776 = CARTESIAN_POINT ( 'NONE',  ( -80.31601416995057718, 70.80054593973557076, 87.20837843453702476 ) ) ;
#83777 = PLANE ( 'NONE',  #45408 ) ;
#83778 = CARTESIAN_POINT ( 'NONE',  ( 112.9285164932676224, -28.85859325239445994, 104.5670538473399347 ) ) ;
#83779 = AXIS2_PLACEMENT_3D ( 'NONE', #4919, #26255, #19441 ) ;
#83780 = ORIENTED_EDGE ( 'NONE', *, *, #39315, .T. ) ;
#83781 = EDGE_LOOP ( 'NONE', ( #74770, #58233, #35004, #74362, #40457, #87007, #12177, #71976 ) ) ;
#83782 = ORIENTED_EDGE ( 'NONE', *, *, #33575, .F. ) ;
#83783 = CARTESIAN_POINT ( 'NONE',  ( 116.9829645355111154, -34.95910688594825189, 45.39872616303996722 ) ) ;
#83784 = CARTESIAN_POINT ( 'NONE',  ( 134.4101120871804653, -100.8945472140119080, 250.2178068554180470 ) ) ;
#83786 = CARTESIAN_POINT ( 'NONE',  ( 97.81168731305311326, -40.51740136754563082, 36.63591984386916067 ) ) ;
#83785 = CARTESIAN_POINT ( 'NONE',  ( 109.2168187703260998, -26.58475186820039582, 180.9222919425769760 ) ) ;
#83787 = CARTESIAN_POINT ( 'NONE',  ( 97.31577621049066806, -39.30573770266337164, 56.53083703567445895 ) ) ;
#83788 = DIRECTION ( 'NONE',  ( 1.387778780781444492E-15, 0.000000000000000000, -1.000000000000000000 ) ) ;
#83789 = CARTESIAN_POINT ( 'NONE',  ( 213.1962561210690126, 52.73749999999999716, -44.45000000000000284 ) ) ;
#83790 = CARTESIAN_POINT ( 'NONE',  ( -479.3614999999999782, 100.8062500000000057, 86.36305401447658880 ) ) ;
#83791 = CARTESIAN_POINT ( 'NONE',  ( 67.08338700029372603, -67.89281568731828997, 245.7496557518025782 ) ) ;
#83792 = CARTESIAN_POINT ( 'NONE',  ( 98.00553567079148820, -41.84099229931894115, 136.7356252759109623 ) ) ;
#83793 = ORIENTED_EDGE ( 'NONE', *, *, #71238, .T. ) ;
#83794 = ORIENTED_EDGE ( 'NONE', *, *, #13588, .T. ) ;
#83795 = VERTEX_POINT ( 'NONE', #6444 ) ;
#83796 = CARTESIAN_POINT ( 'NONE',  ( 7.759765182912740755, 72.46180059790658845, 130.3270382739332831 ) ) ;
#83797 = CARTESIAN_POINT ( 'NONE',  ( 117.0667039024470313, -98.59953881414097054, 7.717806855417813416 ) ) ;
#83798 = CIRCLE ( 'NONE', #40266, 3.968750000000520473 ) ;
#83799 = DIRECTION ( 'NONE',  ( 0.000000000000000000, -1.000000000000000000, 0.000000000000000000 ) ) ;
#83801 = ADVANCED_FACE ( 'NONE', ( #520 ), #34138, .F. ) ;
#83800 = DIRECTION ( 'NONE',  ( 1.825781832977096147E-16, 0.5000000000000003331, -0.8660254037844384856 ) ) ;
#83802 = CARTESIAN_POINT ( 'NONE',  ( 113.2609745038455742, -30.68550774403005121, 192.2718998934009562 ) ) ;
#83803 = VECTOR ( 'NONE', #20851, 1000.000000000000000 ) ;
#83804 = AXIS2_PLACEMENT_3D ( 'NONE', #8815, #17397, #31018 ) ;
#83805 = CYLINDRICAL_SURFACE ( 'NONE', #69695, 13.16666666666669627 ) ;
#83806 = CARTESIAN_POINT ( 'NONE',  ( 107.0620278373210255, -36.73691869758540207, 361.9756252759100903 ) ) ;
#83807 = VERTEX_POINT ( 'NONE', #20973 ) ;
#83809 = ORIENTED_EDGE ( 'NONE', *, *, #56546, .T. ) ;
#83808 = ORIENTED_EDGE ( 'NONE', *, *, #35019, .F. ) ;
#83810 = AXIS2_PLACEMENT_3D ( 'NONE', #70722, #63907, #50249 ) ;
#83811 = CARTESIAN_POINT ( 'NONE',  ( 116.3201542697790529, -32.94256427661516540, 65.13562527591099638 ) ) ;
#83812 = ORIENTED_EDGE ( 'NONE', *, *, #88767, .F. ) ;
#83813 = ORIENTED_EDGE ( 'NONE', *, *, #35315, .F. ) ;
#83814 = CARTESIAN_POINT ( 'NONE',  ( 163.5667039024460223, -18.82844715994111340, 342.9256252759109884 ) ) ;
#83815 = CARTESIAN_POINT ( 'NONE',  ( 109.5261983718769585, -46.49778922373468504, 239.2044404487539566 ) ) ;
#83816 = CIRCLE ( 'NONE', #35946, 5.599999999999994316 ) ;
#83817 = CARTESIAN_POINT ( 'NONE',  ( 108.4179576672466396, -26.73509541248044030, 180.9693683432445823 ) ) ;
#83818 = ORIENTED_EDGE ( 'NONE', *, *, #76774, .F. ) ;
#83819 = VECTOR ( 'NONE', #84583, 1000.000000000000000 ) ;
#83820 = AXIS2_PLACEMENT_3D ( 'NONE', #3942, #66608, #4399 ) ;
#83821 = DIRECTION ( 'NONE',  ( -0.7071067812163264188, 0.7071067811567686157, -7.071067812163272297E-16 ) ) ;
#83822 = CARTESIAN_POINT ( 'NONE',  ( -117.7484220338073300, 73.87720319330706786, 56.41025224552601003 ) ) ;
#83823 = VERTEX_POINT ( 'NONE', #1433 ) ;
#83824 = VERTEX_POINT ( 'NONE', #13708 ) ;
#83825 = VECTOR ( 'NONE', #29140, 1000.000000000000000 ) ;
#83826 = EDGE_CURVE ( 'NONE', #82610, #2655, #84938, .T. ) ;
#83827 = DIRECTION ( 'NONE',  ( 0.000000000000000000, 1.000000000000000000, 1.914177628664063178E-15 ) ) ;
#83828 = EDGE_LOOP ( 'NONE', ( #40694, #64988, #61867, #63722, #5377, #82476 ) ) ;
#83829 = VERTEX_POINT ( 'NONE', #69570 ) ;
#83830 = CARTESIAN_POINT ( 'NONE',  ( 106.8863607564096725, -44.89016293055450291, 270.3766617981627860 ) ) ;
#83831 = CARTESIAN_POINT ( 'NONE',  ( 96.64877318785802629, -35.94450158219160585, 146.2670538473399517 ) ) ;
#83832 = CARTESIAN_POINT ( 'NONE',  ( 102.5676158828201352, -27.34920955258903419, 95.43276813305395478 ) ) ;
#83833 = FACE_OUTER_BOUND ( 'NONE', #89071, .T. ) ;
#83834 = CARTESIAN_POINT ( 'NONE',  ( 100.6563598938200812, -44.95093154396422364, 228.0499109901969348 ) ) ;
#83835 = LINE ( 'NONE', #21610, #68959 ) ;
#83836 = CARTESIAN_POINT ( 'NONE',  ( 51.23005224011598102, -33.89581943344511217, -5.074374724088000832 ) ) ;
#83837 = ORIENTED_EDGE ( 'NONE', *, *, #58202, .T. ) ;
#83838 = CARTESIAN_POINT ( 'NONE',  ( 129.9681501387582898, 79.66749569656610674, 12.37561169055549826 ) ) ;
#83839 = ORIENTED_EDGE ( 'NONE', *, *, #52344, .T. ) ;
#83840 = ORIENTED_EDGE ( 'NONE', *, *, #27657, .F. ) ;
#83841 = CARTESIAN_POINT ( 'NONE',  ( 107.0664832912739968, -36.72944715994100306, 294.6356252759106837 ) ) ;
#83842 = CIRCLE ( 'NONE', #18594, 10.00000000000000888 ) ;
#83843 = VECTOR ( 'NONE', #14712, 1000.000000000000000 ) ;
#83844 = CARTESIAN_POINT ( 'NONE',  ( 103.2806894308011891, -27.47375879996335613, 136.3854383369816503 ) ) ;
#83845 = ORIENTED_EDGE ( 'NONE', *, *, #4282, .F. ) ;
#83846 = CARTESIAN_POINT ( 'NONE',  ( 111.7942743463426609, -25.86259492108981206, 134.7499109901969518 ) ) ;
#83847 = DIRECTION ( 'NONE',  ( -0.7071067811865774377, 0.7071067811865175967, -7.071067811865470403E-16 ) ) ;
#83848 = CARTESIAN_POINT ( 'NONE',  ( 183.5150000000000148, 53.21300000000000097, 41.63456447661469895 ) ) ;
#83849 = CARTESIAN_POINT ( 'NONE',  ( 50.03799999999999670, 101.5999999999999943, 178.6098374884404905 ) ) ;
#83852 = CARTESIAN_POINT ( 'NONE',  ( 107.5091008941355994, -47.12332782054429714, 233.6099109901969655 ) ) ;
#83851 = CARTESIAN_POINT ( 'NONE',  ( 98.03901516409368355, -41.03442269213341120, 56.68020503552938294 ) ) ;
#83850 = DIRECTION ( 'NONE',  ( -1.000000000000000000, 0.000000000000000000, 2.170915417798913171E-16 ) ) ;
#83853 = FACE_BOUND ( 'NONE', #17469, .T. ) ;
#83854 = EDGE_CURVE ( 'NONE', #48254, #56630, #63653, .T. ) ;
#83855 = CARTESIAN_POINT ( 'NONE',  ( -487.2989999999999782, 10.16305401447644030, 97.63125000000000853 ) ) ;
#83856 = ORIENTED_EDGE ( 'NONE', *, *, #29622, .F. ) ;
#83857 = DIRECTION ( 'NONE',  ( 0.000000000000000000, 0.000000000000000000, 1.000000000000000000 ) ) ;
#83858 = EDGE_CURVE ( 'NONE', #23110, #45687, #45720, .T. ) ;
#83859 = CARTESIAN_POINT ( 'NONE',  ( 176.7669697523293735, -48.62818131005481348, 129.9678068554150059 ) ) ;
#83860 = EDGE_CURVE ( 'NONE', #61847, #79697, #61836, .T. ) ;
#83861 = CARTESIAN_POINT ( 'NONE',  ( 41.56648329127499153, -27.82844715994070484, 263.6756252759120116 ) ) ;
#83862 = CARTESIAN_POINT ( 'NONE',  ( 92.91125933621934507, -113.6057974291316981, -19.26696060647573105 ) ) ;
#83864 = ORIENTED_EDGE ( 'NONE', *, *, #51827, .F. ) ;
#83863 = CARTESIAN_POINT ( 'NONE',  ( 115.7319096639420906, -42.60456859047142331, 273.3527681330537575 ) ) ;
#83865 = EDGE_CURVE ( 'NONE', #29557, #26687, #41319, .T. ) ;
#83866 = CARTESIAN_POINT ( 'NONE',  ( 116.3212776292296127, -32.94146857471318413, 287.6356252759109680 ) ) ;
#83867 = CARTESIAN_POINT ( 'NONE',  ( 96.62784866533952766, -37.15519789137512419, 161.3584824187679487 ) ) ;
#83868 = CARTESIAN_POINT ( 'NONE',  ( 97.77247047105220190, -32.00675585678803969, 46.95276813305393659 ) ) ;
#83869 = CARTESIAN_POINT ( 'NONE',  ( 108.1864281049355867, -47.13803512191609713, 198.6613395616249989 ) ) ;
#83870 = AXIS2_PLACEMENT_3D ( 'NONE', #68074, #62595, #20821 ) ;
#83871 = CARTESIAN_POINT ( 'NONE',  ( 107.0667039024470313, -104.2784471599409528, 24.21780685541800082 ) ) ;
#83872 = CARTESIAN_POINT ( 'NONE',  ( 163.0664832912739826, -8.350947159940998787, 335.9181252759120184 ) ) ;
#83874 = CARTESIAN_POINT ( 'NONE',  ( 29.77381068363597194, -48.62134037875381409, 300.4678068554150059 ) ) ;
#83873 = DIRECTION ( 'NONE',  ( -4.299999999999999979E-14, 1.000000000000000000, -4.128053709984630540E-29 ) ) ;
#83875 = DIRECTION ( 'NONE',  ( -0.7071067811865475727, 0.000000000000000000, -0.7071067811865475727 ) ) ;
#83876 = DIRECTION ( 'NONE',  ( 0.8660254037844392627, -0.4999999999999990008, 1.549999999999999706E-14 ) ) ;
#83877 = VERTEX_POINT ( 'NONE', #83212 ) ;
#83878 = DIRECTION ( 'NONE',  ( 0.000000000000000000, 0.000000000000000000, 1.000000000000000000 ) ) ;
#83879 = AXIS2_PLACEMENT_3D ( 'NONE', #36046, #29243, #86882 ) ;
#83880 = AXIS2_PLACEMENT_3D ( 'NONE', #4424, #87989, #53423 ) ;
#83881 = ORIENTED_EDGE ( 'NONE', *, *, #52958, .F. ) ;
#83882 = ORIENTED_EDGE ( 'NONE', *, *, #4031, .T. ) ;
#83883 = ADVANCED_FACE ( 'NONE', ( #20534 ), #76829, .T. ) ;
#83884 = CIRCLE ( 'NONE', #75174, 2.030000000001872529 ) ;
#83886 = ORIENTED_EDGE ( 'NONE', *, *, #1006, .F. ) ;
#83885 = DIRECTION ( 'NONE',  ( 0.000000000000000000, 0.000000000000000000, 1.000000000000000000 ) ) ;
#83887 = CARTESIAN_POINT ( 'NONE',  ( 103.4847015977353379, -25.45917443855082496, 51.32133956162493149 ) ) ;
#83888 = CARTESIAN_POINT ( 'NONE',  ( 167.6524903400755306, -48.32844715993520879, 180.4678068554150059 ) ) ;
#83889 = VECTOR ( 'NONE', #67380, 1000.000000000000000 ) ;
#83890 = DIRECTION ( 'NONE',  ( -1.000000000000000000, 0.000000000000000000, 0.000000000000000000 ) ) ;
#83891 = CARTESIAN_POINT ( 'NONE',  ( 117.4696809092536256, -30.95150704042223211, 175.2299109901969700 ) ) ;
#83892 = VECTOR ( 'NONE', #44887, 1000.000000000000114 ) ;
#83893 = VECTOR ( 'NONE', #37714, 1000.000000000000000 ) ;
#83894 = CARTESIAN_POINT ( 'NONE',  ( 110.2012955024488718, -28.75291567525416170, 269.2009912566482512 ) ) ;
#83895 = EDGE_LOOP ( 'NONE', ( #55836, #11246, #67602, #32567 ) ) ;
#83896 = VERTEX_POINT ( 'NONE', #975 ) ;
#83897 = ORIENTED_EDGE ( 'NONE', *, *, #87559, .F. ) ;
#83898 = ORIENTED_EDGE ( 'NONE', *, *, #36113, .F. ) ;
#83899 = CARTESIAN_POINT ( 'NONE',  ( 107.0664832912739541, -36.72944715994095333, 307.1356252759109680 ) ) ;
#83900 = DIRECTION ( 'NONE',  ( 0.000000000000000000, 0.000000000000000000, -1.000000000000000000 ) ) ;
#83901 = CARTESIAN_POINT ( 'NONE',  ( 105.7990713734985917, -26.72409577044663465, 161.1773275022462144 ) ) ;
#83902 = CARTESIAN_POINT ( 'NONE',  ( 97.81477617152367543, -40.51601309134415629, 21.63528831556280707 ) ) ;
#83903 = CARTESIAN_POINT ( 'NONE',  ( 96.94208673522926745, 93.33885111288432768, 87.44839512528898240 ) ) ;
#83904 = CARTESIAN_POINT ( 'NONE',  ( 179.8608231853569919, -35.55794170701178558, 193.9678068554150059 ) ) ;
#83905 = CIRCLE ( 'NONE', #34530, 16.09746158385918946 ) ;
#83906 = LINE ( 'NONE', #23471, #39884 ) ;
#83907 = CARTESIAN_POINT ( 'NONE',  ( -11.58988490044493957, 87.75625135835190349, 130.0406260143446673 ) ) ;
#83908 = CARTESIAN_POINT ( 'NONE',  ( 97.50674219252212538, -32.62548708300529654, 16.00419670448194154 ) ) ;
#83909 = DIRECTION ( 'NONE',  ( 2.505701470911820065E-15, 0.000000000000000000, 1.000000000000000000 ) ) ;
#83910 = EDGE_LOOP ( 'NONE', ( #84946, #78820, #84576, #63003, #22278, #33972 ) ) ;
#83911 = FACE_OUTER_BOUND ( 'NONE', #73628, .T. ) ;
#83912 = CIRCLE ( 'NONE', #66496, 10.00000000000002487 ) ;
#83914 = EDGE_CURVE ( 'NONE', #62031, #27163, #9451, .T. ) ;
#83913 = CARTESIAN_POINT ( 'NONE',  ( 71.24189083761808661, -0.9290567490904538817, 394.9756252759102040 ) ) ;
#83915 = CARTESIAN_POINT ( 'NONE',  ( 104.1008407059626251, -44.85999997644839254, 95.10428084578198593 ) ) ;
#83916 = B_SPLINE_CURVE_WITH_KNOTS ( 'NONE', 3,
 ( #70083, #61141, #25727, #81169, #67502, #5747, #53849, #74777, #19815, #11665, #82064, #28286, #5293, #33437, #88866, #32984, #55979, #53401 ),
 .UNSPECIFIED., .F., .F.,
 ( 4, 2, 2, 2, 2, 2, 2, 2, 4 ),
 ( 0.4999956047813029492, 0.5624961541836400736, 0.6249967035859771425, 0.6874972529883143224, 0.7499978023906515023, 0.8124983517929885712, 0.8749989011953256401, 0.9374994505976628201, 1.000000000000000000 ),
 .UNSPECIFIED. ) ;
#83917 = EDGE_CURVE ( 'NONE', #27883, #9196, #49549, .T. ) ;
#83918 = CARTESIAN_POINT ( 'NONE',  ( 107.0667039024470313, -104.2784471599413791, 2.217806855418003043 ) ) ;
#83919 = CARTESIAN_POINT ( 'NONE',  ( 102.0670549579451460, -27.97049806049410137, 45.48979194277244886 ) ) ;
#83920 = VERTEX_POINT ( 'NONE', #13265 ) ;
#83921 = ORIENTED_EDGE ( 'NONE', *, *, #11367, .F. ) ;
#83922 = DIRECTION ( 'NONE',  ( -0.8660254037844387076, 0.000000000000000000, 0.4999999999999998890 ) ) ;
#83923 = EDGE_LOOP ( 'NONE', ( #75872, #89333, #67384, #18637 ) ) ;
#83924 = ORIENTED_EDGE ( 'NONE', *, *, #20860, .F. ) ;
#83925 = CARTESIAN_POINT ( 'NONE',  ( 108.4917517584632236, -27.44263408611272936, 141.3749166392299514 ) ) ;
#83926 = AXIS2_PLACEMENT_3D ( 'NONE', #66617, #58896, #58458 ) ;
#83927 = LINE ( 'NONE', #27598, #28649 ) ;
#83928 = CARTESIAN_POINT ( 'NONE',  ( 103.1973475860487639, -46.47157139977531415, 113.2756252759109827 ) ) ;
#83929 = LINE ( 'NONE', #43002, #58988 ) ;
#83930 = CIRCLE ( 'NONE', #46209, 20.63750000000000284 ) ;
#83931 = ORIENTED_EDGE ( 'NONE', *, *, #70183, .T. ) ;
#83932 = AXIS2_PLACEMENT_3D ( 'NONE', #60420, #81361, #59524 ) ;
#83933 = EDGE_CURVE ( 'NONE', #83315, #31262, #85902, .T. ) ;
#83934 =( BOUNDED_CURVE ( )  B_SPLINE_CURVE ( 3, ( #999, #102, #28703, #56838 ),
 .UNSPECIFIED., .F., .T. ) 
 B_SPLINE_CURVE_WITH_KNOTS ( ( 4, 4 ),
 ( 4.777055387349745885, 4.778685762418977134 ),
 .UNSPECIFIED. ) 
 CURVE ( )  GEOMETRIC_REPRESENTATION_ITEM ( )  RATIONAL_B_SPLINE_CURVE ( ( 1.000000000000000000, 0.9999997784897733943, 0.9999997784897733943, 1.000000000000000000 ) ) 
 REPRESENTATION_ITEM ( '' )  );
#83935 = ORIENTED_EDGE ( 'NONE', *, *, #33974, .F. ) ;
#83936 = ORIENTED_EDGE ( 'NONE', *, *, #42183, .T. ) ;
#83937 = VECTOR ( 'NONE', #44231, 1000.000000000000000 ) ;
#83938 = CARTESIAN_POINT ( 'NONE',  ( 86.72755763596092038, -85.76982405743865456, 250.2178068554179902 ) ) ;
#83939 = ORIENTED_EDGE ( 'NONE', *, *, #68360, .F. ) ;
#83940 = CARTESIAN_POINT ( 'NONE',  ( 102.7643194828038276, -25.71402177940525746, 20.37276813305294354 ) ) ;
#83941 = CARTESIAN_POINT ( 'NONE',  ( 117.0891209002388678, -39.67630891660421355, 179.5984824187679294 ) ) ;
#83942 = CARTESIAN_POINT ( 'NONE',  ( 41.56648329127399677, -18.82844715994099971, 21.04262527591200183 ) ) ;
#83943 = CARTESIAN_POINT ( 'NONE',  ( 74.15067561874269586, 127.0000000000000000, -68.53801554307419508 ) ) ;
#83944 = CARTESIAN_POINT ( 'NONE',  ( 96.69923704014651378, -37.82612059164544860, 122.4099109901969626 ) ) ;
#83945 = CARTESIAN_POINT ( 'NONE',  ( 63.03715912545818156, -46.82818131006018092, 313.9678068554150059 ) ) ;
#83946 = VERTEX_POINT ( 'NONE', #85464 ) ;
#83947 = VECTOR ( 'NONE', #25668, 1000.000000000000000 ) ;
#83948 = CARTESIAN_POINT ( 'NONE',  ( 138.8167039024479834, -67.87844715994100397, 63.03480685541479289 ) ) ;
#83949 = AXIS2_PLACEMENT_3D ( 'NONE', #77593, #70784, #835 ) ;
#83950 = CARTESIAN_POINT ( 'NONE',  ( 117.0717238224210917, -35.46104157321313011, 134.9276073507514013 ) ) ;
#83951 = VERTEX_POINT ( 'NONE', #15512 ) ;
#83952 = CYLINDRICAL_SURFACE ( 'NONE', #59077, 0.2500000000000039968 ) ;
#83953 = CARTESIAN_POINT ( 'NONE',  ( 12.27414673259628586, 85.42709173517430088, 117.9189431488524917 ) ) ;
#83954 = CARTESIAN_POINT ( 'NONE',  ( 104.2408938701987040, -46.76453939261368475, 22.35848241876792031 ) ) ;
#83955 = CARTESIAN_POINT ( 'NONE',  ( 17.77918093722091442, 65.59530694298135245, 33.71461300154621910 ) ) ;
#83956 = DIRECTION ( 'NONE',  ( -1.000000000000000078E-15, 0.000000000000000000, 1.000000000000000000 ) ) ;
#83957 = CARTESIAN_POINT ( 'NONE',  ( 180.3503142329310265, -29.99615139349890569, -5.074374724088000832 ) ) ;
#83958 = CARTESIAN_POINT ( 'NONE',  ( 115.5964019700117973, -42.63146254436634308, 13.35657765686398868 ) ) ;
#83960 = CARTESIAN_POINT ( 'NONE',  ( 113.3182355088850386, -45.04474967211692160, 139.0899109901969553 ) ) ;
#83959 = CARTESIAN_POINT ( 'NONE',  ( 97.75853391132390868, -40.38526537496221636, 111.6242890961639773 ) ) ;
#83961 = LINE ( 'NONE', #49404, #32041 ) ;
#83962 = FACE_BOUND ( 'NONE', #57406, .T. ) ;
#83963 = ORIENTED_EDGE ( 'NONE', *, *, #53119, .F. ) ;
#83964 = AXIS2_PLACEMENT_3D ( 'NONE', #38122, #31747, #51730 ) ;
#83965 = PLANE ( 'NONE',  #83146 ) ;
#83966 = DIRECTION ( 'NONE',  ( 0.000000000000000000, 1.000000000000000000, 0.000000000000000000 ) ) ;
#83967 = PLANE ( 'NONE',  #35458 ) ;
#83969 = VERTEX_POINT ( 'NONE', #15957 ) ;
#83968 = EDGE_CURVE ( 'NONE', #34789, #62435, #11377, .T. ) ;
#83970 = CARTESIAN_POINT ( 'NONE',  ( -215.9000000000000057, 0.000000000000000000, -45.33899999999999864 ) ) ;
#83972 = ORIENTED_EDGE ( 'NONE', *, *, #48843, .F. ) ;
#83971 = CARTESIAN_POINT ( 'NONE',  ( 112.8043457091679471, -45.48636447812791062, 178.0384824187679556 ) ) ;
#83973 = CARTESIAN_POINT ( 'NONE',  ( -3.968749999999949818, 127.0000000000000000, -105.4788588808462038 ) ) ;
#83974 = CARTESIAN_POINT ( 'NONE',  ( 104.1798084317939725, -26.65242854998196265, 221.2984824187679465 ) ) ;
#83975 = CARTESIAN_POINT ( 'NONE',  ( 117.4979393226723516, -37.96344061660173708, 49.73276813305393773 ) ) ;
#83976 = CARTESIAN_POINT ( 'NONE',  ( 100.6520717229712574, 79.66695435136416847, 83.15068351451385809 ) ) ;
#83977 = CARTESIAN_POINT ( 'NONE',  ( 181.9694315774339941, -34.03355364505720360, 193.9678068554150059 ) ) ;
#83978 = CIRCLE ( 'NONE', #46191, 3.250000000000002665 ) ;
#83979 = DIRECTION ( 'NONE',  ( 1.000000000000000000, 0.000000000000000000, 0.000000000000000000 ) ) ;
#83980 = ORIENTED_EDGE ( 'NONE', *, *, #24535, .T. ) ;
#83981 = CONTEXT_DEPENDENT_SHAPE_REPRESENTATION ( #61990, #80085 ) ;
#83982 = EDGE_LOOP ( 'NONE', ( #60569, #56221, #50398, #53285 ) ) ;
#83983 = ORIENTED_EDGE ( 'NONE', *, *, #9133, .T. ) ;
#83984 = EDGE_CURVE ( 'NONE', #49178, #6765, #2330, .T. ) ;
#83985 = EDGE_LOOP ( 'NONE', ( #24109, #15192, #740, #20794 ) ) ;
#83986 = DIRECTION ( 'NONE',  ( 1.000000000000000000, 4.163336342344333240E-14, 0.000000000000000000 ) ) ;
#83987 = CARTESIAN_POINT ( 'NONE',  ( 97.61538875609650745, -41.12936756086440226, 252.6727681330536655 ) ) ;
#83988 = CARTESIAN_POINT ( 'NONE',  ( 97.15942515429802029, -38.46280294437263336, 251.4648788724661586 ) ) ;
#83989 = EDGE_CURVE ( 'NONE', #49274, #66921, #6588, .T. ) ;
#83990 = CARTESIAN_POINT ( 'NONE',  ( 136.2777084067364797, -17.08426318378579012, 2.472582314395108671 ) ) ;
#83991 = VECTOR ( 'NONE', #58253, 1000.000000000000000 ) ;
#83993 = CARTESIAN_POINT ( 'NONE',  ( 163.1639762274895702, -34.03355364505878811, 313.9678068554149490 ) ) ;
#83992 = FACE_OUTER_BOUND ( 'NONE', #13749, .T. ) ;
#83994 = FACE_OUTER_BOUND ( 'NONE', #85978, .T. ) ;
#83995 = CARTESIAN_POINT ( 'NONE',  ( 97.75265732597522117, -31.99668793782200993, 50.95276813305294183 ) ) ;
#83996 = EDGE_LOOP ( 'NONE', ( #16376, #41441, #25462, #79651 ) ) ;
#83998 = EDGE_LOOP ( 'NONE', ( #50270, #6872 ) ) ;
#83997 = CIRCLE ( 'NONE', #28814, 34.13125000000000142 ) ;
#83999 = DIRECTION ( 'NONE',  ( -4.299999999999999979E-14, 1.000000000000000000, 0.000000000000000000 ) ) ;
#84000 = CARTESIAN_POINT ( 'NONE',  ( 97.12550670785735463, -37.99649542378719502, 17.42805171007513820 ) ) ;
#84001 = CARTESIAN_POINT ( 'NONE',  ( 98.59486473514179750, -43.92970144294050527, 222.8870538473389615 ) ) ;
#84002 = VECTOR ( 'NONE', #3266, 1000.000000000000000 ) ;
#84003 = CARTESIAN_POINT ( 'NONE',  ( 108.8666348730871078, -46.34312957481623840, 78.72419670448194040 ) ) ;
#84004 = LINE ( 'NONE', #55797, #861 ) ;
#84005 = VECTOR ( 'NONE', #60060, 1000.000000000000000 ) ;
#84006 = CARTESIAN_POINT ( 'NONE',  ( -76.66819259232177330, 55.29345935402049150, 30.84311214076278773 ) ) ;
#84007 = ORIENTED_EDGE ( 'NONE', *, *, #83763, .F. ) ;
#84008 = CARTESIAN_POINT ( 'NONE',  ( 172.5664832912729878, -27.57844715994070484, 258.9256252759120116 ) ) ;
#84009 = ORIENTED_EDGE ( 'NONE', *, *, #22548, .F. ) ;
#84010 = ORIENTED_EDGE ( 'NONE', *, *, #32673, .T. ) ;
#84011 = CARTESIAN_POINT ( 'NONE',  ( -74.89049941105085395, 86.63388195152283799, 91.90730674524705535 ) ) ;
#84012 = CARTESIAN_POINT ( 'NONE',  ( 115.9278856700424143, -36.79130581669468825, 260.2530118773256049 ) ) ;
#84013 = CARTESIAN_POINT ( 'NONE',  ( 181.9790560690580037, -31.62489322948711035, -5.074374724088000832 ) ) ;
#84014 = CARTESIAN_POINT ( 'NONE',  ( 36.23715912545345930, -47.82818131006131779, 117.4678068554150485 ) ) ;
#84015 = EDGE_CURVE ( 'NONE', #73817, #74757, #30473, .T. ) ;
#84016 = FACE_OUTER_BOUND ( 'NONE', #62069, .T. ) ;
#84017 = VECTOR ( 'NONE', #76789, 1000.000000000000000 ) ;
#84018 = CARTESIAN_POINT ( 'NONE',  ( 177.0664832912740110, 12.92155284005802685, 335.5992267699913327 ) ) ;
#84019 = ORIENTED_EDGE ( 'NONE', *, *, #18727, .T. ) ;
#84020 = CARTESIAN_POINT ( 'NONE',  ( 141.9629299006806491, -9.772340378754520884, 14.92562527591104349 ) ) ;
#84021 = LINE ( 'NONE', #20888, #10708 ) ;
#84022 = EDGE_LOOP ( 'NONE', ( #82689, #45786, #36347, #42196 ) ) ;
#84023 = CARTESIAN_POINT ( 'NONE',  ( 111.9289591080100053, -27.50755150920414849, 59.68991099019693536 ) ) ;
#84024 = ORIENTED_EDGE ( 'NONE', *, *, #57005, .F. ) ;
#84025 = CARTESIAN_POINT ( 'NONE',  ( 99.35431583021956214, -34.05534528112548287, 283.8795189410199100 ) ) ;
#84026 = CARTESIAN_POINT ( 'NONE',  ( 100.8881676017241489, -44.70077481762183425, 127.0522015394391673 ) ) ;
#84027 = CARTESIAN_POINT ( 'NONE',  ( 97.38117110781242047, -35.36630255995240191, 181.2156252759109805 ) ) ;
#84028 = CARTESIAN_POINT ( 'NONE',  ( -215.9000000000000057, 3.174999999999999822, -41.27499999999999858 ) ) ;
#84029 = DIRECTION ( 'NONE',  ( 2.900000000000000265E-14, -2.000000000000000155E-15, 1.000000000000000000 ) ) ;
#84030 = FACE_OUTER_BOUND ( 'NONE', #3221, .T. ) ;
#84031 = CARTESIAN_POINT ( 'NONE',  ( 46.48091746482051434, -49.32844715994088602, 129.9678068554150911 ) ) ;
#84032 = VECTOR ( 'NONE', #28465, 1000.000000000000000 ) ;
#84033 = CARTESIAN_POINT ( 'NONE',  ( 97.77292256144662019, -40.53329279276322694, 7.635625275910939536 ) ) ;
#84034 = CARTESIAN_POINT ( 'NONE',  ( 88.20661029664630348, 93.55239623846826191, -79.21650378603804654 ) ) ;
#84035 = VERTEX_POINT ( 'NONE', #36840 ) ;
#84036 = CARTESIAN_POINT ( 'NONE',  ( 151.0667039024469886, -67.87844715994090450, 85.21780685541799016 ) ) ;
#84037 = ORIENTED_EDGE ( 'NONE', *, *, #73173, .T. ) ;
#84038 = CARTESIAN_POINT ( 'NONE',  ( 107.3350663223963153, -26.26422652666180468, 116.0556252759109555 ) ) ;
#84039 = EDGE_CURVE ( 'NONE', #42888, #4612, #89270, .T. ) ;
#84040 = CARTESIAN_POINT ( 'NONE',  ( 124.8317794719591802, 47.79294463634281698, -38.23516268198856949 ) ) ;
#84041 = ORIENTED_EDGE ( 'NONE', *, *, #31797, .F. ) ;
#84042 = LINE ( 'NONE', #3475, #9540 ) ;
#84043 = VERTEX_POINT ( 'NONE', #16402 ) ;
#84044 = ORIENTED_EDGE ( 'NONE', *, *, #26302, .F. ) ;
#84045 = EDGE_CURVE ( 'NONE', #31761, #50719, #44080, .T. ) ;
#84046 = DIRECTION ( 'NONE',  ( 1.000000000000000000, 0.000000000000000000, 0.000000000000000000 ) ) ;
#84047 = CARTESIAN_POINT ( 'NONE',  ( 97.07207478302663617, -35.37842197911977138, 267.2189570788717674 ) ) ;
#84048 = DIRECTION ( 'NONE',  ( 0.000000000000000000, 0.000000000000000000, 1.000000000000000000 ) ) ;
#84049 = CARTESIAN_POINT ( 'NONE',  ( 51.56670390244671154, -32.29483332968566600, 193.9678068554150911 ) ) ;
#84050 = FACE_OUTER_BOUND ( 'NONE', #33325, .T. ) ;
#84051 = CARTESIAN_POINT ( 'NONE',  ( 105.3204089162997263, -26.45171782723944176, 11.20991099019697046 ) ) ;
#84052 = ADVANCED_FACE ( 'NONE', ( #1877 ), #59044, .F. ) ;
#84053 = LINE ( 'NONE', #49498, #81347 ) ;
#84054 = EDGE_LOOP ( 'NONE', ( #60871, #80634, #42361, #7048 ) ) ;
#84055 = CARTESIAN_POINT ( 'NONE',  ( 1.796236281188243881E-22, 69.84999999999999432, 118.5560000000000116 ) ) ;
#84056 = AXIS2_PLACEMENT_3D ( 'NONE', #64086, #78629, #23653 ) ;
#84057 = EDGE_CURVE ( 'NONE', #61299, #73246, #67532, .T. ) ;
#84058 = LINE ( 'NONE', #43585, #49034 ) ;
#84059 = ORIENTED_EDGE ( 'NONE', *, *, #5227, .F. ) ;
#84060 = ORIENTED_EDGE ( 'NONE', *, *, #42027, .T. ) ;
#84061 = VECTOR ( 'NONE', #64342, 1000.000000000000114 ) ;
#84062 = CIRCLE ( 'NONE', #40465, 4.762500000000002842 ) ;
#84063 = CARTESIAN_POINT ( 'NONE',  ( 123.6837132603318992, -20.11243780205710507, 239.5838068554165545 ) ) ;
#84064 = DIRECTION ( 'NONE',  ( 2.108231265501709878E-16, 0.000000000000000000, -1.000000000000000000 ) ) ;
#84065 = CARTESIAN_POINT ( 'NONE',  ( 2.684158038187649039E-15, 69.84999999999999432, -130.5560000000000116 ) ) ;
#84066 = EDGE_CURVE ( 'NONE', #47474, #10820, #70930, .T. ) ;
#84067 = CARTESIAN_POINT ( 'NONE',  ( 116.3254862984629909, -32.93730789470958342, 129.1356252759109680 ) ) ;
#84068 = PLANE ( 'NONE',  #44595 ) ;
#84069 = CARTESIAN_POINT ( 'NONE',  ( 108.9443472801882393, -27.87019791606706320, 184.3448007804579447 ) ) ;
#84070 = CARTESIAN_POINT ( 'NONE',  ( 41.56648329127398966, -27.82844715994070484, 314.1756252759120116 ) ) ;
#84071 = CARTESIAN_POINT ( 'NONE',  ( 126.2502385374383636, 64.84973863628553659, 33.25376590429844725 ) ) ;
#84072 = CARTESIAN_POINT ( 'NONE',  ( 98.26918992425659383, -28.71468409831775404, 80.73848241876795839 ) ) ;
#84073 = EDGE_LOOP ( 'NONE', ( #59976, #84470, #81060 ) ) ;
#84074 = DIRECTION ( 'NONE',  ( 0.000000000000000000, 0.000000000000000000, 1.000000000000000000 ) ) ;
#84075 = EDGE_LOOP ( 'NONE', ( #73483, #80469, #11877, #73857 ) ) ;
#84076 = VECTOR ( 'NONE', #5153, 1000.000000000000000 ) ;
#84077 = DIRECTION ( 'NONE',  ( -1.000000000000000000, -4.299999999999999979E-14, -1.000000000000000078E-15 ) ) ;
#84079 = ORIENTED_EDGE ( 'NONE', *, *, #55176, .T. ) ;
#84078 = EDGE_CURVE ( 'NONE', #29859, #48706, #16772, .T. ) ;
#84080 = CARTESIAN_POINT ( 'NONE',  ( 109.7247418026906729, -27.00076879412921826, 49.86480213811073980 ) ) ;
#84081 = EDGE_LOOP ( 'NONE', ( #10497, #35381, #38472, #62560 ) ) ;
#84082 = DIRECTION ( 'NONE',  ( 1.000000000000000000, 0.000000000000000000, 1.047445008332812253E-14 ) ) ;
#84083 = VECTOR ( 'NONE', #61935, 1000.000000000000000 ) ;
#84084 = CARTESIAN_POINT ( 'NONE',  ( 80.06648329127402519, -46.72944715994105991, -0.5743747240890559880 ) ) ;
#84085 = CARTESIAN_POINT ( 'NONE',  ( 105.7167510403503741, -46.72405128237544858, 273.4686170738095825 ) ) ;
#84086 = LINE ( 'NONE', #84542, #81505 ) ;
#84087 = EDGE_LOOP ( 'NONE', ( #34189, #75987, #39182, #62265 ) ) ;
#84088 = CARTESIAN_POINT ( 'NONE',  ( 96.17000221327154463, -38.71995997157278424, 51.48229194257797303 ) ) ;
#84090 = CARTESIAN_POINT ( 'NONE',  ( 83.89393544538361880, 76.91670260214422683, -100.0338904447224024 ) ) ;
#84089 = LINE ( 'NONE', #77265, #36193 ) ;
#84091 = CARTESIAN_POINT ( 'NONE',  ( 138.8167039024479834, -50.82844715994100682, 63.03480685541479289 ) ) ;
#84092 = CARTESIAN_POINT ( 'NONE',  ( 112.0659116084588049, -45.48839626879258446, 142.9897919413060094 ) ) ;
#84093 = EDGE_LOOP ( 'NONE', ( #34163, #78332, #1242, #214, #63879, #12523, #21583 ) ) ;
#84094 = EDGE_CURVE ( 'NONE', #59559, #36906, #86336, .T. ) ;
#84095 = CARTESIAN_POINT ( 'NONE',  ( 112.8075328016465022, -28.50283045258476378, 120.5906983358263460 ) ) ;
#84096 = ADVANCED_FACE ( 'NONE', ( #8702 ), #64993, .F. ) ;
#84097 = DIRECTION ( 'NONE',  ( 0.000000000000000000, 0.000000000000000000, 1.000000000000000000 ) ) ;
#84098 = ADVANCED_FACE ( 'NONE', ( #2778 ), #76219, .F. ) ;
#84099 = DIRECTION ( 'NONE',  ( 0.000000000000000000, 1.000000000000000000, 1.047445008332813989E-14 ) ) ;
#84100 = CARTESIAN_POINT ( 'NONE',  ( 117.2306693829537210, -39.29235896168534481, 119.6299109901969615 ) ) ;
#84101 = EDGE_CURVE ( 'NONE', #57694, #50013, #72260, .T. ) ;
#84103 = DIRECTION ( 'NONE',  ( -0.5000000000000003331, 0.000000000000000000, -0.8660254037844383745 ) ) ;
#84102 = CARTESIAN_POINT ( 'NONE',  ( 110.7536356736639078, -102.7271463785351528, 2.217806855417947531 ) ) ;
#84104 = DIRECTION ( 'NONE',  ( 0.000000000000000000, -1.000000000000000000, 0.000000000000000000 ) ) ;
#84105 = AXIS2_PLACEMENT_3D ( 'NONE', #10595, #36535, #57402 ) ;
#84106 = VERTEX_POINT ( 'NONE', #57265 ) ;
#84107 = LINE ( 'NONE', #83653, #49073 ) ;
#84108 = CARTESIAN_POINT ( 'NONE',  ( 98.40655050692429029, -32.18313002855528993, 131.9413395616250000 ) ) ;
#84110 = ORIENTED_EDGE ( 'NONE', *, *, #26882, .T. ) ;
#84109 = DIRECTION ( 'NONE',  ( 0.000000000000000000, 0.000000000000000000, -1.000000000000000000 ) ) ;
#84111 = CARTESIAN_POINT ( 'NONE',  ( 96.58568816239609589, -40.17018292043292860, 282.5908633711490552 ) ) ;
#84112 = CARTESIAN_POINT ( 'NONE',  ( -24.79284581386642827, 184.0000000000000000, 85.23828826961327820 ) ) ;
#84113 = CARTESIAN_POINT ( 'NONE',  ( 193.0371591254574639, -23.42818131005411786, 180.4678068554150343 ) ) ;
#84114 = CARTESIAN_POINT ( 'NONE',  ( 88.01156830653434326, -84.35882332054471533, 250.2178068554179902 ) ) ;
#84115 = LINE ( 'NONE', #89, #76151 ) ;
#84116 = VECTOR ( 'NONE', #66072, 1000.000000000000000 ) ;
#84117 = DIRECTION ( 'NONE',  ( -1.000000000000000078E-15, 1.000000000000000000, 0.000000000000000000 ) ) ;
#84118 = DIRECTION ( 'NONE',  ( -0.9254794337955620787, -0.3787978585227822492, 0.000000000000000000 ) ) ;
#84119 = B_SPLINE_CURVE_WITH_KNOTS ( 'NONE', 3,
 ( #40988, #33736, #11958, #32832, #61426, #60073, #89153, #20565, #87805, #48234, #26917, #46888, #54592, #89606, #6473, #68707, #61872, #27364, #25571, #53246, #81014, #46444, #12397, #77764, #41423, #35508, #7375, #41866, #14647, #63231, #69605, #1008, #28712, #549, #49128 ),
 .UNSPECIFIED., .F., .F.,
 ( 4, 2, 2, 1, 1, 2, 2, 2, 2, 2, 2, 1, 1, 2, 2, 2, 1, 1, 1, 2, 4 ),
 ( 0.3333434881890883217, 0.4166701562233613432, 0.4218780729755014502, 0.4270859897276415573, 0.4375018232319191069, 0.4583334902404722633, 0.4999968242575802968, 0.5208284912661340638, 0.5416601582746880528, 0.5624918252832418197, 0.5650957836593112349, 0.5676997420353806501, 0.5729076587875210347, 0.5833234922918014709, 0.6249868263089239928, 0.6275907846849948513, 0.6301947430610657097, 0.6354026598132067605, 0.6458184933174879738, 0.6562343268217694092, 0.6666501603260506226 ),
 .UNSPECIFIED. ) ;
#84120 = CARTESIAN_POINT ( 'NONE',  ( 116.7742277529940225, -35.53649587948895316, 193.9241967044829664 ) ) ;
#84121 = VERTEX_POINT ( 'NONE', #3220 ) ;
#84122 = ORIENTED_EDGE ( 'NONE', *, *, #69334, .T. ) ;
#84123 = VECTOR ( 'NONE', #79278, 1000.000000000000114 ) ;
#84124 = CARTESIAN_POINT ( 'NONE',  ( 103.6521623672117158, -27.97622271609356659, 166.7920594963739802 ) ) ;
#84125 = VECTOR ( 'NONE', #51057, 1000.000000000000000 ) ;
#84126 = CARTESIAN_POINT ( 'NONE',  ( 30.48091746481751230, -49.32844715994156815, 129.9678068554150627 ) ) ;
#84127 = CARTESIAN_POINT ( 'NONE',  ( 99.18317230595245348, -39.95607890373031523, 8.067297591610955720 ) ) ;
#84128 = DIRECTION ( 'NONE',  ( 0.000000000000000000, -1.000000000000000000, 0.000000000000000000 ) ) ;
#84129 = B_SPLINE_CURVE_WITH_KNOTS ( 'NONE', 3,
 ( #48027, #55281, #27602, #54829, #20352, #13531, #42115, #41213, #69842, #35297, #63011, #44800, #17116, #8969, #72081, #86157, #71637, #63924 ),
 .UNSPECIFIED., .F., .F.,
 ( 4, 2, 2, 2, 2, 2, 2, 2, 4 ),
 ( 0.000000000000000000, 0.06250000006729680702, 0.1250000001345936140, 0.1875000002018904210, 0.2500000002691872281, 0.3125000003364840628, 0.3750000004037808421, 0.4375000004710776214, 0.5000000005383744561 ),
 .UNSPECIFIED. ) ;
#84130 = DIRECTION ( 'NONE',  ( 0.9999999853157766072, 0.0001713722456134502174, 0.000000000000000000 ) ) ;
#84131 = AXIS2_PLACEMENT_3D ( 'NONE', #82821, #34188, #34643 ) ;
#84132 = CARTESIAN_POINT ( 'NONE',  ( 51.03742451361402743, -23.42844715994066362, 313.9678068554150059 ) ) ;
#84133 = DIRECTION ( 'NONE',  ( -1.000000000000000078E-15, 1.000000000000000083E-30, 1.000000000000000000 ) ) ;
#84134 = LINE ( 'NONE', #34160, #37238 ) ;
#84136 = CARTESIAN_POINT ( 'NONE',  ( 97.93839266929572318, -41.72010113774609152, 221.7241967044819546 ) ) ;
#84135 = PRODUCT_DEFINITION_FORMATION_WITH_SPECIFIED_SOURCE ( 'ANY', '', #87948, .NOT_KNOWN. ) ;
#84137 = CARTESIAN_POINT ( 'NONE',  ( 83.06670390244796920, -61.87844715994100397, 207.5838068554149913 ) ) ;
#84138 = ORIENTED_EDGE ( 'NONE', *, *, #63009, .F. ) ;
#84139 = ORIENTED_EDGE ( 'NONE', *, *, #51920, .F. ) ;
#84140 = CARTESIAN_POINT ( 'NONE',  ( 105.7154773117002264, -46.72385838984938289, 87.46895860775489950 ) ) ;
#84141 = CARTESIAN_POINT ( 'NONE',  ( -74.87617104506240651, 86.64222086580517157, -91.91945768840214726 ) ) ;
#84142 = AXIS2_PLACEMENT_3D ( 'NONE', #56538, #62463, #89747 ) ;
#84143 = CARTESIAN_POINT ( 'NONE',  ( 98.15071166569833849, -41.26109095279260686, 122.7000959776797799 ) ) ;
#84144 = DIRECTION ( 'NONE',  ( 1.000000000000000000, 8.673617379883546378E-16, 9.757819552368989676E-16 ) ) ;
#84145 = CARTESIAN_POINT ( 'NONE',  ( 99.56037394151449860, -43.88466257697679396, 32.92038718067297509 ) ) ;
#84146 = CARTESIAN_POINT ( 'NONE',  ( 50.87649884952499946, -33.54226604284930602, -5.074374724088000832 ) ) ;
#84147 = EDGE_LOOP ( 'NONE', ( #14321, #17104, #7465, #37299 ) ) ;
#84148 = CARTESIAN_POINT ( 'NONE',  ( 118.2550939253582811, -40.78236016348033388, 19.54991099019698453 ) ) ;
#84149 = EDGE_CURVE ( 'NONE', #46574, #56872, #79532, .T. ) ;
#84150 = DIRECTION ( 'NONE',  ( 1.000000000000000078E-15, -1.000000000000000083E-30, -1.000000000000000000 ) ) ;
#84151 = CARTESIAN_POINT ( 'NONE',  ( 96.51793475972648650, -31.32865002300666646, 245.9499109901969689 ) ) ;
#84152 = EDGE_CURVE ( 'NONE', #82481, #86394, #17296, .T. ) ;
#84153 = EDGE_LOOP ( 'NONE', ( #29585, #13405, #35339, #25947, #1800, #73808, #73140, #9845, #3818, #78700, #70074, #63471, #72435, #55649, #64551, #25953, #58521, #75226, #9634, #64359, #3624, #20134, #22933, #82229, #73419, #65154, #29412, #86958, #35198, #79817, #79329, #8637, #27013, #35745, #85134, #25526, #58333, #67655, #27764, #16109, #48155, #23884, #35167, #81648, #3940, #46620, #83044, #30441 ) ) ;
#84154 = EDGE_CURVE ( 'NONE', #47812, #75087, #17735, .T. ) ;
#84155 = DIRECTION ( 'NONE',  ( 1.000000000000000000, -0.000000000000000000, 0.000000000000000000 ) ) ;
#84156 = DIRECTION ( 'NONE',  ( 0.000000000000000000, 0.000000000000000000, 1.000000000000000000 ) ) ;
#84157 = CARTESIAN_POINT ( 'NONE',  ( 110.8537976423054374, -45.98451334053003592, 167.8855672870433295 ) ) ;
#84158 = CARTESIAN_POINT ( 'NONE',  ( 99.41042786952979782, -33.89845062227509231, 63.86237608387695985 ) ) ;
#84159 = CARTESIAN_POINT ( 'NONE',  ( 114.2683966348991760, -44.29710505712337465, 154.1813395616249807 ) ) ;
#84160 = EDGE_CURVE ( 'NONE', #30939, #31976, #69026, .T. ) ;
#84161 = DIRECTION ( 'NONE',  ( 0.000000000000000000, 0.000000000000000000, 1.000000000000000000 ) ) ;
#84162 = VERTEX_POINT ( 'NONE', #79983 ) ;
#84163 = ADVANCED_FACE ( 'NONE', ( #54005, #10910, #39512, #18624, #33146, #80416 ), #74035, .T. ) ;
#84164 = LINE ( 'NONE', #70067, #43658 ) ;
#84165 = ORIENTED_EDGE ( 'NONE', *, *, #78726, .F. ) ;
#84166 = ORIENTED_EDGE ( 'NONE', *, *, #5852, .T. ) ;
#84167 = EDGE_CURVE ( 'NONE', #58422, #1886, #11816, .T. ) ;
#84168 = LINE ( 'NONE', #71432, #76415 ) ;
#84169 = EDGE_LOOP ( 'NONE', ( #15800, #1488 ) ) ;
#84170 = ORIENTED_EDGE ( 'NONE', *, *, #33789, .T. ) ;
#84171 = DIRECTION ( 'NONE',  ( 0.000000000000000000, 0.000000000000000000, 1.000000000000000000 ) ) ;
#84172 = EDGE_CURVE ( 'NONE', #57450, #88820, #46754, .T. ) ;
#84173 = DIRECTION ( 'NONE',  ( 3.100000000000000258E-29, -3.100000000000000044E-14, -1.000000000000000000 ) ) ;
#84174 = CARTESIAN_POINT ( 'NONE',  ( 99.03715563995052662, -32.54106229299839725, 90.35432458998199934 ) ) ;
#84175 = CARTESIAN_POINT ( 'NONE',  ( 115.3410742220599872, -45.24796585940374882, 268.1899109901965517 ) ) ;
#84176 = AXIS2_PLACEMENT_3D ( 'NONE', #37646, #70834, #36304 ) ;
#84177 = DIRECTION ( 'NONE',  ( 0.000000000000000000, 0.000000000000000000, 1.000000000000000000 ) ) ;
#84178 = FACE_OUTER_BOUND ( 'NONE', #54913, .T. ) ;
#84180 = ORIENTED_EDGE ( 'NONE', *, *, #2442, .F. ) ;
#84179 = EDGE_CURVE ( 'NONE', #11502, #31632, #26943, .T. ) ;
#84181 = VECTOR ( 'NONE', #72796, 1000.000000000000000 ) ;
#84182 = VERTEX_POINT ( 'NONE', #81326 ) ;
#84183 = PLANE ( 'NONE',  #12 ) ;
#84184 = CARTESIAN_POINT ( 'NONE',  ( 146.0667039024470171, -86.77844715994089597, 55.21780685541800437 ) ) ;
#84185 = CARTESIAN_POINT ( 'NONE',  ( 70.40000325710290952, -140.0960478153407109, 246.9444450209567776 ) ) ;
#84186 = VECTOR ( 'NONE', #8084, 1000.000000000000000 ) ;
#84187 = CARTESIAN_POINT ( 'NONE',  ( 96.70615320395830850, -37.17927570127479697, 116.3489586092449599 ) ) ;
#84188 = CARTESIAN_POINT ( 'NONE',  ( 97.58231912995226764, -32.21254287871169453, 75.97276813305397525 ) ) ;
#84189 = DIRECTION ( 'NONE',  ( -1.000000000000000000, -2.756263715554006823E-15, 0.000000000000000000 ) ) ;
#84190 = ORIENTED_EDGE ( 'NONE', *, *, #88997, .T. ) ;
#84191 = UNCERTAINTY_MEASURE_WITH_UNIT (LENGTH_MEASURE( 1.000000000000000082E-05 ), #19161, 'distance_accuracy_value', 'NONE');
#84192 = CARTESIAN_POINT ( 'NONE',  ( 118.0818320075808856, -32.35879749485835788, 249.1270538473389706 ) ) ;
#84193 = DIRECTION ( 'NONE',  ( 0.000000000000000000, 1.000000000000000000, 0.000000000000000000 ) ) ;
#84194 = DIRECTION ( 'NONE',  ( 0.000000000000000000, 0.000000000000000000, -1.000000000000000000 ) ) ;
#84195 = CARTESIAN_POINT ( 'NONE',  ( -215.9000000000000057, 101.5999999999999943, -41.27499999999999858 ) ) ;
#84197 = DIRECTION ( 'NONE',  ( -0.000000000000000000, -0.000000000000000000, 1.000000000000000000 ) ) ;
#84196 = DIRECTION ( 'NONE',  ( 0.000000000000000000, -1.000000000000000000, 0.000000000000000000 ) ) ;
#84198 = DIRECTION ( 'NONE',  ( 3.999999999999999995E-14, -1.000000000000000000, 4.100000000000000342E-29 ) ) ;
#84199 = CARTESIAN_POINT ( 'NONE',  ( 38.10000000000000142, 95.25000000000000000, 283.4005000000000223 ) ) ;
#84200 = B_SPLINE_CURVE_WITH_KNOTS ( 'NONE', 3,
 ( #27548, #47524, #33909, #55227, #82985, #40720, #74360, #33013, #88446, #292, #33463, #68444, #26206, #61603, #27104, #82543, #61167, #53880 ),
 .UNSPECIFIED., .F., .F.,
 ( 4, 2, 2, 2, 2, 2, 2, 2, 4 ),
 ( 0.000000000000000000, 0.06249999974512615575, 0.1249999994902523115, 0.1874999992353784672, 0.2499999989805046230, 0.3124999987256307787, 0.3749999984707569345, 0.4374999982158830902, 0.4999999979610092460 ),
 .UNSPECIFIED. ) ;
#84201 = CARTESIAN_POINT ( 'NONE',  ( 184.5667039024480118, -67.87844715994100397, 310.9178068554150514 ) ) ;
#84202 = CONICAL_SURFACE ( 'NONE', #76990, 10.66800000000000992, 0.02993239667170383839 ) ;
#84203 = CARTESIAN_POINT ( 'NONE',  ( 163.0664832912739826, 19.62155284005901024, 336.6506252759110112 ) ) ;
#84204 = DIRECTION ( 'NONE',  ( -0.7071067811855830110, -0.7071067811875120235, 0.000000000000000000 ) ) ;
#84205 = CARTESIAN_POINT ( 'NONE',  ( 50.03799999999999670, 20.32000000000000028, 206.3750000000000000 ) ) ;
#84206 = ADVANCED_FACE ( 'NONE', ( #26333 ), #18170, .T. ) ;
#84208 = ORIENTED_EDGE ( 'NONE', *, *, #36542, .T. ) ;
#84207 = CARTESIAN_POINT ( 'NONE',  ( 188.5667039024479834, -48.82844715994099971, 134.4678068554150059 ) ) ;
#84209 = CARTESIAN_POINT ( 'NONE',  ( 121.5948191693372138, -127.7054288962554409, 250.2178068554180470 ) ) ;
#84210 = CARTESIAN_POINT ( 'NONE',  ( 116.2381414160656874, -41.80576965393662903, 263.4241967044824833 ) ) ;
#84211 = CARTESIAN_POINT ( 'NONE',  ( 111.7941755367341443, -25.86282203548705283, 130.7499109901969518 ) ) ;
#84212 = CARTESIAN_POINT ( 'NONE',  ( 116.1773114014176969, -43.03338396708490166, 9.356577656862985037 ) ) ;
#84213 = AXIS2_PLACEMENT_3D ( 'NONE', #86301, #65836, #36811 ) ;
#84214 = EDGE_CURVE ( 'NONE', #12137, #55376, #12258, .T. ) ;
#84215 = CARTESIAN_POINT ( 'NONE',  ( 80.06648329127402519, -46.72944715994105991, -0.8743747240890559214 ) ) ;
#84217 = CARTESIAN_POINT ( 'NONE',  ( 82.54568444101083458, -35.53793914064088000, 7.103892432648359012 ) ) ;
#84216 = CYLINDRICAL_SURFACE ( 'NONE', #88523, 2.500000000000002220 ) ;
#84218 = DIRECTION ( 'NONE',  ( 0.000000000000000000, 1.000000000000000000, 0.000000000000000000 ) ) ;
#84219 = EDGE_LOOP ( 'NONE', ( #8939, #14186, #78467, #11628 ) ) ;
#84220 = CARTESIAN_POINT ( 'NONE',  ( 72.96458098368701428, 127.0000000000000000, -80.10833098368678407 ) ) ;
#84221 = ORIENTED_EDGE ( 'NONE', *, *, #45349, .T. ) ;
#84222 = VECTOR ( 'NONE', #81483, 1000.000000000000000 ) ;
#84223 = CARTESIAN_POINT ( 'NONE',  ( 99.71244791179715605, -41.13061414147755812, 161.1781341137909465 ) ) ;
#84225 = ORIENTED_EDGE ( 'NONE', *, *, #18652, .T. ) ;
#84224 = CARTESIAN_POINT ( 'NONE',  ( 101.9922426440110428, -45.44522117600308775, 187.1568647513990697 ) ) ;
#84226 = VECTOR ( 'NONE', #27431, 1000.000000000000114 ) ;
#84227 = CARTESIAN_POINT ( 'NONE',  ( 142.8687636814962616, 5.654319119531167281, 361.9756252759100335 ) ) ;
#84228 = CARTESIAN_POINT ( 'NONE',  ( 114.3286968523003253, -29.23113535793739359, 170.4641967044829585 ) ) ;
#84229 = CARTESIAN_POINT ( 'NONE',  ( 112.0634988668466576, -45.48974152076988986, 148.9902647339903581 ) ) ;
#84230 = FACE_OUTER_BOUND ( 'NONE', #5977, .T. ) ;
#84231 = FACE_OUTER_BOUND ( 'NONE', #29399, .T. ) ;
#84232 = FACE_OUTER_BOUND ( 'NONE', #84081, .T. ) ;
#84233 = DIRECTION ( 'NONE',  ( -2.900000000000000265E-14, 2.000000000000000155E-15, -1.000000000000000000 ) ) ;
#84234 = CARTESIAN_POINT ( 'NONE',  ( 96.20363159075253634, -34.36081134307595164, 106.1556252759109640 ) ) ;
#84235 = VERTEX_POINT ( 'NONE', #68120 ) ;
#84236 = VECTOR ( 'NONE', #35175, 1000.000000000000000 ) ;
#84237 = ORIENTED_EDGE ( 'NONE', *, *, #85702, .T. ) ;
#84238 = ORIENTED_EDGE ( 'NONE', *, *, #14332, .T. ) ;
#84239 = CARTESIAN_POINT ( 'NONE',  ( 99.86128698970316009, -42.75951115570669714, 68.30063092494498278 ) ) ;
#84240 = CARTESIAN_POINT ( 'NONE',  ( 133.7890526427665066, -97.56809487397632097, 250.2178068554180470 ) ) ;
#84242 = DIRECTION ( 'NONE',  ( 3.100000000000000258E-29, -3.100000000000000044E-14, -1.000000000000000000 ) ) ;
#84241 = CARTESIAN_POINT ( 'NONE',  ( 110.2867295656602380, -27.49400189596552835, 205.8099109901959594 ) ) ;
#84243 = CARTESIAN_POINT ( 'NONE',  ( -103.1875000000000000, 101.5999999999999943, -5.041900000001080073 ) ) ;
#84244 = LINE ( 'NONE', #22015, #20505 ) ;
#84245 = PLANE ( 'NONE',  #89523 ) ;
#84246 = DIRECTION ( 'NONE',  ( -0.000000000000000000, 1.000000000000000000, -0.000000000000000000 ) ) ;
#84247 = DIRECTION ( 'NONE',  ( 0.000000000000000000, 0.000000000000000000, 1.000000000000000000 ) ) ;
#84248 = CARTESIAN_POINT ( 'NONE',  ( 117.1424269838423839, -34.14023410701941685, 124.0270538473399426 ) ) ;
#84249 = ORIENTED_EDGE ( 'NONE', *, *, #60042, .T. ) ;
#84250 = ORIENTED_EDGE ( 'NONE', *, *, #43562, .F. ) ;
#84251 = VECTOR ( 'NONE', #24344, 1000.000000000000000 ) ;
#84252 = ORIENTED_EDGE ( 'NONE', *, *, #68252, .F. ) ;
#84253 = CIRCLE ( 'NONE', #36392, 0.5000000000000007772 ) ;
#84254 = CARTESIAN_POINT ( 'NONE',  ( 5.627553765716396761, 71.15732062108085643, 130.4351721735936280 ) ) ;
#84255 = CARTESIAN_POINT ( 'NONE',  ( -98.06216817836258315, 92.11674985319542941, -86.19179098795304128 ) ) ;
#84256 = CARTESIAN_POINT ( 'NONE',  ( 151.0371591254575776, -24.42818131005592264, 129.9678068554149775 ) ) ;
#84257 = CARTESIAN_POINT ( 'NONE',  ( 131.0667039024480118, -58.72944715994098885, 234.8338068554150198 ) ) ;
#84258 = CARTESIAN_POINT ( 'NONE',  ( 106.8982433325019059, -45.38234380569505788, 225.3671379886389730 ) ) ;
#84259 = ADVANCED_FACE ( 'NONE', ( #32696 ), #53103, .T. ) ;
#84260 = CIRCLE ( 'NONE', #13114, 2.500000000000002220 ) ;
#84261 = DIRECTION ( 'NONE',  ( -0.2588190451025206285, 0.000000000000000000, 0.9659258262890683122 ) ) ;
#84262 = EDGE_CURVE ( 'NONE', #65247, #11013, #5450, .T. ) ;
#84263 = EDGE_CURVE ( 'NONE', #2705, #83951, #49682, .T. ) ;
#84264 = DIRECTION ( 'NONE',  ( -2.301579500234999682E-14, 0.000000000000000000, 1.000000000000000000 ) ) ;
#84265 = ORIENTED_EDGE ( 'NONE', *, *, #65874, .T. ) ;
#84267 = EDGE_LOOP ( 'NONE', ( #57332, #47077, #60430, #10041 ) ) ;
#84266 = ORIENTED_EDGE ( 'NONE', *, *, #87139, .T. ) ;
#84268 = AXIS2_PLACEMENT_3D ( 'NONE', #3933, #30310, #58007 ) ;
#84269 = EDGE_CURVE ( 'NONE', #75328, #3377, #12715, .T. ) ;
#84270 = DIRECTION ( 'NONE',  ( 1.000000000000000000, 0.000000000000000000, 0.000000000000000000 ) ) ;
#84271 = ORIENTED_EDGE ( 'NONE', *, *, #31635, .F. ) ;
#84272 = VERTEX_POINT ( 'NONE', #73131 ) ;
#84273 = LINE ( 'NONE', #22044, #84125 ) ;
#84274 = CARTESIAN_POINT ( 'NONE',  ( 111.6463204169710082, -44.35094448583814852, 234.4387261630399450 ) ) ;
#84275 = EDGE_CURVE ( 'NONE', #45317, #22746, #38616, .T. ) ;
#84276 = DIRECTION ( 'NONE',  ( 1.000000000000000078E-15, -1.000000000000000083E-30, -1.000000000000000000 ) ) ;
#84277 = VERTEX_POINT ( 'NONE', #74937 ) ;
#84278 = LINE ( 'NONE', #21137, #78450 ) ;
#84279 = CARTESIAN_POINT ( 'NONE',  ( -124.2065287780126965, 71.69490183950009055, 40.21978412304718375 ) ) ;
#84280 = EDGE_LOOP ( 'NONE', ( #85444, #1361, #41716, #48894, #21554 ) ) ;
#84281 = VERTEX_POINT ( 'NONE', #87228 ) ;
#84282 = EDGE_CURVE ( 'NONE', #29846, #59106, #40406, .T. ) ;
#84283 = CARTESIAN_POINT ( 'NONE',  ( 110.8548543103858322, -45.98408086708722919, 112.8856581590341932 ) ) ;
#84284 = EDGE_LOOP ( 'NONE', ( #741, #50604, #61914, #12224 ) ) ;
#84285 = ORIENTED_EDGE ( 'NONE', *, *, #57123, .T. ) ;
#84286 = EDGE_CURVE ( 'NONE', #55335, #40086, #52216, .T. ) ;
#84287 = CARTESIAN_POINT ( 'NONE',  ( 113.7913882254195101, -32.05415687329151098, 277.1280903695913480 ) ) ;
#84288 = CARTESIAN_POINT ( 'NONE',  ( 114.5434305778746733, -28.56033675696621899, 154.4746728949589851 ) ) ;
#84289 = AXIS2_PLACEMENT_3D ( 'NONE', #34132, #81428, #33698 ) ;
#84290 = CARTESIAN_POINT ( 'NONE',  ( 108.3168256696638281, -47.05733704442519638, 117.6727681330539639 ) ) ;
#84291 = DIRECTION ( 'NONE',  ( 1.000000000000000078E-15, -1.000000000000000083E-30, -1.000000000000000000 ) ) ;
#84292 = CARTESIAN_POINT ( 'NONE',  ( 77.31648329127402519, -36.72944715994107412, -5.074374724089059541 ) ) ;
#84293 = CARTESIAN_POINT ( 'NONE',  ( 100.8232821092315845, -45.85065428865130599, 238.1108633711489517 ) ) ;
#84294 = CARTESIAN_POINT ( 'NONE',  ( 0.000000000000000000, 111.1250000000000000, 0.000000000000000000 ) ) ;
#84295 = VECTOR ( 'NONE', #83876, 1000.000000000000000 ) ;
#84296 = DIRECTION ( 'NONE',  ( -0.7071067811865175967, -0.7071067811865774377, -7.071067811865168663E-16 ) ) ;
#84297 = ORIENTED_EDGE ( 'NONE', *, *, #27845, .F. ) ;
#84298 = CARTESIAN_POINT ( 'NONE',  ( 130.5480269016124453, 69.93117631934794076, -1.660224752217818622 ) ) ;
#84299 = VERTEX_POINT ( 'NONE', #40844 ) ;
#84300 = ADVANCED_FACE ( 'NONE', ( #48096 ), #77182, .F. ) ;
#84301 = ORIENTED_EDGE ( 'NONE', *, *, #74131, .T. ) ;
#84302 = DIRECTION ( 'NONE',  ( 0.000000000000000000, 0.000000000000000000, 1.000000000000000000 ) ) ;
#84303 = CIRCLE ( 'NONE', #1623, 2.116999999999993776 ) ;
#84304 = CARTESIAN_POINT ( 'NONE',  ( 97.60784930588656039, -39.98230802730879674, 137.5900448901282971 ) ) ;
#84305 = AXIS2_PLACEMENT_3D ( 'NONE', #58220, #84609, #9626 ) ;
#84306 = ORIENTED_EDGE ( 'NONE', *, *, #69083, .T. ) ;
#84307 = CARTESIAN_POINT ( 'NONE',  ( 114.7715153371978687, -44.65482214316887877, 118.2022919425779719 ) ) ;
#84308 = DIRECTION ( 'NONE',  ( 0.000000000000000000, 0.000000000000000000, -1.000000000000000000 ) ) ;
#84309 = DIRECTION ( 'NONE',  ( 0.000000000000000000, 0.000000000000000000, -1.000000000000000000 ) ) ;
#84310 = DIRECTION ( 'NONE',  ( 0.000000000000000000, 1.000000000000000000, 0.000000000000000000 ) ) ;
#84313 = CARTESIAN_POINT ( 'NONE',  ( 118.6297112294782892, -39.20734283244433982, 254.6584824187681022 ) ) ;
#84312 = CARTESIAN_POINT ( 'NONE',  ( 105.6178435110047644, -46.65043233106474929, 57.46071414996635696 ) ) ;
#84311 = CARTESIAN_POINT ( 'NONE',  ( -68.53801554307499089, 120.6499999999999915, 74.15067561874188584 ) ) ;
#84314 = DIRECTION ( 'NONE',  ( 0.000000000000000000, -1.000000000000000000, 0.000000000000000000 ) ) ;
#84315 = DIRECTION ( 'NONE',  ( 1.000000000000000000, 0.000000000000000000, 0.000000000000000000 ) ) ;
#84316 = CARTESIAN_POINT ( 'NONE',  ( 69.68306499799194853, -72.55732494038082336, 540.9756252759101471 ) ) ;
#84317 = CARTESIAN_POINT ( 'NONE',  ( -27.27158787008326968, 184.0000000000000000, 0.000000000000000000 ) ) ;
#84318 = CARTESIAN_POINT ( 'NONE',  ( 194.5664832912739826, -18.82844715994099971, 342.9256252759119548 ) ) ;
#84319 = CARTESIAN_POINT ( 'NONE',  ( 51.34673845256598668, -29.62846900982231446, -5.074374724088000832 ) ) ;
#84320 = VECTOR ( 'NONE', #28930, 1000.000000000000114 ) ;
#84322 = ORIENTED_EDGE ( 'NONE', *, *, #25648, .T. ) ;
#84321 = CARTESIAN_POINT ( 'NONE',  ( 106.8354617269136497, -47.19621815579884583, 272.5584824187680510 ) ) ;
#84323 = DIRECTION ( 'NONE',  ( 0.000000000000000000, 0.000000000000000000, 1.000000000000000000 ) ) ;
#84324 = CARTESIAN_POINT ( 'NONE',  ( 114.4785830672529130, -28.49803820358978612, 159.5051490854349652 ) ) ;
#84325 = CARTESIAN_POINT ( 'NONE',  ( 114.0905851706116181, -46.27390148416495208, 29.08133956162595268 ) ) ;
#84326 = CARTESIAN_POINT ( 'NONE',  ( 101.3252678580387709, -46.22870732629148449, 198.1318157521009482 ) ) ;
#84327 = DIRECTION ( 'NONE',  ( 0.000000000000000000, 0.000000000000000000, 1.000000000000000000 ) ) ;
#84328 = ADVANCED_FACE ( 'NONE', ( #62644 ), #34482, .F. ) ;
#84329 = LINE ( 'NONE', #37047, #15634 ) ;
#84331 = CYLINDRICAL_SURFACE ( 'NONE', #26719, 3.000000000000002665 ) ;
#84330 = FACE_OUTER_BOUND ( 'NONE', #41011, .T. ) ;
#84332 = CARTESIAN_POINT ( 'NONE',  ( 105.7995184974070213, -26.72403496479216756, 70.17729194179682395 ) ) ;
#84333 = LINE ( 'NONE', #21192, #29160 ) ;
#84334 = ORIENTED_EDGE ( 'NONE', *, *, #54319, .F. ) ;
#84335 = VECTOR ( 'NONE', #44948, 1000.000000000000000 ) ;
#84336 = CARTESIAN_POINT ( 'NONE',  ( 156.5667039024483813, -48.82844715993569196, 257.2178068554149490 ) ) ;
#84337 = ORIENTED_EDGE ( 'NONE', *, *, #16373, .F. ) ;
#84338 = ORIENTED_EDGE ( 'NONE', *, *, #74276, .T. ) ;
#84339 = VECTOR ( 'NONE', #8663, 999.9999999999998863 ) ;
#84341 = ORIENTED_EDGE ( 'NONE', *, *, #27308, .T. ) ;
#84340 = FACE_OUTER_BOUND ( 'NONE', #76189, .T. ) ;
#84342 = CARTESIAN_POINT ( 'NONE',  ( 97.64212626138838402, -32.24102647341089778, 71.97276813305397525 ) ) ;
#84343 = DIRECTION ( 'NONE',  ( 3.100000000000000258E-29, -3.100000000000000044E-14, -1.000000000000000000 ) ) ;
#84344 = B_SPLINE_CURVE_WITH_KNOTS ( 'NONE', 3,
 ( #63697, #64591, #27821, #7828, #83698, #1478, #35522, #56864, #55499, #14201, #55953, #48692, #76422, #41879, #69616, #35075, #7385, #1022, #62783, #28259, #28725, #84606, #22366, #50043, #37781, #30957, #73174, #24593, #4144, #17337, #16892, #51824, #58644, #11406, #85947, #72745, #85508, #31843 ),
 .UNSPECIFIED., .F., .F.,
 ( 4, 2, 2, 1, 2, 2, 2, 2, 1, 1, 2, 2, 2, 1, 2, 2, 1, 2, 1, 2, 2, 4 ),
 ( 0.000000000000000000, 0.04166793602364177868, 0.05208492002955201344, 0.05729341203250709613, 0.05989765803398427318, 0.06250190403546145024, 0.08333587204728039322, 0.1041698400590993639, 0.1145868240650088354, 0.1197953160679635781, 0.1223995620694415670, 0.1250038080709195421, 0.1666717440945562900, 0.1770887281004662195, 0.1822972201034212258, 0.1875057121063762045, 0.2083396801181911784, 0.2291736481300061246, 0.2395906321359124735, 0.2447991241388655925, 0.2500076161418187115, 0.3333434881890895429 ),
 .UNSPECIFIED. ) ;
#84345 = VECTOR ( 'NONE', #75345, 1000.000000000000000 ) ;
#84346 = DIRECTION ( 'NONE',  ( 1.000000000000000000, 4.163336342344333240E-14, 0.000000000000000000 ) ) ;
#84347 = EDGE_CURVE ( 'NONE', #1345, #8193, #13601, .T. ) ;
#84348 = CARTESIAN_POINT ( 'NONE',  ( 99.25607838769128932, -29.75875458388292571, 186.7470538473389752 ) ) ;
#84349 = CARTESIAN_POINT ( 'NONE',  ( 98.62497865991430501, -35.42670724699001283, 265.6267055423624583 ) ) ;
#84350 = VERTEX_POINT ( 'NONE', #868 ) ;
#84351 = ORIENTED_EDGE ( 'NONE', *, *, #72446, .T. ) ;
#84352 = ORIENTED_EDGE ( 'NONE', *, *, #37020, .T. ) ;
#84353 = EDGE_CURVE ( 'NONE', #71979, #2341, #61740, .T. ) ;
#84354 = EDGE_LOOP ( 'NONE', ( #51615, #58145, #44427, #71454, #73970, #36313 ) ) ;
#84355 = CARTESIAN_POINT ( 'NONE',  ( 104.4081006654926114, -46.45808914125378664, 107.3647919429337492 ) ) ;
#84356 = FACE_BOUND ( 'NONE', #87133, .T. ) ;
#84357 = CYLINDRICAL_SURFACE ( 'NONE', #72381, 2.500000000000002220 ) ;
#84358 = CARTESIAN_POINT ( 'NONE',  ( 87.71306776503782032, 93.55256755804781221, 96.70275196374507232 ) ) ;
#84359 = CARTESIAN_POINT ( 'NONE',  ( 90.44969454456422397, -23.41243780205710578, 239.5838068554175209 ) ) ;
#84360 = FACE_OUTER_BOUND ( 'NONE', #28131, .T. ) ;
#84361 = VECTOR ( 'NONE', #15507, 1000.000000000000000 ) ;
#84362 = LINE ( 'NONE', #1229, #41912 ) ;
#84363 = CARTESIAN_POINT ( 'NONE',  ( 97.21286698537356585, -39.96429565625729907, 286.5908633711495668 ) ) ;
#84364 = LINE ( 'NONE', #79218, #44352 ) ;
#84365 = VERTEX_POINT ( 'NONE', #28565 ) ;
#84366 = CARTESIAN_POINT ( 'NONE',  ( 130.5667039024470455, -104.2784471599409386, 23.21780685541800082 ) ) ;
#84367 = VECTOR ( 'NONE', #65417, 1000.000000000000000 ) ;
#84368 = DIRECTION ( 'NONE',  ( 1.000000000000000000, 0.000000000000000000, 0.000000000000000000 ) ) ;
#84369 = CARTESIAN_POINT ( 'NONE',  ( 100.6253115865833365, -30.05058211904245624, 113.5052332267339779 ) ) ;
#84370 = AXIS2_PLACEMENT_3D ( 'NONE', #66594, #79366, #53387 ) ;
#84371 = EDGE_CURVE ( 'NONE', #15176, #30425, #10984, .T. ) ;
#84372 = LINE ( 'NONE', #89837, #60097 ) ;
#84373 = EDGE_CURVE ( 'NONE', #10389, #6370, #418, .T. ) ;
#84374 = DIRECTION ( 'NONE',  ( -1.000000000000000000, 0.000000000000000000, 0.000000000000000000 ) ) ;
#84375 = ORIENTED_EDGE ( 'NONE', *, *, #58705, .T. ) ;
#84376 = VERTEX_POINT ( 'NONE', #20865 ) ;
#84377 = CYLINDRICAL_SURFACE ( 'NONE', #14855, 9.999999999999998224 ) ;
#84378 = EDGE_CURVE ( 'NONE', #78030, #46083, #39965, .T. ) ;
#84379 = ORIENTED_EDGE ( 'NONE', *, *, #15565, .T. ) ;
#84380 = EDGE_LOOP ( 'NONE', ( #47961, #54274, #44531, #16950 ) ) ;
#84381 = AXIS2_PLACEMENT_3D ( 'NONE', #33047, #18521, #33499 ) ;
#84382 = CARTESIAN_POINT ( 'NONE',  ( 99.36575536895223593, -31.34657530650553880, 157.2606309249449623 ) ) ;
#84383 = EDGE_CURVE ( 'NONE', #20396, #36063, #5155, .T. ) ;
#84384 = CARTESIAN_POINT ( 'NONE',  ( -12.70000000000000107, 82.54999999999999716, 117.8738102209307641 ) ) ;
#84385 = CARTESIAN_POINT ( 'NONE',  ( 101.7448744985357223, -27.01524695604527082, 96.46324432352997746 ) ) ;
#84386 = VECTOR ( 'NONE', #81077, 1000.000000000000000 ) ;
#84387 = DIRECTION ( 'NONE',  ( 0.000000000000000000, 0.000000000000000000, 1.000000000000000000 ) ) ;
#84388 = VERTEX_POINT ( 'NONE', #82667 ) ;
#84389 = EDGE_LOOP ( 'NONE', ( #76644, #21552, #86250, #45254, #46803, #2691, #51445, #23740, #81680, #75569, #56976, #80020, #16582, #50465, #46975, #3391, #7594, #32704, #36109, #72680, #21475, #13624, #36456, #68264 ) ) ;
#84390 = ORIENTED_EDGE ( 'NONE', *, *, #12588, .T. ) ;
#84391 = ADVANCED_FACE ( 'NONE', ( #83108 ), #70361, .T. ) ;
#84392 = CIRCLE ( 'NONE', #29201, 188.9759999999999991 ) ;
#84393 = DIRECTION ( 'NONE',  ( -0.7071067811865490160, 0.000000000000000000, -0.7071067811865461294 ) ) ;
#84394 = VERTEX_POINT ( 'NONE', #49445 ) ;
#84395 = CARTESIAN_POINT ( 'NONE',  ( 100.6033219294167793, -44.83909144599476804, 272.0289586092449667 ) ) ;
#84396 = CARTESIAN_POINT ( 'NONE',  ( 98.53347975398118308, -44.98838784992466344, 187.9384824187679612 ) ) ;
#84397 = DIRECTION ( 'NONE',  ( 0.000000000000000000, 0.7071067811865671127, 0.7071067811865279218 ) ) ;
#84398 = FACE_OUTER_BOUND ( 'NONE', #21963, .T. ) ;
#84399 = CARTESIAN_POINT ( 'NONE',  ( 96.60720999893194971, -36.88735532319633847, 132.3384824187679669 ) ) ;
#84400 = AXIS2_PLACEMENT_3D ( 'NONE', #74785, #88428, #12565 ) ;
#84401 = DIRECTION ( 'NONE',  ( -0.9254794337955620787, -0.3787978585227822492, 0.000000000000000000 ) ) ;
#84402 = VERTEX_POINT ( 'NONE', #34027 ) ;
#84403 = CARTESIAN_POINT ( 'NONE',  ( 97.75865386173192917, -40.38557078241878884, 116.6246290760604438 ) ) ;
#84404 = ORIENTED_EDGE ( 'NONE', *, *, #33116, .T. ) ;
#84405 = DIRECTION ( 'NONE',  ( -3.999999999999999995E-14, 1.000000000000000000, -4.100000000000000342E-29 ) ) ;
#84406 = ORIENTED_EDGE ( 'NONE', *, *, #56184, .F. ) ;
#84407 = ORIENTED_EDGE ( 'NONE', *, *, #2352, .F. ) ;
#84408 = CARTESIAN_POINT ( 'NONE',  ( 103.1875000000000000, 117.4749999999999943, 3.602774393244745134E-13 ) ) ;
#84409 = CARTESIAN_POINT ( 'NONE',  ( 97.02380861106273358, -36.97117146848575686, 132.3454236201547758 ) ) ;
#84410 = CARTESIAN_POINT ( 'NONE',  ( 115.6733145644062262, -43.66497474544748059, 43.27467289495795200 ) ) ;
#84411 = CARTESIAN_POINT ( 'NONE',  ( 10.79358099957683237, 68.92650925838135834, 36.56259317987532143 ) ) ;
#84412 = DIRECTION ( 'NONE',  ( 1.000000000000000078E-15, -1.000000000000000083E-30, -1.000000000000000000 ) ) ;
#84413 = CARTESIAN_POINT ( 'NONE',  ( 131.3179999999999836, 53.97500000000000142, 71.43750000000000000 ) ) ;
#84414 = CARTESIAN_POINT ( 'NONE',  ( 101.5072281473882043, -27.97539281467247108, 65.51467289495899138 ) ) ;
#84416 = CARTESIAN_POINT ( 'NONE',  ( 98.87380182923587313, -30.31772012733814492, 151.7984824187679465 ) ) ;
#84415 = CARTESIAN_POINT ( 'NONE',  ( 97.80519586107577368, -40.50152893159460632, 111.6342583986536425 ) ) ;
#84417 = CARTESIAN_POINT ( 'NONE',  ( 113.2454986963039261, -28.75867294333132662, 70.55229194275597138 ) ) ;
#84418 = DIRECTION ( 'NONE',  ( 0.000000000000000000, 0.000000000000000000, -1.000000000000000000 ) ) ;
#84419 = ORIENTED_EDGE ( 'NONE', *, *, #28236, .F. ) ;
#84420 = CARTESIAN_POINT ( 'NONE',  ( 29.56648329127298069, -81.37844715994266664, 342.9256252759109884 ) ) ;
#84421 = VECTOR ( 'NONE', #82755, 1000.000000000000000 ) ;
#84422 = FACE_OUTER_BOUND ( 'NONE', #32966, .T. ) ;
#84423 = PLANE ( 'NONE',  #86242 ) ;
#84424 = ORIENTED_EDGE ( 'NONE', *, *, #62188, .T. ) ;
#84425 = DIRECTION ( 'NONE',  ( -1.000000000000000078E-15, 1.000000000000000000, 0.000000000000000000 ) ) ;
#84427 = ORIENTED_EDGE ( 'NONE', *, *, #45571, .T. ) ;
#84426 = CARTESIAN_POINT ( 'NONE',  ( 101.9504156919933280, -46.58027128656367921, 167.1832443235299763 ) ) ;
#84428 = CARTESIAN_POINT ( 'NONE',  ( 162.5667039024470171, -32.29483332968611364, 193.9678068554150059 ) ) ;
#84429 = CARTESIAN_POINT ( 'NONE',  ( 98.82211989244140682, -29.33244250316893087, 231.7565776568629587 ) ) ;
#84430 = CARTESIAN_POINT ( 'NONE',  ( 109.2641226286370824, -47.00117516105910198, 103.7441967044829880 ) ) ;
#84431 = CARTESIAN_POINT ( 'NONE',  ( 140.0667039024470455, -118.2784471599408960, 51.21780685541800437 ) ) ;
#84432 = EDGE_CURVE ( 'NONE', #2876, #25445, #89013, .T. ) ;
#84433 = DIRECTION ( 'NONE',  ( -3.100000000000000258E-29, 3.100000000000000044E-14, 1.000000000000000000 ) ) ;
#84434 = DIRECTION ( 'NONE',  ( 0.000000000000000000, -1.000000000000000000, 0.000000000000000000 ) ) ;
#84435 = VERTEX_POINT ( 'NONE', #76275 ) ;
#84436 = AXIS2_PLACEMENT_3D ( 'NONE', #65159, #11077, #2942 ) ;
#84437 = ITEM_DEFINED_TRANSFORMATION ( 'NONE', 'NONE', #26088,  #50656 ) ;
#84438 = ADVANCED_FACE ( 'NONE', ( #63086 ), #14510, .F. ) ;
#84439 = VERTEX_POINT ( 'NONE', #56251 ) ;
#84440 = ORIENTED_EDGE ( 'NONE', *, *, #55593, .F. ) ;
#84441 = ORIENTED_EDGE ( 'NONE', *, *, #34464, .F. ) ;
#84442 = CARTESIAN_POINT ( 'NONE',  ( 63.56670390244708813, -40.82844715994014706, 180.4678068554151196 ) ) ;
#84443 = CARTESIAN_POINT ( 'NONE',  ( 96.26801084314395496, -34.37000373589627600, 252.1432443235302969 ) ) ;
#84444 = LINE ( 'NONE', #62175, #83803 ) ;
#84445 = CARTESIAN_POINT ( 'NONE',  ( 134.9467300988947613, -16.12360705087671775, 1.744847597652565030 ) ) ;
#84446 = VECTOR ( 'NONE', #67019, 1000.000000000000000 ) ;
#84448 = DIRECTION ( 'NONE',  ( 0.000000000000000000, 0.000000000000000000, -1.000000000000000000 ) ) ;
#84447 = CARTESIAN_POINT ( 'NONE',  ( 90.44969454456408187, -20.11243780205710507, 239.5838068554175209 ) ) ;
#84449 = LINE ( 'NONE', #14042, #52961 ) ;
#84450 = CARTESIAN_POINT ( 'NONE',  ( 107.6080043092626113, -48.59286871074260006, 42.61276813305398292 ) ) ;
#84451 = ORIENTED_EDGE ( 'NONE', *, *, #9495, .T. ) ;
#84452 = VECTOR ( 'NONE', #16938, 1000.000000000000000 ) ;
#84453 = ORIENTED_EDGE ( 'NONE', *, *, #23863, .T. ) ;
#84455 = EDGE_CURVE ( 'NONE', #59488, #82044, #68573, .T. ) ;
#84454 = AXIS2_PLACEMENT_3D ( 'NONE', #72543, #79371, #45252 ) ;
#84456 = DIRECTION ( 'NONE',  ( -0.000000000000000000, -0.000000000000000000, 1.000000000000000000 ) ) ;
#84457 = CARTESIAN_POINT ( 'NONE',  ( 113.2469266849859650, -28.75976546129976086, 15.55424117046798038 ) ) ;
#84458 = CARTESIAN_POINT ( 'NONE',  ( 97.82556271424805061, -33.52526948863204126, 282.0613395616247772 ) ) ;
#84459 = CIRCLE ( 'NONE', #27820, 2.117000000000007987 ) ;
#84460 = DIRECTION ( 'NONE',  ( -0.9254794337955620787, -0.3787978585227822492, 0.000000000000000000 ) ) ;
#84461 = CARTESIAN_POINT ( 'NONE',  ( 99.34849973496659459, -28.72665311504493246, 111.6870538473389587 ) ) ;
#84462 = DIRECTION ( 'NONE',  ( 1.639958061481212836E-42, -4.100000000000000342E-29, -1.000000000000000000 ) ) ;
#84463 = AXIS2_PLACEMENT_3D ( 'NONE', #41924, #20614, #84198 ) ;
#84464 = CARTESIAN_POINT ( 'NONE',  ( 52.65249034007741358, -48.32844715994062312, 180.4678068554151196 ) ) ;
#84465 = PRODUCT_RELATED_PRODUCT_CATEGORY ( 'part', '', ( #36229 ) ) ;
#84466 = ORIENTED_EDGE ( 'NONE', *, *, #72063, .T. ) ;
#84467 = CARTESIAN_POINT ( 'NONE',  ( 48.16670390244701139, -26.71338133339251542, 313.9678068554150059 ) ) ;
#84468 = CARTESIAN_POINT ( 'NONE',  ( 80.06648329127401098, -33.97944715994105991, 1.625625275910943746 ) ) ;
#84469 = ORIENTED_EDGE ( 'NONE', *, *, #7673, .F. ) ;
#84470 = ORIENTED_EDGE ( 'NONE', *, *, #76617, .T. ) ;
#84471 = CARTESIAN_POINT ( 'NONE',  ( -77.01901799881224520, 91.23868085022589014, 90.13147184857939465 ) ) ;
#84472 = CARTESIAN_POINT ( 'NONE',  ( 106.8709381294020488, -45.58890767966684621, 268.9901547344683763 ) ) ;
#84473 = DIRECTION ( 'NONE',  ( 0.000000000000000000, 1.000000000000000000, 0.000000000000000000 ) ) ;
#84474 =( BOUNDED_CURVE ( )  B_SPLINE_CURVE ( 3, ( #52029, #38866, #4361, #72941 ),
 .UNSPECIFIED., .F., .T. ) 
 B_SPLINE_CURVE_WITH_KNOTS ( ( 4, 4 ),
 ( -3.022471162239526166E-12, 1.570796326791795705 ),
 .UNSPECIFIED. ) 
 CURVE ( )  GEOMETRIC_REPRESENTATION_ITEM ( )  RATIONAL_B_SPLINE_CURVE ( ( 1.000000000000000000, 0.8047378541243834782, 0.8047378541243834782, 1.000000000000000000 ) ) 
 REPRESENTATION_ITEM ( '' )  );
#84475 = LINE ( 'NONE', #68588, #27607 ) ;
#84476 = DIRECTION ( 'NONE',  ( -0.7071067811865513475, -0.7071067811865436870, -7.071067811865520693E-16 ) ) ;
#84477 = ADVANCED_FACE ( 'NONE', ( #26771 ), #42185, .T. ) ;
#84478 = CARTESIAN_POINT ( 'NONE',  ( 86.12934247706293434, 70.27763793881260312, -81.47036787067791863 ) ) ;
#84479 = ORIENTED_EDGE ( 'NONE', *, *, #56218, .T. ) ;
#84480 = CARTESIAN_POINT ( 'NONE',  ( -71.77848634863190114, 120.6499999999999915, 77.39114642429879609 ) ) ;
#84481 = DIRECTION ( 'NONE',  ( -0.000000000000000000, 1.000000000000000000, 0.000000000000000000 ) ) ;
#84482 = ADVANCED_FACE ( 'NONE', ( #69467 ), #77733, .T. ) ;
#84483 = ORIENTED_EDGE ( 'NONE', *, *, #82743, .F. ) ;
#84484 = CARTESIAN_POINT ( 'NONE',  ( 101.1408812403245747, -27.39851324166288649, 65.51467289495799662 ) ) ;
#84485 = ORIENTED_EDGE ( 'NONE', *, *, #44068, .T. ) ;
#84486 = ADVANCED_FACE ( 'NONE', ( #82218 ), #77626, .T. ) ;
#84487 = CARTESIAN_POINT ( 'NONE',  ( 110.1408960893143956, -44.29103306967431308, 280.7023760838771409 ) ) ;
#84488 = LINE ( 'NONE', #62667, #11229 ) ;
#84489 = CARTESIAN_POINT ( 'NONE',  ( 102.2868918306627961, -45.93239726994513461, 167.1832443235309995 ) ) ;
#84490 = CARTESIAN_POINT ( 'NONE',  ( 23.49602674866495988, 79.64193718108693076, 299.1106646571903411 ) ) ;
#84491 = ADVANCED_FACE ( 'NONE', ( #65335 ), #15411, .F. ) ;
#84492 = FACE_OUTER_BOUND ( 'NONE', #64034, .T. ) ;
#84493 = DIRECTION ( 'NONE',  ( 0.000000000000000000, 0.000000000000000000, -1.000000000000000000 ) ) ;
#84494 = VECTOR ( 'NONE', #7563, 1000.000000000000000 ) ;
#84495 = LINE ( 'NONE', #49925, #85709 ) ;
#84496 = CARTESIAN_POINT ( 'NONE',  ( 106.8354761508916226, -47.19556465630029862, 268.5584824187679374 ) ) ;
#84497 = CARTESIAN_POINT ( 'NONE',  ( 74.36911441044796334, 82.54999999999999716, -92.32962665258483526 ) ) ;
#84498 = EDGE_LOOP ( 'NONE', ( #18531, #59321, #81035, #26010 ) ) ;
#84499 = VECTOR ( 'NONE', #19778, 1000.000000000000000 ) ;
#84500 = CARTESIAN_POINT ( 'NONE',  ( 136.8164763767841521, -36.77596264856137509, 6.749779334551647914 ) ) ;
#84501 = VERTEX_POINT ( 'NONE', #51684 ) ;
#84502 = CARTESIAN_POINT ( 'NONE',  ( 97.89440201276070752, -31.60978508062128967, 106.9213395616259703 ) ) ;
#84503 = CARTESIAN_POINT ( 'NONE',  ( 141.0667039024479834, -48.82844715994099971, 205.9178068554149945 ) ) ;
#84504 = EDGE_LOOP ( 'NONE', ( #46674, #13866, #85133, #75506 ) ) ;
#84505 = ORIENTED_EDGE ( 'NONE', *, *, #69567, .T. ) ;
#84506 = ORIENTED_EDGE ( 'NONE', *, *, #65709, .F. ) ;
#84507 = EDGE_CURVE ( 'NONE', #78550, #51823, #57617, .T. ) ;
#84508 = CARTESIAN_POINT ( 'NONE',  ( 113.1782937098645192, -44.75186864062681025, 123.0939586030858379 ) ) ;
#84509 = LINE ( 'NONE', #22267, #34699 ) ;
#84511 = EDGE_CURVE ( 'NONE', #38582, #8395, #50144, .T. ) ;
#84510 = DIRECTION ( 'NONE',  ( 0.000000000000000000, 0.000000000000000000, 1.000000000000000000 ) ) ;
#84512 = LINE ( 'NONE', #15001, #37913 ) ;
#84513 = LINE ( 'NONE', #22270, #67879 ) ;
#84514 = CARTESIAN_POINT ( 'NONE',  ( 118.0755232325510917, -37.71687819837586630, 29.74324432352998215 ) ) ;
#84515 = VECTOR ( 'NONE', #58739, 1000.000000000000000 ) ;
#84516 = DIRECTION ( 'NONE',  ( -2.999999999999999839E-15, 1.000000000000000000, -2.999999999999999900E-30 ) ) ;
#84517 = ORIENTED_EDGE ( 'NONE', *, *, #85700, .T. ) ;
#84518 = CARTESIAN_POINT ( 'NONE',  ( 107.0667039024470313, -104.2784471599418197, -11.78219314458200984 ) ) ;
#84519 = FACE_OUTER_BOUND ( 'NONE', #46700, .T. ) ;
#84520 = ORIENTED_EDGE ( 'NONE', *, *, #4086, .F. ) ;
#84521 = ORIENTED_EDGE ( 'NONE', *, *, #3964, .F. ) ;
#84522 = VECTOR ( 'NONE', #51951, 1000.000000000000000 ) ;
#84523 = LINE ( 'NONE', #21835, #72078 ) ;
#84524 = DIRECTION ( 'NONE',  ( -3.576143065239989638E-15, 0.000000000000000000, 1.000000000000000000 ) ) ;
#84525 = DIRECTION ( 'NONE',  ( 1.000000000000000078E-15, 1.000000000000000083E-30, -1.000000000000000000 ) ) ;
#84526 = FACE_OUTER_BOUND ( 'NONE', #2711, .T. ) ;
#84527 = CARTESIAN_POINT ( 'NONE',  ( 113.2432932581317289, -30.83002766685618923, 233.8552769709339429 ) ) ;
#84529 = DIRECTION ( 'NONE',  ( 0.000000000000000000, 1.000000000000000000, 0.000000000000000000 ) ) ;
#84528 = AXIS2_PLACEMENT_3D ( 'NONE', #17591, #38911, #10758 ) ;
#84530 = CARTESIAN_POINT ( 'NONE',  ( 124.4845670069425836, 71.14632460481045939, 39.35078757465099386 ) ) ;
#84531 = CARTESIAN_POINT ( 'NONE',  ( 107.2329094490511068, -25.63056496568808029, 80.07657765686299456 ) ) ;
#84532 = ORIENTED_EDGE ( 'NONE', *, *, #25582, .T. ) ;
#84533 = CARTESIAN_POINT ( 'NONE',  ( 131.4308125312103641, -19.51428458726955739, 6.911392308671674201 ) ) ;
#84534 = ORIENTED_EDGE ( 'NONE', *, *, #67949, .T. ) ;
#84535 = CARTESIAN_POINT ( 'NONE',  ( 111.0682029062220266, -27.51397330308390465, 275.7507068285485730 ) ) ;
#84536 = ORIENTED_EDGE ( 'NONE', *, *, #82410, .T. ) ;
#84537 = CARTESIAN_POINT ( 'NONE',  ( 80.06648329127398256, -8.729447159941058132, 4.925625275910944012 ) ) ;
#84538 = ORIENTED_EDGE ( 'NONE', *, *, #72286, .T. ) ;
#84539 = DIRECTION ( 'NONE',  ( -0.7071067811865774377, 0.7071067811865175967, -7.071067811865470403E-16 ) ) ;
#84540 = CARTESIAN_POINT ( 'NONE',  ( 117.0714725379134364, -35.45898311558699589, 274.9271173339710117 ) ) ;
#84541 = ADVANCED_FACE ( 'NONE', ( #79431 ), #78087, .T. ) ;
#84542 = CARTESIAN_POINT ( 'NONE',  ( 57.56670390244832447, -48.82844715994039575, 259.7178068554150627 ) ) ;
#84543 = ORIENTED_EDGE ( 'NONE', *, *, #64093, .F. ) ;
#84544 = CARTESIAN_POINT ( 'NONE',  ( 101.7446525173404979, -27.01484174591878329, 100.4632443235299633 ) ) ;
#84545 =( NAMED_UNIT ( * ) PLANE_ANGLE_UNIT ( ) SI_UNIT ( $, .RADIAN. ) );
#84548 = EDGE_CURVE ( 'NONE', #5714, #70652, #23130, .T. ) ;
#84547 = CARTESIAN_POINT ( 'NONE',  ( 91.13743891206681269, 69.93117631934792655, -93.48535127324109339 ) ) ;
#84546 = CARTESIAN_POINT ( 'NONE',  ( 97.33772238324482373, -34.07151022348116243, 166.1148286285612414 ) ) ;
#84549 = DIRECTION ( 'NONE',  ( -0.0001713722456143218888, 0.9999999853157766072, 0.000000000000000000 ) ) ;
#84550 = CARTESIAN_POINT ( 'NONE',  ( 117.0608945229600408, -38.08045312664489757, 143.7189586087818896 ) ) ;
#84551 = EDGE_LOOP ( 'NONE', ( #68195, #82416 ) ) ;
#84552 = VECTOR ( 'NONE', #66650, 1000.000000000000000 ) ;
#84553 = CARTESIAN_POINT ( 'NONE',  ( 36.23715912545429063, -47.82818131006125384, 249.9678068554150343 ) ) ;
#84554 = CARTESIAN_POINT ( 'NONE',  ( 98.34985896237778036, -31.65658472535170276, 155.9064586015307157 ) ) ;
#84555 = DIRECTION ( 'NONE',  ( 0.000000000000000000, -1.000000000000000000, 0.000000000000000000 ) ) ;
#84556 = CARTESIAN_POINT ( 'NONE',  ( 97.59729452806701033, -30.98317272244041121, 121.8803871806729546 ) ) ;
#84558 = CARTESIAN_POINT ( 'NONE',  ( 177.3246001664175537, -48.34074026909178912, 129.9678068554150059 ) ) ;
#84557 = DIRECTION ( 'NONE',  ( 0.000000000000000000, 0.000000000000000000, -1.000000000000000000 ) ) ;
#84559 = CYLINDRICAL_SURFACE ( 'NONE', #20471, 23.50000000000000711 ) ;
#84560 = AXIS2_PLACEMENT_3D ( 'NONE', #41325, #69054, #20464 ) ;
#84561 = ORIENTED_EDGE ( 'NONE', *, *, #61559, .F. ) ;
#84562 = EDGE_CURVE ( 'NONE', #15841, #23774, #55901, .T. ) ;
#84563 = CARTESIAN_POINT ( 'NONE',  ( 50.87649884952499946, -33.54226604284930602, -5.074374724088000832 ) ) ;
#84564 = CARTESIAN_POINT ( 'NONE',  ( 114.0663967180212950, -29.08153105160607410, 150.4746728949579619 ) ) ;
#84566 = EDGE_LOOP ( 'NONE', ( #46180, #40025, #58320, #78164 ) ) ;
#84565 = CARTESIAN_POINT ( 'NONE',  ( 164.0167039024470057, -75.72844715994088460, 222.2178068554179902 ) ) ;
#84567 = CARTESIAN_POINT ( 'NONE',  ( 113.7419942178972576, -29.10023054337259296, 285.5032443235299979 ) ) ;
#84568 = DIRECTION ( 'NONE',  ( -0.7071067811865774377, 0.7071067811865175967, -7.071067811865782003E-16 ) ) ;
#84569 = DIRECTION ( 'NONE',  ( 0.000000000000000000, 0.000000000000000000, -1.000000000000000000 ) ) ;
#84570 = DIRECTION ( 'NONE',  ( 0.000000000000000000, 0.000000000000000000, 1.000000000000000000 ) ) ;
#84571 = DIRECTION ( 'NONE',  ( 9.351236661543306751E-17, -3.725950533538267725E-29, -1.000000000000000000 ) ) ;
#84572 = ADVANCED_FACE ( 'NONE', ( #50804 ), #78978, .T. ) ;
#84573 = CARTESIAN_POINT ( 'NONE',  ( 51.03742451361402743, -23.42844715994066362, 313.9678068554150059 ) ) ;
#84574 = CARTESIAN_POINT ( 'NONE',  ( 105.2318265017783716, -27.12228994480470945, 235.2270538473399313 ) ) ;
#84575 = ORIENTED_EDGE ( 'NONE', *, *, #76501, .F. ) ;
#84576 = ORIENTED_EDGE ( 'NONE', *, *, #67396, .F. ) ;
#84577 = CARTESIAN_POINT ( 'NONE',  ( 108.4114243528872095, -27.43637152299345061, 146.4053928297069547 ) ) ;
#84578 = AXIS2_PLACEMENT_3D ( 'NONE', #79389, #85319, #2633 ) ;
#84579 = DIRECTION ( 'NONE',  ( 1.000000000000000000, 0.000000000000000000, 0.000000000000000000 ) ) ;
#84580 = CARTESIAN_POINT ( 'NONE',  ( 104.6647032408819200, -45.25937870008434771, 18.79015473446898810 ) ) ;
#84581 = CARTESIAN_POINT ( 'NONE',  ( 23.75871628398702384, 82.86657936785965717, 298.1325000000000500 ) ) ;
#84582 = EDGE_CURVE ( 'NONE', #86385, #47600, #72606, .T. ) ;
#84583 = DIRECTION ( 'NONE',  ( 3.999999999999999995E-14, -1.000000000000000000, 4.100000000000000342E-29 ) ) ;
#84584 = DIRECTION ( 'NONE',  ( 0.000000000000000000, 0.000000000000000000, 1.000000000000000000 ) ) ;
#84585 = CARTESIAN_POINT ( 'NONE',  ( 194.0371591254573502, -24.42818131005417825, 236.4678068554149775 ) ) ;
#84586 = CARTESIAN_POINT ( 'NONE',  ( 97.75833061367904975, -40.38474740428294751, 37.62395470578984913 ) ) ;
#84587 = CARTESIAN_POINT ( 'NONE',  ( 110.2492204789523242, -26.78788743924345184, 234.8299109901969643 ) ) ;
#84588 = CARTESIAN_POINT ( 'NONE',  ( 10.91422574807192625, 88.85956302702116716, 117.8518595483441800 ) ) ;
#84589 = VERTEX_POINT ( 'NONE', #78542 ) ;
#84591 = ORIENTED_EDGE ( 'NONE', *, *, #58355, .T. ) ;
#84590 = EDGE_CURVE ( 'NONE', #43506, #44014, #71272, .T. ) ;
#84592 = DIRECTION ( 'NONE',  ( 0.000000000000000000, 0.000000000000000000, 1.000000000000000000 ) ) ;
#84593 = CARTESIAN_POINT ( 'NONE',  ( -90.65736737572414938, 90.28416741362501341, -76.39920031718057203 ) ) ;
#84594 = CYLINDRICAL_SURFACE ( 'NONE', #62099, 9.999999999999998224 ) ;
#84595 = DIRECTION ( 'NONE',  ( 0.000000000000000000, 0.000000000000000000, -1.000000000000000000 ) ) ;
#84596 = CARTESIAN_POINT ( 'NONE',  ( 114.9268010244024225, -42.60560063232393446, 24.31562527591096767 ) ) ;
#84597 = CARTESIAN_POINT ( 'NONE',  ( 9.720633968232110273E-16, 127.0000000000000000, -111.1250000000000000 ) ) ;
#84598 = VERTEX_POINT ( 'NONE', #16742 ) ;
#84599 = CARTESIAN_POINT ( 'NONE',  ( 96.64260770218685082, -42.46999856532355011, 22.72705384733997391 ) ) ;
#84600 = CARTESIAN_POINT ( 'NONE',  ( 0.000000000000000000, 211.0000000000000000, 154.6557476874258441 ) ) ;
#84601 = AXIS2_PLACEMENT_3D ( 'NONE', #31342, #65855, #51770 ) ;
#84602 = CARTESIAN_POINT ( 'NONE',  ( 112.6638099339533028, -45.52472799210174514, 263.0270538473394595 ) ) ;
#84603 = ORIENTED_EDGE ( 'NONE', *, *, #82656, .T. ) ;
#84604 = EDGE_CURVE ( 'NONE', #88157, #68103, #43077, .T. ) ;
#84605 = AXIS2_PLACEMENT_3D ( 'NONE', #2101, #44754, #58390 ) ;
#84606 = CARTESIAN_POINT ( 'NONE',  ( 77.97204591016883057, -38.52018918693340055, 7.480061334638488546 ) ) ;
#84608 = ADVANCED_FACE ( 'NONE', ( #70816 ), #1778, .T. ) ;
#84607 = DIRECTION ( 'NONE',  ( -4.237773401492740281E-14, 1.000000000000000000, 0.000000000000000000 ) ) ;
#84609 = DIRECTION ( 'NONE',  ( 3.999999999999999995E-14, -1.000000000000000000, 4.100000000000000342E-29 ) ) ;
#84610 = EDGE_CURVE ( 'NONE', #48706, #29859, #12492, .T. ) ;
#84611 = CARTESIAN_POINT ( 'NONE',  ( 113.0992926495536182, -42.93477843977468922, 116.0204713219719679 ) ) ;
#84612 = CARTESIAN_POINT ( 'NONE',  ( 106.9748050991984059, -47.17592283179411083, 183.5699109901969734 ) ) ;
#84613 = DIRECTION ( 'NONE',  ( -1.000000000000000000, 0.000000000000000000, 0.000000000000000000 ) ) ;
#84614 = EDGE_LOOP ( 'NONE', ( #6715, #45135, #25785, #21694 ) ) ;
#84615 = EDGE_CURVE ( 'NONE', #51989, #25435, #16298, .T. ) ;
#84616 = DIRECTION ( 'NONE',  ( 1.000000000000000078E-15, -1.000000000000000083E-30, -1.000000000000000000 ) ) ;
#84617 = EDGE_LOOP ( 'NONE', ( #9679, #59546, #61515, #74536 ) ) ;
#84618 = ORIENTED_EDGE ( 'NONE', *, *, #18183, .F. ) ;
#84619 = AXIS2_PLACEMENT_3D ( 'NONE', #55127, #69242, #635 ) ;
#84620 = CARTESIAN_POINT ( 'NONE',  ( 140.9629299006807059, -46.47944715994099596, 14.92562527591100618 ) ) ;
#84621 = ORIENTED_EDGE ( 'NONE', *, *, #43528, .F. ) ;
#84622 = VERTEX_POINT ( 'NONE', #71710 ) ;
#84623 = CARTESIAN_POINT ( 'NONE',  ( 117.0715500276773184, -35.45963891618318797, 169.9274906265435732 ) ) ;
#84624 = CARTESIAN_POINT ( 'NONE',  ( 103.2832018370665565, -27.47273118576459794, 41.38522229241210226 ) ) ;
#84625 = CARTESIAN_POINT ( 'NONE',  ( 115.5717340297064197, -37.51483979961712123, 78.17527697093396455 ) ) ;
#84626 = CARTESIAN_POINT ( 'NONE',  ( 117.5411534933602837, -36.54545762053501079, 288.8413395616251478 ) ) ;
#84627 = CARTESIAN_POINT ( 'NONE',  ( -6.364581335559162056, 71.52860519235655090, 130.4026037055029690 ) ) ;
#84628 = DIRECTION ( 'NONE',  ( 0.000000000000000000, 0.000000000000000000, 1.000000000000000000 ) ) ;
#84629 = ORIENTED_EDGE ( 'NONE', *, *, #79687, .F. ) ;
#84630 = ORIENTED_EDGE ( 'NONE', *, *, #41118, .F. ) ;
#84631 = DIRECTION ( 'NONE',  ( 0.000000000000000000, 0.000000000000000000, 1.000000000000000000 ) ) ;
#84632 = LINE ( 'NONE', #22392, #24583 ) ;
#84633 = DIRECTION ( 'NONE',  ( 0.000000000000000000, 0.000000000000000000, 1.000000000000000000 ) ) ;
#84634 = CARTESIAN_POINT ( 'NONE',  ( 99.54941199951403519, -42.98700854487248080, 116.8784824187689679 ) ) ;
#84635 = VECTOR ( 'NONE', #53862, 1000.000000000000000 ) ;
#84636 = CARTESIAN_POINT ( 'NONE',  ( 101.4772741282170472, -27.87691040622789274, 110.5241967044819944 ) ) ;
#84637 = DIRECTION ( 'NONE',  ( 0.000000000000000000, -1.000000000000000000, 0.000000000000000000 ) ) ;
#84638 = ORIENTED_EDGE ( 'NONE', *, *, #43205, .T. ) ;
#84639 = CARTESIAN_POINT ( 'NONE',  ( 100.2480723708022197, -28.84298388537911606, 260.6441967044822263 ) ) ;
#84640 = FACE_OUTER_BOUND ( 'NONE', #18215, .T. ) ;
#84641 = AXIS2_PLACEMENT_3D ( 'NONE', #83267, #13767, #14220 ) ;
#84642 = CARTESIAN_POINT ( 'NONE',  ( 97.84512178009099159, -40.59816388786018138, 27.64300878097207814 ) ) ;
#84644 = DIRECTION ( 'NONE',  ( -4.237773401492740281E-14, 1.000000000000000000, 0.000000000000000000 ) ) ;
#84643 = DIRECTION ( 'NONE',  ( 1.000000000000000000, 1.000000000000000078E-15, 0.000000000000000000 ) ) ;
#84645 = CARTESIAN_POINT ( 'NONE',  ( 105.1754357245111180, -25.42735205269929821, 322.5490683446364528 ) ) ;
#84646 = FACE_OUTER_BOUND ( 'NONE', #43634, .T. ) ;
#84647 = DIRECTION ( 'NONE',  ( 0.7071067811861589947, -0.7071067811869361508, 0.000000000000000000 ) ) ;
#84648 = LINE ( 'NONE', #63744, #50103 ) ;
#84649 = DIRECTION ( 'NONE',  ( 0.000000000000000000, 0.000000000000000000, 1.000000000000000000 ) ) ;
#84650 = CARTESIAN_POINT ( 'NONE',  ( 100.3567573962561710, -39.47573163423117393, -2.114374724089040924 ) ) ;
#84652 = ORIENTED_EDGE ( 'NONE', *, *, #36573, .T. ) ;
#84651 = CARTESIAN_POINT ( 'NONE',  ( 37.36643805256573359, -48.62818131006097389, 129.9678068554150911 ) ) ;
#84653 = CARTESIAN_POINT ( 'NONE',  ( -47.02966122971772478, 65.60000000000000853, -8.565507749926083175E-15 ) ) ;
#84654 = CARTESIAN_POINT ( 'NONE',  ( 103.9326413674837539, -26.76323430032771000, 250.3184824187677577 ) ) ;
#84655 = CARTESIAN_POINT ( 'NONE',  ( 97.42522746746806206, -42.13501527293522742, 177.7451490854349743 ) ) ;
#84656 = CARTESIAN_POINT ( 'NONE',  ( 115.4621199703947241, -43.00579008905405232, 24.31562527591096767 ) ) ;
#84658 = CARTESIAN_POINT ( 'NONE',  ( 82.81648124396181743, -36.63640413216758418, 6.749771997051381867 ) ) ;
#84657 = FACE_OUTER_BOUND ( 'NONE', #71539, .T. ) ;
#84659 = CARTESIAN_POINT ( 'NONE',  ( 107.0667039024470313, -104.2784471599413934, 2.217806855418003043 ) ) ;
#84660 = EDGE_CURVE ( 'NONE', #18083, #81364, #28436, .T. ) ;
#84661 = VECTOR ( 'NONE', #88456, 1000.000000000000000 ) ;
#84662 = ORIENTED_EDGE ( 'NONE', *, *, #76357, .T. ) ;
#84663 = EDGE_CURVE ( 'NONE', #11696, #55509, #30812, .T. ) ;
#84664 = DIRECTION ( 'NONE',  ( 9.351236661543306751E-17, -3.725950533538267725E-29, -1.000000000000000000 ) ) ;
#84665 = VERTEX_POINT ( 'NONE', #23574 ) ;
#84666 = CARTESIAN_POINT ( 'NONE',  ( 99.85230398470191915, -41.30238370604462261, 186.1981341137909567 ) ) ;
#84667 = EDGE_CURVE ( 'NONE', #36009, #1539, #58808, .T. ) ;
#84669 = ORIENTED_EDGE ( 'NONE', *, *, #23869, .T. ) ;
#84668 = CARTESIAN_POINT ( 'NONE',  ( 108.3302456646921144, -46.73522246767858945, 187.6775912052179081 ) ) ;
#84670 = VECTOR ( 'NONE', #5796, 1000.000000000000000 ) ;
#84671 = DIRECTION ( 'NONE',  ( -1.000000000000000000, 0.000000000000000000, 0.000000000000000000 ) ) ;
#84672 = CARTESIAN_POINT ( 'NONE',  ( 113.0129699484215564, -46.01939436189636012, 214.0175300378159591 ) ) ;
#84673 = CARTESIAN_POINT ( 'NONE',  ( 194.5667039024482108, -40.82844715993405060, 180.4678068554150343 ) ) ;
#84674 = DIRECTION ( 'NONE',  ( 0.000000000000000000, -1.000000000000000000, 0.000000000000000000 ) ) ;
#84675 = CARTESIAN_POINT ( 'NONE',  ( 124.0667039024470313, -104.2784471599414360, 0.2178068554180012661 ) ) ;
#84676 = EDGE_CURVE ( 'NONE', #79139, #81090, #11196, .T. ) ;
#84677 = ADVANCED_FACE ( 'NONE', ( #88474 ), #66664, .T. ) ;
#84678 = CARTESIAN_POINT ( 'NONE',  ( 145.7671917778935438, -138.5331951669010948, 246.9855771338589818 ) ) ;
#84679 = CARTESIAN_POINT ( 'NONE',  ( 97.81168883536605563, -40.51740680051663190, 96.63562987897269352 ) ) ;
#84680 = CARTESIAN_POINT ( 'NONE',  ( 102.0112516875887252, -27.67497761899947406, 105.4937205140069665 ) ) ;
#84681 = VERTEX_POINT ( 'NONE', #25780 ) ;
#84682 = ORIENTED_EDGE ( 'NONE', *, *, #67522, .T. ) ;
#84683 = ADVANCED_FACE ( 'NONE', ( #73479 ), #11253, .F. ) ;
#84684 = AXIS2_PLACEMENT_3D ( 'NONE', #44684, #3370, #71532 ) ;
#84685 = CARTESIAN_POINT ( 'NONE',  ( 98.21780894689015895, -37.20823830323941905, 72.80158330589698323 ) ) ;
#84686 = EDGE_CURVE ( 'NONE', #83131, #54506, #74862, .T. ) ;
#84687 = CARTESIAN_POINT ( 'NONE',  ( 129.5675368918761876, -88.37796714256971597, 250.2178068554179902 ) ) ;
#84689 = CARTESIAN_POINT ( 'NONE',  ( 116.8171228645041140, -34.15291831569319214, 39.03145860967040193 ) ) ;
#84688 = CARTESIAN_POINT ( 'NONE',  ( 100.4443968677459935, -27.79860430499269697, 181.5841967044819683 ) ) ;
#84690 = DIRECTION ( 'NONE',  ( -1.000000000000000078E-15, 1.000000000000000000, 0.000000000000000000 ) ) ;
#84691 = ADVANCED_FACE ( 'NONE', ( #318 ), #68014, .F. ) ;
#84692 = DIRECTION ( 'NONE',  ( 0.000000000000000000, -0.000000000000000000, 1.000000000000000000 ) ) ;
#84693 = DIRECTION ( 'NONE',  ( -0.7071067811865779928, 0.7071067811865171526, -7.071067811865475333E-16 ) ) ;
#84694 = DIRECTION ( 'NONE',  ( 0.9825752044328148749, 0.1858654557302456822, 0.000000000000000000 ) ) ;
#84695 = CARTESIAN_POINT ( 'NONE',  ( 179.8585841295805778, -30.08671355699668837, 237.4678068554150059 ) ) ;
#84696 = ADVANCED_FACE ( 'NONE', ( #13060 ), #20329, .T. ) ;
#84697 = CARTESIAN_POINT ( 'NONE',  ( 116.9011659702704264, -33.23038410113876040, 114.0984824187679720 ) ) ;
#84698 = ORIENTED_EDGE ( 'NONE', *, *, #24812, .F. ) ;
#84699 = VERTEX_POINT ( 'NONE', #21217 ) ;
#84701 = VERTEX_POINT ( 'NONE', #76172 ) ;
#84700 = EDGE_CURVE ( 'NONE', #14757, #28401, #18312, .T. ) ;
#84702 = CARTESIAN_POINT ( 'NONE',  ( 11.02410282832817856, 76.19023921641802133, 130.0905510769329965 ) ) ;
#84703 = CARTESIAN_POINT ( 'NONE',  ( -100.0339087179664830, 88.18319050751490806, -83.89391322244402716 ) ) ;
#84704 = CARTESIAN_POINT ( 'NONE',  ( 109.6430121197684571, -46.48008673816740099, 78.78145860836009717 ) ) ;
#84705 = DIRECTION ( 'NONE',  ( 0.7071067811865490160, 0.000000000000000000, -0.7071067811865461294 ) ) ;
#84706 = CARTESIAN_POINT ( 'NONE',  ( 98.93571844094823575, -36.00806725600566693, 229.0738046553059633 ) ) ;
#84707 = AXIS2_PLACEMENT_3D ( 'NONE', #57355, #24194, #51425 ) ;
#84708 = CARTESIAN_POINT ( 'NONE',  ( 69.25310000000000343, 82.54999999999999716, 344.4418053999999643 ) ) ;
#84709 = CARTESIAN_POINT ( 'NONE',  ( 113.8435853237685933, -28.76095960330615142, 139.5156252759109634 ) ) ;
#84710 = B_SPLINE_CURVE_WITH_KNOTS ( 'NONE', 3,
 ( #52496, #74768, #18450, #67952, #61132, #12097, #46138, #5282, #60673, #88412, #19361, #12547, #40233, #62922, #42466, #63379, #49288, #55634, #13442, #68852, #76565, #14346, #84298, #68409, #22068, #83382, #20707, #42025, #28866, #35666, #48828, #7076, #6623, #75673, #35211, #69753, #34319, #62025, #27510, #89759, #55186, #28402, #49738, #41570, #83838, #253, #82947, #77461 ),
 .UNSPECIFIED., .F., .F.,
 ( 4, 2, 2, 2, 2, 2, 2, 2, 2, 1, 2, 2, 2, 2, 2, 2, 2, 2, 2, 2, 2, 1, 2, 2, 4 ),
 ( 0.05959919981814688905, 0.06208168506169057382, 0.06332292768346242662, 0.06456417030523425860, 0.06704665554877799194, 0.06828789817054985167, 0.06952914079232172528, 0.07201162603586544475, 0.07325286865763730448, 0.07449411127940915034, 0.07573535390118101007, 0.07697659652295286981, 0.07945908176649658927, 0.08194156701004030874, 0.08318280963181216847, 0.08442405225358402820, 0.08690653749712774767, 0.08814778011889960740, 0.08938902274067146714, 0.09187150798421522824, 0.09311275060598708797, 0.09435399322775894770, 0.09559523584953080744, 0.09683647847130266717, 0.09931896371484640051 ),
 .UNSPECIFIED. ) ;
#84711 = DIRECTION ( 'NONE',  ( 0.000000000000000000, 1.000000000000000000, 0.000000000000000000 ) ) ;
#84712 = ORIENTED_EDGE ( 'NONE', *, *, #82525, .F. ) ;
#84714 = EDGE_LOOP ( 'NONE', ( #37510, #5213, #15767, #756, #38176 ) ) ;
#84713 = ORIENTED_EDGE ( 'NONE', *, *, #82758, .T. ) ;
#84715 = EDGE_CURVE ( 'NONE', #45258, #4000, #37133, .T. ) ;
#84716 = DIRECTION ( 'NONE',  ( 0.000000000000000000, 1.000000000000000000, 0.000000000000000000 ) ) ;
#84717 = ORIENTED_EDGE ( 'NONE', *, *, #87034, .T. ) ;
#84718 = ORIENTED_EDGE ( 'NONE', *, *, #36957, .T. ) ;
#84720 = EDGE_CURVE ( 'NONE', #88514, #59215, #75730, .T. ) ;
#84719 = DIRECTION ( 'NONE',  ( -0.9999999853157766072, -0.0001713722456150811827, 0.000000000000000000 ) ) ;
#84721 = DIRECTION ( 'NONE',  ( -1.000000000000000078E-15, 1.000000000000000083E-30, 1.000000000000000000 ) ) ;
#84722 = EDGE_CURVE ( 'NONE', #47173, #79701, #50215, .T. ) ;
#84723 = CARTESIAN_POINT ( 'NONE',  ( 104.4082965424966147, -28.27590814835049926, 246.7501547344679693 ) ) ;
#84724 = DIRECTION ( 'NONE',  ( 1.000000000000000000, 3.552853285012605541E-15, 0.000000000000000000 ) ) ;
#84725 = EDGE_LOOP ( 'NONE', ( #43100, #22753, #27609, #43778 ) ) ;
#84726 = EDGE_CURVE ( 'NONE', #38527, #15084, #3799, .T. ) ;
#84727 = CARTESIAN_POINT ( 'NONE',  ( 113.6715427071513318, -42.59351399727410126, 9.635625275910943088 ) ) ;
#84728 = CARTESIAN_POINT ( 'NONE',  ( -126.1761431753821370, 65.30360745155232394, 33.53545494772723146 ) ) ;
#84729 = EDGE_LOOP ( 'NONE', ( #8495, #63515, #74075, #25288 ) ) ;
#84730 = EDGE_LOOP ( 'NONE', ( #29304, #13927, #70365, #35432, #15672 ) ) ;
#84731 = CIRCLE ( 'NONE', #76006, 7.143750000000001599 ) ;
#84732 = CARTESIAN_POINT ( 'NONE',  ( 152.0368932755772562, -23.42844715993587812, 193.9678068554149775 ) ) ;
#84733 = AXIS2_PLACEMENT_3D ( 'NONE', #21250, #69402, #68950 ) ;
#84734 = ORIENTED_EDGE ( 'NONE', *, *, #45147, .T. ) ;
#84735 = ORIENTED_EDGE ( 'NONE', *, *, #40174, .T. ) ;
#84736 = AXIS2_PLACEMENT_3D ( 'NONE', #53406, #73882, #80275 ) ;
#84737 = CARTESIAN_POINT ( 'NONE',  ( 98.59685088459899305, -34.95005064942726136, 258.9918998934010119 ) ) ;
#84738 = CARTESIAN_POINT ( 'NONE',  ( 113.5789493677227711, -44.94383383376451491, 168.1099109901969939 ) ) ;
#84739 = CARTESIAN_POINT ( 'NONE',  ( 117.6568287320716877, -39.81301747186228113, 138.5889586092439743 ) ) ;
#84740 = CARTESIAN_POINT ( 'NONE',  ( 116.3916404119186154, -39.77162857537385321, 249.5838068554167819 ) ) ;
#84741 = CARTESIAN_POINT ( 'NONE',  ( 107.2431676328701684, -47.18842012194354396, 208.5899109901969837 ) ) ;
#84742 = DIRECTION ( 'NONE',  ( 0.000000000000000000, 0.000000000000000000, 1.000000000000000000 ) ) ;
#84743 = FACE_OUTER_BOUND ( 'NONE', #75398, .T. ) ;
#84744 = VERTEX_POINT ( 'NONE', #61191 ) ;
#84745 = CARTESIAN_POINT ( 'NONE',  ( 30.00000000000001776, 127.0000000000000000, 114.8826257785461280 ) ) ;
#84746 = ORIENTED_EDGE ( 'NONE', *, *, #19132, .T. ) ;
#84747 = ORIENTED_EDGE ( 'NONE', *, *, #74422, .F. ) ;
#84748 = CARTESIAN_POINT ( 'NONE',  ( 117.9786848761844453, -34.69554937534774552, 203.9851490854349549 ) ) ;
#84749 = ORIENTED_EDGE ( 'NONE', *, *, #47846, .F. ) ;
#84750 = CARTESIAN_POINT ( 'NONE',  ( 109.5085389712880612, -46.86470218963918200, 132.7641967044819751 ) ) ;
#84751 = DIRECTION ( 'NONE',  ( 0.000000000000000000, 0.000000000000000000, 1.000000000000000000 ) ) ;
#84752 = DIRECTION ( 'NONE',  ( 0.000000000000000000, -1.000000000000000000, 0.000000000000000000 ) ) ;
#84753 = DIRECTION ( 'NONE',  ( 1.000000000000000000, 0.000000000000000000, 0.000000000000000000 ) ) ;
#84756 = CARTESIAN_POINT ( 'NONE',  ( 96.83034234600431489, -40.83861266248838007, 247.6422919425769749 ) ) ;
#84755 = CARTESIAN_POINT ( 'NONE',  ( 109.3947377649931383, -46.48697826211399331, 57.76270257490259041 ) ) ;
#84754 = DIRECTION ( 'NONE',  ( -6.524622321627019585E-16, -4.013151879589939944E-16, -1.000000000000000000 ) ) ;
#84757 = CARTESIAN_POINT ( 'NONE',  ( 107.0667039024470313, -104.2784471599413791, 2.217806855418003043 ) ) ;
#84758 = CARTESIAN_POINT ( 'NONE',  ( 164.7812970173265512, -35.65087443490954655, 342.9256252759109884 ) ) ;
#84759 = LINE ( 'NONE', #77935, #571 ) ;
#84760 = DIRECTION ( 'NONE',  ( -1.000000000000000000, 6.745093096447288888E-17, -2.283216351027200160E-14 ) ) ;
#84761 = DIRECTION ( 'NONE',  ( 0.000000000000000000, 0.000000000000000000, -1.000000000000000000 ) ) ;
#84762 = FACE_OUTER_BOUND ( 'NONE', #61355, .T. ) ;
#84764 = ORIENTED_EDGE ( 'NONE', *, *, #12685, .F. ) ;
#84763 = CARTESIAN_POINT ( 'NONE',  ( 113.7843247631140571, -29.05179538500707892, 289.5032443235299979 ) ) ;
#84765 = LINE ( 'NONE', #22094, #200 ) ;
#84766 = CARTESIAN_POINT ( 'NONE',  ( 117.7261736041901372, -39.74048882516440528, 143.6194347997209775 ) ) ;
#84767 = CARTESIAN_POINT ( 'NONE',  ( 115.2670960386832775, -44.14051530504124088, 79.25372051400697160 ) ) ;
#84768 = CARTESIAN_POINT ( 'NONE',  ( 114.9980252723336207, -29.89690579156949823, 180.3927681330539770 ) ) ;
#84769 = DIRECTION ( 'NONE',  ( 1.000000000000000000, 0.000000000000000000, 0.000000000000000000 ) ) ;
#84770 = CARTESIAN_POINT ( 'NONE',  ( 182.0374245136174522, -23.42844715993458848, 180.4678068554150343 ) ) ;
#84772 = DIRECTION ( 'NONE',  ( -1.092739197465703932E-16, 1.000000000000000000, 0.000000000000000000 ) ) ;
#84771 = CARTESIAN_POINT ( 'NONE',  ( -458.3598257906459708, 60.32499999999999574, 3.174999999999999822 ) ) ;
#84773 = CARTESIAN_POINT ( 'NONE',  ( 116.3201356630459884, -32.94258242523766711, 69.13562527591093954 ) ) ;
#84774 = CARTESIAN_POINT ( 'NONE',  ( 134.0664832912740110, -8.350947159940998787, 311.1531252759119752 ) ) ;
#84775 = ORIENTED_EDGE ( 'NONE', *, *, #19874, .T. ) ;
#84776 = AXIS2_PLACEMENT_3D ( 'NONE', #81853, #60022, #46839 ) ;
#84777 = LINE ( 'NONE', #12699, #9350 ) ;
#84778 = AXIS2_PLACEMENT_3D ( 'NONE', #62362, #15120, #21040 ) ;
#84779 = EDGE_CURVE ( 'NONE', #83074, #36953, #29940, .T. ) ;
#84780 = VERTEX_POINT ( 'NONE', #26672 ) ;
#84781 = EDGE_CURVE ( 'NONE', #47365, #57167, #82117, .T. ) ;
#84782 = VERTEX_POINT ( 'NONE', #83442 ) ;
#84783 = ADVANCED_FACE ( 'NONE', ( #47553 ), #61631, .F. ) ;
#84785 = EDGE_LOOP ( 'NONE', ( #47568, #86886, #19336, #87026 ) ) ;
#84784 = DIRECTION ( 'NONE',  ( 6.982966722218758611E-15, 0.000000000000000000, -1.000000000000000000 ) ) ;
#84786 = CARTESIAN_POINT ( 'NONE',  ( 113.4461594614341209, -46.68675298423766407, 64.02991099019695298 ) ) ;
#84787 = PLANE ( 'NONE',  #84605 ) ;
#84788 = CARTESIAN_POINT ( 'NONE',  ( 98.60478223830740774, 120.6499999999999915, 3.859079674607175002E-13 ) ) ;
#84789 = EDGE_CURVE ( 'NONE', #65340, #61102, #54806, .T. ) ;
#84790 = CARTESIAN_POINT ( 'NONE',  ( 97.38492667529318680, -42.15761073986299579, 177.7451490854349743 ) ) ;
#84791 = CARTESIAN_POINT ( 'NONE',  ( 99.00226700525801959, -39.63126001020209799, 266.0238483995056527 ) ) ;
#84792 = VERTEX_POINT ( 'NONE', #13504 ) ;
#84793 = ORIENTED_EDGE ( 'NONE', *, *, #25970, .F. ) ;
#84794 = ORIENTED_EDGE ( 'NONE', *, *, #33440, .F. ) ;
#84795 = EDGE_CURVE ( 'NONE', #78177, #56771, #41189, .T. ) ;
#84796 = VECTOR ( 'NONE', #89611, 1000.000000000000000 ) ;
#84797 = CIRCLE ( 'NONE', #80430, 5.499999999999999112 ) ;
#84798 = CARTESIAN_POINT ( 'NONE',  ( 107.0667039024470313, -104.2784471599409528, 249.2178068554179902 ) ) ;
#84799 = CARTESIAN_POINT ( 'NONE',  ( 141.0667039024479834, -48.82844715994099971, 198.9178068554149945 ) ) ;
#84800 = FACE_OUTER_BOUND ( 'NONE', #22641, .T. ) ;
#84801 = VECTOR ( 'NONE', #40248, 1000.000000000000000 ) ;
#84802 = CARTESIAN_POINT ( 'NONE',  ( 100.9552960800314310, -28.70654040160240328, 20.59290076991167595 ) ) ;
#84803 = CARTESIAN_POINT ( 'NONE',  ( 151.0667039024469886, -79.67844715994088745, 120.2178068554179902 ) ) ;
#84804 = LINE ( 'NONE', #37084, #56719 ) ;
#84805 = DIRECTION ( 'NONE',  ( -1.000000000000000078E-15, 0.000000000000000000, -1.000000000000000000 ) ) ;
#84806 = VECTOR ( 'NONE', #76045, 1000.000000000000000 ) ;
#84807 = DIRECTION ( 'NONE',  ( 0.000000000000000000, 0.000000000000000000, -1.000000000000000000 ) ) ;
#84808 = CARTESIAN_POINT ( 'NONE',  ( 104.7405551043178491, -47.51155644559854352, 32.41943479972098174 ) ) ;
#84810 = ORIENTED_EDGE ( 'NONE', *, *, #70012, .T. ) ;
#84809 = EDGE_CURVE ( 'NONE', #67327, #76187, #6683, .T. ) ;
#84811 = DIRECTION ( 'NONE',  ( 0.000000000000000000, 1.000000000000000000, 0.000000000000000000 ) ) ;
#84812 = CARTESIAN_POINT ( 'NONE',  ( 154.4439038579832300, -17.91479848270203945, 396.9756252759102040 ) ) ;
#84813 = CARTESIAN_POINT ( 'NONE',  ( 116.3348466390194460, -36.28970630669515174, 116.6823760838769601 ) ) ;
#84814 = EDGE_CURVE ( 'NONE', #2062, #24255, #86484, .T. ) ;
#84815 = CARTESIAN_POINT ( 'NONE',  ( 97.81135238452728231, -40.51660343587602142, 96.63555416999651015 ) ) ;
#84816 = CARTESIAN_POINT ( 'NONE',  ( 37.56670390244806157, -48.82844715994099971, 300.4678068554150059 ) ) ;
#84817 = VERTEX_POINT ( 'NONE', #18347 ) ;
#84818 = ORIENTED_EDGE ( 'NONE', *, *, #78989, .T. ) ;
#84819 = CARTESIAN_POINT ( 'NONE',  ( 101.9936818365031144, -45.44611147528136286, 137.1550710178724444 ) ) ;
#84820 = VERTEX_POINT ( 'NONE', #39683 ) ;
#84821 = VERTEX_POINT ( 'NONE', #19697 ) ;
#84822 = CARTESIAN_POINT ( 'NONE',  ( 97.47186360698646013, -39.79766782782348855, 128.0044404487539396 ) ) ;
#84823 = CARTESIAN_POINT ( 'NONE',  ( 108.8673596973266058, 37.33800000000000097, 50.79999999999999716 ) ) ;
#84824 = EDGE_CURVE ( 'NONE', #78010, #58653, #40587, .T. ) ;
#84825 = CARTESIAN_POINT ( 'NONE',  ( 101.6996507173639088, -27.72520905039313632, 81.50419670448295051 ) ) ;
#84826 = AXIS2_PLACEMENT_3D ( 'NONE', #6548, #69227, #47863 ) ;
#84827 = CARTESIAN_POINT ( 'NONE',  ( 110.9020743365320243, -45.96463798019833291, 17.88972164584141566 ) ) ;
#84828 = VERTEX_POINT ( 'NONE', #59672 ) ;
#84829 = VECTOR ( 'NONE', #40372, 1000.000000000000000 ) ;
#84830 = ORIENTED_EDGE ( 'NONE', *, *, #44521, .F. ) ;
#84831 = EDGE_LOOP ( 'NONE', ( #48928, #7922, #1787, #47514, #14231 ) ) ;
#84832 = CARTESIAN_POINT ( 'NONE',  ( 113.4731498177359725, -46.72887913999166898, 68.02991099019695298 ) ) ;
#84833 = EDGE_LOOP ( 'NONE', ( #14330, #8584, #22365, #19049 ) ) ;
#84834 = CARTESIAN_POINT ( 'NONE',  ( 105.1480534446306621, -26.53835310083740850, 280.2365776568638580 ) ) ;
#84835 = CARTESIAN_POINT ( 'NONE',  ( 95.88671040095643150, -32.72508343906864781, 172.0527681330539735 ) ) ;
#84836 = CARTESIAN_POINT ( 'NONE',  ( 99.66264782090949836, -39.75983002812326106, 9.635625275910941312 ) ) ;
#84837 = CARTESIAN_POINT ( 'NONE',  ( -110.3179153611602032, 45.92529307294462626, 69.82078934106453971 ) ) ;
#84838 = CARTESIAN_POINT ( 'NONE',  ( 117.2094703596446550, -39.28701360234872197, 119.6299109901969615 ) ) ;
#84839 = DIRECTION ( 'NONE',  ( 0.000000000000000000, 0.000000000000000000, 1.000000000000000000 ) ) ;
#84840 = VERTEX_POINT ( 'NONE', #11086 ) ;
#84841 = CARTESIAN_POINT ( 'NONE',  ( 61.00843881761244347, 65.60000000000000853, -53.97512327982435210 ) ) ;
#84842 = EDGE_CURVE ( 'NONE', #27014, #7823, #52827, .T. ) ;
#84843 = ORIENTED_EDGE ( 'NONE', *, *, #54541, .T. ) ;
#84844 = LINE ( 'NONE', #71657, #9970 ) ;
#84845 = EDGE_LOOP ( 'NONE', ( #17215, #75822 ) ) ;
#84846 = ORIENTED_EDGE ( 'NONE', *, *, #6795, .T. ) ;
#84847 = ADVANCED_FACE ( 'NONE', ( #81949 ), #5179, .F. ) ;
#84848 = VECTOR ( 'NONE', #19550, 1000.000000000000000 ) ;
#84849 = PLANE ( 'NONE',  #34457 ) ;
#84850 = AXIS2_PLACEMENT_3D ( 'NONE', #10900, #10028, #59038 ) ;
#84851 = CONICAL_SURFACE ( 'NONE', #3587, 88.90000000000000568, 0.7853981633974552734 ) ;
#84852 = CARTESIAN_POINT ( 'NONE',  ( 7.336227921918954564, 92.80226562212374120, 118.3292963051747932 ) ) ;
#84853 = CARTESIAN_POINT ( 'NONE',  ( 117.5124197103495050, -37.28486668576427121, 18.78419670448294809 ) ) ;
#84854 = CARTESIAN_POINT ( 'NONE',  ( -72.96458098368600531, 127.0000000000000000, -65.02708098368781009 ) ) ;
#84855 = AXIS2_PLACEMENT_3D ( 'NONE', #39215, #66924, #32845 ) ;
#84856 = CARTESIAN_POINT ( 'NONE',  ( -72.96458098368751166, 127.0000000000000000, 80.90208098368620426 ) ) ;
#84857 = DIRECTION ( 'NONE',  ( -1.000000000000000000, 0.000000000000000000, 0.000000000000000000 ) ) ;
#84858 = CARTESIAN_POINT ( 'NONE',  ( 103.8130989789263197, -45.95327097697902730, 57.30705384734097407 ) ) ;
#84860 = CARTESIAN_POINT ( 'NONE',  ( 108.9412587213990804, -26.46057952311826611, 160.9327681330539690 ) ) ;
#84859 = CARTESIAN_POINT ( 'NONE',  ( 172.5664832912740110, -32.07844715994070839, 263.6756252759120116 ) ) ;
#84861 = CARTESIAN_POINT ( 'NONE',  ( 98.34985890762048655, -31.65658481782444156, 71.90645861000221828 ) ) ;
#84862 = CARTESIAN_POINT ( 'NONE',  ( 194.0371591254574923, -24.42818131005417115, 193.9678068554150343 ) ) ;
#84863 = VERTEX_POINT ( 'NONE', #26514 ) ;
#84864 = LINE ( 'NONE', #84420, #59884 ) ;
#84865 = AXIS2_PLACEMENT_3D ( 'NONE', #58254, #85984, #3302 ) ;
#84866 = CIRCLE ( 'NONE', #77587, 2.750000000000002665 ) ;
#84867 = CARTESIAN_POINT ( 'NONE',  ( 73.17003668186730181, -46.47944715994106701, 14.92562527591093691 ) ) ;
#84868 = DIRECTION ( 'NONE',  ( 0.000000000000000000, 0.000000000000000000, 1.000000000000000000 ) ) ;
#84869 = VERTEX_POINT ( 'NONE', #73767 ) ;
#84870 = CARTESIAN_POINT ( 'NONE',  ( 72.96458098368650269, 127.0000000000000000, 72.96458098368729850 ) ) ;
#84872 = ORIENTED_EDGE ( 'NONE', *, *, #32821, .T. ) ;
#84871 = CARTESIAN_POINT ( 'NONE',  ( 108.6818361061225602, -26.38549717321916788, 189.9527681330539792 ) ) ;
#84873 = CARTESIAN_POINT ( 'NONE',  ( -69.72411017812909506, 120.6499999999999915, -69.72411017813089984 ) ) ;
#84874 = CARTESIAN_POINT ( 'NONE',  ( 102.2271567091324158, -45.98785831331388607, 208.1927681330539599 ) ) ;
#84875 = CARTESIAN_POINT ( 'NONE',  ( 117.6393638915270827, -42.19070237429166070, 89.44705384733997278 ) ) ;
#84876 = CARTESIAN_POINT ( 'NONE',  ( 115.8281814319410046, -31.73477621452418873, 250.2407391550281943 ) ) ;
#84877 = DIRECTION ( 'NONE',  ( -0.8660254037844392627, 0.4999999999999990008, -1.549999999999999706E-14 ) ) ;
#84878 = DIRECTION ( 'NONE',  ( -1.000000000000000000, 0.000000000000000000, 0.000000000000000000 ) ) ;
#84879 = VERTEX_POINT ( 'NONE', #46035 ) ;
#84880 = AXIS2_PLACEMENT_3D ( 'NONE', #21511, #62818, #55532 ) ;
#84881 = EDGE_CURVE ( 'NONE', #62879, #72320, #5637, .T. ) ;
#84882 = ORIENTED_EDGE ( 'NONE', *, *, #38599, .T. ) ;
#84883 = EDGE_CURVE ( 'NONE', #8973, #35850, #80600, .T. ) ;
#84884 = ORIENTED_EDGE ( 'NONE', *, *, #68252, .T. ) ;
#84885 = EDGE_CURVE ( 'NONE', #52538, #51892, #31348, .T. ) ;
#84886 = VERTEX_POINT ( 'NONE', #66954 ) ;
#84887 = CARTESIAN_POINT ( 'NONE',  ( 182.5667039024480118, -32.29483332968430886, 342.9256252759109884 ) ) ;
#84888 = CARTESIAN_POINT ( 'NONE',  ( 96.51815522165868799, -31.32876289826797134, 241.9499109901969689 ) ) ;
#84889 = DIRECTION ( 'NONE',  ( 1.000000000000000000, 1.374769042280159607E-11, 0.000000000000000000 ) ) ;
#84890 = PLANE ( 'NONE',  #44031 ) ;
#84891 = EDGE_CURVE ( 'NONE', #41960, #56128, #60312, .T. ) ;
#84893 = CARTESIAN_POINT ( 'NONE',  ( 74.89107914305698444, 78.46407912418317210, 91.90683392111155570 ) ) ;
#84892 = LINE ( 'NONE', #22661, #3285 ) ;
#84894 = CARTESIAN_POINT ( 'NONE',  ( -47.11752803141011015, 100.5999999999999659, 108.7909173056707317 ) ) ;
#84895 = CARTESIAN_POINT ( 'NONE',  ( 106.2504075017224210, -26.27849585604564098, 25.13848241876792855 ) ) ;
#84896 = ORIENTED_EDGE ( 'NONE', *, *, #25047, .T. ) ;
#84897 = ORIENTED_EDGE ( 'NONE', *, *, #33244, .F. ) ;
#84898 = VECTOR ( 'NONE', #86167, 1000.000000000000000 ) ;
#84899 = EDGE_LOOP ( 'NONE', ( #27453, #50248, #35351, #49069 ) ) ;
#84900 = EDGE_CURVE ( 'NONE', #13709, #68878, #47284, .T. ) ;
#84901 = DIRECTION ( 'NONE',  ( 0.7071067811575898476, -0.7071067812155052978, 0.000000000000000000 ) ) ;
#84902 = AXIS2_PLACEMENT_3D ( 'NONE', #78397, #2076, #1180 ) ;
#84903 = CARTESIAN_POINT ( 'NONE',  ( -3.968749999999949818, 127.0000000000000000, -105.4788588808462038 ) ) ;
#84904 = CARTESIAN_POINT ( 'NONE',  ( 113.9608400058609874, -28.00707201209563024, 270.5441967044819194 ) ) ;
#84905 = ADVANCED_FACE ( 'NONE', ( #32411 ), #71958, .T. ) ;
#84906 = DIRECTION ( 'NONE',  ( 1.000000000000000078E-15, 1.000000000000000083E-30, -1.000000000000000000 ) ) ;
#84907 = CARTESIAN_POINT ( 'NONE',  ( 99.54941199951412045, -42.98700854487240974, 112.8784824187679732 ) ) ;
#84908 = CARTESIAN_POINT ( 'NONE',  ( -74.56320856954198462, 53.97500000000000142, 30.79999999999999361 ) ) ;
#84909 = EDGE_LOOP ( 'NONE', ( #36257, #51952 ) ) ;
#84910 = CARTESIAN_POINT ( 'NONE',  ( 143.9834832912729894, -71.52944715994142655, 361.9756252759109998 ) ) ;
#84911 = DIRECTION ( 'NONE',  ( 0.000000000000000000, 0.000000000000000000, 1.000000000000000000 ) ) ;
#84912 = ORIENTED_EDGE ( 'NONE', *, *, #54097, .T. ) ;
#84913 = ORIENTED_EDGE ( 'NONE', *, *, #57790, .F. ) ;
#84914 = DIRECTION ( 'NONE',  ( 1.000000000000000000, 0.000000000000000000, 6.878358445406130340E-15 ) ) ;
#84915 = CARTESIAN_POINT ( 'NONE',  ( 114.9297498758896126, -40.81563990160193356, 284.8758690201828472 ) ) ;
#84916 = AXIS2_PLACEMENT_3D ( 'NONE', #40521, #33715, #50915 ) ;
#84917 = AXIS2_PLACEMENT_3D ( 'NONE', #80308, #60275, #3987 ) ;
#84918 = CARTESIAN_POINT ( 'NONE',  ( -103.1875000000000000, 127.0000000000000000, -1.080832317973422076E-12 ) ) ;
#84919 = AXIS2_PLACEMENT_3D ( 'NONE', #47697, #49493, #70414 ) ;
#84920 = PLANE ( 'NONE',  #72272 ) ;
#84921 = DIRECTION ( 'NONE',  ( -0.9254794337955623007, -0.3787978585227819162, 0.000000000000000000 ) ) ;
#84922 = CIRCLE ( 'NONE', #83422, 10.00000000000000888 ) ;
#84923 = ORIENTED_EDGE ( 'NONE', *, *, #12561, .T. ) ;
#84924 = DIRECTION ( 'NONE',  ( 0.000000000000000000, 0.000000000000000000, -1.000000000000000000 ) ) ;
#84925 = DIRECTION ( 'NONE',  ( -1.000000000000000078E-15, 1.000000000000000083E-30, 1.000000000000000000 ) ) ;
#84926 = EDGE_LOOP ( 'NONE', ( #47146, #61952, #83749, #59335 ) ) ;
#84927 = CARTESIAN_POINT ( 'NONE',  ( 96.03551326368828711, -41.06051932364815826, 96.62419670448197451 ) ) ;
#84928 = VERTEX_POINT ( 'NONE', #18805 ) ;
#84929 = CARTESIAN_POINT ( 'NONE',  ( 100.5619151801845419, -43.03049977154007166, 41.37337220902998070 ) ) ;
#84930 = AXIS2_PLACEMENT_3D ( 'NONE', #22664, #15839, #43519 ) ;
#84931 = PLANE ( 'NONE',  #34431 ) ;
#84932 = CARTESIAN_POINT ( 'NONE',  ( 99.18511857479137461, -30.88155312011791409, 180.8184824187689799 ) ) ;
#84933 = CARTESIAN_POINT ( 'NONE',  ( -22.10999473297549045, 47.99418752069149008, 31.03039529537862506 ) ) ;
#84934 = LINE ( 'NONE', #57187, #53182 ) ;
#84935 = FACE_OUTER_BOUND ( 'NONE', #75312, .T. ) ;
#84936 = EDGE_CURVE ( 'NONE', #64699, #13223, #32871, .T. ) ;
#84937 = CARTESIAN_POINT ( 'NONE',  ( -55.89999999999999858, 53.97500000000000142, 70.79999999999999716 ) ) ;
#84938 = CIRCLE ( 'NONE', #5098, 2.517499999999998739 ) ;
#84939 = CARTESIAN_POINT ( 'NONE',  ( 115.7313686325390876, -42.60420177353093862, 269.3527681330536439 ) ) ;
#84940 = CARTESIAN_POINT ( 'NONE',  ( 81.76533775135496285, 94.92435932957492639, -85.84941893669241608 ) ) ;
#84941 = ORIENTED_EDGE ( 'NONE', *, *, #47635, .F. ) ;
#84942 = LINE ( 'NONE', #907, #18284 ) ;
#84943 = ORIENTED_EDGE ( 'NONE', *, *, #63109, .F. ) ;
#84944 = CARTESIAN_POINT ( 'NONE',  ( 109.2103426150987104, -26.48265019188898606, 135.9127681330539872 ) ) ;
#84945 = FACE_OUTER_BOUND ( 'NONE', #17965, .T. ) ;
#84946 = ORIENTED_EDGE ( 'NONE', *, *, #38644, .F. ) ;
#84947 = ORIENTED_EDGE ( 'NONE', *, *, #79264, .T. ) ;
#84948 = ORIENTED_EDGE ( 'NONE', *, *, #35969, .F. ) ;
#84949 = DIRECTION ( 'NONE',  ( 1.000000000000000000, 0.000000000000000000, 0.000000000000000000 ) ) ;
#84950 = CARTESIAN_POINT ( 'NONE',  ( 116.3251085584666527, -32.94148239642360210, 265.1356252759109680 ) ) ;
#84951 = DIRECTION ( 'NONE',  ( -0.000000000000000000, 1.000000000000000000, -0.000000000000000000 ) ) ;
#84952 = CARTESIAN_POINT ( 'NONE',  ( 144.5809607762889470, -138.4431012436764377, 247.5929369389089914 ) ) ;
#84953 = DIRECTION ( 'NONE',  ( 0.000000000000000000, 0.000000000000000000, 1.000000000000000000 ) ) ;
#84954 = CARTESIAN_POINT ( 'NONE',  ( 100.4110913530865332, -28.70521849941338033, 36.62705384733894221 ) ) ;
#84955 = FACE_BOUND ( 'NONE', #29132, .T. ) ;
#84956 = ORIENTED_EDGE ( 'NONE', *, *, #42698, .T. ) ;
#84957 = CARTESIAN_POINT ( 'NONE',  ( 12.27439874544222853, 79.26318322085235479, 117.9189513481508982 ) ) ;
#84958 = CARTESIAN_POINT ( 'NONE',  ( 84.06648329127399677, -18.82844715994099971, 199.5838068554169524 ) ) ;
#84959 = VERTEX_POINT ( 'NONE', #74226 ) ;
#84960 = ORIENTED_EDGE ( 'NONE', *, *, #6036, .T. ) ;
#84961 = AXIS2_PLACEMENT_3D ( 'NONE', #52715, #53621, #4614 ) ;
#84962 = ADVANCED_FACE ( 'NONE', ( #12001 ), #46932, .T. ) ;
#84963 = CARTESIAN_POINT ( 'NONE',  ( 70.06670390244705970, -124.7784471599409812, 55.21780685541800437 ) ) ;
#84964 = CARTESIAN_POINT ( 'NONE',  ( 191.6375511031384633, -78.44951497180814215, 342.9256252759109884 ) ) ;
#84965 = VECTOR ( 'NONE', #53306, 1000.000000000000000 ) ;
#84966 = SURFACE_STYLE_USAGE ( .BOTH. , #64949 ) ;
#84967 = PLANE ( 'NONE',  #36165 ) ;
#84968 = DIRECTION ( 'NONE',  ( -1.000000000000000078E-15, 1.000000000000000083E-30, 1.000000000000000000 ) ) ;
#84969 = CARTESIAN_POINT ( 'NONE',  ( 105.4642979808546670, -28.33962392264099250, 234.6495626852199621 ) ) ;
#84971 = CARTESIAN_POINT ( 'NONE',  ( 97.30890135812539654, -33.12136451854836849, 62.04419670448196911 ) ) ;
#84970 = CARTESIAN_POINT ( 'NONE',  ( 61.68306511546570903, -72.55869591834559174, 542.9756252759101471 ) ) ;
#84972 = DIRECTION ( 'NONE',  ( 8.881784197001251337E-16, 0.000000000000000000, 1.000000000000000000 ) ) ;
#84973 = CARTESIAN_POINT ( 'NONE',  ( 117.9021936627155895, -39.13782096276514721, 103.6403871806729455 ) ) ;
#84974 = ORIENTED_EDGE ( 'NONE', *, *, #68593, .T. ) ;
#84975 = CARTESIAN_POINT ( 'NONE',  ( -72.96458098368600531, 127.0000000000000000, -72.96458098368781009 ) ) ;
#84976 = EDGE_LOOP ( 'NONE', ( #20249, #80242, #4700, #16616 ) ) ;
#84977 = DIRECTION ( 'NONE',  ( 1.000000000000000078E-15, -1.000000000000000083E-30, -1.000000000000000000 ) ) ;
#84978 = CARTESIAN_POINT ( 'NONE',  ( 226.4410000000000025, 40.03750000000000142, -2.032000000000000028 ) ) ;
#84979 = ORIENTED_EDGE ( 'NONE', *, *, #26843, .F. ) ;
#84980 = LINE ( 'NONE', #10003, #11374 ) ;
#84981 = ORIENTED_EDGE ( 'NONE', *, *, #45461, .F. ) ;
#84982 = LINE ( 'NONE', #71788, #40656 ) ;
#84983 = CARTESIAN_POINT ( 'NONE',  ( 63.03715912545646205, -24.89890238295017255, 129.9678068554150911 ) ) ;
#84985 = AXIS2_PLACEMENT_3D ( 'NONE', #44532, #8250, #10042 ) ;
#84984 = CARTESIAN_POINT ( 'NONE',  ( 76.06670390244805446, -58.72944715994109544, 239.5838068554169809 ) ) ;
#84986 = VERTEX_POINT ( 'NONE', #52389 ) ;
#84987 = CARTESIAN_POINT ( 'NONE',  ( 113.3557719660652339, -27.61131746675945209, 89.60800622829195561 ) ) ;
#84988 = VECTOR ( 'NONE', #86891, 1000.000000000000000 ) ;
#84989 = VECTOR ( 'NONE', #5689, 1000.000000000000000 ) ;
#84990 = AXIS2_PLACEMENT_3D ( 'NONE', #74390, #38509, #18974 ) ;
#84991 = CARTESIAN_POINT ( 'NONE',  ( 172.5664832912740110, -36.32844715994070839, 78.92562527591199739 ) ) ;
#84992 = CARTESIAN_POINT ( 'NONE',  ( 107.0667039024470313, -104.2784471599421323, -21.78219314458201694 ) ) ;
#84993 = FACE_OUTER_BOUND ( 'NONE', #71413, .T. ) ;
#84994 = ORIENTED_EDGE ( 'NONE', *, *, #69483, .F. ) ;
#84995 = EDGE_CURVE ( 'NONE', #27158, #28006, #24108, .T. ) ;
#84996 = EDGE_CURVE ( 'NONE', #75042, #76300, #46891, .T. ) ;
#84997 = CARTESIAN_POINT ( 'NONE',  ( 99.03451269431035087, -108.3384846469520255, 2.217806855418142042 ) ) ;
#84998 = CARTESIAN_POINT ( 'NONE',  ( 34.96670390244699433, -28.27351298637401200, -5.074374724088000832 ) ) ;
#84999 = EDGE_CURVE ( 'NONE', #9193, #9719, #37007, .T. ) ;
#85000 = CIRCLE ( 'NONE', #8077, 7.937500000000000000 ) ;
#85001 = CARTESIAN_POINT ( 'NONE',  ( 38.10000000000000142, 95.25000000000000000, 283.4005000000000223 ) ) ;
#85002 = CARTESIAN_POINT ( 'NONE',  ( 107.9474582775578568, -25.68820226555254749, 111.0251490854349754 ) ) ;
#85003 = ADVANCED_FACE ( 'NONE', ( #64713 ), #2935, .T. ) ;
#85005 = PLANE ( 'NONE',  #55744 ) ;
#85004 = LINE ( 'NONE', #37733, #55214 ) ;
#85006 = DIRECTION ( 'NONE',  ( 0.000000000000000000, 0.000000000000000000, 1.000000000000000000 ) ) ;
#85007 = VECTOR ( 'NONE', #3659, 1000.000000000000114 ) ;
#85008 = ORIENTED_EDGE ( 'NONE', *, *, #13000, .F. ) ;
#85009 = CARTESIAN_POINT ( 'NONE',  ( -107.7702177616926065, 120.6499999999999915, -1.170464777364108012E-12 ) ) ;
#85010 = CARTESIAN_POINT ( 'NONE',  ( 99.59366209610200826, -44.96145431533973635, 152.9899109901959946 ) ) ;
#85011 = EDGE_CURVE ( 'NONE', #21358, #66312, #61814, .T. ) ;
#85013 = EDGE_LOOP ( 'NONE', ( #27686, #13202, #547, #72254 ) ) ;
#85012 = CARTESIAN_POINT ( 'NONE',  ( 44.45000000000000284, 50.79999999999999716, 257.1750000000000114 ) ) ;
#85014 = CARTESIAN_POINT ( 'NONE',  ( 101.7353989658871853, -28.52926574618699362, 21.53562527591096298 ) ) ;
#85015 = DIRECTION ( 'NONE',  ( 0.000000000000000000, 0.000000000000000000, -1.000000000000000000 ) ) ;
#85016 = FACE_OUTER_BOUND ( 'NONE', #30772, .T. ) ;
#85017 = DIRECTION ( 'NONE',  ( -1.514143847546115117E-15, 0.000000000000000000, 1.000000000000000000 ) ) ;
#85018 = LINE ( 'NONE', #8709, #68898 ) ;
#85019 = DIRECTION ( 'NONE',  ( -1.000000000000000000, 6.745093096447288888E-17, 2.089354330573420398E-14 ) ) ;
#85020 = CARTESIAN_POINT ( 'NONE',  ( 112.7271506738796347, -45.41826929060063378, 223.0480062282919675 ) ) ;
#85021 = EDGE_LOOP ( 'NONE', ( #72774, #69035, #55062, #32465 ) ) ;
#85022 = EDGE_LOOP ( 'NONE', ( #20019, #34915, #57499, #64516 ) ) ;
#85023 = CARTESIAN_POINT ( 'NONE',  ( 108.0145050256332979, -45.54020952213421936, 199.0930118773259778 ) ) ;
#85024 = DIRECTION ( 'NONE',  ( -3.100000000000000258E-29, 3.100000000000000044E-14, 1.000000000000000000 ) ) ;
#85025 = CARTESIAN_POINT ( 'NONE',  ( 106.9482176359816634, -27.83854490981203256, 56.51872616303998598 ) ) ;
#85026 = CIRCLE ( 'NONE', #15387, 1.000000000000000888 ) ;
#85027 = CARTESIAN_POINT ( 'NONE',  ( -100.7545871043104881, 84.62817240485476589, 83.02643542998036708 ) ) ;
#85028 = CARTESIAN_POINT ( 'NONE',  ( 100.8872800922797239, -44.70006565411546262, 267.0523716391360267 ) ) ;
#85029 = DIRECTION ( 'NONE',  ( 0.000000000000000000, 0.000000000000000000, 1.000000000000000000 ) ) ;
#85030 = ORIENTED_EDGE ( 'NONE', *, *, #47577, .F. ) ;
#85031 = CARTESIAN_POINT ( 'NONE',  ( 30.00000000000001776, 172.0000000000000000, 113.8826257785461280 ) ) ;
#85032 = FACE_OUTER_BOUND ( 'NONE', #35396, .T. ) ;
#85033 = CARTESIAN_POINT ( 'NONE',  ( 95.25611604350963546, -37.33230102880722967, 271.3670538473393776 ) ) ;
#85034 = CARTESIAN_POINT ( 'NONE',  ( 188.5667039024479834, -62.87844715994099687, 173.2178068554149775 ) ) ;
#85035 = ORIENTED_EDGE ( 'NONE', *, *, #3428, .T. ) ;
#85036 = ORIENTED_EDGE ( 'NONE', *, *, #6167, .F. ) ;
#85037 = CARTESIAN_POINT ( 'NONE',  ( -85.30119219530070040, 74.16222525595220816, -98.83784439188644910 ) ) ;
#85038 = CARTESIAN_POINT ( 'NONE',  ( -89.13693605261713060, 92.64232203292144163, -78.17042387453736296 ) ) ;
#85039 = CARTESIAN_POINT ( 'NONE',  ( -34.93928583487483763, 53.97499999999997300, 35.93880153443800651 ) ) ;
#85040 = LINE ( 'NONE', #30062, #7085 ) ;
#85041 = VECTOR ( 'NONE', #2707, 1000.000000000000000 ) ;
#85042 = EDGE_CURVE ( 'NONE', #36552, #57278, #70638, .T. ) ;
#85043 = CARTESIAN_POINT ( 'NONE',  ( 115.1412022171004281, -43.23618977845870148, 39.27467289495795200 ) ) ;
#85045 = CARTESIAN_POINT ( 'NONE',  ( 11.30815728993320413, 76.97724414224275336, 117.8147121273327684 ) ) ;
#85044 = VECTOR ( 'NONE', #51907, 999.9999999999997726 ) ;
#85046 = ORIENTED_EDGE ( 'NONE', *, *, #50230, .F. ) ;
#85047 = VECTOR ( 'NONE', #56821, 1000.000000000000000 ) ;
#85048 = CARTESIAN_POINT ( 'NONE',  ( 96.29363189909904008, -41.78481911317979325, 57.67562527591096710 ) ) ;
#85049 = VECTOR ( 'NONE', #1890, 1000.000000000000000 ) ;
#85050 = CARTESIAN_POINT ( 'NONE',  ( 107.0667039024470313, -104.2784471599418197, -11.78219314458200984 ) ) ;
#85051 = AXIS2_PLACEMENT_3D ( 'NONE', #48438, #14414, #88921 ) ;
#85052 = ADVANCED_FACE ( 'NONE', ( #51501, #79251 ), #51069, .T. ) ;
#85053 = CARTESIAN_POINT ( 'NONE',  ( 116.1776873554136813, -43.03363693755514419, 13.35657765686298859 ) ) ;
#85054 = ORIENTED_EDGE ( 'NONE', *, *, #38865, .T. ) ;
#85055 = LINE ( 'NONE', #43231, #53542 ) ;
#85056 = LINE ( 'NONE', #9187, #38455 ) ;
#85057 = CARTESIAN_POINT ( 'NONE',  ( 0.000000000000000000, 184.0000000000000000, 85.23828826961327820 ) ) ;
#85058 = CARTESIAN_POINT ( 'NONE',  ( 107.2759047676296120, -28.56943069780466971, 117.8738046553059462 ) ) ;
#85059 = CARTESIAN_POINT ( 'NONE',  ( 96.62257978078039855, -36.48017157545621814, 192.3070538473399438 ) ) ;
#85060 = CYLINDRICAL_SURFACE ( 'NONE', #79791, 2.117000000000007987 ) ;
#85061 = VERTEX_POINT ( 'NONE', #84732 ) ;
#85062 = AXIS2_PLACEMENT_3D ( 'NONE', #9932, #84906, #85359 ) ;
#85063 = CARTESIAN_POINT ( 'NONE',  ( 107.0664832912739399, -36.72944715994095333, 289.6356252759107406 ) ) ;
#85064 = ORIENTED_EDGE ( 'NONE', *, *, #79133, .T. ) ;
#85065 = VERTEX_POINT ( 'NONE', #52374 ) ;
#85066 = EDGE_CURVE ( 'NONE', #55433, #6845, #25574, .T. ) ;
#85067 = CYLINDRICAL_SURFACE ( 'NONE', #16901, 5.599999999999994316 ) ;
#85068 = VERTEX_POINT ( 'NONE', #45565 ) ;
#85069 = ORIENTED_EDGE ( 'NONE', *, *, #2035, .T. ) ;
#85070 = LINE ( 'NONE', #23733, #45428 ) ;
#85071 = AXIS2_PLACEMENT_3D ( 'NONE', #68340, #25201, #89238 ) ;
#85072 = CARTESIAN_POINT ( 'NONE',  ( 105.8901181204952309, -26.78673948403035610, 41.17015456836836051 ) ) ;
#85073 = CARTESIAN_POINT ( 'NONE',  ( 109.0672552851176249, -45.03324407163384535, 132.1867055423619775 ) ) ;
#85074 = CARTESIAN_POINT ( 'NONE',  ( 100.8351866834200337, -45.15911532695984931, 257.0699109901966608 ) ) ;
#85075 = CARTESIAN_POINT ( 'NONE',  ( 184.5667039024480118, -67.87844715994100397, 10.91780685541479734 ) ) ;
#85076 = ORIENTED_EDGE ( 'NONE', *, *, #303, .T. ) ;
#85077 = EDGE_CURVE ( 'NONE', #63620, #18180, #64812, .T. ) ;
#85078 = ORIENTED_EDGE ( 'NONE', *, *, #88559, .T. ) ;
#85079 = CARTESIAN_POINT ( 'NONE',  ( 32.25690895536977365, -33.54226604285049262, 193.9678068554150911 ) ) ;
#85080 = LINE ( 'NONE', #41910, #12985 ) ;
#85081 = CYLINDRICAL_SURFACE ( 'NONE', #55624, 2.117000000000000881 ) ;
#85082 = CARTESIAN_POINT ( 'NONE',  ( 113.3411949225463502, -28.30449682957925717, 104.5670538473399347 ) ) ;
#85083 = CARTESIAN_POINT ( 'NONE',  ( 96.51917584821923413, -40.19201726479878545, 286.5908633711491120 ) ) ;
#85084 = EDGE_LOOP ( 'NONE', ( #41699, #59371, #73245, #46159 ) ) ;
#85085 = PRODUCT_DEFINITION_CONTEXT ( 'detailed design', #77131, 'design' ) ;
#85086 = CARTESIAN_POINT ( 'NONE',  ( 112.4894639655092305, -46.36118470102660183, 257.9965776568635647 ) ) ;
#85087 = CYLINDRICAL_SURFACE ( 'NONE', #60187, 3.250000000000002665 ) ;
#85088 = FILL_AREA_STYLE ('',( #62819 ) ) ;
#85089 = CARTESIAN_POINT ( 'NONE',  ( 10.77469451420456359, 75.82559005915315709, 130.1106627578315340 ) ) ;
#85090 = CARTESIAN_POINT ( 'NONE',  ( 124.0664832912757163, -36.72944715993921960, -5.074374724089012467 ) ) ;
#85091 = B_SPLINE_CURVE_WITH_KNOTS ( 'NONE', 3,
 ( #51686, #79433, #64445, #57161, #17195, #71276, #2225, #15414, #30375, #64894, #16744, #57619, #10372, #9047, #85361, #29479, #16303, #49899 ),
 .UNSPECIFIED., .F., .F.,
 ( 4, 2, 2, 2, 2, 2, 2, 2, 4 ),
 ( 0.4999879786943189908, 0.5624894813575290753, 0.6249909840207392708, 0.6874924866839493554, 0.7499939893471594399, 0.8124954920103696354, 0.8749969946735797199, 0.9374984973367899155, 1.000000000000000000 ),
 .UNSPECIFIED. ) ;
#85093 = LINE ( 'NONE', #45054, #23908 ) ;
#85092 = CARTESIAN_POINT ( 'NONE',  ( 130.5667039024470455, -104.2784471599409386, 23.21780685541800082 ) ) ;
#85094 = FACE_OUTER_BOUND ( 'NONE', #51893, .T. ) ;
#85095 = FACE_OUTER_BOUND ( 'NONE', #25515, .T. ) ;
#85096 = LINE ( 'NONE', #29224, #74558 ) ;
#85097 = CARTESIAN_POINT ( 'NONE',  ( -12.53577546185475811, 84.62767492864716701, 129.9527996235914600 ) ) ;
#85098 = LINE ( 'NONE', #30113, #88010 ) ;
#85099 = EDGE_CURVE ( 'NONE', #24268, #51571, #46915, .T. ) ;
#85100 = CARTESIAN_POINT ( 'NONE',  ( -41.60202597009397607, 64.60000000000000853, 33.51824159735392783 ) ) ;
#85102 = VERTEX_POINT ( 'NONE', #32396 ) ;
#85101 = CARTESIAN_POINT ( 'NONE',  ( 48.79742451362098166, -36.32844715994040996, -5.074374724088000832 ) ) ;
#85103 = LINE ( 'NONE', #48291, #75742 ) ;
#85104 = CARTESIAN_POINT ( 'NONE',  ( 111.4338919110110311, -46.24429912893436523, 27.91848241876792969 ) ) ;
#85105 = CARTESIAN_POINT ( 'NONE',  ( 117.4263761885577537, -30.97555849962366281, 175.2299109901969700 ) ) ;
#85106 = CARTESIAN_POINT ( 'NONE',  ( 105.3167593786310903, -26.43023667424511913, 11.20991099019697046 ) ) ;
#85107 = VECTOR ( 'NONE', #69393, 1000.000000000000000 ) ;
#85109 = CARTESIAN_POINT ( 'NONE',  ( 80.06648329127399677, -33.97944715994105991, 8.225625275910942946 ) ) ;
#85108 = DIRECTION ( 'NONE',  ( 0.000000000000000000, 0.000000000000000000, 1.000000000000000000 ) ) ;
#85110 = CARTESIAN_POINT ( 'NONE',  ( 115.7830851429092291, -41.80234991274182477, 139.4064549843119778 ) ) ;
#85111 = AXIS2_PLACEMENT_3D ( 'NONE', #16426, #23698, #23265 ) ;
#85112 = CIRCLE ( 'NONE', #16884, 39.10000000000005116 ) ;
#85113 = AXIS2_PLACEMENT_3D ( 'NONE', #23375, #16984, #38748 ) ;
#85114 = CONICAL_SURFACE ( 'NONE', #25557, 1.625000000000001332, 1.029744258676650093 ) ;
#85115 = VERTEX_POINT ( 'NONE', #25148 ) ;
#85116 = DIRECTION ( 'NONE',  ( 4.299999999999999979E-14, -1.000000000000000000, 4.400000000000000367E-29 ) ) ;
#85117 = ORIENTED_EDGE ( 'NONE', *, *, #37878, .T. ) ;
#85118 = CARTESIAN_POINT ( 'NONE',  ( 111.6283393632454022, -28.07768985461837730, 55.68991099019593349 ) ) ;
#85119 = ADVANCED_FACE ( 'NONE', ( #46471 ), #12423, .F. ) ;
#85121 = EDGE_LOOP ( 'NONE', ( #8320, #51487, #85035, #73229 ) ) ;
#85120 = CARTESIAN_POINT ( 'NONE',  ( 6.299229072587491096, 93.57981503384465327, 130.4040377106156257 ) ) ;
#85122 = CARTESIAN_POINT ( 'NONE',  ( 108.3329992365411556, -46.73491031212436297, 48.67725624094877901 ) ) ;
#85123 = CARTESIAN_POINT ( 'NONE',  ( 101.3611157396114635, -46.16939438856402944, 198.1318157521009482 ) ) ;
#85124 = PLANE ( 'NONE',  #70126 ) ;
#85125 = CARTESIAN_POINT ( 'NONE',  ( 97.81169536214920868, -40.51742132101362870, 146.6356105553879274 ) ) ;
#85126 = ADVANCED_FACE ( 'NONE', ( #58765, #80139 ), #40113, .T. ) ;
#85127 = DIRECTION ( 'NONE',  ( -1.000000000000000000, 9.376883653928684652E-16, 1.500301384628589584E-15 ) ) ;
#85128 = CARTESIAN_POINT ( 'NONE',  ( 25.56670390244797275, -58.35344715994099829, 290.4678068554150627 ) ) ;
#85129 = PLANE ( 'NONE',  #33183 ) ;
#85130 = CARTESIAN_POINT ( 'NONE',  ( 110.8541803763881859, -45.98435675075571538, 97.88560012996084936 ) ) ;
#85132 = CARTESIAN_POINT ( 'NONE',  ( 97.31342953368660176, -35.99458159538090030, 146.2670538473399517 ) ) ;
#85131 = VECTOR ( 'NONE', #32294, 1000.000000000000000 ) ;
#85133 = ORIENTED_EDGE ( 'NONE', *, *, #59489, .F. ) ;
#85134 = ORIENTED_EDGE ( 'NONE', *, *, #77237, .T. ) ;
#85135 = CARTESIAN_POINT ( 'NONE',  ( 114.7653520042265143, -30.23343873216411026, 70.81586902018300123 ) ) ;
#85136 = CLOSED_SHELL ( 'NONE', ( #79140, #5602, #25170, #5085 ) ) ;
#85137 = DIRECTION ( 'NONE',  ( -1.000000000000000078E-15, 1.000000000000000000, 0.000000000000000000 ) ) ;
#85139 = DIRECTION ( 'NONE',  ( 0.000000000000000000, 0.000000000000000000, -1.000000000000000000 ) ) ;
#85138 = CARTESIAN_POINT ( 'NONE',  ( 115.4995704134666141, -41.68388727776409297, 234.4041967044819899 ) ) ;
#85140 = LINE ( 'NONE', #50583, #82684 ) ;
#85141 = CARTESIAN_POINT ( 'NONE',  ( 183.5150000000000148, 21.46300000000000097, 59.96543552338529537 ) ) ;
#85142 = DIRECTION ( 'NONE',  ( -1.000000000000000000, 0.000000000000000000, 0.000000000000000000 ) ) ;
#85143 = CARTESIAN_POINT ( 'NONE',  ( -41.60202597009397607, 65.59999999999998010, 50.85338361873603219 ) ) ;
#85144 = CARTESIAN_POINT ( 'NONE',  ( 2.861368367625729547, 70.27219044652896685, 118.5221636901931817 ) ) ;
#85145 = CARTESIAN_POINT ( 'NONE',  ( 114.2249171546291677, -45.12625265263336871, 153.1508633711489722 ) ) ;
#85146 = EDGE_LOOP ( 'NONE', ( #75546, #75025, #32042, #62327 ) ) ;
#85147 = EDGE_LOOP ( 'NONE', ( #2678, #5561, #28181, #45562, #43339, #23220 ) ) ;
#85148 = EDGE_LOOP ( 'NONE', ( #36230, #45467, #33864, #83154 ) ) ;
#85149 = CARTESIAN_POINT ( 'NONE',  ( -100.4326241145870284, 86.63355734047006251, -83.41565754067492833 ) ) ;
#85150 = CARTESIAN_POINT ( 'NONE',  ( 100.9537233733097992, -28.70776136095884468, 130.5940555066760567 ) ) ;
#85151 = CARTESIAN_POINT ( 'NONE',  ( 97.83872692038849550, -40.58291890258023926, 102.6412641178015548 ) ) ;
#85152 = CARTESIAN_POINT ( 'NONE',  ( 109.5637425988213636, -28.92903792723274847, 232.6480903695909603 ) ) ;
#85153 = CONICAL_SURFACE ( 'NONE', #37280, 16.33514202138210791, 0.7853981633974552734 ) ;
#85154 = CARTESIAN_POINT ( 'NONE',  ( 97.81413906161476746, -40.51632882248723888, 267.6361360915977343 ) ) ;
#85155 = ADVANCED_FACE ( 'NONE', ( #66936 ), #38775, .F. ) ;
#85156 = CARTESIAN_POINT ( 'NONE',  ( 117.6792309033718027, -39.81954026856703877, 138.5889586092439743 ) ) ;
#85157 = CARTESIAN_POINT ( 'NONE',  ( 154.5667039024469886, -67.87844715994090450, 155.2178068554179902 ) ) ;
#85158 = VERTEX_POINT ( 'NONE', #60553 ) ;
#85160 = VERTEX_POINT ( 'NONE', #66478 ) ;
#85159 = ORIENTED_EDGE ( 'NONE', *, *, #14533, .F. ) ;
#85161 = CARTESIAN_POINT ( 'NONE',  ( 107.0667039024468039, -54.72944715994092491, 196.8538068554169911 ) ) ;
#85162 = VERTEX_POINT ( 'NONE', #19242 ) ;
#85163 = ORIENTED_EDGE ( 'NONE', *, *, #81943, .T. ) ;
#85164 = CARTESIAN_POINT ( 'NONE',  ( 52.06670390244699576, -67.87844715994100397, 222.2178068554179902 ) ) ;
#85165 = CARTESIAN_POINT ( 'NONE',  ( 125.5177273812784193, -99.45575754528751133, 222.2178068554179902 ) ) ;
#85166 = CARTESIAN_POINT ( 'NONE',  ( 100.2991084500796575, -40.90897653417852098, 9.586185607686982024 ) ) ;
#85167 = DIRECTION ( 'NONE',  ( -1.000000000000000000, 0.000000000000000000, 0.000000000000000000 ) ) ;
#85168 = ORIENTED_EDGE ( 'NONE', *, *, #66949, .F. ) ;
#85169 = AXIS2_PLACEMENT_3D ( 'NONE', #87431, #73794, #38370 ) ;
#85170 = CIRCLE ( 'NONE', #45946, 2.029999999999997140 ) ;
#85171 = CARTESIAN_POINT ( 'NONE',  ( 111.8278880821266767, -43.86989008726008166, 9.635625275910941312 ) ) ;
#85172 = DIRECTION ( 'NONE',  ( -3.100000000000000258E-29, 3.100000000000000044E-14, 1.000000000000000000 ) ) ;
#85173 = ORIENTED_EDGE ( 'NONE', *, *, #3257, .F. ) ;
#85174 = VERTEX_POINT ( 'NONE', #46017 ) ;
#85175 = VECTOR ( 'NONE', #10116, 1000.000000000000000 ) ;
#85177 = EDGE_CURVE ( 'NONE', #10881, #7937, #40092, .T. ) ;
#85176 = AXIS2_PLACEMENT_3D ( 'NONE', #70960, #8732, #49127 ) ;
#85178 = CARTESIAN_POINT ( 'NONE',  ( 112.0330966381960991, -45.41505981916921542, 112.9898362350633221 ) ) ;
#85179 = AXIS2_PLACEMENT_3D ( 'NONE', #35286, #21689, #55268 ) ;
#85180 = VERTEX_POINT ( 'NONE', #24711 ) ;
#85181 = ORIENTED_EDGE ( 'NONE', *, *, #73320, .F. ) ;
#85182 = CARTESIAN_POINT ( 'NONE',  ( 109.7027494226597071, -44.85393009491053817, 12.24956268521998304 ) ) ;
#85183 = EDGE_CURVE ( 'NONE', #51227, #45628, #4268, .T. ) ;
#85184 = CARTESIAN_POINT ( 'NONE',  ( 99.08440026364779385, -45.52245356036965518, 156.9899109901969609 ) ) ;
#85185 = CARTESIAN_POINT ( 'NONE',  ( 98.00553567079148820, -41.84099229931894115, 136.7356252759109623 ) ) ;
#85186 = FACE_OUTER_BOUND ( 'NONE', #14592, .T. ) ;
#85187 = CARTESIAN_POINT ( 'NONE',  ( 101.4046705256369734, -45.52519664383009257, 218.1213395616249784 ) ) ;
#85188 = CARTESIAN_POINT ( 'NONE',  ( 51.06648329127400388, 25.62155284005901379, 327.8006252759110453 ) ) ;
#85189 = CARTESIAN_POINT ( 'NONE',  ( 81.98010489515323229, -91.89993919647076837, 250.2190963482990185 ) ) ;
#85190 = ORIENTED_EDGE ( 'NONE', *, *, #64249, .F. ) ;
#85191 = CARTESIAN_POINT ( 'NONE',  ( -130.0912141755840992, 76.20343663217360586, -11.00834544827219652 ) ) ;
#85193 = EDGE_LOOP ( 'NONE', ( #32921, #33253, #59030, #57202 ) ) ;
#85192 = ADVANCED_FACE ( 'NONE', ( #25598 ), #51940, .F. ) ;
#85194 = EDGE_CURVE ( 'NONE', #21457, #14514, #52809, .T. ) ;
#85195 = EDGE_LOOP ( 'NONE', ( #75478, #31339, #27076, #77044 ) ) ;
#85196 = VECTOR ( 'NONE', #53799, 1000.000000000000000 ) ;
#85197 = AXIS2_PLACEMENT_3D ( 'NONE', #56774, #71326, #85419 ) ;
#85198 = EDGE_CURVE ( 'NONE', #63781, #81490, #11984, .T. ) ;
#85199 = VECTOR ( 'NONE', #39637, 1000.000000000000000 ) ;
#85200 = CARTESIAN_POINT ( 'NONE',  ( 102.2167607299587928, -46.00774749580600798, 212.1927681330539599 ) ) ;
#85201 = EDGE_LOOP ( 'NONE', ( #67013, #30174, #27853, #87177, #48103 ) ) ;
#85202 = CARTESIAN_POINT ( 'NONE',  ( 96.61862839515298162, -36.21153332102672806, 171.2870538473399620 ) ) ;
#85203 = CARTESIAN_POINT ( 'NONE',  ( 164.7812970173289955, -35.65087443492610930, -5.074374724088000832 ) ) ;
#85204 = EDGE_CURVE ( 'NONE', #76607, #66477, #12551, .T. ) ;
#85205 = DIRECTION ( 'NONE',  ( -0.7071067811865475727, 0.7071067811865475727, 0.000000000000000000 ) ) ;
#85206 = DIRECTION ( 'NONE',  ( 0.000000000000000000, -1.000000000000000000, 0.000000000000000000 ) ) ;
#85209 = CARTESIAN_POINT ( 'NONE',  ( 115.2346088729119629, -30.22974330756305505, 240.3613395616249875 ) ) ;
#85208 = CARTESIAN_POINT ( 'NONE',  ( 34.27258461953899626, -35.55794170701810941, 342.9256252759119548 ) ) ;
#85207 = LINE ( 'NONE', #21170, #4152 ) ;
#85210 = CARTESIAN_POINT ( 'NONE',  ( 97.46299999999996544, 82.54999999999999716, 1.020870737183004530E-12 ) ) ;
#85211 = FACE_OUTER_BOUND ( 'NONE', #55615, .T. ) ;
#85212 = LINE ( 'NONE', #10221, #35320 ) ;
#85213 = PLANE ( 'NONE',  #6549 ) ;
#85214 = CARTESIAN_POINT ( 'NONE',  ( 116.8171228659443557, -34.15291831921626198, 260.0314586093679168 ) ) ;
#85215 = EDGE_CURVE ( 'NONE', #69535, #14111, #67369, .T. ) ;
#85216 = CARTESIAN_POINT ( 'NONE',  ( 146.2220825168437841, -137.2276697249587869, 247.1459391770515595 ) ) ;
#85218 = VERTEX_POINT ( 'NONE', #53724 ) ;
#85217 = CARTESIAN_POINT ( 'NONE',  ( 99.18160966223959463, -39.27556854586995883, 195.5838068554172651 ) ) ;
#85219 = LINE ( 'NONE', #8450, #69841 ) ;
#85220 = CARTESIAN_POINT ( 'NONE',  ( 109.6112504147204163, -26.56025234872169349, 199.8813395616249977 ) ) ;
#85221 = CARTESIAN_POINT ( 'NONE',  ( 96.07767081433036083, -37.92107664550148627, 77.40038718067299328 ) ) ;
#85222 = CARTESIAN_POINT ( 'NONE',  ( 117.2394727393827765, -34.25896837304814113, 205.0156252759109634 ) ) ;
#85223 = DIRECTION ( 'NONE',  ( 1.000000000000000000, 0.000000000000000000, 0.000000000000000000 ) ) ;
#85224 = CARTESIAN_POINT ( 'NONE',  ( 107.0667036193247696, -70.87844715994094713, 90.21780599115065513 ) ) ;
#85226 = CARTESIAN_POINT ( 'NONE',  ( 0.000000000000000000, 224.4999999999999432, 154.6557476874258441 ) ) ;
#85225 = DIRECTION ( 'NONE',  ( 0.000000000000000000, 0.000000000000000000, 1.000000000000000000 ) ) ;
#85227 = LINE ( 'NONE', #22102, #4572 ) ;
#85228 = DIRECTION ( 'NONE',  ( -0.7071067811865510144, 0.000000000000000000, 0.7071067811865441310 ) ) ;
#85229 = VERTEX_POINT ( 'NONE', #5161 ) ;
#85230 = CIRCLE ( 'NONE', #51834, 3.250000000000002665 ) ;
#85231 = CARTESIAN_POINT ( 'NONE',  ( 109.7274023519750159, -27.00147441307279550, 64.86589663587605514 ) ) ;
#85232 = ORIENTED_EDGE ( 'NONE', *, *, #56542, .F. ) ;
#85233 = ORIENTED_EDGE ( 'NONE', *, *, #25587, .T. ) ;
#85234 = EDGE_CURVE ( 'NONE', #14474, #27515, #12169, .T. ) ;
#85236 = ORIENTED_EDGE ( 'NONE', *, *, #52324, .T. ) ;
#85235 = DIRECTION ( 'NONE',  ( 0.000000000000000000, 0.000000000000000000, -1.000000000000000000 ) ) ;
#85237 = CARTESIAN_POINT ( 'NONE',  ( 111.0741232671659020, -25.60348521778456288, 95.80133956162495679 ) ) ;
#85238 = CARTESIAN_POINT ( 'NONE',  ( 1.387778780781445676E-14, 238.8000000000000114, 97.27542076772557778 ) ) ;
#85239 = EDGE_CURVE ( 'NONE', #75364, #47935, #32856, .T. ) ;
#85240 = ADVANCED_FACE ( 'NONE', ( #14217 ), #21028, .T. ) ;
#85241 = CARTESIAN_POINT ( 'NONE',  ( 21.03715912545829170, -47.82818131006186491, 249.9678068554150059 ) ) ;
#85242 = CARTESIAN_POINT ( 'NONE',  ( 172.5664832912740110, 0.2215528400590013880, 21.04262527591200183 ) ) ;
#85243 = ADVANCED_FACE ( 'NONE', ( #89181, #13763 ), #69178, .F. ) ;
#85244 = CIRCLE ( 'NONE', #82370, 5.499999999999999112 ) ;
#85245 = CARTESIAN_POINT ( 'NONE',  ( 115.0831197249980420, -29.02584261466826021, 39.43562527591099354 ) ) ;
#85246 = ORIENTED_EDGE ( 'NONE', *, *, #89868, .F. ) ;
#85247 = ORIENTED_EDGE ( 'NONE', *, *, #69379, .T. ) ;
#85248 = ORIENTED_EDGE ( 'NONE', *, *, #35087, .T. ) ;
#85249 = AXIS2_PLACEMENT_3D ( 'NONE', #51324, #51769, #72696 ) ;
#85250 = APPLICATION_CONTEXT ( 'automotive_design' ) ;
#85251 = VECTOR ( 'NONE', #26690, 1000.000000000000000 ) ;
#85252 = CARTESIAN_POINT ( 'NONE',  ( 134.0664832912739826, -9.029447159941003775, 8.225625275910998013 ) ) ;
#85253 = DIRECTION ( 'NONE',  ( 0.000000000000000000, 0.000000000000000000, 1.000000000000000000 ) ) ;
#85254 = AXIS2_PLACEMENT_3D ( 'NONE', #26144, #32051, #87036 ) ;
#85255 = DIRECTION ( 'NONE',  ( -4.299999999999999979E-14, 1.000000000000000000, -4.400000000000000367E-29 ) ) ;
#85256 = DIRECTION ( 'NONE',  ( 0.000000000000000000, 0.000000000000000000, 1.000000000000000000 ) ) ;
#85257 = CARTESIAN_POINT ( 'NONE',  ( 181.9790560690580037, -31.62489322948711035, -5.074374724088000832 ) ) ;
#85258 = DIRECTION ( 'NONE',  ( -1.000000000000000000, 0.000000000000000000, 0.000000000000000000 ) ) ;
#85259 = DIRECTION ( 'NONE',  ( -0.7071067811865171526, -0.7071067811865779928, -7.071067811865164719E-16 ) ) ;
#85260 = CARTESIAN_POINT ( 'NONE',  ( -4.908820038593109558, 94.26296816967553127, 130.4636833037901340 ) ) ;
#85261 = CARTESIAN_POINT ( 'NONE',  ( 116.8729656461675148, -36.55725972750698105, 288.8413395616257731 ) ) ;
#85262 = VERTEX_POINT ( 'NONE', #20589 ) ;
#85263 = AXIS2_PLACEMENT_3D ( 'NONE', #14461, #19472, #83493 ) ;
#85264 = CARTESIAN_POINT ( 'NONE',  ( 103.1875000000000000, 117.4749999999999943, 7.143750000000359535 ) ) ;
#85265 = VECTOR ( 'NONE', #5583, 999.9999999999998863 ) ;
#85266 = DIRECTION ( 'NONE',  ( -1.000000000000000000, 0.000000000000000000, -2.108231265501709878E-16 ) ) ;
#85267 = CARTESIAN_POINT ( 'NONE',  ( 115.3203086601475320, -34.12650808536288594, 126.8757094172099613 ) ) ;
#85268 = AXIS2_PLACEMENT_3D ( 'NONE', #62299, #89576, #20980 ) ;
#85269 = DIRECTION ( 'NONE',  ( 0.000000000000000000, 0.000000000000000000, 1.000000000000000000 ) ) ;
#85270 = DIRECTION ( 'NONE',  ( 1.000000000000000078E-15, 1.000000000000000083E-30, -1.000000000000000000 ) ) ;
#85271 = EDGE_LOOP ( 'NONE', ( #84170, #20037, #56629, #31322 ) ) ;
#85272 = ORIENTED_EDGE ( 'NONE', *, *, #79879, .F. ) ;
#85273 = LINE ( 'NONE', #15322, #42357 ) ;
#85274 = ORIENTED_EDGE ( 'NONE', *, *, #78837, .F. ) ;
#85275 = ORIENTED_EDGE ( 'NONE', *, *, #50702, .F. ) ;
#85276 = CARTESIAN_POINT ( 'NONE',  ( 99.58187507909633496, -41.47380365182278439, 183.2072975916109385 ) ) ;
#85277 = CARTESIAN_POINT ( 'NONE',  ( 97.06670390244701707, -98.59953881414068633, 17.71780685541782319 ) ) ;
#85278 = CARTESIAN_POINT ( 'NONE',  ( 109.2595486427728559, -46.97979643076451595, 103.7441967044829880 ) ) ;
#85279 = VECTOR ( 'NONE', #20023, 1000.000000000000000 ) ;
#85280 = CARTESIAN_POINT ( 'NONE',  ( 98.04153897299465825, -41.04189894509466541, 16.68120577741022004 ) ) ;
#85281 = EDGE_LOOP ( 'NONE', ( #11640, #85856, #81647, #47445, #7511, #24760 ) ) ;
#85282 = EDGE_LOOP ( 'NONE', ( #63721, #25718, #43391, #71561 ) ) ;
#85283 = EDGE_LOOP ( 'NONE', ( #55787, #51502, #38759, #7120 ) ) ;
#85284 = EDGE_CURVE ( 'NONE', #28761, #40995, #33312, .T. ) ;
#85285 = CARTESIAN_POINT ( 'NONE',  ( 108.0149359080884324, -45.33189881898218232, 155.4699951314959776 ) ) ;
#85286 = EDGE_CURVE ( 'NONE', #68811, #68997, #19722, .T. ) ;
#85287 = CARTESIAN_POINT ( 'NONE',  ( 97.60225484043094468, -32.22203741027808377, 75.97276813305397525 ) ) ;
#85288 = ORIENTED_EDGE ( 'NONE', *, *, #17352, .F. ) ;
#85289 = CARTESIAN_POINT ( 'NONE',  ( 111.1204619107249982, -46.98756979655009047, 22.88800622829195675 ) ) ;
#85290 = CARTESIAN_POINT ( 'NONE',  ( 104.5573670441197720, -48.33662538491821437, 178.4070538473399665 ) ) ;
#85291 = FACE_OUTER_BOUND ( 'NONE', #25649, .T. ) ;
#85292 = CARTESIAN_POINT ( 'NONE',  ( -109.7026200886537879, 48.81775394257228839, 70.78279810002825911 ) ) ;
#85293 = CARTESIAN_POINT ( 'NONE',  ( 114.7260775003150712, -43.80144150384058577, 119.2327681330539804 ) ) ;
#85294 = CARTESIAN_POINT ( 'NONE',  ( 100.8874679133985381, -44.70022139721319832, 262.0522919454450630 ) ) ;
#85295 = ORIENTED_EDGE ( 'NONE', *, *, #87467, .T. ) ;
#85296 = PLANE ( 'NONE',  #84454 ) ;
#85297 = EDGE_CURVE ( 'NONE', #34907, #52360, #19684, .T. ) ;
#85298 = EDGE_CURVE ( 'NONE', #42989, #10845, #13322, .T. ) ;
#85299 = CIRCLE ( 'NONE', #83870, 10.00000000000002487 ) ;
#85300 = EDGE_LOOP ( 'NONE', ( #88109, #46409, #80281, #49611 ) ) ;
#85301 = CARTESIAN_POINT ( 'NONE',  ( 50.97905606905900555, -31.62489322948711035, -5.074374724088000832 ) ) ;
#85302 = CARTESIAN_POINT ( 'NONE',  ( -98.14560000000000173, 117.4749999999999943, -1.080832317973422076E-12 ) ) ;
#85303 = EDGE_LOOP ( 'NONE', ( #26545, #40827, #23521, #14124 ) ) ;
#85304 = ADVANCED_FACE ( 'NONE', ( #89633 ), #76433, .T. ) ;
#85305 = CARTESIAN_POINT ( 'NONE',  ( 67.35192090801830034, 120.6499999999999915, 78.57724105935551506 ) ) ;
#85306 = AXIS2_PLACEMENT_3D ( 'NONE', #52318, #58278, #36512 ) ;
#85307 = DIRECTION ( 'NONE',  ( 0.000000000000000000, 1.000000000000000000, 0.000000000000000000 ) ) ;
#85308 = CARTESIAN_POINT ( 'NONE',  ( 101.0660769631361688, -27.44644056990073366, 70.54514908543497143 ) ) ;
#85309 = CARTESIAN_POINT ( 'NONE',  ( 107.0664832912739399, -36.72944715994096754, 298.1356252759109680 ) ) ;
#85310 = EDGE_CURVE ( 'NONE', #51322, #9402, #7397, .T. ) ;
#85311 = FACE_BOUND ( 'NONE', #63128, .T. ) ;
#85312 = DIRECTION ( 'NONE',  ( 1.000000000000000000, 0.000000000000000000, 0.000000000000000000 ) ) ;
#85313 = CARTESIAN_POINT ( 'NONE',  ( 117.2535196871930481, -41.18324016912744412, 58.49848241876892985 ) ) ;
#85315 = CARTESIAN_POINT ( 'NONE',  ( 98.10941331148548272, -42.08998169807667722, 157.7556252759109725 ) ) ;
#85314 = CARTESIAN_POINT ( 'NONE',  ( 113.2454051795150463, -28.75859548762567641, 109.5523015492156986 ) ) ;
#85316 = FACE_BOUND ( 'NONE', #9091, .T. ) ;
#85317 = CYLINDRICAL_SURFACE ( 'NONE', #45240, 27.99999999999999645 ) ;
#85318 = ORIENTED_EDGE ( 'NONE', *, *, #88146, .T. ) ;
#85319 = DIRECTION ( 'NONE',  ( -4.237773401492740281E-14, 1.000000000000000000, 0.000000000000000000 ) ) ;
#85320 = CARTESIAN_POINT ( 'NONE',  ( 74.06670390244701707, -90.27844715994098124, 51.21780685541800437 ) ) ;
#85321 = ORIENTED_EDGE ( 'NONE', *, *, #48140, .T. ) ;
#85322 = EDGE_CURVE ( 'NONE', #89449, #65816, #27386, .T. ) ;
#85323 = VECTOR ( 'NONE', #4058, 1000.000000000000000 ) ;
#85324 = CARTESIAN_POINT ( 'NONE',  ( 59.67078992371374113, -0.9290567490904538817, 542.9756252759101471 ) ) ;
#85326 = ORIENTED_EDGE ( 'NONE', *, *, #51911, .T. ) ;
#85325 = CARTESIAN_POINT ( 'NONE',  ( 102.2167607299587928, -46.00774749580600798, 212.1927681330539599 ) ) ;
#85327 = CARTESIAN_POINT ( 'NONE',  ( 80.06648329127402519, -36.72944715994107412, -5.074374724089057764 ) ) ;
#85328 = CARTESIAN_POINT ( 'NONE',  ( 115.3407290770031324, -45.24761053976980918, 264.1899109901965517 ) ) ;
#85329 = CARTESIAN_POINT ( 'NONE',  ( 117.9205228141932054, -39.05050820906062370, 104.6708633711489824 ) ) ;
#85330 = AXIS2_PLACEMENT_3D ( 'NONE', #50820, #30383, #9488 ) ;
#85331 = DIRECTION ( 'NONE',  ( 0.000000000000000000, 0.000000000000000000, 1.000000000000000000 ) ) ;
#85332 = VECTOR ( 'NONE', #55432, 1000.000000000000000 ) ;
#85333 = LINE ( 'NONE', #30784, #32920 ) ;
#85334 = EDGE_CURVE ( 'NONE', #36762, #81089, #55065, .T. ) ;
#85335 = CARTESIAN_POINT ( 'NONE',  ( 34.96670390244661775, -28.27351298637442056, 117.4678068554150485 ) ) ;
#85336 = ORIENTED_EDGE ( 'NONE', *, *, #59782, .F. ) ;
#85337 = CIRCLE ( 'NONE', #34520, 1.000000000000000888 ) ;
#85338 = ORIENTED_EDGE ( 'NONE', *, *, #30857, .F. ) ;
#85339 = ORIENTED_EDGE ( 'NONE', *, *, #48140, .F. ) ;
#85340 = AXIS2_PLACEMENT_3D ( 'NONE', #34081, #61785, #27280 ) ;
#85341 = ORIENTED_EDGE ( 'NONE', *, *, #50817, .T. ) ;
#85342 = FACE_OUTER_BOUND ( 'NONE', #65922, .T. ) ;
#85343 = CARTESIAN_POINT ( 'NONE',  ( 118.5467753794658705, -33.90456151647279626, 10.01848241876795953 ) ) ;
#85344 = DIRECTION ( 'NONE',  ( 0.000000000000000000, 0.000000000000000000, -1.000000000000000000 ) ) ;
#85345 = CARTESIAN_POINT ( 'NONE',  ( 3.968749999999215294, 127.0000000000000000, 105.4788588808464027 ) ) ;
#85346 = EDGE_CURVE ( 'NONE', #88226, #52020, #61875, .T. ) ;
#85349 = ADVANCED_FACE ( 'NONE', ( #78705, #15571, #8758, #23297, #9635, #79142, #30530, #57779 ), #78257, .T. ) ;
#85348 = CARTESIAN_POINT ( 'NONE',  ( 107.0667039024470313, -104.2784471599413934, 2.217806855418003043 ) ) ;
#85347 = CARTESIAN_POINT ( 'NONE',  ( 194.5664832912739826, 0.2215528400590013880, -5.074374724088000832 ) ) ;
#85350 = LINE ( 'NONE', #51671, #3665 ) ;
#85351 = VECTOR ( 'NONE', #88717, 999.9999999999998863 ) ;
#85352 = CARTESIAN_POINT ( 'NONE',  ( 116.6718245901296171, -38.14650263757180682, 223.1324198280769622 ) ) ;
#85353 = ORIENTED_EDGE ( 'NONE', *, *, #66546, .T. ) ;
#85354 = ORIENTED_EDGE ( 'NONE', *, *, #7427, .T. ) ;
#85355 = ORIENTED_EDGE ( 'NONE', *, *, #17880, .F. ) ;
#85356 = DIRECTION ( 'NONE',  ( -1.000000000000000000, 0.000000000000000000, 0.000000000000000000 ) ) ;
#85357 = CYLINDRICAL_SURFACE ( 'NONE', #41942, 0.5000000000000031086 ) ;
#85358 = CARTESIAN_POINT ( 'NONE',  ( 105.9660761217308931, -46.48152529548401901, 278.4870538473389843 ) ) ;
#85359 = DIRECTION ( 'NONE',  ( -0.9068632946707807507, 0.4214249218767881500, -9.028300618466658994E-16 ) ) ;
#85360 = CARTESIAN_POINT ( 'NONE',  ( 108.2420053567034017, -46.43931755893575541, 113.6727681330529691 ) ) ;
#85361 = CARTESIAN_POINT ( 'NONE',  ( 117.0606848385255319, -38.08193180985016113, 28.71884086846101525 ) ) ;
#85362 = EDGE_LOOP ( 'NONE', ( #61955, #71304 ) ) ;
#85363 = DIRECTION ( 'NONE',  ( 0.000000000000000000, -1.000000000000000000, 0.000000000000000000 ) ) ;
#85364 = CARTESIAN_POINT ( 'NONE',  ( -479.3614999999999782, 89.53805401447711176, 3.968750000000410338 ) ) ;
#85365 = ORIENTED_EDGE ( 'NONE', *, *, #35440, .T. ) ;
#85366 = DIRECTION ( 'NONE',  ( 0.000000000000000000, 0.000000000000000000, 1.000000000000000000 ) ) ;
#85367 = CARTESIAN_POINT ( 'NONE',  ( 114.1852310984691883, -41.65497984893937655, 11.17475703625792072 ) ) ;
#85368 = ADVANCED_FACE ( 'NONE', ( #70529 ), #36457, .F. ) ;
#85369 = CIRCLE ( 'NONE', #83879, 3.000000000000002665 ) ;
#85370 = AXIS2_PLACEMENT_3D ( 'NONE', #50777, #63972, #65735 ) ;
#85371 = LINE ( 'NONE', #3559, #26133 ) ;
#85372 = LINE ( 'NONE', #58515, #46103 ) ;
#85373 = CARTESIAN_POINT ( 'NONE',  ( 117.0719183210286900, -35.46267133667483762, 194.9273074894743729 ) ) ;
#85374 = ORIENTED_EDGE ( 'NONE', *, *, #48325, .F. ) ;
#85375 = CARTESIAN_POINT ( 'NONE',  ( 0.000000000000000000, 114.2999999999999972, 0.000000000000000000 ) ) ;
#85376 = AXIS2_PLACEMENT_3D ( 'NONE', #54702, #6586, #5246 ) ;
#85377 = DIRECTION ( 'NONE',  ( -0.9068632946707805287, 0.4214249218767882610, -9.061988307341536250E-16 ) ) ;
#85378 = ORIENTED_EDGE ( 'NONE', *, *, #15953, .F. ) ;
#85379 = CARTESIAN_POINT ( 'NONE',  ( 116.2317802277880787, -31.76111116818806224, 69.22133956162495849 ) ) ;
#85380 = ORIENTED_EDGE ( 'NONE', *, *, #19511, .T. ) ;
#85381 = CARTESIAN_POINT ( 'NONE',  ( 109.1520131464112069, -27.24676858702523674, 29.32670554236194249 ) ) ;
#85382 = AXIS2_PLACEMENT_3D ( 'NONE', #72922, #30703, #65227 ) ;
#85383 = DIRECTION ( 'NONE',  ( 0.000000000000000000, 0.000000000000000000, -1.000000000000000000 ) ) ;
#85384 = CARTESIAN_POINT ( 'NONE',  ( 116.7742277529940225, -35.53649587948895316, 193.9241967044829664 ) ) ;
#85385 = CARTESIAN_POINT ( 'NONE',  ( 128.0667039024480118, -50.82844715994100682, 198.9178068554149945 ) ) ;
#85386 = CARTESIAN_POINT ( 'NONE',  ( 180.2121375201600131, -29.73316016639650172, 193.9678068554150059 ) ) ;
#85387 = AXIS2_PLACEMENT_3D ( 'NONE', #54422, #26303, #75355 ) ;
#85388 = CARTESIAN_POINT ( 'NONE',  ( 61.00843881761244347, 65.60000000000000853, 0.000000000000000000 ) ) ;
#85389 = ADVANCED_FACE ( 'NONE', ( #64164 ), #77791, .F. ) ;
#85390 = CARTESIAN_POINT ( 'NONE',  ( 105.0131270392176646, -25.82159629633810738, 276.2365776568634033 ) ) ;
#85391 = DIRECTION ( 'NONE',  ( 0.000000000000000000, 0.000000000000000000, 1.000000000000000000 ) ) ;
#85392 = EDGE_LOOP ( 'NONE', ( #50042, #48066, #87975, #1694, #64962 ) ) ;
#85393 = CYLINDRICAL_SURFACE ( 'NONE', #56005, 2.030000000002079918 ) ;
#85394 = EDGE_LOOP ( 'NONE', ( #29739, #37360, #45071, #38842 ) ) ;
#85395 = CARTESIAN_POINT ( 'NONE',  ( 102.2928874563330055, -26.70895414482565045, 136.4422919425779526 ) ) ;
#85396 = DIRECTION ( 'NONE',  ( 0.000000000000000000, 0.000000000000000000, 1.000000000000000000 ) ) ;
#85397 = EDGE_LOOP ( 'NONE', ( #84956, #55803, #50672, #62202 ) ) ;
#85399 = EDGE_CURVE ( 'NONE', #41571, #82149, #38664, .T. ) ;
#85398 = VERTEX_POINT ( 'NONE', #43243 ) ;
#85401 = VERTEX_POINT ( 'NONE', #16454 ) ;
#85400 = EDGE_CURVE ( 'NONE', #76254, #1241, #2831, .T. ) ;
#85402 = VECTOR ( 'NONE', #47149, 1000.000000000000000 ) ;
#85403 = CARTESIAN_POINT ( 'NONE',  ( 112.0659115482700088, -45.48839630408555479, 122.9897919358033249 ) ) ;
#85404 = ADVANCED_FACE ( 'NONE', ( #29194 ), #23730, .F. ) ;
#85405 = CARTESIAN_POINT ( 'NONE',  ( 107.0664832912739968, -36.72944715994100306, 249.5838068554170093 ) ) ;
#85406 = CARTESIAN_POINT ( 'NONE',  ( 112.6571330189593141, -45.46348522128867131, 218.0175300378159591 ) ) ;
#85407 = LINE ( 'NONE', #2718, #3716 ) ;
#85408 = DIRECTION ( 'NONE',  ( 0.000000000000000000, 0.000000000000000000, 1.000000000000000000 ) ) ;
#85409 = DIRECTION ( 'NONE',  ( 0.000000000000000000, 1.000000000000000000, 0.000000000000000000 ) ) ;
#85410 = CARTESIAN_POINT ( 'NONE',  ( 102.7553090513238487, -25.69095112480093945, 16.37276813305293999 ) ) ;
#85411 = DIRECTION ( 'NONE',  ( 1.000000000000000000, -5.337610695313248426E-16, 0.000000000000000000 ) ) ;
#85412 = VERTEX_POINT ( 'NONE', #16905 ) ;
#85413 = SURFACE_STYLE_USAGE ( .BOTH. , #57669 ) ;
#85414 = CIRCLE ( 'NONE', #46188, 0.5000000000000004441 ) ;
#85415 = DIRECTION ( 'NONE',  ( 0.000000000000000000, 0.000000000000000000, -1.000000000000000000 ) ) ;
#85417 = ORIENTED_EDGE ( 'NONE', *, *, #61376, .F. ) ;
#85416 = VECTOR ( 'NONE', #25329, 1000.000000000000000 ) ;
#85418 = ADVANCED_FACE ( 'NONE', ( #29631 ), #85067, .F. ) ;
#85419 = DIRECTION ( 'NONE',  ( 0.000000000000000000, 0.000000000000000000, -1.000000000000000000 ) ) ;
#85420 = PLANE ( 'NONE',  #15055 ) ;
#85421 = CARTESIAN_POINT ( 'NONE',  ( 114.9613132280022683, -29.02649429439048134, 194.4537205140059370 ) ) ;
#85422 = LINE ( 'NONE', #16356, #843 ) ;
#85423 = DIRECTION ( 'NONE',  ( 0.000000000000000000, 0.000000000000000000, -1.000000000000000000 ) ) ;
#85424 = DIRECTION ( 'NONE',  ( 0.000000000000000000, 0.000000000000000000, -1.000000000000000000 ) ) ;
#85425 = EDGE_CURVE ( 'NONE', #42008, #68551, #82211, .T. ) ;
#85426 = CARTESIAN_POINT ( 'NONE',  ( 106.8904373410712481, -45.78382058659838094, 226.9714674471249509 ) ) ;
#85428 = CARTESIAN_POINT ( 'NONE',  ( 112.8057071037347185, -27.31004523576153886, 45.62895860924398761 ) ) ;
#85427 = FACE_OUTER_BOUND ( 'NONE', #82369, .T. ) ;
#85429 = CARTESIAN_POINT ( 'NONE',  ( 123.6120034158685286, 72.65141698275766657, 42.01243221415964513 ) ) ;
#85430 = CARTESIAN_POINT ( 'NONE',  ( 116.6387536407295329, -29.65834838561569242, 109.3327681330539605 ) ) ;
#85431 = ORIENTED_EDGE ( 'NONE', *, *, #11010, .F. ) ;
#85432 = CARTESIAN_POINT ( 'NONE',  ( 131.5922609085388331, -19.93375462384614494, 7.110117206084406227 ) ) ;
#85433 = ORIENTED_EDGE ( 'NONE', *, *, #5030, .F. ) ;
#85434 = CARTESIAN_POINT ( 'NONE',  ( 180.2121375201587625, -29.73316016638863957, 117.4678068554150627 ) ) ;
#85435 = CARTESIAN_POINT ( 'NONE',  ( 115.1492182743862998, -30.73465633580296341, 275.3339211662992625 ) ) ;
#85436 = ORIENTED_EDGE ( 'NONE', *, *, #75931, .F. ) ;
#85437 = EDGE_CURVE ( 'NONE', #19677, #37178, #18375, .T. ) ;
#85438 = CARTESIAN_POINT ( 'NONE',  ( 115.0888839854113002, -30.61760552574517646, 49.34396152961115689 ) ) ;
#85439 = VERTEX_POINT ( 'NONE', #50514 ) ;
#85440 = CYLINDRICAL_SURFACE ( 'NONE', #76, 4.762500000000000178 ) ;
#85441 = FACE_OUTER_BOUND ( 'NONE', #18802, .T. ) ;
#85443 = DIRECTION ( 'NONE',  ( 3.100000000000000258E-29, -3.100000000000000044E-14, -1.000000000000000000 ) ) ;
#85442 = CIRCLE ( 'NONE', #38966, 0.5000000000000004441 ) ;
#85444 = ORIENTED_EDGE ( 'NONE', *, *, #27551, .F. ) ;
#85445 = VECTOR ( 'NONE', #46890, 1000.000000000000000 ) ;
#85446 = CARTESIAN_POINT ( 'NONE',  ( 113.3280054804099137, -28.32220607287434078, 104.5670538473399347 ) ) ;
#85447 = DIRECTION ( 'NONE',  ( 0.000000000000000000, 0.000000000000000000, 1.000000000000000000 ) ) ;
#85448 = CARTESIAN_POINT ( 'NONE',  ( 76.20505178924389611, 120.6499999999999915, -76.20505178924359768 ) ) ;
#85449 = DIRECTION ( 'NONE',  ( 0.000000000000000000, 0.000000000000000000, 1.000000000000000000 ) ) ;
#85450 = FACE_OUTER_BOUND ( 'NONE', #52860, .T. ) ;
#85451 = VERTEX_POINT ( 'NONE', #84620 ) ;
#85452 = CARTESIAN_POINT ( 'NONE',  ( 25.56670390244797275, -62.87844715994099687, 293.2178068554150627 ) ) ;
#85453 = CYLINDRICAL_SURFACE ( 'NONE', #46872, 5.599999999999994316 ) ;
#85454 = VECTOR ( 'NONE', #66213, 1000.000000000000000 ) ;
#85455 = DIRECTION ( 'NONE',  ( 0.000000000000000000, 0.000000000000000000, 1.000000000000000000 ) ) ;
#85458 = ADVANCED_FACE ( 'NONE', ( #42786 ), #22377, .T. ) ;
#85457 = DIRECTION ( 'NONE',  ( 0.000000000000000000, -1.000000000000000000, 0.000000000000000000 ) ) ;
#85456 = CARTESIAN_POINT ( 'NONE',  ( 179.4595971212738164, -26.00627455218718254, 237.4678068554150059 ) ) ;
#85459 = CYLINDRICAL_SURFACE ( 'NONE', #27721, 3.814291549405317117 ) ;
#85460 = ORIENTED_EDGE ( 'NONE', *, *, #9319, .T. ) ;
#85461 = LINE ( 'NONE', #64104, #50577 ) ;
#85462 = CARTESIAN_POINT ( 'NONE',  ( 102.2868918306628387, -45.93239726994502803, 163.1832443235289816 ) ) ;
#85463 = AXIS2_PLACEMENT_3D ( 'NONE', #9542, #85861, #1839 ) ;
#85465 = ORIENTED_EDGE ( 'NONE', *, *, #57696, .F. ) ;
#85464 = CARTESIAN_POINT ( 'NONE',  ( 9.749037034254362410, 224.4999999999999432, 152.4294779587682740 ) ) ;
#85466 = CARTESIAN_POINT ( 'NONE',  ( 116.8666056714781973, -37.25052799200011577, 14.78419670448194445 ) ) ;
#85467 = FACE_OUTER_BOUND ( 'NONE', #23338, .T. ) ;
#85468 = LINE ( 'NONE', #86342, #29855 ) ;
#85469 = CARTESIAN_POINT ( 'NONE',  ( 115.0352726211783079, -42.91098005955615236, 13.30258960125530798 ) ) ;
#85470 = EDGE_CURVE ( 'NONE', #46563, #57647, #83630, .T. ) ;
#85471 = CARTESIAN_POINT ( 'NONE',  ( 113.2466805891969415, -28.75957719968114290, 29.55240580932557393 ) ) ;
#85472 = CARTESIAN_POINT ( 'NONE',  ( 98.59486473514172644, -43.92970144294059054, 226.8870538473399563 ) ) ;
#85473 = ORIENTED_EDGE ( 'NONE', *, *, #70513, .T. ) ;
#85474 = ORIENTED_EDGE ( 'NONE', *, *, #54497, .F. ) ;
#85475 = CIRCLE ( 'NONE', #81129, 1.000000000000000888 ) ;
#85476 = CARTESIAN_POINT ( 'NONE',  ( 99.15781305739687923, -40.79332027783682690, 193.1358690201829518 ) ) ;
#85477 = EDGE_CURVE ( 'NONE', #2816, #7755, #84168, .T. ) ;
#85478 = LINE ( 'NONE', #51794, #85049 ) ;
#85479 = CARTESIAN_POINT ( 'NONE',  ( 113.6566823882007355, -42.65376606380868196, 34.67586902018199169 ) ) ;
#85480 = CARTESIAN_POINT ( 'NONE',  ( -98.05663017059038111, 92.12504059357192432, 86.19814306825486483 ) ) ;
#85481 = FACE_OUTER_BOUND ( 'NONE', #15893, .T. ) ;
#85482 = LINE ( 'NONE', #78671, #12534 ) ;
#85483 = VERTEX_POINT ( 'NONE', #36894 ) ;
#85484 = CARTESIAN_POINT ( 'NONE',  ( 165.6738106836199904, -26.00627455219321860, 117.4678068554150485 ) ) ;
#85485 = DIRECTION ( 'NONE',  ( -0.000000000000000000, 1.000000000000000000, -0.000000000000000000 ) ) ;
#85486 = CARTESIAN_POINT ( 'NONE',  ( 96.99990081654250673, -39.35482002063354656, 276.5299109901967540 ) ) ;
#85487 = DIRECTION ( 'NONE',  ( 0.000000000000000000, 0.000000000000000000, -1.000000000000000000 ) ) ;
#85488 = ORIENTED_EDGE ( 'NONE', *, *, #73052, .T. ) ;
#85489 = VERTEX_POINT ( 'NONE', #2384 ) ;
#85490 = VECTOR ( 'NONE', #75474, 1000.000000000000000 ) ;
#85491 = CARTESIAN_POINT ( 'NONE',  ( 41.56670390244783420, -36.32844715994104234, 249.9678068554150343 ) ) ;
#85492 = CARTESIAN_POINT ( 'NONE',  ( 49.16670390244701139, -28.27351298637340093, -5.074374724088000832 ) ) ;
#85493 = DIRECTION ( 'NONE',  ( -7.559289460184346452E-16, 0.7559289460184345222, -0.6546536707080001793 ) ) ;
#85494 = DIRECTION ( 'NONE',  ( 0.000000000000000000, -1.000000000000000000, 0.000000000000000000 ) ) ;
#85495 = CARTESIAN_POINT ( 'NONE',  ( 104.4155842969358332, -46.14412564300911157, 18.35848241876792031 ) ) ;
#85497 = DIRECTION ( 'NONE',  ( 0.1858654558203195195, -0.9825752044157765042, 0.000000000000000000 ) ) ;
#85496 = AXIS2_PLACEMENT_3D ( 'NONE', #46751, #54003, #75824 ) ;
#85498 = AXIS2_PLACEMENT_3D ( 'NONE', #5029, #31381, #33181 ) ;
#85499 = ORIENTED_EDGE ( 'NONE', *, *, #26338, .F. ) ;
#85500 = CARTESIAN_POINT ( 'NONE',  ( 109.6537587170975030, -46.87336088289573865, 43.77562527591094721 ) ) ;
#85501 = DIRECTION ( 'NONE',  ( 1.000000000000000000, -0.000000000000000000, 0.000000000000000000 ) ) ;
#85502 = CARTESIAN_POINT ( 'NONE',  ( 96.53679867426635042, -40.09171982297686299, 281.5603871806728762 ) ) ;
#85504 = EDGE_LOOP ( 'NONE', ( #63348, #55188, #25241, #43009 ) ) ;
#85503 = EDGE_CURVE ( 'NONE', #10350, #2727, #30085, .T. ) ;
#85505 = B_SPLINE_CURVE_WITH_KNOTS ( 'NONE', 3,
 ( #85125, #52321, #30138, #51449, #16074, #16512, #79200, #71925, #9690, #43753, #16957, #65101, #22892, #72809, #72371, #9252, #10139, #80086, #3328, #79641, #64219, #45082, #31022, #29688, #38281, #36515, #65977, #1989, #50568, #64653, #45965, #40516, #52762, #11926, #26888, #39175, #68237, #32803, #54119, #54561, #67319, #5567, #87337, #88245, #12832, #40060, #66425, #19626, #53217, #6020, #73238 ),
 .UNSPECIFIED., .F., .F.,
 ( 4, 2, 1, 1, 1, 1, 1, 1, 2, 2, 2, 2, 2, 2, 2, 1, 1, 1, 1, 1, 1, 1, 2, 2, 2, 2, 2, 2, 2, 2, 2, 4 ),
 ( 0.5000151712595112263, 0.5001372378680968289, 0.5002593044766825425, 0.5005034376938537477, 0.5009917041281959360, 0.5019682369968807567, 0.5039213027342506201, 0.5078274342089901250, 0.5156396971584693567, 0.5312642230574272650, 0.5625132748553431927, 0.6250113784511752701, 0.6875094820470073476, 0.7500075856428394250, 0.7500686189471321708, 0.7501296522514248055, 0.7502517188599931997, 0.7504958520771425334, 0.7509841185114412010, 0.7519606513800297654, 0.7539137171171848006, 0.7578198485915111915, 0.7656321115401695243, 0.7812566374374917411, 0.8125056892321357305, 0.8437547410267797199, 0.8750037928214238203, 0.9062528446160678097, 0.9375018964107117991, 0.9687509482053557885, 0.9843754741026778943, 1.000000000000000000 ),
 .UNSPECIFIED. ) ;
#85506 = AXIS2_PLACEMENT_3D ( 'NONE', #36446, #42329, #64150 ) ;
#85507 = EDGE_CURVE ( 'NONE', #7119, #60401, #37264, .T. ) ;
#85508 = CARTESIAN_POINT ( 'NONE',  ( 79.68962695805252849, -39.47945062089030444, 8.225625248534937484 ) ) ;
#85509 = DIRECTION ( 'NONE',  ( 1.000000000000000078E-15, -1.000000000000000083E-30, -1.000000000000000000 ) ) ;
#85510 = DIRECTION ( 'NONE',  ( 0.000000000000000000, 1.000000000000000000, 0.000000000000000000 ) ) ;
#85511 = CARTESIAN_POINT ( 'NONE',  ( 102.8475555715194361, -29.17288882023929730, 103.3118998934009767 ) ) ;
#85512 = CARTESIAN_POINT ( 'NONE',  ( 103.8129894719335624, -48.15035030529833904, 213.3556252759109668 ) ) ;
#85513 = DIRECTION ( 'NONE',  ( 0.000000000000000000, 1.000000000000000000, 0.000000000000000000 ) ) ;
#85514 = VERTEX_POINT ( 'NONE', #65924 ) ;
#85515 = EDGE_CURVE ( 'NONE', #231, #87802, #66369, .T. ) ;
#85516 = AXIS2_PLACEMENT_3D ( 'NONE', #23433, #37487, #24743 ) ;
#85517 = CARTESIAN_POINT ( 'NONE',  ( -24.79284581386642827, 184.0000000000000000, 90.32146847885337593 ) ) ;
#85518 = ORIENTED_EDGE ( 'NONE', *, *, #20034, .T. ) ;
#85519 = ORIENTED_EDGE ( 'NONE', *, *, #55926, .T. ) ;
#85520 = ADVANCED_FACE ( 'NONE', ( #52269 ), #10964, .F. ) ;
#85521 = DIRECTION ( 'NONE',  ( 0.000000000000000000, 1.000000000000000000, 0.000000000000000000 ) ) ;
#85522 = ORIENTED_EDGE ( 'NONE', *, *, #6776, .F. ) ;
#85523 = EDGE_LOOP ( 'NONE', ( #42917, #60092, #49411, #15177 ) ) ;
#85524 = CYLINDRICAL_SURFACE ( 'NONE', #83151, 2.117000000000007987 ) ;
#85525 = CARTESIAN_POINT ( 'NONE',  ( 103.6639831185296288, -27.32465593432968021, 41.35270917185196993 ) ) ;
#85526 = EDGE_CURVE ( 'NONE', #11027, #58704, #3866, .T. ) ;
#85527 = VECTOR ( 'NONE', #3500, 1000.000000000000000 ) ;
#85528 = CARTESIAN_POINT ( 'NONE',  ( 108.0580239150950774, -28.21657753114420331, 129.4067055423629711 ) ) ;
#85529 = CARTESIAN_POINT ( 'NONE',  ( 106.2251211966456879, -47.77424462129209815, 267.5280062282920994 ) ) ;
#85530 = CARTESIAN_POINT ( 'NONE',  ( 97.81670390244700286, -67.87844715994096134, 55.21780685541800437 ) ) ;
#85531 = EDGE_LOOP ( 'NONE', ( #43164, #65149, #39652, #21596 ) ) ;
#85532 = EDGE_LOOP ( 'NONE', ( #73455, #84603 ) ) ;
#85533 = DIRECTION ( 'NONE',  ( -0.000000000000000000, -0.000000000000000000, -1.000000000000000000 ) ) ;
#85534 = CARTESIAN_POINT ( 'NONE',  ( 90.44969454456408187, -56.64645651782490177, 239.5838068554174356 ) ) ;
#85535 = DIRECTION ( 'NONE',  ( -1.000000000000000000, 0.000000000000000000, -2.108231265501709878E-16 ) ) ;
#85536 = CARTESIAN_POINT ( 'NONE',  ( 111.7936012040045597, -46.77578388097458628, 287.9146728949587555 ) ) ;
#85537 = ORIENTED_EDGE ( 'NONE', *, *, #45195, .T. ) ;
#85538 = CARTESIAN_POINT ( 'NONE',  ( 110.8926993666852496, -26.99363814275770679, 269.7784824187681920 ) ) ;
#85539 = CARTESIAN_POINT ( 'NONE',  ( 112.1383799374394670, -26.85658479980368440, 15.71086337114896381 ) ) ;
#85540 = DIRECTION ( 'NONE',  ( 1.000000000000000078E-15, 0.000000000000000000, -1.000000000000000000 ) ) ;
#85542 = PLANE ( 'NONE',  #84865 ) ;
#85541 = DIRECTION ( 'NONE',  ( 0.000000000000000000, 0.000000000000000000, -1.000000000000000000 ) ) ;
#85543 = CARTESIAN_POINT ( 'NONE',  ( 83.06670390244796920, -64.87844715994098976, 207.5838068554149913 ) ) ;
#85544 = CARTESIAN_POINT ( 'NONE',  ( 73.06670390244801183, -58.35344715994099829, 10.91780685541479734 ) ) ;
#85545 = CARTESIAN_POINT ( 'NONE',  ( 188.5667039024479834, -58.35344715994099829, 173.2178068554149775 ) ) ;
#85546 = AXIS2_PLACEMENT_3D ( 'NONE', #73252, #38293, #65561 ) ;
#85547 = CARTESIAN_POINT ( 'NONE',  ( 100.9546727792195639, -28.70702575126005485, 11.59395861232007263 ) ) ;
#85548 = DIRECTION ( 'NONE',  ( 0.000000000000000000, 0.000000000000000000, -1.000000000000000000 ) ) ;
#85549 = CARTESIAN_POINT ( 'NONE',  ( 188.5667039024479834, -58.35344715994099829, 257.2178068554150059 ) ) ;
#85550 = VECTOR ( 'NONE', #62058, 1000.000000000000000 ) ;
#85551 = DIRECTION ( 'NONE',  ( -1.000000000000000000, 0.000000000000000000, 0.000000000000000000 ) ) ;
#85552 = CARTESIAN_POINT ( 'NONE',  ( 117.5565198162756104, -37.28721152219886648, 18.78419670448294809 ) ) ;
#85553 = CARTESIAN_POINT ( 'NONE',  ( 107.5657681238088941, -47.77139876010166830, 188.6003871806729535 ) ) ;
#85554 = CARTESIAN_POINT ( 'NONE',  ( 116.7472758669860013, -31.34730438484761805, 25.24229194257798881 ) ) ;
#85557 = ADVANCED_FACE ( 'NONE', ( #17786 ), #19134, .F. ) ;
#85556 = CARTESIAN_POINT ( 'NONE',  ( 71.25416588882602298, -72.55705569728901594, 542.9756252759101471 ) ) ;
#85555 = DIRECTION ( 'NONE',  ( 0.9068632946707807507, -0.4214249218767880945, 9.080193194566099635E-16 ) ) ;
#85558 = CARTESIAN_POINT ( 'NONE',  ( 81.91153210827047815, -34.68812259376856133, 2.188418746634181122 ) ) ;
#85559 = AXIS2_PLACEMENT_3D ( 'NONE', #73284, #52364, #2924 ) ;
#85560 = EDGE_CURVE ( 'NONE', #57775, #77970, #39120, .T. ) ;
#85561 = ORIENTED_EDGE ( 'NONE', *, *, #14742, .F. ) ;
#85562 = CARTESIAN_POINT ( 'NONE',  ( 107.0664832912739968, -18.82844715994099971, 168.9256252759119832 ) ) ;
#85563 = ORIENTED_EDGE ( 'NONE', *, *, #73947, .T. ) ;
#85564 = CARTESIAN_POINT ( 'NONE',  ( 97.89279369561094768, -33.33727167892453735, 62.04419670448196911 ) ) ;
#85565 = VECTOR ( 'NONE', #10183, 1000.000000000000000 ) ;
#85567 = ORIENTED_EDGE ( 'NONE', *, *, #39819, .T. ) ;
#85566 = CARTESIAN_POINT ( 'NONE',  ( -48.02966122971776741, 93.07500000000001705, 75.53254848357481421 ) ) ;
#85568 = CARTESIAN_POINT ( 'NONE',  ( 115.0368097993288785, -42.90903055077831141, 49.30223481898713089 ) ) ;
#85569 = CARTESIAN_POINT ( 'NONE',  ( 114.1099639442525699, -29.07320488188167218, 195.4841967044819739 ) ) ;
#85570 = DIRECTION ( 'NONE',  ( 1.000000000000000000, 4.163336342344333240E-14, 0.000000000000000000 ) ) ;
#85571 = DIRECTION ( 'NONE',  ( 0.000000000000000000, 0.000000000000000000, 1.000000000000000000 ) ) ;
#85572 = AXIS2_PLACEMENT_3D ( 'NONE', #44954, #65420, #16384 ) ;
#85573 = CARTESIAN_POINT ( 'NONE',  ( 98.35000460789950694, -31.65632374290893480, 150.9069170840674872 ) ) ;
#85574 = CARTESIAN_POINT ( 'NONE',  ( 1.387778780781445676E-14, 239.0000000000000000, 82.77542076772560620 ) ) ;
#85575 = CARTESIAN_POINT ( 'NONE',  ( 145.1732792321600698, -139.1256337189776389, 247.0684060528939767 ) ) ;
#85576 = CARTESIAN_POINT ( 'NONE',  ( 110.8610854611956995, -45.98152856190351656, 97.88619379672280729 ) ) ;
#85577 = CIRCLE ( 'NONE', #86990, 0.1499999999999965528 ) ;
#85578 = CARTESIAN_POINT ( 'NONE',  ( 102.6065612795739952, -27.36740250608067626, 140.4422919425779526 ) ) ;
#85579 = ORIENTED_EDGE ( 'NONE', *, *, #5802, .F. ) ;
#85580 = EDGE_LOOP ( 'NONE', ( #78858, #33525, #14334, #76488 ) ) ;
#85581 = CARTESIAN_POINT ( 'NONE',  ( 108.6974651445452764, -45.43968118700122005, 79.15586902018296200 ) ) ;
#85582 = EDGE_CURVE ( 'NONE', #1745, #79206, #45466, .T. ) ;
#85583 = LINE ( 'NONE', #71936, #9486 ) ;
#85585 = PLANE ( 'NONE',  #51997 ) ;
#85584 = CARTESIAN_POINT ( 'NONE',  ( 116.8310051202517457, -36.16593252570071115, 224.8727681330539667 ) ) ;
#85586 = CARTESIAN_POINT ( 'NONE',  ( 68.86456684384336313, 93.07500000000001705, 56.22171674193015889 ) ) ;
#85587 = CARTESIAN_POINT ( 'NONE',  ( 131.0667039024480118, -61.87844715994100397, 207.5838068554149913 ) ) ;
#85588 = VECTOR ( 'NONE', #32092, 1000.000000000000000 ) ;
#85589 = CARTESIAN_POINT ( 'NONE',  ( 182.2300522401149863, -33.89581943344511217, -5.074374724088000832 ) ) ;
#85590 = CARTESIAN_POINT ( 'NONE',  ( 248.6659999999999968, 52.73749999999999716, -10.97647784993501396 ) ) ;
#85591 = CARTESIAN_POINT ( 'NONE',  ( 11.93751238659888614, 78.49696472779160672, 117.9535311651797684 ) ) ;
#85592 = CARTESIAN_POINT ( 'NONE',  ( 117.7782040715257921, -34.09831434418944696, 164.0061014663869798 ) ) ;
#85593 = ORIENTED_EDGE ( 'NONE', *, *, #56491, .T. ) ;
#85594 = VERTEX_POINT ( 'NONE', #31855 ) ;
#85595 = ORIENTED_EDGE ( 'NONE', *, *, #47527, .F. ) ;
#85596 = CARTESIAN_POINT ( 'NONE',  ( 131.1848578969771211, -79.26006987685342153, 249.3134381260879877 ) ) ;
#85597 = CARTESIAN_POINT ( 'NONE',  ( 77.33253968407630907, -18.38436945696972202, 3.076560175368437733 ) ) ;
#85598 = DIRECTION ( 'NONE',  ( 0.000000000000000000, 0.000000000000000000, 1.000000000000000000 ) ) ;
#85599 = CARTESIAN_POINT ( 'NONE',  ( 59.67079009362632291, -0.9310397146383332379, 396.9756252759102040 ) ) ;
#85600 = CARTESIAN_POINT ( 'NONE',  ( 111.8846140958497273, -43.31847907419767552, 225.8966617981629668 ) ) ;
#85601 = CARTESIAN_POINT ( 'NONE',  ( 109.6429999896449914, -46.48009007242004031, 268.7814576145019601 ) ) ;
#85602 = CARTESIAN_POINT ( 'NONE',  ( 97.42502596350711030, -42.13512825026991493, 181.7451490854349743 ) ) ;
#85603 = DIRECTION ( 'NONE',  ( 0.000000000000000000, 0.000000000000000000, -1.000000000000000000 ) ) ;
#85604 = ORIENTED_EDGE ( 'NONE', *, *, #44785, .F. ) ;
#85607 = EDGE_LOOP ( 'NONE', ( #56932, #29696, #34604, #117 ) ) ;
#85606 = ORIENTED_EDGE ( 'NONE', *, *, #49003, .T. ) ;
#85605 = ADVANCED_FACE ( 'NONE', ( #66825 ), #24605, .F. ) ;
#85608 = AXIS2_PLACEMENT_3D ( 'NONE', #69481, #62657, #433 ) ;
#85609 = DIRECTION ( 'NONE',  ( 0.000000000000000000, -1.000000000000000000, 0.000000000000000000 ) ) ;
#85610 = ORIENTED_EDGE ( 'NONE', *, *, #57492, .T. ) ;
#85611 = VERTEX_POINT ( 'NONE', #25951 ) ;
#85612 = CARTESIAN_POINT ( 'NONE',  ( 194.0371591254585439, -46.82818131005407736, 116.4678068554150201 ) ) ;
#85613 = EDGE_CURVE ( 'NONE', #53629, #87604, #32752, .T. ) ;
#85614 = CARTESIAN_POINT ( 'NONE',  ( 132.8008218761653723, -34.28157759251718772, 7.978179524060857730 ) ) ;
#85615 = CARTESIAN_POINT ( 'NONE',  ( 110.8184301750971485, -28.11564833443670608, 281.1692023535160843 ) ) ;
#85616 = DIRECTION ( 'NONE',  ( -0.000000000000000000, -0.000000000000000000, -1.000000000000000000 ) ) ;
#85617 = EDGE_LOOP ( 'NONE', ( #82649, #40664, #65014, #41790 ) ) ;
#85618 = ADVANCED_FACE ( 'NONE', ( #38668 ), #60386, .F. ) ;
#85619 = CARTESIAN_POINT ( 'NONE',  ( 114.1502950862027603, -42.12385254268857437, 9.635625275910941312 ) ) ;
#85620 = CARTESIAN_POINT ( 'NONE',  ( -126.9896596436628755, 56.80590851577779432, 30.30816834133878146 ) ) ;
#85621 = ORIENTED_EDGE ( 'NONE', *, *, #39208, .T. ) ;
#85623 = ORIENTED_EDGE ( 'NONE', *, *, #49984, .T. ) ;
#85622 = CIRCLE ( 'NONE', #53659, 13.49999999999999822 ) ;
#85624 = DIRECTION ( 'NONE',  ( 0.000000000000000000, 0.000000000000000000, -1.000000000000000000 ) ) ;
#85625 = VERTEX_POINT ( 'NONE', #65493 ) ;
#85626 = VERTEX_POINT ( 'NONE', #86391 ) ;
#85627 = EDGE_CURVE ( 'NONE', #74649, #19571, #79589, .T. ) ;
#85628 = CARTESIAN_POINT ( 'NONE',  ( 99.46800687602927837, -39.83949638310546248, 11.05813411379097388 ) ) ;
#85629 = VECTOR ( 'NONE', #54161, 1000.000000000000000 ) ;
#85630 = CARTESIAN_POINT ( 'NONE',  ( 117.3133064751534249, -34.51789172102134984, 183.9956252759109532 ) ) ;
#85631 = CARTESIAN_POINT ( 'NONE',  ( 98.29923130492881000, -31.06375673945261440, 145.8699109901969848 ) ) ;
#85632 = EDGE_CURVE ( 'NONE', #34694, #34850, #25493, .T. ) ;
#85633 = CARTESIAN_POINT ( 'NONE',  ( 57.56670390244808289, -42.82844715994040286, 257.2178068554150627 ) ) ;
#85634 = CARTESIAN_POINT ( 'NONE',  ( 117.4906655440605334, -35.85895469176247019, 249.8927681330537780 ) ) ;
#85635 = CARTESIAN_POINT ( 'NONE',  ( 3.968749999999229949, 127.0000000000000000, 100.8961411191535973 ) ) ;
#85636 = CARTESIAN_POINT ( 'NONE',  ( 48.45959712127302055, -26.00627455219131789, 342.9256252759109884 ) ) ;
#85637 = CARTESIAN_POINT ( 'NONE',  ( -130.5559380315088163, 69.85063703626890685, -0.8489233174136696647 ) ) ;
#85638 = EDGE_LOOP ( 'NONE', ( #69056, #40239, #19114, #13672 ) ) ;
#85639 = ORIENTED_EDGE ( 'NONE', *, *, #8692, .F. ) ;
#85640 = AXIS2_PLACEMENT_3D ( 'NONE', #40371, #32207, #88543 ) ;
#85641 = CARTESIAN_POINT ( 'NONE',  ( 113.6419851944692425, -45.67235822675655754, 183.0689586092439640 ) ) ;
#85642 = ORIENTED_EDGE ( 'NONE', *, *, #66090, .F. ) ;
#85643 = CARTESIAN_POINT ( 'NONE',  ( 95.56927879810542947, -39.60255952144336078, 166.5213395616259788 ) ) ;
#85644 = DIRECTION ( 'NONE',  ( 1.000000000000000078E-15, 1.000000000000000083E-30, -1.000000000000000000 ) ) ;
#85645 = DIRECTION ( 'NONE',  ( 3.100000000000000258E-29, -3.100000000000000044E-14, -1.000000000000000000 ) ) ;
#85646 = DIRECTION ( 'NONE',  ( 0.000000000000000000, 0.000000000000000000, 1.000000000000000000 ) ) ;
#85649 = CARTESIAN_POINT ( 'NONE',  ( 104.4161250475293485, -26.02246701806305751, 236.2575300378159682 ) ) ;
#85648 = CARTESIAN_POINT ( 'NONE',  ( 177.1649999999999920, 14.63749999999999929, -14.28749999999999964 ) ) ;
#85647 = CARTESIAN_POINT ( 'NONE',  ( 70.63919639214310564, 100.5999999999999659, 56.85413200336923012 ) ) ;
#85650 = FACE_OUTER_BOUND ( 'NONE', #75357, .T. ) ;
#85651 = DIRECTION ( 'NONE',  ( 1.000000000000000078E-15, 1.000000000000000083E-30, -1.000000000000000000 ) ) ;
#85652 = AXIS2_PLACEMENT_3D ( 'NONE', #77031, #30219, #57463 ) ;
#85653 = CARTESIAN_POINT ( 'NONE',  ( 97.31592806723080002, -39.30618353892086958, 272.5310398921420756 ) ) ;
#85654 = CARTESIAN_POINT ( 'NONE',  ( 107.0664832912739968, 22.62155284005901024, 333.4006252759110112 ) ) ;
#85655 = CARTESIAN_POINT ( 'NONE',  ( 105.7995184719876960, -26.72403496767840281, 256.1772919438192275 ) ) ;
#85656 = DIRECTION ( 'NONE',  ( -0.4428439315555359745, -0.8965987130731539745, 0.000000000000000000 ) ) ;
#85658 = ORIENTED_EDGE ( 'NONE', *, *, #84604, .F. ) ;
#85657 = CARTESIAN_POINT ( 'NONE',  ( 110.6252048999878497, -43.92627768550128309, 195.5838068554168387 ) ) ;
#85659 = DIRECTION ( 'NONE',  ( 1.000000000000000000, 4.510281037539819615E-14, 0.000000000000000000 ) ) ;
#85660 = CARTESIAN_POINT ( 'NONE',  ( 102.9583934913338652, -26.44260899983745006, 175.3908633711489813 ) ) ;
#85661 = CARTESIAN_POINT ( 'NONE',  ( 117.4474071775726287, -37.68804338056689573, 74.75276813305397638 ) ) ;
#85662 = CARTESIAN_POINT ( 'NONE',  ( 99.25607838769128932, -29.75875458388292571, 186.7470538473389752 ) ) ;
#85663 = CARTESIAN_POINT ( 'NONE',  ( 50.03799999999999670, 0.000000000000000000, 206.3750000000000000 ) ) ;
#85664 = DIRECTION ( 'NONE',  ( 1.000000000000000000, 4.163336342344333240E-14, 0.000000000000000000 ) ) ;
#85665 = CIRCLE ( 'NONE', #18855, 20.63750000000000284 ) ;
#85667 = LINE ( 'NONE', #57031, #55892 ) ;
#85666 = CARTESIAN_POINT ( 'NONE',  ( 168.3595971214442102, -48.62134037892998606, 249.9678068554149775 ) ) ;
#85668 = LINE ( 'NONE', #23445, #85714 ) ;
#85669 = CYLINDRICAL_SURFACE ( 'NONE', #89120, 2.750000000000002665 ) ;
#85670 = EDGE_LOOP ( 'NONE', ( #5634, #62418, #85378, #59273, #26058, #81134 ) ) ;
#85671 = FACE_OUTER_BOUND ( 'NONE', #20269, .T. ) ;
#85672 = EDGE_CURVE ( 'NONE', #22054, #54909, #64882, .T. ) ;
#85673 = ORIENTED_EDGE ( 'NONE', *, *, #51827, .T. ) ;
#85674 = ORIENTED_EDGE ( 'NONE', *, *, #15356, .F. ) ;
#85675 = CARTESIAN_POINT ( 'NONE',  ( 98.52328466580365784, -37.41198607556916755, 100.8124198280769832 ) ) ;
#85676 = AXIS2_PLACEMENT_3D ( 'NONE', #21575, #83799, #49242 ) ;
#85678 = ORIENTED_EDGE ( 'NONE', *, *, #33164, .T. ) ;
#85677 = CARTESIAN_POINT ( 'NONE',  ( -254.0000000000000000, 53.97500000000000142, 0.000000000000000000 ) ) ;
#85679 = CARTESIAN_POINT ( 'NONE',  ( 117.5733473178507467, -42.15660255127702527, 89.44705384733997278 ) ) ;
#85680 = DIRECTION ( 'NONE',  ( -0.2588190451025119132, 0.000000000000000000, -0.9659258262890706437 ) ) ;
#85682 = CARTESIAN_POINT ( 'NONE',  ( 79.87807227643494912, -15.97944715994105813, 8.225625275910944723 ) ) ;
#85681 = AXIS2_PLACEMENT_3D ( 'NONE', #43738, #6994, #35130 ) ;
#85683 = CARTESIAN_POINT ( 'NONE',  ( 46.83715912545429205, -47.82818131006082751, 249.9678068554150343 ) ) ;
#85684 = CARTESIAN_POINT ( 'NONE',  ( 96.85055626654745708, -38.51091292166576352, 46.45181575210194325 ) ) ;
#85685 = ORIENTED_EDGE ( 'NONE', *, *, #81837, .T. ) ;
#85686 = ORIENTED_EDGE ( 'NONE', *, *, #31436, .F. ) ;
#85688 = ORIENTED_EDGE ( 'NONE', *, *, #67456, .F. ) ;
#85687 = CIRCLE ( 'NONE', #81343, 9.571100913904507124 ) ;
#85689 = ADVANCED_FACE ( 'NONE', ( #53164 ), #50339, .F. ) ;
#85690 = CYLINDRICAL_SURFACE ( 'NONE', #51482, 4.762500000000002842 ) ;
#85691 = DIRECTION ( 'NONE',  ( 0.000000000000000000, 0.000000000000000000, -1.000000000000000000 ) ) ;
#85692 = DIRECTION ( 'NONE',  ( 0.000000000000000000, 0.000000000000000000, -1.000000000000000000 ) ) ;
#85693 = CARTESIAN_POINT ( 'NONE',  ( 0.000000000000000000, 92.07499999999998863, 0.000000000000000000 ) ) ;
#85694 = CARTESIAN_POINT ( 'NONE',  ( 165.9667039024459996, -26.71338133339301635, -5.074374724088000832 ) ) ;
#85695 = CARTESIAN_POINT ( 'NONE',  ( 97.80395968718781319, -40.49850023374117569, 52.63358577967416352 ) ) ;
#85696 = VECTOR ( 'NONE', #72203, 1000.000000000000000 ) ;
#85697 = CARTESIAN_POINT ( 'NONE',  ( 67.06670390244678970, -67.87844716023829506, 245.4990141143767630 ) ) ;
#85698 = CARTESIAN_POINT ( 'NONE',  ( 75.69222284415393176, 88.91144712388911842, 91.24829632406283508 ) ) ;
#85699 = CARTESIAN_POINT ( 'NONE',  ( 96.97787942770413849, -32.27031107066116533, 55.98324432352897162 ) ) ;
#85700 = EDGE_CURVE ( 'NONE', #11860, #36556, #5054, .T. ) ;
#85701 = ORIENTED_EDGE ( 'NONE', *, *, #86029, .F. ) ;
#85702 = EDGE_CURVE ( 'NONE', #83669, #87871, #88192, .T. ) ;
#85703 = CARTESIAN_POINT ( 'NONE',  ( 108.4174897361023824, -26.73503600100527677, 269.9689585707081960 ) ) ;
#85704 =( GEOMETRIC_REPRESENTATION_CONTEXT ( 3 ) GLOBAL_UNCERTAINTY_ASSIGNED_CONTEXT ( ( #88101 ) ) GLOBAL_UNIT_ASSIGNED_CONTEXT ( ( #63280, #21966, #41471 ) ) REPRESENTATION_CONTEXT ( 'NONE', 'WORKASPACE' ) );
#85705 = FACE_OUTER_BOUND ( 'NONE', #74174, .T. ) ;
#85706 = CARTESIAN_POINT ( 'NONE',  ( 114.9723337227840005, -34.69788249897437993, 121.8452332267339671 ) ) ;
#85707 = EDGE_CURVE ( 'NONE', #27001, #14582, #51836, .T. ) ;
#85708 = DIRECTION ( 'NONE',  ( 0.000000000000000000, 0.000000000000000000, -1.000000000000000000 ) ) ;
#85709 = VECTOR ( 'NONE', #50375, 1000.000000000000000 ) ;
#85710 = CYLINDRICAL_SURFACE ( 'NONE', #12607, 118.5560000000000116 ) ;
#85711 = ORIENTED_EDGE ( 'NONE', *, *, #70721, .F. ) ;
#85712 = EDGE_LOOP ( 'NONE', ( #33672, #81241 ) ) ;
#85713 = LINE ( 'NONE', #63458, #80137 ) ;
#85714 = VECTOR ( 'NONE', #51111, 1000.000000000000000 ) ;
#85715 = ORIENTED_EDGE ( 'NONE', *, *, #82831, .F. ) ;
#85716 = ORIENTED_EDGE ( 'NONE', *, *, #71760, .F. ) ;
#85717 = EDGE_CURVE ( 'NONE', #61024, #84863, #25699, .T. ) ;
#85718 = CARTESIAN_POINT ( 'NONE',  ( 99.92577194148378794, -31.43111053364522434, 177.2501547344679693 ) ) ;
#85719 = DIRECTION ( 'NONE',  ( 1.000000000000000000, 1.000000000000000078E-15, -0.000000000000000000 ) ) ;
#85720 = CIRCLE ( 'NONE', #45025, 82.41591158490093960 ) ;
#85721 = CARTESIAN_POINT ( 'NONE',  ( 96.67756931115832231, -37.82841265861588909, 122.4099109901969626 ) ) ;
#85722 = DIRECTION ( 'NONE',  ( -1.000000000000000000, -4.163336342344275811E-14, 0.000000000000000000 ) ) ;
#85723 = CARTESIAN_POINT ( 'NONE',  ( 116.7474494541973087, -34.15064250361619003, 19.03369576739390823 ) ) ;
#85724 = VERTEX_POINT ( 'NONE', #13221 ) ;
#85725 = AXIS2_PLACEMENT_3D ( 'NONE', #52259, #11408, #60437 ) ;
#85726 = ORIENTED_EDGE ( 'NONE', *, *, #5922, .F. ) ;
#85727 = EDGE_LOOP ( 'NONE', ( #59342, #8270, #63015, #14240 ) ) ;
#85728 =( REPRESENTATION_RELATIONSHIP ('NONE','NONE', #82876, #48599 ) REPRESENTATION_RELATIONSHIP_WITH_TRANSFORMATION ( #7664 )SHAPE_REPRESENTATION_RELATIONSHIP( ) );
#85729 = EDGE_CURVE ( 'NONE', #73068, #82750, #83611, .T. ) ;
#85730 = CARTESIAN_POINT ( 'NONE',  ( 109.7539934464052465, -29.02185251678796618, 207.6280903695909501 ) ) ;
#85731 = CARTESIAN_POINT ( 'NONE',  ( 114.3686432469292527, -44.20104832357726110, 73.19276813305397411 ) ) ;
#85732 = EDGE_LOOP ( 'NONE', ( #5460, #4690, #26712, #62927 ) ) ;
#85733 = CARTESIAN_POINT ( 'NONE',  ( 115.8731522275743941, -31.19128430790902584, 34.27276813305396530 ) ) ;
#85734 = CARTESIAN_POINT ( 'NONE',  ( 102.6743760996991597, -27.25069970728465307, 176.4213395616249898 ) ) ;
#85735 = EDGE_CURVE ( 'NONE', #76359, #16547, #14109, .T. ) ;
#85736 = CARTESIAN_POINT ( 'NONE',  ( 183.5150000000000148, 37.33800000000000097, 32.46912895322940074 ) ) ;
#85737 = DIRECTION ( 'NONE',  ( 0.000000000000000000, -1.000000000000000000, 0.000000000000000000 ) ) ;
#85738 = CARTESIAN_POINT ( 'NONE',  ( 114.0809025726587436, -44.48955379074138961, 129.1613395616249704 ) ) ;
#85739 = VECTOR ( 'NONE', #89709, 1000.000000000000000 ) ;
#85741 = EDGE_CURVE ( 'NONE', #11195, #20936, #479, .T. ) ;
#85740 = CARTESIAN_POINT ( 'NONE',  ( 182.5667039024459939, -19.82844715994031048, -5.074374724088000832 ) ) ;
#85742 = EDGE_LOOP ( 'NONE', ( #69739, #77698, #70265, #37261 ) ) ;
#85743 = FACE_BOUND ( 'NONE', #78722, .T. ) ;
#85744 = CIRCLE ( 'NONE', #32019, 10.00000000000000711 ) ;
#85745 = EDGE_CURVE ( 'NONE', #80801, #29469, #34389, .T. ) ;
#85746 = ORIENTED_EDGE ( 'NONE', *, *, #2124, .T. ) ;
#85747 = CARTESIAN_POINT ( 'NONE',  ( 108.3338899180770625, -46.73481428249178293, 133.6785589755952799 ) ) ;
#85748 = PLANE ( 'NONE',  #9704 ) ;
#85749 = ORIENTED_EDGE ( 'NONE', *, *, #23023, .F. ) ;
#85750 = VECTOR ( 'NONE', #17603, 1000.000000000000000 ) ;
#85751 = DIRECTION ( 'NONE',  ( 0.7071067811865473507, 0.000000000000000000, -0.7071067811865476838 ) ) ;
#85752 = CARTESIAN_POINT ( 'NONE',  ( 112.5942678722098123, -28.35481117739004731, 130.6124851771425881 ) ) ;
#85753 = CARTESIAN_POINT ( 'NONE',  ( 106.9273489086460387, -26.26968863985776537, 60.08705384733897858 ) ) ;
#85754 = CARTESIAN_POINT ( 'NONE',  ( 15.05032694871533927, 67.26578276466975126, 35.00684828750966204 ) ) ;
#85755 = LINE ( 'NONE', #77135, #40554 ) ;
#85756 = CARTESIAN_POINT ( 'NONE',  ( 153.0667045879000057, -71.37844715994090450, 222.2178068554179902 ) ) ;
#85757 = CARTESIAN_POINT ( 'NONE',  ( 112.5987260342905358, -28.66361022110268308, 44.59848241876795782 ) ) ;
#85759 = CARTESIAN_POINT ( 'NONE',  ( 108.8451227504523189, -46.97957433935474825, 163.7127681330539701 ) ) ;
#85758 = CARTESIAN_POINT ( 'NONE',  ( 72.06648329127402519, -45.72944715994106701, -4.824374724089063982 ) ) ;
#85760 = CARTESIAN_POINT ( 'NONE',  ( 3.968749999999215294, 127.0000000000000000, 105.4788588808464027 ) ) ;
#85761 = CARTESIAN_POINT ( 'NONE',  ( -7.205548786489490269E-13, 117.4749999999999943, 103.1875000000000000 ) ) ;
#85762 = ORIENTED_EDGE ( 'NONE', *, *, #8070, .F. ) ;
#85763 = VECTOR ( 'NONE', #77459, 1000.000000000000000 ) ;
#85764 = CARTESIAN_POINT ( 'NONE',  ( 19.56648329127303043, -71.37844715994266664, 361.9756252759109998 ) ) ;
#85765 = CARTESIAN_POINT ( 'NONE',  ( 33.98325472291465132, 104.3431970271542042, -3.174999999999999822 ) ) ;
#85766 = CARTESIAN_POINT ( 'NONE',  ( 107.0667039024470313, -104.2784471599418197, -11.78219314458200984 ) ) ;
#85767 = CIRCLE ( 'NONE', #78505, 4.750000000000000888 ) ;
#85768 = PLANE ( 'NONE',  #89790 ) ;
#85770 = ORIENTED_EDGE ( 'NONE', *, *, #62549, .F. ) ;
#85769 = CARTESIAN_POINT ( 'NONE',  ( 112.2268274879326668, -45.83864656583022423, 212.9870538473389558 ) ) ;
#85771 = CARTESIAN_POINT ( 'NONE',  ( 109.7247347643963167, -27.00076673087112766, 144.8648027181440909 ) ) ;
#85772 = CARTESIAN_POINT ( 'NONE',  ( 105.6290766085263044, -47.07696477925017575, 253.4670538473393719 ) ) ;
#85773 = CARTESIAN_POINT ( 'NONE',  ( 102.9539626486510713, -46.35650038051790744, 88.25562527591095829 ) ) ;
#85774 = CARTESIAN_POINT ( 'NONE',  ( 33.78309357196401663, -29.99615139349950965, -5.074374724088000832 ) ) ;
#85775 = CARTESIAN_POINT ( 'NONE',  ( 97.06112902794230024, -37.99671193374311429, 192.4271787320971043 ) ) ;
#85776 = CARTESIAN_POINT ( 'NONE',  ( 196.2150000000000034, 43.68799999999999528, 57.14999999999999858 ) ) ;
#85777 = ORIENTED_EDGE ( 'NONE', *, *, #69793, .T. ) ;
#85778 = ORIENTED_EDGE ( 'NONE', *, *, #21302, .F. ) ;
#85779 = ORIENTED_EDGE ( 'NONE', *, *, #75335, .F. ) ;
#85780 = VECTOR ( 'NONE', #29130, 1000.000000000000114 ) ;
#85781 = ORIENTED_EDGE ( 'NONE', *, *, #51084, .T. ) ;
#85782 = DIRECTION ( 'NONE',  ( -0.7071067811865510144, 0.000000000000000000, 0.7071067811865441310 ) ) ;
#85783 = CARTESIAN_POINT ( 'NONE',  ( 110.9930042498355363, -46.38681234365495953, 278.8841967044824059 ) ) ;
#85784 = DIRECTION ( 'NONE',  ( 0.000000000000000000, -1.000000000000000000, 0.000000000000000000 ) ) ;
#85785 = CARTESIAN_POINT ( 'NONE',  ( 132.7641780748886049, -34.30680158339101382, 1.893168945965612471 ) ) ;
#85787 = FACE_OUTER_BOUND ( 'NONE', #26009, .T. ) ;
#85786 = DIRECTION ( 'NONE',  ( -0.000000000000000000, -1.000000000000000000, -0.000000000000000000 ) ) ;
#85788 = FACE_OUTER_BOUND ( 'NONE', #26443, .T. ) ;
#85789 = VECTOR ( 'NONE', #67812, 1000.000000000000000 ) ;
#85790 = CARTESIAN_POINT ( 'NONE',  ( 97.51448592794399417, -38.47012922887837760, 200.8924198280769815 ) ) ;
#85791 = ORIENTED_EDGE ( 'NONE', *, *, #34876, .T. ) ;
#85792 = ORIENTED_EDGE ( 'NONE', *, *, #6307, .T. ) ;
#85793 = ORIENTED_EDGE ( 'NONE', *, *, #86750, .T. ) ;
#85794 = AXIS2_PLACEMENT_3D ( 'NONE', #60328, #73520, #32179 ) ;
#85795 = EDGE_CURVE ( 'NONE', #51345, #70808, #86838, .T. ) ;
#85796 =( NAMED_UNIT ( * ) SI_UNIT ( $, .STERADIAN. ) SOLID_ANGLE_UNIT ( ) );
#85797 = CARTESIAN_POINT ( 'NONE',  ( 163.0822201311030142, 101.5999999999999943, -75.92468371870729982 ) ) ;
#85798 = EDGE_CURVE ( 'NONE', #2462, #1233, #83169, .T. ) ;
#85799 = CARTESIAN_POINT ( 'NONE',  ( 109.8085987287837213, -27.34093086507540704, 255.8499109901960367 ) ) ;
#85800 = DIRECTION ( 'NONE',  ( -0.7071067811865794361, 0.7071067811865157093, -7.071067811865803697E-16 ) ) ;
#85801 = EDGE_CURVE ( 'NONE', #26492, #28372, #34086, .T. ) ;
#85802 = DIRECTION ( 'NONE',  ( 0.000000000000000000, 2.135044278125299371E-15, -1.000000000000000000 ) ) ;
#85803 = CARTESIAN_POINT ( 'NONE',  ( 165.6738106836030227, -28.98061976758901892, 117.4678068554150627 ) ) ;
#85804 = EDGE_CURVE ( 'NONE', #83210, #8807, #6393, .T. ) ;
#85806 = ORIENTED_EDGE ( 'NONE', *, *, #59061, .T. ) ;
#85805 = VECTOR ( 'NONE', #83333, 1000.000000000000000 ) ;
#85807 = ADVANCED_FACE ( 'NONE', ( #5515 ), #33656, .T. ) ;
#85808 = CARTESIAN_POINT ( 'NONE',  ( 77.49614765539782013, -35.75123073100116500, 2.855912073278434438 ) ) ;
#85809 = VERTEX_POINT ( 'NONE', #60909 ) ;
#85810 = DIRECTION ( 'NONE',  ( 0.9068632946707806397, -0.4214249218767879279, 9.068632946707804446E-16 ) ) ;
#85811 = CARTESIAN_POINT ( 'NONE',  ( 103.6908924260029607, -28.08645471411401928, 18.19094751244793073 ) ) ;
#85812 = CIRCLE ( 'NONE', #1700, 0.5000000000000004441 ) ;
#85813 = EDGE_CURVE ( 'NONE', #80451, #18492, #27285, .T. ) ;
#85814 = CARTESIAN_POINT ( 'NONE',  ( 136.8000579002609811, -18.42904715602391263, 6.774297104452461582 ) ) ;
#85815 = EDGE_CURVE ( 'NONE', #52459, #44341, #11170, .T. ) ;
#85816 = DIRECTION ( 'NONE',  ( 1.639958061481212836E-42, -4.100000000000000342E-29, -1.000000000000000000 ) ) ;
#85817 = CIRCLE ( 'NONE', #30687, 4.799999999999970512 ) ;
#85818 = CARTESIAN_POINT ( 'NONE',  ( 107.0664832912739968, -36.72944715994100306, 9.635625275910941312 ) ) ;
#85819 = VERTEX_POINT ( 'NONE', #69077 ) ;
#85820 = FACE_OUTER_BOUND ( 'NONE', #41961, .T. ) ;
#85821 = CARTESIAN_POINT ( 'NONE',  ( 106.5667039024470455, -113.7784471599420613, -19.78219314458171141 ) ) ;
#85822 = EDGE_LOOP ( 'NONE', ( #70442, #44976, #51661, #38019 ) ) ;
#85823 = CARTESIAN_POINT ( 'NONE',  ( 115.1669806615814622, -43.29214270484202132, 88.28419670448195689 ) ) ;
#85824 = ORIENTED_EDGE ( 'NONE', *, *, #23972, .F. ) ;
#85825 = CARTESIAN_POINT ( 'NONE',  ( 114.2970346969270565, -32.18244176163005221, 33.69527697093299423 ) ) ;
#85826 = ADVANCED_FACE ( 'NONE', ( #82725, #26392, #46808 ), #74541, .T. ) ;
#85827 = CARTESIAN_POINT ( 'NONE',  ( 100.6318841171118805, -120.9585416479406206, -9.274842254010108533 ) ) ;
#85828 = CARTESIAN_POINT ( 'NONE',  ( 101.9660762386545514, -28.83879614530413704, 66.97682140113498406 ) ) ;
#85829 = CARTESIAN_POINT ( 'NONE',  ( 116.7946685605787849, -39.38945716434293587, 14.61465845921219575 ) ) ;
#85830 = CARTESIAN_POINT ( 'NONE',  ( 204.2160000000000082, 52.73749999999999716, -41.27499999999999858 ) ) ;
#85831 = DIRECTION ( 'NONE',  ( 1.000000000000000000, 4.163336342344333240E-14, 0.000000000000000000 ) ) ;
#85832 = CARTESIAN_POINT ( 'NONE',  ( 97.78987344453990715, -29.31549002224505429, 41.78991099019596334 ) ) ;
#85833 = CARTESIAN_POINT ( 'NONE',  ( 124.0667039024470313, -104.2784471599417486, -9.937637710810031777 ) ) ;
#85834 = EDGE_LOOP ( 'NONE', ( #35690, #31946, #52150, #77504 ) ) ;
#85835 = LINE ( 'NONE', #79007, #87932 ) ;
#85836 = ORIENTED_EDGE ( 'NONE', *, *, #27922, .F. ) ;
#85837 = CARTESIAN_POINT ( 'NONE',  ( 102.3735796352302714, -26.67091080359734434, 131.4118157521009778 ) ) ;
#85838 = CARTESIAN_POINT ( 'NONE',  ( 125.0906544762830066, 49.12084779284757019, -37.37934391051621219 ) ) ;
#85839 = ORIENTED_EDGE ( 'NONE', *, *, #39487, .T. ) ;
#85840 = VERTEX_POINT ( 'NONE', #20489 ) ;
#85841 = AXIS2_PLACEMENT_3D ( 'NONE', #37050, #16172, #43851 ) ;
#85842 = CARTESIAN_POINT ( 'NONE',  ( -141.3509999999999991, 101.5999999999999943, -141.3509999999999991 ) ) ;
#85843 = DIRECTION ( 'NONE',  ( 0.000000000000000000, 0.000000000000000000, 1.000000000000000000 ) ) ;
#85844 = CARTESIAN_POINT ( 'NONE',  ( 104.6152064257953498, -27.26083179018618452, 200.2784824187689310 ) ) ;
#85845 = CYLINDRICAL_SURFACE ( 'NONE', #2237, 10.00000000000000888 ) ;
#85846 = FACE_OUTER_BOUND ( 'NONE', #55457, .T. ) ;
#85847 = FACE_OUTER_BOUND ( 'NONE', #46721, .T. ) ;
#85848 = CARTESIAN_POINT ( 'NONE',  ( 97.10477362122047396, -39.80301782323012105, 17.56419670448195092 ) ) ;
#85850 = EDGE_CURVE ( 'NONE', #30894, #13404, #48897, .T. ) ;
#85849 = CARTESIAN_POINT ( 'NONE',  ( 127.0664832912740110, -54.72944906728950798, 14.67562527591099197 ) ) ;
#85851 = ORIENTED_EDGE ( 'NONE', *, *, #38752, .F. ) ;
#85852 = CARTESIAN_POINT ( 'NONE',  ( 74.15067561874269586, 120.6499999999999915, -68.53801554307419508 ) ) ;
#85853 = EDGE_CURVE ( 'NONE', #20676, #40647, #28554, .T. ) ;
#85854 = DIRECTION ( 'NONE',  ( 0.000000000000000000, 0.000000000000000000, 1.000000000000000000 ) ) ;
#85855 = AXIS2_PLACEMENT_3D ( 'NONE', #54, #500, #14134 ) ;
#85856 = ORIENTED_EDGE ( 'NONE', *, *, #6124, .T. ) ;
#85857 = AXIS2_PLACEMENT_3D ( 'NONE', #85633, #56085, #35206 ) ;
#85858 = CARTESIAN_POINT ( 'NONE',  ( 0.000000000000000000, 44.45000000000000284, 0.000000000000000000 ) ) ;
#85859 = FACE_OUTER_BOUND ( 'NONE', #20063, .T. ) ;
#85860 = CARTESIAN_POINT ( 'NONE',  ( 101.3060704567421197, -26.40153104436172526, 255.4813395616251626 ) ) ;
#85861 = DIRECTION ( 'NONE',  ( -1.000000000000000000, 0.000000000000000000, 0.000000000000000000 ) ) ;
#85862 = CARTESIAN_POINT ( 'NONE',  ( 41.56648329127499153, -32.07844715994070839, 258.9256252759120116 ) ) ;
#85863 = CARTESIAN_POINT ( 'NONE',  ( 98.70294500015674544, -34.99527330041078699, 215.5867055423629779 ) ) ;
#85865 = CARTESIAN_POINT ( 'NONE',  ( 105.4244226815142298, -47.00233879195495490, 33.44991099019695469 ) ) ;
#85864 = DIRECTION ( 'NONE',  ( -1.000000000000000078E-15, 1.000000000000000083E-30, 1.000000000000000000 ) ) ;
#85866 = DIRECTION ( 'NONE',  ( 0.000000000000000000, 0.000000000000000000, -1.000000000000000000 ) ) ;
#85867 = CARTESIAN_POINT ( 'NONE',  ( 113.3579092357397542, -45.09751872455207433, 143.0899109901969553 ) ) ;
#85868 = ORIENTED_EDGE ( 'NONE', *, *, #86231, .F. ) ;
#85869 = CARTESIAN_POINT ( 'NONE',  ( 131.4143329470395827, -19.45719076514318502, 6.889371645759392315 ) ) ;
#85870 = ORIENTED_EDGE ( 'NONE', *, *, #84039, .F. ) ;
#85871 = DIRECTION ( 'NONE',  ( 0.000000000000000000, -1.000000000000000000, 0.000000000000000000 ) ) ;
#85872 = DIRECTION ( 'NONE',  ( 1.000000000000000000, 1.261617073437676668E-15, 9.462128050782575008E-16 ) ) ;
#85873 = ORIENTED_EDGE ( 'NONE', *, *, #15010, .F. ) ;
#85874 = AXIS2_PLACEMENT_3D ( 'NONE', #45099, #27688, #61741 ) ;
#85875 = DIRECTION ( 'NONE',  ( -0.7071067811865279218, 0.7071067811865670016, -6.612322855859973915E-17 ) ) ;
#85876 = EDGE_LOOP ( 'NONE', ( #9579, #79165, #76989, #34010 ) ) ;
#85877 = FACE_OUTER_BOUND ( 'NONE', #12436, .T. ) ;
#85878 = DIRECTION ( 'NONE',  ( -1.000000000000000000, 1.271620792853953879E-14, 0.000000000000000000 ) ) ;
#85879 = DIRECTION ( 'NONE',  ( 2.900000000000000265E-14, -2.000000000000000155E-15, 1.000000000000000000 ) ) ;
#85880 = ORIENTED_EDGE ( 'NONE', *, *, #6345, .T. ) ;
#85881 = VECTOR ( 'NONE', #51262, 999.9999999999998863 ) ;
#85882 = CARTESIAN_POINT ( 'NONE',  ( 107.2325596213128875, -25.65389481303129315, 80.07657765686299456 ) ) ;
#85883 = DIRECTION ( 'NONE',  ( 1.000000000000000000, 0.000000000000000000, 0.000000000000000000 ) ) ;
#85884 = CARTESIAN_POINT ( 'NONE',  ( 97.06384678839589242, -37.34232347881079761, 166.3752407659725918 ) ) ;
#85885 = DIRECTION ( 'NONE',  ( 0.000000000000000000, 0.000000000000000000, 1.000000000000000000 ) ) ;
#85886 = CARTESIAN_POINT ( 'NONE',  ( -77.39114642429849766, 127.0000000000000000, -71.77848634863219957 ) ) ;
#85887 = VERTEX_POINT ( 'NONE', #19573 ) ;
#85888 = AXIS2_PLACEMENT_3D ( 'NONE', #66621, #16701, #86637 ) ;
#85889 = FACE_OUTER_BOUND ( 'NONE', #57249, .T. ) ;
#85890 = CARTESIAN_POINT ( 'NONE',  ( 107.0664832912739399, -36.72944715994096754, 298.1356252759109680 ) ) ;
#85891 = VECTOR ( 'NONE', #26524, 1000.000000000000000 ) ;
#85892 = LINE ( 'NONE', #23663, #39970 ) ;
#85893 = CIRCLE ( 'NONE', #74270, 5.041900000000001825 ) ;
#85895 = CARTESIAN_POINT ( 'NONE',  ( 163.0664832912739826, -18.82844715994099971, 333.4006252759120343 ) ) ;
#85894 = CARTESIAN_POINT ( 'NONE',  ( 97.81169461453751524, -40.51741999607308742, 142.6356648221729131 ) ) ;
#85896 = CARTESIAN_POINT ( 'NONE',  ( 162.8913605087221868, -31.76306994223289948, 237.4678068554150059 ) ) ;
#85897 = VERTEX_POINT ( 'NONE', #14114 ) ;
#85898 = ADVANCED_FACE ( 'NONE', ( #74992 ), #12775, .T. ) ;
#85899 = FACE_OUTER_BOUND ( 'NONE', #19939, .T. ) ;
#85900 = ADVANCED_FACE ( 'NONE', ( #28631 ), #49506, .T. ) ;
#85901 = CARTESIAN_POINT ( 'NONE',  ( 109.6835627966674878, -27.30531164764932939, 170.8613395616249591 ) ) ;
#85903 = ORIENTED_EDGE ( 'NONE', *, *, #43090, .T. ) ;
#85902 = LINE ( 'NONE', #71376, #71825 ) ;
#85904 = EDGE_CURVE ( 'NONE', #78471, #25006, #57608, .T. ) ;
#85905 = CARTESIAN_POINT ( 'NONE',  ( 100.8736165617014677, -44.32606212243579336, 8.032768133052980986 ) ) ;
#85906 = DIRECTION ( 'NONE',  ( 1.175184669632759901E-16, -1.000000000000000000, -2.000000000000003705E-15 ) ) ;
#85907 = LINE ( 'NONE', #37744, #38590 ) ;
#85908 = CARTESIAN_POINT ( 'NONE',  ( 117.0603303411406984, -38.08442816249873886, 13.71933068259133748 ) ) ;
#85909 = EDGE_CURVE ( 'NONE', #27014, #8926, #63383, .T. ) ;
#85910 = VERTEX_POINT ( 'NONE', #1385 ) ;
#85911 = CARTESIAN_POINT ( 'NONE',  ( 104.4908855836804236, -26.97855169986425494, 30.28161050152675315 ) ) ;
#85912 = CARTESIAN_POINT ( 'NONE',  ( 115.9419818307744663, -40.91744192719425399, 228.4756252759109714 ) ) ;
#85913 = ORIENTED_EDGE ( 'NONE', *, *, #16010, .F. ) ;
#85914 = AXIS2_PLACEMENT_3D ( 'NONE', #393, #28087, #47631 ) ;
#85915 = VERTEX_POINT ( 'NONE', #29089 ) ;
#85916 = CARTESIAN_POINT ( 'NONE',  ( 113.0661788413732580, -30.20779614827405624, 195.9158690201829529 ) ) ;
#85917 = ADVANCED_FACE ( 'NONE', ( #57218 ), #63605, .F. ) ;
#85918 = CIRCLE ( 'NONE', #11983, 2.117000000000007987 ) ;
#85919 = LINE ( 'NONE', #59057, #2311 ) ;
#85920 = CARTESIAN_POINT ( 'NONE',  ( 115.9247622085524085, -36.97270265434710979, 40.23586902018294609 ) ) ;
#85921 = CARTESIAN_POINT ( 'NONE',  ( -100.8465607796065200, 83.38002811471483255, 82.91466710319213007 ) ) ;
#85922 = EDGE_CURVE ( 'NONE', #51377, #79343, #80846, .T. ) ;
#85923 = CARTESIAN_POINT ( 'NONE',  ( 0.000000000000000000, 239.0000000000000000, 149.8557476874258896 ) ) ;
#85924 = DIRECTION ( 'NONE',  ( 0.000000000000000000, 0.000000000000000000, 1.000000000000000000 ) ) ;
#85925 = ORIENTED_EDGE ( 'NONE', *, *, #5216, .F. ) ;
#85926 = CARTESIAN_POINT ( 'NONE',  ( 83.06670390244806867, -51.22944715994108122, 207.5838068554169809 ) ) ;
#85927 = CYLINDRICAL_SURFACE ( 'NONE', #24143, 3.000000000000002665 ) ;
#85928 = ORIENTED_EDGE ( 'NONE', *, *, #41483, .F. ) ;
#85929 = CARTESIAN_POINT ( 'NONE',  ( 108.0121126588926046, -24.94157235513505100, 265.0127681330535552 ) ) ;
#85930 = CARTESIAN_POINT ( 'NONE',  ( 152.0371591254583450, -47.82818131005588214, 249.9678068554149490 ) ) ;
#85931 = ORIENTED_EDGE ( 'NONE', *, *, #24068, .T. ) ;
#85933 = EDGE_CURVE ( 'NONE', #19677, #18647, #84523, .T. ) ;
#85932 = AXIS2_PLACEMENT_3D ( 'NONE', #5247, #32486, #82018 ) ;
#85934 = SURFACE_SIDE_STYLE ('',( #30501 ) ) ;
#85935 = DIRECTION ( 'NONE',  ( -0.7071067811567310901, 0.7071067812163639443, 0.000000000000000000 ) ) ;
#85936 = PLANE ( 'NONE',  #14264 ) ;
#85937 = DIRECTION ( 'NONE',  ( -3.100000000000000258E-29, 3.100000000000000044E-14, 1.000000000000000000 ) ) ;
#85938 = CARTESIAN_POINT ( 'NONE',  ( 100.2135729606528685, -43.75450166055420453, 17.96133956162493206 ) ) ;
#85939 = FACE_OUTER_BOUND ( 'NONE', #61064, .T. ) ;
#85940 = VERTEX_POINT ( 'NONE', #84963 ) ;
#85941 = VECTOR ( 'NONE', #4392, 1000.000000000000000 ) ;
#85942 = CARTESIAN_POINT ( 'NONE',  ( 96.91449086013869874, -32.24229349230230923, 51.98324432352996638 ) ) ;
#85943 = CARTESIAN_POINT ( 'NONE',  ( 80.06648329127399677, -36.72944715994107412, 14.92562527591094224 ) ) ;
#85944 = CARTESIAN_POINT ( 'NONE',  ( 117.4299418851264818, -35.59553461117717887, 278.9127681330539872 ) ) ;
#85945 = VERTEX_POINT ( 'NONE', #36795 ) ;
#85946 = VECTOR ( 'NONE', #87974, 1000.000000000000000 ) ;
#85947 = CARTESIAN_POINT ( 'NONE',  ( 78.94219388974352114, -39.23922437001928643, 8.028287874532400892 ) ) ;
#85948 = DIRECTION ( 'NONE',  ( 0.7071067811566161820, 0.7071067812164789634, 0.000000000000000000 ) ) ;
#85949 = PLANE ( 'NONE',  #37859 ) ;
#85950 = CARTESIAN_POINT ( 'NONE',  ( 115.5296723907996039, -38.53924143319417794, 106.4890427505429642 ) ) ;
#85951 = CARTESIAN_POINT ( 'NONE',  ( 117.4343095520634108, -35.18433407802718449, 214.9441967044829767 ) ) ;
#85952 = FACE_BOUND ( 'NONE', #17522, .T. ) ;
#85953 = DIRECTION ( 'NONE',  ( 1.000000000000000078E-15, -1.000000000000000000, 0.000000000000000000 ) ) ;
#85954 = ORIENTED_EDGE ( 'NONE', *, *, #6920, .T. ) ;
#85955 = EDGE_CURVE ( 'NONE', #41740, #4309, #74986, .T. ) ;
#85956 = CARTESIAN_POINT ( 'NONE',  ( -487.2989999999999782, 89.53805401447691281, 18.25625000000039933 ) ) ;
#85957 = ORIENTED_EDGE ( 'NONE', *, *, #13077, .T. ) ;
#85958 = ORIENTED_EDGE ( 'NONE', *, *, #39825, .F. ) ;
#85959 = DIRECTION ( 'NONE',  ( 0.000000000000000000, 1.000000000000000000, 2.000000000000000155E-15 ) ) ;
#85960 = VERTEX_POINT ( 'NONE', #2281 ) ;
#85961 = EDGE_LOOP ( 'NONE', ( #88741, #1087 ) ) ;
#85962 = FACE_OUTER_BOUND ( 'NONE', #27045, .T. ) ;
#85963 = CARTESIAN_POINT ( 'NONE',  ( 110.1026808908064680, -27.16648640359800382, 40.83168070709650976 ) ) ;
#85964 = CARTESIAN_POINT ( 'NONE',  ( 108.3145574644059224, -45.20850512633867169, 142.1152769709339907 ) ) ;
#85965 = CARTESIAN_POINT ( 'NONE',  ( 96.86726761138238828, -30.64586122335317953, 280.8984824187682534 ) ) ;
#85966 = AXIS2_PLACEMENT_3D ( 'NONE', #5786, #81208, #39394 ) ;
#85967 = CARTESIAN_POINT ( 'NONE',  ( -9.569027000640168978, 74.15895453169299856, 130.2061718688152610 ) ) ;
#85968 = ORIENTED_EDGE ( 'NONE', *, *, #63926, .F. ) ;
#85969 = EDGE_CURVE ( 'NONE', #32919, #4843, #43520, .T. ) ;
#85970 = CARTESIAN_POINT ( 'NONE',  ( 103.4484542752979053, -27.40651198025439328, 136.3710560532725253 ) ) ;
#85971 = ORIENTED_EDGE ( 'NONE', *, *, #33629, .T. ) ;
#85972 = CARTESIAN_POINT ( 'NONE',  ( 151.0667039024469886, -67.87844715994090450, 85.21780685541799016 ) ) ;
#85973 = CARTESIAN_POINT ( 'NONE',  ( 112.0646398527721317, -45.48910543467338385, 32.98989392684662647 ) ) ;
#85974 = LINE ( 'NONE', #44597, #88144 ) ;
#85975 = AXIS2_PLACEMENT_3D ( 'NONE', #65249, #57076, #8506 ) ;
#85976 = EDGE_CURVE ( 'NONE', #241, #48806, #70658, .T. ) ;
#85977 = CARTESIAN_POINT ( 'NONE',  ( 149.4409906032288404, -0.9156555935619370423, 361.9756252759100335 ) ) ;
#85978 = EDGE_LOOP ( 'NONE', ( #58918, #33469, #28606, #9800 ) ) ;
#85979 = CARTESIAN_POINT ( 'NONE',  ( 109.9893001866846163, -26.72224116339410571, 259.8499109901965767 ) ) ;
#85980 = CARTESIAN_POINT ( 'NONE',  ( 118.1215414109737196, -37.72100569522838498, 29.74324432352998215 ) ) ;
#85981 =( NAMED_UNIT ( * ) SI_UNIT ( $, .STERADIAN. ) SOLID_ANGLE_UNIT ( ) );
#85982 = CARTESIAN_POINT ( 'NONE',  ( 115.0372575041536578, -42.90846256976404760, 119.3022919422766392 ) ) ;
#85984 = DIRECTION ( 'NONE',  ( 0.000000000000000000, -1.000000000000000000, 0.000000000000000000 ) ) ;
#85983 = FACE_OUTER_BOUND ( 'NONE', #86226, .T. ) ;
#85985 = DIRECTION ( 'NONE',  ( 0.000000000000000000, 1.000000000000000000, 0.000000000000000000 ) ) ;
#85986 = FACE_OUTER_BOUND ( 'NONE', #89931, .T. ) ;
#85987 = CARTESIAN_POINT ( 'NONE',  ( 131.8668787344651037, -38.38871026388260077, 7.389079501614427947 ) ) ;
#85988 = CARTESIAN_POINT ( 'NONE',  ( 115.8254323908514323, -31.73001882614791214, 10.23979194279731075 ) ) ;
#85989 = FACE_BOUND ( 'NONE', #30618, .T. ) ;
#85990 = CIRCLE ( 'NONE', #40962, 3.499999999999996003 ) ;
#85991 = CARTESIAN_POINT ( 'NONE',  ( 102.4390861222961888, -38.62343645255491253, 9.635625275910941312 ) ) ;
#85992 = CARTESIAN_POINT ( 'NONE',  ( 248.6659999999999968, 52.73749999999999716, 10.66800000000000104 ) ) ;
#85993 = CARTESIAN_POINT ( 'NONE',  ( 100.0090739042524604, -28.97838942479177149, 285.6641967044823787 ) ) ;
#85994 = CARTESIAN_POINT ( 'NONE',  ( 96.61884675261427446, -36.21154414529181764, 167.2870538473399620 ) ) ;
#85995 = CARTESIAN_POINT ( 'NONE',  ( 115.6290845971308414, -28.50119646097363812, 35.43562527591098643 ) ) ;
#85997 = DIRECTION ( 'NONE',  ( 0.000000000000000000, 1.000000000000000000, 0.000000000000000000 ) ) ;
#85996 = CARTESIAN_POINT ( 'NONE',  ( 41.56648329127398966, -18.82844715994071194, 15.92562527591207022 ) ) ;
#85998 = DIRECTION ( 'NONE',  ( 0.9825752044328147639, 0.1858654557302462929, 0.000000000000000000 ) ) ;
#85999 = AXIS2_PLACEMENT_3D ( 'NONE', #67843, #33323, #46483 ) ;
#86000 = ORIENTED_EDGE ( 'NONE', *, *, #75330, .T. ) ;
#86001 = ADVANCED_FACE ( 'NONE', ( #30870 ), #51733, .F. ) ;
#86002 = DIRECTION ( 'NONE',  ( 0.000000000000000000, -1.000000000000000000, 0.000000000000000000 ) ) ;
#86003 = ORIENTED_EDGE ( 'NONE', *, *, #76437, .T. ) ;
#86004 = EDGE_CURVE ( 'NONE', #20045, #17829, #79485, .T. ) ;
#86005 = CIRCLE ( 'NONE', #55478, 118.5560000000000116 ) ;
#86006 = CARTESIAN_POINT ( 'NONE',  ( 107.3052971647831697, -26.36210646096938959, 71.04610146638695767 ) ) ;
#86008 = EDGE_LOOP ( 'NONE', ( #59028, #84994, #13093, #69911 ) ) ;
#86007 = CARTESIAN_POINT ( 'NONE',  ( 3.230156947913894072, 94.83977257127416749, 130.5163774324635142 ) ) ;
#86009 = CARTESIAN_POINT ( 'NONE',  ( 98.30751720600149213, -41.72883398697895529, 47.73978837389122987 ) ) ;
#86010 = EDGE_CURVE ( 'NONE', #71751, #38623, #24064, .T. ) ;
#86011 = CARTESIAN_POINT ( 'NONE',  ( 107.2427983594548948, -47.16656068249876910, 208.5899109901969837 ) ) ;
#86012 = FACE_OUTER_BOUND ( 'NONE', #55163, .T. ) ;
#86013 = DIRECTION ( 'NONE',  ( 0.000000000000000000, 1.000000000000000000, 0.000000000000000000 ) ) ;
#86014 = DIRECTION ( 'NONE',  ( 0.000000000000000000, 0.000000000000000000, -1.000000000000000000 ) ) ;
#86015 = CARTESIAN_POINT ( 'NONE',  ( 97.33784130656839295, -34.07106454601533585, 47.11479194387641201 ) ) ;
#86016 = CARTESIAN_POINT ( 'NONE',  ( 144.1741083578144753, -138.0461846875238905, 247.6591807063120143 ) ) ;
#86017 = EDGE_CURVE ( 'NONE', #829, #43762, #4050, .T. ) ;
#86018 = CARTESIAN_POINT ( 'NONE',  ( 113.3725682976012052, -44.50658906070807319, 98.11867516117681021 ) ) ;
#86019 = CARTESIAN_POINT ( 'NONE',  ( 108.2420053567034017, -46.43931755893584779, 117.6727681330539639 ) ) ;
#86020 = ORIENTED_EDGE ( 'NONE', *, *, #14395, .F. ) ;
#86021 = ORIENTED_EDGE ( 'NONE', *, *, #72155, .F. ) ;
#86022 = CARTESIAN_POINT ( 'NONE',  ( 115.8258230018156354, -33.33084548093709287, 90.54063092494496345 ) ) ;
#86023 = EDGE_CURVE ( 'NONE', #68920, #70782, #24504, .T. ) ;
#86024 = LINE ( 'NONE', #65558, #51554 ) ;
#86026 = CYLINDRICAL_SURFACE ( 'NONE', #10023, 2.116999999999993776 ) ;
#86025 = CARTESIAN_POINT ( 'NONE',  ( 99.34779341711927714, -29.80408710710938891, 231.7565776568629587 ) ) ;
#86027 = CARTESIAN_POINT ( 'NONE',  ( 188.5667039024485518, -48.82844715993430640, 173.2178068554150059 ) ) ;
#86028 = LINE ( 'NONE', #85141, #82887 ) ;
#86029 = EDGE_CURVE ( 'NONE', #52709, #2908, #65390, .T. ) ;
#86030 = DIRECTION ( 'NONE',  ( 1.000000000000000000, 4.299999999999999979E-14, 1.000000000000000078E-15 ) ) ;
#86031 = CARTESIAN_POINT ( 'NONE',  ( 107.0664832912739257, -50.72944715994095333, 312.1356252759112522 ) ) ;
#86032 = AXIS2_PLACEMENT_3D ( 'NONE', #38835, #33368, #67432 ) ;
#86033 = CARTESIAN_POINT ( 'NONE',  ( 0.000000000000000000, 93.07500000000001705, 0.000000000000000000 ) ) ;
#86034 = LINE ( 'NONE', #44207, #3777 ) ;
#86035 = CARTESIAN_POINT ( 'NONE',  ( 101.9826776100855454, -46.51815199768669373, 167.1832443235299763 ) ) ;
#86036 = ORIENTED_EDGE ( 'NONE', *, *, #60049, .T. ) ;
#86037 = ORIENTED_EDGE ( 'NONE', *, *, #37622, .F. ) ;
#86038 = CARTESIAN_POINT ( 'NONE',  ( 112.5622543395261062, -68.63512909430427555, 247.5000682988239760 ) ) ;
#86039 = DIRECTION ( 'NONE',  ( -0.0001713722456129692653, 0.9999999853157764962, 0.000000000000000000 ) ) ;
#86040 = CARTESIAN_POINT ( 'NONE',  ( 99.04406184703033489, -42.84125762489144051, 77.84395860774790776 ) ) ;
#86041 = CARTESIAN_POINT ( 'NONE',  ( 115.0371094337952940, -42.90866003816787355, 104.3022725537445297 ) ) ;
#86042 = CARTESIAN_POINT ( 'NONE',  ( 112.9694095044039841, -31.09161174735247002, 232.2509475124489597 ) ) ;
#86043 = CONICAL_SURFACE ( 'NONE', #25066, 13.31607168056649826, 0.1047197551196538678 ) ;
#86044 = DIRECTION ( 'NONE',  ( -4.237773401492740281E-14, 1.000000000000000000, 0.000000000000000000 ) ) ;
#86045 = CARTESIAN_POINT ( 'NONE',  ( 107.5657785589506688, -47.77162953885341778, 192.6003871806729535 ) ) ;
#86046 = DIRECTION ( 'NONE',  ( 0.000000000000000000, 1.000000000000000000, 0.000000000000000000 ) ) ;
#86047 = EDGE_LOOP ( 'NONE', ( #46140, #25737 ) ) ;
#86049 = ORIENTED_EDGE ( 'NONE', *, *, #84039, .T. ) ;
#86048 = ORIENTED_EDGE ( 'NONE', *, *, #44641, .T. ) ;
#86050 = CARTESIAN_POINT ( 'NONE',  ( 112.4825976992256074, -45.17049497366694766, 64.03124135276239315 ) ) ;
#86051 = CARTESIAN_POINT ( 'NONE',  ( 70.98999999999998067, 52.73749999999999716, -44.45000000000002416 ) ) ;
#86052 = DIRECTION ( 'NONE',  ( 0.000000000000000000, 0.000000000000000000, 1.000000000000000000 ) ) ;
#86053 = CARTESIAN_POINT ( 'NONE',  ( 106.8709381294020488, -45.58890767966684621, 268.9901547344683763 ) ) ;
#86054 = CARTESIAN_POINT ( 'NONE',  ( 115.0372572128023450, -42.90846295832322710, 273.3022919040415672 ) ) ;
#86055 = ORIENTED_EDGE ( 'NONE', *, *, #8787, .T. ) ;
#86056 = EDGE_CURVE ( 'NONE', #53380, #1337, #88106, .T. ) ;
#86057 = CARTESIAN_POINT ( 'NONE',  ( 116.3481150955673087, -39.37902819411457500, 9.635625275910941312 ) ) ;
#86058 = FACE_OUTER_BOUND ( 'NONE', #68183, .T. ) ;
#86059 = ORIENTED_EDGE ( 'NONE', *, *, #42568, .F. ) ;
#86060 = EDGE_LOOP ( 'NONE', ( #66043, #52092, #52498, #42543 ) ) ;
#86061 = AXIS2_PLACEMENT_3D ( 'NONE', #48494, #1286, #36248 ) ;
#86062 = DIRECTION ( 'NONE',  ( -0.9254794337955620787, -0.3787978585227822492, 0.000000000000000000 ) ) ;
#86063 = ORIENTED_EDGE ( 'NONE', *, *, #31166, .T. ) ;
#86064 = VERTEX_POINT ( 'NONE', #18120 ) ;
#86065 = AXIS2_PLACEMENT_3D ( 'NONE', #48708, #89185, #69631 ) ;
#86066 = VECTOR ( 'NONE', #42446, 1000.000000000000000 ) ;
#86067 = CARTESIAN_POINT ( 'NONE',  ( 98.53948418117370522, -33.67937232826720617, 25.48765792331497693 ) ) ;
#86068 = CARTESIAN_POINT ( 'NONE',  ( 116.6812525300504291, -40.81632573062672265, 168.5070538473399608 ) ) ;
#86069 = CARTESIAN_POINT ( 'NONE',  ( 117.2009162446675390, -42.82382785266567993, 128.3956252759109873 ) ) ;
#86070 = DIRECTION ( 'NONE',  ( 1.000000000000000000, 0.000000000000000000, -6.982966722218760189E-15 ) ) ;
#86071 = CARTESIAN_POINT ( 'NONE',  ( 115.9068016902149907, -30.09448287295081670, 260.3508633711493871 ) ) ;
#86072 = CARTESIAN_POINT ( 'NONE',  ( 108.3335911829770453, -46.73484319673156762, 98.67887531062980599 ) ) ;
#86073 = CARTESIAN_POINT ( 'NONE',  ( 75.31670390244798341, -50.82844715994100682, 58.80080685541479824 ) ) ;
#86074 = CARTESIAN_POINT ( 'NONE',  ( -130.4924045281959479, 70.52074417248462623, 4.093845692693608207 ) ) ;
#86075 = ORIENTED_EDGE ( 'NONE', *, *, #23035, .F. ) ;
#86076 = EDGE_LOOP ( 'NONE', ( #12977, #42109, #6224, #37837 ) ) ;
#86077 = ADVANCED_FACE ( 'NONE', ( #52607 ), #24944, .F. ) ;
#86078 = CARTESIAN_POINT ( 'NONE',  ( 117.4703304800641206, -30.95114626853415984, 179.2299109901959753 ) ) ;
#86079 = ORIENTED_EDGE ( 'NONE', *, *, #69904, .F. ) ;
#86080 = CARTESIAN_POINT ( 'NONE',  ( 96.74292298454378169, -35.27647329413149890, 181.2156252759109805 ) ) ;
#86081 = CARTESIAN_POINT ( 'NONE',  ( 164.9190312289450162, -35.91149509760580116, 117.4678068554150485 ) ) ;
#86082 = AXIS2_PLACEMENT_3D ( 'NONE', #26990, #1422, #8231 ) ;
#86083 = CARTESIAN_POINT ( 'NONE',  ( 25.56670390244731550, -48.82844715994178841, 175.7178068554150627 ) ) ;
#86084 = DIRECTION ( 'NONE',  ( 0.000000000000000000, 1.000000000000000000, 0.000000000000000000 ) ) ;
#86087 = CARTESIAN_POINT ( 'NONE',  ( 99.39760893136107711, -29.69972230079153519, 271.7356252759109907 ) ) ;
#86086 = FACE_OUTER_BOUND ( 'NONE', #37794, .T. ) ;
#86085 = DIRECTION ( 'NONE',  ( -3.114895971316861016E-16, 1.000000000000000000, 0.000000000000000000 ) ) ;
#86088 = CARTESIAN_POINT ( 'NONE',  ( 182.5667039024469886, -33.35206098992650681, -5.074374724088000832 ) ) ;
#86089 = CARTESIAN_POINT ( 'NONE',  ( 107.0664832912739399, -36.72944715994095333, 293.6369201390379544 ) ) ;
#86090 = CARTESIAN_POINT ( 'NONE',  ( 80.06648329127399677, -8.350947159940998787, 306.1181252759120071 ) ) ;
#86091 = AXIS2_PLACEMENT_3D ( 'NONE', #3223, #9586, #9146 ) ;
#86092 = CARTESIAN_POINT ( 'NONE',  ( 67.28251452665169552, -137.5317448489894332, 246.4199739687819317 ) ) ;
#86093 = DIRECTION ( 'NONE',  ( -0.7071067811865474617, 0.000000000000000000, -0.7071067811865474617 ) ) ;
#86094 = PLANE ( 'NONE',  #15860 ) ;
#86096 = VERTEX_POINT ( 'NONE', #59446 ) ;
#86095 = CARTESIAN_POINT ( 'NONE',  ( 102.5058979696208041, -43.38806787210953786, 195.5838068554170661 ) ) ;
#86097 = CARTESIAN_POINT ( 'NONE',  ( 135.3099415725432095, -21.18303583363543297, 7.982915248818459375 ) ) ;
#86098 = CARTESIAN_POINT ( 'NONE',  ( 99.99311136543857970, -27.18998042936580362, 185.5841967044829630 ) ) ;
#86099 = CARTESIAN_POINT ( 'NONE',  ( 98.59006141831567049, -43.82340604873675716, 67.86895860924497015 ) ) ;
#86100 = CARTESIAN_POINT ( 'NONE',  ( 100.7971853062899896, -45.88878125878837011, 238.1108633711489517 ) ) ;
#86101 = DIRECTION ( 'NONE',  ( 0.9659258262890695335, 0.000000000000000000, -0.2588190451025166317 ) ) ;
#86102 = DIRECTION ( 'NONE',  ( 0.000000000000000000, 1.000000000000000000, 0.000000000000000000 ) ) ;
#86104 = DIRECTION ( 'NONE',  ( 0.000000000000000000, 0.000000000000000000, 1.000000000000000000 ) ) ;
#86103 = DIRECTION ( 'NONE',  ( -1.000000000000000000, -8.163404592832032979E-16, 0.000000000000000000 ) ) ;
#86105 = DIRECTION ( 'NONE',  ( -0.7071067811865187069, -0.7071067811865764385, -7.071067811865181482E-16 ) ) ;
#86106 = DIRECTION ( 'NONE',  ( 0.000000000000000000, -1.000000000000000000, 0.000000000000000000 ) ) ;
#86107 = ORIENTED_EDGE ( 'NONE', *, *, #20787, .F. ) ;
#86108 = VECTOR ( 'NONE', #76500, 1000.000000000000000 ) ;
#86109 = DIRECTION ( 'NONE',  ( -0.9254794337955620787, -0.3787978585227822492, 0.000000000000000000 ) ) ;
#86110 = ORIENTED_EDGE ( 'NONE', *, *, #11022, .F. ) ;
#86111 = ORIENTED_EDGE ( 'NONE', *, *, #81304, .T. ) ;
#86112 = EDGE_CURVE ( 'NONE', #80585, #62559, #52167, .T. ) ;
#86113 = CARTESIAN_POINT ( 'NONE',  ( 107.7867742379091567, -27.70205266993799142, 114.4476579233149636 ) ) ;
#86115 = ORIENTED_EDGE ( 'NONE', *, *, #57465, .F. ) ;
#86114 = LINE ( 'NONE', #3876, #60388 ) ;
#86116 = EDGE_CURVE ( 'NONE', #67833, #68744, #32640, .T. ) ;
#86117 = CARTESIAN_POINT ( 'NONE',  ( 116.5135284680787322, -32.37261310794437463, 100.1699109901969535 ) ) ;
#86118 = PLANE ( 'NONE',  #10594 ) ;
#86119 = EDGE_CURVE ( 'NONE', #84817, #2920, #10423, .T. ) ;
#86120 = CARTESIAN_POINT ( 'NONE',  ( 77.55659459556460433, -17.60518703966017640, 7.068229416970193135 ) ) ;
#86121 = CARTESIAN_POINT ( 'NONE',  ( 142.8832909413445122, -79.11588146349311046, 361.9756252759100335 ) ) ;
#86122 = EDGE_CURVE ( 'NONE', #74315, #71626, #89524, .T. ) ;
#86123 = CARTESIAN_POINT ( 'NONE',  ( 111.8803212371932148, -27.54331830560560590, 14.68038718067299442 ) ) ;
#86124 = VERTEX_POINT ( 'NONE', #11765 ) ;
#86125 = VERTEX_POINT ( 'NONE', #65818 ) ;
#86126 = EDGE_LOOP ( 'NONE', ( #4717, #37120, #56312, #21157, #79346 ) ) ;
#86127 = CARTESIAN_POINT ( 'NONE',  ( 57.56670390244747892, -48.82844715994040286, 137.2178068554150911 ) ) ;
#86129 = VECTOR ( 'NONE', #61794, 1000.000000000000000 ) ;
#86128 = CYLINDRICAL_SURFACE ( 'NONE', #20243, 4.762500000000002842 ) ;
#86130 = CARTESIAN_POINT ( 'NONE',  ( 46.03715912545343514, -48.62818131006090283, 180.4678068554150911 ) ) ;
#86131 = PLANE ( 'NONE',  #24767 ) ;
#86132 = CYLINDRICAL_SURFACE ( 'NONE', #50954, 88.90000000000000568 ) ;
#86133 = ADVANCED_FACE ( 'NONE', ( #3603, #87617 ), #80820, .T. ) ;
#86134 = FACE_OUTER_BOUND ( 'NONE', #6950, .T. ) ;
#86135 = CARTESIAN_POINT ( 'NONE',  ( -10.56631526105568142, 89.59577849103433778, 130.1277146807724421 ) ) ;
#86136 = CARTESIAN_POINT ( 'NONE',  ( 103.9639062230918825, -47.31423993612443724, 62.33753003781600199 ) ) ;
#86137 = EDGE_LOOP ( 'NONE', ( #64084, #80015, #63012, #41116 ) ) ;
#86138 = FACE_OUTER_BOUND ( 'NONE', #53165, .T. ) ;
#86139 = CARTESIAN_POINT ( 'NONE',  ( 126.8569334184371797, 48.66001727116653086, 30.85758840523601876 ) ) ;
#86140 = DIRECTION ( 'NONE',  ( 1.000000000000000000, 4.237773401492740281E-14, 0.000000000000000000 ) ) ;
#86141 = CARTESIAN_POINT ( 'NONE',  ( 108.0140583617620820, -28.59404368299928123, 127.8023760838769505 ) ) ;
#86142 = AXIS2_PLACEMENT_3D ( 'NONE', #77649, #65350, #71728 ) ;
#86143 = VECTOR ( 'NONE', #72141, 1000.000000000000000 ) ;
#86144 = CARTESIAN_POINT ( 'NONE',  ( 107.0664832912739257, -52.72944715994094622, 302.7856252759109452 ) ) ;
#86145 = CARTESIAN_POINT ( 'NONE',  ( 107.0664832912740110, -46.47944715994103149, 14.92562527591097066 ) ) ;
#86146 = ORIENTED_EDGE ( 'NONE', *, *, #7663, .T. ) ;
#86147 = VERTEX_POINT ( 'NONE', #73986 ) ;
#86148 = LINE ( 'NONE', #66122, #87387 ) ;
#86149 = TOROIDAL_SURFACE ( 'NONE', #67256, 36.57600000000000051, 1.524000000000000021 ) ;
#86150 = ORIENTED_EDGE ( 'NONE', *, *, #39746, .T. ) ;
#86151 = ORIENTED_EDGE ( 'NONE', *, *, #75938, .T. ) ;
#86152 = CARTESIAN_POINT ( 'NONE',  ( 116.1908163682739712, -34.48822628859398520, 160.4377737820879588 ) ) ;
#86153 = DIRECTION ( 'NONE',  ( -1.000000000000000000, 0.000000000000000000, 0.000000000000000000 ) ) ;
#86155 = EDGE_CURVE ( 'NONE', #7552, #69846, #61944, .T. ) ;
#86154 = CARTESIAN_POINT ( 'NONE',  ( 99.40614514399899804, -27.65486269830070398, 146.6356252759109395 ) ) ;
#86156 = CARTESIAN_POINT ( 'NONE',  ( 143.5667039024469886, -67.87844715994090450, 55.21780685541800437 ) ) ;
#86157 = CARTESIAN_POINT ( 'NONE',  ( 99.04406183952015397, -42.84125761515226571, 82.84395860677673795 ) ) ;
#86158 = EDGE_LOOP ( 'NONE', ( #83710, #57827 ) ) ;
#86159 = ORIENTED_EDGE ( 'NONE', *, *, #82650, .T. ) ;
#86160 = B_SPLINE_CURVE_WITH_KNOTS ( 'NONE', 3,
 ( #30088, #56879, #84623, #22381, #58234, #42344, #50060, #52714, #3280, #11423, #37795, #39567, #60452, #66372, #24172, #79592, #32297, #45032 ),
 .UNSPECIFIED., .F., .F.,
 ( 4, 2, 2, 2, 2, 2, 2, 2, 4 ),
 ( 0.000000000000000000, 0.06249555305220369505, 0.1249911061044073901, 0.1874866591566110852, 0.2499822122088147802, 0.3124777652610184475, 0.3749733183132221703, 0.4374688713654258931, 0.4999644244176295604 ),
 .UNSPECIFIED. ) ;
#86161 = VERTEX_POINT ( 'NONE', #44479 ) ;
#86162 = EDGE_CURVE ( 'NONE', #43418, #84840, #45365, .T. ) ;
#86163 = CARTESIAN_POINT ( 'NONE',  ( 107.5268921225462719, -45.37172398690709230, 195.4490427505439811 ) ) ;
#86164 = CARTESIAN_POINT ( 'NONE',  ( 115.0395865772315034, -43.53517906860128051, 63.26419670448196797 ) ) ;
#86165 = ORIENTED_EDGE ( 'NONE', *, *, #45922, .F. ) ;
#86166 = CARTESIAN_POINT ( 'NONE',  ( 99.77739493559400330, -44.20163642594134501, 21.96133956162593748 ) ) ;
#86167 = DIRECTION ( 'NONE',  ( -4.012088370409549976E-14, 1.000000000000000000, 0.000000000000000000 ) ) ;
#86168 = LINE ( 'NONE', #3930, #61185 ) ;
#86169 = CARTESIAN_POINT ( 'NONE',  ( 83.06670390244796920, -58.72944715994093912, 207.5838068554149913 ) ) ;
#86170 = CARTESIAN_POINT ( 'NONE',  ( 97.79428472817266993, -42.74653246722733257, 142.7965776568629508 ) ) ;
#86171 = CARTESIAN_POINT ( 'NONE',  ( 12.70000000000000107, 82.54999999999999716, -117.8738102209307641 ) ) ;
#86172 = VERTEX_POINT ( 'NONE', #87178 ) ;
#86173 = DIRECTION ( 'NONE',  ( -1.000000000000000000, 0.000000000000000000, -1.531877379624855416E-14 ) ) ;
#86174 = ORIENTED_EDGE ( 'NONE', *, *, #78243, .F. ) ;
#86175 = CARTESIAN_POINT ( 'NONE',  ( 147.0667039024470171, -77.84948640091441519, 245.5415602474340062 ) ) ;
#86176 = ORIENTED_EDGE ( 'NONE', *, *, #87521, .F. ) ;
#86177 = VERTEX_POINT ( 'NONE', #9984 ) ;
#86178 = CONICAL_SURFACE ( 'NONE', #84776, 11.57110091390434192, 0.7853981633974471688 ) ;
#86179 = LINE ( 'NONE', #58450, #66347 ) ;
#86180 = ADVANCED_FACE ( 'NONE', ( #80370 ), #58555, .F. ) ;
#86181 = DIRECTION ( 'NONE',  ( 1.000000000000000078E-15, -1.000000000000000000, 0.000000000000000000 ) ) ;
#86182 = CARTESIAN_POINT ( 'NONE',  ( 111.9289591080100053, -27.50755150920414849, 59.68991099019693536 ) ) ;
#86183 = DIRECTION ( 'NONE',  ( -0.4214249218767882055, -0.9068632946707806397, -4.214249218767890910E-16 ) ) ;
#86184 = AXIS2_PLACEMENT_3D ( 'NONE', #39134, #52279, #88203 ) ;
#86185 = CARTESIAN_POINT ( 'NONE',  ( 108.0345720930109081, -87.33724612030414391, -19.23816774842054755 ) ) ;
#86186 = FACE_BOUND ( 'NONE', #10920, .T. ) ;
#86187 = CARTESIAN_POINT ( 'NONE',  ( 97.55373691267104164, -39.00345059616621768, 56.51276813305494784 ) ) ;
#86189 = CARTESIAN_POINT ( 'NONE',  ( 102.6926969729870507, -27.29023857175978662, 176.4213395616249898 ) ) ;
#86188 = CARTESIAN_POINT ( 'NONE',  ( 131.3179999999999836, 53.97500000000000142, 30.16249999999999787 ) ) ;
#86190 = CARTESIAN_POINT ( 'NONE',  ( 165.9667039024459996, -26.71338133339301635, -5.074374724088000832 ) ) ;
#86191 = DIRECTION ( 'NONE',  ( 1.000000000000000000, 3.999999999999999995E-14, 1.000000000000000078E-15 ) ) ;
#86192 = ORIENTED_EDGE ( 'NONE', *, *, #51452, .F. ) ;
#86193 = DIRECTION ( 'NONE',  ( 3.999999999999999995E-14, -1.000000000000000000, 4.100000000000000342E-29 ) ) ;
#86194 = DIRECTION ( 'NONE',  ( 4.299999999999999979E-14, -1.000000000000000000, 4.400000000000000367E-29 ) ) ;
#86195 = DIRECTION ( 'NONE',  ( -1.000000000000000000, 0.000000000000000000, 6.982966722218760189E-15 ) ) ;
#86196 = EDGE_CURVE ( 'NONE', #30286, #56525, #61242, .T. ) ;
#86197 = DIRECTION ( 'NONE',  ( -2.106816776397999944E-14, 1.000000000000000000, -2.206816776398000223E-29 ) ) ;
#86199 = EDGE_LOOP ( 'NONE', ( #49678, #6122 ) ) ;
#86198 = CARTESIAN_POINT ( 'NONE',  ( 97.05395071892901626, -41.52132310946490890, 216.6937205140059461 ) ) ;
#86200 = CARTESIAN_POINT ( 'NONE',  ( 172.5664832912729878, -27.57844715994070484, 258.9256252759120116 ) ) ;
#86201 = CARTESIAN_POINT ( 'NONE',  ( 115.0714481855697926, -30.01693675811307571, 265.3813395616251682 ) ) ;
#86202 = CARTESIAN_POINT ( 'NONE',  ( 114.7393473568293700, -44.74971245420289279, 109.1718157521009687 ) ) ;
#86203 = CARTESIAN_POINT ( 'NONE',  ( 31.75000000000000000, 24.56180297284579694, 3.174999999999999822 ) ) ;
#86204 = CARTESIAN_POINT ( 'NONE',  ( 57.56670390244718760, -42.82844715994040996, 173.2178068554150911 ) ) ;
#86205 = FACE_OUTER_BOUND ( 'NONE', #63534, .T. ) ;
#86206 = DIRECTION ( 'NONE',  ( 0.000000000000000000, 0.000000000000000000, -1.000000000000000000 ) ) ;
#86207 = ORIENTED_EDGE ( 'NONE', *, *, #67549, .F. ) ;
#86208 = AXIS2_PLACEMENT_3D ( 'NONE', #34393, #28477, #55707 ) ;
#86209 = VECTOR ( 'NONE', #26703, 1000.000000000000000 ) ;
#86210 = AXIS2_PLACEMENT_3D ( 'NONE', #70771, #8996, #8089 ) ;
#86211 = ORIENTED_EDGE ( 'NONE', *, *, #31867, .F. ) ;
#86212 = VERTEX_POINT ( 'NONE', #12211 ) ;
#86213 = CIRCLE ( 'NONE', #60045, 7.499999999999992895 ) ;
#86214 = EDGE_LOOP ( 'NONE', ( #54424, #73973, #49739, #70900, #14966, #29952, #17240, #5494 ) ) ;
#86215 = DIRECTION ( 'NONE',  ( 0.7071067811865491270, -0.7071067811865459074, 7.071067811865492096E-16 ) ) ;
#86216 = CARTESIAN_POINT ( 'NONE',  ( 116.5364499171840720, -42.42977282487416346, 274.3832443235299365 ) ) ;
#86217 = DIRECTION ( 'NONE',  ( -0.08544974978095701279, -0.9963424814100680926, 0.000000000000000000 ) ) ;
#86218 = FACE_OUTER_BOUND ( 'NONE', #44958, .T. ) ;
#86219 = ADVANCED_FACE ( 'NONE', ( #19467 ), #48478, .T. ) ;
#86221 = CARTESIAN_POINT ( 'NONE',  ( 75.38287938184939208, 76.93600387762164416, 91.50401754987846914 ) ) ;
#86220 = CARTESIAN_POINT ( 'NONE',  ( 172.5667039024480687, -42.82844715993500273, 300.4678068554149490 ) ) ;
#86222 = CARTESIAN_POINT ( 'NONE',  ( 87.31648329127401098, -36.72944715994105991, 14.92562527591095112 ) ) ;
#86223 = CARTESIAN_POINT ( 'NONE',  ( 98.52747904795083400, -36.52563780154032003, 195.7295626852199462 ) ) ;
#86224 = EDGE_LOOP ( 'NONE', ( #12774, #74600 ) ) ;
#86225 = EDGE_LOOP ( 'NONE', ( #61171, #80751 ) ) ;
#86226 = EDGE_LOOP ( 'NONE', ( #66903, #69151, #30686, #7185 ) ) ;
#86227 = FACE_BOUND ( 'NONE', #9322, .T. ) ;
#86228 = CARTESIAN_POINT ( 'NONE',  ( 108.3331741162412811, -46.73489075662012482, 182.6773131391069853 ) ) ;
#86229 = CARTESIAN_POINT ( 'NONE',  ( 100.6696166679599713, -29.33055989933774299, 256.6441967044817147 ) ) ;
#86230 = DIRECTION ( 'NONE',  ( -0.7071067811861110330, -0.7071067811869841124, 0.000000000000000000 ) ) ;
#86231 = EDGE_CURVE ( 'NONE', #59341, #87723, #40799, .T. ) ;
#86232 = PLANE ( 'NONE',  #62166 ) ;
#86233 = ADVANCED_FACE ( 'NONE', ( #5856 ), #81273, .T. ) ;
#86234 = CARTESIAN_POINT ( 'NONE',  ( 25.56670390244797275, -67.87844715994100397, 142.0928068554150059 ) ) ;
#86235 = EDGE_LOOP ( 'NONE', ( #53276, #78080, #52004, #69934 ) ) ;
#86236 = CARTESIAN_POINT ( 'NONE',  ( 104.0201293345620286, -27.19852536998958925, 56.32266916734289453 ) ) ;
#86237 = EDGE_LOOP ( 'NONE', ( #71162, #32159, #17319, #64328, #24704, #58332 ) ) ;
#86238 = CYLINDRICAL_SURFACE ( 'NONE', #3190, 218.1859999999999786 ) ;
#86239 = CARTESIAN_POINT ( 'NONE',  ( 111.0677264286952521, -45.23305914580045339, 284.3463452106589102 ) ) ;
#86240 = AXIS2_PLACEMENT_3D ( 'NONE', #40935, #13687, #47295 ) ;
#86241 = CARTESIAN_POINT ( 'NONE',  ( 74.15067561874209900, 120.6499999999999915, 68.53801554307469246 ) ) ;
#86242 = AXIS2_PLACEMENT_3D ( 'NONE', #85765, #44386, #9440 ) ;
#86243 = CARTESIAN_POINT ( 'NONE',  ( 194.0371591254575492, -24.42818131005417115, 117.4678068554150627 ) ) ;
#86244 = LINE ( 'NONE', #58080, #24210 ) ;
#86245 = VERTEX_POINT ( 'NONE', #19920 ) ;
#86246 = FACE_OUTER_BOUND ( 'NONE', #45872, .T. ) ;
#86247 = CARTESIAN_POINT ( 'NONE',  ( 151.0371591254585155, -46.82818131005592477, 129.9678068554149775 ) ) ;
#86248 = ORIENTED_EDGE ( 'NONE', *, *, #46823, .F. ) ;
#86249 = CARTESIAN_POINT ( 'NONE',  ( 112.7599586733956727, -27.95389904326713904, 69.61848241876793963 ) ) ;
#86250 = ORIENTED_EDGE ( 'NONE', *, *, #8590, .F. ) ;
#86251 = CARTESIAN_POINT ( 'NONE',  ( 114.1634876701351402, -42.35485373834646339, 47.72765792331495760 ) ) ;
#86252 = CARTESIAN_POINT ( 'NONE',  ( 116.3228127852087113, -32.93589129790882453, 90.13562527591095375 ) ) ;
#86253 = CARTESIAN_POINT ( 'NONE',  ( 116.3620231750148406, -38.09673052741934640, 70.15396425827796634 ) ) ;
#86254 = CARTESIAN_POINT ( 'NONE',  ( 104.4075039567214134, -46.45791419004698497, 13.36474276782575465 ) ) ;
#86255 = DIRECTION ( 'NONE',  ( -1.000000000000000000, 0.000000000000000000, 0.000000000000000000 ) ) ;
#86256 = CARTESIAN_POINT ( 'NONE',  ( 67.06681409635508828, -67.87844715994098976, 245.5130139786259917 ) ) ;
#86257 = CARTESIAN_POINT ( 'NONE',  ( 115.7467025339723250, -43.60978142820201242, 44.30514908543492680 ) ) ;
#86258 = LINE ( 'NONE', #17225, #62827 ) ;
#86259 = ORIENTED_EDGE ( 'NONE', *, *, #3466, .F. ) ;
#86260 = DIRECTION ( 'NONE',  ( 0.5000000000000015543, -0.8660254037844377084, 2.602085213965216006E-14 ) ) ;
#86261 = AXIS2_PLACEMENT_3D ( 'NONE', #56135, #48874, #69801 ) ;
#86262 = ORIENTED_EDGE ( 'NONE', *, *, #71175, .T. ) ;
#86263 = CARTESIAN_POINT ( 'NONE',  ( 99.06808600115306263, -45.54042523694053557, 152.9899109901969894 ) ) ;
#86264 = CARTESIAN_POINT ( 'NONE',  ( 78.98444042533783715, -21.25772566032899746, 1.807989669955657019 ) ) ;
#86265 = AXIS2_PLACEMENT_3D ( 'NONE', #83204, #77731, #43179 ) ;
#86266 = AXIS2_PLACEMENT_3D ( 'NONE', #2217, #84456, #64889 ) ;
#86267 = CIRCLE ( 'NONE', #47075, 9.525000000000000355 ) ;
#86268 = ORIENTED_EDGE ( 'NONE', *, *, #18411, .F. ) ;
#86269 = VERTEX_POINT ( 'NONE', #69416 ) ;
#86270 = EDGE_CURVE ( 'NONE', #39062, #71292, #48048, .T. ) ;
#86271 = DIRECTION ( 'NONE',  ( 1.000000000000000078E-15, -1.000000000000000000, 0.000000000000000000 ) ) ;
#86272 = AXIS2_PLACEMENT_3D ( 'NONE', #3663, #79538, #31359 ) ;
#86273 = LINE ( 'NONE', #51720, #31842 ) ;
#86274 = CARTESIAN_POINT ( 'NONE',  ( 114.9410966442422648, -29.98191058901448969, 229.4022919425779605 ) ) ;
#86275 = CARTESIAN_POINT ( 'NONE',  ( 97.50743367704620823, -39.67470400402397246, 126.5637992372244156 ) ) ;
#86276 = DIRECTION ( 'NONE',  ( 0.000000000000000000, 1.000000000000000000, 0.000000000000000000 ) ) ;
#86277 = CARTESIAN_POINT ( 'NONE',  ( 104.4907123320104461, -46.86782655419724364, 43.37848241876896083 ) ) ;
#86278 = CARTESIAN_POINT ( 'NONE',  ( 108.3330981890487550, -46.73490692371524347, 43.67726424760522264 ) ) ;
#86279 = EDGE_LOOP ( 'NONE', ( #61328, #10491, #21080, #45693 ) ) ;
#86280 = CARTESIAN_POINT ( 'NONE',  ( 114.7582354846073827, -30.31413633156125087, 170.3796143784777257 ) ) ;
#86281 = CARTESIAN_POINT ( 'NONE',  ( 107.0664832912739399, -50.04691774669244353, 305.7008218191032256 ) ) ;
#86282 = ORIENTED_EDGE ( 'NONE', *, *, #24893, .T. ) ;
#86283 = CARTESIAN_POINT ( 'NONE',  ( 107.0667039024479834, -36.72944715994099596, 239.5838068554170093 ) ) ;
#86284 = EDGE_CURVE ( 'NONE', #2245, #79375, #62141, .T. ) ;
#86285 = FACE_OUTER_BOUND ( 'NONE', #19898, .T. ) ;
#86286 = CARTESIAN_POINT ( 'NONE',  ( 113.2071528006340628, -45.12711609280825087, 228.0784824187679760 ) ) ;
#86287 = VECTOR ( 'NONE', #7533, 1000.000000000000000 ) ;
#86288 = EDGE_CURVE ( 'NONE', #41217, #32950, #67784, .T. ) ;
#86289 = FACE_BOUND ( 'NONE', #26511, .T. ) ;
#86290 = DIRECTION ( 'NONE',  ( 0.000000000000000000, 0.000000000000000000, -1.000000000000000000 ) ) ;
#86291 = CARTESIAN_POINT ( 'NONE',  ( 98.63544605819593869, -40.03554478408833006, 246.0343245899819919 ) ) ;
#86293 = CARTESIAN_POINT ( 'NONE',  ( 103.6060256796756960, -46.54035428658114171, 53.30705384733997221 ) ) ;
#86292 = FACE_OUTER_BOUND ( 'NONE', #74560, .T. ) ;
#86294 = CARTESIAN_POINT ( 'NONE',  ( 118.9099480661945165, 74.38787642755048068, 53.90531644923896692 ) ) ;
#86295 = CARTESIAN_POINT ( 'NONE',  ( 107.9493508131109962, -25.66448314884807047, 115.0251490854349612 ) ) ;
#86296 = ORIENTED_EDGE ( 'NONE', *, *, #68684, .T. ) ;
#86297 = PLANE ( 'NONE',  #4617 ) ;
#86298 = ORIENTED_EDGE ( 'NONE', *, *, #32960, .F. ) ;
#86299 = ADVANCED_FACE ( 'NONE', ( #60338 ), #19020, .T. ) ;
#86300 = LINE ( 'NONE', #58569, #56925 ) ;
#86301 = CARTESIAN_POINT ( 'NONE',  ( 172.5664832912729878, -27.82844715994070484, 318.9256252759120116 ) ) ;
#86302 = DIRECTION ( 'NONE',  ( 0.000000000000000000, 0.000000000000000000, -1.000000000000000000 ) ) ;
#86303 = VERTEX_POINT ( 'NONE', #88964 ) ;
#86304 = EDGE_CURVE ( 'NONE', #28720, #19975, #50402, .T. ) ;
#86305 = EDGE_CURVE ( 'NONE', #39081, #75765, #26280, .T. ) ;
#86306 = LINE ( 'NONE', #46728, #83893 ) ;
#86307 = EDGE_LOOP ( 'NONE', ( #20469, #72911 ) ) ;
#86308 = LINE ( 'NONE', #73109, #16032 ) ;
#86309 = CARTESIAN_POINT ( 'NONE',  ( 167.6524903400756159, -49.32844715993520879, 129.9678068554150059 ) ) ;
#86310 = EDGE_CURVE ( 'NONE', #37287, #89758, #67616, .T. ) ;
#86311 = CARTESIAN_POINT ( 'NONE',  ( 0.000000000000000000, 95.25000000000000000, 0.000000000000000000 ) ) ;
#86312 = EDGE_CURVE ( 'NONE', #18344, #42921, #79421, .T. ) ;
#86313 = ORIENTED_EDGE ( 'NONE', *, *, #14732, .T. ) ;
#86314 = CARTESIAN_POINT ( 'NONE',  ( 112.8139912305532704, -47.12176010715679553, 102.9784824187679817 ) ) ;
#86315 = DIRECTION ( 'NONE',  ( 1.000000000000000000, 0.000000000000000000, 0.000000000000000000 ) ) ;
#86316 = AXIS2_PLACEMENT_3D ( 'NONE', #85654, #9333, #42934 ) ;
#86317 = ADVANCED_FACE ( 'NONE', ( #75336 ), #5399, .F. ) ;
#86318 = DIRECTION ( 'NONE',  ( 0.8571673007021115565, -0.5150380749100554878, 7.521945815882500121E-16 ) ) ;
#86319 = CARTESIAN_POINT ( 'NONE',  ( 134.0664832912740110, -41.22944715994101017, 4.925625275910997303 ) ) ;
#86320 = DIRECTION ( 'NONE',  ( 7.067626426349370916E-15, 0.000000000000000000, -1.000000000000000000 ) ) ;
#86321 = ORIENTED_EDGE ( 'NONE', *, *, #81401, .F. ) ;
#86322 = DIRECTION ( 'NONE',  ( 1.000000000000000000, 4.163336342344333240E-14, 0.000000000000000000 ) ) ;
#86323 = PLANE ( 'NONE',  #84601 ) ;
#86324 = EDGE_CURVE ( 'NONE', #55190, #86673, #60794, .T. ) ;
#86325 = CARTESIAN_POINT ( 'NONE',  ( 205.0097499999990305, 52.73749999999999716, -39.68750000000000000 ) ) ;
#86327 = LINE ( 'NONE', #72701, #51415 ) ;
#86326 = CARTESIAN_POINT ( 'NONE',  ( 41.56648329127398966, -27.57844715994070484, 18.92562527591200094 ) ) ;
#86328 = LINE ( 'NONE', #30025, #43661 ) ;
#86329 = VECTOR ( 'NONE', #47318, 1000.000000000000000 ) ;
#86330 = ORIENTED_EDGE ( 'NONE', *, *, #23044, .F. ) ;
#86331 = AXIS2_PLACEMENT_3D ( 'NONE', #84798, #50239, #83435 ) ;
#86332 = VECTOR ( 'NONE', #56865, 1000.000000000000000 ) ;
#86333 = CARTESIAN_POINT ( 'NONE',  ( 115.7831077080300304, -41.80230944217467481, 34.40645861541539574 ) ) ;
#86334 = CARTESIAN_POINT ( 'NONE',  ( 116.8431970675091662, -40.18699730018602168, 174.5680062282909546 ) ) ;
#86335 = B_SPLINE_CURVE_WITH_KNOTS ( 'NONE', 3,
 ( #21828, #7736, #16346, #77233 ),
 .UNSPECIFIED., .F., .F.,
 ( 4, 4 ),
 ( -0.3974825557268080178, -0.3842043193313759986 ),
 .UNSPECIFIED. ) ;
#86337 = VERTEX_POINT ( 'NONE', #54853 ) ;
#86336 = LINE ( 'NONE', #79083, #51567 ) ;
#86338 = CIRCLE ( 'NONE', #45709, 10.00000000000000355 ) ;
#86339 = ADVANCED_FACE ( 'NONE', ( #20377 ), #82616, .F. ) ;
#86340 = CARTESIAN_POINT ( 'NONE',  ( 112.3272512417296554, -28.22507648531182056, 285.6356252759109680 ) ) ;
#86341 = DIRECTION ( 'NONE',  ( -0.7071067811864613084, 0.7071067811866338371, -7.071067811864621391E-16 ) ) ;
#86343 = EDGE_CURVE ( 'NONE', #8253, #26639, #8343, .T. ) ;
#86342 = CARTESIAN_POINT ( 'NONE',  ( 19.56648329127400032, 25.62155284005901379, 323.8756252759109202 ) ) ;
#86344 = FACE_OUTER_BOUND ( 'NONE', #16551, .T. ) ;
#86345 = EDGE_CURVE ( 'NONE', #31932, #33837, #31529, .T. ) ;
#86346 = AXIS2_PLACEMENT_3D ( 'NONE', #9920, #58059, #78530 ) ;
#86347 = ORIENTED_EDGE ( 'NONE', *, *, #66782, .T. ) ;
#86348 = CARTESIAN_POINT ( 'NONE',  ( 112.1405701860857675, -28.01352448884034985, 29.65657790821143891 ) ) ;
#86349 = EDGE_CURVE ( 'NONE', #70164, #38056, #71661, .T. ) ;
#86350 = ORIENTED_EDGE ( 'NONE', *, *, #58210, .F. ) ;
#86351 = ORIENTED_EDGE ( 'NONE', *, *, #89114, .F. ) ;
#86352 = AXIS2_PLACEMENT_3D ( 'NONE', #69682, #76492, #82881 ) ;
#86353 = CARTESIAN_POINT ( 'NONE',  ( 104.9381124493903457, -46.57529615900893560, 178.8387261630399507 ) ) ;
#86354 = DIRECTION ( 'NONE',  ( 1.000000000000000078E-15, 1.000000000000000083E-30, -1.000000000000000000 ) ) ;
#86355 = CARTESIAN_POINT ( 'NONE',  ( 109.2565852557048629, -45.31616550848684000, 44.20729759161095984 ) ) ;
#86356 = CARTESIAN_POINT ( 'NONE',  ( 23.22048716318218098, 86.68168211238419474, 300.5057518000332948 ) ) ;
#86357 = AXIS2_PLACEMENT_3D ( 'NONE', #77828, #44171, #71470 ) ;
#86358 = DIRECTION ( 'NONE',  ( 0.000000000000000000, 0.000000000000000000, -1.000000000000000000 ) ) ;
#86359 = LINE ( 'NONE', #72722, #936 ) ;
#86360 = ORIENTED_EDGE ( 'NONE', *, *, #74093, .T. ) ;
#86361 = DIRECTION ( 'NONE',  ( -1.000000000000000000, 0.000000000000000000, 2.973811673103097665E-16 ) ) ;
#86362 = CARTESIAN_POINT ( 'NONE',  ( 66.21896343372186777, -72.55791859125355359, 542.9756252759101471 ) ) ;
#86363 = EDGE_LOOP ( 'NONE', ( #2667, #88135, #3821, #682 ) ) ;
#86364 = CARTESIAN_POINT ( 'NONE',  ( 97.24442698086039627, -40.26379795196659472, 266.6013395616254797 ) ) ;
#86365 = FACE_OUTER_BOUND ( 'NONE', #85282, .T. ) ;
#86366 = ORIENTED_EDGE ( 'NONE', *, *, #54565, .F. ) ;
#86367 = CARTESIAN_POINT ( 'NONE',  ( 117.0718954855324228, -35.46248235742579880, 83.92729194248475721 ) ) ;
#86368 = CARTESIAN_POINT ( 'NONE',  ( -7.205548786489490269E-13, 127.0000000000000000, 103.1875000000000000 ) ) ;
#86369 = DIRECTION ( 'NONE',  ( -6.524622321627019585E-16, -4.013151879589939944E-16, -1.000000000000000000 ) ) ;
#86370 = PLANE ( 'NONE',  #69461 ) ;
#86371 = CARTESIAN_POINT ( 'NONE',  ( 97.99904154034810233, -44.43610744809739543, 222.8870538473399563 ) ) ;
#86372 = DIRECTION ( 'NONE',  ( 1.000000000000000000, 0.000000000000000000, 0.000000000000000000 ) ) ;
#86373 = ORIENTED_EDGE ( 'NONE', *, *, #18657, .T. ) ;
#86374 = CARTESIAN_POINT ( 'NONE',  ( 101.1169593292293598, -28.07258979649007102, 46.55562527591094835 ) ) ;
#86375 = CARTESIAN_POINT ( 'NONE',  ( -446.0240000000000009, 93.66249999999999432, 95.25000000000000000 ) ) ;
#86376 = VECTOR ( 'NONE', #81309, 1000.000000000000000 ) ;
#86377 = CARTESIAN_POINT ( 'NONE',  ( 105.8935610739654010, -47.12417332243212087, 282.4870538473394390 ) ) ;
#86378 = ORIENTED_EDGE ( 'NONE', *, *, #32449, .F. ) ;
#86379 = PLANE ( 'NONE',  #24539 ) ;
#86380 = FACE_BOUND ( 'NONE', #14531, .T. ) ;
#86381 = DIRECTION ( 'NONE',  ( 1.000000000000000078E-15, -1.000000000000000000, 0.000000000000000000 ) ) ;
#86382 = CARTESIAN_POINT ( 'NONE',  ( 114.7830339860594364, -33.98399025413122843, 111.9166617981629486 ) ) ;
#86383 = CARTESIAN_POINT ( 'NONE',  ( 101.9739164908862961, -45.89159533563675808, 183.1727681330539781 ) ) ;
#86384 = PLANE ( 'NONE',  #49407 ) ;
#86385 = VERTEX_POINT ( 'NONE', #78033 ) ;
#86386 = DIRECTION ( 'NONE',  ( 0.000000000000000000, -1.000000000000000000, 0.000000000000000000 ) ) ;
#86387 = EDGE_LOOP ( 'NONE', ( #40780, #25308, #36367, #32098 ) ) ;
#86388 = ORIENTED_EDGE ( 'NONE', *, *, #29735, .T. ) ;
#86389 = AXIS2_PLACEMENT_3D ( 'NONE', #24561, #4108, #31807 ) ;
#86390 = CIRCLE ( 'NONE', #19660, 0.5000000000000004441 ) ;
#86391 = CARTESIAN_POINT ( 'NONE',  ( 147.4575741623270062, 20.32000000000000028, -135.2444258376734183 ) ) ;
#86392 = VECTOR ( 'NONE', #9262, 1000.000000000000000 ) ;
#86393 = ORIENTED_EDGE ( 'NONE', *, *, #26423, .T. ) ;
#86394 = VERTEX_POINT ( 'NONE', #49395 ) ;
#86395 = DIRECTION ( 'NONE',  ( 0.000000000000000000, 0.000000000000000000, 1.000000000000000000 ) ) ;
#86396 = CARTESIAN_POINT ( 'NONE',  ( 116.5791382887796175, -39.71887157413915759, 249.5838068554168672 ) ) ;
#86397 = CIRCLE ( 'NONE', #58817, 11.17600000000001970 ) ;
#86398 = ADVANCED_FACE ( 'NONE', ( #1273 ), #22176, .T. ) ;
#86399 = ADVANCED_FACE ( 'NONE', ( #70306 ), #8992, .F. ) ;
#86400 = CARTESIAN_POINT ( 'NONE',  ( 97.80494057462277624, -40.50090208643202772, 42.63420498255158009 ) ) ;
#86401 = CARTESIAN_POINT ( 'NONE',  ( 101.0184087763112757, -44.32493413285080663, 121.4638483995059630 ) ) ;
#86403 = CARTESIAN_POINT ( 'NONE',  ( 118.6196304926710212, -33.88663714441439367, 14.01848241876796308 ) ) ;
#86402 = AXIS2_PLACEMENT_3D ( 'NONE', #45500, #79626, #9673 ) ;
#86404 = EDGE_CURVE ( 'NONE', #8253, #72194, #49844, .T. ) ;
#86405 = B_SPLINE_CURVE_WITH_KNOTS ( 'NONE', 3,
 ( #59686, #17044, #3854, #30666, #86092, #45597, #59249, #37484, #3411, #72012, #23864, #44724, #51535, #11102, #31100, #66514, #17920, #79284, #60131, #39261, #79728, #86980, #58796, #86540, #24305, #24741, #17485, #45165, #80172 ),
 .UNSPECIFIED., .F., .F.,
 ( 4, 2, 2, 2, 1, 1, 2, 2, 2, 2, 1, 1, 1, 2, 2, 2, 4 ),
 ( 0.000000000000000000, 0.2500000000002159939, 0.3750000000003109735, 0.4375000000003584355, 0.4687500000003821943, 0.4843750000003940182, 0.4921875000003999023, 0.5000000000004057865, 0.6250000000005055956, 0.6875000000005423439, 0.7187500000005555556, 0.7343750000005554446, 0.7421875000005508927, 0.7460937500005536682, 0.7500000000005564438, 0.8750000000002782219, 1.000000000000000000 ),
 .UNSPECIFIED. ) ;
#86406 = DIRECTION ( 'NONE',  ( -4.299999999999999979E-14, 1.000000000000000000, -4.128053709984630540E-29 ) ) ;
#86407 = ORIENTED_EDGE ( 'NONE', *, *, #74601, .T. ) ;
#86408 = TOROIDAL_SURFACE ( 'NONE', #87827, 15.69999999999999929, 0.2999999999999999889 ) ;
#86409 = EDGE_CURVE ( 'NONE', #2107, #17136, #2168, .T. ) ;
#86410 = ADVANCED_FACE ( 'NONE', ( #56664 ), #83952, .T. ) ;
#86411 = CARTESIAN_POINT ( 'NONE',  ( 100.9542024942777090, -28.70739358321760903, 136.5939626800898736 ) ) ;
#86412 = ORIENTED_EDGE ( 'NONE', *, *, #28165, .F. ) ;
#86413 = DIRECTION ( 'NONE',  ( 1.000000000000000000, 0.000000000000000000, 0.000000000000000000 ) ) ;
#86414 = CARTESIAN_POINT ( 'NONE',  ( 107.0667039024479834, -48.82844715994099971, 160.9178068554150229 ) ) ;
#86415 = DIRECTION ( 'NONE',  ( 1.000000000000000078E-15, -1.000000000000000000, 0.000000000000000000 ) ) ;
#86416 = AXIS2_PLACEMENT_3D ( 'NONE', #61730, #27677, #27223 ) ;
#86417 = EDGE_CURVE ( 'NONE', #60267, #18060, #21723, .T. ) ;
#86418 = CARTESIAN_POINT ( 'NONE',  ( 107.0667039024470313, -104.2784471599413791, 2.217806855418003043 ) ) ;
#86419 = EDGE_LOOP ( 'NONE', ( #73308, #47770, #45460, #16141, #78678, #38996, #54741, #87588, #36404, #69927 ) ) ;
#86420 = APPLICATION_CONTEXT ( 'automotive_design' ) ;
#86421 = CARTESIAN_POINT ( 'NONE',  ( 110.9930863310008959, -46.38701419431276207, 282.8841967044824628 ) ) ;
#86422 = CARTESIAN_POINT ( 'NONE',  ( 96.79082665085387305, -38.90864320302405588, 27.49276813305395706 ) ) ;
#86423 = FILL_AREA_STYLE_COLOUR ( '', #59522 ) ;
#86424 = CIRCLE ( 'NONE', #54538, 7.143750000000004263 ) ;
#86425 = EDGE_CURVE ( 'NONE', #8767, #8874, #16248, .T. ) ;
#86427 = CARTESIAN_POINT ( 'NONE',  ( 107.0664832912739968, -0.7548456658612000547, 333.4006252759120343 ) ) ;
#86426 = LINE ( 'NONE', #29658, #31770 ) ;
#86428 = CARTESIAN_POINT ( 'NONE',  ( 147.4575741623265799, 20.32000000000000028, 135.2444258376725941 ) ) ;
#86429 = DIRECTION ( 'NONE',  ( 1.000000000000000000, -0.000000000000000000, 2.108231265501710124E-16 ) ) ;
#86430 = CARTESIAN_POINT ( 'NONE',  ( 131.4308125312103357, -37.51428458727104953, 6.911392308671625351 ) ) ;
#86431 = DIRECTION ( 'NONE',  ( 4.299999999999999979E-14, -1.000000000000000000, 0.000000000000000000 ) ) ;
#86432 = DIRECTION ( 'NONE',  ( 0.04216478779797398074, -0.9991106698809455455, 0.000000000000000000 ) ) ;
#86433 = ADVANCED_FACE ( 'NONE', ( #64392, #70765 ), #7633, .T. ) ;
#86434 = DIRECTION ( 'NONE',  ( 0.000000000000000000, 0.000000000000000000, 1.000000000000000000 ) ) ;
#86435 = CARTESIAN_POINT ( 'NONE',  ( 117.4518178387850895, -35.59314106485747686, 278.9127681330539872 ) ) ;
#86436 = CARTESIAN_POINT ( 'NONE',  ( 108.6750115452441747, -26.42919841034747819, 185.9527681330539792 ) ) ;
#86437 = CARTESIAN_POINT ( 'NONE',  ( 103.4696982656617479, -25.41196563057017244, 51.32133956162493149 ) ) ;
#86439 = CARTESIAN_POINT ( 'NONE',  ( 113.1782937727292335, -44.75186859144043439, 48.09395860939415002 ) ) ;
#86438 = PLANE ( 'NONE',  #55146 ) ;
#86440 = CARTESIAN_POINT ( 'NONE',  ( 81.48703104221002036, -34.36767655967705792, 1.942446731264919402 ) ) ;
#86441 = EDGE_CURVE ( 'NONE', #23939, #69728, #19947, .T. ) ;
#86442 = AXIS2_PLACEMENT_3D ( 'NONE', #64506, #56776, #8655 ) ;
#86443 = VECTOR ( 'NONE', #45231, 1000.000000000000000 ) ;
#86444 = ORIENTED_EDGE ( 'NONE', *, *, #25582, .F. ) ;
#86445 = CARTESIAN_POINT ( 'NONE',  ( 116.3137647483393806, -32.94861263809731611, 185.1356252759109680 ) ) ;
#86446 = ORIENTED_EDGE ( 'NONE', *, *, #84562, .T. ) ;
#86447 = CARTESIAN_POINT ( 'NONE',  ( 117.3137205126583211, -38.32096045344800928, 64.69181575210097890 ) ) ;
#86449 = VERTEX_POINT ( 'NONE', #15802 ) ;
#86448 = CARTESIAN_POINT ( 'NONE',  ( 3.843954637141310471, 94.65618101170012721, 130.4993963320906403 ) ) ;
#86450 = CARTESIAN_POINT ( 'NONE',  ( 117.0720146172106695, -35.46346990303036506, 49.92721339702549699 ) ) ;
#86451 = CARTESIAN_POINT ( 'NONE',  ( 106.4848323041101850, -24.91801670280283787, 191.1156252759109861 ) ) ;
#86452 = DIRECTION ( 'NONE',  ( -0.5000000000000003331, 0.000000000000000000, -0.8660254037844383745 ) ) ;
#86453 = DIRECTION ( 'NONE',  ( -0.7071067811865439090, 0.000000000000000000, -0.7071067811865512365 ) ) ;
#86454 = DIRECTION ( 'NONE',  ( -0.0001484127181978378183, 0.8660253910675245193, -0.5000000000000061062 ) ) ;
#86455 = CARTESIAN_POINT ( 'NONE',  ( 117.4590087478601248, -92.77844715994211811, -21.78219314458237932 ) ) ;
#86456 = EDGE_CURVE ( 'NONE', #52485, #23727, #36235, .T. ) ;
#86457 = FACE_OUTER_BOUND ( 'NONE', #13765, .T. ) ;
#86458 = CARTESIAN_POINT ( 'NONE',  ( 116.3247715116346939, -32.94624160847306626, 99.13562527591096796 ) ) ;
#86459 = ADVANCED_FACE ( 'NONE', ( #57105 ), #84849, .F. ) ;
#86460 = CARTESIAN_POINT ( 'NONE',  ( 116.5825849560772411, -39.12894369053753252, 123.6299109901969615 ) ) ;
#86461 = ORIENTED_EDGE ( 'NONE', *, *, #61260, .T. ) ;
#86462 = VERTEX_POINT ( 'NONE', #35321 ) ;
#86463 = VECTOR ( 'NONE', #9714, 1000.000000000000000 ) ;
#86464 = CARTESIAN_POINT ( 'NONE',  ( 114.0372341014417543, -43.02906291645705039, 79.68539282970694160 ) ) ;
#86465 = VECTOR ( 'NONE', #70363, 1000.000000000000000 ) ;
#86466 = DIRECTION ( 'NONE',  ( -0.9254794337955620787, -0.3787978585227822492, 0.000000000000000000 ) ) ;
#86467 = VECTOR ( 'NONE', #64564, 1000.000000000000000 ) ;
#86469 = DIRECTION ( 'NONE',  ( 0.000000000000000000, 0.000000000000000000, 1.000000000000000000 ) ) ;
#86468 = CARTESIAN_POINT ( 'NONE',  ( 98.59486473514179750, -43.92970144294050527, 222.8870538473389615 ) ) ;
#86470 = VECTOR ( 'NONE', #69371, 1000.000000000000000 ) ;
#86471 = DIRECTION ( 'NONE',  ( 0.7071067811865171526, 0.7071067811865779928, 7.071067811865162747E-16 ) ) ;
#86472 = CARTESIAN_POINT ( 'NONE',  ( 0.000000000000000000, 172.0000000000000000, 0.000000000000000000 ) ) ;
#86473 = CARTESIAN_POINT ( 'NONE',  ( 117.9083666784913476, 79.66685870724428753, -12.37533002637958113 ) ) ;
#86474 = CARTESIAN_POINT ( 'NONE',  ( -11.00083755277435138, 76.19034529151561230, 118.0446767648407302 ) ) ;
#86475 = CARTESIAN_POINT ( 'NONE',  ( 21.03715912545744615, -47.82818131006197149, 129.9678068554150627 ) ) ;
#86476 = CARTESIAN_POINT ( 'NONE',  ( 119.2637946045970097, -42.39761235918182791, 9.425625275910983092 ) ) ;
#86477 = CARTESIAN_POINT ( 'NONE',  ( 109.8501361970267425, -26.70547878262030395, 174.8613395616249591 ) ) ;
#86478 = ORIENTED_EDGE ( 'NONE', *, *, #68041, .T. ) ;
#86479 = ORIENTED_EDGE ( 'NONE', *, *, #60209, .F. ) ;
#86480 = CARTESIAN_POINT ( 'NONE',  ( 142.8821648370248170, -72.54478064608022692, 396.9756252759102040 ) ) ;
#86481 = CARTESIAN_POINT ( 'NONE',  ( 97.06107108145566542, -37.99641183283564772, 152.4272919321757627 ) ) ;
#86482 = CARTESIAN_POINT ( 'NONE',  ( 257.5940999999999690, 52.73749999999999716, -10.97647784993501396 ) ) ;
#86483 = CARTESIAN_POINT ( 'NONE',  ( 163.2449138993009115, -32.11662333284039761, 117.4678068554150485 ) ) ;
#86484 = CIRCLE ( 'NONE', #80706, 88.90000000000000568 ) ;
#86485 = EDGE_CURVE ( 'NONE', #52873, #15453, #30123, .T. ) ;
#86486 = VECTOR ( 'NONE', #16181, 1000.000000000000000 ) ;
#86487 = CARTESIAN_POINT ( 'NONE',  ( 95.90979441981569664, -32.73335165780250122, 176.0527681330539735 ) ) ;
#86488 = CYLINDRICAL_SURFACE ( 'NONE', #29918, 2.117000000000007987 ) ;
#86489 = ORIENTED_EDGE ( 'NONE', *, *, #7140, .F. ) ;
#86491 = ORIENTED_EDGE ( 'NONE', *, *, #49672, .F. ) ;
#86490 = ORIENTED_EDGE ( 'NONE', *, *, #68606, .F. ) ;
#86492 = CARTESIAN_POINT ( 'NONE',  ( 98.00184567357263177, -40.95613624034808709, 62.67415154770495889 ) ) ;
#86493 = DIRECTION ( 'NONE',  ( -3.999999999999999995E-14, 1.000000000000000000, -4.100000000000000342E-29 ) ) ;
#86494 = CARTESIAN_POINT ( 'NONE',  ( 137.8897065959776000, -5.906223855237799469, -5.074374724088998256 ) ) ;
#86495 = CARTESIAN_POINT ( 'NONE',  ( 107.8719782714504873, -26.68843711164719323, 261.4444404487539941 ) ) ;
#86496 = CARTESIAN_POINT ( 'NONE',  ( 188.5667039024479834, -67.87844715994100397, 137.2178068554150059 ) ) ;
#86497 = ORIENTED_EDGE ( 'NONE', *, *, #42312, .F. ) ;
#86498 = CARTESIAN_POINT ( 'NONE',  ( 111.6189197817724335, -43.97823206604638813, 9.635625275910941312 ) ) ;
#86499 = EDGE_CURVE ( 'NONE', #69509, #46472, #14171, .T. ) ;
#86500 = CARTESIAN_POINT ( 'NONE',  ( 107.0667039024470313, -104.2784471599413934, 2.217806855418003043 ) ) ;
#86501 = ORIENTED_EDGE ( 'NONE', *, *, #59967, .F. ) ;
#86502 = ORIENTED_EDGE ( 'NONE', *, *, #39245, .F. ) ;
#86503 = CARTESIAN_POINT ( 'NONE',  ( 70.30576339899383242, 100.9334329931492675, 95.04579496287460927 ) ) ;
#86504 = ORIENTED_EDGE ( 'NONE', *, *, #53244, .T. ) ;
#86505 = ORIENTED_EDGE ( 'NONE', *, *, #63061, .F. ) ;
#86506 = PLANE ( 'NONE',  #846 ) ;
#86507 = EDGE_CURVE ( 'NONE', #71967, #87130, #48935, .T. ) ;
#86508 = ADVANCED_FACE ( 'NONE', ( #65714 ), #86627, .F. ) ;
#86509 = CARTESIAN_POINT ( 'NONE',  ( 98.88061221520823096, -34.29066745521690507, 30.51813411379100671 ) ) ;
#86510 = CARTESIAN_POINT ( 'NONE',  ( 96.11487883884397831, -35.06878432418778146, 221.1946728949589840 ) ) ;
#86511 = EDGE_CURVE ( 'NONE', #72546, #15662, #86179, .T. ) ;
#86512 = CARTESIAN_POINT ( 'NONE',  ( 116.7751801856528147, -32.99181816784836485, 139.1184824187679396 ) ) ;
#86513 = CYLINDRICAL_SURFACE ( 'NONE', #20602, 15.00000000000000000 ) ;
#86514 = CARTESIAN_POINT ( 'NONE',  ( 106.2269110120561635, -47.75074920971118075, 263.5280062282920994 ) ) ;
#86515 = CARTESIAN_POINT ( 'NONE',  ( 116.7952009943650324, -39.38756004681069101, 99.61577355868260497 ) ) ;
#86516 = CARTESIAN_POINT ( 'NONE',  ( -130.4023353925299773, 71.53177522571070313, -6.370020420675912121 ) ) ;
#86517 = ORIENTED_EDGE ( 'NONE', *, *, #55286, .F. ) ;
#86518 = ADVANCED_FACE ( 'NONE', ( #23522 ), #72147, .T. ) ;
#86519 = ORIENTED_EDGE ( 'NONE', *, *, #79148, .T. ) ;
#86520 = AXIS2_PLACEMENT_3D ( 'NONE', #10837, #43567, #38107 ) ;
#86521 = AXIS2_PLACEMENT_3D ( 'NONE', #24132, #51803, #22803 ) ;
#86522 = EDGE_CURVE ( 'NONE', #87708, #23215, #27201, .T. ) ;
#86524 = CARTESIAN_POINT ( 'NONE',  ( 96.60014388984734524, -36.47963607454698831, 196.3070538473399438 ) ) ;
#86523 = AXIS2_PLACEMENT_3D ( 'NONE', #61367, #26416, #75008 ) ;
#86525 = ORIENTED_EDGE ( 'NONE', *, *, #85707, .T. ) ;
#86526 = VECTOR ( 'NONE', #23914, 1000.000000000000000 ) ;
#86527 = CARTESIAN_POINT ( 'NONE',  ( 107.9182787209079919, -47.15539321873765743, 177.6413395616249886 ) ) ;
#86528 = CARTESIAN_POINT ( 'NONE',  ( 109.7235518845913731, -27.00045683443076783, 264.8648104959339094 ) ) ;
#86529 = CARTESIAN_POINT ( 'NONE',  ( -1.389269728106021784, 70.22718948829736973, 38.08091836535547969 ) ) ;
#86530 = AXIS2_PLACEMENT_3D ( 'NONE', #17314, #23261, #50926 ) ;
#86531 = DIRECTION ( 'NONE',  ( -1.000000000000000000, 0.000000000000000000, 0.000000000000000000 ) ) ;
#86532 = FACE_OUTER_BOUND ( 'NONE', #39007, .T. ) ;
#86535 = CARTESIAN_POINT ( 'NONE',  ( 105.0259480979001552, -25.88970440745778134, 276.2365776568634033 ) ) ;
#86534 = DIRECTION ( 'NONE',  ( -0.000000000000000000, 1.000000000000000000, -0.000000000000000000 ) ) ;
#86533 = LINE ( 'NONE', #85647, #21547 ) ;
#86536 = DIRECTION ( 'NONE',  ( 1.000000000000000000, -9.073094938289460781E-13, 0.000000000000000000 ) ) ;
#86538 = ADVANCED_FACE ( 'NONE', ( #30761 ), #31640, .T. ) ;
#86537 = LINE ( 'NONE', #51969, #16361 ) ;
#86539 = FACE_OUTER_BOUND ( 'NONE', #20845, .T. ) ;
#86540 = CARTESIAN_POINT ( 'NONE',  ( 68.11045611443701375, -137.1406750370357770, 247.2637542258202927 ) ) ;
#86541 = DIRECTION ( 'NONE',  ( -1.000000000000000000, 0.000000000000000000, 0.000000000000000000 ) ) ;
#86542 = CARTESIAN_POINT ( 'NONE',  ( 69.60882292926817172, -140.2205661867621700, 245.5201220391730033 ) ) ;
#86544 = ORIENTED_EDGE ( 'NONE', *, *, #34124, .T. ) ;
#86543 = CARTESIAN_POINT ( 'NONE',  ( 105.3826699058209329, -44.58506565010721800, 195.5838068554169809 ) ) ;
#86545 = CARTESIAN_POINT ( 'NONE',  ( 164.9667039024459996, -26.71338133339301635, -5.074374724088000832 ) ) ;
#86546 = CARTESIAN_POINT ( 'NONE',  ( 96.72113125116129595, -35.27340624960861959, 181.2156252759109805 ) ) ;
#86547 = CARTESIAN_POINT ( 'NONE',  ( 117.9246037767874498, -41.47663949653230020, 54.49848241876792088 ) ) ;
#86548 = CARTESIAN_POINT ( 'NONE',  ( 104.3994723555534989, -25.95519307775132134, 236.2575300378159682 ) ) ;
#86549 = CYLINDRICAL_SURFACE ( 'NONE', #24264, 8.928099999999993486 ) ;
#86550 = CARTESIAN_POINT ( 'NONE',  ( 51.23005224011598102, -33.89581943344511217, -5.074374724088000832 ) ) ;
#86551 = AXIS2_PLACEMENT_3D ( 'NONE', #35536, #63257, #28739 ) ;
#86553 = CARTESIAN_POINT ( 'NONE',  ( -194.1576000000000022, 0.000000000000000000, -45.33899999999999864 ) ) ;
#86552 = DIRECTION ( 'NONE',  ( 0.000000000000000000, 0.000000000000000000, -1.000000000000000000 ) ) ;
#86554 = CARTESIAN_POINT ( 'NONE',  ( 110.2536356736639220, -106.6957733451327215, -19.78219314458193168 ) ) ;
#86555 = CARTESIAN_POINT ( 'NONE',  ( 70.58666025953209555, 82.54999999999999716, 344.4418053999999643 ) ) ;
#86556 = CYLINDRICAL_SURFACE ( 'NONE', #5052, 9.999999999999998224 ) ;
#86557 = ORIENTED_EDGE ( 'NONE', *, *, #4777, .F. ) ;
#86558 = VERTEX_POINT ( 'NONE', #24399 ) ;
#86559 = CARTESIAN_POINT ( 'NONE',  ( 108.0930535991856800, -45.20896867503704897, 117.0952769709339663 ) ) ;
#86561 = VERTEX_POINT ( 'NONE', #52502 ) ;
#86560 = CARTESIAN_POINT ( 'NONE',  ( -11.02183147610883829, 88.91382474694674443, -130.0907465706570179 ) ) ;
#86562 = CARTESIAN_POINT ( 'NONE',  ( 117.8338636819850365, -39.12263375953639155, 99.64038718067195077 ) ) ;
#86563 = CARTESIAN_POINT ( 'NONE',  ( 188.5667039024479834, -48.82844715994099971, 293.2178068554150627 ) ) ;
#86564 = CARTESIAN_POINT ( 'NONE',  ( 78.42773927738372208, -16.51875925606581319, 7.791169830165904031 ) ) ;
#86565 = LINE ( 'NONE', #86121, #57758 ) ;
#86566 = ADVANCED_FACE ( 'NONE', ( #30322 ), #69285, .T. ) ;
#86567 = CARTESIAN_POINT ( 'NONE',  ( 114.9268010244043978, -42.60560063232861694, 28.31562527591097123 ) ) ;
#86568 = ORIENTED_EDGE ( 'NONE', *, *, #56129, .T. ) ;
#86569 = ORIENTED_EDGE ( 'NONE', *, *, #17419, .T. ) ;
#86570 = ORIENTED_EDGE ( 'NONE', *, *, #14538, .F. ) ;
#86571 = CARTESIAN_POINT ( 'NONE',  ( -194.1576000000000022, 101.5999999999999943, 146.9389999999999930 ) ) ;
#86572 = CARTESIAN_POINT ( 'NONE',  ( 41.56648329127398966, -27.57844715994070484, 81.92562527591199739 ) ) ;
#86573 = CARTESIAN_POINT ( 'NONE',  ( 142.8824340801164965, -74.11588153691423031, 540.9756252759101471 ) ) ;
#86574 = CARTESIAN_POINT ( 'NONE',  ( 53.56670390244743629, -48.82844715994058049, 180.4678068554151196 ) ) ;
#86575 = DIRECTION ( 'NONE',  ( 0.000000000000000000, 1.000000000000000000, 0.000000000000000000 ) ) ;
#86576 = CARTESIAN_POINT ( 'NONE',  ( 97.70648437022691724, -40.25111366377705480, 52.61248643207778741 ) ) ;
#86577 = DIRECTION ( 'NONE',  ( -0.2588190451025166317, 0.000000000000000000, -0.9659258262890694224 ) ) ;
#86578 = CARTESIAN_POINT ( 'NONE',  ( 77.69357874334650660, 92.12496802699139664, 89.55214429302449730 ) ) ;
#86579 = CARTESIAN_POINT ( 'NONE',  ( 106.6078071710152244, -25.70885557892963647, 40.09753003781596448 ) ) ;
#86580 = ORIENTED_EDGE ( 'NONE', *, *, #53663, .T. ) ;
#86581 = VERTEX_POINT ( 'NONE', #59343 ) ;
#86582 = CARTESIAN_POINT ( 'NONE',  ( 9.331435647859348646E-23, 95.25000000000000000, 130.5560000000000116 ) ) ;
#86583 = CARTESIAN_POINT ( 'NONE',  ( -15.88716625750469902, 65.60000000000000853, -53.54073290201169044 ) ) ;
#86584 = VECTOR ( 'NONE', #70281, 1000.000000000000000 ) ;
#86585 = CARTESIAN_POINT ( 'NONE',  ( 85.58879520791417406, -87.02121134100643474, 250.2178068554179333 ) ) ;
#86586 = CARTESIAN_POINT ( 'NONE',  ( 114.5787023362084085, -39.92261033116096058, 166.3252332267339852 ) ) ;
#86587 = EDGE_CURVE ( 'NONE', #83823, #87657, #51632, .T. ) ;
#86588 = VECTOR ( 'NONE', #39698, 1000.000000000000000 ) ;
#86589 = CIRCLE ( 'NONE', #85176, 3.299999999999997158 ) ;
#86590 = VECTOR ( 'NONE', #37546, 1000.000000000000000 ) ;
#86591 = CARTESIAN_POINT ( 'NONE',  ( 41.56648329127398966, -27.57844715994070484, 78.92562527591199739 ) ) ;
#86592 = EDGE_LOOP ( 'NONE', ( #16331, #68856, #48676, #75605 ) ) ;
#86593 = ORIENTED_EDGE ( 'NONE', *, *, #46720, .T. ) ;
#86594 = DIRECTION ( 'NONE',  ( 0.000000000000000000, -1.000000000000000000, 0.000000000000000000 ) ) ;
#86595 = VERTEX_POINT ( 'NONE', #38021 ) ;
#86596 = VERTEX_POINT ( 'NONE', #2618 ) ;
#86597 = DIRECTION ( 'NONE',  ( 0.000000000000000000, 0.000000000000000000, -1.000000000000000000 ) ) ;
#86598 = CARTESIAN_POINT ( 'NONE',  ( 103.5819202103828474, -28.00394742224748157, 171.8225356868499603 ) ) ;
#86599 = CARTESIAN_POINT ( 'NONE',  ( -7.205548786489490269E-13, 117.4749999999999943, 96.04375000000000284 ) ) ;
#86600 = AXIS2_PLACEMENT_3D ( 'NONE', #55861, #40907, #36 ) ;
#86601 = CARTESIAN_POINT ( 'NONE',  ( 112.1393456749956101, -28.01282280174694606, 119.6564586061650886 ) ) ;
#86602 = CARTESIAN_POINT ( 'NONE',  ( 97.86672898778118679, -40.64958093551612706, 16.64701983854467571 ) ) ;
#86603 = EDGE_LOOP ( 'NONE', ( #8365, #82374, #14066, #45800 ) ) ;
#86604 = CLOSED_SHELL ( 'NONE', ( #81892, #4816, #25784, #75272, #40256, #84847, #11749, #62500, #46697, #25786, #61370, #8583, #478, #64772, #17083, #7435, #57868, #37236, #57048, #46383, #30114, #87787, #1926, #11895, #54160, #14841, #43945, #41060, #45385, #49246, #83736, #31865, #28047, #78454, #36254, #88597, #6959, #63760, #17620, #79155, #4159, #89903, #59094, #21048, #43720, #47817, #39935, #75225, #27864, #31838, #56080, #31767, #84482, #89199, #775, #56471, #73082, #89178, #30818, #60151, #82417, #53440, #38815, #88376, #3264, #12954, #18297, #81735, #36187, #10814, #34084, #32485, #34212, #47396, #15617, #13518, #34989, #59593, #88770, #52551, #32530, #54184, #27534, #8494, #55700, #79669, #63461, #7401, #34571, #10703, #58246, #63857, #47546, #50285, #45156, #82861, #13372, #47058, #58801, #54064, #2576, #46293, #44848, #58298, #40360, #85618, #33583, #2063, #42905, #74731, #45851, #44626, #85917, #67215, #1420, #75836, #86566, #16975, #40861, #38881, #56346, #13717, #14033, #62254, #84098, #37201, #56433, #74268, #11126, #88422, #9715, #30809, #57762, #44236, #85389, #48007, #69713, #77411, #36405, #62717, #68998, #40419, #36292, #68785, #72481, #80150, #1688, #12065, #43732, #63641, #83040, #14869, #80087, #80536, #61834, #56969, #16467, #61369, #34411, #76965, #33621, #59923, #60733, #67734, #50691, #31503, #89440, #14596, #73496, #56891, #17641, #48813, #37191, #45059, #21571, #7990, #57372, #36352, #51844, #65814, #30813, #77800, #31063, #76261, #266, #9093, #67506, #59861, #56658, #42986, #2546, #60249, #70198, #8928, #46376, #8797, #3238, #34123, #85418, #26962, #24173, #41758, #88882, #33275, #35327, #18838, #43842, #35235, #69496, #80353, #33193, #24784, #65806, #5380, #5578, #1290, #41254, #60203, #34920, #13915, #71352, #9159, #78946, #2465, #11509, #78544, #48732, #47100, #53035, #15242, #47038, #74633, #40333, #1109, #7757, #89719, #89088, #77244, #18087, #59412, #2967, #13580, #69108, #4768, #3761, #50498, #30909, #47953, #81599, #19168, #68456, #11290, #65261, #31621, #19340, #82195, #5962, #37425, #6935, #14611, #47515, #53069, #59109, #59992, #23236, #65685, #15230, #31940, #27582, #21022, #45472, #30064, #41511, #72762, #18712, #561, #69291, #87952, #42392, #81832, #693, #30257, #84052, #6409, #18429, #7666, #79120, #89448, #87009, #12602, #58163, #81149, #28241, #43548, #52123, #24249, #71673, #22838, #39552, #24330, #88571, #56442, #29554, #55012, #18540, #22144, #26601, #83135, #5728, #7148, #19308, #41559, #21912, #58764, #49658, #57882, #15290, #6955, #26115, #70466, #12208, #81912, #34092, #10805, #26019, #68879, #45764, #24986, #44632, #19853, #59284, #41365, #81676, #53139, #25352, #35587, #16249, #39724, #25319, #68554, #79070, #18162, #74630, #52615, #89905, #66587, #22074, #88449, #50605, #68758, #25501, #47500, #66316, #74860, #29350, #63912, #58925, #81663, #75509, #72441, #51342, #28558, #75317, #19169, #11864, #60337, #48148, #18612, #79238, #30915, #5109, #71514, #79102, #81223, #31526, #76276, #73694, #43320, #26410, #47899, #12911, #57472, #54433, #64367, #69698, #19860, #10857, #57459, #1041, #44771, #77200, #10295, #70596, #36873, #18194, #6724, #12755, #2335, #69110, #11039, #54852, #89829, #72399, #33065, #56643, #65676, #47096, #60650, #35195, #19240, #76795, #18076, #35218, #55453, #55983, #64156, #20276, #35349, #51326, #36363, #83055, #46199, #51533, #30315, #83750, #89108, #4871, #54992, #9902, #16264, #28584, #73750, #11646, #7746, #34645, #1446, #21382, #80811, #16483, #14854, #115, #64593, #62587, #76881, #52428, #78189, #80754, #41233, #11085, #33781, #47333, #25403, #22817, #72564, #86538, #88104, #16973, #56353, #49714, #32401, #34394, #32239, #23167, #6142, #28889, #41746, #31245, #46120, #63103, #85807, #48901, #31231, #85404, #88271, #60081, #29127, #26846, #35947, #8180, #62724, #78194, #81226, #81329, #14777, #36686, #35766, #85304, #85826, #82560, #57921, #29080, #12268, #73743, #21578, #20924, #6416, #71645, #38596, #79857, #36733, #75780, #52843, #89824, #3141, #10959, #38538, #5290, #50425, #74100, #7531, #7259, #47150, #48952, #7710, #392, #3292, #30866, #9343, #4267, #77948, #6911, #38039, #27954, #81506, #37471, #40336, #12077, #84691, #43376, #79345, #16913, #86508, #82082, #31032, #23374, #37928, #42345, #35933, #27750, #2842, #66845, #13133, #77701, #73462, #41693, #15395, #44509, #9131, #3546, #81414, #69859, #79011, #41266, #8911, #11527, #87812, #63246, #52823, #17318, #57978, #62413, #44064, #88665, #27935, #89272, #85520, #74294, #52013, #53991, #53366, #27945, #66815, #73728, #86001, #40218, #42798, #78806, #39100, #83642, #75457, #7036, #38809, #16569, #15966, #40041, #28550, #87239, #66715, #3344, #69053, #71193, #22051, #41172, #28677, #10022, #65701, #18874, #55398, #1255, #19004, #87518, #78004, #4200, #80423, #20472, #58006, #22752, #54106, #28696, #17747, #32767, #62731, #57565, #17595, #82980, #50496, #22660, #62246, #40927, #21435, #49772, #25025, #71249, #46611, #74715, #43988, #81731, #36519, #50445, #69160, #6306, #56370, #56765, #38801, #57591, #26406, #8806, #16982, #35017, #78730, #28540, #24798, #32367, #43259, #29011, #68730, #89287, #24864, #6230, #15864, #12841, #80240, #42651, #74483, #39765, #89173, #84206, #42419, #33382, #47912, #9077, #3349, #62199, #3819, #79646, #85243, #17135, #36858, #47956, #56832, #10025, #68025, #85458, #66322, #30701, #26014, #8314, #8737, #62605, #2840, #25708, #81946, #1310, #41863, #85900, #9569, #18630, #79974, #12372, #62030, #82283, #33177, #40898, #39663, #6127, #25795, #74694, #6938, #56959, #9198, #58526, #74834, #51505, #19113, #67023, #876, #66082, #24179, #21878, #37188, #27338, #47560, #32458, #54553, #50401, #66259, #24779, #23051, #44926, #35259, #84696, #22028, #36589, #27415, #27792, #76663, #60486, #53439, #19768, #72679, #51005, #43616, #4561, #57072, #43216, #59137, #66087, #87554, #84541, #79514, #48930, #76520, #51063, #56436, #75967, #32136, #43805, #33699, #10728, #35519, #21414, #23995, #78540, #5902, #17026, #42005, #58483, #75108, #64763, #71621, #54212, #35316, #54988, #54373, #33581, #24659, #20977, #28467, #86928, #33071, #85898, #62669, #32432, #15667, #5912, #41880, #60905, #23548, #56096, #8783, #28887, #65887, #45236, #67236, #22735, #7801, #69177, #5688, #27837, #84391, #73912, #62489, #17982, #69164, #59406, #20360, #51851, #44656, #10812, #62763, #66517, #25082, #69917, #8617, #22045, #45654, #26229, #18929, #52016, #6905, #30756, #65767, #47114, #83648, #67121, #3536, #89308, #49460, #49342, #25755, #59097, #8171, #35747, #7138, #73390, #25235, #49087, #73161, #60511, #39656, #42750, #38508, #57156, #79072, #9809, #5160, #81701, #88210, #72817, #83574, #49671, #84300, #88389, #19327, #61443, #63636, #63188, #54605, #66318, #897, #11238, #71828, #7719, #88260, #56328, #16491, #65532, #29198, #20883, #16183, #55397, #39608, #45012, #85368, #40850, #9735, #59234, #48347, #15245, #20068, #53238, #22616, #83646, #87979, #15792, #2654, #40163, #9471, #65866, #79529, #28598, #85240, #19783, #4285, #76584, #12617, #52425, #73077, #7567, #21108, #84608, #18715, #66913, #31334, #17899, #3771, #15289, #22900, #35494, #10310, #61463, #33592, #56707, #52352, #6024, #41360, #4763, #18488, #45678, #41380, #21774, #19285, #89684, #13575, #33685, #21497, #79796, #72581, #8541, #5331, #63800, #2735, #87988, #78907, #51748, #21705, #17818, #997, #22623, #21550, #55554, #74607, #16983, #71450, #33943, #13723, #56853, #35340, #8700, #56316, #22578, #18931, #88555, #41832, #84783, #22439, #15349, #36812, #56070, #76349, #38083, #47779, #28031, #54387, #4841, #67929, #71861, #15455, #65966, #26335, #60782, #15148, #85349, #46984, #64678, #86180, #42095, #50829, #52453, #28237, #4596, #3645, #13686, #47180, #63853, #25211, #13793, #89057, #16677, #28442, #44223, #4702, #42194, #48072, #82348, #81948, #39617, #77588, #48647, #34349, #12558, #39555, #49895, #21136, #67973, #1897, #16558, #86317, #47511, #70958, #40246, #22650, #43741, #14126, #70874, #40619, #464, #32460, #59476, #24290, #77749, #34533, #17274, #13171, #83883, #88227, #3537, #71155, #59754, #33298, #85003, #10418, #69681, #3154, #49892, #88946, #39290, #86938, #11885, #84572, #73264, #61876, #14662, #362, #35177, #37698, #17797, #82274, #42423, #36410, #39012, #28188, #1580, #62169, #58190, #21198, #45255, #28658, #23488, #86518, #29068, #78857, #54362, #30639, #4679, #48658, #52960, #81258, #38409, #18144, #19843, #25272, #68259, #18497, #41973, #40787, #2626, #43652, #20482, #1790, #23213, #26162, #71973, #69592, #88498, #79693, #7565, #30170, #37095, #62390, #8431, #51626, #23557, #32036, #84163, #42793, #89682, #58029, #43042, #58868, #67795, #11619, #11436, #19734, #44863, #59921, #48699, #24197, #10358, #59830, #60954, #67862, #36901, #44964, #6507, #38197, #14145, #45984, #6832, #84962, #10205, #35521, #44901, #80884, #9838, #68868, #86410, #72099, #29091, #20247, #88284, #88320, #75600, #75668, #48719, #68265, #27866, #83551, #55077, #35718, #83117, #60219, #81906, #38726, #50091, #77368, #21847, #6406, #20993, #78142, #83495, #29905, #52919, #62951, #73619, #63444, #81777, #64544, #5266, #33280, #72686, #87981, #19131, #23763, #19745, #40055, #70846, #37197, #71702, #11961, #79855, #63303, #74594, #22952, #52405, #82228, #81890, #32476, #22383, #11425, #31416, #27976, #54826, #41661, #1509, #64357, #42404, #8381, #84438, #55289, #21393, #58168, #38697, #2134, #26006, #19084, #88793, #70718, #11480, #37312, #42912, #10410 ) ) ;
#86605 = VERTEX_POINT ( 'NONE', #80708 ) ;
#86606 = ORIENTED_EDGE ( 'NONE', *, *, #70625, .F. ) ;
#86607 = EDGE_CURVE ( 'NONE', #64435, #34773, #78926, .T. ) ;
#86608 = CARTESIAN_POINT ( 'NONE',  ( 103.2852591291245830, -43.96353797031052579, 210.0109475124489506 ) ) ;
#86609 = CARTESIAN_POINT ( 'NONE',  ( 116.1429853652930149, -29.07104484579759784, 74.38419670448293175 ) ) ;
#86610 = EDGE_CURVE ( 'NONE', #43140, #25043, #37383, .T. ) ;
#86611 = CARTESIAN_POINT ( 'NONE',  ( 97.82856912889580769, -29.34641599088746133, 45.78991099019697231 ) ) ;
#86612 = DIRECTION ( 'NONE',  ( 0.000000000000000000, 0.000000000000000000, -1.000000000000000000 ) ) ;
#86613 = PLANE ( 'NONE',  #65534 ) ;
#86614 = CARTESIAN_POINT ( 'NONE',  ( 107.7967913059082576, -25.29348262043577478, 322.9250063603933540 ) ) ;
#86615 = EDGE_CURVE ( 'NONE', #1864, #86337, #58952, .T. ) ;
#86616 = CARTESIAN_POINT ( 'NONE',  ( 107.6529936739636639, -47.12767891731729009, 148.6213395616249784 ) ) ;
#86617 = LINE ( 'NONE', #78918, #4490 ) ;
#86618 = ORIENTED_EDGE ( 'NONE', *, *, #12504, .F. ) ;
#86619 = DIRECTION ( 'NONE',  ( -1.000000000000000000, 0.000000000000000000, 0.000000000000000000 ) ) ;
#86620 = ORIENTED_EDGE ( 'NONE', *, *, #2744, .F. ) ;
#86621 = EDGE_CURVE ( 'NONE', #7066, #81364, #38448, .T. ) ;
#86622 = ORIENTED_EDGE ( 'NONE', *, *, #86670, .F. ) ;
#86623 = CARTESIAN_POINT ( 'NONE',  ( 116.7802871385218282, -39.10473973501323286, 9.635625275910941312 ) ) ;
#86624 = DIRECTION ( 'NONE',  ( 0.000000000000000000, 1.000000000000000000, 0.000000000000000000 ) ) ;
#86625 = EDGE_LOOP ( 'NONE', ( #37072, #67428, #54683, #72609 ) ) ;
#86626 = VECTOR ( 'NONE', #54877, 1000.000000000000000 ) ;
#86627 = CYLINDRICAL_SURFACE ( 'NONE', #9765, 3.000000000000002665 ) ;
#86628 = CARTESIAN_POINT ( 'NONE',  ( 41.56648329127399677, -18.82844715994099971, 261.0426252759119734 ) ) ;
#86629 = CARTESIAN_POINT ( 'NONE',  ( 110.3541591212943445, -25.34385655279935534, 64.85276813305395649 ) ) ;
#86630 = DIRECTION ( 'NONE',  ( 0.000000000000000000, 0.000000000000000000, 1.000000000000000000 ) ) ;
#86631 = CARTESIAN_POINT ( 'NONE',  ( 45.66030316258350297, 82.54999999999999716, 358.0130000000000337 ) ) ;
#86632 = DIRECTION ( 'NONE',  ( 1.000000000000000000, 4.163336342344333240E-14, 0.000000000000000000 ) ) ;
#86633 = CARTESIAN_POINT ( 'NONE',  ( 116.9446180447427821, -41.83184233209006209, 93.44705384733997278 ) ) ;
#86635 = CARTESIAN_POINT ( 'NONE',  ( 114.9613132280021830, -29.02649429439055595, 190.4537205140059655 ) ) ;
#86634 = DIRECTION ( 'NONE',  ( 0.000000000000000000, 0.000000000000000000, 1.000000000000000000 ) ) ;
#86636 = CARTESIAN_POINT ( 'NONE',  ( 87.31648329127403940, -54.62589567669624557, -5.074374724089048883 ) ) ;
#86638 = EDGE_CURVE ( 'NONE', #17228, #25149, #17031, .T. ) ;
#86637 = DIRECTION ( 'NONE',  ( 1.000000000000000000, 1.132880637372608296E-15, 0.000000000000000000 ) ) ;
#86639 = ORIENTED_EDGE ( 'NONE', *, *, #33467, .T. ) ;
#86640 = LINE ( 'NONE', #87085, #33844 ) ;
#86641 = CARTESIAN_POINT ( 'NONE',  ( 41.56670390244718050, -42.82844715994109208, 180.4678068554150911 ) ) ;
#86642 = CARTESIAN_POINT ( 'NONE',  ( 97.78523098987417939, -40.45222676762392666, 136.6304043995652080 ) ) ;
#86643 = DIRECTION ( 'NONE',  ( 0.000000000000000000, 0.000000000000000000, -1.000000000000000000 ) ) ;
#86645 = EDGE_LOOP ( 'NONE', ( #21704, #30621, #9562, #63695 ) ) ;
#86644 = CARTESIAN_POINT ( 'NONE',  ( 117.9946794957619431, -34.78331989172042427, 198.9546728949589749 ) ) ;
#86646 = CARTESIAN_POINT ( 'NONE',  ( -27.27158787008326968, 127.0000000000000000, 106.1020876358972771 ) ) ;
#86647 = CARTESIAN_POINT ( 'NONE',  ( 104.4050232528787774, -25.97761772452189888, 236.2575300378159682 ) ) ;
#86648 = CARTESIAN_POINT ( 'NONE',  ( 97.94860405783340696, -41.87310908463563663, 132.7356252759109623 ) ) ;
#86649 = CIRCLE ( 'NONE', #76449, 13.44999999999999396 ) ;
#86650 = FACE_OUTER_BOUND ( 'NONE', #38000, .T. ) ;
#86651 = CARTESIAN_POINT ( 'NONE',  ( 82.16007929299428270, -38.51483178663178819, 7.477467810852441055 ) ) ;
#86652 = CARTESIAN_POINT ( 'NONE',  ( 100.8594679592218597, 81.72130195885952730, -82.89895571708196087 ) ) ;
#86653 = PLANE ( 'NONE',  #13409 ) ;
#86654 = ORIENTED_EDGE ( 'NONE', *, *, #27290, .F. ) ;
#86655 = AXIS2_PLACEMENT_3D ( 'NONE', #81419, #81854, #68662 ) ;
#86656 = VECTOR ( 'NONE', #80339, 1000.000000000000000 ) ;
#86657 = AXIS2_PLACEMENT_3D ( 'NONE', #60189, #46109, #5251 ) ;
#86658 = EDGE_LOOP ( 'NONE', ( #66572, #30057, #5699, #74524 ) ) ;
#86659 = EDGE_LOOP ( 'NONE', ( #19956, #75645, #49969, #69537 ) ) ;
#86660 = ORIENTED_EDGE ( 'NONE', *, *, #79850, .F. ) ;
#86661 = DIRECTION ( 'NONE',  ( 1.387778780781444492E-15, 0.000000000000000000, -1.000000000000000000 ) ) ;
#86662 = CARTESIAN_POINT ( 'NONE',  ( 115.9068016902149907, -30.09448287295081670, 260.3508633711493871 ) ) ;
#86663 = CARTESIAN_POINT ( 'NONE',  ( 52.06670390244699576, -68.87844715994100397, 222.2178068554179902 ) ) ;
#86664 = CARTESIAN_POINT ( 'NONE',  ( 132.3549177284975826, -34.56918551488095659, 2.099346190922506405 ) ) ;
#86665 = CIRCLE ( 'NONE', #56161, 0.5000000000000031086 ) ;
#86666 = VECTOR ( 'NONE', #41972, 1000.000000000000000 ) ;
#86668 = CARTESIAN_POINT ( 'NONE',  ( 84.99964240976864005, 69.93120980984940616, 82.65143893653650764 ) ) ;
#86667 = CARTESIAN_POINT ( 'NONE',  ( 180.2121375201585636, -29.73316016638864312, 237.4678068554150059 ) ) ;
#86669 = VECTOR ( 'NONE', #20815, 1000.000000000000000 ) ;
#86670 = EDGE_CURVE ( 'NONE', #75853, #89067, #18011, .T. ) ;
#86671 = CARTESIAN_POINT ( 'NONE',  ( 111.9460571495898620, -43.77514521526708080, 202.4809912566479397 ) ) ;
#86672 = VERTEX_POINT ( 'NONE', #16688 ) ;
#86673 = VERTEX_POINT ( 'NONE', #58888 ) ;
#86674 = ORIENTED_EDGE ( 'NONE', *, *, #67402, .F. ) ;
#86675 = VECTOR ( 'NONE', #5588, 999.9999999999998863 ) ;
#86676 = CARTESIAN_POINT ( 'NONE',  ( 8.748570571408901218E-16, 127.0000000000000000, -96.04375000000000284 ) ) ;
#86677 = LINE ( 'NONE', #72153, #39034 ) ;
#86678 = ADVANCED_FACE ( 'NONE', ( #73424, #17578 ), #66154, .T. ) ;
#86679 = CARTESIAN_POINT ( 'NONE',  ( 188.5667039024479834, -65.37844715994100397, 257.2178068554150059 ) ) ;
#86680 = CARTESIAN_POINT ( 'NONE',  ( 106.6757791475081376, -27.34201535943007499, 36.52920235351597711 ) ) ;
#86681 = CARTESIAN_POINT ( 'NONE',  ( 118.5215310810514922, 94.92435932957491218, -2.887881501068293666 ) ) ;
#86682 = DIRECTION ( 'NONE',  ( 1.000000000000000000, 0.000000000000000000, 0.000000000000000000 ) ) ;
#86683 = FACE_OUTER_BOUND ( 'NONE', #52179, .T. ) ;
#86684 = VERTEX_POINT ( 'NONE', #44372 ) ;
#86685 = CARTESIAN_POINT ( 'NONE',  ( 102.0651407823954884, -27.97162049558258445, 56.48994194808369684 ) ) ;
#86686 = ORIENTED_EDGE ( 'NONE', *, *, #1605, .F. ) ;
#86687 = CARTESIAN_POINT ( 'NONE',  ( 172.5664832912740110, -18.82844715994099971, 261.0426252759119734 ) ) ;
#86688 = CARTESIAN_POINT ( 'NONE',  ( 110.2473415405206083, -44.77823998140315354, 20.70618560768600247 ) ) ;
#86689 = CIRCLE ( 'NONE', #30082, 0.5000000000000004441 ) ;
#86690 = ADVANCED_FACE ( 'NONE', ( #72102 ), #9875, .F. ) ;
#86691 = CARTESIAN_POINT ( 'NONE',  ( 31.90335556477745627, -33.89581943344423109, 193.9678068554150911 ) ) ;
#86692 = LINE ( 'NONE', #44434, #22942 ) ;
#86693 = DIRECTION ( 'NONE',  ( -0.7071067811865434649, -0.7071067811865516806, -7.071067811865440820E-16 ) ) ;
#86694 = ORIENTED_EDGE ( 'NONE', *, *, #18270, .T. ) ;
#86695 = LINE ( 'NONE', #67583, #36374 ) ;
#86696 = CARTESIAN_POINT ( 'NONE',  ( 121.1771017092910796, 59.51425790832627172, -48.59044173555516011 ) ) ;
#86697 = ORIENTED_EDGE ( 'NONE', *, *, #50674, .F. ) ;
#86698 = CARTESIAN_POINT ( 'NONE',  ( 114.0222564360173720, -28.96386602133403798, 114.4956252759109816 ) ) ;
#86699 = ORIENTED_EDGE ( 'NONE', *, *, #75883, .T. ) ;
#86700 = CARTESIAN_POINT ( 'NONE',  ( 113.9308110932664704, -41.86102644448636312, 27.73813411379200033 ) ) ;
#86701 = CARTESIAN_POINT ( 'NONE',  ( 100.5671124743891909, -44.38319045565923204, 88.01544400472339191 ) ) ;
#86702 = CARTESIAN_POINT ( 'NONE',  ( 104.4236822747140678, -45.74566190472552307, 58.76920235351595778 ) ) ;
#86703 = CARTESIAN_POINT ( 'NONE',  ( 46.03715912545425937, -48.62818131006086020, 313.9678068554150059 ) ) ;
#86704 = FACE_OUTER_BOUND ( 'NONE', #40094, .T. ) ;
#86705 = CIRCLE ( 'NONE', #78027, 3.249999999999975131 ) ;
#86706 = CARTESIAN_POINT ( 'NONE',  ( 67.06332395966860815, -67.87844715994098976, 246.0535151165250056 ) ) ;
#86707 = CARTESIAN_POINT ( 'NONE',  ( 109.6172575917244529, -25.13135243900233817, 25.90419670448196143 ) ) ;
#86708 = DIRECTION ( 'NONE',  ( -1.000000000000000078E-15, 1.000000000000000000, 0.000000000000000000 ) ) ;
#86709 = ORIENTED_EDGE ( 'NONE', *, *, #23831, .F. ) ;
#86710 = LINE ( 'NONE', #52149, #8191 ) ;
#86711 = AXIS2_PLACEMENT_3D ( 'NONE', #69452, #34470, #63984 ) ;
#86712 = ORIENTED_EDGE ( 'NONE', *, *, #62438, .T. ) ;
#86713 = CIRCLE ( 'NONE', #25818, 3.250000000000002665 ) ;
#86714 = CARTESIAN_POINT ( 'NONE',  ( -117.9582931081850745, 78.06989712577872353, 11.89083204515657677 ) ) ;
#86715 = ORIENTED_EDGE ( 'NONE', *, *, #8731, .T. ) ;
#86716 = VERTEX_POINT ( 'NONE', #68858 ) ;
#86717 = EDGE_CURVE ( 'NONE', #82398, #48031, #13448, .T. ) ;
#86718 = DIRECTION ( 'NONE',  ( 0.000000000000000000, 1.000000000000000000, 0.000000000000000000 ) ) ;
#86719 = AXIS2_PLACEMENT_3D ( 'NONE', #17539, #67017, #58848 ) ;
#86720 = CARTESIAN_POINT ( 'NONE',  ( 97.31640351007376921, -35.61153895465465524, 206.2356252759109623 ) ) ;
#86721 = LINE ( 'NONE', #18110, #66953 ) ;
#86722 = DIRECTION ( 'NONE',  ( -1.821231995776174246E-16, 0.000000000000000000, -1.000000000000000000 ) ) ;
#86723 = ADVANCED_FACE ( 'NONE', ( #19367 ), #67500, .T. ) ;
#86724 = CARTESIAN_POINT ( 'NONE',  ( 112.7416762643710229, -27.24439759747685486, 50.65943479972101215 ) ) ;
#86725 = CARTESIAN_POINT ( 'NONE',  ( 97.81339943497903278, -40.52160296963607777, 42.63598487163911699 ) ) ;
#86726 = VERTEX_POINT ( 'NONE', #20272 ) ;
#86727 = CARTESIAN_POINT ( 'NONE',  ( 104.6139328008865448, -27.02899419139365733, 171.2735265809598957 ) ) ;
#86728 = AXIS2_PLACEMENT_3D ( 'NONE', #51357, #79103, #65011 ) ;
#86729 = AXIS2_PLACEMENT_3D ( 'NONE', #25965, #40026, #53630 ) ;
#86730 = CYLINDRICAL_SURFACE ( 'NONE', #75265, 10.00000000000002487 ) ;
#86731 = ORIENTED_EDGE ( 'NONE', *, *, #55736, .T. ) ;
#86732 = AXIS2_PLACEMENT_3D ( 'NONE', #84113, #28223, #20089 ) ;
#86733 = DIRECTION ( 'NONE',  ( -1.000000000000000000, 0.000000000000000000, -1.000000000000000078E-15 ) ) ;
#86734 = CARTESIAN_POINT ( 'NONE',  ( 115.7813355090083860, -41.80530075443426341, 114.4070842759231681 ) ) ;
#86735 = CARTESIAN_POINT ( 'NONE',  ( 111.5990003564989905, -46.09347164638234062, 247.9356252759109509 ) ) ;
#86736 = DIRECTION ( 'NONE',  ( 0.000000000000000000, 0.000000000000000000, 1.000000000000000000 ) ) ;
#86737 = DIRECTION ( 'NONE',  ( -0.9999999999998281375, 0.000000000000000000, 5.861124988064729938E-07 ) ) ;
#86738 = CARTESIAN_POINT ( 'NONE',  ( 79.00802158143601162, -39.26771232012922042, 1.799893082726616855 ) ) ;
#86739 = CARTESIAN_POINT ( 'NONE',  ( 110.7878219579318255, -44.41760495294317934, 247.3581341137909533 ) ) ;
#86741 = CARTESIAN_POINT ( 'NONE',  ( 98.87507392487052016, -43.19978241230791838, 87.85848241876792031 ) ) ;
#86740 = CARTESIAN_POINT ( 'NONE',  ( 31.75000000000000000, 104.3431970271542042, -3.174999999999999822 ) ) ;
#86742 = CARTESIAN_POINT ( 'NONE',  ( 113.7708228275151470, 69.80903686419651422, 64.04023853347004547 ) ) ;
#86743 = CARTESIAN_POINT ( 'NONE',  ( 117.2525043769621362, -39.29786468180206782, 123.6299109901969615 ) ) ;
#86744 = ORIENTED_EDGE ( 'NONE', *, *, #29172, .T. ) ;
#86746 = EDGE_CURVE ( 'NONE', #37134, #4381, #72208, .T. ) ;
#86745 = DIRECTION ( 'NONE',  ( 0.000000000000000000, 1.000000000000000000, 0.000000000000000000 ) ) ;
#86747 = ORIENTED_EDGE ( 'NONE', *, *, #76725, .T. ) ;
#86748 = PLANE ( 'NONE',  #26580 ) ;
#86749 = LINE ( 'NONE', #49967, #17467 ) ;
#86750 = EDGE_CURVE ( 'NONE', #88991, #72189, #82393, .T. ) ;
#86751 = LINE ( 'NONE', #24519, #54300 ) ;
#86752 = ORIENTED_EDGE ( 'NONE', *, *, #70183, .F. ) ;
#86753 = CARTESIAN_POINT ( 'NONE',  ( 97.78493946438445050, -40.45149985807169202, 51.62996325680755660 ) ) ;
#86755 = ORIENTED_EDGE ( 'NONE', *, *, #43007, .F. ) ;
#86754 = CARTESIAN_POINT ( 'NONE',  ( 98.80516515778722919, -28.16326830255935221, 115.6870538473389587 ) ) ;
#86756 = LINE ( 'NONE', #46275, #1579 ) ;
#86757 = CARTESIAN_POINT ( 'NONE',  ( 172.5664832912729878, -18.82844715994071194, 138.9256252759119832 ) ) ;
#86758 = AXIS2_PLACEMENT_3D ( 'NONE', #63684, #77765, #14190 ) ;
#86759 = AXIS2_PLACEMENT_3D ( 'NONE', #35129, #63298, #70113 ) ;
#86760 = DIRECTION ( 'NONE',  ( 0.000000000000000000, 0.000000000000000000, 1.000000000000000000 ) ) ;
#86761 = ORIENTED_EDGE ( 'NONE', *, *, #66138, .T. ) ;
#86762 = CARTESIAN_POINT ( 'NONE',  ( 98.44037697964694189, -30.83566621160791144, 120.8499109901969604 ) ) ;
#86763 =( NAMED_UNIT ( * ) PLANE_ANGLE_UNIT ( ) SI_UNIT ( $, .RADIAN. ) );
#86764 = LINE ( 'NONE', #57246, #72436 ) ;
#86765 = CARTESIAN_POINT ( 'NONE',  ( 131.0667039024480118, -64.87844715994098976, 231.5838068554150198 ) ) ;
#86766 = DIRECTION ( 'NONE',  ( 0.000000000000000000, 0.000000000000000000, 1.000000000000000000 ) ) ;
#86767 = ORIENTED_EDGE ( 'NONE', *, *, #6795, .F. ) ;
#86768 = ORIENTED_EDGE ( 'NONE', *, *, #9797, .T. ) ;
#86769 = DIRECTION ( 'NONE',  ( -4.237773401492740281E-14, 1.000000000000000000, 0.000000000000000000 ) ) ;
#86770 = FACE_OUTER_BOUND ( 'NONE', #26124, .T. ) ;
#86771 = FACE_OUTER_BOUND ( 'NONE', #55361, .T. ) ;
#86772 = AXIS2_PLACEMENT_3D ( 'NONE', #16359, #64065, #1840 ) ;
#86774 = DIRECTION ( 'NONE',  ( 0.000000000000000000, 1.000000000000000000, 0.000000000000000000 ) ) ;
#86773 = CARTESIAN_POINT ( 'NONE',  ( 117.0099953369308281, -35.16094053785537454, 249.9518134712358801 ) ) ;
#86775 = DIRECTION ( 'NONE',  ( 0.000000000000000000, 0.000000000000000000, 1.000000000000000000 ) ) ;
#86776 = AXIS2_PLACEMENT_3D ( 'NONE', #89685, #624, #7000 ) ;
#86777 = VERTEX_POINT ( 'NONE', #26621 ) ;
#86778 = VECTOR ( 'NONE', #71350, 1000.000000000000000 ) ;
#86779 = CARTESIAN_POINT ( 'NONE',  ( 116.8171228623376265, -34.15291831040233461, 35.03145861012588824 ) ) ;
#86780 = EDGE_CURVE ( 'NONE', #51570, #74209, #87962, .T. ) ;
#86781 = CARTESIAN_POINT ( 'NONE',  ( 96.69720940280909360, -36.59277893904148726, 152.3280062282909739 ) ) ;
#86783 = EDGE_LOOP ( 'NONE', ( #67772, #52595, #81313 ) ) ;
#86782 = DIRECTION ( 'NONE',  ( 4.299999999999999979E-14, -1.000000000000000000, 4.400000000000000367E-29 ) ) ;
#86784 = AXIS2_PLACEMENT_3D ( 'NONE', #25680, #68374, #54249 ) ;
#86785 = CARTESIAN_POINT ( 'NONE',  ( 106.9359508110862578, -26.91635713860572920, 56.08705384733897148 ) ) ;
#86786 = CARTESIAN_POINT ( 'NONE',  ( 131.0667039024480118, -58.72944715994092491, 204.3338068554149913 ) ) ;
#86787 = DIRECTION ( 'NONE',  ( 1.000000000000000078E-15, -1.000000000000000083E-30, -1.000000000000000000 ) ) ;
#86788 = VECTOR ( 'NONE', #11608, 1000.000000000000000 ) ;
#86789 = EDGE_LOOP ( 'NONE', ( #64272, #76081, #30003, #62495 ) ) ;
#86790 = DIRECTION ( 'NONE',  ( 1.000000000000000000, 0.000000000000000000, 0.000000000000000000 ) ) ;
#86791 = AXIS2_PLACEMENT_3D ( 'NONE', #73492, #38970, #66678 ) ;
#86792 = CIRCLE ( 'NONE', #37521, 4.750000000000004441 ) ;
#86793 = ORIENTED_EDGE ( 'NONE', *, *, #2813, .F. ) ;
#86794 = VERTEX_POINT ( 'NONE', #6629 ) ;
#86795 = CARTESIAN_POINT ( 'NONE',  ( 99.82831888057269509, -43.73513634207608902, 188.3701547344689686 ) ) ;
#86796 = CYLINDRICAL_SURFACE ( 'NONE', #6694, 2.030000000001807248 ) ;
#86797 = EDGE_CURVE ( 'NONE', #2880, #23552, #26179, .T. ) ;
#86798 = CARTESIAN_POINT ( 'NONE',  ( 23.35572197099206448, 86.13643889426903399, 306.0438936232959577 ) ) ;
#86799 = CARTESIAN_POINT ( 'NONE',  ( 134.0664832912740110, -8.350947159940998787, 4.925625275911999168 ) ) ;
#86800 = VECTOR ( 'NONE', #71765, 1000.000000000000000 ) ;
#86801 = CARTESIAN_POINT ( 'NONE',  ( 42.66648329127298922, 12.92155284005730387, 355.9756252759109998 ) ) ;
#86802 = ORIENTED_EDGE ( 'NONE', *, *, #10397, .F. ) ;
#86803 = DIRECTION ( 'NONE',  ( 9.351236661543306751E-17, -3.725950533538267725E-29, -1.000000000000000000 ) ) ;
#86804 = CARTESIAN_POINT ( 'NONE',  ( 194.5664832912739826, -18.82844715994099971, 342.9256252759119548 ) ) ;
#86805 = VERTEX_POINT ( 'NONE', #11662 ) ;
#86806 = CARTESIAN_POINT ( 'NONE',  ( 117.4688788178166732, -35.86077403649778006, 253.8927681330538348 ) ) ;
#86807 = CARTESIAN_POINT ( 'NONE',  ( 131.0667039024480118, -64.87844715994098976, 207.5838068554149913 ) ) ;
#86808 = ORIENTED_EDGE ( 'NONE', *, *, #72891, .T. ) ;
#86809 = EDGE_CURVE ( 'NONE', #783, #5130, #28692, .T. ) ;
#86810 = EDGE_CURVE ( 'NONE', #26375, #20111, #68273, .T. ) ;
#86811 = CARTESIAN_POINT ( 'NONE',  ( 31.78666935232898894, -29.62846900982320264, -5.074374724088000832 ) ) ;
#86812 = CARTESIAN_POINT ( 'NONE',  ( 168.0371591254543944, -48.62818131005519717, 249.9678068554149775 ) ) ;
#86813 = FACE_OUTER_BOUND ( 'NONE', #35709, .T. ) ;
#86814 = CYLINDRICAL_SURFACE ( 'NONE', #85498, 4.762500000000002842 ) ;
#86815 = AXIS2_PLACEMENT_3D ( 'NONE', #45440, #66344, #78682 ) ;
#86816 = VECTOR ( 'NONE', #16624, 1000.000000000000000 ) ;
#86817 = CARTESIAN_POINT ( 'NONE',  ( 97.01638781908712872, -41.44040028630095662, 207.6632443235299661 ) ) ;
#86818 = DIRECTION ( 'NONE',  ( 0.9659258262890693114, 0.000000000000000000, 0.2588190451025170757 ) ) ;
#86819 = ORIENTED_EDGE ( 'NONE', *, *, #12726, .T. ) ;
#86820 = CARTESIAN_POINT ( 'NONE',  ( 107.6091111025649809, -48.61711588689897212, 38.61276813305397582 ) ) ;
#86821 = CARTESIAN_POINT ( 'NONE',  ( 173.9900000000000091, 20.32000000000000028, -71.37400000000000944 ) ) ;
#86822 = EDGE_CURVE ( 'NONE', #41258, #50227, #82953, .T. ) ;
#86823 = ORIENTED_EDGE ( 'NONE', *, *, #15043, .T. ) ;
#86824 = CARTESIAN_POINT ( 'NONE',  ( 81.77561474849751733, -16.57277681850257878, 2.101554741567897011 ) ) ;
#86825 = LINE ( 'NONE', #51825, #61661 ) ;
#86826 = DIRECTION ( 'NONE',  ( 1.000000000000000000, 1.000000000000000078E-15, 0.000000000000000000 ) ) ;
#86827 = ADVANCED_FACE ( 'NONE', ( #75231 ), #46599, .F. ) ;
#86828 = CARTESIAN_POINT ( 'NONE',  ( 104.2492358271959603, -44.39057208814350020, 140.1138046553059837 ) ) ;
#86829 = CARTESIAN_POINT ( 'NONE',  ( 98.82211989244140682, -29.33244250316893087, 231.7565776568629587 ) ) ;
#86830 = DIRECTION ( 'NONE',  ( 0.000000000000000000, -1.000000000000000000, 0.000000000000000000 ) ) ;
#86831 = ORIENTED_EDGE ( 'NONE', *, *, #48741, .F. ) ;
#86832 = DIRECTION ( 'NONE',  ( 1.000000000000000000, 0.000000000000000000, 0.000000000000000000 ) ) ;
#86833 = ORIENTED_EDGE ( 'NONE', *, *, #9279, .T. ) ;
#86834 = ORIENTED_EDGE ( 'NONE', *, *, #89069, .F. ) ;
#86835 = CIRCLE ( 'NONE', #14352, 3.499999999999996003 ) ;
#86836 = AXIS2_PLACEMENT_3D ( 'NONE', #6924, #55490, #55944 ) ;
#86837 = CARTESIAN_POINT ( 'NONE',  ( 137.0667039024470171, -90.27844715994091018, 230.7030882296565721 ) ) ;
#86838 =( BOUNDED_CURVE ( )  B_SPLINE_CURVE ( 3, ( #68629, #34546, #89074, #67727 ),
 .UNSPECIFIED., .F., .T. ) 
 B_SPLINE_CURVE_WITH_KNOTS ( ( 4, 4 ),
 ( 2.671434693666587812, 3.611750613512999308 ),
 .UNSPECIFIED. ) 
 CURVE ( )  GEOMETRIC_REPRESENTATION_ITEM ( )  RATIONAL_B_SPLINE_CURVE ( ( 1.000000000000000000, 0.9276644927932375939, 0.9276644927932375939, 1.000000000000000000 ) ) 
 REPRESENTATION_ITEM ( '' )  );
#86839 = ORIENTED_EDGE ( 'NONE', *, *, #18188, .T. ) ;
#86840 = ORIENTED_EDGE ( 'NONE', *, *, #37798, .T. ) ;
#86841 = DIRECTION ( 'NONE',  ( 0.9242245927363033076, 0.3818493186865918876, 0.000000000000000000 ) ) ;
#86842 = LINE ( 'NONE', #80937, #13811 ) ;
#86843 = CARTESIAN_POINT ( 'NONE',  ( 163.0664832912739826, -8.350947159940998787, 330.8831252759119934 ) ) ;
#86844 = CARTESIAN_POINT ( 'NONE',  ( 97.73346832622766556, -34.05261013000342274, 140.5267055423629756 ) ) ;
#86845 = CARTESIAN_POINT ( 'NONE',  ( 114.1203865811702087, -46.31439608500644312, 33.08133956162495792 ) ) ;
#86846 = EDGE_CURVE ( 'NONE', #25435, #40826, #6967, .T. ) ;
#86847 = ORIENTED_EDGE ( 'NONE', *, *, #25316, .F. ) ;
#86848 = AXIS2_PLACEMENT_3D ( 'NONE', #1354, #49921, #70850 ) ;
#86849 = EDGE_CURVE ( 'NONE', #81381, #753, #25726, .T. ) ;
#86850 = CYLINDRICAL_SURFACE ( 'NONE', #70234, 2.500000000000002220 ) ;
#86851 = EDGE_LOOP ( 'NONE', ( #56531, #86192, #5055, #59854, #46527, #12305 ) ) ;
#86852 = EDGE_CURVE ( 'NONE', #86777, #33131, #39356, .T. ) ;
#86853 = CIRCLE ( 'NONE', #49146, 4.762500000000000178 ) ;
#86854 = DIRECTION ( 'NONE',  ( -1.000000000000000000, -3.114895971316861016E-16, 0.000000000000000000 ) ) ;
#86855 = ORIENTED_EDGE ( 'NONE', *, *, #44350, .T. ) ;
#86856 = CARTESIAN_POINT ( 'NONE',  ( 130.5667039024479834, -40.02944715994100022, 239.5838068554162987 ) ) ;
#86857 = EDGE_CURVE ( 'NONE', #51387, #70197, #27516, .T. ) ;
#86858 = VECTOR ( 'NONE', #79392, 1000.000000000000000 ) ;
#86859 = LINE ( 'NONE', #39140, #54572 ) ;
#86860 = LINE ( 'NONE', #58671, #51856 ) ;
#86861 = PLANE ( 'NONE',  #33498 ) ;
#86862 = ORIENTED_EDGE ( 'NONE', *, *, #9012, .T. ) ;
#86863 = CARTESIAN_POINT ( 'NONE',  ( 97.77253489752784787, -40.53345146323919579, 11.63562527591094309 ) ) ;
#86864 = CARTESIAN_POINT ( 'NONE',  ( 99.03245663461365211, -44.38790092286875932, 32.92038718067297509 ) ) ;
#86866 = CARTESIAN_POINT ( 'NONE',  ( -24.79284581386642827, 184.0000000000000000, 0.000000000000000000 ) ) ;
#86865 = PLANE ( 'NONE',  #24521 ) ;
#86867 = DIRECTION ( 'NONE',  ( -4.299999999999999979E-14, 1.000000000000000000, -4.400000000000000367E-29 ) ) ;
#86868 = DIRECTION ( 'NONE',  ( 0.000000000000000000, 0.000000000000000000, -1.000000000000000000 ) ) ;
#86869 = FACE_BOUND ( 'NONE', #29071, .T. ) ;
#86870 = AXIS2_PLACEMENT_3D ( 'NONE', #40797, #67613, #13994 ) ;
#86871 = DIRECTION ( 'NONE',  ( -1.000000000000000078E-15, 1.000000000000000000, 0.000000000000000000 ) ) ;
#86872 = CARTESIAN_POINT ( 'NONE',  ( 104.4083387335005426, -46.45815895792671313, 162.3646280642559816 ) ) ;
#86873 = DIRECTION ( 'NONE',  ( -1.000000000000000000, 0.000000000000000000, -1.092739197465703932E-16 ) ) ;
#86874 = CARTESIAN_POINT ( 'NONE',  ( 101.0739185617116078, -45.28721829360737416, 282.0899109901967563 ) ) ;
#86875 = CARTESIAN_POINT ( 'NONE',  ( 115.5173804941753133, -29.60510038635626273, 220.3718157521019521 ) ) ;
#86876 = CARTESIAN_POINT ( 'NONE',  ( 97.75304581901603740, -31.99688534799786765, 46.95276813305393659 ) ) ;
#86878 = CARTESIAN_POINT ( 'NONE',  ( 0.000000000000000000, 125.7300000000000040, 0.000000000000000000 ) ) ;
#86877 = LINE ( 'NONE', #9237, #81336 ) ;
#86879 = DIRECTION ( 'NONE',  ( -0.7071067811861110330, -0.7071067811869841124, 0.000000000000000000 ) ) ;
#86880 = AXIS2_PLACEMENT_3D ( 'NONE', #40963, #27786, #20983 ) ;
#86881 = ORIENTED_EDGE ( 'NONE', *, *, #64888, .F. ) ;
#86882 = DIRECTION ( 'NONE',  ( 0.000000000000000000, 0.000000000000000000, -1.000000000000000000 ) ) ;
#86883 = VERTEX_POINT ( 'NONE', #54296 ) ;
#86884 = CARTESIAN_POINT ( 'NONE',  ( 107.8187922529720026, -26.97765417004757538, 66.01562527591097762 ) ) ;
#86886 = ORIENTED_EDGE ( 'NONE', *, *, #64091, .T. ) ;
#86885 = DIRECTION ( 'NONE',  ( 0.000000000000000000, 0.000000000000000000, 1.000000000000000000 ) ) ;
#86887 = DIRECTION ( 'NONE',  ( 0.000000000000000000, 0.000000000000000000, -1.000000000000000000 ) ) ;
#86888 = CARTESIAN_POINT ( 'NONE',  ( 106.9407056411434951, -47.75886249174716625, 228.5794347997199907 ) ) ;
#86889 = LINE ( 'NONE', #80986, #38218 ) ;
#86890 = CARTESIAN_POINT ( 'NONE',  ( 172.5664832912728457, -27.82844715994070484, 261.9256252759120116 ) ) ;
#86891 = DIRECTION ( 'NONE',  ( -1.000000000000000078E-15, 1.000000000000000083E-30, 1.000000000000000000 ) ) ;
#86892 = CARTESIAN_POINT ( 'NONE',  ( 131.3179999999999836, 37.33800000000000097, 50.79999999999999716 ) ) ;
#86893 = AXIS2_PLACEMENT_3D ( 'NONE', #67294, #11902, #25519 ) ;
#86894 = PLANE ( 'NONE',  #8563 ) ;
#86895 = CARTESIAN_POINT ( 'NONE',  ( 48.45959712127340424, -26.00627455219079209, 237.4678068554150059 ) ) ;
#86896 = CARTESIAN_POINT ( 'NONE',  ( 97.98063455390165188, -41.72806076336413383, 176.7146728949589658 ) ) ;
#86897 = VERTEX_POINT ( 'NONE', #18913 ) ;
#86898 = ORIENTED_EDGE ( 'NONE', *, *, #11974, .T. ) ;
#86899 = AXIS2_PLACEMENT_3D ( 'NONE', #35722, #56150, #49793 ) ;
#86900 = CARTESIAN_POINT ( 'NONE',  ( 112.5403241924349942, -29.76056314593741803, 75.97872616303996551 ) ) ;
#86901 = AXIS2_PLACEMENT_3D ( 'NONE', #39986, #73618, #38207 ) ;
#86902 = LINE ( 'NONE', #52772, #47195 ) ;
#86903 = EDGE_CURVE ( 'NONE', #17773, #28811, #27047, .T. ) ;
#86905 = CARTESIAN_POINT ( 'NONE',  ( 130.3998166246059895, 12.92155284005730387, 358.9756252759109998 ) ) ;
#86904 = CARTESIAN_POINT ( 'NONE',  ( 106.9482321581270270, -47.09886382165559127, 228.5794347997199907 ) ) ;
#86906 = PLANE ( 'NONE',  #33318 ) ;
#86907 = DIRECTION ( 'NONE',  ( 0.000000000000000000, 0.000000000000000000, 1.000000000000000000 ) ) ;
#86908 = EDGE_CURVE ( 'NONE', #49561, #24002, #88232, .T. ) ;
#86909 = CARTESIAN_POINT ( 'NONE',  ( 118.4860207371917085, 70.52018178143197247, 4.092354625463673123 ) ) ;
#86911 = ADVANCED_FACE ( 'NONE', ( #42032, #41576 ), #76113, .T. ) ;
#86910 = AXIS2_PLACEMENT_3D ( 'NONE', #30516, #33194, #75876 ) ;
#86912 = CARTESIAN_POINT ( 'NONE',  ( -5.244729318936814266, 70.97606371242190448, 118.4405590227164851 ) ) ;
#86913 = DIRECTION ( 'NONE',  ( 1.000000000000000000, 0.000000000000000000, 0.000000000000000000 ) ) ;
#86914 = LINE ( 'NONE', #58732, #47261 ) ;
#86915 = CARTESIAN_POINT ( 'NONE',  ( 101.7806060443208480, -45.68981339355064364, 162.1527681330539679 ) ) ;
#86916 = ORIENTED_EDGE ( 'NONE', *, *, #61811, .F. ) ;
#86917 = EDGE_LOOP ( 'NONE', ( #39894, #8602, #86330, #79235 ) ) ;
#86918 = EDGE_CURVE ( 'NONE', #30970, #39820, #62482, .T. ) ;
#86919 = EDGE_CURVE ( 'NONE', #84782, #79006, #35219, .T. ) ;
#86920 = CARTESIAN_POINT ( 'NONE',  ( 182.2420472961728137, -31.76306994223174840, 237.4678068554150059 ) ) ;
#86921 = CARTESIAN_POINT ( 'NONE',  ( 145.8651347429109251, -69.02927824504203613, 247.3313947546042755 ) ) ;
#86922 = AXIS2_PLACEMENT_3D ( 'NONE', #37375, #30999, #58692 ) ;
#86923 = DIRECTION ( 'NONE',  ( -1.000000000000000000, 0.000000000000000000, 0.000000000000000000 ) ) ;
#86924 = CARTESIAN_POINT ( 'NONE',  ( -215.9000000000000057, 3.174999999999999822, -41.27499999999999858 ) ) ;
#86925 = EDGE_CURVE ( 'NONE', #30791, #40389, #46104, .T. ) ;
#86926 = EDGE_CURVE ( 'NONE', #82549, #73698, #30187, .T. ) ;
#86927 = CARTESIAN_POINT ( 'NONE',  ( 156.5667039024485803, -48.82844715993568485, 137.2178068554149775 ) ) ;
#86928 = ADVANCED_FACE ( 'NONE', ( #12333 ), #80486, .F. ) ;
#86929 = CARTESIAN_POINT ( 'NONE',  ( 96.74292298454378169, -35.27647329413149890, 181.2156252759109805 ) ) ;
#86930 = CARTESIAN_POINT ( 'NONE',  ( 20.03715912545732891, -24.95799193693189721, 300.4678068554150059 ) ) ;
#86931 = ORIENTED_EDGE ( 'NONE', *, *, #58920, .T. ) ;
#86933 = ORIENTED_EDGE ( 'NONE', *, *, #36902, .T. ) ;
#86932 = ORIENTED_EDGE ( 'NONE', *, *, #32043, .F. ) ;
#86934 = AXIS2_PLACEMENT_3D ( 'NONE', #42688, #62704, #40912 ) ;
#86935 = DIRECTION ( 'NONE',  ( 0.000000000000000000, -0.5150380749100549327, -0.8571673007021118895 ) ) ;
#86936 = CARTESIAN_POINT ( 'NONE',  ( 8.398627748552550652E-16, 50.79999999999999716, 272.4150000000000205 ) ) ;
#86937 = CARTESIAN_POINT ( 'NONE',  ( 117.0720925080216404, -35.46411601386796519, 164.9271620083415826 ) ) ;
#86938 = ADVANCED_FACE ( 'NONE', ( #31871 ), #45042, .T. ) ;
#86939 = CARTESIAN_POINT ( 'NONE',  ( 112.7530619618799932, -30.23101651580132199, 285.9349166392303800 ) ) ;
#86940 = CARTESIAN_POINT ( 'NONE',  ( 125.0664851986225443, -56.72944715994101728, -4.824374724089012467 ) ) ;
#86941 = ORIENTED_EDGE ( 'NONE', *, *, #20811, .F. ) ;
#86942 = CARTESIAN_POINT ( 'NONE',  ( -479.3614999999999782, 101.9113919710471947, 11.11250000000054072 ) ) ;
#86943 = CIRCLE ( 'NONE', #66636, 5.562599999999973122 ) ;
#86944 = DIRECTION ( 'NONE',  ( 1.000000000000000078E-15, 1.000000000000000083E-30, -1.000000000000000000 ) ) ;
#86945 = ORIENTED_EDGE ( 'NONE', *, *, #11843, .F. ) ;
#86946 = ORIENTED_EDGE ( 'NONE', *, *, #6679, .T. ) ;
#86947 = DIRECTION ( 'NONE',  ( 0.000000000000000000, -1.000000000000000000, 0.000000000000000000 ) ) ;
#86948 = ORIENTED_EDGE ( 'NONE', *, *, #35363, .F. ) ;
#86949 = ORIENTED_EDGE ( 'NONE', *, *, #84814, .F. ) ;
#86950 = CARTESIAN_POINT ( 'NONE',  ( 116.3215253324775773, -32.93968801256757217, 155.1356252759109680 ) ) ;
#86951 = CARTESIAN_POINT ( 'NONE',  ( 110.6296508234850222, -44.49217663217273611, 27.34099125664796048 ) ) ;
#86952 = CARTESIAN_POINT ( 'NONE',  ( 116.3700403630726612, -44.11035778917459993, 198.2927681330539542 ) ) ;
#86953 = CARTESIAN_POINT ( 'NONE',  ( 117.4654710391980217, -40.40706546494233464, 178.5680062282919778 ) ) ;
#86954 = CARTESIAN_POINT ( 'NONE',  ( 1.387778780781445676E-14, 223.9999999999999716, 97.27542076772557778 ) ) ;
#86955 = CARTESIAN_POINT ( 'NONE',  ( 116.5364499171840720, -42.42977282487416346, 274.3832443235299365 ) ) ;
#86956 = DIRECTION ( 'NONE',  ( 1.000000000000000000, 0.000000000000000000, 0.000000000000000000 ) ) ;
#86957 = LINE ( 'NONE', #80596, #55473 ) ;
#86958 = ORIENTED_EDGE ( 'NONE', *, *, #63125, .F. ) ;
#86959 = EDGE_CURVE ( 'NONE', #70182, #59657, #5530, .T. ) ;
#86960 = CIRCLE ( 'NONE', #68088, 2.500000000000002220 ) ;
#86961 = ORIENTED_EDGE ( 'NONE', *, *, #9284, .F. ) ;
#86962 = ADVANCED_FACE ( 'NONE', ( #73198 ), #60923, .F. ) ;
#86963 = CIRCLE ( 'NONE', #50709, 3.999999999999998224 ) ;
#86964 = CIRCLE ( 'NONE', #47774, 4.762499999999999289 ) ;
#86965 = DIRECTION ( 'NONE',  ( 0.7071067811865614505, -0.7071067811865336949, 0.000000000000000000 ) ) ;
#86966 = CARTESIAN_POINT ( 'NONE',  ( 118.0872578842352993, -35.40452791748241879, 238.9337205140059552 ) ) ;
#86967 = VERTEX_POINT ( 'NONE', #79601 ) ;
#86968 = CARTESIAN_POINT ( 'NONE',  ( 107.6530059321349455, -47.12789624220987150, 152.6213395616249500 ) ) ;
#86969 = FACE_OUTER_BOUND ( 'NONE', #27996, .T. ) ;
#86970 = FACE_OUTER_BOUND ( 'NONE', #14058, .T. ) ;
#86971 = CARTESIAN_POINT ( 'NONE',  ( 106.0667039024470171, -87.35579742913141388, -11.78219314458253741 ) ) ;
#86972 = FACE_OUTER_BOUND ( 'NONE', #45259, .T. ) ;
#86975 = CARTESIAN_POINT ( 'NONE',  ( 116.5620552962770802, -42.34175257684895399, 279.4137205140061724 ) ) ;
#86974 = CARTESIAN_POINT ( 'NONE',  ( 74.06670390244701707, -90.27844715994098124, 45.21780685541799727 ) ) ;
#86973 = DIRECTION ( 'NONE',  ( 5.512527431108029424E-15, -1.000000000000000000, 0.000000000000000000 ) ) ;
#86976 = DIRECTION ( 'NONE',  ( 0.000000000000000000, -1.000000000000000000, 0.000000000000000000 ) ) ;
#86977 = CARTESIAN_POINT ( 'NONE',  ( 107.0664832912739968, -36.72944715994100306, -2.364374724089013391 ) ) ;
#86978 = CARTESIAN_POINT ( 'NONE',  ( 193.0371591254583450, -47.82818131005411999, 249.9678068554149775 ) ) ;
#86979 = VECTOR ( 'NONE', #21671, 1000.000000000000000 ) ;
#86980 = CARTESIAN_POINT ( 'NONE',  ( 68.09855418781428682, -137.1459507998173137, 247.2571523348723019 ) ) ;
#86981 = CARTESIAN_POINT ( 'NONE',  ( 56.06670390244699576, -67.87844715994098976, 85.21780685541799016 ) ) ;
#86982 = CARTESIAN_POINT ( 'NONE',  ( 128.0667039024480118, -58.72944715994110254, 310.9178068554150514 ) ) ;
#86984 = EDGE_LOOP ( 'NONE', ( #27207, #94, #49912, #44994 ) ) ;
#86983 = CARTESIAN_POINT ( 'NONE',  ( 109.5808203229745743, -44.32760431976820570, 195.5838068554168103 ) ) ;
#86985 = CARTESIAN_POINT ( 'NONE',  ( 151.0371591254573787, -24.95799193692592866, 249.9678068554149490 ) ) ;
#86986 = CARTESIAN_POINT ( 'NONE',  ( 97.38146765292194118, -40.64695096355149673, 206.6327681330539860 ) ) ;
#86987 = CARTESIAN_POINT ( 'NONE',  ( 113.8563929230154912, -44.64017497981368621, 104.1413395616249744 ) ) ;
#86988 = CARTESIAN_POINT ( 'NONE',  ( 107.5118819425545951, -47.18863449879560079, 233.6099109901969655 ) ) ;
#86989 = CARTESIAN_POINT ( 'NONE',  ( 128.0667039024480118, -58.72944715994112386, 198.9178068554149945 ) ) ;
#86990 = AXIS2_PLACEMENT_3D ( 'NONE', #28854, #7064, #7510 ) ;
#86991 = CARTESIAN_POINT ( 'NONE',  ( 107.0664832912739257, -52.72944715994095333, 311.3356252759109566 ) ) ;
#86993 = CARTESIAN_POINT ( 'NONE',  ( 104.7197490991536881, -46.50674210198418734, 38.38840247910224690 ) ) ;
#86992 = FACE_OUTER_BOUND ( 'NONE', #14491, .T. ) ;
#86994 = DIRECTION ( 'NONE',  ( 0.000000000000000000, 0.000000000000000000, 1.000000000000000000 ) ) ;
#86995 = LINE ( 'NONE', #37501, #17551 ) ;
#86996 = CARTESIAN_POINT ( 'NONE',  ( 29.00000000000003553, 127.0000000000000000, 183.8826257785461280 ) ) ;
#86997 = EDGE_LOOP ( 'NONE', ( #5305, #20138, #53287, #87444, #12198 ) ) ;
#86998 = ORIENTED_EDGE ( 'NONE', *, *, #50973, .F. ) ;
#86999 = CARTESIAN_POINT ( 'NONE',  ( 102.5065049712838601, -29.50707016595331567, 109.9467055423629631 ) ) ;
#87001 = ORIENTED_EDGE ( 'NONE', *, *, #43757, .T. ) ;
#87000 = DIRECTION ( 'NONE',  ( 0.000000000000000000, 0.000000000000000000, 1.000000000000000000 ) ) ;
#87002 = CARTESIAN_POINT ( 'NONE',  ( 98.87507392487052016, -43.19978241230791838, 87.85848241876792031 ) ) ;
#87003 = LINE ( 'NONE', #81987, #43908 ) ;
#87004 = CARTESIAN_POINT ( 'NONE',  ( 78.98444042533766662, -16.20116865955368723, 8.043260881866178380 ) ) ;
#87005 = CARTESIAN_POINT ( 'NONE',  ( 109.7248659318316868, -27.00080518283870035, 175.8647919417129231 ) ) ;
#87006 = CARTESIAN_POINT ( 'NONE',  ( 116.1300133678986413, -31.69047823903573047, 29.24229194257799236 ) ) ;
#87007 = ORIENTED_EDGE ( 'NONE', *, *, #65264, .F. ) ;
#87009 = ADVANCED_FACE ( 'NONE', ( #3725 ), #24181, .F. ) ;
#87008 = CIRCLE ( 'NONE', #63802, 16.33514202138213633 ) ;
#87010 = ORIENTED_EDGE ( 'NONE', *, *, #61869, .F. ) ;
#87011 = ORIENTED_EDGE ( 'NONE', *, *, #764, .F. ) ;
#87012 = LINE ( 'NONE', #3443, #60170 ) ;
#87014 = DIRECTION ( 'NONE',  ( -0.000000000000000000, 1.000000000000000000, -0.000000000000000000 ) ) ;
#87013 = CARTESIAN_POINT ( 'NONE',  ( 102.9676436823274202, -46.25511244710193637, 133.2651490854339613 ) ) ;
#87015 = CARTESIAN_POINT ( 'NONE',  ( 179.4595971212720258, -26.00627455219131789, -5.074374724088000832 ) ) ;
#87016 = EDGE_CURVE ( 'NONE', #43994, #12205, #11438, .T. ) ;
#87017 = CARTESIAN_POINT ( 'NONE',  ( 10.09455232642977052, 74.79837219561763106, -130.1659940687516723 ) ) ;
#87018 = ADVANCED_FACE ( 'NONE', ( #18694 ), #72772, .F. ) ;
#87019 = CYLINDRICAL_SURFACE ( 'NONE', #78120, 0.2500000000000002220 ) ;
#87020 = VECTOR ( 'NONE', #39188, 1000.000000000000000 ) ;
#87021 = EDGE_CURVE ( 'NONE', #20859, #58541, #65003, .T. ) ;
#87022 = CARTESIAN_POINT ( 'NONE',  ( -10.20556736627216843, 90.12022208354639474, 130.1569092081103349 ) ) ;
#87023 = DIRECTION ( 'NONE',  ( 0.000000000000000000, 0.000000000000000000, -1.000000000000000000 ) ) ;
#87024 = CARTESIAN_POINT ( 'NONE',  ( 112.7479404651554376, -27.97242311821432992, 69.61848241876793963 ) ) ;
#87025 = ORIENTED_EDGE ( 'NONE', *, *, #82614, .F. ) ;
#87026 = ORIENTED_EDGE ( 'NONE', *, *, #8109, .F. ) ;
#87027 = CIRCLE ( 'NONE', #17379, 5.041900000000001825 ) ;
#87028 = ADVANCED_FACE ( 'NONE', ( #39137 ), #25508, .T. ) ;
#87029 = FACE_OUTER_BOUND ( 'NONE', #75976, .T. ) ;
#87030 = FACE_OUTER_BOUND ( 'NONE', #58049, .T. ) ;
#87031 = LINE ( 'NONE', #65240, #38061 ) ;
#87032 = CARTESIAN_POINT ( 'NONE',  ( 108.5374814027631203, -28.67222352762033211, 162.7509475124489597 ) ) ;
#87033 = VECTOR ( 'NONE', #77572, 1000.000000000000000 ) ;
#87034 = EDGE_CURVE ( 'NONE', #51043, #29395, #4176, .T. ) ;
#87035 = EDGE_CURVE ( 'NONE', #21921, #24432, #24356, .T. ) ;
#87036 = DIRECTION ( 'NONE',  ( 0.000000000000000000, 0.000000000000000000, -1.000000000000000000 ) ) ;
#87037 = ORIENTED_EDGE ( 'NONE', *, *, #56319, .T. ) ;
#87038 = ORIENTED_EDGE ( 'NONE', *, *, #76638, .F. ) ;
#87039 = VECTOR ( 'NONE', #76427, 1000.000000000000000 ) ;
#87040 = DIRECTION ( 'NONE',  ( 1.000000000000000078E-15, 1.000000000000000083E-30, -1.000000000000000000 ) ) ;
#87041 = ORIENTED_EDGE ( 'NONE', *, *, #22329, .T. ) ;
#87042 = VERTEX_POINT ( 'NONE', #59562 ) ;
#87043 = AXIS2_PLACEMENT_3D ( 'NONE', #36823, #65847, #24533 ) ;
#87044 = FACE_OUTER_BOUND ( 'NONE', #42631, .T. ) ;
#87045 = EDGE_CURVE ( 'NONE', #87386, #4730, #33224, .T. ) ;
#87046 = CARTESIAN_POINT ( 'NONE',  ( 115.2219208674478352, -40.19601845633869175, 164.9387261630399450 ) ) ;
#87047 = CARTESIAN_POINT ( 'NONE',  ( 163.2569089553700223, -33.54226604285010893, -5.074374724088000832 ) ) ;
#87048 = DIRECTION ( 'NONE',  ( 0.000000000000000000, 0.000000000000000000, 1.000000000000000000 ) ) ;
#87049 = CARTESIAN_POINT ( 'NONE',  ( 188.5667039024479834, -62.87844715994099687, 293.2178068554150627 ) ) ;
#87050 = ORIENTED_EDGE ( 'NONE', *, *, #37597, .F. ) ;
#87051 = ORIENTED_EDGE ( 'NONE', *, *, #31363, .F. ) ;
#87052 = ORIENTED_EDGE ( 'NONE', *, *, #77859, .F. ) ;
#87053 = VERTEX_POINT ( 'NONE', #31417 ) ;
#87054 = AXIS2_PLACEMENT_3D ( 'NONE', #60124, #18810, #38353 ) ;
#87055 = CARTESIAN_POINT ( 'NONE',  ( 99.07378970379950545, -35.07216769230775810, 213.9823760838769715 ) ) ;
#87056 = CARTESIAN_POINT ( 'NONE',  ( 98.82253044624914651, -28.18127440817969287, 115.6870538473389587 ) ) ;
#87057 = CARTESIAN_POINT ( 'NONE',  ( 110.5478855402368197, -46.57039549162855963, 37.84705384733994293 ) ) ;
#87058 = LINE ( 'NONE', #17124, #16735 ) ;
#87059 = LINE ( 'NONE', #3483, #61117 ) ;
#87060 = DIRECTION ( 'NONE',  ( -1.175184669632759901E-16, 1.000000000000000000, 2.000000000000003705E-15 ) ) ;
#87061 = CARTESIAN_POINT ( 'NONE',  ( 111.4172602844868862, -47.75239391268459599, 168.8756252759109486 ) ) ;
#87062 = FACE_OUTER_BOUND ( 'NONE', #24970, .T. ) ;
#87063 = VERTEX_POINT ( 'NONE', #17801 ) ;
#87064 = CARTESIAN_POINT ( 'NONE',  ( 194.5664832912739826, -18.82844715994099971, -5.074374724088000832 ) ) ;
#87065 = ORIENTED_EDGE ( 'NONE', *, *, #85515, .F. ) ;
#87066 = ORIENTED_EDGE ( 'NONE', *, *, #48121, .F. ) ;
#87067 = CARTESIAN_POINT ( 'NONE',  ( 51.42025729302798709, -31.94127993907680718, -5.074374724088000832 ) ) ;
#87068 = ORIENTED_EDGE ( 'NONE', *, *, #66474, .F. ) ;
#87069 = ADVANCED_FACE ( 'NONE', ( #66842 ), #88205, .T. ) ;
#87071 = ORIENTED_EDGE ( 'NONE', *, *, #72869, .T. ) ;
#87070 = AXIS2_PLACEMENT_3D ( 'NONE', #30496, #50929, #57288 ) ;
#87072 = DIRECTION ( 'NONE',  ( 0.000000000000000000, 1.000000000000000000, 0.000000000000000000 ) ) ;
#87073 = VERTEX_POINT ( 'NONE', #5067 ) ;
#87074 = CARTESIAN_POINT ( 'NONE',  ( -254.0000000000000000, 53.97500000000000142, 50.79999999999999716 ) ) ;
#87075 = CARTESIAN_POINT ( 'NONE',  ( 97.62219055090962172, -32.23153194184447301, 75.97276813305397525 ) ) ;
#87076 = CARTESIAN_POINT ( 'NONE',  ( 57.91199999999999903, 20.32000000000000028, 178.6098374884404905 ) ) ;
#87077 = CARTESIAN_POINT ( 'NONE',  ( 163.0664832912739826, 0.2215528400590083269, 333.4006252759110112 ) ) ;
#87078 = DIRECTION ( 'NONE',  ( 0.000000000000000000, 0.000000000000000000, 1.000000000000000000 ) ) ;
#87079 = CARTESIAN_POINT ( 'NONE',  ( 96.07333748454163924, -35.06730156692549372, 71.20705384733993526 ) ) ;
#87081 = CARTESIAN_POINT ( 'NONE',  ( 96.66614461754338095, -36.48121138304695421, 192.3070538473399438 ) ) ;
#87080 = CARTESIAN_POINT ( 'NONE',  ( 72.31648329127401098, -45.62589376934781882, 14.92562527591093691 ) ) ;
#87082 = CARTESIAN_POINT ( 'NONE',  ( 109.7211212765799786, -26.99981308150919546, 59.86509729586450135 ) ) ;
#87083 = DIRECTION ( 'NONE',  ( 0.000000000000000000, 1.000000000000000000, 0.000000000000000000 ) ) ;
#87084 = VERTEX_POINT ( 'NONE', #32769 ) ;
#87085 = CARTESIAN_POINT ( 'NONE',  ( 108.8673596973266058, 37.33800000000000097, 42.86249999999999716 ) ) ;
#87086 = VECTOR ( 'NONE', #18982, 1000.000000000000000 ) ;
#87087 = DIRECTION ( 'NONE',  ( -1.000000000000000000, -1.000000000000000078E-15, 0.000000000000000000 ) ) ;
#87088 = DIRECTION ( 'NONE',  ( 1.000000000000000000, 4.299999999999999979E-14, 1.000000000000000078E-15 ) ) ;
#87089 = CYLINDRICAL_SURFACE ( 'NONE', #50597, 13.16666666666670160 ) ;
#87090 = EDGE_CURVE ( 'NONE', #20391, #42590, #75111, .T. ) ;
#87092 = EDGE_LOOP ( 'NONE', ( #52713, #21339, #51583, #59749, #44131, #33757 ) ) ;
#87091 = CARTESIAN_POINT ( 'NONE',  ( 104.1736071946568103, -26.63078081164005440, 225.2984824187679749 ) ) ;
#87093 = CARTESIAN_POINT ( 'NONE',  ( 0.000000000000000000, 124.9679999999999893, -25.39999999999999858 ) ) ;
#87094 = CARTESIAN_POINT ( 'NONE',  ( 96.75463230179867935, -40.77307608890721013, 242.6118157521009664 ) ) ;
#87095 = CARTESIAN_POINT ( 'NONE',  ( 102.5975616584704966, -46.88947854763195267, 128.2346728949589760 ) ) ;
#87096 = DIRECTION ( 'NONE',  ( -1.000000000000000078E-15, 1.000000000000000083E-30, 1.000000000000000000 ) ) ;
#87097 = CARTESIAN_POINT ( 'NONE',  ( 82.41057659162468951, -38.17027654744429555, 7.249284792661043753 ) ) ;
#87098 = CARTESIAN_POINT ( 'NONE',  ( 117.0667039024470455, -109.9573555057414325, 7.717806855418146483 ) ) ;
#87099 = CARTESIAN_POINT ( 'NONE',  ( 117.0607235903083705, -38.08165846641635000, 264.7191046043259917 ) ) ;
#87100 = ORIENTED_EDGE ( 'NONE', *, *, #27130, .T. ) ;
#87101 = VECTOR ( 'NONE', #69543, 1000.000000000000000 ) ;
#87102 = EDGE_CURVE ( 'NONE', #89625, #45788, #32499, .T. ) ;
#87103 = EDGE_LOOP ( 'NONE', ( #52847, #37603, #80006, #44676 ) ) ;
#87104 = ORIENTED_EDGE ( 'NONE', *, *, #36572, .F. ) ;
#87105 = CIRCLE ( 'NONE', #3007, 3.174999999999997158 ) ;
#87106 = EDGE_LOOP ( 'NONE', ( #30081, #22228, #88417, #10069, #36725 ) ) ;
#87107 = DIRECTION ( 'NONE',  ( 0.000000000000000000, 1.000000000000000000, 0.000000000000000000 ) ) ;
#87108 = CARTESIAN_POINT ( 'NONE',  ( 99.38154727845876835, -29.68499927947409489, 271.7356252759109907 ) ) ;
#87109 = DIRECTION ( 'NONE',  ( -1.000000000000000000, -8.540177112501204385E-16, 0.000000000000000000 ) ) ;
#87110 = CARTESIAN_POINT ( 'NONE',  ( 132.0298243561165918, -34.87939921900699147, 2.327894594454071875 ) ) ;
#87111 = COLOUR_RGB ( '', 0.31764706, 0.68627451, 0.89019608) ;
#87113 = CARTESIAN_POINT ( 'NONE',  ( 115.0894713190635628, -30.61837156327993625, 149.3442108353245317 ) ) ;
#87112 = FACE_OUTER_BOUND ( 'NONE', #33848, .T. ) ;
#87114 = CARTESIAN_POINT ( 'NONE',  ( 112.8494018163660968, -30.44343212223953543, 198.9067055423629711 ) ) ;
#87115 = ORIENTED_EDGE ( 'NONE', *, *, #46886, .F. ) ;
#87116 = ORIENTED_EDGE ( 'NONE', *, *, #68497, .F. ) ;
#87117 = ORIENTED_EDGE ( 'NONE', *, *, #59201, .T. ) ;
#87118 = CARTESIAN_POINT ( 'NONE',  ( 0.000000000000000000, 91.07499999999996021, 0.000000000000000000 ) ) ;
#87119 = DIRECTION ( 'NONE',  ( 0.000000000000000000, 0.000000000000000000, 1.000000000000000000 ) ) ;
#87120 = CARTESIAN_POINT ( 'NONE',  ( -194.1576000000000022, 101.5999999999999943, -45.33899999999999864 ) ) ;
#87121 = ADVANCED_FACE ( 'NONE', ( #6411 ), #7760, .T. ) ;
#87122 = CARTESIAN_POINT ( 'NONE',  ( 101.4552306925257454, -43.61128330217721327, 8.464440448754938728 ) ) ;
#87123 = EDGE_CURVE ( 'NONE', #77666, #78013, #40922, .T. ) ;
#87124 = AXIS2_PLACEMENT_3D ( 'NONE', #56749, #22254, #58096 ) ;
#87125 = CARTESIAN_POINT ( 'NONE',  ( 122.2211106478290219, -96.60847398039683753, -19.21044887263825984 ) ) ;
#87126 = AXIS2_PLACEMENT_3D ( 'NONE', #68780, #40617, #25645 ) ;
#87127 = EDGE_CURVE ( 'NONE', #47902, #85594, #50754, .T. ) ;
#87128 = LINE ( 'NONE', #63661, #78210 ) ;
#87129 = CARTESIAN_POINT ( 'NONE',  ( 72.96458098368701428, 117.4749999999999943, -80.10833098368678407 ) ) ;
#87130 = VERTEX_POINT ( 'NONE', #54974 ) ;
#87131 = EDGE_CURVE ( 'NONE', #40908, #274, #81838, .T. ) ;
#87132 = CARTESIAN_POINT ( 'NONE',  ( 103.3524915959513351, -27.44467182146633277, 56.37927426770519901 ) ) ;
#87133 = EDGE_LOOP ( 'NONE', ( #11588, #47903 ) ) ;
#87134 = AXIS2_PLACEMENT_3D ( 'NONE', #1795, #84924, #78559 ) ;
#87135 = LINE ( 'NONE', #37195, #81524 ) ;
#87136 = CARTESIAN_POINT ( 'NONE',  ( 98.54061126669880366, -38.21619907818254802, 44.26999513149598897 ) ) ;
#87137 = CARTESIAN_POINT ( 'NONE',  ( 135.7892066358463410, -16.57943358559917613, 7.744922197151018040 ) ) ;
#87138 = CARTESIAN_POINT ( 'NONE',  ( 117.4590087478601390, -115.7784471599421181, -21.78219314458165812 ) ) ;
#87139 = EDGE_CURVE ( 'NONE', #38611, #81699, #50463, .T. ) ;
#87140 = CARTESIAN_POINT ( 'NONE',  ( 6.162975822039154730E-30, 95.25000000000000000, 118.5560000000000116 ) ) ;
#87141 = ORIENTED_EDGE ( 'NONE', *, *, #32645, .T. ) ;
#87142 = DIRECTION ( 'NONE',  ( 0.000000000000000000, 0.000000000000000000, 1.000000000000000000 ) ) ;
#87143 = CARTESIAN_POINT ( 'NONE',  ( 120.3150230176155020, 57.65353451050373934, -50.68724638474388655 ) ) ;
#87144 = ORIENTED_EDGE ( 'NONE', *, *, #80198, .F. ) ;
#87145 = CARTESIAN_POINT ( 'NONE',  ( 116.9219696586192754, -33.22298239640010564, 114.0984824187679720 ) ) ;
#87146 = VERTEX_POINT ( 'NONE', #5981 ) ;
#87147 = CARTESIAN_POINT ( 'NONE',  ( 113.0365282982730264, -42.83802263516175657, 72.61527697093394806 ) ) ;
#87148 = AXIS2_PLACEMENT_3D ( 'NONE', #67448, #60627, #68805 ) ;
#87149 = AXIS2_PLACEMENT_3D ( 'NONE', #50443, #58164, #2771 ) ;
#87150 = CIRCLE ( 'NONE', #7390, 1.999999999999995781 ) ;
#87151 = CARTESIAN_POINT ( 'NONE',  ( -446.0240000000000009, 3.174999999999999822, 101.5999999999999943 ) ) ;
#87152 = CARTESIAN_POINT ( 'NONE',  ( 115.8905597133153549, -37.54428082998141747, 75.18444044875394638 ) ) ;
#87153 = CARTESIAN_POINT ( 'NONE',  ( 136.8005346357622329, -19.07423037056981840, 3.076719480830218068 ) ) ;
#87154 = FACE_OUTER_BOUND ( 'NONE', #30040, .T. ) ;
#87155 = PLANE ( 'NONE',  #499 ) ;
#87156 = CARTESIAN_POINT ( 'NONE',  ( 104.4853289249099362, -46.88901594738546663, 43.37848241876896083 ) ) ;
#87157 = AXIS2_PLACEMENT_3D ( 'NONE', #62161, #12688, #76246 ) ;
#87158 = DIRECTION ( 'NONE',  ( -3.406823656978775284E-15, 0.000000000000000000, -1.000000000000000000 ) ) ;
#87159 = ORIENTED_EDGE ( 'NONE', *, *, #41175, .F. ) ;
#87160 = DIRECTION ( 'NONE',  ( 0.0001713722456120069274, -0.9999999853157766072, 0.000000000000000000 ) ) ;
#87161 = ORIENTED_EDGE ( 'NONE', *, *, #9405, .T. ) ;
#87162 = DIRECTION ( 'NONE',  ( -1.000000000000000078E-15, 0.000000000000000000, 1.000000000000000000 ) ) ;
#87163 = ORIENTED_EDGE ( 'NONE', *, *, #20529, .F. ) ;
#87164 = ORIENTED_EDGE ( 'NONE', *, *, #3859, .T. ) ;
#87165 = AXIS2_PLACEMENT_3D ( 'NONE', #63477, #1264, #28970 ) ;
#87166 = VERTEX_POINT ( 'NONE', #69093 ) ;
#87167 = CARTESIAN_POINT ( 'NONE',  ( 96.81359797424451585, -35.17473563989037899, 221.1946728949589840 ) ) ;
#87168 = CARTESIAN_POINT ( 'NONE',  ( 116.3201495438094923, -32.94088975182634726, 124.1356252759109537 ) ) ;
#87169 = CARTESIAN_POINT ( 'NONE',  ( 115.0372574793866818, -42.90846260279429458, 189.3022919390266168 ) ) ;
#87170 = CARTESIAN_POINT ( 'NONE',  ( 111.9288574835248511, -27.50774424443475397, 55.68991099019693536 ) ) ;
#87171 = VECTOR ( 'NONE', #10327, 1000.000000000000000 ) ;
#87172 = CARTESIAN_POINT ( 'NONE',  ( 194.0371591254573218, -24.42818131005407878, 237.4678068554150059 ) ) ;
#87173 = ORIENTED_EDGE ( 'NONE', *, *, #4579, .T. ) ;
#87174 = CYLINDRICAL_SURFACE ( 'NONE', #3627, 4.750000000000004441 ) ;
#87175 = CARTESIAN_POINT ( 'NONE',  ( 3.110602869834275287E-15, 198.8420489685532004, 25.39999999999999858 ) ) ;
#87176 = EDGE_CURVE ( 'NONE', #10820, #79159, #6858, .T. ) ;
#87177 = ORIENTED_EDGE ( 'NONE', *, *, #80033, .F. ) ;
#87178 = CARTESIAN_POINT ( 'NONE',  ( 163.0664832912739826, 0.2215528400590083269, 330.1506252759110680 ) ) ;
#87179 = DIRECTION ( 'NONE',  ( 0.9347835805883506488, 0.000000000000000000, 0.3552177606235679130 ) ) ;
#87180 = CARTESIAN_POINT ( 'NONE',  ( 96.79764630557882299, -40.75620882907056597, 246.6118157521009664 ) ) ;
#87181 = CYLINDRICAL_SURFACE ( 'NONE', #44330, 0.4999999999999982236 ) ;
#87182 = EDGE_CURVE ( 'NONE', #57450, #11953, #48, .T. ) ;
#87183 = FACE_OUTER_BOUND ( 'NONE', #44210, .T. ) ;
#87184 = CARTESIAN_POINT ( 'NONE',  ( 182.5667039024476139, -32.29483332967956954, 313.9678068554149490 ) ) ;
#87185 = AXIS2_PLACEMENT_3D ( 'NONE', #47808, #6490, #82371 ) ;
#87186 = CARTESIAN_POINT ( 'NONE',  ( 110.1391594044062003, -28.21056625751448976, 249.2114674471249600 ) ) ;
#87188 = CARTESIAN_POINT ( 'NONE',  ( 97.56228874418796693, -32.49873190831186776, 96.99276813305395706 ) ) ;
#87187 = DIRECTION ( 'NONE',  ( -0.9242245927363026414, -0.3818493186865932754, 0.000000000000000000 ) ) ;
#87189 = CARTESIAN_POINT ( 'NONE',  ( 121.7685547874556420, 74.27669327741411109, 47.08841425960243754 ) ) ;
#87190 = CARTESIAN_POINT ( 'NONE',  ( 109.2104764766756517, -26.48201038666214657, 139.9127681330539872 ) ) ;
#87191 = ORIENTED_EDGE ( 'NONE', *, *, #11468, .T. ) ;
#87192 = CARTESIAN_POINT ( 'NONE',  ( 132.8222787434353620, -21.18254450372675279, 7.982620440117798921 ) ) ;
#87193 = ORIENTED_EDGE ( 'NONE', *, *, #83743, .F. ) ;
#87194 = CARTESIAN_POINT ( 'NONE',  ( 41.56670390244718050, -42.82844715994109208, 180.4678068554150911 ) ) ;
#87195 = VECTOR ( 'NONE', #19179, 1000.000000000000000 ) ;
#87196 = DIRECTION ( 'NONE',  ( 0.000000000000000000, 1.000000000000000000, 0.000000000000000000 ) ) ;
#87197 = DIRECTION ( 'NONE',  ( 0.000000000000000000, -1.000000000000000000, 0.000000000000000000 ) ) ;
#87198 = EDGE_LOOP ( 'NONE', ( #87665, #80522, #2065, #69394 ) ) ;
#87199 = DIRECTION ( 'NONE',  ( 0.000000000000000000, 1.000000000000000000, 0.000000000000000000 ) ) ;
#87201 = ORIENTED_EDGE ( 'NONE', *, *, #56377, .T. ) ;
#87200 = CARTESIAN_POINT ( 'NONE',  ( 96.59500279541983048, -37.56604165528066375, 101.3899109901969524 ) ) ;
#87202 = CARTESIAN_POINT ( 'NONE',  ( 110.7536356736639078, -102.7271463785351528, 2.217806855417947531 ) ) ;
#87203 = DIRECTION ( 'NONE',  ( -4.237773401492740281E-14, 1.000000000000000000, 0.000000000000000000 ) ) ;
#87204 = AXIS2_PLACEMENT_3D ( 'NONE', #45929, #66390, #24622 ) ;
#87205 = DIRECTION ( 'NONE',  ( 2.056463827196271584E-15, -0.8571673007021100021, 0.5150380749100580413 ) ) ;
#87206 = ORIENTED_EDGE ( 'NONE', *, *, #87356, .T. ) ;
#87207 = VECTOR ( 'NONE', #36448, 1000.000000000000000 ) ;
#87208 = EDGE_CURVE ( 'NONE', #62756, #57314, #34103, .T. ) ;
#87209 = CARTESIAN_POINT ( 'NONE',  ( 97.55101884832849635, -31.05922868340991627, 130.9108633711489915 ) ) ;
#87210 = PRODUCT_CONTEXT ( 'NONE', #21423, 'mechanical' ) ;
#87211 = DIRECTION ( 'NONE',  ( -1.000000000000000000, 0.000000000000000000, 0.000000000000000000 ) ) ;
#87212 = PLANE ( 'NONE',  #61576 ) ;
#87213 = VERTEX_POINT ( 'NONE', #48611 ) ;
#87214 = EDGE_LOOP ( 'NONE', ( #27805, #29359, #6580, #50168 ) ) ;
#87215 = DIRECTION ( 'NONE',  ( -3.100000000000000258E-29, 3.100000000000000044E-14, 1.000000000000000000 ) ) ;
#87216 = CARTESIAN_POINT ( 'NONE',  ( 116.3212776292296127, -32.94146857471318413, 287.6356252759109680 ) ) ;
#87217 = DIRECTION ( 'NONE',  ( -4.237773401492740281E-14, 1.000000000000000000, 0.000000000000000000 ) ) ;
#87218 = CIRCLE ( 'NONE', #59627, 8.999999999999994671 ) ;
#87220 = CARTESIAN_POINT ( 'NONE',  ( 226.4410000000000025, 65.43750000000000000, 10.66800000000000104 ) ) ;
#87219 = CARTESIAN_POINT ( 'NONE',  ( 72.06648329127399677, -9.729447159941065237, -4.824374724089063982 ) ) ;
#87221 = CARTESIAN_POINT ( 'NONE',  ( 100.9544813764768634, -28.70716881530696796, 180.5939773098653234 ) ) ;
#87222 = VECTOR ( 'NONE', #40263, 1000.000000000000000 ) ;
#87223 = ORIENTED_EDGE ( 'NONE', *, *, #80199, .T. ) ;
#87224 = CARTESIAN_POINT ( 'NONE',  ( 99.04406200859183684, -42.84125783440281054, 32.84395862863929239 ) ) ;
#87225 = CARTESIAN_POINT ( 'NONE',  ( 104.0204373342842814, -47.42213563049708824, 213.3556252759109668 ) ) ;
#87226 = ADVANCED_FACE ( 'NONE', ( #76351 ), #41805, .F. ) ;
#87227 = VECTOR ( 'NONE', #83177, 1000.000000000000114 ) ;
#87229 = ORIENTED_EDGE ( 'NONE', *, *, #86959, .T. ) ;
#87228 = CARTESIAN_POINT ( 'NONE',  ( 107.9678037105606307, -121.2545485715093463, -19.18411693322849487 ) ) ;
#87230 = CARTESIAN_POINT ( 'NONE',  ( 115.0479362680065663, -42.38275094372907859, 49.33562527591095659 ) ) ;
#87231 = ADVANCED_FACE ( 'NONE', ( #55874 ), #83625, .F. ) ;
#87232 = CARTESIAN_POINT ( 'NONE',  ( 98.15100249062076898, -41.26166231382807581, 51.70074165506993324 ) ) ;
#87233 = ADVANCED_FACE ( 'NONE', ( #47279 ), #26412, .T. ) ;
#87234 = DIRECTION ( 'NONE',  ( 1.000000000000000000, 1.000000000000000078E-15, 1.000000000000000078E-15 ) ) ;
#87235 = AXIS2_PLACEMENT_3D ( 'NONE', #56571, #28421, #21630 ) ;
#87236 = CARTESIAN_POINT ( 'NONE',  ( 6.802569982901797644E-16, 69.84999999999999432, 118.5560000000000116 ) ) ;
#87237 = ORIENTED_EDGE ( 'NONE', *, *, #30816, .T. ) ;
#87238 = DIRECTION ( 'NONE',  ( 0.000000000000000000, 1.000000000000000000, 0.000000000000000000 ) ) ;
#87239 = ADVANCED_FACE ( 'NONE', ( #33671 ), #23214, .T. ) ;
#87240 = ORIENTED_EDGE ( 'NONE', *, *, #54779, .F. ) ;
#87241 = EDGE_LOOP ( 'NONE', ( #70236, #38449, #55231, #45990 ) ) ;
#87242 = CARTESIAN_POINT ( 'NONE',  ( 115.4123442176498173, -41.04489973583525142, 239.8663452106589773 ) ) ;
#87243 = CARTESIAN_POINT ( 'NONE',  ( 180.1667039024460166, -26.71338133339240528, 342.9256252759119548 ) ) ;
#87244 = FACE_OUTER_BOUND ( 'NONE', #7936, .T. ) ;
#87245 = PLANE ( 'NONE',  #53288 ) ;
#87246 = EDGE_CURVE ( 'NONE', #64215, #7655, #70441, .T. ) ;
#87247 = CARTESIAN_POINT ( 'NONE',  ( 82.62351725430391980, -37.74149216370238946, 2.839569540204898157 ) ) ;
#87249 = ORIENTED_EDGE ( 'NONE', *, *, #82217, .T. ) ;
#87248 = CIRCLE ( 'NONE', #48063, 0.5000000000000004441 ) ;
#87250 = DIRECTION ( 'NONE',  ( -0.000000000000000000, -0.000000000000000000, -1.000000000000000000 ) ) ;
#87251 = FACE_OUTER_BOUND ( 'NONE', #83828, .T. ) ;
#87252 = EDGE_CURVE ( 'NONE', #89686, #68890, #30261, .T. ) ;
#87253 = VERTEX_POINT ( 'NONE', #2301 ) ;
#87254 = CARTESIAN_POINT ( 'NONE',  ( 102.3890460933095170, -47.58756240099349100, 287.2527681330536780 ) ) ;
#87255 = DIRECTION ( 'NONE',  ( 0.000000000000000000, 1.000000000000000000, 0.000000000000000000 ) ) ;
#87256 = EDGE_LOOP ( 'NONE', ( #15820, #79984, #7312, #7303 ) ) ;
#87257 =( NAMED_UNIT ( * ) PLANE_ANGLE_UNIT ( ) SI_UNIT ( $, .RADIAN. ) );
#87258 = FACE_OUTER_BOUND ( 'NONE', #87511, .T. ) ;
#87259 = FACE_OUTER_BOUND ( 'NONE', #16060, .T. ) ;
#87260 = CARTESIAN_POINT ( 'NONE',  ( 72.96458098368701428, 117.4749999999999943, -65.82083098368670449 ) ) ;
#87261 = AXIS2_PLACEMENT_3D ( 'NONE', #69547, #26853, #68651 ) ;
#87262 = CARTESIAN_POINT ( 'NONE',  ( 117.2699639542694001, -41.09825485984158178, 209.5165776568640013 ) ) ;
#87263 = CARTESIAN_POINT ( 'NONE',  ( 248.6659999999999968, 52.73749999999999716, 10.66800000000000104 ) ) ;
#87264 = ORIENTED_EDGE ( 'NONE', *, *, #77414, .T. ) ;
#87265 = AXIS2_PLACEMENT_3D ( 'NONE', #22718, #50851, #50394 ) ;
#87266 = CARTESIAN_POINT ( 'NONE',  ( 113.5330014162060195, -28.49676089798827405, 75.54705384733995288 ) ) ;
#87267 = LINE ( 'NONE', #81801, #4785 ) ;
#87268 = ORIENTED_EDGE ( 'NONE', *, *, #261, .F. ) ;
#87269 = ORIENTED_EDGE ( 'NONE', *, *, #4254, .F. ) ;
#87270 = ORIENTED_EDGE ( 'NONE', *, *, #88763, .F. ) ;
#87271 = CARTESIAN_POINT ( 'NONE',  ( 81.14852608520887145, -16.20116861175210587, 1.807989644435677778 ) ) ;
#87272 = DIRECTION ( 'NONE',  ( 0.000000000000000000, -1.000000000000000000, 0.000000000000000000 ) ) ;
#87273 = FACE_OUTER_BOUND ( 'NONE', #79815, .T. ) ;
#87274 = CARTESIAN_POINT ( 'NONE',  ( 115.0083044075158654, -38.73198694842640322, 121.4480903695919807 ) ) ;
#87275 = CARTESIAN_POINT ( 'NONE',  ( 115.4773891788847067, -29.52237647247901009, 225.4022919425769658 ) ) ;
#87276 = DIRECTION ( 'NONE',  ( 0.000000000000000000, 0.000000000000000000, 1.000000000000000000 ) ) ;
#87277 = ORIENTED_EDGE ( 'NONE', *, *, #29104, .T. ) ;
#87278 = DIRECTION ( 'NONE',  ( 1.000000000000000000, 4.299999999999999979E-14, 1.000000000000000078E-15 ) ) ;
#87279 = ADVANCED_FACE ( 'NONE', ( #49521 ), #63619, .F. ) ;
#87280 = ORIENTED_EDGE ( 'NONE', *, *, #22128, .F. ) ;
#87281 = ORIENTED_EDGE ( 'NONE', *, *, #49035, .T. ) ;
#87282 = DIRECTION ( 'NONE',  ( 1.000000000000000078E-15, 0.000000000000000000, -1.000000000000000000 ) ) ;
#87283 = ORIENTED_EDGE ( 'NONE', *, *, #18113, .F. ) ;
#87284 = ORIENTED_EDGE ( 'NONE', *, *, #67745, .T. ) ;
#87285 = CARTESIAN_POINT ( 'NONE',  ( 116.9610908827738882, -34.94244874878751972, 9.968958609244259250 ) ) ;
#87286 = DIRECTION ( 'NONE',  ( 0.000000000000000000, -1.000000000000000000, 0.000000000000000000 ) ) ;
#87287 = B_SPLINE_CURVE_WITH_KNOTS ( 'NONE', 3,
 ( #59482, #65425, #3208, #24981, #52648, #78636, #16392, #44065, #71800, #2766, #46743, #26756, #54438, #80858, #25421, #19503, #82654, #54889, #33134, #25874, #4983, #47186, #20412, #48083, #60829, #19059, #53546, #40830, #47639, #13585, #88562, #13150, #74925, #74475, #41272, #19960, #75816, #81315, #74024, #82204, #5439, #69002, #53090, #26320, #67660, #68557, #53994, #18609, #39938 ),
 .UNSPECIFIED., .F., .F.,
 ( 4, 2, 2, 2, 2, 2, 2, 2, 2, 2, 2, 2, 2, 2, 2, 1, 2, 2, 2, 2, 2, 2, 2, 2, 4 ),
 ( 0.01986933033599077095, 0.02111088875730815148, 0.02235244717862553548, 0.02483556402126030002, 0.02607712244257766321, 0.02731868086389502639, 0.02980179770652973542, 0.03228491454916444792, 0.03352647297048180070, 0.03476803139179915347, 0.03725114823443387985, 0.03849270665575126732, 0.03973426507706865479, 0.04221738191970346443, 0.04345894034102086578, 0.04470049876233826713, 0.04594205718365568236, 0.04718361560497308371, 0.04966673244760788641, 0.05090829086892528776, 0.05214984929024267524, 0.05463296613287745018, 0.05587452455419482378, 0.05711608297551219737, 0.05959919981814691681 ),
 .UNSPECIFIED. ) ;
#87288 = EDGE_CURVE ( 'NONE', #52932, #82905, #49970, .T. ) ;
#87289 = CARTESIAN_POINT ( 'NONE',  ( 98.34938918086412230, -31.65742736436922300, 25.90653489524752118 ) ) ;
#87290 = CARTESIAN_POINT ( 'NONE',  ( 105.9636396274569137, -27.08297541922676643, 159.5895626852199598 ) ) ;
#87291 = AXIS2_PLACEMENT_3D ( 'NONE', #15812, #9435, #16259 ) ;
#87292 = CARTESIAN_POINT ( 'NONE',  ( 110.2977701465690643, -46.68767980799292872, 12.82705384733995402 ) ) ;
#87293 = EDGE_LOOP ( 'NONE', ( #44063, #23951, #32945, #64209, #35266, #44473 ) ) ;
#87294 = CARTESIAN_POINT ( 'NONE',  ( -74.15067561874160162, 120.6499999999999915, -68.53801554307528932 ) ) ;
#87295 = VECTOR ( 'NONE', #88766, 1000.000000000000000 ) ;
#87296 = ORIENTED_EDGE ( 'NONE', *, *, #82005, .F. ) ;
#87297 = CARTESIAN_POINT ( 'NONE',  ( 62.03715912545824551, -47.82818131006021645, 300.4678068554150627 ) ) ;
#87298 = ORIENTED_EDGE ( 'NONE', *, *, #48678, .T. ) ;
#87299 = CARTESIAN_POINT ( 'NONE',  ( 97.20990489797566170, -38.46844655478637520, 167.4655669962249078 ) ) ;
#87300 = DIRECTION ( 'NONE',  ( 0.000000000000000000, -1.000000000000000000, 0.000000000000000000 ) ) ;
#87301 = CARTESIAN_POINT ( 'NONE',  ( 183.5150000000000148, 53.21300000000000097, 41.63456447661469895 ) ) ;
#87302 = PLANE ( 'NONE',  #64056 ) ;
#87303 = VERTEX_POINT ( 'NONE', #29106 ) ;
#87304 = EDGE_CURVE ( 'NONE', #27286, #63455, #43257, .T. ) ;
#87305 = CARTESIAN_POINT ( 'NONE',  ( 105.1595199372206793, -47.03071207059073799, 12.42991099019596923 ) ) ;
#87306 = CARTESIAN_POINT ( 'NONE',  ( 112.9878179797879909, -28.09632633057573159, 40.59848241876795782 ) ) ;
#87307 = SURFACE_STYLE_FILL_AREA ( #65514 ) ;
#87309 = CARTESIAN_POINT ( 'NONE',  ( -194.1576000000000022, 101.5999999999999943, 146.9389999999999930 ) ) ;
#87308 = CARTESIAN_POINT ( 'NONE',  ( 72.96458098368701428, 117.4749999999999943, -72.96458098368670164 ) ) ;
#87310 = DIRECTION ( 'NONE',  ( -0.7071067811865483499, -0.7071067811865466846, -7.071067811865491110E-16 ) ) ;
#87311 = DIRECTION ( 'NONE',  ( 0.000000000000000000, 0.000000000000000000, 1.000000000000000000 ) ) ;
#87312 = CARTESIAN_POINT ( 'NONE',  ( 28.57499999999999929, 91.71543552338529537, 302.8950000000000387 ) ) ;
#87313 = AXIS2_PLACEMENT_3D ( 'NONE', #38374, #44289, #2980 ) ;
#87314 = LINE ( 'NONE', #80063, #38773 ) ;
#87315 = PLANE ( 'NONE',  #83564 ) ;
#87316 = EDGE_CURVE ( 'NONE', #83591, #36325, #78170, .T. ) ;
#87317 = CARTESIAN_POINT ( 'NONE',  ( 99.26081945853924537, -43.75962541195023903, 56.90991099019593236 ) ) ;
#87318 = CARTESIAN_POINT ( 'NONE',  ( 97.09625178000921153, -41.50107833764869980, 212.6937205140059461 ) ) ;
#87319 = CARTESIAN_POINT ( 'NONE',  ( 118.0115981831179113, -38.42934884787886318, 64.69181575210097890 ) ) ;
#87320 = B_SPLINE_CURVE_WITH_KNOTS ( 'NONE', 3,
 ( #2016, #43330, #8844, #36543, #83346, #76522, #29719, #21118, #48791, #69717, #86921, #72836, #24244, #24684, #31936, #2467, #10165, #44667, #17865, #65575, #44212, #45993, #30610, #17429, #30162, #38749, #59629, #2910, #23808, #9721, #18309, #79225, #73725, #52351, #87365, #80553 ),
 .UNSPECIFIED., .F., .F.,
 ( 4, 2, 2, 2, 2, 1, 2, 2, 2, 2, 2, 2, 2, 2, 2, 1, 2, 2, 4 ),
 ( 0.000000000000000000, 0.06249999999997138400, 0.09374999999994827748, 0.1249999999999251710, 0.1874999999998892275, 0.2187499999998792077, 0.2343749999998742950, 0.2499999999998693823, 0.3749999999999009681, 0.4374999999999187872, 0.4687499999999116262, 0.4999999999999044098, 0.6249999999999289457, 0.6874999999999485967, 0.7499999999999681366, 0.8124999999999876765, 0.8437499999999974465, 0.8750000000000072164, 1.000000000000000000 ),
 .UNSPECIFIED. ) ;
#87321 = AXIS2_PLACEMENT_3D ( 'NONE', #81305, #53077, #80848 ) ;
#87323 = DIRECTION ( 'NONE',  ( 0.000000000000000000, -1.000000000000000000, 0.000000000000000000 ) ) ;
#87322 = CARTESIAN_POINT ( 'NONE',  ( 31.75000000000000000, 66.67499999999999716, 295.2750000000000341 ) ) ;
#87324 = DIRECTION ( 'NONE',  ( 0.000000000000000000, 0.000000000000000000, -1.000000000000000000 ) ) ;
#87325 = AXIS2_PLACEMENT_3D ( 'NONE', #42461, #35661, #22063 ) ;
#87326 = EDGE_CURVE ( 'NONE', #42151, #75837, #18635, .T. ) ;
#87327 = ORIENTED_EDGE ( 'NONE', *, *, #28543, .T. ) ;
#87328 = DIRECTION ( 'NONE',  ( 0.000000000000000000, 0.000000000000000000, -1.000000000000000000 ) ) ;
#87329 = ORIENTED_EDGE ( 'NONE', *, *, #12913, .T. ) ;
#87330 = CARTESIAN_POINT ( 'NONE',  ( 109.5220866130624700, -46.80460460589462457, 83.75467289495797729 ) ) ;
#87332 = ORIENTED_EDGE ( 'NONE', *, *, #70814, .F. ) ;
#87331 = PLANE ( 'NONE',  #44239 ) ;
#87333 = PLANE ( 'NONE',  #71748 ) ;
#87334 = CARTESIAN_POINT ( 'NONE',  ( 100.6697571656888499, -44.93374849542860971, 228.0499109901969348 ) ) ;
#87335 = DIRECTION ( 'NONE',  ( 1.000000000000000000, 0.000000000000000000, 0.000000000000000000 ) ) ;
#87336 = PRODUCT_DEFINITION_SHAPE ( 'NONE', 'NONE',  #89939 ) ;
#87337 = CARTESIAN_POINT ( 'NONE',  ( 115.9432244607059204, -41.40609373283200512, 148.4407487842870808 ) ) ;
#87338 = DIRECTION ( 'NONE',  ( 0.7071067811868666508, 0.7071067811862283836, 7.071067811868659373E-16 ) ) ;
#87339 = EDGE_CURVE ( 'NONE', #7800, #42450, #27324, .T. ) ;
#87340 = DIRECTION ( 'NONE',  ( 0.000000000000000000, 0.000000000000000000, -1.000000000000000000 ) ) ;
#87341 = CIRCLE ( 'NONE', #19192, 4.749999999999976907 ) ;
#87342 = CARTESIAN_POINT ( 'NONE',  ( 132.4277392773765030, -38.94013506380868961, 2.060080721660203729 ) ) ;
#87343 = DIRECTION ( 'NONE',  ( 0.000000000000000000, -1.000000000000000000, 0.000000000000000000 ) ) ;
#87344 = CARTESIAN_POINT ( 'NONE',  ( 116.6595528204499601, -34.65899032542078118, 183.9956252759109532 ) ) ;
#87345 = ORIENTED_EDGE ( 'NONE', *, *, #32562, .T. ) ;
#87346 = ORIENTED_EDGE ( 'NONE', *, *, #57682, .T. ) ;
#87347 = CARTESIAN_POINT ( 'NONE',  ( 112.4011824308993397, -28.99526907646757934, 86.03967854399191140 ) ) ;
#87348 = VECTOR ( 'NONE', #5850, 1000.000000000000000 ) ;
#87349 = DIRECTION ( 'NONE',  ( -3.100000000000000258E-29, 3.100000000000000044E-14, 1.000000000000000000 ) ) ;
#87351 = CARTESIAN_POINT ( 'NONE',  ( 76.20505178924339873, 120.6499999999999915, 76.20505178924419454 ) ) ;
#87350 = CARTESIAN_POINT ( 'NONE',  ( 99.87094702832897042, -29.26198151734326203, 261.6746728949581779 ) ) ;
#87352 = DIRECTION ( 'NONE',  ( 0.02150753337723862457, 0.0009076677972192722819, 0.9997682742251809973 ) ) ;
#87353 = LINE ( 'NONE', #25559, #37988 ) ;
#87354 = AXIS2_PLACEMENT_3D ( 'NONE', #45595, #30225, #10219 ) ;
#87355 = CARTESIAN_POINT ( 'NONE',  ( 117.8827794761418204, 80.88465057165900873, -12.61751953376081303 ) ) ;
#87356 = EDGE_CURVE ( 'NONE', #17228, #2012, #64078, .T. ) ;
#87357 = DIRECTION ( 'NONE',  ( 0.000000000000000000, -1.000000000000000000, 0.000000000000000000 ) ) ;
#87358 = CARTESIAN_POINT ( 'NONE',  ( 7.937500000000000000, 120.6499999999999915, -103.1875000000000000 ) ) ;
#87359 = FACE_OUTER_BOUND ( 'NONE', #69398, .T. ) ;
#87360 = EDGE_CURVE ( 'NONE', #15908, #50719, #9555, .T. ) ;
#87361 = CARTESIAN_POINT ( 'NONE',  ( 102.8528367378537496, -46.24122135049443472, 177.2441967044819648 ) ) ;
#87362 = ORIENTED_EDGE ( 'NONE', *, *, #85194, .T. ) ;
#87363 = EDGE_LOOP ( 'NONE', ( #20667, #8252, #10135, #2464 ) ) ;
#87364 = CARTESIAN_POINT ( 'NONE',  ( 68.85834700699179223, -69.56425716864252706, 247.5000682988239760 ) ) ;
#87365 = CARTESIAN_POINT ( 'NONE',  ( 147.0652011257825222, -67.87844715994089029, 245.6323489049700868 ) ) ;
#87366 = DIRECTION ( 'NONE',  ( 0.000000000000000000, 0.000000000000000000, 1.000000000000000000 ) ) ;
#87367 = CARTESIAN_POINT ( 'NONE',  ( 107.0664832912748068, -36.72944715993923381, 14.92562527591097066 ) ) ;
#87368 = EDGE_LOOP ( 'NONE', ( #50964, #53616 ) ) ;
#87369 = CARTESIAN_POINT ( 'NONE',  ( -6.299534494109307659, 93.46997398832955639, 118.1887946445226589 ) ) ;
#87370 =( BOUNDED_CURVE ( )  B_SPLINE_CURVE ( 3, ( #13899, #67508, #19372, #67965 ),
 .UNSPECIFIED., .F., .T. ) 
 B_SPLINE_CURVE_WITH_KNOTS ( ( 4, 4 ),
 ( 3.141592653589793116, 3.611750613512999308 ),
 .UNSPECIFIED. ) 
 CURVE ( )  GEOMETRIC_REPRESENTATION_ITEM ( )  RATIONAL_B_SPLINE_CURVE ( ( 1.000000000000000000, 0.9816639655796099984, 0.9816639655796099984, 1.000000000000000000 ) ) 
 REPRESENTATION_ITEM ( '' )  );
#87371 = CARTESIAN_POINT ( 'NONE',  ( 115.0397999656063917, -29.07403674218411638, 189.4232443235299570 ) ) ;
#87372 = DIRECTION ( 'NONE',  ( 0.02992792722492364568, 0.000000000000000000, 0.9995520592605569021 ) ) ;
#87373 = EDGE_LOOP ( 'NONE', ( #18551, #67611, #56335, #21882, #84872, #81354 ) ) ;
#87375 = ORIENTED_EDGE ( 'NONE', *, *, #86746, .F. ) ;
#87374 = ORIENTED_EDGE ( 'NONE', *, *, #33713, .F. ) ;
#87376 = VECTOR ( 'NONE', #89455, 1000.000000000000000 ) ;
#87377 = CARTESIAN_POINT ( 'NONE',  ( 105.3030533616251319, -46.61669885714199779, 63.43686953697783082 ) ) ;
#87378 = CARTESIAN_POINT ( 'NONE',  ( 72.96458098368650269, 127.0000000000000000, 65.82083098368730134 ) ) ;
#87379 = DIRECTION ( 'NONE',  ( 4.649954031768962643E-17, 0.8660254037844382635, 0.5000000000000008882 ) ) ;
#87380 = CARTESIAN_POINT ( 'NONE',  ( 113.1369140564456615, -42.18651563507969371, 36.06237608387696980 ) ) ;
#87381 = DIRECTION ( 'NONE',  ( 1.000000000000000078E-15, -1.000000000000000083E-30, -1.000000000000000000 ) ) ;
#87382 = ORIENTED_EDGE ( 'NONE', *, *, #42373, .F. ) ;
#87383 = CARTESIAN_POINT ( 'NONE',  ( 90.44969454456405344, -20.11243780205715481, 218.8274735512160589 ) ) ;
#87384 = CARTESIAN_POINT ( 'NONE',  ( 82.54568444100624447, -17.53793914063253112, 7.103892432653575284 ) ) ;
#87385 = ORIENTED_EDGE ( 'NONE', *, *, #24481, .F. ) ;
#87386 = VERTEX_POINT ( 'NONE', #30449 ) ;
#87387 = VECTOR ( 'NONE', #31160, 1000.000000000000000 ) ;
#87388 = DIRECTION ( 'NONE',  ( 0.000000000000000000, -1.000000000000000000, 0.000000000000000000 ) ) ;
#87389 = ORIENTED_EDGE ( 'NONE', *, *, #87471, .F. ) ;
#87390 = ORIENTED_EDGE ( 'NONE', *, *, #7431, .F. ) ;
#87391 = DIRECTION ( 'NONE',  ( 0.000000000000000000, -1.000000000000000000, -3.491483361109380094E-15 ) ) ;
#87392 = CARTESIAN_POINT ( 'NONE',  ( 115.5775591941339542, -37.73626844564258676, 53.15527697093397563 ) ) ;
#87393 = CARTESIAN_POINT ( 'NONE',  ( 113.7648918053778715, -44.74678383396227588, 193.1299109901969757 ) ) ;
#87394 = CARTESIAN_POINT ( 'NONE',  ( 112.4747680694540861, -26.21285726233885427, 169.6984824187679521 ) ) ;
#87396 = CARTESIAN_POINT ( 'NONE',  ( 112.6636929512762180, -45.52454417301038347, 259.0270538473393458 ) ) ;
#87395 = DIRECTION ( 'NONE',  ( -1.000000000000000078E-15, 1.000000000000000000, 0.000000000000000000 ) ) ;
#87397 = CYLINDRICAL_SURFACE ( 'NONE', #15867, 1.499999999999987788 ) ;
#87398 = CARTESIAN_POINT ( 'NONE',  ( 107.0667039024470313, -104.2784471599420755, -19.78219314458201694 ) ) ;
#87399 = EDGE_LOOP ( 'NONE', ( #89163, #50886, #55431, #13828, #85339, #24394, #32837, #84334, #88545, #43883 ) ) ;
#87400 = AXIS2_PLACEMENT_3D ( 'NONE', #42433, #36088, #13410 ) ;
#87401 = ORIENTED_EDGE ( 'NONE', *, *, #30535, .T. ) ;
#87402 = DIRECTION ( 'NONE',  ( 0.000000000000000000, -1.000000000000000000, 0.000000000000000000 ) ) ;
#87403 = CARTESIAN_POINT ( 'NONE',  ( 96.73248008985177648, -40.78176272772311250, 246.6118157521009664 ) ) ;
#87404 = ORIENTED_EDGE ( 'NONE', *, *, #61530, .T. ) ;
#87405 = EDGE_CURVE ( 'NONE', #54125, #13421, #17165, .T. ) ;
#87406 = CARTESIAN_POINT ( 'NONE',  ( 107.2431713256043224, -47.18863871633809026, 212.5899109901969837 ) ) ;
#87407 = CARTESIAN_POINT ( 'NONE',  ( 100.9540432848167200, -28.70751825032547799, 265.5939957159569076 ) ) ;
#87408 = CARTESIAN_POINT ( 'NONE',  ( -9.469228445121002480, 69.24107684194999024, 36.91068001385391995 ) ) ;
#87409 = DIRECTION ( 'NONE',  ( 1.000000000000000078E-15, -1.000000000000000083E-30, -1.000000000000000000 ) ) ;
#87410 = CARTESIAN_POINT ( 'NONE',  ( 143.5890317271348238, -139.7841266254118011, 247.2002237598829311 ) ) ;
#87411 = EDGE_CURVE ( 'NONE', #11589, #64922, #84980, .T. ) ;
#87414 = CARTESIAN_POINT ( 'NONE',  ( 116.1206117333611019, -31.56300607074032882, 285.2384824187680579 ) ) ;
#87413 = CARTESIAN_POINT ( 'NONE',  ( 107.0664832912750057, -36.72944715993903486, 9.125625275910969947 ) ) ;
#87412 = FACE_OUTER_BOUND ( 'NONE', #9699, .T. ) ;
#87415 = CARTESIAN_POINT ( 'NONE',  ( 163.0664832912739826, -0.2185775633789972805, 333.4006252759120343 ) ) ;
#87416 = CYLINDRICAL_SURFACE ( 'NONE', #20695, 6.571100913904384555 ) ;
#87417 = VECTOR ( 'NONE', #37822, 1000.000000000000000 ) ;
#87418 = CARTESIAN_POINT ( 'NONE',  ( 149.4512091874902922, -60.54365471797113685, 361.9756252759100335 ) ) ;
#87419 = EDGE_CURVE ( 'NONE', #42151, #45558, #43606, .T. ) ;
#87420 = DIRECTION ( 'NONE',  ( -4.496403249731880833E-15, 0.000000000000000000, -1.000000000000000000 ) ) ;
#87421 = FACE_BOUND ( 'NONE', #47728, .T. ) ;
#87422 = EDGE_CURVE ( 'NONE', #7174, #78413, #23012, .T. ) ;
#87423 = CARTESIAN_POINT ( 'NONE',  ( 177.0664832912730162, 12.92155284005730387, 358.9756252759109998 ) ) ;
#87425 = ORIENTED_EDGE ( 'NONE', *, *, #20202, .T. ) ;
#87424 = CARTESIAN_POINT ( 'NONE',  ( -12.70000000000000107, 82.54999999999999716, -117.8738102209307641 ) ) ;
#87426 = EDGE_CURVE ( 'NONE', #26963, #83074, #30004, .T. ) ;
#87427 = DIRECTION ( 'NONE',  ( 0.000000000000000000, 0.000000000000000000, -1.000000000000000000 ) ) ;
#87428 = CARTESIAN_POINT ( 'NONE',  ( 100.6239562591623695, -26.75308202300568539, 220.5327681330539633 ) ) ;
#87429 = CARTESIAN_POINT ( 'NONE',  ( 104.1078173601787995, -46.72588569351386667, 103.3470538473389411 ) ) ;
#87430 = CARTESIAN_POINT ( 'NONE',  ( 115.4227270478554317, -30.42340481720227885, 215.3413395616249773 ) ) ;
#87431 = CARTESIAN_POINT ( 'NONE',  ( 83.06670390244796920, -61.87844715994100397, 207.5838068554149913 ) ) ;
#87432 = LINE ( 'NONE', #39273, #70740 ) ;
#87434 = CARTESIAN_POINT ( 'NONE',  ( -92.32962665258560264, 82.54999999999999716, 74.36911441044701121 ) ) ;
#87433 = CARTESIAN_POINT ( 'NONE',  ( 97.81169536214920868, -40.51742132101362870, 146.6356105553879274 ) ) ;
#87435 = LINE ( 'NONE', #30680, #24931 ) ;
#87436 = EDGE_CURVE ( 'NONE', #76720, #87084, #68239, .T. ) ;
#87437 = CARTESIAN_POINT ( 'NONE',  ( 143.0664832912740110, -18.82844715994099971, 323.8756252759120002 ) ) ;
#87438 = EDGE_CURVE ( 'NONE', #9653, #75243, #45823, .T. ) ;
#87439 = EDGE_CURVE ( 'NONE', #47090, #52633, #31320, .T. ) ;
#87440 = ORIENTED_EDGE ( 'NONE', *, *, #89512, .T. ) ;
#87441 = ORIENTED_EDGE ( 'NONE', *, *, #64808, .F. ) ;
#87442 = CARTESIAN_POINT ( 'NONE',  ( 113.1794296094924874, -30.05060732774411036, 153.8971817328389875 ) ) ;
#87444 = ORIENTED_EDGE ( 'NONE', *, *, #22707, .T. ) ;
#87443 = DIRECTION ( 'NONE',  ( 0.000000000000000000, -1.000000000000000000, 0.000000000000000000 ) ) ;
#87445 = PLANE ( 'NONE',  #77972 ) ;
#87446 = CARTESIAN_POINT ( 'NONE',  ( 117.2167691715782070, -39.01263929987993606, 144.6499109901969859 ) ) ;
#87447 = EDGE_CURVE ( 'NONE', #13942, #87997, #17707, .T. ) ;
#87448 = CARTESIAN_POINT ( 'NONE',  ( 107.0664832912739968, -36.72944715994100306, 287.6356252759109680 ) ) ;
#87449 = EDGE_CURVE ( 'NONE', #47202, #35448, #79543, .T. ) ;
#87450 = CARTESIAN_POINT ( 'NONE',  ( 144.0667039024470739, -137.6784471599409017, 55.21780685541800437 ) ) ;
#87451 = CARTESIAN_POINT ( 'NONE',  ( -74.62312585591585901, 79.66685870724428753, 92.12448541806632818 ) ) ;
#87452 = DIRECTION ( 'NONE',  ( 0.000000000000000000, 0.000000000000000000, 1.000000000000000000 ) ) ;
#87453 = CARTESIAN_POINT ( 'NONE',  ( 106.8551140066829817, -47.84553036069068099, 77.56133956162591403 ) ) ;
#87454 = VERTEX_POINT ( 'NONE', #60358 ) ;
#87455 = ORIENTED_EDGE ( 'NONE', *, *, #85194, .F. ) ;
#87456 = VERTEX_POINT ( 'NONE', #73553 ) ;
#87457 = AXIS2_PLACEMENT_3D ( 'NONE', #10071, #57303, #30952 ) ;
#87458 = CARTESIAN_POINT ( 'NONE',  ( 86.06670390244796920, -58.35344715994099829, 310.9178068554150514 ) ) ;
#87460 = DIRECTION ( 'NONE',  ( -4.299999999999999979E-14, 1.000000000000000000, -4.400000000000000367E-29 ) ) ;
#87459 = CARTESIAN_POINT ( 'NONE',  ( 105.8036208730406003, -25.68330614324009886, 156.1670538473389627 ) ) ;
#87461 = CARTESIAN_POINT ( 'NONE',  ( 106.5462518941686909, -24.40236651281373526, 322.0356252759110021 ) ) ;
#87462 = CARTESIAN_POINT ( 'NONE',  ( 188.5667039024479834, -65.37844715994100397, 168.3428068554150059 ) ) ;
#87463 = LINE ( 'NONE', #53348, #45971 ) ;
#87464 = EDGE_CURVE ( 'NONE', #22883, #77441, #25859, .T. ) ;
#87465 = CARTESIAN_POINT ( 'NONE',  ( 87.20679695024468003, 94.30044237600044710, 80.31773325845628619 ) ) ;
#87466 = CYLINDRICAL_SURFACE ( 'NONE', #11028, 0.2500000000000002220 ) ;
#87467 = EDGE_CURVE ( 'NONE', #47446, #48239, #86792, .T. ) ;
#87468 = CARTESIAN_POINT ( 'NONE',  ( 95.37363933861277587, -34.96150835630652409, 71.20705384733993526 ) ) ;
#87469 = EDGE_LOOP ( 'NONE', ( #40722, #33992, #38754, #41108, #14789, #67955 ) ) ;
#87470 = ORIENTED_EDGE ( 'NONE', *, *, #5919, .F. ) ;
#87471 = EDGE_CURVE ( 'NONE', #79424, #71248, #66282, .T. ) ;
#87472 = DIRECTION ( 'NONE',  ( 1.000000000000000000, 1.132880637372608296E-15, 0.000000000000000000 ) ) ;
#87473 = DIRECTION ( 'NONE',  ( 0.2844709403917162205, 0.000000000000000000, 0.9586846635221889512 ) ) ;
#87474 = EDGE_CURVE ( 'NONE', #58142, #85724, #4523, .T. ) ;
#87475 = FACE_OUTER_BOUND ( 'NONE', #19071, .T. ) ;
#87476 = CARTESIAN_POINT ( 'NONE',  ( 100.0385306026334717, -40.93546354753772221, 159.5738046553059917 ) ) ;
#87477 = VECTOR ( 'NONE', #8096, 1000.000000000000000 ) ;
#87478 = AXIS2_PLACEMENT_3D ( 'NONE', #10529, #51839, #16908 ) ;
#87479 = CIRCLE ( 'NONE', #62639, 2.500000000000002220 ) ;
#87480 = CYLINDRICAL_SURFACE ( 'NONE', #82319, 3.000000000000002665 ) ;
#87481 = VERTEX_POINT ( 'NONE', #87641 ) ;
#87482 = ORIENTED_EDGE ( 'NONE', *, *, #70327, .F. ) ;
#87483 = CARTESIAN_POINT ( 'NONE',  ( -55.11501535285000131, 0.000000000000000000, 183.9403141659174992 ) ) ;
#87484 = EDGE_LOOP ( 'NONE', ( #39211, #67895, #85806, #35532 ) ) ;
#87485 = ORIENTED_EDGE ( 'NONE', *, *, #61859, .F. ) ;
#87486 = DIRECTION ( 'NONE',  ( -0.000000000000000000, 1.000000000000000000, -0.000000000000000000 ) ) ;
#87487 = CARTESIAN_POINT ( 'NONE',  ( 98.59150690531237160, -40.78546747480537249, 213.1253928297069535 ) ) ;
#87488 = DIRECTION ( 'NONE',  ( 4.299999999999999979E-14, -1.000000000000000000, 0.000000000000000000 ) ) ;
#87489 = DIRECTION ( 'NONE',  ( 0.000000000000000000, 0.000000000000000000, -1.000000000000000000 ) ) ;
#87490 = CARTESIAN_POINT ( 'NONE',  ( 70.56670390244700286, -67.87844715994098976, 222.2178068554179902 ) ) ;
#87491 = VERTEX_POINT ( 'NONE', #39482 ) ;
#87492 = ORIENTED_EDGE ( 'NONE', *, *, #34080, .F. ) ;
#87493 = CIRCLE ( 'NONE', #55557, 2.517499999999998739 ) ;
#87494 = ORIENTED_EDGE ( 'NONE', *, *, #87865, .T. ) ;
#87495 = ORIENTED_EDGE ( 'NONE', *, *, #24426, .F. ) ;
#87496 = CARTESIAN_POINT ( 'NONE',  ( 115.4521610479674081, -32.75750308622325946, 211.9966617981629611 ) ) ;
#87498 = CARTESIAN_POINT ( 'NONE',  ( 101.6994268497411724, -27.72483345503921370, 85.50419670448295051 ) ) ;
#87497 = AXIS2_PLACEMENT_3D ( 'NONE', #43752, #51015, #79199 ) ;
#87499 = CARTESIAN_POINT ( 'NONE',  ( 104.7644060343265409, -46.87484541886973943, 72.39848241876795498 ) ) ;
#87500 = CARTESIAN_POINT ( 'NONE',  ( 182.5667039024459939, -19.82844715994031048, 342.9256252759119548 ) ) ;
#87501 = DIRECTION ( 'NONE',  ( 0.8660254037844382635, 0.5000000000000008882, -1.550000000000000022E-14 ) ) ;
#87502 = DIRECTION ( 'NONE',  ( -3.100000000000000258E-29, 3.100000000000000044E-14, 1.000000000000000000 ) ) ;
#87503 = CARTESIAN_POINT ( 'NONE',  ( 97.95649862111255857, -30.46988169760521359, 161.8594347997199918 ) ) ;
#87504 = DIRECTION ( 'NONE',  ( 0.000000000000000000, 0.000000000000000000, 1.000000000000000000 ) ) ;
#87505 = ORIENTED_EDGE ( 'NONE', *, *, #384, .T. ) ;
#87506 = DIRECTION ( 'NONE',  ( 1.000000000000000000, 0.000000000000000000, 1.531877379624855416E-14 ) ) ;
#87507 = ORIENTED_EDGE ( 'NONE', *, *, #44128, .T. ) ;
#87508 = ORIENTED_EDGE ( 'NONE', *, *, #70053, .F. ) ;
#87509 = PLANE ( 'NONE',  #44773 ) ;
#87510 = CARTESIAN_POINT ( 'NONE',  ( -100.8961411191535973, 120.6499999999999915, 3.968749999998880451 ) ) ;
#87511 = EDGE_LOOP ( 'NONE', ( #10686, #12586, #53780, #4696, #23611, #2402, #71918, #85778 ) ) ;
#87512 = AXIS2_PLACEMENT_3D ( 'NONE', #42850, #36061, #7011 ) ;
#87513 = DIRECTION ( 'NONE',  ( 1.000000000000000078E-15, 1.000000000000000083E-30, -1.000000000000000000 ) ) ;
#87514 = ORIENTED_EDGE ( 'NONE', *, *, #13813, .F. ) ;
#87515 = CARTESIAN_POINT ( 'NONE',  ( 177.1649999999999920, 5.112500000000000711, -7.937500000000000000 ) ) ;
#87516 = CARTESIAN_POINT ( 'NONE',  ( 96.79149040999978126, -38.49340627261485537, 91.46133956162493917 ) ) ;
#87517 = CARTESIAN_POINT ( 'NONE',  ( 69.68306499799194853, -72.55732494038082336, 540.9756252759101471 ) ) ;
#87518 = ADVANCED_FACE ( 'NONE', ( #30889 ), #18140, .F. ) ;
#87519 = CARTESIAN_POINT ( 'NONE',  ( 168.3595971214164422, -48.62134037890297833, 180.4678068554150059 ) ) ;
#87520 = DIRECTION ( 'NONE',  ( -9.073094938289460781E-13, -1.000000000000000000, 0.000000000000000000 ) ) ;
#87521 = EDGE_CURVE ( 'NONE', #83946, #69728, #24522, .T. ) ;
#87522 = CARTESIAN_POINT ( 'NONE',  ( 112.1775644307544013, -28.39036538331624726, 94.63848241876893042 ) ) ;
#87524 = CARTESIAN_POINT ( 'NONE',  ( 106.4848323041101850, -24.91801670280283787, 191.1156252759109861 ) ) ;
#87523 = LINE ( 'NONE', #25284, #40394 ) ;
#87525 = CARTESIAN_POINT ( 'NONE',  ( 98.34908471767082005, -31.65797358294662089, 60.90658434867807358 ) ) ;
#87526 = CARTESIAN_POINT ( 'NONE',  ( 33.91903122894440514, -35.91149509761246605, 193.9678068554150911 ) ) ;
#87527 = ORIENTED_EDGE ( 'NONE', *, *, #49837, .T. ) ;
#87528 = CYLINDRICAL_SURFACE ( 'NONE', #19396, 0.4999999999999982236 ) ;
#87529 = EDGE_CURVE ( 'NONE', #71312, #12494, #38928, .T. ) ;
#87530 = CARTESIAN_POINT ( 'NONE',  ( -103.1875000000000000, 127.0000000000000000, -1.080832317973422076E-12 ) ) ;
#87531 = CARTESIAN_POINT ( 'NONE',  ( 107.0667039024482818, -36.72944715994102438, 249.5838068554170093 ) ) ;
#87532 = EDGE_CURVE ( 'NONE', #79836, #77844, #39029, .T. ) ;
#87533 = DIRECTION ( 'NONE',  ( 0.9999999853157766072, 0.0001713722456134502174, 0.000000000000000000 ) ) ;
#87535 = ORIENTED_EDGE ( 'NONE', *, *, #11444, .F. ) ;
#87534 = CARTESIAN_POINT ( 'NONE',  ( 98.80440911621268185, -29.31655204712020080, 235.7565776568629872 ) ) ;
#87536 = LINE ( 'NONE', #66631, #45182 ) ;
#87537 = CARTESIAN_POINT ( 'NONE',  ( 116.5562423158612972, -42.44168660689859962, 274.3832443235299365 ) ) ;
#87538 = CARTESIAN_POINT ( 'NONE',  ( 102.2928874563330055, -26.70895414482565045, 136.4422919425779526 ) ) ;
#87539 = PLANE ( 'NONE',  #2683 ) ;
#87540 = CARTESIAN_POINT ( 'NONE',  ( 82.77657790094494317, -37.19711456031350849, 6.808568500764617504 ) ) ;
#87541 = CYLINDRICAL_SURFACE ( 'NONE', #31206, 1.999999999999999112 ) ;
#87542 = CYLINDRICAL_SURFACE ( 'NONE', #88753, 2.500000000000002220 ) ;
#87543 = ORIENTED_EDGE ( 'NONE', *, *, #67334, .F. ) ;
#87544 = EDGE_CURVE ( 'NONE', #35902, #59214, #86306, .T. ) ;
#87545 = AXIS2_PLACEMENT_3D ( 'NONE', #77038, #21634, #49306 ) ;
#87546 = VECTOR ( 'NONE', #27288, 999.9999999999998863 ) ;
#87547 = ADVANCED_FACE ( 'NONE', ( #40375 ), #6752, .F. ) ;
#87548 = ORIENTED_EDGE ( 'NONE', *, *, #43835, .F. ) ;
#87549 = ORIENTED_EDGE ( 'NONE', *, *, #15758, .F. ) ;
#87550 = ORIENTED_EDGE ( 'NONE', *, *, #67396, .T. ) ;
#87551 = CARTESIAN_POINT ( 'NONE',  ( -107.7702177616926065, 120.6499999999999915, -1.170464777364108012E-12 ) ) ;
#87552 = CARTESIAN_POINT ( 'NONE',  ( 106.6078071710152244, -25.70885557892973949, 36.09753003781596448 ) ) ;
#87553 = DIRECTION ( 'NONE',  ( 0.000000000000000000, 0.000000000000000000, 1.000000000000000000 ) ) ;
#87554 = ADVANCED_FACE ( 'NONE', ( #13134 ), #41701, .T. ) ;
#87556 = DIRECTION ( 'NONE',  ( 1.027984282060330356E-15, 1.000000000000000000, 0.000000000000000000 ) ) ;
#87555 = DIRECTION ( 'NONE',  ( 0.000000000000000000, 0.000000000000000000, 1.000000000000000000 ) ) ;
#87557 = CARTESIAN_POINT ( 'NONE',  ( 107.2162147037312678, -27.02129552338790575, 229.4867055423629836 ) ) ;
#87558 = ORIENTED_EDGE ( 'NONE', *, *, #23279, .F. ) ;
#87559 = EDGE_CURVE ( 'NONE', #44745, #82826, #73522, .T. ) ;
#87560 = ORIENTED_EDGE ( 'NONE', *, *, #55902, .T. ) ;
#87561 = VERTEX_POINT ( 'NONE', #60813 ) ;
#87562 = AXIS2_PLACEMENT_3D ( 'NONE', #24571, #88598, #52239 ) ;
#87563 = DIRECTION ( 'NONE',  ( -0.7071067811866279529, 0.7071067811864671926, -7.071067811865978232E-16 ) ) ;
#87564 = CIRCLE ( 'NONE', #51286, 0.9999999999999731326 ) ;
#87565 = CARTESIAN_POINT ( 'NONE',  ( 165.2725846195388328, -35.55794170701241796, 237.4678068554150059 ) ) ;
#87566 = DIRECTION ( 'NONE',  ( -4.237773401492740281E-14, 1.000000000000000000, 0.000000000000000000 ) ) ;
#87567 = CARTESIAN_POINT ( 'NONE',  ( 112.0788320361856307, -29.42159941445254390, 41.03015473446897232 ) ) ;
#87568 = CARTESIAN_POINT ( 'NONE',  ( 117.9189176348423871, 85.83559868056555331, -12.27472195321713855 ) ) ;
#87569 = VECTOR ( 'NONE', #86341, 999.9999999999998863 ) ;
#87570 = LINE ( 'NONE', #3550, #79628 ) ;
#87571 = CARTESIAN_POINT ( 'NONE',  ( 97.78144721833423603, -39.80378292816726571, 241.5813395616259811 ) ) ;
#87572 = CARTESIAN_POINT ( 'NONE',  ( 34.96670390244647564, -26.71338133339322951, 193.9678068554150911 ) ) ;
#87573 = EDGE_LOOP ( 'NONE', ( #24364, #30297, #11653, #73117 ) ) ;
#87574 = EDGE_CURVE ( 'NONE', #41295, #55881, #2701, .T. ) ;
#87575 = DIRECTION ( 'NONE',  ( 0.7071067811866377228, -0.7071067811864573116, 0.000000000000000000 ) ) ;
#87576 = EDGE_CURVE ( 'NONE', #86245, #65225, #34450, .T. ) ;
#87577 = FACE_OUTER_BOUND ( 'NONE', #35889, .T. ) ;
#87578 = CARTESIAN_POINT ( 'NONE',  ( 107.4895849179006575, -45.99858499349326735, 40.43094751244896656 ) ) ;
#87579 = CIRCLE ( 'NONE', #84684, 2.000000000000001776 ) ;
#87580 = CARTESIAN_POINT ( 'NONE',  ( 135.6073602527844457, -16.45223222829654475, 7.843813999037777762 ) ) ;
#87581 = DIRECTION ( 'NONE',  ( 0.000000000000000000, 0.000000000000000000, -1.000000000000000000 ) ) ;
#87582 = CARTESIAN_POINT ( 'NONE',  ( -2.883663860655375721, 94.92521392225150123, 118.5216208257077710 ) ) ;
#87583 = ORIENTED_EDGE ( 'NONE', *, *, #75724, .T. ) ;
#87584 = CARTESIAN_POINT ( 'NONE',  ( 97.81168895331838087, -40.51742574516882200, 287.6356252759109680 ) ) ;
#87585 = CARTESIAN_POINT ( 'NONE',  ( 125.1886942929311743, 55.61998119543657282, -37.04958746976185324 ) ) ;
#87586 = ORIENTED_EDGE ( 'NONE', *, *, #1949, .T. ) ;
#87587 = CARTESIAN_POINT ( 'NONE',  ( 96.63902489370863691, -37.56252461247890295, 101.3899109901969524 ) ) ;
#87588 = ORIENTED_EDGE ( 'NONE', *, *, #85099, .F. ) ;
#87589 = CARTESIAN_POINT ( 'NONE',  ( 110.1208792074641991, -44.70608788829420632, 62.28956268521896078 ) ) ;
#87590 = LINE ( 'NONE', #67137, #40198 ) ;
#87591 = CARTESIAN_POINT ( 'NONE',  ( 99.03873739112161445, -32.90617299384241790, 72.40444044875393104 ) ) ;
#87592 = EDGE_CURVE ( 'NONE', #54435, #57667, #59211, .T. ) ;
#87593 = CARTESIAN_POINT ( 'NONE',  ( 106.0667039024470171, -87.35579742913172652, -21.78219314458254630 ) ) ;
#87594 = DIRECTION ( 'NONE',  ( 1.000000000000000000, 1.132880637372608296E-15, 0.000000000000000000 ) ) ;
#87595 = CARTESIAN_POINT ( 'NONE',  ( 97.33132060198839497, -32.84282867815538509, 37.02419670448292521 ) ) ;
#87596 = CARTESIAN_POINT ( 'NONE',  ( 116.3214902495786873, -32.94210931476069248, 180.1356252759109680 ) ) ;
#87597 = ORIENTED_EDGE ( 'NONE', *, *, #78023, .F. ) ;
#87598 = ADVANCED_FACE ( 'NONE', ( #27644 ), #51935, .F. ) ;
#87599 = CARTESIAN_POINT ( 'NONE',  ( 116.3135889066590636, -32.94480564983713577, 259.1356252759109680 ) ) ;
#87600 = ORIENTED_EDGE ( 'NONE', *, *, #77859, .T. ) ;
#87601 = CARTESIAN_POINT ( 'NONE',  ( -118.1708971306822917, 74.16967745525862199, 9.551705748361122517 ) ) ;
#87602 = VECTOR ( 'NONE', #55075, 1000.000000000000000 ) ;
#87603 = ORIENTED_EDGE ( 'NONE', *, *, #69271, .F. ) ;
#87604 = VERTEX_POINT ( 'NONE', #48500 ) ;
#87605 = DIRECTION ( 'NONE',  ( -0.7071067811865535679, 0.000000000000000000, 0.7071067811865414665 ) ) ;
#87606 = ORIENTED_EDGE ( 'NONE', *, *, #19893, .F. ) ;
#87607 = CARTESIAN_POINT ( 'NONE',  ( 112.0813997088635858, -45.80630777137071874, 252.9661014663878689 ) ) ;
#87608 = CARTESIAN_POINT ( 'NONE',  ( 97.26831979079280188, -34.56112429623405546, 126.1522026196660278 ) ) ;
#87609 = CARTESIAN_POINT ( 'NONE',  ( 104.4081005686254571, -46.45808911557011101, 188.3647919350316897 ) ) ;
#87610 = CARTESIAN_POINT ( 'NONE',  ( 110.3540904097210387, -25.34409450869410563, 60.85276813305395649 ) ) ;
#87611 = DIRECTION ( 'NONE',  ( 1.000000000000000078E-15, -1.000000000000000083E-30, -1.000000000000000000 ) ) ;
#87612 = ORIENTED_EDGE ( 'NONE', *, *, #35202, .T. ) ;
#87613 = CARTESIAN_POINT ( 'NONE',  ( 112.1394879536045011, -28.01289599002803499, 114.6579011162244939 ) ) ;
#87614 = DIRECTION ( 'NONE',  ( 0.000000000000000000, -1.000000000000000000, 0.000000000000000000 ) ) ;
#87615 = ORIENTED_EDGE ( 'NONE', *, *, #23387, .F. ) ;
#87616 = AXIS2_PLACEMENT_3D ( 'NONE', #25800, #66683, #3566 ) ;
#87617 = FACE_BOUND ( 'NONE', #5360, .T. ) ;
#87618 = AXIS2_PLACEMENT_3D ( 'NONE', #54837, #84393, #82602 ) ;
#87619 = DIRECTION ( 'NONE',  ( 0.000000000000000000, 1.000000000000000000, 0.000000000000000000 ) ) ;
#87620 = CARTESIAN_POINT ( 'NONE',  ( 100.6697571656888073, -44.93374849542868787, 232.0499109901969632 ) ) ;
#87621 = DIRECTION ( 'NONE',  ( 0.000000000000000000, 0.000000000000000000, -1.000000000000000000 ) ) ;
#87622 = AXIS2_PLACEMENT_3D ( 'NONE', #22181, #78494, #29885 ) ;
#87623 = EDGE_CURVE ( 'NONE', #9653, #44627, #88984, .T. ) ;
#87624 = DIRECTION ( 'NONE',  ( 0.000000000000000000, 0.000000000000000000, -1.000000000000000000 ) ) ;
#87625 = CARTESIAN_POINT ( 'NONE',  ( 77.71552635664728825, -38.16021090637489976, 2.608895778946703992 ) ) ;
#87626 = EDGE_CURVE ( 'NONE', #73315, #28033, #82637, .T. ) ;
#87627 = CARTESIAN_POINT ( 'NONE',  ( 98.20387719113243463, -34.86749027545791080, 260.5962293518865636 ) ) ;
#87629 = CARTESIAN_POINT ( 'NONE',  ( 96.11054930851091171, -38.00668368623056637, 82.43086337114895912 ) ) ;
#87628 = CARTESIAN_POINT ( 'NONE',  ( 0.000000000000000000, 211.0000000000000000, 154.6557476874258441 ) ) ;
#87630 = CARTESIAN_POINT ( 'NONE',  ( 115.2855339205388532, 71.76331869045601763, 61.27220515712456006 ) ) ;
#87631 = CARTESIAN_POINT ( 'NONE',  ( 114.8040440383551157, -44.68828107661028781, 118.2022919425779719 ) ) ;
#87632 = VERTEX_POINT ( 'NONE', #20398 ) ;
#87633 = CARTESIAN_POINT ( 'NONE',  ( 133.6896269580626040, -21.47945062089170776, 8.225625248534988998 ) ) ;
#87634 = ORIENTED_EDGE ( 'NONE', *, *, #68684, .F. ) ;
#87635 = CARTESIAN_POINT ( 'NONE',  ( 28.57499999999999929, 77.96728223830730542, 294.9574999999999818 ) ) ;
#87636 = CIRCLE ( 'NONE', #89127, 2.517500000000005844 ) ;
#87637 = EDGE_CURVE ( 'NONE', #83459, #54780, #48068, .T. ) ;
#87638 = FACE_OUTER_BOUND ( 'NONE', #87820, .T. ) ;
#87639 = LINE ( 'NONE', #53067, #83331 ) ;
#87640 = ORIENTED_EDGE ( 'NONE', *, *, #27538, .T. ) ;
#87641 = CARTESIAN_POINT ( 'NONE',  ( 42.66648329127298922, 12.92155284005730387, 361.9756252759109998 ) ) ;
#87642 = EDGE_CURVE ( 'NONE', #81179, #26477, #88546, .T. ) ;
#87644 = ORIENTED_EDGE ( 'NONE', *, *, #3006, .T. ) ;
#87643 = CARTESIAN_POINT ( 'NONE',  ( 95.98894329157613470, -41.07880401750329469, 96.62419670448197451 ) ) ;
#87645 = LINE ( 'NONE', #38583, #79854 ) ;
#87646 = DIRECTION ( 'NONE',  ( -0.000000000000000000, -0.000000000000000000, -1.000000000000000000 ) ) ;
#87647 = DIRECTION ( 'NONE',  ( 0.000000000000000000, 1.000000000000000000, 0.000000000000000000 ) ) ;
#87648 = CARTESIAN_POINT ( 'NONE',  ( 97.81170495107971874, -40.51745053935989915, 26.63526479160227112 ) ) ;
#87649 = VERTEX_POINT ( 'NONE', #53978 ) ;
#87650 = EDGE_CURVE ( 'NONE', #85451, #67349, #35089, .T. ) ;
#87651 = CARTESIAN_POINT ( 'NONE',  ( 104.1015100224914960, -46.74719628246504044, 107.3470538473389411 ) ) ;
#87652 = DIRECTION ( 'NONE',  ( 0.000000000000000000, 0.000000000000000000, 1.000000000000000000 ) ) ;
#87653 = LINE ( 'NONE', #52642, #87792 ) ;
#87654 = CARTESIAN_POINT ( 'NONE',  ( 116.8171228670854447, -34.15291832200010447, 144.0314586091287197 ) ) ;
#87655 = ORIENTED_EDGE ( 'NONE', *, *, #9393, .F. ) ;
#87656 = ADVANCED_FACE ( 'NONE', ( #76243, #74904 ), #14924, .T. ) ;
#87657 = VERTEX_POINT ( 'NONE', #7653 ) ;
#87658 = DIRECTION ( 'NONE',  ( 0.000000000000000000, 1.000000000000000000, 0.000000000000000000 ) ) ;
#87659 = CARTESIAN_POINT ( 'NONE',  ( 108.2293999999999983, 117.4749999999999943, 3.602774393244745134E-13 ) ) ;
#87660 = PLANE ( 'NONE',  #68631 ) ;
#87661 = CARTESIAN_POINT ( 'NONE',  ( 103.8797721312301405, -101.8611209747514010, -19.78219314458209865 ) ) ;
#87663 = DIRECTION ( 'NONE',  ( 9.351236661543306751E-17, -3.725950533538267725E-29, -1.000000000000000000 ) ) ;
#87662 = DIRECTION ( 'NONE',  ( 0.000000000000000000, 0.000000000000000000, 1.000000000000000000 ) ) ;
#87664 = PLANE ( 'NONE',  #49490 ) ;
#87665 = ORIENTED_EDGE ( 'NONE', *, *, #22458, .T. ) ;
#87666 = CIRCLE ( 'NONE', #76058, 5.599999999999994316 ) ;
#87667 = CARTESIAN_POINT ( 'NONE',  ( 98.30753431935190179, -41.72887571374209159, 32.73979196285422688 ) ) ;
#87668 = CARTESIAN_POINT ( 'NONE',  ( 115.7764676695377517, -43.63945112744033850, 194.2927681330539542 ) ) ;
#87669 = ORIENTED_EDGE ( 'NONE', *, *, #1227, .F. ) ;
#87670 = CARTESIAN_POINT ( 'NONE',  ( 97.58158007118578325, -32.53714515026965870, 51.98324432352896451 ) ) ;
#87671 = CARTESIAN_POINT ( 'NONE',  ( -479.3614999999999782, 3.174999999999999822, 101.5999999999999943 ) ) ;
#87672 = CARTESIAN_POINT ( 'NONE',  ( -254.0000000000000000, 3.174999999999999822, 142.8750000000000000 ) ) ;
#87673 = CARTESIAN_POINT ( 'NONE',  ( 87.31648329127403940, -46.72944715994105280, -5.074374724089048883 ) ) ;
#87674 = ORIENTED_EDGE ( 'NONE', *, *, #42373, .T. ) ;
#87675 = DIRECTION ( 'NONE',  ( 0.000000000000000000, 1.000000000000000000, 0.000000000000000000 ) ) ;
#87676 = VERTEX_POINT ( 'NONE', #63966 ) ;
#87677 = ORIENTED_EDGE ( 'NONE', *, *, #19603, .F. ) ;
#87678 = ADVANCED_FACE ( 'NONE', ( #22639 ), #1291, .T. ) ;
#87679 = CARTESIAN_POINT ( 'NONE',  ( 115.1079044709731676, -40.52387399376650734, 224.9072975916109840 ) ) ;
#87680 = VECTOR ( 'NONE', #15092, 1000.000000000000000 ) ;
#87681 = CARTESIAN_POINT ( 'NONE',  ( 0.000000000000000000, 92.07499999999998863, 38.10000000000000142 ) ) ;
#87682 = CIRCLE ( 'NONE', #32559, 3.174999999999997158 ) ;
#87683 = VECTOR ( 'NONE', #75384, 1000.000000000000000 ) ;
#87684 = CARTESIAN_POINT ( 'NONE',  ( -117.9171910823874327, 85.85031469618031963, -12.29178224785141005 ) ) ;
#87685 = CIRCLE ( 'NONE', #25306, 2.117000000000007987 ) ;
#87686 = DIRECTION ( 'NONE',  ( 1.000000000000000000, 4.163336342344333240E-14, 0.000000000000000000 ) ) ;
#87687 = CARTESIAN_POINT ( 'NONE',  ( 82.32434691320904108, -38.30306751046272495, 2.518077574344857350 ) ) ;
#87688 = CIRCLE ( 'NONE', #48495, 10.00000000000000711 ) ;
#87689 = ORIENTED_EDGE ( 'NONE', *, *, #78516, .F. ) ;
#87690 = CARTESIAN_POINT ( 'NONE',  ( 73.24325998657060666, -46.55267046464442160, 14.92562527591093868 ) ) ;
#87691 = DIRECTION ( 'NONE',  ( 0.000000000000000000, -1.000000000000000000, 0.000000000000000000 ) ) ;
#87692 = ORIENTED_EDGE ( 'NONE', *, *, #68561, .T. ) ;
#87693 = CARTESIAN_POINT ( 'NONE',  ( 118.5710604172009965, -33.89858672578665733, 14.01848241876796308 ) ) ;
#87694 = EDGE_LOOP ( 'NONE', ( #41660, #77771 ) ) ;
#87695 = ORIENTED_EDGE ( 'NONE', *, *, #21931, .T. ) ;
#87696 = CARTESIAN_POINT ( 'NONE',  ( 107.8084489643801334, -27.48037055177216104, 262.8309475124484038 ) ) ;
#87697 = CARTESIAN_POINT ( 'NONE',  ( 177.0664832912730162, 12.92155284005730387, 355.9756252759109998 ) ) ;
#87698 = CARTESIAN_POINT ( 'NONE',  ( 61.00843881761244347, 49.07499999999999574, -53.97512327982435210 ) ) ;
#87699 = FACE_OUTER_BOUND ( 'NONE', #82891, .T. ) ;
#87700 = PLANE ( 'NONE',  #8586 ) ;
#87701 = CARTESIAN_POINT ( 'NONE',  ( 98.34346157482828232, -29.86603762143552032, 196.8080062282919869 ) ) ;
#87702 = PLANE ( 'NONE',  #54326 ) ;
#87703 = VERTEX_POINT ( 'NONE', #35790 ) ;
#87704 = EDGE_CURVE ( 'NONE', #61739, #53210, #2188, .T. ) ;
#87705 = CARTESIAN_POINT ( 'NONE',  ( 113.4418579183357849, -27.64362872000679516, 80.57753003781597556 ) ) ;
#87706 = DIRECTION ( 'NONE',  ( 0.000000000000000000, 0.000000000000000000, 1.000000000000000000 ) ) ;
#87707 = ORIENTED_EDGE ( 'NONE', *, *, #32998, .F. ) ;
#87708 = VERTEX_POINT ( 'NONE', #35341 ) ;
#87709 = ORIENTED_EDGE ( 'NONE', *, *, #21092, .F. ) ;
#87710 = CARTESIAN_POINT ( 'NONE',  ( 102.0657985602851596, -27.97123491610403434, 160.4896842913302066 ) ) ;
#87711 = PLANE ( 'NONE',  #41301 ) ;
#87712 = CARTESIAN_POINT ( 'NONE',  ( 97.81170238817014706, -40.51743819009087844, 137.6355114220584994 ) ) ;
#87713 = CARTESIAN_POINT ( 'NONE',  ( 105.6960798208838384, -45.90617939248504342, 145.2766617981629622 ) ) ;
#87714 = CARTESIAN_POINT ( 'NONE',  ( 98.88183825371838509, -29.26641886349639066, 226.7261014663869503 ) ) ;
#87715 = CARTESIAN_POINT ( 'NONE',  ( 168.3595971214446934, -48.62134037892948157, 249.9678068554149775 ) ) ;
#87716 = VERTEX_POINT ( 'NONE', #50311 ) ;
#87717 = CARTESIAN_POINT ( 'NONE',  ( 130.5401660959919354, 95.08644067748866746, 2.073645319395265307 ) ) ;
#87718 = DIRECTION ( 'NONE',  ( -4.237773401492740281E-14, 1.000000000000000000, 0.000000000000000000 ) ) ;
#87719 = ORIENTED_EDGE ( 'NONE', *, *, #30016, .F. ) ;
#87720 = VERTEX_POINT ( 'NONE', #43043 ) ;
#87721 = MECHANICAL_DESIGN_GEOMETRIC_PRESENTATION_REPRESENTATION (  '', ( #2145 ), #52912 ) ;
#87722 = CARTESIAN_POINT ( 'NONE',  ( 177.1649999999999920, 25.81350000000000477, -7.937500000000000000 ) ) ;
#87723 = VERTEX_POINT ( 'NONE', #42592 ) ;
#87724 = ORIENTED_EDGE ( 'NONE', *, *, #70395, .F. ) ;
#87725 = LINE ( 'NONE', #17350, #32336 ) ;
#87726 = AXIS2_PLACEMENT_3D ( 'NONE', #42046, #30227, #29781 ) ;
#87727 = CARTESIAN_POINT ( 'NONE',  ( 107.9678037105606023, -87.30234574837481887, -21.78219314458254630 ) ) ;
#87728 = CARTESIAN_POINT ( 'NONE',  ( 102.0657424188261899, -27.97126782499678299, 25.48991181321247268 ) ) ;
#87729 = EDGE_CURVE ( 'NONE', #37766, #85594, #78055, .T. ) ;
#87730 = CARTESIAN_POINT ( 'NONE',  ( 97.64684354035226477, -39.08338314719364348, 165.9438483995059528 ) ) ;
#87731 = CARTESIAN_POINT ( 'NONE',  ( 96.64524470886469487, -32.90705862865544162, 21.03467289495897319 ) ) ;
#87732 = CARTESIAN_POINT ( 'NONE',  ( 78.89953865151133527, -101.2959575815152675, 250.2190963482990185 ) ) ;
#87733 = ORIENTED_EDGE ( 'NONE', *, *, #15284, .F. ) ;
#87734 = EDGE_CURVE ( 'NONE', #21614, #58445, #49861, .T. ) ;
#87735 = LINE ( 'NONE', #24615, #18016 ) ;
#87736 = EDGE_CURVE ( 'NONE', #75279, #78504, #71678, .T. ) ;
#87737 = ORIENTED_EDGE ( 'NONE', *, *, #44521, .T. ) ;
#87738 = CARTESIAN_POINT ( 'NONE',  ( -186.2398777604655038, 101.5999999999999943, -12.69999999999999929 ) ) ;
#87739 = EDGE_CURVE ( 'NONE', #84388, #17172, #62137, .T. ) ;
#87740 = ORIENTED_EDGE ( 'NONE', *, *, #81484, .F. ) ;
#87741 = CARTESIAN_POINT ( 'NONE',  ( 177.1649999999999920, 5.112500000000000711, -58.73749999999999716 ) ) ;
#87742 = CARTESIAN_POINT ( 'NONE',  ( 148.0533267522749838, 101.5999999999999943, -160.2664750769289697 ) ) ;
#87743 = CARTESIAN_POINT ( 'NONE',  ( 116.9280472011850520, -38.65089867813137658, 133.6735763414937423 ) ) ;
#87745 = AXIS2_PLACEMENT_3D ( 'NONE', #56602, #71157, #30258 ) ;
#87744 = DIRECTION ( 'NONE',  ( -6.982966722218760189E-15, 0.000000000000000000, 1.000000000000000000 ) ) ;
#87746 = ORIENTED_EDGE ( 'NONE', *, *, #4979, .T. ) ;
#87747 = CARTESIAN_POINT ( 'NONE',  ( 116.7906267970580103, -31.42506456344890964, 24.21181575210196257 ) ) ;
#87748 = VECTOR ( 'NONE', #73577, 1000.000000000000000 ) ;
#87749 = CARTESIAN_POINT ( 'NONE',  ( 115.7648065088891371, -43.62413145733483333, 44.30514908543492680 ) ) ;
#87750 = AXIS2_PLACEMENT_3D ( 'NONE', #86127, #9819, #37526 ) ;
#87751 =( LENGTH_UNIT ( ) NAMED_UNIT ( * ) SI_UNIT ( .MILLI., .METRE. ) );
#87752 = AXIS2_PLACEMENT_3D ( 'NONE', #27822, #77325, #1023 ) ;
#87754 = CARTESIAN_POINT ( 'NONE',  ( 91.91125933621934507, -111.8737466215628160, -19.26696060647578435 ) ) ;
#87753 = DIRECTION ( 'NONE',  ( 1.000000000000000078E-15, 0.000000000000000000, 1.000000000000000000 ) ) ;
#87755 = DIRECTION ( 'NONE',  ( 0.000000000000000000, 0.000000000000000000, -1.000000000000000000 ) ) ;
#87756 = CARTESIAN_POINT ( 'NONE',  ( 176.7669697523291461, -48.62818131005482059, 249.9678068554149775 ) ) ;
#87757 = LINE ( 'NONE', #11906, #78925 ) ;
#87758 = EDGE_CURVE ( 'NONE', #35953, #67515, #23099, .T. ) ;
#87759 = AXIS2_PLACEMENT_3D ( 'NONE', #730, #70682, #76600 ) ;
#87760 = CARTESIAN_POINT ( 'NONE',  ( 46.48091746482047171, -48.32844715994088602, 129.9678068554150911 ) ) ;
#87761 = CARTESIAN_POINT ( 'NONE',  ( 147.0667039024470171, -77.84948640091441519, 245.5415602474340062 ) ) ;
#87762 = VERTEX_POINT ( 'NONE', #43493 ) ;
#87763 = CARTESIAN_POINT ( 'NONE',  ( 118.7820429505835733, -34.63792632846725184, 48.96705384733895983 ) ) ;
#87764 = CARTESIAN_POINT ( 'NONE',  ( 98.03678599612689482, -44.40402742967116723, 222.8870538473399563 ) ) ;
#87765 = CARTESIAN_POINT ( 'NONE',  ( 117.1124756048696440, -32.06433792440376607, 55.16038718067301261 ) ) ;
#87767 = FACE_OUTER_BOUND ( 'NONE', #17129, .T. ) ;
#87766 = CARTESIAN_POINT ( 'NONE',  ( 97.81555608408764613, -40.52686364465421320, 171.6367057649424623 ) ) ;
#87768 = LINE ( 'NONE', #88679, #87195 ) ;
#87769 = VECTOR ( 'NONE', #80521, 1000.000000000000000 ) ;
#87770 = VECTOR ( 'NONE', #49632, 1000.000000000000000 ) ;
#87771 = ORIENTED_EDGE ( 'NONE', *, *, #7022, .F. ) ;
#87772 = CARTESIAN_POINT ( 'NONE',  ( 112.1393456656949041, -28.01282279600963676, 185.6564586070249447 ) ) ;
#87773 = ORIENTED_EDGE ( 'NONE', *, *, #23826, .T. ) ;
#87774 = CARTESIAN_POINT ( 'NONE',  ( 97.83387747045378546, -32.00739517038279303, 91.96229194257693962 ) ) ;
#87776 = ORIENTED_EDGE ( 'NONE', *, *, #68228, .F. ) ;
#87775 = CARTESIAN_POINT ( 'NONE',  ( -33.98325472291460159, 124.5870000000000033, -3.175000000000234746 ) ) ;
#87777 = CARTESIAN_POINT ( 'NONE',  ( 110.2492204789523100, -26.78788743924354065, 230.8299109901969643 ) ) ;
#87778 = CARTESIAN_POINT ( 'NONE',  ( 241.3336515812914911, 65.43750000000000000, 10.66800000000000104 ) ) ;
#87779 = DIRECTION ( 'NONE',  ( -0.000000000000000000, -0.000000000000000000, 1.000000000000000000 ) ) ;
#87780 = DIRECTION ( 'NONE',  ( -1.000000000000000000, -1.206764157201257538E-15, 0.000000000000000000 ) ) ;
#87781 = CARTESIAN_POINT ( 'NONE',  ( 188.5667039024479834, -62.87844715994099687, 293.2178068554150627 ) ) ;
#87782 = CARTESIAN_POINT ( 'NONE',  ( 133.4132809338130699, -39.40256188477528099, 1.689562700881797053 ) ) ;
#87783 = DIRECTION ( 'NONE',  ( 0.000000000000000000, 0.000000000000000000, 1.000000000000000000 ) ) ;
#87784 = CARTESIAN_POINT ( 'NONE',  ( 116.8150918559700813, -40.26546416881835455, 173.5375300378159693 ) ) ;
#87785 = EDGE_LOOP ( 'NONE', ( #47152, #34424, #39443, #85604 ) ) ;
#87786 = ORIENTED_EDGE ( 'NONE', *, *, #57790, .T. ) ;
#87787 = ADVANCED_FACE ( 'NONE', ( #9442 ), #1743, .F. ) ;
#87788 = CARTESIAN_POINT ( 'NONE',  ( 108.7714652236932835, -45.96901220096565055, 124.1653928297069882 ) ) ;
#87789 = LINE ( 'NONE', #82339, #44295 ) ;
#87791 = CARTESIAN_POINT ( 'NONE',  ( 107.0667039024468039, -54.72944715994100306, 199.5838068554169809 ) ) ;
#87790 = CARTESIAN_POINT ( 'NONE',  ( 101.9853755998761500, -45.08682593082387058, 243.1413395616249886 ) ) ;
#87792 = VECTOR ( 'NONE', #74017, 1000.000000000000000 ) ;
#87793 = CARTESIAN_POINT ( 'NONE',  ( 194.5667039024479834, -40.82844715993405771, 300.4678068554149490 ) ) ;
#87795 = EDGE_CURVE ( 'NONE', #75315, #37650, #36086, .T. ) ;
#87794 = CARTESIAN_POINT ( 'NONE',  ( 186.6899999999999977, 52.73749999999999716, -53.97500000000000142 ) ) ;
#87796 = LINE ( 'NONE', #72826, #82334 ) ;
#87797 = CARTESIAN_POINT ( 'NONE',  ( 106.1656040943334318, -87.30234574837474781, -19.18411693322955003 ) ) ;
#87798 = PLANE ( 'NONE',  #10105 ) ;
#87799 = LINE ( 'NONE', #46880, #35670 ) ;
#87800 = CARTESIAN_POINT ( 'NONE',  ( 117.0473132972741865, -39.66401662079137225, 183.5984824187679578 ) ) ;
#87801 = CARTESIAN_POINT ( 'NONE',  ( 100.9548448467986219, -28.70687276283804934, 170.5930046438545276 ) ) ;
#87802 = VERTEX_POINT ( 'NONE', #37151 ) ;
#87803 = VERTEX_POINT ( 'NONE', #71239 ) ;
#87804 = FACE_OUTER_BOUND ( 'NONE', #31534, .T. ) ;
#87805 = CARTESIAN_POINT ( 'NONE',  ( 81.55977255149463190, -21.04085022825163520, 7.869587501197700341 ) ) ;
#87806 = B_SPLINE_CURVE_WITH_KNOTS ( 'NONE', 3,
 ( #78680, #17323, #4127, #9170, #10938, #71844, #15990, #37316, #9607, #43670, #17762, #72291, #71406, #66342, #31378, #86367, #3251, #23272 ),
 .UNSPECIFIED., .F., .F.,
 ( 4, 2, 2, 2, 2, 2, 2, 2, 4 ),
 ( 0.4999999997770634419, 0.5624999998049304839, 0.6249999998327975259, 0.6874999998606646789, 0.7499999998885317209, 0.8124999999163987630, 0.8749999999442659160, 0.9374999999721329580, 1.000000000000000000 ),
 .UNSPECIFIED. ) ;
#87807 = CARTESIAN_POINT ( 'NONE',  ( 121.3178890780284291, -95.01002112898673602, -19.18411693322930134 ) ) ;
#87808 = LINE ( 'NONE', #88718, #74371 ) ;
#87810 = CARTESIAN_POINT ( 'NONE',  ( 97.70670343771699606, -40.25169526565032641, 96.61288812823406147 ) ) ;
#87809 = AXIS2_PLACEMENT_3D ( 'NONE', #26452, #46422, #32807 ) ;
#87811 = VERTEX_POINT ( 'NONE', #63055 ) ;
#87812 = ADVANCED_FACE ( 'NONE', ( #78506 ), #85768, .F. ) ;
#87813 = CONICAL_SURFACE ( 'NONE', #15331, 1.258750000000002922, 1.029744258676650093 ) ;
#87814 = DIRECTION ( 'NONE',  ( 1.000000000000000000, 1.000000000000000078E-15, 0.000000000000000000 ) ) ;
#87815 = VECTOR ( 'NONE', #37408, 1000.000000000000000 ) ;
#87816 = AXIS2_PLACEMENT_3D ( 'NONE', #45316, #73482, #52121 ) ;
#87817 = CARTESIAN_POINT ( 'NONE',  ( 115.8553914792215380, -44.67901184617146981, 233.2413395616259493 ) ) ;
#87818 = DIRECTION ( 'NONE',  ( 3.999999999999999995E-14, -1.000000000000000000, 4.100000000000000342E-29 ) ) ;
#87819 = EDGE_LOOP ( 'NONE', ( #54462, #73280, #83963, #3376 ) ) ;
#87820 = EDGE_LOOP ( 'NONE', ( #11345, #62326, #29921, #9242 ) ) ;
#87821 = AXIS2_PLACEMENT_3D ( 'NONE', #53879, #12583, #8002 ) ;
#87822 = CARTESIAN_POINT ( 'NONE',  ( 116.6612529692701230, -33.83881916766647180, 65.05964535752768541 ) ) ;
#87823 = PLANE ( 'NONE',  #71029 ) ;
#87824 = CARTESIAN_POINT ( 'NONE',  ( 98.54779198038390575, -41.97720663294746402, 166.7658525804957890 ) ) ;
#87825 = CARTESIAN_POINT ( 'NONE',  ( 110.3993955946342993, -29.27817736879564237, 22.55951894101998434 ) ) ;
#87827 = AXIS2_PLACEMENT_3D ( 'NONE', #62634, #13591, #6774 ) ;
#87826 = CARTESIAN_POINT ( 'NONE',  ( 113.9312237880395600, -28.03689036367077492, 120.5565776568639507 ) ) ;
#87828 = EDGE_CURVE ( 'NONE', #66416, #85229, #4179, .T. ) ;
#87829 = LINE ( 'NONE', #81034, #44879 ) ;
#87830 = ORIENTED_EDGE ( 'NONE', *, *, #82165, .T. ) ;
#87831 = AXIS2_PLACEMENT_3D ( 'NONE', #32240, #67212, #74486 ) ;
#87832 = FACE_OUTER_BOUND ( 'NONE', #18006, .T. ) ;
#87833 = CARTESIAN_POINT ( 'NONE',  ( 106.5394234437989667, -24.24056378642895737, 322.0356252759110021 ) ) ;
#87834 = VERTEX_POINT ( 'NONE', #16265 ) ;
#87835 = EDGE_LOOP ( 'NONE', ( #56495, #79410, #77345, #79144, #84534, #17453 ) ) ;
#87836 = DIRECTION ( 'NONE',  ( 0.000000000000000000, 0.000000000000000000, -1.000000000000000000 ) ) ;
#87837 = EDGE_LOOP ( 'NONE', ( #44646, #71640 ) ) ;
#87838 = ORIENTED_EDGE ( 'NONE', *, *, #85204, .T. ) ;
#87839 = CARTESIAN_POINT ( 'NONE',  ( 105.7976818973216666, -26.72428486692717797, 156.1772091278820653 ) ) ;
#87840 = AXIS2_PLACEMENT_3D ( 'NONE', #9220, #596, #42812 ) ;
#87841 = CARTESIAN_POINT ( 'NONE',  ( 106.1832117796525807, -28.23380338452170335, 49.58099125664799800 ) ) ;
#87842 = CARTESIAN_POINT ( 'NONE',  ( 116.8782924623045290, -40.31758940317881468, 218.5470538473399529 ) ) ;
#87843 = CARTESIAN_POINT ( 'NONE',  ( 102.0615167388204725, -46.55869598106830409, 172.2137205140059564 ) ) ;
#87845 = CARTESIAN_POINT ( 'NONE',  ( 101.0866664386429647, -45.26901348810219616, 278.0899109901965858 ) ) ;
#87844 = DIRECTION ( 'NONE',  ( 0.000000000000000000, 0.000000000000000000, -1.000000000000000000 ) ) ;
#87846 = DIRECTION ( 'NONE',  ( 1.000000000000000000, 0.000000000000000000, 0.000000000000000000 ) ) ;
#87847 = ADVANCED_FACE ( 'NONE', ( #22192 ), #57122, .F. ) ;
#87848 = DIRECTION ( 'NONE',  ( 0.7071067811865779928, -0.7071067811865171526, 7.071067811865475333E-16 ) ) ;
#87849 = ORIENTED_EDGE ( 'NONE', *, *, #29455, .F. ) ;
#87850 = ORIENTED_EDGE ( 'NONE', *, *, #35212, .T. ) ;
#87851 = CIRCLE ( 'NONE', #47238, 3.000000000000002665 ) ;
#87852 = DIRECTION ( 'NONE',  ( 0.000000000000000000, -1.000000000000000000, 0.000000000000000000 ) ) ;
#87853 = CARTESIAN_POINT ( 'NONE',  ( 103.2876017065440664, -26.96590681778891252, 215.3699109901969848 ) ) ;
#87854 = ORIENTED_EDGE ( 'NONE', *, *, #36470, .F. ) ;
#87855 = CARTESIAN_POINT ( 'NONE',  ( 95.40772882630993479, -38.85404833720006224, 201.4699109901969791 ) ) ;
#87856 = CARTESIAN_POINT ( 'NONE',  ( 115.0878329645725131, -30.61624704198809610, 264.3439639102033425 ) ) ;
#87857 = VECTOR ( 'NONE', #60586, 1000.000000000000000 ) ;
#87858 = DIRECTION ( 'NONE',  ( 0.1858654558203329255, -0.9825752044157738396, 0.000000000000000000 ) ) ;
#87859 = CARTESIAN_POINT ( 'NONE',  ( 143.5320129146941213, -139.6569233413941618, 247.2784140332015568 ) ) ;
#87861 = LINE ( 'NONE', #54643, #31145 ) ;
#87860 = CARTESIAN_POINT ( 'NONE',  ( 100.6116892621281949, -31.39203453219122864, 277.6356252759112522 ) ) ;
#87862 = CARTESIAN_POINT ( 'NONE',  ( 109.6428154823273644, -46.48014078660262527, 173.7814426156472223 ) ) ;
#87863 = FACE_OUTER_BOUND ( 'NONE', #60864, .T. ) ;
#87864 = CARTESIAN_POINT ( 'NONE',  ( 19.56648329127400032, 25.62155284005901379, 323.8756252759109202 ) ) ;
#87865 = EDGE_CURVE ( 'NONE', #57278, #65312, #56219, .T. ) ;
#87866 = CYLINDRICAL_SURFACE ( 'NONE', #42837, 9.524999999999998579 ) ;
#87867 = EDGE_CURVE ( 'NONE', #19753, #47917, #77148, .T. ) ;
#87868 = DIRECTION ( 'NONE',  ( -0.7071067811985214391, 0.7071067811745735954, 0.000000000000000000 ) ) ;
#87869 = CARTESIAN_POINT ( 'NONE',  ( -47.16614613999456651, 91.93851508972313979, -43.22209291737998882 ) ) ;
#87871 = VERTEX_POINT ( 'NONE', #4857 ) ;
#87870 = CARTESIAN_POINT ( 'NONE',  ( 99.69663197418856271, -31.46466773810444906, 195.5838068554171230 ) ) ;
#87872 = FACE_OUTER_BOUND ( 'NONE', #16549, .T. ) ;
#87873 = CARTESIAN_POINT ( 'NONE',  ( 113.0381276193345883, -46.05869713813741129, 218.0175300378159591 ) ) ;
#87874 = CARTESIAN_POINT ( 'NONE',  ( 97.93258204476157402, -31.63109636822184711, 106.9213395616259703 ) ) ;
#87875 = CARTESIAN_POINT ( 'NONE',  ( 97.12841500021716001, -40.02000613830777098, 237.5813395616249579 ) ) ;
#87876 = CARTESIAN_POINT ( 'NONE',  ( 49.16670390244701139, -28.27351298637340093, -5.074374724088000832 ) ) ;
#87877 = CARTESIAN_POINT ( 'NONE',  ( 80.06648329127398256, -9.029447159941060619, 4.925625275910944012 ) ) ;
#87879 = FACE_OUTER_BOUND ( 'NONE', #42669, .T. ) ;
#87878 = CARTESIAN_POINT ( 'NONE',  ( 34.33598329127477911, -36.32844715994133367, 300.4678068554150059 ) ) ;
#87880 = PLANE ( 'NONE',  #66811 ) ;
#87881 = LINE ( 'NONE', #25646, #83387 ) ;
#87882 = VECTOR ( 'NONE', #15416, 1000.000000000000114 ) ;
#87883 = AXIS2_PLACEMENT_3D ( 'NONE', #77628, #84462, #89929 ) ;
#87884 = CIRCLE ( 'NONE', #31331, 4.750000000000004441 ) ;
#87885 = AXIS2_PLACEMENT_3D ( 'NONE', #7592, #35279, #68473 ) ;
#87886 = ORIENTED_EDGE ( 'NONE', *, *, #66295, .T. ) ;
#87887 = ORIENTED_EDGE ( 'NONE', *, *, #81101, .F. ) ;
#87888 = CARTESIAN_POINT ( 'NONE',  ( 112.8906599442021275, -43.66427313951261624, 147.5428960185529661 ) ) ;
#87890 = ORIENTED_EDGE ( 'NONE', *, *, #35027, .T. ) ;
#87889 = DIRECTION ( 'NONE',  ( -1.000000000000000000, 0.000000000000000000, 2.544367396927093358E-16 ) ) ;
#87891 = CARTESIAN_POINT ( 'NONE',  ( 179.1667039024473809, -26.71338133338671739, 313.9678068554149490 ) ) ;
#87892 = CARTESIAN_POINT ( 'NONE',  ( 107.3333893024683903, -26.32957087652229689, 116.0556252759109555 ) ) ;
#87893 = CARTESIAN_POINT ( 'NONE',  ( 238.4043397404674920, 52.73749999999999716, -2.903194600000015502 ) ) ;
#87894 = CARTESIAN_POINT ( 'NONE',  ( 152.0368932755773130, -23.42844715993587812, 129.9678068554149775 ) ) ;
#87895 = CARTESIAN_POINT ( 'NONE',  ( 92.91125933621934507, -113.6057974291317691, -21.78219314458173983 ) ) ;
#87896 = DIRECTION ( 'NONE',  ( 0.000000000000000000, -1.000000000000000000, 0.000000000000000000 ) ) ;
#87898 = CARTESIAN_POINT ( 'NONE',  ( 99.16769444712198833, -43.44866735504071187, 76.89943479972100704 ) ) ;
#87897 = AXIS2_PLACEMENT_3D ( 'NONE', #55692, #6243, #88918 ) ;
#87899 = ORIENTED_EDGE ( 'NONE', *, *, #65870, .T. ) ;
#87900 = EDGE_LOOP ( 'NONE', ( #35192, #87332, #29013, #57631 ) ) ;
#87901 = ORIENTED_EDGE ( 'NONE', *, *, #55241, .F. ) ;
#87902 = DIRECTION ( 'NONE',  ( 1.000000000000000078E-15, 1.000000000000000083E-30, -1.000000000000000000 ) ) ;
#87903 = SHAPE_REPRESENTATION ( 'Rotary Table Drive Mechanism', ( #50656 ), #27649 ) ;
#87905 = CARTESIAN_POINT ( 'NONE',  ( 36.65249034007441509, -48.32844715994130524, 180.4678068554150911 ) ) ;
#87904 = CARTESIAN_POINT ( 'NONE',  ( 116.8150918559699818, -40.26546416881831192, 169.5375300378149745 ) ) ;
#87906 = AXIS2_PLACEMENT_3D ( 'NONE', #42279, #13253, #40939 ) ;
#87907 = DIRECTION ( 'NONE',  ( -1.000000000000000000, 1.000000000000000078E-15, 0.000000000000000000 ) ) ;
#87908 = DIRECTION ( 'NONE',  ( 4.299999999999999979E-14, -1.000000000000000000, 0.000000000000000000 ) ) ;
#87909 = CYLINDRICAL_SURFACE ( 'NONE', #54657, 1.000000000000000888 ) ;
#87910 = DIRECTION ( 'NONE',  ( 0.000000000000000000, 1.000000000000000000, 0.000000000000000000 ) ) ;
#87911 = CARTESIAN_POINT ( 'NONE',  ( 67.06804154766946624, -67.87911383296281542, 245.5633152175482223 ) ) ;
#87912 = CARTESIAN_POINT ( 'NONE',  ( 103.8480726019013218, -46.65951555449696997, 82.32705384733995402 ) ) ;
#87913 = ORIENTED_EDGE ( 'NONE', *, *, #22014, .F. ) ;
#87914 = VERTEX_POINT ( 'NONE', #16709 ) ;
#87915 = PLANE ( 'NONE',  #32816 ) ;
#87916 = DIRECTION ( 'NONE',  ( -0.9254794337955620787, -0.3787978585227822492, 0.000000000000000000 ) ) ;
#87917 = CARTESIAN_POINT ( 'NONE',  ( 180.2121375201597004, -29.73316016638962722, 193.9678068554150059 ) ) ;
#87918 = CARTESIAN_POINT ( 'NONE',  ( 100.8299159177638984, -43.59960581930123880, 154.8080903695919801 ) ) ;
#87919 = EDGE_CURVE ( 'NONE', #7620, #73802, #44839, .T. ) ;
#87920 = CARTESIAN_POINT ( 'NONE',  ( 57.14999999999999858, 95.25000000000000000, 280.2255000000000109 ) ) ;
#87921 = ORIENTED_EDGE ( 'NONE', *, *, #44750, .T. ) ;
#87922 = ORIENTED_EDGE ( 'NONE', *, *, #30512, .T. ) ;
#87923 = ADVANCED_FACE ( 'NONE', ( #72117 ), #87089, .F. ) ;
#87924 = CARTESIAN_POINT ( 'NONE',  ( 141.8664832912729992, -71.52944715994142655, 361.9756252759109998 ) ) ;
#87925 = VERTEX_POINT ( 'NONE', #3511 ) ;
#87926 = VERTEX_POINT ( 'NONE', #87982 ) ;
#87927 = FACE_OUTER_BOUND ( 'NONE', #46316, .T. ) ;
#87928 = EDGE_CURVE ( 'NONE', #61077, #37281, #38040, .T. ) ;
#87929 = CARTESIAN_POINT ( 'NONE',  ( 107.5663136956459738, -46.11170142552477813, 194.0625356868489462 ) ) ;
#87930 = EDGE_CURVE ( 'NONE', #54590, #24712, #44760, .T. ) ;
#87931 = CARTESIAN_POINT ( 'NONE',  ( 112.2214490935429438, -49.20647916188104887, 293.6356252759106837 ) ) ;
#87932 = VECTOR ( 'NONE', #16776, 1000.000000000000000 ) ;
#87933 = CARTESIAN_POINT ( 'NONE',  ( 1.387778780781445676E-14, 184.0000000000000000, 97.27542076772557778 ) ) ;
#87934 = ADVANCED_FACE ( 'NONE', ( #24417 ), #72569, .T. ) ;
#87935 = DIRECTION ( 'NONE',  ( -0.2588190451025246253, 0.000000000000000000, 0.9659258262890673130 ) ) ;
#87936 = CIRCLE ( 'NONE', #61788, 2.116999999999993776 ) ;
#87937 = VERTEX_POINT ( 'NONE', #58466 ) ;
#87938 = ORIENTED_EDGE ( 'NONE', *, *, #48176, .F. ) ;
#87939 = AXIS2_PLACEMENT_3D ( 'NONE', #60008, #68201, #20509 ) ;
#87940 = AXIS2_PLACEMENT_3D ( 'NONE', #20995, #63673, #1457 ) ;
#87941 = ORIENTED_EDGE ( 'NONE', *, *, #70487, .T. ) ;
#87942 = ORIENTED_EDGE ( 'NONE', *, *, #1554, .F. ) ;
#87943 = EDGE_CURVE ( 'NONE', #13404, #30894, #37577, .T. ) ;
#87944 = CARTESIAN_POINT ( 'NONE',  ( 114.5355946289170390, -40.02218186577253789, 251.3138046553057734 ) ) ;
#87945 = CARTESIAN_POINT ( 'NONE',  ( 117.1278252906914048, -39.54294340788323581, 98.60991099019594230 ) ) ;
#87946 = CARTESIAN_POINT ( 'NONE',  ( 117.9791962420231073, -38.33460093242097599, 73.72229194257801055 ) ) ;
#87947 = CARTESIAN_POINT ( 'NONE',  ( 104.6193894214979707, -44.52608570832915547, 249.5838068554171798 ) ) ;
#87948 = PRODUCT ( 'Feed Lead', 'Feed Lead', '', ( #88992 ) ) ;
#87949 = CARTESIAN_POINT ( 'NONE',  ( 129.9695788989828600, -140.6784471599409301, 245.6313834131549925 ) ) ;
#87950 = DIRECTION ( 'NONE',  ( 0.000000000000000000, 0.000000000000000000, 1.000000000000000000 ) ) ;
#87951 = CARTESIAN_POINT ( 'NONE',  ( 99.42212199502026237, -27.67378918447352731, 146.6356252759109395 ) ) ;
#87952 = ADVANCED_FACE ( 'NONE', ( #17600 ), #45279, .F. ) ;
#87953 = CARTESIAN_POINT ( 'NONE',  ( 106.0988423365887030, -87.33724229552865381, -19.23816181211554621 ) ) ;
#87954 = VERTEX_POINT ( 'NONE', #4418 ) ;
#87955 = PLANE ( 'NONE',  #33655 ) ;
#87956 = ORIENTED_EDGE ( 'NONE', *, *, #62939, .F. ) ;
#87957 = ORIENTED_EDGE ( 'NONE', *, *, #24898, .F. ) ;
#87958 = PLANE ( 'NONE',  #10751 ) ;
#87959 = CARTESIAN_POINT ( 'NONE',  ( 165.6738106836199904, -26.00627455219321860, -5.074374724088000832 ) ) ;
#87960 = AXIS2_PLACEMENT_3D ( 'NONE', #70985, #63710, #44134 ) ;
#87961 = VERTEX_POINT ( 'NONE', #73896 ) ;
#87962 = LINE ( 'NONE', #19814, #27259 ) ;
#87963 = EDGE_LOOP ( 'NONE', ( #74377, #66988, #62168, #26300 ) ) ;
#87964 = CARTESIAN_POINT ( 'NONE',  ( 105.7154773057149839, -46.72385838908932953, 177.4689586075003547 ) ) ;
#87965 = CARTESIAN_POINT ( 'NONE',  ( 97.54218415029114908, -32.48978251111615378, 100.9927681330539713 ) ) ;
#87966 = LINE ( 'NONE', #46603, #48954 ) ;
#87967 = AXIS2_PLACEMENT_3D ( 'NONE', #87661, #46745, #88119 ) ;
#87968 = CARTESIAN_POINT ( 'NONE',  ( 3.174999999999889688, 104.3431970271541900, 31.75000000000000000 ) ) ;
#87969 = CYLINDRICAL_SURFACE ( 'NONE', #47003, 9.999999999999998224 ) ;
#87972 = CARTESIAN_POINT ( 'NONE',  ( 97.69433714244412670, -41.24514667321082584, 167.6841967044829573 ) ) ;
#87971 = CARTESIAN_POINT ( 'NONE',  ( 115.5439452383992176, -108.5954344580498372, -19.78219314458187839 ) ) ;
#87970 = CARTESIAN_POINT ( 'NONE',  ( 105.7154773207258813, -46.72385839099544569, 143.4689586084740824 ) ) ;
#87973 = DIRECTION ( 'NONE',  ( 0.000000000000000000, 0.000000000000000000, 1.000000000000000000 ) ) ;
#87974 = DIRECTION ( 'NONE',  ( -1.092739197465703932E-16, 0.000000000000000000, 1.000000000000000000 ) ) ;
#87975 = ORIENTED_EDGE ( 'NONE', *, *, #40964, .T. ) ;
#87976 = PLANE ( 'NONE',  #44006 ) ;
#87977 = EDGE_CURVE ( 'NONE', #42544, #41323, #44388, .T. ) ;
#87978 = CARTESIAN_POINT ( 'NONE',  ( 116.3212776292296127, -32.94146857471318413, 287.6356252759109680 ) ) ;
#87979 = ADVANCED_FACE ( 'NONE', ( #10763 ), #9893, .T. ) ;
#87980 = CARTESIAN_POINT ( 'NONE',  ( 105.8009397366041497, -26.72383029953164524, 135.1771514046403411 ) ) ;
#87981 = ADVANCED_FACE ( 'NONE', ( #17156 ), #45712, .F. ) ;
#87982 = CARTESIAN_POINT ( 'NONE',  ( 176.5667039024390306, -48.82844715994099971, 249.9678068554149775 ) ) ;
#87984 = EDGE_LOOP ( 'NONE', ( #27119, #89804, #29910, #32504, #69121, #20846, #44494, #74506 ) ) ;
#87983 = CARTESIAN_POINT ( 'NONE',  ( 96.72907894039983034, -34.86132901292410224, 241.1841967044819626 ) ) ;
#87985 = CARTESIAN_POINT ( 'NONE',  ( 194.0371591254575776, -24.42818131005417115, 116.4678068554150201 ) ) ;
#87986 = CARTESIAN_POINT ( 'NONE',  ( 96.51501197915654018, -40.09867661842082498, 277.5603871806729899 ) ) ;
#87987 = CARTESIAN_POINT ( 'NONE',  ( 96.56348986465089013, -36.88801538493378018, 132.3384824187679669 ) ) ;
#87988 = ADVANCED_FACE ( 'NONE', ( #3961 ), #80725, .F. ) ;
#87989 = DIRECTION ( 'NONE',  ( 4.299999999999999979E-14, -1.000000000000000000, 4.400000000000000367E-29 ) ) ;
#87990 = CARTESIAN_POINT ( 'NONE',  ( 11.39408073823493872, 88.17482193101727717, -130.0579986637597187 ) ) ;
#87991 = AXIS2_PLACEMENT_3D ( 'NONE', #9068, #36768, #23600 ) ;
#87992 = CARTESIAN_POINT ( 'NONE',  ( 100.0252357601327589, 76.93632333215536789, -83.90387289223328082 ) ) ;
#87993 = PLANE ( 'NONE',  #39388 ) ;
#87994 = DIRECTION ( 'NONE',  ( 1.000000000000000078E-15, -1.000000000000000083E-30, -1.000000000000000000 ) ) ;
#87995 = VERTEX_POINT ( 'NONE', #66628 ) ;
#87996 = ORIENTED_EDGE ( 'NONE', *, *, #85239, .T. ) ;
#87997 = VERTEX_POINT ( 'NONE', #11681 ) ;
#87998 = ORIENTED_EDGE ( 'NONE', *, *, #18090, .F. ) ;
#87999 = CYLINDRICAL_SURFACE ( 'NONE', #30608, 81.91591158490091118 ) ;
#88000 = CARTESIAN_POINT ( 'NONE',  ( 97.37192905580968727, -32.85904099757684804, 37.02419670448292521 ) ) ;
#88001 = DIRECTION ( 'NONE',  ( 0.000000000000000000, 1.000000000000000000, 0.000000000000000000 ) ) ;
#88002 = CARTESIAN_POINT ( 'NONE',  ( 77.10595377993877264, -140.3990126765571631, 246.8970167045860080 ) ) ;
#88004 = CARTESIAN_POINT ( 'NONE',  ( 48.45959712127293528, -26.00627455219328610, 117.4678068554150485 ) ) ;
#88003 = CYLINDRICAL_SURFACE ( 'NONE', #74346, 4.762500000000002842 ) ;
#88005 = AXIS2_PLACEMENT_3D ( 'NONE', #25247, #87935, #81142 ) ;
#88006 = CARTESIAN_POINT ( 'NONE',  ( 110.1391594044062003, -28.21056625751448976, 249.2114674471249600 ) ) ;
#88007 = ORIENTED_EDGE ( 'NONE', *, *, #36104, .F. ) ;
#88008 = ORIENTED_EDGE ( 'NONE', *, *, #50859, .T. ) ;
#88009 = VERTEX_POINT ( 'NONE', #39374 ) ;
#88010 = VECTOR ( 'NONE', #57813, 1000.000000000000000 ) ;
#88011 = AXIS2_PLACEMENT_3D ( 'NONE', #52685, #59072, #30944 ) ;
#88012 = FACE_OUTER_BOUND ( 'NONE', #31718, .T. ) ;
#88013 = AXIS2_PLACEMENT_3D ( 'NONE', #40312, #54363, #61207 ) ;
#88014 = CARTESIAN_POINT ( 'NONE',  ( 115.9448851316561928, -41.40291037483353875, 183.4410333944183549 ) ) ;
#88015 = LINE ( 'NONE', #19867, #54200 ) ;
#88016 = DIRECTION ( 'NONE',  ( -0.000000000000000000, 1.000000000000000000, -0.000000000000000000 ) ) ;
#88017 = CARTESIAN_POINT ( 'NONE',  ( 114.7948027157550399, -42.07682430429896669, 9.788249972563944468 ) ) ;
#88018 = CARTESIAN_POINT ( 'NONE',  ( 41.56648329127398966, -27.82844715994070484, 198.9256252759119832 ) ) ;
#88019 = LINE ( 'NONE', #27578, #49113 ) ;
#88020 = CARTESIAN_POINT ( 'NONE',  ( 109.0793648114890715, -47.66380995969711876, 277.7213395616258822 ) ) ;
#88021 = CARTESIAN_POINT ( 'NONE',  ( 0.000000000000000000, 82.54999999999999716, 206.3750000000000000 ) ) ;
#88022 = ORIENTED_EDGE ( 'NONE', *, *, #6926, .F. ) ;
#88023 = CARTESIAN_POINT ( 'NONE',  ( 97.07198842992696086, -35.37925190007393894, 57.21895314611191452 ) ) ;
#88024 = VECTOR ( 'NONE', #86733, 1000.000000000000000 ) ;
#88025 = FACE_OUTER_BOUND ( 'NONE', #44567, .T. ) ;
#88026 = CARTESIAN_POINT ( 'NONE',  ( 98.55283614654496205, -38.28467619158744384, 49.30047132197196191 ) ) ;
#88027 = VECTOR ( 'NONE', #59780, 1000.000000000000000 ) ;
#88028 = ADVANCED_FACE ( 'NONE', ( #32104 ), #59799, .F. ) ;
#88029 = CARTESIAN_POINT ( 'NONE',  ( 136.5762189171834962, -17.60488046388850591, 7.068409955833985236 ) ) ;
#88030 = ADVANCED_FACE ( 'NONE', ( #46166, #67079, #13912, #41592, #26196, #18934 ), #40260, .F. ) ;
#88031 = DIRECTION ( 'NONE',  ( 0.000000000000000000, -1.000000000000000000, 0.000000000000000000 ) ) ;
#88032 = B_SPLINE_CURVE_WITH_KNOTS ( 'NONE', 3,
 ( #76472, #14254, #42377, #7880 ),
 .UNSPECIFIED., .F., .F.,
 ( 4, 4 ),
 ( -0.3974825557268100162, -0.3842043193313829930 ),
 .UNSPECIFIED. ) ;
#88033 = CARTESIAN_POINT ( 'NONE',  ( 113.1781950736253748, -44.75194242080101503, 194.0939235927813513 ) ) ;
#88034 = VERTEX_POINT ( 'NONE', #53869 ) ;
#88035 = LINE ( 'NONE', #74400, #11721 ) ;
#88036 = EDGE_CURVE ( 'NONE', #69124, #66137, #69325, .T. ) ;
#88037 = CARTESIAN_POINT ( 'NONE',  ( 124.6708304737691719, 58.27461704503507889, -38.75682993913466134 ) ) ;
#88038 = EDGE_LOOP ( 'NONE', ( #69278, #64561 ) ) ;
#88039 = CARTESIAN_POINT ( 'NONE',  ( 104.1077555235347631, -46.72609462085661391, 107.3470538473389411 ) ) ;
#88040 = EDGE_LOOP ( 'NONE', ( #43791, #44243, #3832, #4712 ) ) ;
#88041 = B_SPLINE_CURVE_WITH_KNOTS ( 'NONE', 3,
 ( #26445, #40059, #18732, #11924, #67318, #26000, #53669, #81436, #46858, #67777, #74590, #5566, #33258, #54118, #17399, #65976, #31456, #59161, #19625, #35484, #6891, #69126, #6448, #55010, #68680, #48653, #76384, #12831, #47312, #41397, #14619 ),
 .UNSPECIFIED., .F., .F.,
 ( 4, 2, 2, 2, 2, 2, 2, 2, 2, 2, 1, 1, 1, 1, 1, 1, 1, 2, 4 ),
 ( 0.000000000000000000, 0.06250382389165948238, 0.1250076477833189648, 0.1875114716749784471, 0.2500152955666379295, 0.3125191194582974119, 0.3750229433499568943, 0.4375267672416163767, 0.4687786791874462566, 0.4844046351603611411, 0.4922176131468187776, 0.4961241021400474849, 0.4980773466366619773, 0.4990539688849690014, 0.4995422800091225413, 0.4997864355711990614, 0.4999085133522373492, 0.4999695522427566319, 0.5000305911332758591 ),
 .UNSPECIFIED. ) ;
#88042 = CARTESIAN_POINT ( 'NONE',  ( 108.6385355886969108, -45.12496878139073431, 82.14670554236298017 ) ) ;
#88043 = EDGE_CURVE ( 'NONE', #39062, #2317, #41149, .T. ) ;
#88044 = CARTESIAN_POINT ( 'NONE',  ( 98.98640610341819013, -42.64021795225433209, 87.82849860576001788 ) ) ;
#88045 = CARTESIAN_POINT ( 'NONE',  ( 97.22447099779657265, -34.58340453033963513, 102.5872975916109482 ) ) ;
#88046 = EDGE_CURVE ( 'NONE', #33376, #39081, #34794, .T. ) ;
#88047 = DIRECTION ( 'NONE',  ( -0.5000000000000008882, 0.8660254037844382635, -2.684678751731760294E-14 ) ) ;
#88048 = CARTESIAN_POINT ( 'NONE',  ( 143.2705975587811906, -69.15250645760630732, 247.4440349298869819 ) ) ;
#88049 = CARTESIAN_POINT ( 'NONE',  ( 99.48587976144928291, -43.91775078298940116, 77.92991099019597812 ) ) ;
#88050 = AXIS2_PLACEMENT_3D ( 'NONE', #600, #22860, #29219 ) ;
#88052 = EDGE_CURVE ( 'NONE', #32467, #59850, #34341, .T. ) ;
#88051 = CARTESIAN_POINT ( 'NONE',  ( 112.1398324001274887, -28.01310167226245085, 180.6568491273569350 ) ) ;
#88053 = ORIENTED_EDGE ( 'NONE', *, *, #17243, .T. ) ;
#88054 = DIRECTION ( 'NONE',  ( 1.000000000000000000, 0.000000000000000000, 0.000000000000000000 ) ) ;
#88055 = ORIENTED_EDGE ( 'NONE', *, *, #4776, .T. ) ;
#88056 = CARTESIAN_POINT ( 'NONE',  ( -118.5214188546241445, 70.17671898886894155, -2.891923471343901930 ) ) ;
#88057 = VERTEX_POINT ( 'NONE', #47057 ) ;
#88058 = EDGE_LOOP ( 'NONE', ( #89631, #32161, #10701, #25569 ) ) ;
#88059 = EDGE_CURVE ( 'NONE', #72562, #17905, #2770, .T. ) ;
#88060 = PLANE ( 'NONE',  #65884 ) ;
#88061 = ORIENTED_EDGE ( 'NONE', *, *, #8475, .F. ) ;
#88062 = CARTESIAN_POINT ( 'NONE',  ( 104.4938967476557536, -26.68352342390101128, 245.2880062282919482 ) ) ;
#88063 = CARTESIAN_POINT ( 'NONE',  ( 113.7362177204465041, -29.20338847083969114, 124.4983641739881506 ) ) ;
#88064 = CARTESIAN_POINT ( 'NONE',  ( 75.61066417432020614, 20.32000000000000028, 177.0380000000000109 ) ) ;
#88065 = CARTESIAN_POINT ( 'NONE',  ( 117.4876440797474828, -37.01562065295904347, 39.80419670448193159 ) ) ;
#88066 = EDGE_CURVE ( 'NONE', #67042, #75662, #13026, .T. ) ;
#88067 = CARTESIAN_POINT ( 'NONE',  ( 107.0664832912739968, -36.72944715994100306, 394.9756252759102040 ) ) ;
#88068 = EDGE_LOOP ( 'NONE', ( #42393, #58216, #44585, #82200 ) ) ;
#88069 = CARTESIAN_POINT ( 'NONE',  ( 116.3212776292296127, -32.94146857471318413, 287.6356252759109680 ) ) ;
#88070 = VECTOR ( 'NONE', #44734, 999.9999999999998863 ) ;
#88071 = CIRCLE ( 'NONE', #21346, 0.5000000000000004441 ) ;
#88072 = CARTESIAN_POINT ( 'NONE',  ( 182.5667039024469886, -33.35206098992650681, -5.074374724088000832 ) ) ;
#88073 = ORIENTED_EDGE ( 'NONE', *, *, #65643, .T. ) ;
#88074 = CIRCLE ( 'NONE', #9748, 4.875000000000017764 ) ;
#88075 = CARTESIAN_POINT ( 'NONE',  ( 138.8545562996767444, -1.932463243632620342, 361.9756252759100335 ) ) ;
#88076 = VECTOR ( 'NONE', #82437, 1000.000000000000000 ) ;
#88077 = DIRECTION ( 'NONE',  ( -0.0001211784769804366042, 0.7071067708032299226, 0.7071067811865512365 ) ) ;
#88078 = CARTESIAN_POINT ( 'NONE',  ( 116.2977993645976227, -41.52656014244018223, 288.4441967044823514 ) ) ;
#88079 = DIRECTION ( 'NONE',  ( 0.7071067811868710917, -0.7071067811862240537, 0.000000000000000000 ) ) ;
#88080 = CIRCLE ( 'NONE', #72134, 4.875000000000017764 ) ;
#88081 = LINE ( 'NONE', #53962, #73825 ) ;
#88082 = CARTESIAN_POINT ( 'NONE',  ( 97.81375517989221180, -40.51659548082960072, 91.63516306087667829 ) ) ;
#88083 = CARTESIAN_POINT ( 'NONE',  ( 98.62497865991430501, -35.42670724699001283, 265.6267055423624583 ) ) ;
#88085 = CARTESIAN_POINT ( 'NONE',  ( 96.10063762778156615, -37.91858611869021445, 77.40038718067299328 ) ) ;
#88084 = DIRECTION ( 'NONE',  ( -1.000000000000000000, 0.000000000000000000, 0.000000000000000000 ) ) ;
#88086 = CARTESIAN_POINT ( 'NONE',  ( 115.9477166093867595, 72.45386989696044111, 60.01166189639659621 ) ) ;
#88087 = CARTESIAN_POINT ( 'NONE',  ( 114.5591802247839865, -28.54312911867770808, 154.4746728949589851 ) ) ;
#88088 = ORIENTED_EDGE ( 'NONE', *, *, #62139, .F. ) ;
#88089 = DIRECTION ( 'NONE',  ( 1.000000000000000078E-15, -1.000000000000000083E-30, -1.000000000000000000 ) ) ;
#88090 = ORIENTED_EDGE ( 'NONE', *, *, #36008, .F. ) ;
#88091 = B_SPLINE_CURVE_WITH_KNOTS ( 'NONE', 3,
 ( #27797, #84581, #75956, #22341, #15531, #43204, #62315, #99, #64123, #23256, #44990, #86356, #71395, #37756, #72279, #1893, #29592, #31368, #52233, #58189, #79549, #57741, #71830, #2345, #8721, #24126, #86798, #51798, #65454, #17311, #64566, #78669, #10049, #72720, #16419, #30048, #57283, #79996 ),
 .UNSPECIFIED., .F., .F.,
 ( 4, 2, 2, 2, 2, 2, 2, 2, 2, 2, 2, 2, 2, 2, 2, 2, 2, 2, 4 ),
 ( 0.000000000000000000, 0.0009358755680944266103, 0.001871751136188853221, 0.002807626704283279831, 0.003743502272377706441, 0.004679377840472133052, 0.005615253408566559662, 0.006083191192613696639, 0.006551128976660833617, 0.007487004544755115377, 0.008422880112849397138, 0.009358755680943678032, 0.01029463124903796066, 0.01123050681713224155, 0.01216638238522652592, 0.01310225795332080681, 0.01403813352141508944, 0.01450607130546224983, 0.01497400908950941197 ),
 .UNSPECIFIED. ) ;
#88092 = DIRECTION ( 'NONE',  ( 0.000000000000000000, 0.000000000000000000, 1.000000000000000000 ) ) ;
#88093 = CARTESIAN_POINT ( 'NONE',  ( 29.56648329127400388, 25.62155284005901379, 323.8756252759109202 ) ) ;
#88094 = PRODUCT_DEFINITION_SHAPE ( 'NONE', 'NONE',  #32744 ) ;
#88095 = CARTESIAN_POINT ( 'NONE',  ( 134.4427611689536093, -33.99866847873244069, 1.641799428525427151 ) ) ;
#88096 = ORIENTED_EDGE ( 'NONE', *, *, #53097, .F. ) ;
#88097 = EDGE_CURVE ( 'NONE', #24965, #73817, #10026, .T. ) ;
#88098 = DIRECTION ( 'NONE',  ( -9.351236661543306751E-17, 3.725950533538267165E-29, 1.000000000000000000 ) ) ;
#88100 = ORIENTED_EDGE ( 'NONE', *, *, #3317, .T. ) ;
#88099 = CARTESIAN_POINT ( 'NONE',  ( 114.5437501075917481, -29.39581020157643110, 149.4441967044819819 ) ) ;
#88102 = CARTESIAN_POINT ( 'NONE',  ( 71.06648329127399677, -18.82844715994099971, 323.8756252759120002 ) ) ;
#88101 = UNCERTAINTY_MEASURE_WITH_UNIT (LENGTH_MEASURE( 1.000000000000000082E-05 ), #63280, 'distance_accuracy_value', 'NONE');
#88103 = CIRCLE ( 'NONE', #48896, 3.174999999999983391 ) ;
#88104 = ADVANCED_FACE ( 'NONE', ( #33001 ), #88884, .T. ) ;
#88105 = DIRECTION ( 'NONE',  ( -2.279500465453769633E-16, 0.000000000000000000, 1.000000000000000000 ) ) ;
#88106 = CIRCLE ( 'NONE', #66288, 3.500000000000003109 ) ;
#88107 = CARTESIAN_POINT ( 'NONE',  ( 99.90204555947735798, -107.8376143137176939, -19.78219314458190681 ) ) ;
#88108 = DIRECTION ( 'NONE',  ( 0.1811243268507065352, -0.9834602067307444129, 0.000000000000000000 ) ) ;
#88109 = ORIENTED_EDGE ( 'NONE', *, *, #14206, .T. ) ;
#88110 = CIRCLE ( 'NONE', #75057, 11.45913725231036118 ) ;
#88111 = APPLICATION_PROTOCOL_DEFINITION ( 'draft international standard', 'automotive_design', 1998, #85250 ) ;
#88112 = DIRECTION ( 'NONE',  ( -1.000000000000000078E-15, 1.000000000000000083E-30, 1.000000000000000000 ) ) ;
#88113 = CARTESIAN_POINT ( 'NONE',  ( 41.56648329127381203, -27.82844715994070484, 81.92562527591199739 ) ) ;
#88114 = ORIENTED_EDGE ( 'NONE', *, *, #64916, .F. ) ;
#88115 = ORIENTED_EDGE ( 'NONE', *, *, #19617, .F. ) ;
#88116 = PLANE ( 'NONE',  #71351 ) ;
#88117 = DIRECTION ( 'NONE',  ( -1.000000000000000000, -8.953411488912552682E-16, 0.000000000000000000 ) ) ;
#88118 = FACE_OUTER_BOUND ( 'NONE', #85147, .T. ) ;
#88119 = DIRECTION ( 'NONE',  ( -3.100000000000000258E-29, 3.100000000000000044E-14, 1.000000000000000000 ) ) ;
#88121 = DIRECTION ( 'NONE',  ( -1.000000000000000000, 0.000000000000000000, 0.000000000000000000 ) ) ;
#88120 = CARTESIAN_POINT ( 'NONE',  ( 115.0886908286442605, -30.61735931247813625, 104.3439862672049969 ) ) ;
#88122 = FACE_OUTER_BOUND ( 'NONE', #1721, .T. ) ;
#88123 = VECTOR ( 'NONE', #12634, 999.9999999999998863 ) ;
#88124 = VECTOR ( 'NONE', #46514, 1000.000000000000114 ) ;
#88125 = EDGE_CURVE ( 'NONE', #1395, #62569, #74349, .T. ) ;
#88126 = VERTEX_POINT ( 'NONE', #40710 ) ;
#88127 = DIRECTION ( 'NONE',  ( 0.000000000000000000, 0.000000000000000000, -1.000000000000000000 ) ) ;
#88128 = CARTESIAN_POINT ( 'NONE',  ( 102.5357197525642192, -45.39752751535328201, 208.1927681330529651 ) ) ;
#88130 = ORIENTED_EDGE ( 'NONE', *, *, #5270, .F. ) ;
#88129 = DIRECTION ( 'NONE',  ( 0.000000000000000000, -1.000000000000000000, 0.000000000000000000 ) ) ;
#88131 = CARTESIAN_POINT ( 'NONE',  ( 96.07333748454176714, -35.06730156692550793, 67.20705384733894050 ) ) ;
#88132 = CARTESIAN_POINT ( 'NONE',  ( 115.0672684967225479, -42.78377500417700929, 53.31083235052207669 ) ) ;
#88133 = DIRECTION ( 'NONE',  ( 0.000000000000000000, 1.000000000000000000, 0.000000000000000000 ) ) ;
#88134 = DIRECTION ( 'NONE',  ( -1.346944695195362088E-15, 1.000000000000000000, -3.469446951953620425E-31 ) ) ;
#88135 = ORIENTED_EDGE ( 'NONE', *, *, #38969, .T. ) ;
#88136 = LINE ( 'NONE', #12267, #21160 ) ;
#88137 = VECTOR ( 'NONE', #67490, 1000.000000000000114 ) ;
#88138 = ORIENTED_EDGE ( 'NONE', *, *, #25897, .T. ) ;
#88139 = ORIENTED_EDGE ( 'NONE', *, *, #25806, .T. ) ;
#88140 = EDGE_CURVE ( 'NONE', #89690, #54987, #53417, .T. ) ;
#88141 = CARTESIAN_POINT ( 'NONE',  ( 112.1951879357659152, -44.60173489647391420, 219.4796785439919802 ) ) ;
#88142 = CIRCLE ( 'NONE', #33016, 15.50000000000000000 ) ;
#88143 = CARTESIAN_POINT ( 'NONE',  ( 97.86646836935159399, -40.64896943459201140, 52.64654800080118235 ) ) ;
#88144 = VECTOR ( 'NONE', #23743, 1000.000000000000000 ) ;
#88145 = CARTESIAN_POINT ( 'NONE',  ( -117.8914297010765324, 84.62843115047674303, -12.53565398905618977 ) ) ;
#88146 = EDGE_CURVE ( 'NONE', #70996, #45346, #33227, .T. ) ;
#88147 = ADVANCED_FACE ( 'NONE', ( #81185 ), #67523, .F. ) ;
#88148 = CARTESIAN_POINT ( 'NONE',  ( 69.26949937496598864, -71.54137415153812185, 361.9756252759101471 ) ) ;
#88149 = FACE_OUTER_BOUND ( 'NONE', #57317, .T. ) ;
#88150 = ORIENTED_EDGE ( 'NONE', *, *, #26302, .T. ) ;
#88151 = DIRECTION ( 'NONE',  ( 1.000000000000000000, 0.000000000000000000, 1.472650733923983947E-14 ) ) ;
#88153 = EDGE_CURVE ( 'NONE', #12031, #78421, #54911, .T. ) ;
#88152 = CIRCLE ( 'NONE', #6956, 0.5000000000000007772 ) ;
#88154 = CARTESIAN_POINT ( 'NONE',  ( 115.0821730991288376, -30.60891592853656817, 35.34399340870037065 ) ) ;
#88155 = ORIENTED_EDGE ( 'NONE', *, *, #80064, .F. ) ;
#88156 = CARTESIAN_POINT ( 'NONE',  ( 111.4155313275575168, -46.20429869645016652, 27.91848241876792969 ) ) ;
#88157 = VERTEX_POINT ( 'NONE', #47958 ) ;
#88158 = ORIENTED_EDGE ( 'NONE', *, *, #22683, .F. ) ;
#88159 = CARTESIAN_POINT ( 'NONE',  ( 99.00663190570655559, -35.27291570150341471, 239.0023760838769817 ) ) ;
#88160 = VECTOR ( 'NONE', #41683, 1000.000000000000000 ) ;
#88161 = DIRECTION ( 'NONE',  ( 1.694150445170956262E-15, 0.000000000000000000, 1.000000000000000000 ) ) ;
#88162 = CARTESIAN_POINT ( 'NONE',  ( 105.8036208730406003, -25.68330614323999228, 160.1670538473399574 ) ) ;
#88163 = CARTESIAN_POINT ( 'NONE',  ( 23.03808826316528169, 77.78751545737644335, 303.0524246975253959 ) ) ;
#88164 = DIRECTION ( 'NONE',  ( -1.000000000000000000, -3.360405532702990443E-14, 0.000000000000000000 ) ) ;
#88165 = AXIS2_PLACEMENT_3D ( 'NONE', #86799, #73149, #30493 ) ;
#88166 = LINE ( 'NONE', #47236, #57905 ) ;
#88167 = AXIS2_PLACEMENT_3D ( 'NONE', #28507, #63486, #34881 ) ;
#88168 = CARTESIAN_POINT ( 'NONE',  ( 118.8391071721064662, -38.46623720595516005, 219.7099109901969882 ) ) ;
#88169 = CARTESIAN_POINT ( 'NONE',  ( 90.32698471909186821, 90.93965867633431799, -76.79137032886062286 ) ) ;
#88171 = EDGE_CURVE ( 'NONE', #53148, #79585, #75696, .T. ) ;
#88170 = VECTOR ( 'NONE', #10368, 1000.000000000000000 ) ;
#88172 = VERTEX_POINT ( 'NONE', #6647 ) ;
#88173 = CARTESIAN_POINT ( 'NONE',  ( 115.3013748915712711, -44.17149383341634206, 79.25372051400697160 ) ) ;
#88174 = DIRECTION ( 'NONE',  ( 0.000000000000000000, 0.000000000000000000, -1.000000000000000000 ) ) ;
#88175 = ORIENTED_EDGE ( 'NONE', *, *, #66836, .T. ) ;
#88176 = VERTEX_POINT ( 'NONE', #82973 ) ;
#88177 = ORIENTED_EDGE ( 'NONE', *, *, #62063, .F. ) ;
#88178 = EDGE_CURVE ( 'NONE', #79094, #40277, #20726, .T. ) ;
#88179 = DIRECTION ( 'NONE',  ( 0.000000000000000000, -1.000000000000000000, 0.000000000000000000 ) ) ;
#88180 = DIRECTION ( 'NONE',  ( 0.000000000000000000, 0.000000000000000000, 1.000000000000000000 ) ) ;
#88181 = CARTESIAN_POINT ( 'NONE',  ( 109.6408758491008655, -46.48062444223011624, 152.7819551027729688 ) ) ;
#88182 = CARTESIAN_POINT ( 'NONE',  ( 102.2276451341571999, -43.90295244235954897, 149.9099951314959753 ) ) ;
#88183 = CARTESIAN_POINT ( 'NONE',  ( 113.8133276556114595, -26.95691720032833416, 235.5956252759109759 ) ) ;
#88184 = EDGE_CURVE ( 'NONE', #68410, #75721, #17222, .T. ) ;
#88185 = DIRECTION ( 'NONE',  ( 0.000000000000000000, 1.000000000000000000, 0.000000000000000000 ) ) ;
#88186 = ORIENTED_EDGE ( 'NONE', *, *, #6318, .F. ) ;
#88187 = SURFACE_STYLE_USAGE ( .BOTH. , #81378 ) ;
#88188 = LINE ( 'NONE', #24165, #66484 ) ;
#88189 = ORIENTED_EDGE ( 'NONE', *, *, #24809, .T. ) ;
#88191 = ORIENTED_EDGE ( 'NONE', *, *, #16027, .T. ) ;
#88190 = CIRCLE ( 'NONE', #62032, 9.000000000000007105 ) ;
#88192 = LINE ( 'NONE', #81383, #47411 ) ;
#88193 = VERTEX_POINT ( 'NONE', #83862 ) ;
#88194 = ORIENTED_EDGE ( 'NONE', *, *, #20668, .F. ) ;
#88195 = DIRECTION ( 'NONE',  ( 0.000000000000000000, -1.000000000000000000, 0.000000000000000000 ) ) ;
#88196 = PLANE ( 'NONE',  #41342 ) ;
#88197 = CARTESIAN_POINT ( 'NONE',  ( 0.000000000000000000, 239.0000000000000000, 159.6557476874258441 ) ) ;
#88198 = CARTESIAN_POINT ( 'NONE',  ( 103.6069473157389922, -44.53891209398362605, 176.6667055423629620 ) ) ;
#88199 = CARTESIAN_POINT ( 'NONE',  ( 115.4801557161918311, -43.01927310766588874, 28.31562527591097123 ) ) ;
#88200 = ORIENTED_EDGE ( 'NONE', *, *, #13290, .F. ) ;
#88201 = DIRECTION ( 'NONE',  ( -1.000000000000000000, -1.000000000000000078E-15, -0.000000000000000000 ) ) ;
#88202 = EDGE_LOOP ( 'NONE', ( #24538, #36989, #89602, #28542 ) ) ;
#88203 = DIRECTION ( 'NONE',  ( -0.9217329428042198014, -0.3878251953515564066, 1.214306433183767175E-14 ) ) ;
#88204 = ORIENTED_EDGE ( 'NONE', *, *, #32975, .F. ) ;
#88205 = PLANE ( 'NONE',  #25837 ) ;
#88206 = ORIENTED_EDGE ( 'NONE', *, *, #14633, .T. ) ;
#88207 = CARTESIAN_POINT ( 'NONE',  ( 100.7142663445133763, -28.97135979089331315, 166.6218790464526194 ) ) ;
#88208 = CIRCLE ( 'NONE', #72249, 3.299999999999997158 ) ;
#88209 = CARTESIAN_POINT ( 'NONE',  ( -10.01853500445675671, 74.86481845265393531, 118.1328220722729441 ) ) ;
#88210 = ADVANCED_FACE ( 'NONE', ( #35236, #29783 ), #63401, .F. ) ;
#88211 = CARTESIAN_POINT ( 'NONE',  ( 110.8533328532906665, -45.98470352573126974, 132.8855273142165458 ) ) ;
#88213 = CARTESIAN_POINT ( 'NONE',  ( -33.98325472291465132, 104.3431970271541900, 3.174999999999764899 ) ) ;
#88212 = AXIS2_PLACEMENT_3D ( 'NONE', #58273, #8351, #63308 ) ;
#88214 = ORIENTED_EDGE ( 'NONE', *, *, #60790, .T. ) ;
#88215 = VECTOR ( 'NONE', #31454, 1000.000000000000000 ) ;
#88216 = CARTESIAN_POINT ( 'NONE',  ( 117.4065409050533617, -38.22262247076111663, 28.71276813305395592 ) ) ;
#88217 = CARTESIAN_POINT ( 'NONE',  ( 112.7836381133937067, -27.91740111342080866, 65.61848241876793963 ) ) ;
#88219 = DIRECTION ( 'NONE',  ( 0.000000000000000000, 0.000000000000000000, 1.000000000000000000 ) ) ;
#88218 = LINE ( 'NONE', #47292, #36125 ) ;
#88220 = CYLINDRICAL_SURFACE ( 'NONE', #71367, 0.2500000000000046074 ) ;
#88221 = DIRECTION ( 'NONE',  ( 0.000000000000000000, 0.000000000000000000, -1.000000000000000000 ) ) ;
#88222 = AXIS2_PLACEMENT_3D ( 'NONE', #80904, #81359, #39984 ) ;
#88223 = CARTESIAN_POINT ( 'NONE',  ( 99.32888008572089689, -30.27953731386449476, 121.7710324745360566 ) ) ;
#88224 = CIRCLE ( 'NONE', #47594, 0.4999999999999933387 ) ;
#88225 = CARTESIAN_POINT ( 'NONE',  ( 72.96458098368701428, 127.0000000000000000, -72.96458098368670164 ) ) ;
#88226 = VERTEX_POINT ( 'NONE', #49309 ) ;
#88227 = ADVANCED_FACE ( 'NONE', ( #36608 ), #43389, .T. ) ;
#88228 = CARTESIAN_POINT ( 'NONE',  ( 117.9706719164645250, -41.49678058079525300, 58.49848241876792798 ) ) ;
#88229 = CARTESIAN_POINT ( 'NONE',  ( 96.64436219916188975, -36.48069147925158262, 192.3070538473399438 ) ) ;
#88230 = CARTESIAN_POINT ( 'NONE',  ( 116.5531001583795216, -32.35436324414348519, 100.1699109901969535 ) ) ;
#88231 = AXIS2_PLACEMENT_3D ( 'NONE', #40862, #46321, #89481 ) ;
#88232 = CIRCLE ( 'NONE', #5486, 3.250000000000002665 ) ;
#88234 = CARTESIAN_POINT ( 'NONE',  ( 118.4837085360594671, -37.70862757085654238, 300.2406250056037038 ) ) ;
#88233 = CARTESIAN_POINT ( 'NONE',  ( 113.1798327254349346, -44.75071842742295303, 173.0900461106986086 ) ) ;
#88235 = LINE ( 'NONE', #18722, #19035 ) ;
#88236 = EDGE_CURVE ( 'NONE', #3377, #1830, #2078, .T. ) ;
#88237 = FACE_OUTER_BOUND ( 'NONE', #11529, .T. ) ;
#88238 = ORIENTED_EDGE ( 'NONE', *, *, #24595, .F. ) ;
#88239 = CARTESIAN_POINT ( 'NONE',  ( 112.1775644307543587, -28.39036538331633963, 90.63848241876793566 ) ) ;
#88240 = CIRCLE ( 'NONE', #47616, 13.09746158385919124 ) ;
#88242 = ORIENTED_EDGE ( 'NONE', *, *, #24672, .F. ) ;
#88241 = DIRECTION ( 'NONE',  ( -0.9130365726098600421, 0.000000000000000000, -0.4078776986755216494 ) ) ;
#88243 = CARTESIAN_POINT ( 'NONE',  ( 106.5683798796750779, -47.15615894637585370, 243.5384824187679556 ) ) ;
#88244 = DIRECTION ( 'NONE',  ( -0.04216478779797398074, 0.9991106698809455455, 0.000000000000000000 ) ) ;
#88245 = CARTESIAN_POINT ( 'NONE',  ( 116.3423118429748797, -40.59191411747055156, 148.5122355737231317 ) ) ;
#88246 = DIRECTION ( 'NONE',  ( 0.000000000000000000, 0.000000000000000000, 1.000000000000000000 ) ) ;
#88247 = DIRECTION ( 'NONE',  ( -0.000000000000000000, 1.000000000000000000, 0.000000000000000000 ) ) ;
#88248 = CARTESIAN_POINT ( 'NONE',  ( 132.2214349158035418, -38.77077206072119964, 2.188418444516419203 ) ) ;
#88249 = CARTESIAN_POINT ( 'NONE',  ( -29.99999999999998224, 171.0000000000000000, 113.8826257785461280 ) ) ;
#88250 = CARTESIAN_POINT ( 'NONE',  ( 112.4269750522866502, -44.91043508143939533, 178.0384824187689503 ) ) ;
#88251 = AXIS2_PLACEMENT_3D ( 'NONE', #51915, #71956, #65129 ) ;
#88252 = ORIENTED_EDGE ( 'NONE', *, *, #63417, .T. ) ;
#88253 = ORIENTED_EDGE ( 'NONE', *, *, #71445, .T. ) ;
#88254 = VECTOR ( 'NONE', #8361, 1000.000000000000000 ) ;
#88255 = CARTESIAN_POINT ( 'NONE',  ( 103.7844689056781675, -44.99325446404193940, 113.7072975916109669 ) ) ;
#88256 = DIRECTION ( 'NONE',  ( 0.000000000000000000, 0.000000000000000000, -1.000000000000000000 ) ) ;
#88258 = DIRECTION ( 'NONE',  ( 0.000000000000000000, 1.000000000000000000, 0.000000000000000000 ) ) ;
#88257 = CARTESIAN_POINT ( 'NONE',  ( 97.54182784564409303, -34.36413255805981493, 272.1327681330532755 ) ) ;
#88259 = CARTESIAN_POINT ( 'NONE',  ( 92.17622411536551397, -83.77844715994095282, 55.21780685541800437 ) ) ;
#88260 = ADVANCED_FACE ( 'NONE', ( #71130 ), #57021, .T. ) ;
#88261 = DIRECTION ( 'NONE',  ( 0.7071067811865489050, -0.7071067811865462405, 0.000000000000000000 ) ) ;
#88262 = CARTESIAN_POINT ( 'NONE',  ( 107.0664832912739399, -36.72944715994095333, 293.6356252759109680 ) ) ;
#88263 = CARTESIAN_POINT ( 'NONE',  ( 188.5667039024484382, -42.82844715993430640, 175.7178068554150343 ) ) ;
#88264 = EDGE_CURVE ( 'NONE', #47173, #18138, #36146, .T. ) ;
#88265 = PLANE ( 'NONE',  #58866 ) ;
#88266 = CARTESIAN_POINT ( 'NONE',  ( 115.0229693000241156, -29.09019634776596419, 189.4232443235299570 ) ) ;
#88267 = DIRECTION ( 'NONE',  ( 1.000000000000000000, 3.651563665954189830E-16, 0.000000000000000000 ) ) ;
#88268 = VERTEX_POINT ( 'NONE', #14821 ) ;
#88269 = ORIENTED_EDGE ( 'NONE', *, *, #73346, .F. ) ;
#88270 = VECTOR ( 'NONE', #86085, 1000.000000000000000 ) ;
#88271 = ADVANCED_FACE ( 'NONE', ( #9335 ), #8907, .F. ) ;
#88272 = CARTESIAN_POINT ( 'NONE',  ( -99.33321048326486391, 75.15271101351808625, -84.72210942531944511 ) ) ;
#88273 = CARTESIAN_POINT ( 'NONE',  ( 78.92334784197174713, -16.22821065591839584, 1.829869330582365228 ) ) ;
#88274 = DIRECTION ( 'NONE',  ( 0.000000000000000000, 0.000000000000000000, 1.000000000000000000 ) ) ;
#88275 = CARTESIAN_POINT ( 'NONE',  ( 172.5664832912740110, -36.32844715994070839, 254.1756252759120400 ) ) ;
#88277 = CARTESIAN_POINT ( 'NONE',  ( 163.1543517358360020, -31.62489322948790971, 193.9678068554150059 ) ) ;
#88276 = AXIS2_PLACEMENT_3D ( 'NONE', #25432, #44972, #37283 ) ;
#88278 = ORIENTED_EDGE ( 'NONE', *, *, #3570, .T. ) ;
#88279 = CIRCLE ( 'NONE', #21481, 11.45913725231036118 ) ;
#88280 = DIRECTION ( 'NONE',  ( -0.9254794337955620787, -0.3787978585227822492, 0.000000000000000000 ) ) ;
#88281 = CARTESIAN_POINT ( 'NONE',  ( 110.2559530472221923, -26.76685766971437630, 234.8299109901969643 ) ) ;
#88282 = CARTESIAN_POINT ( 'NONE',  ( 135.3099415725499455, -39.18303583363249487, 7.982915248815769971 ) ) ;
#88283 = VERTEX_POINT ( 'NONE', #28892 ) ;
#88284 = ADVANCED_FACE ( 'NONE', ( #42489 ), #50658, .T. ) ;
#88285 = AXIS2_PLACEMENT_3D ( 'NONE', #13630, #41315, #34512 ) ;
#88286 = CARTESIAN_POINT ( 'NONE',  ( -6.314145302152993189, 93.48478343411423452, 118.3897254880733669 ) ) ;
#88287 = CARTESIAN_POINT ( 'NONE',  ( 107.0667039024479834, -48.82844715994099971, 160.9178068554150229 ) ) ;
#88288 = FACE_OUTER_BOUND ( 'NONE', #40295, .T. ) ;
#88289 = CARTESIAN_POINT ( 'NONE',  ( 100.8021347340043690, -42.70095134221056554, 34.73856656006796584 ) ) ;
#88291 = CARTESIAN_POINT ( 'NONE',  ( 97.72691728231733066, -42.68408598780226271, 137.7661014663869992 ) ) ;
#88290 = CIRCLE ( 'NONE', #49088, 3.000000000000002665 ) ;
#88292 = DIRECTION ( 'NONE',  ( 0.000000000000000000, 0.000000000000000000, -1.000000000000000000 ) ) ;
#88293 = EDGE_LOOP ( 'NONE', ( #23702, #80151, #31703, #48788 ) ) ;
#88294 = VECTOR ( 'NONE', #78618, 1000.000000000000000 ) ;
#88295 = DIRECTION ( 'NONE',  ( 0.000000000000000000, -1.000000000000000000, 0.000000000000000000 ) ) ;
#88296 = CARTESIAN_POINT ( 'NONE',  ( 144.0637245237351749, -140.6784087391956746, 245.5331728883010101 ) ) ;
#88297 = EDGE_LOOP ( 'NONE', ( #76345, #24693 ) ) ;
#88298 = ORIENTED_EDGE ( 'NONE', *, *, #3051, .F. ) ;
#88299 = CARTESIAN_POINT ( 'NONE',  ( -31.75000000000000000, 104.3431970271541900, -3.175000000000219647 ) ) ;
#88300 = ORIENTED_EDGE ( 'NONE', *, *, #80669, .T. ) ;
#88301 = ORIENTED_EDGE ( 'NONE', *, *, #1538, .F. ) ;
#88302 = LINE ( 'NONE', #74651, #60283 ) ;
#88303 = CARTESIAN_POINT ( 'NONE',  ( 102.2116477823090293, -29.08462914334738869, 64.93718173283896533 ) ) ;
#88304 = CARTESIAN_POINT ( 'NONE',  ( 95.38311866650811055, -38.85853310224461410, 201.4699109901969791 ) ) ;
#88305 = CARTESIAN_POINT ( 'NONE',  ( 113.6005200848514676, -45.61596423689133672, 183.0689586092439640 ) ) ;
#88307 = CARTESIAN_POINT ( 'NONE',  ( 118.3409026158823281, -33.07932318167559060, 280.0756252759109657 ) ) ;
#88306 = CARTESIAN_POINT ( 'NONE',  ( 77.31648329127399677, -18.72944715994106346, -5.074374724089059541 ) ) ;
#88308 = FACE_OUTER_BOUND ( 'NONE', #89198, .T. ) ;
#88309 = CARTESIAN_POINT ( 'NONE',  ( -479.3614999999999782, 97.78694598552370110, 18.25625000000050235 ) ) ;
#88310 = ORIENTED_EDGE ( 'NONE', *, *, #84507, .T. ) ;
#88311 = EDGE_LOOP ( 'NONE', ( #82465, #47183, #55269, #20235 ) ) ;
#88312 = EDGE_CURVE ( 'NONE', #49237, #24886, #35550, .T. ) ;
#88313 = VECTOR ( 'NONE', #86682, 1000.000000000000000 ) ;
#88314 = DIRECTION ( 'NONE',  ( 0.000000000000000000, -1.000000000000000000, 0.000000000000000000 ) ) ;
#88315 = CARTESIAN_POINT ( 'NONE',  ( 100.6103855434584631, -26.73206753375993827, 220.5327681330539633 ) ) ;
#88316 = ORIENTED_EDGE ( 'NONE', *, *, #68053, .F. ) ;
#88317 = CARTESIAN_POINT ( 'NONE',  ( 103.3034881226635946, -27.00695273605797908, 215.3699109901969848 ) ) ;
#88318 = CARTESIAN_POINT ( 'NONE',  ( 107.0664832912750057, -36.72944715993903486, 9.125625275910969947 ) ) ;
#88319 = DIRECTION ( 'NONE',  ( 1.000000000000000000, 0.000000000000000000, -2.089354330573420398E-14 ) ) ;
#88320 = ADVANCED_FACE ( 'NONE', ( #48851 ), #69774, .T. ) ;
#88321 = CARTESIAN_POINT ( 'NONE',  ( 116.7947957127217222, -39.38901390484394227, 24.61469397140603732 ) ) ;
#88322 = CARTESIAN_POINT ( 'NONE',  ( 116.7833380721246641, -34.07052967118504938, 30.03894244259582180 ) ) ;
#88324 = DIRECTION ( 'NONE',  ( -0.7071067811987160612, -0.7071067811743789733, 0.000000000000000000 ) ) ;
#88323 = CARTESIAN_POINT ( 'NONE',  ( 105.6833081684227835, -28.74817111171022788, 277.6356252759111953 ) ) ;
#88325 = CARTESIAN_POINT ( 'NONE',  ( 97.81930885783896201, -40.53600329143382908, 172.6372235601638465 ) ) ;
#88326 = LINE ( 'NONE', #32426, #13433 ) ;
#88327 = PLANE ( 'NONE',  #32468 ) ;
#88328 = DIRECTION ( 'NONE',  ( 0.000000000000000000, 1.000000000000000000, 0.000000000000000000 ) ) ;
#88329 = DIRECTION ( 'NONE',  ( 4.299999999999999979E-14, -1.000000000000000000, 4.400000000000000367E-29 ) ) ;
#88330 = CARTESIAN_POINT ( 'NONE',  ( 41.56648329127499153, -36.32844715994070839, 194.1756252759119832 ) ) ;
#88332 = ORIENTED_EDGE ( 'NONE', *, *, #57495, .F. ) ;
#88331 = CARTESIAN_POINT ( 'NONE',  ( -450.8499999999999659, 53.97500000000000142, -3.174999999999999822 ) ) ;
#88333 = VECTOR ( 'NONE', #10549, 999.9999999999998863 ) ;
#88334 = CARTESIAN_POINT ( 'NONE',  ( 136.8164806451551669, -18.72944715939129523, 6.749772901088581634 ) ) ;
#88335 = CARTESIAN_POINT ( 'NONE',  ( 98.88149684619317270, -29.26610755689610599, 230.7261014663869503 ) ) ;
#88336 = CARTESIAN_POINT ( 'NONE',  ( 113.3146854497373965, -28.34009065521201265, 100.5670538473389684 ) ) ;
#88337 = CARTESIAN_POINT ( 'NONE',  ( 100.1098231460999841, -44.55235322945014076, 262.9984824187678782 ) ) ;
#88338 = CARTESIAN_POINT ( 'NONE',  ( 125.5177273812784762, -131.0330679306342176, 55.21780685541800437 ) ) ;
#88339 = CARTESIAN_POINT ( 'NONE',  ( 31.85959712127300847, -23.19206098994050436, -5.074374724088000832 ) ) ;
#88341 = FACE_OUTER_BOUND ( 'NONE', #47341, .T. ) ;
#88340 = DIRECTION ( 'NONE',  ( 0.7071067811864677477, 0.7071067811866272868, 7.071067811864671681E-16 ) ) ;
#88342 = FACE_OUTER_BOUND ( 'NONE', #69433, .T. ) ;
#88343 = CARTESIAN_POINT ( 'NONE',  ( 133.4132809338025254, -21.40256188477528099, 1.689562700883915136 ) ) ;
#88344 = CIRCLE ( 'NONE', #59267, 10.26166025953211758 ) ;
#88345 = CIRCLE ( 'NONE', #10010, 4.749999999999976907 ) ;
#88346 = ADVANCED_FACE ( 'NONE', ( #84762 ), #22527, .T. ) ;
#88347 = ORIENTED_EDGE ( 'NONE', *, *, #71521, .T. ) ;
#88348 = ORIENTED_EDGE ( 'NONE', *, *, #37085, .F. ) ;
#88349 = CARTESIAN_POINT ( 'NONE',  ( 108.7098619460078481, -45.63517435782368636, 127.1562293518869780 ) ) ;
#88350 = VECTOR ( 'NONE', #71420, 1000.000000000000000 ) ;
#88352 = VERTEX_POINT ( 'NONE', #45599 ) ;
#88351 = DIRECTION ( 'NONE',  ( 0.000000000000000000, 0.000000000000000000, 1.000000000000000000 ) ) ;
#88353 = DIRECTION ( 'NONE',  ( -0.3535533905932733423, -0.6123724356957724879, 0.7071067811865668906 ) ) ;
#88354 = CARTESIAN_POINT ( 'NONE',  ( 95.80265872640110558, -40.33145541733360773, 127.5727681330539554 ) ) ;
#88355 = DIRECTION ( 'NONE',  ( 0.000000000000000000, 1.000000000000000000, 0.000000000000000000 ) ) ;
#88356 = CIRCLE ( 'NONE', #27378, 2.517499999999998739 ) ;
#88357 = LINE ( 'NONE', #88802, #84806 ) ;
#88358 = CARTESIAN_POINT ( 'NONE',  ( 188.5667039024479834, -67.87844715994100397, 142.0928068554150059 ) ) ;
#88359 = CARTESIAN_POINT ( 'NONE',  ( 131.3164832912740110, -36.72944715994100306, -5.074374724089004474 ) ) ;
#88360 = AXIS2_PLACEMENT_3D ( 'NONE', #80286, #37601, #51649 ) ;
#88361 = CARTESIAN_POINT ( 'NONE',  ( 98.84777479348167617, -29.24180311599940651, 80.73848241876795839 ) ) ;
#88362 = ORIENTED_EDGE ( 'NONE', *, *, #48243, .F. ) ;
#88363 = ORIENTED_EDGE ( 'NONE', *, *, #24559, .F. ) ;
#88364 = EDGE_LOOP ( 'NONE', ( #74812, #31565, #76007, #4515 ) ) ;
#88365 = DIRECTION ( 'NONE',  ( 0.000000000000000000, -1.000000000000000000, 0.000000000000000000 ) ) ;
#88367 = CARTESIAN_POINT ( 'NONE',  ( 107.0667039024470313, -104.2784471599420755, -19.78219314458201694 ) ) ;
#88366 = CARTESIAN_POINT ( 'NONE',  ( 113.7965574739370140, -44.62378898692899298, 149.1508633711479774 ) ) ;
#88368 = CARTESIAN_POINT ( 'NONE',  ( 107.0667039024470313, -104.2784471599420755, -19.78219314458201694 ) ) ;
#88369 = CARTESIAN_POINT ( 'NONE',  ( 11.75210537873753402, 77.68270844259760111, -130.0262747911924635 ) ) ;
#88370 = EDGE_CURVE ( 'NONE', #733, #86726, #58367, .T. ) ;
#88371 = CARTESIAN_POINT ( 'NONE',  ( 25.56670390244797275, -67.87844715994100397, 173.2178068554149775 ) ) ;
#88372 = CARTESIAN_POINT ( 'NONE',  ( 90.81826664111963510, 89.94786999841838337, 76.20774946062938682 ) ) ;
#88373 = CARTESIAN_POINT ( 'NONE',  ( -479.3614999999999782, 101.9113919710471947, 11.11250000000054072 ) ) ;
#88374 = CARTESIAN_POINT ( 'NONE',  ( 117.3319688044107920, -38.62265419183311366, 88.68133956162493803 ) ) ;
#88375 = ORIENTED_EDGE ( 'NONE', *, *, #27705, .F. ) ;
#88376 = ADVANCED_FACE ( 'NONE', ( #31102 ), #30230, .T. ) ;
#88377 = ORIENTED_EDGE ( 'NONE', *, *, #64149, .T. ) ;
#88378 = ADVANCED_FACE ( 'NONE', ( #65191 ), #86094, .T. ) ;
#88379 = DIRECTION ( 'NONE',  ( 0.000000000000000000, 0.000000000000000000, 1.000000000000000000 ) ) ;
#88380 = CARTESIAN_POINT ( 'NONE',  ( -87.44900557253164664, 93.33921197991992358, -96.94152442043716178 ) ) ;
#88381 = LINE ( 'NONE', #53808, #11929 ) ;
#88382 = CARTESIAN_POINT ( 'NONE',  ( 112.6324121799619462, -43.35677846492738041, 145.9385665600669881 ) ) ;
#88383 = ORIENTED_EDGE ( 'NONE', *, *, #37374, .F. ) ;
#88384 = VERTEX_POINT ( 'NONE', #17923 ) ;
#88385 = EDGE_CURVE ( 'NONE', #36180, #82011, #62267, .T. ) ;
#88386 = CARTESIAN_POINT ( 'NONE',  ( 34.33598329127384829, -36.32844715994141893, 193.9678068554150911 ) ) ;
#88387 = ORIENTED_EDGE ( 'NONE', *, *, #83725, .F. ) ;
#88388 = VERTEX_POINT ( 'NONE', #18366 ) ;
#88389 = ADVANCED_FACE ( 'NONE', ( #17046 ), #46051, .F. ) ;
#88390 = CARTESIAN_POINT ( 'NONE',  ( 77.55551418448884249, -19.85480617635147027, 7.067502061099748545 ) ) ;
#88391 = CARTESIAN_POINT ( 'NONE',  ( 115.6778139412940192, -34.63821234579798158, 205.4472975916109476 ) ) ;
#88392 = CARTESIAN_POINT ( 'NONE',  ( 51.42025729304100423, -33.70561438051981185, -5.074374724088000832 ) ) ;
#88393 = CARTESIAN_POINT ( 'NONE',  ( 20.03715912545732891, -24.95799193693189721, 300.4678068554150059 ) ) ;
#88394 = AXIS2_PLACEMENT_3D ( 'NONE', #19514, #19971, #47651 ) ;
#88395 = ORIENTED_EDGE ( 'NONE', *, *, #10720, .F. ) ;
#88397 = VERTEX_POINT ( 'NONE', #31549 ) ;
#88396 = AXIS2_PLACEMENT_3D ( 'NONE', #49477, #11166, #66125 ) ;
#88398 = DIRECTION ( 'NONE',  ( 0.000000000000000000, 0.000000000000000000, 1.000000000000000000 ) ) ;
#88399 = VERTEX_POINT ( 'NONE', #72014 ) ;
#88400 = ORIENTED_EDGE ( 'NONE', *, *, #82529, .F. ) ;
#88401 = CARTESIAN_POINT ( 'NONE',  ( 99.03493788190004921, -39.95360648959476180, 249.4604713219719656 ) ) ;
#88402 = VECTOR ( 'NONE', #35269, 1000.000000000000000 ) ;
#88403 = CARTESIAN_POINT ( 'NONE',  ( 103.3545649297684577, -47.16578287771347533, 102.3165776568629752 ) ) ;
#88404 = CARTESIAN_POINT ( 'NONE',  ( 96.36089708107958529, -41.75325360632975702, 61.67562527591097421 ) ) ;
#88405 = CARTESIAN_POINT ( 'NONE',  ( 107.2533376234434570, -45.00125912700468689, 249.5838068554171230 ) ) ;
#88406 = CYLINDRICAL_SURFACE ( 'NONE', #78665, 12.69999999999999574 ) ;
#88407 = DIRECTION ( 'NONE',  ( -0.000000000000000000, 1.000000000000000000, -0.000000000000000000 ) ) ;
#88408 = MECHANICAL_DESIGN_GEOMETRIC_PRESENTATION_REPRESENTATION (  '', ( #55034 ), #34769 ) ;
#88409 = CARTESIAN_POINT ( 'NONE',  ( 101.2007021600770855, -45.34774740814643934, 193.1013395616249682 ) ) ;
#88410 = CARTESIAN_POINT ( 'NONE',  ( 107.0664832912739399, -36.72944715994095333, 293.6356252759109680 ) ) ;
#88411 = ORIENTED_EDGE ( 'NONE', *, *, #18381, .F. ) ;
#88412 = CARTESIAN_POINT ( 'NONE',  ( 130.1467648208193850, 75.15271101351808625, -10.33160863867446899 ) ) ;
#88413 = VERTEX_POINT ( 'NONE', #51100 ) ;
#88414 = ORIENTED_EDGE ( 'NONE', *, *, #54678, .T. ) ;
#88415 = CIRCLE ( 'NONE', #23138, 7.937500000000000000 ) ;
#88416 = DIRECTION ( 'NONE',  ( 1.000000000000000078E-15, -1.000000000000000083E-30, -1.000000000000000000 ) ) ;
#88417 = ORIENTED_EDGE ( 'NONE', *, *, #11007, .F. ) ;
#88418 = CARTESIAN_POINT ( 'NONE',  ( -7.661254700127833495, 82.54999999999999716, 320.6630000000000109 ) ) ;
#88419 = DIRECTION ( 'NONE',  ( 0.000000000000000000, 1.000000000000000000, 1.809101308280369915E-15 ) ) ;
#88420 = CARTESIAN_POINT ( 'NONE',  ( 96.03551326368828711, -41.06051932364815826, 96.62419670448197451 ) ) ;
#88421 = CARTESIAN_POINT ( 'NONE',  ( -11.32599464014776558, 76.80063784493215451, 130.0638828588391220 ) ) ;
#88422 = ADVANCED_FACE ( 'NONE', ( #30668 ), #38363, .F. ) ;
#88423 = DIRECTION ( 'NONE',  ( -0.7071067811865192621, -0.7071067811865758834, 2.899137802864845566E-29 ) ) ;
#88424 = DIRECTION ( 'NONE',  ( 0.000000000000000000, 1.000000000000000000, 0.000000000000000000 ) ) ;
#88427 = CARTESIAN_POINT ( 'NONE',  ( 102.2473430764597282, -45.94923854148469644, 208.1927681330539599 ) ) ;
#88426 = LINE ( 'NONE', #40250, #59979 ) ;
#88425 = CARTESIAN_POINT ( 'NONE',  ( 130.0664832912740110, -18.82844715994099971, 284.9256252759119548 ) ) ;
#88428 = DIRECTION ( 'NONE',  ( -1.000000000000000078E-15, 1.000000000000000000, 0.000000000000000000 ) ) ;
#88429 = DIRECTION ( 'NONE',  ( 0.000000000000000000, 0.000000000000000000, 1.000000000000000000 ) ) ;
#88430 = VERTEX_POINT ( 'NONE', #66063 ) ;
#88431 = VECTOR ( 'NONE', #12108, 1000.000000000000000 ) ;
#88432 = DIRECTION ( 'NONE',  ( 0.000000000000000000, 1.000000000000000000, 0.000000000000000000 ) ) ;
#88433 = CARTESIAN_POINT ( 'NONE',  ( 41.56648329127499153, -27.82844715994070484, 323.6756252759119548 ) ) ;
#88434 = LINE ( 'NONE', #10762, #19792 ) ;
#88435 = CARTESIAN_POINT ( 'NONE',  ( 107.0664832912739399, -36.72944715994095333, 302.7856252759109452 ) ) ;
#88437 = VERTEX_POINT ( 'NONE', #4306 ) ;
#88436 = CARTESIAN_POINT ( 'NONE',  ( 115.8924960319658055, -44.71257290243538307, 233.2413395616259493 ) ) ;
#88438 = CARTESIAN_POINT ( 'NONE',  ( 183.6524903400784012, -49.32844715993451956, 249.9678068554149775 ) ) ;
#88439 = CARTESIAN_POINT ( 'NONE',  ( 101.0741685120301412, -45.28686133165523131, 278.0899109901965858 ) ) ;
#88440 = CARTESIAN_POINT ( 'NONE',  ( 109.5186955991938191, -46.90685520642291806, 128.7641967044819751 ) ) ;
#88441 = DIRECTION ( 'NONE',  ( 0.000000000000000000, 0.000000000000000000, 1.000000000000000000 ) ) ;
#88442 = CARTESIAN_POINT ( 'NONE',  ( 4.090559613967800878, 94.60197653454002875, -130.4941709638409861 ) ) ;
#88443 = VECTOR ( 'NONE', #84133, 1000.000000000000000 ) ;
#88445 = FACE_OUTER_BOUND ( 'NONE', #71750, .T. ) ;
#88444 = LINE ( 'NONE', #54321, #53524 ) ;
#88446 = CARTESIAN_POINT ( 'NONE',  ( 104.4899545095031925, -26.97880757019963127, 190.2814586045716396 ) ) ;
#88447 = LINE ( 'NONE', #69339, #24808 ) ;
#88448 = ORIENTED_EDGE ( 'NONE', *, *, #4980, .F. ) ;
#88449 = ADVANCED_FACE ( 'NONE', ( #31995 ), #59688, .F. ) ;
#88450 = ORIENTED_EDGE ( 'NONE', *, *, #26660, .T. ) ;
#88451 = VERTEX_POINT ( 'NONE', #2530 ) ;
#88452 = VECTOR ( 'NONE', #54132, 1000.000000000000000 ) ;
#88453 = ORIENTED_EDGE ( 'NONE', *, *, #3749, .F. ) ;
#88454 = LINE ( 'NONE', #26655, #55414 ) ;
#88455 = CARTESIAN_POINT ( 'NONE',  ( 116.7496603916996207, -31.44741115753631178, 20.21181575210195902 ) ) ;
#88456 = DIRECTION ( 'NONE',  ( 9.030537910253610117E-13, -1.000000000000000000, 8.600537910253610331E-28 ) ) ;
#88458 = CARTESIAN_POINT ( 'NONE',  ( 71.25416588882602298, -72.55705569728901594, 542.9756252759101471 ) ) ;
#88457 = AXIS2_PLACEMENT_3D ( 'NONE', #48748, #28788, #34687 ) ;
#88459 = EDGE_CURVE ( 'NONE', #36469, #81025, #82592, .T. ) ;
#88461 = CARTESIAN_POINT ( 'NONE',  ( 70.40117688449606703, -140.5784839457434998, 246.8085677970040024 ) ) ;
#88460 = DIRECTION ( 'NONE',  ( 0.000000000000000000, 2.135044278125299371E-15, -1.000000000000000000 ) ) ;
#88462 = CARTESIAN_POINT ( 'NONE',  ( 100.3746636439974935, -30.62762610928201568, 230.1486103042669811 ) ) ;
#88463 = ORIENTED_EDGE ( 'NONE', *, *, #39603, .F. ) ;
#88464 = EDGE_LOOP ( 'NONE', ( #87913, #46884, #72611, #31354 ) ) ;
#88465 = AXIS2_PLACEMENT_3D ( 'NONE', #9373, #42355, #36909 ) ;
#88467 = VERTEX_POINT ( 'NONE', #23866 ) ;
#88466 = AXIS2_PLACEMENT_3D ( 'NONE', #86051, #51490, #16552 ) ;
#88468 = CARTESIAN_POINT ( 'NONE',  ( 97.81169585860149596, -40.51742224678086046, 106.6356332503197137 ) ) ;
#88470 = EDGE_CURVE ( 'NONE', #60843, #57623, #11572, .T. ) ;
#88469 = CARTESIAN_POINT ( 'NONE',  ( 97.94027119124240244, -40.81832795154717530, 101.6620931678271376 ) ) ;
#88471 = DIRECTION ( 'NONE',  ( 0.9068632946707807507, -0.4214249218767880945, 8.673617379884035472E-16 ) ) ;
#88472 = DIRECTION ( 'NONE',  ( 0.000000000000000000, 0.000000000000000000, -1.000000000000000000 ) ) ;
#88473 = CARTESIAN_POINT ( 'NONE',  ( 105.5822692374337777, -27.99308443639166555, 11.64158330589692980 ) ) ;
#88474 = FACE_OUTER_BOUND ( 'NONE', #61009, .T. ) ;
#88475 = AXIS2_PLACEMENT_3D ( 'NONE', #63252, #43236, #37336 ) ;
#88476 = DIRECTION ( 'NONE',  ( -2.900000000000000265E-14, 2.000000000000000155E-15, -1.000000000000000000 ) ) ;
#88477 = CARTESIAN_POINT ( 'NONE',  ( 117.6440887749188846, -33.30491810902906735, 284.0756252759109657 ) ) ;
#88478 = EDGE_CURVE ( 'NONE', #22589, #67053, #37828, .T. ) ;
#88479 = DIRECTION ( 'NONE',  ( 1.000000000000000000, 0.000000000000000000, 0.000000000000000000 ) ) ;
#88480 = ORIENTED_EDGE ( 'NONE', *, *, #1399, .T. ) ;
#88481 = DIRECTION ( 'NONE',  ( 0.000000000000000000, 0.000000000000000000, -1.000000000000000000 ) ) ;
#88482 = VECTOR ( 'NONE', #73071, 1000.000000000000000 ) ;
#88483 = DIRECTION ( 'NONE',  ( 0.000000000000000000, 0.000000000000000000, 1.000000000000000000 ) ) ;
#88484 = CARTESIAN_POINT ( 'NONE',  ( 115.2001725772484662, -37.69162533786680314, 51.55094751244793372 ) ) ;
#88485 = FACE_OUTER_BOUND ( 'NONE', #4913, .T. ) ;
#88486 = DIRECTION ( 'NONE',  ( -2.999999999999999839E-15, 1.000000000000000000, -2.999999999999999900E-30 ) ) ;
#88487 = VECTOR ( 'NONE', #30658, 1000.000000000000000 ) ;
#88488 = CARTESIAN_POINT ( 'NONE',  ( -6.364298811279507362, 93.57154221663603266, 118.3870716450922629 ) ) ;
#88489 = ORIENTED_EDGE ( 'NONE', *, *, #47667, .F. ) ;
#88490 = CARTESIAN_POINT ( 'NONE',  ( 143.0667039024470171, -118.2784471599408960, 222.2178068554179902 ) ) ;
#88491 = EDGE_CURVE ( 'NONE', #60263, #10962, #3801, .T. ) ;
#88492 = CARTESIAN_POINT ( 'NONE',  ( 125.2163577468151914, 55.36712120389123015, -36.95591843739485682 ) ) ;
#88493 = ORIENTED_EDGE ( 'NONE', *, *, #41453, .T. ) ;
#88494 = CARTESIAN_POINT ( 'NONE',  ( 108.5379876179846264, -26.40851185940291046, 104.9641967044819779 ) ) ;
#88495 = ORIENTED_EDGE ( 'NONE', *, *, #44070, .F. ) ;
#88496 = EDGE_CURVE ( 'NONE', #20192, #81785, #21589, .T. ) ;
#88497 = CARTESIAN_POINT ( 'NONE',  ( 115.4947688602672997, -38.28382951093581710, 88.10384839950596358 ) ) ;
#88498 = ADVANCED_FACE ( 'NONE', ( #41045 ), #76022, .F. ) ;
#88499 = DIRECTION ( 'NONE',  ( -1.000000000000000000, -8.741913579725640327E-16, -2.913971193241879977E-15 ) ) ;
#88500 = CARTESIAN_POINT ( 'NONE',  ( 107.8890265924388814, -27.36996276949999185, 106.4263452106589654 ) ) ;
#88501 = CARTESIAN_POINT ( 'NONE',  ( 86.98314995793998605, 12.92155284005730387, 355.9756252759109998 ) ) ;
#88502 = ADVANCED_FACE ( 'NONE', ( #88773 ), #67866, .T. ) ;
#88503 = CARTESIAN_POINT ( 'NONE',  ( 107.0664832912739968, -36.72944715994100306, 287.6356252759109680 ) ) ;
#88504 = VECTOR ( 'NONE', #14974, 999.9999999999998863 ) ;
#88505 = CARTESIAN_POINT ( 'NONE',  ( 103.9509101786591287, -47.35857741242491414, 58.33753003781600199 ) ) ;
#88506 = CARTESIAN_POINT ( 'NONE',  ( 107.0667039024470313, -104.2784471599420755, -19.78219314458201694 ) ) ;
#88507 = CARTESIAN_POINT ( 'NONE',  ( 70.06202783732101125, -36.73691869758536654, 361.9756252759101471 ) ) ;
#88508 = ORIENTED_EDGE ( 'NONE', *, *, #12325, .T. ) ;
#88509 = CARTESIAN_POINT ( 'NONE',  ( 77.33253953643577461, -19.07457063615845883, 3.076560393663061443 ) ) ;
#88510 = VERTEX_POINT ( 'NONE', #27419 ) ;
#88511 = ORIENTED_EDGE ( 'NONE', *, *, #80802, .T. ) ;
#88512 = CIRCLE ( 'NONE', #58028, 3.000000000000002665 ) ;
#88513 = PLANE ( 'NONE',  #13642 ) ;
#88514 = VERTEX_POINT ( 'NONE', #12460 ) ;
#88515 = CARTESIAN_POINT ( 'NONE',  ( 115.3604274781777264, -30.50455558986040572, 264.3508633711496714 ) ) ;
#88516 = CARTESIAN_POINT ( 'NONE',  ( 96.64920772548965999, -35.94453432339758336, 142.2670538473399517 ) ) ;
#88517 = LINE ( 'NONE', #14449, #24888 ) ;
#88518 = CARTESIAN_POINT ( 'NONE',  ( 104.4068591371749761, -46.45772509445649234, 128.3646896267844966 ) ) ;
#88519 = CARTESIAN_POINT ( 'NONE',  ( 96.63924282488838458, -37.56250720137591514, 97.38991099019594344 ) ) ;
#88520 = CARTESIAN_POINT ( 'NONE',  ( 31.89136050872224004, -31.76306994223876501, 313.9678068554150059 ) ) ;
#88521 = EDGE_LOOP ( 'NONE', ( #33297, #4874, #34972, #31450, #72713 ) ) ;
#88522 = LINE ( 'NONE', #88069, #48284 ) ;
#88523 = AXIS2_PLACEMENT_3D ( 'NONE', #63299, #16057, #617 ) ;
#88524 = CARTESIAN_POINT ( 'NONE',  ( 115.0375705353306586, -42.90806541145470732, 159.3021678111343817 ) ) ;
#88525 = ORIENTED_EDGE ( 'NONE', *, *, #68524, .F. ) ;
#88526 = CIRCLE ( 'NONE', #49340, 2.116999999999993776 ) ;
#88527 = CARTESIAN_POINT ( 'NONE',  ( 37.36643805256657913, -48.62818131006120836, 249.9678068554150343 ) ) ;
#88528 = CARTESIAN_POINT ( 'NONE',  ( 134.0664832912740110, -8.350947159940998787, 306.1181252759120071 ) ) ;
#88529 = CARTESIAN_POINT ( 'NONE',  ( 111.4711666614669099, -26.61707918639087822, 284.7375300378156453 ) ) ;
#88530 = CARTESIAN_POINT ( 'NONE',  ( 72.96458098368650269, 127.0000000000000000, 72.96458098368729850 ) ) ;
#88531 = LINE ( 'NONE', #60798, #23147 ) ;
#88532 = CARTESIAN_POINT ( 'NONE',  ( 77.45242755740703444, -37.60567372264567609, 2.908038864009608648 ) ) ;
#88533 = CARTESIAN_POINT ( 'NONE',  ( 106.0094748626272434, -28.25366608065910157, 269.5981341137911613 ) ) ;
#88535 = CARTESIAN_POINT ( 'NONE',  ( 112.7479404651553949, -27.97242311821442584, 65.61848241876793963 ) ) ;
#88534 = DIRECTION ( 'NONE',  ( 0.000000000000000000, 1.000000000000000000, 1.914177628664063178E-15 ) ) ;
#88536 = DIRECTION ( 'NONE',  ( 9.351236661543306751E-17, -3.725950533538267725E-29, -1.000000000000000000 ) ) ;
#88537 = CARTESIAN_POINT ( 'NONE',  ( 95.52074050172029729, -39.61468907688732344, 166.5213395616259788 ) ) ;
#88538 = ORIENTED_EDGE ( 'NONE', *, *, #62919, .F. ) ;
#88539 = CARTESIAN_POINT ( 'NONE',  ( 118.5256205435843100, -36.72944715994100306, 305.0306255462182321 ) ) ;
#88540 = VERTEX_POINT ( 'NONE', #46505 ) ;
#88541 = VECTOR ( 'NONE', #61892, 1000.000000000000000 ) ;
#88542 = LINE ( 'NONE', #61696, #77297 ) ;
#88543 = DIRECTION ( 'NONE',  ( 0.000000000000000000, 1.000000000000000000, 0.000000000000000000 ) ) ;
#88544 = CARTESIAN_POINT ( 'NONE',  ( 188.5667039024479834, -48.82844715994099971, 173.2178068554149775 ) ) ;
#88545 = ORIENTED_EDGE ( 'NONE', *, *, #5809, .F. ) ;
#88546 = LINE ( 'NONE', #13567, #53424 ) ;
#88548 = ORIENTED_EDGE ( 'NONE', *, *, #41004, .F. ) ;
#88547 = CARTESIAN_POINT ( 'NONE',  ( 117.1686558484209826, -33.85615284218268073, 149.0470538473389581 ) ) ;
#88549 = CARTESIAN_POINT ( 'NONE',  ( 182.2300522401149863, -33.89581943344511217, -5.074374724088000832 ) ) ;
#88550 = CARTESIAN_POINT ( 'NONE',  ( -130.0003666679300522, 86.63355734047007672, 12.03281245963826862 ) ) ;
#88551 = LINE ( 'NONE', #44160, #11137 ) ;
#88552 = LINE ( 'NONE', #34460, #80070 ) ;
#88553 = ORIENTED_EDGE ( 'NONE', *, *, #48916, .F. ) ;
#88554 = ADVANCED_FACE ( 'NONE', ( #25632 ), #40145, .F. ) ;
#88555 = ADVANCED_FACE ( 'NONE', ( #68321 ), #81523, .F. ) ;
#88556 = DIRECTION ( 'NONE',  ( 0.000000000000000000, 0.000000000000000000, -1.000000000000000000 ) ) ;
#88557 = ORIENTED_EDGE ( 'NONE', *, *, #71219, .T. ) ;
#88558 = CIRCLE ( 'NONE', #49362, 3.000000000000002665 ) ;
#88559 = EDGE_CURVE ( 'NONE', #52469, #77842, #82414, .T. ) ;
#88560 = EDGE_LOOP ( 'NONE', ( #77430, #11218, #59505, #27958, #30041, #7608 ) ) ;
#88561 = PLANE ( 'NONE',  #24968 ) ;
#88562 = CARTESIAN_POINT ( 'NONE',  ( 88.80956239834438293, 94.30053025434480674, -95.69832483115219190 ) ) ;
#88563 = CARTESIAN_POINT ( 'NONE',  ( -47.08158946516970644, 101.2663385054221408, 76.19398627647811395 ) ) ;
#88564 = DIRECTION ( 'NONE',  ( 0.000000000000000000, 0.000000000000000000, -1.000000000000000000 ) ) ;
#88565 = ADVANCED_FACE ( 'NONE', ( #68769 ), #53308, .T. ) ;
#88566 = EDGE_CURVE ( 'NONE', #82149, #41571, #46295, .T. ) ;
#88568 = CYLINDRICAL_SURFACE ( 'NONE', #47132, 9.999999999999998224 ) ;
#88567 = DIRECTION ( 'NONE',  ( 1.000000000000000078E-15, -1.000000000000000000, 0.000000000000000000 ) ) ;
#88569 = DIRECTION ( 'NONE',  ( 9.032638163712999905E-13, -1.000000000000000000, 1.217258424823508649E-28 ) ) ;
#88570 = VECTOR ( 'NONE', #31713, 1000.000000000000000 ) ;
#88571 = ADVANCED_FACE ( 'NONE', ( #20175 ), #33345, .F. ) ;
#88572 = VERTEX_POINT ( 'NONE', #88330 ) ;
#88574 = ADVANCED_FACE ( 'NONE', ( #19276 ), #26090, .F. ) ;
#88573 = CARTESIAN_POINT ( 'NONE',  ( 34.67381068360400320, -28.98061976758901892, -5.074374724088000832 ) ) ;
#88575 = CARTESIAN_POINT ( 'NONE',  ( 116.7732407090125690, -35.28285290846963562, 214.9441967044819819 ) ) ;
#88577 = ORIENTED_EDGE ( 'NONE', *, *, #14837, .F. ) ;
#88576 = DIRECTION ( 'NONE',  ( 0.000000000000000000, 0.000000000000000000, -1.000000000000000000 ) ) ;
#88578 = CARTESIAN_POINT ( 'NONE',  ( 98.34688518126465340, -32.29864090244033292, 46.95276813305293473 ) ) ;
#88579 = EDGE_CURVE ( 'NONE', #69807, #88931, #74680, .T. ) ;
#88580 = CARTESIAN_POINT ( 'NONE',  ( 133.5842039024480243, -43.72944715994092491, 231.5838068554170093 ) ) ;
#88581 = FACE_OUTER_BOUND ( 'NONE', #23676, .T. ) ;
#88582 = EDGE_CURVE ( 'NONE', #25689, #79424, #61486, .T. ) ;
#88583 = DIRECTION ( 'NONE',  ( 0.000000000000000000, 1.000000000000000000, 0.000000000000000000 ) ) ;
#88584 = ORIENTED_EDGE ( 'NONE', *, *, #52777, .F. ) ;
#88585 = DIRECTION ( 'NONE',  ( 0.000000000000000000, 0.000000000000000000, 1.000000000000000000 ) ) ;
#88586 = EDGE_LOOP ( 'NONE', ( #33331, #28977, #25898, #32522 ) ) ;
#88587 = ORIENTED_EDGE ( 'NONE', *, *, #36633, .T. ) ;
#88588 = CARTESIAN_POINT ( 'NONE',  ( 98.31940232332729579, -40.15947632561638869, 243.0434880678019738 ) ) ;
#88589 = VECTOR ( 'NONE', #20941, 1000.000000000000000 ) ;
#88590 = DIRECTION ( 'NONE',  ( 1.000000000000000078E-15, -1.000000000000000083E-30, -1.000000000000000000 ) ) ;
#88591 = CARTESIAN_POINT ( 'NONE',  ( -83.89391322244367188, 88.18319050751492227, 100.0339087179667814 ) ) ;
#88592 = CARTESIAN_POINT ( 'NONE',  ( 98.30753412158296101, -41.72887537170915095, 152.7397919317029960 ) ) ;
#88593 = CIRCLE ( 'NONE', #56616, 4.762500000000002842 ) ;
#88594 = CARTESIAN_POINT ( 'NONE',  ( 107.0664832912739968, -36.72944715994100306, 287.6356252759109680 ) ) ;
#88595 = ORIENTED_EDGE ( 'NONE', *, *, #45188, .T. ) ;
#88596 = DIRECTION ( 'NONE',  ( 0.000000000000000000, 1.000000000000000000, 0.000000000000000000 ) ) ;
#88597 = ADVANCED_FACE ( 'NONE', ( #64195 ), #69212, .F. ) ;
#88598 = DIRECTION ( 'NONE',  ( 0.000000000000000000, 0.000000000000000000, -1.000000000000000000 ) ) ;
#88599 = ORIENTED_EDGE ( 'NONE', *, *, #87419, .F. ) ;
#88600 = CARTESIAN_POINT ( 'NONE',  ( 96.65879732087768161, -33.00665786158104709, 26.06514908543494613 ) ) ;
#88601 = ORIENTED_EDGE ( 'NONE', *, *, #56646, .F. ) ;
#88602 = EDGE_CURVE ( 'NONE', #5461, #17136, #22417, .T. ) ;
#88603 = ORIENTED_EDGE ( 'NONE', *, *, #55345, .F. ) ;
#88604 = CARTESIAN_POINT ( 'NONE',  ( 109.9373871219287082, -28.56496087843131448, 252.6376141791152747 ) ) ;
#88605 = EDGE_CURVE ( 'NONE', #45431, #32749, #6985, .T. ) ;
#88606 = FACE_BOUND ( 'NONE', #81765, .T. ) ;
#88607 = CARTESIAN_POINT ( 'NONE',  ( 99.36405074150913208, -30.70139697576582805, 155.7984824187689412 ) ) ;
#88608 = CARTESIAN_POINT ( 'NONE',  ( 23.58193636576847751, 80.15658928983457088, 307.0240681300007282 ) ) ;
#88609 = CARTESIAN_POINT ( 'NONE',  ( 223.2659999999999911, 52.73749999999999716, -44.45000000000000284 ) ) ;
#88611 = EDGE_CURVE ( 'NONE', #29809, #1463, #21523, .T. ) ;
#88610 = DIRECTION ( 'NONE',  ( 0.000000000000000000, 0.000000000000000000, 1.000000000000000000 ) ) ;
#88612 = LINE ( 'NONE', #54487, #21840 ) ;
#88613 = CARTESIAN_POINT ( 'NONE',  ( 105.6260786687505657, -47.09854616955767881, 253.4670538473393719 ) ) ;
#88614 = CARTESIAN_POINT ( 'NONE',  ( 92.22587532767860807, 84.62843115047675724, -74.49778344313808986 ) ) ;
#88615 = ORIENTED_EDGE ( 'NONE', *, *, #12240, .T. ) ;
#88616 = CARTESIAN_POINT ( 'NONE',  ( 98.82360578189442890, -43.24043672769812474, 87.85848241876792031 ) ) ;
#88617 = LINE ( 'NONE', #10947, #46765 ) ;
#88618 = ORIENTED_EDGE ( 'NONE', *, *, #40334, .F. ) ;
#88619 = ORIENTED_EDGE ( 'NONE', *, *, #44132, .F. ) ;
#88620 = ORIENTED_EDGE ( 'NONE', *, *, #35935, .F. ) ;
#88621 = CIRCLE ( 'NONE', #4509, 23.50000000000000711 ) ;
#88622 = DIRECTION ( 'NONE',  ( 1.000000000000000000, 0.000000000000000000, 0.000000000000000000 ) ) ;
#88623 = LINE ( 'NONE', #11407, #13768 ) ;
#88624 = CARTESIAN_POINT ( 'NONE',  ( 167.2371591254545535, -47.82818131005522133, 117.4678068554150485 ) ) ;
#88625 = LINE ( 'NONE', #25, #4075 ) ;
#88626 = CIRCLE ( 'NONE', #56892, 3.000000864267354572 ) ;
#88627 = CARTESIAN_POINT ( 'NONE',  ( 107.5257129551532813, -44.87112140103544533, 150.4395189410199407 ) ) ;
#88628 = CARTESIAN_POINT ( 'NONE',  ( 96.95773401446056994, -39.36581715674629578, 272.5299109901966972 ) ) ;
#88629 = CARTESIAN_POINT ( 'NONE',  ( 126.0667039024479266, -14.72944715994094977, 239.5838068554170377 ) ) ;
#88630 = VERTEX_POINT ( 'NONE', #85100 ) ;
#88631 = CARTESIAN_POINT ( 'NONE',  ( 130.0003666679301944, 86.63355734047007672, -12.03281245963736446 ) ) ;
#88632 = FACE_OUTER_BOUND ( 'NONE', #16096, .T. ) ;
#88633 = AXIS2_PLACEMENT_3D ( 'NONE', #86927, #17870, #51049 ) ;
#88634 = ORIENTED_EDGE ( 'NONE', *, *, #21602, .T. ) ;
#88635 = ORIENTED_EDGE ( 'NONE', *, *, #41069, .T. ) ;
#88636 = VECTOR ( 'NONE', #12763, 1000.000000000000000 ) ;
#88637 = CARTESIAN_POINT ( 'NONE',  ( 180.1667039024473809, -26.71338133338667831, 313.9678068554149490 ) ) ;
#88638 = ORIENTED_EDGE ( 'NONE', *, *, #27135, .T. ) ;
#88639 = VERTEX_POINT ( 'NONE', #34678 ) ;
#88640 = LINE ( 'NONE', #26396, #62888 ) ;
#88641 = CARTESIAN_POINT ( 'NONE',  ( -12.27515439545620701, 79.26608163778621474, -129.9777074703579842 ) ) ;
#88642 = CARTESIAN_POINT ( 'NONE',  ( 130.5667039024482960, -36.72944715994102438, 249.5838068554162987 ) ) ;
#88643 = PLANE ( 'NONE',  #17071 ) ;
#88644 = CARTESIAN_POINT ( 'NONE',  ( 100.5405518937255209, -43.91836718856000488, 156.4124198280769917 ) ) ;
#88645 = CARTESIAN_POINT ( 'NONE',  ( 112.9881877051661263, -28.09578728253486446, 44.59848241876795782 ) ) ;
#88646 = CARTESIAN_POINT ( 'NONE',  ( 255.9983484187079910, 40.03750000000000142, -2.032000000000000028 ) ) ;
#88647 = EDGE_LOOP ( 'NONE', ( #58702, #85606, #83620, #35446 ) ) ;
#88648 = CYLINDRICAL_SURFACE ( 'NONE', #86184, 3.999999999999992895 ) ;
#88649 = ORIENTED_EDGE ( 'NONE', *, *, #88982, .T. ) ;
#88650 = AXIS2_PLACEMENT_3D ( 'NONE', #49349, #7139, #62541 ) ;
#88651 = DIRECTION ( 'NONE',  ( 0.000000000000000000, -1.000000000000000000, 0.000000000000000000 ) ) ;
#88652 = ORIENTED_EDGE ( 'NONE', *, *, #30399, .F. ) ;
#88653 = CARTESIAN_POINT ( 'NONE',  ( 98.58946256649487339, -99.96145986183429955, -19.78219314458215550 ) ) ;
#88654 = CARTESIAN_POINT ( 'NONE',  ( -12.59999999999999787, 82.13878092619209781, 117.8845415480757310 ) ) ;
#88655 = CARTESIAN_POINT ( 'NONE',  ( 100.8871001369827809, -44.69991734071174250, 132.0523233816342952 ) ) ;
#88656 = AXIS2_PLACEMENT_3D ( 'NONE', #17711, #52634, #80395 ) ;
#88657 = DIRECTION ( 'NONE',  ( -1.000000000000000078E-15, 0.000000000000000000, -1.000000000000000000 ) ) ;
#88658 = ORIENTED_EDGE ( 'NONE', *, *, #48644, .F. ) ;
#88659 = CARTESIAN_POINT ( 'NONE',  ( 96.56351739100374232, -40.17746103522156176, 286.5908633711491120 ) ) ;
#88660 = CARTESIAN_POINT ( 'NONE',  ( 107.3220933465437810, -25.63295393647281628, 71.04610146638795243 ) ) ;
#88661 = EDGE_CURVE ( 'NONE', #38273, #7861, #7432, .T. ) ;
#88663 = CARTESIAN_POINT ( 'NONE',  ( 270.8910000000000196, 40.03750000000000142, -58.73749999999999716 ) ) ;
#88662 = CARTESIAN_POINT ( 'NONE',  ( 107.0664832912750057, -36.72944715993903486, 9.125625275910969947 ) ) ;
#88664 = CARTESIAN_POINT ( 'NONE',  ( 97.07207306401238611, -35.37843331541325398, 147.2194715753597904 ) ) ;
#88665 = ADVANCED_FACE ( 'NONE', ( #62387 ), #43277, .F. ) ;
#88666 = DIRECTION ( 'NONE',  ( 1.000000000000000078E-15, -1.000000000000000083E-30, -1.000000000000000000 ) ) ;
#88667 = AXIS2_PLACEMENT_3D ( 'NONE', #26275, #47592, #75327 ) ;
#88668 = EDGE_CURVE ( 'NONE', #34865, #62712, #41482, .T. ) ;
#88669 = CARTESIAN_POINT ( 'NONE',  ( 107.0667039024482818, -36.72944715994102438, 249.5838068554170093 ) ) ;
#88670 = CIRCLE ( 'NONE', #1665, 179.8898777604655095 ) ;
#88671 = CARTESIAN_POINT ( 'NONE',  ( 147.0667039024470739, -137.6758869494786097, 245.5072624240089851 ) ) ;
#88672 = DIRECTION ( 'NONE',  ( -1.000000000000000000, -4.299999999999999979E-14, -9.351236661543306751E-17 ) ) ;
#88673 = EDGE_CURVE ( 'NONE', #35668, #41448, #88415, .T. ) ;
#88674 = ORIENTED_EDGE ( 'NONE', *, *, #35609, .F. ) ;
#88675 = CARTESIAN_POINT ( 'NONE',  ( 118.1298445534695531, -37.63217702543061449, 38.77372051400595865 ) ) ;
#88676 = CARTESIAN_POINT ( 'NONE',  ( 109.9169591795599388, -46.81676508990216234, 68.79562527591099297 ) ) ;
#88678 = CARTESIAN_POINT ( 'NONE',  ( 245.4909999999999854, 65.43750000000000000, -67.11950000000000216 ) ) ;
#88677 = DIRECTION ( 'NONE',  ( -0.9963424814100663163, 0.08544974978097671925, 0.000000000000000000 ) ) ;
#88679 = CARTESIAN_POINT ( 'NONE',  ( -487.2989999999999782, 7.143750000000339995, 6.988054014476278830 ) ) ;
#88680 = ADVANCED_FACE ( 'NONE', ( #609 ), #55544, .T. ) ;
#88681 = CARTESIAN_POINT ( 'NONE',  ( 72.96458098368650269, 127.0000000000000000, 78.00648098368728256 ) ) ;
#88682 = ORIENTED_EDGE ( 'NONE', *, *, #43889, .T. ) ;
#88683 = EDGE_CURVE ( 'NONE', #24180, #14963, #10084, .T. ) ;
#88684 = CARTESIAN_POINT ( 'NONE',  ( 116.7039036015865037, -32.90075090702275418, 95.13943479971997874 ) ) ;
#88686 = ORIENTED_EDGE ( 'NONE', *, *, #81317, .T. ) ;
#88685 = CARTESIAN_POINT ( 'NONE',  ( 41.56648329127398966, -27.57844715994070484, 321.9256252759120116 ) ) ;
#88687 = CIRCLE ( 'NONE', #78520, 15.69999999999999929 ) ;
#88688 = CARTESIAN_POINT ( 'NONE',  ( 118.7655994573050577, -38.45539276985793720, 219.7099109901969882 ) ) ;
#88689 = CARTESIAN_POINT ( 'NONE',  ( 60.32499999999999574, 82.54999999999999716, 358.0130000000000337 ) ) ;
#88690 = LINE ( 'NONE', #47313, #55048 ) ;
#88691 = DIRECTION ( 'NONE',  ( 0.000000000000000000, 1.000000000000000000, 0.000000000000000000 ) ) ;
#88692 = CARTESIAN_POINT ( 'NONE',  ( 113.2454987024005106, -28.75867294838092647, 80.55229194212900268 ) ) ;
#88693 = EDGE_CURVE ( 'NONE', #33706, #75087, #15603, .T. ) ;
#88694 = CARTESIAN_POINT ( 'NONE',  ( 132.8008218761673902, -39.17731672736219650, 1.873071027760403240 ) ) ;
#88695 = FACE_OUTER_BOUND ( 'NONE', #86419, .T. ) ;
#88696 = CARTESIAN_POINT ( 'NONE',  ( 109.2982854457139581, -26.60236246699145113, 179.8918157521019339 ) ) ;
#88697 = EDGE_LOOP ( 'NONE', ( #39266, #85417 ) ) ;
#88698 = VECTOR ( 'NONE', #73559, 1000.000000000000114 ) ;
#88699 = ORIENTED_EDGE ( 'NONE', *, *, #67549, .T. ) ;
#88700 = CARTESIAN_POINT ( 'NONE',  ( 99.59846494627726088, -31.90336481815605296, 142.3015833058969974 ) ) ;
#88701 = VECTOR ( 'NONE', #71204, 1000.000000000000000 ) ;
#88702 = DIRECTION ( 'NONE',  ( 0.000000000000000000, 0.000000000000000000, 1.000000000000000000 ) ) ;
#88704 = CARTESIAN_POINT ( 'NONE',  ( 181.9694315774059987, -34.03355364505895864, 237.4678068554150059 ) ) ;
#88703 = CARTESIAN_POINT ( 'NONE',  ( 112.3177584634462534, -44.98096486020153151, 259.0270538473389479 ) ) ;
#88705 = DIRECTION ( 'NONE',  ( 0.7349399772593259161, -0.6687953793059864260, 0.1121426343770440259 ) ) ;
#88706 = CARTESIAN_POINT ( 'NONE',  ( 135.9998166246059839, 12.92155284005730387, 358.9756252759109998 ) ) ;
#88707 = DIRECTION ( 'NONE',  ( 0.000000000000000000, 0.000000000000000000, -1.000000000000000000 ) ) ;
#88708 = CYLINDRICAL_SURFACE ( 'NONE', #27545, 2.750000000000002665 ) ;
#88709 = CARTESIAN_POINT ( 'NONE',  ( 0.000000000000000000, 152.3879256507328250, 0.000000000000000000 ) ) ;
#88710 = CARTESIAN_POINT ( 'NONE',  ( 96.07698540226623152, -35.78353028925530310, 186.2461014663869889 ) ) ;
#88711 = LINE ( 'NONE', #89601, #85199 ) ;
#88712 = ORIENTED_EDGE ( 'NONE', *, *, #35087, .F. ) ;
#88713 = ORIENTED_EDGE ( 'NONE', *, *, #55087, .F. ) ;
#88714 = AXIS2_PLACEMENT_3D ( 'NONE', #53346, #87908, #25670 ) ;
#88715 = CARTESIAN_POINT ( 'NONE',  ( 107.0664832912739968, -36.72944715994100306, 287.6356252759109680 ) ) ;
#88716 = CARTESIAN_POINT ( 'NONE',  ( 78.76417807489981726, -16.30680158338988761, 1.893168945960760796 ) ) ;
#88717 = DIRECTION ( 'NONE',  ( -0.7071067811892205457, 0.7071067811838745998, -7.071067811892213774E-16 ) ) ;
#88719 = EDGE_CURVE ( 'NONE', #58657, #35463, #21699, .T. ) ;
#88718 = CARTESIAN_POINT ( 'NONE',  ( 105.7809510460201210, -24.27257308096163868, 321.6188579224977389 ) ) ;
#88720 = CYLINDRICAL_SURFACE ( 'NONE', #52807, 12.70000000000000107 ) ;
#88721 = ORIENTED_EDGE ( 'NONE', *, *, #23143, .F. ) ;
#88722 = CARTESIAN_POINT ( 'NONE',  ( 105.7141979885323906, -46.72366441306870399, 62.46885673744021972 ) ) ;
#88723 = CARTESIAN_POINT ( 'NONE',  ( 99.08584233156592802, -29.96666100724374715, 215.7670538473399517 ) ) ;
#88724 = EDGE_LOOP ( 'NONE', ( #77585, #31492, #36865, #6330, #83555, #67936, #28793, #59283, #72779, #50624, #22039, #35773, #46577, #9518, #46822, #44940, #81337, #55003, #35407, #38635, #45737, #89444, #78842, #35068, #54364, #80576, #33824, #81148, #39578, #5470, #6081, #81201, #32209, #52708, #20447, #11272, #32933, #88910, #65918, #39428, #19239, #78938, #5419, #1682, #11630, #47712, #43896, #77294 ) ) ;
#88725 = AXIS2_PLACEMENT_3D ( 'NONE', #55632, #83380, #76563 ) ;
#88726 = CARTESIAN_POINT ( 'NONE',  ( -194.1576000000000022, 101.5999999999999943, 114.2999999999999972 ) ) ;
#88727 = DIRECTION ( 'NONE',  ( -1.000000000000000000, -4.299999999999999979E-14, -1.000000000000000078E-15 ) ) ;
#88728 = CARTESIAN_POINT ( 'NONE',  ( 134.0664828118826506, -39.47944715903992829, 8.225259175038003079 ) ) ;
#88729 = AXIS2_PLACEMENT_3D ( 'NONE', #22520, #77933, #62493 ) ;
#88730 = CARTESIAN_POINT ( 'NONE',  ( 106.6371065190374452, -28.08557299187883061, 42.94618560768698501 ) ) ;
#88731 = CARTESIAN_POINT ( 'NONE',  ( 113.3444227873369243, -45.07958072982976461, 139.0899109901969553 ) ) ;
#88732 = LINE ( 'NONE', #26487, #66734 ) ;
#88733 = ORIENTED_EDGE ( 'NONE', *, *, #42063, .T. ) ;
#88734 = EDGE_CURVE ( 'NONE', #16097, #12031, #72466, .T. ) ;
#88735 = DIRECTION ( 'NONE',  ( 1.000000000000000000, 4.299999999999999979E-14, 1.000000000000000078E-15 ) ) ;
#88736 = CARTESIAN_POINT ( 'NONE',  ( 97.91842249762910910, -40.76970847486229843, 66.65793780748323627 ) ) ;
#88737 = ORIENTED_EDGE ( 'NONE', *, *, #60442, .F. ) ;
#88738 = ORIENTED_EDGE ( 'NONE', *, *, #43669, .T. ) ;
#88739 = EDGE_CURVE ( 'NONE', #71630, #11403, #88032, .T. ) ;
#88740 = DIRECTION ( 'NONE',  ( 1.000000000000000078E-15, -1.000000000000000083E-30, -1.000000000000000000 ) ) ;
#88741 = ORIENTED_EDGE ( 'NONE', *, *, #54718, .T. ) ;
#88742 = ORIENTED_EDGE ( 'NONE', *, *, #89515, .T. ) ;
#88743 = CARTESIAN_POINT ( 'NONE',  ( 32.15435173583699680, -31.62489322948790971, -5.074374724088000832 ) ) ;
#88744 = CARTESIAN_POINT ( 'NONE',  ( 114.0365971503568119, -41.66641429710976752, 52.75813411379098739 ) ) ;
#88745 = CARTESIAN_POINT ( 'NONE',  ( 96.99510461011969653, -33.95209312647379818, 251.1127681330538337 ) ) ;
#88746 = AXIS2_PLACEMENT_3D ( 'NONE', #16387, #65422, #22763 ) ;
#88747 = CARTESIAN_POINT ( 'NONE',  ( 102.9757002774701959, -26.48594595611781344, 175.3908633711489813 ) ) ;
#88749 = CARTESIAN_POINT ( 'NONE',  ( 96.68076663292312389, -33.01451620012166899, 22.06514908543494258 ) ) ;
#88748 = CARTESIAN_POINT ( 'NONE',  ( 74.56648329127402519, -41.22944715994105991, 4.925625275910938683 ) ) ;
#88750 = CYLINDRICAL_SURFACE ( 'NONE', #27460, 0.5000000000000073275 ) ;
#88751 = CARTESIAN_POINT ( 'NONE',  ( -53.64297985755450782, 53.97500000000000142, 70.79999999999999716 ) ) ;
#88752 = EDGE_LOOP ( 'NONE', ( #923, #20421, #63256, #43668, #12976, #48904, #62622, #73132, #66742, #73127, #84630, #86744, #60084, #24915 ) ) ;
#88753 = AXIS2_PLACEMENT_3D ( 'NONE', #51659, #31221, #16718 ) ;
#88754 = PRESENTATION_LAYER_ASSIGNMENT (  '', '', ( #43804 ) ) ;
#88755 = CARTESIAN_POINT ( 'NONE',  ( 97.86673394820853389, -40.64959261906454202, 111.6470208298959363 ) ) ;
#88756 = CARTESIAN_POINT ( 'NONE',  ( 96.81521419041753518, -34.60385362728553815, 216.1641967044819808 ) ) ;
#88757 = ORIENTED_EDGE ( 'NONE', *, *, #26315, .T. ) ;
#88758 = CARTESIAN_POINT ( 'NONE',  ( 109.6058900474308757, -26.58167301968400764, 199.8813395616249977 ) ) ;
#88759 = CARTESIAN_POINT ( 'NONE',  ( 63.03715912545735023, -24.42818131006017879, 249.9678068554150343 ) ) ;
#88760 = FILL_AREA_STYLE_COLOUR ( '', #8595 ) ;
#88761 = LINE ( 'NONE', #5643, #74020 ) ;
#88762 = LINE ( 'NONE', #82851, #67374 ) ;
#88763 = EDGE_CURVE ( 'NONE', #121, #32410, #35573, .T. ) ;
#88765 = CARTESIAN_POINT ( 'NONE',  ( 172.5664832912729878, -27.82844715994070484, 18.92562527591200094 ) ) ;
#88764 = CARTESIAN_POINT ( 'NONE',  ( 98.99084639576925326, -33.78646765538439922, 277.6356252759111385 ) ) ;
#88766 = DIRECTION ( 'NONE',  ( 0.000000000000000000, 1.000000000000000000, 0.000000000000000000 ) ) ;
#88767 = EDGE_CURVE ( 'NONE', #70410, #23818, #77369, .T. ) ;
#88768 = FACE_OUTER_BOUND ( 'NONE', #47973, .T. ) ;
#88769 = CARTESIAN_POINT ( 'NONE',  ( 92.81551872686563343, -113.5468731908973723, -19.18411693322874356 ) ) ;
#88770 = ADVANCED_FACE ( 'NONE', ( #70561 ), #8333, .T. ) ;
#88771 = DIRECTION ( 'NONE',  ( 0.000000000000000000, 0.000000000000000000, 1.000000000000000000 ) ) ;
#88772 = LINE ( 'NONE', #55543, #63364 ) ;
#88773 = FACE_OUTER_BOUND ( 'NONE', #38829, .T. ) ;
#88774 = AXIS2_PLACEMENT_3D ( 'NONE', #6791, #62203, #34491 ) ;
#88776 = ORIENTED_EDGE ( 'NONE', *, *, #14038, .F. ) ;
#88775 = CARTESIAN_POINT ( 'NONE',  ( -12.03238568418269594, 86.63481793440480772, -117.9438919316608150 ) ) ;
#88777 = EDGE_CURVE ( 'NONE', #47693, #49134, #50092, .T. ) ;
#88778 = DIRECTION ( 'NONE',  ( 1.000000000000000000, 0.000000000000000000, 0.000000000000000000 ) ) ;
#88779 = CARTESIAN_POINT ( 'NONE',  ( 115.4056828889858650, -30.43626719779562251, 219.3413395616249773 ) ) ;
#88780 = CARTESIAN_POINT ( 'NONE',  ( 117.8753414029365842, -39.04084647772175032, 104.6708633711489824 ) ) ;
#88781 = CARTESIAN_POINT ( 'NONE',  ( 96.72029611048706954, -35.13276604965626859, 262.2041967044821149 ) ) ;
#88782 = CARTESIAN_POINT ( 'NONE',  ( -44.45000000000000284, 114.2999999999999972, 275.4630000000000223 ) ) ;
#88783 = CARTESIAN_POINT ( 'NONE',  ( 131.0667039024480118, -58.72944715994093912, 210.8338068554149913 ) ) ;
#88785 = CARTESIAN_POINT ( 'NONE',  ( 89.06648138392553449, -56.72944715994104570, -4.824374724089047106 ) ) ;
#88784 = CARTESIAN_POINT ( 'NONE',  ( 237.9979999999999905, 52.73749999999999716, 10.66800000000000104 ) ) ;
#88786 = LINE ( 'NONE', #47862, #21903 ) ;
#88787 = CIRCLE ( 'NONE', #68479, 1.000000000000000888 ) ;
#88788 = CARTESIAN_POINT ( 'NONE',  ( 131.8552587341735318, -20.37463194332409699, 2.472581811075852176 ) ) ;
#88789 = EDGE_CURVE ( 'NONE', #38331, #15124, #80480, .T. ) ;
#88790 = CIRCLE ( 'NONE', #13429, 2.116999999999993776 ) ;
#88791 = ORIENTED_EDGE ( 'NONE', *, *, #73461, .T. ) ;
#88792 = ORIENTED_EDGE ( 'NONE', *, *, #61668, .F. ) ;
#88793 = ADVANCED_FACE ( 'NONE', ( #65524 ), #16936, .T. ) ;
#88794 = AXIS2_PLACEMENT_3D ( 'NONE', #48492, #68081, #81730 ) ;
#88795 = CARTESIAN_POINT ( 'NONE',  ( 103.4870123794286059, -45.04810440550495798, 136.6876579233149300 ) ) ;
#88797 = ORIENTED_EDGE ( 'NONE', *, *, #61403, .F. ) ;
#88796 = CARTESIAN_POINT ( 'NONE',  ( -48.02966122971774610, 65.60000000000000853, -43.00307561052233751 ) ) ;
#88798 = CARTESIAN_POINT ( 'NONE',  ( 112.1392171050070345, -28.01274908269051167, 89.65543061173896433 ) ) ;
#88799 = CARTESIAN_POINT ( 'NONE',  ( 109.1969564574039282, -26.54663071456431211, 135.9127681330539872 ) ) ;
#88800 = CARTESIAN_POINT ( 'NONE',  ( 162.9033555647770015, -33.89581943344391135, -5.074374724088000832 ) ) ;
#88801 = AXIS2_PLACEMENT_3D ( 'NONE', #60474, #46391, #66398 ) ;
#88802 = CARTESIAN_POINT ( 'NONE',  ( 143.7922156418627821, -137.6784471599409017, 222.2178068554179902 ) ) ;
#88803 = CARTESIAN_POINT ( 'NONE',  ( 48.86082318535673608, -35.55794170701784651, 313.9678068554150059 ) ) ;
#88804 = AXIS2_PLACEMENT_3D ( 'NONE', #3031, #30731, #86153 ) ;
#88805 = LINE ( 'NONE', #38838, #33826 ) ;
#88806 = CARTESIAN_POINT ( 'NONE',  ( 116.1466984671188385, -33.09446055034462120, 54.12991099019798469 ) ) ;
#88807 = ORIENTED_EDGE ( 'NONE', *, *, #4086, .T. ) ;
#88808 = ORIENTED_EDGE ( 'NONE', *, *, #52291, .F. ) ;
#88809 = ORIENTED_EDGE ( 'NONE', *, *, #28511, .F. ) ;
#88810 = CARTESIAN_POINT ( 'NONE',  ( 0.000000000000000000, 100.5999999999999659, 0.000000000000000000 ) ) ;
#88812 = CARTESIAN_POINT ( 'NONE',  ( 143.9834832912729894, -1.929447159941392931, 361.9756252759109998 ) ) ;
#88811 = CARTESIAN_POINT ( 'NONE',  ( 96.59955023297828802, -32.98040794253982000, 172.0527681330529788 ) ) ;
#88813 = CARTESIAN_POINT ( 'NONE',  ( 150.5667039024475571, -25.42844715993593852, 180.4678068554149775 ) ) ;
#88814 = DIRECTION ( 'NONE',  ( 0.000000000000000000, 1.000000000000000000, 0.000000000000000000 ) ) ;
#88815 = CYLINDRICAL_SURFACE ( 'NONE', #61942, 11.45913725231036118 ) ;
#88816 = DIRECTION ( 'NONE',  ( 1.000000000000000000, 0.000000000000000000, 0.000000000000000000 ) ) ;
#88817 = CARTESIAN_POINT ( 'NONE',  ( 41.56648329127398966, -18.82844715994071194, 255.9256252759120684 ) ) ;
#88818 = CARTESIAN_POINT ( 'NONE',  ( 111.0741232671659304, -25.60348521778444209, 99.80133956162498521 ) ) ;
#88819 = ORIENTED_EDGE ( 'NONE', *, *, #28672, .T. ) ;
#88820 = VERTEX_POINT ( 'NONE', #71906 ) ;
#88821 = ORIENTED_EDGE ( 'NONE', *, *, #6909, .F. ) ;
#88822 = CARTESIAN_POINT ( 'NONE',  ( 49.35031423293201414, -29.99615139349890569, -5.074374724088000832 ) ) ;
#88823 = FACE_OUTER_BOUND ( 'NONE', #78693, .T. ) ;
#88824 = AXIS2_PLACEMENT_3D ( 'NONE', #48408, #54775, #61168 ) ;
#88826 = ADVANCED_FACE ( 'NONE', ( #23761, #85989, #57814, #17820, #9229, #59138, #79620, #78735, #78287, #37829 ), #3747, .T. ) ;
#88825 = CARTESIAN_POINT ( 'NONE',  ( -147.4575741623270062, 101.5999999999999943, 135.2444258376732193 ) ) ;
#88827 = CARTESIAN_POINT ( 'NONE',  ( 100.4889591185686015, -31.84898980388015843, 178.6366617981629474 ) ) ;
#88828 = AXIS2_PLACEMENT_3D ( 'NONE', #2589, #43895, #16216 ) ;
#88829 = VECTOR ( 'NONE', #37783, 1000.000000000000000 ) ;
#88830 = CARTESIAN_POINT ( 'NONE',  ( 41.56648329127398966, -27.82844715994070484, 254.1756252759120400 ) ) ;
#88831 = ORIENTED_EDGE ( 'NONE', *, *, #64256, .T. ) ;
#88833 = ORIENTED_EDGE ( 'NONE', *, *, #9850, .T. ) ;
#88832 = ORIENTED_EDGE ( 'NONE', *, *, #32220, .T. ) ;
#88834 = LINE ( 'NONE', #67924, #84499 ) ;
#88835 = DIRECTION ( 'NONE',  ( 5.512527431108029424E-15, -1.000000000000000000, 0.000000000000000000 ) ) ;
#88836 = ORIENTED_EDGE ( 'NONE', *, *, #8151, .T. ) ;
#88837 = EDGE_LOOP ( 'NONE', ( #50351, #71542, #78533, #18598 ) ) ;
#88838 = CARTESIAN_POINT ( 'NONE',  ( 1.387778780781445676E-14, 239.0000000000000000, 97.27542076772557778 ) ) ;
#88839 = AXIS2_PLACEMENT_3D ( 'NONE', #45218, #80222, #86140 ) ;
#88840 = CARTESIAN_POINT ( 'NONE',  ( 110.1519232268686181, -46.31854332990749867, 204.2558690201829847 ) ) ;
#88841 = CARTESIAN_POINT ( 'NONE',  ( 25.56670390244797275, -48.82844715994099971, 295.9678068554150059 ) ) ;
#88842 = DIRECTION ( 'NONE',  ( 1.000000000000000078E-15, -1.000000000000000000, 0.000000000000000000 ) ) ;
#88843 = ORIENTED_EDGE ( 'NONE', *, *, #10443, .T. ) ;
#88844 = EDGE_LOOP ( 'NONE', ( #69051, #54970 ) ) ;
#88846 = ADVANCED_FACE ( 'NONE', ( #17377 ), #36929, .F. ) ;
#88845 = AXIS2_PLACEMENT_3D ( 'NONE', #584, #82839, #28284 ) ;
#88847 = CARTESIAN_POINT ( 'NONE',  ( 0.000000000000000000, 11.42999999999999972, -154.1697486074984909 ) ) ;
#88848 = ORIENTED_EDGE ( 'NONE', *, *, #7852, .F. ) ;
#88849 = ORIENTED_EDGE ( 'NONE', *, *, #59032, .T. ) ;
#88850 = VECTOR ( 'NONE', #17916, 1000.000000000000000 ) ;
#88851 = CARTESIAN_POINT ( 'NONE',  ( 107.4137727038933150, -44.88475929872373626, 235.4280903695919562 ) ) ;
#88852 = CARTESIAN_POINT ( 'NONE',  ( 114.7236970816665860, -44.73335358772728654, 113.1718157521009687 ) ) ;
#88853 = CARTESIAN_POINT ( 'NONE',  ( 96.10063762778146668, -37.91858611869022866, 81.40038718067299328 ) ) ;
#88854 = CARTESIAN_POINT ( 'NONE',  ( 105.4761177374140999, -44.76735112088204005, 249.5838068554172082 ) ) ;
#88855 = CARTESIAN_POINT ( 'NONE',  ( 131.8552587341665969, -17.08426237657134905, 7.378668740739960263 ) ) ;
#88856 = CARTESIAN_POINT ( 'NONE',  ( 31.71315051186898870, -31.94127993907790852, 313.9678068554150059 ) ) ;
#88857 = CARTESIAN_POINT ( 'NONE',  ( 113.6855667929701923, -45.58166236755234024, 184.0994347997199725 ) ) ;
#88858 = CARTESIAN_POINT ( 'NONE',  ( 102.6998691488477249, -45.78651595893203563, 277.2188344857675020 ) ) ;
#88859 = ORIENTED_EDGE ( 'NONE', *, *, #15240, .F. ) ;
#88860 = DIRECTION ( 'NONE',  ( 0.000000000000000000, 0.000000000000000000, -1.000000000000000000 ) ) ;
#88861 = ORIENTED_EDGE ( 'NONE', *, *, #78519, .F. ) ;
#88862 = VERTEX_POINT ( 'NONE', #72350 ) ;
#88863 = CARTESIAN_POINT ( 'NONE',  ( 74.06670390244704549, -118.2784471599409812, 45.21780685541799727 ) ) ;
#88864 = ORIENTED_EDGE ( 'NONE', *, *, #84809, .T. ) ;
#88865 = DIRECTION ( 'NONE',  ( -1.000000000000000078E-15, 1.000000000000000083E-30, 1.000000000000000000 ) ) ;
#88866 = CARTESIAN_POINT ( 'NONE',  ( 113.2424586320066169, -28.75634830710533407, 90.55259365063709254 ) ) ;
#88867 = CARTESIAN_POINT ( 'NONE',  ( 103.3623838164489541, -47.14379949381606849, 102.3165776568629752 ) ) ;
#88868 = CARTESIAN_POINT ( 'NONE',  ( -4.682505845377153975, 70.74451999347890307, 130.4720125505715487 ) ) ;
#88869 = CARTESIAN_POINT ( 'NONE',  ( 136.7978637535026678, -36.40984252624616602, 6.777538624683693058 ) ) ;
#88870 = FACE_OUTER_BOUND ( 'NONE', #13266, .T. ) ;
#88873 = CARTESIAN_POINT ( 'NONE',  ( 115.4997179687694171, -29.61999039777962039, 220.3718157521019521 ) ) ;
#88872 = CYLINDRICAL_SURFACE ( 'NONE', #68828, 7.199999999999998401 ) ;
#88871 = CARTESIAN_POINT ( 'NONE',  ( -254.0000000000000000, 3.174999999999999822, -41.27499999999999858 ) ) ;
#88874 = CARTESIAN_POINT ( 'NONE',  ( 107.0667039024479834, -48.82844715994099971, 160.9178068554150229 ) ) ;
#88875 = ADVANCED_FACE ( 'NONE', ( #23327 ), #9664, .T. ) ;
#88876 = LINE ( 'NONE', #53411, #81600 ) ;
#88877 = ORIENTED_EDGE ( 'NONE', *, *, #58100, .T. ) ;
#88878 = DIRECTION ( 'NONE',  ( 1.000000000000000078E-15, -1.000000000000000083E-30, -1.000000000000000000 ) ) ;
#88879 = VECTOR ( 'NONE', #34822, 1000.000000000000000 ) ;
#88880 = EDGE_CURVE ( 'NONE', #88630, #77919, #10555, .T. ) ;
#88881 = DIRECTION ( 'NONE',  ( 0.7071067811861728725, -0.7071067811869222730, 0.000000000000000000 ) ) ;
#88882 = ADVANCED_FACE ( 'NONE', ( #52300 ), #69961, .T. ) ;
#88883 = CARTESIAN_POINT ( 'NONE',  ( 126.8164832912740394, -46.47944715994101017, -5.074374724089010691 ) ) ;
#88884 = CYLINDRICAL_SURFACE ( 'NONE', #53483, 0.5000000000000172085 ) ;
#88886 = ORIENTED_EDGE ( 'NONE', *, *, #33476, .T. ) ;
#88885 = CARTESIAN_POINT ( 'NONE',  ( 101.2695147780440266, -26.33598991146258328, 255.4813395616251626 ) ) ;
#88887 = EDGE_CURVE ( 'NONE', #79111, #41648, #15933, .T. ) ;
#88888 = DIRECTION ( 'NONE',  ( 0.000000000000000000, 1.000000000000000000, 0.000000000000000000 ) ) ;
#88889 = CARTESIAN_POINT ( 'NONE',  ( 116.4744410436840383, -32.23804052137624865, 15.18133956162492915 ) ) ;
#88890 = CARTESIAN_POINT ( 'NONE',  ( 98.13109353019112291, -31.27492705589930821, 166.8899109901969950 ) ) ;
#88891 = DIRECTION ( 'NONE',  ( 1.000000000000000078E-15, 0.000000000000000000, -1.000000000000000000 ) ) ;
#88892 = CARTESIAN_POINT ( 'NONE',  ( 97.07207337491342969, -35.37841122429128404, 102.2188882665558083 ) ) ;
#88894 = CYLINDRICAL_SURFACE ( 'NONE', #76206, 9.999999999999998224 ) ;
#88893 = CARTESIAN_POINT ( 'NONE',  ( 68.06670390244705970, -121.7784471599409954, 45.21780685541799727 ) ) ;
#88895 = PLANE ( 'NONE',  #45210 ) ;
#88896 = CARTESIAN_POINT ( 'NONE',  ( 20.03715912545820288, -46.82818131006190043, 300.4678068554150059 ) ) ;
#88897 = ORIENTED_EDGE ( 'NONE', *, *, #41219, .T. ) ;
#88898 = VECTOR ( 'NONE', #52253, 1000.000000000000000 ) ;
#88899 = ORIENTED_EDGE ( 'NONE', *, *, #74707, .T. ) ;
#88900 = VERTEX_POINT ( 'NONE', #14556 ) ;
#88901 = EDGE_CURVE ( 'NONE', #5885, #40068, #79739, .T. ) ;
#88902 = ORIENTED_EDGE ( 'NONE', *, *, #24879, .T. ) ;
#88903 = DIRECTION ( 'NONE',  ( 0.000000000000000000, 1.000000000000000000, 0.000000000000000000 ) ) ;
#88904 = CARTESIAN_POINT ( 'NONE',  ( 118.0600790064083299, -37.62648441163795354, 34.77372051400695341 ) ) ;
#88905 = CARTESIAN_POINT ( 'NONE',  ( 129.9869660233263744, -139.6169024007319024, 247.4725286609620127 ) ) ;
#88906 = CARTESIAN_POINT ( 'NONE',  ( 71.24189083761808661, -0.9290567490904538817, 394.9756252759101471 ) ) ;
#88907 = DIRECTION ( 'NONE',  ( 0.000000000000000000, 0.000000000000000000, -1.000000000000000000 ) ) ;
#88908 = CARTESIAN_POINT ( 'NONE',  ( 98.42407572851979580, -32.30458340910843162, 245.3724198280769428 ) ) ;
#88909 = ORIENTED_EDGE ( 'NONE', *, *, #56847, .T. ) ;
#88910 = ORIENTED_EDGE ( 'NONE', *, *, #82632, .F. ) ;
#88911 = ORIENTED_EDGE ( 'NONE', *, *, #7044, .T. ) ;
#88912 = AXIS2_PLACEMENT_3D ( 'NONE', #11780, #41248, #19936 ) ;
#88913 = LINE ( 'NONE', #33928, #45635 ) ;
#88914 = CARTESIAN_POINT ( 'NONE',  ( 98.54785118950427147, -41.97730404426498296, 101.7661766900147597 ) ) ;
#88915 = CARTESIAN_POINT ( 'NONE',  ( 107.0664832912739541, -20.72944715994095333, 311.3356252759109566 ) ) ;
#88916 = DIRECTION ( 'NONE',  ( 1.000000000000000078E-15, 0.000000000000000000, 1.000000000000000000 ) ) ;
#88917 = AXIS2_PLACEMENT_3D ( 'NONE', #13794, #55539, #70557 ) ;
#88918 = DIRECTION ( 'NONE',  ( 0.000000000000000000, 0.000000000000000000, 1.000000000000000000 ) ) ;
#88919 = FACE_OUTER_BOUND ( 'NONE', #35215, .T. ) ;
#88920 = CARTESIAN_POINT ( 'NONE',  ( 112.0813997088635858, -45.80630777137071874, 252.9661014663878689 ) ) ;
#88921 = DIRECTION ( 'NONE',  ( 0.7967329428042202455, -0.6043315462976655006, 1.908195823574484964E-14 ) ) ;
#88922 = ORIENTED_EDGE ( 'NONE', *, *, #41193, .F. ) ;
#88923 = FACE_OUTER_BOUND ( 'NONE', #49225, .T. ) ;
#88925 = ADVANCED_FACE ( 'NONE', ( #36335, #57205 ), #78586, .T. ) ;
#88924 = DIRECTION ( 'NONE',  ( 0.000000000000000000, 1.000000000000000000, 0.000000000000000000 ) ) ;
#88926 = CARTESIAN_POINT ( 'NONE',  ( 113.1369140564456615, -42.18651563507969371, 36.06237608387696980 ) ) ;
#88927 = CARTESIAN_POINT ( 'NONE',  ( 97.81067182961875517, -40.51494070217739107, 131.6354111825010307 ) ) ;
#88928 = EDGE_CURVE ( 'NONE', #82506, #56272, #40545, .T. ) ;
#88929 = DIRECTION ( 'NONE',  ( -3.100000000000000258E-29, 3.100000000000000044E-14, 1.000000000000000000 ) ) ;
#88930 = CARTESIAN_POINT ( 'NONE',  ( 179.8585841295807484, -30.08671355699668126, 193.9678068554150059 ) ) ;
#88931 = VERTEX_POINT ( 'NONE', #76769 ) ;
#88932 = CARTESIAN_POINT ( 'NONE',  ( 79.69020591997146141, -33.99866847873249043, 8.209451181319794344 ) ) ;
#88933 = AXIS2_PLACEMENT_3D ( 'NONE', #77963, #79310, #57946 ) ;
#88934 = ORIENTED_EDGE ( 'NONE', *, *, #77098, .T. ) ;
#88935 = CARTESIAN_POINT ( 'NONE',  ( 117.2382404677042729, -39.01746902538002360, 148.6499109901969859 ) ) ;
#88936 = ORIENTED_EDGE ( 'NONE', *, *, #50337, .T. ) ;
#88937 = CARTESIAN_POINT ( 'NONE',  ( 98.71159061831248493, -42.24584867631038065, 87.79035904436562987 ) ) ;
#88938 = CARTESIAN_POINT ( 'NONE',  ( 108.6971488411468414, -45.98241724535997577, 119.1349166392299566 ) ) ;
#88939 = PLANE ( 'NONE',  #14192 ) ;
#88940 = CARTESIAN_POINT ( 'NONE',  ( 99.06670390244704549, -104.2784471599421323, -21.78219314458201694 ) ) ;
#88941 = CARTESIAN_POINT ( 'NONE',  ( 110.8022603587792219, -46.48553390388831019, 58.86705384733998159 ) ) ;
#88942 = CARTESIAN_POINT ( 'NONE',  ( 100.9549047852691785, -28.70684421539622377, 181.5944067750197064 ) ) ;
#88943 = VECTOR ( 'NONE', #11599, 1000.000000000000000 ) ;
#88944 = DIRECTION ( 'NONE',  ( -0.9770521142508956647, -1.387778780781445676E-17, 0.2130003897598659324 ) ) ;
#88945 = VERTEX_POINT ( 'NONE', #49491 ) ;
#88946 = ADVANCED_FACE ( 'NONE', ( #78136 ), #23178, .T. ) ;
#88947 = CARTESIAN_POINT ( 'NONE',  ( 162.7131505118539962, -33.70561438052090608, -5.074374724088000832 ) ) ;
#88948 = ORIENTED_EDGE ( 'NONE', *, *, #89482, .F. ) ;
#88949 = ORIENTED_EDGE ( 'NONE', *, *, #53298, .F. ) ;
#88950 = CARTESIAN_POINT ( 'NONE',  ( 33.98325472291465132, 24.56180297284579694, 3.174999999999999822 ) ) ;
#88951 = EDGE_LOOP ( 'NONE', ( #69896, #85870, #82661, #55185 ) ) ;
#88952 = CARTESIAN_POINT ( 'NONE',  ( 99.34779341711919187, -29.80408710710932496, 235.7565776568639819 ) ) ;
#88953 = CARTESIAN_POINT ( 'NONE',  ( 97.77490566832175034, -42.75910828249967466, 142.7965776568629508 ) ) ;
#88954 = CARTESIAN_POINT ( 'NONE',  ( 165.9667039024459996, -28.27351298637401200, 342.9256252759119548 ) ) ;
#88955 = LINE ( 'NONE', #82159, #56139 ) ;
#88956 = CARTESIAN_POINT ( 'NONE',  ( 109.6838526317122273, -47.46831852615197533, 83.75467289495897205 ) ) ;
#88957 = CARTESIAN_POINT ( 'NONE',  ( 115.0918025260861555, -30.62139641523929967, 95.34367351736931084 ) ) ;
#88958 = EDGE_LOOP ( 'NONE', ( #32296, #21009, #66950, #26110 ) ) ;
#88959 = CARTESIAN_POINT ( 'NONE',  ( 48.79742451362075428, -36.32844715994075813, 313.9678068554150059 ) ) ;
#88960 = EDGE_CURVE ( 'NONE', #6301, #82784, #43619, .T. ) ;
#88961 = DIRECTION ( 'NONE',  ( -1.000000000000000000, 0.000000000000000000, 0.000000000000000000 ) ) ;
#88962 = VERTEX_POINT ( 'NONE', #7288 ) ;
#88963 = CIRCLE ( 'NONE', #38247, 0.3000000000000016542 ) ;
#88964 = CARTESIAN_POINT ( 'NONE',  ( 138.0667039024470171, -104.2784471599409244, 25.71780685541800437 ) ) ;
#88965 = CARTESIAN_POINT ( 'NONE',  ( 142.8682495647594521, 8.654319075478440482, 542.9756252759101471 ) ) ;
#88966 = CARTESIAN_POINT ( 'NONE',  ( 106.2286657330468103, -47.72771449247521502, 267.5280062282920994 ) ) ;
#88967 = DIRECTION ( 'NONE',  ( 0.000000000000000000, 0.000000000000000000, 1.000000000000000000 ) ) ;
#88968 = VECTOR ( 'NONE', #73644, 1000.000000000000000 ) ;
#88969 = DIRECTION ( 'NONE',  ( 9.351236661543306751E-17, -3.725950533538267725E-29, -1.000000000000000000 ) ) ;
#88970 = CARTESIAN_POINT ( 'NONE',  ( 107.0664832912739968, -36.72944715994100306, 287.6356252759109680 ) ) ;
#88971 = CARTESIAN_POINT ( 'NONE',  ( 97.32756240343553600, -42.09278592120095652, 26.72705384733997747 ) ) ;
#88973 = CARTESIAN_POINT ( 'NONE',  ( 118.8789388927531974, -36.16900092901214947, 114.8641967044819694 ) ) ;
#88972 = DIRECTION ( 'NONE',  ( 0.000000000000000000, 0.000000000000000000, -1.000000000000000000 ) ) ;
#88974 = DIRECTION ( 'NONE',  ( 2.999999999999999839E-15, -1.000000000000000000, 2.999999999999999900E-30 ) ) ;
#88975 = CARTESIAN_POINT ( 'NONE',  ( 117.0653594338693892, -39.95035295773606521, 158.5784824187679476 ) ) ;
#88976 = ORIENTED_EDGE ( 'NONE', *, *, #84286, .F. ) ;
#88977 = CARTESIAN_POINT ( 'NONE',  ( 103.3797721312301547, -105.8297479413476196, 2.217806855418058554 ) ) ;
#88978 = ORIENTED_EDGE ( 'NONE', *, *, #79312, .T. ) ;
#88979 = CARTESIAN_POINT ( 'NONE',  ( 0.000000000000000000, 215.0000000000000000, 154.6557476874258441 ) ) ;
#88980 = DIRECTION ( 'NONE',  ( 0.000000000000000000, -1.000000000000000000, 0.000000000000000000 ) ) ;
#88981 = CARTESIAN_POINT ( 'NONE',  ( 135.9759635523953420, -34.74831825237850325, 2.232988539019887142 ) ) ;
#88983 = ORIENTED_EDGE ( 'NONE', *, *, #15771, .T. ) ;
#88982 = EDGE_CURVE ( 'NONE', #8076, #36762, #29968, .T. ) ;
#88984 = LINE ( 'NONE', #54871, #12820 ) ;
#88986 = VERTEX_POINT ( 'NONE', #43575 ) ;
#88985 = CARTESIAN_POINT ( 'NONE',  ( 108.7503283313270543, -25.75779200005056779, 144.9432443235299672 ) ) ;
#88987 = LINE ( 'NONE', #26746, #65433 ) ;
#88988 = CARTESIAN_POINT ( 'NONE',  ( -130.2064250969985153, 90.93081950567959382, 9.551273559374726219 ) ) ;
#88989 = CARTESIAN_POINT ( 'NONE',  ( 0.000000000000000000, 65.60000000000000853, 0.000000000000000000 ) ) ;
#88990 = DIRECTION ( 'NONE',  ( 0.000000000000000000, 0.000000000000000000, 1.000000000000000000 ) ) ;
#88991 = VERTEX_POINT ( 'NONE', #9082 ) ;
#88992 = PRODUCT_CONTEXT ( 'NONE', #13854, 'mechanical' ) ;
#88993 = CIRCLE ( 'NONE', #35284, 3.000000000000002665 ) ;
#88994 = ORIENTED_EDGE ( 'NONE', *, *, #33806, .F. ) ;
#88995 = VERTEX_POINT ( 'NONE', #71314 ) ;
#88996 = ADVANCED_BREP_SHAPE_REPRESENTATION ( '', ( #47652, #50656 ), #27649 ) ;
#88997 = EDGE_CURVE ( 'NONE', #66809, #11502, #463, .T. ) ;
#88998 = VECTOR ( 'NONE', #9251, 999.9999999999998863 ) ;
#88999 = ORIENTED_EDGE ( 'NONE', *, *, #13908, .T. ) ;
#89000 = CARTESIAN_POINT ( 'NONE',  ( 163.1639762274590169, -34.03355364505800651, 117.4678068554150485 ) ) ;
#89001 = CARTESIAN_POINT ( 'NONE',  ( 104.6691943795874096, -26.96177962471290002, 250.2678212403098712 ) ) ;
#89002 = EDGE_CURVE ( 'NONE', #67994, #24090, #63777, .T. ) ;
#89003 = DIRECTION ( 'NONE',  ( 0.000000000000000000, 0.000000000000000000, -1.000000000000000000 ) ) ;
#89004 = DIRECTION ( 'NONE',  ( -0.7071067811865165975, -0.7071067811865784369, -7.071067811865158803E-16 ) ) ;
#89006 = DIRECTION ( 'NONE',  ( -1.000000000000000078E-15, 0.000000000000000000, 1.000000000000000000 ) ) ;
#89005 = LINE ( 'NONE', #26759, #75543 ) ;
#89007 = CARTESIAN_POINT ( 'NONE',  ( 97.60796736720944011, -39.98265213332607004, 181.5900836763981943 ) ) ;
#89008 = CIRCLE ( 'NONE', #20858, 17.33514202138210791 ) ;
#89009 = ORIENTED_EDGE ( 'NONE', *, *, #4054, .F. ) ;
#89010 = CARTESIAN_POINT ( 'NONE',  ( 57.56670390244747892, -48.82844715994040286, 137.2178068554150911 ) ) ;
#89011 = CARTESIAN_POINT ( 'NONE',  ( 172.5664832912740110, -32.07844715994070839, 83.67562527591201160 ) ) ;
#89012 = CARTESIAN_POINT ( 'NONE',  ( 112.8396959964675972, -44.62460075896464673, 224.0784824187679476 ) ) ;
#89014 = ORIENTED_EDGE ( 'NONE', *, *, #88153, .F. ) ;
#89013 = LINE ( 'NONE', #54454, #80646 ) ;
#89015 = CARTESIAN_POINT ( 'NONE',  ( 96.76615086495803553, -37.93025403122315709, 82.43086337114895912 ) ) ;
#89016 = DIRECTION ( 'NONE',  ( 1.000000000000000000, -6.938893903907222067E-14, 0.000000000000000000 ) ) ;
#89017 = DIRECTION ( 'NONE',  ( 0.000000000000000000, 0.000000000000000000, 1.000000000000000000 ) ) ;
#89018 = DIRECTION ( 'NONE',  ( 1.639958061481212836E-42, -4.100000000000000342E-29, -1.000000000000000000 ) ) ;
#89019 = ORIENTED_EDGE ( 'NONE', *, *, #24837, .T. ) ;
#89020 = CARTESIAN_POINT ( 'NONE',  ( 4.163101094985349692E-14, 120.6499999999999915, -107.7702177616926065 ) ) ;
#89021 = ORIENTED_EDGE ( 'NONE', *, *, #10243, .F. ) ;
#89022 = ORIENTED_EDGE ( 'NONE', *, *, #27551, .T. ) ;
#89023 = CARTESIAN_POINT ( 'NONE',  ( 98.91186986371705814, -40.27407823153063759, 228.0844404487539805 ) ) ;
#89024 = VECTOR ( 'NONE', #66169, 999.9999999999998863 ) ;
#89025 = CARTESIAN_POINT ( 'NONE',  ( 98.38035888927598194, -41.69516708799280735, 52.73934900735942932 ) ) ;
#89026 = CARTESIAN_POINT ( 'NONE',  ( -118.5538584119706798, 95.23005795263748041, -0.8256312046391705017 ) ) ;
#89027 = AXIS2_PLACEMENT_3D ( 'NONE', #77242, #21380, #42248 ) ;
#89028 = EDGE_CURVE ( 'NONE', #68284, #79540, #37718, .T. ) ;
#89029 = CARTESIAN_POINT ( 'NONE',  ( 104.4081005625954361, -46.45808911397131169, 153.3647919345398236 ) ) ;
#89030 = B_SPLINE_CURVE_WITH_KNOTS ( 'NONE', 1,
 ( #45994, #73726 ),
 .UNSPECIFIED., .F., .F.,
 ( 2, 2 ),
 ( 0.000000000000000000, 0.002370257936674861985 ),
 .UNSPECIFIED. ) ;
#89031 = DIRECTION ( 'NONE',  ( 4.299999999999999979E-14, -1.000000000000000000, 0.000000000000000000 ) ) ;
#89032 = EDGE_LOOP ( 'NONE', ( #12972, #86916, #40377, #45184, #68704, #50405, #29318, #34022, #53447, #67135, #77959 ) ) ;
#89033 = LINE ( 'NONE', #7263, #42057 ) ;
#89034 = LINE ( 'NONE', #26795, #41181 ) ;
#89035 = ORIENTED_EDGE ( 'NONE', *, *, #49065, .T. ) ;
#89036 = CARTESIAN_POINT ( 'NONE',  ( 110.2841844748215578, -46.64581212076017636, 12.82705384733995402 ) ) ;
#89037 = VERTEX_POINT ( 'NONE', #1821 ) ;
#89038 = CARTESIAN_POINT ( 'NONE',  ( 115.2289877667042930, -36.78642703073501252, 261.6395189410197872 ) ) ;
#89039 = CARTESIAN_POINT ( 'NONE',  ( 41.56648329127398966, -27.82844715994070484, 75.92562527591199739 ) ) ;
#89040 = CARTESIAN_POINT ( 'NONE',  ( 108.6395843534182291, -26.47938140272615470, 144.9432443235309904 ) ) ;
#89041 = LINE ( 'NONE', #19098, #44749 ) ;
#89042 = DIRECTION ( 'NONE',  ( 0.000000000000000000, 1.000000000000000000, 0.000000000000000000 ) ) ;
#89043 = DIRECTION ( 'NONE',  ( 1.639958061481212836E-42, -4.100000000000000342E-29, -1.000000000000000000 ) ) ;
#89044 = CARTESIAN_POINT ( 'NONE',  ( 7.060824191845354036, 71.99373330411334848, 130.3649258744253245 ) ) ;
#89045 = CARTESIAN_POINT ( 'NONE',  ( 106.5652502036378593, -47.22167190867460818, 243.5384824187679556 ) ) ;
#89046 = DIRECTION ( 'NONE',  ( 1.000000000000000000, 0.000000000000000000, 0.000000000000000000 ) ) ;
#89047 = ORIENTED_EDGE ( 'NONE', *, *, #4090, .F. ) ;
#89048 = AXIS2_PLACEMENT_3D ( 'NONE', #31819, #87691, #33171 ) ;
#89049 = CARTESIAN_POINT ( 'NONE',  ( 104.7499416563296961, -46.93859083614567140, 68.39848241876794077 ) ) ;
#89050 = EDGE_CURVE ( 'NONE', #73456, #52361, #73942, .T. ) ;
#89051 = LINE ( 'NONE', #73626, #41009 ) ;
#89052 = VECTOR ( 'NONE', #37621, 1000.000000000000000 ) ;
#89053 = ORIENTED_EDGE ( 'NONE', *, *, #80773, .F. ) ;
#89055 = EDGE_CURVE ( 'NONE', #27791, #19557, #1408, .T. ) ;
#89054 = ORIENTED_EDGE ( 'NONE', *, *, #3523, .F. ) ;
#89056 = ORIENTED_EDGE ( 'NONE', *, *, #52291, .T. ) ;
#89057 = ADVANCED_FACE ( 'NONE', ( #10409 ), #31286, .F. ) ;
#89058 = TOROIDAL_SURFACE ( 'NONE', #13581, 13.50000000000000000, 0.5000000000000000000 ) ;
#89059 = CARTESIAN_POINT ( 'NONE',  ( 97.06112134132980884, -37.99667316087749924, 161.4271097635434558 ) ) ;
#89060 = CARTESIAN_POINT ( 'NONE',  ( 0.000000000000000000, 65.60000000000000853, 0.000000000000000000 ) ) ;
#89061 = PLANE ( 'NONE',  #49440 ) ;
#89062 = DIRECTION ( 'NONE',  ( 0.000000000000000000, 0.000000000000000000, 1.000000000000000000 ) ) ;
#89063 = CARTESIAN_POINT ( 'NONE',  ( 103.8567473457716375, -28.69212669812176841, 173.2090427505439720 ) ) ;
#89064 = CARTESIAN_POINT ( 'NONE',  ( 115.7133342524696360, -42.59197454220085177, 269.3527681330536439 ) ) ;
#89065 = EDGE_CURVE ( 'NONE', #15997, #33670, #17672, .T. ) ;
#89066 = DIRECTION ( 'NONE',  ( 0.000000000000000000, 0.000000000000000000, 1.000000000000000000 ) ) ;
#89067 = VERTEX_POINT ( 'NONE', #79918 ) ;
#89068 = CARTESIAN_POINT ( 'NONE',  ( 130.3837941446096522, 93.33921197991989516, 6.712224447895777324 ) ) ;
#89069 = EDGE_CURVE ( 'NONE', #40033, #14287, #52154, .T. ) ;
#89070 = CARTESIAN_POINT ( 'NONE',  ( 131.0667039024480687, -51.22944715994093201, 207.5838068554170377 ) ) ;
#89071 = EDGE_LOOP ( 'NONE', ( #6665, #54682, #13004, #36670 ) ) ;
#89072 = VERTEX_POINT ( 'NONE', #45350 ) ;
#89073 = EDGE_CURVE ( 'NONE', #61623, #75367, #81595, .T. ) ;
#89074 = CARTESIAN_POINT ( 'NONE',  ( 113.5015236877821962, -87.59835267194286246, -9.274842254011153031 ) ) ;
#89075 = ORIENTED_EDGE ( 'NONE', *, *, #45610, .F. ) ;
#89076 = ORIENTED_EDGE ( 'NONE', *, *, #88236, .F. ) ;
#89077 = DIRECTION ( 'NONE',  ( 0.9242245927363033076, 0.3818493186865917766, 0.000000000000000000 ) ) ;
#89078 = CARTESIAN_POINT ( 'NONE',  ( -9.275599959524004845, 73.86527412294591954, -130.2264118494045420 ) ) ;
#89079 = EDGE_CURVE ( 'NONE', #82011, #17885, #60904, .T. ) ;
#89080 = PLANE ( 'NONE',  #15869 ) ;
#89081 = CARTESIAN_POINT ( 'NONE',  ( -446.0240000000000009, 53.97500000000000142, 50.79999999999999716 ) ) ;
#89082 = CARTESIAN_POINT ( 'NONE',  ( 98.53214291706959216, -37.07752924029257713, 160.7809912566479511 ) ) ;
#89083 = CARTESIAN_POINT ( 'NONE',  ( 112.8421283165351809, -27.25026954951128388, 49.62895860924498947 ) ) ;
#89084 = ORIENTED_EDGE ( 'NONE', *, *, #76985, .F. ) ;
#89085 = FACE_OUTER_BOUND ( 'NONE', #55282, .T. ) ;
#89086 = ORIENTED_EDGE ( 'NONE', *, *, #14063, .F. ) ;
#89087 = CARTESIAN_POINT ( 'NONE',  ( -81.47036787067818864, 70.27763793881258891, -86.12934247706263591 ) ) ;
#89089 = VERTEX_POINT ( 'NONE', #4035 ) ;
#89088 = ADVANCED_FACE ( 'NONE', ( #38549 ), #65375, .F. ) ;
#89090 = DIRECTION ( 'NONE',  ( 0.000000000000000000, -1.000000000000000000, 0.000000000000000000 ) ) ;
#89091 = ORIENTED_EDGE ( 'NONE', *, *, #72210, .T. ) ;
#89092 = CARTESIAN_POINT ( 'NONE',  ( 114.2890383888417034, -29.74243919954670190, 165.4383927227787296 ) ) ;
#89093 = CARTESIAN_POINT ( 'NONE',  ( 138.0264040502034391, -139.2425132489394457, 247.5112265945669776 ) ) ;
#89094 = CYLINDRICAL_SURFACE ( 'NONE', #35931, 3.250000000000002665 ) ;
#89095 = VECTOR ( 'NONE', #21519, 1000.000000000000000 ) ;
#89096 = CARTESIAN_POINT ( 'NONE',  ( 163.1543517358360020, -31.62489322948790971, 117.4678068554150485 ) ) ;
#89097 = ORIENTED_EDGE ( 'NONE', *, *, #27474, .T. ) ;
#89098 = CARTESIAN_POINT ( 'NONE',  ( 115.5918606122963439, -42.76801532637115599, 53.33562527591095659 ) ) ;
#89099 = CARTESIAN_POINT ( 'NONE',  ( 117.0955297935745705, -31.97384786926005873, 60.19086337114898555 ) ) ;
#89100 = VECTOR ( 'NONE', #40919, 1000.000000000000000 ) ;
#89102 = CARTESIAN_POINT ( 'NONE',  ( 47.62500000000000000, 73.02500000000000568, 257.1750000000000114 ) ) ;
#89101 = CARTESIAN_POINT ( 'NONE',  ( 29.56670390244797630, -67.87844715994100397, 10.91780685541479734 ) ) ;
#89103 = CARTESIAN_POINT ( 'NONE',  ( 105.7995310142117660, -26.72403331909748303, 146.1777001516798862 ) ) ;
#89104 = CARTESIAN_POINT ( 'NONE',  ( -1.651467058941123778, 70.03175547422245018, 118.3472173295736951 ) ) ;
#89105 = ORIENTED_EDGE ( 'NONE', *, *, #53565, .T. ) ;
#89106 = ADVANCED_FACE ( 'NONE', ( #31737 ), #58543, .F. ) ;
#89107 = FACE_OUTER_BOUND ( 'NONE', #58901, .T. ) ;
#89108 = ADVANCED_FACE ( 'NONE', ( #37224 ), #64929, .T. ) ;
#89109 = ADVANCED_FACE ( 'NONE', ( #72644 ), #19346, .F. ) ;
#89110 = CARTESIAN_POINT ( 'NONE',  ( -50.03799999999999670, 101.5999999999999943, 191.3008000794699797 ) ) ;
#89111 = CARTESIAN_POINT ( 'NONE',  ( 2.899925867002088431, 70.17843955035350234, 118.5212385615275252 ) ) ;
#89112 = EDGE_LOOP ( 'NONE', ( #67937, #14800, #68591, #24083 ) ) ;
#89113 = CARTESIAN_POINT ( 'NONE',  ( 112.8137514937528891, -47.12132662887700008, 98.97848241876793907 ) ) ;
#89114 = EDGE_CURVE ( 'NONE', #65321, #55858, #75376, .T. ) ;
#89116 = DIRECTION ( 'NONE',  ( 1.000000000000000000, 0.000000000000000000, 0.000000000000000000 ) ) ;
#89115 = CARTESIAN_POINT ( 'NONE',  ( 97.82528869122914728, -40.55050793170509849, 171.6387267483714254 ) ) ;
#89117 = LINE ( 'NONE', #26876, #72672 ) ;
#89118 = AXIS2_PLACEMENT_3D ( 'NONE', #63453, #76639, #13515 ) ;
#89119 = AXIS2_PLACEMENT_3D ( 'NONE', #26542, #12926, #81535 ) ;
#89120 = AXIS2_PLACEMENT_3D ( 'NONE', #58379, #30242, #54102 ) ;
#89121 = CIRCLE ( 'NONE', #44095, 2.500000000000002220 ) ;
#89122 = CARTESIAN_POINT ( 'NONE',  ( 270.8910000000000196, 65.43750000000000000, -67.11950000000000216 ) ) ;
#89123 = ORIENTED_EDGE ( 'NONE', *, *, #87467, .F. ) ;
#89124 = CARTESIAN_POINT ( 'NONE',  ( 116.4859054502388744, -39.36344060769043551, 94.60991099019594230 ) ) ;
#89126 = VERTEX_POINT ( 'NONE', #67938 ) ;
#89125 = CARTESIAN_POINT ( 'NONE',  ( 12.62661858190509534, 84.14780334606243173, 129.9444360960973199 ) ) ;
#89127 = AXIS2_PLACEMENT_3D ( 'NONE', #63394, #14812, #36598 ) ;
#89128 = AXIS2_PLACEMENT_3D ( 'NONE', #79260, #66040, #86956 ) ;
#89129 = CARTESIAN_POINT ( 'NONE',  ( 96.29057984255084079, -34.37493501460200207, 252.1432443235302969 ) ) ;
#89130 = CARTESIAN_POINT ( 'NONE',  ( 125.9611475301394847, -58.72944715994102438, 249.5838068554163840 ) ) ;
#89131 = DIRECTION ( 'NONE',  ( 0.000000000000000000, 1.000000000000000000, 0.000000000000000000 ) ) ;
#89132 = PLANE ( 'NONE',  #55883 ) ;
#89133 = CARTESIAN_POINT ( 'NONE',  ( 112.1393456378820446, -28.01282277885371030, 45.65645860958608893 ) ) ;
#89134 = FACE_OUTER_BOUND ( 'NONE', #29025, .T. ) ;
#89135 = CARTESIAN_POINT ( 'NONE',  ( -98.05713019660782948, 73.00415124681447310, 86.19613171056714407 ) ) ;
#89136 = CARTESIAN_POINT ( 'NONE',  ( 111.8874393434638250, -45.23954810143646910, 212.9870538473399506 ) ) ;
#89137 = ORIENTED_EDGE ( 'NONE', *, *, #14200, .T. ) ;
#89138 = EDGE_LOOP ( 'NONE', ( #24576, #64410, #12589, #52602 ) ) ;
#89139 = CARTESIAN_POINT ( 'NONE',  ( 103.3528332358002331, -45.35993549251112711, 133.6968214011349403 ) ) ;
#89140 = LINE ( 'NONE', #32815, #29856 ) ;
#89142 = FACE_OUTER_BOUND ( 'NONE', #62546, .T. ) ;
#89141 = CARTESIAN_POINT ( 'NONE',  ( 97.44287158780967673, -40.59272077381804422, 247.6422919425769749 ) ) ;
#89143 = DIRECTION ( 'NONE',  ( 0.000000000000000000, 0.000000000000000000, -1.000000000000000000 ) ) ;
#89144 = DIRECTION ( 'NONE',  ( -9.299908063537909262E-17, 6.056575390184510167E-15, -1.000000000000000000 ) ) ;
#89145 = CYLINDRICAL_SURFACE ( 'NONE', #21167, 9.999999999999998224 ) ;
#89146 = DIRECTION ( 'NONE',  ( -4.237773401492740281E-14, 1.000000000000000000, 0.000000000000000000 ) ) ;
#89147 = CARTESIAN_POINT ( 'NONE',  ( 21.03689327557711763, -23.42844715994186089, 249.9678068554150059 ) ) ;
#89148 = CARTESIAN_POINT ( 'NONE',  ( 106.9751875180390641, -47.13234726572967759, 187.5699109901969734 ) ) ;
#89149 = CARTESIAN_POINT ( 'NONE',  ( 183.5150000000000148, 21.46300000000000097, 41.63456447661474868 ) ) ;
#89150 = EDGE_LOOP ( 'NONE', ( #40811, #33744 ) ) ;
#89151 = ORIENTED_EDGE ( 'NONE', *, *, #81334, .F. ) ;
#89152 = CARTESIAN_POINT ( 'NONE',  ( -90.25011051337695278, 70.17666187254640420, -94.33955404248699494 ) ) ;
#89153 = CARTESIAN_POINT ( 'NONE',  ( 81.30994157256897381, -21.18303583361772269, 7.982915248808116537 ) ) ;
#89154 = CARTESIAN_POINT ( 'NONE',  ( 116.8164492606990308, -34.15029442158964201, 125.0311193818890416 ) ) ;
#89155 = DIRECTION ( 'NONE',  ( 0.000000000000000000, 0.000000000000000000, -1.000000000000000000 ) ) ;
#89156 = CONICAL_SURFACE ( 'NONE', #36893, 4.799999999999970512, 0.7853981633975198884 ) ;
#89157 = DIRECTION ( 'NONE',  ( -0.7071067811865414665, 0.000000000000000000, -0.7071067811865534569 ) ) ;
#89158 = ORIENTED_EDGE ( 'NONE', *, *, #34842, .T. ) ;
#89159 = CARTESIAN_POINT ( 'NONE',  ( 116.3283240494693160, -32.94276334974209419, 64.13562527591099638 ) ) ;
#89160 = AXIS2_PLACEMENT_3D ( 'NONE', #86641, #86194, #51647 ) ;
#89161 = CARTESIAN_POINT ( 'NONE',  ( 104.1857688441879191, -26.67323559945603151, 225.2984824187679749 ) ) ;
#89162 = EDGE_CURVE ( 'NONE', #41446, #88268, #7231, .T. ) ;
#89163 = ORIENTED_EDGE ( 'NONE', *, *, #59519, .F. ) ;
#89164 = EDGE_CURVE ( 'NONE', #67043, #27883, #26597, .T. ) ;
#89165 = DIRECTION ( 'NONE',  ( 0.000000000000000000, 0.000000000000000000, -1.000000000000000000 ) ) ;
#89166 = FACE_OUTER_BOUND ( 'NONE', #66123, .T. ) ;
#89167 = CARTESIAN_POINT ( 'NONE',  ( -487.2989999999999782, 7.143750000000339995, 6.988054014476278830 ) ) ;
#89168 = CARTESIAN_POINT ( 'NONE',  ( 98.93870468184483968, -41.20551083899233902, 24.54523322673496466 ) ) ;
#89169 = CARTESIAN_POINT ( 'NONE',  ( 98.83948440537673719, -30.29086274794821065, 151.7984824187679465 ) ) ;
#89170 = EDGE_CURVE ( 'NONE', #74974, #25248, #68111, .T. ) ;
#89171 = CARTESIAN_POINT ( 'NONE',  ( 123.6837132603318707, -22.62993780205694705, 219.5838068554170093 ) ) ;
#89172 = EDGE_LOOP ( 'NONE', ( #20344, #13255, #89091, #50506 ) ) ;
#89173 = ADVANCED_FACE ( 'NONE', ( #54277 ), #44016, .T. ) ;
#89174 = FACE_OUTER_BOUND ( 'NONE', #16683, .T. ) ;
#89175 = CARTESIAN_POINT ( 'NONE',  ( 117.0385479230201327, -38.27385465322490887, 68.70451315128531178 ) ) ;
#89176 = ORIENTED_EDGE ( 'NONE', *, *, #8575, .T. ) ;
#89177 = ORIENTED_EDGE ( 'NONE', *, *, #63864, .T. ) ;
#89178 = ADVANCED_FACE ( 'NONE', ( #23614 ), #51272, .F. ) ;
#89179 = AXIS2_PLACEMENT_3D ( 'NONE', #26808, #13197, #39990 ) ;
#89180 = VECTOR ( 'NONE', #62739, 999.9999999999998863 ) ;
#89181 = FACE_BOUND ( 'NONE', #83424, .T. ) ;
#89182 = CIRCLE ( 'NONE', #74648, 0.9999999999992039701 ) ;
#89183 = ORIENTED_EDGE ( 'NONE', *, *, #1334, .F. ) ;
#89184 = ORIENTED_EDGE ( 'NONE', *, *, #82329, .T. ) ;
#89185 = DIRECTION ( 'NONE',  ( 0.000000000000000000, 1.000000000000000000, 0.000000000000000000 ) ) ;
#89186 = CIRCLE ( 'NONE', #10843, 13.31747058675099815 ) ;
#89187 = ADVANCED_FACE ( 'NONE', ( #34307 ), #47476, .F. ) ;
#89188 = CARTESIAN_POINT ( 'NONE',  ( 111.7311378220509255, -29.53965576977622831, 69.04099125664797043 ) ) ;
#89190 = CARTESIAN_POINT ( 'NONE',  ( 98.92532678050559980, -30.18208626920050719, 240.7870538473399620 ) ) ;
#89189 = CIRCLE ( 'NONE', #38402, 4.750000000000000888 ) ;
#89191 = AXIS2_PLACEMENT_3D ( 'NONE', #982, #44529, #58608 ) ;
#89192 = CARTESIAN_POINT ( 'NONE',  ( 106.3035372762157351, -47.10473409126657174, 222.5184824187679453 ) ) ;
#89194 = CARTESIAN_POINT ( 'NONE',  ( 96.56373827543593791, -40.17738982329606046, 282.5908633711490552 ) ) ;
#89193 = DIRECTION ( 'NONE',  ( 0.000000000000000000, 1.000000000000000000, 0.000000000000000000 ) ) ;
#89195 = DIRECTION ( 'NONE',  ( -4.237773401492740281E-14, 1.000000000000000000, 0.000000000000000000 ) ) ;
#89196 = CARTESIAN_POINT ( 'NONE',  ( 57.56670390244747892, -48.82844715994040286, 137.2178068554150911 ) ) ;
#89197 = EDGE_CURVE ( 'NONE', #3936, #52361, #85577, .T. ) ;
#89198 = EDGE_LOOP ( 'NONE', ( #40023, #459, #68895, #15023 ) ) ;
#89199 = ADVANCED_FACE ( 'NONE', ( #69740 ), #34760, .T. ) ;
#89200 = CARTESIAN_POINT ( 'NONE',  ( 103.5913876162975527, -46.49993820617282125, 102.3165776568639700 ) ) ;
#89201 = CARTESIAN_POINT ( 'NONE',  ( 118.8926602832294037, -35.39890769255473657, 83.91562527591095488 ) ) ;
#89202 = CARTESIAN_POINT ( 'NONE',  ( 96.87130625142565066, -34.19761792387945576, 276.1327681330536734 ) ) ;
#89203 = VERTEX_POINT ( 'NONE', #684 ) ;
#89204 = CARTESIAN_POINT ( 'NONE',  ( 117.0684261367714072, -39.67022423017687771, 183.5984824187679578 ) ) ;
#89205 = CARTESIAN_POINT ( 'NONE',  ( 115.8254323898935496, -31.73001882380996364, 34.23979194300372342 ) ) ;
#89206 = CARTESIAN_POINT ( 'NONE',  ( 165.3359832912740046, -36.32844715994100682, 342.9256252759109884 ) ) ;
#89207 = CARTESIAN_POINT ( 'NONE',  ( 141.0664832912740394, -46.72944715994099596, -4.824374724088994704 ) ) ;
#89208 = CARTESIAN_POINT ( 'NONE',  ( 104.8437968989451861, -46.57283331671013116, 28.40163825079190474 ) ) ;
#89209 = AXIS2_PLACEMENT_3D ( 'NONE', #88318, #13345, #41032 ) ;
#89211 = CARTESIAN_POINT ( 'NONE',  ( 77.39114642429899504, 127.0000000000000000, 71.77848634863160271 ) ) ;
#89210 = CARTESIAN_POINT ( 'NONE',  ( 110.4749035026220554, -45.11497559619134279, 277.6356252759110816 ) ) ;
#89212 = CARTESIAN_POINT ( 'NONE',  ( 115.0371819524543326, -42.90856332754897551, 174.3022820718215655 ) ) ;
#89213 = DIRECTION ( 'NONE',  ( 0.03970846417641692161, -0.4987692715698832657, 0.8658247233767341067 ) ) ;
#89214 = CARTESIAN_POINT ( 'NONE',  ( 199.3900000000000148, 52.73749999999999716, -47.62500000000000000 ) ) ;
#89215 = B_SPLINE_CURVE_WITH_KNOTS ( 'NONE', 3,
 ( #14632, #29151, #56388, #48220, #35959, #69591 ),
 .UNSPECIFIED., .F., .F.,
 ( 4, 2, 4 ),
 ( -0.008552427134052589808, -0.004278148697845064567, -7.255242802014019721E-06 ),
 .UNSPECIFIED. ) ;
#89216 = DIRECTION ( 'NONE',  ( -1.000000000000000000, 0.000000000000000000, -9.974659986866630932E-16 ) ) ;
#89217 = CARTESIAN_POINT ( 'NONE',  ( 51.06648329127400388, 22.62155284005901024, 327.8006252759110453 ) ) ;
#89218 = CARTESIAN_POINT ( 'NONE',  ( 109.7248659271630800, -27.00080518147012043, 75.86479194210151888 ) ) ;
#89219 = EDGE_CURVE ( 'NONE', #63134, #1004, #79361, .T. ) ;
#89221 = ORIENTED_EDGE ( 'NONE', *, *, #49272, .F. ) ;
#89220 = DIRECTION ( 'NONE',  ( 1.000000000000000000, 2.999999999999999839E-15, 1.000000000000000078E-15 ) ) ;
#89222 = DIRECTION ( 'NONE',  ( 0.000000000000000000, -1.000000000000000000, 0.000000000000000000 ) ) ;
#89223 = CARTESIAN_POINT ( 'NONE',  ( 110.5061846383585475, -26.86461981176654845, 209.8099109901969541 ) ) ;
#89224 = CARTESIAN_POINT ( 'NONE',  ( 109.2014185099688603, -26.52530387367253795, 135.9127681330539872 ) ) ;
#89225 = CARTESIAN_POINT ( 'NONE',  ( 108.0180542234412684, -24.86750695335871697, 261.0127681330534415 ) ) ;
#89226 = CARTESIAN_POINT ( 'NONE',  ( 99.09570913299437223, -30.55043168099339823, 155.8022919353178395 ) ) ;
#89227 = EDGE_CURVE ( 'NONE', #30095, #48357, #57987, .T. ) ;
#89228 = CARTESIAN_POINT ( 'NONE',  ( 49.35211078756498893, -35.65087443492551245, 237.4678068554150059 ) ) ;
#89230 = CARTESIAN_POINT ( 'NONE',  ( 182.2300522401149863, -33.89581943344511217, 117.4678068554150627 ) ) ;
#89229 = LINE ( 'NONE', #81083, #75415 ) ;
#89231 = CARTESIAN_POINT ( 'NONE',  ( 107.0664832912739541, -36.72944715994095333, 305.0306255462182321 ) ) ;
#89232 = AXIS2_PLACEMENT_3D ( 'NONE', #61948, #48751, #27881 ) ;
#89233 = CARTESIAN_POINT ( 'NONE',  ( -24.79284581386642827, 127.0000000000000000, 85.23828826961327820 ) ) ;
#89234 = AXIS2_PLACEMENT_3D ( 'NONE', #63399, #49307, #14818 ) ;
#89235 = ORIENTED_EDGE ( 'NONE', *, *, #27052, .F. ) ;
#89236 = ORIENTED_EDGE ( 'NONE', *, *, #42250, .F. ) ;
#89237 = CARTESIAN_POINT ( 'NONE',  ( 99.28690145085043639, -32.09363259137744251, 130.3333722090289655 ) ) ;
#89239 = ORIENTED_EDGE ( 'NONE', *, *, #21734, .T. ) ;
#89238 = DIRECTION ( 'NONE',  ( 0.000000000000000000, 0.000000000000000000, 1.000000000000000000 ) ) ;
#89240 = LINE ( 'NONE', #27005, #38774 ) ;
#89241 = CARTESIAN_POINT ( 'NONE',  ( 117.5589153096731110, -33.32758106675091625, 130.0880062282919880 ) ) ;
#89242 = CARTESIAN_POINT ( 'NONE',  ( 101.9927089507507816, -45.44550910856975889, 148.1569819098927780 ) ) ;
#89243 = CARTESIAN_POINT ( 'NONE',  ( -47.18030668273772221, 93.07500000000001705, 75.34738655934135920 ) ) ;
#89244 = CARTESIAN_POINT ( 'NONE',  ( -74.36911441044730964, 82.54999999999999716, 92.32962665258534685 ) ) ;
#89245 = DIRECTION ( 'NONE',  ( 1.000000000000000078E-15, -1.000000000000000083E-30, -1.000000000000000000 ) ) ;
#89246 = CARTESIAN_POINT ( 'NONE',  ( 107.3052971647831555, -26.36210646096926524, 75.04610146638796664 ) ) ;
#89247 = EDGE_LOOP ( 'NONE', ( #55115, #10030, #29288, #39279, #18070, #34401, #72135, #24062, #31643, #58566, #63337, #37727, #87425, #88899, #6088, #28843, #58249, #25817 ) ) ;
#89248 = ORIENTED_EDGE ( 'NONE', *, *, #34753, .F. ) ;
#89249 = ORIENTED_EDGE ( 'NONE', *, *, #55904, .T. ) ;
#89251 = EDGE_CURVE ( 'NONE', #63134, #9022, #12988, .T. ) ;
#89250 = B_SPLINE_CURVE_WITH_KNOTS ( 'NONE', 3,
 ( #3345, #24675, #87355, #86473, #3787, #59619, #52778, #10592, #44205, #65117, #2902, #60063, #10157, #30600, #25115, #38296, #80544, #79662, #37866, #23800, #52339, #65564, #37414, #58300, #16974, #51903, #11040, #51467, #86909, #79217, #44658, #18298, #65995, #72389, #38741, #4682, #4230, #59178, #45532, #31925, #58729, #24236, #17418, #45100, #80106, #66443, #31474, #32361 ),
 .UNSPECIFIED., .F., .F.,
 ( 4, 2, 2, 2, 2, 2, 2, 2, 2, 1, 2, 2, 2, 2, 2, 2, 2, 2, 2, 2, 2, 1, 2, 2, 4 ),
 ( 0.05960646776571126848, 0.06208927922045068964, 0.06333068494782040370, 0.06457209067519011081, 0.06705490212992956667, 0.06829630785729930154, 0.06953771358466903640, 0.07202052503940852002, 0.07326193076677825489, 0.07450333649414798975, 0.07574474222151772462, 0.07698614794888745949, 0.07946895940362692923, 0.08195177085836638509, 0.08319317658573611995, 0.08443458231310585482, 0.08691739376784532456, 0.08815879949521507331, 0.08940020522258480817, 0.09188301667732426403, 0.09312442240469397114, 0.09436582813206367826, 0.09560723385943339925, 0.09684863958680312024, 0.09933145104154257610 ),
 .UNSPECIFIED. ) ;
#89252 = AXIS2_PLACEMENT_3D ( 'NONE', #33264, #60967, #81880 ) ;
#89253 = VECTOR ( 'NONE', #62179, 1000.000000000000000 ) ;
#89254 = CARTESIAN_POINT ( 'NONE',  ( 179.8608231853570487, -35.55794170701178558, 117.4678068554150627 ) ) ;
#89256 = CARTESIAN_POINT ( 'NONE',  ( 184.5667039024480118, -48.82844715994099971, 20.91780685541479912 ) ) ;
#89255 = CARTESIAN_POINT ( 'NONE',  ( 102.3899016914588884, -28.13915478247121271, 141.4727681330539895 ) ) ;
#89257 = CARTESIAN_POINT ( 'NONE',  ( 98.58946256649485917, -108.5954344580491693, 2.217806855418142042 ) ) ;
#89258 = DIRECTION ( 'NONE',  ( 1.000000000000000000, 6.145690160522439356E-16, 0.000000000000000000 ) ) ;
#89259 = PLANE ( 'NONE',  #3917 ) ;
#89260 = CARTESIAN_POINT ( 'NONE',  ( 90.31319802837550981, 90.93089219781631982, 76.80574412431096221 ) ) ;
#89261 = CARTESIAN_POINT ( 'NONE',  ( 194.0667039024475287, -24.92844715993407334, 180.4678068554150343 ) ) ;
#89262 = CARTESIAN_POINT ( 'NONE',  ( 95.51222647996974047, -34.21005103128000968, 106.1556252759109640 ) ) ;
#89263 = VERTEX_POINT ( 'NONE', #7953 ) ;
#89264 = VERTEX_POINT ( 'NONE', #55618 ) ;
#89265 = ORIENTED_EDGE ( 'NONE', *, *, #25365, .F. ) ;
#89266 = AXIS2_PLACEMENT_3D ( 'NONE', #25880, #24989, #46748 ) ;
#89267 = DIRECTION ( 'NONE',  ( 0.000000000000000000, -1.000000000000000000, 0.000000000000000000 ) ) ;
#89268 = CARTESIAN_POINT ( 'NONE',  ( -83.21537498883982664, 85.85000629251470627, -100.5986936721443499 ) ) ;
#89269 = DIRECTION ( 'NONE',  ( -0.000000000000000000, 0.8660254037844382635, 0.5000000000000008882 ) ) ;
#89271 = CARTESIAN_POINT ( 'NONE',  ( 112.5929834642309117, -30.72215809952430376, 197.3023760838769647 ) ) ;
#89270 = CIRCLE ( 'NONE', #22560, 3.000000000000002665 ) ;
#89272 = ADVANCED_FACE ( 'NONE', ( #83370 ), #6608, .F. ) ;
#89273 = VECTOR ( 'NONE', #47852, 1000.000000000000114 ) ;
#89274 = EDGE_CURVE ( 'NONE', #69124, #77884, #27942, .T. ) ;
#89275 = EDGE_CURVE ( 'NONE', #83807, #44910, #42029, .T. ) ;
#89276 = CARTESIAN_POINT ( 'NONE',  ( 115.0897088867533569, -30.61867969486051066, 25.34382189988804157 ) ) ;
#89277 = VERTEX_POINT ( 'NONE', #21142 ) ;
#89279 = VERTEX_POINT ( 'NONE', #35196 ) ;
#89278 = ORIENTED_EDGE ( 'NONE', *, *, #26702, .T. ) ;
#89280 = DIRECTION ( 'NONE',  ( -1.000000000000000078E-15, 1.000000000000000083E-30, 1.000000000000000000 ) ) ;
#89281 = EDGE_CURVE ( 'NONE', #48706, #57647, #13873, .T. ) ;
#89282 = DIRECTION ( 'NONE',  ( 1.000000000000000078E-15, 0.000000000000000000, -1.000000000000000000 ) ) ;
#89283 = ORIENTED_EDGE ( 'NONE', *, *, #40414, .F. ) ;
#89284 = ORIENTED_EDGE ( 'NONE', *, *, #65190, .T. ) ;
#89285 = DIRECTION ( 'NONE',  ( -4.237773401492740281E-14, 1.000000000000000000, 0.000000000000000000 ) ) ;
#89286 = CARTESIAN_POINT ( 'NONE',  ( 102.9614994733801439, -44.58294233512814486, 208.6244404487539725 ) ) ;
#89287 = ADVANCED_FACE ( 'NONE', ( #239 ), #19794, .F. ) ;
#89288 = CARTESIAN_POINT ( 'NONE',  ( 180.1667039024460166, -26.71338133339240528, -5.074374724088000832 ) ) ;
#89289 = CARTESIAN_POINT ( 'NONE',  ( -123.9668422125822218, 72.11824565187180269, 40.95437521977012807 ) ) ;
#89290 = VERTEX_POINT ( 'NONE', #76550 ) ;
#89291 = EDGE_LOOP ( 'NONE', ( #37986, #69831, #56308, #58008, #56049, #38499 ) ) ;
#89292 = EDGE_CURVE ( 'NONE', #48257, #31385, #21764, .T. ) ;
#89293 = DIRECTION ( 'NONE',  ( 0.000000000000000000, 0.000000000000000000, -1.000000000000000000 ) ) ;
#89294 = AXIS2_PLACEMENT_3D ( 'NONE', #61484, #34676, #62384 ) ;
#89295 = VERTEX_POINT ( 'NONE', #21598 ) ;
#89296 = ORIENTED_EDGE ( 'NONE', *, *, #26214, .F. ) ;
#89297 = EDGE_CURVE ( 'NONE', #61357, #45558, #5811, .T. ) ;
#89298 = CARTESIAN_POINT ( 'NONE',  ( 105.5353399150147737, -28.71163411781831698, 233.0452332267339841 ) ) ;
#89299 = CARTESIAN_POINT ( 'NONE',  ( 117.2597117638302393, -39.02229875088008981, 148.6499109901969859 ) ) ;
#89300 = CARTESIAN_POINT ( 'NONE',  ( 117.0705705820184477, -32.08379757587633208, 59.16038718067295576 ) ) ;
#89301 = CARTESIAN_POINT ( 'NONE',  ( 115.3486850554863707, -40.94587795544506292, 249.5838068554168103 ) ) ;
#89302 = CARTESIAN_POINT ( 'NONE',  ( 131.9645448811557742, -16.94667115355465725, 7.474641677900195624 ) ) ;
#89303 = CARTESIAN_POINT ( 'NONE',  ( 109.3584748782654401, -25.91645705315499981, 180.9222919425779708 ) ) ;
#89304 = DIRECTION ( 'NONE',  ( 0.000000000000000000, 0.000000000000000000, 1.000000000000000000 ) ) ;
#89305 = ORIENTED_EDGE ( 'NONE', *, *, #20635, .F. ) ;
#89306 = CARTESIAN_POINT ( 'NONE',  ( -129.9777455398983079, 79.26455342200334542, 12.27475243033008212 ) ) ;
#89307 = EDGE_LOOP ( 'NONE', ( #6211, #61159, #19781, #68851 ) ) ;
#89308 = ADVANCED_FACE ( 'NONE', ( #77004 ), #14787, .F. ) ;
#89309 = VERTEX_POINT ( 'NONE', #47918 ) ;
#89310 = CARTESIAN_POINT ( 'NONE',  ( 110.0667047667142953, -67.87844715994094713, 173.2178068554179902 ) ) ;
#89311 = ORIENTED_EDGE ( 'NONE', *, *, #26310, .T. ) ;
#89312 = CIRCLE ( 'NONE', #42856, 5.599999999999994316 ) ;
#89313 = CIRCLE ( 'NONE', #50124, 3.500000000000003109 ) ;
#89314 = AXIS2_PLACEMENT_3D ( 'NONE', #51461, #72383, #51030 ) ;
#89315 = CARTESIAN_POINT ( 'NONE',  ( 114.7075677164476986, -44.71649393962480445, 113.1718157521009687 ) ) ;
#89316 = CARTESIAN_POINT ( 'NONE',  ( -7.047141237186552054, 71.98459356607415316, 130.3656662584478170 ) ) ;
#89317 = AXIS2_PLACEMENT_3D ( 'NONE', #66211, #3999, #67568 ) ;
#89318 = CARTESIAN_POINT ( 'NONE',  ( 91.91125933621933086, -100.4807974291314423, -11.78219314458211997 ) ) ;
#89319 = DIRECTION ( 'NONE',  ( 0.000000000000000000, 1.000000000000000000, 0.000000000000000000 ) ) ;
#89322 = CARTESIAN_POINT ( 'NONE',  ( 96.87985868497426623, -34.61725761836213167, 212.1641967044819808 ) ) ;
#89321 = LINE ( 'NONE', #39794, #55694 ) ;
#89320 = CARTESIAN_POINT ( 'NONE',  ( 108.3334480864761957, -46.73485935512827183, 143.6772919419037180 ) ) ;
#89323 = DIRECTION ( 'NONE',  ( 0.000000000000000000, 0.7071067811865120456, 0.7071067811865829889 ) ) ;
#89324 = CARTESIAN_POINT ( 'NONE',  ( 34.92499999999999716, 69.84999999999999432, 295.2750000000000341 ) ) ;
#89325 = ORIENTED_EDGE ( 'NONE', *, *, #28156, .F. ) ;
#89326 = DIRECTION ( 'NONE',  ( 4.299999999999999979E-14, -1.000000000000000000, 4.400000000000000367E-29 ) ) ;
#89327 = AXIS2_PLACEMENT_3D ( 'NONE', #6995, #61946, #13809 ) ;
#89328 = DIRECTION ( 'NONE',  ( 0.000000000000000000, 0.000000000000000000, 1.000000000000000000 ) ) ;
#89329 = PLANE ( 'NONE',  #6762 ) ;
#89330 = AXIS2_PLACEMENT_3D ( 'NONE', #64655, #23787, #45519 ) ;
#89331 = DIRECTION ( 'NONE',  ( 0.000000000000000000, 0.000000000000000000, 1.000000000000000000 ) ) ;
#89333 = ORIENTED_EDGE ( 'NONE', *, *, #31428, .F. ) ;
#89332 = CARTESIAN_POINT ( 'NONE',  ( 109.9724474192709351, -48.26999177473817326, 242.7727681330539724 ) ) ;
#89334 = CARTESIAN_POINT ( 'NONE',  ( 106.7561181679527209, -26.70555286918040139, 195.1009897130665252 ) ) ;
#89335 = CARTESIAN_POINT ( 'NONE',  ( 102.6883137591737665, -46.90427260131782106, 137.2651490854349561 ) ) ;
#89336 = CARTESIAN_POINT ( 'NONE',  ( 101.6089948421187898, -47.24856100052405594, 13.19562527591094891 ) ) ;
#89337 = CARTESIAN_POINT ( 'NONE',  ( 117.0586869608412286, -33.60713302236428746, 170.0670538473399631 ) ) ;
#89338 = DIRECTION ( 'NONE',  ( 0.000000000000000000, -1.000000000000000000, 0.000000000000000000 ) ) ;
#89339 = EDGE_CURVE ( 'NONE', #73485, #78558, #40669, .T. ) ;
#89340 = CARTESIAN_POINT ( 'NONE',  ( 1.598849865763559337E-14, 95.25000000000000000, -130.5560000000000116 ) ) ;
#89341 = AXIS2_PLACEMENT_3D ( 'NONE', #47654, #89466, #24009 ) ;
#89343 = CARTESIAN_POINT ( 'NONE',  ( 194.0371591254575208, -24.42818131005407167, 180.4678068554150343 ) ) ;
#89342 = CARTESIAN_POINT ( 'NONE',  ( 70.06670390244707392, -137.6784471599409869, 222.2178068554179902 ) ) ;
#89344 = FACE_BOUND ( 'NONE', #13610, .T. ) ;
#89345 = DIRECTION ( 'NONE',  ( -0.7071067811865784369, 0.7071067811865165975, -7.071067811865791864E-16 ) ) ;
#89346 = VERTEX_POINT ( 'NONE', #57692 ) ;
#89347 = AXIS2_PLACEMENT_3D ( 'NONE', #13691, #69559, #20523 ) ;
#89348 = VERTEX_POINT ( 'NONE', #50877 ) ;
#89349 = ORIENTED_EDGE ( 'NONE', *, *, #28041, .F. ) ;
#89350 = ORIENTED_EDGE ( 'NONE', *, *, #11710, .T. ) ;
#89351 = CARTESIAN_POINT ( 'NONE',  ( -72.96458098368600531, 117.4749999999999943, -72.96458098368781009 ) ) ;
#89352 = CARTESIAN_POINT ( 'NONE',  ( 96.70769389551976758, -42.43415482991306220, 22.72705384733997391 ) ) ;
#89353 = CARTESIAN_POINT ( 'NONE',  ( 77.11349091887886686, -140.6783563551099689, 245.9764622033119963 ) ) ;
#89354 = CARTESIAN_POINT ( 'NONE',  ( 145.1838268511080798, -139.0510231921375350, 246.8128416193126782 ) ) ;
#89355 = LINE ( 'NONE', #54793, #83889 ) ;
#89356 = CARTESIAN_POINT ( 'NONE',  ( 106.9632158956753756, -45.78494306966059924, 232.0019436376009594 ) ) ;
#89357 = ORIENTED_EDGE ( 'NONE', *, *, #52113, .F. ) ;
#89358 = VERTEX_POINT ( 'NONE', #15485 ) ;
#89359 = ORIENTED_EDGE ( 'NONE', *, *, #39155, .F. ) ;
#89360 = EDGE_CURVE ( 'NONE', #19378, #48818, #43154, .T. ) ;
#89361 = CARTESIAN_POINT ( 'NONE',  ( 67.06670390244701707, -79.67844715994098692, 55.21780685541800437 ) ) ;
#89362 = VECTOR ( 'NONE', #25246, 1000.000000000000000 ) ;
#89363 = CARTESIAN_POINT ( 'NONE',  ( 180.3164832912740110, 12.92155284005802507, 349.2756252759111248 ) ) ;
#89364 = LINE ( 'NONE', #82565, #87569 ) ;
#89365 = CARTESIAN_POINT ( 'NONE',  ( -41.60202597009397607, 65.59999999999998010, 50.85338361873603219 ) ) ;
#89366 = DIRECTION ( 'NONE',  ( 1.000000000000000000, 0.000000000000000000, 0.000000000000000000 ) ) ;
#89367 = DIRECTION ( 'NONE',  ( 1.000000000000000000, 0.000000000000000000, 0.000000000000000000 ) ) ;
#89368 = CARTESIAN_POINT ( 'NONE',  ( 97.83217745605946902, -40.05230289513916375, 266.6013395616258776 ) ) ;
#89369 = FACE_OUTER_BOUND ( 'NONE', #70271, .T. ) ;
#89370 = PRODUCT_RELATED_PRODUCT_CATEGORY ( 'part', '', ( #1904 ) ) ;
#89371 = ORIENTED_EDGE ( 'NONE', *, *, #80199, .F. ) ;
#89372 = CYLINDRICAL_SURFACE ( 'NONE', #54783, 2.749999999999974687 ) ;
#89373 = AXIS2_PLACEMENT_3D ( 'NONE', #83147, #5601, #49929 ) ;
#89374 = LINE ( 'NONE', #59845, #256 ) ;
#89375 = CARTESIAN_POINT ( 'NONE',  ( 98.42956409136928642, -40.12054696651731689, 94.44237608387695104 ) ) ;
#89376 = CIRCLE ( 'NONE', #13958, 23.50000000000000711 ) ;
#89377 = VECTOR ( 'NONE', #36844, 1000.000000000000000 ) ;
#89378 = AXIS2_PLACEMENT_3D ( 'NONE', #87243, #54018, #74498 ) ;
#89379 = CARTESIAN_POINT ( 'NONE',  ( 107.0667039024470313, -104.2784471599420755, -19.78219314458201694 ) ) ;
#89380 = EDGE_CURVE ( 'NONE', #46099, #56697, #17262, .T. ) ;
#89381 = DIRECTION ( 'NONE',  ( -1.000000000000000000, 0.000000000000000000, 1.821231995776179916E-16 ) ) ;
#89382 = EDGE_LOOP ( 'NONE', ( #87830, #82336, #28170, #2139 ) ) ;
#89383 = CARTESIAN_POINT ( 'NONE',  ( 33.98325472291465132, 111.1250000000000000, 3.174999999999999822 ) ) ;
#89384 = EDGE_CURVE ( 'NONE', #34396, #22713, #31315, .T. ) ;
#89385 = ORIENTED_EDGE ( 'NONE', *, *, #33785, .T. ) ;
#89386 = CARTESIAN_POINT ( 'NONE',  ( 96.60699139826044757, -36.88735862350505101, 136.3384824187679385 ) ) ;
#89387 = EDGE_LOOP ( 'NONE', ( #43605, #75866, #60078, #39826, #16906, #67496, #31820, #25249, #21208, #23825, #80649, #20926, #18681 ) ) ;
#89388 = EDGE_CURVE ( 'NONE', #23038, #59691, #43516, .T. ) ;
#89389 = LINE ( 'NONE', #28036, #3975 ) ;
#89390 = CARTESIAN_POINT ( 'NONE',  ( 107.2938360571228600, -27.87074582556254398, 116.4872975916119771 ) ) ;
#89391 = EDGE_CURVE ( 'NONE', #21258, #30095, #37257, .T. ) ;
#89392 = CARTESIAN_POINT ( 'NONE',  ( -3.174999999999644995, 17.78000000000000114, 33.98325472291465132 ) ) ;
#89393 = LINE ( 'NONE', #75309, #22299 ) ;
#89394 = AXIS2_PLACEMENT_3D ( 'NONE', #14410, #82568, #34381 ) ;
#89395 = CARTESIAN_POINT ( 'NONE',  ( 116.7650972879214919, -32.84690348374694224, 50.12991099019698282 ) ) ;
#89396 = LINE ( 'NONE', #27157, #25613 ) ;
#89397 = VERTEX_POINT ( 'NONE', #58571 ) ;
#89398 = EDGE_CURVE ( 'NONE', #46473, #11953, #23641, .T. ) ;
#89399 = CARTESIAN_POINT ( 'NONE',  ( -118.0439878494276655, 76.20320268897033600, -11.00820894928435578 ) ) ;
#89400 = ORIENTED_EDGE ( 'NONE', *, *, #35881, .F. ) ;
#89401 = VECTOR ( 'NONE', #87443, 1000.000000000000000 ) ;
#89402 = EDGE_LOOP ( 'NONE', ( #23738, #89357, #57690, #68393 ) ) ;
#89403 = EDGE_CURVE ( 'NONE', #28049, #3581, #51751, .T. ) ;
#89404 = CYLINDRICAL_SURFACE ( 'NONE', #13702, 5.599999999999994316 ) ;
#89405 = ORIENTED_EDGE ( 'NONE', *, *, #87123, .F. ) ;
#89406 = CARTESIAN_POINT ( 'NONE',  ( 100.5669465097397506, -44.03830869352251653, 266.9984824187685604 ) ) ;
#89407 = CARTESIAN_POINT ( 'NONE',  ( 99.08473320778040261, -45.52208679145996939, 152.9899109901969894 ) ) ;
#89408 = CARTESIAN_POINT ( 'NONE',  ( 10.79070278320184073, 75.83992121942911524, -118.0641357957730264 ) ) ;
#89409 = PLANE ( 'NONE',  #17006 ) ;
#89410 = CARTESIAN_POINT ( 'NONE',  ( 102.5581934769535906, -27.32956362888499768, 91.43276813305395478 ) ) ;
#89411 = DIRECTION ( 'NONE',  ( 0.8660254037844359321, 0.000000000000000000, 0.5000000000000046629 ) ) ;
#89412 = ORIENTED_EDGE ( 'NONE', *, *, #32732, .T. ) ;
#89413 = CARTESIAN_POINT ( 'NONE',  ( 47.62500000000000000, 94.53880000000000905, 225.4249999999999829 ) ) ;
#89414 = DIRECTION ( 'NONE',  ( 1.000000000000000078E-15, 1.000000000000000083E-30, -1.000000000000000000 ) ) ;
#89415 = AXIS2_PLACEMENT_3D ( 'NONE', #29957, #64914, #24037 ) ;
#89416 = VERTEX_POINT ( 'NONE', #30001 ) ;
#89417 = DIRECTION ( 'NONE',  ( -0.7071067811865743291, 0.7071067811865207053, -7.071067811865750448E-16 ) ) ;
#89418 = FACE_OUTER_BOUND ( 'NONE', #38833, .T. ) ;
#89419 = CARTESIAN_POINT ( 'NONE',  ( 98.42358855985509081, -42.06826316073455274, 11.76800622829193799 ) ) ;
#89420 = CARTESIAN_POINT ( 'NONE',  ( 59.56670390244699576, -67.87844715994098976, 85.21780685541799016 ) ) ;
#89421 = CARTESIAN_POINT ( 'NONE',  ( 68.86456684384336313, 93.07500000000001705, 56.22171674193015889 ) ) ;
#89422 = FACE_OUTER_BOUND ( 'NONE', #66086, .T. ) ;
#89423 = CARTESIAN_POINT ( 'NONE',  ( 114.9268010244043978, -42.60560063232861694, 28.31562527591097123 ) ) ;
#89425 = CARTESIAN_POINT ( 'NONE',  ( 102.3703197837810848, -46.01248081495474906, 123.2041967044829818 ) ) ;
#89424 = CARTESIAN_POINT ( 'NONE',  ( 97.78574527986302201, -40.45344939432850140, 101.6305854416151675 ) ) ;
#89426 = FACE_OUTER_BOUND ( 'NONE', #34588, .T. ) ;
#89427 = CARTESIAN_POINT ( 'NONE',  ( 117.2811830599562057, -39.02712847638015603, 148.6499109901969859 ) ) ;
#89428 = CARTESIAN_POINT ( 'NONE',  ( -135.2444258376730204, 101.5999999999999943, 147.4575741623271767 ) ) ;
#89429 = ORIENTED_EDGE ( 'NONE', *, *, #66905, .T. ) ;
#89430 = DIRECTION ( 'NONE',  ( -4.237773401492740281E-14, 1.000000000000000000, 0.000000000000000000 ) ) ;
#89431 = DIRECTION ( 'NONE',  ( 0.000000000000000000, 1.000000000000000000, 0.000000000000000000 ) ) ;
#89432 = PLANE ( 'NONE',  #71723 ) ;
#89433 = EDGE_LOOP ( 'NONE', ( #9201, #59022 ) ) ;
#89434 = CARTESIAN_POINT ( 'NONE',  ( 108.4200078917168639, -26.73535838700381362, 60.96903794334217963 ) ) ;
#89436 = ORIENTED_EDGE ( 'NONE', *, *, #55044, .F. ) ;
#89435 = CARTESIAN_POINT ( 'NONE',  ( 102.5972826210866060, -46.89011293525640411, 132.2346728949579528 ) ) ;
#89437 = DIRECTION ( 'NONE',  ( 0.000000000000000000, 0.000000000000000000, 1.000000000000000000 ) ) ;
#89438 = AXIS2_PLACEMENT_3D ( 'NONE', #61114, #26156, #18890 ) ;
#89439 = CARTESIAN_POINT ( 'NONE',  ( 93.48535127324078076, 69.93117631934792655, 91.13743891206708270 ) ) ;
#89440 = ADVANCED_FACE ( 'NONE', ( #3187 ), #59010, .T. ) ;
#89441 = CARTESIAN_POINT ( 'NONE',  ( 184.5667039024483245, -48.82844715993448403, 300.4678068554149490 ) ) ;
#89443 = VECTOR ( 'NONE', #35502, 1000.000000000000114 ) ;
#89442 = DIRECTION ( 'NONE',  ( -0.7071067811567310901, 0.7071067812163639443, 0.000000000000000000 ) ) ;
#89444 = ORIENTED_EDGE ( 'NONE', *, *, #59574, .F. ) ;
#89445 = VECTOR ( 'NONE', #45711, 1000.000000000000000 ) ;
#89446 = AXIS2_PLACEMENT_3D ( 'NONE', #56728, #84473, #22237 ) ;
#89447 = VECTOR ( 'NONE', #37759, 1000.000000000000000 ) ;
#89448 = ADVANCED_FACE ( 'NONE', ( #22748, #79500 ), #44047, .F. ) ;
#89449 = VERTEX_POINT ( 'NONE', #36365 ) ;
#89450 = VERTEX_POINT ( 'NONE', #64960 ) ;
#89451 = VERTEX_POINT ( 'NONE', #1850 ) ;
#89452 = CARTESIAN_POINT ( 'NONE',  ( 172.5664832912740110, -18.82844715994099971, 258.9256252759120116 ) ) ;
#89453 = CARTESIAN_POINT ( 'NONE',  ( 100.0143388906741393, -29.55856279621482585, 250.6953418232228898 ) ) ;
#89454 = DIRECTION ( 'NONE',  ( -1.000000000000000000, 0.000000000000000000, 0.000000000000000000 ) ) ;
#89456 = CARTESIAN_POINT ( 'NONE',  ( -89.60916260784479448, 223.9999999999999716, 134.1927865330827103 ) ) ;
#89455 = DIRECTION ( 'NONE',  ( 1.000000000000000000, 0.000000000000000000, 0.000000000000000000 ) ) ;
#89457 = CARTESIAN_POINT ( 'NONE',  ( 151.0371591254573502, -24.42818131005592974, 249.9678068554149490 ) ) ;
#89458 = VECTOR ( 'NONE', #3711, 1000.000000000000000 ) ;
#89459 = ORIENTED_EDGE ( 'NONE', *, *, #87360, .F. ) ;
#89460 = ORIENTED_EDGE ( 'NONE', *, *, #21714, .F. ) ;
#89461 = CLOSED_SHELL ( 'NONE', ( #7640, #34210, #83276, #5987, #78115, #55814, #87923 ) ) ;
#89462 = EDGE_CURVE ( 'NONE', #40899, #35252, #82721, .T. ) ;
#89463 = DIRECTION ( 'NONE',  ( -0.9254794337955620787, -0.3787978585227822492, 0.000000000000000000 ) ) ;
#89464 = DIRECTION ( 'NONE',  ( 0.000000000000000000, 0.000000000000000000, 1.000000000000000000 ) ) ;
#89465 = CARTESIAN_POINT ( 'NONE',  ( 106.5981863181247604, -46.53222597210204725, 243.5384824187679556 ) ) ;
#89466 = DIRECTION ( 'NONE',  ( -1.000000000000000078E-15, -1.000000000000000083E-30, 1.000000000000000000 ) ) ;
#89467 = CARTESIAN_POINT ( 'NONE',  ( 112.9285164932675514, -28.85859325239454165, 100.5670538473389684 ) ) ;
#89468 = DIRECTION ( 'NONE',  ( 0.000000000000000000, 0.000000000000000000, 1.000000000000000000 ) ) ;
#89469 = CARTESIAN_POINT ( 'NONE',  ( 103.7104750361727383, -27.30776277115187156, 21.34877412902993399 ) ) ;
#89470 = ORIENTED_CLOSED_SHELL ( 'NONE', *, #11119, .F. );
#89471 = VERTEX_POINT ( 'NONE', #10439 ) ;
#89472 = DIRECTION ( 'NONE',  ( 2.900000000000000265E-14, -2.000000000000000155E-15, 1.000000000000000000 ) ) ;
#89473 = VERTEX_POINT ( 'NONE', #51303 ) ;
#89474 = ORIENTED_EDGE ( 'NONE', *, *, #10297, .F. ) ;
#89475 = CIRCLE ( 'NONE', #50289, 7.937500000000000000 ) ;
#89476 = CARTESIAN_POINT ( 'NONE',  ( -123.4696824136392053, 20.32000000000000028, -179.8898777604655095 ) ) ;
#89477 = CARTESIAN_POINT ( 'NONE',  ( 111.1445474647120051, -44.63080920614596181, 269.3872975916115706 ) ) ;
#89478 = AXIS2_PLACEMENT_3D ( 'NONE', #1751, #37608, #70793 ) ;
#89479 = DIRECTION ( 'NONE',  ( 0.000000000000000000, 0.000000000000000000, -1.000000000000000000 ) ) ;
#89480 = CARTESIAN_POINT ( 'NONE',  ( -118.3662777621132136, 93.33860577356858812, 6.713439888430002611 ) ) ;
#89481 = DIRECTION ( 'NONE',  ( 2.081668171172168119E-15, 0.000000000000000000, -1.000000000000000000 ) ) ;
#89482 = EDGE_CURVE ( 'NONE', #63259, #49134, #37769, .T. ) ;
#89483 = CARTESIAN_POINT ( 'NONE',  ( 77.01855645442600462, 73.86197090048096925, -90.13186587200921451 ) ) ;
#89484 = ORIENTED_EDGE ( 'NONE', *, *, #82703, .F. ) ;
#89485 = CARTESIAN_POINT ( 'NONE',  ( 142.0664832912740110, -9.729447159941040368, 14.82207188531770115 ) ) ;
#89486 = CYLINDRICAL_SURFACE ( 'NONE', #23772, 3.000000000000002665 ) ;
#89487 = ORIENTED_EDGE ( 'NONE', *, *, #82003, .T. ) ;
#89488 = CARTESIAN_POINT ( 'NONE',  ( 117.2669906530413186, -38.88274231480306042, 63.66133956162494911 ) ) ;
#89489 = EDGE_LOOP ( 'NONE', ( #63712, #32830, #87277, #47245 ) ) ;
#89490 = EDGE_CURVE ( 'NONE', #85218, #42076, #86749, .T. ) ;
#89491 = CARTESIAN_POINT ( 'NONE',  ( 115.6911714722407396, -33.30735935496929301, 246.9452332267339614 ) ) ;
#89492 = FACE_OUTER_BOUND ( 'NONE', #33677, .T. ) ;
#89493 = CARTESIAN_POINT ( 'NONE',  ( 117.1372161989437899, -34.25576096370539148, 164.0061014663879746 ) ) ;
#89494 = LINE ( 'NONE', #21805, #18690 ) ;
#89495 = EDGE_CURVE ( 'NONE', #35560, #26742, #39280, .T. ) ;
#89496 = DIRECTION ( 'NONE',  ( 0.000000000000000000, 0.7071067811865378028, 0.7071067811865573427 ) ) ;
#89497 = CARTESIAN_POINT ( 'NONE',  ( 163.0664832912739826, -18.82844715994099971, 333.4006252759120343 ) ) ;
#89498 = VECTOR ( 'NONE', #83112, 1000.000000000000000 ) ;
#89499 = CYLINDRICAL_SURFACE ( 'NONE', #29094, 2.500000000000002220 ) ;
#89500 = CARTESIAN_POINT ( 'NONE',  ( 118.7023651333632159, -39.22291191012653400, 254.6584824187681022 ) ) ;
#89501 = DIRECTION ( 'NONE',  ( 0.000000000000000000, 0.000000000000000000, -1.000000000000000000 ) ) ;
#89502 = ORIENTED_EDGE ( 'NONE', *, *, #86304, .T. ) ;
#89503 = CIRCLE ( 'NONE', #79335, 2.500000000000002220 ) ;
#89504 = ORIENTED_EDGE ( 'NONE', *, *, #61301, .F. ) ;
#89505 = CARTESIAN_POINT ( 'NONE',  ( 98.11234142011190329, -43.28847465721014487, 102.8175300378159847 ) ) ;
#89506 = VECTOR ( 'NONE', #46887, 1000.000000000000000 ) ;
#89507 = DIRECTION ( 'NONE',  ( 9.299908063537919123E-17, 0.000000000000000000, 1.000000000000000000 ) ) ;
#89508 = VECTOR ( 'NONE', #89381, 1000.000000000000000 ) ;
#89509 = ORIENTED_EDGE ( 'NONE', *, *, #62194, .F. ) ;
#89510 = EDGE_LOOP ( 'NONE', ( #4930, #40189, #22801, #57497, #63927 ) ) ;
#89511 = VERTEX_POINT ( 'NONE', #46723 ) ;
#89512 = EDGE_CURVE ( 'NONE', #74550, #40777, #8734, .T. ) ;
#89513 = CARTESIAN_POINT ( 'NONE',  ( 164.9667039024459996, -28.27351298637401200, 342.9256252759119548 ) ) ;
#89515 = EDGE_CURVE ( 'NONE', #83508, #67349, #12680, .T. ) ;
#89514 = DIRECTION ( 'NONE',  ( 0.000000000000000000, 1.000000000000000000, 0.000000000000000000 ) ) ;
#89516 = CARTESIAN_POINT ( 'NONE',  ( 140.9629299006806491, -8.979447159940995959, 14.92562527591100618 ) ) ;
#89517 = DIRECTION ( 'NONE',  ( 0.000000000000000000, 0.000000000000000000, -1.000000000000000000 ) ) ;
#89518 = CARTESIAN_POINT ( 'NONE',  ( 103.0775956431641305, -44.40992243120454930, 165.0014237029239439 ) ) ;
#89519 = CARTESIAN_POINT ( 'NONE',  ( 96.89316087236547048, -34.20304521249558150, 272.1327681330539576 ) ) ;
#89520 = DIRECTION ( 'NONE',  ( -1.000000000000000000, 0.000000000000000000, 0.000000000000000000 ) ) ;
#89521 = ORIENTED_EDGE ( 'NONE', *, *, #69182, .F. ) ;
#89522 = CARTESIAN_POINT ( 'NONE',  ( 129.9681618895520216, 85.43248893795416166, -12.37548408773362674 ) ) ;
#89523 = AXIS2_PLACEMENT_3D ( 'NONE', #85589, #22018, #15187 ) ;
#89524 = CIRCLE ( 'NONE', #32900, 2.029999999999997140 ) ;
#89525 = DIRECTION ( 'NONE',  ( 0.000000000000000000, 0.000000000000000000, -1.000000000000000000 ) ) ;
#89526 = ORIENTED_EDGE ( 'NONE', *, *, #16178, .T. ) ;
#89527 = VERTEX_POINT ( 'NONE', #39024 ) ;
#89528 = AXIS2_PLACEMENT_3D ( 'NONE', #76408, #1003, #76859 ) ;
#89529 = DIRECTION ( 'NONE',  ( 4.237773401492740281E-14, -1.000000000000000000, 0.000000000000000000 ) ) ;
#89530 = ORIENTED_EDGE ( 'NONE', *, *, #23285, .F. ) ;
#89531 = ORIENTED_EDGE ( 'NONE', *, *, #29932, .F. ) ;
#89532 = DIRECTION ( 'NONE',  ( -0.7071067811865274777, 0.7071067811865675568, -7.071067811865283048E-16 ) ) ;
#89533 = CARTESIAN_POINT ( 'NONE',  ( 115.8254304378072987, -31.73001405447006817, 14.23979235309599289 ) ) ;
#89534 = CYLINDRICAL_SURFACE ( 'NONE', #78262, 3.250000000000002665 ) ;
#89535 = CARTESIAN_POINT ( 'NONE',  ( 182.2300522401171179, -33.89581943343741699, 313.9678068554149490 ) ) ;
#89536 = CARTESIAN_POINT ( 'NONE',  ( 104.2579841207466984, -28.11985932224000351, 209.7619436376009787 ) ) ;
#89537 = CARTESIAN_POINT ( 'NONE',  ( 97.73303842741869119, -31.98671872394393034, 50.95276813305294183 ) ) ;
#89538 = CARTESIAN_POINT ( 'NONE',  ( 141.0235900724605642, -46.62589376934778329, -5.074374724089071087 ) ) ;
#89539 = VERTEX_POINT ( 'NONE', #73549 ) ;
#89540 = DIRECTION ( 'NONE',  ( -0.7071067811578587436, 0.7071067812152364018, 0.000000000000000000 ) ) ;
#89541 = ORIENTED_EDGE ( 'NONE', *, *, #65557, .T. ) ;
#89542 = CARTESIAN_POINT ( 'NONE',  ( 115.0878329645715468, -30.61624704198585434, 260.3439639102809338 ) ) ;
#89543 = ORIENTED_EDGE ( 'NONE', *, *, #48192, .F. ) ;
#89544 = DIRECTION ( 'NONE',  ( -0.7071067811865462405, 0.000000000000000000, 0.7071067811865486830 ) ) ;
#89545 = CARTESIAN_POINT ( 'NONE',  ( -12.49830498548568158, 80.89921386390227553, 117.8953739236498990 ) ) ;
#89546 = PLANE ( 'NONE',  #54778 ) ;
#89547 = VECTOR ( 'NONE', #54770, 1000.000000000000000 ) ;
#89548 = DIRECTION ( 'NONE',  ( -1.000000000000000078E-15, 1.000000000000000083E-30, 1.000000000000000000 ) ) ;
#89549 = ORIENTED_EDGE ( 'NONE', *, *, #44765, .T. ) ;
#89550 = CARTESIAN_POINT ( 'NONE',  ( 110.8024161898992190, -46.48594086123524960, 62.86705384733992474 ) ) ;
#89553 = ADVANCED_FACE ( 'NONE', ( #25856 ), #45820, .F. ) ;
#89552 = CARTESIAN_POINT ( 'NONE',  ( 89.37727808479104397, 70.52074417248462623, -95.16685018565999599 ) ) ;
#89551 = CARTESIAN_POINT ( 'NONE',  ( -71.09939861440099662, 20.32000000000000028, 177.8662485265279827 ) ) ;
#89554 = PLANE ( 'NONE',  #56817 ) ;
#89555 = DIRECTION ( 'NONE',  ( 0.000000000000000000, 0.000000000000000000, -1.000000000000000000 ) ) ;
#89556 = VERTEX_POINT ( 'NONE', #88093 ) ;
#89557 = CARTESIAN_POINT ( 'NONE',  ( 98.01104804690241679, -32.31685915242277929, 121.9642353160954684 ) ) ;
#89558 = CARTESIAN_POINT ( 'NONE',  ( 48.79742451362098166, -36.32844715994040996, -5.074374724088000832 ) ) ;
#89559 = CARTESIAN_POINT ( 'NONE',  ( 12.70000000000000107, 82.54999999999999716, 117.8738102209307641 ) ) ;
#89560 = ORIENTED_EDGE ( 'NONE', *, *, #2239, .F. ) ;
#89561 = CARTESIAN_POINT ( 'NONE',  ( 100.2845952792443569, -46.47769036989463132, 83.09276813305294240 ) ) ;
#89562 = VECTOR ( 'NONE', #52491, 1000.000000000000000 ) ;
#89564 = DIRECTION ( 'NONE',  ( -0.0001713722456127401463, 0.9999999853157766072, 1.713722456137401502E-19 ) ) ;
#89563 = CARTESIAN_POINT ( 'NONE',  ( 105.7165518034377811, -46.72402163992320823, 172.4654686376170218 ) ) ;
#89565 = CARTESIAN_POINT ( 'NONE',  ( 71.23990787207000608, 10.64204399490126463, 540.9756252759101471 ) ) ;
#89567 = EDGE_CURVE ( 'NONE', #17862, #67541, #62395, .T. ) ;
#89566 = AXIS2_PLACEMENT_3D ( 'NONE', #629, #34255, #84671 ) ;
#89568 = AXIS2_PLACEMENT_3D ( 'NONE', #80670, #67468, #39755 ) ;
#89569 = CARTESIAN_POINT ( 'NONE',  ( 141.9478362311689068, -91.32555531421861872, 248.3919668373590071 ) ) ;
#89570 = ORIENTED_EDGE ( 'NONE', *, *, #48109, .F. ) ;
#89571 = CARTESIAN_POINT ( 'NONE',  ( 117.0231039428182385, -39.62849705588580917, 134.5889586092439743 ) ) ;
#89573 = VERTEX_POINT ( 'NONE', #39916 ) ;
#89572 = DIRECTION ( 'NONE',  ( -2.973811673103097665E-16, 0.000000000000000000, -1.000000000000000000 ) ) ;
#89574 = CARTESIAN_POINT ( 'NONE',  ( 109.9831304889622743, -26.74336511273928707, 255.8499109901966051 ) ) ;
#89575 = DIRECTION ( 'NONE',  ( -1.000000000000000000, 0.000000000000000000, 0.000000000000000000 ) ) ;
#89576 = DIRECTION ( 'NONE',  ( 0.7071067811865480168, -0.7071067811865470176, 0.000000000000000000 ) ) ;
#89577 = CYLINDRICAL_SURFACE ( 'NONE', #47262, 0.5000000000000197620 ) ;
#89578 = DIRECTION ( 'NONE',  ( 1.000000000000000000, 0.000000000000000000, 0.000000000000000000 ) ) ;
#89579 = EDGE_CURVE ( 'NONE', #22726, #6301, #11782, .T. ) ;
#89580 = AXIS2_PLACEMENT_3D ( 'NONE', #26723, #19924, #75339 ) ;
#89581 = ADVANCED_FACE ( 'NONE', ( #32659, #24959, #38577 ), #81734, .F. ) ;
#89582 = DIRECTION ( 'NONE',  ( 0.000000000000000000, 0.000000000000000000, -1.000000000000000000 ) ) ;
#89583 = CARTESIAN_POINT ( 'NONE',  ( 124.0664832912757021, -36.72944715993921960, 14.92562527591098842 ) ) ;
#89584 = AXIS2_PLACEMENT_3D ( 'NONE', #63672, #36424, #35499 ) ;
#89586 = CARTESIAN_POINT ( 'NONE',  ( 97.99937763885726838, -40.39701179870337455, 206.6327681330539860 ) ) ;
#89585 = AXIS2_PLACEMENT_3D ( 'NONE', #55305, #83062, #50753 ) ;
#89587 = ORIENTED_EDGE ( 'NONE', *, *, #85909, .F. ) ;
#89588 = VERTEX_POINT ( 'NONE', #60809 ) ;
#89589 = CARTESIAN_POINT ( 'NONE',  ( 99.74964917879287896, -31.73022550229359595, 117.2815833058969446 ) ) ;
#89590 = VECTOR ( 'NONE', #48654, 1000.000000000000000 ) ;
#89591 = DIRECTION ( 'NONE',  ( 0.000000000000000000, 0.000000000000000000, 1.000000000000000000 ) ) ;
#89593 = CARTESIAN_POINT ( 'NONE',  ( 78.64819577385250682, -34.37139167075708457, 1.944749297858806125 ) ) ;
#89592 = CARTESIAN_POINT ( 'NONE',  ( 97.95230308628410398, -39.01119097033267025, 12.96539282970593554 ) ) ;
#89594 = CARTESIAN_POINT ( 'NONE',  ( 19.56648329127303043, 25.62155284005700295, 342.9256252759109884 ) ) ;
#89595 = EDGE_CURVE ( 'NONE', #29549, #10090, #19036, .T. ) ;
#89596 = DIRECTION ( 'NONE',  ( 0.000000000000000000, 0.000000000000000000, -1.000000000000000000 ) ) ;
#89597 = CARTESIAN_POINT ( 'NONE',  ( 50.87649884952465840, -33.54226604284966839, 313.9678068554150059 ) ) ;
#89598 = CARTESIAN_POINT ( 'NONE',  ( 181.8764988495240118, -33.54226604284930602, -5.074374724088000832 ) ) ;
#89599 = CARTESIAN_POINT ( 'NONE',  ( 93.47673478713714701, -35.56394370010534800, 302.6356252759109680 ) ) ;
#89600 = CARTESIAN_POINT ( 'NONE',  ( 106.3035372762157351, -47.10473409126657174, 222.5184824187679453 ) ) ;
#89601 = CARTESIAN_POINT ( 'NONE',  ( 63.56670390244745050, -47.82844715994014706, 129.9678068554150911 ) ) ;
#89602 = ORIENTED_EDGE ( 'NONE', *, *, #44758, .T. ) ;
#89604 = ORIENTED_EDGE ( 'NONE', *, *, #57985, .T. ) ;
#89603 = EDGE_CURVE ( 'NONE', #45956, #31479, #33412, .T. ) ;
#89605 = CARTESIAN_POINT ( 'NONE',  ( 45.56670390244500624, -48.82844715994099971, 249.9678068554150343 ) ) ;
#89606 = CARTESIAN_POINT ( 'NONE',  ( 82.26793483429007381, -20.38027623202287586, 7.385026757025396016 ) ) ;
#89607 = CARTESIAN_POINT ( 'NONE',  ( 104.4905352225451054, -26.97864795354891854, 185.2818706022724768 ) ) ;
#89608 = CARTESIAN_POINT ( 'NONE',  ( 19.56648329127400032, -18.82844715994099971, -5.074374724088000832 ) ) ;
#89609 = AXIS2_PLACEMENT_3D ( 'NONE', #20349, #339, #75758 ) ;
#89610 = VECTOR ( 'NONE', #53767, 1000.000000000000000 ) ;
#89611 = DIRECTION ( 'NONE',  ( 0.000000000000000000, 1.000000000000000000, 0.000000000000000000 ) ) ;
#89612 = ORIENTED_EDGE ( 'NONE', *, *, #3644, .F. ) ;
#89613 = CARTESIAN_POINT ( 'NONE',  ( 117.5558648759066926, -37.28717672647940873, 14.78419670448294454 ) ) ;
#89614 = CARTESIAN_POINT ( 'NONE',  ( 117.2277029493381377, -41.08016003417893103, 213.5165776568629781 ) ) ;
#89615 = VERTEX_POINT ( 'NONE', #4520 ) ;
#89616 = EDGE_CURVE ( 'NONE', #45346, #44762, #79799, .T. ) ;
#89617 = FACE_OUTER_BOUND ( 'NONE', #52373, .T. ) ;
#89619 = EDGE_CURVE ( 'NONE', #18344, #1069, #13067, .T. ) ;
#89618 = CYLINDRICAL_SURFACE ( 'NONE', #3655, 9.999999999999998224 ) ;
#89620 = CARTESIAN_POINT ( 'NONE',  ( 0.000000000000000000, 91.07499999999996021, 0.000000000000000000 ) ) ;
#89621 = EDGE_CURVE ( 'NONE', #15468, #33306, #46423, .T. ) ;
#89622 = CARTESIAN_POINT ( 'NONE',  ( 100.9805754248354788, -42.21072563198327998, 54.72809036959092310 ) ) ;
#89623 = CARTESIAN_POINT ( 'NONE',  ( 97.98816800684205930, -30.38363046389439859, 156.8289586092439549 ) ) ;
#89624 = CARTESIAN_POINT ( 'NONE',  ( 154.5667039024469886, -67.87844715994090450, 190.2178068554179902 ) ) ;
#89625 = VERTEX_POINT ( 'NONE', #59905 ) ;
#89626 = EDGE_CURVE ( 'NONE', #12205, #24335, #10879, .T. ) ;
#89627 = VECTOR ( 'NONE', #76341, 1000.000000000000000 ) ;
#89628 = FACE_OUTER_BOUND ( 'NONE', #14628, .T. ) ;
#89629 = CARTESIAN_POINT ( 'NONE',  ( 97.81315821180474757, -40.51681016098617505, 66.63608906629065132 ) ) ;
#89630 = ORIENTED_EDGE ( 'NONE', *, *, #31487, .F. ) ;
#89631 = ORIENTED_EDGE ( 'NONE', *, *, #47795, .F. ) ;
#89632 = AXIS2_PLACEMENT_3D ( 'NONE', #69237, #48764, #3765 ) ;
#89633 = FACE_OUTER_BOUND ( 'NONE', #50165, .T. ) ;
#89634 = ORIENTED_EDGE ( 'NONE', *, *, #56835, .T. ) ;
#89635 = ORIENTED_EDGE ( 'NONE', *, *, #78387, .T. ) ;
#89636 = CARTESIAN_POINT ( 'NONE',  ( 165.2725846195380086, -35.55794170701810941, -5.074374724088000832 ) ) ;
#89637 = CARTESIAN_POINT ( 'NONE',  ( 102.6518059180641416, -28.82227990381128180, 104.9162293518859599 ) ) ;
#89638 = CARTESIAN_POINT ( 'NONE',  ( 118.0743634110212383, -35.49574686983337557, 233.9032443235299752 ) ) ;
#89639 = VECTOR ( 'NONE', #16646, 1000.000000000000000 ) ;
#89640 = CARTESIAN_POINT ( 'NONE',  ( 107.5647246096319236, -47.74832088493825211, 192.6003871806729535 ) ) ;
#89642 = CARTESIAN_POINT ( 'NONE',  ( 116.3171286962602267, -41.53660429022799150, 284.4441967044824082 ) ) ;
#89641 = DIRECTION ( 'NONE',  ( -0.8660254037844420383, -0.4999999999999941158, 0.000000000000000000 ) ) ;
#89643 = FACE_OUTER_BOUND ( 'NONE', #79887, .T. ) ;
#89644 = CARTESIAN_POINT ( 'NONE',  ( 172.5664832912740110, -9.303447159940999356, 78.92562527591199739 ) ) ;
#89645 = AXIS2_PLACEMENT_3D ( 'NONE', #51294, #13330, #6509 ) ;
#89646 = EDGE_LOOP ( 'NONE', ( #82477, #73366, #50591, #71482 ) ) ;
#89647 = CIRCLE ( 'NONE', #62076, 1.000000000000000888 ) ;
#89648 = AXIS2_PLACEMENT_3D ( 'NONE', #51848, #10539, #52283 ) ;
#89649 = VECTOR ( 'NONE', #88916, 1000.000000000000000 ) ;
#89650 = CARTESIAN_POINT ( 'NONE',  ( 98.20607846729126322, -32.50961293922092210, 75.97276813305397525 ) ) ;
#89651 = CARTESIAN_POINT ( 'NONE',  ( 101.9388778781502509, -27.60177885026046596, 60.48419670448296159 ) ) ;
#89652 = CARTESIAN_POINT ( 'NONE',  ( 109.2210686807619453, -48.43357285789136313, 277.7213395616254843 ) ) ;
#89653 = ORIENTED_EDGE ( 'NONE', *, *, #54667, .T. ) ;
#89654 = CARTESIAN_POINT ( 'NONE',  ( 106.9404395787681352, -47.78219344473501451, 232.5794347997199907 ) ) ;
#89655 = CARTESIAN_POINT ( 'NONE',  ( 103.1875000000000000, 101.5999999999999943, 3.602774393244745134E-13 ) ) ;
#89656 = CARTESIAN_POINT ( 'NONE',  ( 0.000000000000000000, 0.000000000000000000, 0.000000000000000000 ) ) ;
#89657 = CARTESIAN_POINT ( 'NONE',  ( 117.0607179957026176, -38.08171581397471073, 24.71885727970600755 ) ) ;
#89658 = CARTESIAN_POINT ( 'NONE',  ( 188.5667039024479834, -58.35344715994099829, 139.9678068554150059 ) ) ;
#89661 = EDGE_CURVE ( 'NONE', #83042, #6555, #31766, .T. ) ;
#89660 = DIRECTION ( 'NONE',  ( 0.000000000000000000, 1.000000000000000000, 0.000000000000000000 ) ) ;
#89659 = CARTESIAN_POINT ( 'NONE',  ( 114.6549693520563835, -40.28990096540307775, 277.6356252759109111 ) ) ;
#89662 = CARTESIAN_POINT ( 'NONE',  ( 99.08963683242468790, -42.79560731373364035, 172.8439316841160291 ) ) ;
#89663 = CARTESIAN_POINT ( 'NONE',  ( 41.56670390244695312, -36.32844715994109208, 129.9678068554150911 ) ) ;
#89664 = CARTESIAN_POINT ( 'NONE',  ( 12.59756045763256260, 84.21337188079040459, -117.8848095194957750 ) ) ;
#89665 = CIRCLE ( 'NONE', #79551, 2.500000000000002220 ) ;
#89666 = LINE ( 'NONE', #20172, #61710 ) ;
#89667 = CARTESIAN_POINT ( 'NONE',  ( 102.0623058274917696, -27.97328479470368379, 40.48947073801728180 ) ) ;
#89668 = DIRECTION ( 'NONE',  ( 0.000000000000000000, 0.000000000000000000, 1.000000000000000000 ) ) ;
#89670 = EDGE_LOOP ( 'NONE', ( #297, #83371, #69505, #54260 ) ) ;
#89669 = FACE_OUTER_BOUND ( 'NONE', #27264, .T. ) ;
#89671 = CARTESIAN_POINT ( 'NONE',  ( 107.0664832912740110, -46.47944715994103149, 14.92562527591097066 ) ) ;
#89672 = CARTESIAN_POINT ( 'NONE',  ( 103.0820296961932456, -47.91685729158425744, 252.3041967044823366 ) ) ;
#89673 = CARTESIAN_POINT ( 'NONE',  ( 114.5121600660089030, -29.42679343410769377, 145.4441967044819819 ) ) ;
#89674 = CARTESIAN_POINT ( 'NONE',  ( 116.2568870038579547, -41.81614494787783798, 259.4241967044827106 ) ) ;
#89675 = LINE ( 'NONE', #26992, #31615 ) ;
#89676 = VECTOR ( 'NONE', #67806, 1000.000000000000000 ) ;
#89678 = LINE ( 'NONE', #5663, #19468 ) ;
#89677 = DIRECTION ( 'NONE',  ( 0.000000000000000000, 0.000000000000000000, 1.000000000000000000 ) ) ;
#89679 = DIRECTION ( 'NONE',  ( 2.108231265501709878E-16, 0.000000000000000000, -1.000000000000000000 ) ) ;
#89680 = AXIS2_PLACEMENT_3D ( 'NONE', #64495, #2271, #29973 ) ;
#89681 = DIRECTION ( 'NONE',  ( 1.000000000000000078E-15, -1.000000000000000000, 0.000000000000000000 ) ) ;
#89682 = ADVANCED_FACE ( 'NONE', ( #87638 ), #53066, .F. ) ;
#89683 = ORIENTED_EDGE ( 'NONE', *, *, #52841, .F. ) ;
#89684 = ADVANCED_FACE ( 'NONE', ( #21276, #7649, #82633, #33996, #28521, #34895, #62156, #89888, #61697, #35337, #63051, #6748, #62606, #27641, #55321, #48950, #831, #34446, #83076 ), #26739, .T. ) ;
#89685 = CARTESIAN_POINT ( 'NONE',  ( 107.0667039024470313, -104.2784471599420755, -19.78219314458201694 ) ) ;
#89686 = VERTEX_POINT ( 'NONE', #20394 ) ;
#89687 = CARTESIAN_POINT ( 'NONE',  ( 109.0154912191213583, -27.88557705556195998, 179.3143245899819647 ) ) ;
#89688 = ADVANCED_FACE ( 'NONE', ( #77145 ), #66744, .T. ) ;
#89690 = VERTEX_POINT ( 'NONE', #20830 ) ;
#89689 = LINE ( 'NONE', #76944, #47151 ) ;
#89691 = DIRECTION ( 'NONE',  ( 0.000000000000000000, 0.000000000000000000, -1.000000000000000000 ) ) ;
#89692 = CARTESIAN_POINT ( 'NONE',  ( 114.9485010938853122, -29.93956786141553295, 180.3927681330539770 ) ) ;
#89693 = DIRECTION ( 'NONE',  ( -0.7071067708032283683, -0.0001211784769705719365, 0.7071067811865527908 ) ) ;
#89694 = DIRECTION ( 'NONE',  ( 0.7071067811862239427, 0.7071067811868709807, 0.000000000000000000 ) ) ;
#89695 = EDGE_CURVE ( 'NONE', #1618, #65123, #380, .T. ) ;
#89696 = EDGE_CURVE ( 'NONE', #73407, #35831, #7206, .T. ) ;
#89697 = CARTESIAN_POINT ( 'NONE',  ( -92.32962665258561685, 81.72118090664557144, 74.36911441044701121 ) ) ;
#89698 = CARTESIAN_POINT ( 'NONE',  ( 160.2664750769284865, 0.000000000000000000, -148.0533267522753818 ) ) ;
#89699 = CARTESIAN_POINT ( 'NONE',  ( 118.1148702536304427, -35.48641528967804248, 83.91562527591095488 ) ) ;
#89700 = ORIENTED_EDGE ( 'NONE', *, *, #37965, .F. ) ;
#89701 = EDGE_LOOP ( 'NONE', ( #46125, #63381, #61848, #63312 ) ) ;
#89702 = VERTEX_POINT ( 'NONE', #28075 ) ;
#89703 = EDGE_CURVE ( 'NONE', #4701, #64147, #72592, .T. ) ;
#89704 = VECTOR ( 'NONE', #11236, 1000.000000000000000 ) ;
#89705 = AXIS2_PLACEMENT_3D ( 'NONE', #44502, #30892, #72234 ) ;
#89706 = DIRECTION ( 'NONE',  ( -0.9999999853157766072, -0.0001713722456134502174, 0.000000000000000000 ) ) ;
#89708 = DIRECTION ( 'NONE',  ( -3.100000000000000258E-29, 3.100000000000000044E-14, 1.000000000000000000 ) ) ;
#89707 = CARTESIAN_POINT ( 'NONE',  ( 113.6884830475838442, -29.53135334845051574, 195.4841967044819739 ) ) ;
#89709 = DIRECTION ( 'NONE',  ( -1.000000000000000000, 0.000000000000000000, 0.000000000000000000 ) ) ;
#89710 = EDGE_CURVE ( 'NONE', #21936, #59397, #72744, .T. ) ;
#89711 = CARTESIAN_POINT ( 'NONE',  ( 163.5667039024461360, -18.82844715994099971, 335.8679285791478719 ) ) ;
#89712 = CARTESIAN_POINT ( 'NONE',  ( 98.58946256649485917, -108.5954344580498514, -19.78219314458187839 ) ) ;
#89713 = VECTOR ( 'NONE', #4128, 1000.000000000000000 ) ;
#89714 = DIRECTION ( 'NONE',  ( -4.554376769437570034E-14, 1.000000000000000000, 0.000000000000000000 ) ) ;
#89715 = CARTESIAN_POINT ( 'NONE',  ( 67.55352479590314374, -68.34655798362497592, 246.8010709169019776 ) ) ;
#89716 = CARTESIAN_POINT ( 'NONE',  ( 116.5783909117432842, -29.70293872869703833, 109.3327681330539605 ) ) ;
#89717 = ORIENTED_EDGE ( 'NONE', *, *, #50711, .F. ) ;
#89718 = ORIENTED_EDGE ( 'NONE', *, *, #8349, .F. ) ;
#89720 = ORIENTED_EDGE ( 'NONE', *, *, #971, .F. ) ;
#89719 = ADVANCED_FACE ( 'NONE', ( #8098 ), #75798, .F. ) ;
#89721 = VECTOR ( 'NONE', #11141, 1000.000000000000000 ) ;
#89722 = DIRECTION ( 'NONE',  ( 1.000000000000000000, 4.272717921125132861E-14, 0.000000000000000000 ) ) ;
#89723 = CARTESIAN_POINT ( 'NONE',  ( -94.61838531165716404, 94.82199753261676278, -89.95770503246875194 ) ) ;
#89724 = AXIS2_PLACEMENT_3D ( 'NONE', #57061, #84805, #77981 ) ;
#89725 = AXIS2_PLACEMENT_3D ( 'NONE', #21743, #9009, #64408 ) ;
#89726 = DIRECTION ( 'NONE',  ( 1.000000000000000078E-15, -1.000000000000000000, 0.000000000000000000 ) ) ;
#89727 = CARTESIAN_POINT ( 'NONE',  ( 98.90610402553750191, -36.53467484046868208, 194.1252332267349630 ) ) ;
#89728 = DIRECTION ( 'NONE',  ( -1.000000000000000000, -1.000000000000000078E-15, 0.000000000000000000 ) ) ;
#89729 = ORIENTED_EDGE ( 'NONE', *, *, #86349, .F. ) ;
#89731 = VERTEX_POINT ( 'NONE', #47619 ) ;
#89730 = ORIENTED_EDGE ( 'NONE', *, *, #76253, .F. ) ;
#89732 = VECTOR ( 'NONE', #32, 1000.000000000000227 ) ;
#89733 = DIRECTION ( 'NONE',  ( -0.7071067811865453523, -0.7071067811865496822, 0.000000000000000000 ) ) ;
#89734 = ORIENTED_EDGE ( 'NONE', *, *, #642, .T. ) ;
#89735 = EDGE_LOOP ( 'NONE', ( #3978, #25474, #25769, #51402, #87655, #64584 ) ) ;
#89736 = DIRECTION ( 'NONE',  ( 0.000000000000000000, 0.000000000000000000, 1.000000000000000000 ) ) ;
#89737 = EDGE_CURVE ( 'NONE', #73246, #86684, #13130, .T. ) ;
#89738 = CARTESIAN_POINT ( 'NONE',  ( 109.5509076938284068, -28.22321920626787062, 256.2815833058970725 ) ) ;
#89739 = ORIENTED_EDGE ( 'NONE', *, *, #66737, .F. ) ;
#89740 = EDGE_CURVE ( 'NONE', #78028, #13668, #30503, .T. ) ;
#89741 = VECTOR ( 'NONE', #48125, 1000.000000000000000 ) ;
#89742 = CYLINDRICAL_SURFACE ( 'NONE', #37780, 1.000000000002049694 ) ;
#89743 = AXIS2_PLACEMENT_3D ( 'NONE', #43303, #24223, #10579 ) ;
#89744 = CARTESIAN_POINT ( 'NONE',  ( -125.7768780727897564, 67.25820441060064070, 35.00145722608366583 ) ) ;
#89745 = ORIENTED_EDGE ( 'NONE', *, *, #68550, .F. ) ;
#89746 = ORIENTED_EDGE ( 'NONE', *, *, #12450, .F. ) ;
#89747 = DIRECTION ( 'NONE',  ( 1.000000000000000000, -1.040834085586083310E-14, 0.000000000000000000 ) ) ;
#89748 = ORIENTED_EDGE ( 'NONE', *, *, #54366, .T. ) ;
#89749 = ORIENTED_EDGE ( 'NONE', *, *, #68561, .F. ) ;
#89750 = CARTESIAN_POINT ( 'NONE',  ( 111.8846140958497273, -43.31847907419767552, 225.8966617981629668 ) ) ;
#89751 = CARTESIAN_POINT ( 'NONE',  ( 99.66888285774223277, -46.01973906766702527, 122.0413395616249659 ) ) ;
#89752 = CARTESIAN_POINT ( 'NONE',  ( 106.0785370228624913, -48.51385081415340750, 112.5099109901969712 ) ) ;
#89753 = CARTESIAN_POINT ( 'NONE',  ( 99.04337972803247681, -36.17635250646264922, 249.5838068554172935 ) ) ;
#89754 = CARTESIAN_POINT ( 'NONE',  ( 133.1188885517785252, -16.14703303315377525, 8.087249882924000488 ) ) ;
#89755 = CARTESIAN_POINT ( 'NONE',  ( 102.6835365363430981, -27.27046913952221985, 176.4213395616249898 ) ) ;
#89756 = CARTESIAN_POINT ( 'NONE',  ( 179.1667039024460166, -26.71338133339251542, -5.074374724088000832 ) ) ;
#89757 = CARTESIAN_POINT ( 'NONE',  ( 97.31588835286031269, -39.30608500589924148, 127.5314679824783894 ) ) ;
#89758 = VERTEX_POINT ( 'NONE', #71234 ) ;
#89759 = CARTESIAN_POINT ( 'NONE',  ( 130.0912141755840423, 76.20343663217360586, 11.00834544827310779 ) ) ;
#89760 = ORIENTED_EDGE ( 'NONE', *, *, #52378, .F. ) ;
#89761 = CIRCLE ( 'NONE', #11414, 34.13125000000000142 ) ;
#89762 = EDGE_LOOP ( 'NONE', ( #45362, #7237, #17108, #20927 ) ) ;
#89763 = CARTESIAN_POINT ( 'NONE',  ( 33.78129701732998313, -35.65087443492610930, 313.9678068554150059 ) ) ;
#89764 = ORIENTED_EDGE ( 'NONE', *, *, #62679, .T. ) ;
#89765 = B_SPLINE_CURVE_WITH_KNOTS ( 'NONE', 3,
 ( #15805, #63490, #28981, #36695, #820, #64395, #44375, #28510, #72105, #15360, #35777, #23083, #43927, #36239, #51188, #56667, #56204, #83955, #21726, #85754, #71664, #63949, #49847, #84411, #37138, #64840, #9879, #1728, #30325, #50296, #77574, #49398 ),
 .UNSPECIFIED., .F., .F.,
 ( 4, 2, 2, 2, 2, 2, 2, 2, 2, 2, 2, 2, 2, 2, 2, 4 ),
 ( 0.01900920079883068256, 0.02107412302369412668, 0.02210658413612584527, 0.02313904524855756734, 0.02520396747342101146, 0.02623642858585272311, 0.02726888969828443129, 0.02933381192314784419, 0.03139873414801125362, 0.03552857859773811411, 0.03759350082260152354, 0.03965842304746493296, 0.04378826749719177958, 0.04585318972205519594, 0.04791811194691859843, 0.05204795639664543117 ),
 .UNSPECIFIED. ) ;
#89766 = CIRCLE ( 'NONE', #31706, 10.00000000000000888 ) ;
#89767 = DIRECTION ( 'NONE',  ( 1.000000000000000000, 1.000000000000000078E-15, 0.000000000000000000 ) ) ;
#89768 = CARTESIAN_POINT ( 'NONE',  ( 117.6081704542122282, -33.40500446796587397, 129.0575300378159795 ) ) ;
#89769 = CARTESIAN_POINT ( 'NONE',  ( -11.41630163197954495, 76.98248777262077169, 130.0559678743007055 ) ) ;
#89770 = LINE ( 'NONE', #27081, #33362 ) ;
#89771 = LINE ( 'NONE', #5299, #13643 ) ;
#89774 = CARTESIAN_POINT ( 'NONE',  ( 97.42226921825846375, -40.63044708855864684, 202.6327681330539860 ) ) ;
#89773 = DIRECTION ( 'NONE',  ( 0.000000000000000000, 0.000000000000000000, 1.000000000000000000 ) ) ;
#89772 = CARTESIAN_POINT ( 'NONE',  ( 100.8874678748097296, -44.70022136769403431, 143.0522919416148966 ) ) ;
#89775 = DIRECTION ( 'NONE',  ( 4.299999999999999979E-14, -1.000000000000000000, 4.400000000000000367E-29 ) ) ;
#89776 = CARTESIAN_POINT ( 'NONE',  ( 63.06670390244700997, -79.67844715994098692, 155.2178068554179902 ) ) ;
#89777 = ORIENTED_EDGE ( 'NONE', *, *, #11254, .F. ) ;
#89778 = DIRECTION ( 'NONE',  ( 0.000000000000000000, 0.000000000000000000, 1.000000000000000000 ) ) ;
#89779 = DIRECTION ( 'NONE',  ( -0.9999999853157766072, -0.0001713722456143218888, 0.000000000000000000 ) ) ;
#89780 = CARTESIAN_POINT ( 'NONE',  ( 184.5664832912729878, -71.37844715994266664, 342.9256252759109884 ) ) ;
#89781 = AXIS2_PLACEMENT_3D ( 'NONE', #23797, #44201, #59175 ) ;
#89782 = DIRECTION ( 'NONE',  ( 0.9834602067019604377, 0.1811243270069963496, 0.000000000000000000 ) ) ;
#89784 = ORIENTED_EDGE ( 'NONE', *, *, #87252, .F. ) ;
#89783 = CARTESIAN_POINT ( 'NONE',  ( 95.18116725028646385, -37.33612674980418689, 271.3670538473392639 ) ) ;
#89785 = LINE ( 'NONE', #13029, #66912 ) ;
#89786 = CARTESIAN_POINT ( 'NONE',  ( 96.61975328461473111, -36.61901104994432643, 111.3184824187679567 ) ) ;
#89787 = CARTESIAN_POINT ( 'NONE',  ( 103.4771999316985500, -25.43557003456049870, 51.32133956162493149 ) ) ;
#89788 = CARTESIAN_POINT ( 'NONE',  ( 95.86339321018937198, -32.71673170297378164, 172.0527681330539735 ) ) ;
#89789 = DIRECTION ( 'NONE',  ( -0.9254794337955620787, -0.3787978585227822492, 0.000000000000000000 ) ) ;
#89790 = AXIS2_PLACEMENT_3D ( 'NONE', #8555, #36709, #2640 ) ;
#89791 = DIRECTION ( 'NONE',  ( 0.4999999999999995004, 0.000000000000000000, 0.8660254037844390407 ) ) ;
#89792 = EDGE_CURVE ( 'NONE', #29468, #61133, #22635, .T. ) ;
#89794 = LINE ( 'NONE', #27547, #26867 ) ;
#89793 = PLANE ( 'NONE',  #5718 ) ;
#89795 = LINE ( 'NONE', #13038, #68450 ) ;
#89796 = DIRECTION ( 'NONE',  ( 9.912705577010326536E-16, 1.000000000000000000, 0.000000000000000000 ) ) ;
#89797 = ORIENTED_EDGE ( 'NONE', *, *, #62383, .F. ) ;
#89798 = EDGE_CURVE ( 'NONE', #3392, #3093, #47858, .T. ) ;
#89799 = ORIENTED_EDGE ( 'NONE', *, *, #38865, .F. ) ;
#89800 = EDGE_CURVE ( 'NONE', #53148, #45118, #60015, .T. ) ;
#89801 = ORIENTED_EDGE ( 'NONE', *, *, #31824, .T. ) ;
#89802 = VECTOR ( 'NONE', #51628, 1000.000000000000000 ) ;
#89803 = ADVANCED_FACE ( 'NONE', ( #84422 ), #20336, .T. ) ;
#89804 = ORIENTED_EDGE ( 'NONE', *, *, #14113, .F. ) ;
#89805 = CARTESIAN_POINT ( 'NONE',  ( 97.81168148112675453, -40.51739256386586163, 162.6360428395636859 ) ) ;
#89806 = CARTESIAN_POINT ( 'NONE',  ( 96.10063762778156615, -37.91858611869021445, 77.40038718067299328 ) ) ;
#89807 = B_SPLINE_CURVE_WITH_KNOTS ( 'NONE', 3,
 ( #74987, #41339, #47257, #69071, #15007, #44028, #22725, #9533, #64055, #22275, #70422, #9094, #49950, #77236, #64942, #15907, #64500, #35431 ),
 .UNSPECIFIED., .F., .F.,
 ( 4, 2, 2, 2, 2, 2, 2, 2, 4 ),
 ( 0.4999048021866459024, 0.5624167019133151646, 0.6249286016399844268, 0.6874405013666536890, 0.7499524010933229512, 0.8124643008199922134, 0.8749762005466614756, 0.9374881002733307378, 1.000000000000000000 ),
 .UNSPECIFIED. ) ;
#89808 = DIRECTION ( 'NONE',  ( 0.000000000000000000, 0.000000000000000000, -1.000000000000000000 ) ) ;
#89809 = CARTESIAN_POINT ( 'NONE',  ( 114.2868575967315223, -43.69575777765361124, 118.2174201252820751 ) ) ;
#89810 = EDGE_CURVE ( 'NONE', #61107, #31976, #71113, .T. ) ;
#89811 = CARTESIAN_POINT ( 'NONE',  ( 97.63545021146504155, -41.27351965004424983, 167.6841967044829573 ) ) ;
#89812 = DIRECTION ( 'NONE',  ( -0.7071067811865765496, 0.7071067811865185959, -7.071067811865773128E-16 ) ) ;
#89813 = CARTESIAN_POINT ( 'NONE',  ( 115.6077113496922948, -36.78907078068826308, 263.2438483995052820 ) ) ;
#89814 = ORIENTED_EDGE ( 'NONE', *, *, #55706, .T. ) ;
#89815 = AXIS2_PLACEMENT_3D ( 'NONE', #38507, #18066, #38956 ) ;
#89816 = ORIENTED_EDGE ( 'NONE', *, *, #74025, .F. ) ;
#89817 = ORIENTED_EDGE ( 'NONE', *, *, #59260, .T. ) ;
#89818 = EDGE_CURVE ( 'NONE', #47880, #80299, #51962, .T. ) ;
#89819 = DIRECTION ( 'NONE',  ( -1.000000000000000078E-15, 1.000000000000000083E-30, 1.000000000000000000 ) ) ;
#89820 = CARTESIAN_POINT ( 'NONE',  ( 110.0667047667142953, -67.87844715994094713, 93.21780685541800437 ) ) ;
#89821 = CARTESIAN_POINT ( 'NONE',  ( 104.4909048318107381, -26.97854783814448965, 20.28044007747010014 ) ) ;
#89822 = CARTESIAN_POINT ( 'NONE',  ( 97.07198150990170404, -35.37932431885595008, 276.2185944750585236 ) ) ;
#89823 = DIRECTION ( 'NONE',  ( 3.100000000000000258E-29, -3.100000000000000044E-14, -1.000000000000000000 ) ) ;
#89824 = ADVANCED_FACE ( 'NONE', ( #86970 ), #73319, .F. ) ;
#89825 = CARTESIAN_POINT ( 'NONE',  ( -492.0614999999999668, 14.28750000000026077, 15.87499999999969802 ) ) ;
#89826 = CARTESIAN_POINT ( 'NONE',  ( 106.5394234437989667, -24.24056378642895737, 322.0356252759110021 ) ) ;
#89827 = CARTESIAN_POINT ( 'NONE',  ( 106.2788006184939888, -47.06957971430152554, 267.5280062282925542 ) ) ;
#89828 = DIRECTION ( 'NONE',  ( -0.7071067811865476838, -0.7071067811865473507, 0.000000000000000000 ) ) ;
#89830 = ORIENTED_EDGE ( 'NONE', *, *, #56240, .F. ) ;
#89829 = ADVANCED_FACE ( 'NONE', ( #11093, #36706, #31091 ), #1287, .F. ) ;
#89831 = VECTOR ( 'NONE', #71460, 1000.000000000000000 ) ;
#89832 = LINE ( 'NONE', #81673, #57724 ) ;
#89833 = CARTESIAN_POINT ( 'NONE',  ( -53.92625078532105931, 53.97500000000000142, 70.79999999999999716 ) ) ;
#89834 = CARTESIAN_POINT ( 'NONE',  ( 111.3320211711901067, -29.76992759232029329, 92.45666179816296903 ) ) ;
#89835 = CIRCLE ( 'NONE', #50640, 2.117000000000007987 ) ;
#89836 = AXIS2_PLACEMENT_3D ( 'NONE', #52035, #50373, #17550 ) ;
#89837 = CARTESIAN_POINT ( 'NONE',  ( 46.32460016641643108, -48.34074026909789268, 129.9678068554150911 ) ) ;
#89838 = DIRECTION ( 'NONE',  ( 0.000000000000000000, 0.000000000000000000, -1.000000000000000000 ) ) ;
#89839 = ORIENTED_EDGE ( 'NONE', *, *, #58078, .T. ) ;
#89840 = AXIS2_PLACEMENT_3D ( 'NONE', #39999, #74529, #75435 ) ;
#89841 = CARTESIAN_POINT ( 'NONE',  ( 77.40046754268342966, -36.03188136815408171, 6.871351212842532696 ) ) ;
#89842 = ORIENTED_EDGE ( 'NONE', *, *, #30302, .F. ) ;
#89843 = CARTESIAN_POINT ( 'NONE',  ( 109.2014631304945027, -26.52509060526352869, 139.9127681330539872 ) ) ;
#89844 = ORIENTED_EDGE ( 'NONE', *, *, #20254, .T. ) ;
#89845 = DIRECTION ( 'NONE',  ( 3.339108161477000479E-13, -1.000000000000000000, 6.848429599184487071E-29 ) ) ;
#89846 = CARTESIAN_POINT ( 'NONE',  ( 115.4287739208600527, -39.66208659201188880, 129.9901547344679500 ) ) ;
#89847 = FACE_OUTER_BOUND ( 'NONE', #59281, .T. ) ;
#89848 = EDGE_CURVE ( 'NONE', #26191, #71530, #34706, .T. ) ;
#89849 = DIRECTION ( 'NONE',  ( -1.000000000000000000, -4.299999999999999979E-14, -1.000000000000000078E-15 ) ) ;
#89850 = CARTESIAN_POINT ( 'NONE',  ( 118.0249073071387471, -38.34132458482030614, 69.72229194257801055 ) ) ;
#89851 = CARTESIAN_POINT ( 'NONE',  ( 151.0371591254582313, -46.82818131005593187, 313.9678068554149490 ) ) ;
#89852 = ORIENTED_EDGE ( 'NONE', *, *, #622, .F. ) ;
#89853 = LINE ( 'NONE', #88947, #51245 ) ;
#89854 = ORIENTED_EDGE ( 'NONE', *, *, #29375, .F. ) ;
#89855 = EDGE_LOOP ( 'NONE', ( #79305, #12085 ) ) ;
#89856 = VECTOR ( 'NONE', #26066, 1000.000000000000000 ) ;
#89857 = VECTOR ( 'NONE', #56320, 1000.000000000000000 ) ;
#89858 = DIRECTION ( 'NONE',  ( 1.000000000000000078E-15, 0.000000000000000000, -1.000000000000000000 ) ) ;
#89859 = ORIENTED_EDGE ( 'NONE', *, *, #48623, .F. ) ;
#89860 = CARTESIAN_POINT ( 'NONE',  ( 106.8506556707805260, -46.50783423188027399, 272.5584824187685626 ) ) ;
#89861 = CARTESIAN_POINT ( 'NONE',  ( 95.54549022710490647, -39.60850420455695087, 162.5213395616259788 ) ) ;
#89862 = CARTESIAN_POINT ( 'NONE',  ( 4.481911866145203760, 70.65984535152513502, -118.4718773200152384 ) ) ;
#89863 = CARTESIAN_POINT ( 'NONE',  ( 109.6410330058590716, -46.48058483609847968, 128.7812978340938912 ) ) ;
#89864 = CARTESIAN_POINT ( 'NONE',  ( 117.5953528424095254, -42.16796915894857278, 89.44705384733997278 ) ) ;
#89865 = DIRECTION ( 'NONE',  ( 1.000000000000000000, 0.000000000000000000, 0.000000000000000000 ) ) ;
#89866 = EDGE_LOOP ( 'NONE', ( #69823, #34715, #53157, #30743 ) ) ;
#89867 = DIRECTION ( 'NONE',  ( 0.000000000000000000, 0.000000000000000000, 1.000000000000000000 ) ) ;
#89868 = EDGE_CURVE ( 'NONE', #43983, #72685, #17473, .T. ) ;
#89869 = DIRECTION ( 'NONE',  ( 0.000000000000000000, 0.000000000000000000, -1.000000000000000000 ) ) ;
#89871 = VERTEX_POINT ( 'NONE', #17909 ) ;
#89870 = AXIS2_PLACEMENT_3D ( 'NONE', #82459, #75630, #12505 ) ;
#89872 = EDGE_CURVE ( 'NONE', #5834, #2213, #35897, .T. ) ;
#89873 = DIRECTION ( 'NONE',  ( 0.000000000000000000, 0.000000000000000000, -1.000000000000000000 ) ) ;
#89874 = APPLICATION_CONTEXT ( 'automotive_design' ) ;
#89875 = DIRECTION ( 'NONE',  ( 0.000000000000000000, 0.000000000000000000, -1.000000000000000000 ) ) ;
#89876 = CARTESIAN_POINT ( 'NONE',  ( 105.0259480979001410, -25.88970440745768542, 280.2365776568631759 ) ) ;
#89877 = LINE ( 'NONE', #12665, #34449 ) ;
#89878 = CARTESIAN_POINT ( 'NONE',  ( 188.5667039024479834, -62.87844715994099687, 178.0928068554149775 ) ) ;
#89879 = CARTESIAN_POINT ( 'NONE',  ( 101.9945362158859155, -45.44663583214662594, 92.15693711078462513 ) ) ;
#89880 = CARTESIAN_POINT ( 'NONE',  ( 105.4283229756613309, -27.08692670426131954, 15.20991099019697401 ) ) ;
#89882 = CARTESIAN_POINT ( 'NONE',  ( 112.7897778137181746, -47.07797880090539167, 98.97848241876793907 ) ) ;
#89881 = FACE_OUTER_BOUND ( 'NONE', #21325, .T. ) ;
#89883 = CARTESIAN_POINT ( 'NONE',  ( 57.56670390244829605, -48.82844715994039575, 293.2178068554150627 ) ) ;
#89884 = CARTESIAN_POINT ( 'NONE',  ( 108.0109225731970213, -26.30163847990888826, 155.0041967044819557 ) ) ;
#89885 = CARTESIAN_POINT ( 'NONE',  ( 71.06670390244701707, -83.77844715994098124, 55.21780685541800437 ) ) ;
#89886 = ORIENTED_EDGE ( 'NONE', *, *, #72216, .T. ) ;
#89887 = CARTESIAN_POINT ( 'NONE',  ( 25.56670390244797275, -48.82844715994099971, 173.2178068554149775 ) ) ;
#89888 = FACE_BOUND ( 'NONE', #11852, .T. ) ;
#89889 = CARTESIAN_POINT ( 'NONE',  ( 136.5183630979163638, -35.48272428400311895, 2.716753546981010903 ) ) ;
#89890 = ORIENTED_EDGE ( 'NONE', *, *, #87544, .F. ) ;
#89891 = VECTOR ( 'NONE', #79961, 1000.000000000000114 ) ;
#89892 = CARTESIAN_POINT ( 'NONE',  ( 48.86082318535681424, -35.55794170701784651, 237.4678068554150059 ) ) ;
#89894 = VERTEX_POINT ( 'NONE', #20163 ) ;
#89893 = CARTESIAN_POINT ( 'NONE',  ( 99.38968898744698777, -27.63536841754259044, 150.6356252759109680 ) ) ;
#89896 = CARTESIAN_POINT ( 'NONE',  ( 173.9900000000000091, 52.73749999999999716, -36.51250000000000284 ) ) ;
#89895 = PRODUCT_DEFINITION_CONTEXT ( 'detailed design', #23172, 'design' ) ;
#89897 = CARTESIAN_POINT ( 'NONE',  ( 110.1438736645959580, -26.08919931346192911, 210.8403871806729626 ) ) ;
#89898 = CARTESIAN_POINT ( 'NONE',  ( 86.93292302958541029, 72.22361908171428979, 97.40459591070944612 ) ) ;
#89899 = LINE ( 'NONE', #13140, #79376 ) ;
#89901 = DIRECTION ( 'NONE',  ( 3.100000000000000258E-29, -3.100000000000000044E-14, -1.000000000000000000 ) ) ;
#89900 = VECTOR ( 'NONE', #8771, 999.9999999999998863 ) ;
#89902 = ORIENTED_EDGE ( 'NONE', *, *, #56428, .T. ) ;
#89903 = ADVANCED_FACE ( 'NONE', ( #40592 ), #26973, .F. ) ;
#89904 = EDGE_LOOP ( 'NONE', ( #31411, #79118 ) ) ;
#89905 = ADVANCED_FACE ( 'NONE', ( #19703 ), #53297, .F. ) ;
#89906 = ORIENTED_EDGE ( 'NONE', *, *, #85099, .T. ) ;
#89907 = CIRCLE ( 'NONE', #42016, 5.035202529042049235 ) ;
#89908 = EDGE_CURVE ( 'NONE', #76564, #57999, #43584, .T. ) ;
#89909 = VERTEX_POINT ( 'NONE', #89206 ) ;
#89910 = CYLINDRICAL_SURFACE ( 'NONE', #35066, 13.44999999999999396 ) ;
#89911 = CARTESIAN_POINT ( 'NONE',  ( 108.1817661827909376, -47.09470796318245078, 198.6613395616249989 ) ) ;
#89912 = CARTESIAN_POINT ( 'NONE',  ( 98.10600417527815864, -32.16171936412747101, 250.9518541729705987 ) ) ;
#89913 = DIRECTION ( 'NONE',  ( -1.000000000000000000, 6.036837696399451257E-13, 0.000000000000000000 ) ) ;
#89914 =( GEOMETRIC_REPRESENTATION_CONTEXT ( 3 ) GLOBAL_UNCERTAINTY_ASSIGNED_CONTEXT ( ( #8778 ) ) GLOBAL_UNIT_ASSIGNED_CONTEXT ( ( #5078, #12346, #80497 ) ) REPRESENTATION_CONTEXT ( 'NONE', 'WORKASPACE' ) );
#89915 = ADVANCED_FACE ( 'NONE', ( #82402 ), #66959, .T. ) ;
#89916 = AXIS2_PLACEMENT_3D ( 'NONE', #36782, #43124, #8638 ) ;
#89918 = CARTESIAN_POINT ( 'NONE',  ( 188.5667039024479834, -67.87844715994100397, 252.3428068554150059 ) ) ;
#89917 = DIRECTION ( 'NONE',  ( 1.000000000000000000, 0.000000000000000000, -1.365069428641121829E-15 ) ) ;
#89919 = DIRECTION ( 'NONE',  ( -0.7071067811865477948, 0.7071067811865473507, 0.000000000000000000 ) ) ;
#89920 = ORIENTED_EDGE ( 'NONE', *, *, #1168, .F. ) ;
#89921 = ORIENTED_EDGE ( 'NONE', *, *, #9959, .T. ) ;
#89922 = AXIS2_PLACEMENT_3D ( 'NONE', #67778, #17839, #60962 ) ;
#89923 = CARTESIAN_POINT ( 'NONE',  ( 103.8797721312301547, -106.6957733451320394, 2.217806855418086087 ) ) ;
#89924 = CARTESIAN_POINT ( 'NONE',  ( 87.06648329127403940, -54.72944906728955061, -4.824374724089049771 ) ) ;
#89925 = CARTESIAN_POINT ( 'NONE',  ( 117.3624379696766198, -35.49166588079122420, 234.9337205140059552 ) ) ;
#89926 = EDGE_CURVE ( 'NONE', #12869, #10387, #32419, .T. ) ;
#89927 = DIRECTION ( 'NONE',  ( 0.9242245927363026414, 0.3818493186865932754, 0.000000000000000000 ) ) ;
#89928 = CARTESIAN_POINT ( 'NONE',  ( 102.8368274790083490, -27.91052165842139487, 91.43276813305296002 ) ) ;
#89929 = DIRECTION ( 'NONE',  ( -2.081668171172166620E-14, -1.000000000000000000, 0.000000000000000000 ) ) ;
#89930 = CARTESIAN_POINT ( 'NONE',  ( 113.5912987900053110, -29.06716993070983435, 20.51551907639133887 ) ) ;
#89931 = EDGE_LOOP ( 'NONE', ( #81527, #31745, #12519, #18581 ) ) ;
#89932 = VERTEX_POINT ( 'NONE', #76010 ) ;
#89933 = NEXT_ASSEMBLY_USAGE_OCCURRENCE ( 'NAUO1', ' ', ' ', #76646, #57145, $ ) ;
#89934 = NEXT_ASSEMBLY_USAGE_OCCURRENCE ( 'NAUO2', ' ', ' ', #76646, #61043, $ ) ;
#89935 = NEXT_ASSEMBLY_USAGE_OCCURRENCE ( 'NAUO3', ' ', ' ', #76646, #3331, $ ) ;
#89936 = NEXT_ASSEMBLY_USAGE_OCCURRENCE ( 'NAUO4', ' ', ' ', #76646, #32744, $ ) ;
#89937 = NEXT_ASSEMBLY_USAGE_OCCURRENCE ( 'NAUO5', ' ', ' ', #76646, #1182, $ ) ;
#89938 = NEXT_ASSEMBLY_USAGE_OCCURRENCE ( 'NAUO6', ' ', ' ', #76646, #61649, $ ) ;
#89939 = NEXT_ASSEMBLY_USAGE_OCCURRENCE ( 'NAUO7', ' ', ' ', #76646, #80551, $ ) ;
#89940 = NEXT_ASSEMBLY_USAGE_OCCURRENCE ( 'NAUO8', ' ', ' ', #76646, #3331, $ ) ;
#89941 = NEXT_ASSEMBLY_USAGE_OCCURRENCE ( 'NAUO9', ' ', ' ', #76646, #61043, $ ) ;
#89942 = NEXT_ASSEMBLY_USAGE_OCCURRENCE ( 'NAUO10', ' ', ' ', #76646, #3331, $ ) ;
#89943 = NEXT_ASSEMBLY_USAGE_OCCURRENCE ( 'NAUO11', ' ', ' ', #76646, #3331, $ ) ;
#89944 = NEXT_ASSEMBLY_USAGE_OCCURRENCE ( 'NAUO12', ' ', ' ', #76646, #61043, $ ) ;
#89945 = NEXT_ASSEMBLY_USAGE_OCCURRENCE ( 'NAUO13', ' ', ' ', #76646, #61043, $ ) ;
#89946 = NEXT_ASSEMBLY_USAGE_OCCURRENCE ( 'NAUO14', ' ', ' ', #76646, #69989, $ ) ;
#89947 = NEXT_ASSEMBLY_USAGE_OCCURRENCE ( 'NAUO15', ' ', ' ', #76646, #68346, $ ) ;
ENDSEC;
END-ISO-10303-21;
